#113266=DIRECTION('ref_axis',(-3.30569703989997E-8,0.289344971519085,-0.957224888652932));
#113267=DIRECTION('',(-6.19323182390956E-32,-1.23467863058847E-16,1.));
#113268=DIRECTION('center_axis',(0.997110719027039,-0.0759619154585161,
-3.74333490112874E-5));
#113269=DIRECTION('ref_axis',(0.0746245599506448,0.979463680395188,0.187302092457309));
#113270=DIRECTION('center_axis',(0.,0.,-1.));
#113271=DIRECTION('ref_axis',(-1.,0.,0.));
#113272=DIRECTION('center_axis',(-0.0109863751058524,0.174010750210057,
-0.984682465759072));
#113273=DIRECTION('ref_axis',(0.115492347803954,-0.977930751386158,-0.174106183382538));
#113274=DIRECTION('center_axis',(1.,-5.01606788234257E-16,0.));
#113275=DIRECTION('ref_axis',(-5.01606788234257E-16,-1.,0.));
#113276=DIRECTION('',(6.19323182390956E-32,1.23467863058847E-16,-1.));
#113277=DIRECTION('center_axis',(1.,0.,0.));
#113278=DIRECTION('ref_axis',(0.,0.97773854081723,0.20982694250404));
#113279=DIRECTION('',(6.19323182390956E-32,1.23467863058847E-16,-1.));
#113280=DIRECTION('center_axis',(0.,0.,-1.));
#113281=DIRECTION('ref_axis',(-1.,0.,0.));
#113282=DIRECTION('center_axis',(0.,0.,-1.));
#113283=DIRECTION('ref_axis',(-1.,0.,0.));
#113284=DIRECTION('center_axis',(-0.998403025832976,0.0564924526119683,
2.83803315785685E-5));
#113285=DIRECTION('ref_axis',(0.0553351197097672,0.977847823027442,0.201870402801399));
#113286=DIRECTION('center_axis',(0.,-1.18842113532926E-16,1.));
#113287=DIRECTION('ref_axis',(0.,1.,1.18842113532926E-16));
#113288=DIRECTION('center_axis',(-1.73309037721552E-31,1.19033121480991E-16,
-1.));
#113289=DIRECTION('ref_axis',(-3.90798504668055E-14,-1.,-1.19033121480991E-16));
#113290=DIRECTION('center_axis',(-1.,5.01606788234257E-16,0.));
#113291=DIRECTION('ref_axis',(0.,0.,1.));
#113292=DIRECTION('',(-6.19323182390956E-32,-1.23467863058847E-16,1.));
#113293=DIRECTION('center_axis',(-1.,0.,0.));
#113294=DIRECTION('ref_axis',(0.,0.976478786201388,0.215613497023408));
#113295=DIRECTION('',(-6.19323182390956E-32,-1.23467863058847E-16,1.));
#113296=DIRECTION('',(-2.85977186515575E-47,-5.70122241611331E-32,-1.));
#113297=DIRECTION('center_axis',(0.999946064618564,-0.0103859437316171,
-5.16237906977087E-6));
#113298=DIRECTION('ref_axis',(0.0101433645819431,0.976483796643044,0.215352053736538));
#113299=DIRECTION('center_axis',(0.,0.,-1.));
#113300=DIRECTION('ref_axis',(-1.,0.,0.));
#113301=DIRECTION('center_axis',(0.,0.,1.));
#113302=DIRECTION('ref_axis',(1.,0.,0.));
#113303=DIRECTION('center_axis',(2.85977186515575E-47,0.,1.));
#113304=DIRECTION('ref_axis',(0.,-1.,0.));
#113305=DIRECTION('center_axis',(1.0547118733939E-12,0.,1.));
#113306=DIRECTION('ref_axis',(1.,0.,-1.0547118733939E-12));
#113307=DIRECTION('',(2.85977186515575E-47,5.70122241611331E-32,1.));
#113308=DIRECTION('center_axis',(0.,0.,1.));
#113309=DIRECTION('ref_axis',(1.,0.,0.));
#113310=DIRECTION('center_axis',(-0.91200931366711,-0.410169491533009,-5.52463721181358E-12));
#113311=DIRECTION('ref_axis',(0.410169491533009,-0.91200931366711,-2.38205677224627E-27));
#113312=DIRECTION('center_axis',(0.,0.,-1.));
#113313=DIRECTION('ref_axis',(1.,0.,0.));
#113314=DIRECTION('center_axis',(-0.908150397510606,-0.418644067796653,
0.));
#113315=DIRECTION('ref_axis',(0.418644067796653,-0.908150397510606,0.));
#113316=DIRECTION('center_axis',(0.,0.,1.));
#113317=DIRECTION('ref_axis',(0.,-1.,0.));
#113318=DIRECTION('',(0.,-1.23467863058847E-16,1.));
#113319=DIRECTION('center_axis',(1.5706724042304E-30,1.99810034797076E-44,
-1.));
#113320=DIRECTION('ref_axis',(1.27213054904966E-14,-1.,2.98704733337335E-59));
#113321=DIRECTION('center_axis',(-0.999990764844661,-0.00426925256430225,
0.000493667835992639));
#113322=DIRECTION('ref_axis',(0.00426925308452771,-0.999990886697524,1.74890393922737E-21));
#113323=DIRECTION('center_axis',(0.,0.,-1.));
#113324=DIRECTION('ref_axis',(-1.,0.,0.));
#113325=DIRECTION('center_axis',(0.,0.,1.));
#113326=DIRECTION('ref_axis',(0.,-1.,0.));
#113327=DIRECTION('',(0.,1.23467863058847E-16,-1.));
#113328=DIRECTION('center_axis',(0.,-6.17339315294237E-17,1.));
#113329=DIRECTION('ref_axis',(0.,-1.,0.));
#113330=DIRECTION('center_axis',(-8.2246118621519E-31,1.09573841495595E-44,
-1.));
#113331=DIRECTION('ref_axis',(-1.33226762955019E-14,-1.,1.36906336112945E-59));
#113332=DIRECTION('center_axis',(0.,0.,1.));
#113333=DIRECTION('ref_axis',(0.664473794614039,0.747311565728258,0.));
#113334=DIRECTION('center_axis',(-1.66533453693774E-13,-1.96105155259282E-14,
-1.));
#113335=DIRECTION('ref_axis',(-1.,3.15330219577248E-42,1.66533453693774E-13));
#113336=DIRECTION('',(0.,-1.23467863058847E-16,1.));
#113337=DIRECTION('center_axis',(-0.99077695153738,-0.134510490459868,0.0163694917007939));
#113338=DIRECTION('ref_axis',(0.134528515815408,-0.990909722645057,-8.11100475129765E-19));
#113339=DIRECTION('center_axis',(0.00303671055821314,-0.143796114085276,
-0.989602675806285));
#113340=DIRECTION('ref_axis',(0.135485018598647,-0.980423214395597,0.142878026335506));
#113341=DIRECTION('center_axis',(-0.989571111262359,-0.142966967401199,
0.017591531686721));
#113342=DIRECTION('ref_axis',(0.142989093957737,-0.989724264130745,-6.72869096378782E-19));
#113343=DIRECTION('center_axis',(0.,0.,-1.));
#113344=DIRECTION('ref_axis',(-1.,0.,0.));
#113345=DIRECTION('center_axis',(0.,0.,1.));
#113346=DIRECTION('ref_axis',(0.,-1.,0.));
#113347=DIRECTION('',(0.,1.23467863058847E-16,-1.));
#113348=DIRECTION('center_axis',(0.,-6.17339315294237E-17,1.));
#113349=DIRECTION('ref_axis',(0.,-1.,0.));
#113350=DIRECTION('center_axis',(2.19322982990717E-31,7.79191761746451E-46,
-1.));
#113351=DIRECTION('ref_axis',(3.5527136788005E-15,-1.,-1.0890276736257E-60));
#113352=DIRECTION('center_axis',(0.,0.,1.));
#113353=DIRECTION('ref_axis',(0.610293066582435,0.792175720961838,0.));
#113354=DIRECTION('center_axis',(0.,0.,-1.));
#113355=DIRECTION('ref_axis',(-1.,0.,0.));
#113356=DIRECTION('',(0.,-1.23467863058847E-16,1.));
#113357=DIRECTION('center_axis',(-0.962287669136798,-0.272033898305467,
-2.53734057564779E-13));
#113358=DIRECTION('ref_axis',(0.272033898305467,-0.962287669136798,2.03523668564842E-29));
#113359=DIRECTION('center_axis',(0.,0.,1.));
#113360=DIRECTION('ref_axis',(1.,0.,0.));
#113361=DIRECTION('center_axis',(0.,0.,-1.));
#113362=DIRECTION('ref_axis',(1.,0.,0.));
#113363=DIRECTION('center_axis',(-0.959851548777671,-0.280508474576272,
0.));
#113364=DIRECTION('ref_axis',(0.280508474576272,-0.959851548777671,0.));
#113365=DIRECTION('center_axis',(0.,0.,-1.));
#113366=DIRECTION('ref_axis',(-1.,0.,0.));
#113367=DIRECTION('center_axis',(0.,0.,1.));
#113368=DIRECTION('ref_axis',(0.,-1.,0.));
#113369=DIRECTION('',(0.,1.23467863058847E-16,-1.));
#113370=DIRECTION('center_axis',(0.,-6.17339315294237E-17,1.));
#113371=DIRECTION('ref_axis',(0.,-1.,0.));
#113372=DIRECTION('center_axis',(1.37076864369198E-30,3.04371781932207E-44,
-1.));
#113373=DIRECTION('ref_axis',(2.22044604925031E-14,-1.,3.98272977783113E-59));
#113374=DIRECTION('center_axis',(0.,0.,1.));
#113375=DIRECTION('ref_axis',(0.550808342809402,0.834631756819474,0.));
#113376=DIRECTION('center_axis',(0.,0.,-1.));
#113377=DIRECTION('ref_axis',(-1.,0.,0.));
#113378=DIRECTION('',(0.,-1.23467863058847E-16,1.));
#113379=DIRECTION('center_axis',(0.,0.,-1.));
#113380=DIRECTION('ref_axis',(0.,1.,0.));
#113381=DIRECTION('',(0.,0.,-1.));
#113382=DIRECTION('center_axis',(0.,0.,-1.));
#113383=DIRECTION('ref_axis',(0.,1.,0.));
#113384=DIRECTION('center_axis',(0.,0.,-1.));
#113385=DIRECTION('ref_axis',(0.,1.,0.));
#113386=DIRECTION('',(0.,0.,-1.));
#113387=DIRECTION('center_axis',(0.,0.,-1.));
#113388=DIRECTION('ref_axis',(0.,-1.,0.));
#113389=DIRECTION('center_axis',(0.,-1.23467863058847E-16,1.));
#113390=DIRECTION('ref_axis',(0.,-1.,0.));
#113391=DIRECTION('center_axis',(0.902736181373369,0.430194591829591,-1.25279811715363E-14));
#113392=DIRECTION('ref_axis',(-0.430194591829591,0.902736181373369,2.66752875008673E-30));
#113393=DIRECTION('center_axis',(0.,0.,1.));
#113394=DIRECTION('ref_axis',(0.,-1.,0.));
#113395=DIRECTION('center_axis',(0.990268068741571,0.139173100960064,0.));
#113396=DIRECTION('ref_axis',(-0.139173100960064,0.990268068741571,0.));
#113397=DIRECTION('center_axis',(0.990268068741571,0.139173100960064,1.71834053708117E-17));
#113398=DIRECTION('ref_axis',(-0.139173100960064,0.990268068741571,-7.54967553857625E-35));
#113399=DIRECTION('',(-0.990268068741571,-0.139173100960059,-1.71834053708117E-17));
#113400=DIRECTION('center_axis',(0.990268068741571,0.139173100960064,7.72565905471723E-15));
#113401=DIRECTION('ref_axis',(-0.139173100960064,0.990268068741571,-6.67502150120727E-33));
#113402=DIRECTION('center_axis',(0.,-1.23467863058847E-16,1.));
#113403=DIRECTION('ref_axis',(0.,-1.,0.));
#113404=DIRECTION('center_axis',(3.11538328111815E-31,7.86084147552191E-46,
-1.));
#113405=DIRECTION('ref_axis',(2.52323414687536E-15,-1.,-6.22301527786114E-61));
#113406=DIRECTION('center_axis',(0.728126055379271,0.685443248911113,0.));
#113407=DIRECTION('ref_axis',(-0.685443248911113,0.728126055379271,0.));
#113408=DIRECTION('center_axis',(0.,-1.23467863058847E-16,1.));
#113409=DIRECTION('ref_axis',(0.,-1.,0.));
#113410=DIRECTION('center_axis',(0.,0.,-1.));
#113411=DIRECTION('ref_axis',(0.,-1.,0.));
#113412=DIRECTION('center_axis',(0.685443248911113,0.728126055379271,1.18468586241421E-15));
#113413=DIRECTION('ref_axis',(-0.728126055379271,0.685443248911113,-2.6468713136043E-31));
#113414=DIRECTION('center_axis',(0.,-1.23467863058847E-16,1.));
#113415=DIRECTION('ref_axis',(0.,-1.,0.));
#113416=DIRECTION('center_axis',(-1.24615331244726E-30,1.2577346360835E-44,
-1.));
#113417=DIRECTION('ref_axis',(-1.00929365875014E-14,-1.,-9.95682444457783E-60));
#113418=DIRECTION('center_axis',(0.139173100960064,0.990268068741571,3.86282952735861E-15));
#113419=DIRECTION('ref_axis',(-0.990268068741571,0.139173100960064,3.00533800087463E-32));
#113420=DIRECTION('center_axis',(0.139173100960064,0.990268068741571,1.22266282302934E-16));
#113421=DIRECTION('ref_axis',(-0.990268068741571,0.139173100960064,-6.46427645420959E-34));
#113422=DIRECTION('',(-0.139173100960065,-0.99026806874157,-1.22266282302933E-16));
#113423=DIRECTION('center_axis',(0.139173100960068,0.99026806874157,0.));
#113424=DIRECTION('ref_axis',(-0.99026806874157,0.139173100960068,0.));
#113425=DIRECTION('center_axis',(0.,-1.23467863058847E-16,1.));
#113426=DIRECTION('ref_axis',(0.,-1.,0.));
#113427=DIRECTION('center_axis',(0.,0.,1.));
#113428=DIRECTION('ref_axis',(0.,-1.,0.));
#113429=DIRECTION('center_axis',(0.425784239486448,0.90482472413443,-1.18178866550092E-14));
#113430=DIRECTION('ref_axis',(-0.90482472413443,0.425784239486448,3.74967935723291E-30));
#113431=DIRECTION('center_axis',(0.,-1.23467863058847E-16,1.));
#113432=DIRECTION('ref_axis',(0.,-1.,0.));
#113433=DIRECTION('center_axis',(-2.19322982990717E-31,3.89595880873225E-46,
-1.));
#113434=DIRECTION('ref_axis',(-1.77635683940025E-15,-1.,-5.4451383681285E-61));
#113435=DIRECTION('center_axis',(-0.425784239486454,0.904824724134427,0.));
#113436=DIRECTION('ref_axis',(-0.904824724134427,-0.425784239486454,0.));
#113437=DIRECTION('center_axis',(0.,-1.23467863058847E-16,1.));
#113438=DIRECTION('ref_axis',(0.,-1.,0.));
#113439=DIRECTION('center_axis',(0.,0.,1.));
#113440=DIRECTION('ref_axis',(0.,-1.,0.));
#113441=DIRECTION('center_axis',(-0.139173100960068,0.99026806874157,0.));
#113442=DIRECTION('ref_axis',(-0.99026806874157,-0.139173100960068,0.));
#113443=DIRECTION('center_axis',(-0.139173100960068,0.99026806874157,1.22266282302933E-16));
#113444=DIRECTION('ref_axis',(-0.99026806874157,-0.139173100960068,-6.9848527780828E-33));
#113445=DIRECTION('',(0.139173100960067,-0.99026806874157,-1.22266282302933E-16));
#113446=DIRECTION('center_axis',(-0.139173100960068,0.99026806874157,2.36226307343407E-14));
#113447=DIRECTION('ref_axis',(-0.99026806874157,-0.139173100960068,-1.46728138438144E-30));
#113448=DIRECTION('center_axis',(0.,-1.23467863058847E-16,1.));
#113449=DIRECTION('ref_axis',(0.,-1.,0.));
#113450=DIRECTION('center_axis',(-6.23076656223629E-31,3.14433659020876E-45,
-1.));
#113451=DIRECTION('ref_axis',(-5.04646829375071E-15,-1.,1.86690458335834E-60));
#113452=DIRECTION('center_axis',(-0.685443248911113,0.728126055379271,1.18468586241421E-15));
#113453=DIRECTION('ref_axis',(-0.728126055379271,-0.685443248911113,2.6468713136043E-31));
#113454=DIRECTION('center_axis',(0.,-1.23467863058847E-16,1.));
#113455=DIRECTION('ref_axis',(0.,-1.,0.));
#113456=DIRECTION('center_axis',(0.,0.,-1.));
#113457=DIRECTION('ref_axis',(0.,-1.,0.));
#113458=DIRECTION('center_axis',(-0.728126055379271,0.685443248911113,-1.18468586241421E-15));
#113459=DIRECTION('ref_axis',(-0.685443248911113,-0.728126055379271,2.48798705504199E-31));
#113460=DIRECTION('center_axis',(0.,-1.23467863058847E-16,1.));
#113461=DIRECTION('ref_axis',(0.,-1.,0.));
#113462=DIRECTION('center_axis',(3.11538328111815E-31,7.86084147552189E-46,
-1.));
#113463=DIRECTION('ref_axis',(2.52323414687536E-15,-1.,3.11150763893057E-61));
#113464=DIRECTION('center_axis',(-0.990268068741571,0.139173100960064,3.86282952735861E-15));
#113465=DIRECTION('ref_axis',(-0.139173100960064,-0.990268068741571,3.33751075060364E-33));
#113466=DIRECTION('center_axis',(-0.990268068741571,0.139173100960064,1.71834053708117E-17));
#113467=DIRECTION('ref_axis',(-0.139173100960064,-0.990268068741571,7.54967553857625E-35));
#113468=DIRECTION('',(0.990268068741571,-0.139173100960059,-1.71834053708117E-17));
#113469=DIRECTION('center_axis',(-0.990268068741572,0.139173100960051,1.7605559658208E-14));
#113470=DIRECTION('ref_axis',(-0.139173100960051,-0.990268068741572,2.08829111071605E-30));
#113471=DIRECTION('center_axis',(0.,-1.23467863058847E-16,1.));
#113472=DIRECTION('ref_axis',(0.,-1.,0.));
#113473=DIRECTION('center_axis',(0.,0.,1.));
#113474=DIRECTION('ref_axis',(0.,-1.,0.));
#113475=DIRECTION('center_axis',(-0.904824724134424,0.42578423948646,0.));
#113476=DIRECTION('ref_axis',(-0.42578423948646,-0.904824724134424,0.));
#113477=DIRECTION('center_axis',(0.,0.,-1.));
#113478=DIRECTION('ref_axis',(0.,-1.,0.));
#113479=DIRECTION('center_axis',(0.,0.,1.));
#113480=DIRECTION('ref_axis',(0.,-1.,0.));
#113481=DIRECTION('',(0.,1.23467863058847E-16,-1.));
#113482=DIRECTION('center_axis',(0.,0.,1.));
#113483=DIRECTION('ref_axis',(1.,0.,0.));
#113484=DIRECTION('center_axis',(0.990268068741572,-0.139173100960052,0.));
#113485=DIRECTION('ref_axis',(0.139173100960052,0.990268068741572,0.));
#113486=DIRECTION('center_axis',(0.990268068741571,-0.139173100960059,0.));
#113487=DIRECTION('ref_axis',(0.139173100960059,0.990268068741571,0.));
#113488=DIRECTION('',(-0.990268068741571,0.139173100960059,0.));
#113489=DIRECTION('center_axis',(0.,0.,1.));
#113490=DIRECTION('ref_axis',(1.,0.,0.));
#113491=DIRECTION('center_axis',(0.904824724134427,-0.425784239486454,0.));
#113492=DIRECTION('ref_axis',(0.425784239486454,0.904824724134427,0.));
#113493=DIRECTION('center_axis',(0.,0.,-1.));
#113494=DIRECTION('ref_axis',(1.,-1.5419764230905E-15,0.));
#113495=DIRECTION('center_axis',(0.,-1.,0.));
#113496=DIRECTION('ref_axis',(0.,0.,-1.));
#113497=DIRECTION('',(0.,1.,0.));
#113498=DIRECTION('',(0.,-1.,0.));
#113499=DIRECTION('center_axis',(0.,1.,0.));
#113500=DIRECTION('ref_axis',(0.,0.,-1.));
#113501=DIRECTION('center_axis',(-1.,0.,-1.6326809185664E-16));
#113502=DIRECTION('ref_axis',(-1.6326809185664E-16,0.,1.));
#113503=DIRECTION('',(1.6326809185664E-16,0.,-1.));
#113504=DIRECTION('',(0.,-1.,0.));
#113505=DIRECTION('center_axis',(0.,-1.,0.));
#113506=DIRECTION('ref_axis',(0.,0.,-1.));
#113507=DIRECTION('center_axis',(0.,-1.,0.));
#113508=DIRECTION('ref_axis',(0.,0.,-1.));
#113509=DIRECTION('',(0.,1.,0.));
#113510=DIRECTION('center_axis',(1.,0.,0.));
#113511=DIRECTION('ref_axis',(0.,1.,0.));
#113512=DIRECTION('',(1.,-4.38004274807345E-16,0.));
#113513=DIRECTION('center_axis',(0.,-1.,0.));
#113514=DIRECTION('ref_axis',(0.,0.,-1.));
#113515=DIRECTION('center_axis',(0.,1.,0.));
#113516=DIRECTION('ref_axis',(0.,0.,1.));
#113517=DIRECTION('',(0.,-1.,0.));
#113518=DIRECTION('center_axis',(0.,0.,-1.));
#113519=DIRECTION('ref_axis',(-1.,0.,0.));
#113520=DIRECTION('center_axis',(-1.,0.,0.));
#113521=DIRECTION('ref_axis',(0.,0.,1.));
#113522=DIRECTION('center_axis',(0.,0.,-1.));
#113523=DIRECTION('ref_axis',(-1.,0.,0.));
#113524=DIRECTION('center_axis',(1.,0.,0.));
#113525=DIRECTION('ref_axis',(0.,0.,-1.));
#113526=DIRECTION('center_axis',(-1.,0.,0.));
#113527=DIRECTION('ref_axis',(0.,0.,1.));
#113528=DIRECTION('',(1.,0.,0.));
#113529=DIRECTION('center_axis',(0.,0.,-1.));
#113530=DIRECTION('ref_axis',(-1.,0.,0.));
#113531=DIRECTION('center_axis',(0.,-1.,0.));
#113532=DIRECTION('ref_axis',(0.,0.,-1.));
#113533=DIRECTION('center_axis',(0.,0.,-1.));
#113534=DIRECTION('ref_axis',(-1.,0.,0.));
#113535=DIRECTION('center_axis',(0.,-1.,0.));
#113536=DIRECTION('ref_axis',(0.,0.,-1.));
#113537=DIRECTION('',(0.,1.,0.));
#113538=DIRECTION('center_axis',(1.,0.,0.));
#113539=DIRECTION('ref_axis',(0.,1.,0.));
#113540=DIRECTION('',(1.,-4.38004274807345E-16,0.));
#113541=DIRECTION('center_axis',(0.,-1.,0.));
#113542=DIRECTION('ref_axis',(0.,0.,-1.));
#113543=DIRECTION('center_axis',(0.,1.,0.));
#113544=DIRECTION('ref_axis',(0.,0.,1.));
#113545=DIRECTION('',(0.,-1.,0.));
#113546=DIRECTION('center_axis',(0.,0.,-1.));
#113547=DIRECTION('ref_axis',(-1.,0.,0.));
#113548=DIRECTION('center_axis',(-1.,0.,0.));
#113549=DIRECTION('ref_axis',(0.,0.,1.));
#113550=DIRECTION('center_axis',(0.,0.,-1.));
#113551=DIRECTION('ref_axis',(-1.,0.,0.));
#113552=DIRECTION('center_axis',(1.,0.,0.));
#113553=DIRECTION('ref_axis',(0.,0.,-1.));
#113554=DIRECTION('center_axis',(-1.,0.,0.));
#113555=DIRECTION('ref_axis',(0.,0.,1.));
#113556=DIRECTION('',(1.,0.,0.));
#113557=DIRECTION('center_axis',(0.,0.,-1.));
#113558=DIRECTION('ref_axis',(-1.,0.,0.));
#113559=DIRECTION('center_axis',(0.,-1.,0.));
#113560=DIRECTION('ref_axis',(0.,0.,-1.));
#113561=DIRECTION('center_axis',(0.,0.,-1.));
#113562=DIRECTION('ref_axis',(-1.,0.,0.));
#113563=DIRECTION('center_axis',(0.,-1.,0.));
#113564=DIRECTION('ref_axis',(0.,0.,-1.));
#113565=DIRECTION('',(0.,1.,0.));
#113566=DIRECTION('center_axis',(1.,0.,0.));
#113567=DIRECTION('ref_axis',(0.,1.,0.));
#113568=DIRECTION('',(1.,-4.38004274807345E-16,0.));
#113569=DIRECTION('center_axis',(1.,0.,-1.73472347597681E-14));
#113570=DIRECTION('ref_axis',(-1.73472347597681E-14,0.,-1.));
#113571=DIRECTION('center_axis',(0.950554487276066,-0.310557831521497,3.79371153572051E-14));
#113572=DIRECTION('ref_axis',(0.310557831521497,0.950554487276066,1.69736969313821E-30));
#113573=DIRECTION('center_axis',(0.,0.,-1.));
#113574=DIRECTION('ref_axis',(-1.,0.,0.));
#113575=DIRECTION('center_axis',(0.,0.,-1.));
#113576=DIRECTION('ref_axis',(-1.,0.,0.));
#113577=DIRECTION('center_axis',(0.,-1.,0.));
#113578=DIRECTION('ref_axis',(0.,0.,-1.));
#113579=DIRECTION('center_axis',(0.,1.,0.));
#113580=DIRECTION('ref_axis',(0.,0.,1.));
#113581=DIRECTION('',(0.,-1.,0.));
#113582=DIRECTION('center_axis',(0.,0.,-1.));
#113583=DIRECTION('ref_axis',(-1.,0.,0.));
#113584=DIRECTION('center_axis',(-1.,0.,0.));
#113585=DIRECTION('ref_axis',(0.,0.,1.));
#113586=DIRECTION('center_axis',(0.,0.,-1.));
#113587=DIRECTION('ref_axis',(-1.,0.,0.));
#113588=DIRECTION('center_axis',(1.,0.,0.));
#113589=DIRECTION('ref_axis',(0.,0.,-1.));
#113590=DIRECTION('center_axis',(-1.,0.,0.));
#113591=DIRECTION('ref_axis',(0.,0.,1.));
#113592=DIRECTION('',(1.,0.,0.));
#113593=DIRECTION('center_axis',(0.,0.,-1.));
#113594=DIRECTION('ref_axis',(-1.,0.,0.));
#113595=DIRECTION('center_axis',(0.,-1.,0.));
#113596=DIRECTION('ref_axis',(0.,0.,-1.));
#113597=DIRECTION('center_axis',(0.,0.,-1.));
#113598=DIRECTION('ref_axis',(-1.,0.,0.));
#113599=DIRECTION('center_axis',(0.,-1.,0.));
#113600=DIRECTION('ref_axis',(0.,0.,-1.));
#113601=DIRECTION('',(0.,1.,0.));
#113602=DIRECTION('center_axis',(0.,0.,-1.));
#113603=DIRECTION('ref_axis',(-1.,0.,0.));
#113604=DIRECTION('center_axis',(0.,0.,-1.));
#113605=DIRECTION('ref_axis',(-1.,0.,0.));
#113606=DIRECTION('center_axis',(0.,-1.,0.));
#113607=DIRECTION('ref_axis',(0.,0.,-1.));
#113608=DIRECTION('center_axis',(0.,1.,0.));
#113609=DIRECTION('ref_axis',(0.,0.,1.));
#113610=DIRECTION('',(0.,-1.,0.));
#113611=DIRECTION('center_axis',(0.,0.,-1.));
#113612=DIRECTION('ref_axis',(-1.,0.,0.));
#113613=DIRECTION('center_axis',(-1.,0.,0.));
#113614=DIRECTION('ref_axis',(0.,0.,1.));
#113615=DIRECTION('center_axis',(0.,0.,-1.));
#113616=DIRECTION('ref_axis',(-1.,0.,0.));
#113617=DIRECTION('center_axis',(1.,0.,0.));
#113618=DIRECTION('ref_axis',(0.,0.,-1.));
#113619=DIRECTION('center_axis',(-1.,0.,0.));
#113620=DIRECTION('ref_axis',(0.,0.,1.));
#113621=DIRECTION('',(1.,0.,0.));
#113622=DIRECTION('center_axis',(0.,0.,-1.));
#113623=DIRECTION('ref_axis',(-1.,0.,0.));
#113624=DIRECTION('center_axis',(0.,-1.,0.));
#113625=DIRECTION('ref_axis',(0.,0.,-1.));
#113626=DIRECTION('center_axis',(0.,0.,-1.));
#113627=DIRECTION('ref_axis',(-1.,0.,0.));
#113628=DIRECTION('center_axis',(0.,-1.,0.));
#113629=DIRECTION('ref_axis',(0.,0.,-1.));
#113630=DIRECTION('center_axis',(0.,-1.,0.));
#113631=DIRECTION('ref_axis',(0.,0.,-1.));
#113632=DIRECTION('',(0.,1.,0.));
#113633=DIRECTION('center_axis',(0.,-1.,0.));
#113634=DIRECTION('ref_axis',(0.,0.,-1.));
#113635=DIRECTION('center_axis',(0.,1.,0.));
#113636=DIRECTION('ref_axis',(0.,0.,-1.));
#113637=DIRECTION('',(0.,1.,0.));
#113638=DIRECTION('center_axis',(1.,0.,0.));
#113639=DIRECTION('ref_axis',(0.,0.,-1.));
#113640=DIRECTION('center_axis',(-1.,0.,0.));
#113641=DIRECTION('ref_axis',(0.,0.,1.));
#113642=DIRECTION('',(1.,0.,0.));
#113643=DIRECTION('center_axis',(0.,0.,-1.));
#113644=DIRECTION('ref_axis',(-1.,0.,0.));
#113645=DIRECTION('center_axis',(0.,0.,-1.));
#113646=DIRECTION('ref_axis',(-1.,0.,0.));
#113647=DIRECTION('center_axis',(0.,0.423401464461212,0.905942161449671));
#113648=DIRECTION('ref_axis',(0.,-0.905942161449671,0.423401464461211));
#113649=DIRECTION('center_axis',(0.999426495211847,-0.0338626728150633,
-7.64099929122785E-6));
#113650=DIRECTION('ref_axis',(-0.00722436375911664,-0.213000171029248,-0.97702545294879));
#113651=DIRECTION('center_axis',(6.703313282803E-15,0.423071618151431,0.90609624539269));
#113652=DIRECTION('ref_axis',(-9.44993610611347E-31,-0.90609624539269,0.423071618151431));
#113653=DIRECTION('center_axis',(-0.999690772268051,-0.0248668391563904,
1.23482154850145E-5));
#113654=DIRECTION('ref_axis',(0.0242988167036592,-0.976749496966587,0.213002318490482));
#113655=DIRECTION('center_axis',(0.,0.,-1.));
#113656=DIRECTION('ref_axis',(-1.,0.,0.));
#113657=DIRECTION('center_axis',(0.,-1.,0.));
#113658=DIRECTION('ref_axis',(1.,0.,0.));
#113659=DIRECTION('',(5.01606788234257E-16,1.,0.));
#113660=DIRECTION('center_axis',(0.,0.,-1.));
#113661=DIRECTION('ref_axis',(0.,-1.,0.));
#113662=DIRECTION('center_axis',(0.,0.,1.));
#113663=DIRECTION('ref_axis',(-1.,-5.55111512312579E-15,0.));
#113664=DIRECTION('center_axis',(0.,0.,-1.));
#113665=DIRECTION('ref_axis',(-1.,0.,0.));
#113666=DIRECTION('center_axis',(0.,1.23467863058847E-16,-1.));
#113667=DIRECTION('ref_axis',(-1.,0.,0.));
#113668=DIRECTION('',(-0.996194698091747,-0.0871557427476402,-1.07609333103578E-17));
#113669=DIRECTION('',(-0.0871557427476402,-0.996194698091747,-1.22998030563942E-16));
#113670=DIRECTION('center_axis',(0.,0.,-1.));
#113671=DIRECTION('ref_axis',(0.,1.,0.));
#113672=DIRECTION('',(-0.707106781186547,-0.707106781186548,-8.73049632275231E-17));
#113673=DIRECTION('center_axis',(0.,0.,-1.));
#113674=DIRECTION('ref_axis',(0.,1.,0.));
#113675=DIRECTION('center_axis',(0.,1.23467863058847E-16,-1.));
#113676=DIRECTION('ref_axis',(-1.,0.,0.));
#113677=DIRECTION('',(0.0871557427476566,-0.996194698091746,-1.22998030563941E-16));
#113678=DIRECTION('',(0.996194698091746,-0.0871557427476568,-1.07609333103598E-17));
#113679=DIRECTION('center_axis',(0.,0.,-1.));
#113680=DIRECTION('ref_axis',(0.,1.,0.));
#113681=DIRECTION('',(0.707106781186547,-0.707106781186548,-8.73049632275231E-17));
#113682=DIRECTION('center_axis',(0.,0.,-1.));
#113683=DIRECTION('ref_axis',(0.,1.,0.));
#113684=DIRECTION('center_axis',(-0.0871557427476394,-0.996194698091747,
-1.22998030563942E-16));
#113685=DIRECTION('ref_axis',(0.996194698091747,-0.0871557427476394,8.16488070285074E-35));
#113686=DIRECTION('',(0.0871557427476402,0.996194698091747,1.22998030563942E-16));
#113687=DIRECTION('center_axis',(0.0871557427476394,0.996194698091747,0.));
#113688=DIRECTION('ref_axis',(-0.996194698091747,0.0871557427476394,0.));
#113689=DIRECTION('center_axis',(0.,4.51531312649963E-33,-1.));
#113690=DIRECTION('ref_axis',(-1.,0.,0.));
#113691=DIRECTION('center_axis',(0.,0.,-1.));
#113692=DIRECTION('ref_axis',(-1.,0.,0.));
#113693=DIRECTION('',(-1.08020383274181E-17,4.42963887209064E-33,-1.));
#113694=DIRECTION('center_axis',(0.,0.,-1.));
#113695=DIRECTION('ref_axis',(-1.,0.,0.));
#113696=DIRECTION('center_axis',(-0.0871557427476469,-0.996194698091747,
1.3824978635387E-14));
#113697=DIRECTION('ref_axis',(0.996194698091747,-0.0871557427476469,-9.13671722807069E-31));
#113698=DIRECTION('center_axis',(0.0871557427476469,0.996194698091747,0.));
#113699=DIRECTION('ref_axis',(-0.996194698091747,0.0871557427476469,0.));
#113700=DIRECTION('center_axis',(-0.0871557427476469,-0.996194698091747,
0.));
#113701=DIRECTION('ref_axis',(0.996194698091747,-0.0871557427476469,0.));
#113702=DIRECTION('',(0.0871557427476402,0.996194698091747,0.));
#113703=DIRECTION('center_axis',(0.,0.,-1.));
#113704=DIRECTION('ref_axis',(-1.,0.,0.));
#113705=DIRECTION('center_axis',(0.,-4.51531312649963E-33,1.));
#113706=DIRECTION('ref_axis',(1.,0.,0.));
#113707=DIRECTION('',(1.08020383274181E-17,-4.42963887209064E-33,1.));
#113708=DIRECTION('center_axis',(-0.0871557427476394,-0.996194698091747,
-1.22998030563942E-16));
#113709=DIRECTION('ref_axis',(0.996194698091747,-0.0871557427476394,8.16488070285074E-35));
#113710=DIRECTION('',(0.0871557427476402,0.996194698091747,1.22998030563942E-16));
#113711=DIRECTION('center_axis',(0.,-4.51531312649963E-33,1.));
#113712=DIRECTION('ref_axis',(-0.737277336810104,-0.675590207615682,-3.0505013325817E-33));
#113713=DIRECTION('center_axis',(0.,0.,1.));
#113714=DIRECTION('ref_axis',(1.,0.,0.));
#113715=DIRECTION('',(-1.08020383274181E-17,4.42963887209064E-33,-1.));
#113716=DIRECTION('center_axis',(-0.0871557427476469,-0.996194698091747,
0.));
#113717=DIRECTION('ref_axis',(0.996194698091747,-0.0871557427476469,0.));
#113718=DIRECTION('center_axis',(0.0871557427476469,0.996194698091747,0.));
#113719=DIRECTION('ref_axis',(-0.996194698091747,0.0871557427476469,0.));
#113720=DIRECTION('center_axis',(-0.0871557427476469,-0.996194698091747,
1.3824978635387E-14));
#113721=DIRECTION('ref_axis',(0.996194698091747,-0.0871557427476469,-9.13671722807069E-31));
#113722=DIRECTION('',(0.0871557427476402,0.996194698091747,0.));
#113723=DIRECTION('center_axis',(0.,0.,-1.));
#113724=DIRECTION('ref_axis',(-1.,0.,0.));
#113725=DIRECTION('center_axis',(0.,-4.73133896404192E-33,1.));
#113726=DIRECTION('ref_axis',(1.,0.,0.));
#113727=DIRECTION('',(1.08020383274181E-17,-4.62223186652937E-33,1.));
#113728=DIRECTION('center_axis',(-0.0871557427476394,-0.996194698091747,
-1.22998030563942E-16));
#113729=DIRECTION('ref_axis',(0.996194698091747,-0.0871557427476394,8.16488070285074E-35));
#113730=DIRECTION('',(0.0871557427476402,0.996194698091747,1.22998030563942E-16));
#113731=DIRECTION('center_axis',(0.0871557427476394,0.996194698091747,0.));
#113732=DIRECTION('ref_axis',(-0.996194698091747,0.0871557427476394,0.));
#113733=DIRECTION('center_axis',(-0.0690733635565107,-0.78951215817867,
-0.609835570080205));
#113734=DIRECTION('ref_axis',(3.95541556389227E-18,0.611295598907861,-0.791402357057319));
#113735=DIRECTION('center_axis',(-0.996194698091743,0.0871557427476822,
-4.52226792607938E-16));
#113736=DIRECTION('ref_axis',(0.039915296454851,0.456233926159048,0.888964213976255));
#113737=DIRECTION('center_axis',(0.,0.,1.));
#113738=DIRECTION('ref_axis',(1.,0.,0.));
#113739=DIRECTION('center_axis',(0.,4.51531312649963E-33,-1.));
#113740=DIRECTION('ref_axis',(-1.,0.,0.));
#113741=DIRECTION('',(1.08020383274181E-17,-4.42963887209064E-33,1.));
#113742=DIRECTION('center_axis',(0.,-4.51531312650048E-33,-1.));
#113743=DIRECTION('ref_axis',(-1.,0.,0.));
#113744=DIRECTION('',(1.08020383274202E-17,-4.37133056147834E-33,-1.));
#113745=DIRECTION('center_axis',(0.,0.,-1.));
#113746=DIRECTION('ref_axis',(-1.,0.,0.));
#113747=DIRECTION('center_axis',(0.0871557427476538,-0.996194698091746,
-6.91248931769351E-15));
#113748=DIRECTION('ref_axis',(0.996194698091746,0.0871557427476538,2.78649888037662E-32));
#113749=DIRECTION('center_axis',(-0.0871557427476538,0.996194698091746,
0.));
#113750=DIRECTION('ref_axis',(-0.996194698091746,-0.0871557427476538,0.));
#113751=DIRECTION('center_axis',(0.0871557427476538,-0.996194698091746,
-6.91248931769351E-15));
#113752=DIRECTION('ref_axis',(0.996194698091746,0.0871557427476538,2.78649888037662E-32));
#113753=DIRECTION('',(-0.0871557427476566,0.996194698091746,0.));
#113754=DIRECTION('center_axis',(0.,0.,-1.));
#113755=DIRECTION('ref_axis',(-1.,0.,0.));
#113756=DIRECTION('center_axis',(0.,4.51531312650048E-33,1.));
#113757=DIRECTION('ref_axis',(-0.737277336810102,0.675590207615685,-3.05050133258229E-33));
#113758=DIRECTION('',(-1.08020383274202E-17,4.37133056147834E-33,1.));
#113759=DIRECTION('center_axis',(0.0871557427476572,-0.996194698091746,
-1.22998030563942E-16));
#113760=DIRECTION('ref_axis',(0.996194698091746,0.0871557427476572,1.44426287624373E-33));
#113761=DIRECTION('',(-0.0871557427476566,0.996194698091746,1.22998030563941E-16));
#113762=DIRECTION('center_axis',(0.0871557427476607,-0.996194698091745,
0.));
#113763=DIRECTION('ref_axis',(0.996194698091745,0.0871557427476607,0.));
#113764=DIRECTION('center_axis',(0.,4.51531312650048E-33,1.));
#113765=DIRECTION('ref_axis',(1.,0.,0.));
#113766=DIRECTION('center_axis',(0.,0.,1.));
#113767=DIRECTION('ref_axis',(1.,0.,0.));
#113768=DIRECTION('',(1.08020383274202E-17,-4.37133056147834E-33,-1.));
#113769=DIRECTION('center_axis',(0.0479130906931042,-0.547649132616206,
0.835335120346889));
#113770=DIRECTION('ref_axis',(2.39380283931159E-17,-0.836295598856108,-0.54827882626808));
#113771=DIRECTION('center_axis',(-0.996194698091723,-0.0871557427479135,
-1.21464724749175E-13));
#113772=DIRECTION('ref_axis',(-0.0257890725821804,0.294770448454491,-0.955220030387392));
#113773=DIRECTION('center_axis',(0.0871557427476572,-0.996194698091746,
-1.22998030563942E-16));
#113774=DIRECTION('ref_axis',(0.996194698091746,0.0871557427476572,1.44426287624373E-33));
#113775=DIRECTION('',(-0.0871557427476566,0.996194698091746,1.22998030563941E-16));
#113776=DIRECTION('center_axis',(-0.0871557427476572,0.996194698091746,
0.));
#113777=DIRECTION('ref_axis',(-0.996194698091746,-0.0871557427476572,0.));
#113778=DIRECTION('center_axis',(0.,-4.73133896404282E-33,-1.));
#113779=DIRECTION('ref_axis',(-1.,0.,0.));
#113780=DIRECTION('',(1.08020383274202E-17,-4.56392355591706E-33,-1.));
#113781=DIRECTION('center_axis',(0.,0.,-1.));
#113782=DIRECTION('ref_axis',(-1.,0.,0.));
#113783=DIRECTION('center_axis',(-0.0871557427476538,0.996194698091746,
0.));
#113784=DIRECTION('ref_axis',(-0.996194698091746,-0.0871557427476538,0.));
#113785=DIRECTION('center_axis',(-0.0871557427476538,0.996194698091746,
0.));
#113786=DIRECTION('ref_axis',(-0.996194698091746,-0.0871557427476538,0.));
#113787=DIRECTION('',(-0.0871557427476566,0.996194698091746,0.));
#113788=DIRECTION('center_axis',(-0.0871557427476538,0.996194698091746,
0.));
#113789=DIRECTION('ref_axis',(-0.996194698091746,-0.0871557427476538,0.));
#113790=DIRECTION('center_axis',(0.,0.,1.));
#113791=DIRECTION('ref_axis',(1.,0.,0.));
#113792=DIRECTION('center_axis',(0.,4.51531312650048E-33,1.));
#113793=DIRECTION('ref_axis',(-0.737277336810104,0.675590207615683,-3.05050133258228E-33));
#113794=DIRECTION('',(-1.08020383274202E-17,4.37133056147834E-33,1.));
#113795=DIRECTION('center_axis',(0.0871557427476572,-0.996194698091746,
-1.22998030563942E-16));
#113796=DIRECTION('ref_axis',(0.996194698091746,0.0871557427476572,1.44426287624373E-33));
#113797=DIRECTION('',(-0.0871557427476566,0.996194698091746,1.22998030563941E-16));
#113798=DIRECTION('center_axis',(0.707106781186548,-0.707106781186548,-8.7304963227523E-17));
#113799=DIRECTION('ref_axis',(0.707106781186548,0.707106781186548,2.5701266908181E-33));
#113800=DIRECTION('center_axis',(-0.707106781186544,0.707106781186551,0.));
#113801=DIRECTION('ref_axis',(-0.707106781186551,-0.707106781186544,0.));
#113802=DIRECTION('center_axis',(-0.707106781186548,0.707106781186548,0.));
#113803=DIRECTION('ref_axis',(-0.707106781186548,-0.707106781186548,0.));
#113804=DIRECTION('',(-0.707106781186547,0.707106781186548,8.73049632275231E-17));
#113805=DIRECTION('center_axis',(0.,-1.07104667533214E-16,1.));
#113806=DIRECTION('ref_axis',(1.,0.,0.));
#113807=DIRECTION('center_axis',(0.,0.,1.));
#113808=DIRECTION('ref_axis',(1.,0.,0.));
#113809=DIRECTION('',(1.87032180698308E-16,1.07104667533214E-16,-1.));
#113810=DIRECTION('center_axis',(0.996194698091745,-0.0871557427476607,
-1.2095289040845E-15));
#113811=DIRECTION('ref_axis',(0.0871557427476607,0.996194698091745,-5.51367835803032E-32));
#113812=DIRECTION('center_axis',(-0.996194698091746,0.0871557427476572,
0.));
#113813=DIRECTION('ref_axis',(-0.0871557427476572,-0.996194698091746,0.));
#113814=DIRECTION('center_axis',(0.996194698091745,-0.0871557427476607,
0.));
#113815=DIRECTION('ref_axis',(0.0871557427476607,0.996194698091745,0.));
#113816=DIRECTION('',(-0.996194698091746,0.0871557427476568,1.54074395550979E-33));
#113817=DIRECTION('center_axis',(0.,0.,-1.));
#113818=DIRECTION('ref_axis',(-1.,0.,0.));
#113819=DIRECTION('center_axis',(-5.40794518211031E-32,0.,1.));
#113820=DIRECTION('ref_axis',(0.,-1.,0.));
#113821=DIRECTION('',(-5.23852944873328E-32,-1.23467863058847E-16,1.));
#113822=DIRECTION('center_axis',(0.996194698091746,-0.0871557427476572,
-1.07609333103598E-17));
#113823=DIRECTION('ref_axis',(0.0871557427476572,0.996194698091746,-1.48387871229006E-34));
#113824=DIRECTION('',(-0.996194698091746,0.0871557427476568,1.07609333103598E-17));
#113825=DIRECTION('center_axis',(-0.996194698091746,0.0871557427476538,
0.));
#113826=DIRECTION('ref_axis',(-0.0871557427476538,-0.996194698091746,0.));
#113827=DIRECTION('center_axis',(-0.955086750882198,0.0835592633859996,
-0.284301156859545));
#113828=DIRECTION('ref_axis',(-0.28529890144429,-2.70823414235005E-19,0.958438593147564));
#113829=DIRECTION('center_axis',(0.,1.07104667533214E-16,-1.));
#113830=DIRECTION('ref_axis',(-1.,0.,0.));
#113831=DIRECTION('center_axis',(0.,0.,-1.));
#113832=DIRECTION('ref_axis',(-1.,0.,0.));
#113833=DIRECTION('',(1.87032180698308E-16,1.07104667533214E-16,-1.));
#113834=DIRECTION('center_axis',(-0.996194698091745,0.0871557427476607,
0.));
#113835=DIRECTION('ref_axis',(-0.0871557427476607,-0.996194698091745,0.));
#113836=DIRECTION('center_axis',(-0.996194698091746,0.0871557427476572,
0.));
#113837=DIRECTION('ref_axis',(-0.0871557427476572,-0.996194698091746,0.));
#113838=DIRECTION('',(-0.996194698091746,0.0871557427476568,1.54074395550979E-33));
#113839=DIRECTION('center_axis',(-0.996194698091746,0.0871557427476538,
0.));
#113840=DIRECTION('ref_axis',(-0.0871557427476538,-0.996194698091746,0.));
#113841=DIRECTION('center_axis',(0.,0.,1.));
#113842=DIRECTION('ref_axis',(1.,0.,0.));
#113843=DIRECTION('center_axis',(0.,0.,1.));
#113844=DIRECTION('ref_axis',(0.,-1.,0.));
#113845=DIRECTION('',(1.54074395550979E-33,-1.23467863058847E-16,1.));
#113846=DIRECTION('center_axis',(0.996194698091746,-0.0871557427476572,
-1.07609333103598E-17));
#113847=DIRECTION('ref_axis',(0.0871557427476572,0.996194698091746,-1.48387871229006E-34));
#113848=DIRECTION('',(-0.996194698091746,0.0871557427476568,1.07609333103598E-17));
#113849=DIRECTION('center_axis',(-0.913306614095669,0.407272671129681,2.94898912583324E-15));
#113850=DIRECTION('ref_axis',(-0.407272671129681,-0.913306614095669,-7.93980541862816E-31));
#113851=DIRECTION('center_axis',(-0.707106781186548,-0.707106781186548,
-8.7304963227523E-17));
#113852=DIRECTION('ref_axis',(0.707106781186548,-0.707106781186548,-2.5701266908181E-33));
#113853=DIRECTION('center_axis',(0.707106781186544,0.707106781186551,0.));
#113854=DIRECTION('ref_axis',(-0.707106781186551,0.707106781186544,0.));
#113855=DIRECTION('center_axis',(0.707106781186548,0.707106781186548,0.));
#113856=DIRECTION('ref_axis',(-0.707106781186548,0.707106781186548,0.));
#113857=DIRECTION('',(0.707106781186547,0.707106781186548,8.73049632275231E-17));
#113858=DIRECTION('center_axis',(6.19323182390956E-32,0.,-1.));
#113859=DIRECTION('ref_axis',(0.,1.,0.));
#113860=DIRECTION('',(6.16356212163056E-32,1.23467863058847E-16,-1.));
#113861=DIRECTION('center_axis',(0.,0.,-1.));
#113862=DIRECTION('ref_axis',(-1.,0.,0.));
#113863=DIRECTION('center_axis',(-0.996194698091747,-0.0871557427476457,
3.00690150789426E-14));
#113864=DIRECTION('ref_axis',(0.0871557427476457,-0.996194698091747,1.22577679051452E-30));
#113865=DIRECTION('center_axis',(0.996194698091747,0.0871557427476457,0.));
#113866=DIRECTION('ref_axis',(-0.0871557427476457,0.996194698091747,0.));
#113867=DIRECTION('center_axis',(-0.996194698091747,-0.0871557427476457,
0.));
#113868=DIRECTION('ref_axis',(0.0871557427476457,-0.996194698091747,0.));
#113869=DIRECTION('',(0.996194698091747,0.0871557427476402,1.54074395550979E-33));
#113870=DIRECTION('center_axis',(0.,0.,-1.));
#113871=DIRECTION('ref_axis',(-1.,0.,0.));
#113872=DIRECTION('center_axis',(-6.19323182390956E-32,0.,1.));
#113873=DIRECTION('ref_axis',(0.675590207615642,0.737277336810141,4.18408677372686E-32));
#113874=DIRECTION('',(-6.16356212163056E-32,-1.23467863058847E-16,1.));
#113875=DIRECTION('center_axis',(-0.996194698091747,-0.0871557427476409,
-1.07609333103578E-17));
#113876=DIRECTION('ref_axis',(0.0871557427476409,-0.996194698091747,2.79703111108876E-34));
#113877=DIRECTION('',(0.996194698091747,0.0871557427476402,1.07609333103578E-17));
#113878=DIRECTION('center_axis',(-0.996194698091747,-0.08715574274764,0.));
#113879=DIRECTION('ref_axis',(0.08715574274764,-0.996194698091747,0.));
#113880=DIRECTION('center_axis',(6.19323182390956E-32,0.,-1.));
#113881=DIRECTION('ref_axis',(0.,1.,0.));
#113882=DIRECTION('',(6.16356212163056E-32,1.23467863058847E-16,-1.));
#113883=DIRECTION('center_axis',(0.,0.,-1.));
#113884=DIRECTION('ref_axis',(-1.,0.,0.));
#113885=DIRECTION('center_axis',(-0.919081670180344,-0.0804092269952343,
0.385776152389619));
#113886=DIRECTION('ref_axis',(0.387029378450866,1.43097488374089E-17,0.922067383771889));
#113887=DIRECTION('center_axis',(-0.996194698091747,-0.0871557427476409,
-1.07609333103578E-17));
#113888=DIRECTION('ref_axis',(0.0871557427476409,-0.996194698091747,2.79703111108876E-34));
#113889=DIRECTION('',(0.996194698091747,0.0871557427476402,1.07609333103578E-17));
#113890=DIRECTION('center_axis',(0.996194698091747,0.0871557427476394,1.20952890408421E-15));
#113891=DIRECTION('ref_axis',(-0.0871557427476394,0.996194698091747,1.39857739234396E-32));
#113892=DIRECTION('center_axis',(0.,1.13523971920422E-16,-1.));
#113893=DIRECTION('ref_axis',(-1.,0.,0.));
#113894=DIRECTION('center_axis',(0.,0.,1.));
#113895=DIRECTION('ref_axis',(1.,0.,0.));
#113896=DIRECTION('',(-1.13659195805196E-16,1.13523971920422E-16,-1.));
#113897=DIRECTION('center_axis',(-0.996194698091747,-0.0871557427476457,
1.3824978635387E-14));
#113898=DIRECTION('ref_axis',(0.0871557427476457,-0.996194698091747,6.24837364119099E-31));
#113899=DIRECTION('center_axis',(0.996194698091747,0.0871557427476457,0.));
#113900=DIRECTION('ref_axis',(-0.0871557427476457,0.996194698091747,0.));
#113901=DIRECTION('center_axis',(-0.996194698091747,-0.0871557427476457,
0.));
#113902=DIRECTION('ref_axis',(0.0871557427476457,-0.996194698091747,0.));
#113903=DIRECTION('',(0.996194698091747,0.0871557427476402,1.54074395550979E-33));
#113904=DIRECTION('center_axis',(0.,0.,-1.));
#113905=DIRECTION('ref_axis',(-1.,0.,0.));
#113906=DIRECTION('center_axis',(-1.13659195805196E-16,0.,1.));
#113907=DIRECTION('ref_axis',(0.675590207615648,0.737277336810135,7.67870396914601E-17));
#113908=DIRECTION('',(-1.13659195805196E-16,-1.33411754197273E-16,1.));
#113909=DIRECTION('center_axis',(-0.996194698091747,-0.0871557427476409,
-1.07609333103578E-17));
#113910=DIRECTION('ref_axis',(0.0871557427476409,-0.996194698091747,2.79703111108876E-34));
#113911=DIRECTION('',(0.996194698091747,0.0871557427476402,1.07609333103578E-17));
#113912=DIRECTION('center_axis',(-0.405419774737912,0.90915150463265,0.0952803645860425));
#113913=DIRECTION('ref_axis',(-0.913306614095667,-0.407272671129684,-4.7539503937481E-18));
#113914=DIRECTION('center_axis',(0.,0.,1.));
#113915=DIRECTION('ref_axis',(1.,0.,0.));
#113916=DIRECTION('center_axis',(0.,0.,-1.));
#113917=DIRECTION('ref_axis',(0.,1.,0.));
#113918=DIRECTION('',(0.,-1.23467863058847E-16,1.));
#113919=DIRECTION('center_axis',(0.,-1.23467863058847E-16,1.));
#113920=DIRECTION('ref_axis',(0.,-1.,-1.21694324257719E-16));
#113921=DIRECTION('center_axis',(0.,-1.18842113532929E-16,1.));
#113922=DIRECTION('ref_axis',(0.,-1.,-1.18842113532929E-16));
#113923=DIRECTION('center_axis',(0.,0.,-1.));
#113924=DIRECTION('ref_axis',(0.,1.,0.));
#113925=DIRECTION('',(0.,1.23467863058847E-16,-1.));
#113926=DIRECTION('center_axis',(0.,0.,-1.));
#113927=DIRECTION('ref_axis',(-1.,0.,0.));
#113928=DIRECTION('center_axis',(-0.279133941838593,0.960252176521172,2.49865799020366E-15));
#113929=DIRECTION('ref_axis',(-0.960252176521172,-0.279133941838593,3.84227067759201E-30));
#113930=DIRECTION('center_axis',(0.,0.,-1.));
#113931=DIRECTION('ref_axis',(-1.,0.,0.));
#113932=DIRECTION('center_axis',(0.,0.,1.));
#113933=DIRECTION('ref_axis',(-1.,0.,0.));
#113934=DIRECTION('center_axis',(-0.270643175546941,0.962679734662503,0.));
#113935=DIRECTION('ref_axis',(-0.962679734662504,-0.270643175546941,0.));
#113936=DIRECTION('center_axis',(0.,0.,1.));
#113937=DIRECTION('ref_axis',(1.,0.,0.));
#113938=DIRECTION('center_axis',(0.,0.,-1.));
#113939=DIRECTION('ref_axis',(0.,1.,0.));
#113940=DIRECTION('',(0.,-1.23467863058847E-16,1.));
#113941=DIRECTION('center_axis',(0.,-1.23467863058847E-16,1.));
#113942=DIRECTION('ref_axis',(0.,-1.,-1.21694324257719E-16));
#113943=DIRECTION('center_axis',(0.,-1.18842113532929E-16,1.));
#113944=DIRECTION('ref_axis',(0.,-1.,-1.18842113532929E-16));
#113945=DIRECTION('center_axis',(0.,0.,-1.));
#113946=DIRECTION('ref_axis',(0.,1.,0.));
#113947=DIRECTION('',(0.,1.23467863058847E-16,-1.));
#113948=DIRECTION('center_axis',(0.,0.,-1.));
#113949=DIRECTION('ref_axis',(-1.,0.,0.));
#113950=DIRECTION('center_axis',(0.141334929101325,-0.989809819863889,-0.0173481502454526));
#113951=DIRECTION('ref_axis',(0.989958799240908,0.1413562018643,-1.53957070961197E-18));
#113952=DIRECTION('center_axis',(0.132860127107541,-0.991003467296,-0.0161342626814395));
#113953=DIRECTION('ref_axis',(0.991132478736687,0.132877423188709,7.57324997548269E-19));
#113954=DIRECTION('center_axis',(0.14258112270268,0.00286725800189432,0.989778966376026));
#113955=DIRECTION('ref_axis',(0.97964031348631,0.142384138292289,-0.141533082193549));
#113956=DIRECTION('center_axis',(0.,0.,-1.));
#113957=DIRECTION('ref_axis',(-1.,0.,0.));
#113958=DIRECTION('center_axis',(0.,0.,-1.));
#113959=DIRECTION('ref_axis',(0.,1.,0.));
#113960=DIRECTION('',(0.,-1.23467863058847E-16,1.));
#113961=DIRECTION('center_axis',(0.,-1.23467863058847E-16,1.));
#113962=DIRECTION('ref_axis',(0.,-1.,-1.21694324257719E-16));
#113963=DIRECTION('center_axis',(0.,-1.18842113532929E-16,1.));
#113964=DIRECTION('ref_axis',(0.,-1.,-1.18842113532929E-16));
#113965=DIRECTION('center_axis',(0.,0.,-1.));
#113966=DIRECTION('ref_axis',(0.,1.,0.));
#113967=DIRECTION('',(0.,1.23467863058847E-16,-1.));
#113968=DIRECTION('center_axis',(3.91353616180368E-12,0.,-1.));
#113969=DIRECTION('ref_axis',(-1.,0.,-3.91353616180368E-12));
#113970=DIRECTION('center_axis',(0.00235261362124023,-0.999997195602435,
-0.000272022820600068));
#113971=DIRECTION('ref_axis',(0.999997232600541,0.00235261370828272,8.12493746167259E-22));
#113972=DIRECTION('center_axis',(-0.00620231251671424,-0.999980508301815,
0.000717172147678158));
#113973=DIRECTION('ref_axis',(0.999980765464846,-0.00620231411175082,5.84684475171815E-22));
#113974=DIRECTION('center_axis',(0.115833873408401,-1.74164817710871E-9,
0.993268601019486));
#113975=DIRECTION('ref_axis',(0.993265814819633,0.00236857700963695,-0.115833548480737));
#113976=DIRECTION('center_axis',(0.,0.,-1.));
#113977=DIRECTION('ref_axis',(-1.,0.,0.));
#113978=DIRECTION('center_axis',(0.,0.,-1.));
#113979=DIRECTION('ref_axis',(0.,1.,0.));
#113980=DIRECTION('',(0.,-1.23467863058847E-16,1.));
#113981=DIRECTION('center_axis',(0.,-1.23467863058847E-16,1.));
#113982=DIRECTION('ref_axis',(0.,-1.,-1.21694324257719E-16));
#113983=DIRECTION('center_axis',(0.,-1.18842113532929E-16,1.));
#113984=DIRECTION('ref_axis',(0.,-1.,-1.18842113532929E-16));
#113985=DIRECTION('center_axis',(0.,0.,-1.));
#113986=DIRECTION('ref_axis',(0.,1.,0.));
#113987=DIRECTION('',(0.,1.23467863058847E-16,-1.));
#113988=DIRECTION('center_axis',(6.61970478432749E-12,0.,-1.));
#113989=DIRECTION('ref_axis',(-1.,0.,-6.61970478432749E-12));
#113990=DIRECTION('center_axis',(-0.136675079747296,-0.990475586151279,
0.0166744059669382));
#113991=DIRECTION('ref_axis',(0.990613308713893,-0.136694083993833,9.06110283290218E-19));
#113992=DIRECTION('center_axis',(-0.14514509610524,-0.989248239790814,0.0179114808817288));
#113993=DIRECTION('ref_axis',(0.989406963861029,-0.145168384517086,-1.21343959465114E-18));
#113994=DIRECTION('center_axis',(0.145269618843932,-0.00325155863630697,
0.989386762195338));
#113995=DIRECTION('ref_axis',(0.979906495320475,-0.137666580604216,-0.144330083535927));
#113996=DIRECTION('center_axis',(1.18805075949821E-12,7.25808302348696E-12,
-1.));
#113997=DIRECTION('ref_axis',(-5.87747175411144E-39,1.,7.25808302348696E-12));
#113998=DIRECTION('center_axis',(0.,0.,-1.));
#113999=DIRECTION('ref_axis',(0.,1.,0.));
#114000=DIRECTION('',(0.,-1.23467863058847E-16,1.));
#114001=DIRECTION('center_axis',(0.,-1.23467863058847E-16,1.));
#114002=DIRECTION('ref_axis',(0.,-1.,-1.21694324257719E-16));
#114003=DIRECTION('center_axis',(0.,-1.18842113532929E-16,1.));
#114004=DIRECTION('ref_axis',(0.,-1.,-1.18842113532929E-16));
#114005=DIRECTION('center_axis',(0.,0.,-1.));
#114006=DIRECTION('ref_axis',(0.,1.,0.));
#114007=DIRECTION('',(0.,1.23467863058847E-16,-1.));
#114008=DIRECTION('center_axis',(0.,0.,-1.));
#114009=DIRECTION('ref_axis',(-1.,0.,0.));
#114010=DIRECTION('center_axis',(0.274464020377229,0.96159736975429,0.));
#114011=DIRECTION('ref_axis',(-0.96159736975429,0.274464020377229,0.));
#114012=DIRECTION('center_axis',(0.,0.,-1.));
#114013=DIRECTION('ref_axis',(-1.,0.,0.));
#114014=DIRECTION('center_axis',(0.,0.,1.));
#114015=DIRECTION('ref_axis',(-1.,0.,0.));
#114016=DIRECTION('center_axis',(0.282954786668892,0.959133248668381,0.));
#114017=DIRECTION('ref_axis',(-0.959133248668381,0.282954786668892,0.));
#114018=DIRECTION('center_axis',(0.,0.,1.));
#114019=DIRECTION('ref_axis',(1.,0.,0.));
#114020=DIRECTION('center_axis',(0.,0.,-1.));
#114021=DIRECTION('ref_axis',(0.,1.,0.));
#114022=DIRECTION('',(0.,-1.23467863058847E-16,1.));
#114023=DIRECTION('center_axis',(0.,-1.23467863058847E-16,1.));
#114024=DIRECTION('ref_axis',(0.,-1.,-1.21694324257719E-16));
#114025=DIRECTION('center_axis',(0.,-1.18842113532929E-16,1.));
#114026=DIRECTION('ref_axis',(0.,-1.,-1.18842113532929E-16));
#114027=DIRECTION('center_axis',(0.,0.,-1.));
#114028=DIRECTION('ref_axis',(0.,1.,0.));
#114029=DIRECTION('center_axis',(0.,0.,1.));
#114030=DIRECTION('ref_axis',(1.,0.,0.));
#114031=DIRECTION('',(0.,1.23467863058847E-16,-1.));
#114032=DIRECTION('center_axis',(-0.388071473886494,-0.870248040119286,
0.303428541544968));
#114033=DIRECTION('ref_axis',(0.913306614096678,-0.407272671127417,-4.84423453041484E-17));
#114034=DIRECTION('center_axis',(0.0871557427476569,0.996194698091746,1.22998030563941E-16));
#114035=DIRECTION('ref_axis',(1.41124413247282E-15,4.52989727324155E-33,
-1.));
#114036=DIRECTION('',(1.54074395550979E-33,-1.23467863058847E-16,1.));
#114037=DIRECTION('',(0.996194698091746,-0.0871557427476568,0.));
#114038=DIRECTION('',(-3.08148791101958E-33,1.23467863058847E-16,-1.));
#114039=DIRECTION('center_axis',(0.,1.23467863058847E-16,-1.));
#114040=DIRECTION('ref_axis',(0.,1.,0.));
#114041=DIRECTION('center_axis',(5.71153601538325E-31,-2.64211616260596E-45,
1.));
#114042=DIRECTION('ref_axis',(4.62592926927148E-15,1.,1.24460305557223E-60));
#114043=DIRECTION('center_axis',(0.707106781186548,0.707106781186547,8.7304963227523E-17));
#114044=DIRECTION('ref_axis',(2.16153073061992E-33,1.23467863058847E-16,
-1.));
#114045=DIRECTION('',(1.23259516440783E-32,1.23467863058847E-16,-1.));
#114046=DIRECTION('',(-1.23259516440783E-32,-1.23467863058847E-16,1.));
#114047=DIRECTION('',(0.707106781186547,-0.707106781186548,0.));
#114048=DIRECTION('center_axis',(-1.67127905768941E-33,0.,-1.));
#114049=DIRECTION('ref_axis',(0.,1.,0.));
#114050=DIRECTION('center_axis',(5.71153601538325E-31,-2.64211616260596E-45,
1.));
#114051=DIRECTION('ref_axis',(4.62592926927148E-15,1.,1.24460305557223E-60));
#114052=DIRECTION('center_axis',(0.,1.23467863058847E-16,-1.));
#114053=DIRECTION('ref_axis',(0.,1.,0.));
#114054=DIRECTION('center_axis',(-2.85576800769162E-31,-6.6052904065149E-46,
1.));
#114055=DIRECTION('ref_axis',(-2.31296463463574E-15,1.,3.11150763893057E-61));
#114056=DIRECTION('center_axis',(0.996194698091746,0.0871557427476566,1.07609333103598E-17));
#114057=DIRECTION('ref_axis',(1.4714164960684E-33,1.23467863058847E-16,
-1.));
#114058=DIRECTION('',(0.,-1.23467863058847E-16,1.));
#114059=DIRECTION('',(0.0871557427476566,-0.996194698091746,-3.51482972517089E-16));
#114060=DIRECTION('',(0.,1.23467863058847E-16,-1.));
#114061=DIRECTION('center_axis',(-4.26141870503966E-34,0.,-1.));
#114062=DIRECTION('ref_axis',(0.,1.,0.));
#114063=DIRECTION('center_axis',(-2.85576800769162E-31,-6.6052904065149E-46,
1.));
#114064=DIRECTION('ref_axis',(-2.31296463463574E-15,1.,3.11150763893057E-61));
#114065=DIRECTION('center_axis',(0.272999209159005,-0.962014257585904,0.));
#114066=DIRECTION('ref_axis',(0.962014257585904,0.272999209159004,0.));
#114067=DIRECTION('center_axis',(0.,0.,-1.));
#114068=DIRECTION('ref_axis',(-1.,0.,0.));
#114069=DIRECTION('center_axis',(-0.384110320270104,0.923287204428827,0.));
#114070=DIRECTION('ref_axis',(-0.923287204428827,-0.384110320270104,0.));
#114071=DIRECTION('center_axis',(0.,0.,-1.));
#114072=DIRECTION('ref_axis',(-1.,0.,0.));
#114073=DIRECTION('center_axis',(-0.886109103059821,-0.368607756298431,
-0.280960814832168));
#114074=DIRECTION('ref_axis',(-0.25934119650515,-0.10807938690911,0.959719224523834));
#114075=DIRECTION('center_axis',(0.,1.18842113532929E-16,-1.));
#114076=DIRECTION('ref_axis',(0.,1.,1.18842113532929E-16));
#114077=DIRECTION('center_axis',(0.,0.,1.));
#114078=DIRECTION('ref_axis',(-1.,1.78263170299393E-15,0.));
#114079=DIRECTION('',(0.,1.23467863058847E-16,-1.));
#114080=DIRECTION('',(0.,-1.23467863058847E-16,1.));
#114081=DIRECTION('center_axis',(0.,0.,-1.));
#114082=DIRECTION('ref_axis',(0.,1.,0.));
#114083=DIRECTION('center_axis',(0.,0.,-1.));
#114084=DIRECTION('ref_axis',(0.,1.,0.));
#114085=DIRECTION('center_axis',(-0.334110320282714,-0.942533974921107,
0.));
#114086=DIRECTION('ref_axis',(0.942533974921107,-0.334110320282714,0.));
#114087=DIRECTION('center_axis',(0.,0.,-1.));
#114088=DIRECTION('ref_axis',(-1.,0.,0.));
#114089=DIRECTION('center_axis',(-0.222999209171599,-0.974818625544692,
0.));
#114090=DIRECTION('ref_axis',(0.974818625544692,-0.222999209171599,0.));
#114091=DIRECTION('center_axis',(0.,0.,-1.));
#114092=DIRECTION('ref_axis',(-1.,0.,0.));
#114093=DIRECTION('center_axis',(0.,0.,-1.));
#114094=DIRECTION('ref_axis',(0.688859710772108,-0.724894681229603,0.));
#114095=DIRECTION('',(0.,1.23467863058847E-16,-1.));
#114096=DIRECTION('center_axis',(0.,4.63518112781003E-12,-1.));
#114097=DIRECTION('ref_axis',(0.,1.,4.63518112781003E-12));
#114098=DIRECTION('center_axis',(-0.997624402707396,0.0684293228260734,
-0.00793592466417746));
#114099=DIRECTION('ref_axis',(-0.0684314777296081,-0.997655818835204,-3.0788904879186E-19));
#114100=DIRECTION('center_axis',(0.00012024518356205,0.117893637119934,
0.993026221138057));
#114101=DIRECTION('ref_axis',(0.0688956039867685,0.990665697053439,-0.117621734526076));
#114102=DIRECTION('center_axis',(-0.996993498376656,0.0769676640255834,
-0.00894107874490511));
#114103=DIRECTION('ref_axis',(-0.07697074071877,-0.997033352036532,7.99587428479913E-19));
#114104=DIRECTION('center_axis',(0.,0.,1.));
#114105=DIRECTION('ref_axis',(1.,0.,0.));
#114106=DIRECTION('center_axis',(0.,0.,-1.));
#114107=DIRECTION('ref_axis',(0.,1.,0.));
#114108=DIRECTION('',(0.,-1.23467863058847E-16,1.));
#114109=DIRECTION('center_axis',(0.,-1.23467863058847E-16,1.));
#114110=DIRECTION('ref_axis',(0.,-1.,-1.21694324257719E-16));
#114111=DIRECTION('center_axis',(0.,-1.18842113532929E-16,1.));
#114112=DIRECTION('ref_axis',(0.,-1.,-1.18842113532929E-16));
#114113=DIRECTION('center_axis',(0.,0.,-1.));
#114114=DIRECTION('ref_axis',(0.634315526883886,-0.773074260568814,0.));
#114115=DIRECTION('',(0.,1.23467863058847E-16,-1.));
#114116=DIRECTION('center_axis',(0.,-1.38777878078144E-14,-1.));
#114117=DIRECTION('ref_axis',(0.,1.,-1.38777878078144E-14));
#114118=DIRECTION('center_axis',(-0.976728808322011,0.212349635823786,-0.0301407889639504));
#114119=DIRECTION('ref_axis',(-0.212446157929364,-0.977172773863994,-1.17576428045677E-20));
#114120=DIRECTION('center_axis',(0.0251527414239144,0.25401807230836,0.966872358969686));
#114121=DIRECTION('ref_axis',(0.213030566219325,0.943601106365079,-0.253446108517911));
#114122=DIRECTION('center_axis',(-0.974807460973989,0.220687770576049,-0.0323623538639763));
#114123=DIRECTION('ref_axis',(-0.220803427003966,-0.975318330917298,-7.28333184199878E-18));
#114124=DIRECTION('center_axis',(2.7755575615626E-13,5.13478148889134E-13,
1.));
#114125=DIRECTION('ref_axis',(-1.14794370197489E-40,-1.,5.13478148889134E-13));
#114126=DIRECTION('center_axis',(0.,0.,-1.));
#114127=DIRECTION('ref_axis',(0.,1.,0.));
#114128=DIRECTION('',(0.,-1.23467863058847E-16,1.));
#114129=DIRECTION('center_axis',(0.,-1.23467863058847E-16,1.));
#114130=DIRECTION('ref_axis',(0.,-1.,-1.21694324257719E-16));
#114131=DIRECTION('center_axis',(0.,-1.18842113532929E-16,1.));
#114132=DIRECTION('ref_axis',(0.,-1.,-1.18842113532929E-16));
#114133=DIRECTION('center_axis',(0.,0.,-1.));
#114134=DIRECTION('ref_axis',(0.574616980402509,-0.818422461711006,0.));
#114135=DIRECTION('center_axis',(0.,0.,-1.));
#114136=DIRECTION('ref_axis',(-1.,0.,0.));
#114137=DIRECTION('',(0.,1.23467863058847E-16,-1.));
#114138=DIRECTION('center_axis',(-0.934252508717439,0.356612184249462,0.));
#114139=DIRECTION('ref_axis',(-0.356612184249462,-0.934252508717439,0.));
#114140=DIRECTION('center_axis',(0.,0.,1.));
#114141=DIRECTION('ref_axis',(1.,0.,0.));
#114142=DIRECTION('center_axis',(0.,0.,1.));
#114143=DIRECTION('ref_axis',(1.,0.,0.));
#114144=DIRECTION('center_axis',(-0.930967150605313,0.365102950541111,0.));
#114145=DIRECTION('ref_axis',(-0.365102950541111,-0.930967150605313,0.));
#114146=DIRECTION('center_axis',(0.,0.,1.));
#114147=DIRECTION('ref_axis',(1.,0.,0.));
#114148=DIRECTION('center_axis',(0.,0.,-1.));
#114149=DIRECTION('ref_axis',(0.,1.,0.));
#114150=DIRECTION('',(0.,-1.23467863058847E-16,1.));
#114151=DIRECTION('center_axis',(0.,1.23467863058847E-16,-1.));
#114152=DIRECTION('ref_axis',(0.,1.,1.21694324257719E-16));
#114153=DIRECTION('center_axis',(4.39608526712911E-31,-1.18842113532929E-16,
1.));
#114154=DIRECTION('ref_axis',(9.50350909079134E-14,1.,1.18842113532929E-16));
#114155=DIRECTION('center_axis',(0.,0.,-1.));
#114156=DIRECTION('ref_axis',(0.,1.,0.));
#114157=DIRECTION('',(0.,1.23467863058847E-16,-1.));
#114158=DIRECTION('center_axis',(0.,0.,-1.));
#114159=DIRECTION('ref_axis',(0.,1.,0.));
#114160=DIRECTION('center_axis',(0.,0.,-1.));
#114161=DIRECTION('ref_axis',(-1.,0.,0.));
#114162=DIRECTION('center_axis',(-0.911656491798923,-0.41095308851605,5.08035184938228E-15));
#114163=DIRECTION('ref_axis',(0.41095308851605,-0.911656491798923,7.81754519040083E-31));
#114164=DIRECTION('center_axis',(-0.911086081553275,-0.412216147184822,
0.));
#114165=DIRECTION('ref_axis',(0.412216147184823,-0.911086081553275,0.));
#114166=DIRECTION('center_axis',(0.,0.,1.));
#114167=DIRECTION('ref_axis',(-1.,0.,0.));
#114168=DIRECTION('center_axis',(0.,0.,-1.));
#114169=DIRECTION('ref_axis',(-1.,0.,0.));
#114170=DIRECTION('center_axis',(0.,0.,-1.));
#114171=DIRECTION('ref_axis',(0.,1.,0.));
#114172=DIRECTION('',(0.,-1.23467863058847E-16,1.));
#114173=DIRECTION('center_axis',(0.,-1.23467863058847E-16,1.));
#114174=DIRECTION('ref_axis',(0.,-1.,-1.21694324257719E-16));
#114175=DIRECTION('center_axis',(0.,-1.18842113532929E-16,1.));
#114176=DIRECTION('ref_axis',(0.,-1.,-1.18842113532929E-16));
#114177=DIRECTION('center_axis',(0.,0.,-1.));
#114178=DIRECTION('ref_axis',(0.,1.,0.));
#114179=DIRECTION('',(0.,1.23467863058847E-16,-1.));
#114180=DIRECTION('center_axis',(0.,0.,-1.));
#114181=DIRECTION('ref_axis',(-1.,0.,0.));
#114182=DIRECTION('center_axis',(-0.959694777166788,-0.28104436425374,-1.95400042656926E-13));
#114183=DIRECTION('ref_axis',(0.28104436425374,-0.959694777166788,-3.56742184214581E-30));
#114184=DIRECTION('center_axis',(0.,0.,-1.));
#114185=DIRECTION('ref_axis',(-1.,0.,0.));
#114186=DIRECTION('center_axis',(-0.962140601075499,-0.272553597962085,
1.24636926569648E-14));
#114187=DIRECTION('ref_axis',(0.272553597962085,-0.962140601075499,-4.52904126028793E-31));
#114188=DIRECTION('center_axis',(0.,0.,1.));
#114189=DIRECTION('ref_axis',(-1.,0.,0.));
#114190=DIRECTION('center_axis',(0.,0.,-1.));
#114191=DIRECTION('ref_axis',(-1.,0.,0.));
#114192=DIRECTION('center_axis',(0.,0.,-1.));
#114193=DIRECTION('ref_axis',(0.,1.,0.));
#114194=DIRECTION('',(0.,-1.23467863058847E-16,1.));
#114195=DIRECTION('center_axis',(0.,-1.23467863058847E-16,1.));
#114196=DIRECTION('ref_axis',(0.,-1.,-1.21694324257719E-16));
#114197=DIRECTION('center_axis',(0.,-1.18842113532929E-16,1.));
#114198=DIRECTION('ref_axis',(0.,-1.,-1.18842113532929E-16));
#114199=DIRECTION('center_axis',(0.,0.,-1.));
#114200=DIRECTION('ref_axis',(0.,1.,0.));
#114201=DIRECTION('',(0.,1.23467863058847E-16,-1.));
#114202=DIRECTION('center_axis',(0.,1.38777878078144E-14,-1.));
#114203=DIRECTION('ref_axis',(0.,1.,1.38777878078144E-14));
#114204=DIRECTION('center_axis',(-0.989538255790606,-0.14315195982541,-0.0179320028170335));
#114205=DIRECTION('ref_axis',(0.143174981115239,-0.989697390510176,-2.48873089681965E-18));
#114206=DIRECTION('center_axis',(-0.99074835547853,-0.134685218959648,-0.0166609696710313));
#114207=DIRECTION('ref_axis',(0.13470391634661,-0.99088589399632,2.11341644556228E-18));
#114208=DIRECTION('center_axis',(0.0035180468195045,-0.149207652782241,
0.988799625656174));
#114209=DIRECTION('ref_axis',(0.144246054961535,-0.978388820119922,-0.148149898050527));
#114210=DIRECTION('center_axis',(-5.55111512312579E-13,-6.5495003047383E-14,
-1.));
#114211=DIRECTION('ref_axis',(-1.,7.99467207819295E-41,5.55111512312579E-13));
#114212=DIRECTION('center_axis',(-5.55111512312579E-13,-6.5495003047383E-14,
-1.));
#114213=DIRECTION('ref_axis',(-1.,7.99467207819295E-41,5.55111512312579E-13));
#114214=DIRECTION('center_axis',(0.,0.,-1.));
#114215=DIRECTION('ref_axis',(0.,1.,0.));
#114216=DIRECTION('',(0.,-1.23467863058847E-16,1.));
#114217=DIRECTION('center_axis',(0.,-1.23467863058847E-16,1.));
#114218=DIRECTION('ref_axis',(0.,-1.,-1.21694324257719E-16));
#114219=DIRECTION('center_axis',(0.,-1.18842113532929E-16,1.));
#114220=DIRECTION('ref_axis',(0.,-1.,-1.18842113532929E-16));
#114221=DIRECTION('center_axis',(0.,0.,-1.));
#114222=DIRECTION('ref_axis',(0.,1.,0.));
#114223=DIRECTION('',(0.,1.23467863058847E-16,-1.));
#114224=DIRECTION('center_axis',(0.,1.38777878078144E-14,-1.));
#114225=DIRECTION('ref_axis',(0.,1.,1.38777878078144E-14));
#114226=DIRECTION('center_axis',(0.999990739418254,0.00427492665558239,
0.00049606433434234));
#114227=DIRECTION('ref_axis',(-0.00427492718156908,0.999990862457049,1.90763185875202E-22));
#114228=DIRECTION('center_axis',(0.,1.18842113532929E-16,-1.));
#114229=DIRECTION('ref_axis',(1.22464679914735E-16,-1.,-1.18842113532929E-16));
#114230=DIRECTION('center_axis',(0.,0.,1.));
#114231=DIRECTION('ref_axis',(-1.,0.,0.));
#114232=DIRECTION('center_axis',(7.9520675071357E-13,-0.116240704649149,
0.99322107236137));
#114233=DIRECTION('ref_axis',(0.00430412409636137,-0.993211872368101,-0.116239627936495));
#114234=DIRECTION('',(0.,-1.23467863058847E-16,1.));
#114235=DIRECTION('center_axis',(0.996194698091747,-0.0871557427476402,
-1.07609333103578E-17));
#114236=DIRECTION('ref_axis',(-4.87735489362744E-35,1.23467863058847E-16,
-1.));
#114237=DIRECTION('',(1.54660695142382E-33,-1.23467863058847E-16,1.));
#114238=DIRECTION('',(-0.0871557427476402,-0.996194698091747,0.));
#114239=DIRECTION('',(-1.54660695142382E-33,1.23467863058847E-16,-1.));
#114240=DIRECTION('center_axis',(0.,1.23467863058847E-16,-1.));
#114241=DIRECTION('ref_axis',(0.,1.,0.));
#114242=DIRECTION('center_axis',(-2.85576800769162E-31,-6.6052904065149E-46,
1.));
#114243=DIRECTION('ref_axis',(-2.31296463463574E-15,1.,3.11150763893057E-61));
#114244=DIRECTION('center_axis',(0.707106781186548,-0.707106781186547,-8.7304963227523E-17));
#114245=DIRECTION('ref_axis',(-2.16153073061992E-33,1.23467863058847E-16,
-1.));
#114246=DIRECTION('',(-1.23259516440783E-32,1.23467863058847E-16,-1.));
#114247=DIRECTION('',(-8.71576399210526E-33,-1.23467863058847E-16,1.));
#114248=DIRECTION('',(-0.707106781186547,-0.707106781186548,0.));
#114249=DIRECTION('center_axis',(1.35502005093696E-32,0.,-1.));
#114250=DIRECTION('ref_axis',(0.,1.,0.));
#114251=DIRECTION('center_axis',(-2.85576800769162E-31,-6.6052904065149E-46,
1.));
#114252=DIRECTION('ref_axis',(-2.31296463463574E-15,1.,3.11150763893057E-61));
#114253=DIRECTION('center_axis',(0.,1.23467863058847E-16,-1.));
#114254=DIRECTION('ref_axis',(0.,1.,0.));
#114255=DIRECTION('center_axis',(0.,0.,1.));
#114256=DIRECTION('ref_axis',(0.,1.,0.));
#114257=DIRECTION('center_axis',(0.0871557427476402,-0.996194698091747,
-1.22998030563942E-16));
#114258=DIRECTION('ref_axis',(1.53780943396195E-34,1.23467863058847E-16,
-1.));
#114259=DIRECTION('',(6.15711282612512E-33,-1.23467863058847E-16,1.));
#114260=DIRECTION('',(-0.996194698091747,-0.0871557427476402,0.));
#114261=DIRECTION('',(5.86299591403052E-36,1.23467863058847E-16,-1.));
#114262=DIRECTION('center_axis',(-5.61645494961161E-33,0.,-1.));
#114263=DIRECTION('ref_axis',(0.,1.,0.));
#114264=DIRECTION('center_axis',(0.,0.,1.));
#114265=DIRECTION('ref_axis',(0.,1.,0.));
#114266=DIRECTION('center_axis',(-0.970284356147939,-0.241967494127993,
1.34486472837252E-14));
#114267=DIRECTION('ref_axis',(0.241967494127993,-0.970284356147939,-2.62269727666659E-30));
#114268=DIRECTION('center_axis',(0.,0.,-1.));
#114269=DIRECTION('ref_axis',(-1.,0.,0.));
#114270=DIRECTION('center_axis',(0.,0.,-1.));
#114271=DIRECTION('ref_axis',(-1.,0.,0.));
#114272=DIRECTION('center_axis',(0.,0.,-1.));
#114273=DIRECTION('ref_axis',(0.,1.,0.));
#114274=DIRECTION('center_axis',(0.,0.,-1.));
#114275=DIRECTION('ref_axis',(0.,1.,0.));
#114276=DIRECTION('center_axis',(-7.4257679719932E-13,0.0392139963569502,
-0.999230835437797));
#114277=DIRECTION('ref_axis',(-0.00367973466771379,-0.9992240703987,-0.0392137308685247));
#114278=DIRECTION('center_axis',(0.,-1.,0.));
#114279=DIRECTION('ref_axis',(-0.00205411287980643,0.,0.999997890307913));
#114280=DIRECTION('center_axis',(-5.01606788234257E-16,-1.,5.70122241611331E-32));
#114281=DIRECTION('ref_axis',(-1.,5.01606788234257E-16,0.));
#114282=DIRECTION('center_axis',(0.,-1.,0.));
#114283=DIRECTION('ref_axis',(0.00228223725611616,0.,-0.999997395693162));
#114284=DIRECTION('center_axis',(-1.45825811553708E-13,0.0304934853273349,
0.999534965547775));
#114285=DIRECTION('ref_axis',(0.00367477153576914,-0.999528216691971,0.030493279435453));
#114286=DIRECTION('center_axis',(7.06462337057814E-14,0.115836593517192,
0.993268283799665));
#114287=DIRECTION('ref_axis',(0.00429820688470854,-0.993259108648899,0.115835523495903));
#114288=DIRECTION('center_axis',(0.,0.,1.));
#114289=DIRECTION('ref_axis',(0.,-1.,0.));
#114290=DIRECTION('center_axis',(0.,0.,1.));
#114291=DIRECTION('ref_axis',(0.,-1.,0.));
#114292=DIRECTION('center_axis',(0.,-1.23467863058847E-16,1.));
#114293=DIRECTION('ref_axis',(0.,-1.,0.));
#114294=DIRECTION('center_axis',(2.19322982990717E-31,3.89595880873225E-46,
-1.));
#114295=DIRECTION('ref_axis',(1.77635683940025E-15,-1.,-5.4451383681285E-61));
#114296=DIRECTION('center_axis',(0.,-1.23467863058847E-16,1.));
#114297=DIRECTION('ref_axis',(0.,-1.,-1.23467863058847E-16));
#114298=DIRECTION('center_axis',(2.19322982990717E-31,3.89595880873225E-46,
-1.));
#114299=DIRECTION('ref_axis',(1.77635683940025E-15,-1.,-5.4451383681285E-61));
#114300=DIRECTION('center_axis',(0.,-1.23467863058847E-16,1.));
#114301=DIRECTION('ref_axis',(1.22464679914735E-16,1.,0.));
#114302=DIRECTION('center_axis',(0.,0.,1.));
#114303=DIRECTION('ref_axis',(0.,-1.,0.));
#114304=DIRECTION('center_axis',(0.,0.,1.));
#114305=DIRECTION('ref_axis',(1.22464679914735E-16,1.,0.));
#114306=DIRECTION('center_axis',(0.,0.,-1.));
#114307=DIRECTION('ref_axis',(1.,-8.89601782552209E-16,0.));
#114308=DIRECTION('center_axis',(0.,0.,1.));
#114309=DIRECTION('ref_axis',(1.,0.,0.));
#114310=DIRECTION('center_axis',(0.,0.,1.));
#114311=DIRECTION('ref_axis',(1.,0.,0.));
#114312=DIRECTION('center_axis',(0.,0.,1.));
#114313=DIRECTION('ref_axis',(1.,0.,0.));
#114314=DIRECTION('',(-1.,0.,0.));
#114315=DIRECTION('center_axis',(0.,-1.,0.));
#114316=DIRECTION('ref_axis',(0.,0.,-1.));
#114317=DIRECTION('',(1.,0.,0.));
#114318=DIRECTION('center_axis',(0.,0.,-1.));
#114319=DIRECTION('ref_axis',(0.,-1.,0.));
#114320=DIRECTION('center_axis',(0.,0.,-1.));
#114321=DIRECTION('ref_axis',(-1.,0.,0.));
#114322=DIRECTION('center_axis',(0.,0.,-1.));
#114323=DIRECTION('ref_axis',(-1.,0.,0.));
#114324=DIRECTION('center_axis',(0.,0.,1.));
#114325=DIRECTION('ref_axis',(0.,-1.,0.));
#114326=DIRECTION('center_axis',(0.,-1.18842113532926E-16,1.));
#114327=DIRECTION('ref_axis',(0.,1.,1.18842113532926E-16));
#114328=DIRECTION('center_axis',(0.,1.19033121480991E-16,-1.));
#114329=DIRECTION('ref_axis',(0.,-1.,-1.19033121480991E-16));
#114330=DIRECTION('center_axis',(0.,-1.23467863058847E-16,1.));
#114331=DIRECTION('ref_axis',(-1.22464679914735E-16,1.,1.21694324257719E-16));
#114332=DIRECTION('center_axis',(0.,-1.18842113532929E-16,1.));
#114333=DIRECTION('ref_axis',(0.,-1.,-1.18842113532929E-16));
#114334=DIRECTION('center_axis',(0.,1.18842113532929E-16,-1.));
#114335=DIRECTION('ref_axis',(0.,1.,1.18842113532929E-16));
#114336=DIRECTION('center_axis',(0.,0.,1.));
#114337=DIRECTION('ref_axis',(-1.,1.78263170299393E-15,0.));
#114338=DIRECTION('center_axis',(0.,0.,-1.));
#114339=DIRECTION('ref_axis',(0.,1.,0.));
#114340=DIRECTION('center_axis',(0.,0.,-1.));
#114341=DIRECTION('ref_axis',(0.,1.,0.));
#114342=DIRECTION('center_axis',(0.,0.,-1.));
#114343=DIRECTION('ref_axis',(0.,-1.,0.));
#114344=DIRECTION('center_axis',(-0.5,0.866025403784438,1.0692630595994E-16));
#114345=DIRECTION('ref_axis',(2.13852611919879E-16,5.48307457472744E-35,
1.));
#114346=DIRECTION('',(0.,1.23467863058847E-16,-1.));
#114347=DIRECTION('',(0.,1.23467863058847E-16,-1.));
#114348=DIRECTION('center_axis',(-1.,0.,0.));
#114349=DIRECTION('ref_axis',(0.,0.,1.));
#114350=DIRECTION('',(0.,1.23467863058847E-16,-1.));
#114351=DIRECTION('center_axis',(-0.5,-0.866025403784439,-1.0692630595994E-16));
#114352=DIRECTION('ref_axis',(-0.866025403784439,0.5,-9.26929360883051E-34));
#114353=DIRECTION('',(0.,1.23467863058847E-16,-1.));
#114354=DIRECTION('center_axis',(0.5,-0.866025403784439,-1.0692630595994E-16));
#114355=DIRECTION('ref_axis',(-4.5474696259435E-34,1.23467863058847E-16,
-1.));
#114356=DIRECTION('',(0.,1.23467863058847E-16,-1.));
#114357=DIRECTION('center_axis',(1.,0.,0.));
#114358=DIRECTION('ref_axis',(0.,1.,0.));
#114359=DIRECTION('',(0.,1.23467863058847E-16,-1.));
#114360=DIRECTION('center_axis',(0.5,0.866025403784439,1.0692630595994E-16));
#114361=DIRECTION('ref_axis',(2.1385261191988E-16,-4.09037363277686E-33,
-1.));
#114362=DIRECTION('center_axis',(0.,0.,-1.));
#114363=DIRECTION('ref_axis',(0.,1.,0.));
#114364=DIRECTION('',(-1.06057523872491E-16,-0.866025403784439,-0.5));
#114365=DIRECTION('center_axis',(0.,0.,-1.));
#114366=DIRECTION('ref_axis',(0.,1.,0.));
#114367=DIRECTION('center_axis',(0.,0.,-1.));
#114368=DIRECTION('ref_axis',(0.,1.,0.));
#114369=DIRECTION('center_axis',(0.,0.,-1.));
#114370=DIRECTION('ref_axis',(0.,1.,0.));
#114371=DIRECTION('center_axis',(0.,0.,-1.));
#114372=DIRECTION('ref_axis',(0.,1.,0.));
#114373=DIRECTION('center_axis',(0.,0.,-1.));
#114374=DIRECTION('ref_axis',(0.,1.,0.));
#114375=DIRECTION('center_axis',(0.,0.,-1.));
#114376=DIRECTION('ref_axis',(0.,1.,0.));
#114377=DIRECTION('center_axis',(0.,0.,-1.));
#114378=DIRECTION('ref_axis',(0.,1.,0.));
#114379=DIRECTION('center_axis',(0.,0.,-1.));
#114380=DIRECTION('ref_axis',(0.,1.,0.));
#114381=DIRECTION('center_axis',(0.,0.,-1.));
#114382=DIRECTION('ref_axis',(0.,1.,0.));
#114383=DIRECTION('center_axis',(0.,0.,-1.));
#114384=DIRECTION('ref_axis',(0.,1.,0.));
#114385=DIRECTION('center_axis',(0.,0.,-1.));
#114386=DIRECTION('ref_axis',(0.,1.,0.));
#114387=DIRECTION('center_axis',(0.,0.,-1.));
#114388=DIRECTION('ref_axis',(0.,1.,0.));
#114389=DIRECTION('center_axis',(0.,1.23467863058847E-16,-1.));
#114390=DIRECTION('ref_axis',(0.,1.,0.));
#114391=DIRECTION('center_axis',(0.,0.,-1.));
#114392=DIRECTION('ref_axis',(0.,1.,0.));
#114393=DIRECTION('center_axis',(-1.,0.,0.));
#114394=DIRECTION('ref_axis',(0.,-1.,0.));
#114395=DIRECTION('center_axis',(0.,0.,1.));
#114396=DIRECTION('ref_axis',(0.,1.,0.));
#114397=DIRECTION('center_axis',(0.,0.,1.));
#114398=DIRECTION('ref_axis',(0.,1.,0.));
#114399=DIRECTION('center_axis',(0.,1.23467863058847E-16,-1.));
#114400=DIRECTION('ref_axis',(-1.,0.,0.));
#114401=DIRECTION('center_axis',(0.,0.,-1.));
#114402=DIRECTION('ref_axis',(0.,1.,0.));
#114403=DIRECTION('center_axis',(0.,1.23467863058847E-16,-1.));
#114404=DIRECTION('ref_axis',(-1.,0.,0.));
#114405=DIRECTION('center_axis',(0.,0.,1.));
#114406=DIRECTION('ref_axis',(0.,-1.,0.));
#114407=DIRECTION('',(0.,0.,-1.));
#114408=DIRECTION('center_axis',(0.,0.,-1.));
#114409=DIRECTION('ref_axis',(-1.,0.,0.));
#114410=DIRECTION('center_axis',(0.,0.,-1.));
#114411=DIRECTION('ref_axis',(1.,0.,0.));
#114412=DIRECTION('',(-0.707106781186552,8.65956056235499E-17,0.707106781186543));
#114413=DIRECTION('center_axis',(0.,0.,1.));
#114414=DIRECTION('ref_axis',(1.,0.,0.));
#114415=DIRECTION('center_axis',(0.,0.,1.));
#114416=DIRECTION('ref_axis',(1.,0.,0.));
#114417=DIRECTION('center_axis',(0.,0.,-1.));
#114418=DIRECTION('ref_axis',(-1.,0.,0.));
#114419=DIRECTION('center_axis',(0.,0.,1.));
#114420=DIRECTION('ref_axis',(1.,0.,0.));
#114421=DIRECTION('',(0.,0.,1.));
#114422=DIRECTION('center_axis',(0.,1.23467863058847E-16,-1.));
#114423=DIRECTION('ref_axis',(-1.,0.,0.));
#114424=DIRECTION('center_axis',(0.,0.,-1.));
#114425=DIRECTION('ref_axis',(0.,1.,0.));
#114426=DIRECTION('center_axis',(0.,0.,-1.));
#114427=DIRECTION('ref_axis',(-1.,0.,0.));
#114428=DIRECTION('center_axis',(0.,0.,1.));
#114429=DIRECTION('ref_axis',(1.,0.,0.));
#114430=DIRECTION('',(0.,0.,1.));
#114431=DIRECTION('center_axis',(0.,0.,1.));
#114432=DIRECTION('ref_axis',(1.,0.,0.));
#114433=DIRECTION('center_axis',(-0.592966514233392,-0.805227118891249,
0.));
#114434=DIRECTION('ref_axis',(0.805227118891249,-0.592966514233392,0.));
#114435=DIRECTION('center_axis',(0.807208114890536,0.590266938981735,-2.28940150095415E-14));
#114436=DIRECTION('ref_axis',(-0.590266938981735,0.807208114890536,-1.47426480814321E-30));
#114437=DIRECTION('center_axis',(0.,-1.23467863058847E-16,1.));
#114438=DIRECTION('ref_axis',(0.,-1.,0.));
#114439=DIRECTION('center_axis',(0.,0.,-1.));
#114440=DIRECTION('ref_axis',(0.,-1.,0.));
#114441=DIRECTION('center_axis',(-1.,0.,0.));
#114442=DIRECTION('ref_axis',(0.,1.,0.));
#114443=DIRECTION('center_axis',(0.,0.,1.));
#114444=DIRECTION('ref_axis',(0.,1.,0.));
#114445=DIRECTION('center_axis',(0.,0.,1.));
#114446=DIRECTION('ref_axis',(0.,1.,0.));
#114447=DIRECTION('center_axis',(-0.168369768252295,0.882882757183484,-0.438371598312161));
#114448=DIRECTION('ref_axis',(-2.05714353600353E-15,-0.444720469017533,
-0.895669416937313));
#114449=DIRECTION('center_axis',(-0.507675385487887,-0.517400512911953,
0.688884904906599));
#114450=DIRECTION('ref_axis',(-1.34605780150592E-16,0.799589295572927,0.600547215800049));
#114451=DIRECTION('center_axis',(-0.506894799267393,-0.516604973631544,
0.690055768539632));
#114452=DIRECTION('ref_axis',(-4.2861068992561E-17,0.800521374177574,0.599304204461181));
#114453=DIRECTION('center_axis',(0.,0.,1.));
#114454=DIRECTION('ref_axis',(1.,0.,0.));
#114455=DIRECTION('center_axis',(-0.663838127753914,0.747876286654537,9.2338686945498E-17));
#114456=DIRECTION('ref_axis',(0.747876286654537,0.663838127753914,1.66533453693772E-13));
#114457=DIRECTION('center_axis',(-0.187328576766759,0.982297309538482,0.));
#114458=DIRECTION('ref_axis',(-0.982297309538482,-0.187328576766759,0.));
#114459=DIRECTION('center_axis',(-0.668574108837973,0.743645521059268,0.));
#114460=DIRECTION('ref_axis',(-0.743645521059268,-0.668574108837973,0.));
#114461=DIRECTION('center_axis',(0.,-1.23467863058847E-16,1.));
#114462=DIRECTION('ref_axis',(0.,-1.,0.));
#114463=DIRECTION('center_axis',(-0.679956281045645,0.733252654865004,0.));
#114464=DIRECTION('ref_axis',(-0.733252654865004,-0.679956281045645,0.));
#114465=DIRECTION('center_axis',(0.,0.,-1.));
#114466=DIRECTION('ref_axis',(0.,-1.,0.));
#114467=DIRECTION('center_axis',(5.71153601538328E-31,-2.64211616260599E-45,
1.));
#114468=DIRECTION('ref_axis',(-4.6259292692715E-15,-1.,-3.11150763893057E-61));
#114469=DIRECTION('center_axis',(-0.775870249713592,0.63089250717485,-1.27793330397298E-14));
#114470=DIRECTION('ref_axis',(-0.63089250717485,-0.775870249713592,-7.13011169472736E-30));
#114471=DIRECTION('center_axis',(0.,-1.23467863058847E-16,1.));
#114472=DIRECTION('ref_axis',(0.,-1.,0.));
#114473=DIRECTION('center_axis',(-0.746021307914873,0.665922073621968,0.));
#114474=DIRECTION('ref_axis',(-0.665922073621968,-0.746021307914873,0.));
#114475=DIRECTION('center_axis',(0.,0.,-1.));
#114476=DIRECTION('ref_axis',(0.,-1.,0.));
#114477=DIRECTION('center_axis',(2.41254715360152E-30,-4.7140880421464E-44,
1.));
#114478=DIRECTION('ref_axis',(-1.95398793972133E-14,-1.,1.49352366668667E-58));
#114479=DIRECTION('center_axis',(0.507468854451513,0.517190025527329,-0.68919506618715));
#114480=DIRECTION('ref_axis',(-1.08020880515219E-16,-0.799836347973839,
-0.600218140728745));
#114481=DIRECTION('center_axis',(0.,-1.23467863058847E-16,1.));
#114482=DIRECTION('ref_axis',(0.,-1.,0.));
#114483=DIRECTION('center_axis',(-0.923323390669864,0.38402332773141,-1.28136860937081E-14));
#114484=DIRECTION('ref_axis',(-0.38402332773141,-0.923323390669864,2.90201745723254E-30));
#114485=DIRECTION('center_axis',(0.,0.,-1.));
#114486=DIRECTION('ref_axis',(0.,-1.,0.));
#114487=DIRECTION('center_axis',(-6.28268961692158E-30,-3.19696055675322E-43,
1.));
#114488=DIRECTION('ref_axis',(5.08852219619863E-14,-1.,-2.38963786669868E-58));
#114489=DIRECTION('center_axis',(0.511561679834273,0.521361253861094,-0.682998602266158));
#114490=DIRECTION('ref_axis',(1.21631079100244E-16,-0.79488081246627,-0.606765600518819));
#114491=DIRECTION('center_axis',(-0.987526870499689,0.134244619791538,-0.0822743100737742));
#114492=DIRECTION('ref_axis',(-0.134701294632915,-0.990886250396188,-7.62230551969098E-18));
#114493=DIRECTION('center_axis',(0.887573437172827,-0.12065692809958,-0.444584411925099));
#114494=DIRECTION('ref_axis',(-0.447856331161543,-5.04904183848934E-18,
-0.89410553439654));
#114495=DIRECTION('center_axis',(0.502571259550305,0.589216419045832,0.632650093338194));
#114496=DIRECTION('ref_axis',(-0.234843565694733,-0.611220822461641,0.755815854452061));
#114497=DIRECTION('center_axis',(0.,0.,1.));
#114498=DIRECTION('ref_axis',(1.,0.,0.));
#114499=DIRECTION('center_axis',(0.606371999687993,-0.771616335224111,0.192148976603301));
#114500=DIRECTION('ref_axis',(0.786267832350933,0.617885827487704,-3.1641897774151E-17));
#114501=DIRECTION('center_axis',(-0.645804421056786,-0.763502881293522,
-1.01980482580395E-14));
#114502=DIRECTION('ref_axis',(0.763502881293522,-0.645804421056786,-6.9816295225584E-30));
#114503=DIRECTION('center_axis',(0.48724015249101,-0.488874385354372,-0.723601319197887));
#114504=DIRECTION('ref_axis',(-1.47352524967685E-15,-0.828613098245121,
0.559821697879442));
#114505=DIRECTION('center_axis',(0.488418020654004,-0.490056204158282,-0.722006062208899));
#114506=DIRECTION('ref_axis',(3.20373038523992E-15,-0.827409999881363,0.561598336977882));
#114507=DIRECTION('center_axis',(-0.753146254930614,-0.657853113304171,
-3.00335537434998E-14));
#114508=DIRECTION('ref_axis',(0.657853113304171,-0.753146254930614,-2.96993835591878E-30));
#114509=DIRECTION('center_axis',(-0.171101227036283,-0.869601781127171,
-0.463159920942141));
#114510=DIRECTION('ref_axis',(-4.21773228904835E-17,-0.470092156192753,
0.882617337630554));
#114511=DIRECTION('center_axis',(0.484433158250521,-0.486057976285942,-0.727373465886845));
#114512=DIRECTION('ref_axis',(-3.34045680200078E-15,-0.831447136037245,
0.555603869654868));
#114513=DIRECTION('center_axis',(1.,0.,0.));
#114514=DIRECTION('ref_axis',(0.,-1.,0.));
#114515=DIRECTION('center_axis',(-0.193053842425666,-0.981173356447606,
0.00539059570228739));
#114516=DIRECTION('ref_axis',(0.981187612482096,-0.193056647416463,-1.03740416739262E-18));
#114517=DIRECTION('center_axis',(-0.663957144707683,-0.747700087626819,
0.0102707815899847));
#114518=DIRECTION('ref_axis',(0.747739527797473,-0.663992167551103,3.3311423852743E-19));
#114519=DIRECTION('center_axis',(0.485576620175616,-0.487205273451398,-0.725841833638689));
#114520=DIRECTION('ref_axis',(1.3020744827461E-16,-0.830298240911906,0.557319326004935));
#114521=DIRECTION('center_axis',(-0.210025631952355,-0.977695880078777,
0.));
#114522=DIRECTION('ref_axis',(0.977695880078777,-0.210025631952355,0.));
#114523=DIRECTION('center_axis',(0.869253009153379,0.170328745809824,-0.464098399510975));
#114524=DIRECTION('ref_axis',(-0.470980702241858,8.1123542202202E-17,-0.882143513333157));
#114525=DIRECTION('center_axis',(0.,1.23467863058847E-16,-1.));
#114526=DIRECTION('ref_axis',(0.,1.,0.));
#114527=DIRECTION('center_axis',(-0.67420688908099,-0.738542531419643,0.));
#114528=DIRECTION('ref_axis',(0.738542531419643,-0.67420688908099,0.));
#114529=DIRECTION('center_axis',(0.,0.,1.));
#114530=DIRECTION('ref_axis',(0.,1.,0.));
#114531=DIRECTION('center_axis',(-4.28365201153744E-31,1.48619034146585E-45,
-1.));
#114532=DIRECTION('ref_axis',(3.46944695195361E-15,1.,1.24460305557223E-60));
#114533=DIRECTION('center_axis',(1.,0.,0.));
#114534=DIRECTION('ref_axis',(0.,-1.,0.));
#114535=DIRECTION('center_axis',(0.752788125817861,0.658228853504028,0.00669432912290745));
#114536=DIRECTION('ref_axis',(0.658243602947644,-0.752804994124312,-1.11021690861332E-13));
#114537=DIRECTION('center_axis',(0.981331609270135,0.192290369398073,0.00356180909645361));
#114538=DIRECTION('ref_axis',(-0.192291589154029,0.981337834153263,-1.28820063606849E-18));
#114539=DIRECTION('center_axis',(0.,1.23467863058847E-16,-1.));
#114540=DIRECTION('ref_axis',(0.,1.,0.));
#114541=DIRECTION('center_axis',(-0.74079592940915,-0.671730147433353,0.));
#114542=DIRECTION('ref_axis',(0.671730147433353,-0.74079592940915,0.));
#114543=DIRECTION('center_axis',(0.,0.,1.));
#114544=DIRECTION('ref_axis',(0.,1.,0.));
#114545=DIRECTION('center_axis',(-1.64492525510334E-30,2.19148451090235E-44,
-1.));
#114546=DIRECTION('ref_axis',(1.33226996430588E-14,1.,1.74244427780112E-59));
#114547=DIRECTION('center_axis',(0.979119873047182,0.203283728330798,0.));
#114548=DIRECTION('ref_axis',(-0.203283728330798,0.979119873047182,0.));
#114549=DIRECTION('center_axis',(0.,1.23467863058847E-16,-1.));
#114550=DIRECTION('ref_axis',(0.,1.,0.));
#114551=DIRECTION('center_axis',(-2.57019120692247E-30,5.35028522927707E-44,
-1.));
#114552=DIRECTION('ref_axis',(2.08166817117217E-14,1.,-1.99136488891557E-59));
#114553=DIRECTION('center_axis',(0.,0.,1.));
#114554=DIRECTION('ref_axis',(0.,1.,0.));
#114555=DIRECTION('center_axis',(0.,-1.23467863058847E-16,1.));
#114556=DIRECTION('ref_axis',(0.,-1.,0.));
#114557=DIRECTION('center_axis',(0.777162624242377,0.629299813666508,0.));
#114558=DIRECTION('ref_axis',(-0.629299813666508,0.777162624242377,0.));
#114559=DIRECTION('center_axis',(0.,0.,-1.));
#114560=DIRECTION('ref_axis',(0.,-1.,0.));
#114561=DIRECTION('center_axis',(0.982297019165463,0.187330099393145,0.));
#114562=DIRECTION('ref_axis',(-0.187330099393145,0.982297019165463,0.));
#114563=DIRECTION('center_axis',(4.46763300492346E-31,-1.61659432440069E-45,
1.));
#114564=DIRECTION('ref_axis',(-3.61845819166247E-15,-1.,1.86690458335834E-60));
#114565=DIRECTION('center_axis',(0.,-1.23467863058847E-16,1.));
#114566=DIRECTION('ref_axis',(0.,-1.,0.));
#114567=DIRECTION('center_axis',(0.635030358342585,0.772487180465338,0.));
#114568=DIRECTION('ref_axis',(-0.772487180465338,0.635030358342585,0.));
#114569=DIRECTION('center_axis',(0.,0.,-1.));
#114570=DIRECTION('ref_axis',(0.,-1.,0.));
#114571=DIRECTION('center_axis',(1.09661491495359E-30,-9.73989702183063E-45,
1.));
#114572=DIRECTION('ref_axis',(-8.88178419700125E-15,-1.,2.48920611114446E-60));
#114573=DIRECTION('center_axis',(0.,-1.23467863058847E-16,1.));
#114574=DIRECTION('ref_axis',(0.,-1.,0.));
#114575=DIRECTION('center_axis',(0.0394959395290733,0.999219730970479,0.));
#114576=DIRECTION('ref_axis',(-0.999219730970479,0.0394959395290733,0.));
#114577=DIRECTION('center_axis',(0.,0.,-1.));
#114578=DIRECTION('ref_axis',(0.,-1.,0.));
#114579=DIRECTION('center_axis',(6.70144950738521E-31,-3.63733722990157E-45,
1.));
#114580=DIRECTION('ref_axis',(-5.42768728749372E-15,-1.,2.48920611114446E-60));
#114581=DIRECTION('center_axis',(0.,-1.23467863058847E-16,1.));
#114582=DIRECTION('ref_axis',(0.,-1.,-1.33055111034894E-16));
#114583=DIRECTION('center_axis',(-0.0394959395290663,0.999219730970479,
0.));
#114584=DIRECTION('ref_axis',(-0.999219730970479,-0.0394959395290663,0.));
#114585=DIRECTION('center_axis',(0.,1.29997489681772E-16,-1.));
#114586=DIRECTION('ref_axis',(0.,-1.,-1.29997489681772E-16));
#114587=DIRECTION('center_axis',(0.,-1.30058395245648E-16,1.));
#114588=DIRECTION('ref_axis',(0.,-1.,-1.30058395245648E-16));
#114589=DIRECTION('center_axis',(0.,-1.23467863058847E-16,1.));
#114590=DIRECTION('ref_axis',(0.,-1.,0.));
#114591=DIRECTION('center_axis',(-0.635030358342616,0.772487180465313,0.));
#114592=DIRECTION('ref_axis',(-0.772487180465313,-0.635030358342616,0.));
#114593=DIRECTION('center_axis',(0.,0.,-1.));
#114594=DIRECTION('ref_axis',(0.,-1.,0.));
#114595=DIRECTION('center_axis',(-5.21223850574408E-31,-2.20036449710098E-45,
1.));
#114596=DIRECTION('ref_axis',(4.22153455693958E-15,-1.,-9.33452291679171E-61));
#114597=DIRECTION('center_axis',(0.,-1.23467863058847E-16,1.));
#114598=DIRECTION('ref_axis',(0.,-1.,0.));
#114599=DIRECTION('center_axis',(-0.774287490710421,0.632834008037937,0.));
#114600=DIRECTION('ref_axis',(-0.632834008037937,-0.774287490710421,0.));
#114601=DIRECTION('center_axis',(0.,0.,-1.));
#114602=DIRECTION('ref_axis',(0.,-1.,0.));
#114603=DIRECTION('center_axis',(0.,0.,1.));
#114604=DIRECTION('ref_axis',(0.,-1.,0.));
#114605=DIRECTION('center_axis',(0.,-1.23467863058847E-16,1.));
#114606=DIRECTION('ref_axis',(0.,-1.,0.));
#114607=DIRECTION('center_axis',(-0.999225121087074,0.0393593367388477,
0.));
#114608=DIRECTION('ref_axis',(-0.0393593367388477,-0.999225121087074,0.));
#114609=DIRECTION('center_axis',(0.,0.,-1.));
#114610=DIRECTION('ref_axis',(0.,-1.,0.));
#114611=DIRECTION('center_axis',(5.21223850574404E-31,-2.20036449710094E-45,
1.));
#114612=DIRECTION('ref_axis',(-4.22153455693955E-15,-1.,2.48920611114446E-60));
#114613=DIRECTION('center_axis',(0.,0.,-1.));
#114614=DIRECTION('ref_axis',(-0.751703367637011,-0.659501362457407,0.));
#114615=DIRECTION('center_axis',(0.659496851377394,-0.751707325375577,0.));
#114616=DIRECTION('ref_axis',(0.751707325375577,0.659496851377394,0.));
#114617=DIRECTION('center_axis',(-0.00318935089126825,-0.00297677156874421,
0.999990483390677));
#114618=DIRECTION('ref_axis',(-0.747789842767528,-0.663921177326532,-0.0043613473913037));
#114619=DIRECTION('center_axis',(0.657034976183429,-0.753860093168249,1.01740733956786E-14));
#114620=DIRECTION('ref_axis',(0.753860093168249,0.657034976183429,-8.45764823615526E-31));
#114621=DIRECTION('center_axis',(-0.00280476608066071,-0.00263885430337773,
0.999992584840107));
#114622=DIRECTION('ref_axis',(0.937191712771117,-0.348810515489431,0.00170815606344439));
#114623=DIRECTION('center_axis',(0.768895279480121,0.207195498703726,-0.604871948853723));
#114624=DIRECTION('ref_axis',(-0.618289095466814,1.21523947502978E-17,-0.785950758271044));
#114625=DIRECTION('center_axis',(0.202724571193613,0.760898522337225,-0.616389638896853));
#114626=DIRECTION('ref_axis',(-1.87348493224475E-17,-0.629459870756021,
-0.777032992290426));
#114627=DIRECTION('center_axis',(0.767736348840716,0.206883199723352,-0.606448876939313));
#114628=DIRECTION('ref_axis',(-0.619859127336644,-1.17584790122141E-16,
-0.784713108248775));
#114629=DIRECTION('center_axis',(0.260190354028299,-0.965557341472079,1.40549396816343E-10));
#114630=DIRECTION('ref_axis',(-0.58403426831887,-0.15738069260472,-0.796326121023605));
#114631=DIRECTION('center_axis',(-0.243334995703589,0.96954396966785,0.0277951568918529));
#114632=DIRECTION('ref_axis',(-0.594809401908895,-0.126526334687349,-0.793846875682815));
#114633=DIRECTION('center_axis',(0.202457297762738,0.759895348634851,-0.617713608159743));
#114634=DIRECTION('ref_axis',(5.55058625584594E-17,-0.630776296546234,-0.775964730973913));
#114635=DIRECTION('center_axis',(0.966468863382725,-0.256741605888852,0.00465659932972454));
#114636=DIRECTION('ref_axis',(-0.154910761359747,-0.597411475844062,-0.786830467473625));
#114637=DIRECTION('center_axis',(-0.966292363520655,0.25744721439873,-4.29897349204163E-11));
#114638=DIRECTION('ref_axis',(-0.159028116924834,-0.596889950284185,-0.786404759190256));
#114639=DIRECTION('center_axis',(0.578576029254642,0.155909851599689,-0.800588468906525));
#114640=DIRECTION('ref_axis',(-0.810499837678775,1.21842170142303E-15,-0.585738860860947));
#114641=DIRECTION('center_axis',(0.153941565569776,0.577798286012631,-0.801530495409122));
#114642=DIRECTION('ref_axis',(-1.29290181198153E-17,-0.811200037627138,
-0.584768756820788));
#114643=DIRECTION('center_axis',(0.0544019837731304,-0.025960154057113,
-0.998181593981215));
#114644=DIRECTION('ref_axis',(-0.998518116145471,-1.61274188638027E-18,
-0.054420324597515));
#114645=DIRECTION('center_axis',(-0.025995718416376,0.0542003143889016,
-0.998191639187667));
#114646=DIRECTION('ref_axis',(1.6064497712818E-18,-0.99852908789078,-0.0542186373492239));
#114647=DIRECTION('center_axis',(0.734334158412678,-0.678788143523695,2.48736119588291E-13));
#114648=DIRECTION('ref_axis',(0.678788143523695,0.734334158412678,-6.81231552358944E-29));
#114649=DIRECTION('center_axis',(-0.680870844883917,0.73240350394237,1.91708814121709E-12));
#114650=DIRECTION('ref_axis',(-0.73240350394237,-0.680870844883917,-1.31317411609931E-27));
#114651=DIRECTION('center_axis',(0.,-1.23467863058847E-16,1.));
#114652=DIRECTION('ref_axis',(0.,-1.,0.));
#114653=DIRECTION('center_axis',(0.,0.,-1.));
#114654=DIRECTION('ref_axis',(0.,1.,0.));
#114655=DIRECTION('center_axis',(-9.86953423458227E-31,-7.88931658768281E-45,
1.));
#114656=DIRECTION('ref_axis',(7.99360577730113E-15,-1.,2.48920611114446E-60));
#114657=DIRECTION('center_axis',(0.0255375237255525,0.0535186253292443,
0.998240247447895));
#114658=DIRECTION('ref_axis',(-2.96412751937958E-19,0.998565915482956,-0.0535360853601283));
#114659=DIRECTION('center_axis',(-0.682537484892591,-0.730850587819765,
8.37209378123771E-13));
#114660=DIRECTION('ref_axis',(0.730850587819765,-0.682537484892591,3.92323810141884E-28));
#114661=DIRECTION('center_axis',(0.,-1.23467863058847E-16,1.));
#114662=DIRECTION('ref_axis',(0.,-1.,0.));
#114663=DIRECTION('center_axis',(-0.735878524541007,-0.677113577710085,
5.64206319996869E-13));
#114664=DIRECTION('ref_axis',(0.677113577710085,-0.735878524541007,-1.38055872491966E-28));
#114665=DIRECTION('center_axis',(0.,0.,1.));
#114666=DIRECTION('ref_axis',(0.,-1.,0.));
#114667=DIRECTION('center_axis',(5.92172054074936E-30,2.84015397156581E-43,
-1.));
#114668=DIRECTION('ref_axis',(-4.79616346638068E-14,1.,-2.78791084448179E-58));
#114669=DIRECTION('center_axis',(-0.152544532818274,0.577842847451632,0.801765432752152));
#114670=DIRECTION('ref_axis',(4.14384419008336E-17,0.811259933931047,-0.58468565879299));
#114671=DIRECTION('center_axis',(-0.0536778879072088,-0.0251150971461135,
0.998242413567548));
#114672=DIRECTION('ref_axis',(0.998557392321894,-9.29874389531901E-20,0.0536948250700053));
#114673=DIRECTION('center_axis',(-0.19315692461333,0.731683694333232,0.653704347485004));
#114674=DIRECTION('ref_axis',(-3.51224977473848E-17,0.66625127354731,-0.745727323152764));
#114675=DIRECTION('center_axis',(-0.576537673896198,0.156770156178271,0.801889910592596));
#114676=DIRECTION('ref_axis',(0.811929324239482,3.97972821433516E-17,0.583755747243673));
#114677=DIRECTION('center_axis',(-0.193538145022295,0.733127767631913,0.651971366509586));
#114678=DIRECTION('ref_axis',(1.09087611421558E-16,0.664535912353125,-0.747256328974871));
#114679=DIRECTION('center_axis',(0.967398007177023,0.253182433216653,0.00630485689132568));
#114680=DIRECTION('ref_axis',(-0.16111421782421,0.634435934472465,-0.755998183770929));
#114681=DIRECTION('center_axis',(-0.966876318105823,-0.255245343710962,
-5.9860823738661E-11));
#114682=DIRECTION('ref_axis',(-0.166411982471238,0.630373124957365,-0.758245854206588));
#114683=DIRECTION('center_axis',(-0.72784499809572,0.197913127261801,0.656560776169652));
#114684=DIRECTION('ref_axis',(0.669809908048189,2.97308687105849E-17,0.742532616846207));
#114685=DIRECTION('center_axis',(-0.72888212476865,0.19819513920631,0.655323992379136));
#114686=DIRECTION('ref_axis',(0.668587032943078,1.18015531912611E-16,0.743633901446385));
#114687=DIRECTION('center_axis',(0.262389207131878,0.964962125671627,-2.3868460211661E-11));
#114688=DIRECTION('ref_axis',(-0.633554268004896,0.172273913779853,-0.754274941996453));
#114689=DIRECTION('center_axis',(-0.257377402244523,-0.96626185396935,0.00974178513293261));
#114690=DIRECTION('ref_axis',(-0.635976884577247,0.161793976065296,-0.754556897518273));
#114691=DIRECTION('center_axis',(0.70592193778968,-0.708289642552581,-8.74510085926821E-17));
#114692=DIRECTION('ref_axis',(-0.708289642552581,-0.70592193778968,-3.19694546253078E-33));
#114693=DIRECTION('',(-0.70592193778968,0.708289642552581,8.74510085926821E-17));
#114694=DIRECTION('center_axis',(-0.705921937789676,0.708289642552585,-6.53108990768421E-15));
#114695=DIRECTION('ref_axis',(-0.708289642552585,-0.705921937789676,-2.24639971032546E-30));
#114696=DIRECTION('',(0.70592193778968,-0.708289642552581,-8.74510085926821E-17));
#114697=DIRECTION('center_axis',(0.,0.,-1.));
#114698=DIRECTION('ref_axis',(0.,1.,0.));
#114699=DIRECTION('center_axis',(0.,0.,1.));
#114700=DIRECTION('ref_axis',(0.,1.,0.));
#114701=DIRECTION('center_axis',(-0.74079592940915,-0.671730147433353,0.));
#114702=DIRECTION('ref_axis',(0.671730147433353,-0.74079592940915,0.));
#114703=DIRECTION('center_axis',(0.,1.23467863058847E-16,-1.));
#114704=DIRECTION('ref_axis',(0.,1.,0.));
#114705=DIRECTION('center_axis',(0.,0.,1.));
#114706=DIRECTION('ref_axis',(0.,1.,0.));
#114707=DIRECTION('center_axis',(-0.674206889080985,-0.738542531419647,
0.));
#114708=DIRECTION('ref_axis',(0.738542531419647,-0.674206889080985,0.));
#114709=DIRECTION('center_axis',(-2.41254715360153E-30,4.71408804214643E-44,
-1.));
#114710=DIRECTION('ref_axis',(1.95398793972133E-14,1.,5.9740946667467E-59));
#114711=DIRECTION('center_axis',(0.,0.,1.));
#114712=DIRECTION('ref_axis',(0.,1.,0.));
#114713=DIRECTION('center_axis',(0.7059219377897,-0.708289642552562,-2.19056695270365E-17));
#114714=DIRECTION('ref_axis',(0.708289642552562,0.7059219377897,4.72941823813195E-33));
#114715=DIRECTION('center_axis',(0.,0.,-1.));
#114716=DIRECTION('ref_axis',(0.,1.,0.));
#114717=DIRECTION('center_axis',(0.,0.,1.));
#114718=DIRECTION('ref_axis',(0.,1.,0.));
#114719=DIRECTION('center_axis',(-0.7059219377897,0.708289642552561,8.74510085926797E-17));
#114720=DIRECTION('ref_axis',(0.708289642552561,0.7059219377897,-8.55019604084016E-33));
#114721=DIRECTION('',(-0.7059219377897,0.708289642552561,8.74510085926797E-17));
#114722=DIRECTION('',(0.7059219377897,-0.708289642552561,-8.74510085926797E-17));
#114723=DIRECTION('center_axis',(-0.964962125666191,0.262389207151869,3.23966346967465E-17));
#114724=DIRECTION('ref_axis',(0.262389207151869,0.964962125666191,-4.57090956622107E-33));
#114725=DIRECTION('',(-0.964962125666191,0.262389207151869,3.23966346967465E-17));
#114726=DIRECTION('center_axis',(-0.964962125666191,0.26238920715187,2.42758782660955E-15));
#114727=DIRECTION('ref_axis',(-0.26238920715187,-0.964962125666191,2.22950724024121E-31));
#114728=DIRECTION('',(0.964962125666191,-0.262389207151869,-3.23966346967465E-17));
#114729=DIRECTION('center_axis',(0.,0.,-1.));
#114730=DIRECTION('ref_axis',(0.,1.,0.));
#114731=DIRECTION('center_axis',(0.,0.,1.));
#114732=DIRECTION('ref_axis',(0.,1.,0.));
#114733=DIRECTION('center_axis',(-0.735878524541004,-0.677113577710087,
0.));
#114734=DIRECTION('ref_axis',(0.677113577710087,-0.735878524541004,0.));
#114735=DIRECTION('center_axis',(0.,1.23467863058847E-16,-1.));
#114736=DIRECTION('ref_axis',(0.,1.,0.));
#114737=DIRECTION('center_axis',(-0.682537484892593,-0.730850587819763,
0.));
#114738=DIRECTION('ref_axis',(0.730850587819763,-0.682537484892593,0.));
#114739=DIRECTION('center_axis',(4.93476711729114E-30,1.97232914692071E-43,
-1.));
#114740=DIRECTION('ref_axis',(-3.99680288865056E-14,1.,0.));
#114741=DIRECTION('center_axis',(0.,0.,1.));
#114742=DIRECTION('ref_axis',(0.,1.,0.));
#114743=DIRECTION('center_axis',(0.255245343760721,-0.966876318092687,-2.36149381309596E-15));
#114744=DIRECTION('ref_axis',(0.966876318092687,0.255245343760721,9.80822191756775E-31));
#114745=DIRECTION('center_axis',(-5.71153601538325E-31,2.64211616260596E-45,
-1.));
#114746=DIRECTION('ref_axis',(4.62592926927148E-15,1.,1.24460305557223E-60));
#114747=DIRECTION('center_axis',(0.,0.,1.));
#114748=DIRECTION('ref_axis',(0.,1.,0.));
#114749=DIRECTION('center_axis',(0.255245343760725,-0.966876318092686,-1.1937815283711E-16));
#114750=DIRECTION('ref_axis',(-0.966876318092686,-0.255245343760725,-8.61241374820812E-33));
#114751=DIRECTION('',(-0.255245343760725,0.966876318092686,1.1937815283711E-16));
#114752=DIRECTION('',(0.255245343760725,-0.966876318092686,-1.1937815283711E-16));
#114753=DIRECTION('center_axis',(0.257447214431338,0.966292363511968,1.19306053212906E-16));
#114754=DIRECTION('ref_axis',(0.966292363511968,-0.257447214431338,-1.5335664280992E-33));
#114755=DIRECTION('',(-0.257447214431338,-0.966292363511968,-1.19306053212906E-16));
#114756=DIRECTION('center_axis',(-0.257447214431328,-0.96629236351197,1.78800005081742E-14));
#114757=DIRECTION('ref_axis',(0.96629236351197,-0.257447214431328,-3.12759209575828E-30));
#114758=DIRECTION('',(0.257447214431338,0.966292363511968,1.19306053212906E-16));
#114759=DIRECTION('center_axis',(0.680870844883904,-0.732403503942382,0.));
#114760=DIRECTION('ref_axis',(0.732403503942382,0.680870844883904,0.));
#114761=DIRECTION('center_axis',(0.,0.,-1.));
#114762=DIRECTION('ref_axis',(0.,-1.,0.));
#114763=DIRECTION('center_axis',(0.,0.,1.));
#114764=DIRECTION('ref_axis',(0.,-1.,0.));
#114765=DIRECTION('center_axis',(0.,-1.23467863058847E-16,1.));
#114766=DIRECTION('ref_axis',(0.,-1.,0.));
#114767=DIRECTION('center_axis',(0.734334158412675,-0.678788143523698,0.));
#114768=DIRECTION('ref_axis',(0.678788143523698,0.734334158412675,0.));
#114769=DIRECTION('center_axis',(0.,0.,-1.));
#114770=DIRECTION('ref_axis',(0.,-1.,0.));
#114771=DIRECTION('center_axis',(4.05747518532827E-30,-1.33339190228861E-43,
1.));
#114772=DIRECTION('ref_axis',(-3.28626015289047E-14,-1.,2.58877435559024E-58));
#114773=DIRECTION('center_axis',(0.,0.,1.));
#114774=DIRECTION('ref_axis',(0.,-1.,0.));
#114775=DIRECTION('center_axis',(0.965557341499939,0.260190353924909,-4.11871123919569E-15));
#114776=DIRECTION('ref_axis',(-0.260190353924909,0.965557341499939,-2.2632930465492E-31));
#114777=DIRECTION('center_axis',(0.,0.,-1.));
#114778=DIRECTION('ref_axis',(0.,-1.,0.));
#114779=DIRECTION('center_axis',(-0.965557341499939,-0.260190353924911,
-3.21251469876339E-17));
#114780=DIRECTION('ref_axis',(-0.260190353924911,0.965557341499939,-9.87488652925334E-34));
#114781=DIRECTION('',(-0.965557341499939,-0.260190353924911,-3.21251469876339E-17));
#114782=DIRECTION('',(0.965557341499939,0.260190353924911,3.21251469876339E-17));
#114783=DIRECTION('center_axis',(-0.700366780446484,-0.713783141330072,
-8.81292791474553E-17));
#114784=DIRECTION('ref_axis',(-0.713783141330072,0.700366780446484,-8.54636793605324E-33));
#114785=DIRECTION('',(-0.700366780446485,-0.713783141330072,-8.81292791474553E-17));
#114786=DIRECTION('center_axis',(-0.700366780446484,-0.713783141330073,
0.));
#114787=DIRECTION('ref_axis',(0.713783141330073,-0.700366780446484,0.));
#114788=DIRECTION('',(0.700366780446485,0.713783141330072,8.81292791474553E-17));
#114789=DIRECTION('center_axis',(0.679956281045647,-0.733252654865001,0.));
#114790=DIRECTION('ref_axis',(0.733252654865001,0.679956281045647,0.));
#114791=DIRECTION('center_axis',(0.,0.,-1.));
#114792=DIRECTION('ref_axis',(0.,-1.,0.));
#114793=DIRECTION('center_axis',(0.,0.,1.));
#114794=DIRECTION('ref_axis',(0.,-1.,0.));
#114795=DIRECTION('center_axis',(0.,-1.23467863058847E-16,1.));
#114796=DIRECTION('ref_axis',(0.,-1.,0.));
#114797=DIRECTION('center_axis',(0.746021307914879,-0.665922073621961,1.23220336456872E-14));
#114798=DIRECTION('ref_axis',(0.665922073621961,0.746021307914879,1.41534494748923E-30));
#114799=DIRECTION('center_axis',(0.,0.,-1.));
#114800=DIRECTION('ref_axis',(0.,-1.,0.));
#114801=DIRECTION('center_axis',(3.28984144636074E-30,-8.76588974171719E-44,
1.));
#114802=DIRECTION('ref_axis',(-2.66453258755498E-14,-1.,1.59309191113245E-58));
#114803=DIRECTION('center_axis',(0.,0.,1.));
#114804=DIRECTION('ref_axis',(0.,-1.,0.));
#114805=DIRECTION('center_axis',(0.700366780446456,0.7137831413301,0.));
#114806=DIRECTION('ref_axis',(-0.7137831413301,0.700366780446456,0.));
#114807=DIRECTION('center_axis',(0.,0.,-1.));
#114808=DIRECTION('ref_axis',(0.,-1.,0.));
#114809=DIRECTION('center_axis',(0.700366780446451,0.713783141330105,8.81292791474594E-17));
#114810=DIRECTION('ref_axis',(0.713783141330105,-0.700366780446451,4.73735951537523E-32));
#114811=DIRECTION('',(-0.700366780446451,-0.713783141330105,-8.81292791474594E-17));
#114812=DIRECTION('',(0.700366780446451,0.713783141330105,8.81292791474594E-17));
#114813=DIRECTION('center_axis',(0.,0.,-1.));
#114814=DIRECTION('ref_axis',(0.,1.,0.));
#114815=DIRECTION('',(0.,1.23467863058847E-16,-1.));
#114816=DIRECTION('',(6.16297582203915E-33,-1.23467863058847E-16,1.));
#114817=DIRECTION('center_axis',(0.,0.,-1.));
#114818=DIRECTION('ref_axis',(0.,1.,0.));
#114819=DIRECTION('',(-7.37292681274632E-34,1.23467863058847E-16,-1.));
#114820=DIRECTION('',(0.,-1.23467863058847E-16,1.));
#114821=DIRECTION('center_axis',(0.,0.,1.));
#114822=DIRECTION('ref_axis',(0.,-1.,0.));
#114823=DIRECTION('',(0.,1.23467863058847E-16,-1.));
#114824=DIRECTION('',(0.,-1.23467863058847E-16,1.));
#114825=DIRECTION('center_axis',(0.,0.,1.));
#114826=DIRECTION('ref_axis',(0.0252625808996282,0.999680850074808,0.));
#114827=DIRECTION('',(5.83684288299471E-35,1.23467863058847E-16,-1.));
#114828=DIRECTION('',(0.,-1.23467863058847E-16,1.));
#114829=DIRECTION('center_axis',(0.,0.,1.));
#114830=DIRECTION('ref_axis',(0.,-1.,0.));
#114831=DIRECTION('',(3.52789515968553E-33,1.23467863058847E-16,-1.));
#114832=DIRECTION('',(0.,-1.23467863058847E-16,1.));
#114833=DIRECTION('center_axis',(0.,0.,1.));
#114834=DIRECTION('ref_axis',(0.,-1.,0.));
#114835=DIRECTION('',(-1.21605822285869E-32,-1.23467863058847E-16,1.));
#114836=DIRECTION('',(0.,1.23467863058847E-16,-1.));
#114837=DIRECTION('center_axis',(0.,0.,-1.));
#114838=DIRECTION('ref_axis',(-0.239106811829941,-0.970993271107746,0.));
#114839=DIRECTION('',(0.,1.23467863058847E-16,-1.));
#114840=DIRECTION('',(6.62645671305077E-33,-1.23467863058847E-16,1.));
#114841=DIRECTION('center_axis',(0.,0.,-1.));
#114842=DIRECTION('ref_axis',(0.,1.,0.));
#114843=DIRECTION('',(6.16297582203915E-33,1.23467863058847E-16,-1.));
#114844=DIRECTION('',(0.,-1.23467863058847E-16,1.));
#114845=DIRECTION('center_axis',(0.,1.23467863058847E-16,-1.));
#114846=DIRECTION('ref_axis',(0.,1.,0.));
#114847=DIRECTION('center_axis',(0.,0.,-1.));
#114848=DIRECTION('ref_axis',(0.,1.,0.));
#114849=DIRECTION('center_axis',(0.,-1.,0.));
#114850=DIRECTION('ref_axis',(0.,0.,1.));
#114851=DIRECTION('center_axis',(0.,0.,1.));
#114852=DIRECTION('ref_axis',(0.,1.,0.));
#114853=DIRECTION('center_axis',(-0.994416787801726,-0.105523704152657,
0.));
#114854=DIRECTION('ref_axis',(0.105523704152657,-0.994416787801726,0.));
#114855=DIRECTION('center_axis',(-7.82779334765923E-17,1.,0.));
#114856=DIRECTION('ref_axis',(0.,0.,1.));
#114857=DIRECTION('center_axis',(0.,-1.,0.));
#114858=DIRECTION('ref_axis',(0.,0.,1.));
#114859=DIRECTION('',(-7.82779334765923E-17,1.,1.23467863058847E-16));
#114860=DIRECTION('',(7.82779334765923E-17,-1.,-1.23467863058847E-16));
#114861=DIRECTION('center_axis',(0.,1.23467863058847E-16,-1.));
#114862=DIRECTION('ref_axis',(0.,1.,1.38375392967352E-16));
#114863=DIRECTION('center_axis',(-0.992522955047552,-0.122058116090968,
0.));
#114864=DIRECTION('ref_axis',(0.122058116090968,-0.992522955047552,0.));
#114865=DIRECTION('center_axis',(6.16166569047948E-31,1.35428930001789E-16,
-1.));
#114866=DIRECTION('ref_axis',(5.15143483426073E-14,1.,1.35428930001789E-16));
#114867=DIRECTION('center_axis',(0.,-1.35726946151947E-16,1.));
#114868=DIRECTION('ref_axis',(0.,1.,1.35726946151947E-16));
#114869=DIRECTION('center_axis',(0.,1.23467863058847E-16,-1.));
#114870=DIRECTION('ref_axis',(0.,1.,0.));
#114871=DIRECTION('center_axis',(-1.,0.,0.));
#114872=DIRECTION('ref_axis',(0.,0.,1.));
#114873=DIRECTION('center_axis',(0.,0.,1.));
#114874=DIRECTION('ref_axis',(0.,1.,0.));
#114875=DIRECTION('center_axis',(0.,0.,-1.));
#114876=DIRECTION('ref_axis',(0.,1.,0.));
#114877=DIRECTION('center_axis',(0.,1.23467863058847E-16,-1.));
#114878=DIRECTION('ref_axis',(0.,1.,0.));
#114879=DIRECTION('center_axis',(-0.848949186868299,-0.528474481990998,
0.));
#114880=DIRECTION('ref_axis',(0.528474481990998,-0.848949186868299,0.));
#114881=DIRECTION('center_axis',(-2.06796993660427E-30,3.463654065723E-44,
-1.));
#114882=DIRECTION('ref_axis',(1.67490542508106E-14,1.,-2.09093313336134E-58));
#114883=DIRECTION('center_axis',(0.,0.,1.));
#114884=DIRECTION('ref_axis',(0.,1.,0.));
#114885=DIRECTION('center_axis',(-1.,0.,-1.17757899099328E-32));
#114886=DIRECTION('ref_axis',(0.,1.,0.));
#114887=DIRECTION('center_axis',(-1.,0.,0.));
#114888=DIRECTION('ref_axis',(0.,0.,1.));
#114889=DIRECTION('',(1.,9.53753439817791E-17,1.17757899099328E-32));
#114890=DIRECTION('',(-1.,-9.53753439817791E-17,-1.17757899099328E-32));
#114891=DIRECTION('center_axis',(0.,1.23467863058847E-16,-1.));
#114892=DIRECTION('ref_axis',(0.,1.,0.));
#114893=DIRECTION('center_axis',(-0.787431540449703,-0.616402116402116,
0.));
#114894=DIRECTION('ref_axis',(0.616402116402116,-0.787431540449703,0.));
#114895=DIRECTION('center_axis',(-7.6763044046751E-31,4.77254954069701E-45,
-1.));
#114896=DIRECTION('ref_axis',(6.21724893790088E-15,1.,-1.86690458335834E-60));
#114897=DIRECTION('center_axis',(0.,0.,1.));
#114898=DIRECTION('ref_axis',(0.,1.,0.));
#114899=DIRECTION('center_axis',(0.,1.23467863058847E-16,-1.));
#114900=DIRECTION('ref_axis',(0.,1.,0.));
#114901=DIRECTION('center_axis',(0.,1.,0.));
#114902=DIRECTION('ref_axis',(0.,0.,-1.));
#114903=DIRECTION('center_axis',(0.,0.,1.));
#114904=DIRECTION('ref_axis',(0.,1.,0.));
#114905=DIRECTION('center_axis',(0.,0.,-1.));
#114906=DIRECTION('ref_axis',(0.,1.,0.));
#114907=DIRECTION('center_axis',(0.,1.23467863058847E-16,-1.));
#114908=DIRECTION('ref_axis',(0.,1.,0.));
#114909=DIRECTION('center_axis',(0.,-1.,0.));
#114910=DIRECTION('ref_axis',(0.,0.,1.));
#114911=DIRECTION('center_axis',(-3.56971000961454E-31,1.03207662601796E-45,
-1.));
#114912=DIRECTION('ref_axis',(2.89120579329468E-15,1.,-3.11150763893057E-61));
#114913=DIRECTION('center_axis',(0.,0.,1.));
#114914=DIRECTION('ref_axis',(0.,1.,0.));
#114915=DIRECTION('center_axis',(0.,-1.,0.));
#114916=DIRECTION('ref_axis',(0.,0.,-1.));
#114917=DIRECTION('',(0.,1.,1.23467863058847E-16));
#114918=DIRECTION('',(0.,-1.,-1.23467863058847E-16));
#114919=DIRECTION('center_axis',(0.,1.23467863058847E-16,-1.));
#114920=DIRECTION('ref_axis',(0.,1.,0.));
#114921=DIRECTION('center_axis',(0.,0.,-1.));
#114922=DIRECTION('ref_axis',(0.,1.,0.));
#114923=DIRECTION('center_axis',(0.,-1.,0.));
#114924=DIRECTION('ref_axis',(0.,0.,1.));
#114925=DIRECTION('center_axis',(0.,0.,1.));
#114926=DIRECTION('ref_axis',(0.,1.,0.));
#114927=DIRECTION('center_axis',(-0.998440322660918,-0.0558294016156522,
0.));
#114928=DIRECTION('ref_axis',(0.0558294016156522,-0.998440322660918,0.));
#114929=DIRECTION('center_axis',(-5.87084501074442E-17,1.,0.));
#114930=DIRECTION('ref_axis',(0.,0.,1.));
#114931=DIRECTION('center_axis',(0.,-1.,0.));
#114932=DIRECTION('ref_axis',(0.,0.,1.));
#114933=DIRECTION('',(-5.87084501074442E-17,1.,1.23467863058847E-16));
#114934=DIRECTION('',(5.87084501074442E-17,-1.,-1.23467863058847E-16));
#114935=DIRECTION('center_axis',(0.,1.23467863058847E-16,-1.));
#114936=DIRECTION('ref_axis',(0.,1.,1.38375392967352E-16));
#114937=DIRECTION('center_axis',(-0.995642397459837,-0.0932535059953692,
0.));
#114938=DIRECTION('ref_axis',(0.0932535059953692,-0.995642397459837,0.));
#114939=DIRECTION('center_axis',(8.0739067668352E-31,1.35428930001789E-16,
-1.));
#114940=DIRECTION('ref_axis',(6.75015598972095E-14,1.,1.35428930001789E-16));
#114941=DIRECTION('center_axis',(0.,-1.35726946151947E-16,1.));
#114942=DIRECTION('ref_axis',(0.,1.,1.35726946151947E-16));
#114943=DIRECTION('center_axis',(0.,1.23467863058847E-16,-1.));
#114944=DIRECTION('ref_axis',(0.,1.,0.));
#114945=DIRECTION('center_axis',(-1.,0.,0.));
#114946=DIRECTION('ref_axis',(0.,0.,1.));
#114947=DIRECTION('center_axis',(0.,0.,1.));
#114948=DIRECTION('ref_axis',(0.,1.,0.));
#114949=DIRECTION('center_axis',(0.,0.,-1.));
#114950=DIRECTION('ref_axis',(0.,1.,0.));
#114951=DIRECTION('center_axis',(0.,1.23467863058847E-16,-1.));
#114952=DIRECTION('ref_axis',(0.,1.,0.));
#114953=DIRECTION('center_axis',(0.,-1.,0.));
#114954=DIRECTION('ref_axis',(0.,0.,1.));
#114955=DIRECTION('center_axis',(0.,0.,-1.));
#114956=DIRECTION('ref_axis',(0.,1.,0.));
#114957=DIRECTION('center_axis',(0.,0.,1.));
#114958=DIRECTION('ref_axis',(0.,1.,0.));
#114959=DIRECTION('center_axis',(-1.,0.,-1.17757899099328E-32));
#114960=DIRECTION('ref_axis',(0.,1.,0.));
#114961=DIRECTION('center_axis',(-1.,0.,0.));
#114962=DIRECTION('ref_axis',(0.,0.,1.));
#114963=DIRECTION('',(1.,9.53753439817791E-17,1.17757899099328E-32));
#114964=DIRECTION('',(-1.,-9.53753439817791E-17,-1.17757899099328E-32));
#114965=DIRECTION('center_axis',(-7.82779334765923E-17,-1.,0.));
#114966=DIRECTION('ref_axis',(0.,0.,-1.));
#114967=DIRECTION('center_axis',(0.,-1.,0.));
#114968=DIRECTION('ref_axis',(0.,0.,1.));
#114969=DIRECTION('',(7.82779334765923E-17,1.,1.23467863058847E-16));
#114970=DIRECTION('',(-7.82779334765923E-17,-1.,-1.23467863058847E-16));
#114971=DIRECTION('center_axis',(0.,1.23467863058847E-16,-1.));
#114972=DIRECTION('ref_axis',(0.,1.,0.));
#114973=DIRECTION('center_axis',(0.,0.,-1.));
#114974=DIRECTION('ref_axis',(0.,1.,0.));
#114975=DIRECTION('center_axis',(0.,0.,1.));
#114976=DIRECTION('ref_axis',(0.,1.,0.));
#114977=DIRECTION('center_axis',(0.,1.23467863058847E-16,-1.));
#114978=DIRECTION('ref_axis',(0.,1.,0.));
#114979=DIRECTION('center_axis',(0.,0.,-1.));
#114980=DIRECTION('ref_axis',(0.,1.,0.));
#114981=DIRECTION('center_axis',(0.,-1.,0.));
#114982=DIRECTION('ref_axis',(0.,0.,1.));
#114983=DIRECTION('center_axis',(0.,0.,1.));
#114984=DIRECTION('ref_axis',(0.,1.,0.));
#114985=DIRECTION('center_axis',(-0.999981180102553,-0.00613509907864248,
0.));
#114986=DIRECTION('ref_axis',(0.00613509907864248,-0.999981180102553,0.));
#114987=DIRECTION('center_axis',(-6.11546355285877E-17,1.,0.));
#114988=DIRECTION('ref_axis',(0.,0.,1.));
#114989=DIRECTION('center_axis',(0.,-1.,0.));
#114990=DIRECTION('ref_axis',(0.,0.,1.));
#114991=DIRECTION('',(-6.11546355285877E-17,1.,1.23467863058847E-16));
#114992=DIRECTION('',(6.11546355285877E-17,-1.,-1.23467863058847E-16));
#114993=DIRECTION('center_axis',(0.,1.23467863058847E-16,-1.));
#114994=DIRECTION('ref_axis',(0.,1.,1.38375392967352E-16));
#114995=DIRECTION('center_axis',(-0.999050847451757,-0.0435592034583644,
0.));
#114996=DIRECTION('ref_axis',(0.0435592034583644,-0.999050847451757,0.));
#114997=DIRECTION('center_axis',(-6.37413692118567E-32,1.35428930001789E-16,
-1.));
#114998=DIRECTION('ref_axis',(-5.32907051820075E-15,1.,1.35428930001789E-16));
#114999=DIRECTION('center_axis',(0.,-1.35726946151947E-16,1.));
#115000=DIRECTION('ref_axis',(0.,1.,1.35726946151947E-16));
#115001=DIRECTION('center_axis',(0.,1.23467863058847E-16,-1.));
#115002=DIRECTION('ref_axis',(0.,1.,0.));
#115003=DIRECTION('center_axis',(-1.,0.,0.));
#115004=DIRECTION('ref_axis',(0.,0.,1.));
#115005=DIRECTION('center_axis',(0.,0.,1.));
#115006=DIRECTION('ref_axis',(0.,1.,0.));
#115007=DIRECTION('center_axis',(0.,0.,-1.));
#115008=DIRECTION('ref_axis',(0.,1.,0.));
#115009=DIRECTION('center_axis',(0.,1.23467863058847E-16,-1.));
#115010=DIRECTION('ref_axis',(0.,1.,0.));
#115011=DIRECTION('center_axis',(0.,-1.,0.));
#115012=DIRECTION('ref_axis',(0.,0.,1.));
#115013=DIRECTION('center_axis',(-1.78485500480727E-31,2.58019156504489E-46,
-1.));
#115014=DIRECTION('ref_axis',(1.44560289664734E-15,1.,-3.88938454866321E-62));
#115015=DIRECTION('center_axis',(0.,0.,1.));
#115016=DIRECTION('ref_axis',(0.,1.,0.));
#115017=DIRECTION('center_axis',(-1.,0.,-1.17757899099328E-32));
#115018=DIRECTION('ref_axis',(0.,1.,0.));
#115019=DIRECTION('center_axis',(-1.,0.,0.));
#115020=DIRECTION('ref_axis',(0.,0.,1.));
#115021=DIRECTION('',(1.,9.53753439817791E-17,1.17757899099328E-32));
#115022=DIRECTION('',(-1.,-9.53753439817791E-17,-1.17757899099328E-32));
#115023=DIRECTION('center_axis',(0.,-1.,-1.23467863058847E-16));
#115024=DIRECTION('ref_axis',(-1.,0.,0.));
#115025=DIRECTION('center_axis',(0.,-1.,0.));
#115026=DIRECTION('ref_axis',(0.,0.,1.));
#115027=DIRECTION('',(-3.13111733906369E-16,1.,1.23467863058847E-16));
#115028=DIRECTION('',(3.13111733906369E-16,-1.,-1.23467863058847E-16));
#115029=DIRECTION('center_axis',(0.,1.23467863058847E-16,-1.));
#115030=DIRECTION('ref_axis',(0.,1.,0.));
#115031=DIRECTION('center_axis',(0.,0.,-1.));
#115032=DIRECTION('ref_axis',(0.,1.,0.));
#115033=DIRECTION('center_axis',(0.,0.,1.));
#115034=DIRECTION('ref_axis',(0.,1.,0.));
#115035=DIRECTION('center_axis',(0.,1.23467863058847E-16,-1.));
#115036=DIRECTION('ref_axis',(0.,1.,0.));
#115037=DIRECTION('center_axis',(-1.,-4.81867632215781E-16,0.));
#115038=DIRECTION('ref_axis',(4.81867632215781E-16,-1.,0.));
#115039=DIRECTION('center_axis',(0.,0.,-1.));
#115040=DIRECTION('ref_axis',(0.,1.,0.));
#115041=DIRECTION('center_axis',(0.,-1.,0.));
#115042=DIRECTION('ref_axis',(0.,0.,1.));
#115043=DIRECTION('center_axis',(0.,0.,1.));
#115044=DIRECTION('ref_axis',(0.,1.,0.));
#115045=DIRECTION('center_axis',(-6.11546355285877E-17,1.,0.));
#115046=DIRECTION('ref_axis',(0.,0.,1.));
#115047=DIRECTION('center_axis',(0.,-1.,0.));
#115048=DIRECTION('ref_axis',(0.,0.,1.));
#115049=DIRECTION('',(-6.11546355285877E-17,1.,1.23467863058847E-16));
#115050=DIRECTION('',(6.11546355285877E-17,-1.,-1.23467863058847E-16));
#115051=DIRECTION('center_axis',(1.,0.,5.88789495496639E-32));
#115052=DIRECTION('ref_axis',(0.,-1.,0.));
#115053=DIRECTION('center_axis',(-1.,0.,0.));
#115054=DIRECTION('ref_axis',(0.,0.,1.));
#115055=DIRECTION('',(1.,4.76876719908896E-16,5.88789495496639E-32));
#115056=DIRECTION('',(-1.,-4.76876719908896E-16,-5.88789495496639E-32));
#115057=DIRECTION('center_axis',(0.,1.23467863058847E-16,-1.));
#115058=DIRECTION('ref_axis',(0.,1.,0.));
#115059=DIRECTION('center_axis',(-1.,0.,0.));
#115060=DIRECTION('ref_axis',(0.,0.,1.));
#115061=DIRECTION('center_axis',(0.,0.,1.));
#115062=DIRECTION('ref_axis',(0.,1.,0.));
#115063=DIRECTION('center_axis',(0.,0.,-1.));
#115064=DIRECTION('ref_axis',(0.,1.,0.));
#115065=DIRECTION('center_axis',(0.,1.23467863058847E-16,-1.));
#115066=DIRECTION('ref_axis',(0.,1.,0.));
#115067=DIRECTION('center_axis',(0.,-1.,0.));
#115068=DIRECTION('ref_axis',(0.,0.,1.));
#115069=DIRECTION('center_axis',(0.,0.,-1.));
#115070=DIRECTION('ref_axis',(0.,1.,0.));
#115071=DIRECTION('center_axis',(0.,0.,1.));
#115072=DIRECTION('ref_axis',(0.,1.,0.));
#115073=DIRECTION('center_axis',(-1.,0.,-1.5273745825629E-32));
#115074=DIRECTION('ref_axis',(0.,1.,0.));
#115075=DIRECTION('center_axis',(-1.,0.,0.));
#115076=DIRECTION('ref_axis',(0.,0.,1.));
#115077=DIRECTION('',(1.,1.23706245878324E-16,1.52737458256291E-32));
#115078=DIRECTION('',(-1.,-1.23706245878324E-16,-1.52737458256291E-32));
#115079=DIRECTION('center_axis',(0.,-1.,-1.23467863058847E-16));
#115080=DIRECTION('ref_axis',(-1.,0.,0.));
#115081=DIRECTION('center_axis',(0.,-1.,0.));
#115082=DIRECTION('ref_axis',(0.,0.,1.));
#115083=DIRECTION('',(-3.13111733906369E-16,1.,1.23467863058847E-16));
#115084=DIRECTION('',(3.13111733906369E-16,-1.,-1.23467863058847E-16));
#115085=DIRECTION('center_axis',(0.,1.23467863058847E-16,-1.));
#115086=DIRECTION('ref_axis',(0.,1.,0.));
#115087=DIRECTION('center_axis',(-1.78485500480727E-31,2.58019156504489E-46,
-1.));
#115088=DIRECTION('ref_axis',(1.44560289664734E-15,1.,-3.88938454866321E-62));
#115089=DIRECTION('center_axis',(0.,0.,1.));
#115090=DIRECTION('ref_axis',(0.,1.,0.));
#115091=DIRECTION('center_axis',(0.,1.23467863058847E-16,-1.));
#115092=DIRECTION('ref_axis',(0.,1.,0.));
#115093=DIRECTION('center_axis',(-1.,0.,0.));
#115094=DIRECTION('ref_axis',(0.,0.,1.));
#115095=DIRECTION('center_axis',(0.,0.,-1.));
#115096=DIRECTION('ref_axis',(0.,1.,0.));
#115097=DIRECTION('center_axis',(0.,-1.,0.));
#115098=DIRECTION('ref_axis',(0.,0.,1.));
#115099=DIRECTION('center_axis',(0.,0.,1.));
#115100=DIRECTION('ref_axis',(0.,1.,0.));
#115101=DIRECTION('center_axis',(-6.11546355285877E-17,1.,0.));
#115102=DIRECTION('ref_axis',(0.,0.,1.));
#115103=DIRECTION('center_axis',(0.,-1.,0.));
#115104=DIRECTION('ref_axis',(0.,0.,1.));
#115105=DIRECTION('',(-6.11546355285877E-17,1.,1.23467863058847E-16));
#115106=DIRECTION('',(6.11546355285877E-17,-1.,-1.23467863058847E-16));
#115107=DIRECTION('center_axis',(1.,0.,-1.5273745825629E-32));
#115108=DIRECTION('ref_axis',(0.,-1.,0.));
#115109=DIRECTION('center_axis',(-1.,0.,0.));
#115110=DIRECTION('ref_axis',(0.,0.,1.));
#115111=DIRECTION('',(1.,-1.23706245878324E-16,-1.52737458256291E-32));
#115112=DIRECTION('',(-1.,1.23706245878324E-16,1.52737458256291E-32));
#115113=DIRECTION('center_axis',(0.,1.23467863058847E-16,-1.));
#115114=DIRECTION('ref_axis',(0.,1.,0.));
#115115=DIRECTION('center_axis',(-0.995922166025996,-0.0902166238455439,
0.));
#115116=DIRECTION('ref_axis',(0.0902166238455439,-0.995922166025996,0.));
#115117=DIRECTION('center_axis',(0.,0.,1.));
#115118=DIRECTION('ref_axis',(0.,1.,0.));
#115119=DIRECTION('center_axis',(1.11553437800454E-31,1.00788733009566E-46,
-1.));
#115120=DIRECTION('ref_axis',(-9.03501810404587E-16,1.,1.55575381946529E-61));
#115121=DIRECTION('center_axis',(0.,1.23467863058847E-16,-1.));
#115122=DIRECTION('ref_axis',(0.,1.,0.));
#115123=DIRECTION('center_axis',(0.,-1.,0.));
#115124=DIRECTION('ref_axis',(0.,0.,1.));
#115125=DIRECTION('center_axis',(1.78485500480727E-31,2.58019156504489E-46,
-1.));
#115126=DIRECTION('ref_axis',(-1.44560289664734E-15,1.,-3.88938454866321E-62));
#115127=DIRECTION('center_axis',(0.,0.,1.));
#115128=DIRECTION('ref_axis',(0.,1.,0.));
#115129=DIRECTION('center_axis',(0.,1.23467863058847E-16,-1.));
#115130=DIRECTION('ref_axis',(0.,1.,0.));
#115131=DIRECTION('center_axis',(-0.913440670994017,-0.406971916198157,
-3.63370493544251E-16));
#115132=DIRECTION('ref_axis',(0.406971916198157,-0.913440670994017,6.94755181634254E-32));
#115133=DIRECTION('center_axis',(-5.48307457476793E-31,2.43497425545765E-45,
-1.));
#115134=DIRECTION('ref_axis',(4.44089209850063E-15,1.,-3.42265840282363E-60));
#115135=DIRECTION('center_axis',(0.,0.,1.));
#115136=DIRECTION('ref_axis',(0.,1.,0.));
#115137=DIRECTION('center_axis',(0.,-1.,-1.23467863058847E-16));
#115138=DIRECTION('ref_axis',(-1.,0.,0.));
#115139=DIRECTION('center_axis',(3.61400724161834E-16,-1.,-1.20466908053943E-16));
#115140=DIRECTION('ref_axis',(1.,3.61400724161834E-16,-2.73691106313441E-47));
#115141=DIRECTION('',(-3.13111733906369E-16,1.,1.23467863058847E-16));
#115142=DIRECTION('',(3.13111733906369E-16,-1.,-1.23467863058847E-16));
#115143=DIRECTION('center_axis',(0.,1.23467863058847E-16,-1.));
#115144=DIRECTION('ref_axis',(0.,1.,0.));
#115145=DIRECTION('center_axis',(-0.99836765577839,-0.0571141304368959,
4.12821761995348E-17));
#115146=DIRECTION('ref_axis',(0.0571141304368959,-0.99836765577839,1.08996476499831E-33));
#115147=DIRECTION('center_axis',(0.,0.,1.));
#115148=DIRECTION('ref_axis',(0.,1.,0.));
#115149=DIRECTION('center_axis',(0.,0.,-1.));
#115150=DIRECTION('ref_axis',(0.,1.,0.));
#115151=DIRECTION('center_axis',(0.,1.23467863058847E-16,-1.));
#115152=DIRECTION('ref_axis',(-0.686617021913638,-0.727019301819729,0.));
#115153=DIRECTION('center_axis',(0.,0.,1.));
#115154=DIRECTION('ref_axis',(0.,1.,0.));
#115155=DIRECTION('center_axis',(-1.78485500480727E-31,2.58019156504489E-46,
-1.));
#115156=DIRECTION('ref_axis',(1.44560289664734E-15,1.,0.));
#115157=DIRECTION('center_axis',(0.,1.23467863058847E-16,-1.));
#115158=DIRECTION('ref_axis',(0.,1.,0.));
#115159=DIRECTION('center_axis',(-1.,0.,0.));
#115160=DIRECTION('ref_axis',(0.,0.,1.));
#115161=DIRECTION('center_axis',(0.,0.,-1.));
#115162=DIRECTION('ref_axis',(0.,1.,0.));
#115163=DIRECTION('center_axis',(0.,-1.,0.));
#115164=DIRECTION('ref_axis',(0.,0.,1.));
#115165=DIRECTION('center_axis',(0.,0.,1.));
#115166=DIRECTION('ref_axis',(0.,1.,0.));
#115167=DIRECTION('center_axis',(-5.87084501074442E-17,1.,0.));
#115168=DIRECTION('ref_axis',(0.,0.,1.));
#115169=DIRECTION('center_axis',(4.81867632215779E-16,-1.,-1.20466908053945E-16));
#115170=DIRECTION('ref_axis',(1.,4.81867632215779E-16,1.09476442525376E-47));
#115171=DIRECTION('',(-5.87084501074442E-17,1.,1.23467863058847E-16));
#115172=DIRECTION('',(5.87084501074442E-17,-1.,-1.23467863058847E-16));
#115173=DIRECTION('center_axis',(1.,0.,-1.5273745825629E-32));
#115174=DIRECTION('ref_axis',(0.,-1.,0.));
#115175=DIRECTION('center_axis',(-1.,0.,0.));
#115176=DIRECTION('ref_axis',(0.,0.,1.));
#115177=DIRECTION('',(1.,-1.23706245878324E-16,-1.52737458256291E-32));
#115178=DIRECTION('',(-1.,1.23706245878324E-16,1.52737458256291E-32));
#115179=DIRECTION('center_axis',(0.,1.23467863058847E-16,-1.));
#115180=DIRECTION('ref_axis',(0.,1.,0.));
#115181=DIRECTION('center_axis',(-1.,0.,0.));
#115182=DIRECTION('ref_axis',(0.,0.,1.));
#115183=DIRECTION('center_axis',(0.,0.,1.));
#115184=DIRECTION('ref_axis',(0.,1.,0.));
#115185=DIRECTION('center_axis',(0.,0.,-1.));
#115186=DIRECTION('ref_axis',(0.,1.,0.));
#115187=DIRECTION('center_axis',(0.,1.23467863058847E-16,-1.));
#115188=DIRECTION('ref_axis',(0.,1.,0.));
#115189=DIRECTION('center_axis',(0.,-1.,0.));
#115190=DIRECTION('ref_axis',(0.,0.,1.));
#115191=DIRECTION('center_axis',(3.56971000961454E-31,1.03207662601796E-45,
-1.));
#115192=DIRECTION('ref_axis',(-2.89120579329468E-15,1.,-3.11150763893057E-61));
#115193=DIRECTION('center_axis',(0.,0.,1.));
#115194=DIRECTION('ref_axis',(0.,1.,0.));
#115195=DIRECTION('center_axis',(-1.,0.,4.58212374768871E-32));
#115196=DIRECTION('ref_axis',(0.,1.,0.));
#115197=DIRECTION('center_axis',(-1.,0.,0.));
#115198=DIRECTION('ref_axis',(0.,0.,1.));
#115199=DIRECTION('',(1.,-3.71118737634973E-16,-4.58212374768871E-32));
#115200=DIRECTION('',(-1.,3.71118737634973E-16,4.58212374768871E-32));
#115201=DIRECTION('center_axis',(-7.82779334765923E-17,-1.,0.));
#115202=DIRECTION('ref_axis',(0.,0.,-1.));
#115203=DIRECTION('center_axis',(-1.20466908053945E-16,-1.,-1.20466908053943E-16));
#115204=DIRECTION('ref_axis',(1.,-1.20466908053945E-16,2.73691106313441E-48));
#115205=DIRECTION('',(7.82779334765923E-17,1.,1.23467863058847E-16));
#115206=DIRECTION('',(-7.82779334765923E-17,-1.,-1.23467863058847E-16));
#115207=DIRECTION('center_axis',(0.,1.23467863058847E-16,-1.));
#115208=DIRECTION('ref_axis',(0.,1.,0.));
#115209=DIRECTION('center_axis',(0.,0.,-1.));
#115210=DIRECTION('ref_axis',(0.,1.,0.));
#115211=DIRECTION('center_axis',(0.,0.,1.));
#115212=DIRECTION('ref_axis',(0.,1.,0.));
#115213=DIRECTION('center_axis',(0.,1.23467863058847E-16,-1.));
#115214=DIRECTION('ref_axis',(0.,1.,0.));
#115215=DIRECTION('center_axis',(-1.,0.,0.));
#115216=DIRECTION('ref_axis',(0.,0.,1.));
#115217=DIRECTION('center_axis',(0.,0.,-1.));
#115218=DIRECTION('ref_axis',(0.,1.,0.));
#115219=DIRECTION('center_axis',(0.,-1.,0.));
#115220=DIRECTION('ref_axis',(0.,0.,1.));
#115221=DIRECTION('center_axis',(0.,0.,1.));
#115222=DIRECTION('ref_axis',(0.,1.,0.));
#115223=DIRECTION('center_axis',(-5.87084501074442E-17,1.,0.));
#115224=DIRECTION('ref_axis',(0.,0.,1.));
#115225=DIRECTION('center_axis',(0.,-1.,0.));
#115226=DIRECTION('ref_axis',(0.,0.,1.));
#115227=DIRECTION('',(-5.87084501074442E-17,1.,1.23467863058847E-16));
#115228=DIRECTION('',(5.87084501074442E-17,-1.,-1.23467863058847E-16));
#115229=DIRECTION('center_axis',(1.,0.,5.88789495496639E-32));
#115230=DIRECTION('ref_axis',(0.,-1.,0.));
#115231=DIRECTION('center_axis',(-1.,0.,0.));
#115232=DIRECTION('ref_axis',(0.,0.,1.));
#115233=DIRECTION('',(1.,4.76876719908896E-16,5.88789495496639E-32));
#115234=DIRECTION('',(-1.,-4.76876719908896E-16,-5.88789495496639E-32));
#115235=DIRECTION('center_axis',(0.,1.23467863058847E-16,-1.));
#115236=DIRECTION('ref_axis',(0.,1.,0.));
#115237=DIRECTION('center_axis',(-1.,0.,0.));
#115238=DIRECTION('ref_axis',(0.,0.,1.));
#115239=DIRECTION('center_axis',(0.,0.,1.));
#115240=DIRECTION('ref_axis',(0.,1.,0.));
#115241=DIRECTION('center_axis',(1.78485500480727E-31,2.58019156504489E-46,
-1.));
#115242=DIRECTION('ref_axis',(-1.44560289664734E-15,1.,-3.88938454866321E-62));
#115243=DIRECTION('center_axis',(0.,1.23467863058847E-16,-1.));
#115244=DIRECTION('ref_axis',(0.,1.,0.));
#115245=DIRECTION('center_axis',(0.,-1.,0.));
#115246=DIRECTION('ref_axis',(0.,0.,1.));
#115247=DIRECTION('center_axis',(0.,0.,-1.));
#115248=DIRECTION('ref_axis',(0.,1.,0.));
#115249=DIRECTION('center_axis',(0.,0.,1.));
#115250=DIRECTION('ref_axis',(0.,1.,0.));
#115251=DIRECTION('center_axis',(-1.,0.,-1.5273745825629E-32));
#115252=DIRECTION('ref_axis',(0.,1.,0.));
#115253=DIRECTION('center_axis',(-1.,0.,0.));
#115254=DIRECTION('ref_axis',(0.,0.,1.));
#115255=DIRECTION('',(1.,1.23706245878324E-16,1.52737458256291E-32));
#115256=DIRECTION('',(-1.,-1.23706245878324E-16,-1.52737458256291E-32));
#115257=DIRECTION('center_axis',(-7.82779334765923E-17,-1.,0.));
#115258=DIRECTION('ref_axis',(0.,0.,-1.));
#115259=DIRECTION('center_axis',(0.,-1.,0.));
#115260=DIRECTION('ref_axis',(0.,0.,1.));
#115261=DIRECTION('',(7.82779334765923E-17,1.,1.23467863058847E-16));
#115262=DIRECTION('',(-7.82779334765923E-17,-1.,-1.23467863058847E-16));
#115263=DIRECTION('center_axis',(0.,1.23467863058847E-16,-1.));
#115264=DIRECTION('ref_axis',(0.,1.,0.));
#115265=DIRECTION('center_axis',(0.,0.,-1.));
#115266=DIRECTION('ref_axis',(0.,1.,0.));
#115267=DIRECTION('center_axis',(0.,0.,1.));
#115268=DIRECTION('ref_axis',(0.,1.,0.));
#115269=DIRECTION('center_axis',(0.,1.23467863058847E-16,-1.));
#115270=DIRECTION('ref_axis',(0.,1.,0.));
#115271=DIRECTION('center_axis',(-1.,0.,0.));
#115272=DIRECTION('ref_axis',(0.,0.,1.));
#115273=DIRECTION('center_axis',(0.,0.,-1.));
#115274=DIRECTION('ref_axis',(0.,1.,0.));
#115275=DIRECTION('center_axis',(0.,-1.,0.));
#115276=DIRECTION('ref_axis',(0.,0.,1.));
#115277=DIRECTION('center_axis',(0.,0.,1.));
#115278=DIRECTION('ref_axis',(0.,1.,0.));
#115279=DIRECTION('center_axis',(-7.82779334765923E-17,1.,0.));
#115280=DIRECTION('ref_axis',(0.,0.,1.));
#115281=DIRECTION('center_axis',(0.,-1.,0.));
#115282=DIRECTION('ref_axis',(0.,0.,1.));
#115283=DIRECTION('',(-7.82779334765923E-17,1.,1.23467863058847E-16));
#115284=DIRECTION('',(7.82779334765923E-17,-1.,-1.23467863058847E-16));
#115285=DIRECTION('center_axis',(1.,0.,5.88789495496639E-32));
#115286=DIRECTION('ref_axis',(0.,-1.,0.));
#115287=DIRECTION('center_axis',(-1.,0.,0.));
#115288=DIRECTION('ref_axis',(0.,0.,1.));
#115289=DIRECTION('',(1.,4.76876719908896E-16,5.88789495496639E-32));
#115290=DIRECTION('',(-1.,-4.76876719908896E-16,-5.88789495496639E-32));
#115291=DIRECTION('center_axis',(0.,1.23467863058847E-16,-1.));
#115292=DIRECTION('ref_axis',(0.,1.,0.));
#115293=DIRECTION('center_axis',(-1.,0.,0.));
#115294=DIRECTION('ref_axis',(0.,0.,1.));
#115295=DIRECTION('center_axis',(0.,0.,1.));
#115296=DIRECTION('ref_axis',(0.,1.,0.));
#115297=DIRECTION('center_axis',(0.,0.,-1.));
#115298=DIRECTION('ref_axis',(0.,1.,0.));
#115299=DIRECTION('center_axis',(0.,1.23467863058847E-16,-1.));
#115300=DIRECTION('ref_axis',(0.,1.,0.));
#115301=DIRECTION('center_axis',(0.,-1.,0.));
#115302=DIRECTION('ref_axis',(0.,0.,1.));
#115303=DIRECTION('center_axis',(0.,0.,-1.));
#115304=DIRECTION('ref_axis',(0.,1.,0.));
#115305=DIRECTION('center_axis',(0.,0.,1.));
#115306=DIRECTION('ref_axis',(0.,1.,0.));
#115307=DIRECTION('center_axis',(-1.,0.,-1.5273745825629E-32));
#115308=DIRECTION('ref_axis',(0.,1.,0.));
#115309=DIRECTION('center_axis',(-1.,0.,0.));
#115310=DIRECTION('ref_axis',(0.,0.,1.));
#115311=DIRECTION('',(1.,1.23706245878324E-16,1.52737458256291E-32));
#115312=DIRECTION('',(-1.,-1.23706245878324E-16,-1.52737458256291E-32));
#115313=DIRECTION('center_axis',(0.,-1.,0.));
#115314=DIRECTION('ref_axis',(0.,0.,-1.));
#115315=DIRECTION('center_axis',(0.,-1.,0.));
#115316=DIRECTION('ref_axis',(0.,0.,1.));
#115317=DIRECTION('',(0.,1.,1.23467863058847E-16));
#115318=DIRECTION('',(0.,-1.,-1.23467863058847E-16));
#115319=DIRECTION('center_axis',(0.,1.23467863058847E-16,-1.));
#115320=DIRECTION('ref_axis',(0.,1.,0.));
#115321=DIRECTION('center_axis',(0.,0.,-1.));
#115322=DIRECTION('ref_axis',(0.,1.,0.));
#115323=DIRECTION('center_axis',(0.,0.,1.));
#115324=DIRECTION('ref_axis',(0.,1.,0.));
#115325=DIRECTION('center_axis',(0.,1.23467863058847E-16,-1.));
#115326=DIRECTION('ref_axis',(0.,1.,0.));
#115327=DIRECTION('center_axis',(-1.,0.,0.));
#115328=DIRECTION('ref_axis',(0.,0.,1.));
#115329=DIRECTION('center_axis',(0.,0.,-1.));
#115330=DIRECTION('ref_axis',(0.,1.,0.));
#115331=DIRECTION('center_axis',(0.,-1.,0.));
#115332=DIRECTION('ref_axis',(0.,0.,1.));
#115333=DIRECTION('center_axis',(0.,0.,1.));
#115334=DIRECTION('ref_axis',(0.,1.,0.));
#115335=DIRECTION('center_axis',(-7.82779334765923E-17,1.,0.));
#115336=DIRECTION('ref_axis',(0.,0.,1.));
#115337=DIRECTION('center_axis',(-4.57774250604992E-15,-1.,-1.20466908053943E-16));
#115338=DIRECTION('ref_axis',(1.,-4.57774250604992E-15,-3.50324616081204E-46));
#115339=DIRECTION('',(-7.82779334765923E-17,1.,1.23467863058847E-16));
#115340=DIRECTION('',(7.82779334765923E-17,-1.,-1.23467863058847E-16));
#115341=DIRECTION('center_axis',(1.,0.,-1.5273745825629E-32));
#115342=DIRECTION('ref_axis',(0.,-1.,0.));
#115343=DIRECTION('center_axis',(-1.,0.,0.));
#115344=DIRECTION('ref_axis',(0.,0.,1.));
#115345=DIRECTION('',(1.,-1.23706245878324E-16,-1.52737458256291E-32));
#115346=DIRECTION('',(-1.,1.23706245878324E-16,1.52737458256291E-32));
#115347=DIRECTION('center_axis',(0.,1.23467863058847E-16,-1.));
#115348=DIRECTION('ref_axis',(0.,1.,0.));
#115349=DIRECTION('center_axis',(-1.,0.,0.));
#115350=DIRECTION('ref_axis',(0.,0.,1.));
#115351=DIRECTION('center_axis',(0.,0.,1.));
#115352=DIRECTION('ref_axis',(0.,1.,0.));
#115353=DIRECTION('center_axis',(0.,0.,-1.));
#115354=DIRECTION('ref_axis',(0.,1.,0.));
#115355=DIRECTION('center_axis',(0.,1.23467863058847E-16,-1.));
#115356=DIRECTION('ref_axis',(0.,1.,0.));
#115357=DIRECTION('center_axis',(0.,-1.,0.));
#115358=DIRECTION('ref_axis',(0.,0.,1.));
#115359=DIRECTION('center_axis',(0.,0.,-1.));
#115360=DIRECTION('ref_axis',(0.,1.,0.));
#115361=DIRECTION('center_axis',(0.,0.,1.));
#115362=DIRECTION('ref_axis',(0.,1.,0.));
#115363=DIRECTION('center_axis',(-1.,0.,4.58212374768871E-32));
#115364=DIRECTION('ref_axis',(0.,1.,0.));
#115365=DIRECTION('center_axis',(-1.,0.,0.));
#115366=DIRECTION('ref_axis',(0.,0.,1.));
#115367=DIRECTION('',(1.,-3.71118737634973E-16,-4.58212374768871E-32));
#115368=DIRECTION('',(-1.,3.71118737634973E-16,4.58212374768871E-32));
#115369=DIRECTION('center_axis',(0.,-1.,0.));
#115370=DIRECTION('ref_axis',(0.,0.,-1.));
#115371=DIRECTION('center_axis',(0.,-1.,-1.20466908053943E-16));
#115372=DIRECTION('ref_axis',(0.,-1.20466908053943E-16,1.));
#115373=DIRECTION('',(0.,1.,1.23467863058847E-16));
#115374=DIRECTION('',(0.,-1.,-1.23467863058847E-16));
#115375=DIRECTION('center_axis',(0.,1.23467863058847E-16,-1.));
#115376=DIRECTION('ref_axis',(0.,1.,0.));
#115377=DIRECTION('center_axis',(0.,0.,-1.));
#115378=DIRECTION('ref_axis',(0.,1.,0.));
#115379=DIRECTION('center_axis',(0.,0.,1.));
#115380=DIRECTION('ref_axis',(0.,1.,0.));
#115381=DIRECTION('center_axis',(0.,1.23467863058847E-16,-1.));
#115382=DIRECTION('ref_axis',(0.,1.,0.));
#115383=DIRECTION('center_axis',(-1.,0.,0.));
#115384=DIRECTION('ref_axis',(0.,0.,1.));
#115385=DIRECTION('center_axis',(0.,0.,-1.));
#115386=DIRECTION('ref_axis',(0.,1.,0.));
#115387=DIRECTION('center_axis',(0.,-1.,0.));
#115388=DIRECTION('ref_axis',(0.,0.,1.));
#115389=DIRECTION('center_axis',(0.,0.,1.));
#115390=DIRECTION('ref_axis',(0.,1.,0.));
#115391=DIRECTION('center_axis',(0.,1.,0.));
#115392=DIRECTION('ref_axis',(0.,0.,1.));
#115393=DIRECTION('center_axis',(-3.61400724161836E-16,-1.,-1.20466908053943E-16));
#115394=DIRECTION('ref_axis',(1.,-3.61400724161836E-16,1.09476442525376E-47));
#115395=DIRECTION('',(0.,1.,1.23467863058847E-16));
#115396=DIRECTION('',(0.,-1.,-1.23467863058847E-16));
#115397=DIRECTION('center_axis',(1.,0.,-1.5273745825629E-32));
#115398=DIRECTION('ref_axis',(0.,-1.,0.));
#115399=DIRECTION('center_axis',(-1.,0.,0.));
#115400=DIRECTION('ref_axis',(0.,0.,1.));
#115401=DIRECTION('',(1.,-1.23706245878324E-16,-1.52737458256291E-32));
#115402=DIRECTION('',(-1.,1.23706245878324E-16,1.52737458256291E-32));
#115403=DIRECTION('center_axis',(0.,1.23467863058847E-16,-1.));
#115404=DIRECTION('ref_axis',(0.,1.,0.));
#115405=DIRECTION('center_axis',(-1.,0.,0.));
#115406=DIRECTION('ref_axis',(0.,0.,1.));
#115407=DIRECTION('center_axis',(0.,0.,1.));
#115408=DIRECTION('ref_axis',(0.,1.,0.));
#115409=DIRECTION('center_axis',(0.,0.,-1.));
#115410=DIRECTION('ref_axis',(0.,1.,0.));
#115411=DIRECTION('center_axis',(0.,1.23467863058847E-16,-1.));
#115412=DIRECTION('ref_axis',(0.,1.,0.));
#115413=DIRECTION('center_axis',(-0.0294983404866172,-0.999564829267485,
0.));
#115414=DIRECTION('ref_axis',(0.999564829267485,-0.0294983404866172,0.));
#115415=DIRECTION('center_axis',(0.,0.,-1.));
#115416=DIRECTION('ref_axis',(0.,1.,0.));
#115417=DIRECTION('center_axis',(0.,0.,1.));
#115418=DIRECTION('ref_axis',(0.,1.,0.));
#115419=DIRECTION('center_axis',(-1.,0.,4.58212374768871E-32));
#115420=DIRECTION('ref_axis',(0.,1.,0.));
#115421=DIRECTION('center_axis',(-1.,0.,0.));
#115422=DIRECTION('ref_axis',(0.,0.,1.));
#115423=DIRECTION('',(1.,-3.71118737634973E-16,-4.58212374768871E-32));
#115424=DIRECTION('',(-1.,3.71118737634973E-16,4.58212374768871E-32));
#115425=DIRECTION('center_axis',(0.,1.23467863058847E-16,-1.));
#115426=DIRECTION('ref_axis',(0.,1.,1.25697703075927E-16));
#115427=DIRECTION('center_axis',(-0.0175200318846342,-0.999846512462169,
-1.20448417884836E-16));
#115428=DIRECTION('ref_axis',(0.999846512462169,-0.0175200318846342,1.51017636338582E-32));
#115429=DIRECTION('center_axis',(1.11644282221188E-31,1.22833149346405E-16,
-1.));
#115430=DIRECTION('ref_axis',(-1.75897069864052E-13,1.,1.22833149346405E-16));
#115431=DIRECTION('center_axis',(0.,-1.22914743790472E-16,1.));
#115432=DIRECTION('ref_axis',(0.,1.,1.22914743790472E-16));
#115433=DIRECTION('center_axis',(0.,1.23467863058847E-16,-1.));
#115434=DIRECTION('ref_axis',(0.,1.,0.));
#115435=DIRECTION('center_axis',(0.,0.,-1.));
#115436=DIRECTION('ref_axis',(0.,1.,0.));
#115437=DIRECTION('center_axis',(0.,0.,1.));
#115438=DIRECTION('ref_axis',(0.,1.,0.));
#115439=DIRECTION('center_axis',(0.,1.23467863058847E-16,-1.));
#115440=DIRECTION('ref_axis',(0.,1.,0.));
#115441=DIRECTION('center_axis',(-1.,0.,0.));
#115442=DIRECTION('ref_axis',(0.,0.,1.));
#115443=DIRECTION('center_axis',(0.,0.,-1.));
#115444=DIRECTION('ref_axis',(0.,1.,0.));
#115445=DIRECTION('center_axis',(0.,-1.,0.));
#115446=DIRECTION('ref_axis',(0.,0.,1.));
#115447=DIRECTION('center_axis',(0.,0.,1.));
#115448=DIRECTION('ref_axis',(0.,1.,0.));
#115449=DIRECTION('center_axis',(0.,1.,0.));
#115450=DIRECTION('ref_axis',(0.,0.,1.));
#115451=DIRECTION('center_axis',(0.,-1.,0.));
#115452=DIRECTION('ref_axis',(0.,0.,1.));
#115453=DIRECTION('',(0.,1.,1.23467863058847E-16));
#115454=DIRECTION('',(0.,-1.,-1.23467863058847E-16));
#115455=DIRECTION('center_axis',(1.,0.,5.88789495496639E-32));
#115456=DIRECTION('ref_axis',(0.,-1.,0.));
#115457=DIRECTION('center_axis',(-1.,0.,0.));
#115458=DIRECTION('ref_axis',(0.,0.,1.));
#115459=DIRECTION('',(1.,4.76876719908896E-16,5.88789495496639E-32));
#115460=DIRECTION('',(-1.,-4.76876719908896E-16,-5.88789495496639E-32));
#115461=DIRECTION('center_axis',(0.,1.23467863058847E-16,-1.));
#115462=DIRECTION('ref_axis',(0.,1.,0.));
#115463=DIRECTION('center_axis',(-1.,0.,0.));
#115464=DIRECTION('ref_axis',(0.,0.,1.));
#115465=DIRECTION('center_axis',(0.,0.,1.));
#115466=DIRECTION('ref_axis',(0.,1.,0.));
#115467=DIRECTION('center_axis',(0.,0.,-1.));
#115468=DIRECTION('ref_axis',(0.,1.,0.));
#115469=DIRECTION('center_axis',(0.,1.23467863058847E-16,-1.));
#115470=DIRECTION('ref_axis',(0.,1.,0.));
#115471=DIRECTION('center_axis',(-0.646912564190485,-0.762564183719962,
0.));
#115472=DIRECTION('ref_axis',(0.762564183719962,-0.646912564190485,0.));
#115473=DIRECTION('center_axis',(0.,0.,-1.));
#115474=DIRECTION('ref_axis',(0.,1.,0.));
#115475=DIRECTION('center_axis',(0.,0.,1.));
#115476=DIRECTION('ref_axis',(0.,1.,0.));
#115477=DIRECTION('center_axis',(-1.,0.,-1.5273745825629E-32));
#115478=DIRECTION('ref_axis',(0.,1.,0.));
#115479=DIRECTION('center_axis',(-1.,0.,0.));
#115480=DIRECTION('ref_axis',(0.,0.,1.));
#115481=DIRECTION('',(1.,1.23706245878324E-16,1.52737458256291E-32));
#115482=DIRECTION('',(-1.,-1.23706245878324E-16,-1.52737458256291E-32));
#115483=DIRECTION('center_axis',(0.,1.23467863058847E-16,-1.));
#115484=DIRECTION('ref_axis',(0.,1.,0.));
#115485=DIRECTION('center_axis',(-0.55837318130784,-0.829589892896582,0.));
#115486=DIRECTION('ref_axis',(0.829589892896582,-0.55837318130784,0.));
#115487=DIRECTION('center_axis',(-6.57968948972152E-31,3.50636292785903E-45,
-1.));
#115488=DIRECTION('ref_axis',(5.32907051820075E-15,1.,0.));
#115489=DIRECTION('center_axis',(0.,0.,1.));
#115490=DIRECTION('ref_axis',(0.,1.,0.));
#115491=DIRECTION('center_axis',(0.,1.23467863058847E-16,-1.));
#115492=DIRECTION('ref_axis',(0.,1.,0.));
#115493=DIRECTION('center_axis',(0.0331928226750539,0.999448966442441,0.));
#115494=DIRECTION('ref_axis',(-0.99944896644244,0.0331928226750539,0.));
#115495=DIRECTION('center_axis',(0.,0.,1.));
#115496=DIRECTION('ref_axis',(0.,1.,0.));
#115497=DIRECTION('center_axis',(0.,0.,-1.));
#115498=DIRECTION('ref_axis',(0.,1.,0.));
#115499=DIRECTION('center_axis',(0.,1.23467863058847E-16,-1.));
#115500=DIRECTION('ref_axis',(0.,1.,0.));
#115501=DIRECTION('center_axis',(-0.03879684915621,-0.999247118832749,0.));
#115502=DIRECTION('ref_axis',(0.999247118832749,-0.03879684915621,0.));
#115503=DIRECTION('center_axis',(-1.18169710663102E-30,1.13098908268507E-44,
-1.));
#115504=DIRECTION('ref_axis',(9.57088814332033E-15,1.,-2.7381267222589E-59));
#115505=DIRECTION('center_axis',(0.,0.,1.));
#115506=DIRECTION('ref_axis',(0.,1.,0.));
#115507=DIRECTION('center_axis',(0.,1.23467863058847E-16,-1.));
#115508=DIRECTION('ref_axis',(0.,1.,1.25697703075927E-16));
#115509=DIRECTION('center_axis',(1.18920911416235E-31,1.22833149346405E-16,
-1.));
#115510=DIRECTION('ref_axis',(-1.87361497136383E-13,1.,1.22833149346405E-16));
#115511=DIRECTION('center_axis',(0.,-1.22914743790472E-16,1.));
#115512=DIRECTION('ref_axis',(0.,1.,1.22914743790472E-16));
#115513=DIRECTION('center_axis',(0.,1.23467863058847E-16,-1.));
#115514=DIRECTION('ref_axis',(0.,1.,0.));
#115515=DIRECTION('center_axis',(-1.,0.,0.));
#115516=DIRECTION('ref_axis',(0.,0.,1.));
#115517=DIRECTION('center_axis',(0.,0.,-1.));
#115518=DIRECTION('ref_axis',(0.,1.,0.));
#115519=DIRECTION('center_axis',(0.,-1.,-9.63735264431547E-16));
#115520=DIRECTION('ref_axis',(0.,-9.63735264431547E-16,1.));
#115521=DIRECTION('center_axis',(0.,0.,1.));
#115522=DIRECTION('ref_axis',(0.,1.,0.));
#115523=DIRECTION('center_axis',(0.,1.,0.));
#115524=DIRECTION('ref_axis',(0.,0.,1.));
#115525=DIRECTION('center_axis',(-3.85494105772624E-15,-1.,0.));
#115526=DIRECTION('ref_axis',(1.,-3.85494105772625E-15,0.));
#115527=DIRECTION('',(0.,1.,1.23467863058847E-16));
#115528=DIRECTION('',(0.,-1.,-1.23467863058847E-16));
#115529=DIRECTION('center_axis',(1.,0.,4.58212374768871E-32));
#115530=DIRECTION('ref_axis',(0.,-1.,0.));
#115531=DIRECTION('center_axis',(-1.,0.,0.));
#115532=DIRECTION('ref_axis',(0.,0.,1.));
#115533=DIRECTION('',(1.,3.71118737634973E-16,4.58212374768871E-32));
#115534=DIRECTION('',(-1.,-3.71118737634973E-16,-4.58212374768871E-32));
#115535=DIRECTION('center_axis',(0.,1.23467863058847E-16,-1.));
#115536=DIRECTION('ref_axis',(0.,1.,0.));
#115537=DIRECTION('center_axis',(-1.,0.,0.));
#115538=DIRECTION('ref_axis',(0.,0.,1.));
#115539=DIRECTION('center_axis',(0.,0.,1.));
#115540=DIRECTION('ref_axis',(0.,1.,0.));
#115541=DIRECTION('center_axis',(0.,0.,-1.));
#115542=DIRECTION('ref_axis',(0.,1.,0.));
#115543=DIRECTION('center_axis',(0.,1.23467863058847E-16,-1.));
#115544=DIRECTION('ref_axis',(0.,1.,0.));
#115545=DIRECTION('center_axis',(-0.0138255496962061,-0.999904422520272,
0.));
#115546=DIRECTION('ref_axis',(0.999904422520272,-0.0138255496962061,0.));
#115547=DIRECTION('center_axis',(0.,0.,-1.));
#115548=DIRECTION('ref_axis',(0.,1.,0.));
#115549=DIRECTION('center_axis',(0.,0.,1.));
#115550=DIRECTION('ref_axis',(0.,1.,0.));
#115551=DIRECTION('center_axis',(-1.,0.,4.58212374768871E-32));
#115552=DIRECTION('ref_axis',(0.,1.,0.));
#115553=DIRECTION('center_axis',(-1.,0.,0.));
#115554=DIRECTION('ref_axis',(0.,0.,1.));
#115555=DIRECTION('',(1.,-3.71118737634973E-16,-4.58212374768871E-32));
#115556=DIRECTION('',(-1.,3.71118737634973E-16,4.58212374768871E-32));
#115557=DIRECTION('center_axis',(0.,1.23467863058847E-16,-1.));
#115558=DIRECTION('ref_axis',(0.,1.,1.25697703075927E-16));
#115559=DIRECTION('center_axis',(-0.00184724109421639,-0.999998293848714,
0.));
#115560=DIRECTION('ref_axis',(0.999998293848714,-0.00184724109421639,0.));
#115561=DIRECTION('center_axis',(5.51984300367294E-32,1.22833149346405E-16,
-1.));
#115562=DIRECTION('ref_axis',(-8.69658697372547E-14,1.,1.22833149346405E-16));
#115563=DIRECTION('center_axis',(0.,-1.22914743790472E-16,1.));
#115564=DIRECTION('ref_axis',(0.,1.,1.22914743790472E-16));
#115565=DIRECTION('center_axis',(0.,1.23467863058847E-16,-1.));
#115566=DIRECTION('ref_axis',(0.,1.,0.));
#115567=DIRECTION('center_axis',(0.,0.,-1.));
#115568=DIRECTION('ref_axis',(0.,1.,0.));
#115569=DIRECTION('center_axis',(0.,0.,1.));
#115570=DIRECTION('ref_axis',(0.,1.,0.));
#115571=DIRECTION('center_axis',(0.,1.23467863058847E-16,-1.));
#115572=DIRECTION('ref_axis',(0.,1.,0.));
#115573=DIRECTION('center_axis',(-1.,0.,0.));
#115574=DIRECTION('ref_axis',(0.,0.,1.));
#115575=DIRECTION('center_axis',(0.,0.,-1.));
#115576=DIRECTION('ref_axis',(0.,1.,0.));
#115577=DIRECTION('center_axis',(0.,-1.,-9.63735264431547E-16));
#115578=DIRECTION('ref_axis',(0.,-9.63735264431547E-16,1.));
#115579=DIRECTION('center_axis',(0.,0.,1.));
#115580=DIRECTION('ref_axis',(0.,1.,0.));
#115581=DIRECTION('center_axis',(-7.82779334765923E-17,1.,0.));
#115582=DIRECTION('ref_axis',(0.,0.,1.));
#115583=DIRECTION('center_axis',(-3.85494105772624E-15,-1.,0.));
#115584=DIRECTION('ref_axis',(1.,-3.85494105772625E-15,0.));
#115585=DIRECTION('',(-7.82779334765923E-17,1.,1.23467863058847E-16));
#115586=DIRECTION('',(7.82779334765923E-17,-1.,-1.23467863058847E-16));
#115587=DIRECTION('center_axis',(1.,0.,4.58212374768871E-32));
#115588=DIRECTION('ref_axis',(0.,-1.,0.));
#115589=DIRECTION('center_axis',(-1.,0.,0.));
#115590=DIRECTION('ref_axis',(0.,0.,1.));
#115591=DIRECTION('',(1.,3.71118737634973E-16,4.58212374768871E-32));
#115592=DIRECTION('',(-1.,-3.71118737634973E-16,-4.58212374768871E-32));
#115593=DIRECTION('center_axis',(0.,1.23467863058847E-16,-1.));
#115594=DIRECTION('ref_axis',(0.,1.,0.));
#115595=DIRECTION('center_axis',(-1.,0.,0.));
#115596=DIRECTION('ref_axis',(0.,0.,1.));
#115597=DIRECTION('center_axis',(0.,0.,1.));
#115598=DIRECTION('ref_axis',(0.,1.,0.));
#115599=DIRECTION('center_axis',(0.,0.,-1.));
#115600=DIRECTION('ref_axis',(0.,1.,0.));
#115601=DIRECTION('center_axis',(0.,1.23467863058847E-16,-1.));
#115602=DIRECTION('ref_axis',(0.,1.,0.));
#115603=DIRECTION('center_axis',(0.,-1.,0.));
#115604=DIRECTION('ref_axis',(0.,0.,1.));
#115605=DIRECTION('center_axis',(0.,0.,-1.));
#115606=DIRECTION('ref_axis',(0.,1.,0.));
#115607=DIRECTION('center_axis',(0.,0.,1.));
#115608=DIRECTION('ref_axis',(0.,1.,0.));
#115609=DIRECTION('center_axis',(-1.,0.,4.58212374768871E-32));
#115610=DIRECTION('ref_axis',(0.,1.,0.));
#115611=DIRECTION('center_axis',(-1.,0.,0.));
#115612=DIRECTION('ref_axis',(0.,0.,1.));
#115613=DIRECTION('',(1.,-3.71118737634973E-16,-4.58212374768871E-32));
#115614=DIRECTION('',(-1.,3.71118737634973E-16,4.58212374768871E-32));
#115615=DIRECTION('center_axis',(0.,-1.,0.));
#115616=DIRECTION('ref_axis',(0.,0.,-1.));
#115617=DIRECTION('center_axis',(0.,-1.,0.));
#115618=DIRECTION('ref_axis',(0.,0.,1.));
#115619=DIRECTION('',(0.,1.,1.23467863058847E-16));
#115620=DIRECTION('',(0.,-1.,-1.23467863058847E-16));
#115621=DIRECTION('center_axis',(0.,1.23467863058847E-16,-1.));
#115622=DIRECTION('ref_axis',(0.,1.,0.));
#115623=DIRECTION('center_axis',(0.,0.,-1.));
#115624=DIRECTION('ref_axis',(0.,1.,0.));
#115625=DIRECTION('center_axis',(0.,0.,1.));
#115626=DIRECTION('ref_axis',(0.,1.,0.));
#115627=DIRECTION('center_axis',(0.,1.23467863058847E-16,-1.));
#115628=DIRECTION('ref_axis',(0.,1.,0.));
#115629=DIRECTION('center_axis',(0.0972343474872435,0.995261514210577,0.));
#115630=DIRECTION('ref_axis',(-0.995261514210577,0.0972343474872435,0.));
#115631=DIRECTION('center_axis',(1.78485500480727E-31,2.58019156504489E-46,
-1.));
#115632=DIRECTION('ref_axis',(-1.44560289664734E-15,1.,-3.88938454866321E-62));
#115633=DIRECTION('center_axis',(-1.,0.,0.));
#115634=DIRECTION('ref_axis',(0.,0.,1.));
#115635=DIRECTION('center_axis',(0.,0.,1.));
#115636=DIRECTION('ref_axis',(0.,1.,0.));
#115637=DIRECTION('center_axis',(-1.,0.,4.58212374768871E-32));
#115638=DIRECTION('ref_axis',(0.,1.,0.));
#115639=DIRECTION('center_axis',(-1.,0.,0.));
#115640=DIRECTION('ref_axis',(0.,0.,1.));
#115641=DIRECTION('',(1.,-3.71118737634973E-16,-4.58212374768871E-32));
#115642=DIRECTION('',(-1.,3.71118737634973E-16,4.58212374768871E-32));
#115643=DIRECTION('center_axis',(0.,1.23467863058847E-16,-1.));
#115644=DIRECTION('ref_axis',(0.,1.,0.));
#115645=DIRECTION('center_axis',(0.359814015251205,0.933024048151389,0.));
#115646=DIRECTION('ref_axis',(-0.933024048151389,0.359814015251205,0.));
#115647=DIRECTION('center_axis',(0.,0.,1.));
#115648=DIRECTION('ref_axis',(0.,1.,0.));
#115649=DIRECTION('center_axis',(-9.86953423458227E-31,7.88931658768281E-45,
-1.));
#115650=DIRECTION('ref_axis',(7.99360577730113E-15,1.,-2.48920611114446E-60));
#115651=DIRECTION('center_axis',(0.,1.23467863058847E-16,-1.));
#115652=DIRECTION('ref_axis',(0.,1.,0.));
#115653=DIRECTION('center_axis',(0.,1.,0.));
#115654=DIRECTION('ref_axis',(0.,0.,-1.));
#115655=DIRECTION('center_axis',(0.,0.,1.));
#115656=DIRECTION('ref_axis',(0.,1.,0.));
#115657=DIRECTION('center_axis',(0.,0.,-1.));
#115658=DIRECTION('ref_axis',(0.,1.,0.));
#115659=DIRECTION('center_axis',(0.,1.23467863058847E-16,-1.));
#115660=DIRECTION('ref_axis',(0.,1.,0.));
#115661=DIRECTION('center_axis',(0.,1.,0.));
#115662=DIRECTION('ref_axis',(0.,0.,-1.));
#115663=DIRECTION('center_axis',(0.,0.,-1.));
#115664=DIRECTION('ref_axis',(0.,1.,0.));
#115665=DIRECTION('center_axis',(0.,0.,1.));
#115666=DIRECTION('ref_axis',(0.,1.,0.));
#115667=DIRECTION('center_axis',(-7.82779334765923E-17,-1.,0.));
#115668=DIRECTION('ref_axis',(0.,0.,-1.));
#115669=DIRECTION('center_axis',(0.,1.,0.));
#115670=DIRECTION('ref_axis',(0.,0.,-1.));
#115671=DIRECTION('',(-7.82779334765923E-17,-1.,-1.23467863058847E-16));
#115672=DIRECTION('',(7.82779334765923E-17,1.,1.23467863058847E-16));
#115673=DIRECTION('center_axis',(-5.87084501074442E-17,1.,0.));
#115674=DIRECTION('ref_axis',(0.,0.,1.));
#115675=DIRECTION('center_axis',(0.,1.,0.));
#115676=DIRECTION('ref_axis',(0.,0.,-1.));
#115677=DIRECTION('',(5.87084501074442E-17,-1.,-1.23467863058847E-16));
#115678=DIRECTION('',(-5.87084501074442E-17,1.,1.23467863058847E-16));
#115679=DIRECTION('center_axis',(0.,1.23467863058847E-16,-1.));
#115680=DIRECTION('ref_axis',(0.,1.,0.));
#115681=DIRECTION('center_axis',(1.,0.,0.));
#115682=DIRECTION('ref_axis',(0.,0.,-1.));
#115683=DIRECTION('center_axis',(0.,0.,1.));
#115684=DIRECTION('ref_axis',(0.,1.,0.));
#115685=DIRECTION('center_axis',(3.56971000961454E-31,1.03207662601795E-45,
-1.));
#115686=DIRECTION('ref_axis',(-2.89120579329468E-15,1.,-2.1780553472514E-60));
#115687=DIRECTION('center_axis',(0.,1.23467863058847E-16,-1.));
#115688=DIRECTION('ref_axis',(0.,1.,0.));
#115689=DIRECTION('center_axis',(-1.,0.,0.));
#115690=DIRECTION('ref_axis',(0.,0.,1.));
#115691=DIRECTION('center_axis',(0.,0.,-1.));
#115692=DIRECTION('ref_axis',(0.,1.,0.));
#115693=DIRECTION('center_axis',(0.,0.,1.));
#115694=DIRECTION('ref_axis',(0.,1.,0.));
#115695=DIRECTION('center_axis',(1.,0.,4.58212374768871E-32));
#115696=DIRECTION('ref_axis',(0.,-1.,0.));
#115697=DIRECTION('',(1.,3.71118737634973E-16,4.58212374768871E-32));
#115698=DIRECTION('',(-1.,-3.71118737634973E-16,-4.58212374768871E-32));
#115699=DIRECTION('center_axis',(0.,1.23467863058847E-16,-1.));
#115700=DIRECTION('ref_axis',(0.,1.,0.));
#115701=DIRECTION('center_axis',(7.70988211545246E-15,1.,0.));
#115702=DIRECTION('ref_axis',(-1.,7.70988211545246E-15,0.));
#115703=DIRECTION('center_axis',(1.78485500480727E-31,2.58019156504489E-46,
-1.));
#115704=DIRECTION('ref_axis',(-1.44560289664734E-15,1.,-3.88938454866321E-62));
#115705=DIRECTION('center_axis',(-1.,0.,0.));
#115706=DIRECTION('ref_axis',(0.,0.,1.));
#115707=DIRECTION('center_axis',(0.,0.,1.));
#115708=DIRECTION('ref_axis',(0.,1.,0.));
#115709=DIRECTION('center_axis',(-1.,0.,4.07299888683441E-32));
#115710=DIRECTION('ref_axis',(0.,1.,0.));
#115711=DIRECTION('center_axis',(-1.,0.,0.));
#115712=DIRECTION('ref_axis',(0.,0.,1.));
#115713=DIRECTION('',(1.,-3.29883322342198E-16,-4.07299888683441E-32));
#115714=DIRECTION('',(-1.,3.29883322342198E-16,4.07299888683441E-32));
#115715=DIRECTION('center_axis',(-5.87084501074442E-17,1.,0.));
#115716=DIRECTION('ref_axis',(0.,0.,1.));
#115717=DIRECTION('center_axis',(0.,1.,0.));
#115718=DIRECTION('ref_axis',(0.,0.,-1.));
#115719=DIRECTION('',(5.87084501074442E-17,-1.,-1.23467863058847E-16));
#115720=DIRECTION('',(-5.87084501074442E-17,1.,1.23467863058847E-16));
#115721=DIRECTION('center_axis',(0.,1.23467863058847E-16,-1.));
#115722=DIRECTION('ref_axis',(0.,1.,0.));
#115723=DIRECTION('center_axis',(0.,1.,0.));
#115724=DIRECTION('ref_axis',(0.,0.,-1.));
#115725=DIRECTION('center_axis',(0.,0.,1.));
#115726=DIRECTION('ref_axis',(0.,1.,0.));
#115727=DIRECTION('center_axis',(0.,0.,-1.));
#115728=DIRECTION('ref_axis',(0.,1.,0.));
#115729=DIRECTION('center_axis',(0.,1.23467863058847E-16,-1.));
#115730=DIRECTION('ref_axis',(0.,1.,0.));
#115731=DIRECTION('center_axis',(-0.359814015251208,0.933024048151388,0.));
#115732=DIRECTION('ref_axis',(-0.933024048151388,-0.359814015251207,0.));
#115733=DIRECTION('center_axis',(0.,0.,-1.));
#115734=DIRECTION('ref_axis',(0.,1.,0.));
#115735=DIRECTION('center_axis',(0.,0.,1.));
#115736=DIRECTION('ref_axis',(0.,1.,0.));
#115737=DIRECTION('center_axis',(-7.82779334765923E-17,-1.,0.));
#115738=DIRECTION('ref_axis',(0.,0.,-1.));
#115739=DIRECTION('center_axis',(-3.85494105772624E-15,1.,0.));
#115740=DIRECTION('ref_axis',(-1.,-3.85494105772625E-15,0.));
#115741=DIRECTION('',(-7.82779334765923E-17,-1.,-1.23467863058847E-16));
#115742=DIRECTION('',(7.82779334765923E-17,1.,1.23467863058847E-16));
#115743=DIRECTION('center_axis',(0.,1.23467863058847E-16,-1.));
#115744=DIRECTION('ref_axis',(0.,1.,0.));
#115745=DIRECTION('center_axis',(-0.0972343474872435,0.995261514210577,
0.));
#115746=DIRECTION('ref_axis',(-0.995261514210577,-0.0972343474872435,0.));
#115747=DIRECTION('center_axis',(0.,0.,1.));
#115748=DIRECTION('ref_axis',(0.,1.,0.));
#115749=DIRECTION('center_axis',(-8.77291931962869E-31,6.2335340939716E-45,
-1.));
#115750=DIRECTION('ref_axis',(7.105427357601E-15,1.,-3.73380916671668E-60));
#115751=DIRECTION('center_axis',(0.,1.23467863058847E-16,-1.));
#115752=DIRECTION('ref_axis',(0.,1.,0.));
#115753=DIRECTION('center_axis',(1.,0.,0.));
#115754=DIRECTION('ref_axis',(0.,0.,-1.));
#115755=DIRECTION('center_axis',(0.,0.,1.));
#115756=DIRECTION('ref_axis',(0.,1.,0.));
#115757=DIRECTION('center_axis',(0.,0.,-1.));
#115758=DIRECTION('ref_axis',(0.,1.,0.));
#115759=DIRECTION('center_axis',(0.,1.23467863058847E-16,-1.));
#115760=DIRECTION('ref_axis',(0.,1.,0.));
#115761=DIRECTION('center_axis',(-1.,0.,0.));
#115762=DIRECTION('ref_axis',(0.,0.,1.));
#115763=DIRECTION('center_axis',(0.,0.,-1.));
#115764=DIRECTION('ref_axis',(0.,1.,0.));
#115765=DIRECTION('center_axis',(0.,0.,1.));
#115766=DIRECTION('ref_axis',(0.,1.,0.));
#115767=DIRECTION('center_axis',(1.,0.,4.58212374768871E-32));
#115768=DIRECTION('ref_axis',(0.,-1.,0.));
#115769=DIRECTION('',(1.,3.71118737634973E-16,4.58212374768871E-32));
#115770=DIRECTION('',(-1.,-3.71118737634973E-16,-4.58212374768871E-32));
#115771=DIRECTION('center_axis',(0.,1.23467863058847E-16,-1.));
#115772=DIRECTION('ref_axis',(0.,1.,0.));
#115773=DIRECTION('center_axis',(0.,1.,0.));
#115774=DIRECTION('ref_axis',(0.,0.,-1.));
#115775=DIRECTION('center_axis',(0.,0.,-1.));
#115776=DIRECTION('ref_axis',(0.,1.,0.));
#115777=DIRECTION('center_axis',(-1.,0.,0.));
#115778=DIRECTION('ref_axis',(0.,0.,1.));
#115779=DIRECTION('center_axis',(0.,0.,1.));
#115780=DIRECTION('ref_axis',(0.,1.,0.));
#115781=DIRECTION('center_axis',(-1.,0.,4.07299888683441E-32));
#115782=DIRECTION('ref_axis',(0.,1.,0.));
#115783=DIRECTION('center_axis',(-1.,0.,0.));
#115784=DIRECTION('ref_axis',(0.,0.,1.));
#115785=DIRECTION('',(1.,-3.29883322342198E-16,-4.07299888683441E-32));
#115786=DIRECTION('',(-1.,3.29883322342198E-16,4.07299888683441E-32));
#115787=DIRECTION('center_axis',(-7.82779334765923E-17,1.,0.));
#115788=DIRECTION('ref_axis',(0.,0.,1.));
#115789=DIRECTION('center_axis',(0.,1.,0.));
#115790=DIRECTION('ref_axis',(0.,0.,-1.));
#115791=DIRECTION('',(7.82779334765923E-17,-1.,-1.23467863058847E-16));
#115792=DIRECTION('',(-7.82779334765923E-17,1.,1.23467863058847E-16));
#115793=DIRECTION('center_axis',(0.,1.23467863058847E-16,-1.));
#115794=DIRECTION('ref_axis',(0.,1.,0.));
#115795=DIRECTION('center_axis',(0.,1.,0.));
#115796=DIRECTION('ref_axis',(0.,0.,-1.));
#115797=DIRECTION('center_axis',(0.,0.,1.));
#115798=DIRECTION('ref_axis',(0.,1.,0.));
#115799=DIRECTION('center_axis',(0.,0.,-1.));
#115800=DIRECTION('ref_axis',(0.,1.,0.));
#115801=DIRECTION('center_axis',(0.,1.23467863058847E-16,-1.));
#115802=DIRECTION('ref_axis',(0.,1.,0.));
#115803=DIRECTION('center_axis',(-1.,0.,0.));
#115804=DIRECTION('ref_axis',(0.,0.,1.));
#115805=DIRECTION('center_axis',(0.,0.,-1.));
#115806=DIRECTION('ref_axis',(0.,1.,0.));
#115807=DIRECTION('center_axis',(0.,0.,1.));
#115808=DIRECTION('ref_axis',(0.,1.,0.));
#115809=DIRECTION('center_axis',(0.,-1.,0.));
#115810=DIRECTION('ref_axis',(0.,0.,-1.));
#115811=DIRECTION('center_axis',(-3.85494105772624E-15,1.,0.));
#115812=DIRECTION('ref_axis',(-1.,-3.85494105772625E-15,0.));
#115813=DIRECTION('',(0.,-1.,-1.23467863058847E-16));
#115814=DIRECTION('',(0.,1.,1.23467863058847E-16));
#115815=DIRECTION('center_axis',(1.,0.,4.58212374768871E-32));
#115816=DIRECTION('ref_axis',(0.,-1.,0.));
#115817=DIRECTION('center_axis',(-1.,0.,0.));
#115818=DIRECTION('ref_axis',(0.,0.,1.));
#115819=DIRECTION('',(1.,3.71118737634973E-16,4.58212374768871E-32));
#115820=DIRECTION('',(-1.,-3.71118737634973E-16,-4.58212374768871E-32));
#115821=DIRECTION('center_axis',(0.,1.23467863058847E-16,-1.));
#115822=DIRECTION('ref_axis',(0.,1.,0.));
#115823=DIRECTION('center_axis',(0.,0.,-1.));
#115824=DIRECTION('ref_axis',(0.,1.,0.));
#115825=DIRECTION('center_axis',(0.,0.,1.));
#115826=DIRECTION('ref_axis',(0.,1.,0.));
#115827=DIRECTION('center_axis',(0.,1.23467863058847E-16,-1.));
#115828=DIRECTION('ref_axis',(0.,1.,0.));
#115829=DIRECTION('center_axis',(0.,1.,0.));
#115830=DIRECTION('ref_axis',(0.,0.,-1.));
#115831=DIRECTION('center_axis',(0.,0.,-1.));
#115832=DIRECTION('ref_axis',(0.,1.,0.));
#115833=DIRECTION('center_axis',(-1.,0.,0.));
#115834=DIRECTION('ref_axis',(0.,0.,1.));
#115835=DIRECTION('center_axis',(0.,0.,1.));
#115836=DIRECTION('ref_axis',(0.,1.,0.));
#115837=DIRECTION('center_axis',(-1.,0.,4.07299888683441E-32));
#115838=DIRECTION('ref_axis',(0.,1.,0.));
#115839=DIRECTION('center_axis',(-1.,0.,0.));
#115840=DIRECTION('ref_axis',(0.,0.,1.));
#115841=DIRECTION('',(1.,-3.29883322342198E-16,-4.07299888683441E-32));
#115842=DIRECTION('',(-1.,3.29883322342198E-16,4.07299888683441E-32));
#115843=DIRECTION('center_axis',(0.,1.,0.));
#115844=DIRECTION('ref_axis',(0.,0.,1.));
#115845=DIRECTION('center_axis',(0.,1.,0.));
#115846=DIRECTION('ref_axis',(0.,0.,-1.));
#115847=DIRECTION('',(0.,-1.,-1.23467863058847E-16));
#115848=DIRECTION('',(0.,1.,1.23467863058847E-16));
#115849=DIRECTION('center_axis',(0.,1.23467863058847E-16,-1.));
#115850=DIRECTION('ref_axis',(0.,1.,0.));
#115851=DIRECTION('center_axis',(-0.0138255496962003,0.999904422520272,
-3.41098746684905E-15));
#115852=DIRECTION('ref_axis',(-0.999904422520272,-0.0138255496962003,-3.38006024551251E-32));
#115853=DIRECTION('center_axis',(0.,0.,1.));
#115854=DIRECTION('ref_axis',(0.,1.,0.));
#115855=DIRECTION('center_axis',(0.,0.,-1.));
#115856=DIRECTION('ref_axis',(0.,1.,0.));
#115857=DIRECTION('center_axis',(0.,1.23467863058847E-16,-1.));
#115858=DIRECTION('ref_axis',(0.,1.,0.));
#115859=DIRECTION('center_axis',(-1.,0.,0.));
#115860=DIRECTION('ref_axis',(0.,0.,1.));
#115861=DIRECTION('center_axis',(0.,0.,-1.));
#115862=DIRECTION('ref_axis',(0.,1.,0.));
#115863=DIRECTION('center_axis',(0.,0.,1.));
#115864=DIRECTION('ref_axis',(0.,1.,0.));
#115865=DIRECTION('center_axis',(0.,1.23467863058847E-16,-1.));
#115866=DIRECTION('ref_axis',(0.,1.,1.25697703075927E-16));
#115867=DIRECTION('center_axis',(-0.00184724109421639,0.999998293848714,
0.));
#115868=DIRECTION('ref_axis',(-0.999998293848714,-0.00184724109421639,0.));
#115869=DIRECTION('center_axis',(0.,-1.22914743790472E-16,1.));
#115870=DIRECTION('ref_axis',(0.,1.,1.22914743790472E-16));
#115871=DIRECTION('center_axis',(0.,1.22833149346405E-16,-1.));
#115872=DIRECTION('ref_axis',(0.,1.,1.22833149346405E-16));
#115873=DIRECTION('center_axis',(1.,0.,4.58212374768871E-32));
#115874=DIRECTION('ref_axis',(0.,-1.,0.));
#115875=DIRECTION('center_axis',(-1.,0.,0.));
#115876=DIRECTION('ref_axis',(0.,0.,1.));
#115877=DIRECTION('',(1.,3.71118737634973E-16,4.58212374768871E-32));
#115878=DIRECTION('',(-1.,-3.71118737634973E-16,-4.58212374768871E-32));
#115879=DIRECTION('center_axis',(0.,1.23467863058847E-16,-1.));
#115880=DIRECTION('ref_axis',(0.,1.,0.));
#115881=DIRECTION('center_axis',(0.,0.,-1.));
#115882=DIRECTION('ref_axis',(0.,1.,0.));
#115883=DIRECTION('center_axis',(0.,0.,1.));
#115884=DIRECTION('ref_axis',(0.,1.,0.));
#115885=DIRECTION('center_axis',(0.,1.23467863058847E-16,-1.));
#115886=DIRECTION('ref_axis',(0.,1.,0.));
#115887=DIRECTION('center_axis',(0.,-1.,0.));
#115888=DIRECTION('ref_axis',(0.,0.,1.));
#115889=DIRECTION('center_axis',(0.,0.,-1.));
#115890=DIRECTION('ref_axis',(0.,1.,0.));
#115891=DIRECTION('center_axis',(1.,0.,0.));
#115892=DIRECTION('ref_axis',(0.,0.,-1.));
#115893=DIRECTION('center_axis',(0.,0.,1.));
#115894=DIRECTION('ref_axis',(0.,1.,0.));
#115895=DIRECTION('center_axis',(1.,0.,4.07299888683441E-32));
#115896=DIRECTION('ref_axis',(0.,-1.,0.));
#115897=DIRECTION('center_axis',(1.,0.,0.));
#115898=DIRECTION('ref_axis',(0.,0.,-1.));
#115899=DIRECTION('',(-1.,-3.29883322342198E-16,-4.07299888683441E-32));
#115900=DIRECTION('',(1.,3.29883322342198E-16,4.07299888683441E-32));
#115901=DIRECTION('center_axis',(0.,-1.,0.));
#115902=DIRECTION('ref_axis',(0.,0.,-1.));
#115903=DIRECTION('center_axis',(0.,-1.,0.));
#115904=DIRECTION('ref_axis',(0.,0.,1.));
#115905=DIRECTION('',(0.,1.,1.23467863058847E-16));
#115906=DIRECTION('',(0.,-1.,-1.23467863058847E-16));
#115907=DIRECTION('center_axis',(0.,1.23467863058847E-16,-1.));
#115908=DIRECTION('ref_axis',(0.,1.,0.));
#115909=DIRECTION('center_axis',(0.,-1.,0.));
#115910=DIRECTION('ref_axis',(0.,0.,1.));
#115911=DIRECTION('center_axis',(0.,0.,1.));
#115912=DIRECTION('ref_axis',(0.,1.,0.));
#115913=DIRECTION('center_axis',(0.,0.,-1.));
#115914=DIRECTION('ref_axis',(0.,1.,0.));
#115915=DIRECTION('center_axis',(0.,1.23467863058847E-16,-1.));
#115916=DIRECTION('ref_axis',(0.,1.,0.));
#115917=DIRECTION('center_axis',(1.,0.,0.));
#115918=DIRECTION('ref_axis',(0.,0.,-1.));
#115919=DIRECTION('center_axis',(0.,0.,-1.));
#115920=DIRECTION('ref_axis',(0.,1.,0.));
#115921=DIRECTION('center_axis',(0.,0.,1.));
#115922=DIRECTION('ref_axis',(0.,1.,0.));
#115923=DIRECTION('center_axis',(-7.82779334765923E-17,1.,0.));
#115924=DIRECTION('ref_axis',(0.,0.,1.));
#115925=DIRECTION('center_axis',(1.5419764230905E-14,-1.,0.));
#115926=DIRECTION('ref_axis',(1.,1.5419764230905E-14,0.));
#115927=DIRECTION('',(-7.82779334765923E-17,1.,1.23467863058847E-16));
#115928=DIRECTION('',(7.82779334765923E-17,-1.,-1.23467863058847E-16));
#115929=DIRECTION('center_axis',(-1.,0.,4.07299888683445E-32));
#115930=DIRECTION('ref_axis',(0.,1.,0.));
#115931=DIRECTION('center_axis',(1.,0.,0.));
#115932=DIRECTION('ref_axis',(0.,0.,-1.));
#115933=DIRECTION('',(-1.,3.29883322342202E-16,4.07299888683446E-32));
#115934=DIRECTION('',(1.,-3.29883322342202E-16,-4.07299888683446E-32));
#115935=DIRECTION('center_axis',(0.,1.23467863058847E-16,-1.));
#115936=DIRECTION('ref_axis',(0.,1.,0.));
#115937=DIRECTION('center_axis',(0.,0.,-1.));
#115938=DIRECTION('ref_axis',(0.,1.,0.));
#115939=DIRECTION('center_axis',(0.,0.,1.));
#115940=DIRECTION('ref_axis',(0.,1.,0.));
#115941=DIRECTION('center_axis',(0.,1.23467863058847E-16,-1.));
#115942=DIRECTION('ref_axis',(0.,1.,0.));
#115943=DIRECTION('center_axis',(0.,-1.,0.));
#115944=DIRECTION('ref_axis',(0.,0.,1.));
#115945=DIRECTION('center_axis',(0.,0.,-1.));
#115946=DIRECTION('ref_axis',(0.,1.,0.));
#115947=DIRECTION('center_axis',(1.,0.,0.));
#115948=DIRECTION('ref_axis',(0.,0.,-1.));
#115949=DIRECTION('center_axis',(0.,0.,1.));
#115950=DIRECTION('ref_axis',(0.,1.,0.));
#115951=DIRECTION('center_axis',(1.,0.,4.07299888683441E-32));
#115952=DIRECTION('ref_axis',(0.,-1.,0.));
#115953=DIRECTION('center_axis',(1.,0.,0.));
#115954=DIRECTION('ref_axis',(0.,0.,-1.));
#115955=DIRECTION('',(-1.,-3.29883322342198E-16,-4.07299888683441E-32));
#115956=DIRECTION('',(1.,3.29883322342198E-16,4.07299888683441E-32));
#115957=DIRECTION('center_axis',(-7.82779334765923E-17,-1.,0.));
#115958=DIRECTION('ref_axis',(0.,0.,-1.));
#115959=DIRECTION('center_axis',(0.,-1.,0.));
#115960=DIRECTION('ref_axis',(0.,0.,1.));
#115961=DIRECTION('',(7.82779334765923E-17,1.,1.23467863058847E-16));
#115962=DIRECTION('',(-7.82779334765923E-17,-1.,-1.23467863058847E-16));
#115963=DIRECTION('center_axis',(0.,1.23467863058847E-16,-1.));
#115964=DIRECTION('ref_axis',(0.,1.,0.));
#115965=DIRECTION('center_axis',(0.,-1.,0.));
#115966=DIRECTION('ref_axis',(0.,0.,1.));
#115967=DIRECTION('center_axis',(0.,0.,1.));
#115968=DIRECTION('ref_axis',(0.,1.,0.));
#115969=DIRECTION('center_axis',(0.,0.,-1.));
#115970=DIRECTION('ref_axis',(0.,1.,0.));
#115971=DIRECTION('center_axis',(0.,1.23467863058847E-16,-1.));
#115972=DIRECTION('ref_axis',(0.,1.,0.));
#115973=DIRECTION('center_axis',(1.,0.,0.));
#115974=DIRECTION('ref_axis',(0.,0.,-1.));
#115975=DIRECTION('center_axis',(0.,0.,-1.));
#115976=DIRECTION('ref_axis',(0.,1.,0.));
#115977=DIRECTION('center_axis',(0.,0.,1.));
#115978=DIRECTION('ref_axis',(0.,1.,0.));
#115979=DIRECTION('center_axis',(-5.87084501074442E-17,1.,0.));
#115980=DIRECTION('ref_axis',(0.,0.,1.));
#115981=DIRECTION('center_axis',(1.5419764230905E-14,-1.,-5.94422822341731E-29));
#115982=DIRECTION('ref_axis',(1.,1.5419764230905E-14,1.59309191113245E-57));
#115983=DIRECTION('',(-5.87084501074442E-17,1.,1.23467863058847E-16));
#115984=DIRECTION('',(5.87084501074442E-17,-1.,-1.23467863058847E-16));
#115985=DIRECTION('center_axis',(-1.,0.,4.07299888683445E-32));
#115986=DIRECTION('ref_axis',(0.,1.,0.));
#115987=DIRECTION('center_axis',(1.,0.,0.));
#115988=DIRECTION('ref_axis',(0.,0.,-1.));
#115989=DIRECTION('',(-1.,3.29883322342202E-16,4.07299888683446E-32));
#115990=DIRECTION('',(1.,-3.29883322342202E-16,-4.07299888683446E-32));
#115991=DIRECTION('center_axis',(0.,1.23467863058847E-16,-1.));
#115992=DIRECTION('ref_axis',(0.,1.,0.));
#115993=DIRECTION('center_axis',(0.,0.,-1.));
#115994=DIRECTION('ref_axis',(0.,1.,0.));
#115995=DIRECTION('center_axis',(0.,0.,1.));
#115996=DIRECTION('ref_axis',(0.,1.,0.));
#115997=DIRECTION('center_axis',(0.,1.23467863058847E-16,-1.));
#115998=DIRECTION('ref_axis',(0.,1.,0.));
#115999=DIRECTION('center_axis',(0.,1.,0.));
#116000=DIRECTION('ref_axis',(0.,0.,-1.));
#116001=DIRECTION('center_axis',(0.,0.,-1.));
#116002=DIRECTION('ref_axis',(0.,1.,0.));
#116003=DIRECTION('center_axis',(-1.,4.81867632215781E-16,7.43028527927166E-30));
#116004=DIRECTION('ref_axis',(-4.81867632215781E-16,-1.,1.36218908067985E-60));
#116005=DIRECTION('center_axis',(0.,0.,1.));
#116006=DIRECTION('ref_axis',(0.,1.,0.));
#116007=DIRECTION('center_axis',(-1.,0.,4.07299888683445E-32));
#116008=DIRECTION('ref_axis',(0.,1.,0.));
#116009=DIRECTION('center_axis',(-1.,0.,0.));
#116010=DIRECTION('ref_axis',(0.,0.,1.));
#116011=DIRECTION('',(1.,-3.29883322342202E-16,-4.07299888683446E-32));
#116012=DIRECTION('',(-1.,3.29883322342202E-16,4.07299888683446E-32));
#116013=DIRECTION('center_axis',(-6.11546355285877E-17,1.,0.));
#116014=DIRECTION('ref_axis',(0.,0.,1.));
#116015=DIRECTION('center_axis',(0.,1.,0.));
#116016=DIRECTION('ref_axis',(0.,0.,-1.));
#116017=DIRECTION('',(6.11546355285877E-17,-1.,-1.23467863058847E-16));
#116018=DIRECTION('',(-6.11546355285877E-17,1.,1.23467863058847E-16));
#116019=DIRECTION('center_axis',(0.,1.23467863058847E-16,-1.));
#116020=DIRECTION('ref_axis',(0.,1.,0.));
#116021=DIRECTION('center_axis',(0.,1.,0.));
#116022=DIRECTION('ref_axis',(0.,0.,-1.));
#116023=DIRECTION('center_axis',(0.,0.,1.));
#116024=DIRECTION('ref_axis',(0.,1.,0.));
#116025=DIRECTION('center_axis',(0.,0.,-1.));
#116026=DIRECTION('ref_axis',(0.,1.,0.));
#116027=DIRECTION('center_axis',(0.,1.23467863058847E-16,-1.));
#116028=DIRECTION('ref_axis',(0.,1.,0.));
#116029=DIRECTION('center_axis',(-0.995922166025996,0.0902166238455435,
0.));
#116030=DIRECTION('ref_axis',(-0.0902166238455435,-0.995922166025996,0.));
#116031=DIRECTION('center_axis',(1.11553437800454E-31,1.00788733009566E-46,
-1.));
#116032=DIRECTION('ref_axis',(-9.03501810404587E-16,1.,1.16681536459896E-61));
#116033=DIRECTION('center_axis',(0.,0.,1.));
#116034=DIRECTION('ref_axis',(0.,1.,0.));
#116035=DIRECTION('center_axis',(0.,-1.,-1.23467863058847E-16));
#116036=DIRECTION('ref_axis',(-1.,0.,0.));
#116037=DIRECTION('center_axis',(0.,1.,0.));
#116038=DIRECTION('ref_axis',(0.,0.,-1.));
#116039=DIRECTION('',(3.13111733906369E-16,-1.,-1.23467863058847E-16));
#116040=DIRECTION('',(-3.13111733906369E-16,1.,1.23467863058847E-16));
#116041=DIRECTION('center_axis',(0.,1.23467863058847E-16,-1.));
#116042=DIRECTION('ref_axis',(0.,1.,0.));
#116043=DIRECTION('center_axis',(-0.913440670994019,0.406971916198153,0.));
#116044=DIRECTION('ref_axis',(-0.406971916198153,-0.913440670994019,0.));
#116045=DIRECTION('center_axis',(0.,0.,1.));
#116046=DIRECTION('ref_axis',(0.,1.,0.));
#116047=DIRECTION('center_axis',(0.,0.,-1.));
#116048=DIRECTION('ref_axis',(0.,1.,0.));
#116049=DIRECTION('center_axis',(0.,1.23467863058847E-16,-1.));
#116050=DIRECTION('ref_axis',(0.,1.,0.));
#116051=DIRECTION('center_axis',(0.,0.,-1.));
#116052=DIRECTION('ref_axis',(0.,1.,0.));
#116053=DIRECTION('center_axis',(0.99836765577839,-0.0571141304368842,0.));
#116054=DIRECTION('ref_axis',(0.0571141304368842,0.99836765577839,0.));
#116055=DIRECTION('center_axis',(0.,0.,1.));
#116056=DIRECTION('ref_axis',(0.,1.,0.));
#116057=DIRECTION('center_axis',(0.,1.23467863058847E-16,-1.));
#116058=DIRECTION('ref_axis',(0.,1.,0.));
#116059=DIRECTION('center_axis',(0.,0.,1.));
#116060=DIRECTION('ref_axis',(0.,1.,0.));
#116061=DIRECTION('center_axis',(0.,0.,-1.));
#116062=DIRECTION('ref_axis',(0.,1.,0.));
#116063=DIRECTION('center_axis',(0.,1.23467863058847E-16,-1.));
#116064=DIRECTION('ref_axis',(0.,1.,0.));
#116065=DIRECTION('center_axis',(0.,1.,0.));
#116066=DIRECTION('ref_axis',(0.,0.,-1.));
#116067=DIRECTION('center_axis',(0.,0.,-1.));
#116068=DIRECTION('ref_axis',(0.,1.,0.));
#116069=DIRECTION('center_axis',(-1.,0.,0.));
#116070=DIRECTION('ref_axis',(0.,0.,1.));
#116071=DIRECTION('center_axis',(0.,0.,1.));
#116072=DIRECTION('ref_axis',(0.,1.,0.));
#116073=DIRECTION('center_axis',(-1.,0.,4.07299888683445E-32));
#116074=DIRECTION('ref_axis',(0.,1.,0.));
#116075=DIRECTION('center_axis',(-1.,0.,0.));
#116076=DIRECTION('ref_axis',(0.,0.,1.));
#116077=DIRECTION('',(1.,-3.29883322342202E-16,-4.07299888683446E-32));
#116078=DIRECTION('',(-1.,3.29883322342202E-16,4.07299888683446E-32));
#116079=DIRECTION('center_axis',(0.,1.,0.));
#116080=DIRECTION('ref_axis',(0.,0.,1.));
#116081=DIRECTION('center_axis',(0.,1.,0.));
#116082=DIRECTION('ref_axis',(0.,0.,-1.));
#116083=DIRECTION('',(0.,-1.,-1.23467863058847E-16));
#116084=DIRECTION('',(0.,1.,1.23467863058847E-16));
#116085=DIRECTION('center_axis',(0.,1.23467863058847E-16,-1.));
#116086=DIRECTION('ref_axis',(0.,1.,0.));
#116087=DIRECTION('center_axis',(-0.0294983404866249,0.999564829267484,
0.));
#116088=DIRECTION('ref_axis',(-0.999564829267484,-0.0294983404866249,0.));
#116089=DIRECTION('center_axis',(0.,0.,1.));
#116090=DIRECTION('ref_axis',(0.,1.,0.));
#116091=DIRECTION('center_axis',(0.,0.,-1.));
#116092=DIRECTION('ref_axis',(0.,1.,0.));
#116093=DIRECTION('center_axis',(0.,1.23467863058847E-16,-1.));
#116094=DIRECTION('ref_axis',(0.,1.,0.));
#116095=DIRECTION('center_axis',(-1.,0.,0.));
#116096=DIRECTION('ref_axis',(0.,0.,1.));
#116097=DIRECTION('center_axis',(0.,0.,-1.));
#116098=DIRECTION('ref_axis',(0.,1.,0.));
#116099=DIRECTION('center_axis',(0.,0.,1.));
#116100=DIRECTION('ref_axis',(0.,1.,0.));
#116101=DIRECTION('center_axis',(0.,1.23467863058847E-16,-1.));
#116102=DIRECTION('ref_axis',(0.,1.,1.25697703075927E-16));
#116103=DIRECTION('center_axis',(-0.0175200318846409,0.999846512462168,
7.7086987446295E-15));
#116104=DIRECTION('ref_axis',(-0.999846512462168,-0.0175200318846409,1.3995963210887E-31));
#116105=DIRECTION('center_axis',(0.,-1.22914743790472E-16,1.));
#116106=DIRECTION('ref_axis',(0.,1.,1.22914743790472E-16));
#116107=DIRECTION('center_axis',(-1.09981052690886E-31,1.22833149346405E-16,
-1.));
#116108=DIRECTION('ref_axis',(1.73276629344662E-13,1.,1.22833149346405E-16));
#116109=DIRECTION('center_axis',(1.,0.,4.07299888683441E-32));
#116110=DIRECTION('ref_axis',(0.,-1.,0.));
#116111=DIRECTION('center_axis',(-1.,0.,0.));
#116112=DIRECTION('ref_axis',(0.,0.,1.));
#116113=DIRECTION('',(1.,3.29883322342198E-16,4.07299888683441E-32));
#116114=DIRECTION('',(-1.,-3.29883322342198E-16,-4.07299888683441E-32));
#116115=DIRECTION('center_axis',(0.,1.23467863058847E-16,-1.));
#116116=DIRECTION('ref_axis',(0.,1.,0.));
#116117=DIRECTION('center_axis',(0.,0.,-1.));
#116118=DIRECTION('ref_axis',(0.,1.,0.));
#116119=DIRECTION('center_axis',(0.,0.,1.));
#116120=DIRECTION('ref_axis',(0.,1.,0.));
#116121=DIRECTION('center_axis',(0.,1.23467863058847E-16,-1.));
#116122=DIRECTION('ref_axis',(0.,1.,0.));
#116123=DIRECTION('center_axis',(-1.5419764230905E-14,1.,0.));
#116124=DIRECTION('ref_axis',(-1.,-1.5419764230905E-14,0.));
#116125=DIRECTION('center_axis',(0.,0.,-1.));
#116126=DIRECTION('ref_axis',(0.,1.,0.));
#116127=DIRECTION('center_axis',(-1.,0.,0.));
#116128=DIRECTION('ref_axis',(0.,0.,1.));
#116129=DIRECTION('center_axis',(0.,0.,1.));
#116130=DIRECTION('ref_axis',(0.,1.,0.));
#116131=DIRECTION('center_axis',(-1.,0.,7.06547394595967E-32));
#116132=DIRECTION('ref_axis',(0.,1.,0.));
#116133=DIRECTION('center_axis',(-1.,0.,0.));
#116134=DIRECTION('ref_axis',(0.,0.,1.));
#116135=DIRECTION('',(1.,-5.72252063890675E-16,-7.06547394595967E-32));
#116136=DIRECTION('',(-1.,5.72252063890675E-16,7.06547394595967E-32));
#116137=DIRECTION('center_axis',(0.,1.,0.));
#116138=DIRECTION('ref_axis',(0.,0.,1.));
#116139=DIRECTION('center_axis',(0.,1.,0.));
#116140=DIRECTION('ref_axis',(0.,0.,-1.));
#116141=DIRECTION('',(0.,-1.,-1.23467863058847E-16));
#116142=DIRECTION('',(0.,1.,1.23467863058847E-16));
#116143=DIRECTION('center_axis',(0.,1.23467863058847E-16,-1.));
#116144=DIRECTION('ref_axis',(0.,1.,0.));
#116145=DIRECTION('center_axis',(-0.64691256419049,0.762564183719958,0.));
#116146=DIRECTION('ref_axis',(-0.762564183719958,-0.64691256419049,0.));
#116147=DIRECTION('center_axis',(0.,0.,1.));
#116148=DIRECTION('ref_axis',(0.,1.,0.));
#116149=DIRECTION('center_axis',(0.,0.,-1.));
#116150=DIRECTION('ref_axis',(0.,1.,0.));
#116151=DIRECTION('center_axis',(0.,1.23467863058847E-16,-1.));
#116152=DIRECTION('ref_axis',(0.,1.,0.));
#116153=DIRECTION('center_axis',(-1.,0.,0.));
#116154=DIRECTION('ref_axis',(0.,0.,1.));
#116155=DIRECTION('center_axis',(0.,0.,-1.));
#116156=DIRECTION('ref_axis',(0.,1.,0.));
#116157=DIRECTION('center_axis',(0.,0.,1.));
#116158=DIRECTION('ref_axis',(0.,1.,0.));
#116159=DIRECTION('center_axis',(0.,1.23467863058847E-16,-1.));
#116160=DIRECTION('ref_axis',(0.,1.,0.));
#116161=DIRECTION('center_axis',(-0.55837318130784,0.829589892896582,0.));
#116162=DIRECTION('ref_axis',(-0.829589892896582,-0.55837318130784,0.));
#116163=DIRECTION('center_axis',(0.,0.,1.));
#116164=DIRECTION('ref_axis',(0.,1.,0.));
#116165=DIRECTION('center_axis',(0.,0.,-1.));
#116166=DIRECTION('ref_axis',(0.,1.,0.));
#116167=DIRECTION('center_axis',(1.,0.,4.07299888683445E-32));
#116168=DIRECTION('ref_axis',(0.,-1.,0.));
#116169=DIRECTION('center_axis',(-1.,0.,0.));
#116170=DIRECTION('ref_axis',(0.,0.,1.));
#116171=DIRECTION('',(1.,3.29883322342202E-16,4.07299888683446E-32));
#116172=DIRECTION('',(-1.,-3.29883322342202E-16,-4.07299888683446E-32));
#116173=DIRECTION('center_axis',(0.,1.23467863058847E-16,-1.));
#116174=DIRECTION('ref_axis',(0.,1.,0.));
#116175=DIRECTION('center_axis',(-0.03879684915621,0.999247118832749,5.83634271056011E-15));
#116176=DIRECTION('ref_axis',(-0.999247118832749,-0.03879684915621,-4.4574149748685E-34));
#116177=DIRECTION('center_axis',(0.,0.,1.));
#116178=DIRECTION('ref_axis',(0.,1.,0.));
#116179=DIRECTION('center_axis',(0.,0.,-1.));
#116180=DIRECTION('ref_axis',(0.,1.,0.));
#116181=DIRECTION('center_axis',(0.,1.23467863058847E-16,-1.));
#116182=DIRECTION('ref_axis',(0.,1.,0.));
#116183=DIRECTION('center_axis',(0.0331928226750423,-0.999448966442441,
0.));
#116184=DIRECTION('ref_axis',(0.999448966442441,0.0331928226750423,0.));
#116185=DIRECTION('center_axis',(0.,0.,-1.));
#116186=DIRECTION('ref_axis',(0.,1.,0.));
#116187=DIRECTION('center_axis',(0.,0.,1.));
#116188=DIRECTION('ref_axis',(0.,1.,0.));
#116189=DIRECTION('center_axis',(0.,1.23467863058847E-16,-1.));
#116190=DIRECTION('ref_axis',(0.,1.,1.25697703075927E-16));
#116191=DIRECTION('center_axis',(-1.17257681885938E-31,1.22833149346405E-16,
-1.));
#116192=DIRECTION('ref_axis',(1.84741056616993E-13,1.,1.22833149346405E-16));
#116193=DIRECTION('center_axis',(0.,-1.22914743790472E-16,1.));
#116194=DIRECTION('ref_axis',(0.,1.,1.22914743790472E-16));
#116195=DIRECTION('center_axis',(0.,1.23467863058847E-16,-1.));
#116196=DIRECTION('ref_axis',(0.,1.,0.));
#116197=DIRECTION('center_axis',(0.,1.,0.));
#116198=DIRECTION('ref_axis',(0.,0.,-1.));
#116199=DIRECTION('center_axis',(0.,0.,-1.));
#116200=DIRECTION('ref_axis',(0.,1.,0.));
#116201=DIRECTION('center_axis',(-1.,0.,0.));
#116202=DIRECTION('ref_axis',(0.,0.,1.));
#116203=DIRECTION('center_axis',(0.,0.,1.));
#116204=DIRECTION('ref_axis',(0.,1.,0.));
#116205=DIRECTION('center_axis',(-1.,0.,7.06547394595967E-32));
#116206=DIRECTION('ref_axis',(0.,1.,0.));
#116207=DIRECTION('center_axis',(-1.,0.,0.));
#116208=DIRECTION('ref_axis',(0.,0.,1.));
#116209=DIRECTION('',(1.,-5.72252063890675E-16,-7.06547394595967E-32));
#116210=DIRECTION('',(-1.,5.72252063890675E-16,7.06547394595967E-32));
#116211=DIRECTION('center_axis',(-7.82779334765923E-17,1.,0.));
#116212=DIRECTION('ref_axis',(0.,0.,1.));
#116213=DIRECTION('center_axis',(0.,1.,0.));
#116214=DIRECTION('ref_axis',(0.,0.,-1.));
#116215=DIRECTION('',(7.82779334765923E-17,-1.,-1.23467863058847E-16));
#116216=DIRECTION('',(-7.82779334765923E-17,1.,1.23467863058847E-16));
#116217=DIRECTION('center_axis',(0.,1.23467863058847E-16,-1.));
#116218=DIRECTION('ref_axis',(0.,1.,0.));
#116219=DIRECTION('center_axis',(0.,1.,0.));
#116220=DIRECTION('ref_axis',(0.,0.,-1.));
#116221=DIRECTION('center_axis',(0.,0.,1.));
#116222=DIRECTION('ref_axis',(0.,1.,0.));
#116223=DIRECTION('center_axis',(0.,0.,-1.));
#116224=DIRECTION('ref_axis',(0.,1.,0.));
#116225=DIRECTION('center_axis',(0.,1.23467863058847E-16,-1.));
#116226=DIRECTION('ref_axis',(0.,1.,0.));
#116227=DIRECTION('center_axis',(-1.,0.,0.));
#116228=DIRECTION('ref_axis',(0.,0.,1.));
#116229=DIRECTION('center_axis',(0.,0.,-1.));
#116230=DIRECTION('ref_axis',(0.,1.,0.));
#116231=DIRECTION('center_axis',(0.,0.,1.));
#116232=DIRECTION('ref_axis',(0.,1.,0.));
#116233=DIRECTION('center_axis',(0.,-1.,0.));
#116234=DIRECTION('ref_axis',(0.,0.,-1.));
#116235=DIRECTION('center_axis',(1.5419764230905E-14,1.,0.));
#116236=DIRECTION('ref_axis',(-1.,1.5419764230905E-14,0.));
#116237=DIRECTION('',(0.,-1.,-1.23467863058847E-16));
#116238=DIRECTION('',(0.,1.,1.23467863058847E-16));
#116239=DIRECTION('center_axis',(1.,0.,4.07299888683445E-32));
#116240=DIRECTION('ref_axis',(0.,-1.,0.));
#116241=DIRECTION('center_axis',(-1.,0.,0.));
#116242=DIRECTION('ref_axis',(0.,0.,1.));
#116243=DIRECTION('',(1.,3.29883322342202E-16,4.07299888683446E-32));
#116244=DIRECTION('',(-1.,-3.29883322342202E-16,-4.07299888683446E-32));
#116245=DIRECTION('center_axis',(0.,1.23467863058847E-16,-1.));
#116246=DIRECTION('ref_axis',(0.,1.,0.));
#116247=DIRECTION('center_axis',(0.,0.,-1.));
#116248=DIRECTION('ref_axis',(0.,1.,0.));
#116249=DIRECTION('center_axis',(0.,0.,1.));
#116250=DIRECTION('ref_axis',(0.,1.,0.));
#116251=DIRECTION('center_axis',(0.,1.23467863058847E-16,-1.));
#116252=DIRECTION('ref_axis',(0.,1.,0.));
#116253=DIRECTION('center_axis',(-1.5419764230905E-14,-1.,0.));
#116254=DIRECTION('ref_axis',(1.,-1.5419764230905E-14,0.));
#116255=DIRECTION('center_axis',(0.,0.,-1.));
#116256=DIRECTION('ref_axis',(0.,1.,0.));
#116257=DIRECTION('center_axis',(1.,0.,0.));
#116258=DIRECTION('ref_axis',(0.,0.,-1.));
#116259=DIRECTION('center_axis',(0.,0.,1.));
#116260=DIRECTION('ref_axis',(0.,1.,0.));
#116261=DIRECTION('center_axis',(1.,0.,-2.35515798198655E-32));
#116262=DIRECTION('ref_axis',(0.,-1.,0.));
#116263=DIRECTION('center_axis',(1.,0.,0.));
#116264=DIRECTION('ref_axis',(0.,0.,-1.));
#116265=DIRECTION('',(-1.,1.90750687963558E-16,2.35515798198656E-32));
#116266=DIRECTION('',(1.,-1.90750687963558E-16,-2.35515798198656E-32));
#116267=DIRECTION('center_axis',(0.,-1.,0.));
#116268=DIRECTION('ref_axis',(0.,0.,-1.));
#116269=DIRECTION('center_axis',(0.,-1.,0.));
#116270=DIRECTION('ref_axis',(0.,0.,1.));
#116271=DIRECTION('',(0.,1.,1.23467863058847E-16));
#116272=DIRECTION('',(0.,-1.,-1.23467863058847E-16));
#116273=DIRECTION('center_axis',(0.,1.23467863058847E-16,-1.));
#116274=DIRECTION('ref_axis',(0.,1.,0.));
#116275=DIRECTION('center_axis',(0.,-1.,0.));
#116276=DIRECTION('ref_axis',(0.,0.,1.));
#116277=DIRECTION('center_axis',(0.,0.,1.));
#116278=DIRECTION('ref_axis',(0.,1.,0.));
#116279=DIRECTION('center_axis',(0.,0.,-1.));
#116280=DIRECTION('ref_axis',(0.,1.,0.));
#116281=DIRECTION('center_axis',(0.,1.23467863058847E-16,-1.));
#116282=DIRECTION('ref_axis',(0.,1.,0.));
#116283=DIRECTION('center_axis',(0.787431540449696,-0.616402116402125,0.));
#116284=DIRECTION('ref_axis',(0.616402116402125,0.787431540449696,0.));
#116285=DIRECTION('center_axis',(0.,0.,-1.));
#116286=DIRECTION('ref_axis',(0.,1.,0.));
#116287=DIRECTION('center_axis',(0.,0.,1.));
#116288=DIRECTION('ref_axis',(0.,1.,0.));
#116289=DIRECTION('center_axis',(-7.82779334765923E-17,1.,0.));
#116290=DIRECTION('ref_axis',(0.,0.,1.));
#116291=DIRECTION('center_axis',(0.,-1.,0.));
#116292=DIRECTION('ref_axis',(0.,0.,1.));
#116293=DIRECTION('',(-7.82779334765923E-17,1.,1.23467863058847E-16));
#116294=DIRECTION('',(7.82779334765923E-17,-1.,-1.23467863058847E-16));
#116295=DIRECTION('center_axis',(0.,1.23467863058847E-16,-1.));
#116296=DIRECTION('ref_axis',(0.,1.,0.));
#116297=DIRECTION('center_axis',(0.873059908686793,-0.487612957009766,0.));
#116298=DIRECTION('ref_axis',(0.487612957009766,0.873059908686793,0.));
#116299=DIRECTION('center_axis',(0.,0.,-1.));
#116300=DIRECTION('ref_axis',(0.,1.,0.));
#116301=DIRECTION('center_axis',(0.,0.,1.));
#116302=DIRECTION('ref_axis',(0.,1.,0.));
#116303=DIRECTION('center_axis',(0.,1.23467863058847E-16,-1.));
#116304=DIRECTION('ref_axis',(0.695782815675814,-0.718252235228152,0.));
#116305=DIRECTION('center_axis',(-0.99949512518498,0.0317725468205174,0.));
#116306=DIRECTION('ref_axis',(-0.0317725468205174,-0.99949512518498,0.));
#116307=DIRECTION('center_axis',(0.,0.,1.));
#116308=DIRECTION('ref_axis',(0.,1.,0.));
#116309=DIRECTION('center_axis',(0.,0.,-1.));
#116310=DIRECTION('ref_axis',(0.,1.,0.));
#116311=DIRECTION('center_axis',(0.,1.23467863058847E-16,-1.));
#116312=DIRECTION('ref_axis',(0.,1.,0.));
#116313=DIRECTION('center_axis',(0.999425898115847,-0.0338802918425069,
0.));
#116314=DIRECTION('ref_axis',(0.0338802918425069,0.999425898115847,0.));
#116315=DIRECTION('center_axis',(0.,0.,-1.));
#116316=DIRECTION('ref_axis',(0.,1.,0.));
#116317=DIRECTION('center_axis',(0.,0.,1.));
#116318=DIRECTION('ref_axis',(0.,1.,0.));
#116319=DIRECTION('center_axis',(0.,1.23467863058847E-16,-1.));
#116320=DIRECTION('ref_axis',(0.,1.,1.25697703075927E-16));
#116321=DIRECTION('center_axis',(0.,1.22833149346405E-16,-1.));
#116322=DIRECTION('ref_axis',(0.,1.,1.22833149346405E-16));
#116323=DIRECTION('center_axis',(0.,-1.22914743790472E-16,1.));
#116324=DIRECTION('ref_axis',(0.,1.,1.22914743790472E-16));
#116325=DIRECTION('center_axis',(0.,1.23467863058847E-16,-1.));
#116326=DIRECTION('ref_axis',(0.,1.,0.));
#116327=DIRECTION('center_axis',(-1.5419764230905E-14,-1.,0.));
#116328=DIRECTION('ref_axis',(1.,-1.5419764230905E-14,0.));
#116329=DIRECTION('center_axis',(0.,0.,-1.));
#116330=DIRECTION('ref_axis',(0.,1.,0.));
#116331=DIRECTION('center_axis',(1.,0.,0.));
#116332=DIRECTION('ref_axis',(0.,0.,-1.));
#116333=DIRECTION('center_axis',(0.,0.,1.));
#116334=DIRECTION('ref_axis',(0.,1.,0.));
#116335=DIRECTION('center_axis',(1.,0.,-2.35515798198655E-32));
#116336=DIRECTION('ref_axis',(0.,-1.,0.));
#116337=DIRECTION('center_axis',(1.,0.,0.));
#116338=DIRECTION('ref_axis',(0.,0.,-1.));
#116339=DIRECTION('',(-1.,1.90750687963558E-16,2.35515798198656E-32));
#116340=DIRECTION('',(1.,-1.90750687963558E-16,-2.35515798198656E-32));
#116341=DIRECTION('center_axis',(-7.82779334765923E-17,-1.,0.));
#116342=DIRECTION('ref_axis',(0.,0.,-1.));
#116343=DIRECTION('center_axis',(0.,-1.,0.));
#116344=DIRECTION('ref_axis',(0.,0.,1.));
#116345=DIRECTION('',(7.82779334765923E-17,1.,1.23467863058847E-16));
#116346=DIRECTION('',(-7.82779334765923E-17,-1.,-1.23467863058847E-16));
#116347=DIRECTION('center_axis',(0.,1.23467863058847E-16,-1.));
#116348=DIRECTION('ref_axis',(0.,1.,0.));
#116349=DIRECTION('center_axis',(0.,-1.,0.));
#116350=DIRECTION('ref_axis',(0.,0.,1.));
#116351=DIRECTION('center_axis',(0.,0.,1.));
#116352=DIRECTION('ref_axis',(0.,1.,0.));
#116353=DIRECTION('center_axis',(0.,0.,-1.));
#116354=DIRECTION('ref_axis',(0.,1.,0.));
#116355=DIRECTION('center_axis',(0.,1.23467863058847E-16,-1.));
#116356=DIRECTION('ref_axis',(0.,1.,0.));
#116357=DIRECTION('center_axis',(0.99960573342019,-0.0280780646320843,0.));
#116358=DIRECTION('ref_axis',(0.0280780646320843,0.99960573342019,0.));
#116359=DIRECTION('center_axis',(0.,0.,-1.));
#116360=DIRECTION('ref_axis',(0.,1.,0.));
#116361=DIRECTION('center_axis',(0.,0.,1.));
#116362=DIRECTION('ref_axis',(0.,1.,0.));
#116363=DIRECTION('center_axis',(-5.87084501074442E-17,1.,0.));
#116364=DIRECTION('ref_axis',(0.,0.,1.));
#116365=DIRECTION('center_axis',(0.,-1.,0.));
#116366=DIRECTION('ref_axis',(0.,0.,1.));
#116367=DIRECTION('',(-5.87084501074442E-17,1.,1.23467863058847E-16));
#116368=DIRECTION('',(5.87084501074442E-17,-1.,-1.23467863058847E-16));
#116369=DIRECTION('center_axis',(0.,1.23467863058847E-16,-1.));
#116370=DIRECTION('ref_axis',(0.,1.,1.25697703075927E-16));
#116371=DIRECTION('center_axis',(0.999858703750256,-0.0168098939573669,
0.));
#116372=DIRECTION('ref_axis',(0.0168098939573669,0.999858703750256,0.));
#116373=DIRECTION('center_axis',(0.,1.22833149346405E-16,-1.));
#116374=DIRECTION('ref_axis',(0.,1.,1.22833149346405E-16));
#116375=DIRECTION('center_axis',(0.,-1.22914743790472E-16,1.));
#116376=DIRECTION('ref_axis',(0.,1.,1.22914743790472E-16));
#116377=DIRECTION('center_axis',(0.,1.23467863058847E-16,-1.));
#116378=DIRECTION('ref_axis',(0.701138397908224,-0.713025207814344,0.));
#116379=DIRECTION('center_axis',(0.,0.,-1.));
#116380=DIRECTION('ref_axis',(0.,1.,0.));
#116381=DIRECTION('center_axis',(0.,0.,1.));
#116382=DIRECTION('ref_axis',(0.,1.,0.));
#116383=DIRECTION('center_axis',(0.,1.23467863058847E-16,-1.));
#116384=DIRECTION('ref_axis',(0.,1.,0.));
#116385=DIRECTION('center_axis',(-1.5419764230905E-14,1.,0.));
#116386=DIRECTION('ref_axis',(-1.,-1.5419764230905E-14,0.));
#116387=DIRECTION('center_axis',(0.,0.,-1.));
#116388=DIRECTION('ref_axis',(0.,1.,0.));
#116389=DIRECTION('center_axis',(-1.,0.,0.));
#116390=DIRECTION('ref_axis',(0.,0.,1.));
#116391=DIRECTION('center_axis',(0.,0.,1.));
#116392=DIRECTION('ref_axis',(0.,1.,0.));
#116393=DIRECTION('center_axis',(-1.,0.,7.06547394595967E-32));
#116394=DIRECTION('ref_axis',(0.,1.,0.));
#116395=DIRECTION('center_axis',(-1.,0.,0.));
#116396=DIRECTION('ref_axis',(0.,0.,1.));
#116397=DIRECTION('',(1.,-5.72252063890675E-16,-7.06547394595967E-32));
#116398=DIRECTION('',(-1.,5.72252063890675E-16,7.06547394595967E-32));
#116399=DIRECTION('center_axis',(-5.87084501074442E-17,1.,0.));
#116400=DIRECTION('ref_axis',(0.,0.,1.));
#116401=DIRECTION('center_axis',(0.,1.,0.));
#116402=DIRECTION('ref_axis',(0.,0.,-1.));
#116403=DIRECTION('',(5.87084501074442E-17,-1.,-1.23467863058847E-16));
#116404=DIRECTION('',(-5.87084501074442E-17,1.,1.23467863058847E-16));
#116405=DIRECTION('center_axis',(0.,1.23467863058847E-16,-1.));
#116406=DIRECTION('ref_axis',(0.,1.,0.));
#116407=DIRECTION('center_axis',(0.,1.,0.));
#116408=DIRECTION('ref_axis',(0.,0.,-1.));
#116409=DIRECTION('center_axis',(0.,0.,1.));
#116410=DIRECTION('ref_axis',(0.,1.,0.));
#116411=DIRECTION('center_axis',(0.,0.,-1.));
#116412=DIRECTION('ref_axis',(0.,1.,0.));
#116413=DIRECTION('center_axis',(0.,1.23467863058847E-16,-1.));
#116414=DIRECTION('ref_axis',(0.,1.,0.));
#116415=DIRECTION('center_axis',(-1.,0.,0.));
#116416=DIRECTION('ref_axis',(0.,0.,1.));
#116417=DIRECTION('center_axis',(0.,0.,-1.));
#116418=DIRECTION('ref_axis',(0.,1.,0.));
#116419=DIRECTION('center_axis',(0.,0.,1.));
#116420=DIRECTION('ref_axis',(0.,1.,0.));
#116421=DIRECTION('center_axis',(-7.82779334765923E-17,-1.,0.));
#116422=DIRECTION('ref_axis',(0.,0.,-1.));
#116423=DIRECTION('center_axis',(1.5419764230905E-14,1.,0.));
#116424=DIRECTION('ref_axis',(-1.,1.5419764230905E-14,0.));
#116425=DIRECTION('',(-7.82779334765923E-17,-1.,-1.23467863058847E-16));
#116426=DIRECTION('',(7.82779334765923E-17,1.,1.23467863058847E-16));
#116427=DIRECTION('center_axis',(1.,0.,4.07299888683445E-32));
#116428=DIRECTION('ref_axis',(0.,-1.,0.));
#116429=DIRECTION('center_axis',(-1.,0.,0.));
#116430=DIRECTION('ref_axis',(0.,0.,1.));
#116431=DIRECTION('',(1.,3.29883322342202E-16,4.07299888683446E-32));
#116432=DIRECTION('',(-1.,-3.29883322342202E-16,-4.07299888683446E-32));
#116433=DIRECTION('center_axis',(0.,1.23467863058847E-16,-1.));
#116434=DIRECTION('ref_axis',(0.,1.,0.));
#116435=DIRECTION('center_axis',(0.,0.,-1.));
#116436=DIRECTION('ref_axis',(0.,1.,0.));
#116437=DIRECTION('center_axis',(0.,0.,1.));
#116438=DIRECTION('ref_axis',(0.,1.,0.));
#116439=DIRECTION('center_axis',(0.,1.23467863058847E-16,-1.));
#116440=DIRECTION('ref_axis',(0.,1.,0.));
#116441=DIRECTION('center_axis',(0.,-1.,0.));
#116442=DIRECTION('ref_axis',(0.,0.,1.));
#116443=DIRECTION('center_axis',(0.,0.,-1.));
#116444=DIRECTION('ref_axis',(0.,1.,0.));
#116445=DIRECTION('center_axis',(1.,0.,0.));
#116446=DIRECTION('ref_axis',(0.,0.,-1.));
#116447=DIRECTION('center_axis',(0.,0.,1.));
#116448=DIRECTION('ref_axis',(0.,1.,0.));
#116449=DIRECTION('center_axis',(1.,0.,-2.35515798198655E-32));
#116450=DIRECTION('ref_axis',(0.,-1.,0.));
#116451=DIRECTION('center_axis',(1.,-4.81867632215781E-16,0.));
#116452=DIRECTION('ref_axis',(4.81867632215781E-16,1.,0.));
#116453=DIRECTION('',(-1.,1.90750687963558E-16,2.35515798198656E-32));
#116454=DIRECTION('',(1.,-1.90750687963558E-16,-2.35515798198656E-32));
#116455=DIRECTION('center_axis',(0.,-1.,-1.23467863058847E-16));
#116456=DIRECTION('ref_axis',(-1.,0.,0.));
#116457=DIRECTION('center_axis',(0.,-1.,0.));
#116458=DIRECTION('ref_axis',(0.,0.,1.));
#116459=DIRECTION('',(-3.13111733906369E-16,1.,1.23467863058847E-16));
#116460=DIRECTION('',(3.13111733906369E-16,-1.,-1.23467863058847E-16));
#116461=DIRECTION('center_axis',(0.,1.23467863058847E-16,-1.));
#116462=DIRECTION('ref_axis',(0.,1.,0.));
#116463=DIRECTION('center_axis',(0.,-1.,0.));
#116464=DIRECTION('ref_axis',(0.,0.,1.));
#116465=DIRECTION('center_axis',(0.,0.,1.));
#116466=DIRECTION('ref_axis',(0.,1.,0.));
#116467=DIRECTION('center_axis',(0.,0.,-1.));
#116468=DIRECTION('ref_axis',(0.,1.,0.));
#116469=DIRECTION('center_axis',(0.,1.23467863058847E-16,-1.));
#116470=DIRECTION('ref_axis',(0.,1.,0.));
#116471=DIRECTION('center_axis',(0.999913989288144,-0.0131154117689341,
0.));
#116472=DIRECTION('ref_axis',(0.0131154117689341,0.999913989288144,0.));
#116473=DIRECTION('center_axis',(0.,0.,-1.));
#116474=DIRECTION('ref_axis',(0.,1.,0.));
#116475=DIRECTION('center_axis',(0.,0.,1.));
#116476=DIRECTION('ref_axis',(0.,1.,0.));
#116477=DIRECTION('center_axis',(-6.11546355285877E-17,1.,0.));
#116478=DIRECTION('ref_axis',(0.,0.,1.));
#116479=DIRECTION('center_axis',(0.,-1.,0.));
#116480=DIRECTION('ref_axis',(0.,0.,1.));
#116481=DIRECTION('',(-6.11546355285877E-17,1.,1.23467863058847E-16));
#116482=DIRECTION('',(6.11546355285877E-17,-1.,-1.23467863058847E-16));
#116483=DIRECTION('center_axis',(0.,1.23467863058847E-16,-1.));
#116484=DIRECTION('ref_axis',(0.,1.,1.25697703075927E-16));
#116485=DIRECTION('center_axis',(0.999998293848715,-0.00184724109421639,
0.));
#116486=DIRECTION('ref_axis',(0.00184724109421639,0.999998293848714,0.));
#116487=DIRECTION('center_axis',(0.,1.22833149346405E-16,-1.));
#116488=DIRECTION('ref_axis',(0.,1.,1.22833149346405E-16));
#116489=DIRECTION('center_axis',(0.,-1.22914743790472E-16,1.));
#116490=DIRECTION('ref_axis',(0.,1.,1.22914743790472E-16));
#116491=DIRECTION('center_axis',(0.,1.23467863058847E-16,-1.));
#116492=DIRECTION('ref_axis',(0.706453380948024,-0.707759578209371,0.));
#116493=DIRECTION('center_axis',(0.,0.,-1.));
#116494=DIRECTION('ref_axis',(0.,1.,0.));
#116495=DIRECTION('center_axis',(0.,0.,1.));
#116496=DIRECTION('ref_axis',(0.,1.,0.));
#116497=DIRECTION('center_axis',(0.,1.23467863058847E-16,-1.));
#116498=DIRECTION('ref_axis',(0.,1.,0.));
#116499=DIRECTION('center_axis',(0.,1.,0.));
#116500=DIRECTION('ref_axis',(0.,0.,-1.));
#116501=DIRECTION('center_axis',(0.,0.,-1.));
#116502=DIRECTION('ref_axis',(0.,1.,0.));
#116503=DIRECTION('center_axis',(-1.,4.81867632215781E-16,-7.43028527927166E-30));
#116504=DIRECTION('ref_axis',(-4.81867632215781E-16,-1.,-1.36218908067985E-60));
#116505=DIRECTION('center_axis',(0.,0.,1.));
#116506=DIRECTION('ref_axis',(0.,1.,0.));
#116507=DIRECTION('center_axis',(-1.,0.,7.06547394595967E-32));
#116508=DIRECTION('ref_axis',(0.,1.,0.));
#116509=DIRECTION('center_axis',(-1.,0.,0.));
#116510=DIRECTION('ref_axis',(0.,0.,1.));
#116511=DIRECTION('',(1.,-5.72252063890675E-16,-7.06547394595967E-32));
#116512=DIRECTION('',(-1.,5.72252063890675E-16,7.06547394595967E-32));
#116513=DIRECTION('center_axis',(-6.11546355285877E-17,1.,0.));
#116514=DIRECTION('ref_axis',(0.,0.,1.));
#116515=DIRECTION('center_axis',(0.,1.,0.));
#116516=DIRECTION('ref_axis',(0.,0.,-1.));
#116517=DIRECTION('',(6.11546355285877E-17,-1.,-1.23467863058847E-16));
#116518=DIRECTION('',(-6.11546355285877E-17,1.,1.23467863058847E-16));
#116519=DIRECTION('center_axis',(0.,1.23467863058847E-16,-1.));
#116520=DIRECTION('ref_axis',(0.,1.,0.));
#116521=DIRECTION('center_axis',(0.,1.,0.));
#116522=DIRECTION('ref_axis',(0.,0.,-1.));
#116523=DIRECTION('center_axis',(0.,0.,1.));
#116524=DIRECTION('ref_axis',(0.,1.,0.));
#116525=DIRECTION('center_axis',(1.78485500480727E-31,2.58019156504489E-46,
-1.));
#116526=DIRECTION('ref_axis',(-1.44560289664734E-15,1.,-3.88938454866321E-62));
#116527=DIRECTION('center_axis',(0.,1.23467863058847E-16,-1.));
#116528=DIRECTION('ref_axis',(0.,1.,0.));
#116529=DIRECTION('center_axis',(-1.,-4.81867632215781E-16,0.));
#116530=DIRECTION('ref_axis',(4.81867632215781E-16,-1.,0.));
#116531=DIRECTION('center_axis',(0.,0.,-1.));
#116532=DIRECTION('ref_axis',(0.,1.,0.));
#116533=DIRECTION('center_axis',(0.,0.,1.));
#116534=DIRECTION('ref_axis',(0.,1.,0.));
#116535=DIRECTION('center_axis',(0.,-1.,-1.23467863058847E-16));
#116536=DIRECTION('ref_axis',(-1.,0.,0.));
#116537=DIRECTION('center_axis',(0.,1.,0.));
#116538=DIRECTION('ref_axis',(0.,0.,-1.));
#116539=DIRECTION('',(3.13111733906369E-16,-1.,-1.23467863058847E-16));
#116540=DIRECTION('',(-3.13111733906369E-16,1.,1.23467863058847E-16));
#116541=DIRECTION('center_axis',(1.,0.,4.07299888683445E-32));
#116542=DIRECTION('ref_axis',(0.,-1.,0.));
#116543=DIRECTION('center_axis',(-1.,0.,0.));
#116544=DIRECTION('ref_axis',(0.,0.,1.));
#116545=DIRECTION('',(1.,3.29883322342202E-16,4.07299888683446E-32));
#116546=DIRECTION('',(-1.,-3.29883322342202E-16,-4.07299888683446E-32));
#116547=DIRECTION('center_axis',(0.,1.23467863058847E-16,-1.));
#116548=DIRECTION('ref_axis',(0.,1.,0.));
#116549=DIRECTION('center_axis',(0.,0.,-1.));
#116550=DIRECTION('ref_axis',(0.,1.,0.));
#116551=DIRECTION('center_axis',(0.,0.,1.));
#116552=DIRECTION('ref_axis',(0.,1.,0.));
#116553=DIRECTION('center_axis',(0.,1.23467863058847E-16,-1.));
#116554=DIRECTION('ref_axis',(0.,1.,0.));
#116555=DIRECTION('center_axis',(0.699822617100543,-0.714316669688274,0.));
#116556=DIRECTION('ref_axis',(0.714316669688274,0.699822617100543,0.));
#116557=DIRECTION('center_axis',(0.,0.,-1.));
#116558=DIRECTION('ref_axis',(0.,1.,0.));
#116559=DIRECTION('center_axis',(1.,0.,0.));
#116560=DIRECTION('ref_axis',(0.,0.,-1.));
#116561=DIRECTION('center_axis',(0.,0.,1.));
#116562=DIRECTION('ref_axis',(0.,1.,0.));
#116563=DIRECTION('center_axis',(1.,0.,-2.35515798198655E-32));
#116564=DIRECTION('ref_axis',(0.,-1.,0.));
#116565=DIRECTION('center_axis',(1.,0.,0.));
#116566=DIRECTION('ref_axis',(0.,0.,-1.));
#116567=DIRECTION('',(-1.,1.90750687963558E-16,2.35515798198656E-32));
#116568=DIRECTION('',(1.,-1.90750687963558E-16,-2.35515798198656E-32));
#116569=DIRECTION('center_axis',(0.,1.23467863058847E-16,-1.));
#116570=DIRECTION('ref_axis',(0.,1.,0.));
#116571=DIRECTION('center_axis',(0.74298130529014,-0.669312169312168,0.));
#116572=DIRECTION('ref_axis',(0.669312169312168,0.742981305290139,0.));
#116573=DIRECTION('center_axis',(0.,0.,-1.));
#116574=DIRECTION('ref_axis',(0.,1.,0.));
#116575=DIRECTION('center_axis',(0.,0.,1.));
#116576=DIRECTION('ref_axis',(0.,1.,0.));
#116577=DIRECTION('center_axis',(0.,1.23467863058847E-16,-1.));
#116578=DIRECTION('ref_axis',(0.,1.,0.));
#116579=DIRECTION('center_axis',(0.,-1.,0.));
#116580=DIRECTION('ref_axis',(0.,0.,1.));
#116581=DIRECTION('center_axis',(0.,0.,1.));
#116582=DIRECTION('ref_axis',(0.,1.,0.));
#116583=DIRECTION('center_axis',(0.,0.,-1.));
#116584=DIRECTION('ref_axis',(0.,1.,0.));
#116585=DIRECTION('center_axis',(0.,1.23467863058847E-16,-1.));
#116586=DIRECTION('ref_axis',(0.406625030395211,-0.913595142640379,0.));
#116587=DIRECTION('center_axis',(0.,1.,0.));
#116588=DIRECTION('ref_axis',(0.,0.,-1.));
#116589=DIRECTION('center_axis',(0.,0.,-1.));
#116590=DIRECTION('ref_axis',(0.,1.,0.));
#116591=DIRECTION('center_axis',(0.,0.,1.));
#116592=DIRECTION('ref_axis',(0.,1.,0.));
#116593=DIRECTION('center_axis',(0.,1.,0.));
#116594=DIRECTION('ref_axis',(0.,0.,1.));
#116595=DIRECTION('',(0.,-1.,-1.23467863058847E-16));
#116596=DIRECTION('',(0.,1.,1.23467863058847E-16));
#116597=DIRECTION('center_axis',(0.,1.23467863058847E-16,-1.));
#116598=DIRECTION('ref_axis',(0.,1.,0.));
#116599=DIRECTION('center_axis',(0.,0.,-1.));
#116600=DIRECTION('ref_axis',(0.,1.,0.));
#116601=DIRECTION('center_axis',(0.,-1.,0.));
#116602=DIRECTION('ref_axis',(0.,0.,1.));
#116603=DIRECTION('center_axis',(0.,0.,1.));
#116604=DIRECTION('ref_axis',(0.,1.,0.));
#116605=DIRECTION('center_axis',(-0.742981305290128,-0.669312169312181,
0.));
#116606=DIRECTION('ref_axis',(0.669312169312181,-0.742981305290128,0.));
#116607=DIRECTION('center_axis',(0.,1.,0.));
#116608=DIRECTION('ref_axis',(0.,0.,1.));
#116609=DIRECTION('center_axis',(0.,-1.,0.));
#116610=DIRECTION('ref_axis',(0.,0.,1.));
#116611=DIRECTION('',(0.,1.,1.23467863058847E-16));
#116612=DIRECTION('',(0.,-1.,-1.23467863058847E-16));
#116613=DIRECTION('center_axis',(0.,1.23467863058847E-16,-1.));
#116614=DIRECTION('ref_axis',(0.,1.,0.));
#116615=DIRECTION('center_axis',(-0.699822617100527,-0.714316669688289,
0.));
#116616=DIRECTION('ref_axis',(0.714316669688289,-0.699822617100527,0.));
#116617=DIRECTION('center_axis',(-1.20627640644894E-30,1.17852753964151E-44,
-1.));
#116618=DIRECTION('ref_axis',(9.76996261670138E-15,1.,-4.97841222228891E-60));
#116619=DIRECTION('center_axis',(0.,0.,1.));
#116620=DIRECTION('ref_axis',(0.,1.,0.));
#116621=DIRECTION('center_axis',(0.,1.23467863058847E-16,-1.));
#116622=DIRECTION('ref_axis',(0.,1.,0.));
#116623=DIRECTION('center_axis',(-1.,0.,0.));
#116624=DIRECTION('ref_axis',(0.,0.,1.));
#116625=DIRECTION('center_axis',(0.,0.,1.));
#116626=DIRECTION('ref_axis',(0.,1.,0.));
#116627=DIRECTION('center_axis',(0.,0.,-1.));
#116628=DIRECTION('ref_axis',(0.,1.,0.));
#116629=DIRECTION('center_axis',(0.,1.23467863058847E-16,-1.));
#116630=DIRECTION('ref_axis',(0.,1.,0.));
#116631=DIRECTION('center_axis',(1.,0.,0.));
#116632=DIRECTION('ref_axis',(0.,0.,-1.));
#116633=DIRECTION('center_axis',(0.,0.,-1.));
#116634=DIRECTION('ref_axis',(0.,1.,0.));
#116635=DIRECTION('center_axis',(0.,0.,1.));
#116636=DIRECTION('ref_axis',(0.,1.,0.));
#116637=DIRECTION('center_axis',(-1.,0.,-1.17757899099328E-32));
#116638=DIRECTION('ref_axis',(0.,1.,0.));
#116639=DIRECTION('',(-1.,-9.53753439817791E-17,-1.17757899099328E-32));
#116640=DIRECTION('',(1.,9.53753439817791E-17,1.17757899099328E-32));
#116641=DIRECTION('center_axis',(0.,1.23467863058847E-16,-1.));
#116642=DIRECTION('ref_axis',(0.,1.,0.));
#116643=DIRECTION('center_axis',(-0.87305990868679,0.487612957009772,0.));
#116644=DIRECTION('ref_axis',(-0.487612957009772,-0.87305990868679,0.));
#116645=DIRECTION('center_axis',(0.,0.,1.));
#116646=DIRECTION('ref_axis',(0.,1.,0.));
#116647=DIRECTION('center_axis',(-0.999425898115847,0.0338802918424838,
-7.7054558576033E-15));
#116648=DIRECTION('ref_axis',(-0.0338802918424838,-0.999425898115847,2.67737997453887E-33));
#116649=DIRECTION('center_axis',(0.,0.,-1.));
#116650=DIRECTION('ref_axis',(0.,1.,0.));
#116651=DIRECTION('center_axis',(0.,1.23467863058847E-16,-1.));
#116652=DIRECTION('ref_axis',(0.,1.,0.));
#116653=DIRECTION('center_axis',(-0.55837318130784,0.829589892896582,0.));
#116654=DIRECTION('ref_axis',(-0.829589892896582,-0.55837318130784,0.));
#116655=DIRECTION('center_axis',(0.,0.,1.));
#116656=DIRECTION('ref_axis',(0.,1.,0.));
#116657=DIRECTION('center_axis',(4.38645965981435E-31,1.5583835234929E-45,
-1.));
#116658=DIRECTION('ref_axis',(-3.5527136788005E-15,1.,-1.24460305557223E-60));
#116659=DIRECTION('center_axis',(0.,1.23467863058847E-16,-1.));
#116660=DIRECTION('ref_axis',(0.,1.,0.));
#116661=DIRECTION('center_axis',(-0.03879684915621,0.999247118832749,5.83634271056011E-15));
#116662=DIRECTION('ref_axis',(-0.999247118832749,-0.03879684915621,-4.4574149748685E-34));
#116663=DIRECTION('center_axis',(0.,0.,1.));
#116664=DIRECTION('ref_axis',(0.,1.,0.));
#116665=DIRECTION('center_axis',(6.64132094812011E-31,3.57235825122499E-45,
-1.));
#116666=DIRECTION('ref_axis',(-5.37898752240871E-15,1.,2.61366641670168E-59));
#116667=DIRECTION('center_axis',(0.,1.23467863058847E-16,-1.));
#116668=DIRECTION('ref_axis',(0.,1.,1.24777965780772E-16));
#116669=DIRECTION('center_axis',(0.0387968491562139,0.999247118832749,0.));
#116670=DIRECTION('ref_axis',(-0.999247118832749,0.0387968491562139,0.));
#116671=DIRECTION('center_axis',(0.,-1.22014183466588E-16,1.));
#116672=DIRECTION('ref_axis',(0.,1.,1.22014183466588E-16));
#116673=DIRECTION('center_axis',(4.09030343683335E-32,1.21933779888604E-16,
-1.));
#116674=DIRECTION('ref_axis',(-2.66628532023081E-14,1.,1.21933779888604E-16));
#116675=DIRECTION('center_axis',(0.,1.23467863058847E-16,-1.));
#116676=DIRECTION('ref_axis',(0.,1.,0.));
#116677=DIRECTION('center_axis',(0.55837318130784,0.829589892896582,0.));
#116678=DIRECTION('ref_axis',(-0.829589892896582,0.55837318130784,0.));
#116679=DIRECTION('center_axis',(0.,0.,1.));
#116680=DIRECTION('ref_axis',(0.,1.,0.));
#116681=DIRECTION('center_axis',(-1.32826418962402E-31,1.42894330048999E-46,
-1.));
#116682=DIRECTION('ref_axis',(1.07579750448174E-15,1.,9.14005368935855E-61));
#116683=DIRECTION('center_axis',(0.,1.23467863058847E-16,-1.));
#116684=DIRECTION('ref_axis',(0.,1.,0.));
#116685=DIRECTION('center_axis',(0.848949186868297,0.528474481991002,8.14895191435076E-15));
#116686=DIRECTION('ref_axis',(-0.528474481991002,0.848949186868297,-1.25969070483717E-30));
#116687=DIRECTION('center_axis',(0.,0.,1.));
#116688=DIRECTION('ref_axis',(0.,1.,0.));
#116689=DIRECTION('center_axis',(-1.53526088093502E-30,1.90901981627881E-44,
-1.));
#116690=DIRECTION('ref_axis',(1.24344978758017E-14,1.,2.98704733337335E-59));
#116691=DIRECTION('center_axis',(0.,1.23467863058847E-16,-1.));
#116692=DIRECTION('ref_axis',(0.,1.,0.));
#116693=DIRECTION('center_axis',(0.992522955047552,0.122058116090968,0.));
#116694=DIRECTION('ref_axis',(-0.122058116090968,0.992522955047552,0.));
#116695=DIRECTION('center_axis',(0.,0.,1.));
#116696=DIRECTION('ref_axis',(0.,1.,0.));
#116697=DIRECTION('center_axis',(-1.32826418962402E-31,1.42894330048999E-46,
-1.));
#116698=DIRECTION('ref_axis',(1.07579750448174E-15,1.,5.05619991326218E-61));
#116699=DIRECTION('center_axis',(0.,1.23467863058847E-16,-1.));
#116700=DIRECTION('ref_axis',(0.,1.,0.));
#116701=DIRECTION('center_axis',(-0.87305990868679,0.487612957009772,0.));
#116702=DIRECTION('ref_axis',(-0.487612957009772,-0.87305990868679,0.));
#116703=DIRECTION('center_axis',(0.,0.,1.));
#116704=DIRECTION('ref_axis',(0.,1.,0.));
#116705=DIRECTION('center_axis',(-0.999425898115848,0.0338802918424761,
0.));
#116706=DIRECTION('ref_axis',(-0.0338802918424761,-0.999425898115848,0.));
#116707=DIRECTION('center_axis',(-4.46213751201822E-31,1.61261972815309E-45,
-1.));
#116708=DIRECTION('ref_axis',(3.61400724161835E-15,1.,1.6490990486332E-59));
#116709=DIRECTION('center_axis',(0.,1.23467863058847E-16,-1.));
#116710=DIRECTION('ref_axis',(0.,1.,0.));
#116711=DIRECTION('center_axis',(-0.55837318130784,0.829589892896582,0.));
#116712=DIRECTION('ref_axis',(-0.829589892896582,-0.55837318130784,0.));
#116713=DIRECTION('center_axis',(0.,0.,1.));
#116714=DIRECTION('ref_axis',(0.,1.,0.));
#116715=DIRECTION('center_axis',(4.38645965981435E-31,1.5583835234929E-45,
-1.));
#116716=DIRECTION('ref_axis',(-3.5527136788005E-15,1.,-1.24460305557223E-60));
#116717=DIRECTION('center_axis',(0.,1.23467863058847E-16,-1.));
#116718=DIRECTION('ref_axis',(0.,1.,0.));
#116719=DIRECTION('center_axis',(-0.0387968491561946,0.99924711883275,0.));
#116720=DIRECTION('ref_axis',(-0.99924711883275,-0.0387968491561946,0.));
#116721=DIRECTION('center_axis',(0.,0.,1.));
#116722=DIRECTION('ref_axis',(0.,1.,0.));
#116723=DIRECTION('center_axis',(-8.92427502403635E-31,6.45047891261223E-45,
-1.));
#116724=DIRECTION('ref_axis',(7.2280144832367E-15,1.,3.73380916671669E-60));
#116725=DIRECTION('center_axis',(0.,1.23467863058847E-16,-1.));
#116726=DIRECTION('ref_axis',(0.,1.,1.25162611019057E-16));
#116727=DIRECTION('center_axis',(0.0387968491562177,0.999247118832749,0.));
#116728=DIRECTION('ref_axis',(-0.999247118832749,0.0387968491562177,0.));
#116729=DIRECTION('center_axis',(0.,-1.22309905988566E-16,1.));
#116730=DIRECTION('ref_axis',(0.,1.,1.22309905988566E-16));
#116731=DIRECTION('center_axis',(3.29067448743359E-32,1.22229112323298E-16,
-1.));
#116732=DIRECTION('ref_axis',(-2.65644604115968E-14,1.,1.22229112323298E-16));
#116733=DIRECTION('center_axis',(0.,1.23467863058847E-16,-1.));
#116734=DIRECTION('ref_axis',(0.,1.,0.));
#116735=DIRECTION('center_axis',(0.55837318130784,0.829589892896582,0.));
#116736=DIRECTION('ref_axis',(-0.829589892896582,0.55837318130784,0.));
#116737=DIRECTION('center_axis',(0.,0.,1.));
#116738=DIRECTION('ref_axis',(0.,1.,0.));
#116739=DIRECTION('center_axis',(0.,0.,-1.));
#116740=DIRECTION('ref_axis',(0.,1.,0.));
#116741=DIRECTION('center_axis',(0.,1.23467863058847E-16,-1.));
#116742=DIRECTION('ref_axis',(0.,1.,0.));
#116743=DIRECTION('center_axis',(0.848949186868305,0.528474481990989,0.));
#116744=DIRECTION('ref_axis',(-0.528474481990989,0.848949186868305,0.));
#116745=DIRECTION('center_axis',(0.,0.,1.));
#116746=DIRECTION('ref_axis',(0.,1.,0.));
#116747=DIRECTION('center_axis',(-1.53526088093502E-30,1.90901981627881E-44,
-1.));
#116748=DIRECTION('ref_axis',(1.24344978758017E-14,1.,3.23596794448779E-59));
#116749=DIRECTION('center_axis',(0.,1.23467863058847E-16,-1.));
#116750=DIRECTION('ref_axis',(0.,1.,0.));
#116751=DIRECTION('center_axis',(0.992522955047553,0.12205811609096,0.));
#116752=DIRECTION('ref_axis',(-0.12205811609096,0.992522955047552,0.));
#116753=DIRECTION('center_axis',(0.,0.,1.));
#116754=DIRECTION('ref_axis',(0.,1.,0.));
#116755=DIRECTION('center_axis',(1.42788400384582E-30,1.65132260162873E-44,
-1.));
#116756=DIRECTION('ref_axis',(-1.15648231731787E-14,1.,-2.48920611114446E-60));
#116757=DIRECTION('center_axis',(0.,1.23467863058847E-16,-1.));
#116758=DIRECTION('ref_axis',(0.,1.,0.));
#116759=DIRECTION('center_axis',(-0.689680595319751,0.724113717892013,0.));
#116760=DIRECTION('ref_axis',(-0.724113717892013,-0.689680595319751,0.));
#116761=DIRECTION('center_axis',(0.,0.,-1.));
#116762=DIRECTION('ref_axis',(0.,1.,0.));
#116763=DIRECTION('center_axis',(0.,0.,1.));
#116764=DIRECTION('ref_axis',(0.,1.,0.));
#116765=DIRECTION('center_axis',(0.68968059531976,-0.724113717892004,-8.94047733597239E-17));
#116766=DIRECTION('ref_axis',(-0.724113717892004,-0.68968059531976,2.34589631629098E-32));
#116767=DIRECTION('center_axis',(-0.689680595319751,0.724113717892013,0.));
#116768=DIRECTION('ref_axis',(-0.724113717892013,-0.689680595319751,0.));
#116769=DIRECTION('',(0.689680595319752,-0.724113717892012,-8.94047733597238E-17));
#116770=DIRECTION('',(-0.689680595319752,0.724113717892012,8.94047733597238E-17));
#116771=DIRECTION('center_axis',(0.,1.23467863058847E-16,-1.));
#116772=DIRECTION('ref_axis',(0.,1.,0.));
#116773=DIRECTION('center_axis',(0.,0.,-1.));
#116774=DIRECTION('ref_axis',(0.,1.,0.));
#116775=DIRECTION('center_axis',(0.,0.,1.));
#116776=DIRECTION('ref_axis',(0.,1.,0.));
#116777=DIRECTION('center_axis',(-0.635568809204586,-0.772044227208691,
0.));
#116778=DIRECTION('ref_axis',(0.772044227208691,-0.635568809204586,0.));
#116779=DIRECTION('center_axis',(0.,1.23467863058847E-16,-1.));
#116780=DIRECTION('ref_axis',(0.,1.,0.));
#116781=DIRECTION('center_axis',(-0.120708341042265,-0.992688015643799,
0.));
#116782=DIRECTION('ref_axis',(0.992688015643799,-0.120708341042265,0.));
#116783=DIRECTION('center_axis',(-2.19322982990717E-31,3.89595880873225E-46,
-1.));
#116784=DIRECTION('ref_axis',(1.77635683940025E-15,1.,7.77876909732643E-62));
#116785=DIRECTION('center_axis',(0.,0.,1.));
#116786=DIRECTION('ref_axis',(0.,1.,0.));
#116787=DIRECTION('center_axis',(0.,1.23467863058847E-16,-1.));
#116788=DIRECTION('ref_axis',(0.,1.,0.));
#116789=DIRECTION('center_axis',(1.,0.,0.));
#116790=DIRECTION('ref_axis',(0.,0.,-1.));
#116791=DIRECTION('center_axis',(0.,0.,-1.));
#116792=DIRECTION('ref_axis',(0.,1.,0.));
#116793=DIRECTION('center_axis',(0.,0.,1.));
#116794=DIRECTION('ref_axis',(0.,1.,0.));
#116795=DIRECTION('center_axis',(-1.,0.,4.58212374768871E-32));
#116796=DIRECTION('ref_axis',(0.,1.,0.));
#116797=DIRECTION('center_axis',(1.,0.,0.));
#116798=DIRECTION('ref_axis',(0.,0.,-1.));
#116799=DIRECTION('',(-1.,3.71118737634973E-16,4.58212374768871E-32));
#116800=DIRECTION('',(1.,-3.71118737634973E-16,-4.58212374768871E-32));
#116801=DIRECTION('center_axis',(0.,1.23467863058847E-16,-1.));
#116802=DIRECTION('ref_axis',(0.,1.,0.));
#116803=DIRECTION('center_axis',(0.,0.,-1.));
#116804=DIRECTION('ref_axis',(0.,1.,0.));
#116805=DIRECTION('center_axis',(0.,0.,1.));
#116806=DIRECTION('ref_axis',(0.,1.,0.));
#116807=DIRECTION('center_axis',(0.,1.23467863058847E-16,-1.));
#116808=DIRECTION('ref_axis',(0.,1.,0.));
#116809=DIRECTION('center_axis',(-1.,0.,0.));
#116810=DIRECTION('ref_axis',(0.,0.,1.));
#116811=DIRECTION('center_axis',(0.,0.,-1.));
#116812=DIRECTION('ref_axis',(0.,1.,0.));
#116813=DIRECTION('center_axis',(0.,0.,1.));
#116814=DIRECTION('ref_axis',(0.,1.,0.));
#116815=DIRECTION('center_axis',(1.,0.,4.58212374768871E-32));
#116816=DIRECTION('ref_axis',(0.,-1.,0.));
#116817=DIRECTION('center_axis',(-1.,0.,0.));
#116818=DIRECTION('ref_axis',(0.,0.,1.));
#116819=DIRECTION('',(1.,3.71118737634973E-16,4.58212374768871E-32));
#116820=DIRECTION('',(-1.,-3.71118737634973E-16,-4.58212374768871E-32));
#116821=DIRECTION('center_axis',(0.,1.23467863058847E-16,-1.));
#116822=DIRECTION('ref_axis',(0.,1.,0.));
#116823=DIRECTION('center_axis',(0.120708341042269,-0.992688015643799,0.));
#116824=DIRECTION('ref_axis',(0.992688015643799,0.120708341042269,0.));
#116825=DIRECTION('center_axis',(1.78485500480727E-31,2.58019156504489E-46,
-1.));
#116826=DIRECTION('ref_axis',(-1.44560289664734E-15,1.,-3.88938454866321E-62));
#116827=DIRECTION('center_axis',(0.,0.,1.));
#116828=DIRECTION('ref_axis',(0.,1.,0.));
#116829=DIRECTION('center_axis',(0.,1.23467863058847E-16,-1.));
#116830=DIRECTION('ref_axis',(0.,1.,0.));
#116831=DIRECTION('center_axis',(0.635568809204587,-0.77204422720869,0.));
#116832=DIRECTION('ref_axis',(0.77204422720869,0.635568809204587,0.));
#116833=DIRECTION('center_axis',(6.57968948972152E-31,3.50636292785902E-45,
-1.));
#116834=DIRECTION('ref_axis',(-5.32907051820075E-15,1.,-4.3561106945028E-60));
#116835=DIRECTION('center_axis',(0.,0.,1.));
#116836=DIRECTION('ref_axis',(0.,1.,0.));
#116837=DIRECTION('center_axis',(0.,1.23467863058847E-16,-1.));
#116838=DIRECTION('ref_axis',(-0.0361435302645206,-0.999346609150208,0.));
#116839=DIRECTION('center_axis',(0.689680595319753,0.724113717892011,0.));
#116840=DIRECTION('ref_axis',(-0.724113717892011,0.689680595319753,0.));
#116841=DIRECTION('center_axis',(1.78485500480727E-31,2.58019156504489E-46,
-1.));
#116842=DIRECTION('ref_axis',(-1.44560289664734E-15,1.,-3.88938454866321E-62));
#116843=DIRECTION('center_axis',(0.,0.,1.));
#116844=DIRECTION('ref_axis',(0.,1.,0.));
#116845=DIRECTION('center_axis',(-0.689680595319751,-0.724113717892013,
-8.9404773359724E-17));
#116846=DIRECTION('ref_axis',(-0.724113717892013,0.689680595319751,4.19197973383322E-33));
#116847=DIRECTION('center_axis',(0.689680595319753,0.724113717892011,0.));
#116848=DIRECTION('ref_axis',(-0.724113717892011,0.689680595319753,0.));
#116849=DIRECTION('',(-0.689680595319751,-0.724113717892013,-8.9404773359724E-17));
#116850=DIRECTION('',(0.689680595319751,0.724113717892013,8.9404773359724E-17));
#116851=DIRECTION('center_axis',(0.,1.23467863058847E-16,-1.));
#116852=DIRECTION('ref_axis',(0.,1.,0.));
#116853=DIRECTION('center_axis',(-8.92427502403635E-32,6.45047891261222E-47,
-1.));
#116854=DIRECTION('ref_axis',(7.2280144832367E-16,1.,-6.80642296016062E-62));
#116855=DIRECTION('center_axis',(0.,0.,1.));
#116856=DIRECTION('ref_axis',(0.,1.,0.));
#116857=DIRECTION('center_axis',(0.,1.23467863058847E-16,-1.));
#116858=DIRECTION('ref_axis',(0.,1.,0.));
#116859=DIRECTION('center_axis',(1.92747052886312E-15,1.,0.));
#116860=DIRECTION('ref_axis',(-1.,1.92747052886312E-15,0.));
#116861=DIRECTION('center_axis',(0.,0.,-1.));
#116862=DIRECTION('ref_axis',(0.,1.,0.));
#116863=DIRECTION('center_axis',(0.,0.,1.));
#116864=DIRECTION('ref_axis',(0.,1.,0.));
#116865=DIRECTION('center_axis',(-6.11546355285877E-17,1.,0.));
#116866=DIRECTION('ref_axis',(0.,0.,1.));
#116867=DIRECTION('center_axis',(0.,1.,0.));
#116868=DIRECTION('ref_axis',(0.,0.,-1.));
#116869=DIRECTION('',(6.11546355285877E-17,-1.,-1.23467863058847E-16));
#116870=DIRECTION('',(-6.11546355285877E-17,1.,1.23467863058847E-16));
#116871=DIRECTION('center_axis',(0.,1.23467863058847E-16,-1.));
#116872=DIRECTION('ref_axis',(0.,1.,0.));
#116873=DIRECTION('center_axis',(0.,0.,-1.));
#116874=DIRECTION('ref_axis',(0.,1.,0.));
#116875=DIRECTION('center_axis',(0.,0.,1.));
#116876=DIRECTION('ref_axis',(0.,1.,0.));
#116877=DIRECTION('center_axis',(-0.992688015643799,-0.120708341042267,
-1.45413606216828E-17));
#116878=DIRECTION('ref_axis',(0.120708341042267,-0.992688015643799,-1.06337197076866E-33));
#116879=DIRECTION('center_axis',(0.,1.23467863058847E-16,-1.));
#116880=DIRECTION('ref_axis',(0.,1.,0.));
#116881=DIRECTION('center_axis',(-0.802069210224766,-0.597231095983306,
0.));
#116882=DIRECTION('ref_axis',(0.597231095983306,-0.802069210224766,0.));
#116883=DIRECTION('center_axis',(8.77291931962869E-31,6.2335340939716E-45,
-1.));
#116884=DIRECTION('ref_axis',(-7.105427357601E-15,1.,-4.97841222228891E-60));
#116885=DIRECTION('center_axis',(0.,0.,1.));
#116886=DIRECTION('ref_axis',(0.,1.,0.));
#116887=DIRECTION('center_axis',(0.,1.23467863058847E-16,-1.));
#116888=DIRECTION('ref_axis',(0.,1.,0.));
#116889=DIRECTION('center_axis',(0.689680595319753,-0.724113717892012,0.));
#116890=DIRECTION('ref_axis',(0.724113717892012,0.689680595319752,0.));
#116891=DIRECTION('center_axis',(0.,0.,-1.));
#116892=DIRECTION('ref_axis',(0.,1.,0.));
#116893=DIRECTION('center_axis',(0.,0.,1.));
#116894=DIRECTION('ref_axis',(0.,1.,0.));
#116895=DIRECTION('center_axis',(-0.68968059531976,0.724113717892004,8.94047733597239E-17));
#116896=DIRECTION('ref_axis',(0.724113717892004,0.68968059531976,-2.34589631629098E-32));
#116897=DIRECTION('center_axis',(0.689680595319752,-0.724113717892012,0.));
#116898=DIRECTION('ref_axis',(0.724113717892012,0.689680595319752,0.));
#116899=DIRECTION('',(-0.689680595319752,0.724113717892012,8.94047733597238E-17));
#116900=DIRECTION('',(0.689680595319752,-0.724113717892012,-8.94047733597238E-17));
#116901=DIRECTION('center_axis',(0.,1.23467863058847E-16,-1.));
#116902=DIRECTION('ref_axis',(-0.0950205176920742,-0.995475314218052,0.));
#116903=DIRECTION('center_axis',(0.,0.,-1.));
#116904=DIRECTION('ref_axis',(0.,1.,0.));
#116905=DIRECTION('center_axis',(0.,0.,1.));
#116906=DIRECTION('ref_axis',(0.,1.,0.));
#116907=DIRECTION('center_axis',(0.,1.23467863058847E-16,-1.));
#116908=DIRECTION('ref_axis',(0.,1.,0.));
#116909=DIRECTION('center_axis',(0.,0.,1.));
#116910=DIRECTION('ref_axis',(0.,1.,0.));
#116911=DIRECTION('center_axis',(-0.689680595319753,-0.724113717892011,
0.));
#116912=DIRECTION('ref_axis',(0.724113717892011,-0.689680595319753,0.));
#116913=DIRECTION('center_axis',(-1.60636950432654E-30,2.08995516768636E-44,
-1.));
#116914=DIRECTION('ref_axis',(1.30104260698261E-14,1.,2.24028550003001E-59));
#116915=DIRECTION('center_axis',(0.689680595319751,0.724113717892013,8.9404773359724E-17));
#116916=DIRECTION('ref_axis',(0.724113717892013,-0.689680595319751,-4.19197973383322E-33));
#116917=DIRECTION('center_axis',(-0.689680595319752,-0.724113717892012,
0.));
#116918=DIRECTION('ref_axis',(0.724113717892012,-0.689680595319752,0.));
#116919=DIRECTION('',(0.689680595319751,0.724113717892013,8.9404773359724E-17));
#116920=DIRECTION('',(-0.689680595319751,-0.724113717892013,-8.9404773359724E-17));
#116921=DIRECTION('center_axis',(0.,1.23467863058847E-16,-1.));
#116922=DIRECTION('ref_axis',(0.,1.,0.));
#116923=DIRECTION('center_axis',(0.802069210224767,-0.597231095983305,0.));
#116924=DIRECTION('ref_axis',(0.597231095983305,0.802069210224766,0.));
#116925=DIRECTION('center_axis',(0.,0.,-1.));
#116926=DIRECTION('ref_axis',(0.,1.,0.));
#116927=DIRECTION('center_axis',(0.,0.,1.));
#116928=DIRECTION('ref_axis',(0.,1.,0.));
#116929=DIRECTION('center_axis',(0.,1.23467863058847E-16,-1.));
#116930=DIRECTION('ref_axis',(0.,1.,0.));
#116931=DIRECTION('center_axis',(0.992688015643799,-0.120708341042267,0.));
#116932=DIRECTION('ref_axis',(0.120708341042267,0.992688015643799,0.));
#116933=DIRECTION('center_axis',(0.,0.,-1.));
#116934=DIRECTION('ref_axis',(0.,1.,0.));
#116935=DIRECTION('center_axis',(0.,0.,1.));
#116936=DIRECTION('ref_axis',(0.,1.,0.));
#116937=DIRECTION('center_axis',(0.,1.23467863058847E-16,-1.));
#116938=DIRECTION('ref_axis',(0.663057938251906,-0.748568080084325,0.));
#116939=DIRECTION('center_axis',(0.,1.,0.));
#116940=DIRECTION('ref_axis',(0.,0.,-1.));
#116941=DIRECTION('center_axis',(0.,0.,-1.));
#116942=DIRECTION('ref_axis',(0.,1.,0.));
#116943=DIRECTION('center_axis',(0.,0.,1.));
#116944=DIRECTION('ref_axis',(0.,1.,0.));
#116945=DIRECTION('center_axis',(-6.11546355285877E-17,1.,0.));
#116946=DIRECTION('ref_axis',(0.,0.,1.));
#116947=DIRECTION('center_axis',(0.,1.,0.));
#116948=DIRECTION('ref_axis',(0.,0.,-1.));
#116949=DIRECTION('',(6.11546355285877E-17,-1.,-1.23467863058847E-16));
#116950=DIRECTION('',(-6.11546355285877E-17,1.,1.23467863058847E-16));
#116951=DIRECTION('center_axis',(0.,1.23467863058847E-16,-1.));
#116952=DIRECTION('ref_axis',(0.,1.,0.));
#116953=DIRECTION('center_axis',(-2.23106875600908E-31,4.03154932038264E-46,
-1.));
#116954=DIRECTION('ref_axis',(1.80700362080917E-15,1.,2.33363072919793E-61));
#116955=DIRECTION('center_axis',(0.,0.,1.));
#116956=DIRECTION('ref_axis',(0.,1.,0.));
#116957=DIRECTION('center_axis',(0.,-1.23467863058847E-16,1.));
#116958=DIRECTION('ref_axis',(0.,-1.,0.));
#116959=DIRECTION('center_axis',(-0.777162624242383,-0.6292998136665,-1.36800580655942E-15));
#116960=DIRECTION('ref_axis',(0.6292998136665,-0.777162624242383,-6.36525986617897E-32));
#116961=DIRECTION('center_axis',(-7.93261518924905E-31,5.09657996678154E-45,
-1.));
#116962=DIRECTION('ref_axis',(6.42484205421795E-15,1.,4.3561106945028E-60));
#116963=DIRECTION('center_axis',(-0.982297019165463,-0.187330099393146,
-5.41061232187394E-15));
#116964=DIRECTION('ref_axis',(0.187330099393146,-0.982297019165463,5.34128931770042E-31));
#116965=DIRECTION('center_axis',(0.,0.,1.));
#116966=DIRECTION('ref_axis',(0.,-1.,0.));
#116967=DIRECTION('center_axis',(0.,-1.23467863058847E-16,1.));
#116968=DIRECTION('ref_axis',(0.,-1.,0.));
#116969=DIRECTION('center_axis',(-0.6350303583426,-0.772487180465326,0.));
#116970=DIRECTION('ref_axis',(0.772487180465326,-0.6350303583426,0.));
#116971=DIRECTION('center_axis',(-3.28984474486076E-31,8.76590731964757E-46,
-1.));
#116972=DIRECTION('ref_axis',(2.66453525910037E-15,1.,-6.22301527786114E-61));
#116973=DIRECTION('center_axis',(0.,0.,1.));
#116974=DIRECTION('ref_axis',(0.,-1.,0.));
#116975=DIRECTION('center_axis',(0.,-1.23467863058847E-16,1.));
#116976=DIRECTION('ref_axis',(0.,-1.,0.));
#116977=DIRECTION('center_axis',(-0.0394959395290685,-0.999219730970479,
7.30821690739571E-16));
#116978=DIRECTION('ref_axis',(0.999219730970479,-0.0394959395290685,1.49001220711228E-32));
#116979=DIRECTION('center_axis',(-1.22040233680755E-31,1.206291116398E-46,
-1.));
#116980=DIRECTION('ref_axis',(9.88437239110456E-16,1.,0.));
#116981=DIRECTION('center_axis',(-4.09907119868247E-31,-1.3608711024552E-45,
1.));
#116982=DIRECTION('ref_axis',(3.31994990204759E-15,-1.,-9.33452291679171E-61));
#116983=DIRECTION('center_axis',(0.,-1.23467863058847E-16,1.));
#116984=DIRECTION('ref_axis',(0.,-1.,-1.32864206562206E-16));
#116985=DIRECTION('center_axis',(0.0394959395290708,-0.999219730970479,
0.));
#116986=DIRECTION('ref_axis',(0.999219730970479,0.0394959395290708,0.));
#116987=DIRECTION('center_axis',(2.45193654393607E-31,1.29750229435012E-16,
-1.));
#116988=DIRECTION('ref_axis',(3.90288690140516E-14,1.,1.29750229435012E-16));
#116989=DIRECTION('center_axis',(0.,-1.29932421951445E-16,1.));
#116990=DIRECTION('ref_axis',(0.,-1.,-1.29932421951445E-16));
#116991=DIRECTION('center_axis',(0.,-1.23467863058847E-16,1.));
#116992=DIRECTION('ref_axis',(0.,-1.,0.));
#116993=DIRECTION('center_axis',(0.6350303583426,-0.772487180465326,1.66587444809586E-15));
#116994=DIRECTION('ref_axis',(0.772487180465326,0.6350303583426,9.8727026228538E-31));
#116995=DIRECTION('center_axis',(1.22040233680755E-31,1.20629111639801E-46,
-1.));
#116996=DIRECTION('ref_axis',(-9.88437239110458E-16,1.,-1.75022304689845E-61));
#116997=DIRECTION('center_axis',(3.41589266556873E-31,-9.45049376705E-46,
1.));
#116998=DIRECTION('ref_axis',(-2.766624918373E-15,-1.,6.22301527786114E-61));
#116999=DIRECTION('center_axis',(0.,-1.23467863058847E-16,1.));
#117000=DIRECTION('ref_axis',(0.,-1.,0.));
#117001=DIRECTION('center_axis',(0.77428749071043,-0.632834008037926,-3.58179916610815E-15));
#117002=DIRECTION('ref_axis',(0.632834008037926,0.77428749071043,7.75406439997931E-31));
#117003=DIRECTION('center_axis',(-1.09661491495359E-30,9.73989702183063E-45,
-1.));
#117004=DIRECTION('ref_axis',(8.88178419700125E-15,1.,-2.48920611114446E-60));
#117005=DIRECTION('center_axis',(-3.28984474486076E-31,-8.76590731964757E-46,
1.));
#117006=DIRECTION('ref_axis',(2.66453525910038E-15,-1.,4.66726145839586E-61));
#117007=DIRECTION('center_axis',(0.,-1.23467863058847E-16,1.));
#117008=DIRECTION('ref_axis',(0.,-1.,0.));
#117009=DIRECTION('center_axis',(0.999225121087074,-0.0393593367388569,
7.28294031357568E-16));
#117010=DIRECTION('ref_axis',(0.0393593367388569,0.999225121087074,-1.34329260515414E-32));
#117011=DIRECTION('center_axis',(-2.4408046736151E-31,4.82516446559199E-46,
-1.));
#117012=DIRECTION('ref_axis',(1.97687447822091E-15,1.,-3.11150763893057E-61));
#117013=DIRECTION('center_axis',(6.83178533113742E-31,-3.78019750681997E-45,
1.));
#117014=DIRECTION('ref_axis',(-5.53324983674598E-15,-1.,5.60071375007503E-60));
#117015=DIRECTION('center_axis',(-1.,0.,0.));
#117016=DIRECTION('ref_axis',(0.,-7.86407975776152E-14,-1.));
#117017=DIRECTION('center_axis',(-0.994526788819783,0.10448189469861,1.81517644375859E-14));
#117018=DIRECTION('ref_axis',(-0.10448189469861,-0.994526788819783,-2.86631910367634E-30));
#117019=DIRECTION('center_axis',(-0.993679318607912,-0.112256009954549,
-1.48651952901285E-13));
#117020=DIRECTION('ref_axis',(0.112256009954549,-0.993679318607912,-2.2981091857326E-29));
#117021=DIRECTION('center_axis',(-0.991556456479175,-0.129675724846491,
3.15431192506052E-12));
#117022=DIRECTION('ref_axis',(0.129675724846491,-0.991556456479175,7.41046500628616E-29));
#117023=DIRECTION('center_axis',(0.000137331807541708,-0.00219823298717573,
-0.999997574452913));
#117024=DIRECTION('ref_axis',(-0.11217860466933,0.993685625182725,-0.00219976354633589));
#117025=DIRECTION('center_axis',(-2.53853736684102E-13,2.16212897560678E-12,
1.));
#117026=DIRECTION('ref_axis',(-0.129669785749043,0.991557233176077,-2.17675059075509E-12));
#117027=DIRECTION('center_axis',(-0.858927270467749,-0.512097592307192,
1.49780811271862E-14));
#117028=DIRECTION('ref_axis',(0.512097592307192,-0.858927270467749,-6.01293732495529E-30));
#117029=DIRECTION('center_axis',(-0.536899969302814,-0.843645910890723,
-1.46316605705353E-12));
#117030=DIRECTION('ref_axis',(0.843645910890723,-0.536899969302814,1.20303121328766E-28));
#117031=DIRECTION('center_axis',(-0.040766102180794,-0.99916871694073,-1.55671748522919E-15));
#117032=DIRECTION('ref_axis',(0.99916871694073,-0.040766102180794,-1.4838474346331E-32));
#117033=DIRECTION('center_axis',(-0.0297586090124609,-0.999557114521048,
7.26582357398889E-15));
#117034=DIRECTION('ref_axis',(0.999557114521048,-0.0297586090124609,1.68195404251657E-31));
#117035=DIRECTION('center_axis',(-0.0210932860527463,5.46714727619952E-5,
-0.999777510396452));
#117036=DIRECTION('ref_axis',(-0.998923256585619,0.0413287487753403,0.0210775230292068));
#117037=DIRECTION('center_axis',(0.,0.,1.));
#117038=DIRECTION('ref_axis',(-0.999557147327683,0.0297575070552604,0.));
#117039=DIRECTION('center_axis',(0.233238585379144,-0.972419540265587,4.54398481782876E-15));
#117040=DIRECTION('ref_axis',(0.972419540265587,0.233238585379145,-6.30780798053809E-30));
#117041=DIRECTION('center_axis',(-0.229570335512527,-0.973292073867175,
-1.03212124729447E-14));
#117042=DIRECTION('ref_axis',(0.973292073867175,-0.229570335512527,2.98849951310675E-30));
#117043=DIRECTION('center_axis',(0.0298379862379757,-0.999554748164033,
-8.0054834066732E-15));
#117044=DIRECTION('ref_axis',(0.999554748164032,0.0298379862379757,9.39450193490723E-31));
#117045=DIRECTION('center_axis',(0.0407665603815583,-0.999168698246025,
-4.49007546874249E-14));
#117046=DIRECTION('ref_axis',(0.999168698246025,0.0407665603815583,1.08335075317432E-30));
#117047=DIRECTION('center_axis',(-0.0206791468565618,0.000130026885512925,
-0.999786155124332));
#117048=DIRECTION('ref_axis',(-0.9993253707471,-0.0303600651974135,0.0206656677215903));
#117049=DIRECTION('center_axis',(-5.11490712329098E-12,-1.76010917473445E-13,
1.));
#117050=DIRECTION('ref_axis',(-0.999168739570265,-0.040765547531809,-5.11784665730284E-12));
#117051=DIRECTION('center_axis',(0.536601093577061,-0.843836042351772,2.84249428416013E-15));
#117052=DIRECTION('ref_axis',(0.843836042351772,0.536601093577061,2.98189956073675E-31));
#117053=DIRECTION('center_axis',(0.882960425292266,-0.469447427693135,5.17032777304292E-14));
#117054=DIRECTION('ref_axis',(0.469447427693135,0.882960425292266,-2.22396706740103E-29));
#117055=DIRECTION('center_axis',(0.999360062311266,-0.0357696219888033,
-1.64961351615811E-15));
#117056=DIRECTION('ref_axis',(0.0357696219888033,0.999360062311266,4.316049615934E-32));
#117057=DIRECTION('center_axis',(0.999556853338411,-0.0297673805400138,
-1.82491045181999E-14));
#117058=DIRECTION('ref_axis',(0.0297673805400138,0.999556853338411,-8.47827291376735E-32));
#117059=DIRECTION('center_axis',(1.57626159414375E-5,-0.0233282309877023,
-0.999727859665081));
#117060=DIRECTION('ref_axis',(-0.0363487305279994,-0.999067219538478,0.023312242119934));
#117061=DIRECTION('center_axis',(-3.70157306512969E-13,-1.12910217712061E-11,
1.));
#117062=DIRECTION('ref_axis',(-0.0297644531368429,-0.999556940513878,-1.12970184589887E-11));
#117063=DIRECTION('center_axis',(0.972436723729276,0.233166932352493,0.));
#117064=DIRECTION('ref_axis',(-0.233166932352493,0.972436723729276,0.));
#117065=DIRECTION('center_axis',(-0.635093426738814,0.772416788158568,0.00535207286497078));
#117066=DIRECTION('ref_axis',(-0.77242785121363,-0.635102522959478,9.38368926324323E-20));
#117067=DIRECTION('center_axis',(0.00691691416309599,0.00571143710532978,
0.999959767082982));
#117068=DIRECTION('ref_axis',(-0.755062687525124,-0.655591277438894,0.0089674329312478));
#117069=DIRECTION('center_axis',(-0.563237659270021,0.823253026831934,-0.0708363818393295));
#117070=DIRECTION('ref_axis',(-0.825326289137892,-0.564656104596307,-9.62895252096333E-18));
#117071=DIRECTION('center_axis',(0.507471952069715,0.412437854735,0.756549558088658));
#117072=DIRECTION('ref_axis',(-0.587169164883915,-0.477074009384416,0.653936358814375));
#117073=DIRECTION('center_axis',(-0.341333328819756,-0.277129686002563,
-0.898159615977553));
#117074=DIRECTION('ref_axis',(-0.751460582051474,-0.493539243236486,0.437865286370611));
#117075=DIRECTION('center_axis',(-0.0353652067153621,0.980391286708013,
-0.193861360515669));
#117076=DIRECTION('ref_axis',(3.63487303375728E-18,-0.193982705344839,-0.981004949032928));
#117077=DIRECTION('center_axis',(-0.0385934612262193,0.999254003953662,
-0.00140724310442582));
#117078=DIRECTION('ref_axis',(-0.999254993383049,-0.0385934994402315,-2.19294060248386E-20));
#117079=DIRECTION('center_axis',(0.0149227809046296,-0.000160750066432761,
0.999888636183795));
#117080=DIRECTION('ref_axis',(-0.999085030892015,-0.0400869256955743,0.0149043428496258));
#117081=DIRECTION('center_axis',(0.0362455094603874,-7.24243967428071E-6,
-0.999342915615808));
#117082=DIRECTION('ref_axis',(-0.99884239871172,-0.0316458184758586,-0.036227126698248));
#117083=DIRECTION('center_axis',(-0.460561989867266,-0.543327519921019,
0.701910150650338));
#117084=DIRECTION('ref_axis',(1.68332661555862E-16,0.790771035553874,0.612112056186654));
#117085=DIRECTION('center_axis',(-0.469907551033905,-0.216399115636686,
0.855779361887735));
#117086=DIRECTION('ref_axis',(-0.876549208984677,-2.3138118535155E-14,-0.481312252314792));
#117087=DIRECTION('center_axis',(0.488505761670049,-0.207277391256933,-0.847583744469469));
#117088=DIRECTION('ref_axis',(-0.866400038259138,1.13916389737517E-16,-0.499350551921758));
#117089=DIRECTION('center_axis',(-0.485723325571869,0.464849177451359,0.740262178703059));
#117090=DIRECTION('ref_axis',(0.836086106459356,-1.21161241824207E-16,0.548598234216658));
#117091=DIRECTION('center_axis',(0.0366457249192154,-0.000264295716704561,
-0.999328284895869));
#117092=DIRECTION('ref_axis',(-0.998575905634023,0.0387881617069405,-0.0366283933388643));
#117093=DIRECTION('center_axis',(0.0387718059368437,0.999247421633299,0.00115647031964687));
#117094=DIRECTION('ref_axis',(-0.999248089842511,0.0387718318640339,-1.43119761272989E-20));
#117095=DIRECTION('center_axis',(0.015774878482318,-2.06992946781092E-6,
0.999875568860738));
#117096=DIRECTION('ref_axis',(-0.99934939359657,0.0324376701882913,0.0157666442505599));
#117097=DIRECTION('center_axis',(0.0362051861961663,0.986513040328005,0.159628336316885));
#117098=DIRECTION('ref_axis',(-3.13261606677306E-17,0.159733060933468,-0.987160244967769));
#117099=DIRECTION('center_axis',(0.586558422242651,0.80833932738343,0.0503661503543409));
#117100=DIRECTION('ref_axis',(-0.809366559200372,0.587303816476745,6.0201141129801E-17));
#117101=DIRECTION('center_axis',(0.635108704314869,0.772391525947514,-0.00694725470670599));
#117102=DIRECTION('ref_axis',(-0.772410166108943,0.635124031423434,-3.90764897276796E-18));
#117103=DIRECTION('center_axis',(0.533623207912185,-0.432878874101261,0.726541225488501));
#117104=DIRECTION('ref_axis',(-0.613440310270918,0.393261638349251,0.684862226683281));
#117105=DIRECTION('center_axis',(-0.367164830643458,0.297433524522046,-0.88131906006222));
#117106=DIRECTION('ref_axis',(-0.67960514144709,0.561137496245174,0.472505621158498));
#117107=DIRECTION('center_axis',(0.00311221115432024,-0.00394761201357374,
0.999987365170741));
#117108=DIRECTION('ref_axis',(-0.641176102355285,-0.767393078417564,-0.0010339077811091));
#117109=DIRECTION('center_axis',(0.119709524432718,0.500158371272784,-0.857619515522967));
#117110=DIRECTION('ref_axis',(-5.19703601812987E-17,-0.863831361964004,
-0.503781081510029));
#117111=DIRECTION('center_axis',(-0.501099625553759,-0.466384922602348,
0.728961088974634));
#117112=DIRECTION('ref_axis',(0.824074180962238,-2.20209609654532E-16,0.566481901097834));
#117113=DIRECTION('center_axis',(-0.089444411535165,0.865796085392892,0.492338131535099));
#117114=DIRECTION('ref_axis',(0.983291169652569,0.155450651542661,-0.0947289323187182));
#117115=DIRECTION('center_axis',(-0.254850131470821,0.841789549783716,0.475858975290195));
#117116=DIRECTION('ref_axis',(-0.487493726574647,-0.536841697226028,0.688586130175333));
#117117=DIRECTION('center_axis',(-2.30425867295841E-5,0.030784145628616,
-0.999526055611836));
#117118=DIRECTION('ref_axis',(-0.0383802756263916,-0.99878963808956,-0.0307605800947844));
#117119=DIRECTION('center_axis',(-0.999263201609641,0.0383614667420372,
0.00120489761000603));
#117120=DIRECTION('ref_axis',(-0.0383614945882391,-0.999263926964722,2.87536200646804E-20));
#117121=DIRECTION('center_axis',(-4.00197585461019E-5,0.0159615005705134,
0.999872606334405));
#117122=DIRECTION('ref_axis',(-0.0321201706221352,-0.999356707583681,0.0159519793978996));
#117123=DIRECTION('center_axis',(-0.974363720155827,0.0344964635874725,
0.222318093829667));
#117124=DIRECTION('ref_axis',(0.222450491940089,1.26241972147447E-18,0.974943987434977));
#117125=DIRECTION('center_axis',(-0.836810598831192,0.541308500745221,0.0820556439542334));
#117126=DIRECTION('ref_axis',(-0.543140105176027,-0.839642082169167,1.69471490770742E-17));
#117127=DIRECTION('center_axis',(-0.774120577489127,0.632943886852024,-0.0109255482495788));
#117128=DIRECTION('ref_axis',(-0.632981666732123,-0.774166784085331,5.39501067277511E-19));
#117129=DIRECTION('center_axis',(-0.266671211339203,-0.334921826443821,
-0.903722211309657));
#117130=DIRECTION('ref_axis',(-0.574038792157477,-0.698019134436299,0.428075639413392));
#117131=DIRECTION('center_axis',(0.0102380851882465,0.0116065194865278,
0.999880227985876));
#117132=DIRECTION('ref_axis',(0.775942434655157,-0.630803416456049,-0.000622807196781762));
#117133=DIRECTION('center_axis',(-1.07824096236302E-8,-0.998305357148899,
-0.0581929023834511));
#117134=DIRECTION('ref_axis',(0.,0.058192902383451,-0.998305357148899));
#117135=DIRECTION('center_axis',(-1.,0.,0.));
#117136=DIRECTION('ref_axis',(0.,-6.93889390390722E-15,-1.));
#117137=DIRECTION('center_axis',(-2.31017521133305E-9,0.986382705137784,
0.164466285314247));
#117138=DIRECTION('ref_axis',(0.99999903088274,0.000228972993696964,-0.00137324613565508));
#117139=DIRECTION('center_axis',(-0.99999635393917,-0.000157155077313813,
0.00269581354111146));
#117140=DIRECTION('ref_axis',(0.00269581357440168,1.24619272072387E-21,
0.999996366287984));
#117141=DIRECTION('center_axis',(-8.12532577157186E-9,-0.998207006171548,
-0.0598562680931181));
#117142=DIRECTION('ref_axis',(0.999311726713681,0.00222038745151431,-0.0370289445175939));
#117143=DIRECTION('center_axis',(0.244344449131117,-0.492606745559265,-0.835245104390514));
#117144=DIRECTION('ref_axis',(-4.32889927015855E-17,-0.86135403585069,0.508005142615435));
#117145=DIRECTION('center_axis',(-0.982994797178248,-0.183632204703407,
0.000664918236953841));
#117146=DIRECTION('ref_axis',(0.183632245296812,-0.982995014477312,5.7655403569157E-20));
#117147=DIRECTION('center_axis',(0.000179526560883581,-0.00456486630691949,
-0.999989564828461));
#117148=DIRECTION('ref_axis',(0.986444685005576,0.164093132907876,-0.000571976160476437));
#117149=DIRECTION('center_axis',(0.330813257101916,0.830741130674896,-0.447696060660149));
#117150=DIRECTION('ref_axis',(-0.932375699002072,0.214461635172499,-0.291001310906903));
#117151=DIRECTION('center_axis',(-0.433391148275503,0.470797811534069,0.768453989026781));
#117152=DIRECTION('ref_axis',(8.06979081629128E-16,0.852695228537141,-0.522408697506075));
#117153=DIRECTION('center_axis',(-0.96720597488598,-0.18129103740974,0.177893681449798));
#117154=DIRECTION('ref_axis',(0.184229551589837,-0.982883244501099,1.61805378326746E-17));
#117155=DIRECTION('center_axis',(-0.831503844166329,-0.548952032819844,
0.0851646804701234));
#117156=DIRECTION('ref_axis',(0.550953708881667,-0.834535805504794,3.15287181374443E-17));
#117157=DIRECTION('center_axis',(-0.777065025633406,-0.629380269512156,
-0.00710086516978589));
#117158=DIRECTION('ref_axis',(0.62939613750826,-0.777084617071837,1.0927692862107E-18));
#117159=DIRECTION('center_axis',(-0.295452400444952,0.370381022938362,-0.880639413675341));
#117160=DIRECTION('ref_axis',(-0.467331061476171,0.747944548358106,0.471360405168853));
#117161=DIRECTION('center_axis',(0.429530667833731,-0.537702321291583,0.725520240288272));
#117162=DIRECTION('ref_axis',(-0.451971122885174,0.567540558793691,0.68820042008274));
#117163=DIRECTION('center_axis',(0.,0.,-1.));
#117164=DIRECTION('ref_axis',(0.,1.,0.));
#117165=DIRECTION('center_axis',(0.,0.,1.));
#117166=DIRECTION('ref_axis',(0.,1.,0.));
#117167=DIRECTION('',(0.,1.23467863058847E-16,-1.));
#117168=DIRECTION('',(3.82498197630791E-33,-1.23467863058847E-16,1.));
#117169=DIRECTION('center_axis',(0.,0.,-1.));
#117170=DIRECTION('ref_axis',(0.,1.,0.));
#117171=DIRECTION('',(0.,-1.23467863058847E-16,1.));
#117172=DIRECTION('center_axis',(0.,0.,1.));
#117173=DIRECTION('ref_axis',(0.,1.,0.));
#117174=DIRECTION('',(0.,1.23467863058847E-16,-1.));
#117175=DIRECTION('center_axis',(0.,0.,-1.));
#117176=DIRECTION('ref_axis',(0.,1.,0.));
#117177=DIRECTION('',(0.,-1.23467863058847E-16,1.));
#117178=DIRECTION('center_axis',(0.,0.,1.));
#117179=DIRECTION('ref_axis',(0.,1.,0.));
#117180=DIRECTION('',(0.,1.23467863058847E-16,-1.));
#117181=DIRECTION('center_axis',(0.,0.,-1.));
#117182=DIRECTION('ref_axis',(0.,1.,0.));
#117183=DIRECTION('',(0.,-1.23467863058847E-16,1.));
#117184=DIRECTION('center_axis',(0.,0.,1.));
#117185=DIRECTION('ref_axis',(0.,1.,0.));
#117186=DIRECTION('',(0.,1.23467863058847E-16,-1.));
#117187=DIRECTION('center_axis',(0.,0.,-1.));
#117188=DIRECTION('ref_axis',(0.,1.,0.));
#117189=DIRECTION('',(0.,-1.23467863058847E-16,1.));
#117190=DIRECTION('center_axis',(0.,0.,1.));
#117191=DIRECTION('ref_axis',(0.,1.,0.));
#117192=DIRECTION('',(0.,1.23467863058847E-16,-1.));
#117193=DIRECTION('center_axis',(0.,0.,-1.));
#117194=DIRECTION('ref_axis',(0.,1.,0.));
#117195=DIRECTION('',(0.,-1.23467863058847E-16,1.));
#117196=DIRECTION('center_axis',(0.,0.,1.));
#117197=DIRECTION('ref_axis',(0.,1.,0.));
#117198=DIRECTION('',(0.,1.23467863058847E-16,-1.));
#117199=DIRECTION('center_axis',(0.,0.,-1.));
#117200=DIRECTION('ref_axis',(0.,1.,0.));
#117201=DIRECTION('',(0.,-1.23467863058847E-16,1.));
#117202=DIRECTION('center_axis',(0.,0.,1.));
#117203=DIRECTION('ref_axis',(0.,1.,0.));
#117204=DIRECTION('',(-1.27503726478586E-32,1.23467863058847E-16,-1.));
#117205=DIRECTION('center_axis',(0.,0.,-1.));
#117206=DIRECTION('ref_axis',(-0.0950205176920726,-0.995475314218053,0.));
#117207=DIRECTION('',(0.,-1.23467863058847E-16,1.));
#117208=DIRECTION('center_axis',(0.,0.,1.));
#117209=DIRECTION('ref_axis',(0.,1.,0.));
#117210=DIRECTION('',(0.,1.23467863058847E-16,-1.));
#117211=DIRECTION('center_axis',(0.,0.,-1.));
#117212=DIRECTION('ref_axis',(0.,1.,0.));
#117213=DIRECTION('',(0.,-1.23467863058847E-16,1.));
#117214=DIRECTION('center_axis',(0.,0.,1.));
#117215=DIRECTION('ref_axis',(0.,1.,0.));
#117216=DIRECTION('',(0.,1.23467863058847E-16,-1.));
#117217=DIRECTION('center_axis',(0.,0.,-1.));
#117218=DIRECTION('ref_axis',(0.,1.,0.));
#117219=DIRECTION('center_axis',(0.,0.,1.));
#117220=DIRECTION('ref_axis',(0.,1.,0.));
#117221=DIRECTION('',(0.,1.23467863058847E-16,-1.));
#117222=DIRECTION('',(0.,-1.23467863058847E-16,1.));
#117223=DIRECTION('center_axis',(0.,0.,-1.));
#117224=DIRECTION('ref_axis',(0.,1.,0.));
#117225=DIRECTION('',(0.,-1.23467863058847E-16,1.));
#117226=DIRECTION('center_axis',(0.,0.,1.));
#117227=DIRECTION('ref_axis',(0.,1.,0.));
#117228=DIRECTION('',(0.,1.23467863058847E-16,-1.));
#117229=DIRECTION('center_axis',(-1.3684555315672E-48,0.,1.));
#117230=DIRECTION('ref_axis',(0.,-1.,0.));
#117231=DIRECTION('',(0.,-1.23467863058847E-16,1.));
#117232=DIRECTION('center_axis',(0.,0.,1.));
#117233=DIRECTION('ref_axis',(0.,1.,0.));
#117234=DIRECTION('',(1.3684555315672E-48,1.23467863058847E-16,-1.));
#117235=DIRECTION('center_axis',(0.,0.,-1.));
#117236=DIRECTION('ref_axis',(0.,1.,0.));
#117237=DIRECTION('',(0.,-1.23467863058847E-16,1.));
#117238=DIRECTION('center_axis',(0.,0.,1.));
#117239=DIRECTION('ref_axis',(0.,1.,0.));
#117240=DIRECTION('',(0.,1.23467863058847E-16,-1.));
#117241=DIRECTION('center_axis',(0.,0.,1.));
#117242=DIRECTION('ref_axis',(0.,-1.,0.));
#117243=DIRECTION('',(0.,-1.23467863058847E-16,1.));
#117244=DIRECTION('center_axis',(0.,0.,1.));
#117245=DIRECTION('ref_axis',(0.,1.,0.));
#117246=DIRECTION('',(0.,1.23467863058847E-16,-1.));
#117247=DIRECTION('center_axis',(0.,0.,-1.));
#117248=DIRECTION('ref_axis',(0.,1.,0.));
#117249=DIRECTION('',(0.,-1.23467863058847E-16,1.));
#117250=DIRECTION('center_axis',(0.,0.,1.));
#117251=DIRECTION('ref_axis',(0.,1.,0.));
#117252=DIRECTION('',(0.,1.23467863058847E-16,-1.));
#117253=DIRECTION('center_axis',(0.,0.,-1.));
#117254=DIRECTION('ref_axis',(0.,1.,0.));
#117255=DIRECTION('',(0.,-1.23467863058847E-16,1.));
#117256=DIRECTION('center_axis',(0.,0.,1.));
#117257=DIRECTION('ref_axis',(0.,1.,0.));
#117258=DIRECTION('',(0.,1.23467863058847E-16,-1.));
#117259=DIRECTION('center_axis',(0.,0.,1.));
#117260=DIRECTION('ref_axis',(0.,-1.,0.));
#117261=DIRECTION('',(0.,-1.23467863058847E-16,1.));
#117262=DIRECTION('center_axis',(0.,0.,1.));
#117263=DIRECTION('ref_axis',(0.,1.,0.));
#117264=DIRECTION('',(0.,1.23467863058847E-16,-1.));
#117265=DIRECTION('center_axis',(1.3684555315672E-48,0.,-1.));
#117266=DIRECTION('ref_axis',(0.,1.,0.));
#117267=DIRECTION('',(-1.3684555315672E-48,-1.23467863058847E-16,1.));
#117268=DIRECTION('center_axis',(0.,0.,1.));
#117269=DIRECTION('ref_axis',(0.,1.,0.));
#117270=DIRECTION('',(0.,1.23467863058847E-16,-1.));
#117271=DIRECTION('center_axis',(0.,0.,-1.));
#117272=DIRECTION('ref_axis',(-0.686617021913642,-0.727019301819726,0.));
#117273=DIRECTION('',(0.,-1.23467863058847E-16,1.));
#117274=DIRECTION('center_axis',(0.,0.,1.));
#117275=DIRECTION('ref_axis',(0.,1.,0.));
#117276=DIRECTION('',(0.,1.23467863058847E-16,-1.));
#117277=DIRECTION('center_axis',(0.,0.,1.));
#117278=DIRECTION('ref_axis',(0.,-1.,0.));
#117279=DIRECTION('',(0.,-1.23467863058847E-16,1.));
#117280=DIRECTION('center_axis',(0.,0.,1.));
#117281=DIRECTION('ref_axis',(0.,1.,0.));
#117282=DIRECTION('',(0.,1.23467863058847E-16,-1.));
#117283=DIRECTION('center_axis',(0.,0.,-1.));
#117284=DIRECTION('ref_axis',(0.,1.,0.));
#117285=DIRECTION('',(0.,-1.23467863058847E-16,1.));
#117286=DIRECTION('center_axis',(0.,0.,1.));
#117287=DIRECTION('ref_axis',(0.,1.,0.));
#117288=DIRECTION('',(0.,1.23467863058847E-16,-1.));
#117289=DIRECTION('center_axis',(0.,0.,-1.));
#117290=DIRECTION('ref_axis',(0.,1.,0.));
#117291=DIRECTION('',(0.,-1.23467863058847E-16,1.));
#117292=DIRECTION('center_axis',(0.,0.,1.));
#117293=DIRECTION('ref_axis',(0.,1.,0.));
#117294=DIRECTION('',(0.,1.23467863058847E-16,-1.));
#117295=DIRECTION('center_axis',(0.,0.,-1.));
#117296=DIRECTION('ref_axis',(0.,1.,0.));
#117297=DIRECTION('',(0.,-1.23467863058847E-16,1.));
#117298=DIRECTION('center_axis',(0.,0.,1.));
#117299=DIRECTION('ref_axis',(0.,1.,0.));
#117300=DIRECTION('',(0.,1.23467863058847E-16,-1.));
#117301=DIRECTION('center_axis',(0.,0.,1.));
#117302=DIRECTION('ref_axis',(0.,-1.,0.));
#117303=DIRECTION('',(0.,-1.23467863058847E-16,1.));
#117304=DIRECTION('center_axis',(0.,0.,1.));
#117305=DIRECTION('ref_axis',(0.,1.,0.));
#117306=DIRECTION('',(0.,1.23467863058847E-16,-1.));
#117307=DIRECTION('center_axis',(0.,0.,-1.));
#117308=DIRECTION('ref_axis',(0.,1.,0.));
#117309=DIRECTION('',(0.,-1.23467863058847E-16,1.));
#117310=DIRECTION('center_axis',(0.,0.,1.));
#117311=DIRECTION('ref_axis',(0.,1.,0.));
#117312=DIRECTION('',(0.,1.23467863058847E-16,-1.));
#117313=DIRECTION('center_axis',(0.,0.,1.));
#117314=DIRECTION('ref_axis',(0.,-1.,0.));
#117315=DIRECTION('',(0.,-1.23467863058847E-16,1.));
#117316=DIRECTION('center_axis',(0.,0.,1.));
#117317=DIRECTION('ref_axis',(0.,1.,0.));
#117318=DIRECTION('',(0.,1.23467863058847E-16,-1.));
#117319=DIRECTION('center_axis',(0.,0.,-1.));
#117320=DIRECTION('ref_axis',(0.,1.,0.));
#117321=DIRECTION('',(0.,-1.23467863058847E-16,1.));
#117322=DIRECTION('center_axis',(0.,0.,1.));
#117323=DIRECTION('ref_axis',(0.,1.,0.));
#117324=DIRECTION('',(0.,1.23467863058847E-16,-1.));
#117325=DIRECTION('center_axis',(0.,0.,-1.));
#117326=DIRECTION('ref_axis',(0.,1.,0.));
#117327=DIRECTION('center_axis',(0.,0.,1.));
#117328=DIRECTION('ref_axis',(0.,1.,0.));
#117329=DIRECTION('',(0.,1.23467863058847E-16,-1.));
#117330=DIRECTION('',(0.,-1.23467863058847E-16,1.));
#117331=DIRECTION('center_axis',(0.,0.,1.));
#117332=DIRECTION('ref_axis',(0.,-1.,0.));
#117333=DIRECTION('',(0.,-1.23467863058847E-16,1.));
#117334=DIRECTION('center_axis',(0.,0.,1.));
#117335=DIRECTION('ref_axis',(0.,1.,0.));
#117336=DIRECTION('',(0.,1.23467863058847E-16,-1.));
#117337=DIRECTION('center_axis',(0.,0.,-1.));
#117338=DIRECTION('ref_axis',(0.,1.,0.));
#117339=DIRECTION('',(0.,-1.23467863058847E-16,1.));
#117340=DIRECTION('center_axis',(0.,0.,1.));
#117341=DIRECTION('ref_axis',(0.,1.,0.));
#117342=DIRECTION('',(0.,1.23467863058847E-16,-1.));
#117343=DIRECTION('center_axis',(0.,0.,1.));
#117344=DIRECTION('ref_axis',(0.,-1.,0.));
#117345=DIRECTION('',(0.,-1.23467863058847E-16,1.));
#117346=DIRECTION('center_axis',(0.,0.,1.));
#117347=DIRECTION('ref_axis',(0.,1.,0.));
#117348=DIRECTION('',(0.,1.23467863058847E-16,-1.));
#117349=DIRECTION('center_axis',(0.,0.,-1.));
#117350=DIRECTION('ref_axis',(0.,1.,0.));
#117351=DIRECTION('',(0.,-1.23467863058847E-16,1.));
#117352=DIRECTION('center_axis',(0.,0.,1.));
#117353=DIRECTION('ref_axis',(0.,1.,0.));
#117354=DIRECTION('',(0.,1.23467863058847E-16,-1.));
#117355=DIRECTION('center_axis',(0.,0.,1.));
#117356=DIRECTION('ref_axis',(0.,-1.,0.));
#117357=DIRECTION('',(0.,-1.23467863058847E-16,1.));
#117358=DIRECTION('center_axis',(0.,0.,1.));
#117359=DIRECTION('ref_axis',(0.,1.,0.));
#117360=DIRECTION('',(0.,1.23467863058847E-16,-1.));
#117361=DIRECTION('center_axis',(0.,0.,-1.));
#117362=DIRECTION('ref_axis',(0.,1.,0.));
#117363=DIRECTION('',(0.,-1.23467863058847E-16,1.));
#117364=DIRECTION('center_axis',(0.,0.,1.));
#117365=DIRECTION('ref_axis',(0.,1.,0.));
#117366=DIRECTION('',(0.,1.23467863058847E-16,-1.));
#117367=DIRECTION('center_axis',(0.,0.,1.));
#117368=DIRECTION('ref_axis',(0.,-1.,0.));
#117369=DIRECTION('',(0.,-1.23467863058847E-16,1.));
#117370=DIRECTION('center_axis',(0.,0.,1.));
#117371=DIRECTION('ref_axis',(0.,1.,0.));
#117372=DIRECTION('',(0.,1.23467863058847E-16,-1.));
#117373=DIRECTION('center_axis',(0.,0.,-1.));
#117374=DIRECTION('ref_axis',(0.,1.,0.));
#117375=DIRECTION('',(0.,-1.23467863058847E-16,1.));
#117376=DIRECTION('center_axis',(0.,0.,1.));
#117377=DIRECTION('ref_axis',(0.,1.,0.));
#117378=DIRECTION('',(0.,1.23467863058847E-16,-1.));
#117379=DIRECTION('center_axis',(0.,0.,1.));
#117380=DIRECTION('ref_axis',(0.,-1.,0.));
#117381=DIRECTION('',(0.,-1.23467863058847E-16,1.));
#117382=DIRECTION('center_axis',(0.,0.,1.));
#117383=DIRECTION('ref_axis',(0.,1.,0.));
#117384=DIRECTION('',(0.,1.23467863058847E-16,-1.));
#117385=DIRECTION('center_axis',(0.,0.,-1.));
#117386=DIRECTION('ref_axis',(0.,1.,0.));
#117387=DIRECTION('',(0.,-1.23467863058847E-16,1.));
#117388=DIRECTION('center_axis',(0.,0.,1.));
#117389=DIRECTION('ref_axis',(0.,1.,0.));
#117390=DIRECTION('',(0.,1.23467863058847E-16,-1.));
#117391=DIRECTION('center_axis',(0.,0.,-1.));
#117392=DIRECTION('ref_axis',(0.695782815675814,-0.718252235228151,0.));
#117393=DIRECTION('',(0.,-1.23467863058847E-16,1.));
#117394=DIRECTION('center_axis',(0.,0.,1.));
#117395=DIRECTION('ref_axis',(0.,1.,0.));
#117396=DIRECTION('',(0.,1.23467863058847E-16,-1.));
#117397=DIRECTION('center_axis',(0.,0.,-1.));
#117398=DIRECTION('ref_axis',(0.,1.,0.));
#117399=DIRECTION('',(0.,-1.23467863058847E-16,1.));
#117400=DIRECTION('center_axis',(0.,0.,1.));
#117401=DIRECTION('ref_axis',(0.,1.,0.));
#117402=DIRECTION('',(0.,1.23467863058847E-16,-1.));
#117403=DIRECTION('center_axis',(0.,0.,1.));
#117404=DIRECTION('ref_axis',(0.,-1.,0.));
#117405=DIRECTION('',(0.,-1.23467863058847E-16,1.));
#117406=DIRECTION('center_axis',(0.,0.,1.));
#117407=DIRECTION('ref_axis',(0.,1.,0.));
#117408=DIRECTION('',(0.,1.23467863058847E-16,-1.));
#117409=DIRECTION('center_axis',(0.,0.,-1.));
#117410=DIRECTION('ref_axis',(0.,1.,0.));
#117411=DIRECTION('',(0.,-1.23467863058847E-16,1.));
#117412=DIRECTION('center_axis',(0.,0.,1.));
#117413=DIRECTION('ref_axis',(0.,1.,0.));
#117414=DIRECTION('',(0.,1.23467863058847E-16,-1.));
#117415=DIRECTION('center_axis',(0.,0.,-1.));
#117416=DIRECTION('ref_axis',(0.,1.,0.));
#117417=DIRECTION('',(0.,-1.23467863058847E-16,1.));
#117418=DIRECTION('center_axis',(0.,0.,1.));
#117419=DIRECTION('ref_axis',(0.,1.,0.));
#117420=DIRECTION('',(0.,1.23467863058847E-16,-1.));
#117421=DIRECTION('center_axis',(0.,0.,-1.));
#117422=DIRECTION('ref_axis',(0.,1.,0.));
#117423=DIRECTION('',(0.,-1.23467863058847E-16,1.));
#117424=DIRECTION('center_axis',(0.,0.,1.));
#117425=DIRECTION('ref_axis',(0.,1.,0.));
#117426=DIRECTION('',(0.,1.23467863058847E-16,-1.));
#117427=DIRECTION('center_axis',(0.,0.,1.));
#117428=DIRECTION('ref_axis',(0.,-1.,0.));
#117429=DIRECTION('',(0.,-1.23467863058847E-16,1.));
#117430=DIRECTION('center_axis',(0.,0.,1.));
#117431=DIRECTION('ref_axis',(0.,1.,0.));
#117432=DIRECTION('',(0.,1.23467863058847E-16,-1.));
#117433=DIRECTION('center_axis',(0.,0.,-1.));
#117434=DIRECTION('ref_axis',(0.,1.,0.));
#117435=DIRECTION('',(0.,-1.23467863058847E-16,1.));
#117436=DIRECTION('center_axis',(0.,0.,1.));
#117437=DIRECTION('ref_axis',(0.,1.,0.));
#117438=DIRECTION('',(0.,1.23467863058847E-16,-1.));
#117439=DIRECTION('center_axis',(0.,0.,1.));
#117440=DIRECTION('ref_axis',(0.,-1.,0.));
#117441=DIRECTION('',(0.,-1.23467863058847E-16,1.));
#117442=DIRECTION('center_axis',(0.,0.,1.));
#117443=DIRECTION('ref_axis',(0.,1.,0.));
#117444=DIRECTION('',(0.,1.23467863058847E-16,-1.));
#117445=DIRECTION('center_axis',(0.,0.,-1.));
#117446=DIRECTION('ref_axis',(0.,1.,0.));
#117447=DIRECTION('',(0.,-1.23467863058847E-16,1.));
#117448=DIRECTION('center_axis',(0.,0.,1.));
#117449=DIRECTION('ref_axis',(0.,1.,0.));
#117450=DIRECTION('',(0.,1.23467863058847E-16,-1.));
#117451=DIRECTION('center_axis',(0.,0.,1.));
#117452=DIRECTION('ref_axis',(0.,-1.,0.));
#117453=DIRECTION('',(0.,-1.23467863058847E-16,1.));
#117454=DIRECTION('center_axis',(0.,0.,1.));
#117455=DIRECTION('ref_axis',(0.,1.,0.));
#117456=DIRECTION('',(0.,1.23467863058847E-16,-1.));
#117457=DIRECTION('center_axis',(0.,0.,-1.));
#117458=DIRECTION('ref_axis',(0.,1.,0.));
#117459=DIRECTION('',(0.,-1.23467863058847E-16,1.));
#117460=DIRECTION('center_axis',(0.,0.,1.));
#117461=DIRECTION('ref_axis',(0.,1.,0.));
#117462=DIRECTION('',(0.,1.23467863058847E-16,-1.));
#117463=DIRECTION('center_axis',(0.,0.,1.));
#117464=DIRECTION('ref_axis',(0.,-1.,0.));
#117465=DIRECTION('',(0.,-1.23467863058847E-16,1.));
#117466=DIRECTION('center_axis',(0.,0.,1.));
#117467=DIRECTION('ref_axis',(0.,1.,0.));
#117468=DIRECTION('',(0.,1.23467863058847E-16,-1.));
#117469=DIRECTION('center_axis',(0.,0.,-1.));
#117470=DIRECTION('ref_axis',(0.,1.,0.));
#117471=DIRECTION('',(0.,-1.23467863058847E-16,1.));
#117472=DIRECTION('center_axis',(0.,0.,1.));
#117473=DIRECTION('ref_axis',(0.,1.,0.));
#117474=DIRECTION('',(0.,1.23467863058847E-16,-1.));
#117475=DIRECTION('center_axis',(0.,0.,1.));
#117476=DIRECTION('ref_axis',(0.,-1.,0.));
#117477=DIRECTION('',(0.,-1.23467863058847E-16,1.));
#117478=DIRECTION('center_axis',(0.,0.,1.));
#117479=DIRECTION('ref_axis',(0.,1.,0.));
#117480=DIRECTION('',(0.,1.23467863058847E-16,-1.));
#117481=DIRECTION('center_axis',(0.,0.,-1.));
#117482=DIRECTION('ref_axis',(0.,1.,0.));
#117483=DIRECTION('',(0.,-1.23467863058847E-16,1.));
#117484=DIRECTION('center_axis',(0.,0.,1.));
#117485=DIRECTION('ref_axis',(0.,1.,0.));
#117486=DIRECTION('',(0.,1.23467863058847E-16,-1.));
#117487=DIRECTION('center_axis',(0.,0.,1.));
#117488=DIRECTION('ref_axis',(0.,-1.,0.));
#117489=DIRECTION('',(0.,-1.23467863058847E-16,1.));
#117490=DIRECTION('center_axis',(0.,0.,1.));
#117491=DIRECTION('ref_axis',(0.,1.,0.));
#117492=DIRECTION('',(0.,1.23467863058847E-16,-1.));
#117493=DIRECTION('center_axis',(0.,0.,-1.));
#117494=DIRECTION('ref_axis',(0.,1.,0.));
#117495=DIRECTION('',(0.,-1.23467863058847E-16,1.));
#117496=DIRECTION('center_axis',(0.,0.,1.));
#117497=DIRECTION('ref_axis',(0.,1.,0.));
#117498=DIRECTION('',(0.,1.23467863058847E-16,-1.));
#117499=DIRECTION('center_axis',(0.,0.,-1.));
#117500=DIRECTION('ref_axis',(0.,1.,0.));
#117501=DIRECTION('',(0.,-1.23467863058847E-16,1.));
#117502=DIRECTION('center_axis',(0.,0.,1.));
#117503=DIRECTION('ref_axis',(0.,1.,0.));
#117504=DIRECTION('',(0.,1.23467863058847E-16,-1.));
#117505=DIRECTION('center_axis',(0.,0.,-1.));
#117506=DIRECTION('ref_axis',(0.406625030395207,-0.91359514264038,0.));
#117507=DIRECTION('',(0.,-1.23467863058847E-16,1.));
#117508=DIRECTION('center_axis',(0.,0.,1.));
#117509=DIRECTION('ref_axis',(0.,1.,0.));
#117510=DIRECTION('',(0.,1.23467863058847E-16,-1.));
#117511=DIRECTION('center_axis',(0.,0.,-1.));
#117512=DIRECTION('ref_axis',(0.,1.,0.));
#117513=DIRECTION('',(0.,-1.23467863058847E-16,1.));
#117514=DIRECTION('center_axis',(0.,0.,1.));
#117515=DIRECTION('ref_axis',(0.,1.,0.));
#117516=DIRECTION('',(0.,1.23467863058847E-16,-1.));
#117517=DIRECTION('center_axis',(0.,0.,-1.));
#117518=DIRECTION('ref_axis',(0.,1.,0.));
#117519=DIRECTION('',(0.,-1.23467863058847E-16,1.));
#117520=DIRECTION('center_axis',(0.,0.,1.));
#117521=DIRECTION('ref_axis',(0.,1.,0.));
#117522=DIRECTION('',(0.,1.23467863058847E-16,-1.));
#117523=DIRECTION('center_axis',(0.,0.,1.));
#117524=DIRECTION('ref_axis',(0.,-1.,0.));
#117525=DIRECTION('',(0.,-1.23467863058847E-16,1.));
#117526=DIRECTION('center_axis',(0.,0.,1.));
#117527=DIRECTION('ref_axis',(0.,1.,0.));
#117528=DIRECTION('',(0.,1.23467863058847E-16,-1.));
#117529=DIRECTION('center_axis',(0.,0.,-1.));
#117530=DIRECTION('ref_axis',(0.,1.,0.));
#117531=DIRECTION('',(0.,-1.23467863058847E-16,1.));
#117532=DIRECTION('center_axis',(0.,0.,1.));
#117533=DIRECTION('ref_axis',(0.,1.,0.));
#117534=DIRECTION('',(0.,1.23467863058847E-16,-1.));
#117535=DIRECTION('center_axis',(0.,0.,1.));
#117536=DIRECTION('ref_axis',(0.,-1.,0.));
#117537=DIRECTION('',(0.,-1.23467863058847E-16,1.));
#117538=DIRECTION('center_axis',(0.,0.,1.));
#117539=DIRECTION('ref_axis',(0.,1.,0.));
#117540=DIRECTION('',(0.,1.23467863058847E-16,-1.));
#117541=DIRECTION('center_axis',(0.,0.,-1.));
#117542=DIRECTION('ref_axis',(0.,1.,0.));
#117543=DIRECTION('',(0.,-1.23467863058847E-16,1.));
#117544=DIRECTION('center_axis',(0.,0.,1.));
#117545=DIRECTION('ref_axis',(0.,1.,0.));
#117546=DIRECTION('',(0.,1.23467863058847E-16,-1.));
#117547=DIRECTION('center_axis',(0.,0.,1.));
#117548=DIRECTION('ref_axis',(0.,-1.,0.));
#117549=DIRECTION('',(0.,-1.23467863058847E-16,1.));
#117550=DIRECTION('center_axis',(0.,0.,1.));
#117551=DIRECTION('ref_axis',(0.,1.,0.));
#117552=DIRECTION('',(0.,1.23467863058847E-16,-1.));
#117553=DIRECTION('center_axis',(0.,0.,-1.));
#117554=DIRECTION('ref_axis',(0.,1.,0.));
#117555=DIRECTION('',(0.,-1.23467863058847E-16,1.));
#117556=DIRECTION('center_axis',(0.,0.,1.));
#117557=DIRECTION('ref_axis',(0.,1.,0.));
#117558=DIRECTION('',(0.,1.23467863058847E-16,-1.));
#117559=DIRECTION('center_axis',(0.,0.,-1.));
#117560=DIRECTION('ref_axis',(0.,1.,0.));
#117561=DIRECTION('',(0.,-1.23467863058847E-16,1.));
#117562=DIRECTION('center_axis',(0.,0.,1.));
#117563=DIRECTION('ref_axis',(0.,1.,0.));
#117564=DIRECTION('',(0.,1.23467863058847E-16,-1.));
#117565=DIRECTION('center_axis',(0.,0.,-1.));
#117566=DIRECTION('ref_axis',(0.,1.,0.));
#117567=DIRECTION('',(0.,-1.23467863058847E-16,1.));
#117568=DIRECTION('center_axis',(0.,0.,1.));
#117569=DIRECTION('ref_axis',(0.,1.,0.));
#117570=DIRECTION('',(0.,1.23467863058847E-16,-1.));
#117571=DIRECTION('center_axis',(0.,0.,1.));
#117572=DIRECTION('ref_axis',(0.,-1.,0.));
#117573=DIRECTION('',(0.,-1.23467863058847E-16,1.));
#117574=DIRECTION('center_axis',(0.,0.,1.));
#117575=DIRECTION('ref_axis',(0.,1.,0.));
#117576=DIRECTION('',(0.,1.23467863058847E-16,-1.));
#117577=DIRECTION('center_axis',(0.,0.,-1.));
#117578=DIRECTION('ref_axis',(0.,1.,0.));
#117579=DIRECTION('',(0.,-1.23467863058847E-16,1.));
#117580=DIRECTION('center_axis',(0.,0.,1.));
#117581=DIRECTION('ref_axis',(0.,1.,0.));
#117582=DIRECTION('',(0.,1.23467863058847E-16,-1.));
#117583=DIRECTION('center_axis',(0.,0.,-1.));
#117584=DIRECTION('ref_axis',(0.,1.,0.));
#117585=DIRECTION('',(0.,-1.23467863058847E-16,1.));
#117586=DIRECTION('center_axis',(0.,0.,1.));
#117587=DIRECTION('ref_axis',(0.,1.,0.));
#117588=DIRECTION('',(0.,1.23467863058847E-16,-1.));
#117589=DIRECTION('center_axis',(0.,0.,-1.));
#117590=DIRECTION('ref_axis',(0.,1.,0.));
#117591=DIRECTION('',(0.,-1.23467863058847E-16,1.));
#117592=DIRECTION('center_axis',(0.,0.,1.));
#117593=DIRECTION('ref_axis',(0.,1.,0.));
#117594=DIRECTION('',(0.,1.23467863058847E-16,-1.));
#117595=DIRECTION('center_axis',(0.,0.,1.));
#117596=DIRECTION('ref_axis',(0.,-1.,0.));
#117597=DIRECTION('',(0.,-1.23467863058847E-16,1.));
#117598=DIRECTION('center_axis',(0.,0.,1.));
#117599=DIRECTION('ref_axis',(0.,1.,0.));
#117600=DIRECTION('',(0.,1.23467863058847E-16,-1.));
#117601=DIRECTION('center_axis',(0.,0.,-1.));
#117602=DIRECTION('ref_axis',(0.,1.,0.));
#117603=DIRECTION('',(0.,-1.23467863058847E-16,1.));
#117604=DIRECTION('center_axis',(0.,0.,1.));
#117605=DIRECTION('ref_axis',(0.,1.,0.));
#117606=DIRECTION('',(0.,1.23467863058847E-16,-1.));
#117607=DIRECTION('center_axis',(0.,0.,-1.));
#117608=DIRECTION('ref_axis',(0.,1.,0.));
#117609=DIRECTION('',(0.,-1.23467863058847E-16,1.));
#117610=DIRECTION('center_axis',(0.,0.,1.));
#117611=DIRECTION('ref_axis',(0.,1.,0.));
#117612=DIRECTION('',(0.,1.23467863058847E-16,-1.));
#117613=DIRECTION('center_axis',(0.,0.,-1.));
#117614=DIRECTION('ref_axis',(0.,1.,0.));
#117615=DIRECTION('',(0.,-1.23467863058847E-16,1.));
#117616=DIRECTION('center_axis',(0.,0.,1.));
#117617=DIRECTION('ref_axis',(0.,1.,0.));
#117618=DIRECTION('',(0.,1.23467863058847E-16,-1.));
#117619=DIRECTION('center_axis',(0.,0.,1.));
#117620=DIRECTION('ref_axis',(0.,-1.,0.));
#117621=DIRECTION('',(0.,-1.23467863058847E-16,1.));
#117622=DIRECTION('center_axis',(0.,0.,1.));
#117623=DIRECTION('ref_axis',(0.,1.,0.));
#117624=DIRECTION('',(0.,1.23467863058847E-16,-1.));
#117625=DIRECTION('center_axis',(0.,0.,-1.));
#117626=DIRECTION('ref_axis',(0.,1.,0.));
#117627=DIRECTION('',(0.,-1.23467863058847E-16,1.));
#117628=DIRECTION('center_axis',(0.,0.,1.));
#117629=DIRECTION('ref_axis',(0.,1.,0.));
#117630=DIRECTION('',(0.,1.23467863058847E-16,-1.));
#117631=DIRECTION('center_axis',(0.,0.,-1.));
#117632=DIRECTION('ref_axis',(0.,1.,0.));
#117633=DIRECTION('',(0.,-1.23467863058847E-16,1.));
#117634=DIRECTION('center_axis',(0.,0.,1.));
#117635=DIRECTION('ref_axis',(0.,1.,0.));
#117636=DIRECTION('',(0.,1.23467863058847E-16,-1.));
#117637=DIRECTION('center_axis',(0.,0.,-1.));
#117638=DIRECTION('ref_axis',(0.,1.,0.));
#117639=DIRECTION('',(0.,-1.23467863058847E-16,1.));
#117640=DIRECTION('center_axis',(0.,0.,1.));
#117641=DIRECTION('ref_axis',(0.,1.,0.));
#117642=DIRECTION('',(0.,1.23467863058847E-16,-1.));
#117643=DIRECTION('center_axis',(0.,0.,1.));
#117644=DIRECTION('ref_axis',(0.,-1.,0.));
#117645=DIRECTION('',(0.,-1.23467863058847E-16,1.));
#117646=DIRECTION('center_axis',(0.,0.,1.));
#117647=DIRECTION('ref_axis',(0.,1.,0.));
#117648=DIRECTION('',(0.,1.23467863058847E-16,-1.));
#117649=DIRECTION('center_axis',(0.,0.,-1.));
#117650=DIRECTION('ref_axis',(0.,1.,0.));
#117651=DIRECTION('',(0.,-1.23467863058847E-16,1.));
#117652=DIRECTION('center_axis',(0.,0.,1.));
#117653=DIRECTION('ref_axis',(0.,1.,0.));
#117654=DIRECTION('',(0.,1.23467863058847E-16,-1.));
#117655=DIRECTION('center_axis',(0.,0.,-1.));
#117656=DIRECTION('ref_axis',(0.,1.,0.));
#117657=DIRECTION('',(0.,-1.23467863058847E-16,1.));
#117658=DIRECTION('center_axis',(0.,0.,1.));
#117659=DIRECTION('ref_axis',(0.,1.,0.));
#117660=DIRECTION('',(0.,1.23467863058847E-16,-1.));
#117661=DIRECTION('center_axis',(0.,0.,-1.));
#117662=DIRECTION('ref_axis',(0.,1.,0.));
#117663=DIRECTION('',(0.,-1.23467863058847E-16,1.));
#117664=DIRECTION('center_axis',(0.,0.,1.));
#117665=DIRECTION('ref_axis',(0.,1.,0.));
#117666=DIRECTION('',(0.,1.23467863058847E-16,-1.));
#117667=DIRECTION('center_axis',(0.,0.,-1.));
#117668=DIRECTION('ref_axis',(0.,1.,0.));
#117669=DIRECTION('',(0.,-1.23467863058847E-16,1.));
#117670=DIRECTION('center_axis',(0.,0.,1.));
#117671=DIRECTION('ref_axis',(0.,1.,0.));
#117672=DIRECTION('',(0.,1.23467863058847E-16,-1.));
#117673=DIRECTION('center_axis',(0.,0.,-1.));
#117674=DIRECTION('ref_axis',(0.,1.,0.));
#117675=DIRECTION('center_axis',(0.,0.,1.));
#117676=DIRECTION('ref_axis',(0.,1.,0.));
#117677=DIRECTION('',(0.,1.23467863058847E-16,-1.));
#117678=DIRECTION('',(0.,-1.23467863058847E-16,1.));
#117679=DIRECTION('center_axis',(0.,0.,1.));
#117680=DIRECTION('ref_axis',(0.,-1.,0.));
#117681=DIRECTION('',(0.,-1.23467863058847E-16,1.));
#117682=DIRECTION('center_axis',(0.,0.,1.));
#117683=DIRECTION('ref_axis',(0.,1.,0.));
#117684=DIRECTION('',(0.,1.23467863058847E-16,-1.));
#117685=DIRECTION('center_axis',(0.,0.,-1.));
#117686=DIRECTION('ref_axis',(0.,1.,0.));
#117687=DIRECTION('',(0.,-1.23467863058847E-16,1.));
#117688=DIRECTION('center_axis',(0.,0.,1.));
#117689=DIRECTION('ref_axis',(0.,1.,0.));
#117690=DIRECTION('',(0.,1.23467863058847E-16,-1.));
#117691=DIRECTION('center_axis',(0.,0.,1.));
#117692=DIRECTION('ref_axis',(0.,-1.,0.));
#117693=DIRECTION('',(0.,-1.23467863058847E-16,1.));
#117694=DIRECTION('center_axis',(0.,0.,1.));
#117695=DIRECTION('ref_axis',(0.,1.,0.));
#117696=DIRECTION('',(0.,1.23467863058847E-16,-1.));
#117697=DIRECTION('center_axis',(1.3684555315672E-48,0.,-1.));
#117698=DIRECTION('ref_axis',(0.,1.,0.));
#117699=DIRECTION('',(-1.3684555315672E-48,-1.23467863058847E-16,1.));
#117700=DIRECTION('center_axis',(0.,0.,1.));
#117701=DIRECTION('ref_axis',(0.,1.,0.));
#117702=DIRECTION('',(0.,1.23467863058847E-16,-1.));
#117703=DIRECTION('center_axis',(0.,0.,-1.));
#117704=DIRECTION('ref_axis',(0.701138397908223,-0.713025207814346,0.));
#117705=DIRECTION('',(0.,-1.23467863058847E-16,1.));
#117706=DIRECTION('center_axis',(0.,0.,1.));
#117707=DIRECTION('ref_axis',(0.,1.,0.));
#117708=DIRECTION('',(1.3684555315672E-48,1.23467863058847E-16,-1.));
#117709=DIRECTION('center_axis',(0.,0.,1.));
#117710=DIRECTION('ref_axis',(0.,-1.,0.));
#117711=DIRECTION('',(0.,-1.23467863058847E-16,1.));
#117712=DIRECTION('center_axis',(0.,0.,1.));
#117713=DIRECTION('ref_axis',(0.,1.,0.));
#117714=DIRECTION('',(0.,1.23467863058847E-16,-1.));
#117715=DIRECTION('center_axis',(1.3684555315672E-48,0.,-1.));
#117716=DIRECTION('ref_axis',(0.,1.,0.));
#117717=DIRECTION('',(-1.3684555315672E-48,-1.23467863058847E-16,1.));
#117718=DIRECTION('center_axis',(0.,0.,1.));
#117719=DIRECTION('ref_axis',(0.,1.,0.));
#117720=DIRECTION('',(0.,1.23467863058847E-16,-1.));
#117721=DIRECTION('center_axis',(-1.3684555315672E-48,0.,1.));
#117722=DIRECTION('ref_axis',(0.,-1.,0.));
#117723=DIRECTION('',(0.,-1.23467863058847E-16,1.));
#117724=DIRECTION('center_axis',(0.,0.,1.));
#117725=DIRECTION('ref_axis',(0.,1.,0.));
#117726=DIRECTION('',(1.3684555315672E-48,1.23467863058847E-16,-1.));
#117727=DIRECTION('center_axis',(0.,0.,-1.));
#117728=DIRECTION('ref_axis',(0.,1.,0.));
#117729=DIRECTION('',(0.,-1.23467863058847E-16,1.));
#117730=DIRECTION('center_axis',(0.,0.,1.));
#117731=DIRECTION('ref_axis',(0.,1.,0.));
#117732=DIRECTION('',(0.,1.23467863058847E-16,-1.));
#117733=DIRECTION('center_axis',(0.,0.,1.));
#117734=DIRECTION('ref_axis',(0.,-1.,0.));
#117735=DIRECTION('',(0.,-1.23467863058847E-16,1.));
#117736=DIRECTION('center_axis',(0.,0.,1.));
#117737=DIRECTION('ref_axis',(0.,1.,0.));
#117738=DIRECTION('',(0.,1.23467863058847E-16,-1.));
#117739=DIRECTION('center_axis',(1.3684555315672E-48,0.,-1.));
#117740=DIRECTION('ref_axis',(0.,1.,0.));
#117741=DIRECTION('',(-1.3684555315672E-48,-1.23467863058847E-16,1.));
#117742=DIRECTION('center_axis',(0.,0.,1.));
#117743=DIRECTION('ref_axis',(0.,1.,0.));
#117744=DIRECTION('',(0.,1.23467863058847E-16,-1.));
#117745=DIRECTION('center_axis',(-1.3684555315672E-48,0.,1.));
#117746=DIRECTION('ref_axis',(0.,-1.,0.));
#117747=DIRECTION('',(0.,-1.23467863058847E-16,1.));
#117748=DIRECTION('center_axis',(0.,0.,1.));
#117749=DIRECTION('ref_axis',(0.,1.,0.));
#117750=DIRECTION('',(1.3684555315672E-48,1.23467863058847E-16,-1.));
#117751=DIRECTION('center_axis',(0.,0.,-1.));
#117752=DIRECTION('ref_axis',(0.,1.,0.));
#117753=DIRECTION('',(0.,-1.23467863058847E-16,1.));
#117754=DIRECTION('center_axis',(0.,0.,1.));
#117755=DIRECTION('ref_axis',(0.,1.,0.));
#117756=DIRECTION('',(0.,1.23467863058847E-16,-1.));
#117757=DIRECTION('center_axis',(0.,0.,1.));
#117758=DIRECTION('ref_axis',(0.,-1.,0.));
#117759=DIRECTION('',(0.,-1.23467863058847E-16,1.));
#117760=DIRECTION('center_axis',(0.,0.,1.));
#117761=DIRECTION('ref_axis',(0.,1.,0.));
#117762=DIRECTION('',(0.,1.23467863058847E-16,-1.));
#117763=DIRECTION('center_axis',(1.3684555315672E-48,0.,-1.));
#117764=DIRECTION('ref_axis',(0.,1.,0.));
#117765=DIRECTION('',(-1.3684555315672E-48,-1.23467863058847E-16,1.));
#117766=DIRECTION('center_axis',(0.,0.,1.));
#117767=DIRECTION('ref_axis',(0.,1.,0.));
#117768=DIRECTION('',(0.,1.23467863058847E-16,-1.));
#117769=DIRECTION('center_axis',(-1.3684555315672E-48,0.,1.));
#117770=DIRECTION('ref_axis',(0.,-1.,0.));
#117771=DIRECTION('',(0.,-1.23467863058847E-16,1.));
#117772=DIRECTION('center_axis',(0.,0.,1.));
#117773=DIRECTION('ref_axis',(0.,1.,0.));
#117774=DIRECTION('',(1.3684555315672E-48,1.23467863058847E-16,-1.));
#117775=DIRECTION('center_axis',(0.,0.,-1.));
#117776=DIRECTION('ref_axis',(0.,1.,0.));
#117777=DIRECTION('',(0.,-1.23467863058847E-16,1.));
#117778=DIRECTION('center_axis',(0.,0.,1.));
#117779=DIRECTION('ref_axis',(0.,1.,0.));
#117780=DIRECTION('',(0.,1.23467863058847E-16,-1.));
#117781=DIRECTION('center_axis',(0.,0.,-1.));
#117782=DIRECTION('ref_axis',(0.,1.,0.));
#117783=DIRECTION('',(0.,-1.23467863058847E-16,1.));
#117784=DIRECTION('center_axis',(0.,0.,1.));
#117785=DIRECTION('ref_axis',(0.,1.,0.));
#117786=DIRECTION('',(0.,1.23467863058847E-16,-1.));
#117787=DIRECTION('center_axis',(0.,0.,1.));
#117788=DIRECTION('ref_axis',(0.,-1.,0.));
#117789=DIRECTION('',(0.,-1.23467863058847E-16,1.));
#117790=DIRECTION('center_axis',(0.,0.,1.));
#117791=DIRECTION('ref_axis',(0.,1.,0.));
#117792=DIRECTION('',(0.,1.23467863058847E-16,-1.));
#117793=DIRECTION('center_axis',(1.3684555315672E-48,0.,-1.));
#117794=DIRECTION('ref_axis',(0.,1.,0.));
#117795=DIRECTION('',(-1.3684555315672E-48,-1.23467863058847E-16,1.));
#117796=DIRECTION('center_axis',(0.,0.,1.));
#117797=DIRECTION('ref_axis',(0.,1.,0.));
#117798=DIRECTION('',(0.,1.23467863058847E-16,-1.));
#117799=DIRECTION('center_axis',(-1.3684555315672E-48,0.,1.));
#117800=DIRECTION('ref_axis',(0.,-1.,0.));
#117801=DIRECTION('',(0.,-1.23467863058847E-16,1.));
#117802=DIRECTION('center_axis',(0.,0.,1.));
#117803=DIRECTION('ref_axis',(0.,1.,0.));
#117804=DIRECTION('',(1.3684555315672E-48,1.23467863058847E-16,-1.));
#117805=DIRECTION('center_axis',(0.,0.,-1.));
#117806=DIRECTION('ref_axis',(0.,1.,0.));
#117807=DIRECTION('',(0.,-1.23467863058847E-16,1.));
#117808=DIRECTION('center_axis',(0.,0.,1.));
#117809=DIRECTION('ref_axis',(0.,1.,0.));
#117810=DIRECTION('',(0.,1.23467863058847E-16,-1.));
#117811=DIRECTION('center_axis',(0.,0.,-1.));
#117812=DIRECTION('ref_axis',(0.,1.,0.));
#117813=DIRECTION('',(0.,-1.23467863058847E-16,1.));
#117814=DIRECTION('center_axis',(0.,0.,1.));
#117815=DIRECTION('ref_axis',(0.,1.,0.));
#117816=DIRECTION('',(0.,1.23467863058847E-16,-1.));
#117817=DIRECTION('center_axis',(0.,0.,-1.));
#117818=DIRECTION('ref_axis',(0.,1.,0.));
#117819=DIRECTION('center_axis',(0.,0.,1.));
#117820=DIRECTION('ref_axis',(0.,1.,0.));
#117821=DIRECTION('',(0.,1.23467863058847E-16,-1.));
#117822=DIRECTION('',(-1.3684555315672E-48,-1.23467863058847E-16,1.));
#117823=DIRECTION('center_axis',(-1.3684555315672E-48,0.,1.));
#117824=DIRECTION('ref_axis',(0.,-1.,0.));
#117825=DIRECTION('',(-1.3684555315672E-48,-1.23467863058847E-16,1.));
#117826=DIRECTION('center_axis',(0.,0.,1.));
#117827=DIRECTION('ref_axis',(0.,1.,0.));
#117828=DIRECTION('',(1.3684555315672E-48,1.23467863058847E-16,-1.));
#117829=DIRECTION('center_axis',(0.,0.,-1.));
#117830=DIRECTION('ref_axis',(0.,1.,0.));
#117831=DIRECTION('',(0.,-1.23467863058847E-16,1.));
#117832=DIRECTION('center_axis',(0.,0.,1.));
#117833=DIRECTION('ref_axis',(0.,1.,0.));
#117834=DIRECTION('',(0.,1.23467863058847E-16,-1.));
#117835=DIRECTION('center_axis',(0.,0.,1.));
#117836=DIRECTION('ref_axis',(0.,-1.,0.));
#117837=DIRECTION('',(0.,-1.23467863058847E-16,1.));
#117838=DIRECTION('center_axis',(0.,0.,1.));
#117839=DIRECTION('ref_axis',(0.,1.,0.));
#117840=DIRECTION('',(0.,1.23467863058847E-16,-1.));
#117841=DIRECTION('center_axis',(0.,0.,-1.));
#117842=DIRECTION('ref_axis',(0.,1.,0.));
#117843=DIRECTION('',(0.,-1.23467863058847E-16,1.));
#117844=DIRECTION('center_axis',(0.,0.,1.));
#117845=DIRECTION('ref_axis',(0.,1.,0.));
#117846=DIRECTION('',(0.,1.23467863058847E-16,-1.));
#117847=DIRECTION('center_axis',(0.,0.,-1.));
#117848=DIRECTION('ref_axis',(0.706453380948025,-0.707759578209369,0.));
#117849=DIRECTION('',(0.,-1.23467863058847E-16,1.));
#117850=DIRECTION('center_axis',(0.,0.,1.));
#117851=DIRECTION('ref_axis',(0.,1.,0.));
#117852=DIRECTION('',(0.,1.23467863058847E-16,-1.));
#117853=DIRECTION('center_axis',(0.,0.,1.));
#117854=DIRECTION('ref_axis',(0.,-1.,0.));
#117855=DIRECTION('',(0.,-1.23467863058847E-16,1.));
#117856=DIRECTION('center_axis',(0.,0.,1.));
#117857=DIRECTION('ref_axis',(0.,1.,0.));
#117858=DIRECTION('',(0.,1.23467863058847E-16,-1.));
#117859=DIRECTION('center_axis',(0.,0.,-1.));
#117860=DIRECTION('ref_axis',(0.,1.,0.));
#117861=DIRECTION('',(0.,-1.23467863058847E-16,1.));
#117862=DIRECTION('center_axis',(0.,0.,1.));
#117863=DIRECTION('ref_axis',(0.,1.,0.));
#117864=DIRECTION('',(0.,1.23467863058847E-16,-1.));
#117865=DIRECTION('center_axis',(0.,0.,1.));
#117866=DIRECTION('ref_axis',(0.,-1.,0.));
#117867=DIRECTION('',(0.,-1.23467863058847E-16,1.));
#117868=DIRECTION('center_axis',(0.,0.,1.));
#117869=DIRECTION('ref_axis',(0.,1.,0.));
#117870=DIRECTION('',(0.,1.23467863058847E-16,-1.));
#117871=DIRECTION('center_axis',(0.,0.,-1.));
#117872=DIRECTION('ref_axis',(0.,1.,0.));
#117873=DIRECTION('',(0.,-1.23467863058847E-16,1.));
#117874=DIRECTION('center_axis',(0.,0.,1.));
#117875=DIRECTION('ref_axis',(0.,1.,0.));
#117876=DIRECTION('',(0.,1.23467863058847E-16,-1.));
#117877=DIRECTION('center_axis',(0.,0.,-1.));
#117878=DIRECTION('ref_axis',(0.,1.,0.));
#117879=DIRECTION('',(0.,-1.23467863058847E-16,1.));
#117880=DIRECTION('center_axis',(0.,0.,1.));
#117881=DIRECTION('ref_axis',(0.,1.,0.));
#117882=DIRECTION('',(0.,1.23467863058847E-16,-1.));
#117883=DIRECTION('center_axis',(0.,0.,1.));
#117884=DIRECTION('ref_axis',(0.,-1.,0.));
#117885=DIRECTION('',(0.,-1.23467863058847E-16,1.));
#117886=DIRECTION('center_axis',(0.,0.,1.));
#117887=DIRECTION('ref_axis',(0.,1.,0.));
#117888=DIRECTION('',(0.,1.23467863058847E-16,-1.));
#117889=DIRECTION('center_axis',(0.,0.,-1.));
#117890=DIRECTION('ref_axis',(0.,1.,0.));
#117891=DIRECTION('',(0.,-1.23467863058847E-16,1.));
#117892=DIRECTION('center_axis',(0.,0.,1.));
#117893=DIRECTION('ref_axis',(0.,1.,0.));
#117894=DIRECTION('',(0.,1.23467863058847E-16,-1.));
#117895=DIRECTION('center_axis',(0.,0.,1.));
#117896=DIRECTION('ref_axis',(0.,-1.,0.));
#117897=DIRECTION('',(0.,-1.23467863058847E-16,1.));
#117898=DIRECTION('center_axis',(0.,0.,1.));
#117899=DIRECTION('ref_axis',(0.,1.,0.));
#117900=DIRECTION('',(0.,1.23467863058847E-16,-1.));
#117901=DIRECTION('center_axis',(0.,0.,-1.));
#117902=DIRECTION('ref_axis',(0.,1.,0.));
#117903=DIRECTION('',(0.,-1.23467863058847E-16,1.));
#117904=DIRECTION('center_axis',(0.,0.,1.));
#117905=DIRECTION('ref_axis',(0.,1.,0.));
#117906=DIRECTION('',(0.,1.23467863058847E-16,-1.));
#117907=DIRECTION('center_axis',(0.,0.,-1.));
#117908=DIRECTION('ref_axis',(0.,1.,0.));
#117909=DIRECTION('',(0.,-1.23467863058847E-16,1.));
#117910=DIRECTION('center_axis',(0.,0.,1.));
#117911=DIRECTION('ref_axis',(0.,1.,0.));
#117912=DIRECTION('',(0.,1.23467863058847E-16,-1.));
#117913=DIRECTION('center_axis',(0.,0.,-1.));
#117914=DIRECTION('ref_axis',(0.,1.,0.));
#117915=DIRECTION('center_axis',(0.,0.,1.));
#117916=DIRECTION('ref_axis',(0.,1.,0.));
#117917=DIRECTION('',(0.,1.23467863058847E-16,-1.));
#117918=DIRECTION('',(0.,-1.23467863058847E-16,1.));
#117919=DIRECTION('center_axis',(0.,0.,1.));
#117920=DIRECTION('ref_axis',(0.,-1.,0.));
#117921=DIRECTION('',(0.,-1.23467863058847E-16,1.));
#117922=DIRECTION('center_axis',(0.,0.,1.));
#117923=DIRECTION('ref_axis',(0.,1.,0.));
#117924=DIRECTION('',(0.,1.23467863058847E-16,-1.));
#117925=DIRECTION('center_axis',(0.,0.,-1.));
#117926=DIRECTION('ref_axis',(-0.0361435302645155,-0.999346609150208,0.));
#117927=DIRECTION('',(0.,-1.23467863058847E-16,1.));
#117928=DIRECTION('center_axis',(0.,0.,1.));
#117929=DIRECTION('ref_axis',(0.,1.,0.));
#117930=DIRECTION('',(1.27503726478586E-32,1.23467863058847E-16,-1.));
#117931=DIRECTION('center_axis',(0.,0.,-1.));
#117932=DIRECTION('ref_axis',(0.,1.,0.));
#117933=DIRECTION('',(0.,-1.23467863058847E-16,1.));
#117934=DIRECTION('center_axis',(0.,0.,1.));
#117935=DIRECTION('ref_axis',(0.,1.,0.));
#117936=DIRECTION('',(0.,1.23467863058847E-16,-1.));
#117937=DIRECTION('center_axis',(0.,0.,-1.));
#117938=DIRECTION('ref_axis',(0.,1.,0.));
#117939=DIRECTION('',(0.,-1.23467863058847E-16,1.));
#117940=DIRECTION('center_axis',(0.,0.,1.));
#117941=DIRECTION('ref_axis',(0.,1.,0.));
#117942=DIRECTION('',(0.,1.23467863058847E-16,-1.));
#117943=DIRECTION('center_axis',(0.,0.,-1.));
#117944=DIRECTION('ref_axis',(0.,1.,0.));
#117945=DIRECTION('center_axis',(0.,0.,1.));
#117946=DIRECTION('ref_axis',(0.,1.,0.));
#117947=DIRECTION('',(0.,1.23467863058847E-16,-1.));
#117948=DIRECTION('',(0.,-1.23467863058847E-16,1.));
#117949=DIRECTION('center_axis',(0.,0.,-1.));
#117950=DIRECTION('ref_axis',(0.663057938251906,-0.748568080084324,0.));
#117951=DIRECTION('',(0.,-1.23467863058847E-16,1.));
#117952=DIRECTION('center_axis',(0.,0.,1.));
#117953=DIRECTION('ref_axis',(0.,1.,0.));
#117954=DIRECTION('',(0.,1.23467863058847E-16,-1.));
#117955=DIRECTION('center_axis',(0.,0.,-1.));
#117956=DIRECTION('ref_axis',(0.,1.,0.));
#117957=DIRECTION('center_axis',(0.,0.,1.));
#117958=DIRECTION('ref_axis',(0.,1.,0.));
#117959=DIRECTION('',(0.,1.23467863058847E-16,-1.));
#117960=DIRECTION('',(0.,-1.23467863058847E-16,1.));
#117961=DIRECTION('center_axis',(0.,0.,-1.));
#117962=DIRECTION('ref_axis',(0.,1.,0.));
#117963=DIRECTION('',(-3.82498197630791E-33,-1.23467863058847E-16,1.));
#117964=DIRECTION('center_axis',(0.,0.,1.));
#117965=DIRECTION('ref_axis',(0.,1.,0.));
#117966=DIRECTION('',(0.,1.23467863058847E-16,-1.));
#117967=DIRECTION('center_axis',(0.,0.,-1.));
#117968=DIRECTION('ref_axis',(0.,1.,0.));
#117969=DIRECTION('',(0.,-1.23467863058847E-16,1.));
#117970=DIRECTION('center_axis',(0.,0.,1.));
#117971=DIRECTION('ref_axis',(0.,1.,0.));
#117972=DIRECTION('',(1.3684555315672E-48,1.23467863058847E-16,-1.));
#117973=DIRECTION('center_axis',(0.,0.,-1.));
#117974=DIRECTION('ref_axis',(0.,1.,0.));
#117975=DIRECTION('',(-1.3684555315672E-48,-1.23467863058847E-16,1.));
#117976=DIRECTION('center_axis',(0.,0.,1.));
#117977=DIRECTION('ref_axis',(0.,1.,0.));
#117978=DIRECTION('',(0.,1.23467863058847E-16,-1.));
#117979=DIRECTION('center_axis',(0.,0.,-1.));
#117980=DIRECTION('ref_axis',(0.,1.,0.));
#117981=DIRECTION('',(0.,-1.23467863058847E-16,1.));
#117982=DIRECTION('center_axis',(0.,0.,1.));
#117983=DIRECTION('ref_axis',(0.,1.,0.));
#117984=DIRECTION('center_axis',(0.,0.,-1.));
#117985=DIRECTION('ref_axis',(0.,1.,0.));
#117986=DIRECTION('center_axis',(0.,0.,1.));
#117987=DIRECTION('ref_axis',(0.,1.,0.));
#117988=DIRECTION('',(0.,1.23467863058847E-16,-1.));
#117989=DIRECTION('center_axis',(0.,0.,-1.));
#117990=DIRECTION('ref_axis',(0.,1.,0.));
#117991=DIRECTION('center_axis',(0.,0.,-1.));
#117992=DIRECTION('ref_axis',(0.,1.,0.));
#117993=DIRECTION('center_axis',(0.,0.,-1.));
#117994=DIRECTION('ref_axis',(0.,1.,0.));
#117995=DIRECTION('center_axis',(-5.48307457476793E-31,2.43497425545765E-45,
-1.));
#117996=DIRECTION('ref_axis',(4.44089209850063E-15,1.,-3.42265840282363E-60));
#117997=DIRECTION('center_axis',(0.,0.,-1.));
#117998=DIRECTION('ref_axis',(0.,1.,0.));
#117999=DIRECTION('center_axis',(0.,0.,-1.));
#118000=DIRECTION('ref_axis',(0.,1.,0.));
#118001=DIRECTION('center_axis',(-0.724113717892013,0.689680595319751,8.51533892972833E-17));
#118002=DIRECTION('ref_axis',(1.17596707800504E-16,6.08324121309175E-33,
1.));
#118003=DIRECTION('',(0.689680595319751,0.724113717892013,8.9404773359724E-17));
#118004=DIRECTION('center_axis',(0.724113717892013,-0.689680595319751,-8.51533892972834E-17));
#118005=DIRECTION('ref_axis',(4.33608168928332E-33,1.23467863058847E-16,
-1.));
#118006=DIRECTION('',(-0.689680595319751,-0.724113717892013,-8.9404773359724E-17));
#118007=DIRECTION('center_axis',(0.,0.,-1.));
#118008=DIRECTION('ref_axis',(0.,1.,0.));
#118009=DIRECTION('center_axis',(2.19322982990717E-31,3.89595880873225E-46,
-1.));
#118010=DIRECTION('ref_axis',(-1.77635683940025E-15,1.,7.77876909732643E-62));
#118011=DIRECTION('center_axis',(0.,0.,-1.));
#118012=DIRECTION('ref_axis',(0.,1.,0.));
#118013=DIRECTION('center_axis',(-4.38645965981435E-31,1.5583835234929E-45,
-1.));
#118014=DIRECTION('ref_axis',(3.5527136788005E-15,1.,-9.33452291679171E-61));
#118015=DIRECTION('center_axis',(0.,0.,-1.));
#118016=DIRECTION('ref_axis',(0.,1.,0.));
#118017=DIRECTION('center_axis',(7.6763044046751E-31,4.77254954069701E-45,
-1.));
#118018=DIRECTION('ref_axis',(-6.21724893790088E-15,1.,-1.86690458335834E-60));
#118019=DIRECTION('center_axis',(0.724113717892013,0.689680595319752,8.51533892972834E-17));
#118020=DIRECTION('ref_axis',(1.94663562866425E-33,1.23467863058847E-16,
-1.));
#118021=DIRECTION('',(0.689680595319752,-0.724113717892012,-8.94047733597238E-17));
#118022=DIRECTION('center_axis',(-0.724113717892013,-0.689680595319752,
-8.51533892972833E-17));
#118023=DIRECTION('ref_axis',(-0.689680595319752,0.724113717892013,-1.8658423912347E-33));
#118024=DIRECTION('',(-0.689680595319752,0.724113717892012,8.94047733597238E-17));
#118025=DIRECTION('center_axis',(0.,0.,-1.));
#118026=DIRECTION('ref_axis',(0.,1.,0.));
#118027=DIRECTION('center_axis',(-1.09661491495359E-31,9.73989702183063E-47,
-1.));
#118028=DIRECTION('ref_axis',(8.88178419700125E-16,1.,0.));
#118029=DIRECTION('center_axis',(0.,0.,-1.));
#118030=DIRECTION('ref_axis',(0.,1.,0.));
#118031=DIRECTION('center_axis',(-9.86953423458227E-31,7.88931658768281E-45,
-1.));
#118032=DIRECTION('ref_axis',(7.99360577730113E-15,1.,-2.48920611114446E-60));
#118033=DIRECTION('center_axis',(-1.,0.,0.));
#118034=DIRECTION('ref_axis',(0.,0.,1.));
#118035=DIRECTION('',(0.,1.,0.));
#118036=DIRECTION('center_axis',(1.,0.,0.));
#118037=DIRECTION('ref_axis',(0.,1.,0.));
#118038=DIRECTION('',(0.,-1.,0.));
#118039=DIRECTION('center_axis',(1.,0.,0.));
#118040=DIRECTION('ref_axis',(0.,1.,0.));
#118041=DIRECTION('',(0.,-1.,0.));
#118042=DIRECTION('center_axis',(-1.,0.,0.));
#118043=DIRECTION('ref_axis',(0.,0.,1.));
#118044=DIRECTION('',(0.,1.,0.));
#118045=DIRECTION('center_axis',(1.,0.,0.));
#118046=DIRECTION('ref_axis',(0.,1.,0.));
#118047=DIRECTION('',(0.,-1.,0.));
#118048=DIRECTION('center_axis',(-1.,0.,0.));
#118049=DIRECTION('ref_axis',(0.,0.,1.));
#118050=DIRECTION('',(0.,1.,0.));
#118051=DIRECTION('center_axis',(1.,0.,0.));
#118052=DIRECTION('ref_axis',(0.,1.,0.));
#118053=DIRECTION('',(0.,-1.,0.));
#118054=DIRECTION('center_axis',(-1.,0.,0.));
#118055=DIRECTION('ref_axis',(0.,0.,1.));
#118056=DIRECTION('',(0.,1.,0.));
#118057=DIRECTION('center_axis',(1.,0.,0.));
#118058=DIRECTION('ref_axis',(0.,1.,0.));
#118059=DIRECTION('',(0.,-1.,0.));
#118060=DIRECTION('center_axis',(-1.,0.,0.));
#118061=DIRECTION('ref_axis',(0.,0.,1.));
#118062=DIRECTION('',(0.,1.,0.));
#118063=DIRECTION('center_axis',(1.,0.,0.));
#118064=DIRECTION('ref_axis',(0.,1.,0.));
#118065=DIRECTION('',(0.,-1.,0.));
#118066=DIRECTION('center_axis',(-1.,0.,0.));
#118067=DIRECTION('ref_axis',(0.,0.,1.));
#118068=DIRECTION('',(0.,1.,0.));
#118069=DIRECTION('center_axis',(1.,0.,0.));
#118070=DIRECTION('ref_axis',(0.,1.,0.));
#118071=DIRECTION('',(0.,-1.,0.));
#118072=DIRECTION('center_axis',(-1.,0.,0.));
#118073=DIRECTION('ref_axis',(0.,0.,1.));
#118074=DIRECTION('',(0.,1.,0.));
#118075=DIRECTION('center_axis',(1.,0.,0.));
#118076=DIRECTION('ref_axis',(0.,1.,0.));
#118077=DIRECTION('',(0.,-1.,0.));
#118078=DIRECTION('center_axis',(-1.,0.,0.));
#118079=DIRECTION('ref_axis',(0.,0.,1.));
#118080=DIRECTION('',(0.,1.,0.));
#118081=DIRECTION('center_axis',(-1.,7.82779334765923E-17,9.66480917101747E-33));
#118082=DIRECTION('ref_axis',(9.66480917101747E-33,0.,1.));
#118083=DIRECTION('',(7.82779334765923E-17,1.,0.));
#118084=DIRECTION('center_axis',(1.,7.82779334765923E-17,9.66480917101747E-33));
#118085=DIRECTION('ref_axis',(-7.82779334765923E-17,1.,1.39213059235047E-65));
#118086=DIRECTION('',(7.82779334765923E-17,-1.,0.));
#118087=DIRECTION('center_axis',(1.,7.82779334765923E-17,9.66480917101747E-33));
#118088=DIRECTION('ref_axis',(-7.82779334765923E-17,1.,1.39213059235047E-65));
#118089=DIRECTION('',(7.82779334765923E-17,-1.,0.));
#118090=DIRECTION('center_axis',(-1.,7.82779334765923E-17,9.66480917101747E-33));
#118091=DIRECTION('ref_axis',(9.66480917101747E-33,0.,1.));
#118092=DIRECTION('',(7.82779334765923E-17,1.,0.));
#118093=DIRECTION('center_axis',(1.,7.82779334765923E-17,9.66480917101747E-33));
#118094=DIRECTION('ref_axis',(-7.82779334765923E-17,1.,1.39213059235047E-65));
#118095=DIRECTION('',(7.82779334765923E-17,-1.,0.));
#118096=DIRECTION('center_axis',(-1.,7.82779334765923E-17,9.66480917101747E-33));
#118097=DIRECTION('ref_axis',(9.66480917101747E-33,0.,1.));
#118098=DIRECTION('',(7.82779334765923E-17,1.,0.));
#118099=DIRECTION('center_axis',(1.,7.82779334765923E-17,9.66480917101747E-33));
#118100=DIRECTION('ref_axis',(-7.82779334765923E-17,1.,1.39213059235047E-65));
#118101=DIRECTION('',(7.82779334765923E-17,-1.,0.));
#118102=DIRECTION('center_axis',(-1.,7.82779334765923E-17,9.66480917101747E-33));
#118103=DIRECTION('ref_axis',(9.66480917101747E-33,0.,1.));
#118104=DIRECTION('',(7.82779334765923E-17,1.,0.));
#118105=DIRECTION('center_axis',(1.,7.82779334765923E-17,9.66480917101747E-33));
#118106=DIRECTION('ref_axis',(-7.82779334765923E-17,1.,1.39213059235047E-65));
#118107=DIRECTION('',(7.82779334765923E-17,-1.,0.));
#118108=DIRECTION('center_axis',(-1.,7.82779334765923E-17,9.66480917101747E-33));
#118109=DIRECTION('ref_axis',(9.66480917101747E-33,0.,1.));
#118110=DIRECTION('',(7.82779334765923E-17,1.,0.));
#118111=DIRECTION('center_axis',(1.,7.82779334765923E-17,9.66480917101747E-33));
#118112=DIRECTION('ref_axis',(-7.82779334765923E-17,1.,1.39213059235047E-65));
#118113=DIRECTION('',(7.82779334765923E-17,-1.,0.));
#118114=DIRECTION('center_axis',(-1.,7.82779334765923E-17,9.66480917101747E-33));
#118115=DIRECTION('ref_axis',(9.66480917101747E-33,0.,1.));
#118116=DIRECTION('',(7.82779334765923E-17,1.,0.));
#118117=DIRECTION('center_axis',(1.,7.82779334765923E-17,9.66480917101747E-33));
#118118=DIRECTION('ref_axis',(-7.82779334765923E-17,1.,1.39213059235047E-65));
#118119=DIRECTION('',(7.82779334765923E-17,-1.,0.));
#118120=DIRECTION('center_axis',(-1.,7.82779334765923E-17,9.66480917101747E-33));
#118121=DIRECTION('ref_axis',(9.66480917101747E-33,0.,1.));
#118122=DIRECTION('',(7.82779334765923E-17,1.,0.));
#118123=DIRECTION('center_axis',(1.,7.82779334765923E-17,9.66480917101747E-33));
#118124=DIRECTION('ref_axis',(-7.82779334765923E-17,1.,1.39213059235047E-65));
#118125=DIRECTION('',(7.82779334765923E-17,-1.,0.));
#118126=DIRECTION('center_axis',(-1.,7.82779334765923E-17,9.66480917101747E-33));
#118127=DIRECTION('ref_axis',(9.66480917101747E-33,0.,1.));
#118128=DIRECTION('',(7.82779334765923E-17,1.,0.));
#118129=DIRECTION('center_axis',(0.,-1.,-1.23467863058847E-16));
#118130=DIRECTION('ref_axis',(0.,1.23467863058847E-16,-1.));
#118131=DIRECTION('',(0.,-1.23467863058847E-16,1.));
#118132=DIRECTION('',(-1.,0.,0.));
#118133=DIRECTION('',(0.,-1.23467863058847E-16,1.));
#118134=DIRECTION('',(1.,0.,0.));
#118135=DIRECTION('center_axis',(1.,7.82779334765923E-17,9.66480917101747E-33));
#118136=DIRECTION('ref_axis',(-7.82779334765923E-17,1.,1.39213059235047E-65));
#118137=DIRECTION('',(0.,-1.23467863058847E-16,1.));
#118138=DIRECTION('',(7.82779334765923E-17,-1.,0.));
#118139=DIRECTION('',(-7.82779334765923E-17,1.,1.23467863058847E-16));
#118140=DIRECTION('center_axis',(-1.,7.82779334765923E-17,9.66480917101747E-33));
#118141=DIRECTION('ref_axis',(9.66480917101747E-33,0.,1.));
#118142=DIRECTION('',(7.82779334765923E-17,1.,0.));
#118143=DIRECTION('',(0.,1.23467863058847E-16,-1.));
#118144=DIRECTION('',(-7.82779334765923E-17,-1.,-1.23467863058847E-16));
#118145=DIRECTION('center_axis',(-1.,-3.13111733906369E-16,-3.86592366840699E-32));
#118146=DIRECTION('ref_axis',(-3.13111733906369E-16,1.,9.91259258008946E-64));
#118147=DIRECTION('',(-3.13111733906369E-16,1.,0.));
#118148=DIRECTION('center_axis',(1.,5.87084501074442E-17,7.2486068782631E-33));
#118149=DIRECTION('ref_axis',(-5.87084501074442E-17,1.,-2.58656569862219E-65));
#118150=DIRECTION('',(5.87084501074442E-17,-1.,0.));
#118151=DIRECTION('center_axis',(1.,5.87084501074442E-17,7.2486068782631E-33));
#118152=DIRECTION('ref_axis',(-5.87084501074442E-17,1.,-2.58656569862219E-65));
#118153=DIRECTION('',(5.87084501074442E-17,-1.,0.));
#118154=DIRECTION('center_axis',(-1.,-3.13111733906369E-16,-3.86592366840699E-32));
#118155=DIRECTION('ref_axis',(-3.13111733906369E-16,1.,9.91259258008946E-64));
#118156=DIRECTION('',(-3.13111733906369E-16,1.,0.));
#118157=DIRECTION('center_axis',(1.,5.87084501074442E-17,7.2486068782631E-33));
#118158=DIRECTION('ref_axis',(-5.87084501074442E-17,1.,-2.58656569862219E-65));
#118159=DIRECTION('',(5.87084501074442E-17,-1.,0.));
#118160=DIRECTION('center_axis',(-1.,-3.13111733906369E-16,-3.86592366840699E-32));
#118161=DIRECTION('ref_axis',(-3.13111733906369E-16,1.,9.91259258008946E-64));
#118162=DIRECTION('',(-3.13111733906369E-16,1.,0.));
#118163=DIRECTION('center_axis',(1.,5.87084501074442E-17,7.2486068782631E-33));
#118164=DIRECTION('ref_axis',(-5.87084501074442E-17,1.,-2.58656569862219E-65));
#118165=DIRECTION('',(5.87084501074442E-17,-1.,0.));
#118166=DIRECTION('center_axis',(-1.,-3.13111733906369E-16,-3.86592366840699E-32));
#118167=DIRECTION('ref_axis',(-3.13111733906369E-16,1.,9.91259258008946E-64));
#118168=DIRECTION('',(-3.13111733906369E-16,1.,0.));
#118169=DIRECTION('center_axis',(1.,5.87084501074442E-17,7.2486068782631E-33));
#118170=DIRECTION('ref_axis',(-5.87084501074442E-17,1.,-2.58656569862219E-65));
#118171=DIRECTION('',(5.87084501074442E-17,-1.,0.));
#118172=DIRECTION('center_axis',(1.,5.87084501074442E-17,7.2486068782631E-33));
#118173=DIRECTION('ref_axis',(-5.87084501074442E-17,1.,-2.58656569862219E-65));
#118174=DIRECTION('',(5.87084501074442E-17,-1.,0.));
#118175=DIRECTION('center_axis',(1.,5.87084501074442E-17,7.2486068782631E-33));
#118176=DIRECTION('ref_axis',(-5.87084501074442E-17,1.,-2.58656569862219E-65));
#118177=DIRECTION('',(5.87084501074442E-17,-1.,0.));
#118178=DIRECTION('center_axis',(-1.,-3.13111733906369E-16,-3.86592366840699E-32));
#118179=DIRECTION('ref_axis',(-3.13111733906369E-16,1.,9.91259258008946E-64));
#118180=DIRECTION('',(-3.13111733906369E-16,1.,0.));
#118181=DIRECTION('center_axis',(1.,5.87084501074442E-17,7.2486068782631E-33));
#118182=DIRECTION('ref_axis',(-5.87084501074442E-17,1.,-2.58656569862219E-65));
#118183=DIRECTION('',(5.87084501074442E-17,-1.,0.));
#118184=DIRECTION('center_axis',(-1.,-3.13111733906369E-16,-3.86592366840699E-32));
#118185=DIRECTION('ref_axis',(-3.13111733906369E-16,1.,9.91259258008946E-64));
#118186=DIRECTION('',(-3.13111733906369E-16,1.,0.));
#118187=DIRECTION('center_axis',(1.,6.11546355285877E-17,7.5506321648574E-33));
#118188=DIRECTION('ref_axis',(-6.11546355285877E-17,1.,2.57447640954701E-65));
#118189=DIRECTION('',(6.11546355285877E-17,-1.,0.));
#118190=DIRECTION('center_axis',(1.,6.11546355285877E-17,7.5506321648574E-33));
#118191=DIRECTION('ref_axis',(-6.11546355285877E-17,1.,2.57447640954701E-65));
#118192=DIRECTION('',(6.11546355285877E-17,-1.,0.));
#118193=DIRECTION('center_axis',(1.,6.11546355285877E-17,7.5506321648574E-33));
#118194=DIRECTION('ref_axis',(-6.11546355285877E-17,1.,2.57447640954701E-65));
#118195=DIRECTION('',(6.11546355285877E-17,-1.,0.));
#118196=DIRECTION('center_axis',(1.,6.11546355285877E-17,7.5506321648574E-33));
#118197=DIRECTION('ref_axis',(-6.11546355285877E-17,1.,2.57447640954701E-65));
#118198=DIRECTION('',(6.11546355285877E-17,-1.,0.));
#118199=DIRECTION('center_axis',(1.,6.11546355285877E-17,7.5506321648574E-33));
#118200=DIRECTION('ref_axis',(-6.11546355285877E-17,1.,2.57447640954701E-65));
#118201=DIRECTION('',(6.11546355285877E-17,-1.,0.));
#118202=DIRECTION('center_axis',(1.,6.11546355285877E-17,7.5506321648574E-33));
#118203=DIRECTION('ref_axis',(-6.11546355285877E-17,1.,2.57447640954701E-65));
#118204=DIRECTION('',(6.11546355285877E-17,-1.,0.));
#118205=DIRECTION('center_axis',(1.,6.11546355285877E-17,7.5506321648574E-33));
#118206=DIRECTION('ref_axis',(-6.11546355285877E-17,1.,2.57447640954701E-65));
#118207=DIRECTION('',(6.11546355285877E-17,-1.,0.));
#118208=DIRECTION('center_axis',(1.,6.11546355285877E-17,7.5506321648574E-33));
#118209=DIRECTION('ref_axis',(-6.11546355285877E-17,1.,2.57447640954701E-65));
#118210=DIRECTION('',(6.11546355285877E-17,-1.,0.));
#118211=DIRECTION('center_axis',(0.,0.,-1.));
#118212=DIRECTION('ref_axis',(0.,1.,0.));
#118213=DIRECTION('',(0.,1.23467863058847E-16,-1.));
#118214=DIRECTION('center_axis',(0.,0.,1.));
#118215=DIRECTION('ref_axis',(0.,1.,0.));
#118216=DIRECTION('',(0.,1.23467863058847E-16,-1.));
#118217=DIRECTION('center_axis',(0.,0.,1.));
#118218=DIRECTION('ref_axis',(0.,1.,0.));
#118219=DIRECTION('center_axis',(0.,0.,-1.));
#118220=DIRECTION('ref_axis',(0.,1.,0.));
#118221=DIRECTION('center_axis',(-2.19322982990717E-31,3.89595880873225E-46,
-1.));
#118222=DIRECTION('ref_axis',(1.77635683940025E-15,1.,1.55575381946529E-61));
#118223=DIRECTION('',(0.,1.23467863058847E-16,-1.));
#118224=DIRECTION('center_axis',(0.,0.,1.));
#118225=DIRECTION('ref_axis',(0.,1.,0.));
#118226=DIRECTION('center_axis',(0.,0.,-1.));
#118227=DIRECTION('ref_axis',(0.,1.,0.));
#118228=DIRECTION('center_axis',(0.,0.,1.));
#118229=DIRECTION('ref_axis',(0.,1.,0.));
#118230=DIRECTION('',(0.,1.23467863058847E-16,-1.));
#118231=DIRECTION('center_axis',(0.,0.,1.));
#118232=DIRECTION('ref_axis',(0.,1.,0.));
#118233=DIRECTION('center_axis',(0.,1.22462808028055E-16,-1.));
#118234=DIRECTION('ref_axis',(0.,1.,1.22462808028055E-16));
#118235=DIRECTION('center_axis',(0.,-1.22462808028055E-16,1.));
#118236=DIRECTION('ref_axis',(0.,1.,1.22462808028055E-16));
#118237=DIRECTION('',(0.,1.23467863058847E-16,-1.));
#118238=DIRECTION('center_axis',(0.,-1.22462808028055E-16,1.));
#118239=DIRECTION('ref_axis',(0.,1.,1.22462808028055E-16));
#118240=DIRECTION('center_axis',(0.,0.,-1.));
#118241=DIRECTION('ref_axis',(0.,1.,0.));
#118242=DIRECTION('center_axis',(0.,0.,1.));
#118243=DIRECTION('ref_axis',(0.,1.,0.));
#118244=DIRECTION('',(0.,1.23467863058847E-16,-1.));
#118245=DIRECTION('center_axis',(0.,0.,1.));
#118246=DIRECTION('ref_axis',(0.,1.,0.));
#118247=DIRECTION('center_axis',(0.,0.,-1.));
#118248=DIRECTION('ref_axis',(0.,1.,0.));
#118249=DIRECTION('center_axis',(4.38645965981435E-31,1.5583835234929E-45,
-1.));
#118250=DIRECTION('ref_axis',(-3.5527136788005E-15,1.,-9.33452291679171E-61));
#118251=DIRECTION('',(0.,1.23467863058847E-16,-1.));
#118252=DIRECTION('center_axis',(0.,0.,1.));
#118253=DIRECTION('ref_axis',(0.,1.,0.));
#118254=DIRECTION('center_axis',(0.,0.,-1.));
#118255=DIRECTION('ref_axis',(0.,1.,0.));
#118256=DIRECTION('center_axis',(0.,0.,1.));
#118257=DIRECTION('ref_axis',(0.,1.,0.));
#118258=DIRECTION('',(0.,1.23467863058847E-16,-1.));
#118259=DIRECTION('center_axis',(0.,0.,1.));
#118260=DIRECTION('ref_axis',(0.,1.,0.));
#118261=DIRECTION('center_axis',(0.,-1.23467863058847E-16,1.));
#118262=DIRECTION('ref_axis',(0.,-1.,-1.23467863058847E-16));
#118263=DIRECTION('',(-0.700366780446485,-0.713783141330072,-8.81292791474553E-17));
#118264=DIRECTION('center_axis',(0.,0.,1.));
#118265=DIRECTION('ref_axis',(0.,-1.,0.));
#118266=DIRECTION('',(0.700366780446451,0.713783141330105,8.81292791474594E-17));
#118267=DIRECTION('center_axis',(0.713783141330072,-0.700366780446485,-8.64727897391324E-17));
#118268=DIRECTION('ref_axis',(-4.34651812646493E-33,1.23467863058847E-16,
-1.));
#118269=DIRECTION('',(0.0133576962200374,0.0136135788205688,-0.999818104668739));
#118270=DIRECTION('center_axis',(0.,1.23467863058847E-16,-1.));
#118271=DIRECTION('ref_axis',(-1.,0.,0.));
#118272=DIRECTION('center_axis',(-7.1617481931302E-31,4.1541690210802E-45,
-1.));
#118273=DIRECTION('ref_axis',(5.80049578546342E-15,1.,-2.48920611114446E-60));
#118274=DIRECTION('',(-0.70592193778968,0.708289642552581,8.74510085926821E-17));
#118275=DIRECTION('center_axis',(-0.708289642552581,-0.70592193778968,-8.71586731452524E-17));
#118276=DIRECTION('ref_axis',(-0.70592193778968,0.708289642552581,-2.39349531189888E-34));
#118277=DIRECTION('',(0.0134621338381862,-0.0135072866467963,-0.999818145544461));
#118278=DIRECTION('center_axis',(-0.966292363511968,0.257447214431338,3.17864574162902E-17));
#118279=DIRECTION('ref_axis',(3.28952795412384E-17,-9.22328292945695E-37,
1.));
#118280=DIRECTION('',(0.,1.23467863058847E-16,-1.));
#118281=DIRECTION('',(-0.257447214431338,-0.966292363511968,-1.19306053212906E-16));
#118282=DIRECTION('center_axis',(0.260190353924911,-0.965557341499939,-1.19215301615779E-16));
#118283=DIRECTION('ref_axis',(-3.12701465369725E-33,1.23467863058847E-16,
-1.));
#118284=DIRECTION('',(0.965557341499939,0.260190353924911,3.21251469876339E-17));
#118285=DIRECTION('',(0.,1.23467863058847E-16,-1.));
#118286=DIRECTION('center_axis',(0.,0.,-1.));
#118287=DIRECTION('ref_axis',(0.,1.,0.));
#118288=DIRECTION('center_axis',(0.,0.,-1.));
#118289=DIRECTION('ref_axis',(0.,-1.,0.));
#118290=DIRECTION('center_axis',(-4.93476711729114E-30,-1.97232914692071E-43,
1.));
#118291=DIRECTION('ref_axis',(3.99680288865056E-14,-1.,0.));
#118292=DIRECTION('center_axis',(-0.966876318092686,-0.255245343760725,
-3.15145971498576E-17));
#118293=DIRECTION('ref_axis',(-0.255245343760725,0.966876318092686,-1.94208817023009E-34));
#118294=DIRECTION('',(0.255245343760725,-0.966876318092686,-1.1937815283711E-16));
#118295=DIRECTION('',(0.,1.23467863058847E-16,-1.));
#118296=DIRECTION('center_axis',(0.262389207151869,0.964962125666191,1.19141811588728E-16));
#118297=DIRECTION('ref_axis',(4.54065214350716E-16,-4.72048517437092E-33,
-1.));
#118298=DIRECTION('',(0.,1.23467863058847E-16,-1.));
#118299=DIRECTION('',(-0.964962125666191,0.262389207151869,3.23966346967465E-17));
#118300=DIRECTION('center_axis',(0.,0.,-1.));
#118301=DIRECTION('ref_axis',(0.,1.,0.));
#118302=DIRECTION('center_axis',(0.,0.,-1.));
#118303=DIRECTION('ref_axis',(0.,-1.,0.));
#118304=DIRECTION('center_axis',(0.,0.,1.));
#118305=DIRECTION('ref_axis',(0.,1.,0.));
#118306=DIRECTION('center_axis',(0.,0.,-1.));
#118307=DIRECTION('ref_axis',(0.,1.,0.));
#118308=DIRECTION('center_axis',(0.,0.,1.));
#118309=DIRECTION('ref_axis',(0.,1.,0.));
#118310=DIRECTION('',(0.,1.23467863058847E-16,-1.));
#118311=DIRECTION('center_axis',(0.,0.,1.));
#118312=DIRECTION('ref_axis',(0.,1.,0.));
#118313=DIRECTION('',(0.,1.23467863058847E-16,-1.));
#118314=DIRECTION('center_axis',(0.,0.,-1.));
#118315=DIRECTION('ref_axis',(0.,1.,0.));
#118316=DIRECTION('center_axis',(0.,0.,1.));
#118317=DIRECTION('ref_axis',(0.,1.,0.));
#118318=DIRECTION('',(0.,1.23467863058847E-16,-1.));
#118319=DIRECTION('center_axis',(0.,0.,1.));
#118320=DIRECTION('ref_axis',(0.,1.,0.));
#118321=DIRECTION('',(0.,1.23467863058847E-16,-1.));
#118322=DIRECTION('center_axis',(0.,0.,-1.));
#118323=DIRECTION('ref_axis',(0.,1.,0.));
#118324=DIRECTION('center_axis',(0.,0.,1.));
#118325=DIRECTION('ref_axis',(0.,1.,0.));
#118326=DIRECTION('',(0.,1.23467863058847E-16,-1.));
#118327=DIRECTION('center_axis',(0.,0.,1.));
#118328=DIRECTION('ref_axis',(0.,1.,0.));
#118329=DIRECTION('center_axis',(0.,0.,-1.));
#118330=DIRECTION('ref_axis',(0.,1.,0.));
#118331=DIRECTION('center_axis',(0.,0.,1.));
#118332=DIRECTION('ref_axis',(0.,1.,0.));
#118333=DIRECTION('',(0.,1.23467863058847E-16,-1.));
#118334=DIRECTION('center_axis',(0.,0.,1.));
#118335=DIRECTION('ref_axis',(0.,1.,0.));
#118336=DIRECTION('center_axis',(0.,1.21568833848598E-16,-1.));
#118337=DIRECTION('ref_axis',(0.,1.,1.21568833848598E-16));
#118338=DIRECTION('center_axis',(0.,-1.21568833848598E-16,1.));
#118339=DIRECTION('ref_axis',(0.,1.,1.21568833848598E-16));
#118340=DIRECTION('center_axis',(0.,-1.21568833848598E-16,1.));
#118341=DIRECTION('ref_axis',(0.,1.,1.21568833848598E-16));
#118342=DIRECTION('center_axis',(0.,0.,-1.));
#118343=DIRECTION('ref_axis',(0.,1.,0.));
#118344=DIRECTION('center_axis',(0.,0.,1.));
#118345=DIRECTION('ref_axis',(0.,1.,0.));
#118346=DIRECTION('',(0.,1.23467863058847E-16,-1.));
#118347=DIRECTION('center_axis',(0.,0.,1.));
#118348=DIRECTION('ref_axis',(0.,1.,0.));
#118349=DIRECTION('',(0.,1.23467863058847E-16,-1.));
#118350=DIRECTION('center_axis',(0.,0.,-1.));
#118351=DIRECTION('ref_axis',(0.,1.,0.));
#118352=DIRECTION('center_axis',(0.,0.,1.));
#118353=DIRECTION('ref_axis',(0.,1.,0.));
#118354=DIRECTION('center_axis',(0.,0.,1.));
#118355=DIRECTION('ref_axis',(0.,1.,0.));
#118356=DIRECTION('center_axis',(0.,0.,1.));
#118357=DIRECTION('ref_axis',(0.,1.,0.));
#118358=DIRECTION('center_axis',(9.45862666529894E-32,-7.24606518465966E-47,
1.));
#118359=DIRECTION('ref_axis',(-7.66080049574581E-16,-1.,2.91703841149741E-62));
#118360=DIRECTION('',(-0.000686915141868458,-0.0174388829355556,0.999847695156391));
#118361=DIRECTION('',(-0.0110444763156131,-0.0135131799871829,0.999847695156391));
#118362=DIRECTION('center_axis',(0.,0.,1.));
#118363=DIRECTION('ref_axis',(0.,1.,0.));
#118364=DIRECTION('',(-0.013481760241072,-0.011082807913809,0.999847695156391));
#118365=DIRECTION('center_axis',(4.38645965981435E-31,-1.5583835234929E-45,
1.));
#118366=DIRECTION('ref_axis',(-3.5527136788005E-15,-1.,1.24460305557223E-60));
#118367=DIRECTION('center_axis',(0.,0.,1.));
#118368=DIRECTION('ref_axis',(0.,1.,0.));
#118369=DIRECTION('center_axis',(1.89172533305981E-31,-2.89842607386392E-46,
1.));
#118370=DIRECTION('ref_axis',(-1.53216009914918E-15,-1.,7.38983064246011E-61));
#118371=DIRECTION('center_axis',(-0.49830877570858,-0.40695051295028,-0.765558387101415));
#118372=DIRECTION('ref_axis',(-0.616776838376874,-0.454175066156573,0.642892946705359));
#118373=DIRECTION('',(-0.0174387888650499,-0.000689299189283617,0.999847695156391));
#118374=DIRECTION('center_axis',(0.,0.,1.));
#118375=DIRECTION('ref_axis',(0.,1.,0.));
#118376=DIRECTION('center_axis',(-6.62103866570927E-31,-3.55057194048325E-45,
1.));
#118377=DIRECTION('ref_axis',(5.36256034702207E-15,-1.,-1.86690458335834E-60));
#118378=DIRECTION('',(-0.0174387888650499,0.000689299189283565,0.999847695156391));
#118379=DIRECTION('center_axis',(0.524694313011686,-0.428071664090414,0.735833220435214));
#118380=DIRECTION('ref_axis',(-0.586317116676987,0.444960261348595,0.676936189394668));
#118381=DIRECTION('',(-0.0134817602410721,0.0110828079138087,0.999847695156391));
#118382=DIRECTION('center_axis',(0.,0.,1.));
#118383=DIRECTION('ref_axis',(0.,1.,0.));
#118384=DIRECTION('',(-0.0109827961190146,0.0135633579861438,0.999847695156391));
#118385=DIRECTION('center_axis',(1.09661491495359E-30,-9.73989702183064E-45,
1.));
#118386=DIRECTION('ref_axis',(-8.88178419700126E-15,-1.,3.73380916671668E-60));
#118387=DIRECTION('center_axis',(0.,0.,1.));
#118388=DIRECTION('ref_axis',(0.,1.,0.));
#118389=DIRECTION('center_axis',(0.,0.,1.));
#118390=DIRECTION('ref_axis',(0.,-1.,0.));
#118391=DIRECTION('center_axis',(-0.424375096187792,0.528257078927607,-0.735425207820941));
#118392=DIRECTION('ref_axis',(-0.426055759035728,0.600170551540012,0.676957752933407));
#118393=DIRECTION('',(-0.003269361032546,0.0171434468206077,0.999847695156391));
#118394=DIRECTION('center_axis',(0.,-1.30002649721837E-16,1.));
#118395=DIRECTION('ref_axis',(0.,1.,1.30002649721837E-16));
#118396=DIRECTION('center_axis',(0.,-1.30002742469137E-16,1.));
#118397=DIRECTION('ref_axis',(0.,-1.,-1.30002742469137E-16));
#118398=DIRECTION('',(-0.0174387888650499,-0.000689299189283839,0.999847695156391));
#118399=DIRECTION('center_axis',(2.57572279529701E-31,-1.30052077910778E-16,
1.));
#118400=DIRECTION('ref_axis',(3.91196650355621E-14,-1.,-1.30052077910778E-16));
#118401=DIRECTION('',(-0.0174387888650499,0.000689299189283565,0.999847695156391));
#118402=DIRECTION('center_axis',(0.,0.,1.));
#118403=DIRECTION('ref_axis',(0.,1.,0.));
#118404=DIRECTION('center_axis',(2.14851878863042E-31,-3.73873238811768E-46,
1.));
#118405=DIRECTION('ref_axis',(-1.74014414391086E-15,-1.,-5.4451383681285E-61));
#118406=DIRECTION('center_axis',(-2.96506482541439E-31,-7.12056498031345E-46,
1.));
#118407=DIRECTION('ref_axis',(2.40148711734095E-15,-1.,1.0890276736257E-60));
#118408=DIRECTION('',(-0.013481760241072,0.0110828079138088,0.999847695156391));
#118409=DIRECTION('center_axis',(0.,0.,1.));
#118410=DIRECTION('ref_axis',(0.,1.,0.));
#118411=DIRECTION('center_axis',(0.,0.,1.));
#118412=DIRECTION('ref_axis',(0.,-1.,0.));
#118413=DIRECTION('center_axis',(0.,0.,1.));
#118414=DIRECTION('ref_axis',(0.,-1.,0.));
#118415=DIRECTION('',(-0.0109827961190146,0.0135633579861438,0.999847695156391));
#118416=DIRECTION('center_axis',(0.,0.,1.));
#118417=DIRECTION('ref_axis',(0.,1.,0.));
#118418=DIRECTION('center_axis',(-3.58086464771735E-31,-1.03853677447713E-45,
1.));
#118419=DIRECTION('ref_axis',(2.90024023985143E-15,-1.,1.55575381946529E-61));
#118420=DIRECTION('center_axis',(0.,0.,1.));
#118421=DIRECTION('ref_axis',(0.,-1.,0.));
#118422=DIRECTION('',(-0.0032693610325459,0.0171434468206077,0.999847695156391));
#118423=DIRECTION('center_axis',(0.,0.,1.));
#118424=DIRECTION('ref_axis',(0.,1.,0.));
#118425=DIRECTION('center_axis',(-2.14851878863041E-31,-3.73873238811767E-46,
1.));
#118426=DIRECTION('ref_axis',(1.74014414391086E-15,-1.,-6.22301527786114E-61));
#118427=DIRECTION('',(-0.000686915141868465,-0.0174388829355556,0.999847695156391));
#118428=DIRECTION('center_axis',(9.63646068259673E-31,-7.52109676045604E-45,
1.));
#118429=DIRECTION('ref_axis',(-7.80483313135807E-15,-1.,-3.73380916671668E-60));
#118430=DIRECTION('',(-0.0110444763156131,-0.0135131799871829,0.999847695156391));
#118431=DIRECTION('center_axis',(0.,0.,1.));
#118432=DIRECTION('ref_axis',(0.,1.,0.));
#118433=DIRECTION('center_axis',(1.09661491495359E-30,-9.73989702183063E-45,
1.));
#118434=DIRECTION('ref_axis',(-8.88178419700125E-15,-1.,2.48920611114446E-60));
#118435=DIRECTION('center_axis',(7.6763044046751E-31,-4.77254954069701E-45,
1.));
#118436=DIRECTION('ref_axis',(-6.21724893790088E-15,-1.,1.86690458335834E-60));
#118437=DIRECTION('',(-0.013481760241072,-0.011082807913809,0.999847695156391));
#118438=DIRECTION('center_axis',(0.,0.,1.));
#118439=DIRECTION('ref_axis',(0.,-1.,0.));
#118440=DIRECTION('center_axis',(-2.14851878863042E-31,-3.73873238811769E-46,
1.));
#118441=DIRECTION('ref_axis',(1.74014414391087E-15,-1.,2.33363072919793E-61));
#118442=DIRECTION('center_axis',(2.22379861906079E-31,-4.00531780142632E-46,
1.));
#118443=DIRECTION('ref_axis',(-1.80111533800572E-15,-1.,8.55664600705907E-61));
#118444=DIRECTION('center_axis',(0.,-1.30362731016209E-16,1.));
#118445=DIRECTION('ref_axis',(0.,1.,1.30362731016209E-16));
#118446=DIRECTION('center_axis',(0.,-1.30357480714758E-16,1.));
#118447=DIRECTION('ref_axis',(0.,-1.,-1.30357480714758E-16));
#118448=DIRECTION('center_axis',(9.64693417405135E-8,-8.44902797496882E-7,
0.999999999999638));
#118449=DIRECTION('ref_axis',(-0.131285471389456,0.9913446045656,8.50254852648554E-7));
#118450=DIRECTION('center_axis',(0.,1.23467863058847E-16,-1.));
#118451=DIRECTION('ref_axis',(-1.,0.,0.));
#118452=DIRECTION('center_axis',(0.,-1.21568833848598E-16,1.));
#118453=DIRECTION('ref_axis',(0.,1.,1.21568833848598E-16));
#118454=DIRECTION('center_axis',(2.34983671542145E-7,7.16718722586561E-6,
0.999999999974288));
#118455=DIRECTION('ref_axis',(-0.0297033272165618,-0.999558758803525,7.17100456465166E-6));
#118456=DIRECTION('center_axis',(0.,-1.21568833848598E-16,1.));
#118457=DIRECTION('ref_axis',(0.,1.,1.21568833848598E-16));
#118458=DIRECTION('center_axis',(0.,1.23467863058847E-16,-1.));
#118459=DIRECTION('ref_axis',(-1.,0.,0.));
#118460=DIRECTION('center_axis',(0.,0.,1.));
#118461=DIRECTION('ref_axis',(0.,1.,0.));
#118462=DIRECTION('center_axis',(0.,-1.23467863058847E-16,1.));
#118463=DIRECTION('ref_axis',(0.,-1.,-1.23467863058847E-16));
#118464=DIRECTION('center_axis',(0.,0.,1.));
#118465=DIRECTION('ref_axis',(0.,1.,0.));
#118466=DIRECTION('center_axis',(0.,1.23467863058847E-16,-1.));
#118467=DIRECTION('ref_axis',(-1.,0.,0.));
#118468=DIRECTION('center_axis',(0.,-1.30925187718918E-16,1.));
#118469=DIRECTION('ref_axis',(0.,1.,1.30925187718918E-16));
#118470=DIRECTION('center_axis',(0.,1.23467863058847E-16,-1.));
#118471=DIRECTION('ref_axis',(-1.,0.,0.));
#118472=DIRECTION('center_axis',(0.,-1.30925187718918E-16,1.));
#118473=DIRECTION('ref_axis',(0.,1.,1.30925187718918E-16));
#118474=DIRECTION('center_axis',(0.,1.23467863058847E-16,-1.));
#118475=DIRECTION('ref_axis',(-1.,0.,0.));
#118476=DIRECTION('center_axis',(0.,-1.21568833848598E-16,1.));
#118477=DIRECTION('ref_axis',(0.,1.,1.21568833848598E-16));
#118478=DIRECTION('center_axis',(0.,1.23467863058847E-16,-1.));
#118479=DIRECTION('ref_axis',(-1.,0.,0.));
#118480=DIRECTION('center_axis',(0.,-1.21568833848598E-16,1.));
#118481=DIRECTION('ref_axis',(0.,1.,1.21568833848598E-16));
#118482=DIRECTION('center_axis',(0.,1.23467863058847E-16,-1.));
#118483=DIRECTION('ref_axis',(-1.,0.,0.));
#118484=DIRECTION('center_axis',(0.,-1.21568833848598E-16,1.));
#118485=DIRECTION('ref_axis',(0.,1.,1.21568833848598E-16));
#118486=DIRECTION('center_axis',(0.,1.23467863058847E-16,-1.));
#118487=DIRECTION('ref_axis',(-1.,0.,0.));
#118488=DIRECTION('center_axis',(0.,-1.21568833848598E-16,1.));
#118489=DIRECTION('ref_axis',(0.,1.,1.21568833848598E-16));
#118490=DIRECTION('center_axis',(0.,1.23467863058847E-16,-1.));
#118491=DIRECTION('ref_axis',(-1.,0.,0.));
#118492=DIRECTION('center_axis',(7.1617481931302E-31,4.1541690210802E-45,
-1.));
#118493=DIRECTION('ref_axis',(-5.80049578546342E-15,1.,-2.48920611114446E-60));
#118494=DIRECTION('',(0.7059219377897,-0.708289642552561,-8.74510085926797E-17));
#118495=DIRECTION('center_axis',(0.,1.21568833848598E-16,-1.));
#118496=DIRECTION('ref_axis',(0.,1.,1.21568833848598E-16));
#118497=DIRECTION('center_axis',(0.,-1.21568833848598E-16,1.));
#118498=DIRECTION('ref_axis',(0.,1.,1.21568833848598E-16));
#118499=DIRECTION('center_axis',(0.,1.21568833848598E-16,-1.));
#118500=DIRECTION('ref_axis',(0.,1.,1.21568833848598E-16));
#118501=DIRECTION('center_axis',(0.,-1.21568833848598E-16,1.));
#118502=DIRECTION('ref_axis',(0.,1.,1.21568833848598E-16));
#118503=DIRECTION('center_axis',(0.,1.21568833848598E-16,-1.));
#118504=DIRECTION('ref_axis',(0.,1.,1.21568833848598E-16));
#118505=DIRECTION('center_axis',(0.,-1.21568833848598E-16,1.));
#118506=DIRECTION('ref_axis',(0.,1.,1.21568833848598E-16));
#118507=DIRECTION('center_axis',(0.,1.21568833848598E-16,-1.));
#118508=DIRECTION('ref_axis',(0.,1.,1.21568833848598E-16));
#118509=DIRECTION('center_axis',(0.,-1.21568833848598E-16,1.));
#118510=DIRECTION('ref_axis',(0.,1.,1.21568833848598E-16));
#118511=DIRECTION('center_axis',(0.,1.21568833848598E-16,-1.));
#118512=DIRECTION('ref_axis',(0.,1.,1.21568833848598E-16));
#118513=DIRECTION('center_axis',(0.,-1.21568833848598E-16,1.));
#118514=DIRECTION('ref_axis',(0.,1.,1.21568833848598E-16));
#118515=DIRECTION('center_axis',(-0.713783141330105,0.700366780446451,8.64727897391283E-17));
#118516=DIRECTION('ref_axis',(1.21147145025014E-16,-2.46367577887085E-33,
1.));
#118517=DIRECTION('',(-0.0133579710326364,-0.0136138588975274,0.999818097183587));
#118518=DIRECTION('center_axis',(0.,0.,-1.));
#118519=DIRECTION('ref_axis',(0.705510697508504,-0.708699270283993,0.));
#118520=DIRECTION('',(-0.0134623247494151,0.0135074781986352,0.999818140386068));
#118521=DIRECTION('center_axis',(0.708289642552561,0.7059219377897,8.71586731452549E-17));
#118522=DIRECTION('ref_axis',(-2.22539097861278E-34,1.23467863058847E-16,
-1.));
#118523=DIRECTION('center_axis',(0.,0.,-1.));
#118524=DIRECTION('ref_axis',(0.,1.,0.));
#118525=DIRECTION('center_axis',(0.,0.,-1.));
#118526=DIRECTION('ref_axis',(0.,1.,0.));
#118527=DIRECTION('',(0.,1.23467863058847E-16,-1.));
#118528=DIRECTION('center_axis',(0.,0.,1.));
#118529=DIRECTION('ref_axis',(0.,1.,0.));
#118530=DIRECTION('',(0.,1.23467863058847E-16,-1.));
#118531=DIRECTION('center_axis',(0.,0.,-1.));
#118532=DIRECTION('ref_axis',(0.,1.,0.));
#118533=DIRECTION('center_axis',(0.,0.,1.));
#118534=DIRECTION('ref_axis',(0.,1.,0.));
#118535=DIRECTION('',(0.,1.23467863058847E-16,-1.));
#118536=DIRECTION('center_axis',(0.,0.,-1.));
#118537=DIRECTION('ref_axis',(0.,1.,0.));
#118538=DIRECTION('center_axis',(0.,0.,1.));
#118539=DIRECTION('ref_axis',(0.,1.,0.));
#118540=DIRECTION('',(0.,1.23467863058847E-16,-1.));
#118541=DIRECTION('center_axis',(0.,1.22914743790472E-16,-1.));
#118542=DIRECTION('ref_axis',(0.,1.,1.22914743790472E-16));
#118543=DIRECTION('center_axis',(0.,-1.22914743790472E-16,1.));
#118544=DIRECTION('ref_axis',(0.,1.,1.22914743790472E-16));
#118545=DIRECTION('center_axis',(0.,0.,-1.));
#118546=DIRECTION('ref_axis',(0.,1.,0.));
#118547=DIRECTION('',(0.,1.23467863058847E-16,-1.));
#118548=DIRECTION('center_axis',(0.,0.,1.));
#118549=DIRECTION('ref_axis',(0.,1.,0.));
#118550=DIRECTION('',(0.,1.23467863058847E-16,-1.));
#118551=DIRECTION('center_axis',(0.,0.,-1.));
#118552=DIRECTION('ref_axis',(0.,1.,0.));
#118553=DIRECTION('center_axis',(0.,0.,1.));
#118554=DIRECTION('ref_axis',(0.,1.,0.));
#118555=DIRECTION('center_axis',(0.,0.,-1.));
#118556=DIRECTION('ref_axis',(0.,1.,0.));
#118557=DIRECTION('',(0.,1.23467863058847E-16,-1.));
#118558=DIRECTION('center_axis',(0.,0.,1.));
#118559=DIRECTION('ref_axis',(0.,1.,0.));
#118560=DIRECTION('',(0.,1.23467863058847E-16,-1.));
#118561=DIRECTION('center_axis',(0.,1.23467863058847E-16,-1.));
#118562=DIRECTION('ref_axis',(-1.,0.,0.));
#118563=DIRECTION('center_axis',(0.,0.,1.));
#118564=DIRECTION('ref_axis',(0.,1.,0.));
#118565=DIRECTION('center_axis',(0.,0.,-1.));
#118566=DIRECTION('ref_axis',(0.,1.,0.));
#118567=DIRECTION('',(-2.13730336808358E-18,-0.0174524064372818,-0.999847695156391));
#118568=DIRECTION('center_axis',(0.,0.,1.));
#118569=DIRECTION('ref_axis',(0.,-1.,0.));
#118570=DIRECTION('center_axis',(0.,0.,1.));
#118571=DIRECTION('ref_axis',(0.,-1.,0.));
#118572=DIRECTION('center_axis',(0.,1.23467863058847E-16,-1.));
#118573=DIRECTION('ref_axis',(-1.,0.,0.));
#118574=DIRECTION('center_axis',(0.,0.,1.));
#118575=DIRECTION('ref_axis',(0.,1.,0.));
#118576=DIRECTION('center_axis',(0.,0.,-1.));
#118577=DIRECTION('ref_axis',(0.,1.,0.));
#118578=DIRECTION('',(-2.13730336808358E-18,-0.0174524064372818,-0.999847695156391));
#118579=DIRECTION('center_axis',(0.,-1.23467863058847E-16,1.));
#118580=DIRECTION('ref_axis',(0.,-1.,-1.23467863058847E-16));
#118581=DIRECTION('center_axis',(0.713783141330072,-0.700366780446485,-8.64727897391324E-17));
#118582=DIRECTION('ref_axis',(-4.34651812646493E-33,1.23467863058847E-16,
-1.));
#118583=DIRECTION('center_axis',(-0.713783141330105,0.700366780446451,8.64727897391283E-17));
#118584=DIRECTION('ref_axis',(1.21147145025014E-16,-2.46367577887085E-33,
1.));
#118585=DIRECTION('center_axis',(0.,0.,1.));
#118586=DIRECTION('ref_axis',(0.,-1.,0.));
#118587=DIRECTION('center_axis',(0.,1.23467863058847E-16,-1.));
#118588=DIRECTION('ref_axis',(-1.,0.,0.));
#118589=DIRECTION('center_axis',(0.,0.,-1.));
#118590=DIRECTION('ref_axis',(0.,1.,0.));
#118591=DIRECTION('center_axis',(-0.708289642552581,-0.70592193778968,-8.71586731452524E-17));
#118592=DIRECTION('ref_axis',(-0.70592193778968,0.708289642552581,-2.39349531189888E-34));
#118593=DIRECTION('center_axis',(0.708289642552561,0.7059219377897,8.71586731452549E-17));
#118594=DIRECTION('ref_axis',(-2.22539097861278E-34,1.23467863058847E-16,
-1.));
#118595=DIRECTION('center_axis',(0.,0.,1.));
#118596=DIRECTION('ref_axis',(0.,-1.,0.));
#118597=DIRECTION('center_axis',(-0.966292363511968,0.257447214431338,3.17864574162902E-17));
#118598=DIRECTION('ref_axis',(3.28952795412384E-17,-9.22328292945695E-37,
1.));
#118599=DIRECTION('center_axis',(0.260190353924911,-0.965557341499939,-1.19215301615779E-16));
#118600=DIRECTION('ref_axis',(-3.12701465369725E-33,1.23467863058847E-16,
-1.));
#118601=DIRECTION('center_axis',(0.,0.,-1.));
#118602=DIRECTION('ref_axis',(0.,1.,0.));
#118603=DIRECTION('center_axis',(-0.966876318092686,-0.255245343760725,
-3.15145971498576E-17));
#118604=DIRECTION('ref_axis',(-0.255245343760725,0.966876318092686,-1.94208817023009E-34));
#118605=DIRECTION('center_axis',(0.262389207151869,0.964962125666191,1.19141811588728E-16));
#118606=DIRECTION('ref_axis',(4.54065214350716E-16,-4.72048517437092E-33,
-1.));
#118607=DIRECTION('center_axis',(0.,0.,-1.));
#118608=DIRECTION('ref_axis',(0.,1.,0.));
#118609=DIRECTION('center_axis',(0.,0.,-1.));
#118610=DIRECTION('ref_axis',(0.,1.,0.));
#118611=DIRECTION('',(0.,1.23467863058847E-16,-1.));
#118612=DIRECTION('center_axis',(0.,0.,1.));
#118613=DIRECTION('ref_axis',(0.,1.,0.));
#118614=DIRECTION('',(0.,1.23467863058847E-16,-1.));
#118615=DIRECTION('center_axis',(0.,0.,-1.));
#118616=DIRECTION('ref_axis',(0.,1.,0.));
#118617=DIRECTION('',(0.,1.23467863058847E-16,-1.));
#118618=DIRECTION('center_axis',(0.,0.,1.));
#118619=DIRECTION('ref_axis',(0.,1.,0.));
#118620=DIRECTION('center_axis',(0.,1.22229112323298E-16,-1.));
#118621=DIRECTION('ref_axis',(0.,1.,1.22229112323298E-16));
#118622=DIRECTION('',(0.,1.23467863058847E-16,-1.));
#118623=DIRECTION('center_axis',(0.,-1.22229112323298E-16,1.));
#118624=DIRECTION('ref_axis',(0.,1.,1.22229112323298E-16));
#118625=DIRECTION('center_axis',(0.,0.,-1.));
#118626=DIRECTION('ref_axis',(0.,1.,0.));
#118627=DIRECTION('',(0.,1.23467863058847E-16,-1.));
#118628=DIRECTION('center_axis',(0.,0.,1.));
#118629=DIRECTION('ref_axis',(0.,1.,0.));
#118630=DIRECTION('center_axis',(0.,0.,-1.));
#118631=DIRECTION('ref_axis',(0.,1.,0.));
#118632=DIRECTION('',(0.,1.23467863058847E-16,-1.));
#118633=DIRECTION('center_axis',(0.,0.,1.));
#118634=DIRECTION('ref_axis',(0.,1.,0.));
#118635=DIRECTION('center_axis',(0.,0.,-1.));
#118636=DIRECTION('ref_axis',(0.,1.,0.));
#118637=DIRECTION('',(0.,1.23467863058847E-16,-1.));
#118638=DIRECTION('center_axis',(0.,0.,1.));
#118639=DIRECTION('ref_axis',(0.,1.,0.));
#118640=DIRECTION('center_axis',(0.,0.,-1.));
#118641=DIRECTION('ref_axis',(0.,1.,0.));
#118642=DIRECTION('center_axis',(0.,0.,1.));
#118643=DIRECTION('ref_axis',(0.,1.,0.));
#118644=DIRECTION('',(0.,1.23467863058847E-16,-1.));
#118645=DIRECTION('center_axis',(0.,0.,-1.));
#118646=DIRECTION('ref_axis',(0.,1.,0.));
#118647=DIRECTION('',(0.,1.23467863058847E-16,-1.));
#118648=DIRECTION('center_axis',(0.,0.,1.));
#118649=DIRECTION('ref_axis',(0.,1.,0.));
#118650=DIRECTION('',(0.,1.23467863058847E-16,-1.));
#118651=DIRECTION('center_axis',(0.,0.,-1.));
#118652=DIRECTION('ref_axis',(0.,1.,0.));
#118653=DIRECTION('',(0.,1.23467863058847E-16,-1.));
#118654=DIRECTION('center_axis',(0.,0.,1.));
#118655=DIRECTION('ref_axis',(0.,1.,0.));
#118656=DIRECTION('',(0.,1.23467863058847E-16,-1.));
#118657=DIRECTION('center_axis',(0.,0.,-1.));
#118658=DIRECTION('ref_axis',(0.,1.,0.));
#118659=DIRECTION('center_axis',(0.,0.,1.));
#118660=DIRECTION('ref_axis',(0.,1.,0.));
#118661=DIRECTION('',(0.,1.23467863058847E-16,-1.));
#118662=DIRECTION('center_axis',(0.,0.,-1.));
#118663=DIRECTION('ref_axis',(0.,1.,0.));
#118664=DIRECTION('center_axis',(0.,0.,1.));
#118665=DIRECTION('ref_axis',(0.,1.,0.));
#118666=DIRECTION('',(0.,1.23467863058847E-16,-1.));
#118667=DIRECTION('center_axis',(0.,1.22014183466588E-16,-1.));
#118668=DIRECTION('ref_axis',(0.,1.,1.22014183466588E-16));
#118669=DIRECTION('center_axis',(0.,-1.22014183466588E-16,1.));
#118670=DIRECTION('ref_axis',(0.,1.,1.22014183466588E-16));
#118671=DIRECTION('',(0.,1.23467863058847E-16,-1.));
#118672=DIRECTION('center_axis',(0.,0.,-1.));
#118673=DIRECTION('ref_axis',(0.,1.,0.));
#118674=DIRECTION('center_axis',(0.,0.,1.));
#118675=DIRECTION('ref_axis',(0.,1.,0.));
#118676=DIRECTION('',(0.,1.23467863058847E-16,-1.));
#118677=DIRECTION('center_axis',(0.,0.,-1.));
#118678=DIRECTION('ref_axis',(0.,1.,0.));
#118679=DIRECTION('center_axis',(0.,0.,1.));
#118680=DIRECTION('ref_axis',(0.,1.,0.));
#118681=DIRECTION('',(-0.459549353210719,-0.545727376107149,0.700711083779054));
#118682=DIRECTION('',(-0.595667475496749,-0.42912133257888,0.678995685230073));
#118683=DIRECTION('',(-0.580626046021037,0.392567954055243,0.713276801901518));
#118684=DIRECTION('',(0.484796374610729,-0.46748816331627,-0.739207205270264));
#118685=DIRECTION('center_axis',(0.,0.,1.));
#118686=DIRECTION('ref_axis',(0.,1.,0.));
#118687=DIRECTION('',(-0.0110444763156131,-0.0135131799871829,0.999847695156391));
#118688=DIRECTION('',(-0.000686915141868466,-0.0174388829355556,0.999847695156391));
#118689=DIRECTION('center_axis',(0.,0.,1.));
#118690=DIRECTION('ref_axis',(0.,1.,0.));
#118691=DIRECTION('',(-0.013481760241072,-0.011082807913809,0.999847695156391));
#118692=DIRECTION('center_axis',(0.,0.,1.));
#118693=DIRECTION('ref_axis',(0.,1.,0.));
#118694=DIRECTION('',(-0.0174387888650499,-0.000689299189283616,0.999847695156391));
#118695=DIRECTION('center_axis',(0.,0.,1.));
#118696=DIRECTION('ref_axis',(0.,1.,0.));
#118697=DIRECTION('',(-0.0134817602410721,0.0110828079138087,0.999847695156391));
#118698=DIRECTION('',(-0.0174387888650499,0.000689299189283565,0.999847695156391));
#118699=DIRECTION('center_axis',(0.,0.,1.));
#118700=DIRECTION('ref_axis',(0.,1.,0.));
#118701=DIRECTION('',(-0.0109827961190146,0.0135633579861438,0.999847695156391));
#118702=DIRECTION('center_axis',(0.,0.,1.));
#118703=DIRECTION('ref_axis',(0.,1.,0.));
#118704=DIRECTION('',(-0.00326936103254579,0.0171434468206077,0.999847695156391));
#118705=DIRECTION('center_axis',(0.,-1.29698951474901E-16,1.));
#118706=DIRECTION('ref_axis',(0.,1.,1.29698951474901E-16));
#118707=DIRECTION('',(-0.0174387888650499,-0.000689299189283839,0.999847695156391));
#118708=DIRECTION('center_axis',(0.,-1.29698951474901E-16,1.));
#118709=DIRECTION('ref_axis',(0.,1.,1.29698951474901E-16));
#118710=DIRECTION('',(-0.0174387888650499,0.000689299189283565,0.999847695156391));
#118711=DIRECTION('center_axis',(0.,0.,1.));
#118712=DIRECTION('ref_axis',(0.,1.,0.));
#118713=DIRECTION('center_axis',(0.,0.,1.));
#118714=DIRECTION('ref_axis',(0.,1.,0.));
#118715=DIRECTION('',(-0.0134817602410721,0.0110828079138088,0.999847695156391));
#118716=DIRECTION('center_axis',(0.,0.,1.));
#118717=DIRECTION('ref_axis',(0.,1.,0.));
#118718=DIRECTION('center_axis',(0.,0.,1.));
#118719=DIRECTION('ref_axis',(0.,1.,0.));
#118720=DIRECTION('',(-0.0109827961190146,0.0135633579861438,0.999847695156391));
#118721=DIRECTION('center_axis',(0.,0.,1.));
#118722=DIRECTION('ref_axis',(0.,1.,0.));
#118723=DIRECTION('center_axis',(0.,0.,1.));
#118724=DIRECTION('ref_axis',(0.,1.,0.));
#118725=DIRECTION('',(-0.0032693610325459,0.0171434468206077,0.999847695156391));
#118726=DIRECTION('center_axis',(0.,0.,1.));
#118727=DIRECTION('ref_axis',(0.,1.,0.));
#118728=DIRECTION('',(-0.000686915141868473,-0.0174388829355556,0.999847695156391));
#118729=DIRECTION('center_axis',(0.,0.,1.));
#118730=DIRECTION('ref_axis',(0.,1.,0.));
#118731=DIRECTION('',(-0.0110444763156131,-0.0135131799871829,0.999847695156391));
#118732=DIRECTION('center_axis',(0.,0.,1.));
#118733=DIRECTION('ref_axis',(0.,1.,0.));
#118734=DIRECTION('center_axis',(0.,0.,1.));
#118735=DIRECTION('ref_axis',(0.,1.,0.));
#118736=DIRECTION('',(-0.013481760241072,-0.011082807913809,0.999847695156391));
#118737=DIRECTION('center_axis',(0.,0.,1.));
#118738=DIRECTION('ref_axis',(0.,-1.,0.));
#118739=DIRECTION('center_axis',(0.,0.,1.));
#118740=DIRECTION('ref_axis',(0.,-1.,0.));
#118741=DIRECTION('center_axis',(0.,-1.30057350048735E-16,1.));
#118742=DIRECTION('ref_axis',(0.,1.,1.30057350048735E-16));
#118743=DIRECTION('center_axis',(0.,1.23467863058847E-16,-1.));
#118744=DIRECTION('ref_axis',(-1.,0.,0.));
#118745=DIRECTION('center_axis',(0.,-1.23467863058847E-16,1.));
#118746=DIRECTION('ref_axis',(0.,-1.,-1.23467863058847E-16));
#118747=DIRECTION('center_axis',(0.,1.22914743790472E-16,-1.));
#118748=DIRECTION('ref_axis',(0.,1.,1.22914743790472E-16));
#118749=DIRECTION('center_axis',(0.,-1.22914743790472E-16,1.));
#118750=DIRECTION('ref_axis',(0.,1.,1.22914743790472E-16));
#118751=DIRECTION('center_axis',(0.,1.22914743790472E-16,-1.));
#118752=DIRECTION('ref_axis',(0.,1.,1.22914743790472E-16));
#118753=DIRECTION('center_axis',(0.,-1.22914743790472E-16,1.));
#118754=DIRECTION('ref_axis',(0.,1.,1.22914743790472E-16));
#118755=DIRECTION('center_axis',(0.,1.22914743790472E-16,-1.));
#118756=DIRECTION('ref_axis',(0.,1.,1.22914743790472E-16));
#118757=DIRECTION('center_axis',(0.,-1.22914743790472E-16,1.));
#118758=DIRECTION('ref_axis',(0.,1.,1.22914743790472E-16));
#118759=DIRECTION('center_axis',(0.,1.22914743790472E-16,-1.));
#118760=DIRECTION('ref_axis',(0.,1.,1.22914743790472E-16));
#118761=DIRECTION('center_axis',(0.,-1.22914743790472E-16,1.));
#118762=DIRECTION('ref_axis',(0.,1.,1.22914743790472E-16));
#118763=DIRECTION('center_axis',(0.,1.22914743790472E-16,-1.));
#118764=DIRECTION('ref_axis',(0.,1.,1.22914743790472E-16));
#118765=DIRECTION('center_axis',(0.,-1.22914743790472E-16,1.));
#118766=DIRECTION('ref_axis',(0.,1.,1.22914743790472E-16));
#118767=DIRECTION('center_axis',(3.29883322342201E-16,1.,1.23467863058847E-16));
#118768=DIRECTION('ref_axis',(1.,-3.29883322342202E-16,0.));
#118769=DIRECTION('',(-1.,3.29883322342202E-16,0.));
#118770=DIRECTION('center_axis',(3.29883322342201E-16,-1.,-1.23467863058847E-16));
#118771=DIRECTION('ref_axis',(1.07891492167253E-48,1.23467863058847E-16,
-1.));
#118772=DIRECTION('',(1.,3.29883322342202E-16,0.));
#118773=DIRECTION('center_axis',(3.71118737634973E-16,1.,1.23467863058847E-16));
#118774=DIRECTION('ref_axis',(1.,-3.71118737634973E-16,0.));
#118775=DIRECTION('',(-1.,3.71118737634973E-16,0.));
#118776=DIRECTION('center_axis',(3.71118737634973E-16,-1.,-1.23467863058847E-16));
#118777=DIRECTION('ref_axis',(9.86109193995912E-49,1.23467863058847E-16,
-1.));
#118778=DIRECTION('',(1.,3.71118737634973E-16,0.));
#118779=DIRECTION('center_axis',(5.72252063890675E-16,1.,1.23467863058847E-16));
#118780=DIRECTION('ref_axis',(1.,-5.72252063890675E-16,0.));
#118781=DIRECTION('',(-1.,5.72252063890675E-16,0.));
#118782=DIRECTION('center_axis',(-1.90750687963558E-16,-1.,-1.23467863058847E-16));
#118783=DIRECTION('ref_axis',(-1.,1.90750687963558E-16,0.));
#118784=DIRECTION('',(1.,-1.90750687963558E-16,0.));
#118785=DIRECTION('center_axis',(-1.23706245878324E-16,-1.,-1.23467863058847E-16));
#118786=DIRECTION('ref_axis',(-1.,1.23706245878324E-16,0.));
#118787=DIRECTION('',(1.,-1.23706245878324E-16,0.));
#118788=DIRECTION('center_axis',(-1.23706245878324E-16,1.,1.23467863058847E-16));
#118789=DIRECTION('ref_axis',(1.,1.23706245878324E-16,0.));
#118790=DIRECTION('',(-1.,-1.23706245878324E-16,0.));
#118791=DIRECTION('center_axis',(4.76876719908896E-16,-1.,-1.23467863058847E-16));
#118792=DIRECTION('ref_axis',(8.72767235901404E-49,1.23467863058847E-16,
-1.));
#118793=DIRECTION('',(1.,4.76876719908896E-16,0.));
#118794=DIRECTION('center_axis',(-9.53753439817791E-17,1.,1.23467863058847E-16));
#118795=DIRECTION('ref_axis',(4.60419424770999E-49,1.23467863058847E-16,
-1.));
#118796=DIRECTION('',(-1.,-9.53753439817791E-17,0.));
#118797=DIRECTION('center_axis',(0.,1.35726946151947E-16,-1.));
#118798=DIRECTION('ref_axis',(0.,1.,1.35726946151947E-16));
#118799=DIRECTION('center_axis',(0.,-1.35726946151947E-16,1.));
#118800=DIRECTION('ref_axis',(0.,1.,1.35726946151947E-16));
#118801=DIRECTION('center_axis',(0.,1.22914743790472E-16,-1.));
#118802=DIRECTION('ref_axis',(0.,1.,1.22914743790472E-16));
#118803=DIRECTION('center_axis',(0.,-1.22914743790472E-16,1.));
#118804=DIRECTION('ref_axis',(0.,1.,1.22914743790472E-16));
#118805=DIRECTION('center_axis',(0.,1.34087697701688E-16,-1.));
#118806=DIRECTION('ref_axis',(0.,1.,1.34087697701688E-16));
#118807=DIRECTION('center_axis',(1.86759697420978E-30,1.34087697701688E-16,
-1.));
#118808=DIRECTION('ref_axis',(1.75859327100625E-13,1.,1.34087697701688E-16));
#118809=DIRECTION('center_axis',(0.,-1.34087697701688E-16,1.));
#118810=DIRECTION('ref_axis',(0.,1.,1.34087697701688E-16));
#118811=DIRECTION('center_axis',(3.29883322342201E-16,1.,1.23467863058847E-16));
#118812=DIRECTION('ref_axis',(1.,-3.29883322342202E-16,0.));
#118813=DIRECTION('',(-1.,3.29883322342202E-16,0.));
#118814=DIRECTION('center_axis',(3.29883322342201E-16,-1.,-1.23467863058847E-16));
#118815=DIRECTION('ref_axis',(1.07891492167253E-48,1.23467863058847E-16,
-1.));
#118816=DIRECTION('',(1.,3.29883322342202E-16,0.));
#118817=DIRECTION('center_axis',(3.29883322342198E-16,1.,1.23467863058847E-16));
#118818=DIRECTION('ref_axis',(1.,-3.29883322342198E-16,0.));
#118819=DIRECTION('',(-1.,3.29883322342198E-16,0.));
#118820=DIRECTION('center_axis',(3.29883322342198E-16,-1.,-1.23467863058847E-16));
#118821=DIRECTION('ref_axis',(8.54897290170095E-49,1.23467863058847E-16,
-1.));
#118822=DIRECTION('',(1.,3.29883322342198E-16,0.));
#118823=DIRECTION('center_axis',(3.71118737634973E-16,1.,1.23467863058847E-16));
#118824=DIRECTION('ref_axis',(1.,-3.71118737634973E-16,0.));
#118825=DIRECTION('',(-1.,3.71118737634973E-16,0.));
#118826=DIRECTION('center_axis',(3.71118737634973E-16,-1.,-1.23467863058847E-16));
#118827=DIRECTION('ref_axis',(9.86109193995912E-49,1.23467863058847E-16,
-1.));
#118828=DIRECTION('',(1.,3.71118737634973E-16,0.));
#118829=DIRECTION('center_axis',(3.71118737634973E-16,1.,1.23467863058847E-16));
#118830=DIRECTION('ref_axis',(1.,-3.71118737634973E-16,0.));
#118831=DIRECTION('',(-1.,3.71118737634973E-16,0.));
#118832=DIRECTION('center_axis',(3.71118737634973E-16,-1.,-1.23467863058847E-16));
#118833=DIRECTION('ref_axis',(9.86109193995912E-49,1.23467863058847E-16,
-1.));
#118834=DIRECTION('',(1.,3.71118737634973E-16,0.));
#118835=DIRECTION('center_axis',(5.72252063890675E-16,1.,1.23467863058847E-16));
#118836=DIRECTION('ref_axis',(1.,-5.72252063890675E-16,0.));
#118837=DIRECTION('',(-1.,5.72252063890675E-16,0.));
#118838=DIRECTION('center_axis',(-1.90750687963558E-16,-1.,-1.23467863058847E-16));
#118839=DIRECTION('ref_axis',(-1.,1.90750687963558E-16,0.));
#118840=DIRECTION('',(1.,-1.90750687963558E-16,0.));
#118841=DIRECTION('center_axis',(-1.23706245878324E-16,-1.,-1.23467863058847E-16));
#118842=DIRECTION('ref_axis',(-1.,1.23706245878324E-16,0.));
#118843=DIRECTION('',(1.,-1.23706245878324E-16,0.));
#118844=DIRECTION('center_axis',(-1.23706245878324E-16,1.,1.23467863058847E-16));
#118845=DIRECTION('ref_axis',(1.,1.23706245878324E-16,0.));
#118846=DIRECTION('',(-1.,-1.23706245878324E-16,0.));
#118847=DIRECTION('center_axis',(4.76876719908896E-16,-1.,-1.23467863058847E-16));
#118848=DIRECTION('ref_axis',(8.72767235901404E-49,1.23467863058847E-16,
-1.));
#118849=DIRECTION('',(1.,4.76876719908896E-16,0.));
#118850=DIRECTION('center_axis',(-9.53753439817791E-17,1.,1.23467863058847E-16));
#118851=DIRECTION('ref_axis',(4.60419424770999E-49,1.23467863058847E-16,
-1.));
#118852=DIRECTION('',(-1.,-9.53753439817791E-17,0.));
#118853=DIRECTION('center_axis',(0.,1.35726946151947E-16,-1.));
#118854=DIRECTION('ref_axis',(0.,1.,1.35726946151947E-16));
#118855=DIRECTION('center_axis',(0.,-1.35726946151947E-16,1.));
#118856=DIRECTION('ref_axis',(0.,1.,1.35726946151947E-16));
#118857=DIRECTION('center_axis',(0.,1.35726946151947E-16,-1.));
#118858=DIRECTION('ref_axis',(0.,1.,1.35726946151947E-16));
#118859=DIRECTION('center_axis',(0.,-1.35726946151947E-16,1.));
#118860=DIRECTION('ref_axis',(0.,1.,1.35726946151947E-16));
#118861=DIRECTION('center_axis',(0.,1.22914743790472E-16,-1.));
#118862=DIRECTION('ref_axis',(0.,1.,1.22914743790472E-16));
#118863=DIRECTION('center_axis',(0.,-1.22914743790472E-16,1.));
#118864=DIRECTION('ref_axis',(0.,1.,1.22914743790472E-16));
#118865=DIRECTION('center_axis',(0.,1.22914743790472E-16,-1.));
#118866=DIRECTION('ref_axis',(0.,1.,1.22914743790472E-16));
#118867=DIRECTION('center_axis',(0.,-1.22914743790472E-16,1.));
#118868=DIRECTION('ref_axis',(0.,1.,1.22914743790472E-16));
#118869=DIRECTION('center_axis',(0.,0.,-1.));
#118870=DIRECTION('ref_axis',(0.,1.,0.));
#118871=DIRECTION('center_axis',(0.,0.,1.));
#118872=DIRECTION('ref_axis',(0.,1.,0.));
#118873=DIRECTION('center_axis',(0.,0.,-1.));
#118874=DIRECTION('ref_axis',(0.,1.,0.));
#118875=DIRECTION('center_axis',(0.,0.,1.));
#118876=DIRECTION('ref_axis',(0.,1.,0.));
#118877=DIRECTION('center_axis',(0.,0.,-1.));
#118878=DIRECTION('ref_axis',(0.,1.,0.));
#118879=DIRECTION('center_axis',(0.,0.,1.));
#118880=DIRECTION('ref_axis',(0.,1.,0.));
#118881=DIRECTION('center_axis',(0.,0.,-1.));
#118882=DIRECTION('ref_axis',(0.,1.,0.));
#118883=DIRECTION('center_axis',(0.,0.,1.));
#118884=DIRECTION('ref_axis',(0.,1.,0.));
#118885=DIRECTION('center_axis',(3.29883322342201E-16,1.,1.23467863058847E-16));
#118886=DIRECTION('ref_axis',(1.,-3.29883322342202E-16,0.));
#118887=DIRECTION('',(-1.,3.29883322342202E-16,0.));
#118888=DIRECTION('center_axis',(3.29883322342201E-16,1.,1.23467863058847E-16));
#118889=DIRECTION('ref_axis',(1.,-3.29883322342202E-16,0.));
#118890=DIRECTION('',(-1.,3.29883322342202E-16,0.));
#118891=DIRECTION('center_axis',(3.29883322342201E-16,-1.,-1.23467863058847E-16));
#118892=DIRECTION('ref_axis',(1.07891492167253E-48,1.23467863058847E-16,
-1.));
#118893=DIRECTION('',(1.,3.29883322342202E-16,0.));
#118894=DIRECTION('center_axis',(3.29883322342201E-16,-1.,-1.23467863058847E-16));
#118895=DIRECTION('ref_axis',(1.07891492167253E-48,1.23467863058847E-16,
-1.));
#118896=DIRECTION('',(1.,3.29883322342202E-16,0.));
#118897=DIRECTION('center_axis',(3.29883322342198E-16,1.,1.23467863058847E-16));
#118898=DIRECTION('ref_axis',(1.,-3.29883322342198E-16,0.));
#118899=DIRECTION('',(-1.,3.29883322342198E-16,0.));
#118900=DIRECTION('center_axis',(3.29883322342198E-16,1.,1.23467863058847E-16));
#118901=DIRECTION('ref_axis',(1.,-3.29883322342198E-16,0.));
#118902=DIRECTION('',(-1.,3.29883322342198E-16,0.));
#118903=DIRECTION('center_axis',(3.29883322342198E-16,-1.,-1.23467863058847E-16));
#118904=DIRECTION('ref_axis',(8.54897290170095E-49,1.23467863058847E-16,
-1.));
#118905=DIRECTION('',(1.,3.29883322342198E-16,0.));
#118906=DIRECTION('center_axis',(3.29883322342198E-16,-1.,-1.23467863058847E-16));
#118907=DIRECTION('ref_axis',(8.54897290170095E-49,1.23467863058847E-16,
-1.));
#118908=DIRECTION('',(1.,3.29883322342198E-16,0.));
#118909=DIRECTION('center_axis',(3.71118737634973E-16,1.,1.23467863058847E-16));
#118910=DIRECTION('ref_axis',(1.,-3.71118737634973E-16,0.));
#118911=DIRECTION('',(-1.,3.71118737634973E-16,0.));
#118912=DIRECTION('center_axis',(3.71118737634973E-16,1.,1.23467863058847E-16));
#118913=DIRECTION('ref_axis',(1.,-3.71118737634973E-16,0.));
#118914=DIRECTION('',(-1.,3.71118737634973E-16,0.));
#118915=DIRECTION('center_axis',(3.71118737634973E-16,-1.,-1.23467863058847E-16));
#118916=DIRECTION('ref_axis',(9.86109193995912E-49,1.23467863058847E-16,
-1.));
#118917=DIRECTION('',(1.,3.71118737634973E-16,0.));
#118918=DIRECTION('center_axis',(3.71118737634973E-16,-1.,-1.23467863058847E-16));
#118919=DIRECTION('ref_axis',(9.86109193995912E-49,1.23467863058847E-16,
-1.));
#118920=DIRECTION('',(1.,3.71118737634973E-16,0.));
#118921=DIRECTION('center_axis',(3.71118737634973E-16,1.,1.23467863058847E-16));
#118922=DIRECTION('ref_axis',(1.,-3.71118737634973E-16,0.));
#118923=DIRECTION('',(-1.,3.71118737634973E-16,0.));
#118924=DIRECTION('center_axis',(3.71118737634973E-16,1.,1.23467863058847E-16));
#118925=DIRECTION('ref_axis',(1.,-3.71118737634973E-16,0.));
#118926=DIRECTION('',(-1.,3.71118737634973E-16,0.));
#118927=DIRECTION('center_axis',(3.71118737634973E-16,-1.,-1.23467863058847E-16));
#118928=DIRECTION('ref_axis',(9.86109193995912E-49,1.23467863058847E-16,
-1.));
#118929=DIRECTION('',(1.,3.71118737634973E-16,0.));
#118930=DIRECTION('center_axis',(3.71118737634973E-16,-1.,-1.23467863058847E-16));
#118931=DIRECTION('ref_axis',(9.86109193995912E-49,1.23467863058847E-16,
-1.));
#118932=DIRECTION('',(1.,3.71118737634973E-16,0.));
#118933=DIRECTION('center_axis',(5.72252063890675E-16,1.,1.23467863058847E-16));
#118934=DIRECTION('ref_axis',(1.,-5.72252063890675E-16,0.));
#118935=DIRECTION('',(-1.,5.72252063890675E-16,0.));
#118936=DIRECTION('center_axis',(5.72252063890675E-16,1.,1.23467863058847E-16));
#118937=DIRECTION('ref_axis',(1.,-5.72252063890675E-16,0.));
#118938=DIRECTION('',(-1.,5.72252063890675E-16,0.));
#118939=DIRECTION('center_axis',(-1.90750687963558E-16,-1.,-1.23467863058847E-16));
#118940=DIRECTION('ref_axis',(-1.,1.90750687963558E-16,0.));
#118941=DIRECTION('',(1.,-1.90750687963558E-16,0.));
#118942=DIRECTION('center_axis',(-1.90750687963558E-16,-1.,-1.23467863058847E-16));
#118943=DIRECTION('ref_axis',(-1.,1.90750687963558E-16,0.));
#118944=DIRECTION('',(1.,-1.90750687963558E-16,0.));
#118945=DIRECTION('center_axis',(-1.23706245878324E-16,-1.,-1.23467863058847E-16));
#118946=DIRECTION('ref_axis',(-1.,1.23706245878324E-16,0.));
#118947=DIRECTION('',(1.,-1.23706245878324E-16,0.));
#118948=DIRECTION('center_axis',(-1.23706245878324E-16,-1.,-1.23467863058847E-16));
#118949=DIRECTION('ref_axis',(-1.,1.23706245878324E-16,0.));
#118950=DIRECTION('',(1.,-1.23706245878324E-16,0.));
#118951=DIRECTION('center_axis',(-1.23706245878324E-16,1.,1.23467863058847E-16));
#118952=DIRECTION('ref_axis',(1.,1.23706245878324E-16,0.));
#118953=DIRECTION('',(-1.,-1.23706245878324E-16,0.));
#118954=DIRECTION('center_axis',(-1.23706245878324E-16,1.,1.23467863058847E-16));
#118955=DIRECTION('ref_axis',(1.,1.23706245878324E-16,0.));
#118956=DIRECTION('',(-1.,-1.23706245878324E-16,0.));
#118957=DIRECTION('center_axis',(4.76876719908896E-16,-1.,-1.23467863058847E-16));
#118958=DIRECTION('ref_axis',(8.72767235901404E-49,1.23467863058847E-16,
-1.));
#118959=DIRECTION('',(1.,4.76876719908896E-16,0.));
#118960=DIRECTION('center_axis',(4.76876719908896E-16,-1.,-1.23467863058847E-16));
#118961=DIRECTION('ref_axis',(8.72767235901404E-49,1.23467863058847E-16,
-1.));
#118962=DIRECTION('',(1.,4.76876719908896E-16,0.));
#118963=DIRECTION('center_axis',(-9.53753439817791E-17,1.,1.23467863058847E-16));
#118964=DIRECTION('ref_axis',(4.60419424770999E-49,1.23467863058847E-16,
-1.));
#118965=DIRECTION('',(-1.,-9.53753439817791E-17,0.));
#118966=DIRECTION('center_axis',(-9.53753439817791E-17,1.,1.23467863058847E-16));
#118967=DIRECTION('ref_axis',(4.60419424770999E-49,1.23467863058847E-16,
-1.));
#118968=DIRECTION('',(-1.,-9.53753439817791E-17,0.));
#118969=DIRECTION('center_axis',(-0.592966514233392,0.805227118891249,0.));
#118970=DIRECTION('ref_axis',(-0.805227118891249,-0.592966514233392,0.));
#118971=DIRECTION('center_axis',(0.807208114890536,-0.590266938981735,2.28940150095415E-14));
#118972=DIRECTION('ref_axis',(0.590266938981735,0.807208114890536,-1.47426480814321E-30));
#118973=DIRECTION('center_axis',(0.,1.23467863058847E-16,-1.));
#118974=DIRECTION('ref_axis',(-0.705921937789672,-0.708289642552589,0.));
#118975=DIRECTION('center_axis',(-1.06667316881548E-30,-9.2152858313306E-45,
1.));
#118976=DIRECTION('ref_axis',(-8.63927780386936E-15,1.,6.22301527786114E-60));
#118977=DIRECTION('center_axis',(0.,0.,-1.));
#118978=DIRECTION('ref_axis',(0.,-1.,0.));
#118979=DIRECTION('center_axis',(0.,0.,-1.));
#118980=DIRECTION('ref_axis',(0.,-1.,0.));
#118981=DIRECTION('center_axis',(0.,-1.23467863058847E-16,1.));
#118982=DIRECTION('ref_axis',(0.,-1.,0.));
#118983=DIRECTION('center_axis',(0.,0.,1.));
#118984=DIRECTION('ref_axis',(0.,-1.,0.));
#118985=DIRECTION('center_axis',(-1.,0.,0.));
#118986=DIRECTION('ref_axis',(0.,1.,0.));
#118987=DIRECTION('center_axis',(0.,0.,-1.));
#118988=DIRECTION('ref_axis',(0.,1.,0.));
#118989=DIRECTION('center_axis',(0.,0.,-1.));
#118990=DIRECTION('ref_axis',(0.,1.,0.));
#118991=DIRECTION('center_axis',(-0.168369768252295,-0.882882757183484,
0.438371598312161));
#118992=DIRECTION('ref_axis',(2.05714353600353E-15,-0.444720469017533,-0.895669416937313));
#118993=DIRECTION('center_axis',(-0.507675385487887,0.517400512911953,-0.688884904906599));
#118994=DIRECTION('ref_axis',(1.34605780150592E-16,0.799589295572927,0.600547215800049));
#118995=DIRECTION('center_axis',(-0.506894799267393,0.516604973631544,-0.690055768539632));
#118996=DIRECTION('ref_axis',(4.2861068992561E-17,0.800521374177574,0.599304204461181));
#118997=DIRECTION('center_axis',(0.,0.,1.));
#118998=DIRECTION('ref_axis',(1.,0.,0.));
#118999=DIRECTION('center_axis',(-0.663838127753914,-0.747876286654537,
-9.2338686945498E-17));
#119000=DIRECTION('ref_axis',(-0.747876286654537,0.663838127753914,1.66533453693772E-13));
#119001=DIRECTION('center_axis',(-0.187328576766759,-0.982297309538482,
0.));
#119002=DIRECTION('ref_axis',(0.982297309538482,-0.187328576766759,0.));
#119003=DIRECTION('center_axis',(-0.668574108837973,-0.743645521059268,
0.));
#119004=DIRECTION('ref_axis',(0.743645521059268,-0.668574108837973,0.));
#119005=DIRECTION('center_axis',(0.,-1.23467863058847E-16,1.));
#119006=DIRECTION('ref_axis',(0.,-1.,0.));
#119007=DIRECTION('center_axis',(-0.679956281045645,-0.733252654865004,
0.));
#119008=DIRECTION('ref_axis',(0.733252654865004,-0.679956281045645,0.));
#119009=DIRECTION('center_axis',(5.71153601538328E-31,2.64211616260599E-45,
-1.));
#119010=DIRECTION('ref_axis',(4.6259292692715E-15,-1.,-3.11150763893057E-61));
#119011=DIRECTION('center_axis',(0.,0.,1.));
#119012=DIRECTION('ref_axis',(0.,-1.,0.));
#119013=DIRECTION('center_axis',(-0.775870249713592,-0.63089250717485,1.27793330397298E-14));
#119014=DIRECTION('ref_axis',(0.63089250717485,-0.775870249713592,-7.13011169472736E-30));
#119015=DIRECTION('center_axis',(0.,-1.23467863058847E-16,1.));
#119016=DIRECTION('ref_axis',(0.,-1.,0.));
#119017=DIRECTION('center_axis',(-0.746021307914873,-0.665922073621968,
0.));
#119018=DIRECTION('ref_axis',(0.665922073621968,-0.746021307914873,0.));
#119019=DIRECTION('center_axis',(2.41254715360152E-30,4.7140880421464E-44,
-1.));
#119020=DIRECTION('ref_axis',(1.95398793972133E-14,-1.,1.49352366668667E-58));
#119021=DIRECTION('center_axis',(0.,0.,1.));
#119022=DIRECTION('ref_axis',(0.,-1.,0.));
#119023=DIRECTION('center_axis',(0.507468854451513,-0.517190025527329,0.68919506618715));
#119024=DIRECTION('ref_axis',(1.08020880515219E-16,-0.799836347973839,-0.600218140728745));
#119025=DIRECTION('center_axis',(0.,-1.23467863058847E-16,1.));
#119026=DIRECTION('ref_axis',(0.,-1.,0.));
#119027=DIRECTION('center_axis',(-0.923323390669864,-0.38402332773141,1.28136860937081E-14));
#119028=DIRECTION('ref_axis',(0.38402332773141,-0.923323390669864,2.90201745723254E-30));
#119029=DIRECTION('center_axis',(-6.28268961692158E-30,3.19696055675322E-43,
-1.));
#119030=DIRECTION('ref_axis',(-5.08852219619863E-14,-1.,-2.38963786669868E-58));
#119031=DIRECTION('center_axis',(0.,0.,1.));
#119032=DIRECTION('ref_axis',(0.,-1.,0.));
#119033=DIRECTION('center_axis',(0.511561679834273,-0.521361253861094,0.682998602266158));
#119034=DIRECTION('ref_axis',(-1.21631079100244E-16,-0.79488081246627,-0.606765600518819));
#119035=DIRECTION('center_axis',(-0.987526870499689,-0.134244619791538,
0.0822743100737742));
#119036=DIRECTION('ref_axis',(0.134701294632915,-0.990886250396188,-7.62230551969098E-18));
#119037=DIRECTION('center_axis',(0.887573437172827,0.12065692809958,0.444584411925099));
#119038=DIRECTION('ref_axis',(0.447856331161543,-5.04904183848934E-18,-0.89410553439654));
#119039=DIRECTION('center_axis',(0.502574642452133,-0.589207696134777,-0.632655529952643));
#119040=DIRECTION('ref_axis',(-0.234516419283699,0.611436391027521,-0.755743070635512));
#119041=DIRECTION('center_axis',(0.,0.,1.));
#119042=DIRECTION('ref_axis',(1.,0.,0.));
#119043=DIRECTION('center_axis',(0.606371999687993,0.771616335224111,-0.192148976603301));
#119044=DIRECTION('ref_axis',(-0.786267832350933,0.617885827487704,-3.1641897774151E-17));
#119045=DIRECTION('center_axis',(-0.645804421056786,0.763502881293522,1.01980482580395E-14));
#119046=DIRECTION('ref_axis',(-0.763502881293522,-0.645804421056786,-6.9816295225584E-30));
#119047=DIRECTION('center_axis',(0.48724015249101,0.488874385354372,0.723601319197887));
#119048=DIRECTION('ref_axis',(1.47352524967685E-15,-0.828613098245121,0.559821697879442));
#119049=DIRECTION('center_axis',(0.488418020654004,0.490056204158282,0.722006062208899));
#119050=DIRECTION('ref_axis',(-3.20373038523992E-15,-0.827409999881363,
0.561598336977882));
#119051=DIRECTION('center_axis',(-0.753146254930614,0.657853113304171,3.00335537434998E-14));
#119052=DIRECTION('ref_axis',(-0.657853113304171,-0.753146254930614,-2.96993835591878E-30));
#119053=DIRECTION('center_axis',(-0.171101227036283,0.869601781127171,0.463159920942141));
#119054=DIRECTION('ref_axis',(4.21773228904835E-17,-0.470092156192753,0.882617337630554));
#119055=DIRECTION('center_axis',(0.484433158250521,0.486057976285942,0.727373465886845));
#119056=DIRECTION('ref_axis',(3.34045680200078E-15,-0.831447136037245,0.555603869654868));
#119057=DIRECTION('center_axis',(1.,0.,0.));
#119058=DIRECTION('ref_axis',(0.,-1.,0.));
#119059=DIRECTION('center_axis',(-0.193053842425666,0.981173356447606,-0.00539059570228739));
#119060=DIRECTION('ref_axis',(-0.981187612482096,-0.193056647416463,-1.03740416739262E-18));
#119061=DIRECTION('center_axis',(-0.663957144707683,0.747700087626819,-0.0102707815899847));
#119062=DIRECTION('ref_axis',(-0.747739527797473,-0.663992167551103,3.3311423852743E-19));
#119063=DIRECTION('center_axis',(0.485576620175616,0.487205273451398,0.725841833638689));
#119064=DIRECTION('ref_axis',(-1.3020744827461E-16,-0.830298240911906,0.557319326004935));
#119065=DIRECTION('center_axis',(-0.210025631952355,0.977695880078777,0.));
#119066=DIRECTION('ref_axis',(-0.977695880078777,-0.210025631952355,0.));
#119067=DIRECTION('center_axis',(0.869253009153379,-0.170328745809824,0.464098399510975));
#119068=DIRECTION('ref_axis',(0.470980702241858,8.1123542202202E-17,-0.882143513333157));
#119069=DIRECTION('center_axis',(0.,1.23467863058847E-16,-1.));
#119070=DIRECTION('ref_axis',(0.,1.,0.));
#119071=DIRECTION('center_axis',(-0.67420688908099,0.738542531419643,0.));
#119072=DIRECTION('ref_axis',(-0.738542531419643,-0.67420688908099,0.));
#119073=DIRECTION('center_axis',(-4.28365201153744E-31,-1.48619034146585E-45,
1.));
#119074=DIRECTION('ref_axis',(-3.46944695195361E-15,1.,1.24460305557223E-60));
#119075=DIRECTION('center_axis',(0.,0.,-1.));
#119076=DIRECTION('ref_axis',(0.,1.,0.));
#119077=DIRECTION('center_axis',(1.,0.,0.));
#119078=DIRECTION('ref_axis',(0.,-1.,0.));
#119079=DIRECTION('center_axis',(0.752788125817861,-0.658228853504028,-0.00669432912290745));
#119080=DIRECTION('ref_axis',(-0.658243602947644,-0.752804994124312,-1.11021690861332E-13));
#119081=DIRECTION('center_axis',(0.981331609270135,-0.192290369398073,-0.00356180909645361));
#119082=DIRECTION('ref_axis',(0.192291589154029,0.981337834153263,-1.28820063606849E-18));
#119083=DIRECTION('center_axis',(0.,1.23467863058847E-16,-1.));
#119084=DIRECTION('ref_axis',(0.,1.,0.));
#119085=DIRECTION('center_axis',(-0.74079592940915,0.671730147433353,0.));
#119086=DIRECTION('ref_axis',(-0.671730147433353,-0.74079592940915,0.));
#119087=DIRECTION('center_axis',(-1.64492525510334E-30,-2.19148451090235E-44,
1.));
#119088=DIRECTION('ref_axis',(-1.33226996430588E-14,1.,1.74244427780112E-59));
#119089=DIRECTION('center_axis',(0.,0.,-1.));
#119090=DIRECTION('ref_axis',(0.,1.,0.));
#119091=DIRECTION('center_axis',(0.979119873047182,-0.203283728330798,0.));
#119092=DIRECTION('ref_axis',(0.203283728330798,0.979119873047182,0.));
#119093=DIRECTION('center_axis',(0.,1.23467863058847E-16,-1.));
#119094=DIRECTION('ref_axis',(0.,1.,0.));
#119095=DIRECTION('center_axis',(0.,0.,-1.));
#119096=DIRECTION('ref_axis',(0.,1.,0.));
#119097=DIRECTION('center_axis',(-2.57019120692247E-30,-5.35028522927707E-44,
1.));
#119098=DIRECTION('ref_axis',(-2.08166817117217E-14,1.,-1.99136488891557E-59));
#119099=DIRECTION('center_axis',(0.,-1.23467863058847E-16,1.));
#119100=DIRECTION('ref_axis',(1.22464679914735E-16,1.,1.21959207089992E-16));
#119101=DIRECTION('center_axis',(2.7383203336382E-32,1.19614019798162E-16,
-1.));
#119102=DIRECTION('ref_axis',(7.105427357601E-15,-1.,-1.19614019798162E-16));
#119103=DIRECTION('center_axis',(0.,-1.19356871810915E-16,1.));
#119104=DIRECTION('ref_axis',(0.,-1.,-1.19356871810915E-16));
#119105=DIRECTION('center_axis',(0.982297019165463,-0.187330099393145,0.));
#119106=DIRECTION('ref_axis',(0.187330099393145,0.982297019165463,0.));
#119107=DIRECTION('center_axis',(0.,-1.23467863058847E-16,1.));
#119108=DIRECTION('ref_axis',(0.,-1.,0.));
#119109=DIRECTION('center_axis',(0.777162624242377,-0.629299813666508,0.));
#119110=DIRECTION('ref_axis',(0.629299813666508,0.777162624242377,0.));
#119111=DIRECTION('center_axis',(4.46763300492346E-31,1.61659432440069E-45,
-1.));
#119112=DIRECTION('ref_axis',(3.61845819166247E-15,-1.,1.86690458335834E-60));
#119113=DIRECTION('center_axis',(0.,0.,1.));
#119114=DIRECTION('ref_axis',(0.,-1.,0.));
#119115=DIRECTION('center_axis',(0.,-1.23467863058847E-16,1.));
#119116=DIRECTION('ref_axis',(0.,-1.,0.));
#119117=DIRECTION('center_axis',(0.635030358342585,-0.772487180465338,0.));
#119118=DIRECTION('ref_axis',(0.772487180465338,0.635030358342585,0.));
#119119=DIRECTION('center_axis',(1.09661491495359E-30,9.73989702183063E-45,
-1.));
#119120=DIRECTION('ref_axis',(8.88178419700125E-15,-1.,2.48920611114446E-60));
#119121=DIRECTION('center_axis',(0.,0.,1.));
#119122=DIRECTION('ref_axis',(0.,-1.,0.));
#119123=DIRECTION('center_axis',(0.,-1.23467863058847E-16,1.));
#119124=DIRECTION('ref_axis',(0.,-1.,0.));
#119125=DIRECTION('center_axis',(0.0394959395290733,-0.999219730970479,
0.));
#119126=DIRECTION('ref_axis',(0.999219730970479,0.0394959395290733,0.));
#119127=DIRECTION('center_axis',(6.70144950738521E-31,3.63733722990157E-45,
-1.));
#119128=DIRECTION('ref_axis',(5.42768728749372E-15,-1.,2.48920611114446E-60));
#119129=DIRECTION('center_axis',(0.,0.,1.));
#119130=DIRECTION('ref_axis',(0.,-1.,0.));
#119131=DIRECTION('center_axis',(0.,-1.23467863058847E-16,1.));
#119132=DIRECTION('ref_axis',(0.,-1.,-1.33055111034894E-16));
#119133=DIRECTION('center_axis',(-0.0394959395290663,-0.999219730970479,
0.));
#119134=DIRECTION('ref_axis',(0.999219730970479,-0.0394959395290663,0.));
#119135=DIRECTION('center_axis',(0.,1.30058395245648E-16,-1.));
#119136=DIRECTION('ref_axis',(0.,-1.,-1.30058395245648E-16));
#119137=DIRECTION('center_axis',(0.,-1.29997489681772E-16,1.));
#119138=DIRECTION('ref_axis',(0.,-1.,-1.29997489681772E-16));
#119139=DIRECTION('center_axis',(0.,-1.23467863058847E-16,1.));
#119140=DIRECTION('ref_axis',(0.,-1.,0.));
#119141=DIRECTION('center_axis',(-0.635030358342616,-0.772487180465313,
0.));
#119142=DIRECTION('ref_axis',(0.772487180465313,-0.635030358342616,0.));
#119143=DIRECTION('center_axis',(-5.21223850574408E-31,2.20036449710098E-45,
-1.));
#119144=DIRECTION('ref_axis',(-4.22153455693958E-15,-1.,-9.33452291679171E-61));
#119145=DIRECTION('center_axis',(0.,0.,1.));
#119146=DIRECTION('ref_axis',(0.,-1.,0.));
#119147=DIRECTION('center_axis',(0.,-1.23467863058847E-16,1.));
#119148=DIRECTION('ref_axis',(0.,-1.,0.));
#119149=DIRECTION('center_axis',(-0.774287490710421,-0.632834008037937,
0.));
#119150=DIRECTION('ref_axis',(0.632834008037937,-0.774287490710421,0.));
#119151=DIRECTION('center_axis',(0.,0.,-1.));
#119152=DIRECTION('ref_axis',(0.,-1.,0.));
#119153=DIRECTION('center_axis',(0.,0.,1.));
#119154=DIRECTION('ref_axis',(0.,-1.,0.));
#119155=DIRECTION('center_axis',(0.,-1.23467863058847E-16,1.));
#119156=DIRECTION('ref_axis',(0.,-1.,0.));
#119157=DIRECTION('center_axis',(-0.999225121087074,-0.0393593367388477,
0.));
#119158=DIRECTION('ref_axis',(0.0393593367388477,-0.999225121087074,0.));
#119159=DIRECTION('center_axis',(5.21223850574404E-31,2.20036449710094E-45,
-1.));
#119160=DIRECTION('ref_axis',(4.22153455693955E-15,-1.,2.48920611114446E-60));
#119161=DIRECTION('center_axis',(0.,0.,1.));
#119162=DIRECTION('ref_axis',(0.,-1.,0.));
#119163=DIRECTION('center_axis',(0.,-1.23467863058847E-16,1.));
#119164=DIRECTION('ref_axis',(0.,-1.,-1.33055111034894E-16));
#119165=DIRECTION('center_axis',(0.,-1.29997489681772E-16,1.));
#119166=DIRECTION('ref_axis',(0.,-1.,-1.29997489681772E-16));
#119167=DIRECTION('center_axis',(-3.39506970834015E-31,1.30058395245648E-16,
-1.));
#119168=DIRECTION('ref_axis',(5.15143483426073E-14,-1.,-1.30058395245648E-16));
#119169=DIRECTION('center_axis',(0.,0.,1.));
#119170=DIRECTION('ref_axis',(0.75170336763964,-0.659501362454411,0.));
#119171=DIRECTION('center_axis',(-0.00318936290742699,0.00297678217545832,
-0.999990483320779));
#119172=DIRECTION('ref_axis',(0.747789842749455,-0.6639211772416,-0.00436136341903465));
#119173=DIRECTION('center_axis',(0.659496851377394,0.751707325375577,0.));
#119174=DIRECTION('ref_axis',(-0.751707325375577,0.659496851377394,0.));
#119175=DIRECTION('center_axis',(0.657034976183429,0.753860093168249,-1.01740733956786E-14));
#119176=DIRECTION('ref_axis',(-0.753860093168249,0.657034976183429,-8.45764823615526E-31));
#119177=DIRECTION('center_axis',(-0.00280476608066071,0.00263885430337773,
-0.999992584840107));
#119178=DIRECTION('ref_axis',(0.937191712771117,0.348810515489431,-0.00170815606344439));
#119179=DIRECTION('center_axis',(0.768895279480121,-0.207195498703726,0.604871948853723));
#119180=DIRECTION('ref_axis',(0.618289095466814,1.21523947502978E-17,-0.785950758271044));
#119181=DIRECTION('center_axis',(0.202724571193613,-0.760898522337225,0.616389638896853));
#119182=DIRECTION('ref_axis',(1.87348493224475E-17,-0.629459870756021,-0.777032992290426));
#119183=DIRECTION('center_axis',(0.767736348840716,-0.206883199723352,0.606448876939313));
#119184=DIRECTION('ref_axis',(0.619859127336644,-1.17584790122141E-16,-0.784713108248775));
#119185=DIRECTION('center_axis',(-0.243334995703589,-0.96954396966785,-0.0277951568918529));
#119186=DIRECTION('ref_axis',(0.594809401908895,-0.126526334687349,-0.793846875682815));
#119187=DIRECTION('center_axis',(0.260190354028299,0.965557341472079,-1.40549396816343E-10));
#119188=DIRECTION('ref_axis',(0.58403426831887,-0.15738069260472,-0.796326121023605));
#119189=DIRECTION('center_axis',(0.202457297762738,-0.759895348634851,0.617713608159743));
#119190=DIRECTION('ref_axis',(-5.55058625584594E-17,-0.630776296546234,
-0.775964730973913));
#119191=DIRECTION('center_axis',(-0.966292363520655,-0.25744721439873,4.29897349204163E-11));
#119192=DIRECTION('ref_axis',(0.159028116924834,-0.596889950284185,-0.786404759190256));
#119193=DIRECTION('center_axis',(0.966468863382725,0.256741605888852,-0.00465659932972454));
#119194=DIRECTION('ref_axis',(0.154910761359747,-0.597411475844062,-0.786830467473625));
#119195=DIRECTION('center_axis',(0.578576029254642,-0.155909851599689,0.800588468906525));
#119196=DIRECTION('ref_axis',(0.810499837678775,1.21842170142303E-15,-0.585738860860947));
#119197=DIRECTION('center_axis',(0.153941565569776,-0.577798286012631,0.801530495409122));
#119198=DIRECTION('ref_axis',(1.29290181198153E-17,-0.811200037627138,-0.584768756820788));
#119199=DIRECTION('center_axis',(0.0544019837731304,0.025960154057113,0.998181593981215));
#119200=DIRECTION('ref_axis',(0.998518116145471,-1.61274188638027E-18,-0.054420324597515));
#119201=DIRECTION('center_axis',(-0.025995718416376,-0.0542003143889016,
0.998191639187667));
#119202=DIRECTION('ref_axis',(-1.6064497712818E-18,-0.99852908789078,-0.0542186373492239));
#119203=DIRECTION('center_axis',(0.734334158412678,0.678788143523695,-2.48736119588291E-13));
#119204=DIRECTION('ref_axis',(-0.678788143523695,0.734334158412678,-6.81231552358944E-29));
#119205=DIRECTION('center_axis',(-0.680870844883917,-0.73240350394237,-1.91708814121709E-12));
#119206=DIRECTION('ref_axis',(0.73240350394237,-0.680870844883917,-1.31317411609931E-27));
#119207=DIRECTION('center_axis',(0.,-1.23467863058847E-16,1.));
#119208=DIRECTION('ref_axis',(0.,-1.,0.));
#119209=DIRECTION('center_axis',(-9.86953423458227E-31,7.88931658768281E-45,
-1.));
#119210=DIRECTION('ref_axis',(-7.99360577730113E-15,-1.,2.48920611114446E-60));
#119211=DIRECTION('center_axis',(0.,0.,1.));
#119212=DIRECTION('ref_axis',(0.,1.,0.));
#119213=DIRECTION('center_axis',(0.0255375237255525,-0.0535186253292443,
-0.998240247447895));
#119214=DIRECTION('ref_axis',(2.96412751937958E-19,0.998565915482956,-0.0535360853601283));
#119215=DIRECTION('center_axis',(-0.682537484892591,0.730850587819765,-8.37209378123771E-13));
#119216=DIRECTION('ref_axis',(-0.730850587819765,-0.682537484892591,3.92323810141884E-28));
#119217=DIRECTION('center_axis',(0.,-1.23467863058847E-16,1.));
#119218=DIRECTION('ref_axis',(0.,-1.,0.));
#119219=DIRECTION('center_axis',(-0.735878524541007,0.677113577710085,-5.64206319996869E-13));
#119220=DIRECTION('ref_axis',(-0.677113577710085,-0.735878524541007,-1.38055872491966E-28));
#119221=DIRECTION('center_axis',(5.92172054074936E-30,-2.84015397156581E-43,
1.));
#119222=DIRECTION('ref_axis',(4.79616346638068E-14,1.,-2.78791084448179E-58));
#119223=DIRECTION('center_axis',(0.,0.,-1.));
#119224=DIRECTION('ref_axis',(0.,-1.,0.));
#119225=DIRECTION('center_axis',(-0.152544532818274,-0.577842847451632,
-0.801765432752152));
#119226=DIRECTION('ref_axis',(-4.14384419008336E-17,0.811259933931047,-0.58468565879299));
#119227=DIRECTION('center_axis',(-0.0536778879072088,0.0251150971461135,
-0.998242413567548));
#119228=DIRECTION('ref_axis',(-0.998557392321894,-9.29874389531901E-20,
0.0536948250700053));
#119229=DIRECTION('center_axis',(-0.19315692461333,-0.731683694333232,-0.653704347485004));
#119230=DIRECTION('ref_axis',(3.51224977473848E-17,0.66625127354731,-0.745727323152764));
#119231=DIRECTION('center_axis',(-0.576537673896198,-0.156770156178271,
-0.801889910592596));
#119232=DIRECTION('ref_axis',(-0.811929324239482,3.97972821433516E-17,0.583755747243673));
#119233=DIRECTION('center_axis',(-0.193538145022295,-0.733127767631913,
-0.651971366509586));
#119234=DIRECTION('ref_axis',(-1.09087611421558E-16,0.664535912353125,-0.747256328974871));
#119235=DIRECTION('center_axis',(-0.966876318111592,0.25524534368911,8.60979798737377E-11));
#119236=DIRECTION('ref_axis',(0.166411982437669,0.630373124965737,-0.758245854206995));
#119237=DIRECTION('center_axis',(0.967398007177023,-0.253182433216653,-0.00630485689132568));
#119238=DIRECTION('ref_axis',(0.16111421782421,0.634435934472465,-0.755998183770929));
#119239=DIRECTION('center_axis',(-0.72784499809572,-0.197913127261801,-0.656560776169652));
#119240=DIRECTION('ref_axis',(-0.669809908048189,2.97308687105849E-17,0.742532616846207));
#119241=DIRECTION('center_axis',(-0.72888212476865,-0.19819513920631,-0.655323992379136));
#119242=DIRECTION('ref_axis',(-0.668587032943078,1.18015531912611E-16,0.743633901446385));
#119243=DIRECTION('center_axis',(-0.257377402244523,0.96626185396935,-0.00974178513293261));
#119244=DIRECTION('ref_axis',(0.635976884577247,0.161793976065296,-0.754556897518273));
#119245=DIRECTION('center_axis',(0.262389207131878,-0.964962125671627,2.3868460211661E-11));
#119246=DIRECTION('ref_axis',(0.633554268004896,0.172273913779853,-0.754274941996453));
#119247=DIRECTION('center_axis',(-0.70592193778968,-0.708289642552581,-8.74510085926821E-17));
#119248=DIRECTION('ref_axis',(0.708289642552581,-0.70592193778968,-3.19694546253078E-33));
#119249=DIRECTION('',(0.70592193778968,0.708289642552581,8.74510085926821E-17));
#119250=DIRECTION('',(-0.70592193778968,-0.708289642552581,-8.74510085926821E-17));
#119251=DIRECTION('center_axis',(-0.705921937789676,-0.708289642552585,
6.53108990768421E-15));
#119252=DIRECTION('ref_axis',(0.708289642552585,-0.705921937789676,-2.24639971032546E-30));
#119253=DIRECTION('center_axis',(0.,0.,1.));
#119254=DIRECTION('ref_axis',(0.,1.,0.));
#119255=DIRECTION('center_axis',(-0.74079592940915,0.671730147433353,0.));
#119256=DIRECTION('ref_axis',(-0.671730147433353,-0.74079592940915,0.));
#119257=DIRECTION('center_axis',(0.,0.,-1.));
#119258=DIRECTION('ref_axis',(0.,1.,0.));
#119259=DIRECTION('center_axis',(0.,1.23467863058847E-16,-1.));
#119260=DIRECTION('ref_axis',(0.,1.,0.));
#119261=DIRECTION('center_axis',(0.,0.,-1.));
#119262=DIRECTION('ref_axis',(0.,1.,0.));
#119263=DIRECTION('center_axis',(0.,0.,-1.));
#119264=DIRECTION('ref_axis',(0.,1.,0.));
#119265=DIRECTION('center_axis',(-2.41254715360153E-30,-4.71408804214643E-44,
1.));
#119266=DIRECTION('ref_axis',(-1.95398793972133E-14,1.,5.9740946667467E-59));
#119267=DIRECTION('center_axis',(-0.674206889080985,0.738542531419647,0.));
#119268=DIRECTION('ref_axis',(-0.738542531419647,-0.674206889080985,0.));
#119269=DIRECTION('center_axis',(0.7059219377897,0.708289642552562,2.19056695270365E-17));
#119270=DIRECTION('ref_axis',(-0.708289642552562,0.7059219377897,4.72941823813195E-33));
#119271=DIRECTION('center_axis',(0.,0.,-1.));
#119272=DIRECTION('ref_axis',(0.,1.,0.));
#119273=DIRECTION('center_axis',(0.,0.,1.));
#119274=DIRECTION('ref_axis',(0.,1.,0.));
#119275=DIRECTION('center_axis',(0.7059219377897,0.708289642552561,8.74510085926797E-17));
#119276=DIRECTION('ref_axis',(-0.708289642552561,0.7059219377897,-8.55019604084016E-33));
#119277=DIRECTION('',(0.7059219377897,0.708289642552561,8.74510085926797E-17));
#119278=DIRECTION('',(-0.7059219377897,-0.708289642552561,-8.74510085926797E-17));
#119279=DIRECTION('center_axis',(0.964962125666191,0.262389207151869,3.23966346967465E-17));
#119280=DIRECTION('ref_axis',(-0.262389207151869,0.964962125666191,-4.57090956622107E-33));
#119281=DIRECTION('',(0.964962125666191,0.262389207151869,3.23966346967465E-17));
#119282=DIRECTION('',(-0.964962125666191,-0.262389207151869,-3.23966346967465E-17));
#119283=DIRECTION('center_axis',(-0.964962125666191,-0.26238920715187,-2.42758782660955E-15));
#119284=DIRECTION('ref_axis',(0.26238920715187,-0.964962125666191,2.22950724024121E-31));
#119285=DIRECTION('center_axis',(0.,0.,1.));
#119286=DIRECTION('ref_axis',(0.,1.,0.));
#119287=DIRECTION('center_axis',(-0.735878524541004,0.677113577710087,0.));
#119288=DIRECTION('ref_axis',(-0.677113577710087,-0.735878524541004,0.));
#119289=DIRECTION('center_axis',(0.,0.,-1.));
#119290=DIRECTION('ref_axis',(0.,1.,0.));
#119291=DIRECTION('center_axis',(0.,1.23467863058847E-16,-1.));
#119292=DIRECTION('ref_axis',(0.,1.,0.));
#119293=DIRECTION('center_axis',(-0.682537484892593,0.730850587819763,0.));
#119294=DIRECTION('ref_axis',(-0.730850587819763,-0.682537484892593,0.));
#119295=DIRECTION('center_axis',(0.,0.,-1.));
#119296=DIRECTION('ref_axis',(0.,1.,0.));
#119297=DIRECTION('center_axis',(4.93476711729114E-30,-1.97232914692071E-43,
1.));
#119298=DIRECTION('ref_axis',(3.99680288865056E-14,1.,0.));
#119299=DIRECTION('center_axis',(0.255245343760721,0.966876318092687,2.36149381309596E-15));
#119300=DIRECTION('ref_axis',(-0.966876318092687,0.255245343760721,9.80822191756775E-31));
#119301=DIRECTION('center_axis',(0.,0.,-1.));
#119302=DIRECTION('ref_axis',(0.,1.,0.));
#119303=DIRECTION('center_axis',(-5.71153601538325E-31,-2.64211616260596E-45,
1.));
#119304=DIRECTION('ref_axis',(-4.62592926927148E-15,1.,1.24460305557223E-60));
#119305=DIRECTION('center_axis',(-0.255245343760725,-0.966876318092686,
-1.1937815283711E-16));
#119306=DIRECTION('ref_axis',(0.966876318092686,-0.255245343760725,-8.61241374820812E-33));
#119307=DIRECTION('',(-0.255245343760725,-0.966876318092686,-1.1937815283711E-16));
#119308=DIRECTION('',(0.255245343760725,0.966876318092686,1.1937815283711E-16));
#119309=DIRECTION('center_axis',(-0.257447214431338,0.966292363511968,1.19306053212906E-16));
#119310=DIRECTION('ref_axis',(-0.966292363511968,-0.257447214431338,-1.5335664280992E-33));
#119311=DIRECTION('',(0.257447214431338,-0.966292363511968,-1.19306053212906E-16));
#119312=DIRECTION('',(-0.257447214431338,0.966292363511968,1.19306053212906E-16));
#119313=DIRECTION('center_axis',(-0.257447214431328,0.96629236351197,-1.78800005081742E-14));
#119314=DIRECTION('ref_axis',(-0.96629236351197,-0.257447214431328,-3.12759209575828E-30));
#119315=DIRECTION('center_axis',(0.680870844883904,0.732403503942382,0.));
#119316=DIRECTION('ref_axis',(-0.732403503942382,0.680870844883904,0.));
#119317=DIRECTION('center_axis',(0.,0.,-1.));
#119318=DIRECTION('ref_axis',(0.,-1.,0.));
#119319=DIRECTION('center_axis',(0.,0.,1.));
#119320=DIRECTION('ref_axis',(0.,-1.,0.));
#119321=DIRECTION('center_axis',(0.,-1.23467863058847E-16,1.));
#119322=DIRECTION('ref_axis',(0.,-1.,0.));
#119323=DIRECTION('center_axis',(0.734334158412675,0.678788143523698,0.));
#119324=DIRECTION('ref_axis',(-0.678788143523698,0.734334158412675,0.));
#119325=DIRECTION('center_axis',(4.05747518532827E-30,1.33339190228861E-43,
-1.));
#119326=DIRECTION('ref_axis',(3.28626015289047E-14,-1.,2.58877435559024E-58));
#119327=DIRECTION('center_axis',(0.,0.,1.));
#119328=DIRECTION('ref_axis',(0.,-1.,0.));
#119329=DIRECTION('center_axis',(-1.14230720307665E-30,1.05684646504238E-44,
-1.));
#119330=DIRECTION('ref_axis',(-9.25185853854296E-15,-1.,-3.73380916671668E-60));
#119331=DIRECTION('center_axis',(0.,0.,1.));
#119332=DIRECTION('ref_axis',(0.,-1.,0.));
#119333=DIRECTION('center_axis',(0.965557341499939,-0.260190353924909,4.11871123919569E-15));
#119334=DIRECTION('ref_axis',(0.260190353924909,0.965557341499939,-2.2632930465492E-31));
#119335=DIRECTION('center_axis',(0.965557341499939,-0.260190353924911,-3.21251469876339E-17));
#119336=DIRECTION('ref_axis',(0.260190353924911,0.965557341499939,-9.87488652925334E-34));
#119337=DIRECTION('',(-0.965557341499939,0.260190353924911,3.21251469876339E-17));
#119338=DIRECTION('',(0.965557341499939,-0.260190353924911,-3.21251469876339E-17));
#119339=DIRECTION('center_axis',(0.700366780446484,-0.713783141330072,-8.81292791474553E-17));
#119340=DIRECTION('ref_axis',(0.713783141330072,0.700366780446484,-8.54636793605324E-33));
#119341=DIRECTION('',(0.700366780446485,-0.713783141330072,-8.81292791474553E-17));
#119342=DIRECTION('',(-0.700366780446485,0.713783141330072,8.81292791474553E-17));
#119343=DIRECTION('center_axis',(-0.700366780446484,0.713783141330073,0.));
#119344=DIRECTION('ref_axis',(-0.713783141330073,-0.700366780446484,0.));
#119345=DIRECTION('center_axis',(0.679956281045647,0.733252654865001,0.));
#119346=DIRECTION('ref_axis',(-0.733252654865001,0.679956281045647,0.));
#119347=DIRECTION('center_axis',(0.,0.,-1.));
#119348=DIRECTION('ref_axis',(0.,-1.,0.));
#119349=DIRECTION('center_axis',(0.,0.,1.));
#119350=DIRECTION('ref_axis',(0.,-1.,0.));
#119351=DIRECTION('center_axis',(0.,-1.23467863058847E-16,1.));
#119352=DIRECTION('ref_axis',(0.,-1.,0.));
#119353=DIRECTION('center_axis',(0.746021307914879,0.665922073621961,-1.23220336456872E-14));
#119354=DIRECTION('ref_axis',(-0.665922073621961,0.746021307914879,1.41534494748923E-30));
#119355=DIRECTION('center_axis',(3.28984144636074E-30,8.76588974171719E-44,
-1.));
#119356=DIRECTION('ref_axis',(2.66453258755498E-14,-1.,1.59309191113245E-58));
#119357=DIRECTION('center_axis',(0.,0.,1.));
#119358=DIRECTION('ref_axis',(0.,-1.,0.));
#119359=DIRECTION('center_axis',(0.,0.,-1.));
#119360=DIRECTION('ref_axis',(0.,-1.,0.));
#119361=DIRECTION('center_axis',(0.,0.,1.));
#119362=DIRECTION('ref_axis',(0.,-1.,0.));
#119363=DIRECTION('center_axis',(0.700366780446456,-0.7137831413301,0.));
#119364=DIRECTION('ref_axis',(0.7137831413301,0.700366780446456,0.));
#119365=DIRECTION('center_axis',(-0.700366780446451,0.713783141330105,8.81292791474594E-17));
#119366=DIRECTION('ref_axis',(-0.713783141330105,-0.700366780446451,4.73735951537523E-32));
#119367=DIRECTION('',(0.700366780446451,-0.713783141330105,-8.81292791474594E-17));
#119368=DIRECTION('',(-0.700366780446451,0.713783141330105,8.81292791474594E-17));
#119369=DIRECTION('center_axis',(0.,0.,-1.));
#119370=DIRECTION('ref_axis',(0.,1.,0.));
#119371=DIRECTION('',(0.,1.23467863058847E-16,-1.));
#119372=DIRECTION('',(-6.16297582203915E-33,-1.23467863058847E-16,1.));
#119373=DIRECTION('center_axis',(0.,0.,-1.));
#119374=DIRECTION('ref_axis',(0.,1.,0.));
#119375=DIRECTION('',(0.,-1.23467863058847E-16,1.));
#119376=DIRECTION('',(7.37292681274632E-34,1.23467863058847E-16,-1.));
#119377=DIRECTION('center_axis',(0.,0.,1.));
#119378=DIRECTION('ref_axis',(0.,-1.,0.));
#119379=DIRECTION('',(0.,1.23467863058847E-16,-1.));
#119380=DIRECTION('',(0.,-1.23467863058847E-16,1.));
#119381=DIRECTION('center_axis',(0.,0.,1.));
#119382=DIRECTION('ref_axis',(-0.0252625808996327,0.999680850074807,0.));
#119383=DIRECTION('',(-5.83684288299471E-35,1.23467863058847E-16,-1.));
#119384=DIRECTION('',(0.,-1.23467863058847E-16,1.));
#119385=DIRECTION('center_axis',(0.,0.,1.));
#119386=DIRECTION('ref_axis',(0.,-1.,0.));
#119387=DIRECTION('',(-3.52789515968553E-33,1.23467863058847E-16,-1.));
#119388=DIRECTION('',(0.,-1.23467863058847E-16,1.));
#119389=DIRECTION('center_axis',(0.,0.,1.));
#119390=DIRECTION('ref_axis',(0.,-1.,0.));
#119391=DIRECTION('',(0.,1.23467863058847E-16,-1.));
#119392=DIRECTION('',(1.21605822285869E-32,-1.23467863058847E-16,1.));
#119393=DIRECTION('center_axis',(0.,0.,-1.));
#119394=DIRECTION('ref_axis',(0.239106811829941,-0.970993271107746,0.));
#119395=DIRECTION('',(-6.62645671305077E-33,-1.23467863058847E-16,1.));
#119396=DIRECTION('',(0.,1.23467863058847E-16,-1.));
#119397=DIRECTION('center_axis',(0.,0.,-1.));
#119398=DIRECTION('ref_axis',(0.,1.,0.));
#119399=DIRECTION('',(0.,-1.23467863058847E-16,1.));
#119400=DIRECTION('',(-6.16297582203915E-33,1.23467863058847E-16,-1.));
#119401=DIRECTION('center_axis',(0.,1.23467863058847E-16,-1.));
#119402=DIRECTION('ref_axis',(0.,1.,0.));
#119403=DIRECTION('center_axis',(4.99759401346035E-30,-2.02287018699519E-43,
1.));
#119404=DIRECTION('ref_axis',(4.04768811061255E-14,1.,2.78791084448179E-58));
#119405=DIRECTION('center_axis',(-0.994416787801726,0.105523704152657,0.));
#119406=DIRECTION('ref_axis',(-0.105523704152657,-0.994416787801726,0.));
#119407=DIRECTION('center_axis',(0.,0.,-1.));
#119408=DIRECTION('ref_axis',(0.,1.,0.));
#119409=DIRECTION('center_axis',(0.,1.,0.));
#119410=DIRECTION('ref_axis',(0.,0.,1.));
#119411=DIRECTION('center_axis',(7.82779334765923E-17,1.,0.));
#119412=DIRECTION('ref_axis',(0.,0.,1.));
#119413=DIRECTION('center_axis',(0.,1.,0.));
#119414=DIRECTION('ref_axis',(0.,0.,1.));
#119415=DIRECTION('',(-7.82779334765923E-17,-1.,-1.23467863058847E-16));
#119416=DIRECTION('',(7.82779334765923E-17,1.,1.23467863058847E-16));
#119417=DIRECTION('center_axis',(0.,1.23467863058847E-16,-1.));
#119418=DIRECTION('ref_axis',(0.,1.,1.38375392967352E-16));
#119419=DIRECTION('center_axis',(-0.992522955047552,0.122058116090968,0.));
#119420=DIRECTION('ref_axis',(-0.122058116090968,-0.992522955047552,0.));
#119421=DIRECTION('center_axis',(0.,1.35726946151947E-16,-1.));
#119422=DIRECTION('ref_axis',(0.,1.,1.35726946151947E-16));
#119423=DIRECTION('center_axis',(6.16166569047948E-31,-1.35428930001789E-16,
1.));
#119424=DIRECTION('ref_axis',(-5.15143483426073E-14,1.,1.35428930001789E-16));
#119425=DIRECTION('center_axis',(0.,1.23467863058847E-16,-1.));
#119426=DIRECTION('ref_axis',(0.,1.,0.));
#119427=DIRECTION('center_axis',(-1.,0.,0.));
#119428=DIRECTION('ref_axis',(0.,0.,1.));
#119429=DIRECTION('center_axis',(0.,0.,1.));
#119430=DIRECTION('ref_axis',(0.,1.,0.));
#119431=DIRECTION('center_axis',(0.,0.,-1.));
#119432=DIRECTION('ref_axis',(0.,1.,0.));
#119433=DIRECTION('center_axis',(0.,1.23467863058847E-16,-1.));
#119434=DIRECTION('ref_axis',(0.,1.,0.));
#119435=DIRECTION('center_axis',(-0.848949186868299,0.528474481990998,0.));
#119436=DIRECTION('ref_axis',(-0.528474481990998,-0.848949186868299,0.));
#119437=DIRECTION('center_axis',(0.,0.,-1.));
#119438=DIRECTION('ref_axis',(0.,1.,0.));
#119439=DIRECTION('center_axis',(-2.06796993660427E-30,-3.463654065723E-44,
1.));
#119440=DIRECTION('ref_axis',(-1.67490542508106E-14,1.,-2.09093313336134E-58));
#119441=DIRECTION('center_axis',(1.,0.,-1.17757899099328E-32));
#119442=DIRECTION('ref_axis',(0.,1.,0.));
#119443=DIRECTION('center_axis',(-1.,0.,0.));
#119444=DIRECTION('ref_axis',(0.,0.,1.));
#119445=DIRECTION('',(1.,-9.53753439817791E-17,-1.17757899099328E-32));
#119446=DIRECTION('',(-1.,9.53753439817791E-17,1.17757899099328E-32));
#119447=DIRECTION('center_axis',(0.,1.23467863058847E-16,-1.));
#119448=DIRECTION('ref_axis',(0.,1.,0.));
#119449=DIRECTION('center_axis',(-0.787431540449703,0.616402116402116,0.));
#119450=DIRECTION('ref_axis',(-0.616402116402116,-0.787431540449703,0.));
#119451=DIRECTION('center_axis',(0.,0.,-1.));
#119452=DIRECTION('ref_axis',(0.,1.,0.));
#119453=DIRECTION('center_axis',(-7.6763044046751E-31,-4.77254954069701E-45,
1.));
#119454=DIRECTION('ref_axis',(-6.21724893790088E-15,1.,-1.86690458335834E-60));
#119455=DIRECTION('center_axis',(0.,1.23467863058847E-16,-1.));
#119456=DIRECTION('ref_axis',(0.,1.,0.));
#119457=DIRECTION('center_axis',(0.,-1.,0.));
#119458=DIRECTION('ref_axis',(0.,0.,-1.));
#119459=DIRECTION('center_axis',(0.,0.,1.));
#119460=DIRECTION('ref_axis',(0.,1.,0.));
#119461=DIRECTION('center_axis',(0.,0.,-1.));
#119462=DIRECTION('ref_axis',(0.,1.,0.));
#119463=DIRECTION('center_axis',(0.,1.23467863058847E-16,-1.));
#119464=DIRECTION('ref_axis',(0.,1.,0.));
#119465=DIRECTION('center_axis',(0.,1.,0.));
#119466=DIRECTION('ref_axis',(0.,0.,1.));
#119467=DIRECTION('center_axis',(0.,0.,-1.));
#119468=DIRECTION('ref_axis',(0.,1.,0.));
#119469=DIRECTION('center_axis',(-3.56971000961454E-31,-1.03207662601796E-45,
1.));
#119470=DIRECTION('ref_axis',(-2.89120579329468E-15,1.,-3.11150763893057E-61));
#119471=DIRECTION('center_axis',(0.,-1.,0.));
#119472=DIRECTION('ref_axis',(0.,0.,-1.));
#119473=DIRECTION('',(0.,-1.,-1.23467863058847E-16));
#119474=DIRECTION('',(0.,1.,1.23467863058847E-16));
#119475=DIRECTION('center_axis',(0.,1.23467863058847E-16,-1.));
#119476=DIRECTION('ref_axis',(0.,1.,0.));
#119477=DIRECTION('center_axis',(3.56971000961454E-30,-1.03207662601796E-43,
1.));
#119478=DIRECTION('ref_axis',(2.89120579329468E-14,1.,-3.98272977783113E-59));
#119479=DIRECTION('center_axis',(-0.998440322660918,0.0558294016156522,
0.));
#119480=DIRECTION('ref_axis',(-0.0558294016156522,-0.998440322660918,0.));
#119481=DIRECTION('center_axis',(0.,0.,-1.));
#119482=DIRECTION('ref_axis',(0.,1.,0.));
#119483=DIRECTION('center_axis',(0.,1.,0.));
#119484=DIRECTION('ref_axis',(0.,0.,1.));
#119485=DIRECTION('center_axis',(5.87084501074442E-17,1.,0.));
#119486=DIRECTION('ref_axis',(0.,0.,1.));
#119487=DIRECTION('center_axis',(0.,1.,0.));
#119488=DIRECTION('ref_axis',(0.,0.,1.));
#119489=DIRECTION('',(-5.87084501074442E-17,-1.,-1.23467863058847E-16));
#119490=DIRECTION('',(5.87084501074442E-17,1.,1.23467863058847E-16));
#119491=DIRECTION('center_axis',(0.,1.23467863058847E-16,-1.));
#119492=DIRECTION('ref_axis',(0.,1.,1.38375392967352E-16));
#119493=DIRECTION('center_axis',(-0.995642397459837,0.0932535059953692,
0.));
#119494=DIRECTION('ref_axis',(-0.0932535059953692,-0.995642397459837,0.));
#119495=DIRECTION('center_axis',(0.,1.35726946151947E-16,-1.));
#119496=DIRECTION('ref_axis',(0.,1.,1.35726946151947E-16));
#119497=DIRECTION('center_axis',(8.0739067668352E-31,-1.35428930001789E-16,
1.));
#119498=DIRECTION('ref_axis',(-6.75015598972095E-14,1.,1.35428930001789E-16));
#119499=DIRECTION('center_axis',(0.,1.23467863058847E-16,-1.));
#119500=DIRECTION('ref_axis',(0.,1.,0.));
#119501=DIRECTION('center_axis',(-1.,0.,0.));
#119502=DIRECTION('ref_axis',(0.,0.,1.));
#119503=DIRECTION('center_axis',(0.,0.,1.));
#119504=DIRECTION('ref_axis',(0.,1.,0.));
#119505=DIRECTION('center_axis',(0.,0.,-1.));
#119506=DIRECTION('ref_axis',(0.,1.,0.));
#119507=DIRECTION('center_axis',(0.,1.23467863058847E-16,-1.));
#119508=DIRECTION('ref_axis',(0.,1.,0.));
#119509=DIRECTION('center_axis',(0.,1.,0.));
#119510=DIRECTION('ref_axis',(0.,0.,1.));
#119511=DIRECTION('center_axis',(0.,0.,-1.));
#119512=DIRECTION('ref_axis',(0.,1.,0.));
#119513=DIRECTION('center_axis',(0.,0.,1.));
#119514=DIRECTION('ref_axis',(0.,1.,0.));
#119515=DIRECTION('center_axis',(1.,0.,-1.17757899099328E-32));
#119516=DIRECTION('ref_axis',(0.,1.,0.));
#119517=DIRECTION('center_axis',(-1.,0.,0.));
#119518=DIRECTION('ref_axis',(0.,0.,1.));
#119519=DIRECTION('',(1.,-9.53753439817791E-17,-1.17757899099328E-32));
#119520=DIRECTION('',(-1.,9.53753439817791E-17,1.17757899099328E-32));
#119521=DIRECTION('center_axis',(7.82779334765923E-17,-1.,0.));
#119522=DIRECTION('ref_axis',(0.,0.,-1.));
#119523=DIRECTION('center_axis',(0.,1.,0.));
#119524=DIRECTION('ref_axis',(0.,0.,1.));
#119525=DIRECTION('',(7.82779334765923E-17,-1.,-1.23467863058847E-16));
#119526=DIRECTION('',(-7.82779334765923E-17,1.,1.23467863058847E-16));
#119527=DIRECTION('center_axis',(0.,1.23467863058847E-16,-1.));
#119528=DIRECTION('ref_axis',(0.,1.,0.));
#119529=DIRECTION('center_axis',(0.,0.,-1.));
#119530=DIRECTION('ref_axis',(0.,1.,0.));
#119531=DIRECTION('center_axis',(0.,0.,1.));
#119532=DIRECTION('ref_axis',(0.,1.,0.));
#119533=DIRECTION('center_axis',(0.,1.23467863058847E-16,-1.));
#119534=DIRECTION('ref_axis',(0.,1.,0.));
#119535=DIRECTION('center_axis',(-6.13543907902499E-30,-3.04885917353938E-43,
1.));
#119536=DIRECTION('ref_axis',(-4.96925995722523E-14,1.,2.78791084448179E-58));
#119537=DIRECTION('center_axis',(-0.999981180102553,0.00613509907864248,
0.));
#119538=DIRECTION('ref_axis',(-0.00613509907864248,-0.999981180102553,0.));
#119539=DIRECTION('center_axis',(0.,0.,-1.));
#119540=DIRECTION('ref_axis',(0.,1.,0.));
#119541=DIRECTION('center_axis',(0.,1.,0.));
#119542=DIRECTION('ref_axis',(0.,0.,1.));
#119543=DIRECTION('center_axis',(6.11546355285877E-17,1.,0.));
#119544=DIRECTION('ref_axis',(0.,0.,1.));
#119545=DIRECTION('center_axis',(0.,1.,0.));
#119546=DIRECTION('ref_axis',(0.,0.,1.));
#119547=DIRECTION('',(-6.11546355285877E-17,-1.,-1.23467863058847E-16));
#119548=DIRECTION('',(6.11546355285877E-17,1.,1.23467863058847E-16));
#119549=DIRECTION('center_axis',(0.,1.23467863058847E-16,-1.));
#119550=DIRECTION('ref_axis',(0.,1.,1.38375392967352E-16));
#119551=DIRECTION('center_axis',(-0.999050847451757,0.0435592034583644,
0.));
#119552=DIRECTION('ref_axis',(-0.0435592034583644,-0.999050847451757,0.));
#119553=DIRECTION('center_axis',(0.,1.35726946151947E-16,-1.));
#119554=DIRECTION('ref_axis',(0.,1.,1.35726946151947E-16));
#119555=DIRECTION('center_axis',(-6.37413692118567E-32,-1.35428930001789E-16,
1.));
#119556=DIRECTION('ref_axis',(5.32907051820075E-15,1.,1.35428930001789E-16));
#119557=DIRECTION('center_axis',(0.,1.23467863058847E-16,-1.));
#119558=DIRECTION('ref_axis',(0.,1.,0.));
#119559=DIRECTION('center_axis',(-1.,0.,0.));
#119560=DIRECTION('ref_axis',(0.,0.,1.));
#119561=DIRECTION('center_axis',(0.,0.,1.));
#119562=DIRECTION('ref_axis',(0.,1.,0.));
#119563=DIRECTION('center_axis',(0.,0.,-1.));
#119564=DIRECTION('ref_axis',(0.,1.,0.));
#119565=DIRECTION('center_axis',(0.,1.23467863058847E-16,-1.));
#119566=DIRECTION('ref_axis',(0.,1.,0.));
#119567=DIRECTION('center_axis',(0.,1.,0.));
#119568=DIRECTION('ref_axis',(0.,0.,1.));
#119569=DIRECTION('center_axis',(0.,0.,-1.));
#119570=DIRECTION('ref_axis',(0.,1.,0.));
#119571=DIRECTION('center_axis',(-1.78485500480727E-31,-2.58019156504489E-46,
1.));
#119572=DIRECTION('ref_axis',(-1.44560289664734E-15,1.,-3.88938454866321E-62));
#119573=DIRECTION('center_axis',(1.,0.,-1.17757899099328E-32));
#119574=DIRECTION('ref_axis',(0.,1.,0.));
#119575=DIRECTION('center_axis',(-1.,0.,0.));
#119576=DIRECTION('ref_axis',(0.,0.,1.));
#119577=DIRECTION('',(1.,-9.53753439817791E-17,-1.17757899099328E-32));
#119578=DIRECTION('',(-1.,9.53753439817791E-17,1.17757899099328E-32));
#119579=DIRECTION('center_axis',(0.,-1.,-1.23467863058847E-16));
#119580=DIRECTION('ref_axis',(1.,0.,0.));
#119581=DIRECTION('center_axis',(0.,1.,0.));
#119582=DIRECTION('ref_axis',(0.,0.,1.));
#119583=DIRECTION('',(-3.13111733906369E-16,-1.,-1.23467863058847E-16));
#119584=DIRECTION('',(3.13111733906369E-16,1.,1.23467863058847E-16));
#119585=DIRECTION('center_axis',(0.,1.23467863058847E-16,-1.));
#119586=DIRECTION('ref_axis',(0.,1.,0.));
#119587=DIRECTION('center_axis',(0.,0.,-1.));
#119588=DIRECTION('ref_axis',(0.,1.,0.));
#119589=DIRECTION('center_axis',(0.,0.,1.));
#119590=DIRECTION('ref_axis',(0.,1.,0.));
#119591=DIRECTION('center_axis',(0.,1.23467863058847E-16,-1.));
#119592=DIRECTION('ref_axis',(0.,1.,0.));
#119593=DIRECTION('center_axis',(-1.,4.81867632215781E-16,0.));
#119594=DIRECTION('ref_axis',(-4.81867632215781E-16,-1.,0.));
#119595=DIRECTION('center_axis',(0.,0.,-1.));
#119596=DIRECTION('ref_axis',(0.,1.,0.));
#119597=DIRECTION('center_axis',(0.,1.,0.));
#119598=DIRECTION('ref_axis',(0.,0.,1.));
#119599=DIRECTION('center_axis',(0.,0.,1.));
#119600=DIRECTION('ref_axis',(0.,1.,0.));
#119601=DIRECTION('center_axis',(6.11546355285877E-17,1.,0.));
#119602=DIRECTION('ref_axis',(0.,0.,1.));
#119603=DIRECTION('center_axis',(0.,1.,0.));
#119604=DIRECTION('ref_axis',(0.,0.,1.));
#119605=DIRECTION('',(-6.11546355285877E-17,-1.,-1.23467863058847E-16));
#119606=DIRECTION('',(6.11546355285877E-17,1.,1.23467863058847E-16));
#119607=DIRECTION('center_axis',(-1.,0.,5.88789495496639E-32));
#119608=DIRECTION('ref_axis',(0.,-1.,0.));
#119609=DIRECTION('center_axis',(-1.,0.,0.));
#119610=DIRECTION('ref_axis',(0.,0.,1.));
#119611=DIRECTION('',(1.,-4.76876719908896E-16,-5.88789495496639E-32));
#119612=DIRECTION('',(-1.,4.76876719908896E-16,5.88789495496639E-32));
#119613=DIRECTION('center_axis',(0.,1.23467863058847E-16,-1.));
#119614=DIRECTION('ref_axis',(0.,1.,0.));
#119615=DIRECTION('center_axis',(-1.,0.,0.));
#119616=DIRECTION('ref_axis',(0.,0.,1.));
#119617=DIRECTION('center_axis',(0.,0.,1.));
#119618=DIRECTION('ref_axis',(0.,1.,0.));
#119619=DIRECTION('center_axis',(0.,0.,-1.));
#119620=DIRECTION('ref_axis',(0.,1.,0.));
#119621=DIRECTION('center_axis',(0.,1.23467863058847E-16,-1.));
#119622=DIRECTION('ref_axis',(0.,1.,0.));
#119623=DIRECTION('center_axis',(0.,1.,0.));
#119624=DIRECTION('ref_axis',(0.,0.,1.));
#119625=DIRECTION('center_axis',(0.,0.,-1.));
#119626=DIRECTION('ref_axis',(0.,1.,0.));
#119627=DIRECTION('center_axis',(0.,0.,1.));
#119628=DIRECTION('ref_axis',(0.,1.,0.));
#119629=DIRECTION('center_axis',(1.,0.,-1.5273745825629E-32));
#119630=DIRECTION('ref_axis',(0.,1.,0.));
#119631=DIRECTION('center_axis',(-1.,0.,0.));
#119632=DIRECTION('ref_axis',(0.,0.,1.));
#119633=DIRECTION('',(1.,-1.23706245878324E-16,-1.52737458256291E-32));
#119634=DIRECTION('',(-1.,1.23706245878324E-16,1.52737458256291E-32));
#119635=DIRECTION('center_axis',(0.,-1.,-1.23467863058847E-16));
#119636=DIRECTION('ref_axis',(1.,0.,0.));
#119637=DIRECTION('center_axis',(0.,1.,0.));
#119638=DIRECTION('ref_axis',(0.,0.,1.));
#119639=DIRECTION('',(-3.13111733906369E-16,-1.,-1.23467863058847E-16));
#119640=DIRECTION('',(3.13111733906369E-16,1.,1.23467863058847E-16));
#119641=DIRECTION('center_axis',(0.,1.23467863058847E-16,-1.));
#119642=DIRECTION('ref_axis',(0.,1.,0.));
#119643=DIRECTION('center_axis',(0.,0.,-1.));
#119644=DIRECTION('ref_axis',(0.,1.,0.));
#119645=DIRECTION('center_axis',(-1.78485500480727E-31,-2.58019156504489E-46,
1.));
#119646=DIRECTION('ref_axis',(-1.44560289664734E-15,1.,-3.88938454866321E-62));
#119647=DIRECTION('center_axis',(0.,1.23467863058847E-16,-1.));
#119648=DIRECTION('ref_axis',(0.,1.,0.));
#119649=DIRECTION('center_axis',(-1.,0.,0.));
#119650=DIRECTION('ref_axis',(0.,0.,1.));
#119651=DIRECTION('center_axis',(0.,0.,-1.));
#119652=DIRECTION('ref_axis',(0.,1.,0.));
#119653=DIRECTION('center_axis',(0.,1.,0.));
#119654=DIRECTION('ref_axis',(0.,0.,1.));
#119655=DIRECTION('center_axis',(0.,0.,1.));
#119656=DIRECTION('ref_axis',(0.,1.,0.));
#119657=DIRECTION('center_axis',(6.11546355285877E-17,1.,0.));
#119658=DIRECTION('ref_axis',(0.,0.,1.));
#119659=DIRECTION('center_axis',(0.,1.,0.));
#119660=DIRECTION('ref_axis',(0.,0.,1.));
#119661=DIRECTION('',(-6.11546355285877E-17,-1.,-1.23467863058847E-16));
#119662=DIRECTION('',(6.11546355285877E-17,1.,1.23467863058847E-16));
#119663=DIRECTION('center_axis',(-1.,0.,-1.5273745825629E-32));
#119664=DIRECTION('ref_axis',(0.,-1.,0.));
#119665=DIRECTION('center_axis',(-1.,0.,0.));
#119666=DIRECTION('ref_axis',(0.,0.,1.));
#119667=DIRECTION('',(1.,1.23706245878324E-16,1.52737458256291E-32));
#119668=DIRECTION('',(-1.,-1.23706245878324E-16,-1.52737458256291E-32));
#119669=DIRECTION('center_axis',(0.,1.23467863058847E-16,-1.));
#119670=DIRECTION('ref_axis',(0.,1.,0.));
#119671=DIRECTION('center_axis',(-0.995922166025996,0.0902166238455439,
0.));
#119672=DIRECTION('ref_axis',(-0.0902166238455439,-0.995922166025996,0.));
#119673=DIRECTION('center_axis',(1.11553437800454E-31,-1.00788733009566E-46,
1.));
#119674=DIRECTION('ref_axis',(9.03501810404587E-16,1.,1.55575381946529E-61));
#119675=DIRECTION('center_axis',(0.,0.,-1.));
#119676=DIRECTION('ref_axis',(0.,1.,0.));
#119677=DIRECTION('center_axis',(0.,1.23467863058847E-16,-1.));
#119678=DIRECTION('ref_axis',(0.,1.,0.));
#119679=DIRECTION('center_axis',(0.,1.,0.));
#119680=DIRECTION('ref_axis',(0.,0.,1.));
#119681=DIRECTION('center_axis',(0.,0.,-1.));
#119682=DIRECTION('ref_axis',(0.,1.,0.));
#119683=DIRECTION('center_axis',(1.78485500480727E-31,-2.58019156504489E-46,
1.));
#119684=DIRECTION('ref_axis',(1.44560289664734E-15,1.,-3.88938454866321E-62));
#119685=DIRECTION('center_axis',(0.,1.23467863058847E-16,-1.));
#119686=DIRECTION('ref_axis',(0.,1.,0.));
#119687=DIRECTION('center_axis',(-0.913440670994017,0.406971916198157,3.63370493544251E-16));
#119688=DIRECTION('ref_axis',(-0.406971916198157,-0.913440670994017,6.94755181634254E-32));
#119689=DIRECTION('center_axis',(0.,0.,-1.));
#119690=DIRECTION('ref_axis',(0.,1.,0.));
#119691=DIRECTION('center_axis',(-5.48307457476793E-31,-2.43497425545765E-45,
1.));
#119692=DIRECTION('ref_axis',(-4.44089209850063E-15,1.,-3.42265840282363E-60));
#119693=DIRECTION('center_axis',(0.,-1.,-1.23467863058847E-16));
#119694=DIRECTION('ref_axis',(1.,0.,0.));
#119695=DIRECTION('center_axis',(3.61400724161834E-16,1.,1.20466908053943E-16));
#119696=DIRECTION('ref_axis',(-1.,3.61400724161834E-16,-2.73691106313441E-47));
#119697=DIRECTION('',(-3.13111733906369E-16,-1.,-1.23467863058847E-16));
#119698=DIRECTION('',(3.13111733906369E-16,1.,1.23467863058847E-16));
#119699=DIRECTION('center_axis',(0.,1.23467863058847E-16,-1.));
#119700=DIRECTION('ref_axis',(0.,1.,0.));
#119701=DIRECTION('center_axis',(-0.99836765577839,0.0571141304368959,-4.12821761995348E-17));
#119702=DIRECTION('ref_axis',(-0.0571141304368959,-0.99836765577839,1.08996476499831E-33));
#119703=DIRECTION('center_axis',(0.,0.,1.));
#119704=DIRECTION('ref_axis',(0.,1.,0.));
#119705=DIRECTION('center_axis',(0.,0.,-1.));
#119706=DIRECTION('ref_axis',(0.,1.,0.));
#119707=DIRECTION('center_axis',(0.,1.23467863058847E-16,-1.));
#119708=DIRECTION('ref_axis',(0.686617021913638,-0.727019301819729,0.));
#119709=DIRECTION('center_axis',(-1.78485500480727E-31,-2.58019156504489E-46,
1.));
#119710=DIRECTION('ref_axis',(-1.44560289664734E-15,1.,0.));
#119711=DIRECTION('center_axis',(0.,0.,-1.));
#119712=DIRECTION('ref_axis',(0.,1.,0.));
#119713=DIRECTION('center_axis',(0.,1.23467863058847E-16,-1.));
#119714=DIRECTION('ref_axis',(0.,1.,0.));
#119715=DIRECTION('center_axis',(-1.,0.,0.));
#119716=DIRECTION('ref_axis',(0.,0.,1.));
#119717=DIRECTION('center_axis',(0.,0.,-1.));
#119718=DIRECTION('ref_axis',(0.,1.,0.));
#119719=DIRECTION('center_axis',(0.,1.,0.));
#119720=DIRECTION('ref_axis',(0.,0.,1.));
#119721=DIRECTION('center_axis',(0.,0.,1.));
#119722=DIRECTION('ref_axis',(0.,1.,0.));
#119723=DIRECTION('center_axis',(5.87084501074442E-17,1.,0.));
#119724=DIRECTION('ref_axis',(0.,0.,1.));
#119725=DIRECTION('center_axis',(4.81867632215779E-16,1.,1.20466908053945E-16));
#119726=DIRECTION('ref_axis',(-1.,4.81867632215779E-16,1.09476442525376E-47));
#119727=DIRECTION('',(-5.87084501074442E-17,-1.,-1.23467863058847E-16));
#119728=DIRECTION('',(5.87084501074442E-17,1.,1.23467863058847E-16));
#119729=DIRECTION('center_axis',(-1.,0.,-1.5273745825629E-32));
#119730=DIRECTION('ref_axis',(0.,-1.,0.));
#119731=DIRECTION('center_axis',(-1.,0.,0.));
#119732=DIRECTION('ref_axis',(0.,0.,1.));
#119733=DIRECTION('',(1.,1.23706245878324E-16,1.52737458256291E-32));
#119734=DIRECTION('',(-1.,-1.23706245878324E-16,-1.52737458256291E-32));
#119735=DIRECTION('center_axis',(0.,1.23467863058847E-16,-1.));
#119736=DIRECTION('ref_axis',(0.,1.,0.));
#119737=DIRECTION('center_axis',(-1.,0.,0.));
#119738=DIRECTION('ref_axis',(0.,0.,1.));
#119739=DIRECTION('center_axis',(0.,0.,1.));
#119740=DIRECTION('ref_axis',(0.,1.,0.));
#119741=DIRECTION('center_axis',(0.,0.,-1.));
#119742=DIRECTION('ref_axis',(0.,1.,0.));
#119743=DIRECTION('center_axis',(0.,1.23467863058847E-16,-1.));
#119744=DIRECTION('ref_axis',(0.,1.,0.));
#119745=DIRECTION('center_axis',(0.,1.,0.));
#119746=DIRECTION('ref_axis',(0.,0.,1.));
#119747=DIRECTION('center_axis',(0.,0.,-1.));
#119748=DIRECTION('ref_axis',(0.,1.,0.));
#119749=DIRECTION('center_axis',(3.56971000961454E-31,-1.03207662601796E-45,
1.));
#119750=DIRECTION('ref_axis',(2.89120579329468E-15,1.,-3.11150763893057E-61));
#119751=DIRECTION('center_axis',(1.,0.,4.58212374768871E-32));
#119752=DIRECTION('ref_axis',(0.,1.,0.));
#119753=DIRECTION('center_axis',(-1.,0.,0.));
#119754=DIRECTION('ref_axis',(0.,0.,1.));
#119755=DIRECTION('',(1.,3.71118737634973E-16,4.58212374768871E-32));
#119756=DIRECTION('',(-1.,-3.71118737634973E-16,-4.58212374768871E-32));
#119757=DIRECTION('center_axis',(7.82779334765923E-17,-1.,0.));
#119758=DIRECTION('ref_axis',(0.,0.,-1.));
#119759=DIRECTION('center_axis',(-1.20466908053945E-16,1.,1.20466908053943E-16));
#119760=DIRECTION('ref_axis',(-1.,-1.20466908053945E-16,2.73691106313441E-48));
#119761=DIRECTION('',(7.82779334765923E-17,-1.,-1.23467863058847E-16));
#119762=DIRECTION('',(-7.82779334765923E-17,1.,1.23467863058847E-16));
#119763=DIRECTION('center_axis',(0.,1.23467863058847E-16,-1.));
#119764=DIRECTION('ref_axis',(0.,1.,0.));
#119765=DIRECTION('center_axis',(0.,0.,-1.));
#119766=DIRECTION('ref_axis',(0.,1.,0.));
#119767=DIRECTION('center_axis',(0.,0.,1.));
#119768=DIRECTION('ref_axis',(0.,1.,0.));
#119769=DIRECTION('center_axis',(0.,1.23467863058847E-16,-1.));
#119770=DIRECTION('ref_axis',(0.,1.,0.));
#119771=DIRECTION('center_axis',(-1.,0.,0.));
#119772=DIRECTION('ref_axis',(0.,0.,1.));
#119773=DIRECTION('center_axis',(0.,0.,-1.));
#119774=DIRECTION('ref_axis',(0.,1.,0.));
#119775=DIRECTION('center_axis',(0.,1.,0.));
#119776=DIRECTION('ref_axis',(0.,0.,1.));
#119777=DIRECTION('center_axis',(0.,0.,1.));
#119778=DIRECTION('ref_axis',(0.,1.,0.));
#119779=DIRECTION('center_axis',(5.87084501074442E-17,1.,0.));
#119780=DIRECTION('ref_axis',(0.,0.,1.));
#119781=DIRECTION('center_axis',(0.,1.,0.));
#119782=DIRECTION('ref_axis',(0.,0.,1.));
#119783=DIRECTION('',(-5.87084501074442E-17,-1.,-1.23467863058847E-16));
#119784=DIRECTION('',(5.87084501074442E-17,1.,1.23467863058847E-16));
#119785=DIRECTION('center_axis',(-1.,0.,5.88789495496639E-32));
#119786=DIRECTION('ref_axis',(0.,-1.,0.));
#119787=DIRECTION('center_axis',(-1.,0.,0.));
#119788=DIRECTION('ref_axis',(0.,0.,1.));
#119789=DIRECTION('',(1.,-4.76876719908896E-16,-5.88789495496639E-32));
#119790=DIRECTION('',(-1.,4.76876719908896E-16,5.88789495496639E-32));
#119791=DIRECTION('center_axis',(0.,1.23467863058847E-16,-1.));
#119792=DIRECTION('ref_axis',(0.,1.,0.));
#119793=DIRECTION('center_axis',(-1.,0.,0.));
#119794=DIRECTION('ref_axis',(0.,0.,1.));
#119795=DIRECTION('center_axis',(1.78485500480727E-31,-2.58019156504489E-46,
1.));
#119796=DIRECTION('ref_axis',(1.44560289664734E-15,1.,-3.88938454866321E-62));
#119797=DIRECTION('center_axis',(0.,0.,-1.));
#119798=DIRECTION('ref_axis',(0.,1.,0.));
#119799=DIRECTION('center_axis',(0.,1.23467863058847E-16,-1.));
#119800=DIRECTION('ref_axis',(0.,1.,0.));
#119801=DIRECTION('center_axis',(0.,1.,0.));
#119802=DIRECTION('ref_axis',(0.,0.,1.));
#119803=DIRECTION('center_axis',(0.,0.,-1.));
#119804=DIRECTION('ref_axis',(0.,1.,0.));
#119805=DIRECTION('center_axis',(0.,0.,1.));
#119806=DIRECTION('ref_axis',(0.,1.,0.));
#119807=DIRECTION('center_axis',(1.,0.,-1.5273745825629E-32));
#119808=DIRECTION('ref_axis',(0.,1.,0.));
#119809=DIRECTION('center_axis',(-1.,0.,0.));
#119810=DIRECTION('ref_axis',(0.,0.,1.));
#119811=DIRECTION('',(1.,-1.23706245878324E-16,-1.52737458256291E-32));
#119812=DIRECTION('',(-1.,1.23706245878324E-16,1.52737458256291E-32));
#119813=DIRECTION('center_axis',(7.82779334765923E-17,-1.,0.));
#119814=DIRECTION('ref_axis',(0.,0.,-1.));
#119815=DIRECTION('center_axis',(0.,1.,0.));
#119816=DIRECTION('ref_axis',(0.,0.,1.));
#119817=DIRECTION('',(7.82779334765923E-17,-1.,-1.23467863058847E-16));
#119818=DIRECTION('',(-7.82779334765923E-17,1.,1.23467863058847E-16));
#119819=DIRECTION('center_axis',(0.,1.23467863058847E-16,-1.));
#119820=DIRECTION('ref_axis',(0.,1.,0.));
#119821=DIRECTION('center_axis',(0.,0.,-1.));
#119822=DIRECTION('ref_axis',(0.,1.,0.));
#119823=DIRECTION('center_axis',(0.,0.,1.));
#119824=DIRECTION('ref_axis',(0.,1.,0.));
#119825=DIRECTION('center_axis',(0.,1.23467863058847E-16,-1.));
#119826=DIRECTION('ref_axis',(0.,1.,0.));
#119827=DIRECTION('center_axis',(-1.,0.,0.));
#119828=DIRECTION('ref_axis',(0.,0.,1.));
#119829=DIRECTION('center_axis',(0.,0.,-1.));
#119830=DIRECTION('ref_axis',(0.,1.,0.));
#119831=DIRECTION('center_axis',(0.,1.,0.));
#119832=DIRECTION('ref_axis',(0.,0.,1.));
#119833=DIRECTION('center_axis',(0.,0.,1.));
#119834=DIRECTION('ref_axis',(0.,1.,0.));
#119835=DIRECTION('center_axis',(7.82779334765923E-17,1.,0.));
#119836=DIRECTION('ref_axis',(0.,0.,1.));
#119837=DIRECTION('center_axis',(0.,1.,0.));
#119838=DIRECTION('ref_axis',(0.,0.,1.));
#119839=DIRECTION('',(-7.82779334765923E-17,-1.,-1.23467863058847E-16));
#119840=DIRECTION('',(7.82779334765923E-17,1.,1.23467863058847E-16));
#119841=DIRECTION('center_axis',(-1.,0.,5.88789495496639E-32));
#119842=DIRECTION('ref_axis',(0.,-1.,0.));
#119843=DIRECTION('center_axis',(-1.,0.,0.));
#119844=DIRECTION('ref_axis',(0.,0.,1.));
#119845=DIRECTION('',(1.,-4.76876719908896E-16,-5.88789495496639E-32));
#119846=DIRECTION('',(-1.,4.76876719908896E-16,5.88789495496639E-32));
#119847=DIRECTION('center_axis',(0.,1.23467863058847E-16,-1.));
#119848=DIRECTION('ref_axis',(0.,1.,0.));
#119849=DIRECTION('center_axis',(-1.,0.,0.));
#119850=DIRECTION('ref_axis',(0.,0.,1.));
#119851=DIRECTION('center_axis',(0.,0.,1.));
#119852=DIRECTION('ref_axis',(0.,1.,0.));
#119853=DIRECTION('center_axis',(0.,0.,-1.));
#119854=DIRECTION('ref_axis',(0.,1.,0.));
#119855=DIRECTION('center_axis',(0.,1.23467863058847E-16,-1.));
#119856=DIRECTION('ref_axis',(0.,1.,0.));
#119857=DIRECTION('center_axis',(0.,1.,0.));
#119858=DIRECTION('ref_axis',(0.,0.,1.));
#119859=DIRECTION('center_axis',(0.,0.,-1.));
#119860=DIRECTION('ref_axis',(0.,1.,0.));
#119861=DIRECTION('center_axis',(0.,0.,1.));
#119862=DIRECTION('ref_axis',(0.,1.,0.));
#119863=DIRECTION('center_axis',(1.,0.,-1.5273745825629E-32));
#119864=DIRECTION('ref_axis',(0.,1.,0.));
#119865=DIRECTION('center_axis',(-1.,0.,0.));
#119866=DIRECTION('ref_axis',(0.,0.,1.));
#119867=DIRECTION('',(1.,-1.23706245878324E-16,-1.52737458256291E-32));
#119868=DIRECTION('',(-1.,1.23706245878324E-16,1.52737458256291E-32));
#119869=DIRECTION('center_axis',(0.,-1.,0.));
#119870=DIRECTION('ref_axis',(0.,0.,-1.));
#119871=DIRECTION('center_axis',(0.,1.,0.));
#119872=DIRECTION('ref_axis',(0.,0.,1.));
#119873=DIRECTION('',(0.,-1.,-1.23467863058847E-16));
#119874=DIRECTION('',(0.,1.,1.23467863058847E-16));
#119875=DIRECTION('center_axis',(0.,1.23467863058847E-16,-1.));
#119876=DIRECTION('ref_axis',(0.,1.,0.));
#119877=DIRECTION('center_axis',(0.,0.,-1.));
#119878=DIRECTION('ref_axis',(0.,1.,0.));
#119879=DIRECTION('center_axis',(0.,0.,1.));
#119880=DIRECTION('ref_axis',(0.,1.,0.));
#119881=DIRECTION('center_axis',(0.,1.23467863058847E-16,-1.));
#119882=DIRECTION('ref_axis',(0.,1.,0.));
#119883=DIRECTION('center_axis',(-1.,0.,0.));
#119884=DIRECTION('ref_axis',(0.,0.,1.));
#119885=DIRECTION('center_axis',(0.,0.,-1.));
#119886=DIRECTION('ref_axis',(0.,1.,0.));
#119887=DIRECTION('center_axis',(0.,1.,0.));
#119888=DIRECTION('ref_axis',(0.,0.,1.));
#119889=DIRECTION('center_axis',(0.,0.,1.));
#119890=DIRECTION('ref_axis',(0.,1.,0.));
#119891=DIRECTION('center_axis',(7.82779334765923E-17,1.,0.));
#119892=DIRECTION('ref_axis',(0.,0.,1.));
#119893=DIRECTION('center_axis',(-4.57774250604992E-15,1.,1.20466908053943E-16));
#119894=DIRECTION('ref_axis',(-1.,-4.57774250604992E-15,-3.50324616081204E-46));
#119895=DIRECTION('',(-7.82779334765923E-17,-1.,-1.23467863058847E-16));
#119896=DIRECTION('',(7.82779334765923E-17,1.,1.23467863058847E-16));
#119897=DIRECTION('center_axis',(-1.,0.,-1.5273745825629E-32));
#119898=DIRECTION('ref_axis',(0.,-1.,0.));
#119899=DIRECTION('center_axis',(-1.,0.,0.));
#119900=DIRECTION('ref_axis',(0.,0.,1.));
#119901=DIRECTION('',(1.,1.23706245878324E-16,1.52737458256291E-32));
#119902=DIRECTION('',(-1.,-1.23706245878324E-16,-1.52737458256291E-32));
#119903=DIRECTION('center_axis',(0.,1.23467863058847E-16,-1.));
#119904=DIRECTION('ref_axis',(0.,1.,0.));
#119905=DIRECTION('center_axis',(-1.,0.,0.));
#119906=DIRECTION('ref_axis',(0.,0.,1.));
#119907=DIRECTION('center_axis',(0.,0.,1.));
#119908=DIRECTION('ref_axis',(0.,1.,0.));
#119909=DIRECTION('center_axis',(0.,0.,-1.));
#119910=DIRECTION('ref_axis',(0.,1.,0.));
#119911=DIRECTION('center_axis',(0.,1.23467863058847E-16,-1.));
#119912=DIRECTION('ref_axis',(0.,1.,0.));
#119913=DIRECTION('center_axis',(0.,1.,0.));
#119914=DIRECTION('ref_axis',(0.,0.,1.));
#119915=DIRECTION('center_axis',(0.,0.,-1.));
#119916=DIRECTION('ref_axis',(0.,1.,0.));
#119917=DIRECTION('center_axis',(0.,0.,1.));
#119918=DIRECTION('ref_axis',(0.,1.,0.));
#119919=DIRECTION('center_axis',(1.,0.,4.58212374768871E-32));
#119920=DIRECTION('ref_axis',(0.,1.,0.));
#119921=DIRECTION('center_axis',(-1.,0.,0.));
#119922=DIRECTION('ref_axis',(0.,0.,1.));
#119923=DIRECTION('',(1.,3.71118737634973E-16,4.58212374768871E-32));
#119924=DIRECTION('',(-1.,-3.71118737634973E-16,-4.58212374768871E-32));
#119925=DIRECTION('center_axis',(0.,-1.,0.));
#119926=DIRECTION('ref_axis',(0.,0.,-1.));
#119927=DIRECTION('center_axis',(0.,1.,1.20466908053943E-16));
#119928=DIRECTION('ref_axis',(0.,-1.20466908053943E-16,1.));
#119929=DIRECTION('',(0.,-1.,-1.23467863058847E-16));
#119930=DIRECTION('',(0.,1.,1.23467863058847E-16));
#119931=DIRECTION('center_axis',(0.,1.23467863058847E-16,-1.));
#119932=DIRECTION('ref_axis',(0.,1.,0.));
#119933=DIRECTION('center_axis',(0.,0.,-1.));
#119934=DIRECTION('ref_axis',(0.,1.,0.));
#119935=DIRECTION('center_axis',(0.,0.,1.));
#119936=DIRECTION('ref_axis',(0.,1.,0.));
#119937=DIRECTION('center_axis',(0.,1.23467863058847E-16,-1.));
#119938=DIRECTION('ref_axis',(0.,1.,0.));
#119939=DIRECTION('center_axis',(-1.,0.,0.));
#119940=DIRECTION('ref_axis',(0.,0.,1.));
#119941=DIRECTION('center_axis',(0.,0.,-1.));
#119942=DIRECTION('ref_axis',(0.,1.,0.));
#119943=DIRECTION('center_axis',(0.,1.,0.));
#119944=DIRECTION('ref_axis',(0.,0.,1.));
#119945=DIRECTION('center_axis',(0.,0.,1.));
#119946=DIRECTION('ref_axis',(0.,1.,0.));
#119947=DIRECTION('center_axis',(0.,1.,0.));
#119948=DIRECTION('ref_axis',(0.,0.,1.));
#119949=DIRECTION('center_axis',(-3.61400724161836E-16,1.,1.20466908053943E-16));
#119950=DIRECTION('ref_axis',(-1.,-3.61400724161836E-16,1.09476442525376E-47));
#119951=DIRECTION('',(0.,-1.,-1.23467863058847E-16));
#119952=DIRECTION('',(0.,1.,1.23467863058847E-16));
#119953=DIRECTION('center_axis',(-1.,0.,-1.5273745825629E-32));
#119954=DIRECTION('ref_axis',(0.,-1.,0.));
#119955=DIRECTION('center_axis',(-1.,0.,0.));
#119956=DIRECTION('ref_axis',(0.,0.,1.));
#119957=DIRECTION('',(1.,1.23706245878324E-16,1.52737458256291E-32));
#119958=DIRECTION('',(-1.,-1.23706245878324E-16,-1.52737458256291E-32));
#119959=DIRECTION('center_axis',(0.,1.23467863058847E-16,-1.));
#119960=DIRECTION('ref_axis',(0.,1.,0.));
#119961=DIRECTION('center_axis',(-1.,0.,0.));
#119962=DIRECTION('ref_axis',(0.,0.,1.));
#119963=DIRECTION('center_axis',(0.,0.,1.));
#119964=DIRECTION('ref_axis',(0.,1.,0.));
#119965=DIRECTION('center_axis',(0.,0.,-1.));
#119966=DIRECTION('ref_axis',(0.,1.,0.));
#119967=DIRECTION('center_axis',(0.,1.23467863058847E-16,-1.));
#119968=DIRECTION('ref_axis',(0.,1.,0.));
#119969=DIRECTION('center_axis',(-0.0294983404866172,0.999564829267485,
0.));
#119970=DIRECTION('ref_axis',(-0.999564829267485,-0.0294983404866172,0.));
#119971=DIRECTION('center_axis',(0.,0.,-1.));
#119972=DIRECTION('ref_axis',(0.,1.,0.));
#119973=DIRECTION('center_axis',(0.,0.,1.));
#119974=DIRECTION('ref_axis',(0.,1.,0.));
#119975=DIRECTION('center_axis',(1.,0.,4.58212374768871E-32));
#119976=DIRECTION('ref_axis',(0.,1.,0.));
#119977=DIRECTION('center_axis',(-1.,0.,0.));
#119978=DIRECTION('ref_axis',(0.,0.,1.));
#119979=DIRECTION('',(1.,3.71118737634973E-16,4.58212374768871E-32));
#119980=DIRECTION('',(-1.,-3.71118737634973E-16,-4.58212374768871E-32));
#119981=DIRECTION('center_axis',(0.,1.23467863058847E-16,-1.));
#119982=DIRECTION('ref_axis',(0.,1.,1.25697703075927E-16));
#119983=DIRECTION('center_axis',(-0.0175200318846342,0.999846512462169,
1.20448417884836E-16));
#119984=DIRECTION('ref_axis',(-0.999846512462169,-0.0175200318846342,1.51017636338582E-32));
#119985=DIRECTION('center_axis',(0.,1.22914743790472E-16,-1.));
#119986=DIRECTION('ref_axis',(0.,1.,1.22914743790472E-16));
#119987=DIRECTION('center_axis',(1.11644282221188E-31,-1.22833149346405E-16,
1.));
#119988=DIRECTION('ref_axis',(1.75897069864052E-13,1.,1.22833149346405E-16));
#119989=DIRECTION('center_axis',(0.,1.23467863058847E-16,-1.));
#119990=DIRECTION('ref_axis',(0.,1.,0.));
#119991=DIRECTION('center_axis',(0.,0.,-1.));
#119992=DIRECTION('ref_axis',(0.,1.,0.));
#119993=DIRECTION('center_axis',(0.,0.,1.));
#119994=DIRECTION('ref_axis',(0.,1.,0.));
#119995=DIRECTION('center_axis',(0.,1.23467863058847E-16,-1.));
#119996=DIRECTION('ref_axis',(0.,1.,0.));
#119997=DIRECTION('center_axis',(-1.,0.,0.));
#119998=DIRECTION('ref_axis',(0.,0.,1.));
#119999=DIRECTION('center_axis',(0.,0.,-1.));
#120000=DIRECTION('ref_axis',(0.,1.,0.));
#120001=DIRECTION('center_axis',(0.,1.,0.));
#120002=DIRECTION('ref_axis',(0.,0.,1.));
#120003=DIRECTION('center_axis',(0.,0.,1.));
#120004=DIRECTION('ref_axis',(0.,1.,0.));
#120005=DIRECTION('center_axis',(0.,1.,0.));
#120006=DIRECTION('ref_axis',(0.,0.,1.));
#120007=DIRECTION('center_axis',(0.,1.,0.));
#120008=DIRECTION('ref_axis',(0.,0.,1.));
#120009=DIRECTION('',(0.,-1.,-1.23467863058847E-16));
#120010=DIRECTION('',(0.,1.,1.23467863058847E-16));
#120011=DIRECTION('center_axis',(-1.,0.,5.88789495496639E-32));
#120012=DIRECTION('ref_axis',(0.,-1.,0.));
#120013=DIRECTION('center_axis',(-1.,0.,0.));
#120014=DIRECTION('ref_axis',(0.,0.,1.));
#120015=DIRECTION('',(1.,-4.76876719908896E-16,-5.88789495496639E-32));
#120016=DIRECTION('',(-1.,4.76876719908896E-16,5.88789495496639E-32));
#120017=DIRECTION('center_axis',(0.,1.23467863058847E-16,-1.));
#120018=DIRECTION('ref_axis',(0.,1.,0.));
#120019=DIRECTION('center_axis',(-1.,0.,0.));
#120020=DIRECTION('ref_axis',(0.,0.,1.));
#120021=DIRECTION('center_axis',(0.,0.,1.));
#120022=DIRECTION('ref_axis',(0.,1.,0.));
#120023=DIRECTION('center_axis',(0.,0.,-1.));
#120024=DIRECTION('ref_axis',(0.,1.,0.));
#120025=DIRECTION('center_axis',(0.,1.23467863058847E-16,-1.));
#120026=DIRECTION('ref_axis',(0.,1.,0.));
#120027=DIRECTION('center_axis',(-0.646912564190485,0.762564183719962,0.));
#120028=DIRECTION('ref_axis',(-0.762564183719962,-0.646912564190485,0.));
#120029=DIRECTION('center_axis',(0.,0.,-1.));
#120030=DIRECTION('ref_axis',(0.,1.,0.));
#120031=DIRECTION('center_axis',(0.,0.,1.));
#120032=DIRECTION('ref_axis',(0.,1.,0.));
#120033=DIRECTION('center_axis',(1.,0.,-1.5273745825629E-32));
#120034=DIRECTION('ref_axis',(0.,1.,0.));
#120035=DIRECTION('center_axis',(-1.,0.,0.));
#120036=DIRECTION('ref_axis',(0.,0.,1.));
#120037=DIRECTION('',(1.,-1.23706245878324E-16,-1.52737458256291E-32));
#120038=DIRECTION('',(-1.,1.23706245878324E-16,1.52737458256291E-32));
#120039=DIRECTION('center_axis',(0.,1.23467863058847E-16,-1.));
#120040=DIRECTION('ref_axis',(0.,1.,0.));
#120041=DIRECTION('center_axis',(-0.55837318130784,0.829589892896582,0.));
#120042=DIRECTION('ref_axis',(-0.829589892896582,-0.55837318130784,0.));
#120043=DIRECTION('center_axis',(0.,0.,-1.));
#120044=DIRECTION('ref_axis',(0.,1.,0.));
#120045=DIRECTION('center_axis',(-6.57968948972152E-31,-3.50636292785903E-45,
1.));
#120046=DIRECTION('ref_axis',(-5.32907051820075E-15,1.,0.));
#120047=DIRECTION('center_axis',(0.,1.23467863058847E-16,-1.));
#120048=DIRECTION('ref_axis',(0.,1.,0.));
#120049=DIRECTION('center_axis',(0.0331928226750539,-0.999448966442441,
0.));
#120050=DIRECTION('ref_axis',(0.99944896644244,0.0331928226750539,0.));
#120051=DIRECTION('center_axis',(0.,0.,1.));
#120052=DIRECTION('ref_axis',(0.,1.,0.));
#120053=DIRECTION('center_axis',(0.,0.,-1.));
#120054=DIRECTION('ref_axis',(0.,1.,0.));
#120055=DIRECTION('center_axis',(0.,1.23467863058847E-16,-1.));
#120056=DIRECTION('ref_axis',(0.,1.,0.));
#120057=DIRECTION('center_axis',(-0.03879684915621,0.999247118832749,0.));
#120058=DIRECTION('ref_axis',(-0.999247118832749,-0.03879684915621,0.));
#120059=DIRECTION('center_axis',(0.,0.,-1.));
#120060=DIRECTION('ref_axis',(0.,1.,0.));
#120061=DIRECTION('center_axis',(-1.18169710663102E-30,-1.13098908268507E-44,
1.));
#120062=DIRECTION('ref_axis',(-9.57088814332033E-15,1.,-2.7381267222589E-59));
#120063=DIRECTION('center_axis',(0.,1.23467863058847E-16,-1.));
#120064=DIRECTION('ref_axis',(0.,1.,1.25697703075927E-16));
#120065=DIRECTION('center_axis',(0.,1.22914743790472E-16,-1.));
#120066=DIRECTION('ref_axis',(0.,1.,1.22914743790472E-16));
#120067=DIRECTION('center_axis',(1.18920911416235E-31,-1.22833149346405E-16,
1.));
#120068=DIRECTION('ref_axis',(1.87361497136383E-13,1.,1.22833149346405E-16));
#120069=DIRECTION('center_axis',(0.,1.23467863058847E-16,-1.));
#120070=DIRECTION('ref_axis',(0.,1.,0.));
#120071=DIRECTION('center_axis',(-1.,0.,0.));
#120072=DIRECTION('ref_axis',(0.,0.,1.));
#120073=DIRECTION('center_axis',(0.,0.,-1.));
#120074=DIRECTION('ref_axis',(0.,1.,0.));
#120075=DIRECTION('center_axis',(0.,1.,9.63735264431547E-16));
#120076=DIRECTION('ref_axis',(0.,-9.63735264431547E-16,1.));
#120077=DIRECTION('center_axis',(0.,0.,1.));
#120078=DIRECTION('ref_axis',(0.,1.,0.));
#120079=DIRECTION('center_axis',(0.,1.,0.));
#120080=DIRECTION('ref_axis',(0.,0.,1.));
#120081=DIRECTION('center_axis',(-3.85494105772624E-15,1.,0.));
#120082=DIRECTION('ref_axis',(-1.,-3.85494105772625E-15,0.));
#120083=DIRECTION('',(0.,-1.,-1.23467863058847E-16));
#120084=DIRECTION('',(0.,1.,1.23467863058847E-16));
#120085=DIRECTION('center_axis',(-1.,0.,4.58212374768871E-32));
#120086=DIRECTION('ref_axis',(0.,-1.,0.));
#120087=DIRECTION('center_axis',(-1.,0.,0.));
#120088=DIRECTION('ref_axis',(0.,0.,1.));
#120089=DIRECTION('',(1.,-3.71118737634973E-16,-4.58212374768871E-32));
#120090=DIRECTION('',(-1.,3.71118737634973E-16,4.58212374768871E-32));
#120091=DIRECTION('center_axis',(0.,1.23467863058847E-16,-1.));
#120092=DIRECTION('ref_axis',(0.,1.,0.));
#120093=DIRECTION('center_axis',(-1.,0.,0.));
#120094=DIRECTION('ref_axis',(0.,0.,1.));
#120095=DIRECTION('center_axis',(0.,0.,1.));
#120096=DIRECTION('ref_axis',(0.,1.,0.));
#120097=DIRECTION('center_axis',(0.,0.,-1.));
#120098=DIRECTION('ref_axis',(0.,1.,0.));
#120099=DIRECTION('center_axis',(0.,1.23467863058847E-16,-1.));
#120100=DIRECTION('ref_axis',(0.,1.,0.));
#120101=DIRECTION('center_axis',(-0.0138255496962061,0.999904422520272,
0.));
#120102=DIRECTION('ref_axis',(-0.999904422520272,-0.0138255496962061,0.));
#120103=DIRECTION('center_axis',(0.,0.,-1.));
#120104=DIRECTION('ref_axis',(0.,1.,0.));
#120105=DIRECTION('center_axis',(0.,0.,1.));
#120106=DIRECTION('ref_axis',(0.,1.,0.));
#120107=DIRECTION('center_axis',(1.,0.,4.58212374768871E-32));
#120108=DIRECTION('ref_axis',(0.,1.,0.));
#120109=DIRECTION('center_axis',(-1.,0.,0.));
#120110=DIRECTION('ref_axis',(0.,0.,1.));
#120111=DIRECTION('',(1.,3.71118737634973E-16,4.58212374768871E-32));
#120112=DIRECTION('',(-1.,-3.71118737634973E-16,-4.58212374768871E-32));
#120113=DIRECTION('center_axis',(0.,1.23467863058847E-16,-1.));
#120114=DIRECTION('ref_axis',(0.,1.,1.25697703075927E-16));
#120115=DIRECTION('center_axis',(-0.00184724109421639,0.999998293848714,
0.));
#120116=DIRECTION('ref_axis',(-0.999998293848714,-0.00184724109421639,0.));
#120117=DIRECTION('center_axis',(0.,1.22914743790472E-16,-1.));
#120118=DIRECTION('ref_axis',(0.,1.,1.22914743790472E-16));
#120119=DIRECTION('center_axis',(5.51984300367294E-32,-1.22833149346405E-16,
1.));
#120120=DIRECTION('ref_axis',(8.69658697372547E-14,1.,1.22833149346405E-16));
#120121=DIRECTION('center_axis',(0.,1.23467863058847E-16,-1.));
#120122=DIRECTION('ref_axis',(0.,1.,0.));
#120123=DIRECTION('center_axis',(0.,0.,-1.));
#120124=DIRECTION('ref_axis',(0.,1.,0.));
#120125=DIRECTION('center_axis',(0.,0.,1.));
#120126=DIRECTION('ref_axis',(0.,1.,0.));
#120127=DIRECTION('center_axis',(0.,1.23467863058847E-16,-1.));
#120128=DIRECTION('ref_axis',(0.,1.,0.));
#120129=DIRECTION('center_axis',(-1.,0.,0.));
#120130=DIRECTION('ref_axis',(0.,0.,1.));
#120131=DIRECTION('center_axis',(0.,0.,-1.));
#120132=DIRECTION('ref_axis',(0.,1.,0.));
#120133=DIRECTION('center_axis',(0.,1.,9.63735264431547E-16));
#120134=DIRECTION('ref_axis',(0.,-9.63735264431547E-16,1.));
#120135=DIRECTION('center_axis',(0.,0.,1.));
#120136=DIRECTION('ref_axis',(0.,1.,0.));
#120137=DIRECTION('center_axis',(7.82779334765923E-17,1.,0.));
#120138=DIRECTION('ref_axis',(0.,0.,1.));
#120139=DIRECTION('center_axis',(-3.85494105772624E-15,1.,0.));
#120140=DIRECTION('ref_axis',(-1.,-3.85494105772625E-15,0.));
#120141=DIRECTION('',(-7.82779334765923E-17,-1.,-1.23467863058847E-16));
#120142=DIRECTION('',(7.82779334765923E-17,1.,1.23467863058847E-16));
#120143=DIRECTION('center_axis',(-1.,0.,4.58212374768871E-32));
#120144=DIRECTION('ref_axis',(0.,-1.,0.));
#120145=DIRECTION('center_axis',(-1.,0.,0.));
#120146=DIRECTION('ref_axis',(0.,0.,1.));
#120147=DIRECTION('',(1.,-3.71118737634973E-16,-4.58212374768871E-32));
#120148=DIRECTION('',(-1.,3.71118737634973E-16,4.58212374768871E-32));
#120149=DIRECTION('center_axis',(0.,1.23467863058847E-16,-1.));
#120150=DIRECTION('ref_axis',(0.,1.,0.));
#120151=DIRECTION('center_axis',(-1.,0.,0.));
#120152=DIRECTION('ref_axis',(0.,0.,1.));
#120153=DIRECTION('center_axis',(0.,0.,1.));
#120154=DIRECTION('ref_axis',(0.,1.,0.));
#120155=DIRECTION('center_axis',(0.,0.,-1.));
#120156=DIRECTION('ref_axis',(0.,1.,0.));
#120157=DIRECTION('center_axis',(0.,1.23467863058847E-16,-1.));
#120158=DIRECTION('ref_axis',(0.,1.,0.));
#120159=DIRECTION('center_axis',(0.,1.,0.));
#120160=DIRECTION('ref_axis',(0.,0.,1.));
#120161=DIRECTION('center_axis',(0.,0.,-1.));
#120162=DIRECTION('ref_axis',(0.,1.,0.));
#120163=DIRECTION('center_axis',(0.,0.,1.));
#120164=DIRECTION('ref_axis',(0.,1.,0.));
#120165=DIRECTION('center_axis',(1.,0.,4.58212374768871E-32));
#120166=DIRECTION('ref_axis',(0.,1.,0.));
#120167=DIRECTION('center_axis',(-1.,0.,0.));
#120168=DIRECTION('ref_axis',(0.,0.,1.));
#120169=DIRECTION('',(1.,3.71118737634973E-16,4.58212374768871E-32));
#120170=DIRECTION('',(-1.,-3.71118737634973E-16,-4.58212374768871E-32));
#120171=DIRECTION('center_axis',(0.,-1.,0.));
#120172=DIRECTION('ref_axis',(0.,0.,-1.));
#120173=DIRECTION('center_axis',(0.,1.,0.));
#120174=DIRECTION('ref_axis',(0.,0.,1.));
#120175=DIRECTION('',(0.,-1.,-1.23467863058847E-16));
#120176=DIRECTION('',(0.,1.,1.23467863058847E-16));
#120177=DIRECTION('center_axis',(0.,1.23467863058847E-16,-1.));
#120178=DIRECTION('ref_axis',(0.,1.,0.));
#120179=DIRECTION('center_axis',(0.,0.,-1.));
#120180=DIRECTION('ref_axis',(0.,1.,0.));
#120181=DIRECTION('center_axis',(0.,0.,1.));
#120182=DIRECTION('ref_axis',(0.,1.,0.));
#120183=DIRECTION('center_axis',(0.,1.23467863058847E-16,-1.));
#120184=DIRECTION('ref_axis',(0.,1.,0.));
#120185=DIRECTION('center_axis',(0.0972343474872435,-0.995261514210577,
0.));
#120186=DIRECTION('ref_axis',(0.995261514210577,0.0972343474872435,0.));
#120187=DIRECTION('center_axis',(0.,0.,-1.));
#120188=DIRECTION('ref_axis',(0.,1.,0.));
#120189=DIRECTION('center_axis',(-1.,0.,0.));
#120190=DIRECTION('ref_axis',(0.,0.,1.));
#120191=DIRECTION('center_axis',(1.78485500480727E-31,-2.58019156504489E-46,
1.));
#120192=DIRECTION('ref_axis',(1.44560289664734E-15,1.,-3.88938454866321E-62));
#120193=DIRECTION('center_axis',(1.,0.,4.58212374768871E-32));
#120194=DIRECTION('ref_axis',(0.,1.,0.));
#120195=DIRECTION('center_axis',(-1.,0.,0.));
#120196=DIRECTION('ref_axis',(0.,0.,1.));
#120197=DIRECTION('',(1.,3.71118737634973E-16,4.58212374768871E-32));
#120198=DIRECTION('',(-1.,-3.71118737634973E-16,-4.58212374768871E-32));
#120199=DIRECTION('center_axis',(0.,1.23467863058847E-16,-1.));
#120200=DIRECTION('ref_axis',(0.,1.,0.));
#120201=DIRECTION('center_axis',(0.359814015251205,-0.933024048151389,0.));
#120202=DIRECTION('ref_axis',(0.933024048151389,0.359814015251205,0.));
#120203=DIRECTION('center_axis',(-9.86953423458227E-31,-7.88931658768281E-45,
1.));
#120204=DIRECTION('ref_axis',(-7.99360577730113E-15,1.,-2.48920611114446E-60));
#120205=DIRECTION('center_axis',(0.,0.,-1.));
#120206=DIRECTION('ref_axis',(0.,1.,0.));
#120207=DIRECTION('center_axis',(0.,1.23467863058847E-16,-1.));
#120208=DIRECTION('ref_axis',(0.,1.,0.));
#120209=DIRECTION('center_axis',(0.,-1.,0.));
#120210=DIRECTION('ref_axis',(0.,0.,-1.));
#120211=DIRECTION('center_axis',(0.,0.,1.));
#120212=DIRECTION('ref_axis',(0.,1.,0.));
#120213=DIRECTION('center_axis',(0.,0.,-1.));
#120214=DIRECTION('ref_axis',(0.,1.,0.));
#120215=DIRECTION('center_axis',(0.,1.23467863058847E-16,-1.));
#120216=DIRECTION('ref_axis',(0.,1.,0.));
#120217=DIRECTION('center_axis',(0.,-1.,0.));
#120218=DIRECTION('ref_axis',(0.,0.,-1.));
#120219=DIRECTION('center_axis',(0.,0.,-1.));
#120220=DIRECTION('ref_axis',(0.,1.,0.));
#120221=DIRECTION('center_axis',(0.,0.,1.));
#120222=DIRECTION('ref_axis',(0.,1.,0.));
#120223=DIRECTION('center_axis',(7.82779334765923E-17,-1.,0.));
#120224=DIRECTION('ref_axis',(0.,0.,-1.));
#120225=DIRECTION('center_axis',(0.,-1.,0.));
#120226=DIRECTION('ref_axis',(0.,0.,-1.));
#120227=DIRECTION('',(-7.82779334765923E-17,1.,1.23467863058847E-16));
#120228=DIRECTION('',(7.82779334765923E-17,-1.,-1.23467863058847E-16));
#120229=DIRECTION('center_axis',(5.87084501074442E-17,1.,0.));
#120230=DIRECTION('ref_axis',(0.,0.,1.));
#120231=DIRECTION('center_axis',(0.,-1.,0.));
#120232=DIRECTION('ref_axis',(0.,0.,-1.));
#120233=DIRECTION('',(5.87084501074442E-17,1.,1.23467863058847E-16));
#120234=DIRECTION('',(-5.87084501074442E-17,-1.,-1.23467863058847E-16));
#120235=DIRECTION('center_axis',(0.,1.23467863058847E-16,-1.));
#120236=DIRECTION('ref_axis',(0.,1.,0.));
#120237=DIRECTION('center_axis',(1.,0.,0.));
#120238=DIRECTION('ref_axis',(0.,0.,-1.));
#120239=DIRECTION('center_axis',(3.56971000961454E-31,-1.03207662601795E-45,
1.));
#120240=DIRECTION('ref_axis',(2.89120579329468E-15,1.,-2.1780553472514E-60));
#120241=DIRECTION('center_axis',(0.,0.,-1.));
#120242=DIRECTION('ref_axis',(0.,1.,0.));
#120243=DIRECTION('center_axis',(0.,1.23467863058847E-16,-1.));
#120244=DIRECTION('ref_axis',(0.,1.,0.));
#120245=DIRECTION('center_axis',(-1.,0.,0.));
#120246=DIRECTION('ref_axis',(0.,0.,1.));
#120247=DIRECTION('center_axis',(0.,0.,-1.));
#120248=DIRECTION('ref_axis',(0.,1.,0.));
#120249=DIRECTION('center_axis',(0.,0.,1.));
#120250=DIRECTION('ref_axis',(0.,1.,0.));
#120251=DIRECTION('center_axis',(-1.,0.,4.58212374768871E-32));
#120252=DIRECTION('ref_axis',(0.,-1.,0.));
#120253=DIRECTION('',(1.,-3.71118737634973E-16,-4.58212374768871E-32));
#120254=DIRECTION('',(-1.,3.71118737634973E-16,4.58212374768871E-32));
#120255=DIRECTION('center_axis',(0.,1.23467863058847E-16,-1.));
#120256=DIRECTION('ref_axis',(0.,1.,0.));
#120257=DIRECTION('center_axis',(7.70988211545246E-15,-1.,0.));
#120258=DIRECTION('ref_axis',(1.,7.70988211545246E-15,0.));
#120259=DIRECTION('center_axis',(0.,0.,-1.));
#120260=DIRECTION('ref_axis',(0.,1.,0.));
#120261=DIRECTION('center_axis',(-1.,0.,0.));
#120262=DIRECTION('ref_axis',(0.,0.,1.));
#120263=DIRECTION('center_axis',(1.78485500480727E-31,-2.58019156504489E-46,
1.));
#120264=DIRECTION('ref_axis',(1.44560289664734E-15,1.,-3.88938454866321E-62));
#120265=DIRECTION('center_axis',(1.,0.,4.07299888683441E-32));
#120266=DIRECTION('ref_axis',(0.,1.,0.));
#120267=DIRECTION('center_axis',(-1.,0.,0.));
#120268=DIRECTION('ref_axis',(0.,0.,1.));
#120269=DIRECTION('',(1.,3.29883322342198E-16,4.07299888683441E-32));
#120270=DIRECTION('',(-1.,-3.29883322342198E-16,-4.07299888683441E-32));
#120271=DIRECTION('center_axis',(5.87084501074442E-17,1.,0.));
#120272=DIRECTION('ref_axis',(0.,0.,1.));
#120273=DIRECTION('center_axis',(0.,-1.,0.));
#120274=DIRECTION('ref_axis',(0.,0.,-1.));
#120275=DIRECTION('',(5.87084501074442E-17,1.,1.23467863058847E-16));
#120276=DIRECTION('',(-5.87084501074442E-17,-1.,-1.23467863058847E-16));
#120277=DIRECTION('center_axis',(0.,1.23467863058847E-16,-1.));
#120278=DIRECTION('ref_axis',(0.,1.,0.));
#120279=DIRECTION('center_axis',(0.,-1.,0.));
#120280=DIRECTION('ref_axis',(0.,0.,-1.));
#120281=DIRECTION('center_axis',(0.,0.,1.));
#120282=DIRECTION('ref_axis',(0.,1.,0.));
#120283=DIRECTION('center_axis',(0.,0.,-1.));
#120284=DIRECTION('ref_axis',(0.,1.,0.));
#120285=DIRECTION('center_axis',(0.,1.23467863058847E-16,-1.));
#120286=DIRECTION('ref_axis',(0.,1.,0.));
#120287=DIRECTION('center_axis',(-0.359814015251208,-0.933024048151388,
0.));
#120288=DIRECTION('ref_axis',(0.933024048151388,-0.359814015251207,0.));
#120289=DIRECTION('center_axis',(0.,0.,-1.));
#120290=DIRECTION('ref_axis',(0.,1.,0.));
#120291=DIRECTION('center_axis',(0.,0.,1.));
#120292=DIRECTION('ref_axis',(0.,1.,0.));
#120293=DIRECTION('center_axis',(7.82779334765923E-17,-1.,0.));
#120294=DIRECTION('ref_axis',(0.,0.,-1.));
#120295=DIRECTION('center_axis',(-3.85494105772624E-15,-1.,0.));
#120296=DIRECTION('ref_axis',(1.,-3.85494105772625E-15,0.));
#120297=DIRECTION('',(-7.82779334765923E-17,1.,1.23467863058847E-16));
#120298=DIRECTION('',(7.82779334765923E-17,-1.,-1.23467863058847E-16));
#120299=DIRECTION('center_axis',(0.,1.23467863058847E-16,-1.));
#120300=DIRECTION('ref_axis',(0.,1.,0.));
#120301=DIRECTION('center_axis',(-0.0972343474872435,-0.995261514210577,
0.));
#120302=DIRECTION('ref_axis',(0.995261514210577,-0.0972343474872435,0.));
#120303=DIRECTION('center_axis',(-8.77291931962869E-31,-6.2335340939716E-45,
1.));
#120304=DIRECTION('ref_axis',(-7.105427357601E-15,1.,-3.73380916671668E-60));
#120305=DIRECTION('center_axis',(0.,0.,-1.));
#120306=DIRECTION('ref_axis',(0.,1.,0.));
#120307=DIRECTION('center_axis',(0.,1.23467863058847E-16,-1.));
#120308=DIRECTION('ref_axis',(0.,1.,0.));
#120309=DIRECTION('center_axis',(1.,0.,0.));
#120310=DIRECTION('ref_axis',(0.,0.,-1.));
#120311=DIRECTION('center_axis',(0.,0.,1.));
#120312=DIRECTION('ref_axis',(0.,1.,0.));
#120313=DIRECTION('center_axis',(0.,0.,-1.));
#120314=DIRECTION('ref_axis',(0.,1.,0.));
#120315=DIRECTION('center_axis',(0.,1.23467863058847E-16,-1.));
#120316=DIRECTION('ref_axis',(0.,1.,0.));
#120317=DIRECTION('center_axis',(-1.,0.,0.));
#120318=DIRECTION('ref_axis',(0.,0.,1.));
#120319=DIRECTION('center_axis',(0.,0.,-1.));
#120320=DIRECTION('ref_axis',(0.,1.,0.));
#120321=DIRECTION('center_axis',(0.,0.,1.));
#120322=DIRECTION('ref_axis',(0.,1.,0.));
#120323=DIRECTION('center_axis',(-1.,0.,4.58212374768871E-32));
#120324=DIRECTION('ref_axis',(0.,-1.,0.));
#120325=DIRECTION('',(1.,-3.71118737634973E-16,-4.58212374768871E-32));
#120326=DIRECTION('',(-1.,3.71118737634973E-16,4.58212374768871E-32));
#120327=DIRECTION('center_axis',(0.,1.23467863058847E-16,-1.));
#120328=DIRECTION('ref_axis',(0.,1.,0.));
#120329=DIRECTION('center_axis',(0.,-1.,0.));
#120330=DIRECTION('ref_axis',(0.,0.,-1.));
#120331=DIRECTION('center_axis',(0.,0.,-1.));
#120332=DIRECTION('ref_axis',(0.,1.,0.));
#120333=DIRECTION('center_axis',(-1.,0.,0.));
#120334=DIRECTION('ref_axis',(0.,0.,1.));
#120335=DIRECTION('center_axis',(0.,0.,1.));
#120336=DIRECTION('ref_axis',(0.,1.,0.));
#120337=DIRECTION('center_axis',(1.,0.,4.07299888683441E-32));
#120338=DIRECTION('ref_axis',(0.,1.,0.));
#120339=DIRECTION('center_axis',(-1.,0.,0.));
#120340=DIRECTION('ref_axis',(0.,0.,1.));
#120341=DIRECTION('',(1.,3.29883322342198E-16,4.07299888683441E-32));
#120342=DIRECTION('',(-1.,-3.29883322342198E-16,-4.07299888683441E-32));
#120343=DIRECTION('center_axis',(7.82779334765923E-17,1.,0.));
#120344=DIRECTION('ref_axis',(0.,0.,1.));
#120345=DIRECTION('center_axis',(0.,-1.,0.));
#120346=DIRECTION('ref_axis',(0.,0.,-1.));
#120347=DIRECTION('',(7.82779334765923E-17,1.,1.23467863058847E-16));
#120348=DIRECTION('',(-7.82779334765923E-17,-1.,-1.23467863058847E-16));
#120349=DIRECTION('center_axis',(0.,1.23467863058847E-16,-1.));
#120350=DIRECTION('ref_axis',(0.,1.,0.));
#120351=DIRECTION('center_axis',(0.,-1.,0.));
#120352=DIRECTION('ref_axis',(0.,0.,-1.));
#120353=DIRECTION('center_axis',(0.,0.,1.));
#120354=DIRECTION('ref_axis',(0.,1.,0.));
#120355=DIRECTION('center_axis',(0.,0.,-1.));
#120356=DIRECTION('ref_axis',(0.,1.,0.));
#120357=DIRECTION('center_axis',(0.,1.23467863058847E-16,-1.));
#120358=DIRECTION('ref_axis',(0.,1.,0.));
#120359=DIRECTION('center_axis',(-1.,0.,0.));
#120360=DIRECTION('ref_axis',(0.,0.,1.));
#120361=DIRECTION('center_axis',(0.,0.,-1.));
#120362=DIRECTION('ref_axis',(0.,1.,0.));
#120363=DIRECTION('center_axis',(0.,0.,1.));
#120364=DIRECTION('ref_axis',(0.,1.,0.));
#120365=DIRECTION('center_axis',(0.,-1.,0.));
#120366=DIRECTION('ref_axis',(0.,0.,-1.));
#120367=DIRECTION('center_axis',(-3.85494105772624E-15,-1.,0.));
#120368=DIRECTION('ref_axis',(1.,-3.85494105772625E-15,0.));
#120369=DIRECTION('',(0.,1.,1.23467863058847E-16));
#120370=DIRECTION('',(0.,-1.,-1.23467863058847E-16));
#120371=DIRECTION('center_axis',(-1.,0.,4.58212374768871E-32));
#120372=DIRECTION('ref_axis',(0.,-1.,0.));
#120373=DIRECTION('center_axis',(-1.,0.,0.));
#120374=DIRECTION('ref_axis',(0.,0.,1.));
#120375=DIRECTION('',(1.,-3.71118737634973E-16,-4.58212374768871E-32));
#120376=DIRECTION('',(-1.,3.71118737634973E-16,4.58212374768871E-32));
#120377=DIRECTION('center_axis',(0.,1.23467863058847E-16,-1.));
#120378=DIRECTION('ref_axis',(0.,1.,0.));
#120379=DIRECTION('center_axis',(0.,0.,-1.));
#120380=DIRECTION('ref_axis',(0.,1.,0.));
#120381=DIRECTION('center_axis',(0.,0.,1.));
#120382=DIRECTION('ref_axis',(0.,1.,0.));
#120383=DIRECTION('center_axis',(0.,1.23467863058847E-16,-1.));
#120384=DIRECTION('ref_axis',(0.,1.,0.));
#120385=DIRECTION('center_axis',(0.,-1.,0.));
#120386=DIRECTION('ref_axis',(0.,0.,-1.));
#120387=DIRECTION('center_axis',(0.,0.,-1.));
#120388=DIRECTION('ref_axis',(0.,1.,0.));
#120389=DIRECTION('center_axis',(-1.,0.,0.));
#120390=DIRECTION('ref_axis',(0.,0.,1.));
#120391=DIRECTION('center_axis',(0.,0.,1.));
#120392=DIRECTION('ref_axis',(0.,1.,0.));
#120393=DIRECTION('center_axis',(1.,0.,4.07299888683441E-32));
#120394=DIRECTION('ref_axis',(0.,1.,0.));
#120395=DIRECTION('center_axis',(-1.,0.,0.));
#120396=DIRECTION('ref_axis',(0.,0.,1.));
#120397=DIRECTION('',(1.,3.29883322342198E-16,4.07299888683441E-32));
#120398=DIRECTION('',(-1.,-3.29883322342198E-16,-4.07299888683441E-32));
#120399=DIRECTION('center_axis',(0.,1.,0.));
#120400=DIRECTION('ref_axis',(0.,0.,1.));
#120401=DIRECTION('center_axis',(0.,-1.,0.));
#120402=DIRECTION('ref_axis',(0.,0.,-1.));
#120403=DIRECTION('',(0.,1.,1.23467863058847E-16));
#120404=DIRECTION('',(0.,-1.,-1.23467863058847E-16));
#120405=DIRECTION('center_axis',(0.,1.23467863058847E-16,-1.));
#120406=DIRECTION('ref_axis',(0.,1.,0.));
#120407=DIRECTION('center_axis',(-0.0138255496962003,-0.999904422520272,
3.41098746684905E-15));
#120408=DIRECTION('ref_axis',(0.999904422520272,-0.0138255496962003,-3.38006024551251E-32));
#120409=DIRECTION('center_axis',(0.,0.,1.));
#120410=DIRECTION('ref_axis',(0.,1.,0.));
#120411=DIRECTION('center_axis',(0.,0.,-1.));
#120412=DIRECTION('ref_axis',(0.,1.,0.));
#120413=DIRECTION('center_axis',(0.,1.23467863058847E-16,-1.));
#120414=DIRECTION('ref_axis',(0.,1.,0.));
#120415=DIRECTION('center_axis',(-1.,0.,0.));
#120416=DIRECTION('ref_axis',(0.,0.,1.));
#120417=DIRECTION('center_axis',(0.,0.,-1.));
#120418=DIRECTION('ref_axis',(0.,1.,0.));
#120419=DIRECTION('center_axis',(0.,0.,1.));
#120420=DIRECTION('ref_axis',(0.,1.,0.));
#120421=DIRECTION('center_axis',(0.,1.23467863058847E-16,-1.));
#120422=DIRECTION('ref_axis',(0.,1.,1.25697703075927E-16));
#120423=DIRECTION('center_axis',(-0.00184724109421639,-0.999998293848714,
0.));
#120424=DIRECTION('ref_axis',(0.999998293848714,-0.00184724109421639,0.));
#120425=DIRECTION('center_axis',(0.,-1.22833149346405E-16,1.));
#120426=DIRECTION('ref_axis',(0.,1.,1.22833149346405E-16));
#120427=DIRECTION('center_axis',(0.,1.22914743790472E-16,-1.));
#120428=DIRECTION('ref_axis',(0.,1.,1.22914743790472E-16));
#120429=DIRECTION('center_axis',(-1.,0.,4.58212374768871E-32));
#120430=DIRECTION('ref_axis',(0.,-1.,0.));
#120431=DIRECTION('center_axis',(-1.,0.,0.));
#120432=DIRECTION('ref_axis',(0.,0.,1.));
#120433=DIRECTION('',(1.,-3.71118737634973E-16,-4.58212374768871E-32));
#120434=DIRECTION('',(-1.,3.71118737634973E-16,4.58212374768871E-32));
#120435=DIRECTION('center_axis',(0.,1.23467863058847E-16,-1.));
#120436=DIRECTION('ref_axis',(0.,1.,0.));
#120437=DIRECTION('center_axis',(0.,0.,-1.));
#120438=DIRECTION('ref_axis',(0.,1.,0.));
#120439=DIRECTION('center_axis',(0.,0.,1.));
#120440=DIRECTION('ref_axis',(0.,1.,0.));
#120441=DIRECTION('center_axis',(0.,1.23467863058847E-16,-1.));
#120442=DIRECTION('ref_axis',(0.,1.,0.));
#120443=DIRECTION('center_axis',(0.,1.,0.));
#120444=DIRECTION('ref_axis',(0.,0.,1.));
#120445=DIRECTION('center_axis',(0.,0.,-1.));
#120446=DIRECTION('ref_axis',(0.,1.,0.));
#120447=DIRECTION('center_axis',(1.,0.,0.));
#120448=DIRECTION('ref_axis',(0.,0.,-1.));
#120449=DIRECTION('center_axis',(0.,0.,1.));
#120450=DIRECTION('ref_axis',(0.,1.,0.));
#120451=DIRECTION('center_axis',(-1.,0.,4.07299888683441E-32));
#120452=DIRECTION('ref_axis',(0.,-1.,0.));
#120453=DIRECTION('center_axis',(1.,0.,0.));
#120454=DIRECTION('ref_axis',(0.,0.,-1.));
#120455=DIRECTION('',(-1.,3.29883322342198E-16,4.07299888683441E-32));
#120456=DIRECTION('',(1.,-3.29883322342198E-16,-4.07299888683441E-32));
#120457=DIRECTION('center_axis',(0.,-1.,0.));
#120458=DIRECTION('ref_axis',(0.,0.,-1.));
#120459=DIRECTION('center_axis',(0.,1.,0.));
#120460=DIRECTION('ref_axis',(0.,0.,1.));
#120461=DIRECTION('',(0.,-1.,-1.23467863058847E-16));
#120462=DIRECTION('',(0.,1.,1.23467863058847E-16));
#120463=DIRECTION('center_axis',(0.,1.23467863058847E-16,-1.));
#120464=DIRECTION('ref_axis',(0.,1.,0.));
#120465=DIRECTION('center_axis',(0.,1.,0.));
#120466=DIRECTION('ref_axis',(0.,0.,1.));
#120467=DIRECTION('center_axis',(0.,0.,1.));
#120468=DIRECTION('ref_axis',(0.,1.,0.));
#120469=DIRECTION('center_axis',(0.,0.,-1.));
#120470=DIRECTION('ref_axis',(0.,1.,0.));
#120471=DIRECTION('center_axis',(0.,1.23467863058847E-16,-1.));
#120472=DIRECTION('ref_axis',(0.,1.,0.));
#120473=DIRECTION('center_axis',(1.,0.,0.));
#120474=DIRECTION('ref_axis',(0.,0.,-1.));
#120475=DIRECTION('center_axis',(0.,0.,-1.));
#120476=DIRECTION('ref_axis',(0.,1.,0.));
#120477=DIRECTION('center_axis',(0.,0.,1.));
#120478=DIRECTION('ref_axis',(0.,1.,0.));
#120479=DIRECTION('center_axis',(7.82779334765923E-17,1.,0.));
#120480=DIRECTION('ref_axis',(0.,0.,1.));
#120481=DIRECTION('center_axis',(1.5419764230905E-14,1.,0.));
#120482=DIRECTION('ref_axis',(-1.,1.5419764230905E-14,0.));
#120483=DIRECTION('',(-7.82779334765923E-17,-1.,-1.23467863058847E-16));
#120484=DIRECTION('',(7.82779334765923E-17,1.,1.23467863058847E-16));
#120485=DIRECTION('center_axis',(1.,0.,4.07299888683445E-32));
#120486=DIRECTION('ref_axis',(0.,1.,0.));
#120487=DIRECTION('center_axis',(1.,0.,0.));
#120488=DIRECTION('ref_axis',(0.,0.,-1.));
#120489=DIRECTION('',(-1.,-3.29883322342202E-16,-4.07299888683446E-32));
#120490=DIRECTION('',(1.,3.29883322342202E-16,4.07299888683446E-32));
#120491=DIRECTION('center_axis',(0.,1.23467863058847E-16,-1.));
#120492=DIRECTION('ref_axis',(0.,1.,0.));
#120493=DIRECTION('center_axis',(0.,0.,-1.));
#120494=DIRECTION('ref_axis',(0.,1.,0.));
#120495=DIRECTION('center_axis',(0.,0.,1.));
#120496=DIRECTION('ref_axis',(0.,1.,0.));
#120497=DIRECTION('center_axis',(0.,1.23467863058847E-16,-1.));
#120498=DIRECTION('ref_axis',(0.,1.,0.));
#120499=DIRECTION('center_axis',(0.,1.,0.));
#120500=DIRECTION('ref_axis',(0.,0.,1.));
#120501=DIRECTION('center_axis',(0.,0.,-1.));
#120502=DIRECTION('ref_axis',(0.,1.,0.));
#120503=DIRECTION('center_axis',(1.,0.,0.));
#120504=DIRECTION('ref_axis',(0.,0.,-1.));
#120505=DIRECTION('center_axis',(0.,0.,1.));
#120506=DIRECTION('ref_axis',(0.,1.,0.));
#120507=DIRECTION('center_axis',(-1.,0.,4.07299888683441E-32));
#120508=DIRECTION('ref_axis',(0.,-1.,0.));
#120509=DIRECTION('center_axis',(1.,0.,0.));
#120510=DIRECTION('ref_axis',(0.,0.,-1.));
#120511=DIRECTION('',(-1.,3.29883322342198E-16,4.07299888683441E-32));
#120512=DIRECTION('',(1.,-3.29883322342198E-16,-4.07299888683441E-32));
#120513=DIRECTION('center_axis',(7.82779334765923E-17,-1.,0.));
#120514=DIRECTION('ref_axis',(0.,0.,-1.));
#120515=DIRECTION('center_axis',(0.,1.,0.));
#120516=DIRECTION('ref_axis',(0.,0.,1.));
#120517=DIRECTION('',(7.82779334765923E-17,-1.,-1.23467863058847E-16));
#120518=DIRECTION('',(-7.82779334765923E-17,1.,1.23467863058847E-16));
#120519=DIRECTION('center_axis',(0.,1.23467863058847E-16,-1.));
#120520=DIRECTION('ref_axis',(0.,1.,0.));
#120521=DIRECTION('center_axis',(0.,1.,0.));
#120522=DIRECTION('ref_axis',(0.,0.,1.));
#120523=DIRECTION('center_axis',(0.,0.,1.));
#120524=DIRECTION('ref_axis',(0.,1.,0.));
#120525=DIRECTION('center_axis',(0.,0.,-1.));
#120526=DIRECTION('ref_axis',(0.,1.,0.));
#120527=DIRECTION('center_axis',(0.,1.23467863058847E-16,-1.));
#120528=DIRECTION('ref_axis',(0.,1.,0.));
#120529=DIRECTION('center_axis',(1.,0.,0.));
#120530=DIRECTION('ref_axis',(0.,0.,-1.));
#120531=DIRECTION('center_axis',(0.,0.,-1.));
#120532=DIRECTION('ref_axis',(0.,1.,0.));
#120533=DIRECTION('center_axis',(0.,0.,1.));
#120534=DIRECTION('ref_axis',(0.,1.,0.));
#120535=DIRECTION('center_axis',(5.87084501074442E-17,1.,0.));
#120536=DIRECTION('ref_axis',(0.,0.,1.));
#120537=DIRECTION('center_axis',(1.5419764230905E-14,1.,5.94422822341731E-29));
#120538=DIRECTION('ref_axis',(-1.,1.5419764230905E-14,1.59309191113245E-57));
#120539=DIRECTION('',(-5.87084501074442E-17,-1.,-1.23467863058847E-16));
#120540=DIRECTION('',(5.87084501074442E-17,1.,1.23467863058847E-16));
#120541=DIRECTION('center_axis',(1.,0.,4.07299888683445E-32));
#120542=DIRECTION('ref_axis',(0.,1.,0.));
#120543=DIRECTION('center_axis',(1.,0.,0.));
#120544=DIRECTION('ref_axis',(0.,0.,-1.));
#120545=DIRECTION('',(-1.,-3.29883322342202E-16,-4.07299888683446E-32));
#120546=DIRECTION('',(1.,3.29883322342202E-16,4.07299888683446E-32));
#120547=DIRECTION('center_axis',(0.,1.23467863058847E-16,-1.));
#120548=DIRECTION('ref_axis',(0.,1.,0.));
#120549=DIRECTION('center_axis',(0.,0.,-1.));
#120550=DIRECTION('ref_axis',(0.,1.,0.));
#120551=DIRECTION('center_axis',(0.,0.,1.));
#120552=DIRECTION('ref_axis',(0.,1.,0.));
#120553=DIRECTION('center_axis',(0.,1.23467863058847E-16,-1.));
#120554=DIRECTION('ref_axis',(0.,1.,0.));
#120555=DIRECTION('center_axis',(0.,-1.,0.));
#120556=DIRECTION('ref_axis',(0.,0.,-1.));
#120557=DIRECTION('center_axis',(0.,0.,-1.));
#120558=DIRECTION('ref_axis',(0.,1.,0.));
#120559=DIRECTION('center_axis',(-1.,-4.81867632215781E-16,-7.43028527927166E-30));
#120560=DIRECTION('ref_axis',(4.81867632215781E-16,-1.,1.36218908067985E-60));
#120561=DIRECTION('center_axis',(0.,0.,1.));
#120562=DIRECTION('ref_axis',(0.,1.,0.));
#120563=DIRECTION('center_axis',(1.,0.,4.07299888683445E-32));
#120564=DIRECTION('ref_axis',(0.,1.,0.));
#120565=DIRECTION('center_axis',(-1.,0.,0.));
#120566=DIRECTION('ref_axis',(0.,0.,1.));
#120567=DIRECTION('',(1.,3.29883322342202E-16,4.07299888683446E-32));
#120568=DIRECTION('',(-1.,-3.29883322342202E-16,-4.07299888683446E-32));
#120569=DIRECTION('center_axis',(6.11546355285877E-17,1.,0.));
#120570=DIRECTION('ref_axis',(0.,0.,1.));
#120571=DIRECTION('center_axis',(0.,-1.,0.));
#120572=DIRECTION('ref_axis',(0.,0.,-1.));
#120573=DIRECTION('',(6.11546355285877E-17,1.,1.23467863058847E-16));
#120574=DIRECTION('',(-6.11546355285877E-17,-1.,-1.23467863058847E-16));
#120575=DIRECTION('center_axis',(0.,1.23467863058847E-16,-1.));
#120576=DIRECTION('ref_axis',(0.,1.,0.));
#120577=DIRECTION('center_axis',(0.,-1.,0.));
#120578=DIRECTION('ref_axis',(0.,0.,-1.));
#120579=DIRECTION('center_axis',(0.,0.,1.));
#120580=DIRECTION('ref_axis',(0.,1.,0.));
#120581=DIRECTION('center_axis',(0.,0.,-1.));
#120582=DIRECTION('ref_axis',(0.,1.,0.));
#120583=DIRECTION('center_axis',(0.,1.23467863058847E-16,-1.));
#120584=DIRECTION('ref_axis',(0.,1.,0.));
#120585=DIRECTION('center_axis',(-0.995922166025996,-0.0902166238455435,
0.));
#120586=DIRECTION('ref_axis',(0.0902166238455435,-0.995922166025996,0.));
#120587=DIRECTION('center_axis',(0.,0.,-1.));
#120588=DIRECTION('ref_axis',(0.,1.,0.));
#120589=DIRECTION('center_axis',(1.11553437800454E-31,-1.00788733009566E-46,
1.));
#120590=DIRECTION('ref_axis',(9.03501810404587E-16,1.,1.16681536459896E-61));
#120591=DIRECTION('center_axis',(0.,-1.,-1.23467863058847E-16));
#120592=DIRECTION('ref_axis',(1.,0.,0.));
#120593=DIRECTION('center_axis',(0.,-1.,0.));
#120594=DIRECTION('ref_axis',(0.,0.,-1.));
#120595=DIRECTION('',(3.13111733906369E-16,1.,1.23467863058847E-16));
#120596=DIRECTION('',(-3.13111733906369E-16,-1.,-1.23467863058847E-16));
#120597=DIRECTION('center_axis',(0.,1.23467863058847E-16,-1.));
#120598=DIRECTION('ref_axis',(0.,1.,0.));
#120599=DIRECTION('center_axis',(-0.913440670994019,-0.406971916198153,
0.));
#120600=DIRECTION('ref_axis',(0.406971916198153,-0.913440670994019,0.));
#120601=DIRECTION('center_axis',(0.,0.,1.));
#120602=DIRECTION('ref_axis',(0.,1.,0.));
#120603=DIRECTION('center_axis',(0.,0.,-1.));
#120604=DIRECTION('ref_axis',(0.,1.,0.));
#120605=DIRECTION('center_axis',(0.,1.23467863058847E-16,-1.));
#120606=DIRECTION('ref_axis',(0.,1.,0.));
#120607=DIRECTION('center_axis',(0.,0.,1.));
#120608=DIRECTION('ref_axis',(0.,1.,0.));
#120609=DIRECTION('center_axis',(0.,0.,-1.));
#120610=DIRECTION('ref_axis',(0.,1.,0.));
#120611=DIRECTION('center_axis',(0.99836765577839,0.0571141304368842,0.));
#120612=DIRECTION('ref_axis',(-0.0571141304368842,0.99836765577839,0.));
#120613=DIRECTION('center_axis',(0.,1.23467863058847E-16,-1.));
#120614=DIRECTION('ref_axis',(0.,1.,0.));
#120615=DIRECTION('center_axis',(0.,0.,1.));
#120616=DIRECTION('ref_axis',(0.,1.,0.));
#120617=DIRECTION('center_axis',(0.,0.,-1.));
#120618=DIRECTION('ref_axis',(0.,1.,0.));
#120619=DIRECTION('center_axis',(0.,1.23467863058847E-16,-1.));
#120620=DIRECTION('ref_axis',(0.,1.,0.));
#120621=DIRECTION('center_axis',(0.,-1.,0.));
#120622=DIRECTION('ref_axis',(0.,0.,-1.));
#120623=DIRECTION('center_axis',(0.,0.,-1.));
#120624=DIRECTION('ref_axis',(0.,1.,0.));
#120625=DIRECTION('center_axis',(-1.,0.,0.));
#120626=DIRECTION('ref_axis',(0.,0.,1.));
#120627=DIRECTION('center_axis',(0.,0.,1.));
#120628=DIRECTION('ref_axis',(0.,1.,0.));
#120629=DIRECTION('center_axis',(1.,0.,4.07299888683445E-32));
#120630=DIRECTION('ref_axis',(0.,1.,0.));
#120631=DIRECTION('center_axis',(-1.,0.,0.));
#120632=DIRECTION('ref_axis',(0.,0.,1.));
#120633=DIRECTION('',(1.,3.29883322342202E-16,4.07299888683446E-32));
#120634=DIRECTION('',(-1.,-3.29883322342202E-16,-4.07299888683446E-32));
#120635=DIRECTION('center_axis',(0.,1.,0.));
#120636=DIRECTION('ref_axis',(0.,0.,1.));
#120637=DIRECTION('center_axis',(0.,-1.,0.));
#120638=DIRECTION('ref_axis',(0.,0.,-1.));
#120639=DIRECTION('',(0.,1.,1.23467863058847E-16));
#120640=DIRECTION('',(0.,-1.,-1.23467863058847E-16));
#120641=DIRECTION('center_axis',(0.,1.23467863058847E-16,-1.));
#120642=DIRECTION('ref_axis',(0.,1.,0.));
#120643=DIRECTION('center_axis',(-0.0294983404866249,-0.999564829267484,
0.));
#120644=DIRECTION('ref_axis',(0.999564829267484,-0.0294983404866249,0.));
#120645=DIRECTION('center_axis',(0.,0.,1.));
#120646=DIRECTION('ref_axis',(0.,1.,0.));
#120647=DIRECTION('center_axis',(0.,0.,-1.));
#120648=DIRECTION('ref_axis',(0.,1.,0.));
#120649=DIRECTION('center_axis',(0.,1.23467863058847E-16,-1.));
#120650=DIRECTION('ref_axis',(0.,1.,0.));
#120651=DIRECTION('center_axis',(-1.,0.,0.));
#120652=DIRECTION('ref_axis',(0.,0.,1.));
#120653=DIRECTION('center_axis',(0.,0.,-1.));
#120654=DIRECTION('ref_axis',(0.,1.,0.));
#120655=DIRECTION('center_axis',(0.,0.,1.));
#120656=DIRECTION('ref_axis',(0.,1.,0.));
#120657=DIRECTION('center_axis',(0.,1.23467863058847E-16,-1.));
#120658=DIRECTION('ref_axis',(0.,1.,1.25697703075927E-16));
#120659=DIRECTION('center_axis',(-0.0175200318846409,-0.999846512462168,
-7.7086987446295E-15));
#120660=DIRECTION('ref_axis',(0.999846512462168,-0.0175200318846409,1.3995963210887E-31));
#120661=DIRECTION('center_axis',(-1.09981052690886E-31,-1.22833149346405E-16,
1.));
#120662=DIRECTION('ref_axis',(-1.73276629344662E-13,1.,1.22833149346405E-16));
#120663=DIRECTION('center_axis',(0.,1.22914743790472E-16,-1.));
#120664=DIRECTION('ref_axis',(0.,1.,1.22914743790472E-16));
#120665=DIRECTION('center_axis',(-1.,0.,4.07299888683441E-32));
#120666=DIRECTION('ref_axis',(0.,-1.,0.));
#120667=DIRECTION('center_axis',(-1.,0.,0.));
#120668=DIRECTION('ref_axis',(0.,0.,1.));
#120669=DIRECTION('',(1.,-3.29883322342198E-16,-4.07299888683441E-32));
#120670=DIRECTION('',(-1.,3.29883322342198E-16,4.07299888683441E-32));
#120671=DIRECTION('center_axis',(0.,1.23467863058847E-16,-1.));
#120672=DIRECTION('ref_axis',(0.,1.,0.));
#120673=DIRECTION('center_axis',(0.,0.,-1.));
#120674=DIRECTION('ref_axis',(0.,1.,0.));
#120675=DIRECTION('center_axis',(0.,0.,1.));
#120676=DIRECTION('ref_axis',(0.,1.,0.));
#120677=DIRECTION('center_axis',(0.,1.23467863058847E-16,-1.));
#120678=DIRECTION('ref_axis',(0.,1.,0.));
#120679=DIRECTION('center_axis',(-1.5419764230905E-14,-1.,0.));
#120680=DIRECTION('ref_axis',(1.,-1.5419764230905E-14,0.));
#120681=DIRECTION('center_axis',(0.,0.,-1.));
#120682=DIRECTION('ref_axis',(0.,1.,0.));
#120683=DIRECTION('center_axis',(-1.,0.,0.));
#120684=DIRECTION('ref_axis',(0.,0.,1.));
#120685=DIRECTION('center_axis',(0.,0.,1.));
#120686=DIRECTION('ref_axis',(0.,1.,0.));
#120687=DIRECTION('center_axis',(1.,0.,7.06547394595967E-32));
#120688=DIRECTION('ref_axis',(0.,1.,0.));
#120689=DIRECTION('center_axis',(-1.,0.,0.));
#120690=DIRECTION('ref_axis',(0.,0.,1.));
#120691=DIRECTION('',(1.,5.72252063890675E-16,7.06547394595967E-32));
#120692=DIRECTION('',(-1.,-5.72252063890675E-16,-7.06547394595967E-32));
#120693=DIRECTION('center_axis',(0.,1.,0.));
#120694=DIRECTION('ref_axis',(0.,0.,1.));
#120695=DIRECTION('center_axis',(0.,-1.,0.));
#120696=DIRECTION('ref_axis',(0.,0.,-1.));
#120697=DIRECTION('',(0.,1.,1.23467863058847E-16));
#120698=DIRECTION('',(0.,-1.,-1.23467863058847E-16));
#120699=DIRECTION('center_axis',(0.,1.23467863058847E-16,-1.));
#120700=DIRECTION('ref_axis',(0.,1.,0.));
#120701=DIRECTION('center_axis',(-0.64691256419049,-0.762564183719958,0.));
#120702=DIRECTION('ref_axis',(0.762564183719958,-0.64691256419049,0.));
#120703=DIRECTION('center_axis',(0.,0.,1.));
#120704=DIRECTION('ref_axis',(0.,1.,0.));
#120705=DIRECTION('center_axis',(0.,0.,-1.));
#120706=DIRECTION('ref_axis',(0.,1.,0.));
#120707=DIRECTION('center_axis',(0.,1.23467863058847E-16,-1.));
#120708=DIRECTION('ref_axis',(0.,1.,0.));
#120709=DIRECTION('center_axis',(-1.,0.,0.));
#120710=DIRECTION('ref_axis',(0.,0.,1.));
#120711=DIRECTION('center_axis',(0.,0.,-1.));
#120712=DIRECTION('ref_axis',(0.,1.,0.));
#120713=DIRECTION('center_axis',(0.,0.,1.));
#120714=DIRECTION('ref_axis',(0.,1.,0.));
#120715=DIRECTION('center_axis',(0.,1.23467863058847E-16,-1.));
#120716=DIRECTION('ref_axis',(0.,1.,0.));
#120717=DIRECTION('center_axis',(-0.55837318130784,-0.829589892896582,0.));
#120718=DIRECTION('ref_axis',(0.829589892896582,-0.55837318130784,0.));
#120719=DIRECTION('center_axis',(0.,0.,1.));
#120720=DIRECTION('ref_axis',(0.,1.,0.));
#120721=DIRECTION('center_axis',(0.,0.,-1.));
#120722=DIRECTION('ref_axis',(0.,1.,0.));
#120723=DIRECTION('center_axis',(-1.,0.,4.07299888683445E-32));
#120724=DIRECTION('ref_axis',(0.,-1.,0.));
#120725=DIRECTION('center_axis',(-1.,0.,0.));
#120726=DIRECTION('ref_axis',(0.,0.,1.));
#120727=DIRECTION('',(1.,-3.29883322342202E-16,-4.07299888683446E-32));
#120728=DIRECTION('',(-1.,3.29883322342202E-16,4.07299888683446E-32));
#120729=DIRECTION('center_axis',(0.,1.23467863058847E-16,-1.));
#120730=DIRECTION('ref_axis',(0.,1.,0.));
#120731=DIRECTION('center_axis',(-0.03879684915621,-0.999247118832749,-5.83634271056011E-15));
#120732=DIRECTION('ref_axis',(0.999247118832749,-0.03879684915621,-4.4574149748685E-34));
#120733=DIRECTION('center_axis',(0.,0.,1.));
#120734=DIRECTION('ref_axis',(0.,1.,0.));
#120735=DIRECTION('center_axis',(0.,0.,-1.));
#120736=DIRECTION('ref_axis',(0.,1.,0.));
#120737=DIRECTION('center_axis',(0.,1.23467863058847E-16,-1.));
#120738=DIRECTION('ref_axis',(0.,1.,0.));
#120739=DIRECTION('center_axis',(0.0331928226750423,0.999448966442441,0.));
#120740=DIRECTION('ref_axis',(-0.999448966442441,0.0331928226750423,0.));
#120741=DIRECTION('center_axis',(0.,0.,-1.));
#120742=DIRECTION('ref_axis',(0.,1.,0.));
#120743=DIRECTION('center_axis',(0.,0.,1.));
#120744=DIRECTION('ref_axis',(0.,1.,0.));
#120745=DIRECTION('center_axis',(0.,1.23467863058847E-16,-1.));
#120746=DIRECTION('ref_axis',(0.,1.,1.25697703075927E-16));
#120747=DIRECTION('center_axis',(0.,1.22914743790472E-16,-1.));
#120748=DIRECTION('ref_axis',(0.,1.,1.22914743790472E-16));
#120749=DIRECTION('center_axis',(-1.17257681885938E-31,-1.22833149346405E-16,
1.));
#120750=DIRECTION('ref_axis',(-1.84741056616993E-13,1.,1.22833149346405E-16));
#120751=DIRECTION('center_axis',(0.,1.23467863058847E-16,-1.));
#120752=DIRECTION('ref_axis',(0.,1.,0.));
#120753=DIRECTION('center_axis',(0.,-1.,0.));
#120754=DIRECTION('ref_axis',(0.,0.,-1.));
#120755=DIRECTION('center_axis',(0.,0.,-1.));
#120756=DIRECTION('ref_axis',(0.,1.,0.));
#120757=DIRECTION('center_axis',(-1.,0.,0.));
#120758=DIRECTION('ref_axis',(0.,0.,1.));
#120759=DIRECTION('center_axis',(0.,0.,1.));
#120760=DIRECTION('ref_axis',(0.,1.,0.));
#120761=DIRECTION('center_axis',(1.,0.,7.06547394595967E-32));
#120762=DIRECTION('ref_axis',(0.,1.,0.));
#120763=DIRECTION('center_axis',(-1.,0.,0.));
#120764=DIRECTION('ref_axis',(0.,0.,1.));
#120765=DIRECTION('',(1.,5.72252063890675E-16,7.06547394595967E-32));
#120766=DIRECTION('',(-1.,-5.72252063890675E-16,-7.06547394595967E-32));
#120767=DIRECTION('center_axis',(7.82779334765923E-17,1.,0.));
#120768=DIRECTION('ref_axis',(0.,0.,1.));
#120769=DIRECTION('center_axis',(0.,-1.,0.));
#120770=DIRECTION('ref_axis',(0.,0.,-1.));
#120771=DIRECTION('',(7.82779334765923E-17,1.,1.23467863058847E-16));
#120772=DIRECTION('',(-7.82779334765923E-17,-1.,-1.23467863058847E-16));
#120773=DIRECTION('center_axis',(0.,1.23467863058847E-16,-1.));
#120774=DIRECTION('ref_axis',(0.,1.,0.));
#120775=DIRECTION('center_axis',(0.,-1.,0.));
#120776=DIRECTION('ref_axis',(0.,0.,-1.));
#120777=DIRECTION('center_axis',(0.,0.,1.));
#120778=DIRECTION('ref_axis',(0.,1.,0.));
#120779=DIRECTION('center_axis',(0.,0.,-1.));
#120780=DIRECTION('ref_axis',(0.,1.,0.));
#120781=DIRECTION('center_axis',(0.,1.23467863058847E-16,-1.));
#120782=DIRECTION('ref_axis',(0.,1.,0.));
#120783=DIRECTION('center_axis',(-1.,0.,0.));
#120784=DIRECTION('ref_axis',(0.,0.,1.));
#120785=DIRECTION('center_axis',(0.,0.,-1.));
#120786=DIRECTION('ref_axis',(0.,1.,0.));
#120787=DIRECTION('center_axis',(0.,0.,1.));
#120788=DIRECTION('ref_axis',(0.,1.,0.));
#120789=DIRECTION('center_axis',(0.,-1.,0.));
#120790=DIRECTION('ref_axis',(0.,0.,-1.));
#120791=DIRECTION('center_axis',(1.5419764230905E-14,-1.,0.));
#120792=DIRECTION('ref_axis',(1.,1.5419764230905E-14,0.));
#120793=DIRECTION('',(0.,1.,1.23467863058847E-16));
#120794=DIRECTION('',(0.,-1.,-1.23467863058847E-16));
#120795=DIRECTION('center_axis',(-1.,0.,4.07299888683445E-32));
#120796=DIRECTION('ref_axis',(0.,-1.,0.));
#120797=DIRECTION('center_axis',(-1.,0.,0.));
#120798=DIRECTION('ref_axis',(0.,0.,1.));
#120799=DIRECTION('',(1.,-3.29883322342202E-16,-4.07299888683446E-32));
#120800=DIRECTION('',(-1.,3.29883322342202E-16,4.07299888683446E-32));
#120801=DIRECTION('center_axis',(0.,1.23467863058847E-16,-1.));
#120802=DIRECTION('ref_axis',(0.,1.,0.));
#120803=DIRECTION('center_axis',(0.,0.,-1.));
#120804=DIRECTION('ref_axis',(0.,1.,0.));
#120805=DIRECTION('center_axis',(0.,0.,1.));
#120806=DIRECTION('ref_axis',(0.,1.,0.));
#120807=DIRECTION('center_axis',(0.,1.23467863058847E-16,-1.));
#120808=DIRECTION('ref_axis',(0.,1.,0.));
#120809=DIRECTION('center_axis',(-1.5419764230905E-14,1.,0.));
#120810=DIRECTION('ref_axis',(-1.,-1.5419764230905E-14,0.));
#120811=DIRECTION('center_axis',(0.,0.,-1.));
#120812=DIRECTION('ref_axis',(0.,1.,0.));
#120813=DIRECTION('center_axis',(1.,0.,0.));
#120814=DIRECTION('ref_axis',(0.,0.,-1.));
#120815=DIRECTION('center_axis',(0.,0.,1.));
#120816=DIRECTION('ref_axis',(0.,1.,0.));
#120817=DIRECTION('center_axis',(-1.,0.,-2.35515798198655E-32));
#120818=DIRECTION('ref_axis',(0.,-1.,0.));
#120819=DIRECTION('center_axis',(1.,0.,0.));
#120820=DIRECTION('ref_axis',(0.,0.,-1.));
#120821=DIRECTION('',(-1.,-1.90750687963558E-16,-2.35515798198656E-32));
#120822=DIRECTION('',(1.,1.90750687963558E-16,2.35515798198656E-32));
#120823=DIRECTION('center_axis',(0.,-1.,0.));
#120824=DIRECTION('ref_axis',(0.,0.,-1.));
#120825=DIRECTION('center_axis',(0.,1.,0.));
#120826=DIRECTION('ref_axis',(0.,0.,1.));
#120827=DIRECTION('',(0.,-1.,-1.23467863058847E-16));
#120828=DIRECTION('',(0.,1.,1.23467863058847E-16));
#120829=DIRECTION('center_axis',(0.,1.23467863058847E-16,-1.));
#120830=DIRECTION('ref_axis',(0.,1.,0.));
#120831=DIRECTION('center_axis',(0.,1.,0.));
#120832=DIRECTION('ref_axis',(0.,0.,1.));
#120833=DIRECTION('center_axis',(0.,0.,1.));
#120834=DIRECTION('ref_axis',(0.,1.,0.));
#120835=DIRECTION('center_axis',(0.,0.,-1.));
#120836=DIRECTION('ref_axis',(0.,1.,0.));
#120837=DIRECTION('center_axis',(0.,1.23467863058847E-16,-1.));
#120838=DIRECTION('ref_axis',(0.,1.,0.));
#120839=DIRECTION('center_axis',(0.787431540449696,0.616402116402125,0.));
#120840=DIRECTION('ref_axis',(-0.616402116402125,0.787431540449696,0.));
#120841=DIRECTION('center_axis',(0.,0.,-1.));
#120842=DIRECTION('ref_axis',(0.,1.,0.));
#120843=DIRECTION('center_axis',(0.,0.,1.));
#120844=DIRECTION('ref_axis',(0.,1.,0.));
#120845=DIRECTION('center_axis',(7.82779334765923E-17,1.,0.));
#120846=DIRECTION('ref_axis',(0.,0.,1.));
#120847=DIRECTION('center_axis',(0.,1.,0.));
#120848=DIRECTION('ref_axis',(0.,0.,1.));
#120849=DIRECTION('',(-7.82779334765923E-17,-1.,-1.23467863058847E-16));
#120850=DIRECTION('',(7.82779334765923E-17,1.,1.23467863058847E-16));
#120851=DIRECTION('center_axis',(0.,1.23467863058847E-16,-1.));
#120852=DIRECTION('ref_axis',(0.,1.,0.));
#120853=DIRECTION('center_axis',(0.873059908686793,0.487612957009766,0.));
#120854=DIRECTION('ref_axis',(-0.487612957009766,0.873059908686793,0.));
#120855=DIRECTION('center_axis',(0.,0.,-1.));
#120856=DIRECTION('ref_axis',(0.,1.,0.));
#120857=DIRECTION('center_axis',(0.,0.,1.));
#120858=DIRECTION('ref_axis',(0.,1.,0.));
#120859=DIRECTION('center_axis',(0.,1.23467863058847E-16,-1.));
#120860=DIRECTION('ref_axis',(-0.695782815675815,-0.718252235228151,0.));
#120861=DIRECTION('center_axis',(-0.99949512518498,-0.0317725468205174,
0.));
#120862=DIRECTION('ref_axis',(0.0317725468205174,-0.99949512518498,0.));
#120863=DIRECTION('center_axis',(0.,0.,1.));
#120864=DIRECTION('ref_axis',(0.,1.,0.));
#120865=DIRECTION('center_axis',(0.,0.,-1.));
#120866=DIRECTION('ref_axis',(0.,1.,0.));
#120867=DIRECTION('center_axis',(0.,1.23467863058847E-16,-1.));
#120868=DIRECTION('ref_axis',(0.,1.,0.));
#120869=DIRECTION('center_axis',(0.999425898115847,0.0338802918425069,0.));
#120870=DIRECTION('ref_axis',(-0.0338802918425069,0.999425898115847,0.));
#120871=DIRECTION('center_axis',(0.,0.,-1.));
#120872=DIRECTION('ref_axis',(0.,1.,0.));
#120873=DIRECTION('center_axis',(0.,0.,1.));
#120874=DIRECTION('ref_axis',(0.,1.,0.));
#120875=DIRECTION('center_axis',(0.,1.23467863058847E-16,-1.));
#120876=DIRECTION('ref_axis',(0.,1.,1.25697703075927E-16));
#120877=DIRECTION('center_axis',(0.,1.22914743790472E-16,-1.));
#120878=DIRECTION('ref_axis',(0.,1.,1.22914743790472E-16));
#120879=DIRECTION('center_axis',(0.,-1.22833149346405E-16,1.));
#120880=DIRECTION('ref_axis',(0.,1.,1.22833149346405E-16));
#120881=DIRECTION('center_axis',(0.,1.23467863058847E-16,-1.));
#120882=DIRECTION('ref_axis',(0.,1.,0.));
#120883=DIRECTION('center_axis',(-1.5419764230905E-14,1.,0.));
#120884=DIRECTION('ref_axis',(-1.,-1.5419764230905E-14,0.));
#120885=DIRECTION('center_axis',(0.,0.,-1.));
#120886=DIRECTION('ref_axis',(0.,1.,0.));
#120887=DIRECTION('center_axis',(1.,0.,0.));
#120888=DIRECTION('ref_axis',(0.,0.,-1.));
#120889=DIRECTION('center_axis',(0.,0.,1.));
#120890=DIRECTION('ref_axis',(0.,1.,0.));
#120891=DIRECTION('center_axis',(-1.,0.,-2.35515798198655E-32));
#120892=DIRECTION('ref_axis',(0.,-1.,0.));
#120893=DIRECTION('center_axis',(1.,0.,0.));
#120894=DIRECTION('ref_axis',(0.,0.,-1.));
#120895=DIRECTION('',(-1.,-1.90750687963558E-16,-2.35515798198656E-32));
#120896=DIRECTION('',(1.,1.90750687963558E-16,2.35515798198656E-32));
#120897=DIRECTION('center_axis',(7.82779334765923E-17,-1.,0.));
#120898=DIRECTION('ref_axis',(0.,0.,-1.));
#120899=DIRECTION('center_axis',(0.,1.,0.));
#120900=DIRECTION('ref_axis',(0.,0.,1.));
#120901=DIRECTION('',(7.82779334765923E-17,-1.,-1.23467863058847E-16));
#120902=DIRECTION('',(-7.82779334765923E-17,1.,1.23467863058847E-16));
#120903=DIRECTION('center_axis',(0.,1.23467863058847E-16,-1.));
#120904=DIRECTION('ref_axis',(0.,1.,0.));
#120905=DIRECTION('center_axis',(0.,1.,0.));
#120906=DIRECTION('ref_axis',(0.,0.,1.));
#120907=DIRECTION('center_axis',(0.,0.,1.));
#120908=DIRECTION('ref_axis',(0.,1.,0.));
#120909=DIRECTION('center_axis',(0.,0.,-1.));
#120910=DIRECTION('ref_axis',(0.,1.,0.));
#120911=DIRECTION('center_axis',(0.,1.23467863058847E-16,-1.));
#120912=DIRECTION('ref_axis',(0.,1.,0.));
#120913=DIRECTION('center_axis',(0.99960573342019,0.0280780646320843,0.));
#120914=DIRECTION('ref_axis',(-0.0280780646320843,0.99960573342019,0.));
#120915=DIRECTION('center_axis',(0.,0.,-1.));
#120916=DIRECTION('ref_axis',(0.,1.,0.));
#120917=DIRECTION('center_axis',(0.,0.,1.));
#120918=DIRECTION('ref_axis',(0.,1.,0.));
#120919=DIRECTION('center_axis',(5.87084501074442E-17,1.,0.));
#120920=DIRECTION('ref_axis',(0.,0.,1.));
#120921=DIRECTION('center_axis',(0.,1.,0.));
#120922=DIRECTION('ref_axis',(0.,0.,1.));
#120923=DIRECTION('',(-5.87084501074442E-17,-1.,-1.23467863058847E-16));
#120924=DIRECTION('',(5.87084501074442E-17,1.,1.23467863058847E-16));
#120925=DIRECTION('center_axis',(0.,1.23467863058847E-16,-1.));
#120926=DIRECTION('ref_axis',(0.,1.,1.25697703075927E-16));
#120927=DIRECTION('center_axis',(0.999858703750256,0.0168098939573669,0.));
#120928=DIRECTION('ref_axis',(-0.0168098939573669,0.999858703750256,0.));
#120929=DIRECTION('center_axis',(0.,1.22914743790472E-16,-1.));
#120930=DIRECTION('ref_axis',(0.,1.,1.22914743790472E-16));
#120931=DIRECTION('center_axis',(0.,-1.22833149346405E-16,1.));
#120932=DIRECTION('ref_axis',(0.,1.,1.22833149346405E-16));
#120933=DIRECTION('center_axis',(0.,1.23467863058847E-16,-1.));
#120934=DIRECTION('ref_axis',(-0.701138397908224,-0.713025207814344,0.));
#120935=DIRECTION('center_axis',(0.,0.,-1.));
#120936=DIRECTION('ref_axis',(0.,1.,0.));
#120937=DIRECTION('center_axis',(0.,0.,1.));
#120938=DIRECTION('ref_axis',(0.,1.,0.));
#120939=DIRECTION('center_axis',(0.,1.23467863058847E-16,-1.));
#120940=DIRECTION('ref_axis',(0.,1.,0.));
#120941=DIRECTION('center_axis',(-1.5419764230905E-14,-1.,0.));
#120942=DIRECTION('ref_axis',(1.,-1.5419764230905E-14,0.));
#120943=DIRECTION('center_axis',(0.,0.,-1.));
#120944=DIRECTION('ref_axis',(0.,1.,0.));
#120945=DIRECTION('center_axis',(-1.,0.,0.));
#120946=DIRECTION('ref_axis',(0.,0.,1.));
#120947=DIRECTION('center_axis',(0.,0.,1.));
#120948=DIRECTION('ref_axis',(0.,1.,0.));
#120949=DIRECTION('center_axis',(1.,0.,7.06547394595967E-32));
#120950=DIRECTION('ref_axis',(0.,1.,0.));
#120951=DIRECTION('center_axis',(-1.,0.,0.));
#120952=DIRECTION('ref_axis',(0.,0.,1.));
#120953=DIRECTION('',(1.,5.72252063890675E-16,7.06547394595967E-32));
#120954=DIRECTION('',(-1.,-5.72252063890675E-16,-7.06547394595967E-32));
#120955=DIRECTION('center_axis',(5.87084501074442E-17,1.,0.));
#120956=DIRECTION('ref_axis',(0.,0.,1.));
#120957=DIRECTION('center_axis',(0.,-1.,0.));
#120958=DIRECTION('ref_axis',(0.,0.,-1.));
#120959=DIRECTION('',(5.87084501074442E-17,1.,1.23467863058847E-16));
#120960=DIRECTION('',(-5.87084501074442E-17,-1.,-1.23467863058847E-16));
#120961=DIRECTION('center_axis',(0.,1.23467863058847E-16,-1.));
#120962=DIRECTION('ref_axis',(0.,1.,0.));
#120963=DIRECTION('center_axis',(0.,-1.,0.));
#120964=DIRECTION('ref_axis',(0.,0.,-1.));
#120965=DIRECTION('center_axis',(0.,0.,1.));
#120966=DIRECTION('ref_axis',(0.,1.,0.));
#120967=DIRECTION('center_axis',(0.,0.,-1.));
#120968=DIRECTION('ref_axis',(0.,1.,0.));
#120969=DIRECTION('center_axis',(0.,1.23467863058847E-16,-1.));
#120970=DIRECTION('ref_axis',(0.,1.,0.));
#120971=DIRECTION('center_axis',(-1.,0.,0.));
#120972=DIRECTION('ref_axis',(0.,0.,1.));
#120973=DIRECTION('center_axis',(0.,0.,-1.));
#120974=DIRECTION('ref_axis',(0.,1.,0.));
#120975=DIRECTION('center_axis',(0.,0.,1.));
#120976=DIRECTION('ref_axis',(0.,1.,0.));
#120977=DIRECTION('center_axis',(7.82779334765923E-17,-1.,0.));
#120978=DIRECTION('ref_axis',(0.,0.,-1.));
#120979=DIRECTION('center_axis',(1.5419764230905E-14,-1.,0.));
#120980=DIRECTION('ref_axis',(1.,1.5419764230905E-14,0.));
#120981=DIRECTION('',(-7.82779334765923E-17,1.,1.23467863058847E-16));
#120982=DIRECTION('',(7.82779334765923E-17,-1.,-1.23467863058847E-16));
#120983=DIRECTION('center_axis',(-1.,0.,4.07299888683445E-32));
#120984=DIRECTION('ref_axis',(0.,-1.,0.));
#120985=DIRECTION('center_axis',(-1.,0.,0.));
#120986=DIRECTION('ref_axis',(0.,0.,1.));
#120987=DIRECTION('',(1.,-3.29883322342202E-16,-4.07299888683446E-32));
#120988=DIRECTION('',(-1.,3.29883322342202E-16,4.07299888683446E-32));
#120989=DIRECTION('center_axis',(0.,1.23467863058847E-16,-1.));
#120990=DIRECTION('ref_axis',(0.,1.,0.));
#120991=DIRECTION('center_axis',(0.,0.,-1.));
#120992=DIRECTION('ref_axis',(0.,1.,0.));
#120993=DIRECTION('center_axis',(0.,0.,1.));
#120994=DIRECTION('ref_axis',(0.,1.,0.));
#120995=DIRECTION('center_axis',(0.,1.23467863058847E-16,-1.));
#120996=DIRECTION('ref_axis',(0.,1.,0.));
#120997=DIRECTION('center_axis',(0.,1.,0.));
#120998=DIRECTION('ref_axis',(0.,0.,1.));
#120999=DIRECTION('center_axis',(0.,0.,-1.));
#121000=DIRECTION('ref_axis',(0.,1.,0.));
#121001=DIRECTION('center_axis',(1.,0.,0.));
#121002=DIRECTION('ref_axis',(0.,0.,-1.));
#121003=DIRECTION('center_axis',(0.,0.,1.));
#121004=DIRECTION('ref_axis',(0.,1.,0.));
#121005=DIRECTION('center_axis',(-1.,0.,-2.35515798198655E-32));
#121006=DIRECTION('ref_axis',(0.,-1.,0.));
#121007=DIRECTION('center_axis',(1.,4.81867632215781E-16,0.));
#121008=DIRECTION('ref_axis',(-4.81867632215781E-16,1.,0.));
#121009=DIRECTION('',(-1.,-1.90750687963558E-16,-2.35515798198656E-32));
#121010=DIRECTION('',(1.,1.90750687963558E-16,2.35515798198656E-32));
#121011=DIRECTION('center_axis',(0.,-1.,-1.23467863058847E-16));
#121012=DIRECTION('ref_axis',(1.,0.,0.));
#121013=DIRECTION('center_axis',(0.,1.,0.));
#121014=DIRECTION('ref_axis',(0.,0.,1.));
#121015=DIRECTION('',(-3.13111733906369E-16,-1.,-1.23467863058847E-16));
#121016=DIRECTION('',(3.13111733906369E-16,1.,1.23467863058847E-16));
#121017=DIRECTION('center_axis',(0.,1.23467863058847E-16,-1.));
#121018=DIRECTION('ref_axis',(0.,1.,0.));
#121019=DIRECTION('center_axis',(0.,1.,0.));
#121020=DIRECTION('ref_axis',(0.,0.,1.));
#121021=DIRECTION('center_axis',(0.,0.,1.));
#121022=DIRECTION('ref_axis',(0.,1.,0.));
#121023=DIRECTION('center_axis',(0.,0.,-1.));
#121024=DIRECTION('ref_axis',(0.,1.,0.));
#121025=DIRECTION('center_axis',(0.,1.23467863058847E-16,-1.));
#121026=DIRECTION('ref_axis',(0.,1.,0.));
#121027=DIRECTION('center_axis',(0.999913989288144,0.0131154117689341,0.));
#121028=DIRECTION('ref_axis',(-0.0131154117689341,0.999913989288144,0.));
#121029=DIRECTION('center_axis',(0.,0.,-1.));
#121030=DIRECTION('ref_axis',(0.,1.,0.));
#121031=DIRECTION('center_axis',(0.,0.,1.));
#121032=DIRECTION('ref_axis',(0.,1.,0.));
#121033=DIRECTION('center_axis',(6.11546355285877E-17,1.,0.));
#121034=DIRECTION('ref_axis',(0.,0.,1.));
#121035=DIRECTION('center_axis',(0.,1.,0.));
#121036=DIRECTION('ref_axis',(0.,0.,1.));
#121037=DIRECTION('',(-6.11546355285877E-17,-1.,-1.23467863058847E-16));
#121038=DIRECTION('',(6.11546355285877E-17,1.,1.23467863058847E-16));
#121039=DIRECTION('center_axis',(0.,1.23467863058847E-16,-1.));
#121040=DIRECTION('ref_axis',(0.,1.,1.25697703075927E-16));
#121041=DIRECTION('center_axis',(0.999998293848715,0.00184724109421639,
0.));
#121042=DIRECTION('ref_axis',(-0.00184724109421639,0.999998293848714,0.));
#121043=DIRECTION('center_axis',(0.,1.22914743790472E-16,-1.));
#121044=DIRECTION('ref_axis',(0.,1.,1.22914743790472E-16));
#121045=DIRECTION('center_axis',(0.,-1.22833149346405E-16,1.));
#121046=DIRECTION('ref_axis',(0.,1.,1.22833149346405E-16));
#121047=DIRECTION('center_axis',(0.,1.23467863058847E-16,-1.));
#121048=DIRECTION('ref_axis',(-0.706453380948024,-0.707759578209371,0.));
#121049=DIRECTION('center_axis',(0.,0.,-1.));
#121050=DIRECTION('ref_axis',(0.,1.,0.));
#121051=DIRECTION('center_axis',(0.,0.,1.));
#121052=DIRECTION('ref_axis',(0.,1.,0.));
#121053=DIRECTION('center_axis',(0.,1.23467863058847E-16,-1.));
#121054=DIRECTION('ref_axis',(0.,1.,0.));
#121055=DIRECTION('center_axis',(0.,-1.,0.));
#121056=DIRECTION('ref_axis',(0.,0.,-1.));
#121057=DIRECTION('center_axis',(0.,0.,-1.));
#121058=DIRECTION('ref_axis',(0.,1.,0.));
#121059=DIRECTION('center_axis',(-1.,-4.81867632215781E-16,7.43028527927166E-30));
#121060=DIRECTION('ref_axis',(4.81867632215781E-16,-1.,-1.36218908067985E-60));
#121061=DIRECTION('center_axis',(0.,0.,1.));
#121062=DIRECTION('ref_axis',(0.,1.,0.));
#121063=DIRECTION('center_axis',(1.,0.,7.06547394595967E-32));
#121064=DIRECTION('ref_axis',(0.,1.,0.));
#121065=DIRECTION('center_axis',(-1.,0.,0.));
#121066=DIRECTION('ref_axis',(0.,0.,1.));
#121067=DIRECTION('',(1.,5.72252063890675E-16,7.06547394595967E-32));
#121068=DIRECTION('',(-1.,-5.72252063890675E-16,-7.06547394595967E-32));
#121069=DIRECTION('center_axis',(6.11546355285877E-17,1.,0.));
#121070=DIRECTION('ref_axis',(0.,0.,1.));
#121071=DIRECTION('center_axis',(0.,-1.,0.));
#121072=DIRECTION('ref_axis',(0.,0.,-1.));
#121073=DIRECTION('',(6.11546355285877E-17,1.,1.23467863058847E-16));
#121074=DIRECTION('',(-6.11546355285877E-17,-1.,-1.23467863058847E-16));
#121075=DIRECTION('center_axis',(0.,1.23467863058847E-16,-1.));
#121076=DIRECTION('ref_axis',(0.,1.,0.));
#121077=DIRECTION('center_axis',(0.,-1.,0.));
#121078=DIRECTION('ref_axis',(0.,0.,-1.));
#121079=DIRECTION('center_axis',(1.78485500480727E-31,-2.58019156504489E-46,
1.));
#121080=DIRECTION('ref_axis',(1.44560289664734E-15,1.,-3.88938454866321E-62));
#121081=DIRECTION('center_axis',(0.,0.,-1.));
#121082=DIRECTION('ref_axis',(0.,1.,0.));
#121083=DIRECTION('center_axis',(0.,1.23467863058847E-16,-1.));
#121084=DIRECTION('ref_axis',(0.,1.,0.));
#121085=DIRECTION('center_axis',(-1.,4.81867632215781E-16,0.));
#121086=DIRECTION('ref_axis',(-4.81867632215781E-16,-1.,0.));
#121087=DIRECTION('center_axis',(0.,0.,-1.));
#121088=DIRECTION('ref_axis',(0.,1.,0.));
#121089=DIRECTION('center_axis',(0.,0.,1.));
#121090=DIRECTION('ref_axis',(0.,1.,0.));
#121091=DIRECTION('center_axis',(0.,-1.,-1.23467863058847E-16));
#121092=DIRECTION('ref_axis',(1.,0.,0.));
#121093=DIRECTION('center_axis',(0.,-1.,0.));
#121094=DIRECTION('ref_axis',(0.,0.,-1.));
#121095=DIRECTION('',(3.13111733906369E-16,1.,1.23467863058847E-16));
#121096=DIRECTION('',(-3.13111733906369E-16,-1.,-1.23467863058847E-16));
#121097=DIRECTION('center_axis',(-1.,0.,4.07299888683445E-32));
#121098=DIRECTION('ref_axis',(0.,-1.,0.));
#121099=DIRECTION('center_axis',(-1.,0.,0.));
#121100=DIRECTION('ref_axis',(0.,0.,1.));
#121101=DIRECTION('',(1.,-3.29883322342202E-16,-4.07299888683446E-32));
#121102=DIRECTION('',(-1.,3.29883322342202E-16,4.07299888683446E-32));
#121103=DIRECTION('center_axis',(0.,1.23467863058847E-16,-1.));
#121104=DIRECTION('ref_axis',(0.,1.,0.));
#121105=DIRECTION('center_axis',(0.,0.,-1.));
#121106=DIRECTION('ref_axis',(0.,1.,0.));
#121107=DIRECTION('center_axis',(0.,0.,1.));
#121108=DIRECTION('ref_axis',(0.,1.,0.));
#121109=DIRECTION('center_axis',(0.,1.23467863058847E-16,-1.));
#121110=DIRECTION('ref_axis',(0.,1.,0.));
#121111=DIRECTION('center_axis',(0.699822617100543,0.714316669688274,0.));
#121112=DIRECTION('ref_axis',(-0.714316669688274,0.699822617100543,0.));
#121113=DIRECTION('center_axis',(0.,0.,-1.));
#121114=DIRECTION('ref_axis',(0.,1.,0.));
#121115=DIRECTION('center_axis',(1.,0.,0.));
#121116=DIRECTION('ref_axis',(0.,0.,-1.));
#121117=DIRECTION('center_axis',(0.,0.,1.));
#121118=DIRECTION('ref_axis',(0.,1.,0.));
#121119=DIRECTION('center_axis',(-1.,0.,-2.35515798198655E-32));
#121120=DIRECTION('ref_axis',(0.,-1.,0.));
#121121=DIRECTION('center_axis',(1.,0.,0.));
#121122=DIRECTION('ref_axis',(0.,0.,-1.));
#121123=DIRECTION('',(-1.,-1.90750687963558E-16,-2.35515798198656E-32));
#121124=DIRECTION('',(1.,1.90750687963558E-16,2.35515798198656E-32));
#121125=DIRECTION('center_axis',(0.,1.23467863058847E-16,-1.));
#121126=DIRECTION('ref_axis',(0.,1.,0.));
#121127=DIRECTION('center_axis',(0.74298130529014,0.669312169312168,0.));
#121128=DIRECTION('ref_axis',(-0.669312169312168,0.742981305290139,0.));
#121129=DIRECTION('center_axis',(0.,0.,-1.));
#121130=DIRECTION('ref_axis',(0.,1.,0.));
#121131=DIRECTION('center_axis',(0.,0.,1.));
#121132=DIRECTION('ref_axis',(0.,1.,0.));
#121133=DIRECTION('center_axis',(0.,1.23467863058847E-16,-1.));
#121134=DIRECTION('ref_axis',(0.,1.,0.));
#121135=DIRECTION('center_axis',(0.,1.,0.));
#121136=DIRECTION('ref_axis',(0.,0.,1.));
#121137=DIRECTION('center_axis',(0.,0.,1.));
#121138=DIRECTION('ref_axis',(0.,1.,0.));
#121139=DIRECTION('center_axis',(0.,0.,-1.));
#121140=DIRECTION('ref_axis',(0.,1.,0.));
#121141=DIRECTION('center_axis',(0.,1.23467863058847E-16,-1.));
#121142=DIRECTION('ref_axis',(-0.406625030395211,-0.913595142640379,0.));
#121143=DIRECTION('center_axis',(0.,-1.,0.));
#121144=DIRECTION('ref_axis',(0.,0.,-1.));
#121145=DIRECTION('center_axis',(0.,0.,-1.));
#121146=DIRECTION('ref_axis',(0.,1.,0.));
#121147=DIRECTION('center_axis',(0.,0.,1.));
#121148=DIRECTION('ref_axis',(0.,1.,0.));
#121149=DIRECTION('center_axis',(0.,1.,0.));
#121150=DIRECTION('ref_axis',(0.,0.,1.));
#121151=DIRECTION('',(0.,1.,1.23467863058847E-16));
#121152=DIRECTION('',(0.,-1.,-1.23467863058847E-16));
#121153=DIRECTION('center_axis',(0.,1.23467863058847E-16,-1.));
#121154=DIRECTION('ref_axis',(0.,1.,0.));
#121155=DIRECTION('center_axis',(7.13942001922908E-31,-4.12830650407183E-45,
1.));
#121156=DIRECTION('ref_axis',(5.78241158658936E-15,1.,0.));
#121157=DIRECTION('center_axis',(-0.742981305290128,0.669312169312181,0.));
#121158=DIRECTION('ref_axis',(-0.669312169312181,-0.742981305290128,0.));
#121159=DIRECTION('center_axis',(0.,0.,-1.));
#121160=DIRECTION('ref_axis',(0.,1.,0.));
#121161=DIRECTION('center_axis',(0.,1.,0.));
#121162=DIRECTION('ref_axis',(0.,0.,1.));
#121163=DIRECTION('center_axis',(0.,1.,0.));
#121164=DIRECTION('ref_axis',(0.,0.,1.));
#121165=DIRECTION('center_axis',(0.,1.,0.));
#121166=DIRECTION('ref_axis',(0.,0.,1.));
#121167=DIRECTION('',(0.,-1.,-1.23467863058847E-16));
#121168=DIRECTION('',(0.,1.,1.23467863058847E-16));
#121169=DIRECTION('center_axis',(0.,1.23467863058847E-16,-1.));
#121170=DIRECTION('ref_axis',(0.,1.,0.));
#121171=DIRECTION('center_axis',(-0.699822617100527,0.714316669688289,0.));
#121172=DIRECTION('ref_axis',(-0.714316669688289,-0.699822617100527,0.));
#121173=DIRECTION('center_axis',(0.,0.,-1.));
#121174=DIRECTION('ref_axis',(0.,1.,0.));
#121175=DIRECTION('center_axis',(-1.20627640644894E-30,-1.17852753964151E-44,
1.));
#121176=DIRECTION('ref_axis',(-9.76996261670138E-15,1.,-4.97841222228891E-60));
#121177=DIRECTION('center_axis',(0.,1.23467863058847E-16,-1.));
#121178=DIRECTION('ref_axis',(0.,1.,0.));
#121179=DIRECTION('center_axis',(-1.,0.,0.));
#121180=DIRECTION('ref_axis',(0.,0.,1.));
#121181=DIRECTION('center_axis',(0.,0.,1.));
#121182=DIRECTION('ref_axis',(0.,1.,0.));
#121183=DIRECTION('center_axis',(0.,0.,-1.));
#121184=DIRECTION('ref_axis',(0.,1.,0.));
#121185=DIRECTION('center_axis',(0.,1.23467863058847E-16,-1.));
#121186=DIRECTION('ref_axis',(0.,1.,0.));
#121187=DIRECTION('center_axis',(1.,0.,0.));
#121188=DIRECTION('ref_axis',(0.,0.,-1.));
#121189=DIRECTION('center_axis',(0.,0.,-1.));
#121190=DIRECTION('ref_axis',(0.,1.,0.));
#121191=DIRECTION('center_axis',(0.,0.,1.));
#121192=DIRECTION('ref_axis',(0.,1.,0.));
#121193=DIRECTION('center_axis',(1.,0.,-1.17757899099328E-32));
#121194=DIRECTION('ref_axis',(0.,1.,0.));
#121195=DIRECTION('',(-1.,9.53753439817791E-17,1.17757899099328E-32));
#121196=DIRECTION('',(1.,-9.53753439817791E-17,-1.17757899099328E-32));
#121197=DIRECTION('center_axis',(0.,1.23467863058847E-16,-1.));
#121198=DIRECTION('ref_axis',(0.,1.,0.));
#121199=DIRECTION('center_axis',(0.,0.,-1.));
#121200=DIRECTION('ref_axis',(0.,1.,0.));
#121201=DIRECTION('center_axis',(-1.,1.22464679914735E-16,1.51204523292581E-32));
#121202=DIRECTION('ref_axis',(-1.22464679914735E-16,-1.,0.));
#121203=DIRECTION('center_axis',(0.,0.,1.));
#121204=DIRECTION('ref_axis',(0.,1.,0.));
#121205=DIRECTION('center_axis',(0.,1.23467863058847E-16,-1.));
#121206=DIRECTION('ref_axis',(0.,1.,0.));
#121207=DIRECTION('center_axis',(0.,0.,-1.));
#121208=DIRECTION('ref_axis',(0.,1.,0.));
#121209=DIRECTION('center_axis',(-1.,1.22464679914735E-16,1.51204523292581E-32));
#121210=DIRECTION('ref_axis',(-1.22464679914735E-16,-1.,0.));
#121211=DIRECTION('center_axis',(0.,0.,1.));
#121212=DIRECTION('ref_axis',(0.,1.,0.));
#121213=DIRECTION('center_axis',(0.,1.23467863058847E-16,-1.));
#121214=DIRECTION('ref_axis',(1.22464679914735E-16,-1.,-1.24777965780772E-16));
#121215=DIRECTION('center_axis',(-0.999425898115847,-0.0338802918424838,
7.7054558576033E-15));
#121216=DIRECTION('ref_axis',(0.0338802918424838,-0.999425898115847,2.67737997453887E-33));
#121217=DIRECTION('center_axis',(3.13384100142148E-32,-1.21933779888604E-16,
1.));
#121218=DIRECTION('ref_axis',(2.04281036531029E-14,1.,1.21933779888604E-16));
#121219=DIRECTION('center_axis',(0.,1.22014183466588E-16,-1.));
#121220=DIRECTION('ref_axis',(0.,1.,1.22014183466588E-16));
#121221=DIRECTION('center_axis',(0.,1.23467863058847E-16,-1.));
#121222=DIRECTION('ref_axis',(0.,1.,0.));
#121223=DIRECTION('center_axis',(-0.87305990868679,-0.487612957009772,0.));
#121224=DIRECTION('ref_axis',(0.487612957009772,-0.87305990868679,0.));
#121225=DIRECTION('center_axis',(0.,0.,1.));
#121226=DIRECTION('ref_axis',(0.,1.,0.));
#121227=DIRECTION('center_axis',(0.,0.,-1.));
#121228=DIRECTION('ref_axis',(0.,1.,0.));
#121229=DIRECTION('center_axis',(0.,1.23467863058847E-16,-1.));
#121230=DIRECTION('ref_axis',(0.,1.,0.));
#121231=DIRECTION('center_axis',(-0.55837318130784,-0.829589892896582,0.));
#121232=DIRECTION('ref_axis',(0.829589892896582,-0.55837318130784,0.));
#121233=DIRECTION('center_axis',(4.38645965981435E-31,-1.5583835234929E-45,
1.));
#121234=DIRECTION('ref_axis',(3.5527136788005E-15,1.,-1.24460305557223E-60));
#121235=DIRECTION('center_axis',(0.,0.,-1.));
#121236=DIRECTION('ref_axis',(0.,1.,0.));
#121237=DIRECTION('center_axis',(0.,1.23467863058847E-16,-1.));
#121238=DIRECTION('ref_axis',(0.,1.,0.));
#121239=DIRECTION('center_axis',(-0.03879684915621,-0.999247118832749,-5.83634271056011E-15));
#121240=DIRECTION('ref_axis',(0.999247118832749,-0.03879684915621,-4.4574149748685E-34));
#121241=DIRECTION('center_axis',(6.64132094812011E-31,-3.57235825122499E-45,
1.));
#121242=DIRECTION('ref_axis',(5.37898752240871E-15,1.,2.61366641670168E-59));
#121243=DIRECTION('center_axis',(0.,0.,-1.));
#121244=DIRECTION('ref_axis',(0.,1.,0.));
#121245=DIRECTION('center_axis',(0.,1.23467863058847E-16,-1.));
#121246=DIRECTION('ref_axis',(0.,1.,1.24777965780772E-16));
#121247=DIRECTION('center_axis',(0.0387968491562139,-0.999247118832749,
0.));
#121248=DIRECTION('ref_axis',(0.999247118832749,0.0387968491562139,0.));
#121249=DIRECTION('center_axis',(4.09030343683335E-32,-1.21933779888604E-16,
1.));
#121250=DIRECTION('ref_axis',(2.66628532023081E-14,1.,1.21933779888604E-16));
#121251=DIRECTION('center_axis',(0.,1.22014183466588E-16,-1.));
#121252=DIRECTION('ref_axis',(0.,1.,1.22014183466588E-16));
#121253=DIRECTION('center_axis',(0.,1.23467863058847E-16,-1.));
#121254=DIRECTION('ref_axis',(0.,1.,0.));
#121255=DIRECTION('center_axis',(0.55837318130784,-0.829589892896582,0.));
#121256=DIRECTION('ref_axis',(0.829589892896582,0.55837318130784,0.));
#121257=DIRECTION('center_axis',(-1.32826418962402E-31,-1.42894330048999E-46,
1.));
#121258=DIRECTION('ref_axis',(-1.07579750448174E-15,1.,9.14005368935855E-61));
#121259=DIRECTION('center_axis',(0.,0.,-1.));
#121260=DIRECTION('ref_axis',(0.,1.,0.));
#121261=DIRECTION('center_axis',(0.,1.23467863058847E-16,-1.));
#121262=DIRECTION('ref_axis',(0.,1.,0.));
#121263=DIRECTION('center_axis',(0.848949186868297,-0.528474481991002,-8.14895191435076E-15));
#121264=DIRECTION('ref_axis',(0.528474481991002,0.848949186868297,-1.25969070483717E-30));
#121265=DIRECTION('center_axis',(-1.53526088093502E-30,-1.90901981627881E-44,
1.));
#121266=DIRECTION('ref_axis',(-1.24344978758017E-14,1.,2.98704733337335E-59));
#121267=DIRECTION('center_axis',(0.,0.,-1.));
#121268=DIRECTION('ref_axis',(0.,1.,0.));
#121269=DIRECTION('center_axis',(0.,1.23467863058847E-16,-1.));
#121270=DIRECTION('ref_axis',(0.,1.,0.));
#121271=DIRECTION('center_axis',(0.992522955047552,-0.122058116090968,0.));
#121272=DIRECTION('ref_axis',(0.122058116090968,0.992522955047552,0.));
#121273=DIRECTION('center_axis',(-1.32826418962402E-31,-1.42894330048999E-46,
1.));
#121274=DIRECTION('ref_axis',(-1.07579750448174E-15,1.,5.05619991326218E-61));
#121275=DIRECTION('center_axis',(0.,0.,-1.));
#121276=DIRECTION('ref_axis',(0.,1.,0.));
#121277=DIRECTION('center_axis',(0.,1.23467863058847E-16,-1.));
#121278=DIRECTION('ref_axis',(0.,1.,1.35086937000622E-16));
#121279=DIRECTION('center_axis',(1.70695598787294E-31,-1.32203597548532E-16,
1.));
#121280=DIRECTION('ref_axis',(-1.95399252334027E-14,1.,1.32203597548532E-16));
#121281=DIRECTION('center_axis',(0.,1.32487572930867E-16,-1.));
#121282=DIRECTION('ref_axis',(0.,1.,1.32487572930867E-16));
#121283=DIRECTION('center_axis',(0.,1.23467863058847E-16,-1.));
#121284=DIRECTION('ref_axis',(1.22464679914735E-16,-1.,-1.25162611019057E-16));
#121285=DIRECTION('center_axis',(-0.999425898115848,-0.0338802918424761,
0.));
#121286=DIRECTION('ref_axis',(0.0338802918424761,-0.999425898115848,0.));
#121287=DIRECTION('center_axis',(2.53053284261581E-32,-1.22229112323298E-16,
1.));
#121288=DIRECTION('ref_axis',(2.04281036531029E-14,1.,1.22229112323298E-16));
#121289=DIRECTION('center_axis',(0.,1.22309905988566E-16,-1.));
#121290=DIRECTION('ref_axis',(0.,1.,1.22309905988566E-16));
#121291=DIRECTION('center_axis',(0.,1.23467863058847E-16,-1.));
#121292=DIRECTION('ref_axis',(0.,1.,0.));
#121293=DIRECTION('center_axis',(-0.87305990868679,-0.487612957009772,0.));
#121294=DIRECTION('ref_axis',(0.487612957009772,-0.87305990868679,0.));
#121295=DIRECTION('center_axis',(-4.46213751201822E-31,-1.61261972815309E-45,
1.));
#121296=DIRECTION('ref_axis',(-3.61400724161835E-15,1.,1.6490990486332E-59));
#121297=DIRECTION('center_axis',(0.,0.,-1.));
#121298=DIRECTION('ref_axis',(0.,1.,0.));
#121299=DIRECTION('center_axis',(0.,1.23467863058847E-16,-1.));
#121300=DIRECTION('ref_axis',(0.,1.,0.));
#121301=DIRECTION('center_axis',(-0.55837318130784,-0.829589892896582,0.));
#121302=DIRECTION('ref_axis',(0.829589892896582,-0.55837318130784,0.));
#121303=DIRECTION('center_axis',(4.38645965981435E-31,-1.5583835234929E-45,
1.));
#121304=DIRECTION('ref_axis',(3.5527136788005E-15,1.,-1.24460305557223E-60));
#121305=DIRECTION('center_axis',(0.,0.,-1.));
#121306=DIRECTION('ref_axis',(0.,1.,0.));
#121307=DIRECTION('center_axis',(0.,1.23467863058847E-16,-1.));
#121308=DIRECTION('ref_axis',(0.,1.,0.));
#121309=DIRECTION('center_axis',(-0.0387968491561946,-0.99924711883275,
0.));
#121310=DIRECTION('ref_axis',(0.99924711883275,-0.0387968491561946,0.));
#121311=DIRECTION('center_axis',(-8.92427502403635E-31,-6.45047891261223E-45,
1.));
#121312=DIRECTION('ref_axis',(-7.2280144832367E-15,1.,3.73380916671669E-60));
#121313=DIRECTION('center_axis',(0.,0.,-1.));
#121314=DIRECTION('ref_axis',(0.,1.,0.));
#121315=DIRECTION('center_axis',(0.,1.23467863058847E-16,-1.));
#121316=DIRECTION('ref_axis',(0.,1.,1.25162611019057E-16));
#121317=DIRECTION('center_axis',(0.0387968491562177,-0.999247118832749,
0.));
#121318=DIRECTION('ref_axis',(0.999247118832749,0.0387968491562177,0.));
#121319=DIRECTION('center_axis',(3.29067448743359E-32,-1.22229112323298E-16,
1.));
#121320=DIRECTION('ref_axis',(2.65644604115968E-14,1.,1.22229112323298E-16));
#121321=DIRECTION('center_axis',(0.,1.22309905988566E-16,-1.));
#121322=DIRECTION('ref_axis',(0.,1.,1.22309905988566E-16));
#121323=DIRECTION('center_axis',(0.,1.23467863058847E-16,-1.));
#121324=DIRECTION('ref_axis',(0.,1.,0.));
#121325=DIRECTION('center_axis',(0.55837318130784,-0.829589892896582,0.));
#121326=DIRECTION('ref_axis',(0.829589892896582,0.55837318130784,0.));
#121327=DIRECTION('center_axis',(0.,0.,1.));
#121328=DIRECTION('ref_axis',(0.,1.,0.));
#121329=DIRECTION('center_axis',(0.,0.,-1.));
#121330=DIRECTION('ref_axis',(0.,1.,0.));
#121331=DIRECTION('center_axis',(0.,1.23467863058847E-16,-1.));
#121332=DIRECTION('ref_axis',(0.,1.,0.));
#121333=DIRECTION('center_axis',(0.848949186868305,-0.528474481990989,0.));
#121334=DIRECTION('ref_axis',(0.528474481990989,0.848949186868305,0.));
#121335=DIRECTION('center_axis',(-1.53526088093502E-30,-1.90901981627881E-44,
1.));
#121336=DIRECTION('ref_axis',(-1.24344978758017E-14,1.,3.23596794448779E-59));
#121337=DIRECTION('center_axis',(0.,0.,-1.));
#121338=DIRECTION('ref_axis',(0.,1.,0.));
#121339=DIRECTION('center_axis',(0.,1.23467863058847E-16,-1.));
#121340=DIRECTION('ref_axis',(0.,1.,0.));
#121341=DIRECTION('center_axis',(0.992522955047553,-0.12205811609096,0.));
#121342=DIRECTION('ref_axis',(0.12205811609096,0.992522955047552,0.));
#121343=DIRECTION('center_axis',(1.42788400384582E-30,-1.65132260162873E-44,
1.));
#121344=DIRECTION('ref_axis',(1.15648231731787E-14,1.,-2.48920611114446E-60));
#121345=DIRECTION('center_axis',(0.,0.,-1.));
#121346=DIRECTION('ref_axis',(0.,1.,0.));
#121347=DIRECTION('center_axis',(0.,1.23467863058847E-16,-1.));
#121348=DIRECTION('ref_axis',(0.,1.,1.36448859403292E-16));
#121349=DIRECTION('center_axis',(-1.91158623550752E-31,-1.33250839261027E-16,
1.));
#121350=DIRECTION('ref_axis',(1.95399252334028E-14,1.,1.33250839261027E-16));
#121351=DIRECTION('center_axis',(0.,1.33539336354386E-16,-1.));
#121352=DIRECTION('ref_axis',(0.,1.,1.33539336354386E-16));
#121353=DIRECTION('center_axis',(0.,1.23467863058847E-16,-1.));
#121354=DIRECTION('ref_axis',(0.,1.,0.));
#121355=DIRECTION('center_axis',(-0.689680595319751,-0.724113717892013,
0.));
#121356=DIRECTION('ref_axis',(0.724113717892013,-0.689680595319751,0.));
#121357=DIRECTION('center_axis',(0.,0.,-1.));
#121358=DIRECTION('ref_axis',(0.,1.,0.));
#121359=DIRECTION('center_axis',(0.,0.,1.));
#121360=DIRECTION('ref_axis',(0.,1.,0.));
#121361=DIRECTION('center_axis',(-0.68968059531976,-0.724113717892004,-8.94047733597239E-17));
#121362=DIRECTION('ref_axis',(0.724113717892004,-0.68968059531976,2.34589631629098E-32));
#121363=DIRECTION('center_axis',(-0.689680595319751,-0.724113717892013,
0.));
#121364=DIRECTION('ref_axis',(0.724113717892013,-0.689680595319751,0.));
#121365=DIRECTION('',(0.689680595319752,0.724113717892012,8.94047733597238E-17));
#121366=DIRECTION('',(-0.689680595319752,-0.724113717892012,-8.94047733597238E-17));
#121367=DIRECTION('center_axis',(0.,1.23467863058847E-16,-1.));
#121368=DIRECTION('ref_axis',(0.,1.,0.));
#121369=DIRECTION('center_axis',(1.78485500480727E-31,-2.58019156504489E-46,
1.));
#121370=DIRECTION('ref_axis',(1.44560289664734E-15,1.,-3.88938454866321E-62));
#121371=DIRECTION('center_axis',(-0.635568809204586,0.772044227208691,0.));
#121372=DIRECTION('ref_axis',(-0.772044227208691,-0.635568809204586,0.));
#121373=DIRECTION('center_axis',(0.,0.,-1.));
#121374=DIRECTION('ref_axis',(0.,1.,0.));
#121375=DIRECTION('center_axis',(0.,1.23467863058847E-16,-1.));
#121376=DIRECTION('ref_axis',(0.,1.,0.));
#121377=DIRECTION('center_axis',(-0.120708341042265,0.992688015643799,0.));
#121378=DIRECTION('ref_axis',(-0.992688015643799,-0.120708341042265,0.));
#121379=DIRECTION('center_axis',(0.,0.,-1.));
#121380=DIRECTION('ref_axis',(0.,1.,0.));
#121381=DIRECTION('center_axis',(-2.19322982990717E-31,-3.89595880873225E-46,
1.));
#121382=DIRECTION('ref_axis',(-1.77635683940025E-15,1.,7.77876909732643E-62));
#121383=DIRECTION('center_axis',(0.,1.23467863058847E-16,-1.));
#121384=DIRECTION('ref_axis',(0.,1.,0.));
#121385=DIRECTION('center_axis',(1.,0.,0.));
#121386=DIRECTION('ref_axis',(0.,0.,-1.));
#121387=DIRECTION('center_axis',(0.,0.,-1.));
#121388=DIRECTION('ref_axis',(0.,1.,0.));
#121389=DIRECTION('center_axis',(0.,0.,1.));
#121390=DIRECTION('ref_axis',(0.,1.,0.));
#121391=DIRECTION('center_axis',(1.,0.,4.58212374768871E-32));
#121392=DIRECTION('ref_axis',(0.,1.,0.));
#121393=DIRECTION('center_axis',(1.,0.,0.));
#121394=DIRECTION('ref_axis',(0.,0.,-1.));
#121395=DIRECTION('',(-1.,-3.71118737634973E-16,-4.58212374768871E-32));
#121396=DIRECTION('',(1.,3.71118737634973E-16,4.58212374768871E-32));
#121397=DIRECTION('center_axis',(0.,1.23467863058847E-16,-1.));
#121398=DIRECTION('ref_axis',(0.,1.,0.));
#121399=DIRECTION('center_axis',(0.,0.,-1.));
#121400=DIRECTION('ref_axis',(0.,1.,0.));
#121401=DIRECTION('center_axis',(0.,0.,1.));
#121402=DIRECTION('ref_axis',(0.,1.,0.));
#121403=DIRECTION('center_axis',(0.,1.23467863058847E-16,-1.));
#121404=DIRECTION('ref_axis',(0.,1.,0.));
#121405=DIRECTION('center_axis',(-1.,0.,0.));
#121406=DIRECTION('ref_axis',(0.,0.,1.));
#121407=DIRECTION('center_axis',(0.,0.,-1.));
#121408=DIRECTION('ref_axis',(0.,1.,0.));
#121409=DIRECTION('center_axis',(0.,0.,1.));
#121410=DIRECTION('ref_axis',(0.,1.,0.));
#121411=DIRECTION('center_axis',(-1.,0.,4.58212374768871E-32));
#121412=DIRECTION('ref_axis',(0.,-1.,0.));
#121413=DIRECTION('center_axis',(-1.,0.,0.));
#121414=DIRECTION('ref_axis',(0.,0.,1.));
#121415=DIRECTION('',(1.,-3.71118737634973E-16,-4.58212374768871E-32));
#121416=DIRECTION('',(-1.,3.71118737634973E-16,4.58212374768871E-32));
#121417=DIRECTION('center_axis',(0.,1.23467863058847E-16,-1.));
#121418=DIRECTION('ref_axis',(0.,1.,0.));
#121419=DIRECTION('center_axis',(0.120708341042269,0.992688015643799,0.));
#121420=DIRECTION('ref_axis',(-0.992688015643799,0.120708341042269,0.));
#121421=DIRECTION('center_axis',(0.,0.,-1.));
#121422=DIRECTION('ref_axis',(0.,1.,0.));
#121423=DIRECTION('center_axis',(1.78485500480727E-31,-2.58019156504489E-46,
1.));
#121424=DIRECTION('ref_axis',(1.44560289664734E-15,1.,-3.88938454866321E-62));
#121425=DIRECTION('center_axis',(0.,1.23467863058847E-16,-1.));
#121426=DIRECTION('ref_axis',(0.,1.,0.));
#121427=DIRECTION('center_axis',(0.635568809204587,0.77204422720869,0.));
#121428=DIRECTION('ref_axis',(-0.77204422720869,0.635568809204587,0.));
#121429=DIRECTION('center_axis',(0.,0.,-1.));
#121430=DIRECTION('ref_axis',(0.,1.,0.));
#121431=DIRECTION('center_axis',(6.57968948972152E-31,-3.50636292785902E-45,
1.));
#121432=DIRECTION('ref_axis',(5.32907051820075E-15,1.,-4.3561106945028E-60));
#121433=DIRECTION('center_axis',(0.,1.23467863058847E-16,-1.));
#121434=DIRECTION('ref_axis',(0.0361435302645206,-0.999346609150208,0.));
#121435=DIRECTION('center_axis',(0.689680595319753,-0.724113717892011,0.));
#121436=DIRECTION('ref_axis',(0.724113717892011,0.689680595319753,0.));
#121437=DIRECTION('center_axis',(0.,0.,-1.));
#121438=DIRECTION('ref_axis',(0.,1.,0.));
#121439=DIRECTION('center_axis',(1.78485500480727E-31,-2.58019156504489E-46,
1.));
#121440=DIRECTION('ref_axis',(1.44560289664734E-15,1.,-3.88938454866321E-62));
#121441=DIRECTION('center_axis',(0.689680595319751,-0.724113717892013,-8.9404773359724E-17));
#121442=DIRECTION('ref_axis',(0.724113717892013,0.689680595319751,4.19197973383322E-33));
#121443=DIRECTION('center_axis',(0.689680595319753,-0.724113717892011,0.));
#121444=DIRECTION('ref_axis',(0.724113717892011,0.689680595319753,0.));
#121445=DIRECTION('',(-0.689680595319751,0.724113717892013,8.9404773359724E-17));
#121446=DIRECTION('',(0.689680595319751,-0.724113717892013,-8.9404773359724E-17));
#121447=DIRECTION('center_axis',(0.,1.23467863058847E-16,-1.));
#121448=DIRECTION('ref_axis',(0.,1.,0.));
#121449=DIRECTION('center_axis',(0.,0.,-1.));
#121450=DIRECTION('ref_axis',(0.,1.,0.));
#121451=DIRECTION('center_axis',(-8.92427502403635E-32,-6.45047891261222E-47,
1.));
#121452=DIRECTION('ref_axis',(-7.2280144832367E-16,1.,-6.80642296016062E-62));
#121453=DIRECTION('center_axis',(0.,1.23467863058847E-16,-1.));
#121454=DIRECTION('ref_axis',(0.,1.,0.));
#121455=DIRECTION('center_axis',(1.92747052886312E-15,-1.,0.));
#121456=DIRECTION('ref_axis',(1.,1.92747052886312E-15,0.));
#121457=DIRECTION('center_axis',(0.,0.,-1.));
#121458=DIRECTION('ref_axis',(0.,1.,0.));
#121459=DIRECTION('center_axis',(0.,0.,1.));
#121460=DIRECTION('ref_axis',(0.,1.,0.));
#121461=DIRECTION('center_axis',(6.11546355285877E-17,1.,0.));
#121462=DIRECTION('ref_axis',(0.,0.,1.));
#121463=DIRECTION('center_axis',(0.,-1.,0.));
#121464=DIRECTION('ref_axis',(0.,0.,-1.));
#121465=DIRECTION('',(6.11546355285877E-17,1.,1.23467863058847E-16));
#121466=DIRECTION('',(-6.11546355285877E-17,-1.,-1.23467863058847E-16));
#121467=DIRECTION('center_axis',(0.,1.23467863058847E-16,-1.));
#121468=DIRECTION('ref_axis',(0.,1.,0.));
#121469=DIRECTION('center_axis',(-2.63266113209072E-30,-5.61352927370078E-44,
1.));
#121470=DIRECTION('ref_axis',(-2.13226427255483E-14,1.,-2.98704733337335E-59));
#121471=DIRECTION('center_axis',(-0.992688015643799,0.120708341042267,1.45413606216828E-17));
#121472=DIRECTION('ref_axis',(-0.120708341042267,-0.992688015643799,-1.06337197076866E-33));
#121473=DIRECTION('center_axis',(0.,0.,-1.));
#121474=DIRECTION('ref_axis',(0.,1.,0.));
#121475=DIRECTION('center_axis',(0.,1.23467863058847E-16,-1.));
#121476=DIRECTION('ref_axis',(0.,1.,0.));
#121477=DIRECTION('center_axis',(-0.802069210224766,0.597231095983306,0.));
#121478=DIRECTION('ref_axis',(-0.597231095983306,-0.802069210224766,0.));
#121479=DIRECTION('center_axis',(0.,0.,-1.));
#121480=DIRECTION('ref_axis',(0.,1.,0.));
#121481=DIRECTION('center_axis',(8.77291931962869E-31,-6.2335340939716E-45,
1.));
#121482=DIRECTION('ref_axis',(7.105427357601E-15,1.,-4.97841222228891E-60));
#121483=DIRECTION('center_axis',(0.,1.23467863058847E-16,-1.));
#121484=DIRECTION('ref_axis',(0.,1.,0.));
#121485=DIRECTION('center_axis',(0.689680595319753,0.724113717892012,0.));
#121486=DIRECTION('ref_axis',(-0.724113717892012,0.689680595319752,0.));
#121487=DIRECTION('center_axis',(0.,0.,-1.));
#121488=DIRECTION('ref_axis',(0.,1.,0.));
#121489=DIRECTION('center_axis',(0.,0.,1.));
#121490=DIRECTION('ref_axis',(0.,1.,0.));
#121491=DIRECTION('center_axis',(0.68968059531976,0.724113717892004,8.94047733597239E-17));
#121492=DIRECTION('ref_axis',(-0.724113717892004,0.68968059531976,-2.34589631629098E-32));
#121493=DIRECTION('center_axis',(0.689680595319752,0.724113717892012,0.));
#121494=DIRECTION('ref_axis',(-0.724113717892012,0.689680595319752,0.));
#121495=DIRECTION('',(-0.689680595319752,-0.724113717892012,-8.94047733597238E-17));
#121496=DIRECTION('',(0.689680595319752,0.724113717892012,8.94047733597238E-17));
#121497=DIRECTION('center_axis',(0.,1.23467863058847E-16,-1.));
#121498=DIRECTION('ref_axis',(0.0950205176920742,-0.995475314218052,0.));
#121499=DIRECTION('center_axis',(0.,0.,-1.));
#121500=DIRECTION('ref_axis',(0.,1.,0.));
#121501=DIRECTION('center_axis',(0.,0.,1.));
#121502=DIRECTION('ref_axis',(0.,1.,0.));
#121503=DIRECTION('center_axis',(0.,1.23467863058847E-16,-1.));
#121504=DIRECTION('ref_axis',(0.,1.,0.));
#121505=DIRECTION('center_axis',(-1.60636950432654E-30,-2.08995516768636E-44,
1.));
#121506=DIRECTION('ref_axis',(-1.30104260698261E-14,1.,2.24028550003001E-59));
#121507=DIRECTION('center_axis',(-0.689680595319753,0.724113717892011,0.));
#121508=DIRECTION('ref_axis',(-0.724113717892011,-0.689680595319753,0.));
#121509=DIRECTION('center_axis',(0.,0.,-1.));
#121510=DIRECTION('ref_axis',(0.,1.,0.));
#121511=DIRECTION('center_axis',(-0.689680595319751,0.724113717892013,8.9404773359724E-17));
#121512=DIRECTION('ref_axis',(-0.724113717892013,-0.689680595319751,-4.19197973383322E-33));
#121513=DIRECTION('center_axis',(-0.689680595319752,0.724113717892012,0.));
#121514=DIRECTION('ref_axis',(-0.724113717892012,-0.689680595319752,0.));
#121515=DIRECTION('',(0.689680595319751,-0.724113717892013,-8.9404773359724E-17));
#121516=DIRECTION('',(-0.689680595319751,0.724113717892013,8.9404773359724E-17));
#121517=DIRECTION('center_axis',(0.,1.23467863058847E-16,-1.));
#121518=DIRECTION('ref_axis',(0.,1.,0.));
#121519=DIRECTION('center_axis',(0.802069210224767,0.597231095983305,0.));
#121520=DIRECTION('ref_axis',(-0.597231095983305,0.802069210224766,0.));
#121521=DIRECTION('center_axis',(0.,0.,-1.));
#121522=DIRECTION('ref_axis',(0.,1.,0.));
#121523=DIRECTION('center_axis',(0.,0.,1.));
#121524=DIRECTION('ref_axis',(0.,1.,0.));
#121525=DIRECTION('center_axis',(0.,1.23467863058847E-16,-1.));
#121526=DIRECTION('ref_axis',(0.,1.,0.));
#121527=DIRECTION('center_axis',(0.992688015643799,0.120708341042267,0.));
#121528=DIRECTION('ref_axis',(-0.120708341042267,0.992688015643799,0.));
#121529=DIRECTION('center_axis',(0.,0.,-1.));
#121530=DIRECTION('ref_axis',(0.,1.,0.));
#121531=DIRECTION('center_axis',(0.,0.,1.));
#121532=DIRECTION('ref_axis',(0.,1.,0.));
#121533=DIRECTION('center_axis',(0.,1.23467863058847E-16,-1.));
#121534=DIRECTION('ref_axis',(-0.663057938251906,-0.748568080084325,0.));
#121535=DIRECTION('center_axis',(0.,-1.,0.));
#121536=DIRECTION('ref_axis',(0.,0.,-1.));
#121537=DIRECTION('center_axis',(0.,0.,-1.));
#121538=DIRECTION('ref_axis',(0.,1.,0.));
#121539=DIRECTION('center_axis',(0.,0.,1.));
#121540=DIRECTION('ref_axis',(0.,1.,0.));
#121541=DIRECTION('center_axis',(6.11546355285877E-17,1.,0.));
#121542=DIRECTION('ref_axis',(0.,0.,1.));
#121543=DIRECTION('center_axis',(0.,-1.,0.));
#121544=DIRECTION('ref_axis',(0.,0.,-1.));
#121545=DIRECTION('',(6.11546355285877E-17,1.,1.23467863058847E-16));
#121546=DIRECTION('',(-6.11546355285877E-17,-1.,-1.23467863058847E-16));
#121547=DIRECTION('center_axis',(0.,1.23467863058847E-16,-1.));
#121548=DIRECTION('ref_axis',(0.,1.,0.));
#121549=DIRECTION('center_axis',(0.,0.,-1.));
#121550=DIRECTION('ref_axis',(0.,1.,0.));
#121551=DIRECTION('center_axis',(-2.23106875600908E-31,-4.03154932038264E-46,
1.));
#121552=DIRECTION('ref_axis',(-1.80700362080917E-15,1.,2.33363072919793E-61));
#121553=DIRECTION('center_axis',(0.,-1.23467863058847E-16,1.));
#121554=DIRECTION('ref_axis',(1.22464679914735E-16,1.,1.21161349753609E-16));
#121555=DIRECTION('center_axis',(1.55777898081371E-32,1.19083105035399E-16,
-1.));
#121556=DIRECTION('ref_axis',(3.5527136788005E-15,-1.,-1.19083105035399E-16));
#121557=DIRECTION('center_axis',(0.,-1.18321745853506E-16,1.));
#121558=DIRECTION('ref_axis',(0.,1.,1.18321745853506E-16));
#121559=DIRECTION('center_axis',(-0.982297019165463,0.187330099393146,5.41061232187394E-15));
#121560=DIRECTION('ref_axis',(-0.187330099393146,-0.982297019165463,5.34128931770042E-31));
#121561=DIRECTION('center_axis',(0.,-1.23467863058847E-16,1.));
#121562=DIRECTION('ref_axis',(0.,-1.,0.));
#121563=DIRECTION('center_axis',(-0.777162624242383,0.6292998136665,1.36800580655942E-15));
#121564=DIRECTION('ref_axis',(-0.6292998136665,-0.777162624242383,-6.36525986617897E-32));
#121565=DIRECTION('center_axis',(0.,0.,-1.));
#121566=DIRECTION('ref_axis',(0.,-1.,0.));
#121567=DIRECTION('center_axis',(-7.93261518924905E-31,-5.09657996678154E-45,
1.));
#121568=DIRECTION('ref_axis',(-6.42484205421795E-15,1.,4.3561106945028E-60));
#121569=DIRECTION('center_axis',(0.,-1.23467863058847E-16,1.));
#121570=DIRECTION('ref_axis',(0.,-1.,0.));
#121571=DIRECTION('center_axis',(-0.6350303583426,0.772487180465326,0.));
#121572=DIRECTION('ref_axis',(-0.772487180465326,-0.6350303583426,0.));
#121573=DIRECTION('center_axis',(0.,0.,-1.));
#121574=DIRECTION('ref_axis',(0.,-1.,0.));
#121575=DIRECTION('center_axis',(-3.28984474486076E-31,-8.76590731964757E-46,
1.));
#121576=DIRECTION('ref_axis',(-2.66453525910037E-15,1.,-6.22301527786114E-61));
#121577=DIRECTION('center_axis',(0.,-1.23467863058847E-16,1.));
#121578=DIRECTION('ref_axis',(0.,-1.,0.));
#121579=DIRECTION('center_axis',(-0.0394959395290685,0.999219730970479,
-7.30821690739571E-16));
#121580=DIRECTION('ref_axis',(-0.999219730970479,-0.0394959395290685,1.49001220711228E-32));
#121581=DIRECTION('center_axis',(-4.09907119868247E-31,1.3608711024552E-45,
-1.));
#121582=DIRECTION('ref_axis',(-3.31994990204759E-15,-1.,-9.33452291679171E-61));
#121583=DIRECTION('center_axis',(-1.22040233680755E-31,-1.206291116398E-46,
1.));
#121584=DIRECTION('ref_axis',(-9.88437239110456E-16,1.,0.));
#121585=DIRECTION('center_axis',(0.,-1.23467863058847E-16,1.));
#121586=DIRECTION('ref_axis',(0.,-1.,-1.32864206562206E-16));
#121587=DIRECTION('center_axis',(0.0394959395290708,0.999219730970479,0.));
#121588=DIRECTION('ref_axis',(-0.999219730970479,0.0394959395290708,0.));
#121589=DIRECTION('center_axis',(0.,1.29932421951445E-16,-1.));
#121590=DIRECTION('ref_axis',(0.,-1.,-1.29932421951445E-16));
#121591=DIRECTION('center_axis',(2.45193654393607E-31,-1.29750229435012E-16,
1.));
#121592=DIRECTION('ref_axis',(-3.90288690140516E-14,1.,1.29750229435012E-16));
#121593=DIRECTION('center_axis',(0.,-1.23467863058847E-16,1.));
#121594=DIRECTION('ref_axis',(0.,-1.,0.));
#121595=DIRECTION('center_axis',(0.6350303583426,0.772487180465326,-1.66587444809586E-15));
#121596=DIRECTION('ref_axis',(-0.772487180465326,0.6350303583426,9.8727026228538E-31));
#121597=DIRECTION('center_axis',(3.41589266556873E-31,9.45049376705E-46,
-1.));
#121598=DIRECTION('ref_axis',(2.766624918373E-15,-1.,6.22301527786114E-61));
#121599=DIRECTION('center_axis',(1.22040233680755E-31,-1.20629111639801E-46,
1.));
#121600=DIRECTION('ref_axis',(9.88437239110458E-16,1.,-1.75022304689845E-61));
#121601=DIRECTION('center_axis',(0.,-1.23467863058847E-16,1.));
#121602=DIRECTION('ref_axis',(0.,-1.,0.));
#121603=DIRECTION('center_axis',(0.77428749071043,0.632834008037926,3.58179916610815E-15));
#121604=DIRECTION('ref_axis',(-0.632834008037926,0.77428749071043,7.75406439997931E-31));
#121605=DIRECTION('center_axis',(-3.28984474486076E-31,8.76590731964757E-46,
-1.));
#121606=DIRECTION('ref_axis',(-2.66453525910038E-15,-1.,4.66726145839586E-61));
#121607=DIRECTION('center_axis',(-1.09661491495359E-30,-9.73989702183063E-45,
1.));
#121608=DIRECTION('ref_axis',(-8.88178419700125E-15,1.,-2.48920611114446E-60));
#121609=DIRECTION('center_axis',(0.,-1.23467863058847E-16,1.));
#121610=DIRECTION('ref_axis',(0.,-1.,0.));
#121611=DIRECTION('center_axis',(0.999225121087074,0.0393593367388569,-7.28294031357568E-16));
#121612=DIRECTION('ref_axis',(-0.0393593367388569,0.999225121087074,-1.34329260515414E-32));
#121613=DIRECTION('center_axis',(6.83178533113742E-31,3.78019750681997E-45,
-1.));
#121614=DIRECTION('ref_axis',(5.53324983674598E-15,-1.,5.60071375007503E-60));
#121615=DIRECTION('center_axis',(-2.4408046736151E-31,-4.82516446559199E-46,
1.));
#121616=DIRECTION('ref_axis',(-1.97687447822091E-15,1.,-3.11150763893057E-61));
#121617=DIRECTION('center_axis',(0.,-1.23467863058847E-16,1.));
#121618=DIRECTION('ref_axis',(0.,-1.,-1.32864206562206E-16));
#121619=DIRECTION('center_axis',(1.26316997428288E-31,1.29932421951445E-16,
-1.));
#121620=DIRECTION('ref_axis',(-1.95399252334027E-14,-1.,-1.29932421951445E-16));
#121621=DIRECTION('center_axis',(-2.23194489598359E-31,-1.29750229435012E-16,
1.));
#121622=DIRECTION('ref_axis',(3.5527136788005E-14,1.,1.29750229435012E-16));
#121623=DIRECTION('center_axis',(-0.994526788819783,-0.10448189469861,-1.81517644375859E-14));
#121624=DIRECTION('ref_axis',(0.10448189469861,-0.994526788819783,-2.86631910367634E-30));
#121625=DIRECTION('center_axis',(-0.993679318607912,0.112256009954549,1.48651952901285E-13));
#121626=DIRECTION('ref_axis',(-0.112256009954549,-0.993679318607912,-2.2981091857326E-29));
#121627=DIRECTION('center_axis',(0.173003591922937,0.223692887116409,0.959182594418439));
#121628=DIRECTION('ref_axis',(0.884537270739863,0.393052221940888,-0.251204632718837));
#121629=DIRECTION('center_axis',(-0.991556456479175,0.129675724846491,-3.15431192506052E-12));
#121630=DIRECTION('ref_axis',(-0.129675724846491,-0.991556456479175,7.41046500628616E-29));
#121631=DIRECTION('center_axis',(-2.53853736684027E-13,-2.16212897560618E-12,
-1.));
#121632=DIRECTION('ref_axis',(0.129669785749073,0.991557233176073,-2.1767505907557E-12));
#121633=DIRECTION('center_axis',(0.000137331807541708,0.00219823298717573,
0.999997574452913));
#121634=DIRECTION('ref_axis',(0.11217860466933,0.993685625182725,-0.00219976354633589));
#121635=DIRECTION('center_axis',(-0.858927270467749,0.512097592307192,-1.49780811271862E-14));
#121636=DIRECTION('ref_axis',(-0.512097592307192,-0.858927270467749,-6.01293732495529E-30));
#121637=DIRECTION('center_axis',(-0.536899969302814,0.843645910890723,1.46316605705353E-12));
#121638=DIRECTION('ref_axis',(-0.843645910890723,-0.536899969302814,1.20303121328766E-28));
#121639=DIRECTION('center_axis',(-0.040766102180794,0.99916871694073,1.55671748522919E-15));
#121640=DIRECTION('ref_axis',(-0.99916871694073,-0.040766102180794,-1.4838474346331E-32));
#121641=DIRECTION('center_axis',(-0.0297586090124609,0.999557114521048,
-7.26582357398889E-15));
#121642=DIRECTION('ref_axis',(-0.999557114521048,-0.0297586090124609,1.68195404251657E-31));
#121643=DIRECTION('center_axis',(0.,0.,-1.));
#121644=DIRECTION('ref_axis',(0.999557147327688,0.0297575070551087,0.));
#121645=DIRECTION('center_axis',(-0.0210932860527463,-5.46714727619952E-5,
0.999777510396452));
#121646=DIRECTION('ref_axis',(0.998923256585619,0.0413287487753403,0.0210775230292068));
#121647=DIRECTION('center_axis',(0.233238585379144,0.972419540265587,-4.54398481782876E-15));
#121648=DIRECTION('ref_axis',(-0.972419540265587,0.233238585379145,-6.30780798053809E-30));
#121649=DIRECTION('center_axis',(-0.229570335512527,0.973292073867175,1.03212124729447E-14));
#121650=DIRECTION('ref_axis',(-0.973292073867175,-0.229570335512527,2.98849951310675E-30));
#121651=DIRECTION('center_axis',(0.0298379862379757,0.999554748164033,8.0054834066732E-15));
#121652=DIRECTION('ref_axis',(-0.999554748164032,0.0298379862379757,9.39450193490723E-31));
#121653=DIRECTION('center_axis',(0.0407665603815583,0.999168698246025,4.49007546874249E-14));
#121654=DIRECTION('ref_axis',(-0.999168698246025,0.0407665603815583,1.08335075317432E-30));
#121655=DIRECTION('center_axis',(-1.70507880518925E-12,5.55629427464142E-14,
-1.));
#121656=DIRECTION('ref_axis',(0.999168739570264,-0.040765547531825,-1.70593188493018E-12));
#121657=DIRECTION('center_axis',(-0.0206791468565618,-0.000130026885512925,
0.999786155124332));
#121658=DIRECTION('ref_axis',(0.9993253707471,-0.0303600651974135,0.0206656677215903));
#121659=DIRECTION('center_axis',(0.536601093577061,0.843836042351772,-2.84249428416013E-15));
#121660=DIRECTION('ref_axis',(-0.843836042351772,0.536601093577061,2.98189956073675E-31));
#121661=DIRECTION('center_axis',(0.882960425292266,0.469447427693135,-5.17032777304292E-14));
#121662=DIRECTION('ref_axis',(-0.469447427693135,0.882960425292266,-2.22396706740103E-29));
#121663=DIRECTION('center_axis',(0.999360062311266,0.0357696219888033,1.64961351615811E-15));
#121664=DIRECTION('ref_axis',(-0.0357696219888033,0.999360062311266,4.316049615934E-32));
#121665=DIRECTION('center_axis',(0.999556853338411,0.0297673805400138,1.82491045181999E-14));
#121666=DIRECTION('ref_axis',(-0.0297673805400138,0.999556853338411,-8.47827291376735E-32));
#121667=DIRECTION('center_axis',(0.,0.,-1.));
#121668=DIRECTION('ref_axis',(0.0297644531369321,-0.999556940513875,0.));
#121669=DIRECTION('center_axis',(1.57626159414375E-5,0.0233282309877023,
0.999727859665081));
#121670=DIRECTION('ref_axis',(0.0363487305279994,-0.999067219538478,0.023312242119934));
#121671=DIRECTION('center_axis',(0.972436723729276,-0.233166932352493,0.));
#121672=DIRECTION('ref_axis',(0.233166932352493,0.972436723729276,0.));
#121673=DIRECTION('center_axis',(0.0068520731291586,-0.00565696608596777,
-0.999960523135056));
#121674=DIRECTION('ref_axis',(0.755063620042167,-0.655591356155534,0.00888275987323359));
#121675=DIRECTION('center_axis',(-0.635093426738814,-0.772416788158568,
-0.00535207286497078));
#121676=DIRECTION('ref_axis',(0.77242785121363,-0.635102522959478,9.38368926324323E-20));
#121677=DIRECTION('center_axis',(-0.563237659270021,-0.823253026831934,
0.0708363818393295));
#121678=DIRECTION('ref_axis',(0.825326289137892,-0.564656104596307,-9.62895252096333E-18));
#121679=DIRECTION('center_axis',(-0.341333328819756,0.277129686002563,0.898159615977553));
#121680=DIRECTION('ref_axis',(0.751460582051474,-0.493539243236486,0.437865286370611));
#121681=DIRECTION('center_axis',(0.509059682279704,-0.413543807234115,-0.754877314121705));
#121682=DIRECTION('ref_axis',(0.798913102792373,0.55338237641331,0.235596688562935));
#121683=DIRECTION('center_axis',(-0.0353652067153621,-0.980391286708013,
0.193861360515669));
#121684=DIRECTION('ref_axis',(-3.63487303375728E-18,-0.193982705344839,
-0.981004949032928));
#121685=DIRECTION('center_axis',(-0.0385934612262193,-0.999254003953662,
0.00140724310442582));
#121686=DIRECTION('ref_axis',(0.999254993383049,-0.0385934994402315,-2.19294060248386E-20));
#121687=DIRECTION('center_axis',(0.0362455094603874,7.24243967428071E-6,
0.999342915615808));
#121688=DIRECTION('ref_axis',(0.99884239871172,-0.0316458184758586,-0.036227126698248));
#121689=DIRECTION('center_axis',(0.0149227809046296,0.000160750066432761,
-0.999888636183795));
#121690=DIRECTION('ref_axis',(0.999085030892015,-0.0400869256955743,0.0149043428496258));
#121691=DIRECTION('center_axis',(-0.803581860357368,-0.445034265274962,
0.395222337976698));
#121692=DIRECTION('ref_axis',(0.439140785392348,-0.891532545451671,-0.111018426423077));
#121693=DIRECTION('center_axis',(-0.469907551033905,0.216399115636686,-0.855779361887735));
#121694=DIRECTION('ref_axis',(0.876549208984677,-2.3138118535155E-14,-0.481312252314792));
#121695=DIRECTION('center_axis',(-0.460561989867266,0.543327519921019,-0.701910150650338));
#121696=DIRECTION('ref_axis',(-1.68332661555862E-16,0.790771035553874,0.612112056186654));
#121697=DIRECTION('center_axis',(0.488505761670049,0.207277391256933,0.847583744469469));
#121698=DIRECTION('ref_axis',(0.866400038259138,1.13916389737517E-16,-0.499350551921758));
#121699=DIRECTION('center_axis',(-0.485723325571869,-0.464849177451359,
-0.740262178703059));
#121700=DIRECTION('ref_axis',(-0.836086106459356,-1.21161241824207E-16,
0.548598234216658));
#121701=DIRECTION('center_axis',(0.015774878482318,2.06992946781092E-6,
-0.999875568860738));
#121702=DIRECTION('ref_axis',(0.99934939359657,0.0324376701882913,0.0157666442505599));
#121703=DIRECTION('center_axis',(0.0387718059368437,-0.999247421633299,
-0.00115647031964687));
#121704=DIRECTION('ref_axis',(0.999248089842511,0.0387718318640339,-1.43119761272989E-20));
#121705=DIRECTION('center_axis',(0.0366457249192154,0.000264295716704561,
0.999328284895869));
#121706=DIRECTION('ref_axis',(0.998575905634023,0.0387881617069405,-0.0366283933388643));
#121707=DIRECTION('center_axis',(0.0362051861961663,-0.986513040328005,
-0.159628336316885));
#121708=DIRECTION('ref_axis',(3.13261606677306E-17,0.159733060933468,-0.987160244967769));
#121709=DIRECTION('center_axis',(0.586558422242651,-0.80833932738343,-0.0503661503543409));
#121710=DIRECTION('ref_axis',(0.809366559200372,0.587303816476745,6.0201141129801E-17));
#121711=DIRECTION('center_axis',(0.635108704314869,-0.772391525947514,0.00694725470670599));
#121712=DIRECTION('ref_axis',(0.772410166108943,0.635124031423434,-3.90764897276796E-18));
#121713=DIRECTION('center_axis',(-0.367164830643458,-0.297433524522046,
0.88131906006222));
#121714=DIRECTION('ref_axis',(0.67960514144709,0.561137496245174,0.472505621158498));
#121715=DIRECTION('center_axis',(0.533623207901549,0.432878874093675,-0.726541225500833));
#121716=DIRECTION('ref_axis',(0.613440310257391,0.393261638389221,0.684862226672446));
#121717=DIRECTION('center_axis',(0.00304815896002169,0.0038938690271396,
-0.99998777318073));
#121718=DIRECTION('ref_axis',(-0.641245941557608,0.767334721447853,0.00103329397685693));
#121719=DIRECTION('center_axis',(0.119709524432718,-0.500158371272784,0.857619515522967));
#121720=DIRECTION('ref_axis',(5.19703601812987E-17,-0.863831361964004,-0.503781081510029));
#121721=DIRECTION('center_axis',(-0.998342751080717,-0.0344241690564106,
0.0461164607202445));
#121722=DIRECTION('ref_axis',(0.0536635038266924,-0.267462686432825,0.962072730994481));
#121723=DIRECTION('center_axis',(-0.501099625553759,0.466384922602348,-0.728961088974634));
#121724=DIRECTION('ref_axis',(-0.824074180962238,-2.20209609654532E-16,
0.566481901097834));
#121725=DIRECTION('center_axis',(-0.254850132245688,-0.841789549666582,
-0.475858975082417));
#121726=DIRECTION('ref_axis',(-0.487493661504454,0.536841701873146,-0.688586172619612));
#121727=DIRECTION('center_axis',(-0.0894444115370802,-0.865796085393033,
-0.492338131534503));
#121728=DIRECTION('ref_axis',(0.983291176009294,-0.155450632474041,0.0947288976272861));
#121729=DIRECTION('center_axis',(-4.00197585461019E-5,-0.0159615005705134,
-0.999872606334405));
#121730=DIRECTION('ref_axis',(0.0321201706221352,-0.999356707583681,0.0159519793978996));
#121731=DIRECTION('center_axis',(-0.999263201609641,-0.0383614667420372,
-0.00120489761000603));
#121732=DIRECTION('ref_axis',(0.0383614945882391,-0.999263926964722,2.87536200646804E-20));
#121733=DIRECTION('center_axis',(-2.30441962568634E-5,-0.0307840994537002,
0.999526057033927));
#121734=DIRECTION('ref_axis',(0.0383802756232838,-0.998789639512621,-0.0307605338921488));
#121735=DIRECTION('center_axis',(-0.974363720155827,-0.0344964635874725,
-0.222318093829667));
#121736=DIRECTION('ref_axis',(-0.222450491940089,1.26241972147447E-18,0.974943987434977));
#121737=DIRECTION('center_axis',(-0.836810598831192,-0.541308500745221,
-0.0820556439542334));
#121738=DIRECTION('ref_axis',(0.543140105176027,-0.839642082169167,1.69471490770742E-17));
#121739=DIRECTION('center_axis',(-0.774120577489127,-0.632943886852024,
0.0109255482495788));
#121740=DIRECTION('ref_axis',(0.632981666732123,-0.774166784085331,5.39501067277511E-19));
#121741=DIRECTION('center_axis',(-0.26668203931152,0.334936975495388,0.903713401668167));
#121742=DIRECTION('ref_axis',(0.574033930782738,-0.698011739529375,0.428094216019436));
#121743=DIRECTION('center_axis',(0.0101770580641384,-0.0115323051715096,
-0.999881709717));
#121744=DIRECTION('ref_axis',(0.775808985621547,0.630967538505684,0.000619016109577773));
#121745=DIRECTION('center_axis',(-4.45320928885371E-8,0.998303409681459,
0.0582263017748053));
#121746=DIRECTION('ref_axis',(0.,-0.0582263017748052,0.99830340968146));
#121747=DIRECTION('center_axis',(-8.12532577157186E-9,0.998207006171548,
0.0598562680931181));
#121748=DIRECTION('ref_axis',(0.999311726713681,-0.00222038745151431,0.0370289445175939));
#121749=DIRECTION('center_axis',(-0.99999635393917,0.000157155077313813,
-0.00269581354111146));
#121750=DIRECTION('ref_axis',(-0.00269581357440168,1.24619272072387E-21,
0.999996366287984));
#121751=DIRECTION('center_axis',(-2.33119191152438E-9,-0.986382708044219,
-0.164466267882973));
#121752=DIRECTION('ref_axis',(0.999999030863823,-0.000228975224915186,0.00137325953914107));
#121753=DIRECTION('center_axis',(0.244344449131117,0.492606745559265,0.835245104390514));
#121754=DIRECTION('ref_axis',(4.32889927015855E-17,-0.86135403585069,0.508005142615435));
#121755=DIRECTION('center_axis',(0.330813257101916,-0.830741130674896,0.447696060660149));
#121756=DIRECTION('ref_axis',(0.932375699002072,0.214461635172499,-0.291001310906903));
#121757=DIRECTION('center_axis',(0.000178107895792883,0.00455637129950124,
0.999989603825039));
#121758=DIRECTION('ref_axis',(0.986443060931718,-0.16410289554268,0.000572026372399929));
#121759=DIRECTION('center_axis',(-0.982994797178248,0.183632204703407,-0.000664918236953841));
#121760=DIRECTION('ref_axis',(-0.183632245296812,-0.982995014477312,5.7655403569157E-20));
#121761=DIRECTION('center_axis',(-0.433391148275503,-0.470797811534069,
-0.768453989026781));
#121762=DIRECTION('ref_axis',(-8.06979081629128E-16,0.852695228537141,-0.522408697506075));
#121763=DIRECTION('center_axis',(-0.96720597488598,0.18129103740974,-0.177893681449798));
#121764=DIRECTION('ref_axis',(-0.184229551589837,-0.982883244501099,1.61805378326746E-17));
#121765=DIRECTION('center_axis',(-0.831503844166329,0.548952032819844,-0.0851646804701234));
#121766=DIRECTION('ref_axis',(-0.550953708881667,-0.834535805504794,3.15287181374443E-17));
#121767=DIRECTION('center_axis',(-0.777065025633406,0.629380269512156,0.00710086516978589));
#121768=DIRECTION('ref_axis',(-0.62939613750826,-0.777084617071837,1.0927692862107E-18));
#121769=DIRECTION('center_axis',(-0.295452400444952,-0.370381022938362,
0.880639413675341));
#121770=DIRECTION('ref_axis',(0.467331061476171,0.747944548358106,0.471360405168853));
#121771=DIRECTION('center_axis',(0.,0.,-1.));
#121772=DIRECTION('ref_axis',(0.,1.,0.));
#121773=DIRECTION('center_axis',(0.,0.,-1.));
#121774=DIRECTION('ref_axis',(0.,1.,0.));
#121775=DIRECTION('',(-3.82498197630791E-33,-1.23467863058847E-16,1.));
#121776=DIRECTION('',(0.,1.23467863058847E-16,-1.));
#121777=DIRECTION('center_axis',(0.,0.,-1.));
#121778=DIRECTION('ref_axis',(0.,1.,0.));
#121779=DIRECTION('',(0.,-1.23467863058847E-16,1.));
#121780=DIRECTION('',(0.,1.23467863058847E-16,-1.));
#121781=DIRECTION('center_axis',(0.,0.,-1.));
#121782=DIRECTION('ref_axis',(0.,1.,0.));
#121783=DIRECTION('center_axis',(0.,0.,-1.));
#121784=DIRECTION('ref_axis',(0.,1.,0.));
#121785=DIRECTION('',(0.,-1.23467863058847E-16,1.));
#121786=DIRECTION('',(0.,1.23467863058847E-16,-1.));
#121787=DIRECTION('center_axis',(0.,0.,-1.));
#121788=DIRECTION('ref_axis',(0.,1.,0.));
#121789=DIRECTION('center_axis',(0.,0.,-1.));
#121790=DIRECTION('ref_axis',(0.,1.,0.));
#121791=DIRECTION('',(0.,-1.23467863058847E-16,1.));
#121792=DIRECTION('',(0.,1.23467863058847E-16,-1.));
#121793=DIRECTION('center_axis',(0.,0.,-1.));
#121794=DIRECTION('ref_axis',(0.,1.,0.));
#121795=DIRECTION('center_axis',(0.,0.,-1.));
#121796=DIRECTION('ref_axis',(0.,1.,0.));
#121797=DIRECTION('',(0.,-1.23467863058847E-16,1.));
#121798=DIRECTION('',(0.,1.23467863058847E-16,-1.));
#121799=DIRECTION('center_axis',(0.,0.,-1.));
#121800=DIRECTION('ref_axis',(0.,1.,0.));
#121801=DIRECTION('center_axis',(0.,0.,-1.));
#121802=DIRECTION('ref_axis',(0.,1.,0.));
#121803=DIRECTION('',(0.,-1.23467863058847E-16,1.));
#121804=DIRECTION('',(0.,1.23467863058847E-16,-1.));
#121805=DIRECTION('center_axis',(0.,0.,-1.));
#121806=DIRECTION('ref_axis',(0.,1.,0.));
#121807=DIRECTION('center_axis',(0.,0.,-1.));
#121808=DIRECTION('ref_axis',(0.,1.,0.));
#121809=DIRECTION('',(0.,-1.23467863058847E-16,1.));
#121810=DIRECTION('',(1.27503726478586E-32,1.23467863058847E-16,-1.));
#121811=DIRECTION('center_axis',(0.,0.,-1.));
#121812=DIRECTION('ref_axis',(0.,1.,0.));
#121813=DIRECTION('center_axis',(0.,0.,-1.));
#121814=DIRECTION('ref_axis',(0.0950205176920726,-0.995475314218053,0.));
#121815=DIRECTION('',(0.,-1.23467863058847E-16,1.));
#121816=DIRECTION('',(0.,1.23467863058847E-16,-1.));
#121817=DIRECTION('center_axis',(0.,0.,-1.));
#121818=DIRECTION('ref_axis',(0.,1.,0.));
#121819=DIRECTION('center_axis',(0.,0.,-1.));
#121820=DIRECTION('ref_axis',(0.,1.,0.));
#121821=DIRECTION('',(0.,-1.23467863058847E-16,1.));
#121822=DIRECTION('',(0.,1.23467863058847E-16,-1.));
#121823=DIRECTION('center_axis',(0.,0.,-1.));
#121824=DIRECTION('ref_axis',(0.,1.,0.));
#121825=DIRECTION('center_axis',(0.,0.,-1.));
#121826=DIRECTION('ref_axis',(0.,1.,0.));
#121827=DIRECTION('center_axis',(0.,0.,-1.));
#121828=DIRECTION('ref_axis',(0.,1.,0.));
#121829=DIRECTION('',(0.,-1.23467863058847E-16,1.));
#121830=DIRECTION('',(0.,1.23467863058847E-16,-1.));
#121831=DIRECTION('center_axis',(0.,0.,-1.));
#121832=DIRECTION('ref_axis',(0.,1.,0.));
#121833=DIRECTION('',(0.,-1.23467863058847E-16,1.));
#121834=DIRECTION('',(0.,1.23467863058847E-16,-1.));
#121835=DIRECTION('center_axis',(0.,0.,-1.));
#121836=DIRECTION('ref_axis',(0.,1.,0.));
#121837=DIRECTION('center_axis',(1.3684555315672E-48,0.,1.));
#121838=DIRECTION('ref_axis',(0.,-1.,0.));
#121839=DIRECTION('',(0.,-1.23467863058847E-16,1.));
#121840=DIRECTION('',(-1.3684555315672E-48,1.23467863058847E-16,-1.));
#121841=DIRECTION('center_axis',(0.,0.,-1.));
#121842=DIRECTION('ref_axis',(0.,1.,0.));
#121843=DIRECTION('center_axis',(0.,0.,-1.));
#121844=DIRECTION('ref_axis',(0.,1.,0.));
#121845=DIRECTION('',(0.,-1.23467863058847E-16,1.));
#121846=DIRECTION('',(0.,1.23467863058847E-16,-1.));
#121847=DIRECTION('center_axis',(0.,0.,-1.));
#121848=DIRECTION('ref_axis',(0.,1.,0.));
#121849=DIRECTION('center_axis',(0.,0.,1.));
#121850=DIRECTION('ref_axis',(0.,-1.,0.));
#121851=DIRECTION('',(0.,-1.23467863058847E-16,1.));
#121852=DIRECTION('',(0.,1.23467863058847E-16,-1.));
#121853=DIRECTION('center_axis',(0.,0.,-1.));
#121854=DIRECTION('ref_axis',(0.,1.,0.));
#121855=DIRECTION('center_axis',(0.,0.,-1.));
#121856=DIRECTION('ref_axis',(0.,1.,0.));
#121857=DIRECTION('',(0.,-1.23467863058847E-16,1.));
#121858=DIRECTION('',(0.,1.23467863058847E-16,-1.));
#121859=DIRECTION('center_axis',(0.,0.,-1.));
#121860=DIRECTION('ref_axis',(0.,1.,0.));
#121861=DIRECTION('center_axis',(0.,0.,-1.));
#121862=DIRECTION('ref_axis',(0.,1.,0.));
#121863=DIRECTION('',(0.,-1.23467863058847E-16,1.));
#121864=DIRECTION('',(0.,1.23467863058847E-16,-1.));
#121865=DIRECTION('center_axis',(0.,0.,-1.));
#121866=DIRECTION('ref_axis',(0.,1.,0.));
#121867=DIRECTION('center_axis',(0.,0.,1.));
#121868=DIRECTION('ref_axis',(0.,-1.,0.));
#121869=DIRECTION('',(0.,-1.23467863058847E-16,1.));
#121870=DIRECTION('',(0.,1.23467863058847E-16,-1.));
#121871=DIRECTION('center_axis',(0.,0.,-1.));
#121872=DIRECTION('ref_axis',(0.,1.,0.));
#121873=DIRECTION('center_axis',(-1.3684555315672E-48,0.,-1.));
#121874=DIRECTION('ref_axis',(0.,1.,0.));
#121875=DIRECTION('',(1.3684555315672E-48,-1.23467863058847E-16,1.));
#121876=DIRECTION('',(0.,1.23467863058847E-16,-1.));
#121877=DIRECTION('center_axis',(0.,0.,-1.));
#121878=DIRECTION('ref_axis',(0.,1.,0.));
#121879=DIRECTION('center_axis',(0.,0.,-1.));
#121880=DIRECTION('ref_axis',(0.686617021913642,-0.727019301819726,0.));
#121881=DIRECTION('',(0.,-1.23467863058847E-16,1.));
#121882=DIRECTION('',(0.,1.23467863058847E-16,-1.));
#121883=DIRECTION('center_axis',(0.,0.,-1.));
#121884=DIRECTION('ref_axis',(0.,1.,0.));
#121885=DIRECTION('center_axis',(0.,0.,1.));
#121886=DIRECTION('ref_axis',(0.,-1.,0.));
#121887=DIRECTION('',(0.,-1.23467863058847E-16,1.));
#121888=DIRECTION('',(0.,1.23467863058847E-16,-1.));
#121889=DIRECTION('center_axis',(0.,0.,-1.));
#121890=DIRECTION('ref_axis',(0.,1.,0.));
#121891=DIRECTION('center_axis',(0.,0.,-1.));
#121892=DIRECTION('ref_axis',(0.,1.,0.));
#121893=DIRECTION('',(0.,-1.23467863058847E-16,1.));
#121894=DIRECTION('',(0.,1.23467863058847E-16,-1.));
#121895=DIRECTION('center_axis',(0.,0.,-1.));
#121896=DIRECTION('ref_axis',(0.,1.,0.));
#121897=DIRECTION('center_axis',(0.,0.,-1.));
#121898=DIRECTION('ref_axis',(0.,1.,0.));
#121899=DIRECTION('',(0.,-1.23467863058847E-16,1.));
#121900=DIRECTION('',(0.,1.23467863058847E-16,-1.));
#121901=DIRECTION('center_axis',(0.,0.,-1.));
#121902=DIRECTION('ref_axis',(0.,1.,0.));
#121903=DIRECTION('center_axis',(0.,0.,-1.));
#121904=DIRECTION('ref_axis',(0.,1.,0.));
#121905=DIRECTION('',(0.,-1.23467863058847E-16,1.));
#121906=DIRECTION('',(0.,1.23467863058847E-16,-1.));
#121907=DIRECTION('center_axis',(0.,0.,-1.));
#121908=DIRECTION('ref_axis',(0.,1.,0.));
#121909=DIRECTION('center_axis',(0.,0.,1.));
#121910=DIRECTION('ref_axis',(0.,-1.,0.));
#121911=DIRECTION('',(0.,-1.23467863058847E-16,1.));
#121912=DIRECTION('',(0.,1.23467863058847E-16,-1.));
#121913=DIRECTION('center_axis',(0.,0.,-1.));
#121914=DIRECTION('ref_axis',(0.,1.,0.));
#121915=DIRECTION('center_axis',(0.,0.,-1.));
#121916=DIRECTION('ref_axis',(0.,1.,0.));
#121917=DIRECTION('',(0.,-1.23467863058847E-16,1.));
#121918=DIRECTION('',(0.,1.23467863058847E-16,-1.));
#121919=DIRECTION('center_axis',(0.,0.,-1.));
#121920=DIRECTION('ref_axis',(0.,1.,0.));
#121921=DIRECTION('center_axis',(0.,0.,1.));
#121922=DIRECTION('ref_axis',(0.,-1.,0.));
#121923=DIRECTION('',(0.,-1.23467863058847E-16,1.));
#121924=DIRECTION('',(0.,1.23467863058847E-16,-1.));
#121925=DIRECTION('center_axis',(0.,0.,-1.));
#121926=DIRECTION('ref_axis',(0.,1.,0.));
#121927=DIRECTION('center_axis',(0.,0.,-1.));
#121928=DIRECTION('ref_axis',(0.,1.,0.));
#121929=DIRECTION('',(0.,-1.23467863058847E-16,1.));
#121930=DIRECTION('',(0.,1.23467863058847E-16,-1.));
#121931=DIRECTION('center_axis',(0.,0.,-1.));
#121932=DIRECTION('ref_axis',(0.,1.,0.));
#121933=DIRECTION('center_axis',(0.,0.,-1.));
#121934=DIRECTION('ref_axis',(0.,1.,0.));
#121935=DIRECTION('center_axis',(0.,0.,-1.));
#121936=DIRECTION('ref_axis',(0.,1.,0.));
#121937=DIRECTION('',(0.,-1.23467863058847E-16,1.));
#121938=DIRECTION('',(0.,1.23467863058847E-16,-1.));
#121939=DIRECTION('center_axis',(0.,0.,1.));
#121940=DIRECTION('ref_axis',(0.,-1.,0.));
#121941=DIRECTION('',(0.,-1.23467863058847E-16,1.));
#121942=DIRECTION('',(0.,1.23467863058847E-16,-1.));
#121943=DIRECTION('center_axis',(0.,0.,-1.));
#121944=DIRECTION('ref_axis',(0.,1.,0.));
#121945=DIRECTION('center_axis',(0.,0.,-1.));
#121946=DIRECTION('ref_axis',(0.,1.,0.));
#121947=DIRECTION('',(0.,-1.23467863058847E-16,1.));
#121948=DIRECTION('',(0.,1.23467863058847E-16,-1.));
#121949=DIRECTION('center_axis',(0.,0.,-1.));
#121950=DIRECTION('ref_axis',(0.,1.,0.));
#121951=DIRECTION('center_axis',(0.,0.,1.));
#121952=DIRECTION('ref_axis',(0.,-1.,0.));
#121953=DIRECTION('',(0.,-1.23467863058847E-16,1.));
#121954=DIRECTION('',(0.,1.23467863058847E-16,-1.));
#121955=DIRECTION('center_axis',(0.,0.,-1.));
#121956=DIRECTION('ref_axis',(0.,1.,0.));
#121957=DIRECTION('center_axis',(0.,0.,-1.));
#121958=DIRECTION('ref_axis',(0.,1.,0.));
#121959=DIRECTION('',(0.,-1.23467863058847E-16,1.));
#121960=DIRECTION('',(0.,1.23467863058847E-16,-1.));
#121961=DIRECTION('center_axis',(0.,0.,-1.));
#121962=DIRECTION('ref_axis',(0.,1.,0.));
#121963=DIRECTION('center_axis',(0.,0.,1.));
#121964=DIRECTION('ref_axis',(0.,-1.,0.));
#121965=DIRECTION('',(0.,-1.23467863058847E-16,1.));
#121966=DIRECTION('',(0.,1.23467863058847E-16,-1.));
#121967=DIRECTION('center_axis',(0.,0.,-1.));
#121968=DIRECTION('ref_axis',(0.,1.,0.));
#121969=DIRECTION('center_axis',(0.,0.,-1.));
#121970=DIRECTION('ref_axis',(0.,1.,0.));
#121971=DIRECTION('',(0.,-1.23467863058847E-16,1.));
#121972=DIRECTION('',(0.,1.23467863058847E-16,-1.));
#121973=DIRECTION('center_axis',(0.,0.,-1.));
#121974=DIRECTION('ref_axis',(0.,1.,0.));
#121975=DIRECTION('center_axis',(0.,0.,1.));
#121976=DIRECTION('ref_axis',(0.,-1.,0.));
#121977=DIRECTION('',(0.,-1.23467863058847E-16,1.));
#121978=DIRECTION('',(0.,1.23467863058847E-16,-1.));
#121979=DIRECTION('center_axis',(0.,0.,-1.));
#121980=DIRECTION('ref_axis',(0.,1.,0.));
#121981=DIRECTION('center_axis',(0.,0.,-1.));
#121982=DIRECTION('ref_axis',(0.,1.,0.));
#121983=DIRECTION('',(0.,-1.23467863058847E-16,1.));
#121984=DIRECTION('',(0.,1.23467863058847E-16,-1.));
#121985=DIRECTION('center_axis',(0.,0.,-1.));
#121986=DIRECTION('ref_axis',(0.,1.,0.));
#121987=DIRECTION('center_axis',(0.,0.,1.));
#121988=DIRECTION('ref_axis',(0.,-1.,0.));
#121989=DIRECTION('',(0.,-1.23467863058847E-16,1.));
#121990=DIRECTION('',(0.,1.23467863058847E-16,-1.));
#121991=DIRECTION('center_axis',(0.,0.,-1.));
#121992=DIRECTION('ref_axis',(0.,1.,0.));
#121993=DIRECTION('center_axis',(0.,0.,-1.));
#121994=DIRECTION('ref_axis',(0.,1.,0.));
#121995=DIRECTION('',(0.,-1.23467863058847E-16,1.));
#121996=DIRECTION('',(0.,1.23467863058847E-16,-1.));
#121997=DIRECTION('center_axis',(0.,0.,-1.));
#121998=DIRECTION('ref_axis',(0.,1.,0.));
#121999=DIRECTION('center_axis',(0.,0.,-1.));
#122000=DIRECTION('ref_axis',(-0.695782815675815,-0.718252235228151,0.));
#122001=DIRECTION('',(0.,-1.23467863058847E-16,1.));
#122002=DIRECTION('',(0.,1.23467863058847E-16,-1.));
#122003=DIRECTION('center_axis',(0.,0.,-1.));
#122004=DIRECTION('ref_axis',(0.,1.,0.));
#122005=DIRECTION('center_axis',(0.,0.,-1.));
#122006=DIRECTION('ref_axis',(0.,1.,0.));
#122007=DIRECTION('',(0.,-1.23467863058847E-16,1.));
#122008=DIRECTION('',(0.,1.23467863058847E-16,-1.));
#122009=DIRECTION('center_axis',(0.,0.,-1.));
#122010=DIRECTION('ref_axis',(0.,1.,0.));
#122011=DIRECTION('center_axis',(0.,0.,1.));
#122012=DIRECTION('ref_axis',(0.,-1.,0.));
#122013=DIRECTION('',(0.,-1.23467863058847E-16,1.));
#122014=DIRECTION('',(0.,1.23467863058847E-16,-1.));
#122015=DIRECTION('center_axis',(0.,0.,-1.));
#122016=DIRECTION('ref_axis',(0.,1.,0.));
#122017=DIRECTION('center_axis',(0.,0.,-1.));
#122018=DIRECTION('ref_axis',(0.,1.,0.));
#122019=DIRECTION('',(0.,-1.23467863058847E-16,1.));
#122020=DIRECTION('',(0.,1.23467863058847E-16,-1.));
#122021=DIRECTION('center_axis',(0.,0.,-1.));
#122022=DIRECTION('ref_axis',(0.,1.,0.));
#122023=DIRECTION('center_axis',(0.,0.,-1.));
#122024=DIRECTION('ref_axis',(0.,1.,0.));
#122025=DIRECTION('',(0.,-1.23467863058847E-16,1.));
#122026=DIRECTION('',(0.,1.23467863058847E-16,-1.));
#122027=DIRECTION('center_axis',(0.,0.,-1.));
#122028=DIRECTION('ref_axis',(0.,1.,0.));
#122029=DIRECTION('center_axis',(0.,0.,-1.));
#122030=DIRECTION('ref_axis',(0.,1.,0.));
#122031=DIRECTION('',(0.,-1.23467863058847E-16,1.));
#122032=DIRECTION('',(0.,1.23467863058847E-16,-1.));
#122033=DIRECTION('center_axis',(0.,0.,-1.));
#122034=DIRECTION('ref_axis',(0.,1.,0.));
#122035=DIRECTION('center_axis',(0.,0.,1.));
#122036=DIRECTION('ref_axis',(0.,-1.,0.));
#122037=DIRECTION('',(0.,-1.23467863058847E-16,1.));
#122038=DIRECTION('',(0.,1.23467863058847E-16,-1.));
#122039=DIRECTION('center_axis',(0.,0.,-1.));
#122040=DIRECTION('ref_axis',(0.,1.,0.));
#122041=DIRECTION('center_axis',(0.,0.,-1.));
#122042=DIRECTION('ref_axis',(0.,1.,0.));
#122043=DIRECTION('',(0.,-1.23467863058847E-16,1.));
#122044=DIRECTION('',(0.,1.23467863058847E-16,-1.));
#122045=DIRECTION('center_axis',(0.,0.,-1.));
#122046=DIRECTION('ref_axis',(0.,1.,0.));
#122047=DIRECTION('center_axis',(0.,0.,1.));
#122048=DIRECTION('ref_axis',(0.,-1.,0.));
#122049=DIRECTION('',(0.,-1.23467863058847E-16,1.));
#122050=DIRECTION('',(0.,1.23467863058847E-16,-1.));
#122051=DIRECTION('center_axis',(0.,0.,-1.));
#122052=DIRECTION('ref_axis',(0.,1.,0.));
#122053=DIRECTION('center_axis',(0.,0.,-1.));
#122054=DIRECTION('ref_axis',(0.,1.,0.));
#122055=DIRECTION('',(0.,-1.23467863058847E-16,1.));
#122056=DIRECTION('',(0.,1.23467863058847E-16,-1.));
#122057=DIRECTION('center_axis',(0.,0.,-1.));
#122058=DIRECTION('ref_axis',(0.,1.,0.));
#122059=DIRECTION('center_axis',(0.,0.,1.));
#122060=DIRECTION('ref_axis',(0.,-1.,0.));
#122061=DIRECTION('',(0.,-1.23467863058847E-16,1.));
#122062=DIRECTION('',(0.,1.23467863058847E-16,-1.));
#122063=DIRECTION('center_axis',(0.,0.,-1.));
#122064=DIRECTION('ref_axis',(0.,1.,0.));
#122065=DIRECTION('center_axis',(0.,0.,-1.));
#122066=DIRECTION('ref_axis',(0.,1.,0.));
#122067=DIRECTION('',(0.,-1.23467863058847E-16,1.));
#122068=DIRECTION('',(0.,1.23467863058847E-16,-1.));
#122069=DIRECTION('center_axis',(0.,0.,-1.));
#122070=DIRECTION('ref_axis',(0.,1.,0.));
#122071=DIRECTION('center_axis',(0.,0.,1.));
#122072=DIRECTION('ref_axis',(0.,-1.,0.));
#122073=DIRECTION('',(0.,-1.23467863058847E-16,1.));
#122074=DIRECTION('',(0.,1.23467863058847E-16,-1.));
#122075=DIRECTION('center_axis',(0.,0.,-1.));
#122076=DIRECTION('ref_axis',(0.,1.,0.));
#122077=DIRECTION('center_axis',(0.,0.,-1.));
#122078=DIRECTION('ref_axis',(0.,1.,0.));
#122079=DIRECTION('',(0.,-1.23467863058847E-16,1.));
#122080=DIRECTION('',(0.,1.23467863058847E-16,-1.));
#122081=DIRECTION('center_axis',(0.,0.,-1.));
#122082=DIRECTION('ref_axis',(0.,1.,0.));
#122083=DIRECTION('center_axis',(0.,0.,1.));
#122084=DIRECTION('ref_axis',(0.,-1.,0.));
#122085=DIRECTION('',(0.,-1.23467863058847E-16,1.));
#122086=DIRECTION('',(0.,1.23467863058847E-16,-1.));
#122087=DIRECTION('center_axis',(0.,0.,-1.));
#122088=DIRECTION('ref_axis',(0.,1.,0.));
#122089=DIRECTION('center_axis',(0.,0.,-1.));
#122090=DIRECTION('ref_axis',(0.,1.,0.));
#122091=DIRECTION('',(0.,-1.23467863058847E-16,1.));
#122092=DIRECTION('',(0.,1.23467863058847E-16,-1.));
#122093=DIRECTION('center_axis',(0.,0.,-1.));
#122094=DIRECTION('ref_axis',(0.,1.,0.));
#122095=DIRECTION('center_axis',(0.,0.,1.));
#122096=DIRECTION('ref_axis',(0.,-1.,0.));
#122097=DIRECTION('',(0.,-1.23467863058847E-16,1.));
#122098=DIRECTION('',(0.,1.23467863058847E-16,-1.));
#122099=DIRECTION('center_axis',(0.,0.,-1.));
#122100=DIRECTION('ref_axis',(0.,1.,0.));
#122101=DIRECTION('center_axis',(0.,0.,-1.));
#122102=DIRECTION('ref_axis',(0.,1.,0.));
#122103=DIRECTION('',(0.,-1.23467863058847E-16,1.));
#122104=DIRECTION('',(0.,1.23467863058847E-16,-1.));
#122105=DIRECTION('center_axis',(0.,0.,-1.));
#122106=DIRECTION('ref_axis',(0.,1.,0.));
#122107=DIRECTION('center_axis',(0.,0.,-1.));
#122108=DIRECTION('ref_axis',(0.,1.,0.));
#122109=DIRECTION('',(0.,-1.23467863058847E-16,1.));
#122110=DIRECTION('',(0.,1.23467863058847E-16,-1.));
#122111=DIRECTION('center_axis',(0.,0.,-1.));
#122112=DIRECTION('ref_axis',(0.,1.,0.));
#122113=DIRECTION('center_axis',(0.,0.,-1.));
#122114=DIRECTION('ref_axis',(-0.406625030395207,-0.91359514264038,0.));
#122115=DIRECTION('',(0.,-1.23467863058847E-16,1.));
#122116=DIRECTION('',(0.,1.23467863058847E-16,-1.));
#122117=DIRECTION('center_axis',(0.,0.,-1.));
#122118=DIRECTION('ref_axis',(0.,1.,0.));
#122119=DIRECTION('center_axis',(0.,0.,-1.));
#122120=DIRECTION('ref_axis',(0.,1.,0.));
#122121=DIRECTION('',(0.,-1.23467863058847E-16,1.));
#122122=DIRECTION('',(0.,1.23467863058847E-16,-1.));
#122123=DIRECTION('center_axis',(0.,0.,-1.));
#122124=DIRECTION('ref_axis',(0.,1.,0.));
#122125=DIRECTION('center_axis',(0.,0.,-1.));
#122126=DIRECTION('ref_axis',(0.,1.,0.));
#122127=DIRECTION('',(0.,-1.23467863058847E-16,1.));
#122128=DIRECTION('',(0.,1.23467863058847E-16,-1.));
#122129=DIRECTION('center_axis',(0.,0.,-1.));
#122130=DIRECTION('ref_axis',(0.,1.,0.));
#122131=DIRECTION('center_axis',(0.,0.,1.));
#122132=DIRECTION('ref_axis',(0.,-1.,0.));
#122133=DIRECTION('',(0.,-1.23467863058847E-16,1.));
#122134=DIRECTION('',(0.,1.23467863058847E-16,-1.));
#122135=DIRECTION('center_axis',(0.,0.,-1.));
#122136=DIRECTION('ref_axis',(0.,1.,0.));
#122137=DIRECTION('center_axis',(0.,0.,-1.));
#122138=DIRECTION('ref_axis',(0.,1.,0.));
#122139=DIRECTION('',(0.,-1.23467863058847E-16,1.));
#122140=DIRECTION('',(0.,1.23467863058847E-16,-1.));
#122141=DIRECTION('center_axis',(0.,0.,-1.));
#122142=DIRECTION('ref_axis',(0.,1.,0.));
#122143=DIRECTION('center_axis',(0.,0.,1.));
#122144=DIRECTION('ref_axis',(0.,-1.,0.));
#122145=DIRECTION('',(0.,-1.23467863058847E-16,1.));
#122146=DIRECTION('',(0.,1.23467863058847E-16,-1.));
#122147=DIRECTION('center_axis',(0.,0.,-1.));
#122148=DIRECTION('ref_axis',(0.,1.,0.));
#122149=DIRECTION('center_axis',(0.,0.,-1.));
#122150=DIRECTION('ref_axis',(0.,1.,0.));
#122151=DIRECTION('',(0.,-1.23467863058847E-16,1.));
#122152=DIRECTION('',(0.,1.23467863058847E-16,-1.));
#122153=DIRECTION('center_axis',(0.,0.,-1.));
#122154=DIRECTION('ref_axis',(0.,1.,0.));
#122155=DIRECTION('center_axis',(0.,0.,1.));
#122156=DIRECTION('ref_axis',(0.,-1.,0.));
#122157=DIRECTION('',(0.,-1.23467863058847E-16,1.));
#122158=DIRECTION('',(0.,1.23467863058847E-16,-1.));
#122159=DIRECTION('center_axis',(0.,0.,-1.));
#122160=DIRECTION('ref_axis',(0.,1.,0.));
#122161=DIRECTION('center_axis',(0.,0.,-1.));
#122162=DIRECTION('ref_axis',(0.,1.,0.));
#122163=DIRECTION('',(0.,-1.23467863058847E-16,1.));
#122164=DIRECTION('',(0.,1.23467863058847E-16,-1.));
#122165=DIRECTION('center_axis',(0.,0.,-1.));
#122166=DIRECTION('ref_axis',(0.,1.,0.));
#122167=DIRECTION('center_axis',(0.,0.,-1.));
#122168=DIRECTION('ref_axis',(0.,1.,0.));
#122169=DIRECTION('',(0.,-1.23467863058847E-16,1.));
#122170=DIRECTION('',(0.,1.23467863058847E-16,-1.));
#122171=DIRECTION('center_axis',(0.,0.,-1.));
#122172=DIRECTION('ref_axis',(0.,1.,0.));
#122173=DIRECTION('center_axis',(0.,0.,-1.));
#122174=DIRECTION('ref_axis',(0.,1.,0.));
#122175=DIRECTION('',(0.,-1.23467863058847E-16,1.));
#122176=DIRECTION('',(0.,1.23467863058847E-16,-1.));
#122177=DIRECTION('center_axis',(0.,0.,-1.));
#122178=DIRECTION('ref_axis',(0.,1.,0.));
#122179=DIRECTION('center_axis',(0.,0.,1.));
#122180=DIRECTION('ref_axis',(0.,-1.,0.));
#122181=DIRECTION('',(0.,-1.23467863058847E-16,1.));
#122182=DIRECTION('',(0.,1.23467863058847E-16,-1.));
#122183=DIRECTION('center_axis',(0.,0.,-1.));
#122184=DIRECTION('ref_axis',(0.,1.,0.));
#122185=DIRECTION('center_axis',(0.,0.,-1.));
#122186=DIRECTION('ref_axis',(0.,1.,0.));
#122187=DIRECTION('',(0.,-1.23467863058847E-16,1.));
#122188=DIRECTION('',(0.,1.23467863058847E-16,-1.));
#122189=DIRECTION('center_axis',(0.,0.,-1.));
#122190=DIRECTION('ref_axis',(0.,1.,0.));
#122191=DIRECTION('center_axis',(0.,0.,-1.));
#122192=DIRECTION('ref_axis',(0.,1.,0.));
#122193=DIRECTION('',(0.,-1.23467863058847E-16,1.));
#122194=DIRECTION('',(0.,1.23467863058847E-16,-1.));
#122195=DIRECTION('center_axis',(0.,0.,-1.));
#122196=DIRECTION('ref_axis',(0.,1.,0.));
#122197=DIRECTION('center_axis',(0.,0.,-1.));
#122198=DIRECTION('ref_axis',(0.,1.,0.));
#122199=DIRECTION('',(0.,-1.23467863058847E-16,1.));
#122200=DIRECTION('',(0.,1.23467863058847E-16,-1.));
#122201=DIRECTION('center_axis',(0.,0.,-1.));
#122202=DIRECTION('ref_axis',(0.,1.,0.));
#122203=DIRECTION('center_axis',(0.,0.,1.));
#122204=DIRECTION('ref_axis',(0.,-1.,0.));
#122205=DIRECTION('',(0.,-1.23467863058847E-16,1.));
#122206=DIRECTION('',(0.,1.23467863058847E-16,-1.));
#122207=DIRECTION('center_axis',(0.,0.,-1.));
#122208=DIRECTION('ref_axis',(0.,1.,0.));
#122209=DIRECTION('center_axis',(0.,0.,-1.));
#122210=DIRECTION('ref_axis',(0.,1.,0.));
#122211=DIRECTION('',(0.,-1.23467863058847E-16,1.));
#122212=DIRECTION('',(0.,1.23467863058847E-16,-1.));
#122213=DIRECTION('center_axis',(0.,0.,-1.));
#122214=DIRECTION('ref_axis',(0.,1.,0.));
#122215=DIRECTION('center_axis',(0.,0.,-1.));
#122216=DIRECTION('ref_axis',(0.,1.,0.));
#122217=DIRECTION('',(0.,-1.23467863058847E-16,1.));
#122218=DIRECTION('',(0.,1.23467863058847E-16,-1.));
#122219=DIRECTION('center_axis',(0.,0.,-1.));
#122220=DIRECTION('ref_axis',(0.,1.,0.));
#122221=DIRECTION('center_axis',(0.,0.,-1.));
#122222=DIRECTION('ref_axis',(0.,1.,0.));
#122223=DIRECTION('',(0.,-1.23467863058847E-16,1.));
#122224=DIRECTION('',(0.,1.23467863058847E-16,-1.));
#122225=DIRECTION('center_axis',(0.,0.,-1.));
#122226=DIRECTION('ref_axis',(0.,1.,0.));
#122227=DIRECTION('center_axis',(0.,0.,1.));
#122228=DIRECTION('ref_axis',(0.,-1.,0.));
#122229=DIRECTION('',(0.,-1.23467863058847E-16,1.));
#122230=DIRECTION('',(0.,1.23467863058847E-16,-1.));
#122231=DIRECTION('center_axis',(0.,0.,-1.));
#122232=DIRECTION('ref_axis',(0.,1.,0.));
#122233=DIRECTION('center_axis',(0.,0.,-1.));
#122234=DIRECTION('ref_axis',(0.,1.,0.));
#122235=DIRECTION('',(0.,-1.23467863058847E-16,1.));
#122236=DIRECTION('',(0.,1.23467863058847E-16,-1.));
#122237=DIRECTION('center_axis',(0.,0.,-1.));
#122238=DIRECTION('ref_axis',(0.,1.,0.));
#122239=DIRECTION('center_axis',(0.,0.,-1.));
#122240=DIRECTION('ref_axis',(0.,1.,0.));
#122241=DIRECTION('',(0.,-1.23467863058847E-16,1.));
#122242=DIRECTION('',(0.,1.23467863058847E-16,-1.));
#122243=DIRECTION('center_axis',(0.,0.,-1.));
#122244=DIRECTION('ref_axis',(0.,1.,0.));
#122245=DIRECTION('center_axis',(0.,0.,-1.));
#122246=DIRECTION('ref_axis',(0.,1.,0.));
#122247=DIRECTION('',(0.,-1.23467863058847E-16,1.));
#122248=DIRECTION('',(0.,1.23467863058847E-16,-1.));
#122249=DIRECTION('center_axis',(0.,0.,-1.));
#122250=DIRECTION('ref_axis',(0.,1.,0.));
#122251=DIRECTION('center_axis',(0.,0.,1.));
#122252=DIRECTION('ref_axis',(0.,-1.,0.));
#122253=DIRECTION('',(0.,-1.23467863058847E-16,1.));
#122254=DIRECTION('',(0.,1.23467863058847E-16,-1.));
#122255=DIRECTION('center_axis',(0.,0.,-1.));
#122256=DIRECTION('ref_axis',(0.,1.,0.));
#122257=DIRECTION('center_axis',(0.,0.,-1.));
#122258=DIRECTION('ref_axis',(0.,1.,0.));
#122259=DIRECTION('',(0.,-1.23467863058847E-16,1.));
#122260=DIRECTION('',(0.,1.23467863058847E-16,-1.));
#122261=DIRECTION('center_axis',(0.,0.,-1.));
#122262=DIRECTION('ref_axis',(0.,1.,0.));
#122263=DIRECTION('center_axis',(0.,0.,-1.));
#122264=DIRECTION('ref_axis',(0.,1.,0.));
#122265=DIRECTION('',(0.,-1.23467863058847E-16,1.));
#122266=DIRECTION('',(0.,1.23467863058847E-16,-1.));
#122267=DIRECTION('center_axis',(0.,0.,-1.));
#122268=DIRECTION('ref_axis',(0.,1.,0.));
#122269=DIRECTION('center_axis',(0.,0.,-1.));
#122270=DIRECTION('ref_axis',(0.,1.,0.));
#122271=DIRECTION('',(0.,-1.23467863058847E-16,1.));
#122272=DIRECTION('',(0.,1.23467863058847E-16,-1.));
#122273=DIRECTION('center_axis',(0.,0.,-1.));
#122274=DIRECTION('ref_axis',(0.,1.,0.));
#122275=DIRECTION('center_axis',(0.,0.,-1.));
#122276=DIRECTION('ref_axis',(0.,1.,0.));
#122277=DIRECTION('',(0.,-1.23467863058847E-16,1.));
#122278=DIRECTION('',(0.,1.23467863058847E-16,-1.));
#122279=DIRECTION('center_axis',(0.,0.,-1.));
#122280=DIRECTION('ref_axis',(0.,1.,0.));
#122281=DIRECTION('center_axis',(0.,0.,-1.));
#122282=DIRECTION('ref_axis',(0.,1.,0.));
#122283=DIRECTION('center_axis',(0.,0.,-1.));
#122284=DIRECTION('ref_axis',(0.,1.,0.));
#122285=DIRECTION('',(0.,-1.23467863058847E-16,1.));
#122286=DIRECTION('',(0.,1.23467863058847E-16,-1.));
#122287=DIRECTION('center_axis',(0.,0.,1.));
#122288=DIRECTION('ref_axis',(0.,-1.,0.));
#122289=DIRECTION('',(0.,-1.23467863058847E-16,1.));
#122290=DIRECTION('',(0.,1.23467863058847E-16,-1.));
#122291=DIRECTION('center_axis',(0.,0.,-1.));
#122292=DIRECTION('ref_axis',(0.,1.,0.));
#122293=DIRECTION('center_axis',(0.,0.,-1.));
#122294=DIRECTION('ref_axis',(0.,1.,0.));
#122295=DIRECTION('',(0.,-1.23467863058847E-16,1.));
#122296=DIRECTION('',(0.,1.23467863058847E-16,-1.));
#122297=DIRECTION('center_axis',(0.,0.,-1.));
#122298=DIRECTION('ref_axis',(0.,1.,0.));
#122299=DIRECTION('center_axis',(0.,0.,1.));
#122300=DIRECTION('ref_axis',(0.,-1.,0.));
#122301=DIRECTION('',(0.,-1.23467863058847E-16,1.));
#122302=DIRECTION('',(0.,1.23467863058847E-16,-1.));
#122303=DIRECTION('center_axis',(0.,0.,-1.));
#122304=DIRECTION('ref_axis',(0.,1.,0.));
#122305=DIRECTION('center_axis',(-1.3684555315672E-48,0.,-1.));
#122306=DIRECTION('ref_axis',(0.,1.,0.));
#122307=DIRECTION('',(1.3684555315672E-48,-1.23467863058847E-16,1.));
#122308=DIRECTION('',(0.,1.23467863058847E-16,-1.));
#122309=DIRECTION('center_axis',(0.,0.,-1.));
#122310=DIRECTION('ref_axis',(0.,1.,0.));
#122311=DIRECTION('center_axis',(0.,0.,-1.));
#122312=DIRECTION('ref_axis',(-0.701138397908223,-0.713025207814346,0.));
#122313=DIRECTION('',(0.,-1.23467863058847E-16,1.));
#122314=DIRECTION('',(-1.3684555315672E-48,1.23467863058847E-16,-1.));
#122315=DIRECTION('center_axis',(0.,0.,-1.));
#122316=DIRECTION('ref_axis',(0.,1.,0.));
#122317=DIRECTION('center_axis',(0.,0.,1.));
#122318=DIRECTION('ref_axis',(0.,-1.,0.));
#122319=DIRECTION('',(0.,-1.23467863058847E-16,1.));
#122320=DIRECTION('',(0.,1.23467863058847E-16,-1.));
#122321=DIRECTION('center_axis',(0.,0.,-1.));
#122322=DIRECTION('ref_axis',(0.,1.,0.));
#122323=DIRECTION('center_axis',(-1.3684555315672E-48,0.,-1.));
#122324=DIRECTION('ref_axis',(0.,1.,0.));
#122325=DIRECTION('',(1.3684555315672E-48,-1.23467863058847E-16,1.));
#122326=DIRECTION('',(0.,1.23467863058847E-16,-1.));
#122327=DIRECTION('center_axis',(0.,0.,-1.));
#122328=DIRECTION('ref_axis',(0.,1.,0.));
#122329=DIRECTION('center_axis',(1.3684555315672E-48,0.,1.));
#122330=DIRECTION('ref_axis',(0.,-1.,0.));
#122331=DIRECTION('',(0.,-1.23467863058847E-16,1.));
#122332=DIRECTION('',(-1.3684555315672E-48,1.23467863058847E-16,-1.));
#122333=DIRECTION('center_axis',(0.,0.,-1.));
#122334=DIRECTION('ref_axis',(0.,1.,0.));
#122335=DIRECTION('center_axis',(0.,0.,-1.));
#122336=DIRECTION('ref_axis',(0.,1.,0.));
#122337=DIRECTION('',(0.,-1.23467863058847E-16,1.));
#122338=DIRECTION('',(0.,1.23467863058847E-16,-1.));
#122339=DIRECTION('center_axis',(0.,0.,-1.));
#122340=DIRECTION('ref_axis',(0.,1.,0.));
#122341=DIRECTION('center_axis',(0.,0.,1.));
#122342=DIRECTION('ref_axis',(0.,-1.,0.));
#122343=DIRECTION('',(0.,-1.23467863058847E-16,1.));
#122344=DIRECTION('',(0.,1.23467863058847E-16,-1.));
#122345=DIRECTION('center_axis',(0.,0.,-1.));
#122346=DIRECTION('ref_axis',(0.,1.,0.));
#122347=DIRECTION('center_axis',(-1.3684555315672E-48,0.,-1.));
#122348=DIRECTION('ref_axis',(0.,1.,0.));
#122349=DIRECTION('',(1.3684555315672E-48,-1.23467863058847E-16,1.));
#122350=DIRECTION('',(0.,1.23467863058847E-16,-1.));
#122351=DIRECTION('center_axis',(0.,0.,-1.));
#122352=DIRECTION('ref_axis',(0.,1.,0.));
#122353=DIRECTION('center_axis',(1.3684555315672E-48,0.,1.));
#122354=DIRECTION('ref_axis',(0.,-1.,0.));
#122355=DIRECTION('',(0.,-1.23467863058847E-16,1.));
#122356=DIRECTION('',(-1.3684555315672E-48,1.23467863058847E-16,-1.));
#122357=DIRECTION('center_axis',(0.,0.,-1.));
#122358=DIRECTION('ref_axis',(0.,1.,0.));
#122359=DIRECTION('center_axis',(0.,0.,-1.));
#122360=DIRECTION('ref_axis',(0.,1.,0.));
#122361=DIRECTION('',(0.,-1.23467863058847E-16,1.));
#122362=DIRECTION('',(0.,1.23467863058847E-16,-1.));
#122363=DIRECTION('center_axis',(0.,0.,-1.));
#122364=DIRECTION('ref_axis',(0.,1.,0.));
#122365=DIRECTION('center_axis',(0.,0.,1.));
#122366=DIRECTION('ref_axis',(0.,-1.,0.));
#122367=DIRECTION('',(0.,-1.23467863058847E-16,1.));
#122368=DIRECTION('',(0.,1.23467863058847E-16,-1.));
#122369=DIRECTION('center_axis',(0.,0.,-1.));
#122370=DIRECTION('ref_axis',(0.,1.,0.));
#122371=DIRECTION('center_axis',(-1.3684555315672E-48,0.,-1.));
#122372=DIRECTION('ref_axis',(0.,1.,0.));
#122373=DIRECTION('',(1.3684555315672E-48,-1.23467863058847E-16,1.));
#122374=DIRECTION('',(0.,1.23467863058847E-16,-1.));
#122375=DIRECTION('center_axis',(0.,0.,-1.));
#122376=DIRECTION('ref_axis',(0.,1.,0.));
#122377=DIRECTION('center_axis',(1.3684555315672E-48,0.,1.));
#122378=DIRECTION('ref_axis',(0.,-1.,0.));
#122379=DIRECTION('',(0.,-1.23467863058847E-16,1.));
#122380=DIRECTION('',(-1.3684555315672E-48,1.23467863058847E-16,-1.));
#122381=DIRECTION('center_axis',(0.,0.,-1.));
#122382=DIRECTION('ref_axis',(0.,1.,0.));
#122383=DIRECTION('center_axis',(0.,0.,-1.));
#122384=DIRECTION('ref_axis',(0.,1.,0.));
#122385=DIRECTION('',(0.,-1.23467863058847E-16,1.));
#122386=DIRECTION('',(0.,1.23467863058847E-16,-1.));
#122387=DIRECTION('center_axis',(0.,0.,-1.));
#122388=DIRECTION('ref_axis',(0.,1.,0.));
#122389=DIRECTION('center_axis',(0.,0.,-1.));
#122390=DIRECTION('ref_axis',(0.,1.,0.));
#122391=DIRECTION('',(0.,-1.23467863058847E-16,1.));
#122392=DIRECTION('',(0.,1.23467863058847E-16,-1.));
#122393=DIRECTION('center_axis',(0.,0.,-1.));
#122394=DIRECTION('ref_axis',(0.,1.,0.));
#122395=DIRECTION('center_axis',(0.,0.,1.));
#122396=DIRECTION('ref_axis',(0.,-1.,0.));
#122397=DIRECTION('',(0.,-1.23467863058847E-16,1.));
#122398=DIRECTION('',(0.,1.23467863058847E-16,-1.));
#122399=DIRECTION('center_axis',(0.,0.,-1.));
#122400=DIRECTION('ref_axis',(0.,1.,0.));
#122401=DIRECTION('center_axis',(-1.3684555315672E-48,0.,-1.));
#122402=DIRECTION('ref_axis',(0.,1.,0.));
#122403=DIRECTION('',(1.3684555315672E-48,-1.23467863058847E-16,1.));
#122404=DIRECTION('',(0.,1.23467863058847E-16,-1.));
#122405=DIRECTION('center_axis',(0.,0.,-1.));
#122406=DIRECTION('ref_axis',(0.,1.,0.));
#122407=DIRECTION('center_axis',(1.3684555315672E-48,0.,1.));
#122408=DIRECTION('ref_axis',(0.,-1.,0.));
#122409=DIRECTION('',(0.,-1.23467863058847E-16,1.));
#122410=DIRECTION('',(-1.3684555315672E-48,1.23467863058847E-16,-1.));
#122411=DIRECTION('center_axis',(0.,0.,-1.));
#122412=DIRECTION('ref_axis',(0.,1.,0.));
#122413=DIRECTION('center_axis',(0.,0.,-1.));
#122414=DIRECTION('ref_axis',(0.,1.,0.));
#122415=DIRECTION('',(0.,-1.23467863058847E-16,1.));
#122416=DIRECTION('',(0.,1.23467863058847E-16,-1.));
#122417=DIRECTION('center_axis',(0.,0.,-1.));
#122418=DIRECTION('ref_axis',(0.,1.,0.));
#122419=DIRECTION('center_axis',(0.,0.,-1.));
#122420=DIRECTION('ref_axis',(0.,1.,0.));
#122421=DIRECTION('',(0.,-1.23467863058847E-16,1.));
#122422=DIRECTION('',(0.,1.23467863058847E-16,-1.));
#122423=DIRECTION('center_axis',(0.,0.,-1.));
#122424=DIRECTION('ref_axis',(0.,1.,0.));
#122425=DIRECTION('center_axis',(0.,0.,-1.));
#122426=DIRECTION('ref_axis',(0.,1.,0.));
#122427=DIRECTION('center_axis',(0.,0.,-1.));
#122428=DIRECTION('ref_axis',(0.,1.,0.));
#122429=DIRECTION('',(1.3684555315672E-48,-1.23467863058847E-16,1.));
#122430=DIRECTION('',(0.,1.23467863058847E-16,-1.));
#122431=DIRECTION('center_axis',(1.3684555315672E-48,0.,1.));
#122432=DIRECTION('ref_axis',(0.,-1.,0.));
#122433=DIRECTION('',(1.3684555315672E-48,-1.23467863058847E-16,1.));
#122434=DIRECTION('',(-1.3684555315672E-48,1.23467863058847E-16,-1.));
#122435=DIRECTION('center_axis',(0.,0.,-1.));
#122436=DIRECTION('ref_axis',(0.,1.,0.));
#122437=DIRECTION('center_axis',(0.,0.,-1.));
#122438=DIRECTION('ref_axis',(0.,1.,0.));
#122439=DIRECTION('',(0.,-1.23467863058847E-16,1.));
#122440=DIRECTION('',(0.,1.23467863058847E-16,-1.));
#122441=DIRECTION('center_axis',(0.,0.,-1.));
#122442=DIRECTION('ref_axis',(0.,1.,0.));
#122443=DIRECTION('center_axis',(0.,0.,1.));
#122444=DIRECTION('ref_axis',(0.,-1.,0.));
#122445=DIRECTION('',(0.,-1.23467863058847E-16,1.));
#122446=DIRECTION('',(0.,1.23467863058847E-16,-1.));
#122447=DIRECTION('center_axis',(0.,0.,-1.));
#122448=DIRECTION('ref_axis',(0.,1.,0.));
#122449=DIRECTION('center_axis',(0.,0.,-1.));
#122450=DIRECTION('ref_axis',(0.,1.,0.));
#122451=DIRECTION('',(0.,-1.23467863058847E-16,1.));
#122452=DIRECTION('',(0.,1.23467863058847E-16,-1.));
#122453=DIRECTION('center_axis',(0.,0.,-1.));
#122454=DIRECTION('ref_axis',(0.,1.,0.));
#122455=DIRECTION('center_axis',(0.,0.,-1.));
#122456=DIRECTION('ref_axis',(-0.706453380948025,-0.707759578209369,0.));
#122457=DIRECTION('',(0.,-1.23467863058847E-16,1.));
#122458=DIRECTION('',(0.,1.23467863058847E-16,-1.));
#122459=DIRECTION('center_axis',(0.,0.,-1.));
#122460=DIRECTION('ref_axis',(0.,1.,0.));
#122461=DIRECTION('center_axis',(0.,0.,1.));
#122462=DIRECTION('ref_axis',(0.,-1.,0.));
#122463=DIRECTION('',(0.,-1.23467863058847E-16,1.));
#122464=DIRECTION('',(0.,1.23467863058847E-16,-1.));
#122465=DIRECTION('center_axis',(0.,0.,-1.));
#122466=DIRECTION('ref_axis',(0.,1.,0.));
#122467=DIRECTION('center_axis',(0.,0.,-1.));
#122468=DIRECTION('ref_axis',(0.,1.,0.));
#122469=DIRECTION('',(0.,-1.23467863058847E-16,1.));
#122470=DIRECTION('',(0.,1.23467863058847E-16,-1.));
#122471=DIRECTION('center_axis',(0.,0.,-1.));
#122472=DIRECTION('ref_axis',(0.,1.,0.));
#122473=DIRECTION('center_axis',(0.,0.,1.));
#122474=DIRECTION('ref_axis',(0.,-1.,0.));
#122475=DIRECTION('',(0.,-1.23467863058847E-16,1.));
#122476=DIRECTION('',(0.,1.23467863058847E-16,-1.));
#122477=DIRECTION('center_axis',(0.,0.,-1.));
#122478=DIRECTION('ref_axis',(0.,1.,0.));
#122479=DIRECTION('center_axis',(0.,0.,-1.));
#122480=DIRECTION('ref_axis',(0.,1.,0.));
#122481=DIRECTION('',(0.,-1.23467863058847E-16,1.));
#122482=DIRECTION('',(0.,1.23467863058847E-16,-1.));
#122483=DIRECTION('center_axis',(0.,0.,-1.));
#122484=DIRECTION('ref_axis',(0.,1.,0.));
#122485=DIRECTION('center_axis',(0.,0.,-1.));
#122486=DIRECTION('ref_axis',(0.,1.,0.));
#122487=DIRECTION('',(0.,-1.23467863058847E-16,1.));
#122488=DIRECTION('',(0.,1.23467863058847E-16,-1.));
#122489=DIRECTION('center_axis',(0.,0.,-1.));
#122490=DIRECTION('ref_axis',(0.,1.,0.));
#122491=DIRECTION('center_axis',(0.,0.,1.));
#122492=DIRECTION('ref_axis',(0.,-1.,0.));
#122493=DIRECTION('',(0.,-1.23467863058847E-16,1.));
#122494=DIRECTION('',(0.,1.23467863058847E-16,-1.));
#122495=DIRECTION('center_axis',(0.,0.,-1.));
#122496=DIRECTION('ref_axis',(0.,1.,0.));
#122497=DIRECTION('center_axis',(0.,0.,-1.));
#122498=DIRECTION('ref_axis',(0.,1.,0.));
#122499=DIRECTION('',(0.,-1.23467863058847E-16,1.));
#122500=DIRECTION('',(0.,1.23467863058847E-16,-1.));
#122501=DIRECTION('center_axis',(0.,0.,-1.));
#122502=DIRECTION('ref_axis',(0.,1.,0.));
#122503=DIRECTION('center_axis',(0.,0.,1.));
#122504=DIRECTION('ref_axis',(0.,-1.,0.));
#122505=DIRECTION('',(0.,-1.23467863058847E-16,1.));
#122506=DIRECTION('',(0.,1.23467863058847E-16,-1.));
#122507=DIRECTION('center_axis',(0.,0.,-1.));
#122508=DIRECTION('ref_axis',(0.,1.,0.));
#122509=DIRECTION('center_axis',(0.,0.,-1.));
#122510=DIRECTION('ref_axis',(0.,1.,0.));
#122511=DIRECTION('',(0.,-1.23467863058847E-16,1.));
#122512=DIRECTION('',(0.,1.23467863058847E-16,-1.));
#122513=DIRECTION('center_axis',(0.,0.,-1.));
#122514=DIRECTION('ref_axis',(0.,1.,0.));
#122515=DIRECTION('center_axis',(0.,0.,-1.));
#122516=DIRECTION('ref_axis',(0.,1.,0.));
#122517=DIRECTION('',(0.,-1.23467863058847E-16,1.));
#122518=DIRECTION('',(0.,1.23467863058847E-16,-1.));
#122519=DIRECTION('center_axis',(0.,0.,-1.));
#122520=DIRECTION('ref_axis',(0.,1.,0.));
#122521=DIRECTION('center_axis',(0.,0.,-1.));
#122522=DIRECTION('ref_axis',(0.,1.,0.));
#122523=DIRECTION('center_axis',(0.,0.,-1.));
#122524=DIRECTION('ref_axis',(0.,1.,0.));
#122525=DIRECTION('',(0.,-1.23467863058847E-16,1.));
#122526=DIRECTION('',(0.,1.23467863058847E-16,-1.));
#122527=DIRECTION('center_axis',(0.,0.,1.));
#122528=DIRECTION('ref_axis',(0.,-1.,0.));
#122529=DIRECTION('',(0.,-1.23467863058847E-16,1.));
#122530=DIRECTION('',(0.,1.23467863058847E-16,-1.));
#122531=DIRECTION('center_axis',(0.,0.,-1.));
#122532=DIRECTION('ref_axis',(0.,1.,0.));
#122533=DIRECTION('center_axis',(0.,0.,-1.));
#122534=DIRECTION('ref_axis',(0.0361435302645155,-0.999346609150208,0.));
#122535=DIRECTION('',(0.,-1.23467863058847E-16,1.));
#122536=DIRECTION('',(-1.27503726478586E-32,1.23467863058847E-16,-1.));
#122537=DIRECTION('center_axis',(0.,0.,-1.));
#122538=DIRECTION('ref_axis',(0.,1.,0.));
#122539=DIRECTION('center_axis',(0.,0.,-1.));
#122540=DIRECTION('ref_axis',(0.,1.,0.));
#122541=DIRECTION('',(0.,-1.23467863058847E-16,1.));
#122542=DIRECTION('',(0.,1.23467863058847E-16,-1.));
#122543=DIRECTION('center_axis',(0.,0.,-1.));
#122544=DIRECTION('ref_axis',(0.,1.,0.));
#122545=DIRECTION('center_axis',(0.,0.,-1.));
#122546=DIRECTION('ref_axis',(0.,1.,0.));
#122547=DIRECTION('',(0.,-1.23467863058847E-16,1.));
#122548=DIRECTION('',(0.,1.23467863058847E-16,-1.));
#122549=DIRECTION('center_axis',(0.,0.,-1.));
#122550=DIRECTION('ref_axis',(0.,1.,0.));
#122551=DIRECTION('center_axis',(0.,0.,-1.));
#122552=DIRECTION('ref_axis',(0.,1.,0.));
#122553=DIRECTION('center_axis',(0.,0.,-1.));
#122554=DIRECTION('ref_axis',(0.,1.,0.));
#122555=DIRECTION('',(0.,-1.23467863058847E-16,1.));
#122556=DIRECTION('',(0.,1.23467863058847E-16,-1.));
#122557=DIRECTION('center_axis',(0.,0.,-1.));
#122558=DIRECTION('ref_axis',(-0.663057938251906,-0.748568080084324,0.));
#122559=DIRECTION('',(0.,-1.23467863058847E-16,1.));
#122560=DIRECTION('',(0.,1.23467863058847E-16,-1.));
#122561=DIRECTION('center_axis',(0.,0.,-1.));
#122562=DIRECTION('ref_axis',(0.,1.,0.));
#122563=DIRECTION('center_axis',(0.,0.,-1.));
#122564=DIRECTION('ref_axis',(0.,1.,0.));
#122565=DIRECTION('center_axis',(0.,0.,-1.));
#122566=DIRECTION('ref_axis',(0.,1.,0.));
#122567=DIRECTION('',(0.,-1.23467863058847E-16,1.));
#122568=DIRECTION('',(0.,1.23467863058847E-16,-1.));
#122569=DIRECTION('center_axis',(0.,0.,-1.));
#122570=DIRECTION('ref_axis',(0.,1.,0.));
#122571=DIRECTION('',(3.82498197630791E-33,-1.23467863058847E-16,1.));
#122572=DIRECTION('',(0.,1.23467863058847E-16,-1.));
#122573=DIRECTION('center_axis',(0.,0.,-1.));
#122574=DIRECTION('ref_axis',(0.,1.,0.));
#122575=DIRECTION('center_axis',(0.,0.,-1.));
#122576=DIRECTION('ref_axis',(0.,1.,0.));
#122577=DIRECTION('',(0.,-1.23467863058847E-16,1.));
#122578=DIRECTION('',(-1.3684555315672E-48,1.23467863058847E-16,-1.));
#122579=DIRECTION('center_axis',(0.,0.,-1.));
#122580=DIRECTION('ref_axis',(0.,1.,0.));
#122581=DIRECTION('center_axis',(0.,0.,-1.));
#122582=DIRECTION('ref_axis',(0.,1.,0.));
#122583=DIRECTION('',(1.3684555315672E-48,-1.23467863058847E-16,1.));
#122584=DIRECTION('',(0.,1.23467863058847E-16,-1.));
#122585=DIRECTION('center_axis',(0.,0.,-1.));
#122586=DIRECTION('ref_axis',(0.,1.,0.));
#122587=DIRECTION('center_axis',(0.,0.,-1.));
#122588=DIRECTION('ref_axis',(0.,1.,0.));
#122589=DIRECTION('',(0.,-1.23467863058847E-16,1.));
#122590=DIRECTION('center_axis',(0.,0.,-1.));
#122591=DIRECTION('ref_axis',(0.,1.,0.));
#122592=DIRECTION('center_axis',(0.,0.,-1.));
#122593=DIRECTION('ref_axis',(0.,1.,0.));
#122594=DIRECTION('',(0.,1.23467863058847E-16,-1.));
#122595=DIRECTION('center_axis',(0.,0.,-1.));
#122596=DIRECTION('ref_axis',(0.,1.,0.));
#122597=DIRECTION('center_axis',(0.,1.23467863058847E-16,-1.));
#122598=DIRECTION('ref_axis',(-1.,0.,0.));
#122599=DIRECTION('center_axis',(0.,0.,-1.));
#122600=DIRECTION('ref_axis',(0.,1.,0.));
#122601=DIRECTION('center_axis',(0.,0.,-1.));
#122602=DIRECTION('ref_axis',(0.,1.,0.));
#122603=DIRECTION('',(0.,0.,-1.));
#122604=DIRECTION('center_axis',(0.,1.23467863058847E-16,-1.));
#122605=DIRECTION('ref_axis',(-1.,0.,0.));
#122606=DIRECTION('center_axis',(0.,0.,-1.));
#122607=DIRECTION('ref_axis',(0.,1.,0.));
#122608=DIRECTION('center_axis',(0.,0.,1.));
#122609=DIRECTION('ref_axis',(0.,1.,0.));
#122610=DIRECTION('center_axis',(0.,0.,-1.));
#122611=DIRECTION('ref_axis',(0.,1.,0.));
#122612=DIRECTION('center_axis',(-5.48307457476793E-31,-2.43497425545765E-45,
1.));
#122613=DIRECTION('ref_axis',(-4.44089209850063E-15,1.,-3.42265840282363E-60));
#122614=DIRECTION('center_axis',(0.,0.,-1.));
#122615=DIRECTION('ref_axis',(0.,1.,0.));
#122616=DIRECTION('',(0.,0.,1.));
#122617=DIRECTION('center_axis',(0.,0.,-1.));
#122618=DIRECTION('ref_axis',(0.,1.,0.));
#122619=DIRECTION('center_axis',(0.,0.,-1.));
#122620=DIRECTION('ref_axis',(0.,1.,0.));
#122621=DIRECTION('center_axis',(0.,0.,1.));
#122622=DIRECTION('ref_axis',(0.,1.,0.));
#122623=DIRECTION('center_axis',(0.,0.,-1.));
#122624=DIRECTION('ref_axis',(0.,1.,0.));
#122625=DIRECTION('center_axis',(0.,0.,1.));
#122626=DIRECTION('ref_axis',(0.,1.,0.));
#122627=DIRECTION('center_axis',(-6.57968948972152E-31,3.50636292785902E-45,
-1.));
#122628=DIRECTION('ref_axis',(5.32907051820075E-15,1.,-4.97841222228891E-60));
#122629=DIRECTION('center_axis',(0.,0.,1.));
#122630=DIRECTION('ref_axis',(0.,1.,0.));
#122631=DIRECTION('center_axis',(7.6763044046751E-31,4.77254954069701E-45,
-1.));
#122632=DIRECTION('ref_axis',(-6.21724893790088E-15,1.,-2.48920611114446E-60));
#122633=DIRECTION('center_axis',(0.,0.,-1.));
#122634=DIRECTION('ref_axis',(0.,1.,0.));
#122635=DIRECTION('center_axis',(7.6763044046751E-31,-4.77254954069701E-45,
1.));
#122636=DIRECTION('ref_axis',(6.21724893790088E-15,1.,-2.48920611114446E-60));
#122637=DIRECTION('center_axis',(0.,0.,-1.));
#122638=DIRECTION('ref_axis',(0.,1.,0.));
#122639=DIRECTION('center_axis',(-6.57968948972152E-31,-3.50636292785902E-45,
1.));
#122640=DIRECTION('ref_axis',(-5.32907051820075E-15,1.,-4.97841222228891E-60));
#122641=DIRECTION('center_axis',(0.,0.,-1.));
#122642=DIRECTION('ref_axis',(0.,1.,0.));
#122643=DIRECTION('center_axis',(0.,0.,1.));
#122644=DIRECTION('ref_axis',(0.,1.,0.));
#122645=DIRECTION('center_axis',(0.,0.,-1.));
#122646=DIRECTION('ref_axis',(0.,1.,0.));
#122647=DIRECTION('center_axis',(0.,0.,1.));
#122648=DIRECTION('ref_axis',(0.,1.,0.));
#122649=DIRECTION('center_axis',(0.,0.,-1.));
#122650=DIRECTION('ref_axis',(0.,1.,0.));
#122651=DIRECTION('center_axis',(0.,0.,-1.));
#122652=DIRECTION('ref_axis',(0.,1.,0.));
#122653=DIRECTION('center_axis',(0.,0.,1.));
#122654=DIRECTION('ref_axis',(0.,1.,0.));
#122655=DIRECTION('center_axis',(0.724113717892013,0.689680595319751,8.51533892972834E-17));
#122656=DIRECTION('ref_axis',(-4.33608168928332E-33,1.23467863058847E-16,
-1.));
#122657=DIRECTION('',(-0.689680595319751,0.724113717892013,8.9404773359724E-17));
#122658=DIRECTION('center_axis',(-0.724113717892013,-0.689680595319751,
-8.51533892972834E-17));
#122659=DIRECTION('ref_axis',(-0.689680595319751,0.724113717892013,-2.49214163614276E-33));
#122660=DIRECTION('',(0.689680595319751,-0.724113717892013,-8.9404773359724E-17));
#122661=DIRECTION('center_axis',(0.,0.,-1.));
#122662=DIRECTION('ref_axis',(0.,1.,0.));
#122663=DIRECTION('center_axis',(2.19322982990717E-31,-3.89595880873225E-46,
1.));
#122664=DIRECTION('ref_axis',(1.77635683940025E-15,1.,7.77876909732643E-62));
#122665=DIRECTION('center_axis',(0.,0.,-1.));
#122666=DIRECTION('ref_axis',(0.,1.,0.));
#122667=DIRECTION('center_axis',(-4.38645965981435E-31,-1.5583835234929E-45,
1.));
#122668=DIRECTION('ref_axis',(-3.5527136788005E-15,1.,-9.33452291679171E-61));
#122669=DIRECTION('center_axis',(0.,0.,-1.));
#122670=DIRECTION('ref_axis',(0.,1.,0.));
#122671=DIRECTION('center_axis',(7.6763044046751E-31,-4.77254954069701E-45,
1.));
#122672=DIRECTION('ref_axis',(6.21724893790088E-15,1.,-1.86690458335834E-60));
#122673=DIRECTION('center_axis',(-0.724113717892013,0.689680595319752,8.51533892972836E-17));
#122674=DIRECTION('ref_axis',(1.17596707800504E-16,1.43114502276974E-33,
1.));
#122675=DIRECTION('',(-0.689680595319752,-0.724113717892012,-8.94047733597238E-17));
#122676=DIRECTION('center_axis',(0.724113717892013,-0.689680595319752,-8.51533892972834E-17));
#122677=DIRECTION('ref_axis',(-1.94663562866425E-33,1.23467863058847E-16,
-1.));
#122678=DIRECTION('',(0.689680595319752,0.724113717892012,8.94047733597238E-17));
#122679=DIRECTION('center_axis',(0.,0.,-1.));
#122680=DIRECTION('ref_axis',(0.,1.,0.));
#122681=DIRECTION('center_axis',(-1.09661491495359E-31,-9.73989702183063E-47,
1.));
#122682=DIRECTION('ref_axis',(-8.88178419700125E-16,1.,0.));
#122683=DIRECTION('center_axis',(0.,0.,-1.));
#122684=DIRECTION('ref_axis',(0.,1.,0.));
#122685=DIRECTION('center_axis',(-9.86953423458227E-31,-7.88931658768281E-45,
1.));
#122686=DIRECTION('ref_axis',(-7.99360577730113E-15,1.,-2.48920611114446E-60));
#122687=DIRECTION('center_axis',(1.,0.,0.));
#122688=DIRECTION('ref_axis',(0.,1.,0.));
#122689=DIRECTION('',(0.,1.,0.));
#122690=DIRECTION('center_axis',(-1.,0.,0.));
#122691=DIRECTION('ref_axis',(0.,0.,1.));
#122692=DIRECTION('',(0.,-1.,0.));
#122693=DIRECTION('center_axis',(-1.,0.,0.));
#122694=DIRECTION('ref_axis',(0.,0.,1.));
#122695=DIRECTION('',(0.,-1.,0.));
#122696=DIRECTION('center_axis',(1.,0.,0.));
#122697=DIRECTION('ref_axis',(0.,1.,0.));
#122698=DIRECTION('',(0.,1.,0.));
#122699=DIRECTION('center_axis',(-1.,0.,0.));
#122700=DIRECTION('ref_axis',(0.,0.,1.));
#122701=DIRECTION('',(0.,-1.,0.));
#122702=DIRECTION('center_axis',(1.,0.,0.));
#122703=DIRECTION('ref_axis',(0.,1.,0.));
#122704=DIRECTION('',(0.,1.,0.));
#122705=DIRECTION('center_axis',(-1.,0.,0.));
#122706=DIRECTION('ref_axis',(0.,0.,1.));
#122707=DIRECTION('',(0.,-1.,0.));
#122708=DIRECTION('center_axis',(1.,0.,0.));
#122709=DIRECTION('ref_axis',(0.,1.,0.));
#122710=DIRECTION('',(0.,1.,0.));
#122711=DIRECTION('center_axis',(-1.,0.,0.));
#122712=DIRECTION('ref_axis',(0.,0.,1.));
#122713=DIRECTION('',(0.,-1.,0.));
#122714=DIRECTION('center_axis',(1.,0.,0.));
#122715=DIRECTION('ref_axis',(0.,1.,0.));
#122716=DIRECTION('',(0.,1.,0.));
#122717=DIRECTION('center_axis',(-1.,0.,0.));
#122718=DIRECTION('ref_axis',(0.,0.,1.));
#122719=DIRECTION('',(0.,-1.,0.));
#122720=DIRECTION('center_axis',(1.,0.,0.));
#122721=DIRECTION('ref_axis',(0.,1.,0.));
#122722=DIRECTION('',(0.,1.,0.));
#122723=DIRECTION('center_axis',(-1.,0.,0.));
#122724=DIRECTION('ref_axis',(0.,0.,1.));
#122725=DIRECTION('',(0.,-1.,0.));
#122726=DIRECTION('center_axis',(1.,0.,0.));
#122727=DIRECTION('ref_axis',(0.,1.,0.));
#122728=DIRECTION('',(0.,1.,0.));
#122729=DIRECTION('center_axis',(-1.,0.,0.));
#122730=DIRECTION('ref_axis',(0.,0.,1.));
#122731=DIRECTION('',(0.,-1.,0.));
#122732=DIRECTION('center_axis',(1.,0.,0.));
#122733=DIRECTION('ref_axis',(0.,1.,0.));
#122734=DIRECTION('',(0.,1.,0.));
#122735=DIRECTION('center_axis',(1.,7.82779334765923E-17,9.66480917101747E-33));
#122736=DIRECTION('ref_axis',(-7.82779334765923E-17,1.,1.39213059235047E-65));
#122737=DIRECTION('',(-7.82779334765923E-17,1.,0.));
#122738=DIRECTION('center_axis',(-1.,7.82779334765923E-17,9.66480917101747E-33));
#122739=DIRECTION('ref_axis',(9.66480917101747E-33,0.,1.));
#122740=DIRECTION('',(-7.82779334765923E-17,-1.,0.));
#122741=DIRECTION('center_axis',(-1.,7.82779334765923E-17,9.66480917101747E-33));
#122742=DIRECTION('ref_axis',(9.66480917101747E-33,0.,1.));
#122743=DIRECTION('',(-7.82779334765923E-17,-1.,0.));
#122744=DIRECTION('center_axis',(1.,7.82779334765923E-17,9.66480917101747E-33));
#122745=DIRECTION('ref_axis',(-7.82779334765923E-17,1.,1.39213059235047E-65));
#122746=DIRECTION('',(-7.82779334765923E-17,1.,0.));
#122747=DIRECTION('center_axis',(-1.,7.82779334765923E-17,9.66480917101747E-33));
#122748=DIRECTION('ref_axis',(9.66480917101747E-33,0.,1.));
#122749=DIRECTION('',(-7.82779334765923E-17,-1.,0.));
#122750=DIRECTION('center_axis',(1.,7.82779334765923E-17,9.66480917101747E-33));
#122751=DIRECTION('ref_axis',(-7.82779334765923E-17,1.,1.39213059235047E-65));
#122752=DIRECTION('',(-7.82779334765923E-17,1.,0.));
#122753=DIRECTION('center_axis',(-1.,7.82779334765923E-17,9.66480917101747E-33));
#122754=DIRECTION('ref_axis',(9.66480917101747E-33,0.,1.));
#122755=DIRECTION('',(-7.82779334765923E-17,-1.,0.));
#122756=DIRECTION('center_axis',(1.,7.82779334765923E-17,9.66480917101747E-33));
#122757=DIRECTION('ref_axis',(-7.82779334765923E-17,1.,1.39213059235047E-65));
#122758=DIRECTION('',(-7.82779334765923E-17,1.,0.));
#122759=DIRECTION('center_axis',(-1.,7.82779334765923E-17,9.66480917101747E-33));
#122760=DIRECTION('ref_axis',(9.66480917101747E-33,0.,1.));
#122761=DIRECTION('',(-7.82779334765923E-17,-1.,0.));
#122762=DIRECTION('center_axis',(1.,7.82779334765923E-17,9.66480917101747E-33));
#122763=DIRECTION('ref_axis',(-7.82779334765923E-17,1.,1.39213059235047E-65));
#122764=DIRECTION('',(-7.82779334765923E-17,1.,0.));
#122765=DIRECTION('center_axis',(-1.,7.82779334765923E-17,9.66480917101747E-33));
#122766=DIRECTION('ref_axis',(9.66480917101747E-33,0.,1.));
#122767=DIRECTION('',(-7.82779334765923E-17,-1.,0.));
#122768=DIRECTION('center_axis',(1.,7.82779334765923E-17,9.66480917101747E-33));
#122769=DIRECTION('ref_axis',(-7.82779334765923E-17,1.,1.39213059235047E-65));
#122770=DIRECTION('',(-7.82779334765923E-17,1.,0.));
#122771=DIRECTION('center_axis',(-1.,7.82779334765923E-17,9.66480917101747E-33));
#122772=DIRECTION('ref_axis',(9.66480917101747E-33,0.,1.));
#122773=DIRECTION('',(-7.82779334765923E-17,-1.,0.));
#122774=DIRECTION('center_axis',(1.,7.82779334765923E-17,9.66480917101747E-33));
#122775=DIRECTION('ref_axis',(-7.82779334765923E-17,1.,1.39213059235047E-65));
#122776=DIRECTION('',(-7.82779334765923E-17,1.,0.));
#122777=DIRECTION('center_axis',(-1.,7.82779334765923E-17,9.66480917101747E-33));
#122778=DIRECTION('ref_axis',(9.66480917101747E-33,0.,1.));
#122779=DIRECTION('',(-7.82779334765923E-17,-1.,0.));
#122780=DIRECTION('center_axis',(1.,7.82779334765923E-17,9.66480917101747E-33));
#122781=DIRECTION('ref_axis',(-7.82779334765923E-17,1.,1.39213059235047E-65));
#122782=DIRECTION('',(-7.82779334765923E-17,1.,0.));
#122783=DIRECTION('center_axis',(0.,-1.,-1.23467863058847E-16));
#122784=DIRECTION('ref_axis',(0.,1.23467863058847E-16,-1.));
#122785=DIRECTION('',(0.,-1.23467863058847E-16,1.));
#122786=DIRECTION('',(-1.,0.,0.));
#122787=DIRECTION('',(0.,-1.23467863058847E-16,1.));
#122788=DIRECTION('',(1.,0.,0.));
#122789=DIRECTION('center_axis',(-1.,7.82779334765923E-17,9.66480917101747E-33));
#122790=DIRECTION('ref_axis',(9.66480917101747E-33,0.,1.));
#122791=DIRECTION('',(0.,-1.23467863058847E-16,1.));
#122792=DIRECTION('',(7.82779334765923E-17,1.,1.23467863058847E-16));
#122793=DIRECTION('',(-7.82779334765923E-17,-1.,0.));
#122794=DIRECTION('center_axis',(1.,7.82779334765923E-17,9.66480917101747E-33));
#122795=DIRECTION('ref_axis',(-7.82779334765923E-17,1.,1.39213059235047E-65));
#122796=DIRECTION('',(7.82779334765923E-17,-1.,-1.23467863058847E-16));
#122797=DIRECTION('',(0.,1.23467863058847E-16,-1.));
#122798=DIRECTION('',(-7.82779334765923E-17,1.,0.));
#122799=DIRECTION('center_axis',(1.,-3.13111733906369E-16,-3.86592366840699E-32));
#122800=DIRECTION('ref_axis',(-3.13111733906369E-16,-1.,-9.91259258008946E-64));
#122801=DIRECTION('',(3.13111733906369E-16,1.,0.));
#122802=DIRECTION('center_axis',(-1.,5.87084501074442E-17,7.2486068782631E-33));
#122803=DIRECTION('ref_axis',(7.2486068782631E-33,0.,1.));
#122804=DIRECTION('',(-5.87084501074442E-17,-1.,0.));
#122805=DIRECTION('center_axis',(-1.,5.87084501074442E-17,7.2486068782631E-33));
#122806=DIRECTION('ref_axis',(7.2486068782631E-33,0.,1.));
#122807=DIRECTION('',(-5.87084501074442E-17,-1.,0.));
#122808=DIRECTION('center_axis',(1.,-3.13111733906369E-16,-3.86592366840699E-32));
#122809=DIRECTION('ref_axis',(-3.13111733906369E-16,-1.,-9.91259258008946E-64));
#122810=DIRECTION('',(3.13111733906369E-16,1.,0.));
#122811=DIRECTION('center_axis',(-1.,5.87084501074442E-17,7.2486068782631E-33));
#122812=DIRECTION('ref_axis',(7.2486068782631E-33,0.,1.));
#122813=DIRECTION('',(-5.87084501074442E-17,-1.,0.));
#122814=DIRECTION('center_axis',(1.,-3.13111733906369E-16,-3.86592366840699E-32));
#122815=DIRECTION('ref_axis',(-3.13111733906369E-16,-1.,-9.91259258008946E-64));
#122816=DIRECTION('',(3.13111733906369E-16,1.,0.));
#122817=DIRECTION('center_axis',(-1.,5.87084501074442E-17,7.2486068782631E-33));
#122818=DIRECTION('ref_axis',(7.2486068782631E-33,0.,1.));
#122819=DIRECTION('',(-5.87084501074442E-17,-1.,0.));
#122820=DIRECTION('center_axis',(1.,-3.13111733906369E-16,-3.86592366840699E-32));
#122821=DIRECTION('ref_axis',(-3.13111733906369E-16,-1.,-9.91259258008946E-64));
#122822=DIRECTION('',(3.13111733906369E-16,1.,0.));
#122823=DIRECTION('center_axis',(-1.,5.87084501074442E-17,7.2486068782631E-33));
#122824=DIRECTION('ref_axis',(7.2486068782631E-33,0.,1.));
#122825=DIRECTION('',(-5.87084501074442E-17,-1.,0.));
#122826=DIRECTION('center_axis',(-1.,5.87084501074442E-17,7.2486068782631E-33));
#122827=DIRECTION('ref_axis',(7.2486068782631E-33,0.,1.));
#122828=DIRECTION('',(-5.87084501074442E-17,-1.,0.));
#122829=DIRECTION('center_axis',(-1.,5.87084501074442E-17,7.2486068782631E-33));
#122830=DIRECTION('ref_axis',(7.2486068782631E-33,0.,1.));
#122831=DIRECTION('',(-5.87084501074442E-17,-1.,0.));
#122832=DIRECTION('center_axis',(1.,-3.13111733906369E-16,-3.86592366840699E-32));
#122833=DIRECTION('ref_axis',(-3.13111733906369E-16,-1.,-9.91259258008946E-64));
#122834=DIRECTION('',(3.13111733906369E-16,1.,0.));
#122835=DIRECTION('center_axis',(-1.,5.87084501074442E-17,7.2486068782631E-33));
#122836=DIRECTION('ref_axis',(7.2486068782631E-33,0.,1.));
#122837=DIRECTION('',(-5.87084501074442E-17,-1.,0.));
#122838=DIRECTION('center_axis',(1.,-3.13111733906369E-16,-3.86592366840699E-32));
#122839=DIRECTION('ref_axis',(-3.13111733906369E-16,-1.,-9.91259258008946E-64));
#122840=DIRECTION('',(3.13111733906369E-16,1.,0.));
#122841=DIRECTION('center_axis',(-1.,6.11546355285877E-17,7.5506321648574E-33));
#122842=DIRECTION('ref_axis',(7.5506321648574E-33,0.,1.));
#122843=DIRECTION('',(-6.11546355285877E-17,-1.,0.));
#122844=DIRECTION('center_axis',(-1.,6.11546355285877E-17,7.5506321648574E-33));
#122845=DIRECTION('ref_axis',(7.5506321648574E-33,0.,1.));
#122846=DIRECTION('',(-6.11546355285877E-17,-1.,0.));
#122847=DIRECTION('center_axis',(-1.,6.11546355285877E-17,7.5506321648574E-33));
#122848=DIRECTION('ref_axis',(7.5506321648574E-33,0.,1.));
#122849=DIRECTION('',(-6.11546355285877E-17,-1.,0.));
#122850=DIRECTION('center_axis',(-1.,6.11546355285877E-17,7.5506321648574E-33));
#122851=DIRECTION('ref_axis',(7.5506321648574E-33,0.,1.));
#122852=DIRECTION('',(-6.11546355285877E-17,-1.,0.));
#122853=DIRECTION('center_axis',(-1.,6.11546355285877E-17,7.5506321648574E-33));
#122854=DIRECTION('ref_axis',(7.5506321648574E-33,0.,1.));
#122855=DIRECTION('',(-6.11546355285877E-17,-1.,0.));
#122856=DIRECTION('center_axis',(-1.,6.11546355285877E-17,7.5506321648574E-33));
#122857=DIRECTION('ref_axis',(7.5506321648574E-33,0.,1.));
#122858=DIRECTION('',(-6.11546355285877E-17,-1.,0.));
#122859=DIRECTION('center_axis',(-1.,6.11546355285877E-17,7.5506321648574E-33));
#122860=DIRECTION('ref_axis',(7.5506321648574E-33,0.,1.));
#122861=DIRECTION('',(-6.11546355285877E-17,-1.,0.));
#122862=DIRECTION('center_axis',(-1.,6.11546355285877E-17,7.5506321648574E-33));
#122863=DIRECTION('ref_axis',(7.5506321648574E-33,0.,1.));
#122864=DIRECTION('',(-6.11546355285877E-17,-1.,0.));
#122865=DIRECTION('center_axis',(0.,1.23467863058847E-16,-1.));
#122866=DIRECTION('ref_axis',(-1.,0.,0.));
#122867=DIRECTION('center_axis',(0.,1.34087697701688E-16,-1.));
#122868=DIRECTION('ref_axis',(0.,1.,1.34087697701688E-16));
#122869=DIRECTION('center_axis',(0.,1.22462808028055E-16,-1.));
#122870=DIRECTION('ref_axis',(0.,1.,1.22462808028055E-16));
#122871=DIRECTION('center_axis',(0.,0.,-1.));
#122872=DIRECTION('ref_axis',(0.,1.,0.));
#122873=DIRECTION('center_axis',(0.,0.,-1.));
#122874=DIRECTION('ref_axis',(0.,1.,0.));
#122875=DIRECTION('center_axis',(0.,0.,-1.));
#122876=DIRECTION('ref_axis',(0.,1.,0.));
#122877=DIRECTION('center_axis',(0.,1.22462808028055E-16,-1.));
#122878=DIRECTION('ref_axis',(0.,1.,1.22462808028055E-16));
#122879=DIRECTION('center_axis',(0.,0.,-1.));
#122880=DIRECTION('ref_axis',(0.,1.,0.));
#122881=DIRECTION('center_axis',(0.,0.,-1.));
#122882=DIRECTION('ref_axis',(0.,1.,0.));
#122883=DIRECTION('center_axis',(0.,0.,-1.));
#122884=DIRECTION('ref_axis',(0.,1.,0.));
#122885=DIRECTION('center_axis',(0.,1.34087697701688E-16,-1.));
#122886=DIRECTION('ref_axis',(0.,1.,1.34087697701688E-16));
#122887=DIRECTION('center_axis',(0.,1.22914743790472E-16,-1.));
#122888=DIRECTION('ref_axis',(0.,1.,1.22914743790472E-16));
#122889=DIRECTION('',(-1.,-1.90750687963558E-16,0.));
#122890=DIRECTION('',(-1.,4.76876719908896E-16,0.));
#122891=DIRECTION('',(1.,-1.23706245878324E-16,0.));
#122892=DIRECTION('',(-1.,-1.23706245878324E-16,0.));
#122893=DIRECTION('',(1.,3.71118737634973E-16,0.));
#122894=DIRECTION('',(-1.,3.29883322342198E-16,0.));
#122895=DIRECTION('',(1.,3.29883322342202E-16,0.));
#122896=DIRECTION('',(1.,5.72252063890675E-16,0.));
#122897=DIRECTION('',(-1.,3.29883322342202E-16,0.));
#122898=DIRECTION('center_axis',(0.,1.35726946151947E-16,-1.));
#122899=DIRECTION('ref_axis',(0.,1.,1.35726946151947E-16));
#122900=DIRECTION('',(1.,-9.53753439817791E-17,0.));
#122901=DIRECTION('center_axis',(0.,1.35726946151947E-16,-1.));
#122902=DIRECTION('ref_axis',(0.,1.,1.35726946151947E-16));
#122903=DIRECTION('',(1.,-9.53753439817791E-17,0.));
#122904=DIRECTION('',(1.,5.72252063890675E-16,0.));
#122905=DIRECTION('',(-1.,3.29883322342202E-16,0.));
#122906=DIRECTION('',(-1.,4.76876719908896E-16,0.));
#122907=DIRECTION('',(1.,-1.23706245878324E-16,0.));
#122908=DIRECTION('center_axis',(0.,1.22914743790472E-16,-1.));
#122909=DIRECTION('ref_axis',(0.,1.,1.22914743790472E-16));
#122910=DIRECTION('',(-1.,-1.90750687963558E-16,0.));
#122911=DIRECTION('',(1.,-9.53753439817791E-17,0.));
#122912=DIRECTION('center_axis',(0.,1.35726946151947E-16,-1.));
#122913=DIRECTION('ref_axis',(0.,1.,1.35726946151947E-16));
#122914=DIRECTION('center_axis',(0.,0.,-1.));
#122915=DIRECTION('ref_axis',(0.,1.,0.));
#122916=DIRECTION('center_axis',(0.,0.,-1.));
#122917=DIRECTION('ref_axis',(0.,1.,0.));
#122918=DIRECTION('',(1.,-1.23706245878324E-16,0.));
#122919=DIRECTION('',(-1.,4.76876719908896E-16,0.));
#122920=DIRECTION('center_axis',(0.,0.,-1.));
#122921=DIRECTION('ref_axis',(0.,1.,0.));
#122922=DIRECTION('center_axis',(0.,0.,-1.));
#122923=DIRECTION('ref_axis',(0.,1.,0.));
#122924=DIRECTION('center_axis',(0.,1.22914743790472E-16,-1.));
#122925=DIRECTION('ref_axis',(0.,1.,1.22914743790472E-16));
#122926=DIRECTION('',(1.,3.71118737634973E-16,0.));
#122927=DIRECTION('',(-1.,-1.23706245878324E-16,0.));
#122928=DIRECTION('center_axis',(0.,1.22914743790472E-16,-1.));
#122929=DIRECTION('ref_axis',(0.,1.,1.22914743790472E-16));
#122930=DIRECTION('',(1.,3.71118737634973E-16,0.));
#122931=DIRECTION('',(-1.,3.71118737634973E-16,0.));
#122932=DIRECTION('center_axis',(0.,1.22914743790472E-16,-1.));
#122933=DIRECTION('ref_axis',(0.,1.,1.22914743790472E-16));
#122934=DIRECTION('',(1.,3.29883322342198E-16,0.));
#122935=DIRECTION('',(-1.,3.71118737634973E-16,0.));
#122936=DIRECTION('center_axis',(0.,1.22914743790472E-16,-1.));
#122937=DIRECTION('ref_axis',(0.,1.,1.22914743790472E-16));
#122938=DIRECTION('',(1.,3.29883322342202E-16,0.));
#122939=DIRECTION('',(-1.,3.29883322342198E-16,0.));
#122940=DIRECTION('center_axis',(0.,1.22914743790472E-16,-1.));
#122941=DIRECTION('ref_axis',(0.,1.,1.22914743790472E-16));
#122942=DIRECTION('',(1.,5.72252063890675E-16,0.));
#122943=DIRECTION('',(-1.,3.29883322342202E-16,0.));
#122944=DIRECTION('',(-1.,-1.90750687963558E-16,0.));
#122945=DIRECTION('center_axis',(0.,0.,-1.));
#122946=DIRECTION('ref_axis',(0.,1.,0.));
#122947=DIRECTION('',(-1.,3.29883322342198E-16,0.));
#122948=DIRECTION('',(1.,3.29883322342202E-16,0.));
#122949=DIRECTION('',(-1.,3.71118737634973E-16,0.));
#122950=DIRECTION('',(1.,3.29883322342198E-16,0.));
#122951=DIRECTION('',(-1.,3.71118737634973E-16,0.));
#122952=DIRECTION('',(1.,3.71118737634973E-16,0.));
#122953=DIRECTION('',(1.,5.72252063890675E-16,0.));
#122954=DIRECTION('',(-1.,3.29883322342202E-16,0.));
#122955=DIRECTION('center_axis',(0.,1.22914743790472E-16,-1.));
#122956=DIRECTION('ref_axis',(0.,1.,1.22914743790472E-16));
#122957=DIRECTION('center_axis',(0.,0.,-1.));
#122958=DIRECTION('ref_axis',(0.,1.,0.));
#122959=DIRECTION('center_axis',(0.,0.,-1.));
#122960=DIRECTION('ref_axis',(0.,1.,0.));
#122961=DIRECTION('',(-1.,-1.90750687963558E-16,0.));
#122962=DIRECTION('center_axis',(0.,0.,-1.));
#122963=DIRECTION('ref_axis',(0.,1.,0.));
#122964=DIRECTION('center_axis',(0.,0.,-1.));
#122965=DIRECTION('ref_axis',(0.,1.,0.));
#122966=DIRECTION('center_axis',(0.,1.22914743790472E-16,-1.));
#122967=DIRECTION('ref_axis',(0.,1.,1.22914743790472E-16));
#122968=DIRECTION('',(-1.,-1.23706245878324E-16,0.));
#122969=DIRECTION('',(1.,3.71118737634973E-16,0.));
#122970=DIRECTION('',(-1.,4.76876719908896E-16,0.));
#122971=DIRECTION('',(1.,-1.23706245878324E-16,0.));
#122972=DIRECTION('',(1.,-9.53753439817791E-17,0.));
#122973=DIRECTION('center_axis',(0.,0.,-1.));
#122974=DIRECTION('ref_axis',(0.,1.,0.));
#122975=DIRECTION('',(1.,3.71118737634973E-16,0.));
#122976=DIRECTION('',(-1.,3.71118737634973E-16,0.));
#122977=DIRECTION('',(1.,3.29883322342202E-16,0.));
#122978=DIRECTION('',(-1.,3.71118737634973E-16,0.));
#122979=DIRECTION('',(-1.,-1.23706245878324E-16,0.));
#122980=DIRECTION('',(1.,3.71118737634973E-16,0.));
#122981=DIRECTION('',(-1.,3.71118737634973E-16,0.));
#122982=DIRECTION('',(1.,3.29883322342198E-16,0.));
#122983=DIRECTION('center_axis',(0.,0.,-1.));
#122984=DIRECTION('ref_axis',(0.,1.,0.));
#122985=DIRECTION('',(0.,1.23467863058847E-16,-1.));
#122986=DIRECTION('',(0.,1.23467863058847E-16,-1.));
#122987=DIRECTION('center_axis',(0.,0.,-1.));
#122988=DIRECTION('ref_axis',(0.,1.,0.));
#122989=DIRECTION('center_axis',(0.,0.,-1.));
#122990=DIRECTION('ref_axis',(0.,1.,0.));
#122991=DIRECTION('center_axis',(-2.19322982990717E-31,-3.89595880873225E-46,
1.));
#122992=DIRECTION('ref_axis',(-1.77635683940025E-15,1.,1.55575381946529E-61));
#122993=DIRECTION('',(0.,1.23467863058847E-16,-1.));
#122994=DIRECTION('center_axis',(0.,0.,-1.));
#122995=DIRECTION('ref_axis',(0.,1.,0.));
#122996=DIRECTION('',(0.,1.23467863058847E-16,-1.));
#122997=DIRECTION('center_axis',(0.,0.,-1.));
#122998=DIRECTION('ref_axis',(0.,1.,0.));
#122999=DIRECTION('center_axis',(0.,1.22462808028055E-16,-1.));
#123000=DIRECTION('ref_axis',(0.,1.,1.22462808028055E-16));
#123001=DIRECTION('',(0.,1.23467863058847E-16,-1.));
#123002=DIRECTION('center_axis',(0.,1.22462808028055E-16,-1.));
#123003=DIRECTION('ref_axis',(0.,1.,1.22462808028055E-16));
#123004=DIRECTION('center_axis',(0.,0.,-1.));
#123005=DIRECTION('ref_axis',(0.,1.,0.));
#123006=DIRECTION('',(0.,1.23467863058847E-16,-1.));
#123007=DIRECTION('center_axis',(0.,0.,-1.));
#123008=DIRECTION('ref_axis',(0.,1.,0.));
#123009=DIRECTION('center_axis',(0.,0.,-1.));
#123010=DIRECTION('ref_axis',(0.,1.,0.));
#123011=DIRECTION('center_axis',(4.38645965981435E-31,-1.5583835234929E-45,
1.));
#123012=DIRECTION('ref_axis',(3.5527136788005E-15,1.,-9.33452291679171E-61));
#123013=DIRECTION('',(0.,1.23467863058847E-16,-1.));
#123014=DIRECTION('center_axis',(0.,0.,-1.));
#123015=DIRECTION('ref_axis',(0.,1.,0.));
#123016=DIRECTION('',(0.,1.23467863058847E-16,-1.));
#123017=DIRECTION('center_axis',(0.,0.,-1.));
#123018=DIRECTION('ref_axis',(0.,1.,0.));
#123019=DIRECTION('center_axis',(0.,1.22462808028055E-16,-1.));
#123020=DIRECTION('ref_axis',(1.22464679914735E-16,-1.,-1.22462808028055E-16));
#123021=DIRECTION('center_axis',(0.,1.22462808028055E-16,-1.));
#123022=DIRECTION('ref_axis',(0.,1.,1.22462808028055E-16));
#123023=DIRECTION('center_axis',(0.,-1.23467863058847E-16,1.));
#123024=DIRECTION('ref_axis',(0.,-1.,-1.23467863058847E-16));
#123025=DIRECTION('',(0.700366780446485,-0.713783141330072,-8.81292791474553E-17));
#123026=DIRECTION('',(-0.700366780446451,0.713783141330105,8.81292791474594E-17));
#123027=DIRECTION('center_axis',(0.,0.,-1.));
#123028=DIRECTION('ref_axis',(0.,-1.,0.));
#123029=DIRECTION('center_axis',(-0.713783141330072,-0.700366780446485,
-8.64727897391325E-17));
#123030=DIRECTION('ref_axis',(-0.700366780446485,0.713783141330072,-1.3612391051092E-33));
#123031=DIRECTION('',(-0.507302896983364,0.517020784572389,-0.689444181230387));
#123032=DIRECTION('',(-0.0133576962200374,0.0136135788205688,-0.999818104668739));
#123033=DIRECTION('center_axis',(0.,1.23467863058847E-16,-1.));
#123034=DIRECTION('ref_axis',(-1.,0.,0.));
#123035=DIRECTION('center_axis',(-7.1617481931302E-31,-4.1541690210802E-45,
1.));
#123036=DIRECTION('ref_axis',(-5.80049578546342E-15,1.,-2.48920611114446E-60));
#123037=DIRECTION('',(0.70592193778968,0.708289642552581,8.74510085926821E-17));
#123038=DIRECTION('center_axis',(0.708289642552581,-0.70592193778968,-8.71586731452524E-17));
#123039=DIRECTION('ref_axis',(9.155251692876E-34,1.23467863058847E-16,-1.));
#123040=DIRECTION('',(-0.0134621338381862,-0.0135072866467963,-0.999818145544461));
#123041=DIRECTION('center_axis',(0.966292363511968,0.257447214431338,3.17864574162902E-17));
#123042=DIRECTION('ref_axis',(-3.29101538697003E-33,1.23467863058847E-16,
-1.));
#123043=DIRECTION('',(0.257447214431338,-0.966292363511968,-1.19306053212906E-16));
#123044=DIRECTION('',(0.,1.23467863058847E-16,-1.));
#123045=DIRECTION('center_axis',(-0.260190353924911,-0.965557341499939,
-1.19215301615779E-16));
#123046=DIRECTION('ref_axis',(-0.965557341499939,0.260190353924911,3.58038858923534E-33));
#123047=DIRECTION('',(0.,1.23467863058847E-16,-1.));
#123048=DIRECTION('',(-0.965557341499939,0.260190353924911,3.21251469876339E-17));
#123049=DIRECTION('center_axis',(0.,0.,-1.));
#123050=DIRECTION('ref_axis',(0.,1.,0.));
#123051=DIRECTION('center_axis',(0.,0.,1.));
#123052=DIRECTION('ref_axis',(0.,-1.,0.));
#123053=DIRECTION('center_axis',(-4.93476711729114E-30,1.97232914692071E-43,
-1.));
#123054=DIRECTION('ref_axis',(-3.99680288865056E-14,-1.,0.));
#123055=DIRECTION('center_axis',(0.966876318092686,-0.255245343760725,-3.15145971498576E-17));
#123056=DIRECTION('ref_axis',(-1.08811059507331E-34,1.23467863058847E-16,
-1.));
#123057=DIRECTION('',(0.,1.23467863058847E-16,-1.));
#123058=DIRECTION('',(-0.255245343760725,-0.966876318092686,-1.1937815283711E-16));
#123059=DIRECTION('center_axis',(-0.262389207151869,0.964962125666191,1.19141811588728E-16));
#123060=DIRECTION('ref_axis',(4.54065214350716E-16,4.72048517437092E-33,
1.));
#123061=DIRECTION('',(0.964962125666191,0.262389207151869,3.23966346967465E-17));
#123062=DIRECTION('',(0.,1.23467863058847E-16,-1.));
#123063=DIRECTION('center_axis',(0.,0.,-1.));
#123064=DIRECTION('ref_axis',(0.,1.,0.));
#123065=DIRECTION('center_axis',(0.,0.,1.));
#123066=DIRECTION('ref_axis',(0.,-1.,0.));
#123067=DIRECTION('center_axis',(0.,0.,-1.));
#123068=DIRECTION('ref_axis',(0.,1.,0.));
#123069=DIRECTION('center_axis',(0.,0.,-1.));
#123070=DIRECTION('ref_axis',(0.,1.,0.));
#123071=DIRECTION('center_axis',(0.,0.,-1.));
#123072=DIRECTION('ref_axis',(0.,1.,0.));
#123073=DIRECTION('',(0.,1.23467863058847E-16,-1.));
#123074=DIRECTION('center_axis',(0.,0.,-1.));
#123075=DIRECTION('ref_axis',(0.,1.,0.));
#123076=DIRECTION('',(0.,1.23467863058847E-16,-1.));
#123077=DIRECTION('center_axis',(0.,1.21568833848598E-16,-1.));
#123078=DIRECTION('ref_axis',(1.01064309961486E-15,-1.,-1.21568833848598E-16));
#123079=DIRECTION('center_axis',(0.,1.21568833848598E-16,-1.));
#123080=DIRECTION('ref_axis',(0.,1.,1.21568833848598E-16));
#123081=DIRECTION('center_axis',(0.,1.21568833848598E-16,-1.));
#123082=DIRECTION('ref_axis',(0.,1.,1.21568833848598E-16));
#123083=DIRECTION('center_axis',(0.,1.30925187718918E-16,-1.));
#123084=DIRECTION('ref_axis',(0.,1.,1.30925187718918E-16));
#123085=DIRECTION('center_axis',(0.,1.30925187718918E-16,-1.));
#123086=DIRECTION('ref_axis',(0.,1.,1.30925187718918E-16));
#123087=DIRECTION('',(0.,1.23467863058847E-16,-1.));
#123088=DIRECTION('center_axis',(0.,1.30925187718918E-16,-1.));
#123089=DIRECTION('ref_axis',(0.,1.,1.30925187718918E-16));
#123090=DIRECTION('center_axis',(0.,1.30925187718918E-16,-1.));
#123091=DIRECTION('ref_axis',(0.,1.,1.30925187718918E-16));
#123092=DIRECTION('center_axis',(0.,1.30925187718918E-16,-1.));
#123093=DIRECTION('ref_axis',(0.,1.,1.30925187718918E-16));
#123094=DIRECTION('center_axis',(0.,0.,-1.));
#123095=DIRECTION('ref_axis',(0.,1.,0.));
#123096=DIRECTION('center_axis',(0.,0.,-1.));
#123097=DIRECTION('ref_axis',(0.,1.,0.));
#123098=DIRECTION('center_axis',(0.,0.,-1.));
#123099=DIRECTION('ref_axis',(0.,1.,0.));
#123100=DIRECTION('',(0.,1.23467863058847E-16,-1.));
#123101=DIRECTION('center_axis',(0.,0.,-1.));
#123102=DIRECTION('ref_axis',(0.,1.,0.));
#123103=DIRECTION('center_axis',(0.,0.,-1.));
#123104=DIRECTION('ref_axis',(0.,1.,0.));
#123105=DIRECTION('center_axis',(0.,0.,-1.));
#123106=DIRECTION('ref_axis',(0.,1.,0.));
#123107=DIRECTION('',(0.,1.23467863058847E-16,-1.));
#123108=DIRECTION('center_axis',(0.,0.,-1.));
#123109=DIRECTION('ref_axis',(0.,1.,0.));
#123110=DIRECTION('center_axis',(0.,0.,-1.));
#123111=DIRECTION('ref_axis',(0.,1.,0.));
#123112=DIRECTION('center_axis',(0.,0.,-1.));
#123113=DIRECTION('ref_axis',(0.,1.,0.));
#123114=DIRECTION('',(0.,1.23467863058847E-16,-1.));
#123115=DIRECTION('center_axis',(0.,1.21568833848598E-16,-1.));
#123116=DIRECTION('ref_axis',(0.,1.,1.21568833848598E-16));
#123117=DIRECTION('center_axis',(0.,1.21568833848598E-16,-1.));
#123118=DIRECTION('ref_axis',(0.,1.,1.21568833848598E-16));
#123119=DIRECTION('center_axis',(0.,1.21568833848598E-16,-1.));
#123120=DIRECTION('ref_axis',(0.,1.,1.21568833848598E-16));
#123121=DIRECTION('center_axis',(0.,0.,-1.));
#123122=DIRECTION('ref_axis',(0.,1.,0.));
#123123=DIRECTION('center_axis',(0.,0.,-1.));
#123124=DIRECTION('ref_axis',(0.,1.,0.));
#123125=DIRECTION('',(0.,1.23467863058847E-16,-1.));
#123126=DIRECTION('center_axis',(0.,0.,-1.));
#123127=DIRECTION('ref_axis',(0.,1.,0.));
#123128=DIRECTION('',(0.,1.23467863058847E-16,-1.));
#123129=DIRECTION('center_axis',(0.,0.,-1.));
#123130=DIRECTION('ref_axis',(0.,1.,0.));
#123131=DIRECTION('center_axis',(0.,0.,-1.));
#123132=DIRECTION('ref_axis',(0.,1.,0.));
#123133=DIRECTION('center_axis',(0.,0.,-1.));
#123134=DIRECTION('ref_axis',(0.,1.,0.));
#123135=DIRECTION('center_axis',(0.,0.,1.));
#123136=DIRECTION('ref_axis',(0.,1.,0.));
#123137=DIRECTION('center_axis',(9.45862666529894E-32,7.24606518465966E-47,
-1.));
#123138=DIRECTION('ref_axis',(7.66080049574581E-16,-1.,2.91703841149741E-62));
#123139=DIRECTION('',(0.0110444763156131,-0.0135131799871829,0.999847695156391));
#123140=DIRECTION('',(0.000686915141868458,-0.0174388829355556,0.999847695156391));
#123141=DIRECTION('center_axis',(0.,0.,1.));
#123142=DIRECTION('ref_axis',(0.,1.,0.));
#123143=DIRECTION('center_axis',(4.38645965981435E-31,1.5583835234929E-45,
-1.));
#123144=DIRECTION('ref_axis',(3.5527136788005E-15,-1.,1.24460305557223E-60));
#123145=DIRECTION('',(0.013481760241072,-0.011082807913809,0.999847695156391));
#123146=DIRECTION('center_axis',(0.,0.,1.));
#123147=DIRECTION('ref_axis',(0.,1.,0.));
#123148=DIRECTION('center_axis',(1.89172533305981E-31,2.89842607386392E-46,
-1.));
#123149=DIRECTION('ref_axis',(1.53216009914918E-15,-1.,7.38983064246011E-61));
#123150=DIRECTION('',(0.0174387888650499,-0.000689299189283617,0.999847695156391));
#123151=DIRECTION('center_axis',(-0.49830877570858,0.40695051295028,0.765558387101415));
#123152=DIRECTION('ref_axis',(0.616776838376874,-0.454175066156573,0.642892946705359));
#123153=DIRECTION('center_axis',(0.,0.,1.));
#123154=DIRECTION('ref_axis',(0.,1.,0.));
#123155=DIRECTION('center_axis',(-6.62103866570927E-31,3.55057194048325E-45,
-1.));
#123156=DIRECTION('ref_axis',(-5.36256034702207E-15,-1.,-1.86690458335834E-60));
#123157=DIRECTION('',(0.0134817602410721,0.0110828079138087,0.999847695156391));
#123158=DIRECTION('center_axis',(0.524694312992163,0.428071664074771,-0.735833220458236));
#123159=DIRECTION('ref_axis',(0.586317116694794,0.444960261363177,0.67693618936966));
#123160=DIRECTION('',(0.0174387888650499,0.000689299189283565,0.999847695156391));
#123161=DIRECTION('center_axis',(0.,0.,1.));
#123162=DIRECTION('ref_axis',(0.,1.,0.));
#123163=DIRECTION('center_axis',(1.09661491495359E-30,9.73989702183064E-45,
-1.));
#123164=DIRECTION('ref_axis',(8.88178419700126E-15,-1.,3.73380916671668E-60));
#123165=DIRECTION('',(0.0109827961190146,0.0135633579861438,0.999847695156391));
#123166=DIRECTION('center_axis',(0.,0.,1.));
#123167=DIRECTION('ref_axis',(0.,1.,0.));
#123168=DIRECTION('center_axis',(0.,0.,-1.));
#123169=DIRECTION('ref_axis',(0.,-1.,0.));
#123170=DIRECTION('',(0.003269361032546,0.0171434468206077,0.999847695156391));
#123171=DIRECTION('center_axis',(-0.424375096187792,-0.528257078927607,
0.735425207820941));
#123172=DIRECTION('ref_axis',(0.426055759035728,0.600170551540012,0.676957752933407));
#123173=DIRECTION('center_axis',(0.,-1.30362731016209E-16,1.));
#123174=DIRECTION('ref_axis',(-1.22464679914735E-16,-1.,-1.30362731016209E-16));
#123175=DIRECTION('center_axis',(0.,1.30357480714758E-16,-1.));
#123176=DIRECTION('ref_axis',(0.,-1.,-1.30357480714758E-16));
#123177=DIRECTION('center_axis',(0.,-1.23467863058847E-16,1.));
#123178=DIRECTION('ref_axis',(0.,-1.,-1.23467863058847E-16));
#123179=DIRECTION('center_axis',(2.75730074378449E-32,1.19587307245642E-16,
-1.));
#123180=DIRECTION('ref_axis',(7.105427357601E-15,-1.,-1.19587307245642E-16));
#123181=DIRECTION('center_axis',(0.,1.30052077910778E-16,-1.));
#123182=DIRECTION('ref_axis',(0.,-1.,-1.30052077910778E-16));
#123183=DIRECTION('center_axis',(9.63646068259673E-31,7.52109676045604E-45,
-1.));
#123184=DIRECTION('ref_axis',(7.80483313135807E-15,-1.,-3.73380916671668E-60));
#123185=DIRECTION('center_axis',(7.6763044046751E-31,4.77254954069701E-45,
-1.));
#123186=DIRECTION('ref_axis',(6.21724893790088E-15,-1.,1.86690458335834E-60));
#123187=DIRECTION('center_axis',(2.22379861906079E-31,4.00531780142632E-46,
-1.));
#123188=DIRECTION('ref_axis',(1.80111533800572E-15,-1.,8.55664600705907E-61));
#123189=DIRECTION('center_axis',(2.57572279529701E-31,1.30052077910778E-16,
-1.));
#123190=DIRECTION('ref_axis',(-3.91196650355621E-14,-1.,-1.30052077910778E-16));
#123191=DIRECTION('center_axis',(-2.96506482541439E-31,7.12056498031345E-46,
-1.));
#123192=DIRECTION('ref_axis',(-2.40148711734095E-15,-1.,1.0890276736257E-60));
#123193=DIRECTION('center_axis',(0.,0.,-1.));
#123194=DIRECTION('ref_axis',(0.,-1.,0.));
#123195=DIRECTION('center_axis',(0.,0.,-1.));
#123196=DIRECTION('ref_axis',(0.,-1.,0.));
#123197=DIRECTION('center_axis',(1.83206263248512E-32,1.20889464124791E-16,
-1.));
#123198=DIRECTION('ref_axis',(7.105427357601E-15,-1.,-1.20889464124791E-16));
#123199=DIRECTION('center_axis',(0.,1.30357480714758E-16,-1.));
#123200=DIRECTION('ref_axis',(0.,-1.,-1.30357480714758E-16));
#123201=DIRECTION('center_axis',(0.,-1.30002649721837E-16,1.));
#123202=DIRECTION('ref_axis',(0.,1.,1.30002649721837E-16));
#123203=DIRECTION('center_axis',(0.,1.30002742469137E-16,-1.));
#123204=DIRECTION('ref_axis',(0.,-1.,-1.30002742469137E-16));
#123205=DIRECTION('',(0.0174387888650499,0.000689299189283565,0.999847695156391));
#123206=DIRECTION('',(0.0174387888650499,-0.000689299189283839,0.999847695156391));
#123207=DIRECTION('center_axis',(0.,0.,1.));
#123208=DIRECTION('ref_axis',(0.,1.,0.));
#123209=DIRECTION('center_axis',(2.14851878863042E-31,3.73873238811768E-46,
-1.));
#123210=DIRECTION('ref_axis',(1.74014414391086E-15,-1.,-5.4451383681285E-61));
#123211=DIRECTION('',(0.013481760241072,0.0110828079138088,0.999847695156391));
#123212=DIRECTION('center_axis',(0.,0.,1.));
#123213=DIRECTION('ref_axis',(0.,1.,0.));
#123214=DIRECTION('center_axis',(0.,0.,-1.));
#123215=DIRECTION('ref_axis',(0.,-1.,0.));
#123216=DIRECTION('',(0.0109827961190146,0.0135633579861438,0.999847695156391));
#123217=DIRECTION('center_axis',(0.,0.,1.));
#123218=DIRECTION('ref_axis',(0.,1.,0.));
#123219=DIRECTION('center_axis',(-3.58086464771735E-31,1.03853677447713E-45,
-1.));
#123220=DIRECTION('ref_axis',(-2.90024023985143E-15,-1.,1.55575381946529E-61));
#123221=DIRECTION('',(0.0032693610325459,0.0171434468206077,0.999847695156391));
#123222=DIRECTION('center_axis',(0.,-1.19378624347407E-16,1.));
#123223=DIRECTION('ref_axis',(0.,1.,1.19378624347407E-16));
#123224=DIRECTION('center_axis',(2.90530101061278E-32,1.19379015387349E-16,
-1.));
#123225=DIRECTION('ref_axis',(7.105427357601E-15,-1.,-1.19379015387349E-16));
#123226=DIRECTION('center_axis',(0.,-1.30002649721837E-16,1.));
#123227=DIRECTION('ref_axis',(-1.22464679914735E-16,-1.,-1.30002649721837E-16));
#123228=DIRECTION('center_axis',(0.,1.30002742469137E-16,-1.));
#123229=DIRECTION('ref_axis',(0.,-1.,-1.30002742469137E-16));
#123230=DIRECTION('',(0.000686915141868465,-0.0174388829355556,0.999847695156391));
#123231=DIRECTION('center_axis',(0.,0.,1.));
#123232=DIRECTION('ref_axis',(0.,1.,0.));
#123233=DIRECTION('center_axis',(-2.14851878863041E-31,3.73873238811767E-46,
-1.));
#123234=DIRECTION('ref_axis',(-1.74014414391086E-15,-1.,-6.22301527786114E-61));
#123235=DIRECTION('',(0.0110444763156131,-0.0135131799871829,0.999847695156391));
#123236=DIRECTION('center_axis',(0.,0.,1.));
#123237=DIRECTION('ref_axis',(0.,1.,0.));
#123238=DIRECTION('center_axis',(1.09661491495359E-30,9.73989702183063E-45,
-1.));
#123239=DIRECTION('ref_axis',(8.88178419700125E-15,-1.,2.48920611114446E-60));
#123240=DIRECTION('',(0.013481760241072,-0.011082807913809,0.999847695156391));
#123241=DIRECTION('center_axis',(0.,0.,1.));
#123242=DIRECTION('ref_axis',(0.,-1.,0.));
#123243=DIRECTION('center_axis',(-2.14851878863042E-31,3.73873238811769E-46,
-1.));
#123244=DIRECTION('ref_axis',(-1.74014414391087E-15,-1.,2.33363072919793E-61));
#123245=DIRECTION('center_axis',(0.,-1.30362731016209E-16,1.));
#123246=DIRECTION('ref_axis',(0.,1.,1.30362731016209E-16));
#123247=DIRECTION('center_axis',(9.64691113863996E-8,8.44900850580662E-7,
-0.999999999999639));
#123248=DIRECTION('ref_axis',(0.131285471389481,0.991344604565596,8.5025289246305E-7));
#123249=DIRECTION('center_axis',(0.,-1.20912044068284E-16,1.));
#123250=DIRECTION('ref_axis',(0.,1.,1.20912044068284E-16));
#123251=DIRECTION('center_axis',(0.,1.23467863058847E-16,-1.));
#123252=DIRECTION('ref_axis',(-1.,0.,0.));
#123253=DIRECTION('center_axis',(0.,1.21568833848598E-16,-1.));
#123254=DIRECTION('ref_axis',(0.,1.,1.21568833848598E-16));
#123255=DIRECTION('center_axis',(0.,1.21568833848598E-16,-1.));
#123256=DIRECTION('ref_axis',(0.,1.,1.21568833848598E-16));
#123257=DIRECTION('center_axis',(2.34984018715753E-7,-7.16719780920963E-6,
-0.999999999974288));
#123258=DIRECTION('ref_axis',(0.0297033272169244,-0.999558758803514,7.17101515365848E-6));
#123259=DIRECTION('center_axis',(0.,1.23467863058847E-16,-1.));
#123260=DIRECTION('ref_axis',(-1.,0.,0.));
#123261=DIRECTION('center_axis',(0.,0.,-1.));
#123262=DIRECTION('ref_axis',(0.,1.,0.));
#123263=DIRECTION('center_axis',(0.,-1.23467863058847E-16,1.));
#123264=DIRECTION('ref_axis',(0.,-1.,-1.23467863058847E-16));
#123265=DIRECTION('center_axis',(0.,0.,-1.));
#123266=DIRECTION('ref_axis',(0.,1.,0.));
#123267=DIRECTION('center_axis',(0.,1.23467863058847E-16,-1.));
#123268=DIRECTION('ref_axis',(-1.,0.,0.));
#123269=DIRECTION('center_axis',(0.,1.23467863058847E-16,-1.));
#123270=DIRECTION('ref_axis',(-1.,0.,0.));
#123271=DIRECTION('center_axis',(0.,1.23467863058847E-16,-1.));
#123272=DIRECTION('ref_axis',(-1.,0.,0.));
#123273=DIRECTION('center_axis',(0.,1.23467863058847E-16,-1.));
#123274=DIRECTION('ref_axis',(-1.,0.,0.));
#123275=DIRECTION('center_axis',(0.,1.21568833848598E-16,-1.));
#123276=DIRECTION('ref_axis',(0.,1.,1.21568833848598E-16));
#123277=DIRECTION('center_axis',(0.,1.23467863058847E-16,-1.));
#123278=DIRECTION('ref_axis',(-1.,0.,0.));
#123279=DIRECTION('center_axis',(0.,1.21568833848598E-16,-1.));
#123280=DIRECTION('ref_axis',(0.,1.,1.21568833848598E-16));
#123281=DIRECTION('center_axis',(0.,1.23467863058847E-16,-1.));
#123282=DIRECTION('ref_axis',(-1.,0.,0.));
#123283=DIRECTION('center_axis',(0.,1.21568833848598E-16,-1.));
#123284=DIRECTION('ref_axis',(0.,1.,1.21568833848598E-16));
#123285=DIRECTION('center_axis',(0.,1.23467863058847E-16,-1.));
#123286=DIRECTION('ref_axis',(-1.,0.,0.));
#123287=DIRECTION('center_axis',(0.,1.23467863058847E-16,-1.));
#123288=DIRECTION('ref_axis',(-1.,0.,0.));
#123289=DIRECTION('center_axis',(0.,1.21568833848598E-16,-1.));
#123290=DIRECTION('ref_axis',(0.,1.,1.21568833848598E-16));
#123291=DIRECTION('center_axis',(0.,1.23467863058847E-16,-1.));
#123292=DIRECTION('ref_axis',(-1.,0.,0.));
#123293=DIRECTION('',(-0.7059219377897,-0.708289642552561,-8.74510085926797E-17));
#123294=DIRECTION('center_axis',(7.1617481931302E-31,-4.1541690210802E-45,
1.));
#123295=DIRECTION('ref_axis',(5.80049578546342E-15,1.,-2.48920611114446E-60));
#123296=DIRECTION('center_axis',(0.,1.21568833848598E-16,-1.));
#123297=DIRECTION('ref_axis',(0.,1.,1.21568833848598E-16));
#123298=DIRECTION('center_axis',(0.,1.21568833848598E-16,-1.));
#123299=DIRECTION('ref_axis',(0.,1.,1.21568833848598E-16));
#123300=DIRECTION('center_axis',(0.,1.21568833848598E-16,-1.));
#123301=DIRECTION('ref_axis',(0.,1.,1.21568833848598E-16));
#123302=DIRECTION('center_axis',(0.,1.21568833848598E-16,-1.));
#123303=DIRECTION('ref_axis',(0.,1.,1.21568833848598E-16));
#123304=DIRECTION('center_axis',(0.,1.21568833848598E-16,-1.));
#123305=DIRECTION('ref_axis',(0.,1.,1.21568833848598E-16));
#123306=DIRECTION('center_axis',(0.,1.21568833848598E-16,-1.));
#123307=DIRECTION('ref_axis',(0.,1.,1.21568833848598E-16));
#123308=DIRECTION('center_axis',(0.,1.21568833848598E-16,-1.));
#123309=DIRECTION('ref_axis',(0.,1.,1.21568833848598E-16));
#123310=DIRECTION('center_axis',(0.,1.21568833848598E-16,-1.));
#123311=DIRECTION('ref_axis',(0.,1.,1.21568833848598E-16));
#123312=DIRECTION('center_axis',(0.,1.21568833848598E-16,-1.));
#123313=DIRECTION('ref_axis',(0.,1.,1.21568833848598E-16));
#123314=DIRECTION('center_axis',(0.,1.21568833848598E-16,-1.));
#123315=DIRECTION('ref_axis',(0.,1.,1.21568833848598E-16));
#123316=DIRECTION('center_axis',(0.713783141330105,0.700366780446451,8.64727897391283E-17));
#123317=DIRECTION('ref_axis',(-6.33941656186775E-33,1.23467863058847E-16,
-1.));
#123318=DIRECTION('',(0.0133579710326364,-0.0136138588975274,0.999818097183587));
#123319=DIRECTION('center_axis',(0.,0.,-1.));
#123320=DIRECTION('ref_axis',(-0.705510697508481,-0.708699270284015,0.));
#123321=DIRECTION('',(0.0134623247494151,0.0135074781986352,0.999818140386068));
#123322=DIRECTION('center_axis',(-0.708289642552561,0.7059219377897,8.71586731452547E-17));
#123323=DIRECTION('ref_axis',(1.23055128733987E-16,2.43647158576037E-33,
1.));
#123324=DIRECTION('center_axis',(0.,0.,-1.));
#123325=DIRECTION('ref_axis',(0.,1.,0.));
#123326=DIRECTION('center_axis',(0.,0.,-1.));
#123327=DIRECTION('ref_axis',(0.,1.,0.));
#123328=DIRECTION('',(0.,1.23467863058847E-16,-1.));
#123329=DIRECTION('',(0.,1.23467863058847E-16,-1.));
#123330=DIRECTION('center_axis',(0.,0.,-1.));
#123331=DIRECTION('ref_axis',(0.,1.,0.));
#123332=DIRECTION('',(0.,1.23467863058847E-16,-1.));
#123333=DIRECTION('center_axis',(0.,0.,-1.));
#123334=DIRECTION('ref_axis',(0.,1.,0.));
#123335=DIRECTION('',(0.,1.23467863058847E-16,-1.));
#123336=DIRECTION('center_axis',(0.,1.22914743790472E-16,-1.));
#123337=DIRECTION('ref_axis',(0.,1.,1.22914743790472E-16));
#123338=DIRECTION('center_axis',(0.,0.,-1.));
#123339=DIRECTION('ref_axis',(0.,1.,0.));
#123340=DIRECTION('',(0.,1.23467863058847E-16,-1.));
#123341=DIRECTION('',(0.,1.23467863058847E-16,-1.));
#123342=DIRECTION('center_axis',(0.,0.,-1.));
#123343=DIRECTION('ref_axis',(0.,1.,0.));
#123344=DIRECTION('center_axis',(0.,0.,-1.));
#123345=DIRECTION('ref_axis',(0.,1.,0.));
#123346=DIRECTION('',(0.,1.23467863058847E-16,-1.));
#123347=DIRECTION('',(0.,1.23467863058847E-16,-1.));
#123348=DIRECTION('center_axis',(0.,1.23467863058847E-16,-1.));
#123349=DIRECTION('ref_axis',(-1.,0.,0.));
#123350=DIRECTION('center_axis',(0.,0.,-1.));
#123351=DIRECTION('ref_axis',(0.,1.,0.));
#123352=DIRECTION('center_axis',(0.,0.,-1.));
#123353=DIRECTION('ref_axis',(0.,1.,0.));
#123354=DIRECTION('',(-2.13730336808358E-18,-0.0174524064372818,-0.999847695156391));
#123355=DIRECTION('center_axis',(0.,1.23467863058847E-16,-1.));
#123356=DIRECTION('ref_axis',(-1.,0.,0.));
#123357=DIRECTION('center_axis',(0.,0.,-1.));
#123358=DIRECTION('ref_axis',(0.,1.,0.));
#123359=DIRECTION('center_axis',(0.,0.,-1.));
#123360=DIRECTION('ref_axis',(0.,1.,0.));
#123361=DIRECTION('',(-2.13730336808358E-18,-0.0174524064372818,-0.999847695156391));
#123362=DIRECTION('center_axis',(0.,-1.23467863058847E-16,1.));
#123363=DIRECTION('ref_axis',(0.,-1.,-1.23467863058847E-16));
#123364=DIRECTION('center_axis',(-0.713783141330072,-0.700366780446485,
-8.64727897391325E-17));
#123365=DIRECTION('ref_axis',(-0.700366780446485,0.713783141330072,-1.3612391051092E-33));
#123366=DIRECTION('center_axis',(0.713783141330105,0.700366780446451,8.64727897391283E-17));
#123367=DIRECTION('ref_axis',(-6.33941656186775E-33,1.23467863058847E-16,
-1.));
#123368=DIRECTION('center_axis',(0.,0.,1.));
#123369=DIRECTION('ref_axis',(0.,-1.,0.));
#123370=DIRECTION('center_axis',(0.,1.23467863058847E-16,-1.));
#123371=DIRECTION('ref_axis',(-1.,0.,0.));
#123372=DIRECTION('center_axis',(0.708289642552581,-0.70592193778968,-8.71586731452524E-17));
#123373=DIRECTION('ref_axis',(9.155251692876E-34,1.23467863058847E-16,-1.));
#123374=DIRECTION('center_axis',(-0.708289642552561,0.7059219377897,8.71586731452547E-17));
#123375=DIRECTION('ref_axis',(1.23055128733987E-16,2.43647158576037E-33,
1.));
#123376=DIRECTION('center_axis',(0.,0.,1.));
#123377=DIRECTION('ref_axis',(0.,-1.,0.));
#123378=DIRECTION('center_axis',(0.966292363511968,0.257447214431338,3.17864574162902E-17));
#123379=DIRECTION('ref_axis',(-3.29101538697003E-33,1.23467863058847E-16,
-1.));
#123380=DIRECTION('center_axis',(-0.260190353924911,-0.965557341499939,
-1.19215301615779E-16));
#123381=DIRECTION('ref_axis',(-0.965557341499939,0.260190353924911,3.58038858923534E-33));
#123382=DIRECTION('center_axis',(0.,0.,-1.));
#123383=DIRECTION('ref_axis',(0.,1.,0.));
#123384=DIRECTION('center_axis',(0.966876318092686,-0.255245343760725,-3.15145971498576E-17));
#123385=DIRECTION('ref_axis',(-1.08811059507331E-34,1.23467863058847E-16,
-1.));
#123386=DIRECTION('center_axis',(-0.262389207151869,0.964962125666191,1.19141811588728E-16));
#123387=DIRECTION('ref_axis',(4.54065214350716E-16,4.72048517437092E-33,
1.));
#123388=DIRECTION('center_axis',(0.,0.,-1.));
#123389=DIRECTION('ref_axis',(0.,1.,0.));
#123390=DIRECTION('center_axis',(0.,1.23467863058847E-16,-1.));
#123391=DIRECTION('ref_axis',(-1.,0.,0.));
#123392=DIRECTION('center_axis',(0.,0.,-1.));
#123393=DIRECTION('ref_axis',(0.,1.,0.));
#123394=DIRECTION('',(0.,1.23467863058847E-16,-1.));
#123395=DIRECTION('',(0.,1.23467863058847E-16,-1.));
#123396=DIRECTION('center_axis',(0.,0.,-1.));
#123397=DIRECTION('ref_axis',(0.,1.,0.));
#123398=DIRECTION('center_axis',(0.,0.,-1.));
#123399=DIRECTION('ref_axis',(0.,1.,0.));
#123400=DIRECTION('',(0.,1.23467863058847E-16,-1.));
#123401=DIRECTION('center_axis',(0.,0.,-1.));
#123402=DIRECTION('ref_axis',(0.,1.,0.));
#123403=DIRECTION('center_axis',(0.,1.22229112323298E-16,-1.));
#123404=DIRECTION('ref_axis',(0.,1.,1.22229112323298E-16));
#123405=DIRECTION('',(0.,1.23467863058847E-16,-1.));
#123406=DIRECTION('center_axis',(0.,1.22229112323298E-16,-1.));
#123407=DIRECTION('ref_axis',(0.,1.,1.22229112323298E-16));
#123408=DIRECTION('center_axis',(0.,0.,-1.));
#123409=DIRECTION('ref_axis',(0.,1.,0.));
#123410=DIRECTION('',(0.,1.23467863058847E-16,-1.));
#123411=DIRECTION('center_axis',(0.,0.,-1.));
#123412=DIRECTION('ref_axis',(0.,1.,0.));
#123413=DIRECTION('center_axis',(0.,0.,-1.));
#123414=DIRECTION('ref_axis',(0.,1.,0.));
#123415=DIRECTION('',(0.,1.23467863058847E-16,-1.));
#123416=DIRECTION('center_axis',(0.,0.,-1.));
#123417=DIRECTION('ref_axis',(0.,1.,0.));
#123418=DIRECTION('center_axis',(0.,0.,-1.));
#123419=DIRECTION('ref_axis',(0.,1.,0.));
#123420=DIRECTION('',(0.,1.23467863058847E-16,-1.));
#123421=DIRECTION('center_axis',(0.,0.,-1.));
#123422=DIRECTION('ref_axis',(0.,1.,0.));
#123423=DIRECTION('center_axis',(0.,1.22229112323298E-16,-1.));
#123424=DIRECTION('ref_axis',(1.22464679914735E-16,-1.,-1.22229112323298E-16));
#123425=DIRECTION('center_axis',(0.,1.22229112323298E-16,-1.));
#123426=DIRECTION('ref_axis',(0.,1.,1.22229112323298E-16));
#123427=DIRECTION('center_axis',(0.,1.33250839261027E-16,-1.));
#123428=DIRECTION('ref_axis',(0.,1.,1.33250839261027E-16));
#123429=DIRECTION('center_axis',(0.,1.33250839261027E-16,-1.));
#123430=DIRECTION('ref_axis',(0.,-1.,-1.33250839261027E-16));
#123431=DIRECTION('',(0.,1.23467863058847E-16,-1.));
#123432=DIRECTION('center_axis',(0.,0.,-1.));
#123433=DIRECTION('ref_axis',(0.,1.,0.));
#123434=DIRECTION('center_axis',(0.,0.,-1.));
#123435=DIRECTION('ref_axis',(0.,1.,0.));
#123436=DIRECTION('center_axis',(0.,1.23467863058847E-16,-1.));
#123437=DIRECTION('ref_axis',(-1.,0.,0.));
#123438=DIRECTION('center_axis',(0.,1.22014183466588E-16,-1.));
#123439=DIRECTION('ref_axis',(0.,1.,1.22014183466588E-16));
#123440=DIRECTION('center_axis',(0.,1.32487572930867E-16,-1.));
#123441=DIRECTION('ref_axis',(0.,-1.,-1.32487572930867E-16));
#123442=DIRECTION('center_axis',(0.,0.,-1.));
#123443=DIRECTION('ref_axis',(0.,1.,0.));
#123444=DIRECTION('center_axis',(0.,0.,-1.));
#123445=DIRECTION('ref_axis',(0.,1.,0.));
#123446=DIRECTION('center_axis',(0.,0.,-1.));
#123447=DIRECTION('ref_axis',(0.,1.,0.));
#123448=DIRECTION('center_axis',(0.,1.22014183466588E-16,-1.));
#123449=DIRECTION('ref_axis',(0.,1.,1.22014183466588E-16));
#123450=DIRECTION('center_axis',(0.,0.,-1.));
#123451=DIRECTION('ref_axis',(0.,1.,0.));
#123452=DIRECTION('center_axis',(0.,0.,-1.));
#123453=DIRECTION('ref_axis',(0.,1.,0.));
#123454=DIRECTION('center_axis',(0.,0.,-1.));
#123455=DIRECTION('ref_axis',(0.,1.,0.));
#123456=DIRECTION('center_axis',(0.,0.,-1.));
#123457=DIRECTION('ref_axis',(0.,1.,0.));
#123458=DIRECTION('',(0.,1.23467863058847E-16,-1.));
#123459=DIRECTION('',(0.,1.23467863058847E-16,-1.));
#123460=DIRECTION('center_axis',(0.,1.22014183466588E-16,-1.));
#123461=DIRECTION('ref_axis',(1.22464679914735E-16,-1.,-1.22014183466588E-16));
#123462=DIRECTION('center_axis',(0.,1.32487572930867E-16,-1.));
#123463=DIRECTION('ref_axis',(0.,1.,1.32487572930867E-16));
#123464=DIRECTION('',(0.,1.23467863058847E-16,-1.));
#123465=DIRECTION('center_axis',(0.,0.,-1.));
#123466=DIRECTION('ref_axis',(0.,1.,0.));
#123467=DIRECTION('',(0.,1.23467863058847E-16,-1.));
#123468=DIRECTION('center_axis',(0.,0.,-1.));
#123469=DIRECTION('ref_axis',(0.,1.,0.));
#123470=DIRECTION('',(0.,1.23467863058847E-16,-1.));
#123471=DIRECTION('center_axis',(0.,0.,-1.));
#123472=DIRECTION('ref_axis',(0.,1.,0.));
#123473=DIRECTION('',(0.,1.23467863058847E-16,-1.));
#123474=DIRECTION('center_axis',(0.,1.22014183466588E-16,-1.));
#123475=DIRECTION('ref_axis',(0.,1.,1.22014183466588E-16));
#123476=DIRECTION('',(0.,1.23467863058847E-16,-1.));
#123477=DIRECTION('center_axis',(0.,0.,-1.));
#123478=DIRECTION('ref_axis',(0.,1.,0.));
#123479=DIRECTION('',(0.,1.23467863058847E-16,-1.));
#123480=DIRECTION('center_axis',(0.,0.,-1.));
#123481=DIRECTION('ref_axis',(0.,1.,0.));
#123482=DIRECTION('',(0.459549353210719,-0.545727376107149,0.700711083779054));
#123483=DIRECTION('',(0.595667475496749,-0.42912133257888,0.678995685230073));
#123484=DIRECTION('',(0.580626046021037,0.392567954055243,0.713276801901518));
#123485=DIRECTION('',(-0.484796374610729,-0.46748816331627,-0.739207205270264));
#123486=DIRECTION('center_axis',(0.,0.,1.));
#123487=DIRECTION('ref_axis',(0.,1.,0.));
#123488=DIRECTION('',(0.0110444763156131,-0.0135131799871829,0.999847695156391));
#123489=DIRECTION('',(0.000686915141868466,-0.0174388829355556,0.999847695156391));
#123490=DIRECTION('center_axis',(0.,0.,1.));
#123491=DIRECTION('ref_axis',(0.,1.,0.));
#123492=DIRECTION('',(0.013481760241072,-0.011082807913809,0.999847695156391));
#123493=DIRECTION('center_axis',(0.,0.,1.));
#123494=DIRECTION('ref_axis',(0.,1.,0.));
#123495=DIRECTION('',(0.0174387888650499,-0.000689299189283616,0.999847695156391));
#123496=DIRECTION('center_axis',(0.,0.,1.));
#123497=DIRECTION('ref_axis',(0.,1.,0.));
#123498=DIRECTION('',(0.0134817602410721,0.0110828079138087,0.999847695156391));
#123499=DIRECTION('',(0.0174387888650499,0.000689299189283565,0.999847695156391));
#123500=DIRECTION('center_axis',(0.,0.,1.));
#123501=DIRECTION('ref_axis',(0.,1.,0.));
#123502=DIRECTION('',(0.0109827961190146,0.0135633579861438,0.999847695156391));
#123503=DIRECTION('center_axis',(0.,0.,1.));
#123504=DIRECTION('ref_axis',(0.,1.,0.));
#123505=DIRECTION('',(0.00326936103254579,0.0171434468206077,0.999847695156391));
#123506=DIRECTION('center_axis',(0.,-1.30057350048735E-16,1.));
#123507=DIRECTION('ref_axis',(1.22464679914735E-16,-1.,-1.30057350048735E-16));
#123508=DIRECTION('center_axis',(0.,-1.23467863058847E-16,1.));
#123509=DIRECTION('ref_axis',(0.,-1.,-1.23467863058847E-16));
#123510=DIRECTION('center_axis',(0.,1.18108832406932E-16,-1.));
#123511=DIRECTION('ref_axis',(0.,1.,1.18108832406932E-16));
#123512=DIRECTION('center_axis',(0.,1.29698951474901E-16,-1.));
#123513=DIRECTION('ref_axis',(0.,1.,1.29698951474901E-16));
#123514=DIRECTION('center_axis',(0.,0.,-1.));
#123515=DIRECTION('ref_axis',(0.,1.,0.));
#123516=DIRECTION('center_axis',(0.,0.,-1.));
#123517=DIRECTION('ref_axis',(0.,1.,0.));
#123518=DIRECTION('center_axis',(0.,0.,-1.));
#123519=DIRECTION('ref_axis',(0.,-1.,0.));
#123520=DIRECTION('center_axis',(0.,1.29698951474901E-16,-1.));
#123521=DIRECTION('ref_axis',(0.,1.,1.29698951474901E-16));
#123522=DIRECTION('center_axis',(0.,0.,-1.));
#123523=DIRECTION('ref_axis',(0.,1.,0.));
#123524=DIRECTION('center_axis',(0.,0.,-1.));
#123525=DIRECTION('ref_axis',(0.,1.,0.));
#123526=DIRECTION('center_axis',(0.,0.,-1.));
#123527=DIRECTION('ref_axis',(0.,1.,0.));
#123528=DIRECTION('center_axis',(0.,-1.23467863058847E-16,1.));
#123529=DIRECTION('ref_axis',(0.,-1.,-1.23467863058847E-16));
#123530=DIRECTION('center_axis',(0.,-1.29698951474901E-16,1.));
#123531=DIRECTION('ref_axis',(0.,1.,1.29698951474901E-16));
#123532=DIRECTION('',(0.0174387888650499,-0.000689299189283839,0.999847695156391));
#123533=DIRECTION('',(0.0174387888650499,0.000689299189283565,0.999847695156391));
#123534=DIRECTION('center_axis',(0.,0.,1.));
#123535=DIRECTION('ref_axis',(0.,1.,0.));
#123536=DIRECTION('',(0.0134817602410721,0.0110828079138088,0.999847695156391));
#123537=DIRECTION('center_axis',(0.,0.,1.));
#123538=DIRECTION('ref_axis',(0.,1.,0.));
#123539=DIRECTION('',(0.0109827961190146,0.0135633579861438,0.999847695156391));
#123540=DIRECTION('center_axis',(0.,0.,1.));
#123541=DIRECTION('ref_axis',(0.,1.,0.));
#123542=DIRECTION('',(0.0032693610325459,0.0171434468206077,0.999847695156391));
#123543=DIRECTION('center_axis',(0.,-1.18108832406932E-16,1.));
#123544=DIRECTION('ref_axis',(0.,1.,1.18108832406932E-16));
#123545=DIRECTION('center_axis',(0.,-1.29698951474901E-16,1.));
#123546=DIRECTION('ref_axis',(-1.22464679914735E-16,-1.,-1.29698951474901E-16));
#123547=DIRECTION('',(0.000686915141868473,-0.0174388829355556,0.999847695156391));
#123548=DIRECTION('center_axis',(0.,0.,1.));
#123549=DIRECTION('ref_axis',(0.,1.,0.));
#123550=DIRECTION('',(0.0110444763156131,-0.0135131799871829,0.999847695156391));
#123551=DIRECTION('center_axis',(0.,0.,1.));
#123552=DIRECTION('ref_axis',(0.,1.,0.));
#123553=DIRECTION('',(0.013481760241072,-0.011082807913809,0.999847695156391));
#123554=DIRECTION('center_axis',(0.,0.,1.));
#123555=DIRECTION('ref_axis',(0.,-1.,0.));
#123556=DIRECTION('center_axis',(0.,-1.30057350048735E-16,1.));
#123557=DIRECTION('ref_axis',(0.,1.,1.30057350048735E-16));
#123558=DIRECTION('center_axis',(0.,-1.1960959958765E-16,1.));
#123559=DIRECTION('ref_axis',(0.,1.,1.1960959958765E-16));
#123560=DIRECTION('center_axis',(0.,1.23467863058847E-16,-1.));
#123561=DIRECTION('ref_axis',(-1.,0.,0.));
#123562=DIRECTION('center_axis',(0.,1.23467863058847E-16,-1.));
#123563=DIRECTION('ref_axis',(-1.,0.,0.));
#123564=DIRECTION('center_axis',(0.,-1.23467863058847E-16,1.));
#123565=DIRECTION('ref_axis',(0.,-1.,-1.23467863058847E-16));
#123566=DIRECTION('center_axis',(0.,1.22914743790472E-16,-1.));
#123567=DIRECTION('ref_axis',(0.,1.,1.22914743790472E-16));
#123568=DIRECTION('center_axis',(0.,1.22914743790472E-16,-1.));
#123569=DIRECTION('ref_axis',(0.,1.,1.22914743790472E-16));
#123570=DIRECTION('center_axis',(0.,1.22914743790472E-16,-1.));
#123571=DIRECTION('ref_axis',(0.,1.,1.22914743790472E-16));
#123572=DIRECTION('center_axis',(0.,1.22914743790472E-16,-1.));
#123573=DIRECTION('ref_axis',(0.,1.,1.22914743790472E-16));
#123574=DIRECTION('center_axis',(0.,1.22914743790472E-16,-1.));
#123575=DIRECTION('ref_axis',(0.,1.,1.22914743790472E-16));
#123576=DIRECTION('center_axis',(-3.29883322342201E-16,1.,1.23467863058847E-16));
#123577=DIRECTION('ref_axis',(1.,3.29883322342202E-16,0.));
#123578=DIRECTION('center_axis',(-3.29883322342201E-16,-1.,-1.23467863058847E-16));
#123579=DIRECTION('ref_axis',(-1.,3.29883322342202E-16,0.));
#123580=DIRECTION('center_axis',(-3.71118737634973E-16,1.,1.23467863058847E-16));
#123581=DIRECTION('ref_axis',(1.,3.71118737634973E-16,0.));
#123582=DIRECTION('center_axis',(-3.71118737634973E-16,-1.,-1.23467863058847E-16));
#123583=DIRECTION('ref_axis',(-1.,3.71118737634973E-16,0.));
#123584=DIRECTION('center_axis',(-5.72252063890675E-16,1.,1.23467863058847E-16));
#123585=DIRECTION('ref_axis',(1.,5.72252063890675E-16,0.));
#123586=DIRECTION('center_axis',(1.90750687963558E-16,-1.,-1.23467863058847E-16));
#123587=DIRECTION('ref_axis',(-2.39311615755447E-50,1.23467863058847E-16,
-1.));
#123588=DIRECTION('center_axis',(1.23706245878324E-16,-1.,-1.23467863058847E-16));
#123589=DIRECTION('ref_axis',(9.34199996189111E-49,1.23467863058847E-16,
-1.));
#123590=DIRECTION('center_axis',(1.23706245878324E-16,1.,1.23467863058847E-16));
#123591=DIRECTION('ref_axis',(1.,-1.23706245878324E-16,0.));
#123592=DIRECTION('center_axis',(-4.76876719908896E-16,-1.,-1.23467863058847E-16));
#123593=DIRECTION('ref_axis',(-1.,4.76876719908896E-16,0.));
#123594=DIRECTION('center_axis',(9.53753439817791E-17,1.,1.23467863058847E-16));
#123595=DIRECTION('ref_axis',(-4.60419424770999E-49,1.23467863058847E-16,
-1.));
#123596=DIRECTION('center_axis',(0.,1.35726946151947E-16,-1.));
#123597=DIRECTION('ref_axis',(0.,1.,1.35726946151947E-16));
#123598=DIRECTION('center_axis',(0.,1.22914743790472E-16,-1.));
#123599=DIRECTION('ref_axis',(0.,1.,1.22914743790472E-16));
#123600=DIRECTION('center_axis',(0.,1.34087697701688E-16,-1.));
#123601=DIRECTION('ref_axis',(0.,1.,1.34087697701688E-16));
#123602=DIRECTION('center_axis',(0.,-1.34087697701688E-16,1.));
#123603=DIRECTION('ref_axis',(0.,1.,1.34087697701688E-16));
#123604=DIRECTION('center_axis',(0.,1.34087697701688E-16,-1.));
#123605=DIRECTION('ref_axis',(0.,1.,1.34087697701688E-16));
#123606=DIRECTION('center_axis',(1.86759697420978E-30,-1.34087697701688E-16,
1.));
#123607=DIRECTION('ref_axis',(-1.75859327100625E-13,1.,1.34087697701688E-16));
#123608=DIRECTION('center_axis',(0.,1.23467863058847E-16,-1.));
#123609=DIRECTION('ref_axis',(-1.,0.,0.));
#123610=DIRECTION('center_axis',(-3.29883322342201E-16,1.,1.23467863058847E-16));
#123611=DIRECTION('ref_axis',(1.,3.29883322342202E-16,0.));
#123612=DIRECTION('center_axis',(-3.29883322342201E-16,-1.,-1.23467863058847E-16));
#123613=DIRECTION('ref_axis',(-1.,3.29883322342202E-16,0.));
#123614=DIRECTION('center_axis',(-3.29883322342198E-16,1.,1.23467863058847E-16));
#123615=DIRECTION('ref_axis',(1.,3.29883322342198E-16,0.));
#123616=DIRECTION('center_axis',(-3.29883322342198E-16,-1.,-1.23467863058847E-16));
#123617=DIRECTION('ref_axis',(-1.,3.29883322342198E-16,0.));
#123618=DIRECTION('center_axis',(-3.71118737634973E-16,1.,1.23467863058847E-16));
#123619=DIRECTION('ref_axis',(1.,3.71118737634973E-16,0.));
#123620=DIRECTION('center_axis',(-3.71118737634973E-16,-1.,-1.23467863058847E-16));
#123621=DIRECTION('ref_axis',(-1.,3.71118737634973E-16,0.));
#123622=DIRECTION('center_axis',(-3.71118737634973E-16,1.,1.23467863058847E-16));
#123623=DIRECTION('ref_axis',(1.,3.71118737634973E-16,0.));
#123624=DIRECTION('center_axis',(-3.71118737634973E-16,-1.,-1.23467863058847E-16));
#123625=DIRECTION('ref_axis',(-1.,3.71118737634973E-16,0.));
#123626=DIRECTION('center_axis',(-5.72252063890675E-16,1.,1.23467863058847E-16));
#123627=DIRECTION('ref_axis',(1.,5.72252063890675E-16,0.));
#123628=DIRECTION('center_axis',(1.90750687963558E-16,-1.,-1.23467863058847E-16));
#123629=DIRECTION('ref_axis',(-2.39311615755447E-50,1.23467863058847E-16,
-1.));
#123630=DIRECTION('center_axis',(1.23706245878324E-16,-1.,-1.23467863058847E-16));
#123631=DIRECTION('ref_axis',(9.34199996189111E-49,1.23467863058847E-16,
-1.));
#123632=DIRECTION('center_axis',(1.23706245878324E-16,1.,1.23467863058847E-16));
#123633=DIRECTION('ref_axis',(1.,-1.23706245878324E-16,0.));
#123634=DIRECTION('center_axis',(-4.76876719908896E-16,-1.,-1.23467863058847E-16));
#123635=DIRECTION('ref_axis',(-1.,4.76876719908896E-16,0.));
#123636=DIRECTION('center_axis',(9.53753439817791E-17,1.,1.23467863058847E-16));
#123637=DIRECTION('ref_axis',(-4.60419424770999E-49,1.23467863058847E-16,
-1.));
#123638=DIRECTION('center_axis',(0.,1.35726946151947E-16,-1.));
#123639=DIRECTION('ref_axis',(0.,1.,1.35726946151947E-16));
#123640=DIRECTION('center_axis',(0.,1.35726946151947E-16,-1.));
#123641=DIRECTION('ref_axis',(0.,1.,1.35726946151947E-16));
#123642=DIRECTION('center_axis',(0.,1.22914743790472E-16,-1.));
#123643=DIRECTION('ref_axis',(0.,1.,1.22914743790472E-16));
#123644=DIRECTION('center_axis',(0.,1.22914743790472E-16,-1.));
#123645=DIRECTION('ref_axis',(0.,1.,1.22914743790472E-16));
#123646=DIRECTION('center_axis',(0.,0.,-1.));
#123647=DIRECTION('ref_axis',(0.,1.,0.));
#123648=DIRECTION('center_axis',(0.,0.,-1.));
#123649=DIRECTION('ref_axis',(0.,1.,0.));
#123650=DIRECTION('center_axis',(0.,0.,-1.));
#123651=DIRECTION('ref_axis',(0.,1.,0.));
#123652=DIRECTION('center_axis',(0.,0.,-1.));
#123653=DIRECTION('ref_axis',(0.,1.,0.));
#123654=DIRECTION('center_axis',(-3.29883322342201E-16,1.,1.23467863058847E-16));
#123655=DIRECTION('ref_axis',(1.,3.29883322342202E-16,0.));
#123656=DIRECTION('center_axis',(-3.29883322342201E-16,1.,1.23467863058847E-16));
#123657=DIRECTION('ref_axis',(1.,3.29883322342202E-16,0.));
#123658=DIRECTION('center_axis',(-3.29883322342201E-16,-1.,-1.23467863058847E-16));
#123659=DIRECTION('ref_axis',(-1.,3.29883322342202E-16,0.));
#123660=DIRECTION('center_axis',(-3.29883322342201E-16,-1.,-1.23467863058847E-16));
#123661=DIRECTION('ref_axis',(-1.,3.29883322342202E-16,0.));
#123662=DIRECTION('center_axis',(-3.29883322342198E-16,1.,1.23467863058847E-16));
#123663=DIRECTION('ref_axis',(1.,3.29883322342198E-16,0.));
#123664=DIRECTION('center_axis',(-3.29883322342198E-16,1.,1.23467863058847E-16));
#123665=DIRECTION('ref_axis',(1.,3.29883322342198E-16,0.));
#123666=DIRECTION('center_axis',(-3.29883322342198E-16,-1.,-1.23467863058847E-16));
#123667=DIRECTION('ref_axis',(-1.,3.29883322342198E-16,0.));
#123668=DIRECTION('center_axis',(-3.29883322342198E-16,-1.,-1.23467863058847E-16));
#123669=DIRECTION('ref_axis',(-1.,3.29883322342198E-16,0.));
#123670=DIRECTION('center_axis',(-3.71118737634973E-16,1.,1.23467863058847E-16));
#123671=DIRECTION('ref_axis',(1.,3.71118737634973E-16,0.));
#123672=DIRECTION('center_axis',(-3.71118737634973E-16,1.,1.23467863058847E-16));
#123673=DIRECTION('ref_axis',(1.,3.71118737634973E-16,0.));
#123674=DIRECTION('center_axis',(-3.71118737634973E-16,-1.,-1.23467863058847E-16));
#123675=DIRECTION('ref_axis',(-1.,3.71118737634973E-16,0.));
#123676=DIRECTION('center_axis',(-3.71118737634973E-16,-1.,-1.23467863058847E-16));
#123677=DIRECTION('ref_axis',(-1.,3.71118737634973E-16,0.));
#123678=DIRECTION('center_axis',(-3.71118737634973E-16,1.,1.23467863058847E-16));
#123679=DIRECTION('ref_axis',(1.,3.71118737634973E-16,0.));
#123680=DIRECTION('center_axis',(-3.71118737634973E-16,1.,1.23467863058847E-16));
#123681=DIRECTION('ref_axis',(1.,3.71118737634973E-16,0.));
#123682=DIRECTION('center_axis',(-3.71118737634973E-16,-1.,-1.23467863058847E-16));
#123683=DIRECTION('ref_axis',(-1.,3.71118737634973E-16,0.));
#123684=DIRECTION('center_axis',(-3.71118737634973E-16,-1.,-1.23467863058847E-16));
#123685=DIRECTION('ref_axis',(-1.,3.71118737634973E-16,0.));
#123686=DIRECTION('center_axis',(-5.72252063890675E-16,1.,1.23467863058847E-16));
#123687=DIRECTION('ref_axis',(1.,5.72252063890675E-16,0.));
#123688=DIRECTION('center_axis',(-5.72252063890675E-16,1.,1.23467863058847E-16));
#123689=DIRECTION('ref_axis',(1.,5.72252063890675E-16,0.));
#123690=DIRECTION('center_axis',(1.90750687963558E-16,-1.,-1.23467863058847E-16));
#123691=DIRECTION('ref_axis',(-2.39311615755447E-50,1.23467863058847E-16,
-1.));
#123692=DIRECTION('center_axis',(1.90750687963558E-16,-1.,-1.23467863058847E-16));
#123693=DIRECTION('ref_axis',(-2.39311615755447E-50,1.23467863058847E-16,
-1.));
#123694=DIRECTION('center_axis',(1.23706245878324E-16,-1.,-1.23467863058847E-16));
#123695=DIRECTION('ref_axis',(9.34199996189111E-49,1.23467863058847E-16,
-1.));
#123696=DIRECTION('center_axis',(1.23706245878324E-16,-1.,-1.23467863058847E-16));
#123697=DIRECTION('ref_axis',(9.34199996189111E-49,1.23467863058847E-16,
-1.));
#123698=DIRECTION('center_axis',(1.23706245878324E-16,1.,1.23467863058847E-16));
#123699=DIRECTION('ref_axis',(1.,-1.23706245878324E-16,0.));
#123700=DIRECTION('center_axis',(1.23706245878324E-16,1.,1.23467863058847E-16));
#123701=DIRECTION('ref_axis',(1.,-1.23706245878324E-16,0.));
#123702=DIRECTION('center_axis',(-4.76876719908896E-16,-1.,-1.23467863058847E-16));
#123703=DIRECTION('ref_axis',(-1.,4.76876719908896E-16,0.));
#123704=DIRECTION('center_axis',(-4.76876719908896E-16,-1.,-1.23467863058847E-16));
#123705=DIRECTION('ref_axis',(-1.,4.76876719908896E-16,0.));
#123706=DIRECTION('center_axis',(9.53753439817791E-17,1.,1.23467863058847E-16));
#123707=DIRECTION('ref_axis',(-4.60419424770999E-49,1.23467863058847E-16,
-1.));
#123708=DIRECTION('center_axis',(9.53753439817791E-17,1.,1.23467863058847E-16));
#123709=DIRECTION('ref_axis',(-4.60419424770999E-49,1.23467863058847E-16,
-1.));
#123710=DIRECTION('center_axis',(0.,1.23467863058847E-16,-1.));
#123711=DIRECTION('ref_axis',(0.705921937789673,-0.708289642552588,0.));
#123712=DIRECTION('center_axis',(0.5,0.866025403784438,1.0692630595994E-16));
#123713=DIRECTION('ref_axis',(2.13852611919879E-16,-5.48307457472744E-35,
-1.));
#123714=DIRECTION('',(0.,1.23467863058847E-16,-1.));
#123715=DIRECTION('',(0.,1.23467863058847E-16,-1.));
#123716=DIRECTION('center_axis',(1.,0.,0.));
#123717=DIRECTION('ref_axis',(0.,1.,0.));
#123718=DIRECTION('',(0.,1.23467863058847E-16,-1.));
#123719=DIRECTION('center_axis',(0.5,-0.866025403784439,-1.0692630595994E-16));
#123720=DIRECTION('ref_axis',(4.1166144903646E-33,1.23467863058847E-16,
-1.));
#123721=DIRECTION('',(0.,1.23467863058847E-16,-1.));
#123722=DIRECTION('center_axis',(-0.5,-0.866025403784439,-1.0692630595994E-16));
#123723=DIRECTION('ref_axis',(-0.866025403784439,0.5,-7.83367607530638E-34));
#123724=DIRECTION('',(0.,1.23467863058847E-16,-1.));
#123725=DIRECTION('center_axis',(-1.,0.,0.));
#123726=DIRECTION('ref_axis',(0.,0.,1.));
#123727=DIRECTION('',(0.,1.23467863058847E-16,-1.));
#123728=DIRECTION('center_axis',(-0.5,0.866025403784439,1.0692630595994E-16));
#123729=DIRECTION('ref_axis',(2.1385261191988E-16,4.09037363277686E-33,
1.));
#123730=DIRECTION('center_axis',(0.,0.,-1.));
#123731=DIRECTION('ref_axis',(0.,1.,0.));
#123732=DIRECTION('',(-1.06057523872491E-16,-0.866025403784439,-0.5));
#123733=DIRECTION('center_axis',(0.,0.,-1.));
#123734=DIRECTION('ref_axis',(0.,1.,0.));
#123735=DIRECTION('center_axis',(0.,0.,1.));
#123736=DIRECTION('ref_axis',(0.,1.,0.));
#123737=DIRECTION('center_axis',(0.,0.,-1.));
#123738=DIRECTION('ref_axis',(0.,1.,0.));
#123739=DIRECTION('center_axis',(0.,0.,1.));
#123740=DIRECTION('ref_axis',(0.,1.,0.));
#123741=DIRECTION('center_axis',(0.,0.,-1.));
#123742=DIRECTION('ref_axis',(0.,1.,0.));
#123743=DIRECTION('center_axis',(0.,0.,1.));
#123744=DIRECTION('ref_axis',(0.,1.,0.));
#123745=DIRECTION('center_axis',(0.,0.,-1.));
#123746=DIRECTION('ref_axis',(0.,1.,0.));
#123747=DIRECTION('center_axis',(0.,0.,1.));
#123748=DIRECTION('ref_axis',(0.,1.,0.));
#123749=DIRECTION('center_axis',(0.,0.,-1.));
#123750=DIRECTION('ref_axis',(0.,1.,0.));
#123751=DIRECTION('center_axis',(0.,0.,1.));
#123752=DIRECTION('ref_axis',(0.,1.,0.));
#123753=DIRECTION('center_axis',(0.,0.,-1.));
#123754=DIRECTION('ref_axis',(0.,1.,0.));
#123755=DIRECTION('center_axis',(0.,0.,1.));
#123756=DIRECTION('ref_axis',(0.,1.,0.));
#123757=DIRECTION('center_axis',(0.,1.23467863058847E-16,-1.));
#123758=DIRECTION('ref_axis',(0.,1.,0.));
#123759=DIRECTION('center_axis',(0.,0.,1.));
#123760=DIRECTION('ref_axis',(0.,1.,0.));
#123761=DIRECTION('center_axis',(-1.,0.,0.));
#123762=DIRECTION('ref_axis',(0.,-1.,0.));
#123763=DIRECTION('center_axis',(0.,0.,-1.));
#123764=DIRECTION('ref_axis',(0.,1.,0.));
#123765=DIRECTION('center_axis',(0.,0.,-1.));
#123766=DIRECTION('ref_axis',(0.,1.,0.));
#123767=DIRECTION('center_axis',(0.,1.23467863058847E-16,-1.));
#123768=DIRECTION('ref_axis',(-1.,0.,0.));
#123769=DIRECTION('center_axis',(0.,0.,1.));
#123770=DIRECTION('ref_axis',(0.,1.,0.));
#123771=DIRECTION('center_axis',(0.,1.23467863058847E-16,-1.));
#123772=DIRECTION('ref_axis',(-1.,0.,0.));
#123773=DIRECTION('center_axis',(0.,0.,1.));
#123774=DIRECTION('ref_axis',(0.,-1.,0.));
#123775=DIRECTION('',(0.,0.,-1.));
#123776=DIRECTION('center_axis',(1.51575151553259E-16,1.51575151553259E-16,
-1.));
#123777=DIRECTION('ref_axis',(-1.,-2.17577274266937E-49,-1.51575151553259E-16));
#123778=DIRECTION('center_axis',(1.51575151553259E-16,4.20705558038691E-31,
-1.));
#123779=DIRECTION('ref_axis',(2.77555756156289E-15,-1.,-1.66404192638572E-45));
#123780=DIRECTION('center_axis',(1.51575151553259E-16,4.20705558038691E-31,
-1.));
#123781=DIRECTION('ref_axis',(2.77555756156289E-15,-1.,-1.66404192638572E-45));
#123782=DIRECTION('center_axis',(1.51575151553259E-16,4.20705558038691E-31,
-1.));
#123783=DIRECTION('ref_axis',(2.77555756156289E-15,-1.,-1.66404192638572E-45));
#123784=DIRECTION('center_axis',(1.51575151553259E-16,4.20705558038691E-31,
-1.));
#123785=DIRECTION('ref_axis',(2.77555756156289E-15,-1.,-1.66404192638572E-45));
#123786=DIRECTION('center_axis',(1.51575151553259E-16,4.20705558038691E-31,
-1.));
#123787=DIRECTION('ref_axis',(2.77555756156289E-15,-1.,-1.66404192638572E-45));
#123788=DIRECTION('center_axis',(1.51575151553259E-16,4.20705558038691E-31,
-1.));
#123789=DIRECTION('ref_axis',(2.77555756156289E-15,-1.,-1.66404192638572E-45));
#123790=DIRECTION('center_axis',(-1.51575151553259E-16,-4.20705558038691E-31,
1.));
#123791=DIRECTION('ref_axis',(2.77555756156289E-15,-1.,-1.66404192638572E-45));
#123792=DIRECTION('center_axis',(-1.51575151553259E-16,-4.20705558038691E-31,
1.));
#123793=DIRECTION('ref_axis',(2.77555756156289E-15,-1.,-1.66404192638572E-45));
#123794=DIRECTION('center_axis',(-1.51575151553259E-16,-4.20705558038691E-31,
1.));
#123795=DIRECTION('ref_axis',(2.77555756156289E-15,-1.,-1.66404192638572E-45));
#123796=DIRECTION('center_axis',(-1.51575151553259E-16,-4.20705558038691E-31,
1.));
#123797=DIRECTION('ref_axis',(2.77555756156289E-15,-1.,-1.66404192638572E-45));
#123798=DIRECTION('center_axis',(-1.51575151553259E-16,-4.20705558038691E-31,
1.));
#123799=DIRECTION('ref_axis',(2.77555756156289E-15,-1.,-1.66404192638572E-45));
#123800=DIRECTION('center_axis',(-1.51575151553259E-16,-4.20705558038691E-31,
1.));
#123801=DIRECTION('ref_axis',(2.77555756156289E-15,-1.,-1.66404192638572E-45));
#123802=DIRECTION('center_axis',(1.51575151553259E-16,1.51575151553259E-16,
-1.));
#123803=DIRECTION('ref_axis',(-1.,-2.17577274266937E-49,-1.51575151553259E-16));
#123804=DIRECTION('center_axis',(1.51575151553259E-16,4.20705558038691E-31,
-1.));
#123805=DIRECTION('ref_axis',(2.77555756156289E-15,-1.,-1.66404192638572E-45));
#123806=DIRECTION('center_axis',(-1.51575151553259E-16,-8.41411116077385E-31,
1.));
#123807=DIRECTION('ref_axis',(5.55111512312578E-15,-1.,-3.67840846885265E-45));
#123808=DIRECTION('center_axis',(-1.51575151553259E-16,-8.41411116077385E-31,
1.));
#123809=DIRECTION('ref_axis',(5.55111512312578E-15,-1.,-3.67840846885265E-45));
#123810=DIRECTION('center_axis',(-1.51575151553259E-16,0.,1.));
#123811=DIRECTION('ref_axis',(0.,-1.,0.));
#123812=DIRECTION('center_axis',(-1.51575151553259E-16,-4.20705558038691E-31,
1.));
#123813=DIRECTION('ref_axis',(2.77555756156289E-15,-1.,-1.66404192638572E-45));
#123814=DIRECTION('center_axis',(-1.51575151553258E-16,4.20705558038689E-31,
1.));
#123815=DIRECTION('ref_axis',(-2.77555756156289E-15,-1.,7.00649232162409E-46));
#123816=DIRECTION('center_axis',(1.51575151553259E-16,4.20705558038691E-31,
-1.));
#123817=DIRECTION('ref_axis',(2.77555756156289E-15,-1.,-1.66404192638572E-45));
#123818=DIRECTION('center_axis',(1.51575151553259E-16,4.20705558038691E-31,
-1.));
#123819=DIRECTION('ref_axis',(2.77555756156289E-15,-1.,-1.66404192638572E-45));
#123820=DIRECTION('center_axis',(1.51575151553259E-16,4.20705558038691E-31,
-1.));
#123821=DIRECTION('ref_axis',(2.77555756156289E-15,-1.,-1.66404192638572E-45));
#123822=DIRECTION('center_axis',(1.51575151553259E-16,4.20705558038691E-31,
-1.));
#123823=DIRECTION('ref_axis',(2.77555756156289E-15,-1.,-1.66404192638572E-45));
#123824=DIRECTION('center_axis',(1.51575151553259E-16,4.20705558038691E-31,
-1.));
#123825=DIRECTION('ref_axis',(2.77555756156289E-15,-1.,-1.66404192638572E-45));
#123826=DIRECTION('center_axis',(1.51575151553259E-16,4.20705558038691E-31,
-1.));
#123827=DIRECTION('ref_axis',(2.77555756156289E-15,-1.,-1.66404192638572E-45));
#123828=DIRECTION('center_axis',(-3.49148133884314E-15,1.,1.51575151553259E-16));
#123829=DIRECTION('ref_axis',(1.,3.49148133884314E-15,0.));
#123830=DIRECTION('',(3.95893176803294E-18,-1.51575151553259E-16,1.));
#123831=DIRECTION('',(3.95893176803294E-18,-1.51575151553259E-16,1.));
#123832=DIRECTION('center_axis',(-0.866025403784439,0.499999999999999,7.92161112595944E-17));
#123833=DIRECTION('ref_axis',(9.14708863197643E-17,-1.05181136389903E-33,
1.));
#123834=DIRECTION('',(3.95893176803294E-18,-1.51575151553259E-16,1.));
#123835=DIRECTION('center_axis',(-0.866025403784438,-0.500000000000001,
-7.23590402936645E-17));
#123836=DIRECTION('ref_axis',(-0.500000000000001,0.866025403784438,-2.57334411451296E-33));
#123837=DIRECTION('',(3.95893176803294E-18,-1.51575151553259E-16,1.));
#123838=DIRECTION('center_axis',(3.64171279871685E-15,-1.,-1.51575151553259E-16));
#123839=DIRECTION('ref_axis',(5.87651897213004E-48,1.51575151553259E-16,
-1.));
#123840=DIRECTION('',(3.95893176803294E-18,-1.51575151553259E-16,1.));
#123841=DIRECTION('center_axis',(0.866025403784439,-0.499999999999999,-7.92161112595951E-17));
#123842=DIRECTION('ref_axis',(8.15047850955652E-33,1.5843222251919E-16,
-1.));
#123843=DIRECTION('',(3.95893176803294E-18,-1.51575151553259E-16,1.));
#123844=DIRECTION('center_axis',(0.866025403784438,0.500000000000001,7.23590402936639E-17));
#123845=DIRECTION('ref_axis',(-3.44176788548726E-33,1.44718080587327E-16,
-1.));
#123846=DIRECTION('center_axis',(0.,0.,-1.));
#123847=DIRECTION('ref_axis',(0.,-1.,0.));
#123848=DIRECTION('center_axis',(0.,0.,-1.));
#123849=DIRECTION('ref_axis',(-1.,0.,0.));
#123850=DIRECTION('center_axis',(0.,0.,-1.));
#123851=DIRECTION('ref_axis',(-1.,0.,0.));
#123852=DIRECTION('center_axis',(0.,0.,-1.));
#123853=DIRECTION('ref_axis',(-1.,0.,0.));
#123854=DIRECTION('center_axis',(0.,0.,-1.));
#123855=DIRECTION('ref_axis',(-1.,0.,0.));
#123856=DIRECTION('center_axis',(0.,0.,-1.));
#123857=DIRECTION('ref_axis',(-1.,0.,0.));
#123858=DIRECTION('center_axis',(0.,0.,-1.));
#123859=DIRECTION('ref_axis',(-1.,0.,0.));
#123860=DIRECTION('center_axis',(0.,0.,1.));
#123861=DIRECTION('ref_axis',(-1.,0.,0.));
#123862=DIRECTION('center_axis',(0.,0.,1.));
#123863=DIRECTION('ref_axis',(-1.,0.,0.));
#123864=DIRECTION('center_axis',(0.,0.,1.));
#123865=DIRECTION('ref_axis',(-1.,0.,0.));
#123866=DIRECTION('center_axis',(0.,0.,1.));
#123867=DIRECTION('ref_axis',(-1.,0.,0.));
#123868=DIRECTION('center_axis',(0.,0.,1.));
#123869=DIRECTION('ref_axis',(-1.,0.,0.));
#123870=DIRECTION('center_axis',(0.,0.,1.));
#123871=DIRECTION('ref_axis',(-1.,0.,0.));
#123872=DIRECTION('center_axis',(0.,0.,-1.));
#123873=DIRECTION('ref_axis',(0.,-1.,0.));
#123874=DIRECTION('center_axis',(0.,0.,-1.));
#123875=DIRECTION('ref_axis',(-1.,0.,0.));
#123876=DIRECTION('center_axis',(0.,0.,1.));
#123877=DIRECTION('ref_axis',(-1.,0.,0.));
#123878=DIRECTION('center_axis',(0.,0.,1.));
#123879=DIRECTION('ref_axis',(-1.,-1.38777878078145E-15,0.));
#123880=DIRECTION('center_axis',(0.,0.,1.));
#123881=DIRECTION('ref_axis',(-1.,1.38777878078145E-15,0.));
#123882=DIRECTION('center_axis',(0.,0.,1.));
#123883=DIRECTION('ref_axis',(-1.,-1.38777878078145E-15,0.));
#123884=DIRECTION('center_axis',(0.,0.,1.));
#123885=DIRECTION('ref_axis',(-1.,4.16333634234434E-15,0.));
#123886=DIRECTION('center_axis',(0.,0.,-1.));
#123887=DIRECTION('ref_axis',(-1.,0.,0.));
#123888=DIRECTION('center_axis',(0.,0.,-1.));
#123889=DIRECTION('ref_axis',(-1.,0.,0.));
#123890=DIRECTION('center_axis',(0.,0.,-1.));
#123891=DIRECTION('ref_axis',(-1.,0.,0.));
#123892=DIRECTION('center_axis',(0.,0.,-1.));
#123893=DIRECTION('ref_axis',(-1.,0.,0.));
#123894=DIRECTION('center_axis',(0.,0.,-1.));
#123895=DIRECTION('ref_axis',(-1.,0.,0.));
#123896=DIRECTION('center_axis',(0.,0.,-1.));
#123897=DIRECTION('ref_axis',(-1.,0.,0.));
#123898=DIRECTION('center_axis',(1.,0.,0.));
#123899=DIRECTION('ref_axis',(0.,1.,0.));
#123900=DIRECTION('',(0.,-1.55534083321291E-16,1.));
#123901=DIRECTION('',(0.,-1.55534083321291E-16,1.));
#123902=DIRECTION('center_axis',(0.5,0.866025403784439,1.34696467310564E-16));
#123903=DIRECTION('ref_axis',(2.69392934621129E-16,1.24972477443329E-33,
-1.));
#123904=DIRECTION('',(0.,-1.55534083321291E-16,1.));
#123905=DIRECTION('center_axis',(-0.5,0.866025403784438,1.34696467310564E-16));
#123906=DIRECTION('ref_axis',(2.69392934621128E-16,-2.09027289648572E-32,
1.));
#123907=DIRECTION('',(0.,-1.55534083321291E-16,1.));
#123908=DIRECTION('center_axis',(-1.,-1.50231459873716E-16,-2.33661123974778E-32));
#123909=DIRECTION('ref_axis',(-1.50231459873716E-16,1.,-1.23954453046792E-64));
#123910=DIRECTION('',(0.,-1.55534083321291E-16,1.));
#123911=DIRECTION('center_axis',(-0.5,-0.866025403784439,-1.34696467310564E-16));
#123912=DIRECTION('ref_axis',(-0.866025403784439,0.5,-3.71223821158428E-33));
#123913=DIRECTION('',(0.,-1.55534083321291E-16,1.));
#123914=DIRECTION('center_axis',(0.5,-0.866025403784438,-1.34696467310564E-16));
#123915=DIRECTION('ref_axis',(4.44087077315589E-33,1.55534083321292E-16,
-1.));
#123916=DIRECTION('center_axis',(-0.5,0.866025403784438,1.0692630595994E-16));
#123917=DIRECTION('ref_axis',(2.13852611919879E-16,5.48307457472744E-35,
1.));
#123918=DIRECTION('',(0.,1.23467863058847E-16,-1.));
#123919=DIRECTION('',(0.,1.23467863058847E-16,-1.));
#123920=DIRECTION('center_axis',(-1.,0.,0.));
#123921=DIRECTION('ref_axis',(0.,0.,1.));
#123922=DIRECTION('',(0.,1.23467863058847E-16,-1.));
#123923=DIRECTION('center_axis',(-0.5,-0.866025403784439,-1.0692630595994E-16));
#123924=DIRECTION('ref_axis',(-0.866025403784439,0.5,-9.26929360883051E-34));
#123925=DIRECTION('',(0.,1.23467863058847E-16,-1.));
#123926=DIRECTION('center_axis',(0.5,-0.866025403784439,-1.0692630595994E-16));
#123927=DIRECTION('ref_axis',(-4.5474696259435E-34,1.23467863058847E-16,
-1.));
#123928=DIRECTION('',(0.,1.23467863058847E-16,-1.));
#123929=DIRECTION('center_axis',(1.,0.,0.));
#123930=DIRECTION('ref_axis',(0.,1.,0.));
#123931=DIRECTION('',(0.,1.23467863058847E-16,-1.));
#123932=DIRECTION('center_axis',(0.5,0.866025403784439,1.0692630595994E-16));
#123933=DIRECTION('ref_axis',(2.1385261191988E-16,-4.09037363277686E-33,
-1.));
#123934=DIRECTION('center_axis',(0.,0.,-1.));
#123935=DIRECTION('ref_axis',(0.,1.,0.));
#123936=DIRECTION('',(-1.06057523872491E-16,-0.866025403784439,-0.5));
#123937=DIRECTION('center_axis',(0.,0.,-1.));
#123938=DIRECTION('ref_axis',(0.,1.,0.));
#123939=DIRECTION('center_axis',(0.,0.,-1.));
#123940=DIRECTION('ref_axis',(0.,1.,0.));
#123941=DIRECTION('center_axis',(0.,0.,-1.));
#123942=DIRECTION('ref_axis',(0.,1.,0.));
#123943=DIRECTION('center_axis',(0.,0.,-1.));
#123944=DIRECTION('ref_axis',(0.,1.,0.));
#123945=DIRECTION('center_axis',(0.,0.,-1.));
#123946=DIRECTION('ref_axis',(0.,1.,0.));
#123947=DIRECTION('center_axis',(0.,0.,-1.));
#123948=DIRECTION('ref_axis',(0.,1.,0.));
#123949=DIRECTION('center_axis',(0.,0.,-1.));
#123950=DIRECTION('ref_axis',(0.,1.,0.));
#123951=DIRECTION('center_axis',(0.,0.,-1.));
#123952=DIRECTION('ref_axis',(0.,1.,0.));
#123953=DIRECTION('center_axis',(0.,0.,-1.));
#123954=DIRECTION('ref_axis',(0.,1.,0.));
#123955=DIRECTION('center_axis',(0.,0.,-1.));
#123956=DIRECTION('ref_axis',(0.,1.,0.));
#123957=DIRECTION('center_axis',(0.,0.,-1.));
#123958=DIRECTION('ref_axis',(0.,1.,0.));
#123959=DIRECTION('center_axis',(0.,0.,-1.));
#123960=DIRECTION('ref_axis',(0.,1.,0.));
#123961=DIRECTION('center_axis',(0.,1.23467863058847E-16,-1.));
#123962=DIRECTION('ref_axis',(0.,1.,0.));
#123963=DIRECTION('center_axis',(0.,0.,-1.));
#123964=DIRECTION('ref_axis',(0.,1.,0.));
#123965=DIRECTION('center_axis',(-1.,0.,0.));
#123966=DIRECTION('ref_axis',(0.,-1.,0.));
#123967=DIRECTION('center_axis',(0.,0.,1.));
#123968=DIRECTION('ref_axis',(0.,1.,0.));
#123969=DIRECTION('center_axis',(0.,0.,1.));
#123970=DIRECTION('ref_axis',(0.,1.,0.));
#123971=DIRECTION('center_axis',(0.,1.23467863058847E-16,-1.));
#123972=DIRECTION('ref_axis',(-1.,0.,0.));
#123973=DIRECTION('center_axis',(0.,0.,-1.));
#123974=DIRECTION('ref_axis',(0.,1.,0.));
#123975=DIRECTION('center_axis',(0.,1.23467863058847E-16,-1.));
#123976=DIRECTION('ref_axis',(-1.,0.,0.));
#123977=DIRECTION('center_axis',(0.,0.,1.));
#123978=DIRECTION('ref_axis',(0.,-1.,0.));
#123979=DIRECTION('',(0.,0.,-1.));
#123980=DIRECTION('center_axis',(0.,0.,-1.));
#123981=DIRECTION('ref_axis',(1.,0.,0.));
#123982=DIRECTION('center_axis',(1.,0.,0.));
#123983=DIRECTION('ref_axis',(0.,0.,1.));
#123984=DIRECTION('center_axis',(0.0436193873653361,0.,0.999048221581858));
#123985=DIRECTION('ref_axis',(-0.999048221581858,0.,0.0436193873653362));
#123986=DIRECTION('center_axis',(0.0436193873653361,0.,-0.999048221581858));
#123987=DIRECTION('ref_axis',(0.999048221581858,0.,0.0436193873653362));
#123988=DIRECTION('center_axis',(-1.,0.,0.));
#123989=DIRECTION('ref_axis',(0.,0.,1.));
#123990=DIRECTION('center_axis',(-1.,0.,0.));
#123991=DIRECTION('ref_axis',(0.,0.,1.));
#123992=DIRECTION('center_axis',(-1.,0.,0.));
#123993=DIRECTION('ref_axis',(0.,0.,1.));
#123994=DIRECTION('center_axis',(0.,-1.,0.));
#123995=DIRECTION('ref_axis',(0.,0.,-1.));
#123996=DIRECTION('center_axis',(-1.,0.,0.));
#123997=DIRECTION('ref_axis',(0.,0.,1.));
#123998=DIRECTION('center_axis',(-1.,0.,0.));
#123999=DIRECTION('ref_axis',(0.,0.,1.));
#124000=DIRECTION('center_axis',(0.,-1.,0.));
#124001=DIRECTION('ref_axis',(0.,0.,-1.));
#124002=DIRECTION('center_axis',(1.,0.,0.));
#124003=DIRECTION('ref_axis',(0.,0.,1.));
#124004=DIRECTION('center_axis',(1.,0.,0.));
#124005=DIRECTION('ref_axis',(0.,0.,1.));
#124006=DIRECTION('center_axis',(-1.,0.,0.));
#124007=DIRECTION('ref_axis',(0.,0.,1.));
#124008=DIRECTION('center_axis',(-1.,0.,0.));
#124009=DIRECTION('ref_axis',(0.,0.,1.));
#124010=DIRECTION('',(0.,1.,0.));
#124011=DIRECTION('center_axis',(-1.,0.,0.));
#124012=DIRECTION('ref_axis',(0.,0.,1.));
#124013=DIRECTION('',(0.,-1.,0.));
#124014=DIRECTION('center_axis',(-0.0436193873653361,0.,-0.999048221581858));
#124015=DIRECTION('ref_axis',(-0.999048221581858,0.,0.0436193873653361));
#124016=DIRECTION('',(-0.999048221581858,-8.07120802883996E-16,0.0436193873653362));
#124017=DIRECTION('',(-0.999048221581858,0.,0.0436193873653362));
#124018=DIRECTION('center_axis',(1.,0.,0.));
#124019=DIRECTION('ref_axis',(0.,0.,1.));
#124020=DIRECTION('',(-0.999048221581858,0.,-0.0436193873653362));
#124021=DIRECTION('center_axis',(-0.0436193873653361,0.,0.999048221581858));
#124022=DIRECTION('ref_axis',(0.,1.,0.));
#124023=DIRECTION('',(-0.999048221581858,0.,-0.0436193873653362));
#124024=DIRECTION('center_axis',(1.,0.,0.));
#124025=DIRECTION('ref_axis',(0.,0.,1.));
#124026=DIRECTION('center_axis',(-1.,0.,0.));
#124027=DIRECTION('ref_axis',(0.,0.,1.));
#124028=DIRECTION('center_axis',(-1.,0.,0.));
#124029=DIRECTION('ref_axis',(0.,0.,1.));
#124030=DIRECTION('center_axis',(1.,0.,0.));
#124031=DIRECTION('ref_axis',(0.,0.,-1.));
#124032=DIRECTION('center_axis',(-1.,0.,0.));
#124033=DIRECTION('ref_axis',(0.,0.,1.));
#124034=DIRECTION('',(-1.,0.,0.));
#124035=DIRECTION('center_axis',(1.,0.,0.));
#124036=DIRECTION('ref_axis',(0.,0.,-1.));
#124037=DIRECTION('',(-1.,0.,0.));
#124038=DIRECTION('center_axis',(-1.,0.,0.));
#124039=DIRECTION('ref_axis',(0.,0.,1.));
#124040=DIRECTION('center_axis',(0.,0.,-1.));
#124041=DIRECTION('ref_axis',(1.,0.,0.));
#124042=DIRECTION('center_axis',(0.,0.,1.));
#124043=DIRECTION('ref_axis',(-1.,0.,0.));
#124044=DIRECTION('',(0.707106781186552,-8.65956056235499E-17,0.707106781186543));
#124045=DIRECTION('center_axis',(0.,0.,-1.));
#124046=DIRECTION('ref_axis',(-1.,0.,0.));
#124047=DIRECTION('center_axis',(0.,0.,1.));
#124048=DIRECTION('ref_axis',(1.,0.,0.));
#124049=DIRECTION('center_axis',(0.,0.,-1.));
#124050=DIRECTION('ref_axis',(1.,0.,0.));
#124051=DIRECTION('center_axis',(0.,0.,-1.));
#124052=DIRECTION('ref_axis',(-1.,0.,0.));
#124053=DIRECTION('',(0.,0.,1.));
#124054=DIRECTION('center_axis',(0.,1.23467863058847E-16,-1.));
#124055=DIRECTION('ref_axis',(-1.,0.,0.));
#124056=DIRECTION('center_axis',(0.,0.,1.));
#124057=DIRECTION('ref_axis',(0.,1.,0.));
#124058=DIRECTION('center_axis',(0.,0.,-1.));
#124059=DIRECTION('ref_axis',(1.,0.,0.));
#124060=DIRECTION('center_axis',(0.,0.,-1.));
#124061=DIRECTION('ref_axis',(-1.,0.,0.));
#124062=DIRECTION('',(0.,0.,1.));
#124063=DIRECTION('center_axis',(0.,0.,1.));
#124064=DIRECTION('ref_axis',(1.,0.,0.));
#124065=DIRECTION('center_axis',(0.,1.,0.));
#124066=DIRECTION('ref_axis',(0.,0.,1.));
#124067=DIRECTION('center_axis',(1.,0.,0.));
#124068=DIRECTION('ref_axis',(0.,0.,-1.));
#124069=DIRECTION('center_axis',(0.,-1.,0.));
#124070=DIRECTION('ref_axis',(0.,0.,1.));
#124071=DIRECTION('center_axis',(0.,0.,1.));
#124072=DIRECTION('ref_axis',(1.,0.,0.));
#124073=DIRECTION('center_axis',(0.,1.,0.));
#124074=DIRECTION('ref_axis',(0.,0.,1.));
#124075=DIRECTION('center_axis',(0.,0.,-1.));
#124076=DIRECTION('ref_axis',(-1.,0.,0.));
#124077=DIRECTION('center_axis',(0.,0.,1.));
#124078=DIRECTION('ref_axis',(1.,0.,0.));
#124079=DIRECTION('',(0.,0.,-1.));
#124080=DIRECTION('',(0.,0.,1.));
#124081=DIRECTION('center_axis',(1.,0.,0.));
#124082=DIRECTION('ref_axis',(0.,0.,-1.));
#124083=DIRECTION('center_axis',(1.,0.,0.));
#124084=DIRECTION('ref_axis',(0.,0.,-1.));
#124085=DIRECTION('',(-1.,0.,0.));
#124086=DIRECTION('',(1.,0.,0.));
#124087=DIRECTION('center_axis',(0.,1.,0.));
#124088=DIRECTION('ref_axis',(0.,0.,1.));
#124089=DIRECTION('center_axis',(1.,0.,0.));
#124090=DIRECTION('ref_axis',(0.,0.,-1.));
#124091=DIRECTION('center_axis',(0.,1.,0.));
#124092=DIRECTION('ref_axis',(0.,0.,1.));
#124093=DIRECTION('center_axis',(0.,-1.,0.));
#124094=DIRECTION('ref_axis',(0.,0.,1.));
#124095=DIRECTION('center_axis',(0.,1.,0.));
#124096=DIRECTION('ref_axis',(0.,0.,1.));
#124097=DIRECTION('center_axis',(0.,0.,1.));
#124098=DIRECTION('ref_axis',(1.,0.,0.));
#124099=DIRECTION('center_axis',(0.,-1.,0.));
#124100=DIRECTION('ref_axis',(0.,0.,1.));
#124101=DIRECTION('center_axis',(0.,1.,0.));
#124102=DIRECTION('ref_axis',(0.,0.,1.));
#124103=DIRECTION('center_axis',(-1.,0.,0.));
#124104=DIRECTION('ref_axis',(0.,0.,1.));
#124105=DIRECTION('center_axis',(1.,0.,0.));
#124106=DIRECTION('ref_axis',(0.,0.,-1.));
#124107=DIRECTION('',(-1.,0.,0.));
#124108=DIRECTION('',(1.,0.,0.));
#124109=DIRECTION('center_axis',(0.,0.,-1.));
#124110=DIRECTION('ref_axis',(-1.,0.,0.));
#124111=DIRECTION('center_axis',(0.,0.,1.));
#124112=DIRECTION('ref_axis',(1.,0.,0.));
#124113=DIRECTION('',(0.,0.,-1.));
#124114=DIRECTION('',(0.,0.,1.));
#124115=DIRECTION('center_axis',(0.,1.,0.));
#124116=DIRECTION('ref_axis',(0.,0.,1.));
#124117=DIRECTION('center_axis',(0.,-1.,0.));
#124118=DIRECTION('ref_axis',(0.,0.,1.));
#124119=DIRECTION('center_axis',(0.,1.,0.));
#124120=DIRECTION('ref_axis',(0.,0.,1.));
#124121=DIRECTION('center_axis',(1.,0.,0.));
#124122=DIRECTION('ref_axis',(0.,1.,0.));
#124123=DIRECTION('',(0.,-1.,0.));
#124124=DIRECTION('',(0.,-1.,0.));
#124125=DIRECTION('',(0.,3.03450170724806E-16,1.));
#124126=DIRECTION('center_axis',(0.,-1.,0.));
#124127=DIRECTION('ref_axis',(0.,0.,-1.));
#124128=DIRECTION('',(0.,-1.,0.));
#124129=DIRECTION('center_axis',(0.,1.,0.));
#124130=DIRECTION('ref_axis',(0.,0.,-1.));
#124131=DIRECTION('center_axis',(0.,-1.,0.));
#124132=DIRECTION('ref_axis',(0.,0.,-1.));
#124133=DIRECTION('',(0.,-1.,0.));
#124134=DIRECTION('center_axis',(0.,1.,0.));
#124135=DIRECTION('ref_axis',(0.,0.,-1.));
#124136=DIRECTION('center_axis',(1.,0.,0.));
#124137=DIRECTION('ref_axis',(0.,1.,0.));
#124138=DIRECTION('',(0.,-1.,0.));
#124139=DIRECTION('',(0.,0.,1.));
#124140=DIRECTION('',(0.,1.,0.));
#124141=DIRECTION('',(0.,0.,-1.));
#124142=DIRECTION('center_axis',(-1.,0.,0.));
#124143=DIRECTION('ref_axis',(0.,0.,1.));
#124144=DIRECTION('center_axis',(-1.,0.,0.));
#124145=DIRECTION('ref_axis',(0.,0.,1.));
#124146=DIRECTION('center_axis',(0.,1.,0.));
#124147=DIRECTION('ref_axis',(0.,0.,1.));
#124148=DIRECTION('center_axis',(0.,0.,1.));
#124149=DIRECTION('ref_axis',(1.,0.,0.));
#124150=DIRECTION('center_axis',(0.,1.,0.));
#124151=DIRECTION('ref_axis',(5.20417042793042E-15,0.,1.));
#124152=DIRECTION('center_axis',(1.,0.,0.));
#124153=DIRECTION('ref_axis',(0.,0.,-1.));
#124154=DIRECTION('center_axis',(0.,-1.,0.));
#124155=DIRECTION('ref_axis',(0.,0.,1.));
#124156=DIRECTION('center_axis',(0.,0.,1.));
#124157=DIRECTION('ref_axis',(-1.,0.,0.));
#124158=DIRECTION('center_axis',(0.,0.,1.));
#124159=DIRECTION('ref_axis',(1.,0.,0.));
#124160=DIRECTION('',(0.,0.,-1.));
#124161=DIRECTION('center_axis',(0.,1.,0.));
#124162=DIRECTION('ref_axis',(0.,0.,1.));
#124163=DIRECTION('center_axis',(-1.,0.,0.));
#124164=DIRECTION('ref_axis',(0.,0.,1.));
#124165=DIRECTION('center_axis',(0.,1.,0.));
#124166=DIRECTION('ref_axis',(0.,0.,1.));
#124167=DIRECTION('center_axis',(0.,-1.,0.));
#124168=DIRECTION('ref_axis',(0.,0.,1.));
#124169=DIRECTION('center_axis',(0.,-1.,0.));
#124170=DIRECTION('ref_axis',(0.,0.,-1.));
#124171=DIRECTION('',(0.,-1.,0.));
#124172=DIRECTION('center_axis',(0.,-1.,0.));
#124173=DIRECTION('ref_axis',(0.,0.,-1.));
#124174=DIRECTION('center_axis',(0.,-1.,0.));
#124175=DIRECTION('ref_axis',(0.,0.,-1.));
#124176=DIRECTION('center_axis',(1.,0.,0.));
#124177=DIRECTION('ref_axis',(0.,0.,-1.));
#124178=DIRECTION('center_axis',(0.,1.,0.));
#124179=DIRECTION('ref_axis',(0.,0.,-1.));
#124180=DIRECTION('center_axis',(0.,0.,-1.));
#124181=DIRECTION('ref_axis',(-1.,0.,0.));
#124182=DIRECTION('center_axis',(0.,-1.,0.));
#124183=DIRECTION('ref_axis',(0.,0.,-1.));
#124184=DIRECTION('center_axis',(0.,0.,-1.));
#124185=DIRECTION('ref_axis',(-1.,0.,0.));
#124186=DIRECTION('center_axis',(0.,1.,0.));
#124187=DIRECTION('ref_axis',(0.,0.,-1.));
#124188=DIRECTION('center_axis',(-1.,0.,0.));
#124189=DIRECTION('ref_axis',(0.,0.,1.));
#124190=DIRECTION('center_axis',(0.,-1.,0.));
#124191=DIRECTION('ref_axis',(0.,0.,-1.));
#124192=DIRECTION('center_axis',(0.,0.,1.));
#124193=DIRECTION('ref_axis',(-1.,0.,0.));
#124194=DIRECTION('',(0.,0.,1.));
#124195=DIRECTION('center_axis',(0.,-1.,0.));
#124196=DIRECTION('ref_axis',(0.,0.,-1.));
#124197=DIRECTION('',(0.,1.,0.));
#124198=DIRECTION('center_axis',(0.,-1.,0.));
#124199=DIRECTION('ref_axis',(0.,0.,-1.));
#124200=DIRECTION('',(0.,1.,0.));
#124201=DIRECTION('center_axis',(0.,1.,0.));
#124202=DIRECTION('ref_axis',(0.,0.,-1.));
#124203=DIRECTION('',(0.,-1.,0.));
#124204=DIRECTION('center_axis',(0.,-1.,0.));
#124205=DIRECTION('ref_axis',(-5.20417042793042E-15,0.,1.));
#124206=DIRECTION('center_axis',(0.,0.,1.));
#124207=DIRECTION('ref_axis',(1.,0.,0.));
#124208=DIRECTION('center_axis',(0.,0.,1.));
#124209=DIRECTION('ref_axis',(1.,0.,0.));
#124210=DIRECTION('',(0.,0.,-1.));
#124211=DIRECTION('center_axis',(0.,0.,1.));
#124212=DIRECTION('ref_axis',(1.,0.,0.));
#124213=DIRECTION('',(0.,0.,1.));
#124214=DIRECTION('center_axis',(0.,-1.,0.));
#124215=DIRECTION('ref_axis',(0.,0.,-1.));
#124216=DIRECTION('center_axis',(-1.,0.,0.));
#124217=DIRECTION('ref_axis',(0.,0.,1.));
#124218=DIRECTION('center_axis',(0.,-1.,0.));
#124219=DIRECTION('ref_axis',(0.,0.,-1.));
#124220=DIRECTION('center_axis',(0.,-1.,0.));
#124221=DIRECTION('ref_axis',(0.,0.,-1.));
#124222=DIRECTION('center_axis',(1.,0.,0.));
#124223=DIRECTION('ref_axis',(0.,0.,-1.));
#124224=DIRECTION('center_axis',(0.,1.,0.));
#124225=DIRECTION('ref_axis',(0.,0.,-1.));
#124226=DIRECTION('center_axis',(0.,-1.,0.));
#124227=DIRECTION('ref_axis',(0.,0.,-1.));
#124228=DIRECTION('center_axis',(0.,-1.,0.));
#124229=DIRECTION('ref_axis',(0.,0.,-1.));
#124230=DIRECTION('',(0.,1.,0.));
#124231=DIRECTION('',(0.,-1.,0.));
#124232=DIRECTION('center_axis',(0.,-1.,0.));
#124233=DIRECTION('ref_axis',(0.,0.,1.));
#124234=DIRECTION('center_axis',(0.,1.,0.));
#124235=DIRECTION('ref_axis',(0.,0.,1.));
#124236=DIRECTION('center_axis',(-1.,0.,0.));
#124237=DIRECTION('ref_axis',(0.,0.,1.));
#124238=DIRECTION('center_axis',(0.,1.,0.));
#124239=DIRECTION('ref_axis',(0.,0.,1.));
#124240=DIRECTION('center_axis',(0.,0.,-1.));
#124241=DIRECTION('ref_axis',(-1.,0.,0.));
#124242=DIRECTION('center_axis',(0.,0.,1.));
#124243=DIRECTION('ref_axis',(1.,0.,0.));
#124244=DIRECTION('',(0.,0.,-1.));
#124245=DIRECTION('center_axis',(0.,0.,-1.));
#124246=DIRECTION('ref_axis',(-1.,0.,0.));
#124247=DIRECTION('',(0.,0.,1.));
#124248=DIRECTION('center_axis',(0.,1.,0.));
#124249=DIRECTION('ref_axis',(0.,0.,1.));
#124250=DIRECTION('center_axis',(0.,1.,0.));
#124251=DIRECTION('ref_axis',(0.,0.,1.));
#124252=DIRECTION('center_axis',(1.,0.,0.));
#124253=DIRECTION('ref_axis',(0.,0.,-1.));
#124254=DIRECTION('center_axis',(-1.,0.,0.));
#124255=DIRECTION('ref_axis',(0.,0.,1.));
#124256=DIRECTION('center_axis',(-1.,0.,0.));
#124257=DIRECTION('ref_axis',(0.,0.,1.));
#124258=DIRECTION('center_axis',(-1.,0.,0.));
#124259=DIRECTION('ref_axis',(0.,0.,1.));
#124260=DIRECTION('center_axis',(0.,-1.,0.));
#124261=DIRECTION('ref_axis',(0.,0.,-1.));
#124262=DIRECTION('',(0.,-1.,0.));
#124263=DIRECTION('',(0.,-1.,0.));
#124264=DIRECTION('center_axis',(0.,-1.,0.));
#124265=DIRECTION('ref_axis',(0.,0.,-1.));
#124266=DIRECTION('center_axis',(0.,-1.,0.));
#124267=DIRECTION('ref_axis',(0.,0.,-1.));
#124268=DIRECTION('',(0.,-1.,0.));
#124269=DIRECTION('',(0.,-1.,0.));
#124270=DIRECTION('center_axis',(0.,-1.,0.));
#124271=DIRECTION('ref_axis',(0.,0.,-1.));
#124272=DIRECTION('center_axis',(-1.,0.,0.));
#124273=DIRECTION('ref_axis',(0.,0.,1.));
#124274=DIRECTION('',(1.,0.,0.));
#124275=DIRECTION('',(-1.,0.,0.));
#124276=DIRECTION('center_axis',(0.,0.,-1.));
#124277=DIRECTION('ref_axis',(0.,-1.,0.));
#124278=DIRECTION('',(1.,0.,0.));
#124279=DIRECTION('center_axis',(-1.,0.,0.));
#124280=DIRECTION('ref_axis',(0.,0.,1.));
#124281=DIRECTION('',(-1.,0.,0.));
#124282=DIRECTION('center_axis',(0.,-1.,0.));
#124283=DIRECTION('ref_axis',(0.,0.,-1.));
#124284=DIRECTION('',(1.,0.,0.));
#124285=DIRECTION('center_axis',(1.,0.,0.));
#124286=DIRECTION('ref_axis',(0.,0.,-1.));
#124287=DIRECTION('',(-1.,0.,0.));
#124288=DIRECTION('center_axis',(0.,0.,1.));
#124289=DIRECTION('ref_axis',(1.,0.,0.));
#124290=DIRECTION('',(1.,0.,0.));
#124291=DIRECTION('center_axis',(1.,0.,0.));
#124292=DIRECTION('ref_axis',(0.,0.,-1.));
#124293=DIRECTION('',(-1.,0.,0.));
#124294=DIRECTION('center_axis',(0.,1.,0.));
#124295=DIRECTION('ref_axis',(1.,0.,0.));
#124296=DIRECTION('center_axis',(0.,0.,1.));
#124297=DIRECTION('ref_axis',(1.,0.,0.));
#124298=DIRECTION('',(1.,0.,0.));
#124299=DIRECTION('center_axis',(0.,0.,-1.));
#124300=DIRECTION('ref_axis',(0.,-1.,0.));
#124301=DIRECTION('',(-1.,0.,0.));
#124302=DIRECTION('center_axis',(-1.,0.,0.));
#124303=DIRECTION('ref_axis',(0.,0.,1.));
#124304=DIRECTION('',(-1.,0.,0.));
#124305=DIRECTION('center_axis',(-1.,0.,0.));
#124306=DIRECTION('ref_axis',(0.,0.,1.));
#124307=DIRECTION('',(-1.,0.,0.));
#124308=DIRECTION('center_axis',(-1.,0.,0.));
#124309=DIRECTION('ref_axis',(0.,0.,1.));
#124310=DIRECTION('',(0.,3.03450170724806E-16,1.));
#124311=DIRECTION('center_axis',(0.,-1.,3.03450170724806E-16));
#124312=DIRECTION('ref_axis',(-1.,0.,0.));
#124313=DIRECTION('center_axis',(0.,0.,-1.));
#124314=DIRECTION('ref_axis',(1.,0.,0.));
#124315=DIRECTION('center_axis',(1.,0.,0.));
#124316=DIRECTION('ref_axis',(0.,0.,1.));
#124317=DIRECTION('center_axis',(0.0436193873653361,0.,0.999048221581858));
#124318=DIRECTION('ref_axis',(-0.999048221581858,0.,0.0436193873653362));
#124319=DIRECTION('center_axis',(0.0436193873653361,0.,-0.999048221581858));
#124320=DIRECTION('ref_axis',(0.999048221581858,0.,0.0436193873653362));
#124321=DIRECTION('center_axis',(-1.,0.,0.));
#124322=DIRECTION('ref_axis',(0.,0.,1.));
#124323=DIRECTION('center_axis',(-1.,0.,0.));
#124324=DIRECTION('ref_axis',(0.,0.,1.));
#124325=DIRECTION('center_axis',(-1.,0.,0.));
#124326=DIRECTION('ref_axis',(0.,0.,1.));
#124327=DIRECTION('center_axis',(0.,-1.,0.));
#124328=DIRECTION('ref_axis',(0.,0.,-1.));
#124329=DIRECTION('center_axis',(-1.,0.,0.));
#124330=DIRECTION('ref_axis',(0.,0.,1.));
#124331=DIRECTION('center_axis',(-1.,0.,0.));
#124332=DIRECTION('ref_axis',(0.,0.,1.));
#124333=DIRECTION('center_axis',(0.,-1.,0.));
#124334=DIRECTION('ref_axis',(0.,0.,-1.));
#124335=DIRECTION('center_axis',(1.,0.,0.));
#124336=DIRECTION('ref_axis',(0.,0.,1.));
#124337=DIRECTION('center_axis',(1.,0.,0.));
#124338=DIRECTION('ref_axis',(0.,0.,1.));
#124339=DIRECTION('center_axis',(-1.,0.,0.));
#124340=DIRECTION('ref_axis',(0.,0.,1.));
#124341=DIRECTION('center_axis',(-1.,0.,0.));
#124342=DIRECTION('ref_axis',(0.,0.,1.));
#124343=DIRECTION('',(0.,1.,0.));
#124344=DIRECTION('center_axis',(-1.,0.,0.));
#124345=DIRECTION('ref_axis',(0.,0.,1.));
#124346=DIRECTION('',(0.,-1.,0.));
#124347=DIRECTION('center_axis',(-0.0436193873653361,0.,-0.999048221581858));
#124348=DIRECTION('ref_axis',(-0.999048221581858,0.,0.0436193873653361));
#124349=DIRECTION('',(-0.999048221581858,-8.07120802883996E-16,0.0436193873653362));
#124350=DIRECTION('',(-0.999048221581858,0.,0.0436193873653362));
#124351=DIRECTION('center_axis',(1.,0.,0.));
#124352=DIRECTION('ref_axis',(0.,0.,1.));
#124353=DIRECTION('',(-0.999048221581858,0.,-0.0436193873653362));
#124354=DIRECTION('center_axis',(-0.0436193873653361,0.,0.999048221581858));
#124355=DIRECTION('ref_axis',(0.,1.,0.));
#124356=DIRECTION('',(-0.999048221581858,0.,-0.0436193873653362));
#124357=DIRECTION('center_axis',(1.,0.,0.));
#124358=DIRECTION('ref_axis',(0.,0.,1.));
#124359=DIRECTION('center_axis',(-1.,0.,0.));
#124360=DIRECTION('ref_axis',(0.,0.,1.));
#124361=DIRECTION('center_axis',(-1.,0.,0.));
#124362=DIRECTION('ref_axis',(0.,0.,1.));
#124363=DIRECTION('center_axis',(1.,0.,0.));
#124364=DIRECTION('ref_axis',(0.,0.,-1.));
#124365=DIRECTION('center_axis',(-1.,0.,0.));
#124366=DIRECTION('ref_axis',(0.,0.,1.));
#124367=DIRECTION('',(-1.,0.,0.));
#124368=DIRECTION('center_axis',(1.,0.,0.));
#124369=DIRECTION('ref_axis',(0.,0.,-1.));
#124370=DIRECTION('',(-1.,0.,0.));
#124371=DIRECTION('center_axis',(-1.,0.,0.));
#124372=DIRECTION('ref_axis',(0.,0.,1.));
#124373=DIRECTION('center_axis',(-0.707106781186548,-0.707106781186548,
-8.73049632275228E-17));
#124374=DIRECTION('ref_axis',(0.707106781186548,-0.707106781186548,1.64082548650651E-34));
#124375=DIRECTION('center_axis',(0.707106781186548,0.707106781186548,0.));
#124376=DIRECTION('ref_axis',(-0.707106781186548,0.707106781186548,0.));
#124377=DIRECTION('',(-0.707106781186549,-0.707106781186546,-8.73049632275229E-17));
#124378=DIRECTION('',(0.707106781186549,0.707106781186546,8.73049632275229E-17));
#124379=DIRECTION('center_axis',(0.,-1.23467863058847E-16,1.));
#124380=DIRECTION('ref_axis',(0.,-1.,0.));
#124381=DIRECTION('center_axis',(1.,0.,-1.38777878078144E-14));
#124382=DIRECTION('ref_axis',(-1.38777878078144E-14,0.,-1.));
#124383=DIRECTION('center_axis',(-1.19942256323048E-29,1.16517322770923E-42,
-1.));
#124384=DIRECTION('ref_axis',(-9.71445146547011E-14,-1.,-7.96545955566226E-58));
#124385=DIRECTION('center_axis',(0.,0.,1.));
#124386=DIRECTION('ref_axis',(0.,-1.,0.));
#124387=DIRECTION('center_axis',(-1.,0.,-8.56730402307488E-31));
#124388=DIRECTION('ref_axis',(0.,-1.,0.));
#124389=DIRECTION('center_axis',(1.,0.,0.));
#124390=DIRECTION('ref_axis',(0.,0.,-1.));
#124391=DIRECTION('',(-1.,-6.93889390390722E-15,-8.56730402307488E-31));
#124392=DIRECTION('',(1.,6.93889390390722E-15,8.56730402307488E-31));
#124393=DIRECTION('center_axis',(0.,-1.23467863058847E-16,1.));
#124394=DIRECTION('ref_axis',(0.,-1.,0.));
#124395=DIRECTION('center_axis',(0.,-1.,0.));
#124396=DIRECTION('ref_axis',(0.,0.,-1.));
#124397=DIRECTION('center_axis',(0.,0.,-1.));
#124398=DIRECTION('ref_axis',(0.,-1.,0.));
#124399=DIRECTION('center_axis',(0.,0.,1.));
#124400=DIRECTION('ref_axis',(0.,-1.,0.));
#124401=DIRECTION('center_axis',(0.,1.,0.));
#124402=DIRECTION('ref_axis',(0.,0.,1.));
#124403=DIRECTION('',(0.,1.,1.23467863058847E-16));
#124404=DIRECTION('',(0.,-1.,-1.23467863058847E-16));
#124405=DIRECTION('center_axis',(0.,1.,0.));
#124406=DIRECTION('ref_axis',(0.,0.,1.));
#124407=DIRECTION('center_axis',(0.,-1.,0.));
#124408=DIRECTION('ref_axis',(0.,0.,-1.));
#124409=DIRECTION('',(0.,1.,1.23467863058847E-16));
#124410=DIRECTION('center_axis',(0.,-1.,0.));
#124411=DIRECTION('ref_axis',(0.,0.,1.));
#124412=DIRECTION('',(0.,-1.,-1.23467863058847E-16));
#124413=DIRECTION('center_axis',(0.,-1.23467863058847E-16,1.));
#124414=DIRECTION('ref_axis',(0.,-1.,0.));
#124415=DIRECTION('center_axis',(-1.,2.77555756156289E-14,0.));
#124416=DIRECTION('ref_axis',(-2.77555756156289E-14,-1.,0.));
#124417=DIRECTION('center_axis',(0.,0.,-1.));
#124418=DIRECTION('ref_axis',(0.,-1.,0.));
#124419=DIRECTION('center_axis',(0.,0.,1.));
#124420=DIRECTION('ref_axis',(0.,-1.,0.));
#124421=DIRECTION('center_axis',(1.,-2.77555756156289E-14,-3.42692160922995E-30));
#124422=DIRECTION('ref_axis',(2.77555756156289E-14,1.,-4.38683821655986E-59));
#124423=DIRECTION('center_axis',(-1.,2.77555756156289E-14,0.));
#124424=DIRECTION('ref_axis',(-2.77555756156289E-14,-1.,0.));
#124425=DIRECTION('',(1.,-2.77555756156289E-14,-3.42692160922995E-30));
#124426=DIRECTION('',(-1.,2.77555756156289E-14,3.42692160922995E-30));
#124427=DIRECTION('center_axis',(0.,-1.23467863058847E-16,1.));
#124428=DIRECTION('ref_axis',(0.,-1.,0.));
#124429=DIRECTION('center_axis',(-0.707106781186548,0.707106781186548,0.));
#124430=DIRECTION('ref_axis',(-0.707106781186548,-0.707106781186548,0.));
#124431=DIRECTION('center_axis',(0.,0.,-1.));
#124432=DIRECTION('ref_axis',(0.,-1.,0.));
#124433=DIRECTION('center_axis',(0.,0.,1.));
#124434=DIRECTION('ref_axis',(0.,-1.,0.));
#124435=DIRECTION('center_axis',(0.707106781186548,-0.707106781186548,-8.73049632275231E-17));
#124436=DIRECTION('ref_axis',(0.707106781186548,0.707106781186548,-4.20650685500144E-34));
#124437=DIRECTION('',(0.707106781186546,-0.707106781186549,-8.73049632275233E-17));
#124438=DIRECTION('',(-0.707106781186546,0.707106781186549,8.73049632275232E-17));
#124439=DIRECTION('center_axis',(0.,0.,-1.));
#124440=DIRECTION('ref_axis',(-1.,0.,0.));
#124441=DIRECTION('center_axis',(0.,0.,-1.));
#124442=DIRECTION('ref_axis',(-1.,0.,0.));
#124443=DIRECTION('',(1.03377769602066E-32,0.,1.));
#124444=DIRECTION('center_axis',(0.,0.,-1.));
#124445=DIRECTION('ref_axis',(0.,-1.,0.));
#124446=DIRECTION('',(-1.03377769602066E-32,-1.51929083932157E-64,-1.));
#124447=DIRECTION('center_axis',(0.,1.,0.));
#124448=DIRECTION('ref_axis',(0.,0.,1.));
#124449=DIRECTION('center_axis',(1.,0.,0.));
#124450=DIRECTION('ref_axis',(0.,0.,-1.));
#124451=DIRECTION('center_axis',(0.,-1.,0.));
#124452=DIRECTION('ref_axis',(0.,0.,1.));
#124453=DIRECTION('center_axis',(0.,1.,0.));
#124454=DIRECTION('ref_axis',(0.,0.,1.));
#124455=DIRECTION('center_axis',(1.,0.,0.));
#124456=DIRECTION('ref_axis',(0.,0.,-1.));
#124457=DIRECTION('center_axis',(1.,0.,0.));
#124458=DIRECTION('ref_axis',(0.,0.,-1.));
#124459=DIRECTION('',(-1.,0.,0.));
#124460=DIRECTION('',(1.,0.,0.));
#124461=DIRECTION('center_axis',(0.,-1.23467863058847E-16,1.));
#124462=DIRECTION('ref_axis',(0.,-1.,0.));
#124463=DIRECTION('center_axis',(0.139173100960066,0.99026806874157,0.));
#124464=DIRECTION('ref_axis',(-0.99026806874157,0.139173100960066,0.));
#124465=DIRECTION('center_axis',(0.,0.,1.));
#124466=DIRECTION('ref_axis',(0.,-1.,0.));
#124467=DIRECTION('center_axis',(0.,0.,-1.));
#124468=DIRECTION('ref_axis',(0.,-1.,0.));
#124469=DIRECTION('center_axis',(-0.139173100960066,-0.99026806874157,-1.22266282302934E-16));
#124470=DIRECTION('ref_axis',(0.99026806874157,-0.139173100960066,-1.22723965167578E-33));
#124471=DIRECTION('center_axis',(0.139173100960066,0.99026806874157,0.));
#124472=DIRECTION('ref_axis',(-0.99026806874157,0.139173100960066,0.));
#124473=DIRECTION('',(-0.139173100960065,-0.99026806874157,-1.22266282302933E-16));
#124474=DIRECTION('',(0.139173100960065,0.99026806874157,1.22266282302933E-16));
#124475=DIRECTION('center_axis',(0.,-1.23467863058847E-16,1.));
#124476=DIRECTION('ref_axis',(0.,-1.,0.));
#124477=DIRECTION('center_axis',(-1.,0.,0.));
#124478=DIRECTION('ref_axis',(0.,0.,1.));
#124479=DIRECTION('center_axis',(0.,0.,1.));
#124480=DIRECTION('ref_axis',(0.,-1.,0.));
#124481=DIRECTION('center_axis',(0.,0.,-1.));
#124482=DIRECTION('ref_axis',(0.,-1.,0.));
#124483=DIRECTION('center_axis',(-1.,0.,0.));
#124484=DIRECTION('ref_axis',(0.,0.,1.));
#124485=DIRECTION('center_axis',(-1.,0.,0.));
#124486=DIRECTION('ref_axis',(0.,0.,1.));
#124487=DIRECTION('',(1.,0.,0.));
#124488=DIRECTION('',(-1.,0.,0.));
#124489=DIRECTION('center_axis',(0.,-1.,0.));
#124490=DIRECTION('ref_axis',(0.,0.,-1.));
#124491=DIRECTION('center_axis',(0.,0.,1.));
#124492=DIRECTION('ref_axis',(1.,0.,0.));
#124493=DIRECTION('center_axis',(0.,1.,0.));
#124494=DIRECTION('ref_axis',(0.,0.,-1.));
#124495=DIRECTION('center_axis',(0.,-1.,0.));
#124496=DIRECTION('ref_axis',(0.,0.,-1.));
#124497=DIRECTION('center_axis',(0.,0.,1.));
#124498=DIRECTION('ref_axis',(1.,0.,0.));
#124499=DIRECTION('center_axis',(0.,0.,-1.));
#124500=DIRECTION('ref_axis',(0.,-1.,0.));
#124501=DIRECTION('',(-1.03377769602066E-32,0.,-1.));
#124502=DIRECTION('',(1.03377769602066E-32,1.51929083932157E-64,1.));
#124503=DIRECTION('center_axis',(1.3684555315672E-48,0.,1.));
#124504=DIRECTION('ref_axis',(0.,-1.,0.));
#124505=DIRECTION('center_axis',(0.,0.,-1.));
#124506=DIRECTION('ref_axis',(0.,-1.,0.));
#124507=DIRECTION('',(-1.3684555315672E-48,1.23467863058847E-16,-1.));
#124508=DIRECTION('center_axis',(0.,0.,-1.));
#124509=DIRECTION('ref_axis',(-1.,0.,0.));
#124510=DIRECTION('',(1.3684555315672E-48,-1.23467863058847E-16,1.));
#124511=DIRECTION('center_axis',(0.,1.,1.23467863058847E-16));
#124512=DIRECTION('ref_axis',(0.,0.,1.));
#124513=DIRECTION('center_axis',(1.,0.,0.));
#124514=DIRECTION('ref_axis',(0.,0.,-1.));
#124515=DIRECTION('center_axis',(0.,-1.,0.));
#124516=DIRECTION('ref_axis',(0.,0.,1.));
#124517=DIRECTION('center_axis',(0.,1.,0.));
#124518=DIRECTION('ref_axis',(0.,0.,1.));
#124519=DIRECTION('center_axis',(1.,0.,0.));
#124520=DIRECTION('ref_axis',(0.,0.,-1.));
#124521=DIRECTION('center_axis',(1.,0.,0.));
#124522=DIRECTION('ref_axis',(0.,0.,-1.));
#124523=DIRECTION('',(-1.,0.,0.));
#124524=DIRECTION('',(1.,0.,0.));
#124525=DIRECTION('center_axis',(0.,-1.23467863058847E-16,1.));
#124526=DIRECTION('ref_axis',(0.,-1.,0.));
#124527=DIRECTION('center_axis',(-0.707106781186548,0.707106781186548,0.));
#124528=DIRECTION('ref_axis',(-0.707106781186548,-0.707106781186548,0.));
#124529=DIRECTION('center_axis',(0.,0.,1.));
#124530=DIRECTION('ref_axis',(0.,-1.,0.));
#124531=DIRECTION('center_axis',(0.,0.,-1.));
#124532=DIRECTION('ref_axis',(0.,-1.,0.));
#124533=DIRECTION('center_axis',(-0.707106781186548,0.707106781186548,8.73049632275231E-17));
#124534=DIRECTION('ref_axis',(-0.707106781186548,-0.707106781186548,8.65064369663437E-31));
#124535=DIRECTION('',(0.707106781186546,-0.707106781186549,-8.73049632275232E-17));
#124536=DIRECTION('',(-0.707106781186546,0.707106781186549,8.73049632275232E-17));
#124537=DIRECTION('center_axis',(0.,0.,-1.));
#124538=DIRECTION('ref_axis',(-1.,0.,0.));
#124539=DIRECTION('center_axis',(0.,0.,-1.));
#124540=DIRECTION('ref_axis',(-1.,0.,0.));
#124541=DIRECTION('',(1.03377769602066E-32,0.,1.));
#124542=DIRECTION('center_axis',(0.,0.,-1.));
#124543=DIRECTION('ref_axis',(0.,-1.,0.));
#124544=DIRECTION('',(-1.03377769602066E-32,-1.51929083932157E-64,-1.));
#124545=DIRECTION('center_axis',(0.,1.,0.));
#124546=DIRECTION('ref_axis',(0.,0.,1.));
#124547=DIRECTION('center_axis',(1.,0.,0.));
#124548=DIRECTION('ref_axis',(0.,0.,-1.));
#124549=DIRECTION('center_axis',(0.,-1.,0.));
#124550=DIRECTION('ref_axis',(0.,0.,1.));
#124551=DIRECTION('center_axis',(0.,1.,0.));
#124552=DIRECTION('ref_axis',(0.,0.,1.));
#124553=DIRECTION('center_axis',(1.,0.,0.));
#124554=DIRECTION('ref_axis',(0.,0.,-1.));
#124555=DIRECTION('center_axis',(1.,0.,0.));
#124556=DIRECTION('ref_axis',(0.,0.,-1.));
#124557=DIRECTION('',(-1.,0.,0.));
#124558=DIRECTION('',(1.,0.,0.));
#124559=DIRECTION('center_axis',(0.,-1.23467863058847E-16,1.));
#124560=DIRECTION('ref_axis',(0.,-1.,0.));
#124561=DIRECTION('center_axis',(0.272177601648339,0.962247033334454,0.));
#124562=DIRECTION('ref_axis',(-0.962247033334454,0.272177601648339,0.));
#124563=DIRECTION('center_axis',(0.,0.,1.));
#124564=DIRECTION('ref_axis',(0.,-1.,0.));
#124565=DIRECTION('center_axis',(0.,0.,-1.));
#124566=DIRECTION('ref_axis',(0.,-1.,0.));
#124567=DIRECTION('center_axis',(0.,-1.23467863058847E-16,1.));
#124568=DIRECTION('ref_axis',(0.,-1.,0.));
#124569=DIRECTION('center_axis',(0.139173100960066,0.99026806874157,0.));
#124570=DIRECTION('ref_axis',(-0.99026806874157,0.139173100960066,0.));
#124571=DIRECTION('center_axis',(0.,0.,1.));
#124572=DIRECTION('ref_axis',(0.,-1.,0.));
#124573=DIRECTION('center_axis',(0.,0.,-1.));
#124574=DIRECTION('ref_axis',(0.,-1.,0.));
#124575=DIRECTION('center_axis',(-0.139173100960066,-0.99026806874157,-1.22266282302934E-16));
#124576=DIRECTION('ref_axis',(0.99026806874157,-0.139173100960066,-1.22723965167578E-33));
#124577=DIRECTION('center_axis',(0.139173100960066,0.99026806874157,0.));
#124578=DIRECTION('ref_axis',(-0.99026806874157,0.139173100960066,0.));
#124579=DIRECTION('',(-0.139173100960065,-0.99026806874157,-1.22266282302933E-16));
#124580=DIRECTION('',(0.139173100960065,0.99026806874157,1.22266282302933E-16));
#124581=DIRECTION('center_axis',(0.,-1.23467863058847E-16,1.));
#124582=DIRECTION('ref_axis',(0.,-1.,0.));
#124583=DIRECTION('center_axis',(-1.,0.,0.));
#124584=DIRECTION('ref_axis',(0.,0.,1.));
#124585=DIRECTION('center_axis',(0.,0.,1.));
#124586=DIRECTION('ref_axis',(0.,-1.,0.));
#124587=DIRECTION('center_axis',(0.,0.,-1.));
#124588=DIRECTION('ref_axis',(0.,-1.,0.));
#124589=DIRECTION('center_axis',(-1.,0.,0.));
#124590=DIRECTION('ref_axis',(0.,0.,1.));
#124591=DIRECTION('center_axis',(-1.,0.,0.));
#124592=DIRECTION('ref_axis',(0.,0.,1.));
#124593=DIRECTION('',(1.,0.,0.));
#124594=DIRECTION('',(-1.,0.,0.));
#124595=DIRECTION('center_axis',(0.,-1.,0.));
#124596=DIRECTION('ref_axis',(0.,0.,-1.));
#124597=DIRECTION('center_axis',(0.,0.,1.));
#124598=DIRECTION('ref_axis',(1.,0.,0.));
#124599=DIRECTION('center_axis',(0.,1.,0.));
#124600=DIRECTION('ref_axis',(0.,0.,-1.));
#124601=DIRECTION('center_axis',(0.,-1.,0.));
#124602=DIRECTION('ref_axis',(0.,0.,-1.));
#124603=DIRECTION('center_axis',(0.,0.,1.));
#124604=DIRECTION('ref_axis',(1.,0.,0.));
#124605=DIRECTION('center_axis',(0.,0.,-1.));
#124606=DIRECTION('ref_axis',(0.,-1.,0.));
#124607=DIRECTION('',(-1.03377769602066E-32,0.,-1.));
#124608=DIRECTION('',(1.03377769602066E-32,1.51929083932157E-64,1.));
#124609=DIRECTION('center_axis',(0.,-2.74330011127376E-48,-1.));
#124610=DIRECTION('ref_axis',(-1.,0.,0.));
#124611=DIRECTION('center_axis',(0.,0.,-1.));
#124612=DIRECTION('ref_axis',(-1.,0.,0.));
#124613=DIRECTION('',(1.03377769602066E-32,2.74330011127376E-48,1.));
#124614=DIRECTION('center_axis',(0.,0.,-1.));
#124615=DIRECTION('ref_axis',(0.,-1.,0.));
#124616=DIRECTION('',(-1.03377769602066E-32,-2.74330011127376E-48,-1.));
#124617=DIRECTION('center_axis',(-2.65366540778891E-16,1.,0.));
#124618=DIRECTION('ref_axis',(-1.,0.,0.));
#124619=DIRECTION('center_axis',(1.,0.,0.));
#124620=DIRECTION('ref_axis',(0.,0.,-1.));
#124621=DIRECTION('center_axis',(0.,-1.,0.));
#124622=DIRECTION('ref_axis',(-1.,0.,0.));
#124623=DIRECTION('center_axis',(0.,1.,0.));
#124624=DIRECTION('ref_axis',(-1.,0.,0.));
#124625=DIRECTION('center_axis',(1.,0.,3.27642397172882E-32));
#124626=DIRECTION('ref_axis',(0.,1.,0.));
#124627=DIRECTION('center_axis',(1.,0.,0.));
#124628=DIRECTION('ref_axis',(0.,0.,-1.));
#124629=DIRECTION('',(-1.,-2.65366540778891E-16,-3.27642397172882E-32));
#124630=DIRECTION('',(1.,2.65366540778891E-16,3.27642397172882E-32));
#124631=DIRECTION('center_axis',(0.,-1.23467863058847E-16,1.));
#124632=DIRECTION('ref_axis',(0.,-1.,0.));
#124633=DIRECTION('center_axis',(0.299364406779191,0.954138853602421,0.));
#124634=DIRECTION('ref_axis',(-0.954138853602421,0.299364406779191,0.));
#124635=DIRECTION('center_axis',(0.,0.,1.));
#124636=DIRECTION('ref_axis',(0.,-1.,0.));
#124637=DIRECTION('center_axis',(0.,0.,-1.));
#124638=DIRECTION('ref_axis',(0.,-1.,0.));
#124639=DIRECTION('center_axis',(0.,-1.23467863058847E-16,1.));
#124640=DIRECTION('ref_axis',(0.,-1.,0.));
#124641=DIRECTION('center_axis',(0.395127118643591,0.918626452978801,0.));
#124642=DIRECTION('ref_axis',(-0.918626452978801,0.395127118643591,0.));
#124643=DIRECTION('center_axis',(-2.74153728738396E-30,6.08743563864414E-44,
-1.));
#124644=DIRECTION('ref_axis',(-2.22044604925031E-14,-1.,9.95682444457782E-59));
#124645=DIRECTION('center_axis',(0.,0.,1.));
#124646=DIRECTION('ref_axis',(0.,-1.,0.));
#124647=DIRECTION('center_axis',(0.,-1.23467863058847E-16,1.));
#124648=DIRECTION('ref_axis',(0.,-1.,0.));
#124649=DIRECTION('center_axis',(-1.,0.,0.));
#124650=DIRECTION('ref_axis',(0.,0.,1.));
#124651=DIRECTION('center_axis',(0.,0.,1.));
#124652=DIRECTION('ref_axis',(0.,-1.,0.));
#124653=DIRECTION('center_axis',(0.,0.,-1.));
#124654=DIRECTION('ref_axis',(0.,-1.,0.));
#124655=DIRECTION('center_axis',(-1.,0.,0.));
#124656=DIRECTION('ref_axis',(0.,0.,1.));
#124657=DIRECTION('center_axis',(-1.,0.,0.));
#124658=DIRECTION('ref_axis',(0.,0.,1.));
#124659=DIRECTION('',(1.,0.,0.));
#124660=DIRECTION('',(-1.,0.,0.));
#124661=DIRECTION('center_axis',(0.,-1.,0.));
#124662=DIRECTION('ref_axis',(0.,0.,-1.));
#124663=DIRECTION('center_axis',(0.,0.,1.));
#124664=DIRECTION('ref_axis',(1.,0.,0.));
#124665=DIRECTION('center_axis',(0.,1.,0.));
#124666=DIRECTION('ref_axis',(0.,0.,-1.));
#124667=DIRECTION('center_axis',(0.,-1.,0.));
#124668=DIRECTION('ref_axis',(0.,0.,-1.));
#124669=DIRECTION('center_axis',(0.,0.,1.));
#124670=DIRECTION('ref_axis',(1.,0.,0.));
#124671=DIRECTION('center_axis',(0.,0.,-1.));
#124672=DIRECTION('ref_axis',(0.,-1.,0.));
#124673=DIRECTION('',(-1.03377769602066E-32,0.,-1.));
#124674=DIRECTION('',(1.03377769602066E-32,1.51929083932157E-64,1.));
#124675=DIRECTION('center_axis',(0.,0.,-1.));
#124676=DIRECTION('ref_axis',(-1.,0.,0.));
#124677=DIRECTION('center_axis',(0.,0.,-1.));
#124678=DIRECTION('ref_axis',(-1.,0.,0.));
#124679=DIRECTION('',(1.03377769602066E-32,0.,1.));
#124680=DIRECTION('center_axis',(0.,0.,-1.));
#124681=DIRECTION('ref_axis',(0.,-1.,0.));
#124682=DIRECTION('',(-1.03377769602066E-32,-1.51929083932157E-64,-1.));
#124683=DIRECTION('center_axis',(0.,1.,0.));
#124684=DIRECTION('ref_axis',(0.,0.,1.));
#124685=DIRECTION('center_axis',(1.,0.,0.));
#124686=DIRECTION('ref_axis',(0.,0.,-1.));
#124687=DIRECTION('center_axis',(0.,-1.,0.));
#124688=DIRECTION('ref_axis',(0.,0.,1.));
#124689=DIRECTION('center_axis',(0.,1.,0.));
#124690=DIRECTION('ref_axis',(0.,0.,1.));
#124691=DIRECTION('center_axis',(1.,0.,0.));
#124692=DIRECTION('ref_axis',(0.,0.,-1.));
#124693=DIRECTION('center_axis',(1.,0.,0.));
#124694=DIRECTION('ref_axis',(0.,0.,-1.));
#124695=DIRECTION('',(-1.,0.,0.));
#124696=DIRECTION('',(1.,0.,0.));
#124697=DIRECTION('center_axis',(0.,-1.23467863058847E-16,1.));
#124698=DIRECTION('ref_axis',(0.,-1.,0.));
#124699=DIRECTION('center_axis',(0.161228813558844,0.986917053089269,0.));
#124700=DIRECTION('ref_axis',(-0.986917053089269,0.161228813558844,0.));
#124701=DIRECTION('center_axis',(0.,0.,1.));
#124702=DIRECTION('ref_axis',(0.,-1.,0.));
#124703=DIRECTION('center_axis',(8.56730402307488E-31,5.94476136586342E-45,
-1.));
#124704=DIRECTION('ref_axis',(6.93889390390722E-15,-1.,-9.95682444457783E-60));
#124705=DIRECTION('center_axis',(0.,-1.23467863058847E-16,1.));
#124706=DIRECTION('ref_axis',(0.,-1.,0.));
#124707=DIRECTION('center_axis',(0.256991525423251,0.966413656702258,0.));
#124708=DIRECTION('ref_axis',(-0.966413656702259,0.256991525423251,0.));
#124709=DIRECTION('center_axis',(-4.16713667682363E-30,1.40644112995234E-43,
-1.));
#124710=DIRECTION('ref_axis',(-3.37507799486048E-14,-1.,3.98272977783113E-59));
#124711=DIRECTION('center_axis',(0.,0.,1.));
#124712=DIRECTION('ref_axis',(0.,-1.,0.));
#124713=DIRECTION('center_axis',(0.,-1.23467863058847E-16,1.));
#124714=DIRECTION('ref_axis',(0.,-1.,0.));
#124715=DIRECTION('center_axis',(-1.,0.,0.));
#124716=DIRECTION('ref_axis',(0.,0.,1.));
#124717=DIRECTION('center_axis',(0.,0.,1.));
#124718=DIRECTION('ref_axis',(0.,-1.,0.));
#124719=DIRECTION('center_axis',(0.,0.,-1.));
#124720=DIRECTION('ref_axis',(0.,-1.,0.));
#124721=DIRECTION('center_axis',(-1.,0.,-3.39012271766808E-32));
#124722=DIRECTION('ref_axis',(0.,-1.,0.));
#124723=DIRECTION('center_axis',(-1.,0.,0.));
#124724=DIRECTION('ref_axis',(0.,0.,1.));
#124725=DIRECTION('',(1.,2.74575313258015E-16,3.39012271766808E-32));
#124726=DIRECTION('',(-1.,-2.74575313258015E-16,-3.39012271766808E-32));
#124727=DIRECTION('center_axis',(2.74575313258015E-16,-1.,0.));
#124728=DIRECTION('ref_axis',(1.,0.,0.));
#124729=DIRECTION('center_axis',(0.,0.,1.));
#124730=DIRECTION('ref_axis',(1.,0.,0.));
#124731=DIRECTION('center_axis',(0.,1.,0.));
#124732=DIRECTION('ref_axis',(1.,0.,0.));
#124733=DIRECTION('center_axis',(0.,-1.,0.));
#124734=DIRECTION('ref_axis',(1.,0.,0.));
#124735=DIRECTION('center_axis',(0.,2.83849834724024E-48,1.));
#124736=DIRECTION('ref_axis',(1.,0.,0.));
#124737=DIRECTION('center_axis',(0.,0.,-1.));
#124738=DIRECTION('ref_axis',(0.,-1.,0.));
#124739=DIRECTION('',(-1.03377769602066E-32,-2.83849834724023E-48,-1.));
#124740=DIRECTION('',(1.03377769602066E-32,2.83849834724023E-48,1.));
#124741=DIRECTION('center_axis',(0.,0.,-1.));
#124742=DIRECTION('ref_axis',(-1.,0.,0.));
#124743=DIRECTION('center_axis',(0.,0.,-1.));
#124744=DIRECTION('ref_axis',(-1.,0.,0.));
#124745=DIRECTION('',(1.03377769602066E-32,0.,1.));
#124746=DIRECTION('center_axis',(0.,0.,-1.));
#124747=DIRECTION('ref_axis',(0.,-1.,0.));
#124748=DIRECTION('',(-1.03377769602066E-32,-1.51929083932157E-64,-1.));
#124749=DIRECTION('center_axis',(0.,1.,0.));
#124750=DIRECTION('ref_axis',(0.,0.,1.));
#124751=DIRECTION('center_axis',(1.,0.,0.));
#124752=DIRECTION('ref_axis',(0.,0.,-1.));
#124753=DIRECTION('center_axis',(0.,-1.,0.));
#124754=DIRECTION('ref_axis',(0.,0.,1.));
#124755=DIRECTION('center_axis',(0.,1.,0.));
#124756=DIRECTION('ref_axis',(0.,0.,1.));
#124757=DIRECTION('center_axis',(1.,0.,0.));
#124758=DIRECTION('ref_axis',(0.,0.,-1.));
#124759=DIRECTION('center_axis',(1.,0.,0.));
#124760=DIRECTION('ref_axis',(0.,0.,-1.));
#124761=DIRECTION('',(-1.,0.,0.));
#124762=DIRECTION('',(1.,0.,0.));
#124763=DIRECTION('center_axis',(0.,-1.23467863058847E-16,1.));
#124764=DIRECTION('ref_axis',(0.,-1.,0.));
#124765=DIRECTION('center_axis',(0.0230932203385063,0.999733316027028,0.));
#124766=DIRECTION('ref_axis',(-0.999733316027028,0.0230932203385063,0.));
#124767=DIRECTION('center_axis',(0.,0.,1.));
#124768=DIRECTION('ref_axis',(0.,-1.,0.));
#124769=DIRECTION('center_axis',(0.,0.,-1.));
#124770=DIRECTION('ref_axis',(0.,-1.,0.));
#124771=DIRECTION('center_axis',(0.,-1.23467863058847E-16,1.));
#124772=DIRECTION('ref_axis',(0.,-1.,0.));
#124773=DIRECTION('center_axis',(0.118855932202914,0.99291151034731,0.));
#124774=DIRECTION('ref_axis',(-0.99291151034731,0.118855932202914,0.));
#124775=DIRECTION('center_axis',(-1.3159378979443E-30,1.40254517114361E-44,
-1.));
#124776=DIRECTION('ref_axis',(-1.06581410364015E-14,-1.,-2.48920611114446E-60));
#124777=DIRECTION('center_axis',(0.,0.,1.));
#124778=DIRECTION('ref_axis',(0.,-1.,0.));
#124779=DIRECTION('center_axis',(0.,-1.23467863058847E-16,1.));
#124780=DIRECTION('ref_axis',(0.,-1.,0.));
#124781=DIRECTION('center_axis',(-1.,0.,0.));
#124782=DIRECTION('ref_axis',(0.,0.,1.));
#124783=DIRECTION('center_axis',(0.,0.,1.));
#124784=DIRECTION('ref_axis',(0.,-1.,0.));
#124785=DIRECTION('center_axis',(0.,0.,-1.));
#124786=DIRECTION('ref_axis',(0.,-1.,0.));
#124787=DIRECTION('center_axis',(-1.,0.,0.));
#124788=DIRECTION('ref_axis',(0.,0.,1.));
#124789=DIRECTION('center_axis',(-1.,0.,0.));
#124790=DIRECTION('ref_axis',(0.,0.,1.));
#124791=DIRECTION('',(1.,0.,0.));
#124792=DIRECTION('',(-1.,0.,0.));
#124793=DIRECTION('center_axis',(0.,-1.,0.));
#124794=DIRECTION('ref_axis',(0.,0.,-1.));
#124795=DIRECTION('center_axis',(0.,0.,1.));
#124796=DIRECTION('ref_axis',(1.,0.,0.));
#124797=DIRECTION('center_axis',(0.,1.,0.));
#124798=DIRECTION('ref_axis',(0.,0.,-1.));
#124799=DIRECTION('center_axis',(0.,-1.,0.));
#124800=DIRECTION('ref_axis',(0.,0.,-1.));
#124801=DIRECTION('center_axis',(0.,0.,1.));
#124802=DIRECTION('ref_axis',(1.,0.,0.));
#124803=DIRECTION('center_axis',(0.,0.,-1.));
#124804=DIRECTION('ref_axis',(0.,-1.,0.));
#124805=DIRECTION('',(-1.03377769602066E-32,0.,-1.));
#124806=DIRECTION('',(1.03377769602066E-32,1.51929083932157E-64,1.));
#124807=DIRECTION('center_axis',(0.,-1.63688369328374E-48,-1.));
#124808=DIRECTION('ref_axis',(-1.,0.,0.));
#124809=DIRECTION('center_axis',(0.,0.,-1.));
#124810=DIRECTION('ref_axis',(-1.,0.,0.));
#124811=DIRECTION('',(1.03377769602066E-32,1.63688369328374E-48,1.));
#124812=DIRECTION('center_axis',(0.,0.,-1.));
#124813=DIRECTION('ref_axis',(0.,-1.,0.));
#124814=DIRECTION('',(-1.03377769602066E-32,-1.63688369328374E-48,-1.));
#124815=DIRECTION('center_axis',(-1.58340008648341E-16,1.,0.));
#124816=DIRECTION('ref_axis',(-1.,0.,0.));
#124817=DIRECTION('center_axis',(1.,0.,0.));
#124818=DIRECTION('ref_axis',(0.,0.,-1.));
#124819=DIRECTION('center_axis',(0.,-1.,0.));
#124820=DIRECTION('ref_axis',(-1.,0.,0.));
#124821=DIRECTION('center_axis',(-2.89120579329468E-16,1.,0.));
#124822=DIRECTION('ref_axis',(-1.,-2.89120579329468E-16,0.));
#124823=DIRECTION('center_axis',(1.,0.,1.95499025045301E-32));
#124824=DIRECTION('ref_axis',(0.,1.,0.));
#124825=DIRECTION('center_axis',(1.,0.,0.));
#124826=DIRECTION('ref_axis',(0.,0.,-1.));
#124827=DIRECTION('',(-1.,-1.58340008648341E-16,-1.95499025045301E-32));
#124828=DIRECTION('',(1.,1.58340008648341E-16,1.95499025045301E-32));
#124829=DIRECTION('center_axis',(0.,-1.23467863058847E-16,1.));
#124830=DIRECTION('ref_axis',(0.,-1.,0.));
#124831=DIRECTION('center_axis',(-0.115042372881831,0.993360585307127,0.));
#124832=DIRECTION('ref_axis',(-0.993360585307127,-0.115042372881831,0.));
#124833=DIRECTION('center_axis',(0.,0.,1.));
#124834=DIRECTION('ref_axis',(0.,-1.,0.));
#124835=DIRECTION('center_axis',(0.,0.,-1.));
#124836=DIRECTION('ref_axis',(0.,-1.,0.));
#124837=DIRECTION('center_axis',(0.,-1.23467863058847E-16,1.));
#124838=DIRECTION('ref_axis',(0.,-1.,0.));
#124839=DIRECTION('center_axis',(-0.0192796610174253,0.99981413006171,0.));
#124840=DIRECTION('ref_axis',(-0.99981413006171,-0.0192796610174253,0.));
#124841=DIRECTION('center_axis',(0.,0.,-1.));
#124842=DIRECTION('ref_axis',(0.,-1.,0.));
#124843=DIRECTION('center_axis',(0.,0.,1.));
#124844=DIRECTION('ref_axis',(0.,-1.,0.));
#124845=DIRECTION('center_axis',(0.,-1.23467863058847E-16,1.));
#124846=DIRECTION('ref_axis',(0.,-1.,0.));
#124847=DIRECTION('center_axis',(-1.,0.,0.));
#124848=DIRECTION('ref_axis',(0.,0.,1.));
#124849=DIRECTION('center_axis',(0.,0.,1.));
#124850=DIRECTION('ref_axis',(0.,-1.,0.));
#124851=DIRECTION('center_axis',(0.,0.,-1.));
#124852=DIRECTION('ref_axis',(0.,-1.,0.));
#124853=DIRECTION('center_axis',(-1.,0.,0.));
#124854=DIRECTION('ref_axis',(0.,0.,1.));
#124855=DIRECTION('center_axis',(-1.,0.,0.));
#124856=DIRECTION('ref_axis',(0.,0.,1.));
#124857=DIRECTION('',(1.,0.,0.));
#124858=DIRECTION('',(-1.,0.,0.));
#124859=DIRECTION('center_axis',(0.,-1.,0.));
#124860=DIRECTION('ref_axis',(0.,0.,-1.));
#124861=DIRECTION('center_axis',(0.,0.,1.));
#124862=DIRECTION('ref_axis',(1.,0.,0.));
#124863=DIRECTION('center_axis',(0.,1.,0.));
#124864=DIRECTION('ref_axis',(0.,0.,-1.));
#124865=DIRECTION('center_axis',(0.,-1.,0.));
#124866=DIRECTION('ref_axis',(0.,0.,-1.));
#124867=DIRECTION('center_axis',(0.,0.,1.));
#124868=DIRECTION('ref_axis',(1.,0.,0.));
#124869=DIRECTION('center_axis',(0.,0.,-1.));
#124870=DIRECTION('ref_axis',(0.,-1.,0.));
#124871=DIRECTION('',(-1.03377769602066E-32,0.,-1.));
#124872=DIRECTION('',(1.03377769602066E-32,1.51929083932157E-64,1.));
#124873=DIRECTION('center_axis',(0.,0.,-1.));
#124874=DIRECTION('ref_axis',(-1.,0.,0.));
#124875=DIRECTION('center_axis',(0.,0.,-1.));
#124876=DIRECTION('ref_axis',(-1.,0.,0.));
#124877=DIRECTION('',(1.03377769602066E-32,0.,1.));
#124878=DIRECTION('center_axis',(0.,0.,-1.));
#124879=DIRECTION('ref_axis',(0.,-1.,0.));
#124880=DIRECTION('',(-1.03377769602066E-32,-1.51929083932157E-64,-1.));
#124881=DIRECTION('center_axis',(0.,1.,0.));
#124882=DIRECTION('ref_axis',(0.,0.,1.));
#124883=DIRECTION('center_axis',(1.,0.,0.));
#124884=DIRECTION('ref_axis',(0.,0.,-1.));
#124885=DIRECTION('center_axis',(0.,-1.,0.));
#124886=DIRECTION('ref_axis',(0.,0.,1.));
#124887=DIRECTION('center_axis',(0.,1.,0.));
#124888=DIRECTION('ref_axis',(0.,0.,1.));
#124889=DIRECTION('center_axis',(1.,0.,0.));
#124890=DIRECTION('ref_axis',(0.,0.,-1.));
#124891=DIRECTION('center_axis',(1.,0.,0.));
#124892=DIRECTION('ref_axis',(0.,0.,-1.));
#124893=DIRECTION('',(-1.,0.,0.));
#124894=DIRECTION('',(1.,0.,0.));
#124895=DIRECTION('center_axis',(0.,-1.23467863058847E-16,1.));
#124896=DIRECTION('ref_axis',(0.,-1.,0.));
#124897=DIRECTION('center_axis',(-0.25317796610217,0.967419721465491,0.));
#124898=DIRECTION('ref_axis',(-0.967419721465491,-0.25317796610217,0.));
#124899=DIRECTION('center_axis',(0.,0.,1.));
#124900=DIRECTION('ref_axis',(0.,-1.,0.));
#124901=DIRECTION('center_axis',(0.,0.,-1.));
#124902=DIRECTION('ref_axis',(0.,-1.,0.));
#124903=DIRECTION('center_axis',(0.,-1.23467863058847E-16,1.));
#124904=DIRECTION('ref_axis',(0.,-1.,0.));
#124905=DIRECTION('center_axis',(-0.157415254237766,0.98753249958331,0.));
#124906=DIRECTION('ref_axis',(-0.98753249958331,-0.157415254237765,0.));
#124907=DIRECTION('center_axis',(-3.72849071084219E-30,1.12593209572362E-43,
-1.));
#124908=DIRECTION('ref_axis',(-3.01980662698043E-14,-1.,1.99136488891557E-59));
#124909=DIRECTION('center_axis',(0.,0.,1.));
#124910=DIRECTION('ref_axis',(0.,-1.,0.));
#124911=DIRECTION('center_axis',(0.,-1.23467863058847E-16,1.));
#124912=DIRECTION('ref_axis',(0.,-1.,0.));
#124913=DIRECTION('center_axis',(-1.,0.,0.));
#124914=DIRECTION('ref_axis',(0.,0.,1.));
#124915=DIRECTION('center_axis',(0.,0.,1.));
#124916=DIRECTION('ref_axis',(0.,-1.,0.));
#124917=DIRECTION('center_axis',(0.,0.,-1.));
#124918=DIRECTION('ref_axis',(0.,-1.,0.));
#124919=DIRECTION('center_axis',(-1.,0.,0.));
#124920=DIRECTION('ref_axis',(0.,0.,1.));
#124921=DIRECTION('center_axis',(-1.,0.,0.));
#124922=DIRECTION('ref_axis',(0.,0.,1.));
#124923=DIRECTION('',(1.,0.,0.));
#124924=DIRECTION('',(-1.,0.,0.));
#124925=DIRECTION('center_axis',(0.,-1.,0.));
#124926=DIRECTION('ref_axis',(0.,0.,-1.));
#124927=DIRECTION('center_axis',(0.,0.,1.));
#124928=DIRECTION('ref_axis',(1.,0.,0.));
#124929=DIRECTION('center_axis',(0.,1.,0.));
#124930=DIRECTION('ref_axis',(0.,0.,-1.));
#124931=DIRECTION('center_axis',(0.,-1.,0.));
#124932=DIRECTION('ref_axis',(0.,0.,-1.));
#124933=DIRECTION('center_axis',(0.,0.,1.));
#124934=DIRECTION('ref_axis',(1.,0.,0.));
#124935=DIRECTION('center_axis',(0.,0.,-1.));
#124936=DIRECTION('ref_axis',(0.,-1.,0.));
#124937=DIRECTION('',(-1.03377769602066E-32,0.,-1.));
#124938=DIRECTION('',(1.03377769602066E-32,0.,1.));
#124939=DIRECTION('center_axis',(0.,1.15951658690774E-48,-1.));
#124940=DIRECTION('ref_axis',(-1.,0.,0.));
#124941=DIRECTION('center_axis',(0.,0.,-1.));
#124942=DIRECTION('ref_axis',(-1.,0.,0.));
#124943=DIRECTION('',(1.03377769602066E-32,-1.15951658690774E-48,1.));
#124944=DIRECTION('center_axis',(0.,0.,-1.));
#124945=DIRECTION('ref_axis',(0.,-1.,0.));
#124946=DIRECTION('',(-1.03377769602066E-32,1.15951658690774E-48,-1.));
#124947=DIRECTION('center_axis',(1.12163049306547E-16,1.,0.));
#124948=DIRECTION('ref_axis',(-1.,0.,0.));
#124949=DIRECTION('center_axis',(1.,0.,0.));
#124950=DIRECTION('ref_axis',(0.,0.,-1.));
#124951=DIRECTION('center_axis',(0.,-1.,0.));
#124952=DIRECTION('ref_axis',(-1.,0.,0.));
#124953=DIRECTION('center_axis',(0.,1.,0.));
#124954=DIRECTION('ref_axis',(-1.,0.,0.));
#124955=DIRECTION('center_axis',(1.,0.,-1.38485320120435E-32));
#124956=DIRECTION('ref_axis',(0.,1.,0.));
#124957=DIRECTION('center_axis',(1.,0.,0.));
#124958=DIRECTION('ref_axis',(0.,0.,-1.));
#124959=DIRECTION('',(-1.,1.12163049306547E-16,1.38485320120435E-32));
#124960=DIRECTION('',(1.,-1.12163049306547E-16,-1.38485320120435E-32));
#124961=DIRECTION('center_axis',(0.,-1.23467863058847E-16,1.));
#124962=DIRECTION('ref_axis',(0.,-1.,0.));
#124963=DIRECTION('center_axis',(-0.391313559322503,0.920257408712559,0.));
#124964=DIRECTION('ref_axis',(-0.920257408712559,-0.391313559322503,0.));
#124965=DIRECTION('center_axis',(0.,0.,1.));
#124966=DIRECTION('ref_axis',(0.,-1.,0.));
#124967=DIRECTION('center_axis',(0.,0.,-1.));
#124968=DIRECTION('ref_axis',(0.,-1.,0.));
#124969=DIRECTION('center_axis',(0.,-1.23467863058847E-16,1.));
#124970=DIRECTION('ref_axis',(0.,-1.,0.));
#124971=DIRECTION('center_axis',(-0.295550847458105,0.955327010278049,0.));
#124972=DIRECTION('ref_axis',(-0.955327010278049,-0.295550847458105,0.));
#124973=DIRECTION('center_axis',(2.30289132140253E-30,4.29529458662731E-44,
-1.));
#124974=DIRECTION('ref_axis',(1.86517468137027E-14,-1.,3.48488855560224E-59));
#124975=DIRECTION('center_axis',(0.,0.,1.));
#124976=DIRECTION('ref_axis',(0.,-1.,0.));
#124977=DIRECTION('center_axis',(0.,-1.23467863058847E-16,1.));
#124978=DIRECTION('ref_axis',(0.,-1.,0.));
#124979=DIRECTION('center_axis',(-1.,0.,0.));
#124980=DIRECTION('ref_axis',(0.,0.,1.));
#124981=DIRECTION('center_axis',(0.,0.,1.));
#124982=DIRECTION('ref_axis',(0.,-1.,0.));
#124983=DIRECTION('center_axis',(0.,0.,-1.));
#124984=DIRECTION('ref_axis',(0.,-1.,0.));
#124985=DIRECTION('center_axis',(-1.,0.,1.64684708935465E-32));
#124986=DIRECTION('ref_axis',(0.,-1.,0.));
#124987=DIRECTION('center_axis',(-1.,0.,0.));
#124988=DIRECTION('ref_axis',(0.,0.,1.));
#124989=DIRECTION('',(1.,-1.33382651044161E-16,-1.64684708935465E-32));
#124990=DIRECTION('',(-1.,1.33382651044161E-16,1.64684708935465E-32));
#124991=DIRECTION('center_axis',(-1.33382651044161E-16,-1.,0.));
#124992=DIRECTION('ref_axis',(1.,-1.48029736616688E-16,0.));
#124993=DIRECTION('center_axis',(0.,0.,1.));
#124994=DIRECTION('ref_axis',(1.,0.,0.));
#124995=DIRECTION('center_axis',(0.,1.,0.));
#124996=DIRECTION('ref_axis',(1.,0.,0.));
#124997=DIRECTION('center_axis',(-1.44560289664734E-16,-1.,0.));
#124998=DIRECTION('ref_axis',(1.,-1.44560289664734E-16,0.));
#124999=DIRECTION('center_axis',(0.,-1.37888009685561E-48,1.));
#125000=DIRECTION('ref_axis',(1.,0.,0.));
#125001=DIRECTION('center_axis',(0.,0.,-1.));
#125002=DIRECTION('ref_axis',(0.,-1.,0.));
#125003=DIRECTION('',(-1.03377769602066E-32,1.37888009685561E-48,-1.));
#125004=DIRECTION('',(1.03377769602066E-32,-1.37888009685561E-48,1.));
#125005=DIRECTION('center_axis',(0.,0.,-1.));
#125006=DIRECTION('ref_axis',(-1.,0.,0.));
#125007=DIRECTION('center_axis',(0.,0.,-1.));
#125008=DIRECTION('ref_axis',(-1.,0.,0.));
#125009=DIRECTION('',(1.03377769602066E-32,0.,1.));
#125010=DIRECTION('center_axis',(0.,0.,-1.));
#125011=DIRECTION('ref_axis',(0.,-1.,0.));
#125012=DIRECTION('',(-1.03377769602066E-32,-1.51929083932157E-64,-1.));
#125013=DIRECTION('center_axis',(0.,1.,0.));
#125014=DIRECTION('ref_axis',(0.,0.,1.));
#125015=DIRECTION('center_axis',(1.,0.,0.));
#125016=DIRECTION('ref_axis',(0.,0.,-1.));
#125017=DIRECTION('center_axis',(0.,-1.,0.));
#125018=DIRECTION('ref_axis',(0.,0.,1.));
#125019=DIRECTION('center_axis',(0.,1.,0.));
#125020=DIRECTION('ref_axis',(0.,0.,1.));
#125021=DIRECTION('center_axis',(1.,0.,0.));
#125022=DIRECTION('ref_axis',(0.,0.,-1.));
#125023=DIRECTION('center_axis',(1.,0.,0.));
#125024=DIRECTION('ref_axis',(0.,0.,-1.));
#125025=DIRECTION('',(-1.,0.,0.));
#125026=DIRECTION('',(1.,0.,0.));
#125027=DIRECTION('center_axis',(0.,-1.23467863058847E-16,1.));
#125028=DIRECTION('ref_axis',(0.,-1.,0.));
#125029=DIRECTION('center_axis',(-0.139173100960066,0.99026806874157,0.));
#125030=DIRECTION('ref_axis',(-0.99026806874157,-0.139173100960066,0.));
#125031=DIRECTION('center_axis',(0.,0.,1.));
#125032=DIRECTION('ref_axis',(0.,-1.,0.));
#125033=DIRECTION('center_axis',(0.,0.,-1.));
#125034=DIRECTION('ref_axis',(0.,-1.,0.));
#125035=DIRECTION('center_axis',(0.139173100960066,-0.99026806874157,-1.22266282302933E-16));
#125036=DIRECTION('ref_axis',(0.99026806874157,0.139173100960066,9.57340194962255E-34));
#125037=DIRECTION('center_axis',(-0.139173100960066,0.99026806874157,0.));
#125038=DIRECTION('ref_axis',(-0.99026806874157,-0.139173100960066,0.));
#125039=DIRECTION('',(0.139173100960067,-0.99026806874157,-1.22266282302933E-16));
#125040=DIRECTION('',(-0.139173100960067,0.99026806874157,1.22266282302933E-16));
#125041=DIRECTION('center_axis',(0.,-1.23467863058847E-16,1.));
#125042=DIRECTION('ref_axis',(0.,-1.,0.));
#125043=DIRECTION('center_axis',(-0.322177601635812,0.94667924504776,0.));
#125044=DIRECTION('ref_axis',(-0.94667924504776,-0.322177601635812,0.));
#125045=DIRECTION('center_axis',(0.,0.,1.));
#125046=DIRECTION('ref_axis',(0.,-1.,0.));
#125047=DIRECTION('center_axis',(6.23076656223628E-31,3.14433659020876E-45,
-1.));
#125048=DIRECTION('ref_axis',(5.04646829375071E-15,-1.,-4.3561106945028E-60));
#125049=DIRECTION('center_axis',(0.,-1.23467863058847E-16,1.));
#125050=DIRECTION('ref_axis',(0.,-1.,0.));
#125051=DIRECTION('center_axis',(-1.,0.,0.));
#125052=DIRECTION('ref_axis',(0.,0.,1.));
#125053=DIRECTION('center_axis',(0.,0.,1.));
#125054=DIRECTION('ref_axis',(0.,-1.,0.));
#125055=DIRECTION('center_axis',(0.,0.,-1.));
#125056=DIRECTION('ref_axis',(0.,-1.,0.));
#125057=DIRECTION('center_axis',(-1.,0.,0.));
#125058=DIRECTION('ref_axis',(0.,0.,1.));
#125059=DIRECTION('center_axis',(-1.,0.,0.));
#125060=DIRECTION('ref_axis',(0.,0.,1.));
#125061=DIRECTION('',(1.,0.,0.));
#125062=DIRECTION('',(-1.,0.,0.));
#125063=DIRECTION('center_axis',(0.,-1.,0.));
#125064=DIRECTION('ref_axis',(0.,0.,-1.));
#125065=DIRECTION('center_axis',(0.,0.,1.));
#125066=DIRECTION('ref_axis',(1.,0.,0.));
#125067=DIRECTION('center_axis',(0.,1.,0.));
#125068=DIRECTION('ref_axis',(0.,0.,-1.));
#125069=DIRECTION('center_axis',(0.,-1.,0.));
#125070=DIRECTION('ref_axis',(0.,0.,-1.));
#125071=DIRECTION('center_axis',(0.,0.,1.));
#125072=DIRECTION('ref_axis',(1.,0.,0.));
#125073=DIRECTION('center_axis',(0.,0.,-1.));
#125074=DIRECTION('ref_axis',(0.,-1.,0.));
#125075=DIRECTION('',(-1.03377769602066E-32,0.,-1.));
#125076=DIRECTION('',(1.03377769602066E-32,1.51929083932157E-64,1.));
#125077=DIRECTION('center_axis',(0.,0.,-1.));
#125078=DIRECTION('ref_axis',(-1.,0.,0.));
#125079=DIRECTION('center_axis',(0.,0.,-1.));
#125080=DIRECTION('ref_axis',(-1.,0.,0.));
#125081=DIRECTION('',(1.03377769602066E-32,0.,1.));
#125082=DIRECTION('center_axis',(0.,0.,-1.));
#125083=DIRECTION('ref_axis',(0.,-1.,0.));
#125084=DIRECTION('',(-1.03377769602066E-32,-1.51929083932157E-64,-1.));
#125085=DIRECTION('center_axis',(0.,1.,0.));
#125086=DIRECTION('ref_axis',(0.,0.,1.));
#125087=DIRECTION('center_axis',(1.,0.,0.));
#125088=DIRECTION('ref_axis',(0.,0.,-1.));
#125089=DIRECTION('center_axis',(0.,-1.,0.));
#125090=DIRECTION('ref_axis',(0.,0.,1.));
#125091=DIRECTION('center_axis',(0.,1.,0.));
#125092=DIRECTION('ref_axis',(0.,0.,1.));
#125093=DIRECTION('center_axis',(1.,0.,0.));
#125094=DIRECTION('ref_axis',(0.,0.,-1.));
#125095=DIRECTION('center_axis',(1.,0.,0.));
#125096=DIRECTION('ref_axis',(0.,0.,-1.));
#125097=DIRECTION('',(-1.,0.,0.));
#125098=DIRECTION('',(1.,0.,0.));
#125099=DIRECTION('center_axis',(0.,-1.23467863058847E-16,1.));
#125100=DIRECTION('ref_axis',(0.,-1.,0.));
#125101=DIRECTION('center_axis',(-0.139173100960066,0.99026806874157,0.));
#125102=DIRECTION('ref_axis',(-0.99026806874157,-0.139173100960066,0.));
#125103=DIRECTION('center_axis',(0.,0.,1.));
#125104=DIRECTION('ref_axis',(0.,-1.,0.));
#125105=DIRECTION('center_axis',(0.,0.,-1.));
#125106=DIRECTION('ref_axis',(0.,-1.,0.));
#125107=DIRECTION('center_axis',(0.139173100960066,-0.99026806874157,-1.22266282302933E-16));
#125108=DIRECTION('ref_axis',(0.99026806874157,0.139173100960066,9.57340194962255E-34));
#125109=DIRECTION('center_axis',(-0.139173100960066,0.99026806874157,0.));
#125110=DIRECTION('ref_axis',(-0.99026806874157,-0.139173100960066,0.));
#125111=DIRECTION('',(0.139173100960067,-0.99026806874157,-1.22266282302933E-16));
#125112=DIRECTION('',(-0.139173100960067,0.99026806874157,1.22266282302933E-16));
#125113=DIRECTION('center_axis',(0.,-1.23467863058847E-16,1.));
#125114=DIRECTION('ref_axis',(0.,-1.,0.));
#125115=DIRECTION('center_axis',(-1.,0.,0.));
#125116=DIRECTION('ref_axis',(0.,0.,1.));
#125117=DIRECTION('center_axis',(0.,0.,1.));
#125118=DIRECTION('ref_axis',(0.,-1.,0.));
#125119=DIRECTION('center_axis',(0.,0.,-1.));
#125120=DIRECTION('ref_axis',(0.,-1.,0.));
#125121=DIRECTION('center_axis',(-1.,0.,-2.45282604044407E-32));
#125122=DIRECTION('ref_axis',(0.,-1.,0.));
#125123=DIRECTION('center_axis',(-1.,0.,0.));
#125124=DIRECTION('ref_axis',(0.,0.,1.));
#125125=DIRECTION('',(1.,1.98661091208406E-16,2.45282604044407E-32));
#125126=DIRECTION('',(-1.,-1.98661091208406E-16,-2.45282604044407E-32));
#125127=DIRECTION('center_axis',(1.98661091208406E-16,-1.,0.));
#125128=DIRECTION('ref_axis',(1.,0.,0.));
#125129=DIRECTION('center_axis',(0.,0.,1.));
#125130=DIRECTION('ref_axis',(1.,0.,0.));
#125131=DIRECTION('center_axis',(0.,1.,0.));
#125132=DIRECTION('ref_axis',(1.,0.,0.));
#125133=DIRECTION('center_axis',(0.,-1.,0.));
#125134=DIRECTION('ref_axis',(1.,0.,0.));
#125135=DIRECTION('center_axis',(0.,2.05371405158377E-48,1.));
#125136=DIRECTION('ref_axis',(1.,0.,0.));
#125137=DIRECTION('center_axis',(0.,0.,-1.));
#125138=DIRECTION('ref_axis',(0.,-1.,0.));
#125139=DIRECTION('',(-1.03377769602066E-32,-2.05371405158378E-48,-1.));
#125140=DIRECTION('',(1.03377769602066E-32,2.05371405158377E-48,1.));
#125141=DIRECTION('center_axis',(0.707106781186548,0.707106781186548,8.73049632275229E-17));
#125142=DIRECTION('ref_axis',(-0.707106781186548,0.707106781186548,3.00811589707026E-33));
#125143=DIRECTION('',(0.707106781186548,0.707106781186547,8.7304963227523E-17));
#125144=DIRECTION('center_axis',(0.707106781186537,0.707106781186558,0.));
#125145=DIRECTION('ref_axis',(-0.707106781186558,0.707106781186537,0.));
#125146=DIRECTION('',(-0.707106781186548,-0.707106781186547,-8.7304963227523E-17));
#125147=DIRECTION('center_axis',(0.,-1.23467863058847E-16,1.));
#125148=DIRECTION('ref_axis',(0.,-1.,0.));
#125149=DIRECTION('center_axis',(-1.,0.,0.));
#125150=DIRECTION('ref_axis',(0.,0.,1.));
#125151=DIRECTION('center_axis',(0.,0.,1.));
#125152=DIRECTION('ref_axis',(0.,-1.,0.));
#125153=DIRECTION('center_axis',(0.,0.,-1.));
#125154=DIRECTION('ref_axis',(0.,-1.,0.));
#125155=DIRECTION('center_axis',(-1.,0.,0.));
#125156=DIRECTION('ref_axis',(0.,0.,1.));
#125157=DIRECTION('center_axis',(-1.,0.,0.));
#125158=DIRECTION('ref_axis',(0.,0.,1.));
#125159=DIRECTION('',(1.,0.,0.));
#125160=DIRECTION('',(-1.,0.,0.));
#125161=DIRECTION('center_axis',(0.,-1.,-1.23467863058847E-16));
#125162=DIRECTION('ref_axis',(0.,0.,-1.));
#125163=DIRECTION('center_axis',(0.,0.,1.));
#125164=DIRECTION('ref_axis',(1.,0.,0.));
#125165=DIRECTION('center_axis',(0.,1.,0.));
#125166=DIRECTION('ref_axis',(0.,0.,-1.));
#125167=DIRECTION('center_axis',(0.,-1.,0.));
#125168=DIRECTION('ref_axis',(0.,0.,-1.));
#125169=DIRECTION('center_axis',(1.3684555315672E-48,0.,1.));
#125170=DIRECTION('ref_axis',(0.,-1.,0.));
#125171=DIRECTION('center_axis',(0.,0.,-1.));
#125172=DIRECTION('ref_axis',(0.,-1.,0.));
#125173=DIRECTION('',(-1.3684555315672E-48,1.23467863058847E-16,-1.));
#125174=DIRECTION('',(1.3684555315672E-48,-1.23467863058847E-16,1.));
#125175=DIRECTION('center_axis',(1.74315279842105E-32,0.,-1.));
#125176=DIRECTION('ref_axis',(0.,1.,0.));
#125177=DIRECTION('',(1.74315279842105E-32,1.23467863058847E-16,-1.));
#125178=DIRECTION('',(-2.46519032881566E-32,-1.23467863058847E-16,1.));
#125179=DIRECTION('center_axis',(0.,0.,1.));
#125180=DIRECTION('ref_axis',(0.,-1.,0.));
#125181=DIRECTION('center_axis',(0.,0.,-1.));
#125182=DIRECTION('ref_axis',(0.,1.,0.));
#125183=DIRECTION('',(3.61018765197304E-33,1.23467863058847E-16,-1.));
#125184=DIRECTION('',(0.,-1.23467863058847E-16,1.));
#125185=DIRECTION('center_axis',(0.,0.,1.));
#125186=DIRECTION('ref_axis',(0.,-1.,0.));
#125187=DIRECTION('center_axis',(-5.10557634013221E-33,0.,-1.));
#125188=DIRECTION('ref_axis',(0.,1.,0.));
#125189=DIRECTION('',(-8.71576399210524E-33,1.23467863058847E-16,-1.));
#125190=DIRECTION('',(5.10557634013221E-33,-1.23467863058847E-16,1.));
#125191=DIRECTION('center_axis',(0.,0.,1.));
#125192=DIRECTION('ref_axis',(0.,-1.,0.));
#125193=DIRECTION('center_axis',(-1.74315279842107E-32,0.,-1.));
#125194=DIRECTION('ref_axis',(0.,1.,0.));
#125195=DIRECTION('',(-1.74315279842107E-32,1.23467863058847E-16,-1.));
#125196=DIRECTION('',(2.46519032881566E-32,-1.23467863058847E-16,1.));
#125197=DIRECTION('center_axis',(0.,0.,1.));
#125198=DIRECTION('ref_axis',(0.,-1.,0.));
#125199=DIRECTION('center_axis',(0.,0.,-1.));
#125200=DIRECTION('ref_axis',(0.,1.,0.));
#125201=DIRECTION('',(0.,1.23467863058847E-16,-1.));
#125202=DIRECTION('',(0.,-1.23467863058847E-16,1.));
#125203=DIRECTION('center_axis',(0.,0.,1.));
#125204=DIRECTION('ref_axis',(0.,-1.,0.));
#125205=DIRECTION('center_axis',(0.,0.,1.));
#125206=DIRECTION('ref_axis',(-0.754709580222749,0.656059028990534,0.));
#125207=DIRECTION('',(1.73522765332111E-17,0.,-1.));
#125208=DIRECTION('',(-1.73522765332111E-17,-7.66623374189429E-34,1.));
#125209=DIRECTION('center_axis',(0.,0.,1.));
#125210=DIRECTION('ref_axis',(0.,-1.,0.));
#125211=DIRECTION('center_axis',(0.,0.,1.));
#125212=DIRECTION('ref_axis',(-0.754709580222751,0.656059028990531,0.));
#125213=DIRECTION('',(1.73522765332111E-17,0.,-1.));
#125214=DIRECTION('',(-1.73522765332111E-17,-7.66623374189429E-34,1.));
#125215=DIRECTION('center_axis',(0.,0.,1.));
#125216=DIRECTION('ref_axis',(0.,-1.,0.));
#125217=DIRECTION('center_axis',(0.,0.,1.));
#125218=DIRECTION('ref_axis',(0.,-1.,0.));
#125219=DIRECTION('',(-1.38485320120435E-32,1.55329357889012E-48,-1.));
#125220=DIRECTION('',(0.,-1.23467863058847E-16,1.));
#125221=DIRECTION('center_axis',(0.,0.,1.));
#125222=DIRECTION('ref_axis',(0.,-1.,0.));
#125223=DIRECTION('center_axis',(0.,0.,1.));
#125224=DIRECTION('ref_axis',(0.,-1.,0.));
#125225=DIRECTION('',(0.,0.,-1.));
#125226=DIRECTION('',(0.,-1.23467863058847E-16,1.));
#125227=DIRECTION('center_axis',(0.,0.,1.));
#125228=DIRECTION('ref_axis',(0.,-1.,0.));
#125229=DIRECTION('center_axis',(0.,0.,1.));
#125230=DIRECTION('ref_axis',(0.,-1.,0.));
#125231=DIRECTION('',(1.95499025045301E-32,3.09553173164152E-48,-1.));
#125232=DIRECTION('',(0.,-1.23467863058847E-16,1.));
#125233=DIRECTION('center_axis',(0.,0.,1.));
#125234=DIRECTION('ref_axis',(0.,-1.,0.));
#125235=DIRECTION('center_axis',(0.,0.,1.));
#125236=DIRECTION('ref_axis',(0.,-1.,0.));
#125237=DIRECTION('',(0.,0.,-1.));
#125238=DIRECTION('',(0.,-1.23467863058847E-16,1.));
#125239=DIRECTION('center_axis',(0.,0.,1.));
#125240=DIRECTION('ref_axis',(0.,-1.,0.));
#125241=DIRECTION('center_axis',(0.,0.,1.));
#125242=DIRECTION('ref_axis',(0.,-1.,0.));
#125243=DIRECTION('',(0.,1.23467863058847E-16,-1.));
#125244=DIRECTION('',(0.,0.,1.));
#125245=DIRECTION('center_axis',(0.,0.,1.));
#125246=DIRECTION('ref_axis',(0.,-1.,0.));
#125247=DIRECTION('center_axis',(0.,0.,1.));
#125248=DIRECTION('ref_axis',(0.,-1.,0.));
#125249=DIRECTION('',(0.,1.23467863058847E-16,-1.));
#125250=DIRECTION('',(0.,0.,1.));
#125251=DIRECTION('center_axis',(0.,0.,1.));
#125252=DIRECTION('ref_axis',(0.,-1.,0.));
#125253=DIRECTION('center_axis',(0.,0.,1.));
#125254=DIRECTION('ref_axis',(0.,-1.,0.));
#125255=DIRECTION('',(0.,1.23467863058847E-16,-1.));
#125256=DIRECTION('',(1.64684708935465E-32,-2.19660830642484E-48,1.));
#125257=DIRECTION('center_axis',(0.,0.,1.));
#125258=DIRECTION('ref_axis',(0.,-1.,0.));
#125259=DIRECTION('center_axis',(0.,0.,1.));
#125260=DIRECTION('ref_axis',(0.,-1.,0.));
#125261=DIRECTION('',(0.,1.23467863058847E-16,-1.));
#125262=DIRECTION('',(0.,0.,1.));
#125263=DIRECTION('center_axis',(0.,0.,1.));
#125264=DIRECTION('ref_axis',(0.,-1.,0.));
#125265=DIRECTION('center_axis',(0.,-3.44722219103775E-33,1.));
#125266=DIRECTION('ref_axis',(1.,0.,0.));
#125267=DIRECTION('',(1.73522765332111E-17,4.28072011692203E-33,-1.));
#125268=DIRECTION('',(-1.73522765332111E-17,-3.44722219103775E-33,1.));
#125269=DIRECTION('center_axis',(0.,0.,1.));
#125270=DIRECTION('ref_axis',(0.,-1.,0.));
#125271=DIRECTION('center_axis',(0.,0.,1.));
#125272=DIRECTION('ref_axis',(0.,-1.,0.));
#125273=DIRECTION('',(0.,1.23467863058847E-16,-1.));
#125274=DIRECTION('',(0.,0.,1.));
#125275=DIRECTION('center_axis',(0.,0.,1.));
#125276=DIRECTION('ref_axis',(0.,-1.,0.));
#125277=DIRECTION('center_axis',(0.,0.,1.));
#125278=DIRECTION('ref_axis',(0.,-1.,0.));
#125279=DIRECTION('',(0.,0.,-1.));
#125280=DIRECTION('',(0.,-1.23467863058847E-16,1.));
#125281=DIRECTION('center_axis',(0.,0.,1.));
#125282=DIRECTION('ref_axis',(0.,-1.,0.));
#125283=DIRECTION('center_axis',(0.,0.,1.));
#125284=DIRECTION('ref_axis',(0.,-1.,0.));
#125285=DIRECTION('',(0.,1.23467863058847E-16,-1.));
#125286=DIRECTION('',(-3.39012271766808E-32,-9.30844007186829E-48,1.));
#125287=DIRECTION('center_axis',(0.,0.,1.));
#125288=DIRECTION('ref_axis',(0.,-1.,0.));
#125289=DIRECTION('center_axis',(0.,0.,1.));
#125290=DIRECTION('ref_axis',(0.,-1.,0.));
#125291=DIRECTION('',(3.27642397172882E-32,8.69453295502712E-48,-1.));
#125292=DIRECTION('',(0.,-1.23467863058847E-16,1.));
#125293=DIRECTION('center_axis',(0.,0.,1.));
#125294=DIRECTION('ref_axis',(0.,-1.,0.));
#125295=DIRECTION('center_axis',(0.,0.,1.));
#125296=DIRECTION('ref_axis',(0.,-1.,0.));
#125297=DIRECTION('',(0.,0.,-1.));
#125298=DIRECTION('',(0.,-1.23467863058847E-16,1.));
#125299=DIRECTION('center_axis',(0.,0.,1.));
#125300=DIRECTION('ref_axis',(0.,-1.,0.));
#125301=DIRECTION('center_axis',(0.,0.,1.));
#125302=DIRECTION('ref_axis',(0.,-1.,0.));
#125303=DIRECTION('',(0.,1.23467863058847E-16,-1.));
#125304=DIRECTION('',(0.,0.,1.));
#125305=DIRECTION('center_axis',(0.,0.,1.));
#125306=DIRECTION('ref_axis',(0.,-1.,0.));
#125307=DIRECTION('center_axis',(0.,-4.33074883140017E-34,1.));
#125308=DIRECTION('ref_axis',(-0.754709580222784,-0.656059028990493,-2.84122687313011E-34));
#125309=DIRECTION('',(-1.73522765332109E-17,0.,-1.));
#125310=DIRECTION('',(1.73522765332109E-17,0.,1.));
#125311=DIRECTION('center_axis',(0.,0.,1.));
#125312=DIRECTION('ref_axis',(0.,-1.,0.));
#125313=DIRECTION('center_axis',(0.,-1.72738015942773E-49,1.));
#125314=DIRECTION('ref_axis',(1.,0.,0.));
#125315=DIRECTION('',(-1.73522765332109E-17,0.,-1.));
#125316=DIRECTION('',(1.73522765332109E-17,3.85185988877447E-34,1.));
#125317=DIRECTION('center_axis',(0.,0.,1.));
#125318=DIRECTION('ref_axis',(0.,-1.,0.));
#125319=DIRECTION('center_axis',(0.,-4.33074883140017E-34,1.));
#125320=DIRECTION('ref_axis',(-0.754709580222761,-0.656059028990519,-2.84122687313022E-34));
#125321=DIRECTION('',(-1.73522765332109E-17,0.,-1.));
#125322=DIRECTION('',(1.73522765332109E-17,0.,1.));
#125323=DIRECTION('center_axis',(0.,0.,1.));
#125324=DIRECTION('ref_axis',(0.,-1.,0.));
#125325=DIRECTION('center_axis',(0.,0.,-1.));
#125326=DIRECTION('ref_axis',(0.,1.,0.));
#125327=DIRECTION('',(0.,1.23467863058847E-16,-1.));
#125328=DIRECTION('',(0.,-1.23467863058847E-16,1.));
#125329=DIRECTION('center_axis',(0.,0.,1.));
#125330=DIRECTION('ref_axis',(0.,-1.,0.));
#125331=DIRECTION('center_axis',(0.,-1.23467863058847E-16,1.));
#125332=DIRECTION('ref_axis',(0.,-1.,-1.23467863058847E-16));
#125333=DIRECTION('center_axis',(0.,0.,-1.));
#125334=DIRECTION('ref_axis',(0.,-1.,0.));
#125335=DIRECTION('center_axis',(0.,1.19636298170419E-16,-1.));
#125336=DIRECTION('ref_axis',(0.,1.,1.19636298170419E-16));
#125337=DIRECTION('',(1.23138919323476E-16,1.,0.));
#125338=DIRECTION('',(-1.,0.,0.));
#125339=DIRECTION('center_axis',(0.,0.,-1.));
#125340=DIRECTION('ref_axis',(0.,-1.,0.));
#125341=DIRECTION('',(8.37284837049414E-17,1.,1.23467863058847E-16));
#125342=DIRECTION('',(8.37284837049414E-17,1.,1.23467863058847E-16));
#125343=DIRECTION('',(8.37284837049414E-17,1.,1.23467863058847E-16));
#125344=DIRECTION('',(8.37284837049414E-17,1.,1.23467863058847E-16));
#125345=DIRECTION('',(8.37284837049414E-17,1.,1.23467863058847E-16));
#125346=DIRECTION('',(8.37284837049414E-17,1.,1.23467863058847E-16));
#125347=DIRECTION('',(8.37284837049414E-17,1.,1.23467863058847E-16));
#125348=DIRECTION('',(8.37284837049414E-17,1.,1.23467863058847E-16));
#125349=DIRECTION('',(8.37284837049414E-17,1.,1.23467863058847E-16));
#125350=DIRECTION('',(8.37284837049414E-17,1.,1.23467863058847E-16));
#125351=DIRECTION('',(8.37284837049414E-17,1.,1.23467863058847E-16));
#125352=DIRECTION('center_axis',(0.,1.,1.23467863058847E-16));
#125353=DIRECTION('ref_axis',(0.,1.23467863058847E-16,-1.));
#125354=DIRECTION('',(-1.,0.,0.));
#125355=DIRECTION('center_axis',(0.,-1.19636298170419E-16,1.));
#125356=DIRECTION('ref_axis',(0.,-1.,-1.19636298170419E-16));
#125357=DIRECTION('',(0.,-1.23467863058847E-16,1.));
#125358=DIRECTION('center_axis',(0.,1.19636298170419E-16,-1.));
#125359=DIRECTION('ref_axis',(0.,1.,1.19636298170419E-16));
#125360=DIRECTION('',(0.,-1.23467863058847E-16,1.));
#125361=DIRECTION('center_axis',(-1.,0.,0.));
#125362=DIRECTION('ref_axis',(0.,0.,1.));
#125363=DIRECTION('',(0.,-1.,0.));
#125364=DIRECTION('center_axis',(2.77555756156289E-14,1.,1.23467863058847E-16));
#125365=DIRECTION('ref_axis',(1.,-2.77555756156289E-14,0.));
#125366=DIRECTION('',(-1.,2.77555756156289E-14,0.));
#125367=DIRECTION('center_axis',(-1.,0.,0.));
#125368=DIRECTION('ref_axis',(0.,0.,1.));
#125369=DIRECTION('',(0.,-1.23467863058847E-16,1.));
#125370=DIRECTION('',(0.,-1.,0.));
#125371=DIRECTION('center_axis',(0.,-1.,0.));
#125372=DIRECTION('ref_axis',(0.,0.,-1.));
#125373=DIRECTION('',(1.,0.,0.));
#125374=DIRECTION('center_axis',(0.,1.,0.));
#125375=DIRECTION('ref_axis',(1.,0.,0.));
#125376=DIRECTION('',(-1.,0.,0.));
#125377=DIRECTION('center_axis',(0.,-1.,0.));
#125378=DIRECTION('ref_axis',(0.,0.,-1.));
#125379=DIRECTION('',(1.,0.,0.));
#125380=DIRECTION('center_axis',(0.,1.,0.));
#125381=DIRECTION('ref_axis',(1.,0.,0.));
#125382=DIRECTION('',(-1.,0.,0.));
#125383=DIRECTION('center_axis',(-1.33382651044161E-16,-1.,0.));
#125384=DIRECTION('ref_axis',(-1.,1.33382651044161E-16,0.));
#125385=DIRECTION('',(1.,-1.33382651044161E-16,-1.64684708935465E-32));
#125386=DIRECTION('center_axis',(1.12163049306547E-16,1.,0.));
#125387=DIRECTION('ref_axis',(1.,-1.12163049306547E-16,0.));
#125388=DIRECTION('',(-1.,1.12163049306547E-16,1.38485320120435E-32));
#125389=DIRECTION('center_axis',(0.,1.,0.));
#125390=DIRECTION('ref_axis',(1.,0.,0.));
#125391=DIRECTION('',(-1.,0.,0.));
#125392=DIRECTION('center_axis',(0.,-1.,0.));
#125393=DIRECTION('ref_axis',(0.,0.,-1.));
#125394=DIRECTION('',(1.,0.,0.));
#125395=DIRECTION('center_axis',(0.,-1.,0.));
#125396=DIRECTION('ref_axis',(0.,0.,-1.));
#125397=DIRECTION('',(1.,0.,0.));
#125398=DIRECTION('center_axis',(-1.58340008648341E-16,1.,0.));
#125399=DIRECTION('ref_axis',(1.,1.58340008648341E-16,0.));
#125400=DIRECTION('',(-1.,-1.58340008648341E-16,-1.95499025045301E-32));
#125401=DIRECTION('center_axis',(-1.,8.37284837049414E-17,1.03377769602066E-32));
#125402=DIRECTION('ref_axis',(1.03377769602066E-32,0.,1.));
#125403=DIRECTION('',(-8.37284837049414E-17,-1.,0.));
#125404=DIRECTION('',(-8.37284837049414E-17,-1.,-1.23467863058847E-16));
#125405=DIRECTION('center_axis',(8.37284837049414E-17,1.,0.));
#125406=DIRECTION('ref_axis',(0.,0.,1.));
#125407=DIRECTION('center_axis',(0.,0.,1.));
#125408=DIRECTION('ref_axis',(0.,-1.,0.));
#125409=DIRECTION('center_axis',(0.,0.,-1.));
#125410=DIRECTION('ref_axis',(0.,-1.,0.));
#125411=DIRECTION('center_axis',(0.,-1.,0.));
#125412=DIRECTION('ref_axis',(0.,0.,-1.));
#125413=DIRECTION('',(1.,0.,0.));
#125414=DIRECTION('center_axis',(0.,1.,0.));
#125415=DIRECTION('ref_axis',(1.,0.,0.));
#125416=DIRECTION('',(-1.,0.,0.));
#125417=DIRECTION('center_axis',(-1.,8.37284837049414E-17,1.03377769602066E-32));
#125418=DIRECTION('ref_axis',(1.03377769602066E-32,0.,1.));
#125419=DIRECTION('',(-8.37284837049414E-17,-1.,0.));
#125420=DIRECTION('',(-8.37284837049414E-17,-1.,-1.23467863058847E-16));
#125421=DIRECTION('center_axis',(8.37284837049414E-17,1.,0.));
#125422=DIRECTION('ref_axis',(0.,0.,1.));
#125423=DIRECTION('center_axis',(0.,0.,1.));
#125424=DIRECTION('ref_axis',(0.,-1.,0.));
#125425=DIRECTION('center_axis',(-1.3159378979443E-30,1.40254517114361E-44,
-1.));
#125426=DIRECTION('ref_axis',(-1.06581410364015E-14,-1.,-2.48920611114446E-60));
#125427=DIRECTION('center_axis',(2.74575313258015E-16,-1.,0.));
#125428=DIRECTION('ref_axis',(0.,0.,-1.));
#125429=DIRECTION('',(1.,2.74575313258015E-16,3.39012271766808E-32));
#125430=DIRECTION('center_axis',(0.,1.,0.));
#125431=DIRECTION('ref_axis',(1.,0.,0.));
#125432=DIRECTION('',(-1.,0.,0.));
#125433=DIRECTION('center_axis',(-1.,8.37284837049414E-17,1.03377769602066E-32));
#125434=DIRECTION('ref_axis',(1.03377769602066E-32,0.,1.));
#125435=DIRECTION('',(-8.37284837049414E-17,-1.,0.));
#125436=DIRECTION('',(-8.37284837049414E-17,-1.,-1.23467863058847E-16));
#125437=DIRECTION('center_axis',(8.37284837049414E-17,1.,0.));
#125438=DIRECTION('ref_axis',(0.,0.,1.));
#125439=DIRECTION('center_axis',(0.,0.,1.));
#125440=DIRECTION('ref_axis',(0.,-1.,0.));
#125441=DIRECTION('center_axis',(-4.16713667682363E-30,1.40644112995234E-43,
-1.));
#125442=DIRECTION('ref_axis',(-3.37507799486048E-14,-1.,7.96545955566226E-59));
#125443=DIRECTION('center_axis',(0.,-1.,0.));
#125444=DIRECTION('ref_axis',(0.,0.,-1.));
#125445=DIRECTION('',(1.,0.,0.));
#125446=DIRECTION('center_axis',(-2.65366540778891E-16,1.,0.));
#125447=DIRECTION('ref_axis',(1.,2.65366540778891E-16,0.));
#125448=DIRECTION('',(-1.,-2.65366540778891E-16,-3.27642397172882E-32));
#125449=DIRECTION('center_axis',(-1.,8.37284837049414E-17,1.03377769602066E-32));
#125450=DIRECTION('ref_axis',(1.03377769602066E-32,0.,1.));
#125451=DIRECTION('',(-8.37284837049414E-17,-1.,0.));
#125452=DIRECTION('',(-8.37284837049414E-17,-1.,-1.23467863058847E-16));
#125453=DIRECTION('center_axis',(8.37284837049414E-17,1.,0.));
#125454=DIRECTION('ref_axis',(0.,0.,1.));
#125455=DIRECTION('center_axis',(0.,0.,1.));
#125456=DIRECTION('ref_axis',(0.,-1.,0.));
#125457=DIRECTION('center_axis',(-2.74153728738396E-30,6.08743563864414E-44,
-1.));
#125458=DIRECTION('ref_axis',(-2.22044604925031E-14,-1.,9.95682444457782E-59));
#125459=DIRECTION('center_axis',(1.98661091208406E-16,-1.,0.));
#125460=DIRECTION('ref_axis',(0.,0.,-1.));
#125461=DIRECTION('',(1.,1.98661091208406E-16,2.45282604044407E-32));
#125462=DIRECTION('center_axis',(0.,1.,0.));
#125463=DIRECTION('ref_axis',(1.,0.,0.));
#125464=DIRECTION('',(-1.,0.,0.));
#125465=DIRECTION('center_axis',(-1.,8.37284837049414E-17,1.03377769602066E-32));
#125466=DIRECTION('ref_axis',(1.03377769602066E-32,0.,1.));
#125467=DIRECTION('',(-8.37284837049414E-17,-1.,0.));
#125468=DIRECTION('',(-8.37284837049414E-17,-1.,-1.23467863058847E-16));
#125469=DIRECTION('center_axis',(8.37284837049414E-17,1.,0.));
#125470=DIRECTION('ref_axis',(0.,0.,1.));
#125471=DIRECTION('center_axis',(0.99026806874157,0.139173100960067,1.71834053708127E-17));
#125472=DIRECTION('ref_axis',(1.48746998541713E-33,1.23467863058847E-16,
-1.));
#125473=DIRECTION('',(0.139173100960066,-0.99026806874157,-1.22266282302933E-16));
#125474=DIRECTION('center_axis',(0.,0.,1.));
#125475=DIRECTION('ref_axis',(0.,-1.,0.));
#125476=DIRECTION('',(-3.79382742684518E-34,-1.23467863058847E-16,1.));
#125477=DIRECTION('center_axis',(0.,0.,1.));
#125478=DIRECTION('ref_axis',(0.,-1.,0.));
#125479=DIRECTION('center_axis',(0.99026806874157,-0.139173100960065,-1.71834053708124E-17));
#125480=DIRECTION('ref_axis',(2.50622989185404E-33,1.23467863058847E-16,
-1.));
#125481=DIRECTION('',(-0.139173100960064,-0.99026806874157,-1.22266282302934E-16));
#125482=DIRECTION('center_axis',(0.,0.,1.));
#125483=DIRECTION('ref_axis',(0.,-1.,0.));
#125484=DIRECTION('',(3.05149908249585E-33,1.23467863058847E-16,-1.));
#125485=DIRECTION('center_axis',(0.,0.,1.));
#125486=DIRECTION('ref_axis',(0.,-1.,0.));
#125487=DIRECTION('center_axis',(0.,-1.,0.));
#125488=DIRECTION('ref_axis',(0.,0.,-1.));
#125489=DIRECTION('',(1.,0.,0.));
#125490=DIRECTION('center_axis',(0.,-1.23467863058847E-16,1.));
#125491=DIRECTION('ref_axis',(0.,-1.,-1.23467863058847E-16));
#125492=DIRECTION('',(1.,0.,0.));
#125493=DIRECTION('',(-8.37284837049414E-17,-1.,0.));
#125494=DIRECTION('',(0.139173100960067,-0.99026806874157,-1.22266282302933E-16));
#125495=DIRECTION('',(-8.37284837049414E-17,-1.,0.));
#125496=DIRECTION('center_axis',(2.30289132140253E-30,4.29529458662731E-44,
-1.));
#125497=DIRECTION('ref_axis',(1.86517468137027E-14,-1.,3.48488855560224E-59));
#125498=DIRECTION('',(-8.37284837049414E-17,-1.,0.));
#125499=DIRECTION('center_axis',(-3.72849071084219E-30,1.12593209572362E-43,
-1.));
#125500=DIRECTION('ref_axis',(-3.01980662698043E-14,-1.,1.99136488891557E-59));
#125501=DIRECTION('',(-8.37284837049414E-17,-1.,0.));
#125502=DIRECTION('',(-1.,0.,0.));
#125503=DIRECTION('',(-8.37284837049414E-17,-1.,0.));
#125504=DIRECTION('',(-0.139173100960064,-0.99026806874157,-1.22266282302933E-16));
#125505=DIRECTION('',(-8.37284837049414E-17,-1.,0.));
#125506=DIRECTION('',(0.707106781186546,-0.707106781186549,0.));
#125507=DIRECTION('center_axis',(0.,0.,-1.));
#125508=DIRECTION('ref_axis',(0.,-1.,0.));
#125509=DIRECTION('',(-0.707106781186546,0.707106781186549,0.));
#125510=DIRECTION('',(-1.,0.,0.));
#125511=DIRECTION('',(1.23138919323476E-16,1.,0.));
#125512=DIRECTION('',(1.,6.93889390390722E-15,0.));
#125513=DIRECTION('',(0.707106781186549,0.707106781186546,0.));
#125514=DIRECTION('center_axis',(0.,0.,-1.));
#125515=DIRECTION('ref_axis',(0.,-1.,0.));
#125516=DIRECTION('',(-0.707106781186548,-0.707106781186547,0.));
#125517=DIRECTION('center_axis',(0.99026806874157,0.139173100960067,1.71834053708127E-17));
#125518=DIRECTION('ref_axis',(1.48746998541713E-33,1.23467863058847E-16,
-1.));
#125519=DIRECTION('center_axis',(0.,1.,0.));
#125520=DIRECTION('ref_axis',(1.,0.,0.));
#125521=DIRECTION('center_axis',(8.37284837049414E-17,1.,0.));
#125522=DIRECTION('ref_axis',(0.,0.,1.));
#125523=DIRECTION('',(-8.37284837049414E-17,-1.,-1.23467863058847E-16));
#125524=DIRECTION('center_axis',(-1.,8.37284837049414E-17,1.03377769602066E-32));
#125525=DIRECTION('ref_axis',(1.03377769602066E-32,0.,1.));
#125526=DIRECTION('center_axis',(8.37284837049414E-17,1.,0.));
#125527=DIRECTION('ref_axis',(0.,0.,1.));
#125528=DIRECTION('',(-8.37284837049414E-17,-1.,-1.23467863058847E-16));
#125529=DIRECTION('center_axis',(-1.,8.37284837049414E-17,1.03377769602066E-32));
#125530=DIRECTION('ref_axis',(1.03377769602066E-32,0.,1.));
#125531=DIRECTION('center_axis',(8.37284837049414E-17,1.,0.));
#125532=DIRECTION('ref_axis',(0.,0.,1.));
#125533=DIRECTION('',(-8.37284837049414E-17,-1.,-1.23467863058847E-16));
#125534=DIRECTION('center_axis',(-1.,8.37284837049414E-17,1.03377769602066E-32));
#125535=DIRECTION('ref_axis',(1.03377769602066E-32,0.,1.));
#125536=DIRECTION('center_axis',(8.37284837049414E-17,1.,0.));
#125537=DIRECTION('ref_axis',(0.,0.,1.));
#125538=DIRECTION('',(-8.37284837049414E-17,-1.,-1.23467863058847E-16));
#125539=DIRECTION('center_axis',(-1.,8.37284837049414E-17,1.03377769602066E-32));
#125540=DIRECTION('ref_axis',(1.03377769602066E-32,0.,1.));
#125541=DIRECTION('center_axis',(0.,0.,1.));
#125542=DIRECTION('ref_axis',(0.,-1.,0.));
#125543=DIRECTION('center_axis',(8.37284837049414E-17,1.,0.));
#125544=DIRECTION('ref_axis',(0.,0.,1.));
#125545=DIRECTION('',(-8.37284837049414E-17,-1.,-1.23467863058847E-16));
#125546=DIRECTION('center_axis',(-1.,8.37284837049414E-17,1.03377769602066E-32));
#125547=DIRECTION('ref_axis',(1.03377769602066E-32,0.,1.));
#125548=DIRECTION('center_axis',(0.,0.,1.));
#125549=DIRECTION('ref_axis',(0.,-1.,0.));
#125550=DIRECTION('center_axis',(0.99026806874157,-0.139173100960065,-1.71834053708124E-17));
#125551=DIRECTION('ref_axis',(2.50622989185404E-33,1.23467863058847E-16,
-1.));
#125552=DIRECTION('center_axis',(8.37284837049414E-17,1.,0.));
#125553=DIRECTION('ref_axis',(0.,0.,1.));
#125554=DIRECTION('',(-8.37284837049414E-17,-1.,-1.23467863058847E-16));
#125555=DIRECTION('center_axis',(-1.,8.37284837049414E-17,1.03377769602066E-32));
#125556=DIRECTION('ref_axis',(1.03377769602066E-32,0.,1.));
#125557=DIRECTION('center_axis',(0.707106781186549,0.707106781186546,8.73049632275228E-17));
#125558=DIRECTION('ref_axis',(-1.37111453708203E-33,1.23467863058847E-16,
-1.));
#125559=DIRECTION('',(0.,-1.23467863058847E-16,1.));
#125560=DIRECTION('center_axis',(0.,1.,1.23467863058847E-16));
#125561=DIRECTION('ref_axis',(0.,1.23467863058847E-16,-1.));
#125562=DIRECTION('',(0.,-1.23467863058847E-16,1.));
#125563=DIRECTION('center_axis',(-1.,0.,0.));
#125564=DIRECTION('ref_axis',(0.,0.,1.));
#125565=DIRECTION('center_axis',(6.93889390390722E-15,-1.,-1.23467863058847E-16));
#125566=DIRECTION('ref_axis',(1.7439285617587E-47,1.23467863058847E-16,
-1.));
#125567=DIRECTION('center_axis',(0.707106781186546,-0.707106781186549,-8.73049632275232E-17));
#125568=DIRECTION('ref_axis',(6.2670764807642E-34,1.23467863058847E-16,
-1.));
#125569=DIRECTION('',(0.,-1.23467863058847E-16,1.));
#125570=DIRECTION('center_axis',(0.,0.,1.));
#125571=DIRECTION('ref_axis',(0.,-1.,0.));
#125572=DIRECTION('',(0.,-1.23467863058847E-16,1.));
#125573=DIRECTION('center_axis',(-0.707106781186547,0.707106781186548,8.73049632275232E-17));
#125574=DIRECTION('ref_axis',(1.23467863058848E-16,-3.38443013258907E-33,
1.));
#125575=DIRECTION('center_axis',(0.,-1.,-1.23467863058847E-16));
#125576=DIRECTION('ref_axis',(0.,1.23467863058847E-16,-1.));
#125577=DIRECTION('center_axis',(-0.707106781186549,-0.707106781186546,
-8.73049632275229E-17));
#125578=DIRECTION('ref_axis',(-0.707106781186546,0.707106781186549,-5.88012513992254E-33));
#125579=DIRECTION('',(0.,-1.23467863058847E-16,1.));
#125580=DIRECTION('center_axis',(0.,0.,1.));
#125581=DIRECTION('ref_axis',(0.,-1.,0.));
#125582=DIRECTION('center_axis',(-1.51575151553259E-16,1.51575151553257E-16,
-1.));
#125583=DIRECTION('ref_axis',(-1.,-7.79357634404829E-50,1.51575151553259E-16));
#125584=DIRECTION('center_axis',(-1.51575151553257E-16,-1.68282223215474E-30,
-1.));
#125585=DIRECTION('ref_axis',(-1.11022302462516E-14,1.,-5.25486924121806E-45));
#125586=DIRECTION('center_axis',(-1.51575151553257E-16,-1.68282223215474E-30,
-1.));
#125587=DIRECTION('ref_axis',(-1.11022302462516E-14,1.,-5.25486924121806E-45));
#125588=DIRECTION('center_axis',(-1.51575151553257E-16,-1.68282223215474E-30,
-1.));
#125589=DIRECTION('ref_axis',(-1.11022302462516E-14,1.,-5.25486924121806E-45));
#125590=DIRECTION('center_axis',(-1.51575151553257E-16,-1.68282223215474E-30,
-1.));
#125591=DIRECTION('ref_axis',(-1.11022302462516E-14,1.,-5.25486924121806E-45));
#125592=DIRECTION('center_axis',(-1.51575151553257E-16,-1.68282223215474E-30,
-1.));
#125593=DIRECTION('ref_axis',(-1.11022302462516E-14,1.,-5.25486924121806E-45));
#125594=DIRECTION('center_axis',(-1.51575151553257E-16,-1.68282223215474E-30,
-1.));
#125595=DIRECTION('ref_axis',(-1.11022302462516E-14,1.,-5.25486924121806E-45));
#125596=DIRECTION('center_axis',(1.51575151553257E-16,1.68282223215474E-30,
1.));
#125597=DIRECTION('ref_axis',(-1.11022302462516E-14,1.,-5.25486924121806E-45));
#125598=DIRECTION('center_axis',(1.51575151553257E-16,1.68282223215474E-30,
1.));
#125599=DIRECTION('ref_axis',(-1.11022302462516E-14,1.,-5.25486924121806E-45));
#125600=DIRECTION('center_axis',(1.51575151553257E-16,1.68282223215474E-30,
1.));
#125601=DIRECTION('ref_axis',(-1.11022302462516E-14,1.,-5.25486924121806E-45));
#125602=DIRECTION('center_axis',(1.51575151553257E-16,1.68282223215474E-30,
1.));
#125603=DIRECTION('ref_axis',(-1.11022302462516E-14,1.,-5.25486924121806E-45));
#125604=DIRECTION('center_axis',(1.51575151553257E-16,1.68282223215474E-30,
1.));
#125605=DIRECTION('ref_axis',(-1.11022302462516E-14,1.,-5.25486924121806E-45));
#125606=DIRECTION('center_axis',(1.51575151553257E-16,1.68282223215474E-30,
1.));
#125607=DIRECTION('ref_axis',(-1.11022302462516E-14,1.,-5.25486924121806E-45));
#125608=DIRECTION('center_axis',(-1.51575151553259E-16,1.51575151553257E-16,
-1.));
#125609=DIRECTION('ref_axis',(-1.,-7.79357634404829E-50,1.51575151553259E-16));
#125610=DIRECTION('center_axis',(-1.51575151553257E-16,-1.68282223215474E-30,
-1.));
#125611=DIRECTION('ref_axis',(-1.11022302462516E-14,1.,-5.25486924121806E-45));
#125612=DIRECTION('center_axis',(1.51575151553257E-16,1.68282223215474E-30,
1.));
#125613=DIRECTION('ref_axis',(-1.11022302462516E-14,1.,-5.25486924121806E-45));
#125614=DIRECTION('center_axis',(1.51575151553256E-16,2.10352779019342E-30,
1.));
#125615=DIRECTION('ref_axis',(-1.38777878078145E-14,1.,-8.0574661698677E-45));
#125616=DIRECTION('center_axis',(1.51575151553257E-16,1.26211667411606E-30,
1.));
#125617=DIRECTION('ref_axis',(-8.32667268468868E-15,1.,-4.55422000905566E-45));
#125618=DIRECTION('center_axis',(1.51575151553258E-16,8.41411116077375E-31,
1.));
#125619=DIRECTION('ref_axis',(-5.55111512312578E-15,1.,-2.10194769648723E-45));
#125620=DIRECTION('center_axis',(1.51575151553256E-16,2.94493890627077E-30,
1.));
#125621=DIRECTION('ref_axis',(-1.94289029309402E-14,1.,-3.50324616081204E-45));
#125622=DIRECTION('center_axis',(-1.51575151553257E-16,-1.68282223215474E-30,
-1.));
#125623=DIRECTION('ref_axis',(-1.11022302462516E-14,1.,-5.25486924121806E-45));
#125624=DIRECTION('center_axis',(-1.51575151553257E-16,-1.68282223215474E-30,
-1.));
#125625=DIRECTION('ref_axis',(-1.11022302462516E-14,1.,-5.25486924121806E-45));
#125626=DIRECTION('center_axis',(-1.51575151553257E-16,-1.68282223215474E-30,
-1.));
#125627=DIRECTION('ref_axis',(-1.11022302462516E-14,1.,-5.25486924121806E-45));
#125628=DIRECTION('center_axis',(-1.51575151553257E-16,-1.68282223215474E-30,
-1.));
#125629=DIRECTION('ref_axis',(-1.11022302462516E-14,1.,-5.25486924121806E-45));
#125630=DIRECTION('center_axis',(-1.51575151553257E-16,-1.68282223215474E-30,
-1.));
#125631=DIRECTION('ref_axis',(-1.11022302462516E-14,1.,-5.25486924121806E-45));
#125632=DIRECTION('center_axis',(-1.51575151553257E-16,-1.68282223215474E-30,
-1.));
#125633=DIRECTION('ref_axis',(-1.11022302462516E-14,1.,-5.25486924121806E-45));
#125634=DIRECTION('center_axis',(1.04744440165294E-14,-1.,-1.51575151553259E-16));
#125635=DIRECTION('ref_axis',(1.25902247940101E-46,1.51575151553259E-16,
-1.));
#125636=DIRECTION('',(-3.95893176803294E-18,-1.51575151553259E-16,1.));
#125637=DIRECTION('',(-3.95893176803294E-18,-1.51575151553259E-16,1.));
#125638=DIRECTION('center_axis',(0.866025403784444,-0.49999999999999,-7.23590402936621E-17));
#125639=DIRECTION('ref_axis',(-3.6604109175554E-33,1.44718080587327E-16,
-1.));
#125640=DIRECTION('',(-3.95893176803294E-18,-1.51575151553259E-16,1.));
#125641=DIRECTION('center_axis',(0.866025403784433,0.50000000000001,7.92161112595966E-17));
#125642=DIRECTION('ref_axis',(-8.33872958215071E-33,1.5843222251919E-16,
-1.));
#125643=DIRECTION('',(-3.95893176803294E-18,-1.51575151553259E-16,1.));
#125644=DIRECTION('center_axis',(-1.06246754764031E-14,1.,1.51575151553259E-16));
#125645=DIRECTION('ref_axis',(1.,1.06246754764031E-14,0.));
#125646=DIRECTION('',(-3.95893176803294E-18,-1.51575151553259E-16,1.));
#125647=DIRECTION('center_axis',(-0.866025403784444,0.499999999999991,7.23590402936622E-17));
#125648=DIRECTION('ref_axis',(8.35530227836972E-17,-4.07346201807404E-33,
1.));
#125649=DIRECTION('',(-3.95893176803294E-18,-1.51575151553259E-16,1.));
#125650=DIRECTION('center_axis',(-0.866025403784432,-0.500000000000011,
-7.92161112595969E-17));
#125651=DIRECTION('ref_axis',(-0.500000000000011,0.866025403784432,1.10736588620036E-33));
#125652=DIRECTION('center_axis',(0.,3.03150303106518E-16,-1.));
#125653=DIRECTION('ref_axis',(-1.,0.,0.));
#125654=DIRECTION('center_axis',(0.,3.03150303106518E-16,-1.));
#125655=DIRECTION('ref_axis',(1.,0.,0.));
#125656=DIRECTION('center_axis',(0.,3.03150303106518E-16,-1.));
#125657=DIRECTION('ref_axis',(1.,0.,0.));
#125658=DIRECTION('center_axis',(0.,3.03150303106518E-16,-1.));
#125659=DIRECTION('ref_axis',(1.,0.,0.));
#125660=DIRECTION('center_axis',(0.,3.03150303106518E-16,-1.));
#125661=DIRECTION('ref_axis',(1.,0.,0.));
#125662=DIRECTION('center_axis',(0.,3.03150303106518E-16,-1.));
#125663=DIRECTION('ref_axis',(1.,0.,0.));
#125664=DIRECTION('center_axis',(0.,3.03150303106518E-16,-1.));
#125665=DIRECTION('ref_axis',(1.,0.,0.));
#125666=DIRECTION('center_axis',(0.,-3.03150303106518E-16,1.));
#125667=DIRECTION('ref_axis',(1.,0.,0.));
#125668=DIRECTION('center_axis',(0.,-3.03150303106518E-16,1.));
#125669=DIRECTION('ref_axis',(1.,0.,0.));
#125670=DIRECTION('center_axis',(0.,-3.03150303106518E-16,1.));
#125671=DIRECTION('ref_axis',(1.,0.,0.));
#125672=DIRECTION('center_axis',(0.,-3.03150303106518E-16,1.));
#125673=DIRECTION('ref_axis',(1.,0.,0.));
#125674=DIRECTION('center_axis',(0.,-3.03150303106518E-16,1.));
#125675=DIRECTION('ref_axis',(1.,0.,0.));
#125676=DIRECTION('center_axis',(0.,-3.03150303106518E-16,1.));
#125677=DIRECTION('ref_axis',(1.,0.,0.));
#125678=DIRECTION('center_axis',(0.,3.03150303106518E-16,-1.));
#125679=DIRECTION('ref_axis',(-1.,0.,0.));
#125680=DIRECTION('center_axis',(0.,3.03150303106518E-16,-1.));
#125681=DIRECTION('ref_axis',(1.,0.,0.));
#125682=DIRECTION('center_axis',(0.,-3.03150303106518E-16,1.));
#125683=DIRECTION('ref_axis',(1.,0.,0.));
#125684=DIRECTION('center_axis',(-8.4141111607738E-31,-3.03150303106518E-16,
1.));
#125685=DIRECTION('ref_axis',(1.,-2.77555756156289E-15,2.83543986140725E-45));
#125686=DIRECTION('center_axis',(-8.4141111607738E-31,-3.03150303106518E-16,
1.));
#125687=DIRECTION('ref_axis',(1.,-2.77555756156289E-15,2.83543986140725E-45));
#125688=DIRECTION('center_axis',(8.4141111607738E-31,-3.03150303106518E-16,
1.));
#125689=DIRECTION('ref_axis',(1.,2.77555756156289E-15,-2.83543986140725E-45));
#125690=DIRECTION('center_axis',(-1.68282223215476E-30,-3.03150303106518E-16,
1.));
#125691=DIRECTION('ref_axis',(1.,-5.55111512312578E-15,5.67087972281449E-45));
#125692=DIRECTION('center_axis',(0.,3.03150303106518E-16,-1.));
#125693=DIRECTION('ref_axis',(1.,0.,0.));
#125694=DIRECTION('center_axis',(0.,3.03150303106518E-16,-1.));
#125695=DIRECTION('ref_axis',(1.,0.,0.));
#125696=DIRECTION('center_axis',(0.,3.03150303106518E-16,-1.));
#125697=DIRECTION('ref_axis',(1.,0.,0.));
#125698=DIRECTION('center_axis',(0.,3.03150303106518E-16,-1.));
#125699=DIRECTION('ref_axis',(1.,0.,0.));
#125700=DIRECTION('center_axis',(0.,3.03150303106518E-16,-1.));
#125701=DIRECTION('ref_axis',(1.,0.,0.));
#125702=DIRECTION('center_axis',(0.,3.03150303106518E-16,-1.));
#125703=DIRECTION('ref_axis',(1.,0.,0.));
#125704=DIRECTION('center_axis',(-1.,0.,0.));
#125705=DIRECTION('ref_axis',(0.,0.,1.));
#125706=DIRECTION('',(0.,-1.47616219785226E-16,1.));
#125707=DIRECTION('',(0.,-1.47616219785226E-16,1.));
#125708=DIRECTION('center_axis',(-0.5,-0.866025403784439,-1.27839396344633E-16));
#125709=DIRECTION('ref_axis',(-0.866025403784439,0.5,-4.56072208893389E-33));
#125710=DIRECTION('',(0.,-1.47616219785226E-16,1.));
#125711=DIRECTION('center_axis',(0.5,-0.866025403784438,-1.27839396344633E-16));
#125712=DIRECTION('ref_axis',(-5.60121745056272E-33,1.47616219785226E-16,
-1.));
#125713=DIRECTION('',(0.,-1.47616219785226E-16,1.));
#125714=DIRECTION('center_axis',(1.,1.50231459873716E-16,2.21766001993738E-32));
#125715=DIRECTION('ref_axis',(-1.50231459873716E-16,1.,5.05166336074856E-65));
#125716=DIRECTION('',(0.,-1.47616219785226E-16,1.));
#125717=DIRECTION('center_axis',(0.5,0.866025403784439,1.27839396344633E-16));
#125718=DIRECTION('ref_axis',(2.55678792689265E-16,1.22570872579745E-32,
-1.));
#125719=DIRECTION('',(0.,-1.47616219785226E-16,1.));
#125720=DIRECTION('center_axis',(-0.5,0.866025403784438,1.27839396344632E-16));
#125721=DIRECTION('ref_axis',(2.55678792689264E-16,1.21193584857665E-32,
1.));
#125722=DIRECTION('center_axis',(0.5,0.866025403784438,1.0692630595994E-16));
#125723=DIRECTION('ref_axis',(2.13852611919879E-16,-5.48307457472744E-35,
-1.));
#125724=DIRECTION('',(0.,1.23467863058847E-16,-1.));
#125725=DIRECTION('',(0.,1.23467863058847E-16,-1.));
#125726=DIRECTION('center_axis',(1.,0.,0.));
#125727=DIRECTION('ref_axis',(0.,1.,0.));
#125728=DIRECTION('',(0.,1.23467863058847E-16,-1.));
#125729=DIRECTION('center_axis',(0.5,-0.866025403784439,-1.0692630595994E-16));
#125730=DIRECTION('ref_axis',(4.1166144903646E-33,1.23467863058847E-16,
-1.));
#125731=DIRECTION('',(0.,1.23467863058847E-16,-1.));
#125732=DIRECTION('center_axis',(-0.5,-0.866025403784439,-1.0692630595994E-16));
#125733=DIRECTION('ref_axis',(-0.866025403784439,0.5,-7.83367607530638E-34));
#125734=DIRECTION('',(0.,1.23467863058847E-16,-1.));
#125735=DIRECTION('center_axis',(-1.,0.,0.));
#125736=DIRECTION('ref_axis',(0.,0.,1.));
#125737=DIRECTION('',(0.,1.23467863058847E-16,-1.));
#125738=DIRECTION('center_axis',(-0.5,0.866025403784439,1.0692630595994E-16));
#125739=DIRECTION('ref_axis',(2.1385261191988E-16,4.09037363277686E-33,
1.));
#125740=DIRECTION('center_axis',(0.,0.,-1.));
#125741=DIRECTION('ref_axis',(0.,1.,0.));
#125742=DIRECTION('',(-1.06057523872491E-16,-0.866025403784439,-0.5));
#125743=DIRECTION('center_axis',(0.,0.,-1.));
#125744=DIRECTION('ref_axis',(0.,1.,0.));
#125745=DIRECTION('center_axis',(0.,0.,1.));
#125746=DIRECTION('ref_axis',(0.,1.,0.));
#125747=DIRECTION('center_axis',(0.,0.,-1.));
#125748=DIRECTION('ref_axis',(0.,1.,0.));
#125749=DIRECTION('center_axis',(0.,0.,1.));
#125750=DIRECTION('ref_axis',(0.,1.,0.));
#125751=DIRECTION('center_axis',(0.,0.,-1.));
#125752=DIRECTION('ref_axis',(0.,1.,0.));
#125753=DIRECTION('center_axis',(0.,0.,1.));
#125754=DIRECTION('ref_axis',(0.,1.,0.));
#125755=DIRECTION('center_axis',(0.,0.,-1.));
#125756=DIRECTION('ref_axis',(0.,1.,0.));
#125757=DIRECTION('center_axis',(0.,0.,1.));
#125758=DIRECTION('ref_axis',(0.,1.,0.));
#125759=DIRECTION('center_axis',(0.,0.,-1.));
#125760=DIRECTION('ref_axis',(0.,1.,0.));
#125761=DIRECTION('center_axis',(0.,0.,1.));
#125762=DIRECTION('ref_axis',(0.,1.,0.));
#125763=DIRECTION('center_axis',(0.,0.,-1.));
#125764=DIRECTION('ref_axis',(0.,1.,0.));
#125765=DIRECTION('center_axis',(0.,0.,1.));
#125766=DIRECTION('ref_axis',(0.,1.,0.));
#125767=DIRECTION('center_axis',(0.,1.23467863058847E-16,-1.));
#125768=DIRECTION('ref_axis',(0.,1.,0.));
#125769=DIRECTION('center_axis',(0.,0.,1.));
#125770=DIRECTION('ref_axis',(0.,1.,0.));
#125771=DIRECTION('center_axis',(-1.,0.,0.));
#125772=DIRECTION('ref_axis',(0.,-1.,0.));
#125773=DIRECTION('center_axis',(0.,0.,-1.));
#125774=DIRECTION('ref_axis',(0.,1.,0.));
#125775=DIRECTION('center_axis',(0.,0.,-1.));
#125776=DIRECTION('ref_axis',(0.,1.,0.));
#125777=DIRECTION('center_axis',(0.,1.23467863058847E-16,-1.));
#125778=DIRECTION('ref_axis',(-1.,0.,0.));
#125779=DIRECTION('center_axis',(0.,0.,1.));
#125780=DIRECTION('ref_axis',(0.,1.,0.));
#125781=DIRECTION('center_axis',(0.,1.23467863058847E-16,-1.));
#125782=DIRECTION('ref_axis',(-1.,0.,0.));
#125783=DIRECTION('center_axis',(0.,0.,1.));
#125784=DIRECTION('ref_axis',(0.,-1.,0.));
#125785=DIRECTION('',(0.,0.,-1.));
#125786=DIRECTION('center_axis',(0.,0.581981048437469,0.813202348287082));
#125787=DIRECTION('ref_axis',(0.,-0.813202348287082,0.581981048437469));
#125788=DIRECTION('center_axis',(-4.57440509151562E-13,-3.7199169624361E-13,
1.));
#125789=DIRECTION('ref_axis',(1.53744223053601E-12,-1.,-3.71991696242907E-13));
#125790=DIRECTION('center_axis',(6.93710496602244E-15,-1.,3.73149770104689E-14));
#125791=DIRECTION('ref_axis',(-7.99856117158489E-13,-3.73149770104744E-14,
-1.));
#125792=DIRECTION('',(0.,-0.581981048437474,-0.813202348287079));
#125793=DIRECTION('center_axis',(0.,-0.581981048437448,0.813202348287097));
#125794=DIRECTION('ref_axis',(0.,-0.813202348287097,-0.581981048437448));
#125795=DIRECTION('',(0.,0.581981048437457,-0.813202348287091));
#125796=DIRECTION('center_axis',(-2.04313070362676E-13,-1.,-2.05422270127779E-14));
#125797=DIRECTION('ref_axis',(-1.51334794436645E-12,2.05422270130871E-14,
-1.));
#125798=DIRECTION('center_axis',(0.,-0.581981048437448,0.813202348287097));
#125799=DIRECTION('ref_axis',(0.,-0.813202348287097,-0.581981048437448));
#125800=DIRECTION('center_axis',(0.,0.,-1.));
#125801=DIRECTION('ref_axis',(-1.,0.,0.));
#125802=DIRECTION('center_axis',(0.,-1.,0.));
#125803=DIRECTION('ref_axis',(-4.85369761888787E-14,0.,1.));
#125804=DIRECTION('center_axis',(-1.,2.31296463463574E-14,0.));
#125805=DIRECTION('ref_axis',(-2.31296463463574E-14,-1.,0.));
#125806=DIRECTION('center_axis',(0.,-1.,0.));
#125807=DIRECTION('ref_axis',(0.,0.,1.));
#125808=DIRECTION('center_axis',(1.,0.,0.));
#125809=DIRECTION('ref_axis',(0.,0.,1.));
#125810=DIRECTION('',(-1.,0.,0.));
#125811=DIRECTION('center_axis',(-1.,-9.25185853854296E-15,0.));
#125812=DIRECTION('ref_axis',(9.25185853854296E-15,-1.,0.));
#125813=DIRECTION('',(1.,0.,0.));
#125814=DIRECTION('center_axis',(0.,0.,-1.));
#125815=DIRECTION('ref_axis',(-1.,0.,0.));
#125816=DIRECTION('center_axis',(0.,-1.,0.));
#125817=DIRECTION('ref_axis',(0.,0.,1.));
#125818=DIRECTION('center_axis',(0.79173164804714,0.610869051008938,0.));
#125819=DIRECTION('ref_axis',(0.610869051008938,-0.79173164804714,0.));
#125820=DIRECTION('center_axis',(1.,0.,0.));
#125821=DIRECTION('ref_axis',(0.,0.,1.));
#125822=DIRECTION('center_axis',(0.,0.598310875192794,0.801264061733729));
#125823=DIRECTION('ref_axis',(0.,-0.801264061733729,0.598310875192794));
#125824=DIRECTION('center_axis',(0.,0.,-1.));
#125825=DIRECTION('ref_axis',(-1.,0.,0.));
#125826=DIRECTION('center_axis',(-1.,0.,0.));
#125827=DIRECTION('ref_axis',(0.,0.,1.));
#125828=DIRECTION('center_axis',(0.,0.,-1.));
#125829=DIRECTION('ref_axis',(-1.,0.,0.));
#125830=DIRECTION('center_axis',(-1.8733679913752E-13,0.0769742127966581,
0.997033083986853));
#125831=DIRECTION('ref_axis',(5.10679254440911E-30,0.997033083986853,-0.0769742127966581));
#125832=DIRECTION('center_axis',(0.,-1.,0.));
#125833=DIRECTION('ref_axis',(9.86527759356758E-14,0.,1.));
#125834=DIRECTION('center_axis',(1.,0.,0.));
#125835=DIRECTION('ref_axis',(0.,0.,1.));
#125836=DIRECTION('center_axis',(1.,0.,0.));
#125837=DIRECTION('ref_axis',(0.,2.66826051581462E-14,1.));
#125838=DIRECTION('center_axis',(1.,0.,0.));
#125839=DIRECTION('ref_axis',(0.,0.,1.));
#125840=DIRECTION('center_axis',(2.95998963611366E-29,-0.0769742127965279,
0.997033083986863));
#125841=DIRECTION('ref_axis',(1.85037170770858E-14,-0.997033083986863,-0.0769742127965279));
#125842=DIRECTION('center_axis',(1.,0.,0.));
#125843=DIRECTION('ref_axis',(0.,2.66826051581462E-14,1.));
#125844=DIRECTION('center_axis',(0.,0.,-1.));
#125845=DIRECTION('ref_axis',(-1.,0.,0.));
#125846=DIRECTION('center_axis',(2.36831436293266E-13,-0.598310875192877,
0.801264061733667));
#125847=DIRECTION('ref_axis',(4.05016586084113E-29,0.801264061733667,0.598310875192877));
#125848=DIRECTION('center_axis',(0.,-1.,0.));
#125849=DIRECTION('ref_axis',(0.,0.,1.));
#125850=DIRECTION('center_axis',(1.,0.,0.));
#125851=DIRECTION('ref_axis',(0.,0.,1.));
#125852=DIRECTION('center_axis',(0.,0.,1.));
#125853=DIRECTION('ref_axis',(1.,0.,0.));
#125854=DIRECTION('center_axis',(-1.,0.,0.));
#125855=DIRECTION('ref_axis',(0.,0.,1.));
#125856=DIRECTION('center_axis',(0.,0.,1.));
#125857=DIRECTION('ref_axis',(-1.,0.,0.));
#125858=DIRECTION('center_axis',(1.,0.,0.));
#125859=DIRECTION('ref_axis',(0.,0.,-1.));
#125860=DIRECTION('center_axis',(0.,0.,-1.));
#125861=DIRECTION('ref_axis',(-1.,0.,0.));
#125862=DIRECTION('center_axis',(0.,0.,-1.));
#125863=DIRECTION('ref_axis',(1.,0.,0.));
#125864=DIRECTION('center_axis',(1.,0.,-9.25185853854296E-15));
#125865=DIRECTION('ref_axis',(-9.25185853854296E-15,0.,-1.));
#125866=DIRECTION('center_axis',(0.,0.,1.));
#125867=DIRECTION('ref_axis',(1.,0.,0.));
#125868=DIRECTION('center_axis',(0.,0.581981048437445,0.813202348287099));
#125869=DIRECTION('ref_axis',(0.,-0.813202348287099,0.581981048437445));
#125870=DIRECTION('center_axis',(6.06486161256154E-14,-1.,-1.46202248832107E-14));
#125871=DIRECTION('ref_axis',(7.25749190859778E-12,1.46202248836508E-14,
-1.));
#125872=DIRECTION('',(0.,-0.581981048437472,-0.81320234828708));
#125873=DIRECTION('center_axis',(1.71540190931773E-13,1.39496886091321E-13,
-1.));
#125874=DIRECTION('ref_axis',(1.40059985610807E-12,1.,1.39496886091562E-13));
#125875=DIRECTION('',(0.,0.581981048437472,0.81320234828708));
#125876=DIRECTION('center_axis',(0.,-0.581981048437456,0.813202348287091));
#125877=DIRECTION('ref_axis',(0.,-0.813202348287091,-0.581981048437456));
#125878=DIRECTION('center_axis',(8.57700954657943E-14,-1.,4.99165700837713E-14));
#125879=DIRECTION('ref_axis',(-3.54373217756707E-13,-4.99165700838017E-14,
-1.));
#125880=DIRECTION('',(0.,-0.581981048437457,0.813202348287091));
#125881=DIRECTION('',(0.,0.581981048437457,-0.813202348287091));
#125882=DIRECTION('center_axis',(-1.,0.,0.));
#125883=DIRECTION('ref_axis',(0.,0.,1.));
#125884=DIRECTION('',(0.,0.,-1.));
#125885=DIRECTION('',(0.,1.,0.));
#125886=DIRECTION('center_axis',(-1.,0.,0.));
#125887=DIRECTION('ref_axis',(0.,0.,1.));
#125888=DIRECTION('',(0.,0.,-1.));
#125889=DIRECTION('',(0.,1.,0.));
#125890=DIRECTION('center_axis',(1.,0.,0.));
#125891=DIRECTION('ref_axis',(0.,1.,0.));
#125892=DIRECTION('',(0.,0.,1.));
#125893=DIRECTION('',(0.,0.,1.));
#125894=DIRECTION('',(0.,-1.,0.));
#125895=DIRECTION('',(0.,3.03450170724806E-16,1.));
#125896=DIRECTION('',(0.,-1.,0.));
#125897=DIRECTION('',(0.,0.,1.));
#125898=DIRECTION('center_axis',(0.,0.581981048437469,0.813202348287082));
#125899=DIRECTION('ref_axis',(0.,-0.813202348287082,0.581981048437469));
#125900=DIRECTION('',(0.,-0.581981048437474,-0.813202348287079));
#125901=DIRECTION('center_axis',(1.64603085965779E-13,-1.,1.37148117178086E-13));
#125902=DIRECTION('ref_axis',(6.31098224630747E-13,-1.37148117177982E-13,
-1.));
#125903=DIRECTION('center_axis',(-4.57440509151577E-13,3.71991696243625E-13,
-1.));
#125904=DIRECTION('ref_axis',(1.52275222876736E-12,1.,3.71991696242928E-13));
#125905=DIRECTION('center_axis',(0.,-0.581981048437448,0.813202348287097));
#125906=DIRECTION('ref_axis',(0.,-0.813202348287097,-0.581981048437448));
#125907=DIRECTION('center_axis',(0.,0.581981048437448,-0.813202348287097));
#125908=DIRECTION('ref_axis',(0.,-0.813202348287097,-0.581981048437448));
#125909=DIRECTION('center_axis',(2.04313070362666E-13,-1.,-2.05422270127758E-14));
#125910=DIRECTION('ref_axis',(7.96460775263604E-12,2.05422270144031E-14,
-1.));
#125911=DIRECTION('',(0.,0.581981048437457,-0.813202348287091));
#125912=DIRECTION('center_axis',(0.,0.,-1.));
#125913=DIRECTION('ref_axis',(1.,0.,0.));
#125914=DIRECTION('center_axis',(-1.,-2.31296463463574E-14,0.));
#125915=DIRECTION('ref_axis',(2.31296463463574E-14,-1.,0.));
#125916=DIRECTION('center_axis',(0.,-1.,0.));
#125917=DIRECTION('ref_axis',(-1.61789920629596E-14,0.,1.));
#125918=DIRECTION('center_axis',(0.,1.,0.));
#125919=DIRECTION('ref_axis',(0.,0.,1.));
#125920=DIRECTION('center_axis',(-1.,0.,0.));
#125921=DIRECTION('ref_axis',(0.,0.,1.));
#125922=DIRECTION('center_axis',(-1.,9.25185853854296E-15,0.));
#125923=DIRECTION('ref_axis',(-9.25185853854296E-15,-1.,0.));
#125924=DIRECTION('',(-1.,0.,0.));
#125925=DIRECTION('',(-1.,0.,0.));
#125926=DIRECTION('center_axis',(0.,0.,-1.));
#125927=DIRECTION('ref_axis',(1.,0.,0.));
#125928=DIRECTION('center_axis',(0.79173164804714,-0.610869051008938,0.));
#125929=DIRECTION('ref_axis',(-0.610869051008938,-0.79173164804714,0.));
#125930=DIRECTION('center_axis',(0.,-1.,0.));
#125931=DIRECTION('ref_axis',(1.29431936503677E-13,0.,1.));
#125932=DIRECTION('center_axis',(-1.,0.,0.));
#125933=DIRECTION('ref_axis',(0.,0.,1.));
#125934=DIRECTION('center_axis',(0.,0.,1.));
#125935=DIRECTION('ref_axis',(1.,0.,0.));
#125936=DIRECTION('center_axis',(0.,-0.598310875192794,-0.801264061733729));
#125937=DIRECTION('ref_axis',(0.,-0.801264061733729,0.598310875192794));
#125938=DIRECTION('center_axis',(-1.,0.,0.));
#125939=DIRECTION('ref_axis',(0.,0.,1.));
#125940=DIRECTION('center_axis',(0.,0.,-1.));
#125941=DIRECTION('ref_axis',(1.,0.,0.));
#125942=DIRECTION('center_axis',(0.,-1.,0.));
#125943=DIRECTION('ref_axis',(2.30189810516577E-13,0.,1.));
#125944=DIRECTION('center_axis',(-1.8733679913752E-13,-0.0769742127966581,
-0.997033083986853));
#125945=DIRECTION('ref_axis',(-5.10679254440911E-30,0.997033083986853,-0.0769742127966581));
#125946=DIRECTION('center_axis',(-1.,0.,0.));
#125947=DIRECTION('ref_axis',(0.,0.,1.));
#125948=DIRECTION('center_axis',(1.,0.,0.));
#125949=DIRECTION('ref_axis',(0.,2.66826051581462E-14,1.));
#125950=DIRECTION('center_axis',(-1.,0.,0.));
#125951=DIRECTION('ref_axis',(0.,0.,1.));
#125952=DIRECTION('center_axis',(1.,0.,0.));
#125953=DIRECTION('ref_axis',(0.,2.66826051581462E-14,1.));
#125954=DIRECTION('center_axis',(2.95998963611366E-29,0.0769742127965279,
-0.997033083986863));
#125955=DIRECTION('ref_axis',(-1.85037170770858E-14,-0.997033083986863,
-0.0769742127965279));
#125956=DIRECTION('center_axis',(0.,0.,-1.));
#125957=DIRECTION('ref_axis',(1.,0.,0.));
#125958=DIRECTION('center_axis',(0.,-1.,0.));
#125959=DIRECTION('ref_axis',(-2.19228390968164E-14,0.,1.));
#125960=DIRECTION('center_axis',(2.36831436293266E-13,0.598310875192877,
-0.801264061733667));
#125961=DIRECTION('ref_axis',(-4.05016586084113E-29,0.801264061733667,0.598310875192877));
#125962=DIRECTION('center_axis',(-1.,0.,0.));
#125963=DIRECTION('ref_axis',(0.,0.,1.));
#125964=DIRECTION('center_axis',(0.,0.,-1.));
#125965=DIRECTION('ref_axis',(-1.,0.,0.));
#125966=DIRECTION('center_axis',(-1.,0.,0.));
#125967=DIRECTION('ref_axis',(0.,0.,1.));
#125968=DIRECTION('center_axis',(0.,0.,1.));
#125969=DIRECTION('ref_axis',(1.,0.,0.));
#125970=DIRECTION('center_axis',(0.,0.,1.));
#125971=DIRECTION('ref_axis',(1.,0.,0.));
#125972=DIRECTION('center_axis',(1.,0.,0.));
#125973=DIRECTION('ref_axis',(0.,0.,-1.));
#125974=DIRECTION('center_axis',(0.,0.,-1.));
#125975=DIRECTION('ref_axis',(-1.,0.,0.));
#125976=DIRECTION('center_axis',(1.,0.,9.25185853854296E-15));
#125977=DIRECTION('ref_axis',(9.25185853854296E-15,0.,-1.));
#125978=DIRECTION('center_axis',(0.,0.,-1.));
#125979=DIRECTION('ref_axis',(-1.,0.,0.));
#125980=DIRECTION('center_axis',(0.,0.581981048437445,0.813202348287099));
#125981=DIRECTION('ref_axis',(0.,-0.813202348287099,0.581981048437445));
#125982=DIRECTION('center_axis',(-6.06486161256147E-14,-1.,-1.46202248832103E-14));
#125983=DIRECTION('ref_axis',(-6.92803770888931E-12,1.46202248836305E-14,
-1.));
#125984=DIRECTION('',(0.,0.581981048437472,0.81320234828708));
#125985=DIRECTION('center_axis',(1.71540190931776E-13,-1.39496886091324E-13,
1.));
#125986=DIRECTION('ref_axis',(1.4629488977046E-12,-1.,-1.39496886091575E-13));
#125987=DIRECTION('',(0.,-0.581981048437472,-0.81320234828708));
#125988=DIRECTION('center_axis',(0.,-0.581981048437456,0.813202348287091));
#125989=DIRECTION('ref_axis',(0.,-0.813202348287091,-0.581981048437456));
#125990=DIRECTION('center_axis',(-8.5770095465791E-14,-1.,4.99165700837693E-14));
#125991=DIRECTION('ref_axis',(8.1434249535045E-13,-4.99165700838392E-14,
-1.));
#125992=DIRECTION('',(0.,0.581981048437457,-0.813202348287091));
#125993=DIRECTION('',(0.,-0.581981048437457,0.813202348287091));
#125994=DIRECTION('center_axis',(1.,0.,0.));
#125995=DIRECTION('ref_axis',(0.,1.,0.));
#125996=DIRECTION('',(0.,0.,1.));
#125997=DIRECTION('',(0.,1.,0.));
#125998=DIRECTION('center_axis',(1.,0.,0.));
#125999=DIRECTION('ref_axis',(0.,1.,0.));
#126000=DIRECTION('',(0.,0.,1.));
#126001=DIRECTION('',(0.,1.,0.));
#126002=DIRECTION('center_axis',(0.,0.81320234828708,-0.581981048437472));
#126003=DIRECTION('ref_axis',(-1.,0.,0.));
#126004=DIRECTION('',(1.,0.,0.));
#126005=DIRECTION('',(-1.,0.,0.));
#126006=DIRECTION('center_axis',(0.,0.813202348287091,0.581981048437457));
#126007=DIRECTION('ref_axis',(1.,0.,0.));
#126008=DIRECTION('',(-1.,0.,0.));
#126009=DIRECTION('',(1.,0.,0.));
#126010=DIRECTION('center_axis',(-1.,0.,0.));
#126011=DIRECTION('ref_axis',(0.,0.,1.));
#126012=DIRECTION('',(0.,0.,-1.));
#126013=DIRECTION('',(0.,0.,1.));
#126014=DIRECTION('',(0.,-1.,0.));
#126015=DIRECTION('',(0.,3.03450170724806E-16,1.));
#126016=DIRECTION('',(0.,-1.,0.));
#126017=DIRECTION('',(0.,0.,1.));
#126018=DIRECTION('center_axis',(0.,-1.,0.));
#126019=DIRECTION('ref_axis',(0.,0.,-1.));
#126020=DIRECTION('center_axis',(0.,-1.,0.));
#126021=DIRECTION('ref_axis',(0.,0.,1.));
#126022=DIRECTION('',(0.,-1.,0.));
#126023=DIRECTION('center_axis',(1.,0.,0.));
#126024=DIRECTION('ref_axis',(0.,0.,-1.));
#126025=DIRECTION('center_axis',(0.,0.,-1.));
#126026=DIRECTION('ref_axis',(1.,0.,0.));
#126027=DIRECTION('center_axis',(0.,0.,-1.));
#126028=DIRECTION('ref_axis',(-1.,0.,0.));
#126029=DIRECTION('',(0.,0.,-1.));
#126030=DIRECTION('center_axis',(0.,1.,0.));
#126031=DIRECTION('ref_axis',(0.,0.,1.));
#126032=DIRECTION('center_axis',(1.,0.,0.));
#126033=DIRECTION('ref_axis',(0.,0.,-1.));
#126034=DIRECTION('center_axis',(0.,1.,0.));
#126035=DIRECTION('ref_axis',(0.,0.,1.));
#126036=DIRECTION('center_axis',(0.,-1.,0.));
#126037=DIRECTION('ref_axis',(0.,0.,1.));
#126038=DIRECTION('center_axis',(1.,0.,0.));
#126039=DIRECTION('ref_axis',(0.,0.,1.));
#126040=DIRECTION('',(-1.,0.,0.));
#126041=DIRECTION('',(1.,0.,0.));
#126042=DIRECTION('center_axis',(0.,0.,1.));
#126043=DIRECTION('ref_axis',(-1.,0.,0.));
#126044=DIRECTION('center_axis',(0.,0.,1.));
#126045=DIRECTION('ref_axis',(1.,0.,0.));
#126046=DIRECTION('',(0.,0.,-1.));
#126047=DIRECTION('center_axis',(0.,-1.,0.));
#126048=DIRECTION('ref_axis',(0.,0.,-1.));
#126049=DIRECTION('center_axis',(1.,0.,0.));
#126050=DIRECTION('ref_axis',(0.,0.,-1.));
#126051=DIRECTION('center_axis',(0.,-1.,0.));
#126052=DIRECTION('ref_axis',(0.,0.,-1.));
#126053=DIRECTION('center_axis',(0.,1.,0.));
#126054=DIRECTION('ref_axis',(0.,0.,-1.));
#126055=DIRECTION('center_axis',(1.,0.,0.));
#126056=DIRECTION('ref_axis',(0.,0.,1.));
#126057=DIRECTION('',(-1.,0.,0.));
#126058=DIRECTION('',(1.,0.,0.));
#126059=DIRECTION('center_axis',(0.,-1.,0.));
#126060=DIRECTION('ref_axis',(0.,0.,-1.));
#126061=DIRECTION('center_axis',(0.,1.,0.));
#126062=DIRECTION('ref_axis',(0.,0.,-1.));
#126063=DIRECTION('',(0.,-1.,0.));
#126064=DIRECTION('center_axis',(0.,-1.,0.));
#126065=DIRECTION('ref_axis',(0.,0.,-1.));
#126066=DIRECTION('center_axis',(0.,1.,0.));
#126067=DIRECTION('ref_axis',(0.,0.,-1.));
#126068=DIRECTION('',(0.,-1.,0.));
#126069=DIRECTION('center_axis',(0.,-1.,3.03450170724806E-16));
#126070=DIRECTION('ref_axis',(-1.,0.,0.));
#126071=DIRECTION('',(1.,0.,0.));
#126072=DIRECTION('center_axis',(0.,-1.,0.));
#126073=DIRECTION('ref_axis',(0.,0.,-1.));
#126074=DIRECTION('center_axis',(0.,-1.,0.));
#126075=DIRECTION('ref_axis',(0.,0.,-1.));
#126076=DIRECTION('',(-1.,0.,0.));
#126077=DIRECTION('center_axis',(0.,-1.,0.));
#126078=DIRECTION('ref_axis',(0.,0.,-1.));
#126079=DIRECTION('center_axis',(0.,1.,0.));
#126080=DIRECTION('ref_axis',(0.,0.,1.));
#126081=DIRECTION('',(0.,-1.,0.));
#126082=DIRECTION('center_axis',(1.,0.,0.));
#126083=DIRECTION('ref_axis',(0.,0.,-1.));
#126084=DIRECTION('center_axis',(-1.,0.,0.));
#126085=DIRECTION('ref_axis',(0.,0.,1.));
#126086=DIRECTION('',(-1.,0.,0.));
#126087=DIRECTION('center_axis',(0.,0.,-1.));
#126088=DIRECTION('ref_axis',(-1.,0.,0.));
#126089=DIRECTION('center_axis',(0.,0.,1.));
#126090=DIRECTION('ref_axis',(1.,0.,0.));
#126091=DIRECTION('',(0.,0.,-1.));
#126092=DIRECTION('center_axis',(0.,1.,0.));
#126093=DIRECTION('ref_axis',(0.,0.,1.));
#126094=DIRECTION('center_axis',(1.,0.,0.));
#126095=DIRECTION('ref_axis',(0.,0.,-1.));
#126096=DIRECTION('center_axis',(0.,1.,0.));
#126097=DIRECTION('ref_axis',(0.,0.,1.));
#126098=DIRECTION('center_axis',(0.,-1.,0.));
#126099=DIRECTION('ref_axis',(0.,0.,1.));
#126100=DIRECTION('center_axis',(-1.,0.,0.));
#126101=DIRECTION('ref_axis',(0.,0.,1.));
#126102=DIRECTION('',(-1.,0.,0.));
#126103=DIRECTION('',(1.,0.,0.));
#126104=DIRECTION('center_axis',(0.,0.,1.));
#126105=DIRECTION('ref_axis',(1.,0.,0.));
#126106=DIRECTION('center_axis',(0.,0.,-1.));
#126107=DIRECTION('ref_axis',(-1.,0.,0.));
#126108=DIRECTION('',(0.,0.,-1.));
#126109=DIRECTION('center_axis',(0.,-1.,0.));
#126110=DIRECTION('ref_axis',(0.,0.,-1.));
#126111=DIRECTION('center_axis',(1.,0.,0.));
#126112=DIRECTION('ref_axis',(0.,0.,-1.));
#126113=DIRECTION('center_axis',(0.,-1.,0.));
#126114=DIRECTION('ref_axis',(0.,0.,-1.));
#126115=DIRECTION('center_axis',(0.,1.,0.));
#126116=DIRECTION('ref_axis',(0.,0.,-1.));
#126117=DIRECTION('center_axis',(-1.,0.,0.));
#126118=DIRECTION('ref_axis',(0.,0.,1.));
#126119=DIRECTION('',(-1.,0.,0.));
#126120=DIRECTION('',(1.,0.,0.));
#126121=DIRECTION('center_axis',(0.,1.,0.));
#126122=DIRECTION('ref_axis',(1.,0.,0.));
#126123=DIRECTION('',(1.,0.,0.));
#126124=DIRECTION('',(-1.,0.,0.));
#126125=DIRECTION('center_axis',(0.,0.,1.));
#126126=DIRECTION('ref_axis',(1.,0.,0.));
#126127=DIRECTION('',(0.,-1.,0.));
#126128=DIRECTION('center_axis',(0.,0.,-1.));
#126129=DIRECTION('ref_axis',(0.,-1.,0.));
#126130=DIRECTION('',(0.,-1.,0.));
#126131=DIRECTION('center_axis',(0.,-1.,0.));
#126132=DIRECTION('ref_axis',(0.,0.,-1.));
#126133=DIRECTION('center_axis',(0.,-1.,0.));
#126134=DIRECTION('ref_axis',(0.,0.,-1.));
#126135=DIRECTION('center_axis',(0.,0.,-1.));
#126136=DIRECTION('ref_axis',(0.,1.,0.));
#126137=DIRECTION('',(0.,0.,-1.));
#126138=DIRECTION('center_axis',(0.,0.,1.));
#126139=DIRECTION('ref_axis',(-1.,0.,0.));
#126140=DIRECTION('center_axis',(0.,0.,-1.));
#126141=DIRECTION('ref_axis',(0.,1.,0.));
#126142=DIRECTION('',(0.,0.,-1.));
#126143=DIRECTION('center_axis',(0.,0.,-1.));
#126144=DIRECTION('ref_axis',(0.,1.,0.));
#126145=DIRECTION('',(0.,0.,-1.));
#126146=DIRECTION('center_axis',(0.,0.,-1.));
#126147=DIRECTION('ref_axis',(0.,1.,0.));
#126148=DIRECTION('',(0.,0.,-1.));
#126149=DIRECTION('center_axis',(0.,0.,-1.));
#126150=DIRECTION('ref_axis',(0.,1.,0.));
#126151=DIRECTION('',(0.,0.,-1.));
#126152=DIRECTION('center_axis',(0.,0.,-1.));
#126153=DIRECTION('ref_axis',(0.,1.,0.));
#126154=DIRECTION('',(0.,0.,-1.));
#126155=DIRECTION('center_axis',(0.,0.,-1.));
#126156=DIRECTION('ref_axis',(0.,1.,0.));
#126157=DIRECTION('',(0.,0.,-1.));
#126158=DIRECTION('center_axis',(0.,0.,-1.));
#126159=DIRECTION('ref_axis',(0.,1.,0.));
#126160=DIRECTION('',(0.,0.,-1.));
#126161=DIRECTION('center_axis',(0.,0.,-1.));
#126162=DIRECTION('ref_axis',(0.,1.,0.));
#126163=DIRECTION('',(0.,0.,-1.));
#126164=DIRECTION('center_axis',(0.,0.,-1.));
#126165=DIRECTION('ref_axis',(0.,1.,0.));
#126166=DIRECTION('',(0.,0.,-1.));
#126167=DIRECTION('center_axis',(0.,0.,-1.));
#126168=DIRECTION('ref_axis',(0.,1.,0.));
#126169=DIRECTION('',(0.,0.,-1.));
#126170=DIRECTION('center_axis',(0.,0.,-1.));
#126171=DIRECTION('ref_axis',(0.,1.,0.));
#126172=DIRECTION('',(0.,0.,-1.));
#126173=DIRECTION('center_axis',(0.,0.,-1.));
#126174=DIRECTION('ref_axis',(0.,1.,0.));
#126175=DIRECTION('',(0.,0.,-1.));
#126176=DIRECTION('center_axis',(0.,0.,-1.));
#126177=DIRECTION('ref_axis',(0.,1.,0.));
#126178=DIRECTION('',(0.,0.,-1.));
#126179=DIRECTION('center_axis',(0.,0.,-1.));
#126180=DIRECTION('ref_axis',(0.,1.,0.));
#126181=DIRECTION('',(0.,0.,-1.));
#126182=DIRECTION('center_axis',(0.,0.,-1.));
#126183=DIRECTION('ref_axis',(0.,1.,0.));
#126184=DIRECTION('',(0.,0.,-1.));
#126185=DIRECTION('center_axis',(0.,0.,-1.));
#126186=DIRECTION('ref_axis',(0.,1.,0.));
#126187=DIRECTION('',(0.,0.,-1.));
#126188=DIRECTION('center_axis',(0.,0.,-1.));
#126189=DIRECTION('ref_axis',(0.,1.,0.));
#126190=DIRECTION('',(0.,0.,-1.));
#126191=DIRECTION('center_axis',(0.,0.,-1.));
#126192=DIRECTION('ref_axis',(0.,1.,0.));
#126193=DIRECTION('',(0.,0.,-1.));
#126194=DIRECTION('center_axis',(0.,0.,-1.));
#126195=DIRECTION('ref_axis',(0.,1.,0.));
#126196=DIRECTION('',(0.,0.,-1.));
#126197=DIRECTION('center_axis',(0.,0.,-1.));
#126198=DIRECTION('ref_axis',(1.,0.,0.));
#126199=DIRECTION('center_axis',(0.,0.,-1.));
#126200=DIRECTION('ref_axis',(0.,1.,0.));
#126201=DIRECTION('',(0.,0.,-1.));
#126202=DIRECTION('center_axis',(0.,0.,-1.));
#126203=DIRECTION('ref_axis',(0.,1.,0.));
#126204=DIRECTION('',(0.,0.,-1.));
#126205=DIRECTION('center_axis',(0.,0.,-1.));
#126206=DIRECTION('ref_axis',(0.,1.,0.));
#126207=DIRECTION('',(0.,0.,-1.));
#126208=DIRECTION('center_axis',(0.,0.,-1.));
#126209=DIRECTION('ref_axis',(0.,1.,0.));
#126210=DIRECTION('',(0.,0.,-1.));
#126211=DIRECTION('center_axis',(0.,0.,-1.));
#126212=DIRECTION('ref_axis',(0.,1.,0.));
#126213=DIRECTION('',(0.,0.,-1.));
#126214=DIRECTION('center_axis',(0.,0.,-1.));
#126215=DIRECTION('ref_axis',(0.,1.,0.));
#126216=DIRECTION('',(0.,0.,-1.));
#126217=DIRECTION('center_axis',(0.,0.,-1.));
#126218=DIRECTION('ref_axis',(0.,1.,0.));
#126219=DIRECTION('',(0.,0.,-1.));
#126220=DIRECTION('center_axis',(0.,0.,-1.));
#126221=DIRECTION('ref_axis',(0.,1.,0.));
#126222=DIRECTION('',(0.,0.,-1.));
#126223=DIRECTION('center_axis',(0.,0.,-1.));
#126224=DIRECTION('ref_axis',(0.,1.,0.));
#126225=DIRECTION('',(0.,0.,-1.));
#126226=DIRECTION('center_axis',(0.,0.,-1.));
#126227=DIRECTION('ref_axis',(0.,1.,0.));
#126228=DIRECTION('',(0.,0.,-1.));
#126229=DIRECTION('center_axis',(0.,0.,-1.));
#126230=DIRECTION('ref_axis',(0.,1.,0.));
#126231=DIRECTION('',(0.,0.,-1.));
#126232=DIRECTION('center_axis',(0.,0.,-1.));
#126233=DIRECTION('ref_axis',(0.,1.,0.));
#126234=DIRECTION('',(0.,0.,-1.));
#126235=DIRECTION('center_axis',(0.,0.,-1.));
#126236=DIRECTION('ref_axis',(0.,1.,0.));
#126237=DIRECTION('',(0.,0.,-1.));
#126238=DIRECTION('center_axis',(0.,0.,-1.));
#126239=DIRECTION('ref_axis',(0.,1.,0.));
#126240=DIRECTION('',(0.,0.,-1.));
#126241=DIRECTION('center_axis',(0.,0.,-1.));
#126242=DIRECTION('ref_axis',(0.,1.,0.));
#126243=DIRECTION('',(0.,0.,-1.));
#126244=DIRECTION('center_axis',(0.,0.,-1.));
#126245=DIRECTION('ref_axis',(0.,1.,0.));
#126246=DIRECTION('',(0.,0.,-1.));
#126247=DIRECTION('center_axis',(0.,0.,-1.));
#126248=DIRECTION('ref_axis',(0.,1.,0.));
#126249=DIRECTION('',(0.,0.,-1.));
#126250=DIRECTION('center_axis',(0.,0.,-1.));
#126251=DIRECTION('ref_axis',(0.,1.,0.));
#126252=DIRECTION('',(0.,0.,-1.));
#126253=DIRECTION('center_axis',(0.,0.,1.));
#126254=DIRECTION('ref_axis',(1.,-1.06448650818115E-14,0.));
#126255=DIRECTION('',(0.,0.,1.));
#126256=DIRECTION('center_axis',(0.,0.,1.));
#126257=DIRECTION('ref_axis',(1.,-1.06448650818115E-14,0.));
#126258=DIRECTION('',(0.,0.,1.));
#126259=DIRECTION('center_axis',(0.,0.,1.));
#126260=DIRECTION('ref_axis',(1.,-1.06448650818115E-14,0.));
#126261=DIRECTION('',(0.,0.,1.));
#126262=DIRECTION('center_axis',(0.,0.,1.));
#126263=DIRECTION('ref_axis',(1.,-1.06448650818115E-14,0.));
#126264=DIRECTION('',(0.,0.,1.));
#126265=DIRECTION('center_axis',(0.,0.,1.));
#126266=DIRECTION('ref_axis',(1.,-1.06448650818115E-14,0.));
#126267=DIRECTION('',(0.,0.,1.));
#126268=DIRECTION('center_axis',(0.,0.,1.));
#126269=DIRECTION('ref_axis',(1.,-1.06448650818115E-14,0.));
#126270=DIRECTION('',(0.,0.,1.));
#126271=DIRECTION('center_axis',(0.,0.,1.));
#126272=DIRECTION('ref_axis',(1.,-1.06448650818115E-14,0.));
#126273=DIRECTION('',(0.,0.,1.));
#126274=DIRECTION('center_axis',(0.,0.,1.));
#126275=DIRECTION('ref_axis',(1.,-1.06448650818115E-14,0.));
#126276=DIRECTION('',(0.,0.,1.));
#126277=DIRECTION('center_axis',(0.,0.,1.));
#126278=DIRECTION('ref_axis',(1.,-1.06448650818115E-14,0.));
#126279=DIRECTION('',(0.,0.,1.));
#126280=DIRECTION('center_axis',(0.,0.,1.));
#126281=DIRECTION('ref_axis',(1.,-1.06448650818115E-14,0.));
#126282=DIRECTION('',(0.,0.,1.));
#126283=DIRECTION('center_axis',(0.,0.,1.));
#126284=DIRECTION('ref_axis',(1.,-1.06448650818115E-14,0.));
#126285=DIRECTION('',(0.,0.,1.));
#126286=DIRECTION('center_axis',(0.,0.,1.));
#126287=DIRECTION('ref_axis',(1.,-1.06448650818115E-14,0.));
#126288=DIRECTION('',(0.,0.,1.));
#126289=DIRECTION('center_axis',(0.,0.,1.));
#126290=DIRECTION('ref_axis',(1.,-1.06448650818115E-14,0.));
#126291=DIRECTION('',(0.,0.,1.));
#126292=DIRECTION('center_axis',(0.,0.,1.));
#126293=DIRECTION('ref_axis',(1.,-1.06448650818115E-14,0.));
#126294=DIRECTION('',(0.,0.,1.));
#126295=DIRECTION('center_axis',(0.,0.,1.));
#126296=DIRECTION('ref_axis',(1.,-1.06448650818115E-14,0.));
#126297=DIRECTION('',(0.,0.,1.));
#126298=DIRECTION('center_axis',(0.,0.,1.));
#126299=DIRECTION('ref_axis',(1.,-1.06448650818115E-14,0.));
#126300=DIRECTION('',(0.,0.,1.));
#126301=DIRECTION('center_axis',(0.,0.,1.));
#126302=DIRECTION('ref_axis',(1.,-1.06448650818115E-14,0.));
#126303=DIRECTION('',(0.,0.,1.));
#126304=DIRECTION('center_axis',(0.,0.,1.));
#126305=DIRECTION('ref_axis',(1.,-1.06448650818115E-14,0.));
#126306=DIRECTION('',(0.,0.,1.));
#126307=DIRECTION('center_axis',(0.,0.,1.));
#126308=DIRECTION('ref_axis',(1.,-1.06448650818115E-14,0.));
#126309=DIRECTION('',(0.,0.,1.));
#126310=DIRECTION('center_axis',(0.,0.,1.));
#126311=DIRECTION('ref_axis',(1.,-1.06448650818115E-14,0.));
#126312=DIRECTION('center_axis',(0.,0.,-1.));
#126313=DIRECTION('ref_axis',(0.,1.,0.));
#126314=DIRECTION('',(0.,0.,-1.));
#126315=DIRECTION('center_axis',(0.,0.,1.));
#126316=DIRECTION('ref_axis',(-1.,0.,0.));
#126317=DIRECTION('center_axis',(0.,0.,-1.));
#126318=DIRECTION('ref_axis',(0.,1.,0.));
#126319=DIRECTION('',(0.,0.,-1.));
#126320=DIRECTION('center_axis',(0.,0.,-1.));
#126321=DIRECTION('ref_axis',(0.,1.,0.));
#126322=DIRECTION('',(0.,0.,-1.));
#126323=DIRECTION('center_axis',(0.,0.,-1.));
#126324=DIRECTION('ref_axis',(0.,1.,0.));
#126325=DIRECTION('',(0.,0.,-1.));
#126326=DIRECTION('center_axis',(0.,0.,-1.));
#126327=DIRECTION('ref_axis',(0.,1.,0.));
#126328=DIRECTION('',(0.,0.,-1.));
#126329=DIRECTION('center_axis',(0.,0.,-1.));
#126330=DIRECTION('ref_axis',(0.,1.,0.));
#126331=DIRECTION('',(0.,0.,-1.));
#126332=DIRECTION('center_axis',(0.,0.,-1.));
#126333=DIRECTION('ref_axis',(0.,1.,0.));
#126334=DIRECTION('',(0.,0.,-1.));
#126335=DIRECTION('center_axis',(0.,0.,-1.));
#126336=DIRECTION('ref_axis',(0.,1.,0.));
#126337=DIRECTION('',(0.,0.,-1.));
#126338=DIRECTION('center_axis',(0.,0.,-1.));
#126339=DIRECTION('ref_axis',(0.,1.,0.));
#126340=DIRECTION('',(0.,0.,-1.));
#126341=DIRECTION('center_axis',(0.,0.,-1.));
#126342=DIRECTION('ref_axis',(0.,1.,0.));
#126343=DIRECTION('',(0.,0.,-1.));
#126344=DIRECTION('center_axis',(0.,0.,-1.));
#126345=DIRECTION('ref_axis',(0.,1.,0.));
#126346=DIRECTION('',(0.,0.,-1.));
#126347=DIRECTION('center_axis',(0.,0.,-1.));
#126348=DIRECTION('ref_axis',(0.,1.,0.));
#126349=DIRECTION('',(0.,0.,-1.));
#126350=DIRECTION('center_axis',(0.,0.,-1.));
#126351=DIRECTION('ref_axis',(0.,1.,0.));
#126352=DIRECTION('',(0.,0.,-1.));
#126353=DIRECTION('center_axis',(0.,0.,-1.));
#126354=DIRECTION('ref_axis',(0.,1.,0.));
#126355=DIRECTION('',(0.,0.,-1.));
#126356=DIRECTION('center_axis',(0.,0.,-1.));
#126357=DIRECTION('ref_axis',(0.,1.,0.));
#126358=DIRECTION('',(0.,0.,-1.));
#126359=DIRECTION('center_axis',(0.,0.,-1.));
#126360=DIRECTION('ref_axis',(0.,1.,0.));
#126361=DIRECTION('',(0.,0.,-1.));
#126362=DIRECTION('center_axis',(0.,0.,-1.));
#126363=DIRECTION('ref_axis',(0.,1.,0.));
#126364=DIRECTION('',(0.,0.,-1.));
#126365=DIRECTION('center_axis',(0.,0.,-1.));
#126366=DIRECTION('ref_axis',(0.,1.,0.));
#126367=DIRECTION('',(0.,0.,-1.));
#126368=DIRECTION('center_axis',(0.18797044408042,-0.201600124387681,0.961261932045101));
#126369=DIRECTION('ref_axis',(-0.567481399358022,-0.82110585529472,-0.0612375357390118));
#126370=DIRECTION('center_axis',(0.,0.,1.));
#126371=DIRECTION('ref_axis',(-3.72570277863391E-14,-1.,0.));
#126372=DIRECTION('',(0.,0.,1.));
#126373=DIRECTION('center_axis',(0.,0.,1.));
#126374=DIRECTION('ref_axis',(-3.72570277863391E-14,-1.,0.));
#126375=DIRECTION('',(0.,0.,1.));
#126376=DIRECTION('center_axis',(0.,0.,1.));
#126377=DIRECTION('ref_axis',(-3.72570277863391E-14,-1.,0.));
#126378=DIRECTION('',(0.,0.,1.));
#126379=DIRECTION('center_axis',(0.,0.,1.));
#126380=DIRECTION('ref_axis',(-3.72570277863391E-14,-1.,0.));
#126381=DIRECTION('',(0.,0.,1.));
#126382=DIRECTION('center_axis',(0.,0.,1.));
#126383=DIRECTION('ref_axis',(-3.72570277863391E-14,-1.,0.));
#126384=DIRECTION('',(0.,0.,1.));
#126385=DIRECTION('center_axis',(0.,0.,1.));
#126386=DIRECTION('ref_axis',(-3.72570277863391E-14,-1.,0.));
#126387=DIRECTION('',(0.,0.,1.));
#126388=DIRECTION('center_axis',(0.,0.,1.));
#126389=DIRECTION('ref_axis',(-3.72570277863391E-14,-1.,0.));
#126390=DIRECTION('',(0.,0.,1.));
#126391=DIRECTION('center_axis',(0.,0.,1.));
#126392=DIRECTION('ref_axis',(-3.72570277863391E-14,-1.,0.));
#126393=DIRECTION('',(0.,0.,1.));
#126394=DIRECTION('center_axis',(0.,0.,1.));
#126395=DIRECTION('ref_axis',(-3.72570277863391E-14,-1.,0.));
#126396=DIRECTION('',(0.,0.,1.));
#126397=DIRECTION('center_axis',(0.,0.,1.));
#126398=DIRECTION('ref_axis',(-3.72570277863391E-14,-1.,0.));
#126399=DIRECTION('',(0.,0.,1.));
#126400=DIRECTION('center_axis',(0.,0.,1.));
#126401=DIRECTION('ref_axis',(-3.72570277863391E-14,-1.,0.));
#126402=DIRECTION('',(0.,0.,1.));
#126403=DIRECTION('center_axis',(0.,0.,1.));
#126404=DIRECTION('ref_axis',(-3.72570277863391E-14,-1.,0.));
#126405=DIRECTION('',(0.,0.,1.));
#126406=DIRECTION('center_axis',(0.,0.,1.));
#126407=DIRECTION('ref_axis',(-3.72570277863391E-14,-1.,0.));
#126408=DIRECTION('',(0.,0.,1.));
#126409=DIRECTION('center_axis',(0.,0.,1.));
#126410=DIRECTION('ref_axis',(-3.72570277863391E-14,-1.,0.));
#126411=DIRECTION('',(0.,0.,1.));
#126412=DIRECTION('center_axis',(0.,0.,1.));
#126413=DIRECTION('ref_axis',(-3.72570277863391E-14,-1.,0.));
#126414=DIRECTION('',(0.,0.,1.));
#126415=DIRECTION('center_axis',(0.,0.,1.));
#126416=DIRECTION('ref_axis',(-3.72570277863391E-14,-1.,0.));
#126417=DIRECTION('',(0.,0.,1.));
#126418=DIRECTION('center_axis',(0.,0.,1.));
#126419=DIRECTION('ref_axis',(-3.72570277863391E-14,-1.,0.));
#126420=DIRECTION('',(0.,0.,1.));
#126421=DIRECTION('center_axis',(0.,0.,1.));
#126422=DIRECTION('ref_axis',(-3.72570277863391E-14,-1.,0.));
#126423=DIRECTION('',(0.,0.,1.));
#126424=DIRECTION('center_axis',(0.,0.,1.));
#126425=DIRECTION('ref_axis',(-3.72570277863391E-14,-1.,0.));
#126426=DIRECTION('',(0.,0.,1.));
#126427=DIRECTION('center_axis',(0.,0.,1.));
#126428=DIRECTION('ref_axis',(-3.72570277863391E-14,-1.,0.));
#126429=DIRECTION('center_axis',(0.,0.,-1.));
#126430=DIRECTION('ref_axis',(0.,1.,0.));
#126431=DIRECTION('',(0.,0.,-1.));
#126432=DIRECTION('center_axis',(0.,0.,-1.));
#126433=DIRECTION('ref_axis',(1.,0.,0.));
#126434=DIRECTION('center_axis',(0.,0.,-1.));
#126435=DIRECTION('ref_axis',(0.,1.,0.));
#126436=DIRECTION('',(0.,0.,-1.));
#126437=DIRECTION('center_axis',(0.,0.,-1.));
#126438=DIRECTION('ref_axis',(0.,1.,0.));
#126439=DIRECTION('',(0.,0.,-1.));
#126440=DIRECTION('center_axis',(0.,0.,-1.));
#126441=DIRECTION('ref_axis',(0.,1.,0.));
#126442=DIRECTION('',(0.,0.,-1.));
#126443=DIRECTION('center_axis',(0.,0.,-1.));
#126444=DIRECTION('ref_axis',(0.,1.,0.));
#126445=DIRECTION('',(0.,0.,-1.));
#126446=DIRECTION('center_axis',(0.,0.,-1.));
#126447=DIRECTION('ref_axis',(0.,1.,0.));
#126448=DIRECTION('',(0.,0.,-1.));
#126449=DIRECTION('center_axis',(0.,0.,-1.));
#126450=DIRECTION('ref_axis',(0.,1.,0.));
#126451=DIRECTION('',(0.,0.,-1.));
#126452=DIRECTION('center_axis',(0.,0.,-1.));
#126453=DIRECTION('ref_axis',(0.,1.,0.));
#126454=DIRECTION('',(0.,0.,-1.));
#126455=DIRECTION('center_axis',(0.,0.,-1.));
#126456=DIRECTION('ref_axis',(0.,1.,0.));
#126457=DIRECTION('',(0.,0.,-1.));
#126458=DIRECTION('center_axis',(0.,0.,-1.));
#126459=DIRECTION('ref_axis',(0.,1.,0.));
#126460=DIRECTION('',(0.,0.,-1.));
#126461=DIRECTION('center_axis',(0.,0.,-1.));
#126462=DIRECTION('ref_axis',(0.,1.,0.));
#126463=DIRECTION('',(0.,0.,-1.));
#126464=DIRECTION('center_axis',(0.,0.,-1.));
#126465=DIRECTION('ref_axis',(0.,1.,0.));
#126466=DIRECTION('',(0.,0.,-1.));
#126467=DIRECTION('center_axis',(0.,0.,-1.));
#126468=DIRECTION('ref_axis',(0.,1.,0.));
#126469=DIRECTION('',(0.,0.,-1.));
#126470=DIRECTION('center_axis',(0.,0.,-1.));
#126471=DIRECTION('ref_axis',(0.,1.,0.));
#126472=DIRECTION('',(0.,0.,-1.));
#126473=DIRECTION('center_axis',(0.,0.,-1.));
#126474=DIRECTION('ref_axis',(0.,1.,0.));
#126475=DIRECTION('',(0.,0.,-1.));
#126476=DIRECTION('center_axis',(0.,0.,-1.));
#126477=DIRECTION('ref_axis',(0.,1.,0.));
#126478=DIRECTION('',(0.,0.,-1.));
#126479=DIRECTION('center_axis',(0.,0.,-1.));
#126480=DIRECTION('ref_axis',(0.,1.,0.));
#126481=DIRECTION('',(0.,0.,-1.));
#126482=DIRECTION('center_axis',(0.,0.,-1.));
#126483=DIRECTION('ref_axis',(0.,1.,0.));
#126484=DIRECTION('',(0.,0.,-1.));
#126485=DIRECTION('center_axis',(0.,0.,-1.));
#126486=DIRECTION('ref_axis',(0.,1.,0.));
#126487=DIRECTION('',(0.,0.,-1.));
#126488=DIRECTION('center_axis',(0.,0.,1.));
#126489=DIRECTION('ref_axis',(-1.,-2.66121627045289E-15,0.));
#126490=DIRECTION('',(0.,0.,1.));
#126491=DIRECTION('center_axis',(0.,0.,1.));
#126492=DIRECTION('ref_axis',(-1.,-2.66121627045289E-15,0.));
#126493=DIRECTION('',(0.,0.,1.));
#126494=DIRECTION('center_axis',(0.,0.,1.));
#126495=DIRECTION('ref_axis',(-1.,-2.66121627045289E-15,0.));
#126496=DIRECTION('',(0.,0.,1.));
#126497=DIRECTION('center_axis',(0.,0.,1.));
#126498=DIRECTION('ref_axis',(-1.,-2.66121627045289E-15,0.));
#126499=DIRECTION('',(0.,0.,1.));
#126500=DIRECTION('center_axis',(0.,0.,1.));
#126501=DIRECTION('ref_axis',(-1.,-2.66121627045289E-15,0.));
#126502=DIRECTION('',(0.,0.,1.));
#126503=DIRECTION('center_axis',(0.,0.,1.));
#126504=DIRECTION('ref_axis',(-1.,-2.66121627045289E-15,0.));
#126505=DIRECTION('',(0.,0.,1.));
#126506=DIRECTION('center_axis',(0.,0.,1.));
#126507=DIRECTION('ref_axis',(-1.,-2.66121627045289E-15,0.));
#126508=DIRECTION('',(0.,0.,1.));
#126509=DIRECTION('center_axis',(0.,0.,1.));
#126510=DIRECTION('ref_axis',(-1.,-2.66121627045289E-15,0.));
#126511=DIRECTION('',(0.,0.,1.));
#126512=DIRECTION('center_axis',(0.,0.,1.));
#126513=DIRECTION('ref_axis',(-1.,-2.66121627045289E-15,0.));
#126514=DIRECTION('',(0.,0.,1.));
#126515=DIRECTION('center_axis',(0.,0.,1.));
#126516=DIRECTION('ref_axis',(-1.,-2.66121627045289E-15,0.));
#126517=DIRECTION('',(0.,0.,1.));
#126518=DIRECTION('center_axis',(0.,0.,1.));
#126519=DIRECTION('ref_axis',(-1.,-2.66121627045289E-15,0.));
#126520=DIRECTION('',(0.,0.,1.));
#126521=DIRECTION('center_axis',(0.,0.,1.));
#126522=DIRECTION('ref_axis',(-1.,-2.66121627045289E-15,0.));
#126523=DIRECTION('',(0.,0.,1.));
#126524=DIRECTION('center_axis',(0.,0.,1.));
#126525=DIRECTION('ref_axis',(-1.,-2.66121627045289E-15,0.));
#126526=DIRECTION('',(0.,0.,1.));
#126527=DIRECTION('center_axis',(0.,0.,1.));
#126528=DIRECTION('ref_axis',(-1.,-2.66121627045289E-15,0.));
#126529=DIRECTION('',(0.,0.,1.));
#126530=DIRECTION('center_axis',(0.,0.,1.));
#126531=DIRECTION('ref_axis',(-1.,-2.66121627045289E-15,0.));
#126532=DIRECTION('',(0.,0.,1.));
#126533=DIRECTION('center_axis',(0.,0.,1.));
#126534=DIRECTION('ref_axis',(-1.,-2.66121627045289E-15,0.));
#126535=DIRECTION('',(0.,0.,1.));
#126536=DIRECTION('center_axis',(0.,0.,1.));
#126537=DIRECTION('ref_axis',(-1.,-2.66121627045289E-15,0.));
#126538=DIRECTION('',(0.,0.,1.));
#126539=DIRECTION('center_axis',(0.,0.,1.));
#126540=DIRECTION('ref_axis',(-1.,-2.66121627045289E-15,0.));
#126541=DIRECTION('',(0.,0.,1.));
#126542=DIRECTION('center_axis',(0.,0.,1.));
#126543=DIRECTION('ref_axis',(-1.,-2.66121627045289E-15,0.));
#126544=DIRECTION('',(0.,0.,1.));
#126545=DIRECTION('center_axis',(0.,0.,1.));
#126546=DIRECTION('ref_axis',(-1.,-2.66121627045289E-15,0.));
#126547=DIRECTION('center_axis',(0.,0.,1.));
#126548=DIRECTION('ref_axis',(-1.59672976227174E-14,1.,0.));
#126549=DIRECTION('',(0.,0.,1.));
#126550=DIRECTION('center_axis',(0.,0.,1.));
#126551=DIRECTION('ref_axis',(-1.59672976227174E-14,1.,0.));
#126552=DIRECTION('',(0.,0.,1.));
#126553=DIRECTION('center_axis',(0.,0.,1.));
#126554=DIRECTION('ref_axis',(-1.59672976227174E-14,1.,0.));
#126555=DIRECTION('',(0.,0.,1.));
#126556=DIRECTION('center_axis',(0.,0.,1.));
#126557=DIRECTION('ref_axis',(-1.59672976227174E-14,1.,0.));
#126558=DIRECTION('',(0.,0.,1.));
#126559=DIRECTION('center_axis',(0.,0.,1.));
#126560=DIRECTION('ref_axis',(-1.59672976227174E-14,1.,0.));
#126561=DIRECTION('',(0.,0.,1.));
#126562=DIRECTION('center_axis',(0.,0.,1.));
#126563=DIRECTION('ref_axis',(-1.59672976227174E-14,1.,0.));
#126564=DIRECTION('',(0.,0.,1.));
#126565=DIRECTION('center_axis',(0.,0.,1.));
#126566=DIRECTION('ref_axis',(-1.59672976227174E-14,1.,0.));
#126567=DIRECTION('',(0.,0.,1.));
#126568=DIRECTION('center_axis',(0.,0.,1.));
#126569=DIRECTION('ref_axis',(-1.59672976227174E-14,1.,0.));
#126570=DIRECTION('',(0.,0.,1.));
#126571=DIRECTION('center_axis',(0.,0.,1.));
#126572=DIRECTION('ref_axis',(-1.59672976227174E-14,1.,0.));
#126573=DIRECTION('',(0.,0.,1.));
#126574=DIRECTION('center_axis',(0.,0.,1.));
#126575=DIRECTION('ref_axis',(-1.59672976227174E-14,1.,0.));
#126576=DIRECTION('',(0.,0.,1.));
#126577=DIRECTION('center_axis',(0.,0.,1.));
#126578=DIRECTION('ref_axis',(-1.59672976227174E-14,1.,0.));
#126579=DIRECTION('',(0.,0.,1.));
#126580=DIRECTION('center_axis',(0.,0.,1.));
#126581=DIRECTION('ref_axis',(-1.59672976227174E-14,1.,0.));
#126582=DIRECTION('',(0.,0.,1.));
#126583=DIRECTION('center_axis',(0.,0.,1.));
#126584=DIRECTION('ref_axis',(-1.59672976227174E-14,1.,0.));
#126585=DIRECTION('',(0.,0.,1.));
#126586=DIRECTION('center_axis',(0.,0.,1.));
#126587=DIRECTION('ref_axis',(-1.59672976227174E-14,1.,0.));
#126588=DIRECTION('',(0.,0.,1.));
#126589=DIRECTION('center_axis',(0.,0.,1.));
#126590=DIRECTION('ref_axis',(-1.59672976227174E-14,1.,0.));
#126591=DIRECTION('',(0.,0.,1.));
#126592=DIRECTION('center_axis',(0.,0.,1.));
#126593=DIRECTION('ref_axis',(-1.59672976227174E-14,1.,0.));
#126594=DIRECTION('',(0.,0.,1.));
#126595=DIRECTION('center_axis',(0.,0.,1.));
#126596=DIRECTION('ref_axis',(-1.59672976227174E-14,1.,0.));
#126597=DIRECTION('',(0.,0.,1.));
#126598=DIRECTION('center_axis',(0.,0.,1.));
#126599=DIRECTION('ref_axis',(-1.59672976227174E-14,1.,0.));
#126600=DIRECTION('',(0.,0.,1.));
#126601=DIRECTION('center_axis',(0.,0.,1.));
#126602=DIRECTION('ref_axis',(-1.59672976227174E-14,1.,0.));
#126603=DIRECTION('',(0.,0.,1.));
#126604=DIRECTION('center_axis',(0.,0.,1.));
#126605=DIRECTION('ref_axis',(-1.59672976227174E-14,1.,0.));
#126606=DIRECTION('center_axis',(0.,-1.,0.));
#126607=DIRECTION('ref_axis',(0.,0.,-1.));
#126608=DIRECTION('',(-1.,0.,0.));
#126609=DIRECTION('',(0.,0.,1.));
#126610=DIRECTION('',(-1.,0.,0.));
#126611=DIRECTION('',(1.23917670974841E-16,0.,1.));
#126612=DIRECTION('',(-1.,0.,0.));
#126613=DIRECTION('',(0.,0.,-1.));
#126614=DIRECTION('',(-1.,0.,0.));
#126615=DIRECTION('',(0.,0.,-1.));
#126616=DIRECTION('center_axis',(-1.,0.,0.));
#126617=DIRECTION('ref_axis',(0.,0.,1.));
#126618=DIRECTION('',(0.,0.,-1.));
#126619=DIRECTION('center_axis',(1.,0.,0.));
#126620=DIRECTION('ref_axis',(0.,0.,1.));
#126621=DIRECTION('',(0.,1.,0.));
#126622=DIRECTION('',(0.,1.,0.));
#126623=DIRECTION('center_axis',(1.,0.,0.));
#126624=DIRECTION('ref_axis',(0.,0.,1.));
#126625=DIRECTION('center_axis',(0.,1.,0.));
#126626=DIRECTION('ref_axis',(0.,0.,1.));
#126627=DIRECTION('',(1.,0.,0.));
#126628=DIRECTION('',(-1.,0.,0.));
#126629=DIRECTION('',(0.,0.,-1.));
#126630=DIRECTION('',(1.,0.,0.));
#126631=DIRECTION('center_axis',(1.,0.,0.));
#126632=DIRECTION('ref_axis',(0.,0.,-1.));
#126633=DIRECTION('',(0.,1.,0.));
#126634=DIRECTION('',(0.,0.,-1.));
#126635=DIRECTION('',(0.,-1.,0.));
#126636=DIRECTION('',(0.,0.,1.));
#126637=DIRECTION('center_axis',(1.,0.,-1.23917670974841E-16));
#126638=DIRECTION('ref_axis',(-1.23917670974841E-16,0.,-1.));
#126639=DIRECTION('',(-2.06949078009218E-16,-1.,0.));
#126640=DIRECTION('',(1.23917670974841E-16,0.,1.));
#126641=DIRECTION('',(0.,-1.,0.));
#126642=DIRECTION('center_axis',(-1.,0.,0.));
#126643=DIRECTION('ref_axis',(0.,0.,1.));
#126644=DIRECTION('',(0.,1.,0.));
#126645=DIRECTION('',(0.,-1.,0.));
#126646=DIRECTION('',(0.,0.,-1.));
#126647=DIRECTION('center_axis',(0.,1.,0.));
#126648=DIRECTION('ref_axis',(1.,0.,0.));
#126649=DIRECTION('',(-1.,0.,0.));
#126650=DIRECTION('',(-1.,0.,0.));
#126651=DIRECTION('center_axis',(0.,0.,-1.));
#126652=DIRECTION('ref_axis',(-1.,0.,0.));
#126653=DIRECTION('',(-1.,0.,0.));
#126654=DIRECTION('center_axis',(0.,0.,-1.));
#126655=DIRECTION('ref_axis',(0.,-1.,0.));
#126656=DIRECTION('',(-1.,0.,0.));
#126657=DIRECTION('',(0.,1.,0.));
#126658=DIRECTION('center_axis',(-5.2588194754836E-31,1.51575151553259E-16,
-1.));
#126659=DIRECTION('ref_axis',(-1.,-3.46944695195361E-15,-1.08106823316757E-45));
#126660=DIRECTION('',(0.,1.,0.));
#126661=DIRECTION('center_axis',(-1.57764584264508E-30,1.51575151553259E-16,
-1.));
#126662=DIRECTION('ref_axis',(1.,1.04083408558608E-14,2.98046123744179E-45));
#126663=DIRECTION('center_axis',(0.,0.,-1.));
#126664=DIRECTION('ref_axis',(0.,1.,0.));
#126665=DIRECTION('',(-0.38268343236509,0.923879532511287,1.43936534571762E-16));
#126666=DIRECTION('',(0.923879532511287,0.38268343236509,5.95203168551499E-17));
#126667=DIRECTION('center_axis',(5.37437186243472E-32,-1.25279059425027E-16,
1.));
#126668=DIRECTION('ref_axis',(1.77635683940025E-15,1.,1.25279059425027E-16));
#126669=DIRECTION('',(-0.923879532511287,-0.38268343236509,-5.95203168551499E-17));
#126670=DIRECTION('',(-0.38268343236509,0.923879532511287,1.43936534571762E-16));
#126671=DIRECTION('center_axis',(1.93192743997308E-15,8.00230547157578E-16,
1.));
#126672=DIRECTION('ref_axis',(0.92387953251129,0.382683432365083,-2.09110319255771E-15));
#126673=DIRECTION('center_axis',(0.,0.,-1.));
#126674=DIRECTION('ref_axis',(0.,-1.,0.));
#126675=DIRECTION('center_axis',(0.,0.,-1.));
#126676=DIRECTION('ref_axis',(-1.,0.,0.));
#126677=DIRECTION('center_axis',(0.,0.,-1.));
#126678=DIRECTION('ref_axis',(-1.,0.,0.));
#126679=DIRECTION('center_axis',(0.,0.,1.));
#126680=DIRECTION('ref_axis',(0.,-1.,0.));
#126681=DIRECTION('',(0.,0.,1.));
#126682=DIRECTION('center_axis',(0.,0.,-1.));
#126683=DIRECTION('ref_axis',(0.,1.,0.));
#126684=DIRECTION('center_axis',(0.,0.,1.));
#126685=DIRECTION('ref_axis',(0.,-1.,0.));
#126686=DIRECTION('',(0.,0.,-1.));
#126687=DIRECTION('center_axis',(0.,0.,-1.));
#126688=DIRECTION('ref_axis',(-1.,0.,0.));
#126689=DIRECTION('center_axis',(-1.51575151553259E-16,1.51575151553257E-16,
-1.));
#126690=DIRECTION('ref_axis',(-1.,-7.79357634404829E-50,1.51575151553259E-16));
#126691=DIRECTION('center_axis',(-1.51575151553257E-16,-1.75293982516118E-30,
-1.));
#126692=DIRECTION('ref_axis',(-1.15648231731787E-14,1.,2.10194769648723E-45));
#126693=DIRECTION('center_axis',(-1.51575151553257E-16,-1.40235186012895E-30,
-1.));
#126694=DIRECTION('ref_axis',(-9.25185853854297E-15,1.,-3.50324616081204E-46));
#126695=DIRECTION('center_axis',(1.57764584264508E-30,-1.51575151553259E-16,
1.));
#126696=DIRECTION('ref_axis',(-1.,-1.04083408558608E-14,-2.98046123744179E-45));
#126697=DIRECTION('',(1.57764584264508E-30,-1.51575151553259E-16,1.));
#126698=DIRECTION('center_axis',(-1.57764584264508E-30,1.51575151553259E-16,
-1.));
#126699=DIRECTION('ref_axis',(1.,1.04083408558608E-14,2.98046123744179E-45));
#126700=DIRECTION('center_axis',(1.57764584264509E-30,-1.51575151553259E-16,
1.));
#126701=DIRECTION('ref_axis',(-1.,-1.04083408558608E-14,1.09360074820117E-47));
#126702=DIRECTION('',(-1.57764584264509E-30,1.51575151553259E-16,-1.));
#126703=DIRECTION('center_axis',(0.,0.,-1.));
#126704=DIRECTION('ref_axis',(-1.,0.,0.));
#126705=DIRECTION('center_axis',(1.51575151553259E-16,1.51575151553259E-16,
-1.));
#126706=DIRECTION('ref_axis',(-1.,-2.17577274266937E-49,-1.51575151553259E-16));
#126707=DIRECTION('center_axis',(1.51575151553259E-16,7.01175930064484E-31,
-1.));
#126708=DIRECTION('ref_axis',(4.62592926927148E-15,-1.,1.75162308040602E-46));
#126709=DIRECTION('center_axis',(1.51575151553259E-16,7.01175930064484E-31,
-1.));
#126710=DIRECTION('ref_axis',(4.62592926927148E-15,-1.,8.75811540203011E-47));
#126711=DIRECTION('center_axis',(5.2588194754836E-31,-1.51575151553259E-16,
1.));
#126712=DIRECTION('ref_axis',(1.,3.46944695195361E-15,1.08106823316757E-45));
#126713=DIRECTION('',(5.2588194754836E-31,-1.51575151553259E-16,1.));
#126714=DIRECTION('center_axis',(-5.2588194754836E-31,1.51575151553259E-16,
-1.));
#126715=DIRECTION('ref_axis',(-1.,-3.46944695195361E-15,-1.08106823316757E-45));
#126716=DIRECTION('center_axis',(5.25881947548361E-31,-1.51575151553259E-16,
1.));
#126717=DIRECTION('ref_axis',(1.,3.46944695195362E-15,6.8773879687219E-46));
#126718=DIRECTION('',(-5.25881947548361E-31,1.51575151553259E-16,-1.));
#126719=DIRECTION('center_axis',(0.,0.,-1.));
#126720=DIRECTION('ref_axis',(-1.,0.,0.));
#126721=DIRECTION('center_axis',(0.,3.03150303106518E-16,-1.));
#126722=DIRECTION('ref_axis',(-1.,0.,0.));
#126723=DIRECTION('center_axis',(0.,3.03150303106518E-16,-1.));
#126724=DIRECTION('ref_axis',(1.,0.,0.));
#126725=DIRECTION('center_axis',(0.,3.03150303106518E-16,-1.));
#126726=DIRECTION('ref_axis',(1.,0.,0.));
#126727=DIRECTION('center_axis',(0.,0.,1.));
#126728=DIRECTION('ref_axis',(0.,1.,0.));
#126729=DIRECTION('',(0.,0.,1.));
#126730=DIRECTION('center_axis',(0.,0.,-1.));
#126731=DIRECTION('ref_axis',(0.,-1.,0.));
#126732=DIRECTION('center_axis',(0.,0.,1.));
#126733=DIRECTION('ref_axis',(0.,1.,0.));
#126734=DIRECTION('center_axis',(0.,0.,-1.));
#126735=DIRECTION('ref_axis',(0.,-1.,0.));
#126736=DIRECTION('',(0.,0.,-1.));
#126737=DIRECTION('center_axis',(0.,0.,-1.));
#126738=DIRECTION('ref_axis',(0.,-1.,0.));
#126739=DIRECTION('center_axis',(0.,0.,-1.));
#126740=DIRECTION('ref_axis',(-1.,0.,0.));
#126741=DIRECTION('center_axis',(-0.868162779195992,-0.359604797490499,
-0.342020143325665));
#126742=DIRECTION('ref_axis',(0.315985410125154,0.130885442385879,-0.939692620785909));
#126743=DIRECTION('center_axis',(-0.868162779195992,-0.359604797490498,
-0.342020143325665));
#126744=DIRECTION('ref_axis',(0.38268343236509,-0.923879532511287,1.23981593187411E-17));
#126745=DIRECTION('center_axis',(-0.868162779195992,-0.359604797490498,
-0.342020143325665));
#126746=DIRECTION('ref_axis',(0.38268343236509,-0.923879532511287,1.23981593187411E-17));
#126747=DIRECTION('center_axis',(0.868162779195992,0.359604797490499,0.342020143325665));
#126748=DIRECTION('ref_axis',(0.38268343236509,-0.923879532511287,1.71567912920634E-16));
#126749=DIRECTION('center_axis',(-0.868162779195992,-0.359604797490499,
-0.342020143325665));
#126750=DIRECTION('ref_axis',(0.382683432365091,-0.923879532511286,0.));
#126751=DIRECTION('center_axis',(-0.868162779195992,-0.359604797490499,
-0.342020143325665));
#126752=DIRECTION('ref_axis',(0.382683432365091,-0.923879532511286,-1.45911995829617E-16));
#126753=DIRECTION('center_axis',(0.315985410125159,0.130885442385866,-0.93969262078591));
#126754=DIRECTION('ref_axis',(-0.38268343236509,0.923879532511287,0.));
#126755=DIRECTION('center_axis',(0.868162779195992,0.359604797490499,0.342020143325665));
#126756=DIRECTION('ref_axis',(0.382683432365091,-0.923879532511287,-1.04982926230618E-18));
#126757=DIRECTION('center_axis',(0.868162779195992,0.359604797490499,0.342020143325665));
#126758=DIRECTION('ref_axis',(0.382683432365091,-0.923879532511287,-1.04982926230618E-18));
#126759=DIRECTION('center_axis',(-0.868162779195992,-0.359604797490499,
-0.342020143325665));
#126760=DIRECTION('ref_axis',(0.382683432365091,-0.923879532511286,0.));
#126761=DIRECTION('center_axis',(-0.868162779195992,-0.359604797490499,
-0.342020143325665));
#126762=DIRECTION('ref_axis',(-0.382683432365091,0.923879532511286,1.1958072337233E-16));
#126763=DIRECTION('center_axis',(-0.868162779195992,-0.359604797490499,
-0.342020143325665));
#126764=DIRECTION('ref_axis',(-0.382683432365091,0.923879532511286,1.1958072337233E-16));
#126765=DIRECTION('center_axis',(0.315985410125158,0.130885442385866,-0.93969262078591));
#126766=DIRECTION('ref_axis',(-0.382683432365091,0.923879532511286,0.));
#126767=DIRECTION('center_axis',(0.868162779195992,0.359604797490499,0.342020143325665));
#126768=DIRECTION('ref_axis',(0.382683432365091,-0.923879532511286,-1.88969662411402E-16));
#126769=DIRECTION('center_axis',(0.868162779195992,0.359604797490499,0.342020143325665));
#126770=DIRECTION('ref_axis',(0.382683432365091,-0.923879532511286,-1.88969662411402E-16));
#126771=DIRECTION('center_axis',(-0.489406279098172,0.734660423998332,0.469846310392955));
#126772=DIRECTION('ref_axis',(0.692544317692113,6.99668119051868E-17,0.721375330900888));
#126773=DIRECTION('',(-0.868162779195992,-0.359604797490499,-0.342020143325665));
#126774=DIRECTION('',(-0.868162779195992,-0.359604797490499,-0.342020143325665));
#126775=DIRECTION('center_axis',(-0.315985410125159,-0.130885442385866,
0.93969262078591));
#126776=DIRECTION('ref_axis',(-0.382683432365091,0.923879532511286,-9.25792640816383E-18));
#126777=DIRECTION('',(-0.868162779195992,-0.359604797490499,-0.342020143325665));
#126778=DIRECTION('center_axis',(0.173420868973012,-0.865545866384198,0.469846310392956));
#126779=DIRECTION('ref_axis',(-0.980512713657042,-0.196455639666833,-1.27106818020157E-17));
#126780=DIRECTION('',(-0.868162779195992,-0.359604797490499,-0.342020143325665));
#126781=DIRECTION('center_axis',(0.489406279098172,-0.734660423998332,-0.469846310392956));
#126782=DIRECTION('ref_axis',(2.69783883395398E-17,0.538780036928174,-0.842446480085041));
#126783=DIRECTION('',(-0.868162779195992,-0.359604797490499,-0.342020143325665));
#126784=DIRECTION('center_axis',(0.315985410125159,0.130885442385866,-0.93969262078591));
#126785=DIRECTION('ref_axis',(4.33389766930712E-18,-0.990438688967689,-0.137953627701358));
#126786=DIRECTION('',(-0.868162779195992,-0.359604797490499,-0.342020143325665));
#126787=DIRECTION('center_axis',(-0.173420868973013,0.865545866384198,-0.469846310392955));
#126788=DIRECTION('ref_axis',(-0.938135943967436,-1.39985742631978E-17,
0.346267166558321));
#126789=DIRECTION('center_axis',(-0.868162779195992,-0.359604797490499,
-0.342020143325665));
#126790=DIRECTION('ref_axis',(0.38268343236509,-0.923879532511287,1.84142372121514E-16));
#126791=DIRECTION('',(-0.765494963633587,0.620300746446016,-0.171010071662833));
#126792=DIRECTION('center_axis',(-0.868162779195992,-0.359604797490499,
-0.342020143325665));
#126793=DIRECTION('ref_axis',(0.38268343236509,-0.923879532511287,4.70737048728512E-17));
#126794=DIRECTION('center_axis',(-0.868162779195992,-0.359604797490499,
-0.342020143325665));
#126795=DIRECTION('ref_axis',(0.38268343236509,-0.923879532511287,4.70737048728512E-17));
#126796=DIRECTION('center_axis',(-0.868162779195992,-0.359604797490499,
-0.342020143325665));
#126797=DIRECTION('ref_axis',(0.38268343236509,-0.923879532511287,4.70737048728512E-17));
#126798=DIRECTION('center_axis',(-0.868162779195992,-0.359604797490499,
-0.342020143325665));
#126799=DIRECTION('ref_axis',(0.38268343236509,-0.923879532511287,4.70737048728512E-17));
#126800=DIRECTION('center_axis',(-0.868162779195992,-0.359604797490499,
-0.342020143325665));
#126801=DIRECTION('ref_axis',(0.38268343236509,-0.923879532511287,4.70737048728512E-17));
#126802=DIRECTION('center_axis',(-0.868162779195992,-0.359604797490499,
-0.342020143325665));
#126803=DIRECTION('ref_axis',(0.38268343236509,-0.923879532511287,4.70737048728512E-17));
#126804=DIRECTION('center_axis',(-0.868162779195992,-0.359604797490499,
-0.342020143325665));
#126805=DIRECTION('ref_axis',(0.38268343236509,-0.923879532511287,4.70737048728512E-17));
#126806=DIRECTION('center_axis',(-0.868162779195992,-0.359604797490499,
-0.342020143325665));
#126807=DIRECTION('ref_axis',(0.38268343236509,-0.923879532511287,4.70737048728512E-17));
#126808=DIRECTION('center_axis',(-0.868162779195992,-0.359604797490499,
-0.342020143325665));
#126809=DIRECTION('ref_axis',(0.38268343236509,-0.923879532511287,4.70737048728512E-17));
#126810=DIRECTION('center_axis',(-0.868162779195992,-0.359604797490499,
-0.342020143325665));
#126811=DIRECTION('ref_axis',(0.38268343236509,-0.923879532511287,4.70737048728512E-17));
#126812=DIRECTION('center_axis',(-0.868162779195992,-0.359604797490499,
-0.342020143325665));
#126813=DIRECTION('ref_axis',(0.38268343236509,-0.923879532511287,4.70737048728512E-17));
#126814=DIRECTION('center_axis',(-0.868162779195992,-0.359604797490499,
-0.342020143325665));
#126815=DIRECTION('ref_axis',(0.38268343236509,-0.923879532511287,4.70737048728512E-17));
#126816=DIRECTION('center_axis',(0.868162779195992,0.3596047974905,0.342020143325665));
#126817=DIRECTION('ref_axis',(-0.382683432365091,0.923879532511286,1.50485916215286E-17));
#126818=DIRECTION('',(-0.884481838416343,0.399002491585443,-0.241844762647972));
#126819=DIRECTION('center_axis',(-0.868162779195992,-0.359604797490499,
-0.342020143325665));
#126820=DIRECTION('ref_axis',(-0.38268343236509,0.923879532511287,-1.64291196909507E-17));
#126821=DIRECTION('center_axis',(0.868162779195992,0.359604797490499,0.342020143325665));
#126822=DIRECTION('ref_axis',(-0.382683432365091,0.923879532511286,1.45911995829617E-16));
#126823=DIRECTION('',(-0.868162779195992,-0.359604797490499,-0.342020143325665));
#126824=DIRECTION('center_axis',(0.207767103126159,0.124142226786913,-0.970268796976874));
#126825=DIRECTION('ref_axis',(0.558629433047175,-0.829307248729054,0.0135145750520801));
#126826=DIRECTION('center_axis',(-0.382637984861907,0.923898340295368,-0.000171290056814656));
#126827=DIRECTION('ref_axis',(0.892345806659134,0.369618341309029,0.259039076407058));
#126828=DIRECTION('center_axis',(0.803015285854003,0.544766314634934,0.241652877334176));
#126829=DIRECTION('ref_axis',(-0.561404803271713,0.827541326377994,1.44349153113304E-16));
#126830=DIRECTION('center_axis',(0.0669619156029896,-0.957600006962959,
0.280211221265884));
#126831=DIRECTION('ref_axis',(4.52485696084786E-18,-0.280841561131646,-0.959754144320898));
#126832=DIRECTION('center_axis',(0.0693609655093104,-0.991908018991874,
0.106336909505741));
#126833=DIRECTION('ref_axis',(3.26002624601434E-19,-0.106593626600315,-0.994302669597237));
#126834=DIRECTION('center_axis',(0.997564050259817,0.0697564737442329,5.27888523360413E-13));
#126835=DIRECTION('ref_axis',(0.0681007776048493,-0.973886492346363,-0.216581125943402));
#126836=DIRECTION('center_axis',(-0.997974582307943,-0.063160693020796,
0.00758023247798644));
#126837=DIRECTION('ref_axis',(0.0591504890733341,-0.96518844253331,-0.254779296730542));
#126838=DIRECTION('center_axis',(0.424778659972963,-0.88724503879059,0.179886995564043));
#126839=DIRECTION('ref_axis',(0.901958432317943,0.431822864575925,-3.94566691152879E-17));
#126840=DIRECTION('center_axis',(0.240037971429266,-0.880321972893445,-0.409163776882944));
#126841=DIRECTION('ref_axis',(-3.13002221110141E-17,0.421486569103856,-0.906834644279243));
#126842=DIRECTION('center_axis',(-0.877516698994613,0.406924946271124,0.253725306360719));
#126843=DIRECTION('ref_axis',(-0.420691523302729,-0.907203749011891,-9.67787277356546E-18));
#126844=DIRECTION('center_axis',(-0.489478788704461,0.506750770244223,0.709657785320009));
#126845=DIRECTION('ref_axis',(4.89383052204965E-17,-0.813813546305325,0.581126072251065));
#126846=DIRECTION('',(-0.489348180803406,0.50550620705824,0.710634809568169));
#126847=DIRECTION('',(-0.0114108069061362,0.703450190767272,-0.710652955102024));
#126848=DIRECTION('center_axis',(-0.0122131352712882,0.704440676751092,
-0.709657785320015));
#126849=DIRECTION('ref_axis',(1.46094887112304E-18,0.709710717758151,0.704493220051982));
#126850=DIRECTION('center_axis',(0.332758619521767,0.908237397405967,-0.253725306359464));
#126851=DIRECTION('ref_axis',(-0.938963751759069,0.344016093929534,5.28665875370305E-17));
#126852=DIRECTION('',(-0.796920821694072,-0.55369873650563,-0.241526216263399));
#126853=DIRECTION('center_axis',(0.315985410124948,0.130885442386372,-0.93969262078591));
#126854=DIRECTION('ref_axis',(-0.947846471025676,1.41403886388541E-17,-0.31872726172101));
#126855=DIRECTION('center_axis',(0.868162779110503,0.359604797646558,0.342020143378583));
#126856=DIRECTION('ref_axis',(-0.305572312858413,-0.155701183571717,0.93935227846039));
#126857=DIRECTION('center_axis',(0.31598541012516,0.130885442385866,-0.939692620785909));
#126858=DIRECTION('ref_axis',(-0.947846471025611,1.76887230820116E-17,-0.318727261721202));
#126859=DIRECTION('center_axis',(0.315985410125156,0.130885442385873,-0.93969262078591));
#126860=DIRECTION('ref_axis',(-0.947846471025612,-3.00392539194327E-17,
-0.318727261721199));
#126861=DIRECTION('',(-0.315985410125159,-0.130885442385866,0.93969262078591));
#126862=DIRECTION('',(0.315985410125159,0.130885442385866,-0.93969262078591));
#126863=DIRECTION('center_axis',(0.315985410125156,0.130885442385873,-0.93969262078591));
#126864=DIRECTION('ref_axis',(-0.947846471025612,-3.00392539194327E-17,
-0.318727261721199));
#126865=DIRECTION('center_axis',(0.315985410126442,0.130885442386398,-0.939692620785404));
#126866=DIRECTION('ref_axis',(-0.947846471025169,5.20709087205665E-17,-0.318727261722518));
#126867=DIRECTION('center_axis',(0.868162779214872,0.359604797427702,0.342020143343766));
#126868=DIRECTION('ref_axis',(-0.32168655692517,-0.117021230958172,0.939587031944707));
#126869=DIRECTION('center_axis',(-0.315985410125157,-0.130885442385866,
0.93969262078591));
#126870=DIRECTION('ref_axis',(0.947846471025612,-2.96658686303126E-17,0.318727261721199));
#126871=DIRECTION('center_axis',(0.315985410125168,0.130885442385872,-0.939692620785906));
#126872=DIRECTION('ref_axis',(-0.947846471025608,-1.83411763673086E-17,
-0.318727261721211));
#126873=DIRECTION('',(-0.315985410125159,-0.130885442385866,0.93969262078591));
#126874=DIRECTION('',(0.315985410125159,0.130885442385866,-0.93969262078591));
#126875=DIRECTION('center_axis',(-0.483641379709625,0.875232579647714,0.00767771813624582));
#126876=DIRECTION('ref_axis',(-0.583254653729399,-0.328814087806622,0.742761943399699));
#126877=DIRECTION('center_axis',(0.382683432364578,-0.923879532511499,2.29641113224045E-12));
#126878=DIRECTION('ref_axis',(-0.336984534075557,-0.139583564321541,0.931105714924559));
#126879=DIRECTION('center_axis',(0.897231051697274,0.371645270195287,0.238445450809354));
#126880=DIRECTION('ref_axis',(-0.38268343236509,0.923879532511287,-5.599049694823E-17));
#126881=DIRECTION('center_axis',(0.89730838161834,0.371677301297369,0.238104288028965));
#126882=DIRECTION('ref_axis',(-0.38268343236509,0.923879532511287,1.43867310709335E-17));
#126883=DIRECTION('center_axis',(-0.333396134868013,0.924692779654905,-0.183821327677601));
#126884=DIRECTION('ref_axis',(-0.288398744889462,0.0856014296512129,0.953676338800461));
#126885=DIRECTION('center_axis',(0.382683432406618,-0.923879532494085,-1.8240588452439E-10));
#126886=DIRECTION('ref_axis',(-0.220298531052334,-0.0912506395364631,0.97115491967058));
#126887=DIRECTION('center_axis',(0.382683432365091,-0.923879532511286,0.));
#126888=DIRECTION('ref_axis',(-0.923879532511287,-0.382683432365088,0.));
#126889=DIRECTION('center_axis',(0.,0.,1.));
#126890=DIRECTION('ref_axis',(1.,0.,0.));
#126891=DIRECTION('center_axis',(0.207956138914421,-0.978138151943684,-1.20768627396809E-16));
#126892=DIRECTION('ref_axis',(-0.978138151943684,-0.207956138914421,-6.93889390390724E-15));
#126893=DIRECTION('center_axis',(0.,0.,-1.));
#126894=DIRECTION('ref_axis',(0.,1.,0.));
#126895=DIRECTION('center_axis',(0.,0.,1.));
#126896=DIRECTION('ref_axis',(1.,0.,0.));
#126897=DIRECTION('',(0.,-1.23467863058847E-16,1.));
#126898=DIRECTION('',(-5.72527083528863E-17,2.61688128046977E-16,-1.));
#126899=DIRECTION('center_axis',(-0.923879532511287,-0.38268343236509,7.73840192406943E-15));
#126900=DIRECTION('ref_axis',(0.38268343236509,-0.923879532511287,1.1683584407418E-30));
#126901=DIRECTION('center_axis',(-0.923879532511287,-0.38268343236509,-5.95203168551499E-17));
#126902=DIRECTION('ref_axis',(0.38268343236509,-0.923879532511287,-2.30223036877952E-33));
#126903=DIRECTION('',(0.923879532511287,0.38268343236509,5.95203168551499E-17));
#126904=DIRECTION('center_axis',(-0.382683432316632,0.923879532531359,-2.13765135084401E-10));
#126905=DIRECTION('ref_axis',(-0.219984261016821,-0.0911204641832574,0.971238377491289));
#126906=DIRECTION('center_axis',(0.418112262482855,-0.889598787804806,-0.183837245131902));
#126907=DIRECTION('ref_axis',(-0.143722924471232,-0.264610116560947,0.953585448292411));
#126908=DIRECTION('center_axis',(0.897308381618341,0.371677301297376,0.238104288028952));
#126909=DIRECTION('ref_axis',(-0.382683432365096,0.923879532511284,6.65294430386245E-16));
#126910=DIRECTION('center_axis',(0.382683432365091,-0.923879532511286,0.));
#126911=DIRECTION('ref_axis',(-0.923879532511286,-0.382683432365091,0.));
#126912=DIRECTION('center_axis',(-0.5446009241609,0.838695316192414,1.03551918447742E-16));
#126913=DIRECTION('ref_axis',(-0.838695316192414,-0.5446009241609,4.64565385920393E-32));
#126914=DIRECTION('center_axis',(3.84325181751198E-15,-6.93889390390722E-15,
1.));
#126915=DIRECTION('ref_axis',(5.60519385729927E-45,-1.,-6.93889390390722E-15));
#126916=DIRECTION('center_axis',(0.,0.,-1.));
#126917=DIRECTION('ref_axis',(0.,1.,0.));
#126918=DIRECTION('center_axis',(0.,0.,1.));
#126919=DIRECTION('ref_axis',(1.,0.,0.));
#126920=DIRECTION('',(5.72527083528863E-17,-2.61688128046977E-16,1.));
#126921=DIRECTION('',(0.,1.23467863058847E-16,-1.));
#126922=DIRECTION('center_axis',(-0.923879532511287,-0.38268343236509,0.));
#126923=DIRECTION('ref_axis',(0.38268343236509,-0.923879532511287,0.));
#126924=DIRECTION('center_axis',(0.923879532511287,0.38268343236509,5.95203168551498E-17));
#126925=DIRECTION('ref_axis',(-0.38268343236509,0.923879532511287,-1.86999513136017E-32));
#126926=DIRECTION('',(-0.923879532511287,-0.38268343236509,-5.95203168551499E-17));
#126927=DIRECTION('center_axis',(-0.38268343236509,0.923879532511287,-2.16840434497101E-16));
#126928=DIRECTION('ref_axis',(-5.66631362003227E-16,-2.40839253845808E-32,
1.));
#126929=DIRECTION('center_axis',(0.868162779195992,0.359604797490499,0.342020143325665));
#126930=DIRECTION('ref_axis',(-0.382683432365091,0.923879532511286,9.04008445983594E-17));
#126931=DIRECTION('center_axis',(-0.868162779195992,-0.359604797490499,
-0.342020143325665));
#126932=DIRECTION('ref_axis',(0.38268343236509,-0.923879532511287,-1.25544037310089E-16));
#126933=DIRECTION('center_axis',(-0.38268343236509,0.923879532511287,2.63677968348474E-16));
#126934=DIRECTION('ref_axis',(6.89023736195924E-16,-2.65450765404649E-32,
1.));
#126935=DIRECTION('center_axis',(-0.38268343236509,0.923879532511287,2.63677968348474E-16));
#126936=DIRECTION('ref_axis',(6.89023736195924E-16,-2.65450765404649E-32,
1.));
#126937=DIRECTION('center_axis',(0.868162779195992,0.359604797490499,0.342020143325665));
#126938=DIRECTION('ref_axis',(2.46876234589468E-17,0.689168323296269,-0.724601284959535));
#126939=DIRECTION('center_axis',(0.,0.,-1.));
#126940=DIRECTION('ref_axis',(0.,1.,0.));
#126941=DIRECTION('',(0.,1.23467863058847E-16,-1.));
#126942=DIRECTION('center_axis',(1.42788400384581E-31,1.65132260162873E-46,
-1.));
#126943=DIRECTION('ref_axis',(-1.15648231731787E-15,1.,-3.88938454866321E-62));
#126944=DIRECTION('',(0.,-1.23467863058847E-16,1.));
#126945=DIRECTION('center_axis',(0.,0.,-1.));
#126946=DIRECTION('ref_axis',(0.,1.,0.));
#126947=DIRECTION('',(0.,1.23467863058847E-16,-1.));
#126948=DIRECTION('center_axis',(0.,0.,-1.));
#126949=DIRECTION('ref_axis',(0.,1.,0.));
#126950=DIRECTION('',(0.,-1.23467863058847E-16,1.));
#126951=DIRECTION('center_axis',(0.,0.,-1.));
#126952=DIRECTION('ref_axis',(0.,1.,0.));
#126953=DIRECTION('',(0.,1.23467863058847E-16,-1.));
#126954=DIRECTION('center_axis',(4.28365201153745E-31,1.48619034146585E-45,
-1.));
#126955=DIRECTION('ref_axis',(-3.46944695195361E-15,1.,-6.22301527786114E-61));
#126956=DIRECTION('',(0.,-1.23467863058847E-16,1.));
#126957=DIRECTION('center_axis',(0.901958432317944,0.431822864575923,-2.31577870403057E-15));
#126958=DIRECTION('ref_axis',(-0.431822864575923,0.901958432317944,-1.23890881716737E-31));
#126959=DIRECTION('center_axis',(0.992770886529525,0.0694213030853436,0.0979114372140112));
#126960=DIRECTION('ref_axis',(0.0981482265735623,2.06880671420837E-18,-0.995171807086829));
#126961=DIRECTION('center_axis',(0.,0.,-1.));
#126962=DIRECTION('ref_axis',(0.,1.,0.));
#126963=DIRECTION('',(0.,1.23467863058847E-16,-1.));
#126964=DIRECTION('center_axis',(0.,0.,1.));
#126965=DIRECTION('ref_axis',(0.,1.,0.));
#126966=DIRECTION('',(0.,-1.23467863058847E-16,1.));
#126967=DIRECTION('center_axis',(0.,0.,-1.));
#126968=DIRECTION('ref_axis',(0.,1.,0.));
#126969=DIRECTION('',(0.,1.23467863058847E-16,-1.));
#126970=DIRECTION('center_axis',(0.,0.,1.));
#126971=DIRECTION('ref_axis',(0.,1.,0.));
#126972=DIRECTION('',(0.,-1.23467863058847E-16,1.));
#126973=DIRECTION('center_axis',(-0.0697564737441281,0.997564050259824,
1.23167101549909E-16));
#126974=DIRECTION('ref_axis',(1.76567270303392E-15,-9.8268693212801E-33,
1.));
#126975=DIRECTION('',(0.997564050259824,0.0697564737441281,8.61268274770809E-18));
#126976=DIRECTION('center_axis',(0.98660590693345,0.0689902057164932,0.147814532165213));
#126977=DIRECTION('ref_axis',(0.148167565509255,-4.52088703569399E-18,-0.988962270529599));
#126978=DIRECTION('center_axis',(0.747470084264675,0.664295471254592,-6.06224791631038E-16));
#126979=DIRECTION('ref_axis',(-0.664295471254592,0.747470084264675,9.59955536918487E-32));
#126980=DIRECTION('center_axis',(0.,0.,-1.));
#126981=DIRECTION('ref_axis',(0.,1.,0.));
#126982=DIRECTION('center_axis',(1.10148875902005E-31,1.02798428206033E-16,
-1.));
#126983=DIRECTION('ref_axis',(-5.32907051820075E-15,1.,1.02798428206033E-16));
#126984=DIRECTION('center_axis',(0.,-1.02798428206033E-16,1.));
#126985=DIRECTION('ref_axis',(0.,-1.,-1.02798428206033E-16));
#126986=DIRECTION('center_axis',(0.664295471254592,0.747470084264675,-2.95837698315952E-15));
#126987=DIRECTION('ref_axis',(-0.747470084264675,0.664295471254592,-5.32960101812494E-31));
#126988=DIRECTION('center_axis',(0.0689902057164909,0.986605906933449,-0.14781453216522));
#126989=DIRECTION('ref_axis',(4.37731061835132E-18,-0.148167565509262,-0.988962270529598));
#126990=DIRECTION('center_axis',(-0.997564050259824,0.0697564737441242,
8.61268274770762E-18));
#126991=DIRECTION('ref_axis',(8.63371404118299E-18,-2.27387344266631E-35,
1.));
#126992=DIRECTION('',(0.0697564737441243,0.997564050259824,1.23167101549909E-16));
#126993=DIRECTION('center_axis',(0.0694213030853413,0.992770886529525,-0.0979114372140151));
#126994=DIRECTION('ref_axis',(-3.30612675079287E-17,-0.0981482265735662,
-0.995171807086829));
#126995=DIRECTION('center_axis',(0.431822864575922,0.901958432317945,1.52768647491022E-15));
#126996=DIRECTION('ref_axis',(-0.901958432317945,0.431822864575922,-1.17097176385396E-30));
#126997=DIRECTION('center_axis',(0.,0.,-1.));
#126998=DIRECTION('ref_axis',(0.,1.,0.));
#126999=DIRECTION('',(0.,1.23467863058847E-16,-1.));
#127000=DIRECTION('center_axis',(0.,0.,1.));
#127001=DIRECTION('ref_axis',(0.,1.,0.));
#127002=DIRECTION('',(0.,-1.23467863058847E-16,1.));
#127003=DIRECTION('center_axis',(0.,0.,-1.));
#127004=DIRECTION('ref_axis',(0.,1.,0.));
#127005=DIRECTION('',(-1.53699078067169E-33,1.23467863058847E-16,-1.));
#127006=DIRECTION('center_axis',(0.,0.,1.));
#127007=DIRECTION('ref_axis',(0.,1.,0.));
#127008=DIRECTION('',(0.,-1.23467863058847E-16,1.));
#127009=DIRECTION('center_axis',(-0.997564050259824,-0.069756473744129,
-8.6126827477082E-18));
#127010=DIRECTION('ref_axis',(-0.069756473744129,0.997564050259824,-8.38175983410215E-37));
#127011=DIRECTION('',(1.53699078067169E-33,-1.23467863058847E-16,1.));
#127012=DIRECTION('',(-0.069756473744129,0.997564050259824,1.23167101549909E-16));
#127013=DIRECTION('center_axis',(-0.0689902057164932,0.98660590693345,0.147814532165213));
#127014=DIRECTION('ref_axis',(5.43774297173137E-18,0.148167565509255,-0.988962270529599));
#127015=DIRECTION('center_axis',(-0.664295471254594,0.747470084264672,2.08541328321077E-15));
#127016=DIRECTION('ref_axis',(-0.747470084264672,-0.664295471254594,-8.18696566210924E-31));
#127017=DIRECTION('center_axis',(0.,0.,-1.));
#127018=DIRECTION('ref_axis',(0.,1.,0.));
#127019=DIRECTION('center_axis',(0.,1.02798428206033E-16,-1.));
#127020=DIRECTION('ref_axis',(0.,1.,1.02798428206033E-16));
#127021=DIRECTION('center_axis',(0.,-1.02798428206033E-16,1.));
#127022=DIRECTION('ref_axis',(0.,-1.,-1.02798428206033E-16));
#127023=DIRECTION('center_axis',(-0.747470084264675,0.664295471254592,1.01845764994016E-15));
#127024=DIRECTION('ref_axis',(-0.664295471254592,-0.747470084264675,3.38786561065658E-30));
#127025=DIRECTION('center_axis',(-0.986605906933449,0.068990205716489,-0.147814532165218));
#127026=DIRECTION('ref_axis',(-0.14816756550926,4.04951997064162E-18,0.988962270529599));
#127027=DIRECTION('center_axis',(-0.0697564737441252,-0.997564050259824,
-1.23167101549909E-16));
#127028=DIRECTION('ref_axis',(-0.997564050259824,0.0697564737441252,1.56258158132391E-34));
#127029=DIRECTION('',(-0.997564050259824,0.0697564737441252,8.61268274770774E-18));
#127030=DIRECTION('center_axis',(-0.992770886529525,0.0694213030853416,
-0.0979114372140158));
#127031=DIRECTION('ref_axis',(-0.0981482265735668,2.47795101036114E-18,
0.995171807086829));
#127032=DIRECTION('center_axis',(-0.901958432317947,0.431822864575918,-5.06803925803546E-15));
#127033=DIRECTION('ref_axis',(-0.431822864575917,-0.901958432317947,6.66597837156041E-31));
#127034=DIRECTION('center_axis',(0.,-1.23467863058847E-16,1.));
#127035=DIRECTION('ref_axis',(0.,-1.,-1.05265590482978E-16));
#127036=DIRECTION('center_axis',(0.,1.04559862480377E-16,-1.));
#127037=DIRECTION('ref_axis',(0.,-1.,-1.04559862480377E-16));
#127038=DIRECTION('center_axis',(0.,-1.23467863058847E-16,1.));
#127039=DIRECTION('ref_axis',(0.,-1.,-1.05265590482978E-16));
#127040=DIRECTION('center_axis',(0.,1.04559862480377E-16,-1.));
#127041=DIRECTION('ref_axis',(0.,-1.,-1.04559862480377E-16));
#127042=DIRECTION('center_axis',(0.,0.,-1.));
#127043=DIRECTION('ref_axis',(0.,1.,0.));
#127044=DIRECTION('',(0.,1.23467863058847E-16,-1.));
#127045=DIRECTION('',(0.,-1.23467863058847E-16,1.));
#127046=DIRECTION('center_axis',(1.42788400384581E-31,-1.65132260162873E-46,
1.));
#127047=DIRECTION('ref_axis',(1.15648231731787E-15,1.,-3.88938454866321E-62));
#127048=DIRECTION('center_axis',(0.,0.,-1.));
#127049=DIRECTION('ref_axis',(0.,1.,0.));
#127050=DIRECTION('',(0.,1.23467863058847E-16,-1.));
#127051=DIRECTION('',(-1.53699078067169E-33,-1.23467863058847E-16,1.));
#127052=DIRECTION('center_axis',(0.,0.,1.));
#127053=DIRECTION('ref_axis',(0.,1.,0.));
#127054=DIRECTION('center_axis',(0.,0.,-1.));
#127055=DIRECTION('ref_axis',(0.,1.,0.));
#127056=DIRECTION('',(0.,1.23467863058847E-16,-1.));
#127057=DIRECTION('',(0.,-1.23467863058847E-16,1.));
#127058=DIRECTION('center_axis',(0.,0.,1.));
#127059=DIRECTION('ref_axis',(0.,1.,0.));
#127060=DIRECTION('center_axis',(0.,0.,-1.));
#127061=DIRECTION('ref_axis',(0.,1.,0.));
#127062=DIRECTION('',(0.,1.23467863058847E-16,-1.));
#127063=DIRECTION('',(0.,-1.23467863058847E-16,1.));
#127064=DIRECTION('center_axis',(4.28365201153745E-31,-1.48619034146585E-45,
1.));
#127065=DIRECTION('ref_axis',(3.46944695195361E-15,1.,-6.22301527786114E-61));
#127066=DIRECTION('center_axis',(0.,1.18842113532929E-16,-1.));
#127067=DIRECTION('ref_axis',(0.,1.,1.18842113532929E-16));
#127068=DIRECTION('center_axis',(0.,1.18842113532929E-16,-1.));
#127069=DIRECTION('ref_axis',(0.,-1.,-1.18842113532929E-16));
#127070=DIRECTION('center_axis',(0.,-1.18842113532929E-16,1.));
#127071=DIRECTION('ref_axis',(0.,1.,1.18842113532929E-16));
#127072=DIRECTION('center_axis',(0.901958432317944,-0.431822864575923,2.31577870403057E-15));
#127073=DIRECTION('ref_axis',(0.431822864575923,0.901958432317944,-1.23890881716737E-31));
#127074=DIRECTION('center_axis',(0.992770886529525,-0.0694213030853436,
-0.0979114372140112));
#127075=DIRECTION('ref_axis',(-0.0981482265735623,2.06880671420837E-18,
-0.995171807086829));
#127076=DIRECTION('center_axis',(0.,0.,-1.));
#127077=DIRECTION('ref_axis',(0.,1.,0.));
#127078=DIRECTION('',(0.,1.23467863058847E-16,-1.));
#127079=DIRECTION('',(0.,-1.23467863058847E-16,1.));
#127080=DIRECTION('center_axis',(0.,0.,-1.));
#127081=DIRECTION('ref_axis',(0.,1.,0.));
#127082=DIRECTION('center_axis',(0.,0.,-1.));
#127083=DIRECTION('ref_axis',(0.,1.,0.));
#127084=DIRECTION('',(0.,1.23467863058847E-16,-1.));
#127085=DIRECTION('',(0.,-1.23467863058847E-16,1.));
#127086=DIRECTION('center_axis',(0.,0.,-1.));
#127087=DIRECTION('ref_axis',(0.,1.,0.));
#127088=DIRECTION('center_axis',(0.0697564737441281,0.997564050259824,1.23167101549909E-16));
#127089=DIRECTION('ref_axis',(1.76567270303392E-15,9.8268693212801E-33,
-1.));
#127090=DIRECTION('',(-0.997564050259824,0.0697564737441281,8.61268274770809E-18));
#127091=DIRECTION('center_axis',(0.98660590693345,-0.0689902057164932,-0.147814532165213));
#127092=DIRECTION('ref_axis',(-0.148167565509255,-4.52088703569399E-18,
-0.988962270529599));
#127093=DIRECTION('center_axis',(0.747470084264675,-0.664295471254592,6.06224791631038E-16));
#127094=DIRECTION('ref_axis',(0.664295471254592,0.747470084264675,9.59955536918487E-32));
#127095=DIRECTION('center_axis',(0.,0.,-1.));
#127096=DIRECTION('ref_axis',(0.,1.,0.));
#127097=DIRECTION('center_axis',(0.,1.02798428206033E-16,-1.));
#127098=DIRECTION('ref_axis',(0.,-1.,-1.02798428206033E-16));
#127099=DIRECTION('center_axis',(1.10148875902005E-31,-1.02798428206033E-16,
1.));
#127100=DIRECTION('ref_axis',(5.32907051820075E-15,1.,1.02798428206033E-16));
#127101=DIRECTION('center_axis',(0.664295471254592,-0.747470084264675,2.95837698315952E-15));
#127102=DIRECTION('ref_axis',(0.747470084264675,0.664295471254592,-5.32960101812494E-31));
#127103=DIRECTION('center_axis',(0.0689902057164909,-0.986605906933449,
0.14781453216522));
#127104=DIRECTION('ref_axis',(-4.37731061835132E-18,-0.148167565509262,
-0.988962270529598));
#127105=DIRECTION('center_axis',(0.997564050259824,0.0697564737441242,8.61268274770761E-18));
#127106=DIRECTION('ref_axis',(-6.56745262755161E-34,1.23467863058847E-16,
-1.));
#127107=DIRECTION('',(-0.0697564737441243,0.997564050259824,1.23167101549909E-16));
#127108=DIRECTION('center_axis',(0.0694213030853413,-0.992770886529525,
0.0979114372140151));
#127109=DIRECTION('ref_axis',(3.30612675079287E-17,-0.0981482265735662,
-0.995171807086829));
#127110=DIRECTION('center_axis',(0.431822864575922,-0.901958432317945,-1.52768647491022E-15));
#127111=DIRECTION('ref_axis',(0.901958432317945,0.431822864575922,-1.17097176385396E-30));
#127112=DIRECTION('center_axis',(0.,1.18842113532929E-16,-1.));
#127113=DIRECTION('ref_axis',(0.,1.,1.18842113532929E-16));
#127114=DIRECTION('center_axis',(0.,-1.18842113532929E-16,1.));
#127115=DIRECTION('ref_axis',(0.,1.,1.18842113532929E-16));
#127116=DIRECTION('center_axis',(8.21698180771796E-33,1.18842113532929E-16,
-1.));
#127117=DIRECTION('ref_axis',(1.77635683940025E-15,-1.,-1.18842113532929E-16));
#127118=DIRECTION('center_axis',(-0.431822864575923,-0.901958432317944,
1.69742941656691E-16));
#127119=DIRECTION('ref_axis',(0.901958432317944,-0.431822864575923,7.92903681942359E-33));
#127120=DIRECTION('center_axis',(-0.0694213030853481,-0.992770886529524,
-0.0979114372140207));
#127121=DIRECTION('ref_axis',(-3.05094293527062E-18,0.0981482265735718,
-0.995171807086828));
#127122=DIRECTION('center_axis',(0.,0.,-1.));
#127123=DIRECTION('ref_axis',(0.,1.,0.));
#127124=DIRECTION('',(0.,1.23467863058847E-16,-1.));
#127125=DIRECTION('',(0.,-1.23467863058847E-16,1.));
#127126=DIRECTION('center_axis',(0.,0.,-1.));
#127127=DIRECTION('ref_axis',(0.,1.,0.));
#127128=DIRECTION('center_axis',(0.,0.,-1.));
#127129=DIRECTION('ref_axis',(0.,1.,0.));
#127130=DIRECTION('',(1.53699078067169E-33,1.23467863058847E-16,-1.));
#127131=DIRECTION('',(0.,-1.23467863058847E-16,1.));
#127132=DIRECTION('center_axis',(0.,0.,-1.));
#127133=DIRECTION('ref_axis',(0.,1.,0.));
#127134=DIRECTION('center_axis',(0.997564050259824,-0.069756473744129,-8.6126827477082E-18));
#127135=DIRECTION('ref_axis',(-2.43965120172245E-34,1.23467863058847E-16,
-1.));
#127136=DIRECTION('',(0.069756473744129,0.997564050259824,1.23167101549909E-16));
#127137=DIRECTION('center_axis',(-0.0689902057164932,-0.98660590693345,
-0.147814532165213));
#127138=DIRECTION('ref_axis',(-5.43774297173137E-18,0.148167565509255,-0.988962270529599));
#127139=DIRECTION('center_axis',(-0.664295471254594,-0.747470084264672,
-2.08541328321077E-15));
#127140=DIRECTION('ref_axis',(0.747470084264672,-0.664295471254594,-8.18696566210924E-31));
#127141=DIRECTION('center_axis',(0.,0.,-1.));
#127142=DIRECTION('ref_axis',(0.,1.,0.));
#127143=DIRECTION('center_axis',(0.,1.02798428206033E-16,-1.));
#127144=DIRECTION('ref_axis',(0.,-1.,-1.02798428206033E-16));
#127145=DIRECTION('center_axis',(0.,-1.02798428206033E-16,1.));
#127146=DIRECTION('ref_axis',(0.,1.,1.02798428206033E-16));
#127147=DIRECTION('center_axis',(-0.747470084264675,-0.664295471254592,
-1.01845764994016E-15));
#127148=DIRECTION('ref_axis',(0.664295471254592,-0.747470084264675,3.38786561065658E-30));
#127149=DIRECTION('center_axis',(-0.986605906933449,-0.068990205716489,
0.147814532165218));
#127150=DIRECTION('ref_axis',(0.14816756550926,4.04951997064162E-18,0.988962270529599));
#127151=DIRECTION('center_axis',(0.0697564737441252,-0.997564050259824,
-1.23167101549909E-16));
#127152=DIRECTION('ref_axis',(9.67324855439588E-34,1.23467863058847E-16,
-1.));
#127153=DIRECTION('',(0.997564050259824,0.0697564737441252,8.61268274770774E-18));
#127154=DIRECTION('center_axis',(-0.992770886529525,-0.0694213030853416,
0.0979114372140158));
#127155=DIRECTION('ref_axis',(0.0981482265735668,2.47795101036114E-18,0.995171807086829));
#127156=DIRECTION('center_axis',(-0.901958432317947,-0.431822864575918,
5.06803925803546E-15));
#127157=DIRECTION('ref_axis',(0.431822864575917,-0.901958432317947,6.66597837156041E-31));
#127158=DIRECTION('center_axis',(0.,1.18842113532929E-16,-1.));
#127159=DIRECTION('ref_axis',(1.22464679914735E-16,-1.,-1.18842113532929E-16));
#127160=DIRECTION('center_axis',(-8.21698180771796E-33,1.18842113532929E-16,
-1.));
#127161=DIRECTION('ref_axis',(-1.77635683940025E-15,-1.,-1.18842113532929E-16));
#127162=DIRECTION('center_axis',(8.21698180771796E-33,-1.18842113532929E-16,
1.));
#127163=DIRECTION('ref_axis',(1.77635683940025E-15,1.,1.18842113532929E-16));
#127164=DIRECTION('center_axis',(0.,-1.23467863058847E-16,1.));
#127165=DIRECTION('ref_axis',(0.,-1.,-1.21694324257719E-16));
#127166=DIRECTION('center_axis',(0.,-1.21202576459344E-16,1.));
#127167=DIRECTION('ref_axis',(0.,-1.,-1.21202576459344E-16));
#127168=DIRECTION('center_axis',(0.,1.23467863058847E-16,-1.));
#127169=DIRECTION('ref_axis',(0.923879532507622,0.382683432373937,0.));
#127170=DIRECTION('center_axis',(0.,1.26979970650999E-16,-1.));
#127171=DIRECTION('ref_axis',(0.,1.,1.26979970650999E-16));
#127172=DIRECTION('center_axis',(0.,-1.28766298379097E-16,1.));
#127173=DIRECTION('ref_axis',(0.,1.,1.28766298379097E-16));
#127174=DIRECTION('center_axis',(0.,1.55534083321291E-16,-1.));
#127175=DIRECTION('ref_axis',(0.923879532511285,0.382683432365093,6.24515698316632E-17));
#127176=DIRECTION('center_axis',(0.,1.28766298379097E-16,-1.));
#127177=DIRECTION('ref_axis',(0.,1.,1.28766298379097E-16));
#127178=DIRECTION('center_axis',(0.,-1.23467863058847E-16,1.));
#127179=DIRECTION('ref_axis',(1.22464679914735E-16,1.,1.21694324257719E-16));
#127180=DIRECTION('center_axis',(0.,-1.21202576459343E-16,1.));
#127181=DIRECTION('ref_axis',(0.,-1.,-1.21202576459343E-16));
#127182=DIRECTION('center_axis',(0.,-1.23467863058847E-16,1.));
#127183=DIRECTION('ref_axis',(0.,-1.,-1.21694324257719E-16));
#127184=DIRECTION('center_axis',(0.,-1.21202576459343E-16,1.));
#127185=DIRECTION('ref_axis',(0.,-1.,-1.21202576459343E-16));
#127186=DIRECTION('center_axis',(0.,-1.23467863058847E-16,1.));
#127187=DIRECTION('ref_axis',(0.,-1.,-1.05265590482978E-16));
#127188=DIRECTION('center_axis',(0.,-1.04559862480377E-16,1.));
#127189=DIRECTION('ref_axis',(0.,-1.,-1.04559862480377E-16));
#127190=DIRECTION('center_axis',(0.,-1.23467863058847E-16,1.));
#127191=DIRECTION('ref_axis',(0.,-1.,-1.05265590482978E-16));
#127192=DIRECTION('center_axis',(0.,-1.04559862480377E-16,1.));
#127193=DIRECTION('ref_axis',(0.,-1.,-1.04559862480377E-16));
#127194=DIRECTION('center_axis',(0.,0.,-1.));
#127195=DIRECTION('ref_axis',(0.,1.,0.));
#127196=DIRECTION('',(0.,1.23467863058847E-16,-1.));
#127197=DIRECTION('center_axis',(0.,0.,-1.));
#127198=DIRECTION('ref_axis',(0.,1.,0.));
#127199=DIRECTION('center_axis',(0.,1.18842113532929E-16,-1.));
#127200=DIRECTION('ref_axis',(0.,1.,1.18842113532929E-16));
#127201=DIRECTION('center_axis',(1.64339636154359E-32,-1.18842113532929E-16,
1.));
#127202=DIRECTION('ref_axis',(-3.5527136788005E-15,-1.,-1.18842113532929E-16));
#127203=DIRECTION('center_axis',(0.,1.18842113532929E-16,-1.));
#127204=DIRECTION('ref_axis',(0.,1.,1.18842113532929E-16));
#127205=DIRECTION('center_axis',(0.,-1.23467863058847E-16,1.));
#127206=DIRECTION('ref_axis',(0.,-1.,-1.21694324257719E-16));
#127207=DIRECTION('center_axis',(0.,1.21202576459343E-16,-1.));
#127208=DIRECTION('ref_axis',(0.,-1.,-1.21202576459343E-16));
#127209=DIRECTION('center_axis',(0.,0.,-1.));
#127210=DIRECTION('ref_axis',(0.,1.,0.));
#127211=DIRECTION('',(-0.654839500710631,0.0924107866510669,-0.75009697694337));
#127212=DIRECTION('',(0.425886568670936,-0.388175269924452,-0.817276324412236));
#127213=DIRECTION('center_axis',(0.189676565537595,0.200807286409187,0.961092729246685));
#127214=DIRECTION('ref_axis',(-0.938097396016776,0.326004004576076,0.117024205132558));
#127215=DIRECTION('',(0.425886568671724,-0.38817526992251,-0.817276324412748));
#127216=DIRECTION('',(-0.654839500710178,0.0924107866496375,-0.750096976943942));
#127217=DIRECTION('center_axis',(0.200678112292284,0.188576796953589,0.961336094660723));
#127218=DIRECTION('ref_axis',(0.903627963715395,-0.41466272120114,-0.107290870243625));
#127219=DIRECTION('center_axis',(0.,0.,1.));
#127220=DIRECTION('ref_axis',(-1.59672976227174E-14,1.,0.));
#127221=DIRECTION('center_axis',(0.,0.,-1.));
#127222=DIRECTION('ref_axis',(0.535742164068221,-0.844381627961847,0.));
#127223=DIRECTION('',(-0.425886568670953,-0.388175269924826,-0.81727632441205));
#127224=DIRECTION('center_axis',(-0.188086755331098,0.201586350617653,0.961242069259183));
#127225=DIRECTION('ref_axis',(0.629481269533852,-0.726522398490792,0.275533184566283));
#127226=DIRECTION('',(-0.425886568671143,-0.388175269923767,-0.817276324412454));
#127227=DIRECTION('',(0.654839500710178,0.0924107866496375,-0.750096976943942));
#127228=DIRECTION('center_axis',(0.,0.,1.));
#127229=DIRECTION('ref_axis',(-1.,-2.66121627045289E-15,0.));
#127230=DIRECTION('center_axis',(0.,0.,-1.));
#127231=DIRECTION('ref_axis',(0.,1.,0.));
#127232=DIRECTION('center_axis',(0.,0.,-1.));
#127233=DIRECTION('ref_axis',(0.,1.,0.));
#127234=DIRECTION('',(0.435638227654975,-0.396444898338133,-0.808115571677281));
#127235=DIRECTION('center_axis',(-0.201738744861899,-0.187890027474552,
0.96124857159694));
#127236=DIRECTION('ref_axis',(-0.681118454259118,0.732173219627526,0.000166517061419875));
#127237=DIRECTION('',(0.435638227812403,-0.396444898257199,-0.80811557163212));
#127238=DIRECTION('',(-0.141856700036149,0.637752802814605,-0.757065412733252));
#127239=DIRECTION('center_axis',(0.,0.,1.));
#127240=DIRECTION('ref_axis',(-3.72570277863391E-14,-1.,0.));
#127241=DIRECTION('center_axis',(0.,0.,-1.));
#127242=DIRECTION('ref_axis',(0.,1.,0.));
#127243=DIRECTION('center_axis',(0.,0.,-1.));
#127244=DIRECTION('ref_axis',(0.,1.,0.));
#127245=DIRECTION('',(0.141856700036448,0.637752802815158,-0.75706541273273));
#127246=DIRECTION('',(-0.435638227813814,-0.39644489825645,-0.808115571631727));
#127247=DIRECTION('center_axis',(0.200985107811872,-0.189230679181084,0.961143452609711));
#127248=DIRECTION('ref_axis',(0.32607544192224,0.938135929232121,0.116515168364468));
#127249=DIRECTION('',(-0.43563822781117,-0.396444898257902,-0.80811557163244));
#127250=DIRECTION('',(0.141856700036051,0.637752802814614,-0.757065412733263));
#127251=DIRECTION('center_axis',(0.188364697331784,-0.201014679344831,0.961307359530239));
#127252=DIRECTION('ref_axis',(-0.494479298944248,-0.865119964932013,-0.0840099350769745));
#127253=DIRECTION('center_axis',(0.,0.,-1.));
#127254=DIRECTION('ref_axis',(0.,-1.,0.));
#127255=DIRECTION('center_axis',(0.,0.,1.));
#127256=DIRECTION('ref_axis',(1.,-1.06448650818115E-14,0.));
#127257=DIRECTION('center_axis',(0.,0.,-1.));
#127258=DIRECTION('ref_axis',(0.,1.,0.));
#127259=DIRECTION('center_axis',(0.,0.,-1.));
#127260=DIRECTION('ref_axis',(0.,1.,0.));
#127261=DIRECTION('center_axis',(0.,1.18842113532929E-16,-1.));
#127262=DIRECTION('ref_axis',(0.927815008667248,0.373040627401085,4.43329365939947E-17));
#127263=DIRECTION('center_axis',(0.,1.28766298379097E-16,-1.));
#127264=DIRECTION('ref_axis',(0.923879532511286,0.382683432365091,4.92767290366603E-17));
#127265=DIRECTION('',(-0.141856700036947,0.637752802814889,-0.757065412732863));
#127266=DIRECTION('',(0.654839500710788,0.0924107866506205,-0.750096976943288));
#127267=DIRECTION('center_axis',(0.,0.,1.));
#127268=DIRECTION('ref_axis',(1.,0.,0.));
#127269=DIRECTION('center_axis',(0.,0.,1.));
#127270=DIRECTION('ref_axis',(1.,0.,0.));
#127271=DIRECTION('',(0.,-1.,0.));
#127272=DIRECTION('',(1.,0.,0.));
#127273=DIRECTION('center_axis',(-1.,0.,0.));
#127274=DIRECTION('ref_axis',(0.,0.,1.));
#127275=DIRECTION('center_axis',(-1.,-1.73472347597681E-16,0.));
#127276=DIRECTION('ref_axis',(1.73472347597681E-16,-1.,0.));
#127277=DIRECTION('center_axis',(-1.,0.,4.35694038576837E-17));
#127278=DIRECTION('ref_axis',(4.35694038576837E-17,0.,1.));
#127279=DIRECTION('center_axis',(-1.,0.,-2.60208521396521E-16));
#127280=DIRECTION('ref_axis',(-2.60208521396521E-16,0.,1.));
#127281=DIRECTION('center_axis',(-1.,0.,0.));
#127282=DIRECTION('ref_axis',(0.,0.,1.));
#127283=DIRECTION('center_axis',(-1.,0.,0.));
#127284=DIRECTION('ref_axis',(0.,0.,1.));
#127285=DIRECTION('center_axis',(0.,0.,-1.));
#127286=DIRECTION('ref_axis',(-1.,0.,0.));
#127287=DIRECTION('center_axis',(0.,0.,-1.));
#127288=DIRECTION('ref_axis',(-1.,0.,0.));
#127289=DIRECTION('center_axis',(0.,0.,1.));
#127290=DIRECTION('ref_axis',(1.,0.,0.));
#127291=DIRECTION('center_axis',(-1.,0.,0.));
#127292=DIRECTION('ref_axis',(0.,0.,1.));
#127293=DIRECTION('center_axis',(-1.,0.,0.));
#127294=DIRECTION('ref_axis',(0.,0.,1.));
#127295=DIRECTION('center_axis',(1.,0.,0.));
#127296=DIRECTION('ref_axis',(0.,0.,-1.));
#127297=DIRECTION('center_axis',(0.,1.,0.));
#127298=DIRECTION('ref_axis',(0.,0.,-1.));
#127299=DIRECTION('center_axis',(1.,0.,0.));
#127300=DIRECTION('ref_axis',(0.,0.,-1.));
#127301=DIRECTION('center_axis',(0.,1.,0.));
#127302=DIRECTION('ref_axis',(0.,0.,-1.));
#127303=DIRECTION('center_axis',(0.,1.,0.));
#127304=DIRECTION('ref_axis',(0.,0.,1.));
#127305=DIRECTION('center_axis',(5.58059449121998E-15,0.707106781186545,
-0.70710678118655));
#127306=DIRECTION('ref_axis',(1.98375245311818E-13,0.70710678118655,0.707106781186545));
#127307=DIRECTION('center_axis',(0.,1.,0.));
#127308=DIRECTION('ref_axis',(0.,0.,1.));
#127309=DIRECTION('center_axis',(9.84810792568227E-16,0.707106781186547,
0.707106781186548));
#127310=DIRECTION('ref_axis',(-8.25384288032917E-14,-0.707106781186548,
0.707106781186547));
#127311=DIRECTION('center_axis',(0.,0.,-1.));
#127312=DIRECTION('ref_axis',(-1.,0.,0.));
#127313=DIRECTION('axis',(0.,0.,1.));
#127314=DIRECTION('refdir',(1.,0.,0.));
#127315=DIRECTION('center_axis',(0.,0.,-1.));
#127316=DIRECTION('ref_axis',(-1.,0.,0.));
#127317=DIRECTION('',(0.,-1.,0.));
#127318=DIRECTION('',(-1.,0.,0.));
#127319=DIRECTION('',(0.,-1.,0.));
#127320=DIRECTION('',(-1.,0.,0.));
#127321=DIRECTION('center_axis',(0.,1.,1.52503162723236E-17));
#127322=DIRECTION('ref_axis',(0.,-1.52503162723236E-17,1.));
#127323=DIRECTION('',(0.,1.52503162723236E-17,-1.));
#127324=DIRECTION('',(-1.,0.,0.));
#127325=DIRECTION('',(0.,1.52503162723236E-17,-1.));
#127326=DIRECTION('center_axis',(0.,0.,1.));
#127327=DIRECTION('ref_axis',(1.,0.,0.));
#127328=DIRECTION('',(0.,1.,0.));
#127329=DIRECTION('',(-1.,0.,0.));
#127330=DIRECTION('',(0.,1.,0.));
#127331=DIRECTION('center_axis',(0.,-1.,0.));
#127332=DIRECTION('ref_axis',(0.,0.,-1.));
#127333=DIRECTION('',(0.,0.,1.));
#127334=DIRECTION('',(0.,0.,1.));
#127335=DIRECTION('center_axis',(1.,0.,0.));
#127336=DIRECTION('ref_axis',(0.,0.,-1.));
#127337=DIRECTION('center_axis',(1.,0.,0.));
#127338=DIRECTION('ref_axis',(0.,0.,-1.));
#127339=DIRECTION('axis',(0.,0.,1.));
#127340=DIRECTION('refdir',(1.,0.,0.));
#127341=DIRECTION('axis',(0.,0.,1.));
#127342=DIRECTION('refdir',(1.,0.,0.));
#127343=DIRECTION('center_axis',(1.,0.,0.));
#127344=DIRECTION('ref_axis',(0.,0.,-1.));
#127345=DIRECTION('center_axis',(1.,0.,0.));
#127346=DIRECTION('ref_axis',(0.,0.,-1.));
#127347=DIRECTION('center_axis',(0.,1.,1.15813679845853E-16));
#127348=DIRECTION('ref_axis',(0.,-1.15813679845853E-16,1.));
#127349=DIRECTION('center_axis',(-1.,0.,0.));
#127350=DIRECTION('ref_axis',(0.,0.,-1.));
#127351=DIRECTION('center_axis',(1.,0.,0.));
#127352=DIRECTION('ref_axis',(0.,0.,-1.));
#127353=DIRECTION('',(-1.,0.,0.));
#127354=DIRECTION('center_axis',(-1.,0.,0.));
#127355=DIRECTION('ref_axis',(0.,0.,1.));
#127356=DIRECTION('center_axis',(-1.,0.,0.));
#127357=DIRECTION('ref_axis',(0.,0.,1.));
#127358=DIRECTION('',(-1.,0.,0.));
#127359=DIRECTION('',(1.,0.,0.));
#127360=DIRECTION('center_axis',(-1.,0.,0.));
#127361=DIRECTION('ref_axis',(0.,0.,1.));
#127362=DIRECTION('',(-1.,0.,0.));
#127363=DIRECTION('center_axis',(-1.,0.,0.));
#127364=DIRECTION('ref_axis',(0.,0.,-1.));
#127365=DIRECTION('',(-1.,0.,0.));
#127366=DIRECTION('center_axis',(1.,0.,0.));
#127367=DIRECTION('ref_axis',(0.,0.587785252292479,-0.809016994374943));
#127368=DIRECTION('center_axis',(-1.,0.,0.));
#127369=DIRECTION('ref_axis',(0.,0.,1.));
#127370=DIRECTION('center_axis',(1.,0.,0.));
#127371=DIRECTION('ref_axis',(0.,0.866025403784443,-0.499999999999992));
#127372=DIRECTION('',(-1.,0.,0.));
#127373=DIRECTION('center_axis',(-1.,0.,0.));
#127374=DIRECTION('ref_axis',(0.,6.00877412544304E-16,-1.));
#127375=DIRECTION('',(-1.,0.,0.));
#127376=DIRECTION('center_axis',(-1.,0.,0.));
#127377=DIRECTION('ref_axis',(0.,0.,1.));
#127378=DIRECTION('center_axis',(1.,0.,0.));
#127379=DIRECTION('ref_axis',(0.,0.743144825477386,0.669130606358867));
#127380=DIRECTION('',(-1.,0.,0.));
#127381=DIRECTION('center_axis',(-1.,0.,0.));
#127382=DIRECTION('ref_axis',(0.,0.,-1.));
#127383=DIRECTION('',(-1.,0.,0.));
#127384=DIRECTION('center_axis',(-1.,0.,0.));
#127385=DIRECTION('ref_axis',(0.,0.,1.));
#127386=DIRECTION('center_axis',(1.,0.,0.));
#127387=DIRECTION('ref_axis',(0.,0.406736643075789,0.913545457642606));
#127388=DIRECTION('',(-1.,0.,0.));
#127389=DIRECTION('center_axis',(-1.,0.,0.));
#127390=DIRECTION('ref_axis',(0.,0.,-1.));
#127391=DIRECTION('',(-1.,0.,0.));
#127392=DIRECTION('center_axis',(-1.,0.,0.));
#127393=DIRECTION('ref_axis',(0.,0.,1.));
#127394=DIRECTION('center_axis',(1.,0.,0.));
#127395=DIRECTION('ref_axis',(0.,0.95105651629515,0.309016994374958));
#127396=DIRECTION('',(-1.,0.,0.));
#127397=DIRECTION('center_axis',(-1.,0.,0.));
#127398=DIRECTION('ref_axis',(0.,-1.80263223763291E-15,-1.));
#127399=DIRECTION('',(-1.,0.,0.));
#127400=DIRECTION('center_axis',(-1.,0.,0.));
#127401=DIRECTION('ref_axis',(0.,0.,1.));
#127402=DIRECTION('center_axis',(1.,0.,0.));
#127403=DIRECTION('ref_axis',(0.,0.994521895368274,-0.104528463267644));
#127404=DIRECTION('',(-1.,0.,0.));
#127405=DIRECTION('center_axis',(-1.,0.,0.));
#127406=DIRECTION('ref_axis',(0.,-2.66639351816535E-15,-1.));
#127407=DIRECTION('',(-1.,0.,0.));
#127408=DIRECTION('center_axis',(-1.,0.,0.));
#127409=DIRECTION('ref_axis',(0.,0.,1.));
#127410=DIRECTION('',(-1.,0.,0.));
#127411=DIRECTION('',(-1.,0.,0.));
#127412=DIRECTION('center_axis',(-1.,0.,0.));
#127413=DIRECTION('ref_axis',(0.,-1.,-1.83697019872103E-16));
#127414=DIRECTION('center_axis',(1.,0.,0.));
#127415=DIRECTION('ref_axis',(0.,0.,1.));
#127416=DIRECTION('',(-1.,0.,0.));
#127417=DIRECTION('center_axis',(1.,0.,0.));
#127418=DIRECTION('ref_axis',(0.,0.,1.));
#127419=DIRECTION('',(1.,0.,0.));
#127420=DIRECTION('center_axis',(-1.,0.,0.));
#127421=DIRECTION('ref_axis',(0.,0.,1.));
#127422=DIRECTION('center_axis',(1.,0.,0.));
#127423=DIRECTION('ref_axis',(0.,-0.994521895368273,-0.104528463267657));
#127424=DIRECTION('center_axis',(-1.,0.,0.));
#127425=DIRECTION('ref_axis',(0.,0.,1.));
#127426=DIRECTION('center_axis',(1.,0.,0.));
#127427=DIRECTION('ref_axis',(0.,-0.866025403784436,-0.500000000000004));
#127428=DIRECTION('center_axis',(-1.,0.,0.));
#127429=DIRECTION('ref_axis',(0.,0.,1.));
#127430=DIRECTION('center_axis',(1.,0.,0.));
#127431=DIRECTION('ref_axis',(0.,-0.587785252292469,-0.80901699437495));
#127432=DIRECTION('center_axis',(-1.,0.,0.));
#127433=DIRECTION('ref_axis',(0.,0.,1.));
#127434=DIRECTION('center_axis',(1.,0.,0.));
#127435=DIRECTION('ref_axis',(0.,-0.207911690817753,-0.978147600733807));
#127436=DIRECTION('center_axis',(-1.,0.,0.));
#127437=DIRECTION('ref_axis',(0.,0.,1.));
#127438=DIRECTION('center_axis',(1.,0.,0.));
#127439=DIRECTION('ref_axis',(0.,0.207911690817766,-0.978147600733804));
#127440=DIRECTION('center_axis',(-1.,0.,0.));
#127441=DIRECTION('ref_axis',(0.,0.,1.));
#127442=DIRECTION('center_axis',(-1.,0.,0.));
#127443=DIRECTION('ref_axis',(0.,0.,1.));
#127444=DIRECTION('center_axis',(-1.,0.,0.));
#127445=DIRECTION('ref_axis',(0.,0.,1.));
#127446=DIRECTION('center_axis',(-1.,0.,0.));
#127447=DIRECTION('ref_axis',(0.,0.,1.));
#127448=DIRECTION('center_axis',(-1.,0.,0.));
#127449=DIRECTION('ref_axis',(0.,0.,1.));
#127450=DIRECTION('center_axis',(-1.,0.,0.));
#127451=DIRECTION('ref_axis',(0.,0.,1.));
#127452=DIRECTION('center_axis',(-1.,0.,0.));
#127453=DIRECTION('ref_axis',(0.,0.,1.));
#127454=DIRECTION('center_axis',(1.,0.,0.));
#127455=DIRECTION('ref_axis',(0.,0.,1.));
#127456=DIRECTION('center_axis',(-1.,0.,0.));
#127457=DIRECTION('ref_axis',(0.,0.,1.));
#127458=DIRECTION('center_axis',(1.,0.,0.));
#127459=DIRECTION('ref_axis',(0.,-0.406736643075801,0.913545457642601));
#127460=DIRECTION('center_axis',(-1.,0.,0.));
#127461=DIRECTION('ref_axis',(0.,0.,1.));
#127462=DIRECTION('center_axis',(1.,0.,0.));
#127463=DIRECTION('ref_axis',(0.,-0.743144825477396,0.669130606358857));
#127464=DIRECTION('center_axis',(-1.,0.,0.));
#127465=DIRECTION('ref_axis',(0.,0.,1.));
#127466=DIRECTION('center_axis',(1.,0.,0.));
#127467=DIRECTION('ref_axis',(0.,-0.951056516295155,0.309016994374945));
#127468=DIRECTION('center_axis',(-1.,0.,0.));
#127469=DIRECTION('ref_axis',(0.,0.,1.));
#127470=DIRECTION('',(0.,1.,0.));
#127471=DIRECTION('',(0.,-1.,0.));
#127472=DIRECTION('',(0.,0.,1.));
#127473=DIRECTION('center_axis',(-1.,0.,0.));
#127474=DIRECTION('ref_axis',(0.,0.,1.));
#127475=DIRECTION('',(0.,1.,0.));
#127476=DIRECTION('',(0.,0.,1.));
#127477=DIRECTION('',(0.,-1.,0.));
#127478=DIRECTION('center_axis',(-1.,0.,0.));
#127479=DIRECTION('ref_axis',(0.,0.,1.));
#127480=DIRECTION('center_axis',(-1.,0.,0.));
#127481=DIRECTION('ref_axis',(0.,0.,1.));
#127482=DIRECTION('center_axis',(-1.,0.,0.));
#127483=DIRECTION('ref_axis',(0.,0.,1.));
#127484=DIRECTION('center_axis',(-1.,0.,0.));
#127485=DIRECTION('ref_axis',(0.,0.,1.));
#127486=DIRECTION('center_axis',(-1.,0.,0.));
#127487=DIRECTION('ref_axis',(0.,0.,1.));
#127488=DIRECTION('center_axis',(-1.,0.,0.));
#127489=DIRECTION('ref_axis',(0.,0.,1.));
#127490=DIRECTION('center_axis',(-1.,0.,0.));
#127491=DIRECTION('ref_axis',(0.,0.,1.));
#127492=DIRECTION('center_axis',(-1.,0.,0.));
#127493=DIRECTION('ref_axis',(0.,0.,1.));
#127494=DIRECTION('center_axis',(-1.,0.,0.));
#127495=DIRECTION('ref_axis',(0.,0.,1.));
#127496=DIRECTION('center_axis',(-1.,0.,0.));
#127497=DIRECTION('ref_axis',(0.,0.,1.));
#127498=DIRECTION('center_axis',(-1.,0.,0.));
#127499=DIRECTION('ref_axis',(0.,0.,1.));
#127500=DIRECTION('center_axis',(-1.,0.,0.));
#127501=DIRECTION('ref_axis',(0.,0.,1.));
#127502=DIRECTION('center_axis',(-1.,0.,0.));
#127503=DIRECTION('ref_axis',(0.,0.,1.));
#127504=DIRECTION('center_axis',(-1.,0.,0.));
#127505=DIRECTION('ref_axis',(0.,0.,1.));
#127506=DIRECTION('center_axis',(-1.,0.,0.));
#127507=DIRECTION('ref_axis',(0.,0.,1.));
#127508=DIRECTION('center_axis',(-1.,0.,0.));
#127509=DIRECTION('ref_axis',(0.,0.,1.));
#127510=DIRECTION('center_axis',(-1.,0.,0.));
#127511=DIRECTION('ref_axis',(0.,0.,1.));
#127512=DIRECTION('center_axis',(-1.,0.,0.));
#127513=DIRECTION('ref_axis',(0.,0.,1.));
#127514=DIRECTION('center_axis',(-1.,0.,0.));
#127515=DIRECTION('ref_axis',(0.,0.,1.));
#127516=DIRECTION('center_axis',(-1.,0.,0.));
#127517=DIRECTION('ref_axis',(0.,0.,1.));
#127518=DIRECTION('center_axis',(-1.,0.,0.));
#127519=DIRECTION('ref_axis',(0.,0.,1.));
#127520=DIRECTION('center_axis',(-1.,0.,0.));
#127521=DIRECTION('ref_axis',(0.,0.,1.));
#127522=DIRECTION('center_axis',(-1.,0.,0.));
#127523=DIRECTION('ref_axis',(0.,0.,1.));
#127524=DIRECTION('center_axis',(-1.,0.,0.));
#127525=DIRECTION('ref_axis',(0.,0.,1.));
#127526=DIRECTION('center_axis',(-1.,0.,0.));
#127527=DIRECTION('ref_axis',(0.,0.,1.));
#127528=DIRECTION('center_axis',(-1.,0.,0.));
#127529=DIRECTION('ref_axis',(0.,0.,1.));
#127530=DIRECTION('center_axis',(-1.,0.,0.));
#127531=DIRECTION('ref_axis',(0.,0.,1.));
#127532=DIRECTION('center_axis',(-1.,0.,0.));
#127533=DIRECTION('ref_axis',(0.,0.,1.));
#127534=DIRECTION('center_axis',(-1.,0.,0.));
#127535=DIRECTION('ref_axis',(0.,0.,1.));
#127536=DIRECTION('',(1.,0.,0.));
#127537=DIRECTION('center_axis',(-1.,0.,0.));
#127538=DIRECTION('ref_axis',(0.,0.,1.));
#127539=DIRECTION('',(-1.,0.,0.));
#127540=DIRECTION('center_axis',(-1.,0.,0.));
#127541=DIRECTION('ref_axis',(0.,0.,1.));
#127542=DIRECTION('',(-1.,0.,0.));
#127543=DIRECTION('',(1.,0.,0.));
#127544=DIRECTION('center_axis',(-1.,0.,0.));
#127545=DIRECTION('ref_axis',(0.,0.,1.));
#127546=DIRECTION('center_axis',(-1.,0.,0.));
#127547=DIRECTION('ref_axis',(0.,0.,1.));
#127548=DIRECTION('',(-1.,0.,0.));
#127549=DIRECTION('',(1.,0.,0.));
#127550=DIRECTION('center_axis',(-1.,0.,0.));
#127551=DIRECTION('ref_axis',(0.,0.,1.));
#127552=DIRECTION('center_axis',(-1.,0.,0.));
#127553=DIRECTION('ref_axis',(0.,0.,1.));
#127554=DIRECTION('',(-1.,0.,0.));
#127555=DIRECTION('',(1.,0.,0.));
#127556=DIRECTION('center_axis',(-1.,0.,0.));
#127557=DIRECTION('ref_axis',(0.,0.,1.));
#127558=DIRECTION('center_axis',(-1.,0.,0.));
#127559=DIRECTION('ref_axis',(0.,0.,1.));
#127560=DIRECTION('center_axis',(-1.,0.,0.));
#127561=DIRECTION('ref_axis',(0.,0.,1.));
#127562=DIRECTION('',(-1.,0.,0.));
#127563=DIRECTION('center_axis',(-1.,0.,0.));
#127564=DIRECTION('ref_axis',(0.,0.,1.));
#127565=DIRECTION('',(-1.,0.,0.));
#127566=DIRECTION('',(1.,0.,0.));
#127567=DIRECTION('center_axis',(-1.,0.,0.));
#127568=DIRECTION('ref_axis',(0.,0.,1.));
#127569=DIRECTION('center_axis',(-1.,0.,0.));
#127570=DIRECTION('ref_axis',(0.,0.,1.));
#127571=DIRECTION('',(1.,0.,0.));
#127572=DIRECTION('center_axis',(-1.,0.,0.));
#127573=DIRECTION('ref_axis',(0.,0.,1.));
#127574=DIRECTION('',(-1.,0.,0.));
#127575=DIRECTION('center_axis',(-1.,0.,0.));
#127576=DIRECTION('ref_axis',(0.,0.,1.));
#127577=DIRECTION('',(1.,0.,0.));
#127578=DIRECTION('center_axis',(-1.,0.,0.));
#127579=DIRECTION('ref_axis',(0.,0.,1.));
#127580=DIRECTION('',(-1.,0.,0.));
#127581=DIRECTION('center_axis',(-1.,0.,0.));
#127582=DIRECTION('ref_axis',(0.,0.,1.));
#127583=DIRECTION('',(-1.,0.,0.));
#127584=DIRECTION('',(1.,0.,0.));
#127585=DIRECTION('center_axis',(-1.,0.,0.));
#127586=DIRECTION('ref_axis',(0.,0.,1.));
#127587=DIRECTION('center_axis',(-1.,0.,0.));
#127588=DIRECTION('ref_axis',(0.,0.,1.));
#127589=DIRECTION('',(1.,0.,0.));
#127590=DIRECTION('center_axis',(-1.,0.,0.));
#127591=DIRECTION('ref_axis',(0.,0.,1.));
#127592=DIRECTION('',(-1.,0.,0.));
#127593=DIRECTION('center_axis',(-1.,0.,0.));
#127594=DIRECTION('ref_axis',(0.,0.,1.));
#127595=DIRECTION('',(1.,0.,0.));
#127596=DIRECTION('center_axis',(-1.,0.,0.));
#127597=DIRECTION('ref_axis',(0.,0.,1.));
#127598=DIRECTION('',(-1.,0.,0.));
#127599=DIRECTION('center_axis',(-1.,0.,0.));
#127600=DIRECTION('ref_axis',(0.,0.,1.));
#127601=DIRECTION('',(-1.,0.,0.));
#127602=DIRECTION('',(1.,0.,0.));
#127603=DIRECTION('center_axis',(-1.,0.,0.));
#127604=DIRECTION('ref_axis',(0.,0.,1.));
#127605=DIRECTION('center_axis',(-1.,0.,0.));
#127606=DIRECTION('ref_axis',(0.,0.,1.));
#127607=DIRECTION('',(1.,0.,0.));
#127608=DIRECTION('center_axis',(-1.,0.,0.));
#127609=DIRECTION('ref_axis',(0.,0.,1.));
#127610=DIRECTION('',(-1.,0.,0.));
#127611=DIRECTION('center_axis',(-1.,0.,0.));
#127612=DIRECTION('ref_axis',(0.,0.,1.));
#127613=DIRECTION('',(-1.,0.,0.));
#127614=DIRECTION('',(1.,0.,0.));
#127615=DIRECTION('center_axis',(-1.,0.,0.));
#127616=DIRECTION('ref_axis',(0.,0.,1.));
#127617=DIRECTION('center_axis',(-1.,0.,0.));
#127618=DIRECTION('ref_axis',(0.,0.,1.));
#127619=DIRECTION('center_axis',(-1.,0.,0.));
#127620=DIRECTION('ref_axis',(0.,0.,1.));
#127621=DIRECTION('center_axis',(-1.,0.,0.));
#127622=DIRECTION('ref_axis',(0.,0.,1.));
#127623=DIRECTION('center_axis',(-1.,0.,0.));
#127624=DIRECTION('ref_axis',(0.,0.,1.));
#127625=DIRECTION('center_axis',(-1.,0.,0.));
#127626=DIRECTION('ref_axis',(0.,0.,1.));
#127627=DIRECTION('center_axis',(-1.,0.,0.));
#127628=DIRECTION('ref_axis',(0.,0.,1.));
#127629=DIRECTION('center_axis',(-1.,0.,0.));
#127630=DIRECTION('ref_axis',(0.,0.,1.));
#127631=DIRECTION('center_axis',(-1.,0.,0.));
#127632=DIRECTION('ref_axis',(0.,0.,1.));
#127633=DIRECTION('center_axis',(-1.,0.,0.));
#127634=DIRECTION('ref_axis',(0.,0.,1.));
#127635=DIRECTION('center_axis',(-1.,0.,0.));
#127636=DIRECTION('ref_axis',(0.,0.,1.));
#127637=DIRECTION('center_axis',(-1.,0.,0.));
#127638=DIRECTION('ref_axis',(0.,0.,1.));
#127639=DIRECTION('center_axis',(-1.,0.,0.));
#127640=DIRECTION('ref_axis',(0.,0.,1.));
#127641=DIRECTION('center_axis',(-1.,0.,0.));
#127642=DIRECTION('ref_axis',(0.,0.,1.));
#127643=DIRECTION('center_axis',(-1.,0.,0.));
#127644=DIRECTION('ref_axis',(0.,0.,1.));
#127645=DIRECTION('center_axis',(-1.,0.,0.));
#127646=DIRECTION('ref_axis',(0.,0.,1.));
#127647=DIRECTION('center_axis',(-1.,0.,0.));
#127648=DIRECTION('ref_axis',(0.,0.,1.));
#127649=DIRECTION('center_axis',(-1.,0.,0.));
#127650=DIRECTION('ref_axis',(0.,0.,1.));
#127651=DIRECTION('center_axis',(-1.,0.,0.));
#127652=DIRECTION('ref_axis',(0.,0.,1.));
#127653=DIRECTION('center_axis',(-1.,0.,0.));
#127654=DIRECTION('ref_axis',(0.,0.,1.));
#127655=DIRECTION('center_axis',(-1.,0.,0.));
#127656=DIRECTION('ref_axis',(0.,0.,1.));
#127657=DIRECTION('center_axis',(-1.,0.,0.));
#127658=DIRECTION('ref_axis',(0.,0.,1.));
#127659=DIRECTION('center_axis',(-1.,0.,0.));
#127660=DIRECTION('ref_axis',(0.,0.,1.));
#127661=DIRECTION('center_axis',(-1.,0.,0.));
#127662=DIRECTION('ref_axis',(0.,0.,1.));
#127663=DIRECTION('center_axis',(-1.,0.,0.));
#127664=DIRECTION('ref_axis',(0.,0.,1.));
#127665=DIRECTION('center_axis',(-1.,0.,0.));
#127666=DIRECTION('ref_axis',(0.,0.,1.));
#127667=DIRECTION('center_axis',(-1.,0.,0.));
#127668=DIRECTION('ref_axis',(0.,0.,1.));
#127669=DIRECTION('center_axis',(-1.,0.,0.));
#127670=DIRECTION('ref_axis',(0.,0.,1.));
#127671=DIRECTION('center_axis',(-1.,0.,0.));
#127672=DIRECTION('ref_axis',(0.,0.,1.));
#127673=DIRECTION('center_axis',(-1.,0.,0.));
#127674=DIRECTION('ref_axis',(0.,0.,1.));
#127675=DIRECTION('center_axis',(-1.,0.,0.));
#127676=DIRECTION('ref_axis',(0.,0.,1.));
#127677=DIRECTION('center_axis',(-1.,0.,0.));
#127678=DIRECTION('ref_axis',(0.,0.,1.));
#127679=DIRECTION('',(1.,0.,0.));
#127680=DIRECTION('center_axis',(-1.,0.,0.));
#127681=DIRECTION('ref_axis',(0.,0.,1.));
#127682=DIRECTION('center_axis',(-1.,0.,0.));
#127683=DIRECTION('ref_axis',(0.,0.,1.));
#127684=DIRECTION('center_axis',(-1.,0.,0.));
#127685=DIRECTION('ref_axis',(0.,0.,1.));
#127686=DIRECTION('center_axis',(1.,0.,0.));
#127687=DIRECTION('ref_axis',(0.,0.,-1.));
#127688=DIRECTION('center_axis',(-1.,0.,0.));
#127689=DIRECTION('ref_axis',(0.,-3.56770963698181E-15,-1.));
#127690=DIRECTION('center_axis',(-1.,0.,0.));
#127691=DIRECTION('ref_axis',(0.,0.,-1.));
#127692=DIRECTION('center_axis',(-1.,0.,0.));
#127693=DIRECTION('ref_axis',(0.,-3.60526447526582E-15,-1.));
#127694=DIRECTION('center_axis',(-1.,0.,0.));
#127695=DIRECTION('ref_axis',(0.,1.20175482508861E-15,-1.));
#127696=DIRECTION('center_axis',(-1.,0.,0.));
#127697=DIRECTION('ref_axis',(0.,-1.20175482508861E-15,-1.));
#127698=DIRECTION('center_axis',(-1.,0.,0.));
#127699=DIRECTION('ref_axis',(0.,0.,-1.));
#127700=DIRECTION('center_axis',(-1.,0.,0.));
#127701=DIRECTION('ref_axis',(0.,0.,-1.));
#127702=DIRECTION('center_axis',(-1.,0.,0.));
#127703=DIRECTION('ref_axis',(0.,-1.20175482508861E-15,-1.));
#127704=DIRECTION('center_axis',(-1.,0.,0.));
#127705=DIRECTION('ref_axis',(0.,0.,-1.));
#127706=DIRECTION('center_axis',(-1.,0.,0.));
#127707=DIRECTION('ref_axis',(0.,0.,1.));
#127708=DIRECTION('',(-1.,0.,0.));
#127709=DIRECTION('center_axis',(-1.,0.,0.));
#127710=DIRECTION('ref_axis',(0.,0.,1.));
#127711=DIRECTION('',(-1.,0.,0.));
#127712=DIRECTION('center_axis',(-1.,0.,0.));
#127713=DIRECTION('ref_axis',(0.,0.,1.));
#127714=DIRECTION('center_axis',(-1.,0.,0.));
#127715=DIRECTION('ref_axis',(0.,0.,1.));
#127716=DIRECTION('',(-1.,0.,0.));
#127717=DIRECTION('center_axis',(-1.,0.,0.));
#127718=DIRECTION('ref_axis',(0.,-0.913545457642603,-0.406736643075796));
#127719=DIRECTION('center_axis',(-1.,0.,0.));
#127720=DIRECTION('ref_axis',(0.,0.,1.));
#127721=DIRECTION('center_axis',(-1.,0.,0.));
#127722=DIRECTION('ref_axis',(0.,0.,1.));
#127723=DIRECTION('center_axis',(-1.,0.,0.));
#127724=DIRECTION('ref_axis',(0.,0.,1.));
#127725=DIRECTION('center_axis',(-1.,0.,0.));
#127726=DIRECTION('ref_axis',(0.,0.,1.));
#127727=DIRECTION('center_axis',(-1.,0.,0.));
#127728=DIRECTION('ref_axis',(0.,0.160274827576825,-0.987072428773704));
#127729=DIRECTION('center_axis',(-1.,0.,0.));
#127730=DIRECTION('ref_axis',(0.,0.,1.));
#127731=DIRECTION('center_axis',(-1.,0.,0.));
#127732=DIRECTION('ref_axis',(0.,0.,1.));
#127733=DIRECTION('center_axis',(-1.,0.,0.));
#127734=DIRECTION('ref_axis',(0.,0.,1.));
#127735=DIRECTION('center_axis',(-1.,0.,0.));
#127736=DIRECTION('ref_axis',(0.,0.,1.));
#127737=DIRECTION('',(-1.,0.,0.));
#127738=DIRECTION('center_axis',(-1.,0.,0.));
#127739=DIRECTION('ref_axis',(0.,0.,1.));
#127740=DIRECTION('',(-1.,0.,0.));
#127741=DIRECTION('center_axis',(-1.,0.,0.));
#127742=DIRECTION('ref_axis',(0.,0.,1.));
#127743=DIRECTION('center_axis',(-1.,0.,0.));
#127744=DIRECTION('ref_axis',(0.,0.,1.));
#127745=DIRECTION('center_axis',(-1.,0.,0.));
#127746=DIRECTION('ref_axis',(0.,0.,1.));
#127747=DIRECTION('center_axis',(-1.,0.,0.));
#127748=DIRECTION('ref_axis',(0.,0.,1.));
#127749=DIRECTION('center_axis',(-1.,0.,0.));
#127750=DIRECTION('ref_axis',(0.,0.0484514595736587,-0.99882553835251));
#127751=DIRECTION('center_axis',(-1.,0.,0.));
#127752=DIRECTION('ref_axis',(0.,0.,1.));
#127753=DIRECTION('',(-1.,0.,0.));
#127754=DIRECTION('center_axis',(-1.,0.,0.));
#127755=DIRECTION('ref_axis',(0.,0.,1.));
#127756=DIRECTION('',(-1.,0.,0.));
#127757=DIRECTION('center_axis',(-1.,0.,0.));
#127758=DIRECTION('ref_axis',(0.,0.499999999999999,-0.866025403784439));
#127759=DIRECTION('center_axis',(-1.,0.,0.));
#127760=DIRECTION('ref_axis',(0.,0.,1.));
#127761=DIRECTION('',(-1.,0.,0.));
#127762=DIRECTION('center_axis',(-1.,0.,0.));
#127763=DIRECTION('ref_axis',(0.,0.,1.));
#127764=DIRECTION('',(-1.,0.,0.));
#127765=DIRECTION('center_axis',(-1.,0.,0.));
#127766=DIRECTION('ref_axis',(0.,0.,1.));
#127767=DIRECTION('center_axis',(-1.,0.,0.));
#127768=DIRECTION('ref_axis',(0.,0.,1.));
#127769=DIRECTION('',(-1.,0.,0.));
#127770=DIRECTION('center_axis',(-1.,0.,0.));
#127771=DIRECTION('ref_axis',(0.,0.809016994374948,-0.587785252292472));
#127772=DIRECTION('center_axis',(-1.,0.,0.));
#127773=DIRECTION('ref_axis',(0.,0.,1.));
#127774=DIRECTION('',(-1.,0.,0.));
#127775=DIRECTION('center_axis',(-1.,0.,0.));
#127776=DIRECTION('ref_axis',(0.,0.,1.));
#127777=DIRECTION('',(-1.,0.,0.));
#127778=DIRECTION('center_axis',(-1.,0.,0.));
#127779=DIRECTION('ref_axis',(0.,-0.669130606358862,-0.743144825477391));
#127780=DIRECTION('center_axis',(-1.,0.,0.));
#127781=DIRECTION('ref_axis',(0.,0.,1.));
#127782=DIRECTION('',(-1.,0.,0.));
#127783=DIRECTION('center_axis',(-1.,0.,0.));
#127784=DIRECTION('ref_axis',(0.,0.,1.));
#127785=DIRECTION('',(-1.,0.,0.));
#127786=DIRECTION('center_axis',(-1.,0.,0.));
#127787=DIRECTION('ref_axis',(0.,-0.309016994374949,-0.951056516295153));
#127788=DIRECTION('center_axis',(-1.,0.,0.));
#127789=DIRECTION('ref_axis',(0.,0.,1.));
#127790=DIRECTION('',(-1.,0.,0.));
#127791=DIRECTION('center_axis',(-1.,0.,0.));
#127792=DIRECTION('ref_axis',(0.,0.,1.));
#127793=DIRECTION('',(-1.,0.,0.));
#127794=DIRECTION('center_axis',(-1.,0.,0.));
#127795=DIRECTION('ref_axis',(0.,0.104528463267655,-0.994521895368273));
#127796=DIRECTION('center_axis',(0.,-1.,0.));
#127797=DIRECTION('ref_axis',(0.,0.,-1.));
#127798=DIRECTION('',(-1.,0.,0.));
#127799=DIRECTION('',(-1.,0.,0.));
#127800=DIRECTION('center_axis',(0.,0.,1.));
#127801=DIRECTION('ref_axis',(1.,0.,0.));
#127802=DIRECTION('center_axis',(0.,0.,-1.));
#127803=DIRECTION('ref_axis',(-1.,0.,0.));
#127804=DIRECTION('center_axis',(1.,0.,0.));
#127805=DIRECTION('ref_axis',(0.,0.,-1.));
#127806=DIRECTION('center_axis',(-1.,0.,0.));
#127807=DIRECTION('ref_axis',(0.,0.,-1.));
#127808=DIRECTION('',(1.,0.,0.));
#127809=DIRECTION('center_axis',(1.,0.,0.));
#127810=DIRECTION('ref_axis',(0.,0.,-1.));
#127811=DIRECTION('center_axis',(1.,0.,0.));
#127812=DIRECTION('ref_axis',(0.,-1.,1.83697019872103E-16));
#127813=DIRECTION('center_axis',(-1.,0.,0.));
#127814=DIRECTION('ref_axis',(0.,8.89160511826737E-16,-1.));
#127815=DIRECTION('',(1.,0.,0.));
#127816=DIRECTION('center_axis',(1.,0.,0.));
#127817=DIRECTION('ref_axis',(0.,0.,-1.));
#127818=DIRECTION('',(1.,0.,0.));
#127819=DIRECTION('center_axis',(0.,0.,-1.));
#127820=DIRECTION('ref_axis',(-1.,0.,0.));
#127821=DIRECTION('',(0.,-1.,0.));
#127822=DIRECTION('',(1.,0.,0.));
#127823=DIRECTION('',(0.,1.,0.));
#127824=DIRECTION('center_axis',(0.,1.,0.));
#127825=DIRECTION('ref_axis',(0.,0.,1.));
#127826=DIRECTION('',(0.,0.,-1.));
#127827=DIRECTION('',(1.,0.,0.));
#127828=DIRECTION('',(0.,0.,1.));
#127829=DIRECTION('center_axis',(0.,0.,1.));
#127830=DIRECTION('ref_axis',(1.,0.,0.));
#127831=DIRECTION('',(0.,1.,0.));
#127832=DIRECTION('',(0.,-1.,0.));
#127833=DIRECTION('center_axis',(1.,0.,0.));
#127834=DIRECTION('ref_axis',(0.,0.,-1.));
#127835=DIRECTION('center_axis',(1.,0.,0.));
#127836=DIRECTION('ref_axis',(0.,0.,-1.));
#127837=DIRECTION('axis',(0.,0.,1.));
#127838=DIRECTION('refdir',(1.,0.,0.));
#127839=DIRECTION('center_axis',(1.,0.,0.));
#127840=DIRECTION('ref_axis',(0.,0.,-1.));
#127841=DIRECTION('center_axis',(1.,0.,0.));
#127842=DIRECTION('ref_axis',(0.,0.,-1.));
#127843=DIRECTION('center_axis',(0.,1.,8.58242907100461E-17));
#127844=DIRECTION('ref_axis',(0.,-8.58242907100461E-17,1.));
#127845=DIRECTION('center_axis',(-1.,0.,0.));
#127846=DIRECTION('ref_axis',(0.,0.,-1.));
#127847=DIRECTION('center_axis',(1.,0.,0.));
#127848=DIRECTION('ref_axis',(0.,0.,-1.));
#127849=DIRECTION('',(-1.,0.,0.));
#127850=DIRECTION('center_axis',(-1.,0.,0.));
#127851=DIRECTION('ref_axis',(0.,0.,1.));
#127852=DIRECTION('center_axis',(-1.,0.,0.));
#127853=DIRECTION('ref_axis',(0.,0.,1.));
#127854=DIRECTION('',(-1.,0.,0.));
#127855=DIRECTION('',(-1.,0.,0.));
#127856=DIRECTION('center_axis',(-1.,0.,0.));
#127857=DIRECTION('ref_axis',(0.,0.,1.));
#127858=DIRECTION('',(-1.,0.,0.));
#127859=DIRECTION('',(1.,0.,0.));
#127860=DIRECTION('center_axis',(-1.,0.,0.));
#127861=DIRECTION('ref_axis',(0.,0.,1.));
#127862=DIRECTION('center_axis',(1.,0.,0.));
#127863=DIRECTION('ref_axis',(0.,0.994521895368274,-0.104528463267644));
#127864=DIRECTION('',(-1.,0.,0.));
#127865=DIRECTION('center_axis',(-1.,0.,0.));
#127866=DIRECTION('ref_axis',(0.,0.,-1.));
#127867=DIRECTION('',(-1.,0.,0.));
#127868=DIRECTION('center_axis',(-1.,0.,0.));
#127869=DIRECTION('ref_axis',(0.,0.,1.));
#127870=DIRECTION('center_axis',(1.,0.,0.));
#127871=DIRECTION('ref_axis',(0.,0.951056516295157,-0.309016994374938));
#127872=DIRECTION('',(-1.,0.,0.));
#127873=DIRECTION('center_axis',(-1.,0.,0.));
#127874=DIRECTION('ref_axis',(0.,-2.06015112872333E-15,-1.));
#127875=DIRECTION('',(-1.,0.,0.));
#127876=DIRECTION('center_axis',(-1.,0.,0.));
#127877=DIRECTION('ref_axis',(0.,0.,1.));
#127878=DIRECTION('center_axis',(1.,0.,0.));
#127879=DIRECTION('ref_axis',(0.,0.743144825477399,-0.669130606358852));
#127880=DIRECTION('',(-1.,0.,0.));
#127881=DIRECTION('center_axis',(-1.,0.,0.));
#127882=DIRECTION('ref_axis',(0.,0.,-1.));
#127883=DIRECTION('',(-1.,0.,0.));
#127884=DIRECTION('center_axis',(-1.,0.,0.));
#127885=DIRECTION('ref_axis',(0.,0.,1.));
#127886=DIRECTION('center_axis',(1.,0.,0.));
#127887=DIRECTION('ref_axis',(0.,0.866025403784443,-0.499999999999993));
#127888=DIRECTION('',(-1.,0.,0.));
#127889=DIRECTION('center_axis',(-1.,0.,0.));
#127890=DIRECTION('ref_axis',(0.,0.,-1.));
#127891=DIRECTION('',(-1.,0.,0.));
#127892=DIRECTION('center_axis',(-1.,0.,0.));
#127893=DIRECTION('ref_axis',(0.,0.,1.));
#127894=DIRECTION('',(-1.,0.,0.));
#127895=DIRECTION('center_axis',(-1.,0.,0.));
#127896=DIRECTION('ref_axis',(0.,4.12030225744667E-15,-1.));
#127897=DIRECTION('',(-1.,0.,0.));
#127898=DIRECTION('center_axis',(1.,0.,0.));
#127899=DIRECTION('ref_axis',(0.,0.406736643075806,-0.913545457642598));
#127900=DIRECTION('center_axis',(-1.,0.,0.));
#127901=DIRECTION('ref_axis',(0.,0.,1.));
#127902=DIRECTION('',(-1.,0.,0.));
#127903=DIRECTION('center_axis',(-1.,0.,0.));
#127904=DIRECTION('ref_axis',(0.,0.,-1.));
#127905=DIRECTION('',(-1.,0.,0.));
#127906=DIRECTION('center_axis',(1.,0.,0.));
#127907=DIRECTION('ref_axis',(0.,0.58778525229248,-0.809016994374943));
#127908=DIRECTION('center_axis',(-1.,0.,0.));
#127909=DIRECTION('ref_axis',(0.,0.,1.));
#127910=DIRECTION('center_axis',(1.,0.,0.));
#127911=DIRECTION('ref_axis',(0.,0.587785252292463,0.809016994374955));
#127912=DIRECTION('',(-1.,0.,0.));
#127913=DIRECTION('center_axis',(-1.,0.,0.));
#127914=DIRECTION('ref_axis',(0.,0.,-1.));
#127915=DIRECTION('',(-1.,0.,0.));
#127916=DIRECTION('center_axis',(-1.,0.,0.));
#127917=DIRECTION('ref_axis',(0.,0.,1.));
#127918=DIRECTION('center_axis',(1.,0.,0.));
#127919=DIRECTION('ref_axis',(0.,0.743144825477386,0.669130606358867));
#127920=DIRECTION('',(-1.,0.,0.));
#127921=DIRECTION('center_axis',(-1.,0.,0.));
#127922=DIRECTION('ref_axis',(0.,0.,-1.));
#127923=DIRECTION('',(-1.,0.,0.));
#127924=DIRECTION('center_axis',(-1.,0.,0.));
#127925=DIRECTION('ref_axis',(0.,0.,1.));
#127926=DIRECTION('center_axis',(1.,0.,0.));
#127927=DIRECTION('ref_axis',(0.,0.406736643075789,0.913545457642606));
#127928=DIRECTION('',(-1.,0.,0.));
#127929=DIRECTION('center_axis',(-1.,0.,0.));
#127930=DIRECTION('ref_axis',(0.,0.,-1.));
#127931=DIRECTION('',(-1.,0.,0.));
#127932=DIRECTION('center_axis',(-1.,0.,0.));
#127933=DIRECTION('ref_axis',(0.,0.,1.));
#127934=DIRECTION('center_axis',(1.,0.,0.));
#127935=DIRECTION('ref_axis',(0.,0.866025403784433,0.50000000000001));
#127936=DIRECTION('',(-1.,0.,0.));
#127937=DIRECTION('center_axis',(-1.,0.,0.));
#127938=DIRECTION('ref_axis',(0.,0.,-1.));
#127939=DIRECTION('',(-1.,0.,0.));
#127940=DIRECTION('center_axis',(-1.,0.,0.));
#127941=DIRECTION('ref_axis',(0.,0.,1.));
#127942=DIRECTION('center_axis',(1.,0.,0.));
#127943=DIRECTION('ref_axis',(0.,0.951056516295151,0.309016994374957));
#127944=DIRECTION('',(-1.,0.,0.));
#127945=DIRECTION('center_axis',(-1.,0.,0.));
#127946=DIRECTION('ref_axis',(0.,0.,-1.));
#127947=DIRECTION('',(-1.,0.,0.));
#127948=DIRECTION('center_axis',(-1.,0.,0.));
#127949=DIRECTION('ref_axis',(0.,0.,1.));
#127950=DIRECTION('center_axis',(1.,0.,0.));
#127951=DIRECTION('ref_axis',(0.,0.994521895368272,0.104528463267663));
#127952=DIRECTION('',(-1.,0.,0.));
#127953=DIRECTION('center_axis',(-1.,0.,0.));
#127954=DIRECTION('ref_axis',(0.,3.60526447526583E-15,-1.));
#127955=DIRECTION('',(-1.,0.,0.));
#127956=DIRECTION('center_axis',(-1.,0.,0.));
#127957=DIRECTION('ref_axis',(0.,0.,1.));
#127958=DIRECTION('center_axis',(-1.,0.,0.));
#127959=DIRECTION('ref_axis',(0.,0.,1.));
#127960=DIRECTION('center_axis',(-1.,0.,0.));
#127961=DIRECTION('ref_axis',(0.,0.,1.));
#127962=DIRECTION('center_axis',(-1.,0.,0.));
#127963=DIRECTION('ref_axis',(0.,0.,1.));
#127964=DIRECTION('center_axis',(-1.,0.,0.));
#127965=DIRECTION('ref_axis',(0.,0.,1.));
#127966=DIRECTION('',(1.,0.,0.));
#127967=DIRECTION('',(-1.,0.,0.));
#127968=DIRECTION('center_axis',(-1.,0.,0.));
#127969=DIRECTION('ref_axis',(0.,0.,1.));
#127970=DIRECTION('center_axis',(-1.,0.,0.));
#127971=DIRECTION('ref_axis',(0.,0.,1.));
#127972=DIRECTION('center_axis',(-1.,0.,0.));
#127973=DIRECTION('ref_axis',(0.,-1.,-1.83697019872103E-16));
#127974=DIRECTION('center_axis',(1.,0.,0.));
#127975=DIRECTION('ref_axis',(0.,0.,1.));
#127976=DIRECTION('',(-1.,0.,0.));
#127977=DIRECTION('center_axis',(1.,0.,0.));
#127978=DIRECTION('ref_axis',(0.,0.,1.));
#127979=DIRECTION('',(1.,0.,0.));
#127980=DIRECTION('center_axis',(-1.,0.,0.));
#127981=DIRECTION('ref_axis',(0.,0.,1.));
#127982=DIRECTION('center_axis',(1.,0.,0.));
#127983=DIRECTION('ref_axis',(0.,-0.994521895368273,-0.104528463267657));
#127984=DIRECTION('center_axis',(-1.,0.,0.));
#127985=DIRECTION('ref_axis',(0.,0.,1.));
#127986=DIRECTION('center_axis',(1.,0.,0.));
#127987=DIRECTION('ref_axis',(0.,-0.951056516295153,-0.30901699437495));
#127988=DIRECTION('center_axis',(-1.,0.,0.));
#127989=DIRECTION('ref_axis',(0.,0.,1.));
#127990=DIRECTION('center_axis',(1.,0.,0.));
#127991=DIRECTION('ref_axis',(0.,-0.866025403784437,-0.500000000000003));
#127992=DIRECTION('center_axis',(-1.,0.,0.));
#127993=DIRECTION('ref_axis',(0.,0.,1.));
#127994=DIRECTION('center_axis',(1.,0.,0.));
#127995=DIRECTION('ref_axis',(0.,-0.74314482547739,-0.669130606358862));
#127996=DIRECTION('center_axis',(-1.,0.,0.));
#127997=DIRECTION('ref_axis',(0.,0.,1.));
#127998=DIRECTION('center_axis',(1.,0.,0.));
#127999=DIRECTION('ref_axis',(0.,-0.587785252292469,-0.80901699437495));
#128000=DIRECTION('center_axis',(-1.,0.,0.));
#128001=DIRECTION('ref_axis',(0.,0.,1.));
#128002=DIRECTION('center_axis',(1.,0.,0.));
#128003=DIRECTION('ref_axis',(0.,-0.406736643075793,-0.913545457642604));
#128004=DIRECTION('center_axis',(-1.,0.,0.));
#128005=DIRECTION('ref_axis',(0.,0.,1.));
#128006=DIRECTION('center_axis',(1.,0.,0.));
#128007=DIRECTION('ref_axis',(0.,-0.207911690817753,-0.978147600733807));
#128008=DIRECTION('center_axis',(-1.,0.,0.));
#128009=DIRECTION('ref_axis',(0.,0.,1.));
#128010=DIRECTION('center_axis',(1.,0.,0.));
#128011=DIRECTION('ref_axis',(0.,8.24060451489334E-15,-1.));
#128012=DIRECTION('center_axis',(-1.,0.,0.));
#128013=DIRECTION('ref_axis',(0.,0.,1.));
#128014=DIRECTION('center_axis',(1.,0.,0.));
#128015=DIRECTION('ref_axis',(0.,0.207911690817766,-0.978147600733804));
#128016=DIRECTION('center_axis',(-1.,0.,0.));
#128017=DIRECTION('ref_axis',(0.,0.,1.));
#128018=DIRECTION('center_axis',(-1.,0.,0.));
#128019=DIRECTION('ref_axis',(0.,0.,1.));
#128020=DIRECTION('center_axis',(-1.,0.,0.));
#128021=DIRECTION('ref_axis',(0.,0.,1.));
#128022=DIRECTION('center_axis',(-1.,0.,0.));
#128023=DIRECTION('ref_axis',(0.,0.,1.));
#128024=DIRECTION('center_axis',(-1.,0.,0.));
#128025=DIRECTION('ref_axis',(0.,0.,1.));
#128026=DIRECTION('center_axis',(-1.,0.,0.));
#128027=DIRECTION('ref_axis',(0.,0.,1.));
#128028=DIRECTION('center_axis',(-1.,0.,0.));
#128029=DIRECTION('ref_axis',(0.,0.,1.));
#128030=DIRECTION('center_axis',(-1.,0.,0.));
#128031=DIRECTION('ref_axis',(0.,0.,1.));
#128032=DIRECTION('center_axis',(-1.,0.,0.));
#128033=DIRECTION('ref_axis',(0.,0.,1.));
#128034=DIRECTION('center_axis',(-1.,0.,0.));
#128035=DIRECTION('ref_axis',(0.,0.,1.));
#128036=DIRECTION('center_axis',(-1.,0.,0.));
#128037=DIRECTION('ref_axis',(0.,0.,1.));
#128038=DIRECTION('center_axis',(-1.,0.,0.));
#128039=DIRECTION('ref_axis',(0.,0.,1.));
#128040=DIRECTION('center_axis',(-1.,0.,0.));
#128041=DIRECTION('ref_axis',(0.,0.,1.));
#128042=DIRECTION('center_axis',(1.,0.,0.));
#128043=DIRECTION('ref_axis',(0.,0.207911690817747,0.978147600733808));
#128044=DIRECTION('center_axis',(-1.,0.,0.));
#128045=DIRECTION('ref_axis',(0.,0.,1.));
#128046=DIRECTION('center_axis',(1.,0.,0.));
#128047=DIRECTION('ref_axis',(0.,0.,1.));
#128048=DIRECTION('center_axis',(-1.,0.,0.));
#128049=DIRECTION('ref_axis',(0.,0.,1.));
#128050=DIRECTION('center_axis',(1.,0.,0.));
#128051=DIRECTION('ref_axis',(0.,-0.20791169081776,0.978147600733806));
#128052=DIRECTION('center_axis',(-1.,0.,0.));
#128053=DIRECTION('ref_axis',(0.,0.,1.));
#128054=DIRECTION('center_axis',(1.,0.,0.));
#128055=DIRECTION('ref_axis',(0.,-0.406736643075801,0.9135454576426));
#128056=DIRECTION('center_axis',(-1.,0.,0.));
#128057=DIRECTION('ref_axis',(0.,0.,1.));
#128058=DIRECTION('center_axis',(1.,0.,0.));
#128059=DIRECTION('ref_axis',(0.,-0.587785252292474,0.809016994374947));
#128060=DIRECTION('center_axis',(-1.,0.,0.));
#128061=DIRECTION('ref_axis',(0.,0.,1.));
#128062=DIRECTION('center_axis',(1.,0.,0.));
#128063=DIRECTION('ref_axis',(0.,-0.743144825477395,0.669130606358857));
#128064=DIRECTION('center_axis',(-1.,0.,0.));
#128065=DIRECTION('ref_axis',(0.,0.,1.));
#128066=DIRECTION('center_axis',(1.,0.,0.));
#128067=DIRECTION('ref_axis',(0.,-0.866025403784439,0.499999999999999));
#128068=DIRECTION('center_axis',(-1.,0.,0.));
#128069=DIRECTION('ref_axis',(0.,0.,1.));
#128070=DIRECTION('center_axis',(1.,0.,0.));
#128071=DIRECTION('ref_axis',(0.,-0.951056516295155,0.309016994374944));
#128072=DIRECTION('center_axis',(-1.,0.,0.));
#128073=DIRECTION('ref_axis',(0.,0.,1.));
#128074=DIRECTION('center_axis',(1.,0.,0.));
#128075=DIRECTION('ref_axis',(0.,-0.994521895368274,0.104528463267651));
#128076=DIRECTION('',(0.,1.,0.));
#128077=DIRECTION('',(0.,-1.,0.));
#128078=DIRECTION('',(0.,0.,1.));
#128079=DIRECTION('center_axis',(-1.,0.,0.));
#128080=DIRECTION('ref_axis',(0.,0.,1.));
#128081=DIRECTION('',(0.,1.,0.));
#128082=DIRECTION('',(0.,0.,1.));
#128083=DIRECTION('',(0.,-1.,0.));
#128084=DIRECTION('center_axis',(-1.,0.,0.));
#128085=DIRECTION('ref_axis',(0.,0.,1.));
#128086=DIRECTION('center_axis',(-1.,0.,0.));
#128087=DIRECTION('ref_axis',(0.,0.,1.));
#128088=DIRECTION('center_axis',(-1.,0.,0.));
#128089=DIRECTION('ref_axis',(0.,0.,1.));
#128090=DIRECTION('center_axis',(-1.,0.,0.));
#128091=DIRECTION('ref_axis',(0.,0.,1.));
#128092=DIRECTION('center_axis',(-1.,0.,0.));
#128093=DIRECTION('ref_axis',(0.,0.,1.));
#128094=DIRECTION('center_axis',(-1.,0.,0.));
#128095=DIRECTION('ref_axis',(0.,0.,1.));
#128096=DIRECTION('center_axis',(-1.,0.,0.));
#128097=DIRECTION('ref_axis',(0.,0.,1.));
#128098=DIRECTION('center_axis',(-1.,0.,0.));
#128099=DIRECTION('ref_axis',(0.,0.,1.));
#128100=DIRECTION('center_axis',(-1.,0.,0.));
#128101=DIRECTION('ref_axis',(0.,0.,1.));
#128102=DIRECTION('center_axis',(-1.,0.,0.));
#128103=DIRECTION('ref_axis',(0.,0.,1.));
#128104=DIRECTION('center_axis',(-1.,0.,0.));
#128105=DIRECTION('ref_axis',(0.,0.,1.));
#128106=DIRECTION('center_axis',(-1.,0.,0.));
#128107=DIRECTION('ref_axis',(0.,0.,1.));
#128108=DIRECTION('center_axis',(-1.,0.,0.));
#128109=DIRECTION('ref_axis',(0.,0.,1.));
#128110=DIRECTION('center_axis',(-1.,0.,0.));
#128111=DIRECTION('ref_axis',(0.,0.,1.));
#128112=DIRECTION('center_axis',(-1.,0.,0.));
#128113=DIRECTION('ref_axis',(0.,0.,1.));
#128114=DIRECTION('center_axis',(-1.,0.,0.));
#128115=DIRECTION('ref_axis',(0.,0.,1.));
#128116=DIRECTION('center_axis',(-1.,0.,0.));
#128117=DIRECTION('ref_axis',(0.,0.,1.));
#128118=DIRECTION('center_axis',(-1.,0.,0.));
#128119=DIRECTION('ref_axis',(0.,0.,1.));
#128120=DIRECTION('center_axis',(-1.,0.,0.));
#128121=DIRECTION('ref_axis',(0.,0.,1.));
#128122=DIRECTION('center_axis',(-1.,0.,0.));
#128123=DIRECTION('ref_axis',(0.,0.,1.));
#128124=DIRECTION('center_axis',(-1.,0.,0.));
#128125=DIRECTION('ref_axis',(0.,0.,1.));
#128126=DIRECTION('center_axis',(-1.,0.,0.));
#128127=DIRECTION('ref_axis',(0.,0.,1.));
#128128=DIRECTION('center_axis',(-1.,0.,0.));
#128129=DIRECTION('ref_axis',(0.,0.,1.));
#128130=DIRECTION('center_axis',(-1.,0.,0.));
#128131=DIRECTION('ref_axis',(0.,0.,1.));
#128132=DIRECTION('center_axis',(-1.,0.,0.));
#128133=DIRECTION('ref_axis',(0.,0.,1.));
#128134=DIRECTION('center_axis',(-1.,0.,0.));
#128135=DIRECTION('ref_axis',(0.,0.,1.));
#128136=DIRECTION('center_axis',(-1.,0.,0.));
#128137=DIRECTION('ref_axis',(0.,0.,1.));
#128138=DIRECTION('center_axis',(-1.,0.,0.));
#128139=DIRECTION('ref_axis',(0.,0.,1.));
#128140=DIRECTION('center_axis',(-1.,0.,0.));
#128141=DIRECTION('ref_axis',(0.,9.62924104759778E-15,-1.));
#128142=DIRECTION('center_axis',(-1.,0.,0.));
#128143=DIRECTION('ref_axis',(0.,0.,1.));
#128144=DIRECTION('center_axis',(-1.,0.,0.));
#128145=DIRECTION('ref_axis',(0.,0.,1.));
#128146=DIRECTION('center_axis',(-1.,0.,0.));
#128147=DIRECTION('ref_axis',(0.,0.,1.));
#128148=DIRECTION('center_axis',(-1.,0.,0.));
#128149=DIRECTION('ref_axis',(0.,0.,1.));
#128150=DIRECTION('center_axis',(-1.,0.,0.));
#128151=DIRECTION('ref_axis',(0.,0.,1.));
#128152=DIRECTION('center_axis',(-1.,0.,0.));
#128153=DIRECTION('ref_axis',(0.,0.,1.));
#128154=DIRECTION('center_axis',(-1.,0.,0.));
#128155=DIRECTION('ref_axis',(0.,0.,1.));
#128156=DIRECTION('center_axis',(-1.,0.,0.));
#128157=DIRECTION('ref_axis',(0.,0.,1.));
#128158=DIRECTION('center_axis',(-1.,0.,0.));
#128159=DIRECTION('ref_axis',(0.,0.,1.));
#128160=DIRECTION('center_axis',(-1.,0.,0.));
#128161=DIRECTION('ref_axis',(0.,0.,1.));
#128162=DIRECTION('center_axis',(-1.,0.,0.));
#128163=DIRECTION('ref_axis',(0.,0.,1.));
#128164=DIRECTION('center_axis',(-1.,0.,0.));
#128165=DIRECTION('ref_axis',(0.,0.,1.));
#128166=DIRECTION('center_axis',(-1.,0.,0.));
#128167=DIRECTION('ref_axis',(0.,0.,1.));
#128168=DIRECTION('center_axis',(-1.,0.,0.));
#128169=DIRECTION('ref_axis',(0.,0.,1.));
#128170=DIRECTION('center_axis',(-1.,0.,0.));
#128171=DIRECTION('ref_axis',(0.,0.,1.));
#128172=DIRECTION('center_axis',(-1.,0.,0.));
#128173=DIRECTION('ref_axis',(0.,0.,1.));
#128174=DIRECTION('center_axis',(-1.,0.,0.));
#128175=DIRECTION('ref_axis',(0.,0.,1.));
#128176=DIRECTION('center_axis',(-1.,0.,0.));
#128177=DIRECTION('ref_axis',(0.,0.,1.));
#128178=DIRECTION('center_axis',(-1.,0.,0.));
#128179=DIRECTION('ref_axis',(0.,0.,1.));
#128180=DIRECTION('center_axis',(-1.,0.,0.));
#128181=DIRECTION('ref_axis',(0.,0.,1.));
#128182=DIRECTION('center_axis',(-1.,0.,0.));
#128183=DIRECTION('ref_axis',(0.,0.,1.));
#128184=DIRECTION('center_axis',(-1.,0.,0.));
#128185=DIRECTION('ref_axis',(0.,0.,1.));
#128186=DIRECTION('center_axis',(-1.,0.,0.));
#128187=DIRECTION('ref_axis',(0.,0.,1.));
#128188=DIRECTION('center_axis',(-1.,0.,0.));
#128189=DIRECTION('ref_axis',(0.,0.,1.));
#128190=DIRECTION('center_axis',(-1.,0.,0.));
#128191=DIRECTION('ref_axis',(0.,0.,1.));
#128192=DIRECTION('center_axis',(-1.,0.,0.));
#128193=DIRECTION('ref_axis',(0.,0.,1.));
#128194=DIRECTION('center_axis',(-1.,0.,0.));
#128195=DIRECTION('ref_axis',(0.,0.,1.));
#128196=DIRECTION('center_axis',(-1.,0.,0.));
#128197=DIRECTION('ref_axis',(0.,0.,1.));
#128198=DIRECTION('',(1.,0.,0.));
#128199=DIRECTION('center_axis',(-1.,0.,0.));
#128200=DIRECTION('ref_axis',(0.,0.,1.));
#128201=DIRECTION('',(-1.,0.,0.));
#128202=DIRECTION('center_axis',(-1.,0.,0.));
#128203=DIRECTION('ref_axis',(0.,0.,1.));
#128204=DIRECTION('',(-1.,0.,0.));
#128205=DIRECTION('',(1.,0.,0.));
#128206=DIRECTION('center_axis',(-1.,0.,0.));
#128207=DIRECTION('ref_axis',(0.,0.,1.));
#128208=DIRECTION('center_axis',(-1.,0.,0.));
#128209=DIRECTION('ref_axis',(0.,0.,1.));
#128210=DIRECTION('',(-1.,0.,0.));
#128211=DIRECTION('',(1.,0.,0.));
#128212=DIRECTION('center_axis',(-1.,0.,0.));
#128213=DIRECTION('ref_axis',(0.,0.,1.));
#128214=DIRECTION('center_axis',(-1.,0.,0.));
#128215=DIRECTION('ref_axis',(0.,0.,1.));
#128216=DIRECTION('',(-1.,0.,0.));
#128217=DIRECTION('',(1.,0.,0.));
#128218=DIRECTION('center_axis',(-1.,0.,0.));
#128219=DIRECTION('ref_axis',(0.,0.,1.));
#128220=DIRECTION('center_axis',(-1.,0.,0.));
#128221=DIRECTION('ref_axis',(0.,0.,1.));
#128222=DIRECTION('',(1.,0.,0.));
#128223=DIRECTION('center_axis',(-1.,0.,0.));
#128224=DIRECTION('ref_axis',(0.,0.,1.));
#128225=DIRECTION('',(-1.,0.,0.));
#128226=DIRECTION('center_axis',(-1.,0.,0.));
#128227=DIRECTION('ref_axis',(0.,0.,1.));
#128228=DIRECTION('',(1.,0.,0.));
#128229=DIRECTION('center_axis',(-1.,0.,0.));
#128230=DIRECTION('ref_axis',(0.,0.,1.));
#128231=DIRECTION('center_axis',(-1.,0.,0.));
#128232=DIRECTION('ref_axis',(0.,0.,1.));
#128233=DIRECTION('',(-1.,0.,0.));
#128234=DIRECTION('',(1.,0.,0.));
#128235=DIRECTION('center_axis',(-1.,0.,0.));
#128236=DIRECTION('ref_axis',(0.,0.,1.));
#128237=DIRECTION('center_axis',(-1.,0.,0.));
#128238=DIRECTION('ref_axis',(0.,0.,1.));
#128239=DIRECTION('',(1.,0.,0.));
#128240=DIRECTION('center_axis',(-1.,0.,0.));
#128241=DIRECTION('ref_axis',(0.,0.,1.));
#128242=DIRECTION('',(-1.,0.,0.));
#128243=DIRECTION('center_axis',(-1.,0.,0.));
#128244=DIRECTION('ref_axis',(0.,0.,1.));
#128245=DIRECTION('',(-1.,0.,0.));
#128246=DIRECTION('',(1.,0.,0.));
#128247=DIRECTION('center_axis',(-1.,0.,0.));
#128248=DIRECTION('ref_axis',(0.,0.,1.));
#128249=DIRECTION('center_axis',(-1.,0.,0.));
#128250=DIRECTION('ref_axis',(0.,0.,1.));
#128251=DIRECTION('',(-1.,0.,0.));
#128252=DIRECTION('center_axis',(-1.,0.,0.));
#128253=DIRECTION('ref_axis',(0.,0.,1.));
#128254=DIRECTION('center_axis',(-1.,0.,0.));
#128255=DIRECTION('ref_axis',(0.,0.,1.));
#128256=DIRECTION('',(1.,0.,0.));
#128257=DIRECTION('center_axis',(-1.,0.,0.));
#128258=DIRECTION('ref_axis',(0.,0.,1.));
#128259=DIRECTION('',(-1.,0.,0.));
#128260=DIRECTION('center_axis',(-1.,0.,0.));
#128261=DIRECTION('ref_axis',(0.,0.,1.));
#128262=DIRECTION('',(-1.,0.,0.));
#128263=DIRECTION('',(1.,0.,0.));
#128264=DIRECTION('center_axis',(-1.,0.,0.));
#128265=DIRECTION('ref_axis',(0.,0.,1.));
#128266=DIRECTION('center_axis',(-1.,0.,0.));
#128267=DIRECTION('ref_axis',(0.,0.,1.));
#128268=DIRECTION('',(1.,0.,0.));
#128269=DIRECTION('center_axis',(-1.,0.,0.));
#128270=DIRECTION('ref_axis',(0.,0.,1.));
#128271=DIRECTION('',(-1.,0.,0.));
#128272=DIRECTION('center_axis',(-1.,0.,0.));
#128273=DIRECTION('ref_axis',(0.,0.,1.));
#128274=DIRECTION('',(-1.,0.,0.));
#128275=DIRECTION('',(1.,0.,0.));
#128276=DIRECTION('center_axis',(-1.,0.,0.));
#128277=DIRECTION('ref_axis',(0.,0.,1.));
#128278=DIRECTION('center_axis',(-1.,0.,0.));
#128279=DIRECTION('ref_axis',(0.,9.64749793678664E-15,-1.));
#128280=DIRECTION('',(1.,0.,0.));
#128281=DIRECTION('center_axis',(-1.,0.,0.));
#128282=DIRECTION('ref_axis',(0.,0.,1.));
#128283=DIRECTION('',(-1.,0.,0.));
#128284=DIRECTION('center_axis',(-1.,0.,0.));
#128285=DIRECTION('ref_axis',(0.,0.,1.));
#128286=DIRECTION('',(-1.,0.,0.));
#128287=DIRECTION('',(1.,0.,0.));
#128288=DIRECTION('center_axis',(-1.,0.,0.));
#128289=DIRECTION('ref_axis',(0.,0.,1.));
#128290=DIRECTION('center_axis',(-1.,0.,0.));
#128291=DIRECTION('ref_axis',(0.,0.,1.));
#128292=DIRECTION('',(-1.,0.,0.));
#128293=DIRECTION('',(1.,0.,0.));
#128294=DIRECTION('center_axis',(-1.,0.,0.));
#128295=DIRECTION('ref_axis',(0.,0.,1.));
#128296=DIRECTION('center_axis',(-1.,0.,0.));
#128297=DIRECTION('ref_axis',(0.,0.,1.));
#128298=DIRECTION('',(1.,0.,0.));
#128299=DIRECTION('center_axis',(-1.,0.,0.));
#128300=DIRECTION('ref_axis',(0.,0.,1.));
#128301=DIRECTION('',(-1.,0.,0.));
#128302=DIRECTION('center_axis',(-1.,0.,0.));
#128303=DIRECTION('ref_axis',(0.,0.,1.));
#128304=DIRECTION('',(-1.,0.,0.));
#128305=DIRECTION('',(1.,0.,0.));
#128306=DIRECTION('center_axis',(-1.,0.,0.));
#128307=DIRECTION('ref_axis',(0.,0.,1.));
#128308=DIRECTION('center_axis',(-1.,0.,0.));
#128309=DIRECTION('ref_axis',(0.,0.,1.));
#128310=DIRECTION('',(1.,0.,0.));
#128311=DIRECTION('center_axis',(-1.,0.,0.));
#128312=DIRECTION('ref_axis',(0.,0.,1.));
#128313=DIRECTION('',(-1.,0.,0.));
#128314=DIRECTION('center_axis',(-1.,0.,0.));
#128315=DIRECTION('ref_axis',(0.,0.,1.));
#128316=DIRECTION('',(-1.,0.,0.));
#128317=DIRECTION('',(1.,0.,0.));
#128318=DIRECTION('center_axis',(-1.,0.,0.));
#128319=DIRECTION('ref_axis',(0.,0.,1.));
#128320=DIRECTION('center_axis',(-1.,0.,0.));
#128321=DIRECTION('ref_axis',(0.,0.,1.));
#128322=DIRECTION('',(1.,0.,0.));
#128323=DIRECTION('center_axis',(-1.,0.,0.));
#128324=DIRECTION('ref_axis',(0.,0.,1.));
#128325=DIRECTION('',(-1.,0.,0.));
#128326=DIRECTION('center_axis',(-1.,0.,0.));
#128327=DIRECTION('ref_axis',(0.,0.,1.));
#128328=DIRECTION('',(-1.,0.,0.));
#128329=DIRECTION('',(1.,0.,0.));
#128330=DIRECTION('center_axis',(-1.,0.,0.));
#128331=DIRECTION('ref_axis',(0.,0.,1.));
#128332=DIRECTION('center_axis',(-1.,0.,0.));
#128333=DIRECTION('ref_axis',(0.,0.,1.));
#128334=DIRECTION('',(-1.,0.,0.));
#128335=DIRECTION('',(1.,0.,0.));
#128336=DIRECTION('center_axis',(-1.,0.,0.));
#128337=DIRECTION('ref_axis',(0.,0.,1.));
#128338=DIRECTION('center_axis',(-1.,0.,0.));
#128339=DIRECTION('ref_axis',(0.,0.,1.));
#128340=DIRECTION('',(1.,0.,0.));
#128341=DIRECTION('center_axis',(-1.,0.,0.));
#128342=DIRECTION('ref_axis',(0.,0.,1.));
#128343=DIRECTION('',(-1.,0.,0.));
#128344=DIRECTION('center_axis',(-1.,0.,0.));
#128345=DIRECTION('ref_axis',(0.,0.,1.));
#128346=DIRECTION('',(1.,0.,0.));
#128347=DIRECTION('center_axis',(-1.,0.,0.));
#128348=DIRECTION('ref_axis',(0.,0.,1.));
#128349=DIRECTION('',(-1.,0.,0.));
#128350=DIRECTION('center_axis',(-1.,0.,0.));
#128351=DIRECTION('ref_axis',(0.,0.,1.));
#128352=DIRECTION('',(-1.,0.,0.));
#128353=DIRECTION('',(1.,0.,0.));
#128354=DIRECTION('center_axis',(-1.,0.,0.));
#128355=DIRECTION('ref_axis',(0.,0.,1.));
#128356=DIRECTION('center_axis',(-1.,0.,0.));
#128357=DIRECTION('ref_axis',(0.,0.,1.));
#128358=DIRECTION('',(-1.,0.,0.));
#128359=DIRECTION('',(1.,0.,0.));
#128360=DIRECTION('center_axis',(-1.,0.,0.));
#128361=DIRECTION('ref_axis',(0.,0.,1.));
#128362=DIRECTION('center_axis',(-1.,0.,0.));
#128363=DIRECTION('ref_axis',(0.,0.,1.));
#128364=DIRECTION('center_axis',(-1.,0.,0.));
#128365=DIRECTION('ref_axis',(0.,0.,1.));
#128366=DIRECTION('center_axis',(-1.,0.,0.));
#128367=DIRECTION('ref_axis',(0.,0.,1.));
#128368=DIRECTION('center_axis',(-1.,0.,0.));
#128369=DIRECTION('ref_axis',(0.,0.,1.));
#128370=DIRECTION('center_axis',(-1.,0.,0.));
#128371=DIRECTION('ref_axis',(0.,0.,1.));
#128372=DIRECTION('center_axis',(-1.,0.,0.));
#128373=DIRECTION('ref_axis',(0.,0.,1.));
#128374=DIRECTION('center_axis',(-1.,0.,0.));
#128375=DIRECTION('ref_axis',(0.,0.,1.));
#128376=DIRECTION('center_axis',(-1.,0.,0.));
#128377=DIRECTION('ref_axis',(0.,0.,1.));
#128378=DIRECTION('center_axis',(-1.,0.,0.));
#128379=DIRECTION('ref_axis',(0.,0.,1.));
#128380=DIRECTION('center_axis',(-1.,0.,0.));
#128381=DIRECTION('ref_axis',(0.,0.,1.));
#128382=DIRECTION('center_axis',(-1.,0.,0.));
#128383=DIRECTION('ref_axis',(0.,0.,1.));
#128384=DIRECTION('center_axis',(-1.,0.,0.));
#128385=DIRECTION('ref_axis',(0.,0.,1.));
#128386=DIRECTION('center_axis',(-1.,0.,0.));
#128387=DIRECTION('ref_axis',(0.,0.,1.));
#128388=DIRECTION('center_axis',(-1.,0.,0.));
#128389=DIRECTION('ref_axis',(0.,0.,1.));
#128390=DIRECTION('center_axis',(-1.,0.,0.));
#128391=DIRECTION('ref_axis',(0.,0.,1.));
#128392=DIRECTION('center_axis',(-1.,0.,0.));
#128393=DIRECTION('ref_axis',(0.,0.,1.));
#128394=DIRECTION('center_axis',(-1.,0.,0.));
#128395=DIRECTION('ref_axis',(0.,0.,1.));
#128396=DIRECTION('center_axis',(-1.,0.,0.));
#128397=DIRECTION('ref_axis',(0.,0.,1.));
#128398=DIRECTION('center_axis',(-1.,0.,0.));
#128399=DIRECTION('ref_axis',(0.,0.,1.));
#128400=DIRECTION('center_axis',(-1.,0.,0.));
#128401=DIRECTION('ref_axis',(0.,0.,1.));
#128402=DIRECTION('center_axis',(-1.,0.,0.));
#128403=DIRECTION('ref_axis',(0.,0.,1.));
#128404=DIRECTION('center_axis',(-1.,0.,0.));
#128405=DIRECTION('ref_axis',(0.,0.,1.));
#128406=DIRECTION('center_axis',(-1.,0.,0.));
#128407=DIRECTION('ref_axis',(0.,0.,1.));
#128408=DIRECTION('center_axis',(-1.,0.,0.));
#128409=DIRECTION('ref_axis',(0.,0.,1.));
#128410=DIRECTION('center_axis',(-1.,0.,0.));
#128411=DIRECTION('ref_axis',(0.,0.,1.));
#128412=DIRECTION('center_axis',(-1.,0.,0.));
#128413=DIRECTION('ref_axis',(0.,0.,1.));
#128414=DIRECTION('center_axis',(-1.,0.,0.));
#128415=DIRECTION('ref_axis',(0.,0.,1.));
#128416=DIRECTION('center_axis',(-1.,0.,0.));
#128417=DIRECTION('ref_axis',(0.,0.,1.));
#128418=DIRECTION('center_axis',(-1.,0.,0.));
#128419=DIRECTION('ref_axis',(0.,1.05802772004469E-14,-1.));
#128420=DIRECTION('center_axis',(-1.,0.,0.));
#128421=DIRECTION('ref_axis',(0.,0.,1.));
#128422=DIRECTION('center_axis',(-1.,0.,0.));
#128423=DIRECTION('ref_axis',(0.,0.,1.));
#128424=DIRECTION('center_axis',(-1.,0.,0.));
#128425=DIRECTION('ref_axis',(0.,0.,1.));
#128426=DIRECTION('center_axis',(-1.,0.,0.));
#128427=DIRECTION('ref_axis',(0.,0.,1.));
#128428=DIRECTION('center_axis',(-1.,0.,0.));
#128429=DIRECTION('ref_axis',(0.,0.,1.));
#128430=DIRECTION('center_axis',(-1.,0.,0.));
#128431=DIRECTION('ref_axis',(0.,0.,1.));
#128432=DIRECTION('center_axis',(-1.,0.,0.));
#128433=DIRECTION('ref_axis',(0.,0.,1.));
#128434=DIRECTION('center_axis',(-1.,0.,0.));
#128435=DIRECTION('ref_axis',(0.,0.,1.));
#128436=DIRECTION('center_axis',(-1.,0.,0.));
#128437=DIRECTION('ref_axis',(0.,0.,1.));
#128438=DIRECTION('center_axis',(-1.,0.,0.));
#128439=DIRECTION('ref_axis',(0.,0.,1.));
#128440=DIRECTION('center_axis',(-1.,0.,0.));
#128441=DIRECTION('ref_axis',(0.,0.,1.));
#128442=DIRECTION('center_axis',(-1.,0.,0.));
#128443=DIRECTION('ref_axis',(0.,0.,1.));
#128444=DIRECTION('center_axis',(-1.,0.,0.));
#128445=DIRECTION('ref_axis',(0.,0.,1.));
#128446=DIRECTION('center_axis',(-1.,0.,0.));
#128447=DIRECTION('ref_axis',(0.,0.,1.));
#128448=DIRECTION('center_axis',(-1.,0.,0.));
#128449=DIRECTION('ref_axis',(0.,0.,1.));
#128450=DIRECTION('center_axis',(-1.,0.,0.));
#128451=DIRECTION('ref_axis',(0.,0.,1.));
#128452=DIRECTION('center_axis',(-1.,0.,0.));
#128453=DIRECTION('ref_axis',(0.,0.,1.));
#128454=DIRECTION('center_axis',(-1.,0.,0.));
#128455=DIRECTION('ref_axis',(0.,0.,1.));
#128456=DIRECTION('center_axis',(-1.,0.,0.));
#128457=DIRECTION('ref_axis',(0.,0.,1.));
#128458=DIRECTION('center_axis',(-1.,0.,0.));
#128459=DIRECTION('ref_axis',(0.,0.,1.));
#128460=DIRECTION('center_axis',(-1.,0.,0.));
#128461=DIRECTION('ref_axis',(0.,0.,1.));
#128462=DIRECTION('center_axis',(-1.,0.,0.));
#128463=DIRECTION('ref_axis',(0.,0.,1.));
#128464=DIRECTION('center_axis',(-1.,0.,0.));
#128465=DIRECTION('ref_axis',(0.,0.,1.));
#128466=DIRECTION('center_axis',(-1.,0.,0.));
#128467=DIRECTION('ref_axis',(0.,0.,1.));
#128468=DIRECTION('center_axis',(-1.,0.,0.));
#128469=DIRECTION('ref_axis',(0.,0.,1.));
#128470=DIRECTION('center_axis',(-1.,0.,0.));
#128471=DIRECTION('ref_axis',(0.,0.,1.));
#128472=DIRECTION('center_axis',(-1.,0.,0.));
#128473=DIRECTION('ref_axis',(0.,0.,1.));
#128474=DIRECTION('center_axis',(-1.,0.,0.));
#128475=DIRECTION('ref_axis',(0.,0.,1.));
#128476=DIRECTION('center_axis',(-1.,0.,0.));
#128477=DIRECTION('ref_axis',(0.,0.,1.));
#128478=DIRECTION('center_axis',(-1.,0.,0.));
#128479=DIRECTION('ref_axis',(0.,0.,1.));
#128480=DIRECTION('',(-1.,0.,0.));
#128481=DIRECTION('',(1.,0.,0.));
#128482=DIRECTION('center_axis',(-1.,0.,0.));
#128483=DIRECTION('ref_axis',(0.,0.,1.));
#128484=DIRECTION('center_axis',(-1.,0.,0.));
#128485=DIRECTION('ref_axis',(0.,0.,1.));
#128486=DIRECTION('center_axis',(-1.,0.,0.));
#128487=DIRECTION('ref_axis',(0.,0.,1.));
#128488=DIRECTION('center_axis',(1.,0.,0.));
#128489=DIRECTION('ref_axis',(0.,0.,-1.));
#128490=DIRECTION('center_axis',(-1.,0.,0.));
#128491=DIRECTION('ref_axis',(0.,-3.090226693085E-15,-1.));
#128492=DIRECTION('center_axis',(-1.,0.,0.));
#128493=DIRECTION('ref_axis',(0.,-7.21052895053167E-15,-1.));
#128494=DIRECTION('center_axis',(-1.,0.,0.));
#128495=DIRECTION('ref_axis',(0.,3.54088475249323E-15,-1.));
#128496=DIRECTION('center_axis',(-1.,0.,0.));
#128497=DIRECTION('ref_axis',(0.,0.,-1.));
#128498=DIRECTION('center_axis',(-1.,0.,0.));
#128499=DIRECTION('ref_axis',(0.,0.,-1.));
#128500=DIRECTION('center_axis',(-1.,0.,0.));
#128501=DIRECTION('ref_axis',(0.,0.,-1.));
#128502=DIRECTION('center_axis',(-1.,0.,0.));
#128503=DIRECTION('ref_axis',(0.,0.,-1.));
#128504=DIRECTION('center_axis',(-1.,0.,0.));
#128505=DIRECTION('ref_axis',(0.,0.,-1.));
#128506=DIRECTION('center_axis',(-1.,0.,0.));
#128507=DIRECTION('ref_axis',(0.,0.,-1.));
#128508=DIRECTION('center_axis',(-1.,0.,0.));
#128509=DIRECTION('ref_axis',(0.,0.,-1.));
#128510=DIRECTION('center_axis',(-1.,0.,0.));
#128511=DIRECTION('ref_axis',(0.,4.12030225744667E-15,-1.));
#128512=DIRECTION('center_axis',(-1.,0.,0.));
#128513=DIRECTION('ref_axis',(0.,0.,-1.));
#128514=DIRECTION('center_axis',(-1.,0.,0.));
#128515=DIRECTION('ref_axis',(0.,8.24060451489334E-15,-1.));
#128516=DIRECTION('center_axis',(-1.,0.,0.));
#128517=DIRECTION('ref_axis',(0.,0.,-1.));
#128518=DIRECTION('center_axis',(-1.,0.,0.));
#128519=DIRECTION('ref_axis',(0.,2.06015112872333E-15,-1.));
#128520=DIRECTION('center_axis',(-1.,0.,0.));
#128521=DIRECTION('ref_axis',(0.,-4.12030225744667E-15,-1.));
#128522=DIRECTION('center_axis',(-1.,0.,0.));
#128523=DIRECTION('ref_axis',(0.,4.12030225744667E-15,-1.));
#128524=DIRECTION('center_axis',(-1.,0.,0.));
#128525=DIRECTION('ref_axis',(0.,4.12030225744667E-15,-1.));
#128526=DIRECTION('center_axis',(-1.,0.,0.));
#128527=DIRECTION('ref_axis',(0.,0.,1.));
#128528=DIRECTION('',(-1.,0.,0.));
#128529=DIRECTION('center_axis',(-1.,0.,0.));
#128530=DIRECTION('ref_axis',(0.,0.,1.));
#128531=DIRECTION('',(-1.,0.,0.));
#128532=DIRECTION('center_axis',(-1.,0.,0.));
#128533=DIRECTION('ref_axis',(0.,0.,1.));
#128534=DIRECTION('center_axis',(-1.,0.,0.));
#128535=DIRECTION('ref_axis',(0.,0.,1.));
#128536=DIRECTION('',(-1.,0.,0.));
#128537=DIRECTION('center_axis',(-1.,0.,0.));
#128538=DIRECTION('ref_axis',(0.,0.,1.));
#128539=DIRECTION('',(-1.,0.,0.));
#128540=DIRECTION('center_axis',(-1.,0.,0.));
#128541=DIRECTION('ref_axis',(0.,0.,1.));
#128542=DIRECTION('center_axis',(-1.,0.,0.));
#128543=DIRECTION('ref_axis',(0.,0.,1.));
#128544=DIRECTION('center_axis',(-1.,0.,0.));
#128545=DIRECTION('ref_axis',(0.,0.,1.));
#128546=DIRECTION('center_axis',(-1.,0.,0.));
#128547=DIRECTION('ref_axis',(0.,0.,1.));
#128548=DIRECTION('center_axis',(-1.,0.,0.));
#128549=DIRECTION('ref_axis',(0.,0.,1.));
#128550=DIRECTION('center_axis',(-1.,0.,0.));
#128551=DIRECTION('ref_axis',(0.,0.,1.));
#128552=DIRECTION('center_axis',(-1.,0.,0.));
#128553=DIRECTION('ref_axis',(0.,0.,1.));
#128554=DIRECTION('center_axis',(-1.,0.,0.));
#128555=DIRECTION('ref_axis',(0.,0.,1.));
#128556=DIRECTION('',(-1.,0.,0.));
#128557=DIRECTION('center_axis',(-1.,0.,0.));
#128558=DIRECTION('ref_axis',(0.,0.,1.));
#128559=DIRECTION('',(-1.,0.,0.));
#128560=DIRECTION('center_axis',(-1.,0.,0.));
#128561=DIRECTION('ref_axis',(0.,0.,1.));
#128562=DIRECTION('center_axis',(-1.,0.,0.));
#128563=DIRECTION('ref_axis',(0.,0.0500387861363127,-0.998747275281392));
#128564=DIRECTION('center_axis',(-1.,0.,0.));
#128565=DIRECTION('ref_axis',(0.,0.,1.));
#128566=DIRECTION('center_axis',(-1.,0.,0.));
#128567=DIRECTION('ref_axis',(0.,0.,1.));
#128568=DIRECTION('center_axis',(-1.,0.,0.));
#128569=DIRECTION('ref_axis',(0.,0.,1.));
#128570=DIRECTION('center_axis',(-1.,0.,0.));
#128571=DIRECTION('ref_axis',(0.,0.,1.));
#128572=DIRECTION('center_axis',(-1.,0.,0.));
#128573=DIRECTION('ref_axis',(0.,0.,1.));
#128574=DIRECTION('center_axis',(-1.,0.,0.));
#128575=DIRECTION('ref_axis',(0.,0.,1.));
#128576=DIRECTION('',(-1.,0.,0.));
#128577=DIRECTION('center_axis',(-1.,0.,0.));
#128578=DIRECTION('ref_axis',(0.,0.,1.));
#128579=DIRECTION('',(-1.,0.,0.));
#128580=DIRECTION('center_axis',(-1.,0.,0.));
#128581=DIRECTION('ref_axis',(0.,0.,1.));
#128582=DIRECTION('center_axis',(-1.,0.,0.));
#128583=DIRECTION('ref_axis',(0.,0.,1.));
#128584=DIRECTION('center_axis',(-1.,0.,0.));
#128585=DIRECTION('ref_axis',(0.,0.,1.));
#128586=DIRECTION('center_axis',(-1.,0.,0.));
#128587=DIRECTION('ref_axis',(0.,0.,1.));
#128588=DIRECTION('center_axis',(-1.,0.,0.));
#128589=DIRECTION('ref_axis',(0.,-0.0500387861362921,-0.998747275281393));
#128590=DIRECTION('center_axis',(-1.,0.,0.));
#128591=DIRECTION('ref_axis',(0.,0.,1.));
#128592=DIRECTION('center_axis',(-1.,0.,0.));
#128593=DIRECTION('ref_axis',(0.,0.,1.));
#128594=DIRECTION('center_axis',(-1.,0.,0.));
#128595=DIRECTION('ref_axis',(0.,0.,1.));
#128596=DIRECTION('center_axis',(-1.,0.,0.));
#128597=DIRECTION('ref_axis',(0.,0.,1.));
#128598=DIRECTION('center_axis',(-1.,0.,0.));
#128599=DIRECTION('ref_axis',(0.,0.,1.));
#128600=DIRECTION('center_axis',(-1.,0.,0.));
#128601=DIRECTION('ref_axis',(0.,0.,1.));
#128602=DIRECTION('center_axis',(-1.,0.,0.));
#128603=DIRECTION('ref_axis',(0.,0.,1.));
#128604=DIRECTION('center_axis',(-1.,0.,0.));
#128605=DIRECTION('ref_axis',(0.,0.,1.));
#128606=DIRECTION('center_axis',(-1.,0.,0.));
#128607=DIRECTION('ref_axis',(0.,0.,1.));
#128608=DIRECTION('',(-1.,0.,0.));
#128609=DIRECTION('center_axis',(-1.,0.,0.));
#128610=DIRECTION('ref_axis',(0.,0.,1.));
#128611=DIRECTION('',(-1.,0.,0.));
#128612=DIRECTION('center_axis',(-1.,0.,0.));
#128613=DIRECTION('ref_axis',(0.,0.309016994374949,-0.951056516295153));
#128614=DIRECTION('center_axis',(-1.,0.,0.));
#128615=DIRECTION('ref_axis',(0.,0.,1.));
#128616=DIRECTION('',(-1.,0.,0.));
#128617=DIRECTION('center_axis',(-1.,0.,0.));
#128618=DIRECTION('ref_axis',(0.,0.,1.));
#128619=DIRECTION('',(-1.,0.,0.));
#128620=DIRECTION('center_axis',(-1.,0.,0.));
#128621=DIRECTION('ref_axis',(0.,0.669130606358861,-0.743144825477392));
#128622=DIRECTION('center_axis',(-1.,0.,0.));
#128623=DIRECTION('ref_axis',(0.,0.,1.));
#128624=DIRECTION('',(-1.,0.,0.));
#128625=DIRECTION('center_axis',(-1.,0.,0.));
#128626=DIRECTION('ref_axis',(0.,0.,1.));
#128627=DIRECTION('',(-1.,0.,0.));
#128628=DIRECTION('center_axis',(-1.,0.,0.));
#128629=DIRECTION('ref_axis',(0.,0.500000000000004,-0.866025403784436));
#128630=DIRECTION('center_axis',(-1.,0.,0.));
#128631=DIRECTION('ref_axis',(0.,0.,1.));
#128632=DIRECTION('',(-1.,0.,0.));
#128633=DIRECTION('center_axis',(-1.,0.,0.));
#128634=DIRECTION('ref_axis',(0.,0.913545457642602,-0.406736643075798));
#128635=DIRECTION('center_axis',(-1.,0.,0.));
#128636=DIRECTION('ref_axis',(0.,0.,1.));
#128637=DIRECTION('',(-1.,0.,0.));
#128638=DIRECTION('center_axis',(-1.,0.,0.));
#128639=DIRECTION('ref_axis',(0.,0.,1.));
#128640=DIRECTION('',(-1.,0.,0.));
#128641=DIRECTION('center_axis',(-1.,0.,0.));
#128642=DIRECTION('ref_axis',(0.,0.809016994374951,-0.587785252292468));
#128643=DIRECTION('center_axis',(-1.,0.,0.));
#128644=DIRECTION('ref_axis',(0.,0.,1.));
#128645=DIRECTION('',(-1.,0.,0.));
#128646=DIRECTION('center_axis',(-1.,0.,0.));
#128647=DIRECTION('ref_axis',(0.,0.,1.));
#128648=DIRECTION('',(-1.,0.,0.));
#128649=DIRECTION('center_axis',(-1.,0.,0.));
#128650=DIRECTION('ref_axis',(0.,0.,1.));
#128651=DIRECTION('center_axis',(-1.,0.,0.));
#128652=DIRECTION('ref_axis',(0.,0.,1.));
#128653=DIRECTION('',(-1.,0.,0.));
#128654=DIRECTION('center_axis',(-1.,0.,0.));
#128655=DIRECTION('ref_axis',(0.,0.,1.));
#128656=DIRECTION('',(-1.,0.,0.));
#128657=DIRECTION('center_axis',(-1.,0.,0.));
#128658=DIRECTION('ref_axis',(0.,0.,1.));
#128659=DIRECTION('center_axis',(-1.,0.,0.));
#128660=DIRECTION('ref_axis',(0.,0.,1.));
#128661=DIRECTION('',(-1.,0.,0.));
#128662=DIRECTION('center_axis',(-1.,0.,0.));
#128663=DIRECTION('ref_axis',(0.,0.,1.));
#128664=DIRECTION('',(-1.,0.,0.));
#128665=DIRECTION('center_axis',(-1.,0.,0.));
#128666=DIRECTION('ref_axis',(0.,-0.809016994374947,-0.587785252292473));
#128667=DIRECTION('center_axis',(-1.,0.,0.));
#128668=DIRECTION('ref_axis',(0.,0.,1.));
#128669=DIRECTION('',(-1.,0.,0.));
#128670=DIRECTION('center_axis',(-1.,0.,0.));
#128671=DIRECTION('ref_axis',(0.,0.,1.));
#128672=DIRECTION('',(-1.,0.,0.));
#128673=DIRECTION('center_axis',(-1.,0.,0.));
#128674=DIRECTION('ref_axis',(0.,-0.669130606358855,-0.743144825477397));
#128675=DIRECTION('center_axis',(-1.,0.,0.));
#128676=DIRECTION('ref_axis',(0.,0.,1.));
#128677=DIRECTION('',(-1.,0.,0.));
#128678=DIRECTION('center_axis',(-1.,0.,0.));
#128679=DIRECTION('ref_axis',(0.,-0.9135454576426,-0.406736643075802));
#128680=DIRECTION('center_axis',(-1.,0.,0.));
#128681=DIRECTION('ref_axis',(0.,0.,1.));
#128682=DIRECTION('',(-1.,0.,0.));
#128683=DIRECTION('center_axis',(-1.,0.,0.));
#128684=DIRECTION('ref_axis',(0.,0.,1.));
#128685=DIRECTION('',(-1.,0.,0.));
#128686=DIRECTION('center_axis',(-1.,0.,0.));
#128687=DIRECTION('ref_axis',(0.,-0.499999999999997,-0.866025403784441));
#128688=DIRECTION('center_axis',(-1.,0.,0.));
#128689=DIRECTION('ref_axis',(0.,0.,1.));
#128690=DIRECTION('',(-1.,0.,0.));
#128691=DIRECTION('center_axis',(-1.,0.,0.));
#128692=DIRECTION('ref_axis',(0.,0.,1.));
#128693=DIRECTION('',(-1.,0.,0.));
#128694=DIRECTION('center_axis',(-1.,0.,0.));
#128695=DIRECTION('ref_axis',(0.,-0.309016994374942,-0.951056516295155));
#128696=DIRECTION('center_axis',(-1.,0.,0.));
#128697=DIRECTION('ref_axis',(0.,0.,1.));
#128698=DIRECTION('',(-1.,0.,0.));
#128699=DIRECTION('center_axis',(-1.,0.,0.));
#128700=DIRECTION('ref_axis',(0.,0.,1.));
#128701=DIRECTION('',(-1.,0.,0.));
#128702=DIRECTION('center_axis',(-1.,0.,0.));
#128703=DIRECTION('ref_axis',(0.,-0.104528463267644,-0.994521895368274));
#128704=DIRECTION('center_axis',(-1.,0.,0.));
#128705=DIRECTION('ref_axis',(0.,0.,1.));
#128706=DIRECTION('',(-1.,0.,0.));
#128707=DIRECTION('center_axis',(-1.,0.,0.));
#128708=DIRECTION('ref_axis',(0.,0.,1.));
#128709=DIRECTION('',(-1.,0.,0.));
#128710=DIRECTION('center_axis',(-1.,0.,0.));
#128711=DIRECTION('ref_axis',(0.,0.104528463267661,-0.994521895368273));
#128712=DIRECTION('center_axis',(0.,-1.,0.));
#128713=DIRECTION('ref_axis',(0.,0.,-1.));
#128714=DIRECTION('',(-1.,0.,0.));
#128715=DIRECTION('',(-1.,0.,0.));
#128716=DIRECTION('center_axis',(0.,0.,1.));
#128717=DIRECTION('ref_axis',(1.,0.,0.));
#128718=DIRECTION('center_axis',(0.,0.,-1.));
#128719=DIRECTION('ref_axis',(-1.,0.,0.));
#128720=DIRECTION('axis',(0.,0.,1.));
#128721=DIRECTION('refdir',(1.,0.,0.));
#128722=DIRECTION('center_axis',(0.,0.,-1.));
#128723=DIRECTION('ref_axis',(-1.,0.,0.));
#128724=DIRECTION('center_axis',(0.,0.,1.));
#128725=DIRECTION('ref_axis',(1.,0.,0.));
#128726=DIRECTION('',(0.,0.,-1.));
#128727=DIRECTION('center_axis',(0.,0.,1.));
#128728=DIRECTION('ref_axis',(1.,0.,0.));
#128729=DIRECTION('center_axis',(0.,0.,-1.));
#128730=DIRECTION('ref_axis',(-1.,0.,0.));
#128731=DIRECTION('center_axis',(0.,0.,1.));
#128732=DIRECTION('ref_axis',(1.,0.,0.));
#128733=DIRECTION('',(0.,0.,-1.));
#128734=DIRECTION('center_axis',(0.,0.,1.));
#128735=DIRECTION('ref_axis',(1.,0.,0.));
#128736=DIRECTION('',(0.,0.,-1.));
#128737=DIRECTION('center_axis',(0.,0.,-1.));
#128738=DIRECTION('ref_axis',(-1.,0.,0.));
#128739=DIRECTION('center_axis',(0.,0.,1.));
#128740=DIRECTION('ref_axis',(1.,0.,0.));
#128741=DIRECTION('',(0.,0.,-1.));
#128742=DIRECTION('center_axis',(0.,0.,1.));
#128743=DIRECTION('ref_axis',(1.,0.,0.));
#128744=DIRECTION('center_axis',(0.,0.,-1.));
#128745=DIRECTION('ref_axis',(-1.,0.,0.));
#128746=DIRECTION('center_axis',(0.,0.,-1.));
#128747=DIRECTION('ref_axis',(1.,0.,0.));
#128748=DIRECTION('',(0.,0.,-1.));
#128749=DIRECTION('center_axis',(0.,0.,-1.));
#128750=DIRECTION('ref_axis',(1.,0.,0.));
#128751=DIRECTION('center_axis',(0.,0.,-1.));
#128752=DIRECTION('ref_axis',(1.,1.22464679914735E-16,0.));
#128753=DIRECTION('center_axis',(0.,0.,1.));
#128754=DIRECTION('ref_axis',(1.,0.,0.));
#128755=DIRECTION('',(0.,0.,-1.));
#128756=DIRECTION('center_axis',(0.,0.,1.));
#128757=DIRECTION('ref_axis',(1.,0.,0.));
#128758=DIRECTION('center_axis',(0.,0.,-1.));
#128759=DIRECTION('ref_axis',(-1.,0.,0.));
#128760=DIRECTION('center_axis',(0.,0.,1.));
#128761=DIRECTION('ref_axis',(1.,0.,0.));
#128762=DIRECTION('center_axis',(0.,0.,1.));
#128763=DIRECTION('ref_axis',(1.,0.,0.));
#128764=DIRECTION('center_axis',(0.,0.,1.));
#128765=DIRECTION('ref_axis',(1.,0.,0.));
#128766=DIRECTION('center_axis',(0.,0.,1.));
#128767=DIRECTION('ref_axis',(1.,0.,0.));
#128768=DIRECTION('center_axis',(0.,0.,-1.));
#128769=DIRECTION('ref_axis',(-1.,0.,0.));
#128770=DIRECTION('center_axis',(0.,0.,1.));
#128771=DIRECTION('ref_axis',(1.,0.,0.));
#128772=DIRECTION('',(0.,0.,-1.));
#128773=DIRECTION('center_axis',(0.,0.,1.));
#128774=DIRECTION('ref_axis',(1.,0.,0.));
#128775=DIRECTION('center_axis',(0.,0.,-1.));
#128776=DIRECTION('ref_axis',(-1.,0.,0.));
#128777=DIRECTION('center_axis',(0.,0.,1.));
#128778=DIRECTION('ref_axis',(1.,0.,0.));
#128779=DIRECTION('',(0.,0.,-1.));
#128780=DIRECTION('center_axis',(0.,0.,1.));
#128781=DIRECTION('ref_axis',(1.,0.,0.));
#128782=DIRECTION('center_axis',(0.,0.,-1.));
#128783=DIRECTION('ref_axis',(-1.,0.,0.));
#128784=DIRECTION('center_axis',(0.,0.,1.));
#128785=DIRECTION('ref_axis',(1.,0.,0.));
#128786=DIRECTION('',(0.,0.,-1.));
#128787=DIRECTION('center_axis',(0.,0.,1.));
#128788=DIRECTION('ref_axis',(1.,0.,0.));
#128789=DIRECTION('',(0.,0.,-1.));
#128790=DIRECTION('center_axis',(0.,0.,1.));
#128791=DIRECTION('ref_axis',(1.,0.,0.));
#128792=DIRECTION('center_axis',(0.,0.,-1.));
#128793=DIRECTION('ref_axis',(1.,0.,0.));
#128794=DIRECTION('center_axis',(0.,0.,1.));
#128795=DIRECTION('ref_axis',(1.,0.,0.));
#128796=DIRECTION('center_axis',(0.,0.,-1.));
#128797=DIRECTION('ref_axis',(1.,0.,0.));
#128798=DIRECTION('center_axis',(0.,0.,1.));
#128799=DIRECTION('ref_axis',(1.,0.,0.));
#128800=DIRECTION('center_axis',(0.,0.,-1.));
#128801=DIRECTION('ref_axis',(1.,0.,0.));
#128802=DIRECTION('center_axis',(0.,0.,-1.));
#128803=DIRECTION('ref_axis',(1.,0.,0.));
#128804=DIRECTION('center_axis',(0.,0.,1.));
#128805=DIRECTION('ref_axis',(1.,0.,0.));
#128806=DIRECTION('center_axis',(0.,0.,-1.));
#128807=DIRECTION('ref_axis',(-1.,0.,0.));
#128808=DIRECTION('',(0.,0.,-1.));
#128809=DIRECTION('center_axis',(0.,0.,-1.));
#128810=DIRECTION('ref_axis',(1.,-3.21624529935327E-16,0.));
#128811=DIRECTION('',(0.,0.,-1.));
#128812=DIRECTION('center_axis',(0.,0.,-1.));
#128813=DIRECTION('ref_axis',(-1.,0.,0.));
#128814=DIRECTION('center_axis',(0.,0.,-1.));
#128815=DIRECTION('ref_axis',(-1.,0.,0.));
#128816=DIRECTION('center_axis',(0.,0.,1.));
#128817=DIRECTION('ref_axis',(1.,0.,0.));
#128818=DIRECTION('',(0.,0.,1.));
#128819=DIRECTION('center_axis',(0.,0.,1.));
#128820=DIRECTION('ref_axis',(1.,0.,0.));
#128821=DIRECTION('center_axis',(0.,0.,1.));
#128822=DIRECTION('ref_axis',(1.,0.,0.));
#128823=DIRECTION('center_axis',(0.,0.,1.));
#128824=DIRECTION('ref_axis',(1.,0.,0.));
#128825=DIRECTION('center_axis',(0.,0.,-1.));
#128826=DIRECTION('ref_axis',(-1.,0.,0.));
#128827=DIRECTION('center_axis',(0.,0.,1.));
#128828=DIRECTION('ref_axis',(1.,0.,0.));
#128829=DIRECTION('',(0.,0.,1.));
#128830=DIRECTION('center_axis',(0.,0.,1.));
#128831=DIRECTION('ref_axis',(1.,0.,0.));
#128832=DIRECTION('center_axis',(0.,0.,1.));
#128833=DIRECTION('ref_axis',(1.,0.,0.));
#128834=DIRECTION('center_axis',(0.,0.,1.));
#128835=DIRECTION('ref_axis',(1.,0.,0.));
#128836=DIRECTION('',(0.,-0.00452103900291789,0.999989780050943));
#128837=DIRECTION('',(1.,0.,0.));
#128838=DIRECTION('',(-3.43690365988575E-17,-0.924224592736303,-0.381849318686593));
#128839=DIRECTION('',(1.,-5.83333790925112E-17,5.11827728358266E-17));
#128840=DIRECTION('',(1.,0.,-3.49148133884313E-15));
#128841=DIRECTION('',(-3.49148133884313E-15,0.,-1.));
#128842=DIRECTION('',(1.,0.,-3.49148133884313E-15));
#128843=DIRECTION('',(-3.49148133884313E-15,0.,-1.));
#128844=DIRECTION('',(1.,0.,-3.49148133884313E-15));
#128845=DIRECTION('',(-3.49148133884313E-15,0.,-1.));
#128846=DIRECTION('',(1.,0.,-3.49148133884313E-15));
#128847=DIRECTION('',(-3.49148133884313E-15,0.,-1.));
#128848=DIRECTION('',(1.,0.,-3.49148133884313E-15));
#128849=DIRECTION('',(-3.49148133884313E-15,0.,-1.));
#128850=DIRECTION('',(1.,0.,-3.49148133884313E-15));
#128851=DIRECTION('',(-3.49148133884313E-15,0.,-1.));
#128852=DIRECTION('',(1.,0.,-3.49148133884313E-15));
#128853=DIRECTION('',(-3.49148133884313E-15,0.,-1.));
#128854=DIRECTION('',(1.,0.,-3.49148133884313E-15));
#128855=DIRECTION('',(-3.49148133884313E-15,0.,-1.));
#128856=DIRECTION('',(1.,0.,-3.49148133884313E-15));
#128857=DIRECTION('',(-3.49148133884313E-15,0.,-1.));
#128858=DIRECTION('',(1.,0.,-3.49148133884313E-15));
#128859=DIRECTION('',(-3.49148133884313E-15,0.,-1.));
#128860=DIRECTION('',(1.,0.,-3.49148133884313E-15));
#128861=DIRECTION('',(-3.49148133884313E-15,0.,-1.));
#128862=DIRECTION('',(1.,0.,-3.49148133884313E-15));
#128863=DIRECTION('',(-3.49148133884313E-15,0.,-1.));
#128864=DIRECTION('',(1.,0.,-3.49148133884313E-15));
#128865=DIRECTION('',(-3.49148133884313E-15,0.,-1.));
#128866=DIRECTION('',(1.,0.,-3.49148133884313E-15));
#128867=DIRECTION('',(-3.49148133884313E-15,0.,-1.));
#128868=DIRECTION('',(1.,0.,-3.49148133884313E-15));
#128869=DIRECTION('',(-3.49148133884313E-15,0.,-1.));
#128870=DIRECTION('',(1.,0.,-3.49148133884313E-15));
#128871=DIRECTION('',(-3.49148133884313E-15,0.,-1.));
#128872=DIRECTION('',(1.,0.,-3.49148133884313E-15));
#128873=DIRECTION('',(-3.49148133884313E-15,0.,-1.));
#128874=DIRECTION('',(1.,0.,-3.49148133884313E-15));
#128875=DIRECTION('',(-3.49148133884313E-15,0.,-1.));
#128876=DIRECTION('',(1.,0.,-3.49148133884313E-15));
#128877=DIRECTION('',(-3.49148133884313E-15,0.,-1.));
#128878=DIRECTION('',(1.,0.,-3.49148133884313E-15));
#128879=DIRECTION('',(-3.49148133884313E-15,0.,-1.));
#128880=DIRECTION('',(1.,0.,-3.49148133884313E-15));
#128881=DIRECTION('',(-3.49148133884313E-15,0.,-1.));
#128882=DIRECTION('',(1.,0.,-3.49148133884313E-15));
#128883=DIRECTION('',(-3.49148133884313E-15,0.,-1.));
#128884=DIRECTION('',(1.,0.,-3.49148133884313E-15));
#128885=DIRECTION('',(-3.49148133884313E-15,0.,-1.));
#128886=DIRECTION('',(1.,0.,-3.49148133884313E-15));
#128887=DIRECTION('',(-3.49148133884313E-15,0.,-1.));
#128888=DIRECTION('',(1.,0.,-3.49148133884313E-15));
#128889=DIRECTION('',(-3.49148133884313E-15,0.,-1.));
#128890=DIRECTION('',(1.,0.,-3.49148133884313E-15));
#128891=DIRECTION('',(-3.49148133884313E-15,0.,-1.));
#128892=DIRECTION('',(1.,0.,-3.49148133884313E-15));
#128893=DIRECTION('',(-3.49148133884313E-15,0.,-1.));
#128894=DIRECTION('',(1.,0.,-3.49148133884313E-15));
#128895=DIRECTION('',(-3.49148133884313E-15,0.,-1.));
#128896=DIRECTION('',(1.,0.,-3.49148133884313E-15));
#128897=DIRECTION('',(-3.49148133884313E-15,0.,-1.));
#128898=DIRECTION('',(1.,0.,-3.49148133884313E-15));
#128899=DIRECTION('',(-3.49148133884313E-15,0.,-1.));
#128900=DIRECTION('',(1.,0.,-3.49148133884313E-15));
#128901=DIRECTION('',(-3.49148133884313E-15,0.,-1.));
#128902=DIRECTION('',(1.,0.,-3.49148133884313E-15));
#128903=DIRECTION('',(-3.49148133884313E-15,0.,-1.));
#128904=DIRECTION('',(1.,0.,-3.49148133884313E-15));
#128905=DIRECTION('',(-3.49148133884313E-15,0.,-1.));
#128906=DIRECTION('',(1.,0.,-3.49148133884313E-15));
#128907=DIRECTION('',(-3.49148133884313E-15,0.,-1.));
#128908=DIRECTION('',(1.,0.,-3.49148133884313E-15));
#128909=DIRECTION('',(-3.49148133884313E-15,0.,-1.));
#128910=DIRECTION('',(1.,0.,-3.49148133884313E-15));
#128911=DIRECTION('',(-3.49148133884313E-15,0.,-1.));
#128912=DIRECTION('',(1.,0.,-3.49148133884313E-15));
#128913=DIRECTION('',(-3.49148133884313E-15,0.,-1.));
#128914=DIRECTION('',(1.,0.,-3.49148133884313E-15));
#128915=DIRECTION('',(-3.49148133884313E-15,0.,-1.));
#128916=DIRECTION('',(1.,0.,-3.49148133884313E-15));
#128917=DIRECTION('',(-3.49148133884313E-15,0.,-1.));
#128918=DIRECTION('',(1.,0.,-3.49148133884313E-15));
#128919=DIRECTION('',(-3.49148133884313E-15,0.,-1.));
#128920=DIRECTION('',(1.,0.,-3.49148133884313E-15));
#128921=DIRECTION('',(-3.49148133884313E-15,0.,-1.));
#128922=DIRECTION('',(1.,0.,-3.49148133884313E-15));
#128923=DIRECTION('',(-3.49148133884313E-15,0.,-1.));
#128924=DIRECTION('',(1.,0.,-3.49148133884313E-15));
#128925=DIRECTION('',(-3.49148133884313E-15,0.,-1.));
#128926=DIRECTION('',(1.,0.,-3.49148133884313E-15));
#128927=DIRECTION('',(-3.49148133884313E-15,0.,-1.));
#128928=DIRECTION('',(1.,0.,-3.49148133884313E-15));
#128929=DIRECTION('',(-3.49148133884313E-15,0.,-1.));
#128930=DIRECTION('',(1.,0.,-3.49148133884313E-15));
#128931=DIRECTION('',(-3.49148133884313E-15,0.,-1.));
#128932=DIRECTION('',(1.,0.,-3.49148133884313E-15));
#128933=DIRECTION('',(-3.49148133884313E-15,0.,-1.));
#128934=DIRECTION('',(1.,0.,-3.49148133884313E-15));
#128935=DIRECTION('',(-3.49148133884313E-15,0.,-1.));
#128936=DIRECTION('',(1.,0.,-3.49148133884313E-15));
#128937=DIRECTION('',(-3.49148133884313E-15,0.,-1.));
#128938=DIRECTION('',(1.,0.,-3.49148133884313E-15));
#128939=DIRECTION('',(-3.49148133884313E-15,0.,-1.));
#128940=DIRECTION('',(1.,0.,-3.49148133884313E-15));
#128941=DIRECTION('',(-3.49148133884313E-15,0.,-1.));
#128942=DIRECTION('',(1.,0.,-3.49148133884313E-15));
#128943=DIRECTION('',(-3.49148133884313E-15,0.,-1.));
#128944=DIRECTION('',(1.,0.,-3.49148133884313E-15));
#128945=DIRECTION('',(-3.49148133884313E-15,0.,-1.));
#128946=DIRECTION('',(1.,0.,-3.49148133884313E-15));
#128947=DIRECTION('',(-3.49148133884313E-15,0.,-1.));
#128948=DIRECTION('',(1.,0.,-3.49148133884313E-15));
#128949=DIRECTION('',(-3.49148133884313E-15,0.,-1.));
#128950=DIRECTION('',(1.,0.,-3.49148133884313E-15));
#128951=DIRECTION('',(-3.49148133884313E-15,0.,-1.));
#128952=DIRECTION('',(1.,0.,-3.49148133884313E-15));
#128953=DIRECTION('',(-3.49148133884313E-15,0.,-1.));
#128954=DIRECTION('',(1.,0.,-3.49148133884313E-15));
#128955=DIRECTION('',(-3.49148133884313E-15,0.,-1.));
#128956=DIRECTION('',(1.,0.,-3.49148133884313E-15));
#128957=DIRECTION('',(-3.49148133884313E-15,0.,-1.));
#128958=DIRECTION('',(1.,0.,-3.49148133884313E-15));
#128959=DIRECTION('',(-3.49148133884313E-15,0.,-1.));
#128960=DIRECTION('',(1.,0.,-3.49148133884313E-15));
#128961=DIRECTION('',(-3.49148133884313E-15,0.,-1.));
#128962=DIRECTION('',(1.,0.,-3.49148133884313E-15));
#128963=DIRECTION('',(-3.49148133884313E-15,0.,-1.));
#128964=DIRECTION('',(1.,0.,-3.49148133884313E-15));
#128965=DIRECTION('',(-3.49148133884313E-15,0.,-1.));
#128966=DIRECTION('',(1.,0.,-3.49148133884313E-15));
#128967=DIRECTION('',(-3.49148133884313E-15,0.,-1.));
#128968=DIRECTION('',(1.,0.,-3.49148133884313E-15));
#128969=DIRECTION('',(-3.49148133884313E-15,0.,-1.));
#128970=DIRECTION('',(1.,0.,-3.49148133884313E-15));
#128971=DIRECTION('',(-3.49148133884313E-15,0.,-1.));
#128972=DIRECTION('',(1.,0.,-3.49148133884313E-15));
#128973=DIRECTION('',(-3.49148133884313E-15,0.,-1.));
#128974=DIRECTION('',(1.,0.,-3.49148133884313E-15));
#128975=DIRECTION('',(-3.49148133884313E-15,0.,-1.));
#128976=DIRECTION('',(1.,0.,-3.49148133884313E-15));
#128977=DIRECTION('',(-3.49148133884313E-15,0.,-1.));
#128978=DIRECTION('',(1.,0.,-3.49148133884313E-15));
#128979=DIRECTION('',(-3.49148133884313E-15,0.,-1.));
#128980=DIRECTION('',(1.,0.,-3.49148133884313E-15));
#128981=DIRECTION('',(-3.49148133884313E-15,0.,-1.));
#128982=DIRECTION('',(1.,0.,-3.49148133884313E-15));
#128983=DIRECTION('',(-3.49148133884313E-15,0.,-1.));
#128984=DIRECTION('',(1.,0.,-3.49148133884313E-15));
#128985=DIRECTION('',(-3.49148133884313E-15,0.,-1.));
#128986=DIRECTION('',(1.,0.,-3.49148133884313E-15));
#128987=DIRECTION('',(-3.49148133884313E-15,0.,-1.));
#128988=DIRECTION('',(1.,0.,-3.49148133884313E-15));
#128989=DIRECTION('',(-3.49148133884313E-15,0.,-1.));
#128990=DIRECTION('',(1.,0.,-3.49148133884313E-15));
#128991=DIRECTION('',(-3.49148133884313E-15,0.,-1.));
#128992=DIRECTION('',(1.,0.,-3.49148133884313E-15));
#128993=DIRECTION('',(-3.49148133884313E-15,0.,-1.));
#128994=DIRECTION('',(1.,0.,-3.49148133884313E-15));
#128995=DIRECTION('',(-3.49148133884313E-15,0.,-1.));
#128996=DIRECTION('',(1.,0.,-3.49148133884313E-15));
#128997=DIRECTION('',(-3.49148133884313E-15,0.,-1.));
#128998=DIRECTION('',(1.,0.,-3.49148133884313E-15));
#128999=DIRECTION('',(-3.49148133884313E-15,0.,-1.));
#129000=DIRECTION('',(1.,0.,-3.49148133884313E-15));
#129001=DIRECTION('',(-3.49148133884313E-15,0.,-1.));
#129002=DIRECTION('',(1.,0.,-3.49148133884313E-15));
#129003=DIRECTION('',(-3.49148133884313E-15,0.,-1.));
#129004=DIRECTION('',(1.,0.,-3.49148133884313E-15));
#129005=DIRECTION('',(-3.49148133884313E-15,0.,-1.));
#129006=DIRECTION('',(1.,0.,-3.49148133884313E-15));
#129007=DIRECTION('',(-3.49148133884313E-15,0.,-1.));
#129008=DIRECTION('',(1.,0.,-3.49148133884313E-15));
#129009=DIRECTION('',(-3.49148133884313E-15,0.,-1.));
#129010=DIRECTION('',(1.,0.,-3.49148133884313E-15));
#129011=DIRECTION('',(-3.49148133884313E-15,0.,-1.));
#129012=DIRECTION('',(1.,0.,-3.49148133884313E-15));
#129013=DIRECTION('',(-3.49148133884313E-15,0.,-1.));
#129014=DIRECTION('',(1.,0.,-3.49148133884313E-15));
#129015=DIRECTION('',(-3.49148133884313E-15,0.,-1.));
#129016=DIRECTION('',(1.,0.,-3.49148133884313E-15));
#129017=DIRECTION('',(-3.49148133884313E-15,0.,-1.));
#129018=DIRECTION('',(1.,0.,-3.49148133884313E-15));
#129019=DIRECTION('',(-3.49148133884313E-15,0.,-1.));
#129020=DIRECTION('',(1.,0.,-3.49148133884313E-15));
#129021=DIRECTION('',(-3.49148133884313E-15,0.,-1.));
#129022=DIRECTION('',(1.,0.,-3.49148133884313E-15));
#129023=DIRECTION('',(-3.49148133884313E-15,0.,-1.));
#129024=DIRECTION('',(1.,0.,-3.49148133884313E-15));
#129025=DIRECTION('',(-3.49148133884313E-15,0.,-1.));
#129026=DIRECTION('',(1.,0.,-3.49148133884313E-15));
#129027=DIRECTION('',(-3.49148133884313E-15,0.,-1.));
#129028=DIRECTION('',(1.,0.,-3.49148133884313E-15));
#129029=DIRECTION('',(-3.49148133884313E-15,0.,-1.));
#129030=DIRECTION('',(1.,0.,-3.49148133884313E-15));
#129031=DIRECTION('',(-3.49148133884313E-15,0.,-1.));
#129032=DIRECTION('',(1.,0.,-3.49148133884313E-15));
#129033=DIRECTION('',(-3.49148133884313E-15,0.,-1.));
#129034=DIRECTION('',(1.,0.,-3.49148133884313E-15));
#129035=DIRECTION('',(-3.49148133884313E-15,0.,-1.));
#129036=DIRECTION('',(1.,0.,-3.49148133884313E-15));
#129037=DIRECTION('',(-3.49148133884313E-15,0.,-1.));
#129038=DIRECTION('',(1.,0.,-3.49148133884313E-15));
#129039=DIRECTION('',(-3.49148133884313E-15,0.,-1.));
#129040=DIRECTION('',(1.,0.,-3.49148133884313E-15));
#129041=DIRECTION('',(-3.49148133884313E-15,0.,-1.));
#129042=DIRECTION('',(1.,0.,-3.49148133884313E-15));
#129043=DIRECTION('',(-3.49148133884313E-15,0.,-1.));
#129044=DIRECTION('',(1.,0.,-3.49148133884313E-15));
#129045=DIRECTION('',(-3.49148133884313E-15,0.,-1.));
#129046=DIRECTION('',(1.,0.,-3.49148133884313E-15));
#129047=DIRECTION('',(-3.49148133884313E-15,0.,-1.));
#129048=DIRECTION('',(1.,0.,-3.49148133884313E-15));
#129049=DIRECTION('',(-3.49148133884313E-15,0.,-1.));
#129050=DIRECTION('',(1.,0.,-3.49148133884313E-15));
#129051=DIRECTION('',(-3.49148133884313E-15,0.,-1.));
#129052=DIRECTION('',(1.,0.,-3.49148133884313E-15));
#129053=DIRECTION('',(-3.49148133884313E-15,0.,-1.));
#129054=DIRECTION('',(1.,0.,-3.49148133884313E-15));
#129055=DIRECTION('',(-3.49148133884313E-15,0.,-1.));
#129056=DIRECTION('',(1.,0.,-3.49148133884313E-15));
#129057=DIRECTION('',(-3.49148133884313E-15,0.,-1.));
#129058=DIRECTION('',(1.,0.,-3.49148133884313E-15));
#129059=DIRECTION('',(-3.49148133884313E-15,0.,-1.));
#129060=DIRECTION('',(1.,0.,-3.49148133884313E-15));
#129061=DIRECTION('',(-3.49148133884313E-15,0.,-1.));
#129062=DIRECTION('',(1.,0.,-3.49148133884313E-15));
#129063=DIRECTION('',(-3.49148133884313E-15,0.,-1.));
#129064=DIRECTION('',(1.,0.,-3.49148133884313E-15));
#129065=DIRECTION('',(-3.49148133884313E-15,0.,-1.));
#129066=DIRECTION('',(1.,0.,-3.49148133884313E-15));
#129067=DIRECTION('',(-3.49148133884313E-15,0.,-1.));
#129068=DIRECTION('',(1.,0.,-3.49148133884313E-15));
#129069=DIRECTION('',(-3.49148133884313E-15,0.,-1.));
#129070=DIRECTION('',(1.,0.,-3.49148133884313E-15));
#129071=DIRECTION('',(-3.49148133884313E-15,0.,-1.));
#129072=DIRECTION('',(1.,0.,-3.49148133884313E-15));
#129073=DIRECTION('',(-3.49148133884313E-15,0.,-1.));
#129074=DIRECTION('',(1.,0.,-3.49148133884313E-15));
#129075=DIRECTION('',(-3.49148133884313E-15,0.,-1.));
#129076=DIRECTION('',(1.,0.,-3.49148133884313E-15));
#129077=DIRECTION('',(-3.49148133884313E-15,0.,-1.));
#129078=DIRECTION('',(1.,0.,-3.49148133884313E-15));
#129079=DIRECTION('',(-3.49148133884313E-15,0.,-1.));
#129080=DIRECTION('',(1.,0.,-3.49148133884313E-15));
#129081=DIRECTION('',(-3.49148133884313E-15,0.,-1.));
#129082=DIRECTION('',(1.,0.,-3.49148133884313E-15));
#129083=DIRECTION('',(-3.49148133884313E-15,0.,-1.));
#129084=DIRECTION('',(1.,9.65374577791131E-30,-3.4914813388431E-15));
#129085=DIRECTION('',(-3.49135697470333E-15,-0.00844022167184764,-0.999964380694698));
#129086=DIRECTION('',(1.,1.06745972397395E-29,-3.49148133884309E-15));
#129087=DIRECTION('',(-2.96571340095325E-15,0.527726941461837,-0.849414077617821));
#129088=DIRECTION('',(1.,9.32689713996097E-30,-3.49148133884309E-15));
#129089=DIRECTION('',(-1.74202794907944E-15,0.866638468234047,-0.498936634631036));
#129090=DIRECTION('',(1.,6.74969661092022E-30,-3.49148133884308E-15));
#129091=DIRECTION('',(1.21048069720614E-16,0.999398830619188,0.0346695450936394));
#129092=DIRECTION('',(1.,4.04481835547107E-30,-3.49148133884307E-15));
#129093=DIRECTION('',(1.67188041123057E-15,0.877899145282375,0.478845581281143));
#129094=DIRECTION('',(1.,-4.25185483557716E-31,-3.49148133884305E-15));
#129095=DIRECTION('',(3.48798059263881E-15,-0.0447694294319336,0.998997346437086));
#129096=DIRECTION('',(1.,2.74231679625196E-30,-3.49148133884305E-15));
#129097=DIRECTION('',(2.84394206430947E-15,0.580111071720941,0.814537380644241));
#129098=DIRECTION('',(1.,4.00099730444732E-32,-3.49148133884313E-15));
#129099=DIRECTION('',(2.96571340092003E-15,0.527726941477166,0.849414077608298));
#129100=DIRECTION('',(1.,-1.48059218504606E-31,-3.49148133884313E-15));
#129101=DIRECTION('',(1.7420279491673E-15,0.866638468219562,0.498936634656196));
#129102=DIRECTION('',(1.,-1.87556957514649E-33,-3.49148133884313E-15));
#129103=DIRECTION('',(3.49135697470389E-15,-0.00844022165414145,0.999964380694847));
#129104=DIRECTION('',(1.,5.95872724299332E-30,3.49148133884308E-15));
#129105=DIRECTION('',(1.2104806976182E-16,0.999398830618778,-0.034669545105441));
#129106=DIRECTION('',(1.,3.54798802181784E-30,3.49148133884307E-15));
#129107=DIRECTION('',(1.67188041122573E-15,0.877899145283131,-0.478845581279757));
#129108=DIRECTION('',(1.,3.50592938271775E-30,3.49148133884305E-15));
#129109=DIRECTION('',(2.84394206430153E-15,0.580111071724131,-0.814537380641969));
#129110=DIRECTION('',(1.,-3.11014044088404E-31,3.49148133884305E-15));
#129111=DIRECTION('',(3.48798059264001E-15,-0.0447694294242762,-0.998997346437429));
#129112=DIRECTION('axis',(0.,0.,1.));
#129113=DIRECTION('refdir',(1.,0.,0.));
#129114=DIRECTION('center_axis',(0.,0.,-1.));
#129115=DIRECTION('ref_axis',(-1.,0.,0.));
#129116=DIRECTION('center_axis',(0.,0.,1.));
#129117=DIRECTION('ref_axis',(1.,0.,0.));
#129118=DIRECTION('',(0.,0.,-1.));
#129119=DIRECTION('center_axis',(0.,0.,1.));
#129120=DIRECTION('ref_axis',(1.,0.,0.));
#129121=DIRECTION('center_axis',(0.,0.,1.));
#129122=DIRECTION('ref_axis',(1.,0.,0.));
#129123=DIRECTION('center_axis',(0.,0.,1.));
#129124=DIRECTION('ref_axis',(1.,0.,0.));
#129125=DIRECTION('',(0.,0.,1.));
#129126=DIRECTION('center_axis',(0.,0.,1.));
#129127=DIRECTION('ref_axis',(1.,0.,0.));
#129128=DIRECTION('center_axis',(0.,0.,-1.));
#129129=DIRECTION('ref_axis',(-1.,0.,0.));
#129130=DIRECTION('center_axis',(0.,0.,1.));
#129131=DIRECTION('ref_axis',(1.,0.,0.));
#129132=DIRECTION('',(0.,0.,1.));
#129133=DIRECTION('center_axis',(0.,0.,1.));
#129134=DIRECTION('ref_axis',(1.,0.,0.));
#129135=DIRECTION('center_axis',(0.,0.,-1.));
#129136=DIRECTION('ref_axis',(-1.,0.,0.));
#129137=DIRECTION('center_axis',(0.,0.,1.));
#129138=DIRECTION('ref_axis',(1.,0.,0.));
#129139=DIRECTION('',(0.,0.,-1.));
#129140=DIRECTION('center_axis',(0.,0.,-1.));
#129141=DIRECTION('ref_axis',(-1.,0.,0.));
#129142=DIRECTION('center_axis',(0.,0.,1.));
#129143=DIRECTION('ref_axis',(1.,0.,0.));
#129144=DIRECTION('center_axis',(0.,0.,1.));
#129145=DIRECTION('ref_axis',(1.,0.,0.));
#129146=DIRECTION('center_axis',(0.,0.,1.));
#129147=DIRECTION('ref_axis',(1.,0.,0.));
#129148=DIRECTION('center_axis',(0.,0.,-1.));
#129149=DIRECTION('ref_axis',(1.,0.,0.));
#129150=DIRECTION('axis',(0.,0.,1.));
#129151=DIRECTION('refdir',(1.,0.,0.));
#129152=DIRECTION('center_axis',(0.,0.,1.));
#129153=DIRECTION('ref_axis',(1.,0.,0.));
#129154=DIRECTION('center_axis',(0.,0.,1.));
#129155=DIRECTION('ref_axis',(1.,0.,0.));
#129156=DIRECTION('center_axis',(1.22464679914735E-16,-1.,0.));
#129157=DIRECTION('ref_axis',(-1.,-1.22464679914735E-16,0.));
#129158=DIRECTION('center_axis',(0.,0.,1.));
#129159=DIRECTION('ref_axis',(1.,0.,0.));
#129160=DIRECTION('center_axis',(0.,0.,1.));
#129161=DIRECTION('ref_axis',(1.,0.,0.));
#129162=DIRECTION('center_axis',(0.,0.,1.));
#129163=DIRECTION('ref_axis',(1.,0.,0.));
#129164=DIRECTION('center_axis',(-1.22464679914735E-16,1.,0.));
#129165=DIRECTION('ref_axis',(-1.,-1.22464679914735E-16,0.));
#129166=DIRECTION('center_axis',(0.,0.,1.));
#129167=DIRECTION('ref_axis',(1.,0.,0.));
#129168=DIRECTION('center_axis',(0.,0.,1.));
#129169=DIRECTION('ref_axis',(1.,0.,0.));
#129170=DIRECTION('center_axis',(0.,0.,1.));
#129171=DIRECTION('ref_axis',(1.,0.,0.));
#129172=DIRECTION('center_axis',(-1.22464679914735E-16,1.,0.));
#129173=DIRECTION('ref_axis',(-1.,-1.22464679914735E-16,0.));
#129174=DIRECTION('center_axis',(0.,0.,1.));
#129175=DIRECTION('ref_axis',(1.,0.,0.));
#129176=DIRECTION('center_axis',(0.,0.,1.));
#129177=DIRECTION('ref_axis',(1.,0.,0.));
#129178=DIRECTION('',(-0.0416304744296221,-5.09826272572225E-18,0.999133076020789));
#129179=DIRECTION('center_axis',(0.,0.,1.));
#129180=DIRECTION('ref_axis',(1.,0.,0.));
#129181=DIRECTION('center_axis',(0.,0.,1.));
#129182=DIRECTION('ref_axis',(1.,0.,0.));
#129183=DIRECTION('center_axis',(1.22464679914735E-16,-1.,0.));
#129184=DIRECTION('ref_axis',(-1.,-1.22464679914735E-16,0.));
#129185=DIRECTION('center_axis',(0.,0.,1.));
#129186=DIRECTION('ref_axis',(1.,0.,0.));
#129187=DIRECTION('center_axis',(0.,0.,1.));
#129188=DIRECTION('ref_axis',(1.,0.,0.));
#129189=DIRECTION('center_axis',(0.,0.,1.));
#129190=DIRECTION('ref_axis',(1.,0.,0.));
#129191=DIRECTION('center_axis',(1.22464679914735E-16,-1.,0.));
#129192=DIRECTION('ref_axis',(-1.,-1.22464679914735E-16,0.));
#129193=DIRECTION('center_axis',(0.,0.,1.));
#129194=DIRECTION('ref_axis',(1.,0.,0.));
#129195=DIRECTION('center_axis',(0.,0.,1.));
#129196=DIRECTION('ref_axis',(1.,0.,0.));
#129197=DIRECTION('',(0.,0.,-1.));
#129198=DIRECTION('center_axis',(0.,0.,1.));
#129199=DIRECTION('ref_axis',(1.,0.,0.));
#129200=DIRECTION('',(0.,0.,-1.));
#129201=DIRECTION('center_axis',(0.,0.,1.));
#129202=DIRECTION('ref_axis',(1.,0.,0.));
#129203=DIRECTION('',(0.,0.,-1.));
#129204=DIRECTION('center_axis',(0.,0.,1.));
#129205=DIRECTION('ref_axis',(1.,0.,0.));
#129206=DIRECTION('center_axis',(0.,0.,1.));
#129207=DIRECTION('ref_axis',(1.,0.,0.));
#129208=DIRECTION('center_axis',(1.22464679914735E-16,-1.,0.));
#129209=DIRECTION('ref_axis',(-1.,-1.22464679914735E-16,0.));
#129210=DIRECTION('center_axis',(0.,0.,1.));
#129211=DIRECTION('ref_axis',(1.,0.,0.));
#129212=DIRECTION('center_axis',(0.,0.,-1.));
#129213=DIRECTION('ref_axis',(-1.,0.,0.));
#129214=DIRECTION('center_axis',(0.,0.,1.));
#129215=DIRECTION('ref_axis',(1.,0.,0.));
#129216=DIRECTION('center_axis',(-1.,6.12323399573677E-17,0.));
#129217=DIRECTION('ref_axis',(0.,1.,0.));
#129218=DIRECTION('center_axis',(0.,-1.22464679914735E-16,-1.));
#129219=DIRECTION('ref_axis',(0.,-1.,1.22464679914735E-16));
#129220=DIRECTION('center_axis',(0.,0.,1.));
#129221=DIRECTION('ref_axis',(1.,0.,0.));
#129222=DIRECTION('center_axis',(0.,0.,1.));
#129223=DIRECTION('ref_axis',(1.,0.,0.));
#129224=DIRECTION('center_axis',(0.,0.,1.));
#129225=DIRECTION('ref_axis',(1.,0.,0.));
#129226=DIRECTION('center_axis',(0.,0.,1.));
#129227=DIRECTION('ref_axis',(1.,0.,0.));
#129228=DIRECTION('center_axis',(1.22464679914735E-16,-1.,0.));
#129229=DIRECTION('ref_axis',(-1.,-1.22464679914735E-16,0.));
#129230=DIRECTION('center_axis',(0.,0.,1.));
#129231=DIRECTION('ref_axis',(1.,0.,0.));
#129232=DIRECTION('center_axis',(0.,0.,1.));
#129233=DIRECTION('ref_axis',(1.,0.,0.));
#129234=DIRECTION('',(0.,0.,-1.));
#129235=DIRECTION('center_axis',(0.,0.,1.));
#129236=DIRECTION('ref_axis',(1.,0.,0.));
#129237=DIRECTION('center_axis',(0.,0.,1.));
#129238=DIRECTION('ref_axis',(1.,0.,0.));
#129239=DIRECTION('center_axis',(1.22464679914735E-16,-1.,0.));
#129240=DIRECTION('ref_axis',(-1.,-1.22464679914735E-16,0.));
#129241=DIRECTION('center_axis',(0.,0.,1.));
#129242=DIRECTION('ref_axis',(1.,0.,0.));
#129243=DIRECTION('center_axis',(0.,0.,-1.));
#129244=DIRECTION('ref_axis',(-1.,0.,0.));
#129245=DIRECTION('center_axis',(0.,0.,1.));
#129246=DIRECTION('ref_axis',(1.,0.,0.));
#129247=DIRECTION('center_axis',(-1.,0.,0.));
#129248=DIRECTION('ref_axis',(0.,0.,-1.));
#129249=DIRECTION('center_axis',(0.,1.,0.));
#129250=DIRECTION('ref_axis',(0.,0.,1.));
#129251=DIRECTION('center_axis',(-1.,0.,0.));
#129252=DIRECTION('ref_axis',(0.,0.,-1.));
#129253=DIRECTION('center_axis',(0.,1.,0.));
#129254=DIRECTION('ref_axis',(0.,0.,1.));
#129255=DIRECTION('center_axis',(-0.866025403784438,-0.500000000000001,
0.));
#129256=DIRECTION('ref_axis',(0.,0.,-1.));
#129257=DIRECTION('center_axis',(-0.500000000000001,0.866025403784438,0.));
#129258=DIRECTION('ref_axis',(0.,0.,1.));
#129259=DIRECTION('center_axis',(-0.499999999999998,-0.86602540378444,0.));
#129260=DIRECTION('ref_axis',(0.,0.,-1.));
#129261=DIRECTION('center_axis',(-0.86602540378444,0.499999999999998,0.));
#129262=DIRECTION('ref_axis',(0.,0.,1.));
#129263=DIRECTION('center_axis',(3.39128835318872E-15,-1.,0.));
#129264=DIRECTION('ref_axis',(0.,0.,-1.));
#129265=DIRECTION('center_axis',(-1.,-3.49148133884313E-15,0.));
#129266=DIRECTION('ref_axis',(0.,0.,1.));
#129267=DIRECTION('center_axis',(0.500000000000004,-0.866025403784436,0.));
#129268=DIRECTION('ref_axis',(0.,0.,-1.));
#129269=DIRECTION('center_axis',(-0.866025403784436,-0.500000000000004,
0.));
#129270=DIRECTION('ref_axis',(0.,0.,1.));
#129271=DIRECTION('center_axis',(0.866025403784442,-0.499999999999995,0.));
#129272=DIRECTION('ref_axis',(0.,0.,-1.));
#129273=DIRECTION('center_axis',(-0.499999999999995,-0.866025403784442,
0.));
#129274=DIRECTION('ref_axis',(0.,0.,1.));
#129275=DIRECTION('center_axis',(1.,0.,0.));
#129276=DIRECTION('ref_axis',(0.,0.,-1.));
#129277=DIRECTION('center_axis',(0.,-1.,0.));
#129278=DIRECTION('ref_axis',(0.,0.,1.));
#129279=DIRECTION('center_axis',(0.866025403784435,0.500000000000007,0.));
#129280=DIRECTION('ref_axis',(0.,0.,-1.));
#129281=DIRECTION('center_axis',(0.500000000000007,-0.866025403784435,0.));
#129282=DIRECTION('ref_axis',(0.,0.,1.));
#129283=DIRECTION('center_axis',(0.499999999999992,0.866025403784443,0.));
#129284=DIRECTION('ref_axis',(0.,0.,-1.));
#129285=DIRECTION('center_axis',(0.866025403784443,-0.499999999999992,0.));
#129286=DIRECTION('ref_axis',(0.,0.,1.));
#129287=DIRECTION('center_axis',(-1.01738650595661E-14,1.,0.));
#129288=DIRECTION('ref_axis',(0.,0.,-1.));
#129289=DIRECTION('center_axis',(1.,1.04744440165294E-14,0.));
#129290=DIRECTION('ref_axis',(0.,0.,1.));
#129291=DIRECTION('center_axis',(-0.500000000000011,0.866025403784433,0.));
#129292=DIRECTION('ref_axis',(0.,0.,-1.));
#129293=DIRECTION('center_axis',(0.866025403784433,0.50000000000001,0.));
#129294=DIRECTION('ref_axis',(0.,0.,1.));
#129295=DIRECTION('center_axis',(-0.866025403784445,0.499999999999989,0.));
#129296=DIRECTION('ref_axis',(0.,0.,-1.));
#129297=DIRECTION('center_axis',(0.499999999999989,0.866025403784445,0.));
#129298=DIRECTION('ref_axis',(0.,0.,1.));
#129299=DIRECTION('center_axis',(-0.866025403784438,-0.500000000000001,
0.));
#129300=DIRECTION('ref_axis',(0.,0.,-1.));
#129301=DIRECTION('center_axis',(-0.500000000000001,0.866025403784438,0.));
#129302=DIRECTION('ref_axis',(0.,0.,1.));
#129303=DIRECTION('center_axis',(-0.499999999999998,-0.86602540378444,0.));
#129304=DIRECTION('ref_axis',(0.,0.,-1.));
#129305=DIRECTION('center_axis',(-0.86602540378444,0.499999999999998,0.));
#129306=DIRECTION('ref_axis',(0.,0.,1.));
#129307=DIRECTION('center_axis',(3.39128835318872E-15,-1.,0.));
#129308=DIRECTION('ref_axis',(0.,0.,-1.));
#129309=DIRECTION('center_axis',(-1.,-3.49148133884313E-15,0.));
#129310=DIRECTION('ref_axis',(0.,0.,1.));
#129311=DIRECTION('center_axis',(0.500000000000004,-0.866025403784436,0.));
#129312=DIRECTION('ref_axis',(0.,0.,-1.));
#129313=DIRECTION('center_axis',(-0.866025403784436,-0.500000000000004,
0.));
#129314=DIRECTION('ref_axis',(0.,0.,1.));
#129315=DIRECTION('center_axis',(0.866025403784442,-0.499999999999995,0.));
#129316=DIRECTION('ref_axis',(0.,0.,-1.));
#129317=DIRECTION('center_axis',(-0.499999999999995,-0.866025403784442,
0.));
#129318=DIRECTION('ref_axis',(0.,0.,1.));
#129319=DIRECTION('center_axis',(1.,0.,0.));
#129320=DIRECTION('ref_axis',(0.,0.,-1.));
#129321=DIRECTION('center_axis',(0.,-1.,0.));
#129322=DIRECTION('ref_axis',(0.,0.,1.));
#129323=DIRECTION('center_axis',(0.866025403784435,0.500000000000007,0.));
#129324=DIRECTION('ref_axis',(0.,0.,-1.));
#129325=DIRECTION('center_axis',(0.500000000000007,-0.866025403784435,0.));
#129326=DIRECTION('ref_axis',(0.,0.,1.));
#129327=DIRECTION('center_axis',(0.499999999999992,0.866025403784443,0.));
#129328=DIRECTION('ref_axis',(0.,0.,-1.));
#129329=DIRECTION('center_axis',(0.866025403784443,-0.499999999999992,0.));
#129330=DIRECTION('ref_axis',(0.,0.,1.));
#129331=DIRECTION('center_axis',(-1.01738650595661E-14,1.,0.));
#129332=DIRECTION('ref_axis',(0.,0.,-1.));
#129333=DIRECTION('center_axis',(1.,1.04744440165294E-14,0.));
#129334=DIRECTION('ref_axis',(0.,0.,1.));
#129335=DIRECTION('center_axis',(-0.500000000000011,0.866025403784433,0.));
#129336=DIRECTION('ref_axis',(0.,0.,-1.));
#129337=DIRECTION('center_axis',(0.866025403784433,0.50000000000001,0.));
#129338=DIRECTION('ref_axis',(0.,0.,1.));
#129339=DIRECTION('center_axis',(-0.866025403784445,0.499999999999989,0.));
#129340=DIRECTION('ref_axis',(0.,0.,-1.));
#129341=DIRECTION('center_axis',(0.499999999999989,0.866025403784445,0.));
#129342=DIRECTION('ref_axis',(0.,0.,1.));
#129343=DIRECTION('axis',(0.,0.,1.));
#129344=DIRECTION('refdir',(1.,0.,0.));
#129345=DIRECTION('center_axis',(0.,0.,1.));
#129346=DIRECTION('ref_axis',(1.,0.,0.));
#129347=DIRECTION('center_axis',(0.,0.,1.));
#129348=DIRECTION('ref_axis',(1.,0.,0.));
#129349=DIRECTION('',(0.,0.,-1.));
#129350=DIRECTION('center_axis',(0.,0.,1.));
#129351=DIRECTION('ref_axis',(1.,0.,0.));
#129352=DIRECTION('center_axis',(0.,0.,1.));
#129353=DIRECTION('ref_axis',(1.,0.,0.));
#129354=DIRECTION('center_axis',(0.,0.,1.));
#129355=DIRECTION('ref_axis',(1.,0.,0.));
#129356=DIRECTION('',(0.,0.,-1.));
#129357=DIRECTION('center_axis',(0.,0.,1.));
#129358=DIRECTION('ref_axis',(1.,0.,0.));
#129359=DIRECTION('center_axis',(0.,0.,-1.));
#129360=DIRECTION('ref_axis',(-1.,0.,0.));
#129361=DIRECTION('center_axis',(0.,0.,1.));
#129362=DIRECTION('ref_axis',(1.,0.,0.));
#129363=DIRECTION('',(0.,0.,1.));
#129364=DIRECTION('center_axis',(0.,0.,1.));
#129365=DIRECTION('ref_axis',(1.,0.,0.));
#129366=DIRECTION('center_axis',(0.,0.,-1.));
#129367=DIRECTION('ref_axis',(-1.,0.,0.));
#129368=DIRECTION('center_axis',(0.,0.,1.));
#129369=DIRECTION('ref_axis',(1.,0.,0.));
#129370=DIRECTION('',(0.,0.,1.));
#129371=DIRECTION('center_axis',(0.,0.,1.));
#129372=DIRECTION('ref_axis',(1.,0.,0.));
#129373=DIRECTION('center_axis',(-0.5,-0.866025403784439,0.));
#129374=DIRECTION('ref_axis',(0.866025403784439,-0.5,0.));
#129375=DIRECTION('',(-0.866025403784439,0.5,0.));
#129376=DIRECTION('',(0.,0.,-1.));
#129377=DIRECTION('',(-0.866025403784439,0.5,0.));
#129378=DIRECTION('',(0.,0.,-1.));
#129379=DIRECTION('center_axis',(0.5,-0.866025403784439,0.));
#129380=DIRECTION('ref_axis',(0.866025403784439,0.5,0.));
#129381=DIRECTION('',(-0.866025403784439,-0.5,0.));
#129382=DIRECTION('',(0.,0.,-1.));
#129383=DIRECTION('',(-0.866025403784439,-0.5,0.));
#129384=DIRECTION('center_axis',(1.,1.38777878078145E-16,0.));
#129385=DIRECTION('ref_axis',(-1.38777878078145E-16,1.,0.));
#129386=DIRECTION('',(1.38777878078145E-16,-1.,0.));
#129387=DIRECTION('',(0.,0.,-1.));
#129388=DIRECTION('',(1.38777878078145E-16,-1.,0.));
#129389=DIRECTION('center_axis',(0.5,0.866025403784439,0.));
#129390=DIRECTION('ref_axis',(-0.866025403784439,0.5,0.));
#129391=DIRECTION('',(0.866025403784438,-0.5,0.));
#129392=DIRECTION('',(0.,0.,-1.));
#129393=DIRECTION('',(0.866025403784438,-0.5,0.));
#129394=DIRECTION('center_axis',(-0.5,0.866025403784439,0.));
#129395=DIRECTION('ref_axis',(-0.866025403784439,-0.5,0.));
#129396=DIRECTION('',(0.866025403784439,0.5,0.));
#129397=DIRECTION('',(0.,0.,-1.));
#129398=DIRECTION('',(0.866025403784439,0.5,0.));
#129399=DIRECTION('center_axis',(-1.,-1.38777878078144E-16,0.));
#129400=DIRECTION('ref_axis',(1.38777878078145E-16,-1.,0.));
#129401=DIRECTION('',(-1.38777878078144E-16,1.,0.));
#129402=DIRECTION('',(-1.38777878078144E-16,1.,0.));
#129403=DIRECTION('center_axis',(0.,0.,1.));
#129404=DIRECTION('ref_axis',(1.,0.,0.));
#129405=DIRECTION('center_axis',(0.,0.,1.));
#129406=DIRECTION('ref_axis',(1.,0.,0.));
#129407=DIRECTION('center_axis',(0.,0.,1.));
#129408=DIRECTION('ref_axis',(1.,0.,0.));
#129409=DIRECTION('center_axis',(0.,0.,1.));
#129410=DIRECTION('ref_axis',(1.,0.,0.));
#129411=DIRECTION('center_axis',(0.,0.,-1.));
#129412=DIRECTION('ref_axis',(1.,0.,0.));
#129413=DIRECTION('center_axis',(0.,0.,-1.));
#129414=DIRECTION('ref_axis',(1.,0.,0.));
#129415=DIRECTION('axis',(0.,0.,1.));
#129416=DIRECTION('refdir',(1.,0.,0.));
#129417=DIRECTION('center_axis',(-1.8547604288613E-34,-1.,8.30248970910064E-18));
#129418=DIRECTION('ref_axis',(-1.,0.,-2.23398100310589E-17));
#129419=DIRECTION('',(1.8547604288613E-34,1.,-8.30248970910064E-18));
#129420=DIRECTION('center_axis',(-1.8547604288613E-34,-1.,8.30248970910064E-18));
#129421=DIRECTION('ref_axis',(-1.,0.,-2.23398100310589E-17));
#129422=DIRECTION('center_axis',(-1.8547604288613E-34,-1.,8.30248970910064E-18));
#129423=DIRECTION('ref_axis',(-1.,0.,-2.23398100310589E-17));
#129424=DIRECTION('',(1.8547604288613E-34,1.,-8.30248970910064E-18));
#129425=DIRECTION('center_axis',(-1.8547604288613E-34,-1.,8.30248970910064E-18));
#129426=DIRECTION('ref_axis',(-1.,0.,-2.23398100310589E-17));
#129427=DIRECTION('center_axis',(-1.8547604288613E-34,-1.,8.30248970910064E-18));
#129428=DIRECTION('ref_axis',(-1.,0.,-2.23398100310589E-17));
#129429=DIRECTION('',(1.8547604288613E-34,1.,-8.30248970910064E-18));
#129430=DIRECTION('center_axis',(-1.8547604288613E-34,-1.,8.30248970910064E-18));
#129431=DIRECTION('ref_axis',(-1.,0.,-2.23398100310589E-17));
#129432=DIRECTION('',(1.8547604288613E-34,1.,-8.30248970910064E-18));
#129433=DIRECTION('center_axis',(-1.8547604288613E-34,-1.,8.30248970910064E-18));
#129434=DIRECTION('ref_axis',(-1.,0.,-2.23398100310589E-17));
#129435=DIRECTION('',(1.8547604288613E-34,1.,-8.30248970910064E-18));
#129436=DIRECTION('center_axis',(1.85999217976422E-14,1.,-1.41266321642785E-14));
#129437=DIRECTION('ref_axis',(-0.505304800152355,2.12071862805656E-14,0.862940935952739));
#129438=DIRECTION('center_axis',(-5.75903090556243E-16,1.,0.));
#129439=DIRECTION('ref_axis',(-1.,-5.75903090556243E-16,0.));
#129440=DIRECTION('',(0.707106781186546,0.707106781186549,-8.65956056235492E-17));
#129441=DIRECTION('center_axis',(5.75903090556247E-16,-1.,0.));
#129442=DIRECTION('ref_axis',(1.,5.75903090556247E-16,0.));
#129443=DIRECTION('',(-0.707106781186543,-0.707106781186552,-8.65956056235488E-17));
#129444=DIRECTION('center_axis',(5.7590309055625E-16,-1.,0.));
#129445=DIRECTION('ref_axis',(1.,5.7590309055625E-16,0.));
#129446=DIRECTION('',(5.7590309055625E-16,-1.,0.));
#129447=DIRECTION('center_axis',(-5.75903090556247E-16,1.,0.));
#129448=DIRECTION('ref_axis',(1.,5.75903090556247E-16,1.77635683940025E-15));
#129449=DIRECTION('center_axis',(5.7590309055625E-16,-1.,0.));
#129450=DIRECTION('ref_axis',(1.,5.7590309055625E-16,0.));
#129451=DIRECTION('',(5.7590309055625E-16,-1.,0.));
#129452=DIRECTION('center_axis',(-5.75903090556247E-16,1.,0.));
#129453=DIRECTION('ref_axis',(1.,5.75903090556247E-16,1.77635683940025E-15));
#129454=DIRECTION('center_axis',(5.7590309055625E-16,-1.,0.));
#129455=DIRECTION('ref_axis',(1.,5.7590309055625E-16,0.));
#129456=DIRECTION('',(5.7590309055625E-16,-1.,0.));
#129457=DIRECTION('center_axis',(5.7590309055625E-16,-1.,0.));
#129458=DIRECTION('ref_axis',(1.,5.7590309055625E-16,0.));
#129459=DIRECTION('',(5.7590309055625E-16,-1.,0.));
#129460=DIRECTION('center_axis',(5.7590309055625E-16,-1.,0.));
#129461=DIRECTION('ref_axis',(1.,5.7590309055625E-16,0.));
#129462=DIRECTION('',(5.7590309055625E-16,-1.,0.));
#129463=DIRECTION('center_axis',(5.7590309055625E-16,-1.,0.));
#129464=DIRECTION('ref_axis',(1.,5.7590309055625E-16,0.));
#129465=DIRECTION('',(5.7590309055625E-16,-1.,0.));
#129466=DIRECTION('center_axis',(5.75903090556243E-16,-1.,0.));
#129467=DIRECTION('ref_axis',(-1.,-5.75903090556243E-16,0.));
#129468=DIRECTION('center_axis',(5.7590309055625E-16,-1.,0.));
#129469=DIRECTION('ref_axis',(1.,5.7590309055625E-16,0.));
#129470=DIRECTION('center_axis',(5.75903090556247E-16,-1.,0.));
#129471=DIRECTION('ref_axis',(1.,5.75903090556247E-16,0.));
#129472=DIRECTION('',(-0.707106781186543,-0.707106781186552,-8.65956056235488E-17));
#129473=DIRECTION('center_axis',(0.,1.,0.));
#129474=DIRECTION('ref_axis',(0.,0.,1.));
#129475=DIRECTION('center_axis',(-5.75903090556243E-16,1.,0.));
#129476=DIRECTION('ref_axis',(-1.,-5.75903090556243E-16,0.));
#129477=DIRECTION('',(0.707106781186546,0.707106781186549,-8.65956056235492E-17));
#129478=DIRECTION('center_axis',(0.,-1.,0.));
#129479=DIRECTION('ref_axis',(0.,0.,1.));
#129480=DIRECTION('center_axis',(0.,1.,0.));
#129481=DIRECTION('ref_axis',(0.,0.,1.));
#129482=DIRECTION('center_axis',(0.,1.,0.));
#129483=DIRECTION('ref_axis',(0.,0.,1.));
#129484=DIRECTION('center_axis',(0.,-1.,0.));
#129485=DIRECTION('ref_axis',(0.,0.,1.));
#129486=DIRECTION('center_axis',(0.,-1.,0.));
#129487=DIRECTION('ref_axis',(0.,0.,1.));
#129488=DIRECTION('center_axis',(0.,-1.,0.));
#129489=DIRECTION('ref_axis',(1.77635683940025E-15,0.,1.));
#129490=DIRECTION('center_axis',(0.,-1.,0.));
#129491=DIRECTION('ref_axis',(0.,0.,1.));
#129492=DIRECTION('center_axis',(0.,-1.,0.));
#129493=DIRECTION('ref_axis',(-8.88178419700125E-16,0.,1.));
#129494=DIRECTION('center_axis',(-0.866025403784439,-4.98746706539683E-16,
0.5));
#129495=DIRECTION('ref_axis',(0.5,1.55703595698071E-32,0.866025403784439));
#129496=DIRECTION('',(-5.7590309055625E-16,1.,0.));
#129497=DIRECTION('',(-5.7590309055625E-16,1.,0.));
#129498=DIRECTION('center_axis',(-0.866025403784439,-4.98746706539683E-16,
-0.5));
#129499=DIRECTION('ref_axis',(-0.5,-4.12937143755386E-33,0.866025403784439));
#129500=DIRECTION('',(-5.7590309055625E-16,1.,0.));
#129501=DIRECTION('center_axis',(0.,0.,-1.));
#129502=DIRECTION('ref_axis',(-1.,0.,0.));
#129503=DIRECTION('',(-5.7590309055625E-16,1.,0.));
#129504=DIRECTION('center_axis',(0.866025403784439,4.98746706539683E-16,
-0.5));
#129505=DIRECTION('ref_axis',(-0.5,-4.50262904462734E-32,-0.866025403784439));
#129506=DIRECTION('',(-5.7590309055625E-16,1.,0.));
#129507=DIRECTION('center_axis',(0.866025403784439,4.98746706539683E-16,
0.5));
#129508=DIRECTION('ref_axis',(0.5,1.3768929580165E-32,-0.866025403784439));
#129509=DIRECTION('',(-5.7590309055625E-16,1.,0.));
#129510=DIRECTION('center_axis',(0.,0.,1.));
#129511=DIRECTION('ref_axis',(1.,0.,0.));
#129512=DIRECTION('center_axis',(0.,1.,0.));
#129513=DIRECTION('ref_axis',(0.,0.,1.));
#129514=DIRECTION('center_axis',(0.,1.,0.));
#129515=DIRECTION('ref_axis',(0.,0.,1.));
#129516=DIRECTION('center_axis',(0.,1.,0.));
#129517=DIRECTION('ref_axis',(0.,0.,1.));
#129518=DIRECTION('center_axis',(0.,1.,0.));
#129519=DIRECTION('ref_axis',(0.,0.,1.));
#129520=DIRECTION('center_axis',(0.,1.,0.));
#129521=DIRECTION('ref_axis',(0.,0.,1.));
#129522=DIRECTION('center_axis',(0.,1.,0.));
#129523=DIRECTION('ref_axis',(0.,0.,1.));
#129524=DIRECTION('center_axis',(0.,1.,0.));
#129525=DIRECTION('ref_axis',(0.,0.,1.));
#129526=DIRECTION('center_axis',(0.,-1.,0.));
#129527=DIRECTION('ref_axis',(0.,0.,1.));
#129528=DIRECTION('center_axis',(0.,-1.,0.));
#129529=DIRECTION('ref_axis',(0.,0.,1.));
#129530=DIRECTION('center_axis',(0.,-1.,0.));
#129531=DIRECTION('ref_axis',(0.,0.,1.));
#129532=DIRECTION('center_axis',(0.,-1.,0.));
#129533=DIRECTION('ref_axis',(0.,0.,1.));
#129534=DIRECTION('center_axis',(0.,-1.,0.));
#129535=DIRECTION('ref_axis',(0.,0.,1.));
#129536=DIRECTION('center_axis',(0.,-1.,0.));
#129537=DIRECTION('ref_axis',(0.,0.,1.));
#129538=DIRECTION('center_axis',(0.,1.,0.));
#129539=DIRECTION('ref_axis',(0.,0.,1.));
#129540=DIRECTION('center_axis',(0.,1.,0.));
#129541=DIRECTION('ref_axis',(0.,0.,1.));
#129542=DIRECTION('center_axis',(0.,1.,0.));
#129543=DIRECTION('ref_axis',(0.,0.,1.));
#129544=DIRECTION('center_axis',(0.,1.,0.));
#129545=DIRECTION('ref_axis',(0.,0.,1.));
#129546=DIRECTION('center_axis',(0.,1.,0.));
#129547=DIRECTION('ref_axis',(0.,0.,1.));
#129548=DIRECTION('center_axis',(0.,1.,0.));
#129549=DIRECTION('ref_axis',(0.,0.,1.));
#129550=DIRECTION('center_axis',(-1.8547604288613E-34,-1.,8.30248970910064E-18));
#129551=DIRECTION('ref_axis',(-1.,0.,-2.23398100310589E-17));
#129552=DIRECTION('center_axis',(-1.8547604288613E-34,-1.,8.30248970910064E-18));
#129553=DIRECTION('ref_axis',(-1.,0.,-2.23398100310589E-17));
#129554=DIRECTION('',(1.8547604288613E-34,1.,-8.30248970910064E-18));
#129555=DIRECTION('center_axis',(-2.90604864291398E-15,-1.,-4.10722704360696E-16));
#129556=DIRECTION('ref_axis',(-0.743877835774618,2.42999009464821E-15,-0.668315618135077));
#129557=DIRECTION('center_axis',(-1.8547604288613E-34,-1.,8.30248970910064E-18));
#129558=DIRECTION('ref_axis',(-1.,0.,-2.23398100310589E-17));
#129559=DIRECTION('',(1.8547604288613E-34,1.,-8.30248970910064E-18));
#129560=DIRECTION('center_axis',(-1.8547604288613E-34,-1.,8.30248970910064E-18));
#129561=DIRECTION('ref_axis',(-1.,0.,-2.23398100310589E-17));
#129562=DIRECTION('',(1.8547604288613E-34,1.,-8.30248970910064E-18));
#129563=DIRECTION('center_axis',(-1.8547604288613E-34,-1.,8.30248970910064E-18));
#129564=DIRECTION('ref_axis',(-1.,0.,-2.23398100310589E-17));
#129565=DIRECTION('',(1.8547604288613E-34,1.,-8.30248970910064E-18));
#129566=DIRECTION('center_axis',(-1.8547604288613E-34,-1.,8.30248970910064E-18));
#129567=DIRECTION('ref_axis',(-1.,0.,-2.23398100310589E-17));
#129568=DIRECTION('',(1.8547604288613E-34,1.,-8.30248970910064E-18));
#129569=DIRECTION('center_axis',(-1.8547604288613E-34,-1.,8.30248970910064E-18));
#129570=DIRECTION('ref_axis',(-1.,0.,-2.23398100310589E-17));
#129571=DIRECTION('',(1.8547604288613E-34,1.,-8.30248970910064E-18));
#129572=DIRECTION('center_axis',(-5.7590309055625E-16,1.,0.));
#129573=DIRECTION('ref_axis',(-1.,0.,-2.23398100310589E-17));
#129574=DIRECTION('center_axis',(5.7590309055625E-16,-1.,0.));
#129575=DIRECTION('ref_axis',(1.,5.7590309055625E-16,0.));
#129576=DIRECTION('',(5.7590309055625E-16,-1.,0.));
#129577=DIRECTION('center_axis',(-5.7590309055625E-16,1.,0.));
#129578=DIRECTION('ref_axis',(-1.,-5.7590309055625E-16,0.));
#129579=DIRECTION('center_axis',(5.7590309055625E-16,-1.,0.));
#129580=DIRECTION('ref_axis',(1.,5.7590309055625E-16,0.));
#129581=DIRECTION('',(5.7590309055625E-16,-1.,0.));
#129582=DIRECTION('center_axis',(5.7590309055625E-16,-1.,0.));
#129583=DIRECTION('ref_axis',(1.,5.7590309055625E-16,0.));
#129584=DIRECTION('',(5.7590309055625E-16,-1.,0.));
#129585=DIRECTION('center_axis',(5.7590309055625E-16,-1.,0.));
#129586=DIRECTION('ref_axis',(1.,5.7590309055625E-16,0.));
#129587=DIRECTION('',(5.7590309055625E-16,-1.,0.));
#129588=DIRECTION('center_axis',(5.7590309055625E-16,-1.,0.));
#129589=DIRECTION('ref_axis',(1.,5.7590309055625E-16,0.));
#129590=DIRECTION('',(5.7590309055625E-16,-1.,0.));
#129591=DIRECTION('center_axis',(5.7590309055625E-16,-1.,0.));
#129592=DIRECTION('ref_axis',(1.,5.7590309055625E-16,0.));
#129593=DIRECTION('',(5.7590309055625E-16,-1.,0.));
#129594=DIRECTION('center_axis',(5.7590309055625E-16,-1.,0.));
#129595=DIRECTION('ref_axis',(1.,5.7590309055625E-16,0.));
#129596=DIRECTION('',(5.7590309055625E-16,-1.,0.));
#129597=DIRECTION('center_axis',(0.,-1.,0.));
#129598=DIRECTION('ref_axis',(0.,0.,1.));
#129599=DIRECTION('center_axis',(5.7590309055625E-16,-1.,0.));
#129600=DIRECTION('ref_axis',(1.,5.7590309055625E-16,0.));
#129601=DIRECTION('center_axis',(-6.12323399573677E-17,0.,1.));
#129602=DIRECTION('ref_axis',(-1.,0.,0.));
#129603=DIRECTION('center_axis',(4.12652725799652E-17,1.,0.));
#129604=DIRECTION('ref_axis',(-1.,4.12652725799652E-17,0.));
#129605=DIRECTION('center_axis',(-6.12323399573677E-17,0.,1.));
#129606=DIRECTION('ref_axis',(-1.,0.,0.));
#129607=DIRECTION('center_axis',(4.12652725799652E-17,1.,0.));
#129608=DIRECTION('ref_axis',(-1.,4.12652725799652E-17,0.));
#129609=DIRECTION('center_axis',(0.866025403784439,0.,0.5));
#129610=DIRECTION('ref_axis',(0.5,0.,-0.866025403784439));
#129611=DIRECTION('center_axis',(-4.32612527870318E-16,0.,1.));
#129612=DIRECTION('ref_axis',(1.,0.,4.32612527870318E-16));
#129613=DIRECTION('center_axis',(-0.866025403784439,0.,0.5));
#129614=DIRECTION('ref_axis',(0.5,0.,0.866025403784439));
#129615=DIRECTION('center_axis',(-0.866025403784439,0.,-0.5));
#129616=DIRECTION('ref_axis',(-0.5,0.,0.866025403784439));
#129617=DIRECTION('center_axis',(0.,0.,-1.));
#129618=DIRECTION('ref_axis',(-1.,0.,0.));
#129619=DIRECTION('center_axis',(0.866025403784438,0.,-0.500000000000001));
#129620=DIRECTION('ref_axis',(-0.500000000000001,0.,-0.866025403784438));
#129621=DIRECTION('center_axis',(0.,-1.,0.));
#129622=DIRECTION('ref_axis',(0.,0.,1.));
#129623=DIRECTION('',(-7.02428546843655E-17,0.819152044288991,0.573576436351047));
#129624=DIRECTION('center_axis',(0.,1.,0.));
#129625=DIRECTION('ref_axis',(0.,0.,1.));
#129626=DIRECTION('center_axis',(0.,1.,0.));
#129627=DIRECTION('ref_axis',(0.,0.,1.));
#129628=DIRECTION('',(-8.659560562355E-17,0.707106781186542,-0.707106781186553));
#129629=DIRECTION('center_axis',(0.,-1.,0.));
#129630=DIRECTION('ref_axis',(0.,0.,1.));
#129631=DIRECTION('center_axis',(0.,1.,0.));
#129632=DIRECTION('ref_axis',(0.,0.,1.));
#129633=DIRECTION('center_axis',(0.866025403784439,0.,0.5));
#129634=DIRECTION('ref_axis',(0.5,0.,-0.866025403784439));
#129635=DIRECTION('',(0.,-1.,0.));
#129636=DIRECTION('',(0.,-1.,0.));
#129637=DIRECTION('center_axis',(0.866025403784438,0.,-0.500000000000001));
#129638=DIRECTION('ref_axis',(-0.500000000000001,0.,-0.866025403784438));
#129639=DIRECTION('',(0.,-1.,0.));
#129640=DIRECTION('center_axis',(0.,0.,-1.));
#129641=DIRECTION('ref_axis',(-1.,0.,0.));
#129642=DIRECTION('',(0.,-1.,0.));
#129643=DIRECTION('center_axis',(-0.866025403784439,0.,-0.5));
#129644=DIRECTION('ref_axis',(-0.5,0.,0.866025403784439));
#129645=DIRECTION('',(0.,-1.,0.));
#129646=DIRECTION('center_axis',(-0.866025403784439,0.,0.5));
#129647=DIRECTION('ref_axis',(0.5,0.,0.866025403784439));
#129648=DIRECTION('',(0.,-1.,0.));
#129649=DIRECTION('center_axis',(-4.32612527870318E-16,0.,1.));
#129650=DIRECTION('ref_axis',(1.,0.,4.32612527870318E-16));
#129651=DIRECTION('center_axis',(4.12652725799652E-17,1.,0.));
#129652=DIRECTION('ref_axis',(-1.,4.12652725799652E-17,0.));
#129653=DIRECTION('center_axis',(-5.7590309055625E-16,1.,0.));
#129654=DIRECTION('ref_axis',(-1.,-5.7590309055625E-16,0.));
#129655=DIRECTION('center_axis',(-1.8547604288613E-34,-1.,8.30248970910064E-18));
#129656=DIRECTION('ref_axis',(-1.,0.,-2.23398100310589E-17));
#129657=DIRECTION('center_axis',(-1.8547604288613E-34,-1.,8.30248970910064E-18));
#129658=DIRECTION('ref_axis',(-1.,0.,-2.23398100310589E-17));
#129659=DIRECTION('',(-1.8547604288613E-34,-1.,8.30248970910064E-18));
#129660=DIRECTION('center_axis',(-4.29158568362712E-14,-1.,1.24422947616665E-14));
#129661=DIRECTION('ref_axis',(-1.,4.32980053228238E-14,1.0804960395692E-14));
#129662=DIRECTION('center_axis',(-5.75903090556246E-16,1.,0.));
#129663=DIRECTION('ref_axis',(-1.,-5.75903090556246E-16,0.));
#129664=DIRECTION('',(0.707106781186546,0.707106781186549,-8.65956056235492E-17));
#129665=DIRECTION('center_axis',(0.,1.,0.));
#129666=DIRECTION('ref_axis',(0.,0.,-1.));
#129667=DIRECTION('center_axis',(5.75903090556246E-16,-1.,0.));
#129668=DIRECTION('ref_axis',(-1.,-5.75903090556246E-16,-8.88178419700125E-16));
#129669=DIRECTION('center_axis',(5.7590309055625E-16,-1.,0.));
#129670=DIRECTION('ref_axis',(1.,5.7590309055625E-16,0.));
#129671=DIRECTION('center_axis',(0.,-1.,0.));
#129672=DIRECTION('ref_axis',(0.,0.,-1.));
#129673=DIRECTION('center_axis',(-1.8547604288613E-34,-1.,8.30248970910064E-18));
#129674=DIRECTION('ref_axis',(-1.,0.,-2.23398100310589E-17));
#129675=DIRECTION('center_axis',(0.,-1.,0.));
#129676=DIRECTION('ref_axis',(-1.,0.,-2.23398100310589E-17));
#129677=DIRECTION('center_axis',(0.,-1.,0.));
#129678=DIRECTION('ref_axis',(0.,0.,-1.));
#129679=DIRECTION('center_axis',(-1.8547604288613E-34,-1.,8.30248970910064E-18));
#129680=DIRECTION('ref_axis',(-1.,0.,-2.23398100310589E-17));
#129681=DIRECTION('',(-1.8547604288613E-34,-1.,8.30248970910064E-18));
#129682=DIRECTION('center_axis',(-5.7590309055625E-16,1.,0.));
#129683=DIRECTION('ref_axis',(-1.,0.,-2.23398100310589E-17));
#129684=DIRECTION('center_axis',(-1.8547604288613E-34,-1.,8.30248970910064E-18));
#129685=DIRECTION('ref_axis',(-1.,0.,-2.23398100310589E-17));
#129686=DIRECTION('',(-1.8547604288613E-34,-1.,8.30248970910064E-18));
#129687=DIRECTION('center_axis',(-1.8547604288613E-34,-1.,8.30248970910064E-18));
#129688=DIRECTION('ref_axis',(-1.,0.,-2.23398100310589E-17));
#129689=DIRECTION('',(-1.8547604288613E-34,-1.,8.30248970910064E-18));
#129690=DIRECTION('center_axis',(-1.8547604288613E-34,-1.,8.30248970910064E-18));
#129691=DIRECTION('ref_axis',(-1.,0.,-2.23398100310589E-17));
#129692=DIRECTION('',(-1.8547604288613E-34,-1.,8.30248970910064E-18));
#129693=DIRECTION('center_axis',(-1.8547604288613E-34,-1.,8.30248970910064E-18));
#129694=DIRECTION('ref_axis',(-1.,0.,-2.23398100310589E-17));
#129695=DIRECTION('',(-1.8547604288613E-34,-1.,8.30248970910064E-18));
#129696=DIRECTION('center_axis',(-1.8547604288613E-34,-1.,8.30248970910064E-18));
#129697=DIRECTION('ref_axis',(-1.,0.,-2.23398100310589E-17));
#129698=DIRECTION('',(-1.8547604288613E-34,-1.,8.30248970910064E-18));
#129699=DIRECTION('center_axis',(-1.8547604288613E-34,-1.,8.30248970910064E-18));
#129700=DIRECTION('ref_axis',(-1.,0.,-2.23398100310589E-17));
#129701=DIRECTION('',(-1.8547604288613E-34,-1.,8.30248970910064E-18));
#129702=DIRECTION('center_axis',(-1.8547604288613E-34,-1.,8.30248970910064E-18));
#129703=DIRECTION('ref_axis',(-1.,0.,-2.23398100310589E-17));
#129704=DIRECTION('',(-1.8547604288613E-34,-1.,8.30248970910064E-18));
#129705=DIRECTION('center_axis',(-1.8547604288613E-34,-1.,8.30248970910064E-18));
#129706=DIRECTION('ref_axis',(-1.,0.,-2.23398100310589E-17));
#129707=DIRECTION('',(-1.8547604288613E-34,-1.,8.30248970910064E-18));
#129708=DIRECTION('center_axis',(-1.8547604288613E-34,-1.,8.30248970910064E-18));
#129709=DIRECTION('ref_axis',(-1.,0.,-2.23398100310589E-17));
#129710=DIRECTION('',(-1.8547604288613E-34,-1.,8.30248970910064E-18));
#129711=DIRECTION('center_axis',(-1.8547604288613E-34,-1.,8.30248970910064E-18));
#129712=DIRECTION('ref_axis',(-1.,0.,-2.23398100310589E-17));
#129713=DIRECTION('',(-1.8547604288613E-34,-1.,8.30248970910064E-18));
#129714=DIRECTION('center_axis',(-1.8547604288613E-34,-1.,8.30248970910064E-18));
#129715=DIRECTION('ref_axis',(-1.,0.,-2.23398100310589E-17));
#129716=DIRECTION('',(-1.8547604288613E-34,-1.,8.30248970910064E-18));
#129717=DIRECTION('center_axis',(-1.8547604288613E-34,-1.,8.30248970910064E-18));
#129718=DIRECTION('ref_axis',(-1.,0.,-2.23398100310589E-17));
#129719=DIRECTION('',(-1.8547604288613E-34,-1.,8.30248970910064E-18));
#129720=DIRECTION('center_axis',(-1.8547604288613E-34,-1.,8.30248970910064E-18));
#129721=DIRECTION('ref_axis',(-1.,0.,-2.23398100310589E-17));
#129722=DIRECTION('',(-1.8547604288613E-34,-1.,8.30248970910064E-18));
#129723=DIRECTION('center_axis',(-1.8547604288613E-34,-1.,8.30248970910064E-18));
#129724=DIRECTION('ref_axis',(-1.,0.,-2.23398100310589E-17));
#129725=DIRECTION('',(-1.8547604288613E-34,-1.,8.30248970910064E-18));
#129726=DIRECTION('center_axis',(-1.8547604288613E-34,-1.,8.30248970910064E-18));
#129727=DIRECTION('ref_axis',(-1.,0.,-2.23398100310589E-17));
#129728=DIRECTION('',(-1.8547604288613E-34,-1.,8.30248970910064E-18));
#129729=DIRECTION('center_axis',(-1.8547604288613E-34,-1.,8.30248970910064E-18));
#129730=DIRECTION('ref_axis',(-1.,0.,-2.23398100310589E-17));
#129731=DIRECTION('',(-1.8547604288613E-34,-1.,8.30248970910064E-18));
#129732=DIRECTION('center_axis',(-1.8547604288613E-34,-1.,8.30248970910064E-18));
#129733=DIRECTION('ref_axis',(-1.,0.,-2.23398100310589E-17));
#129734=DIRECTION('',(-1.8547604288613E-34,-1.,8.30248970910064E-18));
#129735=DIRECTION('center_axis',(-1.8547604288613E-34,-1.,8.30248970910064E-18));
#129736=DIRECTION('ref_axis',(-1.,0.,-2.23398100310589E-17));
#129737=DIRECTION('',(-1.8547604288613E-34,-1.,8.30248970910064E-18));
#129738=DIRECTION('center_axis',(-1.8547604288613E-34,-1.,8.30248970910064E-18));
#129739=DIRECTION('ref_axis',(-1.,0.,-2.23398100310589E-17));
#129740=DIRECTION('',(-1.8547604288613E-34,-1.,8.30248970910064E-18));
#129741=DIRECTION('center_axis',(-1.8547604288613E-34,-1.,8.30248970910064E-18));
#129742=DIRECTION('ref_axis',(-1.,0.,-2.23398100310589E-17));
#129743=DIRECTION('',(-1.8547604288613E-34,-1.,8.30248970910064E-18));
#129744=DIRECTION('center_axis',(0.,-1.,0.));
#129745=DIRECTION('ref_axis',(-1.,0.,-2.23398100310589E-17));
#129746=DIRECTION('center_axis',(-1.8547604288613E-34,-1.,8.30248970910064E-18));
#129747=DIRECTION('ref_axis',(-1.,0.,-2.23398100310589E-17));
#129748=DIRECTION('',(-1.8547604288613E-34,-1.,8.30248970910064E-18));
#129749=DIRECTION('center_axis',(-1.8547604288613E-34,-1.,8.30248970910064E-18));
#129750=DIRECTION('ref_axis',(-1.,0.,-2.23398100310589E-17));
#129751=DIRECTION('',(-1.8547604288613E-34,-1.,8.30248970910064E-18));
#129752=DIRECTION('center_axis',(-1.8547604288613E-34,-1.,8.30248970910064E-18));
#129753=DIRECTION('ref_axis',(-1.,0.,-2.23398100310589E-17));
#129754=DIRECTION('',(-1.8547604288613E-34,-1.,8.30248970910064E-18));
#129755=DIRECTION('center_axis',(-1.8547604288613E-34,-1.,8.30248970910064E-18));
#129756=DIRECTION('ref_axis',(-1.,0.,-2.23398100310589E-17));
#129757=DIRECTION('',(-1.8547604288613E-34,-1.,8.30248970910064E-18));
#129758=DIRECTION('center_axis',(-1.8547604288613E-34,-1.,8.30248970910064E-18));
#129759=DIRECTION('ref_axis',(-1.,0.,-2.23398100310589E-17));
#129760=DIRECTION('',(-1.8547604288613E-34,-1.,8.30248970910064E-18));
#129761=DIRECTION('center_axis',(-1.8547604288613E-34,-1.,8.30248970910064E-18));
#129762=DIRECTION('ref_axis',(-1.,0.,-2.23398100310589E-17));
#129763=DIRECTION('',(-1.8547604288613E-34,-1.,8.30248970910064E-18));
#129764=DIRECTION('center_axis',(-1.8547604288613E-34,-1.,8.30248970910064E-18));
#129765=DIRECTION('ref_axis',(-1.,0.,-2.23398100310589E-17));
#129766=DIRECTION('',(-1.8547604288613E-34,-1.,8.30248970910064E-18));
#129767=DIRECTION('center_axis',(-1.8547604288613E-34,-1.,8.30248970910064E-18));
#129768=DIRECTION('ref_axis',(-1.,0.,-2.23398100310589E-17));
#129769=DIRECTION('',(-1.8547604288613E-34,-1.,8.30248970910064E-18));
#129770=DIRECTION('center_axis',(-1.8547604288613E-34,-1.,8.30248970910064E-18));
#129771=DIRECTION('ref_axis',(-1.,0.,-2.23398100310589E-17));
#129772=DIRECTION('',(-1.8547604288613E-34,-1.,8.30248970910064E-18));
#129773=DIRECTION('center_axis',(-1.8547604288613E-34,-1.,8.30248970910064E-18));
#129774=DIRECTION('ref_axis',(-1.,0.,-2.23398100310589E-17));
#129775=DIRECTION('',(-1.8547604288613E-34,-1.,8.30248970910064E-18));
#129776=DIRECTION('center_axis',(-1.8547604288613E-34,-1.,8.30248970910064E-18));
#129777=DIRECTION('ref_axis',(-1.,0.,-2.23398100310589E-17));
#129778=DIRECTION('',(-1.8547604288613E-34,-1.,8.30248970910064E-18));
#129779=DIRECTION('center_axis',(-1.8547604288613E-34,-1.,8.30248970910064E-18));
#129780=DIRECTION('ref_axis',(-1.,0.,-2.23398100310589E-17));
#129781=DIRECTION('',(-1.8547604288613E-34,-1.,8.30248970910064E-18));
#129782=DIRECTION('center_axis',(5.7590309055625E-16,-1.,0.));
#129783=DIRECTION('ref_axis',(1.,5.7590309055625E-16,0.));
#129784=DIRECTION('',(-5.7590309055625E-16,1.,0.));
#129785=DIRECTION('center_axis',(5.7590309055625E-16,-1.,0.));
#129786=DIRECTION('ref_axis',(-1.,-5.7590309055625E-16,8.88178419700125E-16));
#129787=DIRECTION('center_axis',(5.7590309055625E-16,-1.,0.));
#129788=DIRECTION('ref_axis',(1.,5.7590309055625E-16,0.));
#129789=DIRECTION('',(-5.7590309055625E-16,1.,0.));
#129790=DIRECTION('center_axis',(5.7590309055625E-16,-1.,0.));
#129791=DIRECTION('ref_axis',(1.,5.7590309055625E-16,0.));
#129792=DIRECTION('',(-5.7590309055625E-16,1.,0.));
#129793=DIRECTION('center_axis',(5.7590309055625E-16,-1.,0.));
#129794=DIRECTION('ref_axis',(1.,5.7590309055625E-16,0.));
#129795=DIRECTION('',(-5.7590309055625E-16,1.,0.));
#129796=DIRECTION('center_axis',(5.7590309055625E-16,-1.,0.));
#129797=DIRECTION('ref_axis',(1.,5.7590309055625E-16,0.));
#129798=DIRECTION('',(-5.7590309055625E-16,1.,0.));
#129799=DIRECTION('center_axis',(5.7590309055625E-16,-1.,0.));
#129800=DIRECTION('ref_axis',(1.,5.7590309055625E-16,0.));
#129801=DIRECTION('',(-5.7590309055625E-16,1.,0.));
#129802=DIRECTION('center_axis',(5.7590309055625E-16,-1.,0.));
#129803=DIRECTION('ref_axis',(1.,5.7590309055625E-16,0.));
#129804=DIRECTION('',(-5.7590309055625E-16,1.,0.));
#129805=DIRECTION('center_axis',(5.7590309055625E-16,-1.,0.));
#129806=DIRECTION('ref_axis',(1.,5.7590309055625E-16,0.));
#129807=DIRECTION('',(-5.7590309055625E-16,1.,0.));
#129808=DIRECTION('center_axis',(5.7590309055625E-16,-1.,0.));
#129809=DIRECTION('ref_axis',(1.,5.7590309055625E-16,0.));
#129810=DIRECTION('',(-5.7590309055625E-16,1.,0.));
#129811=DIRECTION('center_axis',(5.7590309055625E-16,-1.,0.));
#129812=DIRECTION('ref_axis',(1.,5.7590309055625E-16,0.));
#129813=DIRECTION('',(-5.7590309055625E-16,1.,0.));
#129814=DIRECTION('center_axis',(5.7590309055625E-16,-1.,0.));
#129815=DIRECTION('ref_axis',(1.,5.7590309055625E-16,0.));
#129816=DIRECTION('',(-5.7590309055625E-16,1.,0.));
#129817=DIRECTION('center_axis',(5.7590309055625E-16,-1.,0.));
#129818=DIRECTION('ref_axis',(1.,5.7590309055625E-16,0.));
#129819=DIRECTION('',(-5.7590309055625E-16,1.,0.));
#129820=DIRECTION('center_axis',(5.7590309055625E-16,-1.,0.));
#129821=DIRECTION('ref_axis',(1.,5.7590309055625E-16,0.));
#129822=DIRECTION('',(-5.7590309055625E-16,1.,0.));
#129823=DIRECTION('center_axis',(5.7590309055625E-16,-1.,0.));
#129824=DIRECTION('ref_axis',(1.,5.7590309055625E-16,0.));
#129825=DIRECTION('',(-5.7590309055625E-16,1.,0.));
#129826=DIRECTION('center_axis',(-5.7590309055625E-16,1.,0.));
#129827=DIRECTION('ref_axis',(1.,5.7590309055625E-16,-3.5527136788005E-15));
#129828=DIRECTION('center_axis',(5.7590309055625E-16,-1.,0.));
#129829=DIRECTION('ref_axis',(1.,5.7590309055625E-16,0.));
#129830=DIRECTION('',(-5.7590309055625E-16,1.,0.));
#129831=DIRECTION('center_axis',(5.7590309055625E-16,-1.,0.));
#129832=DIRECTION('ref_axis',(1.,5.7590309055625E-16,0.));
#129833=DIRECTION('',(-5.7590309055625E-16,1.,0.));
#129834=DIRECTION('center_axis',(5.7590309055625E-16,-1.,0.));
#129835=DIRECTION('ref_axis',(1.,5.7590309055625E-16,0.));
#129836=DIRECTION('',(-5.7590309055625E-16,1.,0.));
#129837=DIRECTION('center_axis',(5.7590309055625E-16,-1.,0.));
#129838=DIRECTION('ref_axis',(1.,5.7590309055625E-16,0.));
#129839=DIRECTION('',(-5.7590309055625E-16,1.,0.));
#129840=DIRECTION('center_axis',(5.7590309055625E-16,-1.,0.));
#129841=DIRECTION('ref_axis',(1.,5.7590309055625E-16,0.));
#129842=DIRECTION('',(-5.7590309055625E-16,1.,0.));
#129843=DIRECTION('center_axis',(5.7590309055625E-16,-1.,0.));
#129844=DIRECTION('ref_axis',(1.,5.7590309055625E-16,0.));
#129845=DIRECTION('',(-5.7590309055625E-16,1.,0.));
#129846=DIRECTION('center_axis',(5.7590309055625E-16,-1.,0.));
#129847=DIRECTION('ref_axis',(1.,5.7590309055625E-16,0.));
#129848=DIRECTION('',(-5.7590309055625E-16,1.,0.));
#129849=DIRECTION('center_axis',(5.7590309055625E-16,-1.,0.));
#129850=DIRECTION('ref_axis',(1.,5.7590309055625E-16,0.));
#129851=DIRECTION('',(-5.7590309055625E-16,1.,0.));
#129852=DIRECTION('center_axis',(5.7590309055625E-16,-1.,0.));
#129853=DIRECTION('ref_axis',(1.,5.7590309055625E-16,0.));
#129854=DIRECTION('',(-5.7590309055625E-16,1.,0.));
#129855=DIRECTION('center_axis',(5.7590309055625E-16,-1.,0.));
#129856=DIRECTION('ref_axis',(1.,5.7590309055625E-16,0.));
#129857=DIRECTION('',(-5.7590309055625E-16,1.,0.));
#129858=DIRECTION('center_axis',(5.7590309055625E-16,-1.,0.));
#129859=DIRECTION('ref_axis',(1.,5.7590309055625E-16,0.));
#129860=DIRECTION('',(-5.7590309055625E-16,1.,0.));
#129861=DIRECTION('center_axis',(5.7590309055625E-16,-1.,0.));
#129862=DIRECTION('ref_axis',(1.,5.7590309055625E-16,0.));
#129863=DIRECTION('',(-5.7590309055625E-16,1.,0.));
#129864=DIRECTION('center_axis',(5.7590309055625E-16,-1.,0.));
#129865=DIRECTION('ref_axis',(1.,5.7590309055625E-16,0.));
#129866=DIRECTION('',(-5.7590309055625E-16,1.,0.));
#129867=DIRECTION('center_axis',(5.7590309055625E-16,-1.,0.));
#129868=DIRECTION('ref_axis',(1.,5.7590309055625E-16,0.));
#129869=DIRECTION('',(-5.7590309055625E-16,1.,0.));
#129870=DIRECTION('center_axis',(5.7590309055625E-16,-1.,0.));
#129871=DIRECTION('ref_axis',(1.,5.7590309055625E-16,0.));
#129872=DIRECTION('',(-5.7590309055625E-16,1.,0.));
#129873=DIRECTION('center_axis',(5.7590309055625E-16,-1.,0.));
#129874=DIRECTION('ref_axis',(1.,5.7590309055625E-16,0.));
#129875=DIRECTION('',(-5.7590309055625E-16,1.,0.));
#129876=DIRECTION('center_axis',(5.7590309055625E-16,-1.,0.));
#129877=DIRECTION('ref_axis',(1.,5.7590309055625E-16,0.));
#129878=DIRECTION('',(-5.7590309055625E-16,1.,0.));
#129879=DIRECTION('center_axis',(5.7590309055625E-16,-1.,0.));
#129880=DIRECTION('ref_axis',(1.,5.7590309055625E-16,0.));
#129881=DIRECTION('',(-5.7590309055625E-16,1.,0.));
#129882=DIRECTION('center_axis',(5.7590309055625E-16,-1.,0.));
#129883=DIRECTION('ref_axis',(1.,5.7590309055625E-16,0.));
#129884=DIRECTION('center_axis',(-5.7590309055625E-16,1.,0.));
#129885=DIRECTION('ref_axis',(-1.,-5.7590309055625E-16,0.));
#129886=DIRECTION('center_axis',(5.7590309055625E-16,-1.,0.));
#129887=DIRECTION('ref_axis',(1.,5.7590309055625E-16,0.));
#129888=DIRECTION('',(-0.707106781186543,-0.707106781186552,-8.65956056235488E-17));
#129889=DIRECTION('center_axis',(0.,1.,0.));
#129890=DIRECTION('ref_axis',(0.,0.,1.));
#129891=DIRECTION('center_axis',(-4.06800079821994E-15,1.,1.09435932434982E-14));
#129892=DIRECTION('ref_axis',(-0.0356547078254615,1.0603593140283E-14,-0.99936416876426));
#129893=DIRECTION('center_axis',(5.7590309055625E-16,-1.,0.));
#129894=DIRECTION('ref_axis',(1.,5.7590309055625E-16,0.));
#129895=DIRECTION('center_axis',(-1.00842205057537E-14,-1.,9.21063889230093E-14));
#129896=DIRECTION('ref_axis',(-0.481354876138532,8.48287451222583E-14,0.876525802938886));
#129897=DIRECTION('',(0.707106781186546,0.707106781186549,8.65956056235493E-17));
#129898=DIRECTION('center_axis',(-5.7590309055625E-16,1.,0.));
#129899=DIRECTION('ref_axis',(-1.,-5.7590309055625E-16,0.));
#129900=DIRECTION('center_axis',(5.7590309055625E-16,-1.,0.));
#129901=DIRECTION('ref_axis',(1.,5.7590309055625E-16,0.));
#129902=DIRECTION('center_axis',(0.,-1.,0.));
#129903=DIRECTION('ref_axis',(0.,0.,-1.));
#129904=DIRECTION('center_axis',(-1.8547604288613E-34,-1.,8.30248970910064E-18));
#129905=DIRECTION('ref_axis',(-1.,0.,-2.23398100310589E-17));
#129906=DIRECTION('center_axis',(-5.7590309055625E-16,1.,0.));
#129907=DIRECTION('ref_axis',(-1.,-5.7590309055625E-16,0.));
#129908=DIRECTION('center_axis',(0.,-1.,0.));
#129909=DIRECTION('ref_axis',(0.,0.,-1.));
#129910=DIRECTION('',(0.,0.,-1.));
#129911=DIRECTION('',(-1.,0.,0.));
#129912=DIRECTION('',(0.,0.,1.));
#129913=DIRECTION('',(1.,0.,0.));
#129914=DIRECTION('center_axis',(0.,-1.,0.));
#129915=DIRECTION('ref_axis',(0.,0.,-1.));
#129916=DIRECTION('',(0.,0.,-1.));
#129917=DIRECTION('',(1.,0.,0.));
#129918=DIRECTION('',(0.,0.,1.));
#129919=DIRECTION('',(-1.,0.,0.));
#129920=DIRECTION('center_axis',(0.,1.,0.));
#129921=DIRECTION('ref_axis',(0.,0.,1.));
#129922=DIRECTION('center_axis',(0.,1.,0.));
#129923=DIRECTION('ref_axis',(0.,0.,1.));
#129924=DIRECTION('center_axis',(0.,1.,0.));
#129925=DIRECTION('ref_axis',(0.,0.,1.));
#129926=DIRECTION('center_axis',(0.,1.,0.));
#129927=DIRECTION('ref_axis',(0.,0.,1.));
#129928=DIRECTION('center_axis',(0.,1.,0.));
#129929=DIRECTION('ref_axis',(0.,0.,1.));
#129930=DIRECTION('center_axis',(0.,1.,0.));
#129931=DIRECTION('ref_axis',(0.,0.,1.));
#129932=DIRECTION('center_axis',(-1.,0.,0.));
#129933=DIRECTION('ref_axis',(0.,0.,1.));
#129934=DIRECTION('',(0.,-1.,0.));
#129935=DIRECTION('',(0.,-1.,0.));
#129936=DIRECTION('center_axis',(0.,0.,1.));
#129937=DIRECTION('ref_axis',(1.,0.,0.));
#129938=DIRECTION('',(0.,-1.,0.));
#129939=DIRECTION('center_axis',(1.,0.,0.));
#129940=DIRECTION('ref_axis',(0.,0.,-1.));
#129941=DIRECTION('',(0.,-1.,0.));
#129942=DIRECTION('center_axis',(0.,0.,-1.));
#129943=DIRECTION('ref_axis',(-1.,0.,0.));
#129944=DIRECTION('center_axis',(0.866025403784439,4.98746706539683E-16,
0.5));
#129945=DIRECTION('ref_axis',(0.5,-2.05225318506028E-32,-0.866025403784439));
#129946=DIRECTION('',(-5.7590309055625E-16,1.,0.));
#129947=DIRECTION('',(-5.7590309055625E-16,1.,0.));
#129948=DIRECTION('center_axis',(0.,0.,1.));
#129949=DIRECTION('ref_axis',(1.,0.,0.));
#129950=DIRECTION('',(-5.7590309055625E-16,1.,0.));
#129951=DIRECTION('center_axis',(-0.866025403784439,-4.98746706539683E-16,
0.5));
#129952=DIRECTION('ref_axis',(0.5,-2.05225318506028E-32,0.866025403784439));
#129953=DIRECTION('',(-5.7590309055625E-16,1.,0.));
#129954=DIRECTION('center_axis',(-0.866025403784439,-4.98746706539683E-16,
-0.5));
#129955=DIRECTION('ref_axis',(-0.5,-1.07348290155056E-32,0.866025403784439));
#129956=DIRECTION('',(-5.7590309055625E-16,1.,0.));
#129957=DIRECTION('center_axis',(-1.66923844304129E-16,-9.61319578222781E-32,
-1.));
#129958=DIRECTION('ref_axis',(-1.,-9.085955592469E-64,1.66923844304129E-16));
#129959=DIRECTION('',(-5.7590309055625E-16,1.,0.));
#129960=DIRECTION('center_axis',(0.866025403784439,4.98746706539683E-16,
-0.5));
#129961=DIRECTION('ref_axis',(-0.5,-2.03743871581167E-32,-0.866025403784439));
#129962=DIRECTION('center_axis',(0.,1.,0.));
#129963=DIRECTION('ref_axis',(0.,0.,1.));
#129964=DIRECTION('center_axis',(0.,1.,0.));
#129965=DIRECTION('ref_axis',(0.,0.,1.));
#129966=DIRECTION('center_axis',(0.,-1.,0.));
#129967=DIRECTION('ref_axis',(0.,0.,1.));
#129968=DIRECTION('center_axis',(0.,-1.,0.));
#129969=DIRECTION('ref_axis',(0.,0.,1.));
#129970=DIRECTION('center_axis',(0.,-1.,0.));
#129971=DIRECTION('ref_axis',(1.77635683940025E-15,0.,1.));
#129972=DIRECTION('center_axis',(0.,-1.,0.));
#129973=DIRECTION('ref_axis',(0.,0.,1.));
#129974=DIRECTION('center_axis',(0.,-1.,0.));
#129975=DIRECTION('ref_axis',(1.77635683940025E-15,0.,1.));
#129976=DIRECTION('center_axis',(-2.16306263935159E-15,1.,3.41586791986892E-31));
#129977=DIRECTION('ref_axis',(7.38873627842809E-46,-3.41586791986892E-31,
1.));
#129978=DIRECTION('center_axis',(-2.16306263935159E-15,1.,3.41586791986892E-31));
#129979=DIRECTION('ref_axis',(7.38873627842809E-46,-3.41586791986892E-31,
1.));
#129980=DIRECTION('center_axis',(-2.16306263935159E-15,1.,3.41586791986892E-31));
#129981=DIRECTION('ref_axis',(7.38873627842809E-46,-3.41586791986892E-31,
1.));
#129982=DIRECTION('center_axis',(-2.16306263935159E-15,1.,3.41586791986892E-31));
#129983=DIRECTION('ref_axis',(7.38873627842809E-46,-3.41586791986892E-31,
1.));
#129984=DIRECTION('center_axis',(-2.16306263935159E-15,1.,3.41586791986892E-31));
#129985=DIRECTION('ref_axis',(7.38873627842809E-46,-3.41586791986892E-31,
1.));
#129986=DIRECTION('center_axis',(-2.16306263935159E-15,1.,3.41586791986892E-31));
#129987=DIRECTION('ref_axis',(7.38873627842809E-46,-3.41586791986892E-31,
1.));
#129988=DIRECTION('center_axis',(2.16306263935159E-15,-1.,-3.41586791986892E-31));
#129989=DIRECTION('ref_axis',(7.38873627842809E-46,-3.41586791986892E-31,
1.));
#129990=DIRECTION('center_axis',(2.16306263935159E-15,-1.,-3.41586791986892E-31));
#129991=DIRECTION('ref_axis',(7.38873627842809E-46,-3.41586791986892E-31,
1.));
#129992=DIRECTION('center_axis',(2.16306263935159E-15,-1.,-3.41586791986892E-31));
#129993=DIRECTION('ref_axis',(7.38873627842809E-46,-3.41586791986892E-31,
1.));
#129994=DIRECTION('center_axis',(2.16306263935159E-15,-1.,-3.41586791986892E-31));
#129995=DIRECTION('ref_axis',(7.38873627842809E-46,-3.41586791986892E-31,
1.));
#129996=DIRECTION('center_axis',(2.16306263935159E-15,-1.,-3.41586791986892E-31));
#129997=DIRECTION('ref_axis',(7.38873627842809E-46,-3.41586791986892E-31,
1.));
#129998=DIRECTION('center_axis',(2.16306263935159E-15,-1.,-3.41586791986892E-31));
#129999=DIRECTION('ref_axis',(7.38873627842809E-46,-3.41586791986892E-31,
1.));
#130000=DIRECTION('center_axis',(-5.7590309055625E-16,1.,0.));
#130001=DIRECTION('ref_axis',(-1.,-5.7590309055625E-16,0.));
#130002=DIRECTION('center_axis',(-1.8547604288613E-34,-1.,8.30248970910064E-18));
#130003=DIRECTION('ref_axis',(-1.,0.,-2.23398100310589E-17));
#130004=DIRECTION('center_axis',(0.,-1.,0.));
#130005=DIRECTION('ref_axis',(0.,0.,-1.));
#130006=DIRECTION('center_axis',(0.,-1.,0.));
#130007=DIRECTION('ref_axis',(0.,0.,-1.));
#130008=DIRECTION('',(0.,-1.,0.));
#130009=DIRECTION('center_axis',(0.,-1.,0.));
#130010=DIRECTION('ref_axis',(0.,0.,-1.));
#130011=DIRECTION('center_axis',(0.,-1.,0.));
#130012=DIRECTION('ref_axis',(0.,0.,-1.));
#130013=DIRECTION('center_axis',(0.,-1.,0.));
#130014=DIRECTION('ref_axis',(0.,0.,-1.));
#130015=DIRECTION('',(0.,-1.,0.));
#130016=DIRECTION('center_axis',(0.,-1.,0.));
#130017=DIRECTION('ref_axis',(0.,0.,-1.));
#130018=DIRECTION('center_axis',(0.,-1.,0.));
#130019=DIRECTION('ref_axis',(0.,0.,-1.));
#130020=DIRECTION('center_axis',(0.,-1.,0.));
#130021=DIRECTION('ref_axis',(0.,0.,-1.));
#130022=DIRECTION('',(0.,-1.,0.));
#130023=DIRECTION('center_axis',(0.,-1.,0.));
#130024=DIRECTION('ref_axis',(0.,0.,-1.));
#130025=DIRECTION('center_axis',(0.,-1.,0.));
#130026=DIRECTION('ref_axis',(0.,0.,-1.));
#130027=DIRECTION('center_axis',(0.,-1.,0.));
#130028=DIRECTION('ref_axis',(0.,0.,-1.));
#130029=DIRECTION('',(0.,-1.,0.));
#130030=DIRECTION('center_axis',(0.,-1.,0.));
#130031=DIRECTION('ref_axis',(0.,0.,-1.));
#130032=DIRECTION('center_axis',(0.,-1.,0.));
#130033=DIRECTION('ref_axis',(0.,0.,-1.));
#130034=DIRECTION('center_axis',(0.,-1.,0.));
#130035=DIRECTION('ref_axis',(0.,0.,-1.));
#130036=DIRECTION('',(0.,-1.,0.));
#130037=DIRECTION('center_axis',(0.,-1.,0.));
#130038=DIRECTION('ref_axis',(0.,0.,-1.));
#130039=DIRECTION('center_axis',(0.,-1.,0.));
#130040=DIRECTION('ref_axis',(0.,0.,-1.));
#130041=DIRECTION('center_axis',(0.,-1.,0.));
#130042=DIRECTION('ref_axis',(0.,0.,-1.));
#130043=DIRECTION('',(0.,-1.,0.));
#130044=DIRECTION('center_axis',(0.,-1.,0.));
#130045=DIRECTION('ref_axis',(0.,0.,-1.));
#130046=DIRECTION('center_axis',(0.,-1.,0.));
#130047=DIRECTION('ref_axis',(0.,0.,-1.));
#130048=DIRECTION('center_axis',(0.,-1.,0.));
#130049=DIRECTION('ref_axis',(0.,0.,-1.));
#130050=DIRECTION('',(0.,-1.,0.));
#130051=DIRECTION('center_axis',(0.,-1.,0.));
#130052=DIRECTION('ref_axis',(0.,0.,-1.));
#130053=DIRECTION('center_axis',(0.,-1.,0.));
#130054=DIRECTION('ref_axis',(0.,0.,-1.));
#130055=DIRECTION('center_axis',(0.,-1.,0.));
#130056=DIRECTION('ref_axis',(0.,0.,-1.));
#130057=DIRECTION('',(0.,-1.,0.));
#130058=DIRECTION('center_axis',(0.,-1.,0.));
#130059=DIRECTION('ref_axis',(0.,0.,-1.));
#130060=DIRECTION('center_axis',(0.,-1.,0.));
#130061=DIRECTION('ref_axis',(0.,0.,-1.));
#130062=DIRECTION('center_axis',(0.,-1.,0.));
#130063=DIRECTION('ref_axis',(0.,0.,-1.));
#130064=DIRECTION('',(0.,-1.,0.));
#130065=DIRECTION('center_axis',(0.,-1.,0.));
#130066=DIRECTION('ref_axis',(0.,0.,-1.));
#130067=DIRECTION('center_axis',(0.,-1.,0.));
#130068=DIRECTION('ref_axis',(0.,0.,-1.));
#130069=DIRECTION('center_axis',(0.,-1.,0.));
#130070=DIRECTION('ref_axis',(0.,0.,-1.));
#130071=DIRECTION('',(0.,1.,0.));
#130072=DIRECTION('center_axis',(0.,1.,0.));
#130073=DIRECTION('ref_axis',(0.,0.,1.));
#130074=DIRECTION('center_axis',(0.,1.,0.));
#130075=DIRECTION('ref_axis',(0.,0.,1.));
#130076=DIRECTION('center_axis',(0.,1.,0.));
#130077=DIRECTION('ref_axis',(0.,0.,1.));
#130078=DIRECTION('',(0.,1.,0.));
#130079=DIRECTION('center_axis',(0.,1.,0.));
#130080=DIRECTION('ref_axis',(0.,0.,1.));
#130081=DIRECTION('center_axis',(-6.12323399573677E-17,0.,1.));
#130082=DIRECTION('ref_axis',(-1.,0.,0.));
#130083=DIRECTION('center_axis',(1.22000879772301E-18,1.,0.));
#130084=DIRECTION('ref_axis',(-1.,1.22000879772301E-18,0.));
#130085=DIRECTION('center_axis',(1.22000879772301E-18,1.,0.));
#130086=DIRECTION('ref_axis',(-1.,1.22000879772301E-18,0.));
#130087=DIRECTION('center_axis',(0.,1.,0.));
#130088=DIRECTION('ref_axis',(0.,0.,1.));
#130089=DIRECTION('center_axis',(0.,1.,0.));
#130090=DIRECTION('ref_axis',(0.,0.,1.));
#130091=DIRECTION('center_axis',(-1.,0.,1.22464679914735E-16));
#130092=DIRECTION('ref_axis',(-1.22464679914735E-16,0.,-1.));
#130093=DIRECTION('center_axis',(0.,-1.,0.));
#130094=DIRECTION('ref_axis',(0.,0.,1.));
#130095=DIRECTION('center_axis',(0.,-1.,0.));
#130096=DIRECTION('ref_axis',(0.,0.,-1.));
#130097=DIRECTION('center_axis',(0.,-1.,0.));
#130098=DIRECTION('ref_axis',(0.,0.,-1.));
#130099=DIRECTION('center_axis',(-1.,0.,-1.22464679914735E-16));
#130100=DIRECTION('ref_axis',(-1.22464679914735E-16,0.,1.));
#130101=DIRECTION('center_axis',(0.,1.,0.));
#130102=DIRECTION('ref_axis',(0.,0.,-1.));
#130103=DIRECTION('center_axis',(0.,1.,0.));
#130104=DIRECTION('ref_axis',(0.,0.,-1.));
#130105=DIRECTION('center_axis',(0.,1.,0.));
#130106=DIRECTION('ref_axis',(0.,0.,1.));
#130107=DIRECTION('',(0.,1.,0.));
#130108=DIRECTION('center_axis',(0.,1.,0.));
#130109=DIRECTION('ref_axis',(0.,0.,1.));
#130110=DIRECTION('center_axis',(0.,1.,0.));
#130111=DIRECTION('ref_axis',(0.,0.,1.));
#130112=DIRECTION('center_axis',(1.,0.,-1.22464679914735E-16));
#130113=DIRECTION('ref_axis',(-1.22464679914735E-16,0.,-1.));
#130114=DIRECTION('center_axis',(0.,1.,0.));
#130115=DIRECTION('ref_axis',(0.,0.,1.));
#130116=DIRECTION('center_axis',(0.,1.,0.));
#130117=DIRECTION('ref_axis',(0.,0.,1.));
#130118=DIRECTION('',(0.,1.,0.));
#130119=DIRECTION('center_axis',(0.,1.,0.));
#130120=DIRECTION('ref_axis',(0.,0.,1.));
#130121=DIRECTION('center_axis',(0.,-1.,0.));
#130122=DIRECTION('ref_axis',(0.,0.,-1.));
#130123=DIRECTION('center_axis',(0.,-1.,0.));
#130124=DIRECTION('ref_axis',(0.,0.,-1.));
#130125=DIRECTION('center_axis',(0.,1.,0.));
#130126=DIRECTION('ref_axis',(0.,0.,1.));
#130127=DIRECTION('center_axis',(0.,-1.,0.));
#130128=DIRECTION('ref_axis',(0.,0.,-1.));
#130129=DIRECTION('center_axis',(0.,-1.,0.));
#130130=DIRECTION('ref_axis',(0.,0.,-1.));
#130131=DIRECTION('center_axis',(0.,-1.,0.));
#130132=DIRECTION('ref_axis',(0.,0.,-1.));
#130133=DIRECTION('center_axis',(0.,-1.,0.));
#130134=DIRECTION('ref_axis',(0.,0.,-1.));
#130135=DIRECTION('center_axis',(0.,-1.,0.));
#130136=DIRECTION('ref_axis',(0.,0.,-1.));
#130137=DIRECTION('center_axis',(0.,-1.,0.));
#130138=DIRECTION('ref_axis',(0.,0.,-1.));
#130139=DIRECTION('center_axis',(0.,-1.,0.));
#130140=DIRECTION('ref_axis',(0.,0.,-1.));
#130141=DIRECTION('center_axis',(0.,-1.,0.));
#130142=DIRECTION('ref_axis',(0.,0.,-1.));
#130143=DIRECTION('center_axis',(0.,-1.,0.));
#130144=DIRECTION('ref_axis',(0.,0.,-1.));
#130145=DIRECTION('center_axis',(0.,1.,0.));
#130146=DIRECTION('ref_axis',(0.,0.,1.));
#130147=DIRECTION('axis',(0.,0.,1.));
#130148=DIRECTION('refdir',(1.,0.,0.));
#130149=DIRECTION('center_axis',(0.,0.,-1.));
#130150=DIRECTION('ref_axis',(-1.,0.,0.));
#130151=DIRECTION('',(0.,1.,0.));
#130152=DIRECTION('',(-1.,0.,0.));
#130153=DIRECTION('',(0.,-1.,0.));
#130154=DIRECTION('',(1.,0.,0.));
#130155=DIRECTION('',(0.,1.,0.));
#130156=DIRECTION('',(1.,0.,0.));
#130157=DIRECTION('',(0.,-1.,0.));
#130158=DIRECTION('',(-1.,0.,0.));
#130159=DIRECTION('center_axis',(0.,0.,-1.));
#130160=DIRECTION('ref_axis',(-1.,0.,0.));
#130161=DIRECTION('',(0.,1.,0.));
#130162=DIRECTION('',(1.,0.,0.));
#130163=DIRECTION('',(0.,-1.,0.));
#130164=DIRECTION('',(-1.,0.,0.));
#130165=DIRECTION('',(1.,0.,0.));
#130166=DIRECTION('',(0.,1.,0.));
#130167=DIRECTION('',(-1.,0.,0.));
#130168=DIRECTION('',(0.,-1.,0.));
#130169=DIRECTION('center_axis',(-1.,0.,0.));
#130170=DIRECTION('ref_axis',(0.,0.,1.));
#130171=DIRECTION('',(0.,0.,-1.));
#130172=DIRECTION('',(0.,0.,-1.));
#130173=DIRECTION('center_axis',(0.,-1.,0.));
#130174=DIRECTION('ref_axis',(0.,0.,-1.));
#130175=DIRECTION('',(0.,0.,-1.));
#130176=DIRECTION('center_axis',(1.,0.,0.));
#130177=DIRECTION('ref_axis',(0.,0.,-1.));
#130178=DIRECTION('',(0.,0.,-1.));
#130179=DIRECTION('center_axis',(0.,1.,0.));
#130180=DIRECTION('ref_axis',(0.,0.,1.));
#130181=DIRECTION('center_axis',(-1.,0.,0.));
#130182=DIRECTION('ref_axis',(0.,0.,1.));
#130183=DIRECTION('',(0.,0.,-1.));
#130184=DIRECTION('',(0.,0.,-1.));
#130185=DIRECTION('center_axis',(0.,-1.,0.));
#130186=DIRECTION('ref_axis',(0.,0.,-1.));
#130187=DIRECTION('',(0.,0.,-1.));
#130188=DIRECTION('center_axis',(1.,0.,0.));
#130189=DIRECTION('ref_axis',(0.,0.,-1.));
#130190=DIRECTION('',(0.,0.,-1.));
#130191=DIRECTION('center_axis',(0.,1.,0.));
#130192=DIRECTION('ref_axis',(0.,0.,1.));
#130193=DIRECTION('axis',(0.,0.,1.));
#130194=DIRECTION('refdir',(1.,0.,0.));
#130195=DIRECTION('center_axis',(-1.,0.,0.));
#130196=DIRECTION('ref_axis',(0.,0.,1.));
#130197=DIRECTION('',(0.,1.,0.));
#130198=DIRECTION('',(0.,0.,-1.));
#130199=DIRECTION('',(0.,1.,0.));
#130200=DIRECTION('',(0.,0.,-1.));
#130201=DIRECTION('center_axis',(0.,-1.,0.));
#130202=DIRECTION('ref_axis',(0.,0.,-1.));
#130203=DIRECTION('',(-1.,0.,0.));
#130204=DIRECTION('',(0.,0.,-1.));
#130205=DIRECTION('',(-1.,0.,0.));
#130206=DIRECTION('center_axis',(1.,4.2700885562506E-16,0.));
#130207=DIRECTION('ref_axis',(-4.2700885562506E-16,1.,0.));
#130208=DIRECTION('',(4.2700885562506E-16,-1.,0.));
#130209=DIRECTION('',(0.,0.,-1.));
#130210=DIRECTION('',(4.2700885562506E-16,-1.,0.));
#130211=DIRECTION('center_axis',(-5.55111512312578E-16,1.,0.));
#130212=DIRECTION('ref_axis',(-1.,-5.55111512312578E-16,0.));
#130213=DIRECTION('',(1.,5.55111512312578E-16,0.));
#130214=DIRECTION('',(1.,5.55111512312578E-16,0.));
#130215=DIRECTION('center_axis',(0.,0.,-1.));
#130216=DIRECTION('ref_axis',(-1.,0.,0.));
#130217=DIRECTION('center_axis',(0.,0.,-1.));
#130218=DIRECTION('ref_axis',(-1.,0.,0.));
#130219=DIRECTION('axis',(0.,0.,1.));
#130220=DIRECTION('refdir',(1.,0.,0.));
#130221=DIRECTION('axis',(0.,0.,1.));
#130222=DIRECTION('refdir',(1.,0.,0.));
#130223=DIRECTION('center_axis',(0.,-1.,0.));
#130224=DIRECTION('ref_axis',(0.,0.,-1.));
#130225=DIRECTION('center_axis',(0.,-1.,0.));
#130226=DIRECTION('ref_axis',(0.,0.,-1.));
#130227=DIRECTION('',(0.,-1.,0.));
#130228=DIRECTION('center_axis',(0.,-1.,0.));
#130229=DIRECTION('ref_axis',(0.,0.,-1.));
#130230=DIRECTION('center_axis',(0.,-1.,0.));
#130231=DIRECTION('ref_axis',(0.,0.,-1.));
#130232=DIRECTION('center_axis',(0.,-1.,0.));
#130233=DIRECTION('ref_axis',(0.,0.,1.));
#130234=DIRECTION('',(0.,-1.,0.));
#130235=DIRECTION('center_axis',(0.,-1.,0.));
#130236=DIRECTION('ref_axis',(0.,0.,-1.));
#130237=DIRECTION('center_axis',(1.,0.,0.));
#130238=DIRECTION('ref_axis',(0.,0.,-1.));
#130239=DIRECTION('center_axis',(-1.,-1.40133336246657E-16,0.));
#130240=DIRECTION('ref_axis',(1.40133336246657E-16,-1.,0.));
#130241=DIRECTION('',(1.,0.,0.));
#130242=DIRECTION('center_axis',(1.,0.,0.));
#130243=DIRECTION('ref_axis',(0.,0.,-1.));
#130244=DIRECTION('center_axis',(1.,0.,0.));
#130245=DIRECTION('ref_axis',(0.,0.,-1.));
#130246=DIRECTION('center_axis',(-1.,-1.40133336246657E-16,0.));
#130247=DIRECTION('ref_axis',(1.40133336246657E-16,-1.,0.));
#130248=DIRECTION('',(1.,0.,0.));
#130249=DIRECTION('center_axis',(1.,0.,0.));
#130250=DIRECTION('ref_axis',(0.,0.,-1.));
#130251=DIRECTION('center_axis',(1.,0.,0.));
#130252=DIRECTION('ref_axis',(0.,0.,-1.));
#130253=DIRECTION('center_axis',(-1.,-1.40133336246657E-16,0.));
#130254=DIRECTION('ref_axis',(1.40133336246657E-16,-1.,0.));
#130255=DIRECTION('',(1.,0.,0.));
#130256=DIRECTION('center_axis',(1.,0.,0.));
#130257=DIRECTION('ref_axis',(0.,0.,-1.));
#130258=DIRECTION('center_axis',(1.,0.,0.));
#130259=DIRECTION('ref_axis',(0.,0.,-1.));
#130260=DIRECTION('center_axis',(1.,0.,0.));
#130261=DIRECTION('ref_axis',(0.,0.,-1.));
#130262=DIRECTION('',(1.,0.,0.));
#130263=DIRECTION('center_axis',(1.,0.,0.));
#130264=DIRECTION('ref_axis',(0.,0.,-1.));
#130265=DIRECTION('center_axis',(1.,0.,0.));
#130266=DIRECTION('ref_axis',(0.,0.,-1.));
#130267=DIRECTION('center_axis',(1.,0.,0.));
#130268=DIRECTION('ref_axis',(0.,0.,-1.));
#130269=DIRECTION('',(1.,0.,0.));
#130270=DIRECTION('center_axis',(1.,0.,0.));
#130271=DIRECTION('ref_axis',(0.,0.,-1.));
#130272=DIRECTION('center_axis',(1.,0.,0.));
#130273=DIRECTION('ref_axis',(0.,0.,-1.));
#130274=DIRECTION('center_axis',(1.,0.,0.));
#130275=DIRECTION('ref_axis',(0.,0.,-1.));
#130276=DIRECTION('',(1.,0.,0.));
#130277=DIRECTION('center_axis',(1.,0.,0.));
#130278=DIRECTION('ref_axis',(0.,0.,-1.));
#130279=DIRECTION('center_axis',(0.,-0.450478595617232,0.892787228230068));
#130280=DIRECTION('ref_axis',(0.,-0.892787228230068,-0.450478595617232));
#130281=DIRECTION('',(1.,0.,0.));
#130282=DIRECTION('',(1.25109252850285E-16,-0.892787228230068,-0.450478595617232));
#130283=DIRECTION('',(1.,0.,0.));
#130284=DIRECTION('',(0.,-0.892787228230068,-0.450478595617232));
#130285=DIRECTION('',(1.,0.,0.));
#130286=DIRECTION('',(0.,-0.892787228230068,-0.450478595617232));
#130287=DIRECTION('',(1.,0.,0.));
#130288=DIRECTION('',(0.,0.892787228230068,0.450478595617232));
#130289=DIRECTION('center_axis',(0.,-0.450478595617233,-0.892787228230067));
#130290=DIRECTION('ref_axis',(0.,0.892787228230067,-0.450478595617233));
#130291=DIRECTION('',(1.,0.,0.));
#130292=DIRECTION('',(-1.25109252850285E-16,0.892787228230067,-0.450478595617233));
#130293=DIRECTION('',(-1.,0.,0.));
#130294=DIRECTION('',(0.,-0.892787228230067,0.450478595617233));
#130295=DIRECTION('',(1.,0.,0.));
#130296=DIRECTION('',(0.,0.892787228230067,-0.450478595617233));
#130297=DIRECTION('',(1.,0.,0.));
#130298=DIRECTION('',(0.,0.892787228230067,-0.450478595617233));
#130299=DIRECTION('center_axis',(0.,-1.,-2.31296463463574E-16));
#130300=DIRECTION('ref_axis',(0.,2.31296463463574E-16,-1.));
#130301=DIRECTION('',(-3.24123450872038E-32,2.31296463463574E-16,-1.));
#130302=DIRECTION('',(0.,2.31296463463574E-16,-1.));
#130303=DIRECTION('center_axis',(0.,-1.,-2.31296463463574E-16));
#130304=DIRECTION('ref_axis',(0.,2.31296463463574E-16,-1.));
#130305=DIRECTION('',(0.,-2.31296463463574E-16,1.));
#130306=DIRECTION('',(0.,2.31296463463574E-16,-1.));
#130307=DIRECTION('center_axis',(0.,1.,1.22464679914735E-16));
#130308=DIRECTION('ref_axis',(0.,-1.22464679914735E-16,1.));
#130309=DIRECTION('',(0.,-1.22464679914735E-16,1.));
#130310=DIRECTION('',(0.,-1.22464679914735E-16,1.));
#130311=DIRECTION('center_axis',(-1.,0.,0.));
#130312=DIRECTION('ref_axis',(0.,0.,1.));
#130313=DIRECTION('center_axis',(-1.,0.,0.));
#130314=DIRECTION('ref_axis',(0.,0.,1.));
#130315=DIRECTION('center_axis',(-1.,-1.40133336246657E-16,0.));
#130316=DIRECTION('ref_axis',(1.40133336246657E-16,-1.,0.));
#130317=DIRECTION('',(0.,0.,-1.));
#130318=DIRECTION('center_axis',(0.,-1.,0.));
#130319=DIRECTION('ref_axis',(0.,0.,-1.));
#130320=DIRECTION('',(0.,0.,-1.));
#130321=DIRECTION('center_axis',(1.,0.,0.));
#130322=DIRECTION('ref_axis',(0.,0.,-1.));
#130323=DIRECTION('axis',(0.,0.,1.));
#130324=DIRECTION('refdir',(1.,0.,0.));
#130325=DIRECTION('center_axis',(-1.,7.59645419660784E-65,0.));
#130326=DIRECTION('ref_axis',(0.,0.,1.));
#130327=DIRECTION('center_axis',(-1.,7.59645419660784E-65,0.));
#130328=DIRECTION('ref_axis',(0.,0.,1.));
#130329=DIRECTION('',(-1.,7.59645419660784E-65,0.));
#130330=DIRECTION('center_axis',(-1.,7.59645419660784E-65,0.));
#130331=DIRECTION('ref_axis',(0.,0.,1.));
#130332=DIRECTION('center_axis',(-1.,7.59645419660784E-65,0.));
#130333=DIRECTION('ref_axis',(0.,0.,1.));
#130334=DIRECTION('center_axis',(-1.,7.59645419660784E-65,0.));
#130335=DIRECTION('ref_axis',(0.,0.,1.));
#130336=DIRECTION('',(-1.,7.59645419660784E-65,0.));
#130337=DIRECTION('center_axis',(-1.,7.59645419660784E-65,0.));
#130338=DIRECTION('ref_axis',(0.,0.,1.));
#130339=DIRECTION('center_axis',(7.59645419660784E-65,-1.,0.));
#130340=DIRECTION('ref_axis',(0.,0.,-1.));
#130341=DIRECTION('',(-1.,0.,1.22464679914735E-16));
#130342=DIRECTION('',(0.,0.,1.));
#130343=DIRECTION('',(-1.,0.,1.22464679914735E-16));
#130344=DIRECTION('',(0.,0.,-1.));
#130345=DIRECTION('center_axis',(-7.59645419660784E-65,1.,0.));
#130346=DIRECTION('ref_axis',(0.,0.,1.));
#130347=DIRECTION('',(1.,-7.59645419660784E-65,0.));
#130348=DIRECTION('',(0.,0.,-1.));
#130349=DIRECTION('',(1.,-7.59645419660784E-65,0.));
#130350=DIRECTION('',(0.,0.,1.));
#130351=DIRECTION('center_axis',(0.,0.,-1.));
#130352=DIRECTION('ref_axis',(-1.,7.59645419660784E-65,0.));
#130353=DIRECTION('',(7.59645419660784E-65,-1.,0.));
#130354=DIRECTION('',(7.59645419660784E-65,-1.,0.));
#130355=DIRECTION('',(1.,-7.59645419660784E-65,0.));
#130356=DIRECTION('center_axis',(0.,0.,-1.));
#130357=DIRECTION('ref_axis',(-1.,7.59645419660784E-65,0.));
#130358=DIRECTION('',(7.59645419660784E-65,-1.,0.));
#130359=DIRECTION('',(1.,-7.59645419660784E-65,0.));
#130360=DIRECTION('',(7.59645419660784E-65,-1.,0.));
#130361=DIRECTION('center_axis',(1.22464679914735E-16,0.,1.));
#130362=DIRECTION('ref_axis',(1.,0.,-1.22464679914735E-16));
#130363=DIRECTION('',(-7.59645419660784E-65,1.,0.));
#130364=DIRECTION('',(-1.,0.,1.22464679914735E-16));
#130365=DIRECTION('',(7.59645419660784E-65,-1.,0.));
#130366=DIRECTION('center_axis',(1.22464679914735E-16,0.,1.));
#130367=DIRECTION('ref_axis',(1.,0.,-1.22464679914735E-16));
#130368=DIRECTION('',(-7.59645419660784E-65,1.,0.));
#130369=DIRECTION('',(7.59645419660784E-65,-1.,0.));
#130370=DIRECTION('',(-1.,0.,1.22464679914735E-16));
#130371=DIRECTION('center_axis',(7.59645419660784E-65,1.,0.));
#130372=DIRECTION('ref_axis',(1.,-7.59645419660784E-65,0.));
#130373=DIRECTION('',(0.,0.,-1.));
#130374=DIRECTION('',(0.,0.,1.));
#130375=DIRECTION('center_axis',(7.59645419660784E-65,1.,0.));
#130376=DIRECTION('ref_axis',(1.,-7.59645419660784E-65,0.));
#130377=DIRECTION('',(0.,0.,-1.));
#130378=DIRECTION('',(0.,0.,-1.));
#130379=DIRECTION('center_axis',(-7.59645419660784E-65,1.,0.));
#130380=DIRECTION('ref_axis',(0.,0.,1.));
#130381=DIRECTION('',(1.,-7.59645419660784E-65,0.));
#130382=DIRECTION('center_axis',(7.59645419660784E-65,-1.,0.));
#130383=DIRECTION('ref_axis',(0.,0.,1.));
#130384=DIRECTION('center_axis',(7.59645419660784E-65,-1.,0.));
#130385=DIRECTION('ref_axis',(1.,7.59645419660784E-65,0.));
#130386=DIRECTION('center_axis',(-7.59645419660784E-65,1.,0.));
#130387=DIRECTION('ref_axis',(0.,0.,1.));
#130388=DIRECTION('',(0.,0.,-1.));
#130389=DIRECTION('',(0.,0.,-1.));
#130390=DIRECTION('',(-1.,7.59645419660784E-65,0.));
#130391=DIRECTION('center_axis',(7.59645419660784E-65,-1.,0.));
#130392=DIRECTION('ref_axis',(0.,0.,-1.));
#130393=DIRECTION('center_axis',(7.59645419660784E-65,-1.,0.));
#130394=DIRECTION('ref_axis',(0.,0.,1.));
#130395=DIRECTION('',(-1.,7.59645419660784E-65,0.));
#130396=DIRECTION('center_axis',(7.59645419660784E-65,-1.,0.));
#130397=DIRECTION('ref_axis',(1.,7.59645419660784E-65,0.));
#130398=DIRECTION('center_axis',(-7.59645419660784E-65,1.,0.));
#130399=DIRECTION('ref_axis',(0.,0.,1.));
#130400=DIRECTION('center_axis',(7.59645419660784E-65,-1.,0.));
#130401=DIRECTION('ref_axis',(0.,0.,1.));
#130402=DIRECTION('center_axis',(7.59645419660784E-65,-1.,0.));
#130403=DIRECTION('ref_axis',(1.,7.59645419660784E-65,0.));
#130404=DIRECTION('center_axis',(7.59645419660784E-65,-1.,0.));
#130405=DIRECTION('ref_axis',(0.,0.,-1.));
#130406=DIRECTION('',(1.,-7.59645419660784E-65,0.));
#130407=DIRECTION('center_axis',(7.59645419660784E-65,-1.,0.));
#130408=DIRECTION('ref_axis',(0.,0.,1.));
#130409=DIRECTION('center_axis',(7.59645419660784E-65,-1.,0.));
#130410=DIRECTION('ref_axis',(1.,7.59645419660784E-65,0.));
#130411=DIRECTION('center_axis',(7.59645419660784E-65,-1.,0.));
#130412=DIRECTION('ref_axis',(0.,0.,-1.));
#130413=DIRECTION('',(0.,0.,-1.));
#130414=DIRECTION('',(0.,0.,-1.));
#130415=DIRECTION('center_axis',(7.59645419660784E-65,-1.,0.));
#130416=DIRECTION('ref_axis',(0.,0.,-1.));
#130417=DIRECTION('',(7.59645419660784E-65,-1.,0.));
#130418=DIRECTION('center_axis',(-1.,7.59645419660784E-65,0.));
#130419=DIRECTION('ref_axis',(0.,0.,1.));
#130420=DIRECTION('',(7.59645419660784E-65,-1.,0.));
#130421=DIRECTION('center_axis',(7.59645419660784E-65,-1.,0.));
#130422=DIRECTION('ref_axis',(0.,0.,-1.));
#130423=DIRECTION('center_axis',(7.59645419660784E-65,-1.,0.));
#130424=DIRECTION('ref_axis',(0.,0.,-1.));
#130425=DIRECTION('',(7.59645419660784E-65,-1.,0.));
#130426=DIRECTION('center_axis',(-1.,7.59645419660784E-65,0.));
#130427=DIRECTION('ref_axis',(0.,0.,1.));
#130428=DIRECTION('',(7.59645419660784E-65,-1.,0.));
#130429=DIRECTION('center_axis',(7.59645419660784E-65,-1.,0.));
#130430=DIRECTION('ref_axis',(0.,0.,-1.));
#130431=DIRECTION('center_axis',(1.,-7.59645419660784E-65,0.));
#130432=DIRECTION('ref_axis',(0.,0.,-1.));
#130433=DIRECTION('center_axis',(1.,-7.59645419660784E-65,0.));
#130434=DIRECTION('ref_axis',(0.,0.,-1.));
#130435=DIRECTION('',(0.,0.,1.));
#130436=DIRECTION('',(1.,0.,0.));
#130437=DIRECTION('',(5.40642287378652E-49,-2.22044604925031E-16,-1.));
#130438=DIRECTION('',(-1.,-3.97558035948902E-33,3.42113882891801E-49));
#130439=DIRECTION('axis',(0.,0.,1.));
#130440=DIRECTION('refdir',(1.,0.,0.));
#130441=DIRECTION('axis',(0.,0.,1.));
#130442=DIRECTION('refdir',(1.,0.,0.));
#130443=DIRECTION('center_axis',(0.,0.,1.));
#130444=DIRECTION('ref_axis',(-1.,0.,0.));
#130445=DIRECTION('',(-0.513541252058171,-6.28906650563163E-17,-0.858064905723644));
#130446=DIRECTION('center_axis',(-9.49891985197351E-13,2.74163925470746E-14,
1.));
#130447=DIRECTION('ref_axis',(0.353289074262459,-0.935514206202543,3.61145267726798E-13));
#130448=DIRECTION('center_axis',(-9.49891985197351E-13,2.74163925470746E-14,
1.));
#130449=DIRECTION('ref_axis',(0.353289074262459,-0.935514206202543,3.61145267726798E-13));
#130450=DIRECTION('center_axis',(0.,0.,1.));
#130451=DIRECTION('ref_axis',(-1.,0.,0.));
#130452=DIRECTION('',(-0.513541252058171,-6.28906650563163E-17,-0.858064905723644));
#130453=DIRECTION('center_axis',(0.,0.,-1.));
#130454=DIRECTION('ref_axis',(-1.,0.,0.));
#130455=DIRECTION('center_axis',(0.,0.,1.));
#130456=DIRECTION('ref_axis',(0.,-1.,0.));
#130457=DIRECTION('',(0.,0.,-1.));
#130458=DIRECTION('center_axis',(0.,0.,1.));
#130459=DIRECTION('ref_axis',(0.,-1.,0.));
#130460=DIRECTION('center_axis',(0.,0.,1.));
#130461=DIRECTION('ref_axis',(0.,-1.,0.));
#130462=DIRECTION('',(0.,0.,-1.));
#130463=DIRECTION('center_axis',(0.,0.,1.));
#130464=DIRECTION('ref_axis',(0.,-1.,0.));
#130465=DIRECTION('',(0.,0.,-1.));
#130466=DIRECTION('center_axis',(0.,0.,1.));
#130467=DIRECTION('ref_axis',(0.,-1.,0.));
#130468=DIRECTION('',(0.,0.,-1.));
#130469=DIRECTION('center_axis',(0.,0.,1.));
#130470=DIRECTION('ref_axis',(0.,-1.,0.));
#130471=DIRECTION('',(0.,0.,-1.));
#130472=DIRECTION('center_axis',(0.,0.,1.));
#130473=DIRECTION('ref_axis',(0.,-1.,0.));
#130474=DIRECTION('',(0.,0.,-1.));
#130475=DIRECTION('center_axis',(0.,0.,1.));
#130476=DIRECTION('ref_axis',(0.,-1.,0.));
#130477=DIRECTION('',(0.,0.,-1.));
#130478=DIRECTION('center_axis',(0.,0.,1.));
#130479=DIRECTION('ref_axis',(0.,-1.,0.));
#130480=DIRECTION('',(0.,0.,-1.));
#130481=DIRECTION('center_axis',(0.,0.,1.));
#130482=DIRECTION('ref_axis',(0.,-1.,0.));
#130483=DIRECTION('',(0.,0.,-1.));
#130484=DIRECTION('center_axis',(0.,0.,1.));
#130485=DIRECTION('ref_axis',(0.,-1.,0.));
#130486=DIRECTION('',(0.,0.,-1.));
#130487=DIRECTION('center_axis',(0.,0.,1.));
#130488=DIRECTION('ref_axis',(0.,-1.,0.));
#130489=DIRECTION('',(0.,0.,-1.));
#130490=DIRECTION('center_axis',(0.,0.,1.));
#130491=DIRECTION('ref_axis',(0.,-1.,0.));
#130492=DIRECTION('',(0.,0.,-1.));
#130493=DIRECTION('center_axis',(0.,0.,1.));
#130494=DIRECTION('ref_axis',(0.,-1.,0.));
#130495=DIRECTION('',(0.,0.,-1.));
#130496=DIRECTION('center_axis',(0.,0.,1.));
#130497=DIRECTION('ref_axis',(0.,-1.,0.));
#130498=DIRECTION('',(0.,0.,-1.));
#130499=DIRECTION('center_axis',(0.,0.,1.));
#130500=DIRECTION('ref_axis',(0.,-1.,0.));
#130501=DIRECTION('',(0.,0.,-1.));
#130502=DIRECTION('center_axis',(0.,0.,1.));
#130503=DIRECTION('ref_axis',(0.,-1.,0.));
#130504=DIRECTION('',(0.,0.,-1.));
#130505=DIRECTION('center_axis',(0.,0.,1.));
#130506=DIRECTION('ref_axis',(0.,-1.,0.));
#130507=DIRECTION('center_axis',(0.,0.,1.));
#130508=DIRECTION('ref_axis',(0.,-1.,0.));
#130509=DIRECTION('',(0.,0.,-1.));
#130510=DIRECTION('center_axis',(0.,0.,-1.));
#130511=DIRECTION('ref_axis',(-1.,0.,0.));
#130512=DIRECTION('',(0.,0.,-1.));
#130513=DIRECTION('center_axis',(0.,0.,-1.));
#130514=DIRECTION('ref_axis',(-1.,0.,0.));
#130515=DIRECTION('center_axis',(0.,0.,-1.));
#130516=DIRECTION('ref_axis',(7.84913906999881E-16,1.,0.));
#130517=DIRECTION('',(0.,0.,1.));
#130518=DIRECTION('center_axis',(0.,0.,-1.));
#130519=DIRECTION('ref_axis',(7.84913906999881E-16,1.,0.));
#130520=DIRECTION('',(0.,0.,1.));
#130521=DIRECTION('center_axis',(0.,0.,-1.));
#130522=DIRECTION('ref_axis',(7.84913906999881E-16,1.,0.));
#130523=DIRECTION('',(0.,0.,1.));
#130524=DIRECTION('center_axis',(0.,0.,-1.));
#130525=DIRECTION('ref_axis',(7.84913906999881E-16,1.,0.));
#130526=DIRECTION('',(0.,0.,1.));
#130527=DIRECTION('center_axis',(0.,0.,-1.));
#130528=DIRECTION('ref_axis',(7.84913906999881E-16,1.,0.));
#130529=DIRECTION('',(0.,0.,1.));
#130530=DIRECTION('center_axis',(0.,0.,-1.));
#130531=DIRECTION('ref_axis',(7.84913906999881E-16,1.,0.));
#130532=DIRECTION('',(0.,0.,1.));
#130533=DIRECTION('center_axis',(0.,0.,-1.));
#130534=DIRECTION('ref_axis',(7.84913906999881E-16,1.,0.));
#130535=DIRECTION('',(0.,0.,1.));
#130536=DIRECTION('center_axis',(0.,0.,-1.));
#130537=DIRECTION('ref_axis',(7.84913906999881E-16,1.,0.));
#130538=DIRECTION('',(0.,0.,1.));
#130539=DIRECTION('center_axis',(0.,0.,-1.));
#130540=DIRECTION('ref_axis',(7.84913906999881E-16,1.,0.));
#130541=DIRECTION('',(0.,0.,1.));
#130542=DIRECTION('center_axis',(0.,0.,-1.));
#130543=DIRECTION('ref_axis',(7.84913906999881E-16,1.,0.));
#130544=DIRECTION('',(0.,0.,1.));
#130545=DIRECTION('center_axis',(0.,0.,-1.));
#130546=DIRECTION('ref_axis',(7.84913906999881E-16,1.,0.));
#130547=DIRECTION('',(0.,0.,1.));
#130548=DIRECTION('center_axis',(0.,0.,-1.));
#130549=DIRECTION('ref_axis',(7.84913906999881E-16,1.,0.));
#130550=DIRECTION('',(0.,0.,1.));
#130551=DIRECTION('center_axis',(0.,0.,-1.));
#130552=DIRECTION('ref_axis',(7.84913906999881E-16,1.,0.));
#130553=DIRECTION('',(0.,0.,1.));
#130554=DIRECTION('center_axis',(0.,0.,-1.));
#130555=DIRECTION('ref_axis',(7.84913906999881E-16,1.,0.));
#130556=DIRECTION('',(0.,0.,1.));
#130557=DIRECTION('center_axis',(0.,0.,-1.));
#130558=DIRECTION('ref_axis',(7.84913906999881E-16,1.,0.));
#130559=DIRECTION('',(0.,0.,1.));
#130560=DIRECTION('center_axis',(0.,0.,-1.));
#130561=DIRECTION('ref_axis',(7.84913906999881E-16,1.,0.));
#130562=DIRECTION('',(0.,0.,1.));
#130563=DIRECTION('center_axis',(0.,0.,-1.));
#130564=DIRECTION('ref_axis',(7.84913906999881E-16,1.,0.));
#130565=DIRECTION('',(0.,0.,1.));
#130566=DIRECTION('center_axis',(0.,0.,1.));
#130567=DIRECTION('ref_axis',(7.84913906999881E-16,1.,0.));
#130568=DIRECTION('center_axis',(0.,8.12506049434301E-17,1.));
#130569=DIRECTION('ref_axis',(0.,-1.,8.12506049434301E-17));
#130570=DIRECTION('center_axis',(0.,0.,1.));
#130571=DIRECTION('ref_axis',(0.,-1.,0.));
#130572=DIRECTION('center_axis',(0.,0.,1.));
#130573=DIRECTION('ref_axis',(0.,-1.,0.));
#130574=DIRECTION('center_axis',(0.,0.,1.));
#130575=DIRECTION('ref_axis',(7.84913906999881E-16,1.,0.));
#130576=DIRECTION('',(8.659560562355E-17,-0.707106781186553,-0.707106781186542));
#130577=DIRECTION('center_axis',(0.,0.,-1.));
#130578=DIRECTION('ref_axis',(7.84913906999881E-16,1.,0.));
#130579=DIRECTION('center_axis',(0.,0.,1.));
#130580=DIRECTION('ref_axis',(1.,0.,0.));
#130581=DIRECTION('center_axis',(0.,0.,1.));
#130582=DIRECTION('ref_axis',(1.,0.,0.));
#130583=DIRECTION('center_axis',(0.,0.,1.));
#130584=DIRECTION('ref_axis',(1.,0.,0.));
#130585=DIRECTION('center_axis',(0.,0.,1.));
#130586=DIRECTION('ref_axis',(1.,0.,0.));
#130587=DIRECTION('',(0.,0.,1.));
#130588=DIRECTION('',(0.,0.,1.));
#130589=DIRECTION('',(0.,0.,1.));
#130590=DIRECTION('',(0.,0.,1.));
#130591=DIRECTION('',(0.,0.,1.));
#130592=DIRECTION('',(0.,0.,1.));
#130593=DIRECTION('',(0.,0.,1.));
#130594=DIRECTION('',(0.,0.,1.));
#130595=DIRECTION('',(0.,0.,1.));
#130596=DIRECTION('',(0.,0.,1.));
#130597=DIRECTION('',(0.,0.,1.));
#130598=DIRECTION('',(0.,0.,1.));
#130599=DIRECTION('',(0.,0.,1.));
#130600=DIRECTION('',(0.,0.,1.));
#130601=DIRECTION('',(0.,0.,1.));
#130602=DIRECTION('',(0.,0.,1.));
#130603=DIRECTION('center_axis',(0.,0.,1.));
#130604=DIRECTION('ref_axis',(1.,0.,0.));
#130605=DIRECTION('center_axis',(0.,0.,1.));
#130606=DIRECTION('ref_axis',(1.,0.,0.));
#130607=DIRECTION('center_axis',(0.,0.,1.));
#130608=DIRECTION('ref_axis',(1.,0.,0.));
#130609=DIRECTION('',(0.,-1.,0.));
#130610=DIRECTION('',(1.,0.,0.));
#130611=DIRECTION('',(0.,1.,0.));
#130612=DIRECTION('',(-1.,0.,0.));
#130613=DIRECTION('',(0.,0.,1.));
#130614=DIRECTION('',(0.,0.,1.));
#130615=DIRECTION('',(0.,0.,1.));
#130616=DIRECTION('',(0.,0.,1.));
#130617=DIRECTION('',(0.,0.,1.));
#130618=DIRECTION('',(0.,0.,1.));
#130619=DIRECTION('',(0.,0.,1.));
#130620=DIRECTION('',(0.,0.,1.));
#130621=DIRECTION('',(0.,0.,1.));
#130622=DIRECTION('',(0.,0.,1.));
#130623=DIRECTION('',(0.,0.,1.));
#130624=DIRECTION('',(0.,0.,1.));
#130625=DIRECTION('',(0.,0.,1.));
#130626=DIRECTION('',(0.,0.,1.));
#130627=DIRECTION('',(0.,0.,1.));
#130628=DIRECTION('',(0.,0.,1.));
#130629=DIRECTION('center_axis',(1.,0.,0.));
#130630=DIRECTION('ref_axis',(0.,1.,0.));
#130631=DIRECTION('',(0.,0.,1.));
#130632=DIRECTION('',(0.,0.,1.));
#130633=DIRECTION('',(0.,1.,0.));
#130634=DIRECTION('center_axis',(0.,1.,0.));
#130635=DIRECTION('ref_axis',(1.,0.,0.));
#130636=DIRECTION('',(0.,0.,1.));
#130637=DIRECTION('',(-1.,0.,0.));
#130638=DIRECTION('center_axis',(-1.,0.,0.));
#130639=DIRECTION('ref_axis',(0.,0.,1.));
#130640=DIRECTION('',(0.,0.,1.));
#130641=DIRECTION('',(0.,-1.,0.));
#130642=DIRECTION('center_axis',(0.,-1.,0.));
#130643=DIRECTION('ref_axis',(0.,0.,-1.));
#130644=DIRECTION('',(1.,0.,0.));
#130645=DIRECTION('center_axis',(0.,0.,1.));
#130646=DIRECTION('ref_axis',(1.,0.,0.));
#130647=DIRECTION('center_axis',(0.,0.,1.));
#130648=DIRECTION('ref_axis',(1.,0.,0.));
#130649=DIRECTION('center_axis',(0.,0.,1.));
#130650=DIRECTION('ref_axis',(1.,0.,0.));
#130651=DIRECTION('center_axis',(0.,0.,1.));
#130652=DIRECTION('ref_axis',(1.,0.,0.));
#130653=DIRECTION('center_axis',(0.,0.,1.));
#130654=DIRECTION('ref_axis',(1.,0.,0.));
#130655=DIRECTION('center_axis',(0.,0.,1.));
#130656=DIRECTION('ref_axis',(1.,0.,0.));
#130657=DIRECTION('center_axis',(0.,0.,1.));
#130658=DIRECTION('ref_axis',(1.,0.,0.));
#130659=DIRECTION('center_axis',(0.,0.,-1.));
#130660=DIRECTION('ref_axis',(1.,0.,0.));
#130661=DIRECTION('center_axis',(0.,0.,-1.));
#130662=DIRECTION('ref_axis',(1.,0.,0.));
#130663=DIRECTION('center_axis',(0.,0.,-1.));
#130664=DIRECTION('ref_axis',(1.,0.,0.));
#130665=DIRECTION('center_axis',(0.,0.,-1.));
#130666=DIRECTION('ref_axis',(1.,0.,0.));
#130667=DIRECTION('center_axis',(0.,0.,-1.));
#130668=DIRECTION('ref_axis',(1.,0.,0.));
#130669=DIRECTION('center_axis',(0.,0.,-1.));
#130670=DIRECTION('ref_axis',(1.,0.,0.));
#130671=DIRECTION('center_axis',(0.5,0.866025403784439,0.));
#130672=DIRECTION('ref_axis',(0.,0.,-1.));
#130673=DIRECTION('',(0.,0.,-1.));
#130674=DIRECTION('',(0.866025403784439,-0.5,0.));
#130675=DIRECTION('',(0.,0.,-1.));
#130676=DIRECTION('center_axis',(-0.5,0.866025403784439,0.));
#130677=DIRECTION('ref_axis',(0.,0.,1.));
#130678=DIRECTION('',(0.866025403784439,0.5,0.));
#130679=DIRECTION('',(0.,0.,-1.));
#130680=DIRECTION('center_axis',(-1.,0.,0.));
#130681=DIRECTION('ref_axis',(0.,0.,1.));
#130682=DIRECTION('',(0.,1.,0.));
#130683=DIRECTION('',(0.,0.,-1.));
#130684=DIRECTION('center_axis',(-0.5,-0.866025403784439,0.));
#130685=DIRECTION('ref_axis',(-0.866025403784439,0.5,0.));
#130686=DIRECTION('',(-0.866025403784439,0.5,0.));
#130687=DIRECTION('',(0.,0.,-1.));
#130688=DIRECTION('center_axis',(0.5,-0.866025403784439,0.));
#130689=DIRECTION('ref_axis',(0.,0.,-1.));
#130690=DIRECTION('',(-0.866025403784439,-0.5,0.));
#130691=DIRECTION('',(0.,0.,-1.));
#130692=DIRECTION('center_axis',(1.,1.58138378814438E-16,0.));
#130693=DIRECTION('ref_axis',(-1.58138378814438E-16,1.,0.));
#130694=DIRECTION('',(1.58138378814438E-16,-1.,0.));
#130695=DIRECTION('center_axis',(0.,0.,1.));
#130696=DIRECTION('ref_axis',(1.,0.,0.));
#130697=DIRECTION('center_axis',(0.,0.,1.));
#130698=DIRECTION('ref_axis',(0.,-1.,0.));
#130699=DIRECTION('center_axis',(0.,0.,1.));
#130700=DIRECTION('ref_axis',(-1.,0.,0.));
#130701=DIRECTION('axis',(0.,0.,1.));
#130702=DIRECTION('refdir',(1.,0.,0.));
#130703=DIRECTION('center_axis',(0.,0.,1.));
#130704=DIRECTION('ref_axis',(1.,0.,0.));
#130705=DIRECTION('',(-0.70710678118655,-8.65956056235497E-17,0.707106781186545));
#130706=DIRECTION('center_axis',(0.,0.,1.));
#130707=DIRECTION('ref_axis',(-6.16388274026379E-15,1.,0.));
#130708=DIRECTION('center_axis',(0.,0.,-1.));
#130709=DIRECTION('ref_axis',(-1.,0.,0.));
#130710=DIRECTION('',(0.,0.,-1.));
#130711=DIRECTION('center_axis',(0.,0.,-1.));
#130712=DIRECTION('ref_axis',(1.,0.,0.));
#130713=DIRECTION('center_axis',(0.,0.,-1.));
#130714=DIRECTION('ref_axis',(-1.,0.,0.));
#130715=DIRECTION('',(0.,0.,-1.));
#130716=DIRECTION('center_axis',(0.,0.,-1.));
#130717=DIRECTION('ref_axis',(-1.,0.,0.));
#130718=DIRECTION('',(0.,0.,-1.));
#130719=DIRECTION('center_axis',(0.,0.,-1.));
#130720=DIRECTION('ref_axis',(-1.,0.,0.));
#130721=DIRECTION('',(0.,0.,-1.));
#130722=DIRECTION('center_axis',(0.,0.,-1.));
#130723=DIRECTION('ref_axis',(-1.,0.,0.));
#130724=DIRECTION('',(0.,0.,-1.));
#130725=DIRECTION('center_axis',(0.,0.,1.));
#130726=DIRECTION('ref_axis',(1.,0.,0.));
#130727=DIRECTION('center_axis',(0.,0.,1.));
#130728=DIRECTION('ref_axis',(1.,0.,0.));
#130729=DIRECTION('center_axis',(0.,0.,1.));
#130730=DIRECTION('ref_axis',(-6.16388274026379E-15,1.,0.));
#130731=DIRECTION('',(0.,0.,1.));
#130732=DIRECTION('center_axis',(0.,0.,1.));
#130733=DIRECTION('ref_axis',(-6.16388274026379E-15,1.,0.));
#130734=DIRECTION('',(0.,0.,1.));
#130735=DIRECTION('center_axis',(0.,0.,1.));
#130736=DIRECTION('ref_axis',(-6.16388274026379E-15,1.,0.));
#130737=DIRECTION('',(0.,0.,1.));
#130738=DIRECTION('center_axis',(0.,0.,1.));
#130739=DIRECTION('ref_axis',(-6.16388274026379E-15,1.,0.));
#130740=DIRECTION('',(0.,0.,1.));
#130741=DIRECTION('center_axis',(0.,0.,-1.));
#130742=DIRECTION('ref_axis',(-6.16388274026379E-15,1.,0.));
#130743=DIRECTION('center_axis',(0.,0.,1.));
#130744=DIRECTION('ref_axis',(-6.16388274026379E-15,1.,0.));
#130745=DIRECTION('center_axis',(0.,0.,-1.));
#130746=DIRECTION('ref_axis',(-6.16388274026379E-15,1.,0.));
#130747=DIRECTION('center_axis',(0.,0.,-1.));
#130748=DIRECTION('ref_axis',(-1.,0.,0.));
#130749=DIRECTION('',(0.,0.,1.));
#130750=DIRECTION('',(0.,0.,-1.));
#130751=DIRECTION('center_axis',(0.,0.,-1.));
#130752=DIRECTION('ref_axis',(-1.,0.,0.));
#130753=DIRECTION('',(0.,0.,1.));
#130754=DIRECTION('',(0.,0.,-1.));
#130755=DIRECTION('center_axis',(0.,0.,-1.));
#130756=DIRECTION('ref_axis',(-1.,0.,0.));
#130757=DIRECTION('',(0.,0.,1.));
#130758=DIRECTION('',(0.,0.,-1.));
#130759=DIRECTION('center_axis',(0.,0.,-1.));
#130760=DIRECTION('ref_axis',(-1.,0.,0.));
#130761=DIRECTION('',(0.,0.,1.));
#130762=DIRECTION('',(0.,0.,-1.));
#130763=DIRECTION('center_axis',(0.,0.,-1.));
#130764=DIRECTION('ref_axis',(-1.,0.,0.));
#130765=DIRECTION('',(0.,0.,1.));
#130766=DIRECTION('',(0.,0.,-1.));
#130767=DIRECTION('center_axis',(0.,0.,-1.));
#130768=DIRECTION('ref_axis',(-1.,0.,0.));
#130769=DIRECTION('',(0.,0.,1.));
#130770=DIRECTION('',(0.,0.,-1.));
#130771=DIRECTION('center_axis',(0.,0.,1.));
#130772=DIRECTION('ref_axis',(1.,0.,0.));
#130773=DIRECTION('center_axis',(0.,0.,-1.));
#130774=DIRECTION('ref_axis',(1.,0.,0.));
#130775=DIRECTION('center_axis',(0.,0.,1.));
#130776=DIRECTION('ref_axis',(1.,0.,0.));
#130777=DIRECTION('center_axis',(0.,0.,-1.));
#130778=DIRECTION('ref_axis',(1.,0.,0.));
#130779=DIRECTION('center_axis',(0.,0.,1.));
#130780=DIRECTION('ref_axis',(1.,0.,0.));
#130781=DIRECTION('center_axis',(0.,0.,-1.));
#130782=DIRECTION('ref_axis',(1.,1.77635683940025E-15,0.));
#130783=DIRECTION('center_axis',(0.,0.,1.));
#130784=DIRECTION('ref_axis',(1.,0.,0.));
#130785=DIRECTION('center_axis',(0.,0.,-1.));
#130786=DIRECTION('ref_axis',(1.,0.,0.));
#130787=DIRECTION('center_axis',(0.,0.,1.));
#130788=DIRECTION('ref_axis',(1.,0.,0.));
#130789=DIRECTION('center_axis',(0.,0.,-1.));
#130790=DIRECTION('ref_axis',(1.,1.77635683940025E-15,0.));
#130791=DIRECTION('center_axis',(0.,0.,1.));
#130792=DIRECTION('ref_axis',(1.,0.,0.));
#130793=DIRECTION('center_axis',(0.,0.,1.));
#130794=DIRECTION('ref_axis',(1.,0.,0.));
#130795=DIRECTION('center_axis',(0.,0.,-1.));
#130796=DIRECTION('ref_axis',(1.,0.,0.));
#130797=DIRECTION('center_axis',(0.,0.,1.));
#130798=DIRECTION('ref_axis',(1.,0.,0.));
#130799=DIRECTION('center_axis',(0.,0.,-1.));
#130800=DIRECTION('ref_axis',(1.,0.,0.));
#130801=DIRECTION('center_axis',(0.,0.,1.));
#130802=DIRECTION('ref_axis',(1.,0.,0.));
#130803=DIRECTION('center_axis',(0.,0.,-1.));
#130804=DIRECTION('ref_axis',(1.,0.,0.));
#130805=DIRECTION('center_axis',(0.,0.,1.));
#130806=DIRECTION('ref_axis',(1.,0.,0.));
#130807=DIRECTION('center_axis',(0.,0.,-1.));
#130808=DIRECTION('ref_axis',(1.,0.,0.));
#130809=DIRECTION('center_axis',(0.,0.,1.));
#130810=DIRECTION('ref_axis',(1.,0.,0.));
#130811=DIRECTION('center_axis',(0.,0.,-1.));
#130812=DIRECTION('ref_axis',(1.,0.,0.));
#130813=DIRECTION('center_axis',(0.,0.,1.));
#130814=DIRECTION('ref_axis',(1.,0.,0.));
#130815=DIRECTION('center_axis',(0.,0.,-1.));
#130816=DIRECTION('ref_axis',(1.,0.,0.));
#130817=DIRECTION('center_axis',(0.,0.,1.));
#130818=DIRECTION('ref_axis',(1.,0.,0.));
#130819=DIRECTION('center_axis',(0.,0.,-1.));
#130820=DIRECTION('ref_axis',(-1.,0.,0.));
#130821=DIRECTION('center_axis',(-1.,0.,0.));
#130822=DIRECTION('ref_axis',(0.,0.,1.));
#130823=DIRECTION('center_axis',(-0.5,0.866025403784439,0.));
#130824=DIRECTION('ref_axis',(0.,0.,1.));
#130825=DIRECTION('center_axis',(0.5,0.866025403784439,0.));
#130826=DIRECTION('ref_axis',(0.,0.,-1.));
#130827=DIRECTION('center_axis',(1.,0.,0.));
#130828=DIRECTION('ref_axis',(0.,1.,0.));
#130829=DIRECTION('center_axis',(0.5,-0.866025403784439,0.));
#130830=DIRECTION('ref_axis',(0.,0.,-1.));
#130831=DIRECTION('center_axis',(-0.5,-0.866025403784439,0.));
#130832=DIRECTION('ref_axis',(-0.866025403784439,0.5,0.));
#130833=DIRECTION('center_axis',(0.,0.,1.));
#130834=DIRECTION('ref_axis',(1.,0.,0.));
#130835=DIRECTION('center_axis',(0.,0.,-1.));
#130836=DIRECTION('ref_axis',(1.,0.,0.));
#130837=DIRECTION('center_axis',(0.,0.,1.));
#130838=DIRECTION('ref_axis',(1.,0.,0.));
#130839=DIRECTION('center_axis',(0.,0.,1.));
#130840=DIRECTION('ref_axis',(1.,0.,0.));
#130841=DIRECTION('center_axis',(0.,0.,-1.));
#130842=DIRECTION('ref_axis',(-1.,0.,0.));
#130843=DIRECTION('',(0.707106781186547,-8.65956056235493E-17,-0.707106781186548));
#130844=DIRECTION('center_axis',(0.,0.,1.));
#130845=DIRECTION('ref_axis',(1.,0.,0.));
#130846=DIRECTION('',(-0.70710678118655,-8.65956056235497E-17,0.707106781186545));
#130847=DIRECTION('',(1.,5.31067157344458E-32,-1.22464679914734E-16));
#130848=DIRECTION('',(1.1808214670939E-16,-0.265125543547439,0.964213900625102));
#130849=DIRECTION('',(1.,-4.45628041133992E-31,-1.22464679914735E-16));
#130850=DIRECTION('',(-1.21962262477508E-16,-0.0904890518706492,-0.995897450288709));
#130851=DIRECTION('',(0.,1.,0.));
#130852=DIRECTION('',(1.,0.,0.));
#130853=DIRECTION('',(3.90064541592219E-19,1.,0.));
#130854=DIRECTION('',(-1.,3.90064541592219E-19,1.11699870097193E-17));
#130855=DIRECTION('',(1.,2.0186787935127E-15,3.23718682095607E-15));
#130856=DIRECTION('',(2.13318284168551E-15,0.407621673022892,-0.913150903017688));
#130857=DIRECTION('',(1.,8.34286578595115E-16,1.67622553865062E-15));
#130858=DIRECTION('',(-1.61396175467979E-15,-0.0697393352651721,0.997565248551077));
#130859=DIRECTION('',(1.,-5.83333790925111E-17,-6.80836812848342E-17));
#130860=DIRECTION('',(1.11599864470576E-18,-0.751231511739873,0.660038798684612));
#130861=DIRECTION('',(0.,0.,1.));
#130862=DIRECTION('',(1.,0.,0.));
#130863=DIRECTION('',(0.,0.,1.));
#130864=DIRECTION('',(1.,0.,0.));
#130865=DIRECTION('',(1.,0.,-3.49148133884313E-15));
#130866=DIRECTION('',(-3.49148133884313E-15,0.,-1.));
#130867=DIRECTION('',(-1.21076774565012E-16,5.55111512312578E-17,-1.));
#130868=DIRECTION('',(-1.,-4.76186235917668E-17,1.21076774565012E-16));
#130869=DIRECTION('',(0.,0.,1.));
#130870=DIRECTION('',(1.,0.,0.));
#130871=DIRECTION('',(0.,0.,1.));
#130872=DIRECTION('',(1.,0.,0.));
#130873=DIRECTION('',(0.,0.,1.));
#130874=DIRECTION('',(1.,0.,0.));
#130875=DIRECTION('',(0.,0.,1.));
#130876=DIRECTION('',(1.,0.,0.));
#130877=DIRECTION('',(1.,2.0186787935127E-15,3.23718682095607E-15));
#130878=DIRECTION('',(2.13318284168551E-15,0.407621673022892,-0.913150903017688));
#130879=DIRECTION('',(1.,2.0186787935127E-15,3.23718682095607E-15));
#130880=DIRECTION('',(2.13318284168551E-15,0.407621673022892,-0.913150903017688));
#130881=DIRECTION('',(1.,2.0186787935127E-15,3.23718682095607E-15));
#130882=DIRECTION('',(2.13318284168551E-15,0.407621673022892,-0.913150903017688));
#130883=DIRECTION('',(1.,2.0186787935127E-15,3.23718682095607E-15));
#130884=DIRECTION('',(2.13318284168551E-15,0.407621673022892,-0.913150903017688));
#130885=DIRECTION('',(1.,2.0186787935127E-15,3.23718682095607E-15));
#130886=DIRECTION('',(2.13318284168551E-15,0.407621673022892,-0.913150903017688));
#130887=DIRECTION('',(1.,2.0186787935127E-15,3.23718682095607E-15));
#130888=DIRECTION('',(2.13318284168551E-15,0.407621673022892,-0.913150903017688));
#130889=DIRECTION('',(1.,2.0186787935127E-15,3.23718682095607E-15));
#130890=DIRECTION('',(2.13318284168551E-15,0.407621673022892,-0.913150903017688));
#130891=DIRECTION('',(1.,2.0186787935127E-15,3.23718682095607E-15));
#130892=DIRECTION('',(2.13318284168551E-15,0.407621673022892,-0.913150903017688));
#130893=DIRECTION('',(1.,2.0186787935127E-15,3.23718682095607E-15));
#130894=DIRECTION('',(2.13318284168551E-15,0.407621673022892,-0.913150903017688));
#130895=DIRECTION('',(1.,2.0186787935127E-15,3.23718682095607E-15));
#130896=DIRECTION('',(2.13318284168551E-15,0.407621673022892,-0.913150903017688));
#130897=DIRECTION('',(1.,2.0186787935127E-15,3.23718682095607E-15));
#130898=DIRECTION('',(2.13318284168551E-15,0.407621673022892,-0.913150903017688));
#130899=DIRECTION('',(1.,8.34286578595119E-16,1.67622553865062E-15));
#130900=DIRECTION('',(7.41987019546992E-16,-0.998523097623667,0.0543288460399947));
#130901=DIRECTION('',(1.,8.34286578595119E-16,1.67622553865062E-15));
#130902=DIRECTION('',(7.41987019546992E-16,-0.998523097623667,0.0543288460399947));
#130903=DIRECTION('',(1.,8.34286578595119E-16,1.67622553865062E-15));
#130904=DIRECTION('',(7.41987019546992E-16,-0.998523097623667,0.0543288460399947));
#130905=DIRECTION('',(1.,8.34286578595119E-16,1.67622553865062E-15));
#130906=DIRECTION('',(7.41987019546992E-16,-0.998523097623667,0.0543288460399947));
#130907=DIRECTION('',(1.,8.34286578595119E-16,1.67622553865062E-15));
#130908=DIRECTION('',(7.41987019546992E-16,-0.998523097623667,0.0543288460399947));
#130909=DIRECTION('',(1.,8.34286578595119E-16,1.67622553865062E-15));
#130910=DIRECTION('',(7.41987019546992E-16,-0.998523097623667,0.0543288460399947));
#130911=DIRECTION('',(1.,8.34286578595119E-16,1.67622553865062E-15));
#130912=DIRECTION('',(7.41987019546992E-16,-0.998523097623667,0.0543288460399947));
#130913=DIRECTION('',(1.,8.34286578595119E-16,1.67622553865062E-15));
#130914=DIRECTION('',(7.41987019546992E-16,-0.998523097623667,0.0543288460399947));
#130915=DIRECTION('',(1.,8.34286578595119E-16,1.67622553865062E-15));
#130916=DIRECTION('',(7.41987019546992E-16,-0.998523097623667,0.0543288460399947));
#130917=DIRECTION('',(1.,8.34286578595119E-16,1.67622553865062E-15));
#130918=DIRECTION('',(7.41987019546992E-16,-0.998523097623667,0.0543288460399947));
#130919=DIRECTION('',(1.,8.34286578595119E-16,1.67622553865062E-15));
#130920=DIRECTION('',(7.41987019546992E-16,-0.998523097623667,0.0543288460399947));
#130921=DIRECTION('',(1.,8.34286578595119E-16,1.67622553865062E-15));
#130922=DIRECTION('',(7.41987019546992E-16,-0.998523097623667,0.0543288460399947));
#130923=DIRECTION('',(1.,8.34286578595115E-16,1.67622553865062E-15));
#130924=DIRECTION('',(-1.61396175467979E-15,-0.0697393352651721,0.997565248551077));
#130925=DIRECTION('',(1.,8.34286578595115E-16,1.67622553865062E-15));
#130926=DIRECTION('',(-1.61396175467979E-15,-0.0697393352651721,0.997565248551077));
#130927=DIRECTION('',(1.,8.34286578595115E-16,1.67622553865062E-15));
#130928=DIRECTION('',(-1.61396175467979E-15,-0.0697393352651721,0.997565248551077));
#130929=DIRECTION('',(1.,8.34286578595115E-16,1.67622553865062E-15));
#130930=DIRECTION('',(-1.61396175467979E-15,-0.0697393352651721,0.997565248551077));
#130931=DIRECTION('',(1.,8.34286578595115E-16,1.67622553865062E-15));
#130932=DIRECTION('',(-1.61396175467979E-15,-0.0697393352651721,0.997565248551077));
#130933=DIRECTION('',(1.,8.34286578595115E-16,1.67622553865062E-15));
#130934=DIRECTION('',(-1.61396175467979E-15,-0.0697393352651721,0.997565248551077));
#130935=DIRECTION('',(1.,8.34286578595115E-16,1.67622553865062E-15));
#130936=DIRECTION('',(-1.61396175467979E-15,-0.0697393352651721,0.997565248551077));
#130937=DIRECTION('',(1.,8.34286578595115E-16,1.67622553865062E-15));
#130938=DIRECTION('',(-1.61396175467979E-15,-0.0697393352651721,0.997565248551077));
#130939=DIRECTION('',(1.,8.34286578595115E-16,1.67622553865062E-15));
#130940=DIRECTION('',(-1.61396175467979E-15,-0.0697393352651721,0.997565248551077));
#130941=DIRECTION('',(1.,8.34286578595115E-16,1.67622553865062E-15));
#130942=DIRECTION('',(-1.61396175467979E-15,-0.0697393352651721,0.997565248551077));
#130943=DIRECTION('',(1.,8.34286578595115E-16,1.67622553865062E-15));
#130944=DIRECTION('',(-1.61396175467979E-15,-0.0697393352651721,0.997565248551077));
#130945=DIRECTION('',(1.,-5.83333790925111E-17,-6.80836812848342E-17));
#130946=DIRECTION('',(1.11599864470576E-18,-0.751231511739873,0.660038798684612));
#130947=DIRECTION('',(1.,-5.83333790925111E-17,-6.80836812848342E-17));
#130948=DIRECTION('',(1.11599864470576E-18,-0.751231511739873,0.660038798684612));
#130949=DIRECTION('',(1.,-5.83333790925111E-17,-6.80836812848342E-17));
#130950=DIRECTION('',(1.11599864470576E-18,-0.751231511739873,0.660038798684612));
#130951=DIRECTION('',(1.,-5.83333790925111E-17,-6.80836812848342E-17));
#130952=DIRECTION('',(1.11599864470576E-18,-0.751231511739873,0.660038798684612));
#130953=DIRECTION('',(1.,-5.83333790925111E-17,-6.80836812848342E-17));
#130954=DIRECTION('',(1.11599864470576E-18,-0.751231511739873,0.660038798684612));
#130955=DIRECTION('',(1.,-5.83333790925111E-17,-6.80836812848342E-17));
#130956=DIRECTION('',(1.11599864470576E-18,-0.751231511739873,0.660038798684612));
#130957=DIRECTION('',(1.,-5.83333790925111E-17,-6.80836812848342E-17));
#130958=DIRECTION('',(1.11599864470576E-18,-0.751231511739873,0.660038798684612));
#130959=DIRECTION('',(1.,-5.83333790925111E-17,-6.80836812848342E-17));
#130960=DIRECTION('',(1.11599864470576E-18,-0.751231511739873,0.660038798684612));
#130961=DIRECTION('',(1.,-5.83333790925111E-17,-6.80836812848342E-17));
#130962=DIRECTION('',(1.11599864470576E-18,-0.751231511739873,0.660038798684612));
#130963=DIRECTION('',(1.,-5.83333790925111E-17,-6.80836812848342E-17));
#130964=DIRECTION('',(1.11599864470576E-18,-0.751231511739873,0.660038798684612));
#130965=DIRECTION('',(1.,-5.83333790925111E-17,-6.80836812848342E-17));
#130966=DIRECTION('',(1.11599864470576E-18,-0.751231511739873,0.660038798684612));
#130967=DIRECTION('',(0.,0.,1.));
#130968=DIRECTION('',(1.,0.,0.));
#130969=DIRECTION('',(5.40642287378652E-49,-2.22044604925031E-16,-1.));
#130970=DIRECTION('',(-1.,-3.97558035948902E-33,3.42113882891801E-49));
#130971=DIRECTION('',(0.,0.,1.));
#130972=DIRECTION('',(1.,0.,0.));
#130973=DIRECTION('',(-1.11699870097193E-17,2.1785079312686E-36,-1.));
#130974=DIRECTION('',(-1.,3.90064541592219E-19,1.11699870097193E-17));
#130975=DIRECTION('',(0.,0.,1.));
#130976=DIRECTION('',(1.,0.,0.));
#130977=DIRECTION('',(-1.11699870097193E-17,2.1785079312686E-36,-1.));
#130978=DIRECTION('',(-1.,3.90064541592219E-19,1.11699870097193E-17));
#130979=DIRECTION('',(1.,0.,-3.49148133884313E-15));
#130980=DIRECTION('',(-3.49148133884313E-15,0.,-1.));
#130981=DIRECTION('',(-1.11699870097193E-17,2.1785079312686E-36,-1.));
#130982=DIRECTION('',(-1.,3.90064541592219E-19,1.11699870097193E-17));
#130983=DIRECTION('',(0.,0.,1.));
#130984=DIRECTION('',(1.,0.,0.));
#130985=DIRECTION('',(0.,0.,1.));
#130986=DIRECTION('',(1.,0.,0.));
#130987=DIRECTION('',(0.,0.,1.));
#130988=DIRECTION('',(1.,0.,0.));
#130989=DIRECTION('',(-1.40241613969251E-16,-0.158552753262548,0.987350507384721));
#130990=DIRECTION('',(1.,-5.41084509282512E-17,1.33349371996123E-16));
#130991=DIRECTION('',(5.55111512312578E-17,-0.282983625147426,0.959124740530877));
#130992=DIRECTION('',(1.,1.30606871313547E-16,-1.93421611744877E-17));
#130993=DIRECTION('',(5.55111512312578E-17,-0.371153744479045,0.928571428571428));
#130994=DIRECTION('',(1.,3.02043455234294E-17,-4.77084410822903E-17));
#130995=DIRECTION('',(-5.55111512312578E-17,-0.421153577725023,0.906989340604074));
#130996=DIRECTION('',(1.,-2.33787199446791E-17,5.03480224514116E-17));
#130997=DIRECTION('',(5.55111512312578E-17,-0.429956734220656,0.902849492827187));
#130998=DIRECTION('',(1.,1.80087733049557E-16,2.42773380481109E-17));
#130999=DIRECTION('',(-1.11699870097193E-17,2.1785079312686E-36,-1.));
#131000=DIRECTION('',(-1.,3.90064541592219E-19,1.11699870097193E-17));
#131001=DIRECTION('',(-1.11699870097193E-17,2.17850793126864E-36,-1.));
#131002=DIRECTION('',(-1.,3.90064541592225E-19,1.11699870097193E-17));
#131003=DIRECTION('',(2.47416513115296E-17,0.282983625147426,-0.959124740530877));
#131004=DIRECTION('',(-1.,1.25290154811922E-16,1.11699870097193E-17));
#131005=DIRECTION('',(-1.51208220980365E-16,0.158552753262548,-0.987350507384721));
#131006=DIRECTION('',(-1.,-5.37183484095654E-17,1.44519122512297E-16));
#131007=DIRECTION('',(1.13467952761192E-16,0.371153744479045,-0.928571428571428));
#131008=DIRECTION('',(-1.,5.590121577285E-17,-9.98523154527963E-17));
#131009=DIRECTION('',(-9.96678207526618E-18,0.421153577725023,-0.906989340604074));
#131010=DIRECTION('',(-1.,3.90064541592224E-19,1.11699870097193E-17));
#131011=DIRECTION('',(-5.04850524604105E-17,0.429956734220656,-0.902849492827187));
#131012=DIRECTION('',(-1.,1.39167942619737E-16,1.22192289472235E-16));
#131013=CARTESIAN_POINT('',(0.,0.,0.));
#131014=CARTESIAN_POINT('',(0.,0.,0.));
#131015=CARTESIAN_POINT('Origin',(-55.,-786.679542586191,65.));
#131016=CARTESIAN_POINT('',(-50.,-786.679542586191,72.5));
#131017=CARTESIAN_POINT('Origin',(-50.,-786.679542586191,65.));
#131018=CARTESIAN_POINT('',(-45.,-786.679542586191,72.5));
#131019=CARTESIAN_POINT('',(-55.,-786.679542586191,72.5));
#131020=CARTESIAN_POINT('Origin',(-45.,-786.679542586191,65.));
#131021=CARTESIAN_POINT('Origin',(-55.,-646.67954258619,65.));
#131022=CARTESIAN_POINT('',(-50.,-646.67954258619,72.5));
#131023=CARTESIAN_POINT('Origin',(-50.,-646.67954258619,65.));
#131024=CARTESIAN_POINT('',(-45.,-646.67954258619,72.5));
#131025=CARTESIAN_POINT('',(-55.,-646.67954258619,72.5));
#131026=CARTESIAN_POINT('Origin',(-45.,-646.67954258619,65.));
#131027=CARTESIAN_POINT('Origin',(-55.,-506.67954258619,65.));
#131028=CARTESIAN_POINT('',(-50.,-506.67954258619,72.5));
#131029=CARTESIAN_POINT('Origin',(-50.,-506.67954258619,65.));
#131030=CARTESIAN_POINT('',(-45.,-506.67954258619,72.5));
#131031=CARTESIAN_POINT('',(-55.,-506.67954258619,72.5));
#131032=CARTESIAN_POINT('Origin',(-45.,-506.67954258619,65.));
#131033=CARTESIAN_POINT('Origin',(-55.,-366.67954258619,65.));
#131034=CARTESIAN_POINT('',(-50.,-366.67954258619,72.5));
#131035=CARTESIAN_POINT('Origin',(-50.,-366.67954258619,65.));
#131036=CARTESIAN_POINT('',(-45.,-366.67954258619,72.5));
#131037=CARTESIAN_POINT('',(-55.,-366.67954258619,72.5));
#131038=CARTESIAN_POINT('Origin',(-45.,-366.67954258619,65.));
#131039=CARTESIAN_POINT('Origin',(-55.,-226.67954258619,65.));
#131040=CARTESIAN_POINT('',(-50.,-226.67954258619,72.5));
#131041=CARTESIAN_POINT('Origin',(-50.,-226.67954258619,65.));
#131042=CARTESIAN_POINT('',(-45.,-226.67954258619,72.5));
#131043=CARTESIAN_POINT('',(-55.,-226.67954258619,72.5));
#131044=CARTESIAN_POINT('Origin',(-45.,-226.67954258619,65.));
#131045=CARTESIAN_POINT('Origin',(-55.,-86.6795425861914,65.));
#131046=CARTESIAN_POINT('',(-50.,-86.6795425861914,72.5));
#131047=CARTESIAN_POINT('Origin',(-50.,-86.6795425861914,65.));
#131048=CARTESIAN_POINT('',(-45.,-86.6795425861914,72.5));
#131049=CARTESIAN_POINT('',(-55.,-86.6795425861914,72.5));
#131050=CARTESIAN_POINT('Origin',(-45.,-86.6795425861914,65.));
#131051=CARTESIAN_POINT('Origin',(-55.,53.3204574138085,65.));
#131052=CARTESIAN_POINT('',(-50.,53.3204574138085,72.5));
#131053=CARTESIAN_POINT('Origin',(-50.,53.3204574138085,65.));
#131054=CARTESIAN_POINT('',(-45.,53.3204574138085,72.5));
#131055=CARTESIAN_POINT('',(-55.,53.3204574138085,72.5));
#131056=CARTESIAN_POINT('Origin',(-45.,53.3204574138085,65.));
#131057=CARTESIAN_POINT('Origin',(-55.,193.320457413809,65.));
#131058=CARTESIAN_POINT('',(-50.,193.320457413809,72.5));
#131059=CARTESIAN_POINT('Origin',(-50.,193.320457413809,65.));
#131060=CARTESIAN_POINT('',(-45.,193.320457413809,72.5));
#131061=CARTESIAN_POINT('',(-55.,193.320457413809,72.5));
#131062=CARTESIAN_POINT('Origin',(-45.,193.320457413809,65.));
#131063=CARTESIAN_POINT('Origin',(-55.,333.32045741381,65.));
#131064=CARTESIAN_POINT('',(-50.,333.32045741381,72.5));
#131065=CARTESIAN_POINT('Origin',(-50.,333.32045741381,65.));
#131066=CARTESIAN_POINT('',(-45.,333.32045741381,72.5));
#131067=CARTESIAN_POINT('',(-55.,333.32045741381,72.5));
#131068=CARTESIAN_POINT('Origin',(-45.,333.32045741381,65.));
#131069=CARTESIAN_POINT('Origin',(-55.,473.320457413809,65.));
#131070=CARTESIAN_POINT('',(-50.,473.320457413809,72.5));
#131071=CARTESIAN_POINT('Origin',(-50.,473.320457413809,65.));
#131072=CARTESIAN_POINT('',(-45.,473.320457413809,72.5));
#131073=CARTESIAN_POINT('',(-55.,473.320457413809,72.5));
#131074=CARTESIAN_POINT('Origin',(-45.,473.320457413809,65.));
#131075=CARTESIAN_POINT('Origin',(-55.,613.320457413809,65.));
#131076=CARTESIAN_POINT('',(-50.,613.320457413809,72.5));
#131077=CARTESIAN_POINT('Origin',(-50.,613.320457413809,65.));
#131078=CARTESIAN_POINT('',(-45.,613.320457413809,72.5));
#131079=CARTESIAN_POINT('',(-55.,613.320457413809,72.5));
#131080=CARTESIAN_POINT('Origin',(-45.,613.320457413809,65.));
#131081=CARTESIAN_POINT('Origin',(-55.,753.32045741381,65.));
#131082=CARTESIAN_POINT('',(-50.,753.32045741381,72.5));
#131083=CARTESIAN_POINT('Origin',(-50.,753.32045741381,65.));
#131084=CARTESIAN_POINT('',(-45.,753.32045741381,72.5));
#131085=CARTESIAN_POINT('',(-55.,753.32045741381,72.5));
#131086=CARTESIAN_POINT('Origin',(-45.,753.32045741381,65.));
#131087=CARTESIAN_POINT('Origin',(0.,900.,5.));
#131088=CARTESIAN_POINT('',(0.,-900.,5.));
#131089=CARTESIAN_POINT('',(0.,-900.,0.));
#131090=CARTESIAN_POINT('',(0.,-900.,5.));
#131091=CARTESIAN_POINT('',(0.,900.,0.));
#131092=CARTESIAN_POINT('',(0.,900.,0.));
#131093=CARTESIAN_POINT('',(0.,900.,5.));
#131094=CARTESIAN_POINT('',(0.,900.,5.));
#131095=CARTESIAN_POINT('',(0.,900.,5.));
#131096=CARTESIAN_POINT('Origin',(0.,900.,0.));
#131097=CARTESIAN_POINT('',(-48.,-900.,5.8783046359073E-15));
#131098=CARTESIAN_POINT('',(0.,-900.,0.));
#131099=CARTESIAN_POINT('',(-48.,900.,5.8783046359073E-15));
#131100=CARTESIAN_POINT('',(-48.,900.,5.8783046359073E-15));
#131101=CARTESIAN_POINT('',(0.,900.,0.));
#131102=CARTESIAN_POINT('Origin',(-50.,900.,6.12323399573677E-15));
#131103=CARTESIAN_POINT('',(-50.,-900.,2.00000000000001));
#131104=CARTESIAN_POINT('',(-50.,-900.,128.));
#131105=CARTESIAN_POINT('',(-50.,-900.,6.12323399573677E-15));
#131106=CARTESIAN_POINT('',(-50.,900.,128.));
#131107=CARTESIAN_POINT('',(-50.,900.,128.));
#131108=CARTESIAN_POINT('',(-50.,900.,2.00000000000001));
#131109=CARTESIAN_POINT('',(-50.,900.,6.12323399573677E-15));
#131110=CARTESIAN_POINT('',(-50.,900.,2.00000000000001));
#131111=CARTESIAN_POINT('Origin',(-50.,900.,130.));
#131112=CARTESIAN_POINT('',(-48.,900.,130.));
#131113=CARTESIAN_POINT('',(0.,900.,130.));
#131114=CARTESIAN_POINT('',(-50.,900.,130.));
#131115=CARTESIAN_POINT('',(-48.,-900.,130.));
#131116=CARTESIAN_POINT('',(-48.,900.,130.));
#131117=CARTESIAN_POINT('',(0.,-900.,130.));
#131118=CARTESIAN_POINT('',(-50.,-900.,130.));
#131119=CARTESIAN_POINT('',(0.,900.,130.));
#131120=CARTESIAN_POINT('Origin',(0.,900.,130.));
#131121=CARTESIAN_POINT('',(0.,-900.,125.));
#131122=CARTESIAN_POINT('',(0.,-900.,130.));
#131123=CARTESIAN_POINT('',(0.,900.,125.));
#131124=CARTESIAN_POINT('',(0.,900.,125.));
#131125=CARTESIAN_POINT('',(0.,900.,130.));
#131126=CARTESIAN_POINT('Origin',(0.,900.,125.));
#131127=CARTESIAN_POINT('',(-43.,-900.,125.));
#131128=CARTESIAN_POINT('',(0.,-900.,125.));
#131129=CARTESIAN_POINT('',(-43.,900.,125.));
#131130=CARTESIAN_POINT('',(-43.,900.,125.));
#131131=CARTESIAN_POINT('',(0.,900.,125.));
#131132=CARTESIAN_POINT('Origin',(-45.,900.,125.));
#131133=CARTESIAN_POINT('',(-45.,-900.,123.));
#131134=CARTESIAN_POINT('',(-45.,-900.,7.00000000000001));
#131135=CARTESIAN_POINT('',(-45.,-900.,125.));
#131136=CARTESIAN_POINT('',(-45.,900.,7.00000000000001));
#131137=CARTESIAN_POINT('',(-45.,900.,7.));
#131138=CARTESIAN_POINT('',(-45.,900.,123.));
#131139=CARTESIAN_POINT('',(-45.,900.,125.));
#131140=CARTESIAN_POINT('',(-45.,-900.,123.));
#131141=CARTESIAN_POINT('Origin',(-45.,900.,5.));
#131142=CARTESIAN_POINT('',(-43.,900.,5.));
#131143=CARTESIAN_POINT('',(-45.,900.,5.));
#131144=CARTESIAN_POINT('',(-43.,-900.,5.));
#131145=CARTESIAN_POINT('',(-43.,-900.,5.));
#131146=CARTESIAN_POINT('',(-45.,-900.,5.));
#131147=CARTESIAN_POINT('Origin',(0.,900.,0.));
#131148=CARTESIAN_POINT('Origin',(-48.,900.,128.));
#131149=CARTESIAN_POINT('Origin',(-43.,900.,123.));
#131150=CARTESIAN_POINT('Origin',(-43.,900.,7.));
#131151=CARTESIAN_POINT('Origin',(-48.,900.,2.00000000000001));
#131152=CARTESIAN_POINT('Origin',(0.,-900.,0.));
#131153=CARTESIAN_POINT('Origin',(-48.,-900.,128.));
#131154=CARTESIAN_POINT('Origin',(-48.,-900.,2.00000000000001));
#131155=CARTESIAN_POINT('Origin',(-43.,-900.,7.));
#131156=CARTESIAN_POINT('Origin',(-43.,-900.,123.));
#131157=CARTESIAN_POINT('Origin',(-48.,900.,128.));
#131158=CARTESIAN_POINT('Origin',(-48.,900.,2.00000000000001));
#131159=CARTESIAN_POINT('Origin',(-43.,900.,7.));
#131160=CARTESIAN_POINT('Origin',(-43.,900.,123.));
#131161=CARTESIAN_POINT('',(0.,0.,0.));
#131162=CARTESIAN_POINT('Origin',(-55.,-753.32045741381,64.9999999999994));
#131163=CARTESIAN_POINT('',(-50.,-753.32045741381,72.4999999999994));
#131164=CARTESIAN_POINT('Origin',(-50.,-753.32045741381,64.9999999999994));
#131165=CARTESIAN_POINT('',(-45.,-753.32045741381,72.4999999999994));
#131166=CARTESIAN_POINT('',(-55.,-753.32045741381,72.4999999999994));
#131167=CARTESIAN_POINT('Origin',(-45.,-753.32045741381,64.9999999999994));
#131168=CARTESIAN_POINT('Origin',(-55.,366.67954258619,64.9999999999994));
#131169=CARTESIAN_POINT('',(-50.,366.67954258619,72.4999999999994));
#131170=CARTESIAN_POINT('Origin',(-50.,366.67954258619,64.9999999999994));
#131171=CARTESIAN_POINT('',(-45.,366.67954258619,72.4999999999994));
#131172=CARTESIAN_POINT('',(-55.,366.67954258619,72.4999999999994));
#131173=CARTESIAN_POINT('Origin',(-45.,366.67954258619,64.9999999999994));
#131174=CARTESIAN_POINT('Origin',(-55.,-333.32045741381,64.9999999999994));
#131175=CARTESIAN_POINT('',(-50.,-333.32045741381,72.4999999999994));
#131176=CARTESIAN_POINT('Origin',(-50.,-333.32045741381,64.9999999999994));
#131177=CARTESIAN_POINT('',(-45.,-333.32045741381,72.4999999999994));
#131178=CARTESIAN_POINT('',(-55.,-333.32045741381,72.4999999999994));
#131179=CARTESIAN_POINT('Origin',(-45.,-333.32045741381,64.9999999999994));
#131180=CARTESIAN_POINT('Origin',(-55.,86.6795425861912,65.));
#131181=CARTESIAN_POINT('',(-50.,86.6795425861912,72.5));
#131182=CARTESIAN_POINT('Origin',(-50.,86.6795425861912,65.));
#131183=CARTESIAN_POINT('',(-45.,86.6795425861912,72.5));
#131184=CARTESIAN_POINT('',(-55.,86.6795425861912,72.5));
#131185=CARTESIAN_POINT('Origin',(-45.,86.6795425861912,65.));
#131186=CARTESIAN_POINT('Origin',(-55.,786.679542586191,65.));
#131187=CARTESIAN_POINT('',(-50.,786.679542586191,72.5));
#131188=CARTESIAN_POINT('Origin',(-50.,786.679542586191,65.));
#131189=CARTESIAN_POINT('',(-45.,786.679542586191,72.5));
#131190=CARTESIAN_POINT('',(-55.,786.679542586191,72.5));
#131191=CARTESIAN_POINT('Origin',(-45.,786.679542586191,65.));
#131192=CARTESIAN_POINT('Origin',(-55.,646.679542586191,64.9999999999994));
#131193=CARTESIAN_POINT('',(-50.,646.679542586191,72.4999999999994));
#131194=CARTESIAN_POINT('Origin',(-50.,646.679542586191,64.9999999999994));
#131195=CARTESIAN_POINT('',(-45.,646.679542586191,72.4999999999994));
#131196=CARTESIAN_POINT('',(-55.,646.679542586191,72.4999999999994));
#131197=CARTESIAN_POINT('Origin',(-45.,646.679542586191,64.9999999999994));
#131198=CARTESIAN_POINT('Origin',(-55.,506.679542586191,64.9999999999994));
#131199=CARTESIAN_POINT('',(-50.,506.679542586191,72.4999999999994));
#131200=CARTESIAN_POINT('Origin',(-50.,506.679542586191,64.9999999999994));
#131201=CARTESIAN_POINT('',(-45.,506.679542586191,72.4999999999994));
#131202=CARTESIAN_POINT('',(-55.,506.679542586191,72.4999999999994));
#131203=CARTESIAN_POINT('Origin',(-45.,506.679542586191,64.9999999999994));
#131204=CARTESIAN_POINT('Origin',(-55.,226.67954258619,64.9999999999994));
#131205=CARTESIAN_POINT('',(-50.,226.67954258619,72.4999999999994));
#131206=CARTESIAN_POINT('Origin',(-50.,226.67954258619,64.9999999999994));
#131207=CARTESIAN_POINT('',(-45.,226.67954258619,72.4999999999994));
#131208=CARTESIAN_POINT('',(-55.,226.67954258619,72.4999999999994));
#131209=CARTESIAN_POINT('Origin',(-45.,226.67954258619,64.9999999999994));
#131210=CARTESIAN_POINT('Origin',(-55.,-53.3204574138096,64.9999999999994));
#131211=CARTESIAN_POINT('',(-50.,-53.3204574138096,72.4999999999994));
#131212=CARTESIAN_POINT('Origin',(-50.,-53.3204574138096,64.9999999999994));
#131213=CARTESIAN_POINT('',(-45.,-53.3204574138096,72.4999999999994));
#131214=CARTESIAN_POINT('',(-55.,-53.3204574138096,72.4999999999994));
#131215=CARTESIAN_POINT('Origin',(-45.,-53.3204574138096,64.9999999999994));
#131216=CARTESIAN_POINT('Origin',(-55.,-193.32045741381,64.9999999999994));
#131217=CARTESIAN_POINT('',(-50.,-193.32045741381,72.4999999999994));
#131218=CARTESIAN_POINT('Origin',(-50.,-193.32045741381,64.9999999999994));
#131219=CARTESIAN_POINT('',(-45.,-193.32045741381,72.4999999999994));
#131220=CARTESIAN_POINT('',(-55.,-193.32045741381,72.4999999999994));
#131221=CARTESIAN_POINT('Origin',(-45.,-193.32045741381,64.9999999999994));
#131222=CARTESIAN_POINT('Origin',(-55.,-473.32045741381,64.9999999999994));
#131223=CARTESIAN_POINT('',(-50.,-473.32045741381,72.4999999999994));
#131224=CARTESIAN_POINT('Origin',(-50.,-473.32045741381,64.9999999999994));
#131225=CARTESIAN_POINT('',(-45.,-473.32045741381,72.4999999999994));
#131226=CARTESIAN_POINT('',(-55.,-473.32045741381,72.4999999999994));
#131227=CARTESIAN_POINT('Origin',(-45.,-473.32045741381,64.9999999999994));
#131228=CARTESIAN_POINT('Origin',(-55.,-613.32045741381,64.9999999999994));
#131229=CARTESIAN_POINT('',(-50.,-613.32045741381,72.4999999999994));
#131230=CARTESIAN_POINT('Origin',(-50.,-613.32045741381,64.9999999999994));
#131231=CARTESIAN_POINT('',(-45.,-613.32045741381,72.4999999999994));
#131232=CARTESIAN_POINT('',(-55.,-613.32045741381,72.4999999999994));
#131233=CARTESIAN_POINT('Origin',(-45.,-613.32045741381,64.9999999999994));
#131234=CARTESIAN_POINT('Origin',(0.,900.,5.));
#131235=CARTESIAN_POINT('',(0.,-900.,5.));
#131236=CARTESIAN_POINT('',(0.,-900.,0.));
#131237=CARTESIAN_POINT('',(0.,-900.,5.));
#131238=CARTESIAN_POINT('',(0.,900.,0.));
#131239=CARTESIAN_POINT('',(0.,900.,0.));
#131240=CARTESIAN_POINT('',(0.,900.,5.));
#131241=CARTESIAN_POINT('',(0.,900.,5.));
#131242=CARTESIAN_POINT('',(0.,900.,5.));
#131243=CARTESIAN_POINT('Origin',(0.,900.,0.));
#131244=CARTESIAN_POINT('',(-48.,-900.,5.8783046359073E-15));
#131245=CARTESIAN_POINT('',(0.,-900.,0.));
#131246=CARTESIAN_POINT('',(-48.,900.,5.8783046359073E-15));
#131247=CARTESIAN_POINT('',(-48.,900.,5.8783046359073E-15));
#131248=CARTESIAN_POINT('',(0.,900.,0.));
#131249=CARTESIAN_POINT('Origin',(-50.,900.,6.12323399573677E-15));
#131250=CARTESIAN_POINT('',(-50.,-900.,2.00000000000001));
#131251=CARTESIAN_POINT('',(-50.,-900.,128.));
#131252=CARTESIAN_POINT('',(-50.,-900.,6.12323399573677E-15));
#131253=CARTESIAN_POINT('',(-50.,900.,128.));
#131254=CARTESIAN_POINT('',(-50.,900.,128.));
#131255=CARTESIAN_POINT('',(-50.,900.,2.00000000000001));
#131256=CARTESIAN_POINT('',(-50.,900.,6.12323399573677E-15));
#131257=CARTESIAN_POINT('',(-50.,900.,2.00000000000001));
#131258=CARTESIAN_POINT('Origin',(-50.,900.,130.));
#131259=CARTESIAN_POINT('',(-48.,900.,130.));
#131260=CARTESIAN_POINT('',(0.,900.,130.));
#131261=CARTESIAN_POINT('',(-50.,900.,130.));
#131262=CARTESIAN_POINT('',(-48.,-900.,130.));
#131263=CARTESIAN_POINT('',(-48.,900.,130.));
#131264=CARTESIAN_POINT('',(0.,-900.,130.));
#131265=CARTESIAN_POINT('',(-50.,-900.,130.));
#131266=CARTESIAN_POINT('',(0.,900.,130.));
#131267=CARTESIAN_POINT('Origin',(0.,900.,130.));
#131268=CARTESIAN_POINT('',(0.,-900.,125.));
#131269=CARTESIAN_POINT('',(0.,-900.,130.));
#131270=CARTESIAN_POINT('',(0.,900.,125.));
#131271=CARTESIAN_POINT('',(0.,900.,125.));
#131272=CARTESIAN_POINT('',(0.,900.,130.));
#131273=CARTESIAN_POINT('Origin',(0.,900.,125.));
#131274=CARTESIAN_POINT('',(-43.,-900.,125.));
#131275=CARTESIAN_POINT('',(0.,-900.,125.));
#131276=CARTESIAN_POINT('',(-43.,900.,125.));
#131277=CARTESIAN_POINT('',(-43.,900.,125.));
#131278=CARTESIAN_POINT('',(0.,900.,125.));
#131279=CARTESIAN_POINT('Origin',(-45.,900.,125.));
#131280=CARTESIAN_POINT('',(-45.,-900.,123.));
#131281=CARTESIAN_POINT('',(-45.,-900.,7.00000000000001));
#131282=CARTESIAN_POINT('',(-45.,-900.,125.));
#131283=CARTESIAN_POINT('',(-45.,900.,7.00000000000001));
#131284=CARTESIAN_POINT('',(-45.,900.,7.));
#131285=CARTESIAN_POINT('',(-45.,900.,123.));
#131286=CARTESIAN_POINT('',(-45.,900.,125.));
#131287=CARTESIAN_POINT('',(-45.,-900.,123.));
#131288=CARTESIAN_POINT('Origin',(-45.,900.,5.));
#131289=CARTESIAN_POINT('',(-43.,900.,5.));
#131290=CARTESIAN_POINT('',(-45.,900.,5.));
#131291=CARTESIAN_POINT('',(-43.,-900.,5.));
#131292=CARTESIAN_POINT('',(-43.,-900.,5.));
#131293=CARTESIAN_POINT('',(-45.,-900.,5.));
#131294=CARTESIAN_POINT('Origin',(0.,900.,0.));
#131295=CARTESIAN_POINT('Origin',(-48.,900.,128.));
#131296=CARTESIAN_POINT('Origin',(-43.,900.,123.));
#131297=CARTESIAN_POINT('Origin',(-43.,900.,7.));
#131298=CARTESIAN_POINT('Origin',(-48.,900.,2.00000000000001));
#131299=CARTESIAN_POINT('Origin',(0.,-900.,0.));
#131300=CARTESIAN_POINT('Origin',(-48.,-900.,128.));
#131301=CARTESIAN_POINT('Origin',(-48.,-900.,2.00000000000001));
#131302=CARTESIAN_POINT('Origin',(-43.,-900.,7.));
#131303=CARTESIAN_POINT('Origin',(-43.,-900.,123.));
#131304=CARTESIAN_POINT('Origin',(-48.,900.,128.));
#131305=CARTESIAN_POINT('Origin',(-48.,900.,2.00000000000001));
#131306=CARTESIAN_POINT('Origin',(-43.,900.,7.));
#131307=CARTESIAN_POINT('Origin',(-43.,900.,123.));
#131308=CARTESIAN_POINT('',(0.,0.,0.));
#131309=CARTESIAN_POINT('Origin',(-44.5079524583208,31.5404524382925,-39.8944822890418));
#131310=CARTESIAN_POINT('',(-46.5079524583208,31.5404524382925,-40.4194822890418));
#131311=CARTESIAN_POINT('Origin',(-44.5079524583208,31.5404524382925,-40.4194822890418));
#131312=CARTESIAN_POINT('',(-45.9829524583208,31.5404524382925,-39.8944822890418));
#131313=CARTESIAN_POINT('',(-45.9829524583208,31.5404524382925,-39.8944822890418));
#131314=CARTESIAN_POINT('Origin',(-44.5079524583208,31.5404524382925,-39.8944822890418));
#131315=CARTESIAN_POINT('Origin',(-44.5079524583208,31.5404524382925,-39.8944822890418));
#131316=CARTESIAN_POINT('Origin',(-44.5079524583208,31.5404524382925,-39.8944822890418));
#131317=CARTESIAN_POINT('',(-46.5079524583208,31.5404524382925,-55.24995));
#131318=CARTESIAN_POINT('Origin',(-44.5079524583208,31.5404524382925,-55.24995));
#131319=CARTESIAN_POINT('',(-46.5079524583208,31.5404524382925,-39.8944822890418));
#131320=CARTESIAN_POINT('Origin',(0.,45.41999998,-55.24995));
#131321=CARTESIAN_POINT('',(-47.0079524583208,31.5404524382925,-55.24995));
#131322=CARTESIAN_POINT('Origin',(-44.5079524583208,31.5404524382925,-55.24995));
#131323=CARTESIAN_POINT('Origin',(-44.5079524583208,31.5404524382925,-48.1788821881345));
#131324=CARTESIAN_POINT('',(-47.0079524583208,31.5404524382925,-179.64995));
#131325=CARTESIAN_POINT('Origin',(-44.5079524583208,31.5404524382925,-179.64995));
#131326=CARTESIAN_POINT('',(-47.0079524583208,31.5404524382925,-48.1788821881345));
#131327=CARTESIAN_POINT('Origin',(-44.5079524583208,31.5404524382925,-179.64995));
#131328=CARTESIAN_POINT('Origin',(44.5079524583208,31.5404524382925,-39.8944822890418));
#131329=CARTESIAN_POINT('',(46.5079524583208,31.5404524382925,-40.4194822890418));
#131330=CARTESIAN_POINT('Origin',(44.5079524583208,31.5404524382925,-40.4194822890418));
#131331=CARTESIAN_POINT('',(45.9829524583208,31.5404524382925,-39.8944822890418));
#131332=CARTESIAN_POINT('',(45.9829524583208,31.5404524382925,-39.8944822890418));
#131333=CARTESIAN_POINT('Origin',(44.5079524583208,31.5404524382925,-39.8944822890418));
#131334=CARTESIAN_POINT('Origin',(44.5079524583208,31.5404524382925,-39.8944822890418));
#131335=CARTESIAN_POINT('Origin',(44.5079524583208,31.5404524382925,-39.8944822890418));
#131336=CARTESIAN_POINT('',(46.5079524583208,31.5404524382925,-55.24995));
#131337=CARTESIAN_POINT('Origin',(44.5079524583208,31.5404524382925,-55.24995));
#131338=CARTESIAN_POINT('',(46.5079524583208,31.5404524382925,-39.8944822890418));
#131339=CARTESIAN_POINT('Origin',(0.,45.41999998,-55.24995));
#131340=CARTESIAN_POINT('',(47.0079524583208,31.5404524382925,-55.24995));
#131341=CARTESIAN_POINT('Origin',(44.5079524583208,31.5404524382925,-55.24995));
#131342=CARTESIAN_POINT('Origin',(44.5079524583208,31.5404524382925,-48.1788821881345));
#131343=CARTESIAN_POINT('',(47.0079524583208,31.5404524382925,-179.64995));
#131344=CARTESIAN_POINT('Origin',(44.5079524583208,31.5404524382925,-179.64995));
#131345=CARTESIAN_POINT('',(47.0079524583208,31.5404524382925,-48.1788821881345));
#131346=CARTESIAN_POINT('Origin',(44.5079524583208,31.5404524382925,-179.64995));
#131347=CARTESIAN_POINT('Origin',(-57.8922230010149,-38.7834964612722,-55.24995));
#131348=CARTESIAN_POINT('',(-52.9112495105562,-38.347717747534,-54.9585476429427));
#131349=CARTESIAN_POINT('',(-52.9112495105562,-38.347717747534,-52.64995));
#131350=CARTESIAN_POINT('',(-52.9112495105562,-38.347717747534,-52.64995));
#131351=CARTESIAN_POINT('',(-53.3256899305366,-36.7471331056238,-52.64995));
#131352=CARTESIAN_POINT('Origin',(-57.8922230010149,-38.7834964612722,-52.64995));
#131353=CARTESIAN_POINT('',(-53.3256899305366,-36.7471331056238,-54.8057004429536));
#131354=CARTESIAN_POINT('',(-53.3256899305366,-36.7471331056238,-55.24995));
#131355=CARTESIAN_POINT('',(-53.1795531264094,-37.1129448598587,-54.74995));
#131356=CARTESIAN_POINT('Ctrl Pts',(-53.1795531264094,-37.1129448598586,
-54.74995));
#131357=CARTESIAN_POINT('Ctrl Pts',(-53.2037450099618,-37.0446989219713,
-54.7499500137454));
#131358=CARTESIAN_POINT('Ctrl Pts',(-53.2291153576388,-36.9778304553028,
-54.7554548649733));
#131359=CARTESIAN_POINT('Ctrl Pts',(-53.2555724802117,-36.9122732840979,
-54.7662993117295));
#131360=CARTESIAN_POINT('Ctrl Pts',(-53.2781697189553,-36.8562803829428,
-54.7755616399256));
#131361=CARTESIAN_POINT('Ctrl Pts',(-53.3015600056389,-36.8012443229211,
-54.7887202323915));
#131362=CARTESIAN_POINT('Ctrl Pts',(-53.3256899305359,-36.7471331056253,
-54.8057004429567));
#131363=CARTESIAN_POINT('',(-53.0181298732915,-37.6685004154142,-54.74995));
#131364=CARTESIAN_POINT('Origin',(-57.8922230010149,-38.7834964612722,-54.74995));
#131365=CARTESIAN_POINT('Ctrl Pts',(-52.9112495105562,-38.347717747534,
-54.9585476429427));
#131366=CARTESIAN_POINT('Ctrl Pts',(-52.9283556128915,-38.1521941031454,
-54.8226237570584));
#131367=CARTESIAN_POINT('Ctrl Pts',(-52.9626456126999,-37.9110442829472,
-54.7499500131212));
#131368=CARTESIAN_POINT('Ctrl Pts',(-53.0181298732915,-37.6685004154142,
-54.74995));
#131369=CARTESIAN_POINT('Origin',(-25.30491873532,-68.8967968514054,-55.24995));
#131370=CARTESIAN_POINT('',(-24.0682702937655,-66.1635386067456,-54.74995));
#131371=CARTESIAN_POINT('',(-24.579016252936,-65.9859437829616,-54.74995));
#131372=CARTESIAN_POINT('Origin',(-25.30491873532,-68.8967968514054,-54.74995));
#131373=CARTESIAN_POINT('',(-24.0682702937655,-66.1635386067456,-52.64995));
#131374=CARTESIAN_POINT('',(-24.0682702937655,-66.1635386067456,-55.24995));
#131375=CARTESIAN_POINT('',(-25.043451507077,-65.9082127571302,-52.64995));
#131376=CARTESIAN_POINT('Origin',(-25.30491873532,-68.8967968514054,-52.64995));
#131377=CARTESIAN_POINT('',(-25.043451507077,-65.9082127571302,-54.8278826162281));
#131378=CARTESIAN_POINT('',(-25.043451507077,-65.9082127571302,-55.24995));
#131379=CARTESIAN_POINT('Ctrl Pts',(-24.579016252936,-65.9859437829616,
-54.74995));
#131380=CARTESIAN_POINT('Ctrl Pts',(-24.7361092859404,-65.946768249212,
-54.749950009163));
#131381=CARTESIAN_POINT('Ctrl Pts',(-24.8931309886626,-65.9213640983868,
-54.7753029040978));
#131382=CARTESIAN_POINT('Ctrl Pts',(-25.043451507077,-65.9082127571302,
-54.8278826162281));
#131383=CARTESIAN_POINT('Origin',(-25.30491873532,-68.8967968514054,-54.74995));
#131384=CARTESIAN_POINT('',(-24.2743783673579,-66.6190816475223,-55.24995));
#131385=CARTESIAN_POINT('Origin',(-24.2743783673579,-66.6190816475223,-54.74995));
#131386=CARTESIAN_POINT('',(-24.7,-66.4710859610356,-55.24995));
#131387=CARTESIAN_POINT('Origin',(-24.7,-66.4710859610356,-54.74995));
#131388=CARTESIAN_POINT('Origin',(-25.30491873532,-68.8967968514054,-55.24995));
#131389=CARTESIAN_POINT('Ctrl Pts',(-24.7,-66.4710859610356,-55.24995));
#131390=CARTESIAN_POINT('Ctrl Pts',(-24.579016252936,-65.9859437829616,
-55.24995));
#131391=CARTESIAN_POINT('Ctrl Pts',(-24.579016252936,-65.9859437829616,
-54.74995));
#131392=CARTESIAN_POINT('Ctrl Pts',(-24.7654791450057,-66.4384278647148,
-55.24995));
#131393=CARTESIAN_POINT('Ctrl Pts',(-24.67310951117,-65.9624790000681,-55.2343403176332));
#131394=CARTESIAN_POINT('Ctrl Pts',(-24.7361092859404,-65.946768249212,
-54.749950009163));
#131395=CARTESIAN_POINT('Ctrl Pts',(-24.8308799729202,-66.4172697443503,
-55.2626259569449));
#131396=CARTESIAN_POINT('Ctrl Pts',(-24.7709452774937,-65.9414368141194,
-55.24317591549));
#131397=CARTESIAN_POINT('Ctrl Pts',(-24.8931309886626,-65.9213640983868,
-54.7753029040978));
#131398=CARTESIAN_POINT('Ctrl Pts',(-24.8935146892254,-66.4063101061761,
-55.2889163081141));
#131399=CARTESIAN_POINT('Ctrl Pts',(-24.8576734148988,-65.9244662341272,
-55.273872259957));
#131400=CARTESIAN_POINT('Ctrl Pts',(-25.043451507077,-65.9082127571302,
-54.8278826162281));
#131401=CARTESIAN_POINT('',(-24.8935146892254,-66.4063101061761,-55.2889163081141));
#131402=CARTESIAN_POINT('Origin',(-25.0870293784509,-66.4063101061761,-54.8278826162281));
#131403=CARTESIAN_POINT('Ctrl Pts',(-24.8935146892254,-66.4063101061761,
-55.2889163081141));
#131404=CARTESIAN_POINT('Ctrl Pts',(-24.870965187297,-66.410255751606,-55.2794513602487));
#131405=CARTESIAN_POINT('Ctrl Pts',(-24.8480399226665,-66.4155232380401,
-55.271770535973));
#131406=CARTESIAN_POINT('Ctrl Pts',(-24.8248933073001,-66.4221732960834,
-55.2657995463271));
#131407=CARTESIAN_POINT('Ctrl Pts',(-24.8005026591807,-66.4291807666419,
-55.2595076412226));
#131408=CARTESIAN_POINT('Ctrl Pts',(-24.7758648518602,-66.4377234172793,
-55.2551132760505));
#131409=CARTESIAN_POINT('Ctrl Pts',(-24.7511183249211,-66.44787230635,-55.2525699472664));
#131410=CARTESIAN_POINT('Ctrl Pts',(-24.7341178138436,-66.4548444484004,
-55.2508227166642));
#131411=CARTESIAN_POINT('Ctrl Pts',(-24.7170650830423,-66.4625746537229,
-55.24995));
#131412=CARTESIAN_POINT('Ctrl Pts',(-24.7,-66.4710859610356,-55.24995));
#131413=CARTESIAN_POINT('Origin',(-42.8449509429986,-61.3393238500942,-52.64995));
#131414=CARTESIAN_POINT('',(-43.1064181712415,-64.3279079443695,-59.64995));
#131415=CARTESIAN_POINT('',(-43.1064181712415,-64.3279079443695,-52.64995));
#131416=CARTESIAN_POINT('',(-43.1064181712415,-64.3279079443695,-52.64995));
#131417=CARTESIAN_POINT('',(-44.9662712865582,-63.4606441936539,-52.64995));
#131418=CARTESIAN_POINT('Origin',(-42.8449509429986,-61.3393238500942,-52.64995));
#131419=CARTESIAN_POINT('',(-44.9662712865582,-63.4606441936539,-59.64995));
#131420=CARTESIAN_POINT('',(-44.9662712865582,-63.4606441936539,-52.64995));
#131421=CARTESIAN_POINT('Origin',(-42.8449509429986,-61.3393238500942,-59.64995));
#131422=CARTESIAN_POINT('Origin',(-44.1941738241591,-64.2327416560529,-52.64995));
#131423=CARTESIAN_POINT('',(-33.8064221286261,-65.1415521689341,-59.64995));
#131424=CARTESIAN_POINT('',(-39.4564221286262,-64.6472412200127,-59.64995));
#131425=CARTESIAN_POINT('',(-44.1941738241591,-64.2327416560529,-59.64995));
#131426=CARTESIAN_POINT('',(-33.8064221286261,-65.1415521689341,-55.74995));
#131427=CARTESIAN_POINT('',(-33.8064221286261,-65.1415521689341,-52.64995));
#131428=CARTESIAN_POINT('',(-32.8064221286262,-65.22904083246,-54.74995));
#131429=CARTESIAN_POINT('Ctrl Pts',(-32.8064221286262,-65.22904083246,-54.74995));
#131430=CARTESIAN_POINT('Ctrl Pts',(-33.0689568200132,-65.2060720231813,
-54.7499500000659));
#131431=CARTESIAN_POINT('Ctrl Pts',(-33.3284088181247,-65.1833729146174,
-54.8577231271255));
#131432=CARTESIAN_POINT('Ctrl Pts',(-33.5135289098127,-65.1671770052039,
-55.0428432188135));
#131433=CARTESIAN_POINT('Ctrl Pts',(-33.6986490015007,-65.1509810957903,
-55.2279633105015));
#131434=CARTESIAN_POINT('Ctrl Pts',(-33.8064221285606,-65.1415521689398,
-55.487415308613));
#131435=CARTESIAN_POINT('Ctrl Pts',(-33.8064221286261,-65.1415521689341,
-55.74995));
#131436=CARTESIAN_POINT('',(-32.3064221286262,-65.2727851642229,-54.74995));
#131437=CARTESIAN_POINT('',(-44.1941738241591,-64.2327416560529,-54.74995));
#131438=CARTESIAN_POINT('',(-31.3064221286262,-65.3602738277489,-55.74995));
#131439=CARTESIAN_POINT('Ctrl Pts',(-31.3064221286262,-65.3602738277489,
-55.74995));
#131440=CARTESIAN_POINT('Ctrl Pts',(-31.3064221286917,-65.3602738277431,
-55.4874153086129));
#131441=CARTESIAN_POINT('Ctrl Pts',(-31.4141952557525,-65.3508449008926,
-55.2279633105016));
#131442=CARTESIAN_POINT('Ctrl Pts',(-31.5993153474396,-65.3346489914791,
-55.0428432188135));
#131443=CARTESIAN_POINT('Ctrl Pts',(-31.7844354391267,-65.3184530820656,
-54.8577231271254));
#131444=CARTESIAN_POINT('Ctrl Pts',(-32.0438874372397,-65.2957539735015,
-54.7499500000659));
#131445=CARTESIAN_POINT('Ctrl Pts',(-32.3064221286262,-65.2727851642229,
-54.74995));
#131446=CARTESIAN_POINT('',(-31.3064221286262,-65.3602738277489,-59.64995));
#131447=CARTESIAN_POINT('',(-31.3064221286262,-65.3602738277489,-52.64995));
#131448=CARTESIAN_POINT('',(-28.7021688185769,-65.588116469328,-59.64995));
#131449=CARTESIAN_POINT('',(-44.1941738241591,-64.2327416560529,-59.64995));
#131450=CARTESIAN_POINT('',(-25.6564221281368,-65.8545847710806,-60.0322609860572));
#131451=CARTESIAN_POINT('Ctrl Pts',(-25.6564221266688,-65.8545847543119,
-60.0322609860537));
#131452=CARTESIAN_POINT('Ctrl Pts',(-25.7808509976504,-65.8436986122352,
-59.9993769765733));
#131453=CARTESIAN_POINT('Ctrl Pts',(-25.9056363008897,-65.8327812988126,
-59.9689324054821));
#131454=CARTESIAN_POINT('Ctrl Pts',(-26.0307566852339,-65.8218346938133,
-59.9407811370796));
#131455=CARTESIAN_POINT('Ctrl Pts',(-26.2520372217489,-65.8024751734605,
-59.8909944631628));
#131456=CARTESIAN_POINT('Ctrl Pts',(-26.474388494988,-65.783021979914,-59.8484921029749));
#131457=CARTESIAN_POINT('Ctrl Pts',(-26.6976513564664,-65.763489017205,
-59.812264924349));
#131458=CARTESIAN_POINT('Ctrl Pts',(-26.7996931166554,-65.7545615230246,
-59.7957073784626));
#131459=CARTESIAN_POINT('Ctrl Pts',(-26.9019251840797,-65.7456173770719,
-59.7804614113619));
#131460=CARTESIAN_POINT('Ctrl Pts',(-27.0043315823481,-65.7366579782249,
-59.7664341473284));
#131461=CARTESIAN_POINT('Ctrl Pts',(-27.0579416473936,-65.7319677053213,
-59.7590908313837));
#131462=CARTESIAN_POINT('Ctrl Pts',(-27.1116030957325,-65.7272729367138,
-59.7520917680714));
#131463=CARTESIAN_POINT('Ctrl Pts',(-27.1653166053581,-65.7225736127227,
-59.7454407818488));
#131464=CARTESIAN_POINT('Ctrl Pts',(-27.466811923079,-65.6961961857093,
-59.7081086242913));
#131465=CARTESIAN_POINT('Ctrl Pts',(-27.7698631240412,-65.6696826439603,
-59.681449712741));
#131466=CARTESIAN_POINT('Ctrl Pts',(-28.0745495814084,-65.6430260356544,
-59.6659440379886));
#131467=CARTESIAN_POINT('Ctrl Pts',(-28.2829846777342,-65.6247903294534,
-59.6553366521582));
#131468=CARTESIAN_POINT('Ctrl Pts',(-28.4921848717831,-65.6064876841949,
-59.6499500008557));
#131469=CARTESIAN_POINT('Ctrl Pts',(-28.7021688185769,-65.588116469328,
-59.64995));
#131470=CARTESIAN_POINT('',(-25.6564221286262,-65.8545847766702,-55.74995));
#131471=CARTESIAN_POINT('',(-25.6564221286262,-65.8545847766702,-52.64995));
#131472=CARTESIAN_POINT('Ctrl Pts',(-25.043451507077,-65.9082127571302,
-54.8278826162281));
#131473=CARTESIAN_POINT('Ctrl Pts',(-25.0742713040834,-65.90551637428,-54.8408189450663));
#131474=CARTESIAN_POINT('Ctrl Pts',(-25.104915072702,-65.9028353919181,
-54.8555499531048));
#131475=CARTESIAN_POINT('Ctrl Pts',(-25.1350929986057,-65.9001951655129,
-54.8720618327809));
#131476=CARTESIAN_POINT('Ctrl Pts',(-25.1657431004607,-65.8975136290646,
-54.8888320639594));
#131477=CARTESIAN_POINT('Ctrl Pts',(-25.1959121242359,-65.8948741814946,
-54.9074392518001));
#131478=CARTESIAN_POINT('Ctrl Pts',(-25.2252929736523,-65.892303690246,
-54.9278152010716));
#131479=CARTESIAN_POINT('Ctrl Pts',(-25.2553889373856,-65.8896706346014,
-54.9486870901588));
#131480=CARTESIAN_POINT('Ctrl Pts',(-25.2846571909018,-65.8871099942175,
-54.9714147499623));
#131481=CARTESIAN_POINT('Ctrl Pts',(-25.3127736146752,-65.8846501258785,
-54.9958704922167));
#131482=CARTESIAN_POINT('Ctrl Pts',(-25.3411372062356,-65.88216863316,-55.0205412216878));
#131483=CARTESIAN_POINT('Ctrl Pts',(-25.3683278367126,-65.8797897612392,
-55.0469701419947));
#131484=CARTESIAN_POINT('Ctrl Pts',(-25.3940301284273,-65.8775411020875,
-55.0749758606088));
#131485=CARTESIAN_POINT('Ctrl Pts',(-25.4197097931075,-65.8752944225448,
-55.1029569243646));
#131486=CARTESIAN_POINT('Ctrl Pts',(-25.4439029560561,-65.873177795052,
-55.1325114406684));
#131487=CARTESIAN_POINT('Ctrl Pts',(-25.4663241567112,-65.871216194172,
-55.1634160027496));
#131488=CARTESIAN_POINT('Ctrl Pts',(-25.4741688835925,-65.8705298695015,
-55.1742288870657));
#131489=CARTESIAN_POINT('Ctrl Pts',(-25.4817970097154,-65.8698624949418,
-55.1852066986187));
#131490=CARTESIAN_POINT('Ctrl Pts',(-25.4891974219829,-65.869215042763,
-55.1963388451498));
#131491=CARTESIAN_POINT('Ctrl Pts',(-25.510338242743,-65.8673654606088,
-55.228140142967));
#131492=CARTESIAN_POINT('Ctrl Pts',(-25.5295950731415,-65.8656807062535,
-55.2611692657123));
#131493=CARTESIAN_POINT('Ctrl Pts',(-25.5468557307134,-65.864170594391,
-55.295083999148));
#131494=CARTESIAN_POINT('Ctrl Pts',(-25.5641515040968,-65.862657410293,
-55.3290677301512));
#131495=CARTESIAN_POINT('Ctrl Pts',(-25.5794427196934,-65.8613196022768,
-55.363939731283));
#131496=CARTESIAN_POINT('Ctrl Pts',(-25.5926659905796,-65.8601627159795,
-55.3993402855053));
#131497=CARTESIAN_POINT('Ctrl Pts',(-25.6056853291763,-65.8590236714457,
-55.4341948843334));
#131498=CARTESIAN_POINT('Ctrl Pts',(-25.6166999804352,-65.8580600143278,
-55.4695609780295));
#131499=CARTESIAN_POINT('Ctrl Pts',(-25.6256992872677,-65.8572726770004,
-55.5050939643816));
#131500=CARTESIAN_POINT('Ctrl Pts',(-25.6345695399044,-65.8564966304521,
-55.5401173913793));
#131501=CARTESIAN_POINT('Ctrl Pts',(-25.641481865841,-65.855891880294,-55.5753022272925));
#131502=CARTESIAN_POINT('Ctrl Pts',(-25.6464749038184,-65.8554550460744,
-55.6103291116175));
#131503=CARTESIAN_POINT('Ctrl Pts',(-25.6513699614093,-65.8550267840279,
-55.6446686493459));
#131504=CARTESIAN_POINT('Ctrl Pts',(-25.6544204578572,-65.8547599001706,
-55.6788558270728));
#131505=CARTESIAN_POINT('Ctrl Pts',(-25.6557087574904,-65.8546471885575,
-55.7126093508298));
#131506=CARTESIAN_POINT('Ctrl Pts',(-25.6561862637138,-65.8546054121762,
-55.7251200410772));
#131507=CARTESIAN_POINT('Ctrl Pts',(-25.6564221286231,-65.8545847766705,
-55.7375713926724));
#131508=CARTESIAN_POINT('Ctrl Pts',(-25.6564221286262,-65.8545847766702,
-55.74995));
#131509=CARTESIAN_POINT('',(-44.1941738241591,-64.2327416560529,-52.64995));
#131510=CARTESIAN_POINT('',(-41.9564221286262,-64.428519561198,-59.64995));
#131511=CARTESIAN_POINT('',(-44.1941738241591,-64.2327416560529,-59.64995));
#131512=CARTESIAN_POINT('',(-41.9564221286262,-64.428519561198,-55.74995));
#131513=CARTESIAN_POINT('',(-41.9564221286262,-64.428519561198,-52.64995));
#131514=CARTESIAN_POINT('',(-40.9564221286262,-64.5160082247239,-54.74995));
#131515=CARTESIAN_POINT('Ctrl Pts',(-40.9564221286262,-64.5160082247239,
-54.74995));
#131516=CARTESIAN_POINT('Ctrl Pts',(-41.2189568200132,-64.4930394154452,
-54.7499500000659));
#131517=CARTESIAN_POINT('Ctrl Pts',(-41.4784088181247,-64.4703403068813,
-54.8577231271255));
#131518=CARTESIAN_POINT('Ctrl Pts',(-41.6635289098127,-64.4541443974678,
-55.0428432188135));
#131519=CARTESIAN_POINT('Ctrl Pts',(-41.8486490015007,-64.4379484880542,
-55.2279633105015));
#131520=CARTESIAN_POINT('Ctrl Pts',(-41.9564221285606,-64.4285195612037,
-55.487415308613));
#131521=CARTESIAN_POINT('Ctrl Pts',(-41.9564221286262,-64.428519561198,
-55.74995));
#131522=CARTESIAN_POINT('',(-40.4564221286262,-64.5597525564868,-54.74995));
#131523=CARTESIAN_POINT('',(-44.1941738241591,-64.2327416560529,-54.74995));
#131524=CARTESIAN_POINT('',(-39.4564221286262,-64.6472412200127,-55.74995));
#131525=CARTESIAN_POINT('Ctrl Pts',(-39.4564221286262,-64.6472412200127,
-55.74995));
#131526=CARTESIAN_POINT('Ctrl Pts',(-39.4564221286917,-64.647241220007,
-55.4874153086129));
#131527=CARTESIAN_POINT('Ctrl Pts',(-39.5641952557525,-64.6378122931564,
-55.2279633105016));
#131528=CARTESIAN_POINT('Ctrl Pts',(-39.7493153474396,-64.6216163837429,
-55.0428432188135));
#131529=CARTESIAN_POINT('Ctrl Pts',(-39.9344354391268,-64.6054204743294,
-54.8577231271254));
#131530=CARTESIAN_POINT('Ctrl Pts',(-40.1938874372398,-64.5827213657654,
-54.7499500000659));
#131531=CARTESIAN_POINT('Ctrl Pts',(-40.4564221286262,-64.5597525564868,
-54.74995));
#131532=CARTESIAN_POINT('',(-39.4564221286262,-64.6472412200127,-52.64995));
#131533=CARTESIAN_POINT('Origin',(-42.8449509429986,-61.3393238500942,-59.64995));
#131534=CARTESIAN_POINT('',(-43.0192624284939,-63.3317132462777,-60.64995));
#131535=CARTESIAN_POINT('Origin',(-43.0192624284939,-63.3317132462777,-59.64995));
#131536=CARTESIAN_POINT('',(-44.2591645053717,-62.7535374124673,-60.64995));
#131537=CARTESIAN_POINT('Origin',(-44.2591645053717,-62.7535374124673,-59.64995));
#131538=CARTESIAN_POINT('Origin',(-42.8449509429986,-61.3393238500942,-60.64995));
#131539=CARTESIAN_POINT('Origin',(-48.3718238300662,-55.8124509630266,-52.64995));
#131540=CARTESIAN_POINT('',(-50.4931441736259,-57.9337713065862,-59.64995));
#131541=CARTESIAN_POINT('',(-50.4931441736259,-57.9337713065862,-52.64995));
#131542=CARTESIAN_POINT('',(-50.4931441736259,-57.9337713065862,-52.64995));
#131543=CARTESIAN_POINT('',(-51.3604079243415,-56.0739181912695,-52.64995));
#131544=CARTESIAN_POINT('Origin',(-48.3718238300662,-55.8124509630266,-52.64995));
#131545=CARTESIAN_POINT('',(-51.3604079243415,-56.0739181912695,-59.64995));
#131546=CARTESIAN_POINT('',(-51.3604079243415,-56.0739181912695,-52.64995));
#131547=CARTESIAN_POINT('Origin',(-48.3718238300662,-55.8124509630266,-59.64995));
#131548=CARTESIAN_POINT('Origin',(-51.265241636025,-57.1616738441871,-52.64995));
#131549=CARTESIAN_POINT('',(-51.265241636025,-57.1616738441871,-52.64995));
#131550=CARTESIAN_POINT('',(-51.265241636025,-57.1616738441871,-59.64995));
#131551=CARTESIAN_POINT('Origin',(-48.3718238300662,-55.8124509630266,-59.64995));
#131552=CARTESIAN_POINT('',(-49.7860373924393,-57.2266645253997,-60.64995));
#131553=CARTESIAN_POINT('Origin',(-49.7860373924393,-57.2266645253997,-59.64995));
#131554=CARTESIAN_POINT('',(-50.3642132262497,-55.9867624485218,-60.64995));
#131555=CARTESIAN_POINT('Origin',(-50.3642132262497,-55.9867624485218,-59.64995));
#131556=CARTESIAN_POINT('Origin',(-48.3718238300662,-55.8124509630266,-60.64995));
#131557=CARTESIAN_POINT('Origin',(-52.9858497431864,-37.4950331867729,-52.64995));
#131558=CARTESIAN_POINT('',(-52.6206164493,-41.6696688386047,-59.64995));
#131559=CARTESIAN_POINT('',(-52.8772422786263,-38.736422148331,-60.0032396521556));
#131560=CARTESIAN_POINT('Ctrl Pts',(-52.6206164493,-41.6696688386047,-59.64995));
#131561=CARTESIAN_POINT('Ctrl Pts',(-52.6471771938443,-41.3660781392638,
-59.649950001162));
#131562=CARTESIAN_POINT('Ctrl Pts',(-52.6736027803766,-41.0640322847433,
-59.6612277190036));
#131563=CARTESIAN_POINT('Ctrl Pts',(-52.6998985433591,-40.7634703219199,
-59.6832689389194));
#131564=CARTESIAN_POINT('Ctrl Pts',(-52.7166476389898,-40.5720272722695,
-59.6973081018229));
#131565=CARTESIAN_POINT('Ctrl Pts',(-52.7333441220444,-40.3811856093979,
-59.715714898338));
#131566=CARTESIAN_POINT('Ctrl Pts',(-52.7499897489645,-40.1909252438875,
-59.7383666003326));
#131567=CARTESIAN_POINT('Ctrl Pts',(-52.7543856861046,-40.1406794579502,
-59.7443486795034));
#131568=CARTESIAN_POINT('Ctrl Pts',(-52.7587779570344,-40.0904755740926,
-59.7506312543479));
#131569=CARTESIAN_POINT('Ctrl Pts',(-52.7631665715902,-40.0403134816151,
-59.7572129455377));
#131570=CARTESIAN_POINT('Ctrl Pts',(-52.7801318002605,-39.8464000361234,
-59.7826560311971));
#131571=CARTESIAN_POINT('Ctrl Pts',(-52.7970456659898,-39.6530737072156,
-59.8124579292866));
#131572=CARTESIAN_POINT('Ctrl Pts',(-52.813898709432,-39.4604424150672,
-59.8472750881764));
#131573=CARTESIAN_POINT('Ctrl Pts',(-52.8286848633261,-39.2914357937844,
-59.8778222039694));
#131574=CARTESIAN_POINT('Ctrl Pts',(-52.8434252414647,-39.1229522134554,
-59.9121898106588));
#131575=CARTESIAN_POINT('Ctrl Pts',(-52.8581158408284,-38.9550379662894,
-59.9506823384324));
#131576=CARTESIAN_POINT('Ctrl Pts',(-52.8645007938114,-38.882057651002,
-59.9674122875614));
#131577=CARTESIAN_POINT('Ctrl Pts',(-52.870876360439,-38.8091846968969,
-59.9849220508822));
#131578=CARTESIAN_POINT('Ctrl Pts',(-52.8772422685109,-38.7364221474456,
-60.003239652154));
#131579=CARTESIAN_POINT('',(-52.3829313330767,-44.3864221486262,-59.64995));
#131580=CARTESIAN_POINT('',(-52.9858497431864,-37.4950331867729,-59.64995));
#131581=CARTESIAN_POINT('',(-52.3829313330767,-44.3864221486262,-55.74995));
#131582=CARTESIAN_POINT('',(-52.3829313330767,-44.3864221486262,-52.64995));
#131583=CARTESIAN_POINT('',(-52.2954426695508,-45.3864221486261,-54.74995));
#131584=CARTESIAN_POINT('Ctrl Pts',(-52.2954426695508,-45.3864221486261,
-54.74995));
#131585=CARTESIAN_POINT('Ctrl Pts',(-52.3184114788294,-45.123887457239,
-54.7499500000658));
#131586=CARTESIAN_POINT('Ctrl Pts',(-52.3411105873933,-44.8644354591276,
-54.8577231271254));
#131587=CARTESIAN_POINT('Ctrl Pts',(-52.3573064968069,-44.6793153674396,
-55.0428432188135));
#131588=CARTESIAN_POINT('Ctrl Pts',(-52.3735024062205,-44.4941952757516,
-55.2279633105015));
#131589=CARTESIAN_POINT('Ctrl Pts',(-52.3829313330709,-44.3864221486917,
-55.4874153086129));
#131590=CARTESIAN_POINT('Ctrl Pts',(-52.3829313330767,-44.3864221486262,
-55.74995));
#131591=CARTESIAN_POINT('',(-52.2516983377878,-45.8864221486262,-54.74995));
#131592=CARTESIAN_POINT('',(-52.9858497431864,-37.4950331867729,-54.74995));
#131593=CARTESIAN_POINT('',(-52.1642096742619,-46.8864221486262,-55.74995));
#131594=CARTESIAN_POINT('Ctrl Pts',(-52.1642096742619,-46.8864221486262,
-55.74995));
#131595=CARTESIAN_POINT('Ctrl Pts',(-52.1642096742676,-46.8864221485606,
-55.487415308613));
#131596=CARTESIAN_POINT('Ctrl Pts',(-52.1736386011181,-46.7786490215007,
-55.2279633105015));
#131597=CARTESIAN_POINT('Ctrl Pts',(-52.1898345105317,-46.5935289298127,
-55.0428432188135));
#131598=CARTESIAN_POINT('Ctrl Pts',(-52.2060304199453,-46.4084088381247,
-54.8577231271255));
#131599=CARTESIAN_POINT('Ctrl Pts',(-52.2287295285091,-46.1489568400132,
-54.7499500000658));
#131600=CARTESIAN_POINT('Ctrl Pts',(-52.2516983377878,-45.8864221486262,
-54.74995));
#131601=CARTESIAN_POINT('',(-52.1642096742619,-46.8864221486262,-59.64995));
#131602=CARTESIAN_POINT('',(-52.1642096742619,-46.8864221486262,-52.64995));
#131603=CARTESIAN_POINT('',(-51.6698987253405,-52.5364221486262,-59.64995));
#131604=CARTESIAN_POINT('',(-52.9858497431864,-37.4950331867729,-59.64995));
#131605=CARTESIAN_POINT('',(-51.6698987253405,-52.5364221486262,-55.74995));
#131606=CARTESIAN_POINT('',(-51.6698987253405,-52.5364221486262,-52.64995));
#131607=CARTESIAN_POINT('',(-51.5824100618146,-53.5364221486262,-54.74995));
#131608=CARTESIAN_POINT('Ctrl Pts',(-51.5824100618146,-53.5364221486262,
-54.74995));
#131609=CARTESIAN_POINT('Ctrl Pts',(-51.6053788710933,-53.2738874572391,
-54.7499500000658));
#131610=CARTESIAN_POINT('Ctrl Pts',(-51.6280779796571,-53.0144354591276,
-54.8577231271254));
#131611=CARTESIAN_POINT('Ctrl Pts',(-51.6442738890707,-52.8293153674396,
-55.0428432188135));
#131612=CARTESIAN_POINT('Ctrl Pts',(-51.6604697984843,-52.6441952757516,
-55.2279633105015));
#131613=CARTESIAN_POINT('Ctrl Pts',(-51.6698987253348,-52.5364221486917,
-55.4874153086129));
#131614=CARTESIAN_POINT('Ctrl Pts',(-51.6698987253405,-52.5364221486262,
-55.74995));
#131615=CARTESIAN_POINT('',(-51.5386657300517,-54.0364221486261,-54.74995));
#131616=CARTESIAN_POINT('',(-52.9858497431864,-37.4950331867729,-54.74995));
#131617=CARTESIAN_POINT('',(-51.4511770665258,-55.0364221486262,-55.74995));
#131618=CARTESIAN_POINT('Ctrl Pts',(-51.4511770665258,-55.0364221486262,
-55.74995));
#131619=CARTESIAN_POINT('Ctrl Pts',(-51.4511770665315,-55.0364221485606,
-55.4874153086129));
#131620=CARTESIAN_POINT('Ctrl Pts',(-51.460605993382,-54.9286490214999,
-55.2279633105015));
#131621=CARTESIAN_POINT('Ctrl Pts',(-51.4768019027956,-54.7435289298127,
-55.0428432188135));
#131622=CARTESIAN_POINT('Ctrl Pts',(-51.4929978122091,-54.5584088381255,
-54.8577231271254));
#131623=CARTESIAN_POINT('Ctrl Pts',(-51.5156969207731,-54.2989568400126,
-54.7499500000658));
#131624=CARTESIAN_POINT('Ctrl Pts',(-51.5386657300517,-54.0364221486262,
-54.74995));
#131625=CARTESIAN_POINT('',(-51.4511770665258,-55.0364221486262,-59.64995));
#131626=CARTESIAN_POINT('',(-51.4511770665258,-55.0364221486262,-52.64995));
#131627=CARTESIAN_POINT('',(-52.9858497431864,-37.4950331867729,-59.64995));
#131628=CARTESIAN_POINT('',(-52.9858497431864,-37.4950331867729,-52.64995));
#131629=CARTESIAN_POINT('',(-52.877242281998,-38.7364221486262,-55.74995));
#131630=CARTESIAN_POINT('Origin',(-52.9541266237314,-37.8576301013502,-55.6904184160493));
#131631=CARTESIAN_POINT('',(-52.877242281998,-38.7364221486262,-52.64995));
#131632=CARTESIAN_POINT('Ctrl Pts',(-1.2393865421354,-71.3418443611208,
-56.1920015047684));
#131633=CARTESIAN_POINT('Ctrl Pts',(-0.749999999999951,-71.3522348691612,
-56.1920015047684));
#131634=CARTESIAN_POINT('Ctrl Pts',(-0.749999999999965,-71.8417317029411,
-56.1920015047684));
#131635=CARTESIAN_POINT('Ctrl Pts',(-1.23938657388158,-71.3418443604468,
-55.8977818815622));
#131636=CARTESIAN_POINT('Ctrl Pts',(-0.817143227758975,-71.350809303989,
-55.9852769982734));
#131637=CARTESIAN_POINT('Ctrl Pts',(-0.749999999999968,-71.7679993860759,
-55.9713019100196));
#131638=CARTESIAN_POINT('Ctrl Pts',(-1.17148444765176,-71.3435038399877,
-55.5953607449048));
#131639=CARTESIAN_POINT('Ctrl Pts',(-0.822125649397247,-71.3503107976076,
-55.7434666115786));
#131640=CARTESIAN_POINT('Ctrl Pts',(-0.715758200751532,-71.705555960146,
-55.7746050694403));
#131641=CARTESIAN_POINT('Ctrl Pts',(-0.911534986295056,-71.3479485504093,
-55.2320500655911));
#131642=CARTESIAN_POINT('Ctrl Pts',(-0.680372527884655,-71.3515033251648,
-55.4569572564689));
#131643=CARTESIAN_POINT('Ctrl Pts',(-0.584670453989408,-71.6422004184537,
-55.5485996630821));
#131644=CARTESIAN_POINT('Ctrl Pts',(-0.802354774810878,-71.3496303532999,
-55.1310699758717));
#131645=CARTESIAN_POINT('Ctrl Pts',(-0.61343369370942,-71.3521282334297,
-55.3772175182816));
#131646=CARTESIAN_POINT('Ctrl Pts',(-0.529612862082923,-71.6265518657637,
-55.4878844649265));
#131647=CARTESIAN_POINT('Ctrl Pts',(-0.543457447472851,-71.3526142995993,
-54.9878205454944));
#131648=CARTESIAN_POINT('Ctrl Pts',(-0.446700352388622,-71.3534136965962,
-55.2655230738672));
#131649=CARTESIAN_POINT('Ctrl Pts',(-0.399055664911118,-71.6054835497946,
-55.4025039623078));
#131650=CARTESIAN_POINT('Ctrl Pts',(-0.399927732415193,-71.3538238656642,
-54.9488753843798));
#131651=CARTESIAN_POINT('Ctrl Pts',(-0.350200382979481,-71.3540360830669,
-55.2347429562386));
#131652=CARTESIAN_POINT('Ctrl Pts',(-0.326675282358978,-71.6004595978917,
-55.3797802668488));
#131653=CARTESIAN_POINT('Ctrl Pts',(-0.24960231081565,-71.3544665017672,
-54.948950578459));
#131654=CARTESIAN_POINT('Ctrl Pts',(-0.249744175924072,-71.3544658952987,
-55.234934426787));
#131655=CARTESIAN_POINT('Ctrl Pts',(-0.250869887203208,-71.6009673739965,
-55.3799259279328));
#131656=CARTESIAN_POINT('',(-0.749999999999963,-71.8417317505524,-56.1920013490171));
#131657=CARTESIAN_POINT('',(-1.2393865421354,-71.3418443611208,-56.1920015047684));
#131658=CARTESIAN_POINT('Origin',(-1.24999999999996,-71.8417317029411,-56.1920015047684));
#131659=CARTESIAN_POINT('',(-0.250869887203081,-71.6009673739936,-55.3799259279326));
#131660=CARTESIAN_POINT('Ctrl Pts',(-0.749999999999961,-71.8417316609121,
-56.1920013789646));
#131661=CARTESIAN_POINT('Ctrl Pts',(-0.749999986987558,-71.7679993623464,
-55.9713018352718));
#131662=CARTESIAN_POINT('Ctrl Pts',(-0.715758184146415,-71.7055559521206,
-55.7746050408118));
#131663=CARTESIAN_POINT('Ctrl Pts',(-0.584670453989408,-71.6422004184537,
-55.5485996630821));
#131664=CARTESIAN_POINT('Ctrl Pts',(-0.529612862082923,-71.6265518657637,
-55.4878844649265));
#131665=CARTESIAN_POINT('Ctrl Pts',(-0.399055664911118,-71.6054835497946,
-55.4025039623078));
#131666=CARTESIAN_POINT('Ctrl Pts',(-0.326675282358978,-71.6004595978917,
-55.3797802668488));
#131667=CARTESIAN_POINT('Ctrl Pts',(-0.250869887203096,-71.6009673739964,
-55.3799259279342));
#131668=CARTESIAN_POINT('',(-0.249602310815417,-71.3544665017672,-54.9489505784606));
#131669=CARTESIAN_POINT('Origin',(-0.251739774406202,-71.8544619329957,
-54.9489505784606));
#131670=CARTESIAN_POINT('Ctrl Pts',(-0.249602310815417,-71.3544665017672,
-54.9489505784606));
#131671=CARTESIAN_POINT('Ctrl Pts',(-0.399927732415193,-71.3538238656642,
-54.9488753843798));
#131672=CARTESIAN_POINT('Ctrl Pts',(-0.543457447472851,-71.3526142995993,
-54.9878205454944));
#131673=CARTESIAN_POINT('Ctrl Pts',(-0.802354774810878,-71.3496303532999,
-55.1310699758717));
#131674=CARTESIAN_POINT('Ctrl Pts',(-0.911534986295056,-71.3479485504093,
-55.2320500655911));
#131675=CARTESIAN_POINT('Ctrl Pts',(-1.17148444765176,-71.3435038399877,
-55.5953607449048));
#131676=CARTESIAN_POINT('Ctrl Pts',(-1.23938657388158,-71.3418443604468,
-55.8977818815622));
#131677=CARTESIAN_POINT('Ctrl Pts',(-1.2393865421354,-71.3418443611208,
-56.1920015047684));
#131678=CARTESIAN_POINT('Origin',(-1.24999999999996,-71.8417317029411,-55.24995));
#131679=CARTESIAN_POINT('',(-0.749999999999965,-71.8417317029411,-60.42825533736));
#131680=CARTESIAN_POINT('',(-1.2393865421354,-71.3418443611208,-60.42825533736));
#131681=CARTESIAN_POINT('Origin',(-1.24999999999996,-71.8417317029411,-60.42825533736));
#131682=CARTESIAN_POINT('',(-0.749999999999965,-71.8417317029411,-55.24995));
#131683=CARTESIAN_POINT('',(-1.2393865421354,-71.3418443611208,-55.24995));
#131684=CARTESIAN_POINT('Origin',(0.,-12.9675000200281,-60.42825533736));
#131685=CARTESIAN_POINT('',(-6.84677576889373,-70.8578246683297,-60.8508735991007));
#131686=CARTESIAN_POINT('',(-1.24035792914739,-71.2481103336038,-60.8508735991007));
#131687=CARTESIAN_POINT('Origin',(0.,-12.9675000200281,-60.8508735991007));
#131688=CARTESIAN_POINT('Origin',(-1.24990493606806,-70.3423238919629,-60.4282489645659));
#131689=CARTESIAN_POINT('',(-6.84141371258755,-70.9528017323285,-60.42825533736));
#131690=CARTESIAN_POINT('Origin',(0.,-12.9675000200281,-60.42825533736));
#131691=CARTESIAN_POINT('Origin',(-6.92387950998942,-69.4954305645409,-60.33066203808));
#131692=CARTESIAN_POINT('Origin',(-6.9,-71.449357516634,-55.24995));
#131693=CARTESIAN_POINT('',(-6.9,-70.949357516634,-56.0666111687498));
#131694=CARTESIAN_POINT('',(-7.40000000638209,-71.4493575166325,-56.0666111687523));
#131695=CARTESIAN_POINT('Origin',(-6.9,-71.449357516634,-56.0666111687498));
#131696=CARTESIAN_POINT('',(-7.4,-71.449357516634,-60.42825533736));
#131697=CARTESIAN_POINT('',(-7.4,-71.449357516634,-55.24995));
#131698=CARTESIAN_POINT('',(-6.9,-70.949357516634,-60.42825533736));
#131699=CARTESIAN_POINT('Origin',(-6.9,-71.449357516634,-60.42825533736));
#131700=CARTESIAN_POINT('Origin',(-6.9,-71.449357516634,-60.42825533736));
#131701=CARTESIAN_POINT('',(-6.84141371258755,-70.9528017323285,-56.0666111687498));
#131702=CARTESIAN_POINT('',(-6.84141371258755,-70.9528017323285,-55.24995));
#131703=CARTESIAN_POINT('Origin',(-6.9,-71.449357516634,-56.0666111687498));
#131704=CARTESIAN_POINT('Ctrl Pts',(-7.86502491569091,-70.8228501557662,
-54.8850140141151));
#131705=CARTESIAN_POINT('Ctrl Pts',(-7.87072047725574,-70.8220758845275,
-55.2299609924928));
#131706=CARTESIAN_POINT('Ctrl Pts',(-7.91618843693208,-71.1413940909409,
-55.352394666395));
#131707=CARTESIAN_POINT('Ctrl Pts',(-7.72241706825884,-70.8422366821738,
-54.8874327557878));
#131708=CARTESIAN_POINT('Ctrl Pts',(-7.77985413280654,-70.8344428879727,
-55.236521459352));
#131709=CARTESIAN_POINT('Ctrl Pts',(-7.844285602846,-71.157562039706,-55.3560236134997));
#131710=CARTESIAN_POINT('Ctrl Pts',(-7.5794821547774,-70.8610938450093,
-54.9239881329105));
#131711=CARTESIAN_POINT('Ctrl Pts',(-7.69016530757976,-70.8464897855799,
-55.2681271844367));
#131712=CARTESIAN_POINT('Ctrl Pts',(-7.77219443565847,-71.177222127411,
-55.3781864762555));
#131713=CARTESIAN_POINT('Ctrl Pts',(-7.32391158111293,-70.8939799308472,
-55.0534925677837));
#131714=CARTESIAN_POINT('Ctrl Pts',(-7.53737924067218,-70.8668804541439,
-55.3692852810369));
#131715=CARTESIAN_POINT('Ctrl Pts',(-7.64331486532417,-71.2207339188645,
-55.4539331018544));
#131716=CARTESIAN_POINT('Ctrl Pts',(-7.20960774580809,-70.9082476913312,
-55.1469663768362));
#131717=CARTESIAN_POINT('Ctrl Pts',(-7.47303212720142,-70.8754018535837,
-55.4405214339084));
#131718=CARTESIAN_POINT('Ctrl Pts',(-7.58567352642291,-71.2449041853563,
-55.5078568245776));
#131719=CARTESIAN_POINT('Ctrl Pts',(-7.02628770602923,-70.9307639518508,
-55.3693141862512));
#131720=CARTESIAN_POINT('Ctrl Pts',(-7.38267219174721,-70.8874980297502,
-55.6027965247728));
#131721=CARTESIAN_POINT('Ctrl Pts',(-7.49322857950783,-71.2966779191941,
-55.6376571876191));
#131722=CARTESIAN_POINT('Ctrl Pts',(-6.95597670016225,-70.9391888126349,
-55.4992549495758));
#131723=CARTESIAN_POINT('Ctrl Pts',(-7.35664509914443,-70.8910885028411,
-55.6963616877968));
#131724=CARTESIAN_POINT('Ctrl Pts',(-7.45777202258463,-71.3246266217341,
-55.7141753031788));
#131725=CARTESIAN_POINT('Ctrl Pts',(-6.86374100295758,-70.950181682438,
-55.7748476118441));
#131726=CARTESIAN_POINT('Ctrl Pts',(-7.34624804767826,-70.8930407983775,
-55.8848711139694));
#131727=CARTESIAN_POINT('Ctrl Pts',(-7.41125924474539,-71.38419243799,-55.8811540356734));
#131728=CARTESIAN_POINT('Ctrl Pts',(-6.84141371299613,-70.9528017322803,
-55.9212771125469));
#131729=CARTESIAN_POINT('Ctrl Pts',(-7.36384050363832,-70.8911630457611,
-55.9819410866112));
#131730=CARTESIAN_POINT('Ctrl Pts',(-7.4,-71.4160375965177,-55.9720928529598));
#131731=CARTESIAN_POINT('Ctrl Pts',(-6.84141371258755,-70.9528017323285,
-56.0666111687498));
#131732=CARTESIAN_POINT('Ctrl Pts',(-7.3999999999998,-70.8868967568689,
-56.06661116875));
#131733=CARTESIAN_POINT('Ctrl Pts',(-7.4,-71.4493575166339,-56.06661116875));
#131734=CARTESIAN_POINT('',(-7.86502491569136,-70.8228501557662,-54.8850140141151));
#131735=CARTESIAN_POINT('Ctrl Pts',(-6.84141371258755,-70.9528017323285,
-56.0666111687498));
#131736=CARTESIAN_POINT('Ctrl Pts',(-6.84141371272281,-70.9528017323125,
-56.0185004951022));
#131737=CARTESIAN_POINT('Ctrl Pts',(-6.84385625486988,-70.9525150960356,
-55.9705185340178));
#131738=CARTESIAN_POINT('Ctrl Pts',(-6.84874395952159,-70.951938515923,
-55.922884915407));
#131739=CARTESIAN_POINT('Ctrl Pts',(-6.85371160739848,-70.9513525052747,
-55.8744722020329));
#131740=CARTESIAN_POINT('Ctrl Pts',(-6.86120476133718,-70.9504670347036,
-55.8264180258316));
#131741=CARTESIAN_POINT('Ctrl Pts',(-6.87128050874744,-70.9492722819139,
-55.7789472465282));
#131742=CARTESIAN_POINT('Ctrl Pts',(-6.88084558986922,-70.9481380824458,
-55.7338824154579));
#131743=CARTESIAN_POINT('Ctrl Pts',(-6.89273836925603,-70.9467251353176,
-55.6893423359324));
#131744=CARTESIAN_POINT('Ctrl Pts',(-6.90705554696955,-70.9450193012212,
-55.645530903299));
#131745=CARTESIAN_POINT('Ctrl Pts',(-6.90781992104138,-70.9449282291272,
-55.6431918722535));
#131746=CARTESIAN_POINT('Ctrl Pts',(-6.90859121688158,-70.9448363208197,
-55.6408549230079));
#131747=CARTESIAN_POINT('Ctrl Pts',(-6.90936945309023,-70.944743573674,
-55.638520088397));
#131748=CARTESIAN_POINT('Ctrl Pts',(-6.90953264041296,-70.9447241256476,
-55.6380305000112));
#131749=CARTESIAN_POINT('Ctrl Pts',(-6.90969612810931,-70.9447046413087,
-55.6375410188016));
#131750=CARTESIAN_POINT('Ctrl Pts',(-6.90985991625218,-70.9446851206452,
-55.6370516451987));
#131751=CARTESIAN_POINT('Ctrl Pts',(-6.93890470840657,-70.9412234926851,
-55.5502703047941));
#131752=CARTESIAN_POINT('Ctrl Pts',(-6.97755496303225,-70.9365992546703,
-55.4665613054832));
#131753=CARTESIAN_POINT('Ctrl Pts',(-7.02515534568038,-70.9308292795787,
-55.3886379526022));
#131754=CARTESIAN_POINT('Ctrl Pts',(-7.05265246384246,-70.9274961616906,
-55.3436242883719));
#131755=CARTESIAN_POINT('Ctrl Pts',(-7.08313672341662,-70.92378064339,-55.3005419198596));
#131756=CARTESIAN_POINT('Ctrl Pts',(-7.11648530834341,-70.9196854249332,
-55.2599212236758));
#131757=CARTESIAN_POINT('Ctrl Pts',(-7.11697272521332,-70.9196255699628,
-55.2593275189465));
#131758=CARTESIAN_POINT('Ctrl Pts',(-7.11746075366589,-70.9195656339149,
-55.2587343401393));
#131759=CARTESIAN_POINT('Ctrl Pts',(-7.11794939330103,-70.9195056167998,
-55.2581416889457));
#131760=CARTESIAN_POINT('Ctrl Pts',(-7.1776695866293,-70.912170489928,-55.1857094887856));
#131761=CARTESIAN_POINT('Ctrl Pts',(-7.24707274855763,-70.9035491680656,
-55.1207030262982));
#131762=CARTESIAN_POINT('Ctrl Pts',(-7.32365993963484,-70.8938669826859,
-55.0662525944787));
#131763=CARTESIAN_POINT('Ctrl Pts',(-7.36395975880774,-70.8887722623481,
-55.0376010337496));
#131764=CARTESIAN_POINT('Ctrl Pts',(-7.406247882039,-70.8833838941671,-55.0118727368965));
#131765=CARTESIAN_POINT('Ctrl Pts',(-7.450155212976,-70.8777352422905,-54.9895263260323));
#131766=CARTESIAN_POINT('Ctrl Pts',(-7.45066930715087,-70.8776691043822,
-54.989264680439));
#131767=CARTESIAN_POINT('Ctrl Pts',(-7.45118359869241,-70.877602933957,
-54.9890035107279));
#131768=CARTESIAN_POINT('Ctrl Pts',(-7.45169808724107,-70.8775367310404,
-54.9887428173532));
#131769=CARTESIAN_POINT('Ctrl Pts',(-7.48702485166255,-70.8729909839197,
-54.9708426066328));
#131770=CARTESIAN_POINT('Ctrl Pts',(-7.52340553096599,-70.8682741670682,
-54.9551443604244));
#131771=CARTESIAN_POINT('Ctrl Pts',(-7.56060369340833,-70.8634146986663,
-54.9417107539087));
#131772=CARTESIAN_POINT('Ctrl Pts',(-7.59755058615547,-70.8585880554651,
-54.9283678899994));
#131773=CARTESIAN_POINT('Ctrl Pts',(-7.63530511490777,-70.8536205390166,
-54.9172587967144));
#131774=CARTESIAN_POINT('Ctrl Pts',(-7.67365359691511,-70.8485368945066,
-54.9084923483496));
#131775=CARTESIAN_POINT('Ctrl Pts',(-7.71043547056378,-70.8436609265346,
-54.9000840260582));
#131776=CARTESIAN_POINT('Ctrl Pts',(-7.74776474509219,-70.8386779998652,
-54.8938307755624));
#131777=CARTESIAN_POINT('Ctrl Pts',(-7.78545391476949,-70.8336090347271,
-54.8898753244176));
#131778=CARTESIAN_POINT('Ctrl Pts',(-7.81182391853939,-70.8300624288733,
-54.887107811562));
#131779=CARTESIAN_POINT('Ctrl Pts',(-7.83837014274923,-70.8264736832847,
-54.8854661001065));
#131780=CARTESIAN_POINT('Ctrl Pts',(-7.86502491569091,-70.8228501557662,
-54.8850140141151));
#131781=CARTESIAN_POINT('',(-7.91618843693321,-71.1413940908982,-55.3523946663788));
#131782=CARTESIAN_POINT('Origin',(-7.93237687386467,-71.3182931027643,-54.8850140141151));
#131783=CARTESIAN_POINT('Ctrl Pts',(-7.91618843693208,-71.1413940909408,
-55.3523946663949));
#131784=CARTESIAN_POINT('Ctrl Pts',(-7.844285602846,-71.157562039706,-55.3560236134997));
#131785=CARTESIAN_POINT('Ctrl Pts',(-7.77219443565847,-71.177222127411,
-55.3781864762555));
#131786=CARTESIAN_POINT('Ctrl Pts',(-7.64331486532417,-71.2207339188645,
-55.4539331018544));
#131787=CARTESIAN_POINT('Ctrl Pts',(-7.58567352642291,-71.2449041853563,
-55.5078568245776));
#131788=CARTESIAN_POINT('Ctrl Pts',(-7.49322857950783,-71.2966779191941,
-55.6376571876191));
#131789=CARTESIAN_POINT('Ctrl Pts',(-7.45777202258463,-71.3246266217341,
-55.7141753031788));
#131790=CARTESIAN_POINT('Ctrl Pts',(-7.41125924474539,-71.38419243799,-55.8811540356734));
#131791=CARTESIAN_POINT('Ctrl Pts',(-7.4,-71.4160375965177,-55.9720928529598));
#131792=CARTESIAN_POINT('Ctrl Pts',(-7.4,-71.449357516634,-56.06661116875));
#131793=CARTESIAN_POINT('Ctrl Pts',(-8.35962920986988,-70.7534564084689,
-54.8763024037297));
#131794=CARTESIAN_POINT('Ctrl Pts',(-8.36589323739404,-70.752550220344,
-55.2292031667489));
#131795=CARTESIAN_POINT('Ctrl Pts',(-8.41560835021369,-71.0814043774777,
-55.3473655916165));
#131796=CARTESIAN_POINT('Ctrl Pts',(-8.19486187074245,-70.7772925435282,
-54.8793138184774));
#131797=CARTESIAN_POINT('Ctrl Pts',(-8.2013544983267,-70.7763714724242,
-55.2294679275358));
#131798=CARTESIAN_POINT('Ctrl Pts',(-8.24918690883785,-71.102010310254,
-55.3491521481271));
#131799=CARTESIAN_POINT('Ctrl Pts',(-8.02999374674379,-70.8004238120746,
-54.8822160506073));
#131800=CARTESIAN_POINT('Ctrl Pts',(-8.03626733023182,-70.7995543826982,
-55.2297202388378));
#131801=CARTESIAN_POINT('Ctrl Pts',(-8.08271475024063,-71.1220068981801,
-55.3508246944299));
#131802=CARTESIAN_POINT('Ctrl Pts',(-7.86502491569137,-70.8228501557662,
-54.8850140141151));
#131803=CARTESIAN_POINT('Ctrl Pts',(-7.87072047725699,-70.8220758845274,
-55.2299609924931));
#131804=CARTESIAN_POINT('Ctrl Pts',(-7.91618843693366,-71.141394090941,
-55.3523946663951));
#131805=CARTESIAN_POINT('',(-8.35962920986979,-70.7534564084689,-54.8763024037297));
#131806=CARTESIAN_POINT('Origin',(-0.0280298706588222,-14.2420762575821,
-46.319218516546));
#131807=CARTESIAN_POINT('',(-8.41560835064733,-71.0814043774055,-55.3473655916053));
#131808=CARTESIAN_POINT('Origin',(-8.4312167004274,-71.248305103724,-54.8763024037297));
#131809=CARTESIAN_POINT('Origin',(-0.0696643368815508,-4.70111132130388,
-43.5213887605807));
#131810=CARTESIAN_POINT('Ctrl Pts',(-9.32018679685842,-70.6063261212332,
-55.8925850873));
#131811=CARTESIAN_POINT('Ctrl Pts',(-8.89999999999995,-70.674270243298,
-55.8925850872999));
#131812=CARTESIAN_POINT('Ctrl Pts',(-8.9,-71.0999148696911,-55.8925850873));
#131813=CARTESIAN_POINT('Ctrl Pts',(-9.32018679646957,-70.606326121296,
-55.7609765242912));
#131814=CARTESIAN_POINT('Ctrl Pts',(-8.92045674363165,-70.670962391591,
-55.8099505084873));
#131815=CARTESIAN_POINT('Ctrl Pts',(-8.9,-71.0753963340341,-55.8158206410579));
#131816=CARTESIAN_POINT('Ctrl Pts',(-9.29866745626329,-70.6098198655576,
-55.6301334688925));
#131817=CARTESIAN_POINT('Ctrl Pts',(-8.92288173642606,-70.6704214883702,
-55.7222104842267));
#131818=CARTESIAN_POINT('Ctrl Pts',(-8.88914819160783,-71.0574685211989,
-55.7424878932553));
#131819=CARTESIAN_POINT('Ctrl Pts',(-9.20823066610786,-70.6243360556297,
-55.3829240249879));
#131820=CARTESIAN_POINT('Ctrl Pts',(-8.88787909971282,-70.6754793338957,
-55.5563944136962));
#131821=CARTESIAN_POINT('Ctrl Pts',(-8.84354256567003,-71.0340357122248,
-55.606998619986));
#131822=CARTESIAN_POINT('Ctrl Pts',(-9.14039822217997,-70.6351795268323,
-55.2697323706429));
#131823=CARTESIAN_POINT('Ctrl Pts',(-8.8515542998134,-70.6809070626089,
-55.4791108159719));
#131824=CARTESIAN_POINT('Ctrl Pts',(-8.80933590722104,-71.0287732217429,
-55.5465658668829));
#131825=CARTESIAN_POINT('Ctrl Pts',(-8.96386239650929,-70.6628838067398,
-55.0780797399289));
#131826=CARTESIAN_POINT('Ctrl Pts',(-8.74741150404566,-70.6964574226719,
-55.3507681953891));
#131827=CARTESIAN_POINT('Ctrl Pts',(-8.72031210976081,-71.028802992332,
-55.4457995958176));
#131828=CARTESIAN_POINT('Ctrl Pts',(-8.85596081453515,-70.679599541712,
-55.0012953993776));
#131829=CARTESIAN_POINT('Ctrl Pts',(-8.67980906181977,-70.7065384951403,
-55.2998814604833));
#131830=CARTESIAN_POINT('Ctrl Pts',(-8.66589931539785,-71.0341559413021,
-55.4063653507056));
#131831=CARTESIAN_POINT('Ctrl Pts',(-8.61934915026951,-70.7154116132197,
-54.8994528680703));
#131832=CARTESIAN_POINT('Ctrl Pts',(-8.53037007175256,-70.7286009969627,
-55.2361886195963));
#131833=CARTESIAN_POINT('Ctrl Pts',(-8.5465803724842,-71.0525391488732,
-55.3555557927532));
#131834=CARTESIAN_POINT('Ctrl Pts',(-8.48994814797731,-70.7346037655486,
-54.8739206038906));
#131835=CARTESIAN_POINT('Ctrl Pts',(-8.44749087161521,-70.7407315090392,
-55.2227831389152));
#131836=CARTESIAN_POINT('Ctrl Pts',(-8.48132333269968,-71.0655965765406,
-55.3439422058852));
#131837=CARTESIAN_POINT('Ctrl Pts',(-8.35962920986983,-70.7534564084689,
-54.8763024037294));
#131838=CARTESIAN_POINT('Ctrl Pts',(-8.36589323739407,-70.7525502203441,
-55.2292031667485));
#131839=CARTESIAN_POINT('Ctrl Pts',(-8.41560835021371,-71.0814043774774,
-55.3473655916161));
#131840=CARTESIAN_POINT('',(-9.32018679685842,-70.6063261212332,-55.8925850873));
#131841=CARTESIAN_POINT('Ctrl Pts',(-8.35962920986984,-70.7534564084689,
-54.8763024037297));
#131842=CARTESIAN_POINT('Ctrl Pts',(-8.42669320976301,-70.7437545672695,
-54.8750766952757));
#131843=CARTESIAN_POINT('Ctrl Pts',(-8.49356141096547,-70.7339558949385,
-54.8812481493055));
#131844=CARTESIAN_POINT('Ctrl Pts',(-8.5587840601874,-70.7242909712569,
-54.894476436547));
#131845=CARTESIAN_POINT('Ctrl Pts',(-8.62027176255611,-70.715179505258,
-54.9069472116299));
#131846=CARTESIAN_POINT('Ctrl Pts',(-8.68029576330479,-70.7061871116828,
-54.9256889700024));
#131847=CARTESIAN_POINT('Ctrl Pts',(-8.73765415640112,-70.6975057024889,
-54.9503761135537));
#131848=CARTESIAN_POINT('Ctrl Pts',(-8.73812533670876,-70.6974343875717,
-54.950578910307));
#131849=CARTESIAN_POINT('Ctrl Pts',(-8.7385963482321,-70.6973630921029,
-54.9507821155763));
#131850=CARTESIAN_POINT('Ctrl Pts',(-8.73906719037139,-70.697291816191,
-54.9509857288994));
#131851=CARTESIAN_POINT('Ctrl Pts',(-8.81806341257093,-70.6853333967876,
-54.9851472492404));
#131852=CARTESIAN_POINT('Ctrl Pts',(-8.89230144999735,-70.6739241189874,
-55.0307996075112));
#131853=CARTESIAN_POINT('Ctrl Pts',(-8.95909820839892,-70.6635530304614,
-55.0858633072379));
#131854=CARTESIAN_POINT('Ctrl Pts',(-8.99202329692719,-70.658440970894,
-55.1130050014095));
#131855=CARTESIAN_POINT('Ctrl Pts',(-9.02314073107063,-70.6535810854988,
-55.1424341547024));
#131856=CARTESIAN_POINT('Ctrl Pts',(-9.05213028602995,-70.6490316704449,
-55.1739060774789));
#131857=CARTESIAN_POINT('Ctrl Pts',(-9.05261593139238,-70.6489554567077,
-55.1744333085235));
#131858=CARTESIAN_POINT('Ctrl Pts',(-9.05310095531286,-70.6488793344915,
-55.1749610621635));
#131859=CARTESIAN_POINT('Ctrl Pts',(-9.05358535746144,-70.6488033038874,
-55.1754893372344));
#131860=CARTESIAN_POINT('Ctrl Pts',(-9.1020755169914,-70.641192404282,-55.2283713125433));
#131861=CARTESIAN_POINT('Ctrl Pts',(-9.14429186553979,-70.6345063768039,
-55.2864243412901));
#131862=CARTESIAN_POINT('Ctrl Pts',(-9.17994788064335,-70.6288295105426,
-55.348502954041));
#131863=CARTESIAN_POINT('Ctrl Pts',(-9.20880098471981,-70.6242357495014,
-55.3987374143254));
#131864=CARTESIAN_POINT('Ctrl Pts',(-9.23335776597293,-70.6203028545583,
-55.4516091557798));
#131865=CARTESIAN_POINT('Ctrl Pts',(-9.25344901950571,-70.6170779672838,
-55.5065287627148));
#131866=CARTESIAN_POINT('Ctrl Pts',(-9.25361952044245,-70.6170505998375,
-55.506994828429));
#131867=CARTESIAN_POINT('Ctrl Pts',(-9.25378968425506,-70.6170232859403,
-55.5074609965585));
#131868=CARTESIAN_POINT('Ctrl Pts',(-9.25395951106862,-70.6169960255762,
-55.5079272667724));
#131869=CARTESIAN_POINT('Ctrl Pts',(-9.26917261736368,-70.6145540388982,
-55.5496958083666));
#131870=CARTESIAN_POINT('Ctrl Pts',(-9.28164780823391,-70.6125470433612,
-55.5921779695173));
#131871=CARTESIAN_POINT('Ctrl Pts',(-9.2915203488035,-70.6109563835461,
-55.6352174890368));
#131872=CARTESIAN_POINT('Ctrl Pts',(-9.30173630321666,-70.609310393029,
-55.6797541274306));
#131873=CARTESIAN_POINT('Ctrl Pts',(-9.30916540444186,-70.6081101941254,
-55.7248883638109));
#131874=CARTESIAN_POINT('Ctrl Pts',(-9.31390296845358,-70.6073438342246,
-55.7704597578367));
#131875=CARTESIAN_POINT('Ctrl Pts',(-9.31810307746837,-70.606664414354,
-55.8108612853708));
#131876=CARTESIAN_POINT('Ctrl Pts',(-9.32018679673735,-70.6063261212527,
-55.8516070077996));
#131877=CARTESIAN_POINT('Ctrl Pts',(-9.32018679685842,-70.6063261212332,
-55.8925850873));
#131878=CARTESIAN_POINT('',(-8.89999999157093,-71.0999148696892,-55.8925850873042));
#131879=CARTESIAN_POINT('Origin',(-9.4,-71.0999148696911,-55.8925850873));
#131880=CARTESIAN_POINT('Ctrl Pts',(-8.9,-71.0999148696911,-55.8925850873));
#131881=CARTESIAN_POINT('Ctrl Pts',(-8.9,-71.0753963340341,-55.8158206410579));
#131882=CARTESIAN_POINT('Ctrl Pts',(-8.88914819160783,-71.0574685211989,
-55.7424878932553));
#131883=CARTESIAN_POINT('Ctrl Pts',(-8.84354256567003,-71.0340357122248,
-55.606998619986));
#131884=CARTESIAN_POINT('Ctrl Pts',(-8.80933590722104,-71.0287732217429,
-55.5465658668829));
#131885=CARTESIAN_POINT('Ctrl Pts',(-8.72031210976081,-71.028802992332,
-55.4457995958176));
#131886=CARTESIAN_POINT('Ctrl Pts',(-8.66589931539785,-71.0341559413021,
-55.4063653507056));
#131887=CARTESIAN_POINT('Ctrl Pts',(-8.5465803724842,-71.0525391488732,
-55.3555557927532));
#131888=CARTESIAN_POINT('Ctrl Pts',(-8.48132333269968,-71.0655965765406,
-55.3439422058852));
#131889=CARTESIAN_POINT('Ctrl Pts',(-8.41560835021378,-71.0814043774777,
-55.3473655916165));
#131890=CARTESIAN_POINT('Origin',(-9.4,-71.0999148696911,-55.24995));
#131891=CARTESIAN_POINT('',(-8.9,-71.0999148696911,-60.4282553373601));
#131892=CARTESIAN_POINT('',(-9.32018679685842,-70.6063261212332,-60.4282553373601));
#131893=CARTESIAN_POINT('Origin',(-9.4,-71.0999148696911,-60.4282553373601));
#131894=CARTESIAN_POINT('',(-8.9,-71.0999148696911,-55.24995));
#131895=CARTESIAN_POINT('',(-9.32018679685842,-70.6063261212332,-55.24995));
#131896=CARTESIAN_POINT('Origin',(0.,-12.9675000200281,-60.42825533736));
#131897=CARTESIAN_POINT('',(-14.9339094669349,-69.3159372152925,-60.8508735991008));
#131898=CARTESIAN_POINT('',(-9.32749162718857,-70.5102313269446,-60.8508735991008));
#131899=CARTESIAN_POINT('Origin',(0.,-12.9675000200281,-60.8508735991007));
#131900=CARTESIAN_POINT('Origin',(-9.4006078237226,-69.5628833426966,-60.4240593941771));
#131901=CARTESIAN_POINT('',(-14.9222139673106,-69.4159516070034,-60.4282553373601));
#131902=CARTESIAN_POINT('Origin',(0.,-12.9675000200281,-60.42825533736));
#131903=CARTESIAN_POINT('Origin',(-15.0817374974215,-68.0546682136643,-60.3659067766217));
#131904=CARTESIAN_POINT('Origin',(-15.05,-69.8993466109593,-55.24995));
#131905=CARTESIAN_POINT('',(-14.9222139673106,-69.4159516070034,-55.74995));
#131906=CARTESIAN_POINT('',(-15.55,-69.8993466109593,-55.74995));
#131907=CARTESIAN_POINT('Origin',(-15.05,-69.8993466109593,-55.74995));
#131908=CARTESIAN_POINT('',(-15.55,-69.8993466109592,-60.4282553373601));
#131909=CARTESIAN_POINT('',(-15.55,-69.8993466109593,-55.24995));
#131910=CARTESIAN_POINT('',(-15.05,-69.3993466109593,-60.4282553373601));
#131911=CARTESIAN_POINT('Origin',(-15.05,-69.8993466109592,-60.4282553373601));
#131912=CARTESIAN_POINT('Origin',(-15.05,-69.8993466109592,-60.4282553373601));
#131913=CARTESIAN_POINT('',(-14.9222139673106,-69.4159516070034,-55.24995));
#131914=CARTESIAN_POINT('Ctrl Pts',(-15.9137232010189,-69.1444843653509,
-54.74995));
#131915=CARTESIAN_POINT('Ctrl Pts',(-15.9137232010189,-69.1444843653508,
-55.24995));
#131916=CARTESIAN_POINT('Ctrl Pts',(-16.05,-69.6255546658887,-55.24995));
#131917=CARTESIAN_POINT('Ctrl Pts',(-15.6596579837658,-69.2164555398362,
-54.7499500371751));
#131918=CARTESIAN_POINT('Ctrl Pts',(-15.771227820187,-69.1848502198413,
-55.2866827527478));
#131919=CARTESIAN_POINT('Ctrl Pts',(-15.9218478003938,-69.698160151404,
-55.24995));
#131920=CARTESIAN_POINT('Ctrl Pts',(-15.40465081614,-69.286534600552,-54.8528648356211));
#131921=CARTESIAN_POINT('Ctrl Pts',(-15.6724279126842,-69.212867833855,
-55.3793785506899));
#131922=CARTESIAN_POINT('Ctrl Pts',(-15.7932840899848,-69.7688213437999,
-55.3014074151129));
#131923=CARTESIAN_POINT('Ctrl Pts',(-15.0344159790517,-69.3864973437867,
-55.2190131651604));
#131924=CARTESIAN_POINT('Ctrl Pts',(-15.5617369148846,-69.2455690283436,
-55.5713612535417));
#131925=CARTESIAN_POINT('Ctrl Pts',(-15.6065814283354,-69.8696401180232,
-55.4844815852779));
#131926=CARTESIAN_POINT('Ctrl Pts',(-14.9222139938746,-69.4159515999812,
-55.4795342126294));
#131927=CARTESIAN_POINT('Ctrl Pts',(-15.5500000039585,-69.2499956362206,
-55.6640902421462));
#131928=CARTESIAN_POINT('Ctrl Pts',(-15.55,-69.8993466038797,-55.6147421042263));
#131929=CARTESIAN_POINT('Ctrl Pts',(-14.9222139673106,-69.4159516070034,
-55.74995));
#131930=CARTESIAN_POINT('Ctrl Pts',(-15.55,-69.2499956375816,-55.74995));
#131931=CARTESIAN_POINT('Ctrl Pts',(-15.55,-69.8993466109593,-55.74995));
#131932=CARTESIAN_POINT('',(-15.913723201019,-69.1444843653509,-54.74995));
#131933=CARTESIAN_POINT('Ctrl Pts',(-14.9222139673106,-69.4159516070034,
-55.74995));
#131934=CARTESIAN_POINT('Ctrl Pts',(-14.9222139938746,-69.4159515999812,
-55.4795342126294));
#131935=CARTESIAN_POINT('Ctrl Pts',(-15.0344159790517,-69.3864973437867,
-55.2190131651604));
#131936=CARTESIAN_POINT('Ctrl Pts',(-15.40465081614,-69.286534600552,-54.8528648356211));
#131937=CARTESIAN_POINT('Ctrl Pts',(-15.6596579837658,-69.2164555398362,
-54.7499500371751));
#131938=CARTESIAN_POINT('Ctrl Pts',(-15.913723201019,-69.1444843653509,
-54.74995));
#131939=CARTESIAN_POINT('',(-16.05,-69.6255546658886,-55.24995));
#131940=CARTESIAN_POINT('Origin',(-16.05,-69.6255546658886,-54.74995));
#131941=CARTESIAN_POINT('Ctrl Pts',(-16.05,-69.6255546658886,-55.24995));
#131942=CARTESIAN_POINT('Ctrl Pts',(-15.9218478003938,-69.698160151404,
-55.24995));
#131943=CARTESIAN_POINT('Ctrl Pts',(-15.7932840899848,-69.7688213437999,
-55.3014074151129));
#131944=CARTESIAN_POINT('Ctrl Pts',(-15.6065814283354,-69.8696401180232,
-55.4844815852779));
#131945=CARTESIAN_POINT('Ctrl Pts',(-15.55,-69.8993466038797,-55.6147421042263));
#131946=CARTESIAN_POINT('Ctrl Pts',(-15.55,-69.8993466109593,-55.74995));
#131947=CARTESIAN_POINT('Origin',(0.,-12.9675000200281,-54.74995));
#131948=CARTESIAN_POINT('',(-16.4094778178732,-69.001678821881,-54.74995));
#131949=CARTESIAN_POINT('Origin',(0.,-12.9675000200281,-54.74995));
#131950=CARTESIAN_POINT('',(-16.55,-69.4815262104643,-55.24995));
#131951=CARTESIAN_POINT('Origin',(-16.55,-69.4815262104644,-54.74995));
#131952=CARTESIAN_POINT('Origin',(0.,-12.9675000200281,-55.24995));
#131953=CARTESIAN_POINT('Ctrl Pts',(-17.4009870515814,-68.7017426890013,
-55.74995));
#131954=CARTESIAN_POINT('Ctrl Pts',(-17.05,-68.8113256105117,-55.74995));
#131955=CARTESIAN_POINT('Ctrl Pts',(-17.05,-69.1790215814778,-55.74995));
#131956=CARTESIAN_POINT('Ctrl Pts',(-17.4009870278268,-68.7017426964178,
-55.6164169522954));
#131957=CARTESIAN_POINT('Ctrl Pts',(-17.0499999824983,-68.8113256158083,
-55.6678220871153));
#131958=CARTESIAN_POINT('Ctrl Pts',(-17.05,-69.179021588958,-55.683183477332));
#131959=CARTESIAN_POINT('Ctrl Pts',(-17.3738309471109,-68.7102398223756,
-55.4822907797671));
#131960=CARTESIAN_POINT('Ctrl Pts',(-17.0296370884236,-68.8175010382642,
-55.5850039716587));
#131961=CARTESIAN_POINT('Ctrl Pts',(-17.0363056762739,-69.1875914802515,
-55.6161203882819));
#131962=CARTESIAN_POINT('Ctrl Pts',(-17.2712219065013,-68.7421173320939,
-55.237857759257));
#131963=CARTESIAN_POINT('Ctrl Pts',(-16.9553391166104,-68.8399176416641,
-55.4404431349053));
#131964=CARTESIAN_POINT('Ctrl Pts',(-16.9845618032129,-69.2197419714937,
-55.4939038812302));
#131965=CARTESIAN_POINT('Ctrl Pts',(-17.1955506950046,-68.7655509085055,
-55.1267370897427));
#131966=CARTESIAN_POINT('Ctrl Pts',(-16.9005894152091,-68.8563914475931,
-55.377823329943));
#131967=CARTESIAN_POINT('Ctrl Pts',(-16.9464021983051,-69.2433762217045,
-55.4383435435979));
#131968=CARTESIAN_POINT('Ctrl Pts',(-17.0112333722604,-68.8220198533602,
-54.9445960314883));
#131969=CARTESIAN_POINT('Ctrl Pts',(-16.7737497934953,-68.8942921521941,
-55.2851829950906));
#131970=CARTESIAN_POINT('Ctrl Pts',(-16.8534543357224,-69.300328736023,
-55.3472730170175));
#131971=CARTESIAN_POINT('Ctrl Pts',(-16.9010650546211,-68.8555068833233,
-54.8720727600904));
#131972=CARTESIAN_POINT('Ctrl Pts',(-16.6998467063121,-68.9162473809411,
-55.2547261014823));
#131973=CARTESIAN_POINT('Ctrl Pts',(-16.7978984661854,-69.3341025322853,
-55.3110113805052));
#131974=CARTESIAN_POINT('Ctrl Pts',(-16.6652454739222,-68.9262786380983,
-54.7753009573657));
#131975=CARTESIAN_POINT('Ctrl Pts',(-16.5521913264397,-68.9598430749121,
-55.2279532590823));
#131976=CARTESIAN_POINT('Ctrl Pts',(-16.6789789583454,-69.4054803385803,
-55.2626254782229));
#131977=CARTESIAN_POINT('Ctrl Pts',(-16.5367871504596,-68.9643965824736,
-54.7499500149468));
#131978=CARTESIAN_POINT('Ctrl Pts',(-16.4764075692004,-68.9820786017848,
-55.2322379892913));
#131979=CARTESIAN_POINT('Ctrl Pts',(-16.6141964540128,-69.4439266482582,
-55.24995));
#131980=CARTESIAN_POINT('Ctrl Pts',(-16.4094778178732,-69.001678821881,
-54.74995));
#131981=CARTESIAN_POINT('Ctrl Pts',(-16.4094778178731,-69.001678821881,
-55.24995));
#131982=CARTESIAN_POINT('Ctrl Pts',(-16.55,-69.4815262104644,-55.24995));
#131983=CARTESIAN_POINT('',(-17.4009870515814,-68.7017426890012,-55.74995));
#131984=CARTESIAN_POINT('Ctrl Pts',(-16.4094778178732,-69.001678821881,
-54.74995));
#131985=CARTESIAN_POINT('Ctrl Pts',(-16.4504095598616,-68.9896920572568,
-54.7499500048056));
#131986=CARTESIAN_POINT('Ctrl Pts',(-16.4912475287742,-68.9776812452657,
-54.7525666780149));
#131987=CARTESIAN_POINT('Ctrl Pts',(-16.5317041745654,-68.965736321318,
-54.757667934043));
#131988=CARTESIAN_POINT('Ctrl Pts',(-16.5749366447117,-68.9529718284177,
-54.7631191990857));
#131989=CARTESIAN_POINT('Ctrl Pts',(-16.6177350648204,-68.9402821612408,
-54.771407370512));
#131990=CARTESIAN_POINT('Ctrl Pts',(-16.659758562013,-68.9277728443736,
-54.7824337221976));
#131991=CARTESIAN_POINT('Ctrl Pts',(-16.7017820592057,-68.9152635275064,
-54.7934600738833));
#131992=CARTESIAN_POINT('Ctrl Pts',(-16.7430322683556,-68.9029340622973,
-54.8072249335998));
#131993=CARTESIAN_POINT('Ctrl Pts',(-16.7831545131606,-68.8908929861314,
-54.8236888710244));
#131994=CARTESIAN_POINT('Ctrl Pts',(-16.7835975596796,-68.890760023559,
-54.8238706726708));
#131995=CARTESIAN_POINT('Ctrl Pts',(-16.7840405080022,-68.8906270844636,
-54.8240528195673));
#131996=CARTESIAN_POINT('Ctrl Pts',(-16.7844833577117,-68.8904941689839,
-54.8242353115275));
#131997=CARTESIAN_POINT('Ctrl Pts',(-16.8581304439988,-68.8683899706622,
-54.8545842106015));
#131998=CARTESIAN_POINT('Ctrl Pts',(-16.9287006566096,-68.8470438209494,
-54.8943416412349));
#131999=CARTESIAN_POINT('Ctrl Pts',(-16.9936792242025,-68.8272773402426,
-54.9420858838156));
#132000=CARTESIAN_POINT('Ctrl Pts',(-17.0324101749564,-68.815495384758,
-54.970544189018));
#132001=CARTESIAN_POINT('Ctrl Pts',(-17.0691551792516,-68.8042744590646,
-55.0018396382534));
#132002=CARTESIAN_POINT('Ctrl Pts',(-17.1033900455892,-68.7937859900155,
-55.0356687800906));
#132003=CARTESIAN_POINT('Ctrl Pts',(-17.103886172442,-68.7936339926019,
-55.0361590272412));
#132004=CARTESIAN_POINT('Ctrl Pts',(-17.1043818163765,-68.7934821358841,
-55.0366498500402));
#132005=CARTESIAN_POINT('Ctrl Pts',(-17.1048769761793,-68.7933304202781,
-55.0371412470353));
#132006=CARTESIAN_POINT('Ctrl Pts',(-17.1669690008271,-68.7743055941548,
-55.0987614233146));
#132007=CARTESIAN_POINT('Ctrl Pts',(-17.2214535479523,-68.7574981762719,
-55.1694239623158));
#132008=CARTESIAN_POINT('Ctrl Pts',(-17.2659841189476,-68.7437133283472,
-55.2463463516028));
#132009=CARTESIAN_POINT('Ctrl Pts',(-17.2871667241188,-68.7371560580403,
-55.2829373174196));
#132010=CARTESIAN_POINT('Ctrl Pts',(-17.3060972390716,-68.7312826257117,
-55.3209455236331));
#132011=CARTESIAN_POINT('Ctrl Pts',(-17.322524151481,-68.7261792841162,
-55.3600753258131));
#132012=CARTESIAN_POINT('Ctrl Pts',(-17.3227235277485,-68.7261173439796,
-55.3605502509672));
#132013=CARTESIAN_POINT('Ctrl Pts',(-17.3229225385083,-68.7260555164805,
-55.3610253536613));
#132014=CARTESIAN_POINT('Ctrl Pts',(-17.3231211835968,-68.7259938016769,
-55.3615006331605));
#132015=CARTESIAN_POINT('Ctrl Pts',(-17.3377397858477,-68.7214521129136,
-55.3964771936486));
#132016=CARTESIAN_POINT('Ctrl Pts',(-17.3503329508714,-68.717534766207,
-55.4322944098896));
#132017=CARTESIAN_POINT('Ctrl Pts',(-17.3608936617493,-68.7142467873541,
-55.4687543689715));
#132018=CARTESIAN_POINT('Ctrl Pts',(-17.3714744037536,-68.7109525719968,
-55.5052834838195));
#132019=CARTESIAN_POINT('Ctrl Pts',(-17.3800152474177,-68.70829001851,-55.5424589028238));
#132020=CARTESIAN_POINT('Ctrl Pts',(-17.3864625050711,-68.7062785938727,
-55.5800999366541));
#132021=CARTESIAN_POINT('Ctrl Pts',(-17.3927323721603,-68.7043225117965,
-55.6167053108928));
#132022=CARTESIAN_POINT('Ctrl Pts',(-17.3970223360455,-68.7029821923561,
-55.6537520599017));
#132023=CARTESIAN_POINT('Ctrl Pts',(-17.399236871165,-68.7022899564979,
-55.6910754862815));
#132024=CARTESIAN_POINT('Ctrl Pts',(-17.4003972743764,-68.7019272290316,
-55.7106327393814));
#132025=CARTESIAN_POINT('Ctrl Pts',(-17.4009870480798,-68.7017426900946,
-55.7302658927369));
#132026=CARTESIAN_POINT('Ctrl Pts',(-17.4009870515814,-68.7017426890013,
-55.74995));
#132027=CARTESIAN_POINT('',(-17.05,-69.1790215814778,-55.74995));
#132028=CARTESIAN_POINT('Origin',(-17.55,-69.1790215814778,-55.74995));
#132029=CARTESIAN_POINT('Ctrl Pts',(-17.05,-69.1790215814778,-55.74995));
#132030=CARTESIAN_POINT('Ctrl Pts',(-17.05,-69.1790215840141,-55.7273117036717));
#132031=CARTESIAN_POINT('Ctrl Pts',(-17.0484581724605,-69.1800068330463,
-55.704632518585));
#132032=CARTESIAN_POINT('Ctrl Pts',(-17.045383935534,-69.1819358319623,
-55.6821653674136));
#132033=CARTESIAN_POINT('Ctrl Pts',(-17.0423062744033,-69.183866979472,
-55.6596731914591));
#132034=CARTESIAN_POINT('Ctrl Pts',(-17.0376928923171,-69.1867439804066,
-55.6373943130373));
#132035=CARTESIAN_POINT('Ctrl Pts',(-17.0316050134448,-69.1905251993378,
-55.6155751101402));
#132036=CARTESIAN_POINT('Ctrl Pts',(-17.0258391557959,-69.1941064089108,
-55.5949100442681));
#132037=CARTESIAN_POINT('Ctrl Pts',(-17.0187512873944,-69.1984987083453,
-55.5746577770516));
#132038=CARTESIAN_POINT('Ctrl Pts',(-17.0104337397434,-69.2036667258726,
-55.555012134756));
#132039=CARTESIAN_POINT('Ctrl Pts',(-17.0013343801787,-69.2093205137066,
-55.5335198908125));
#132040=CARTESIAN_POINT('Ctrl Pts',(-16.9907376252434,-69.2159093376612,
-55.512693370794));
#132041=CARTESIAN_POINT('Ctrl Pts',(-16.9787804466987,-69.2233149929863,
-55.4927587705056));
#132042=CARTESIAN_POINT('Ctrl Pts',(-16.9667872973728,-69.2307429267449,
-55.4727642009576));
#132043=CARTESIAN_POINT('Ctrl Pts',(-16.9534260163454,-69.2389926138138,
-55.4536675252671));
#132044=CARTESIAN_POINT('Ctrl Pts',(-16.9388754710694,-69.2479447794443,
-55.4356637164931));
#132045=CARTESIAN_POINT('Ctrl Pts',(-16.9266858743886,-69.2554443807571,
-55.4205811774192));
#132046=CARTESIAN_POINT('Ctrl Pts',(-16.9136625469686,-69.2634369892112,
-55.4062651589592));
#132047=CARTESIAN_POINT('Ctrl Pts',(-16.8999282670137,-69.2718524788637,
-55.3928082803077));
#132048=CARTESIAN_POINT('Ctrl Pts',(-16.8836819568998,-69.2818071801734,
-55.3768901088086));
#132049=CARTESIAN_POINT('Ctrl Pts',(-16.8663408763305,-69.2924092697525,
-55.3620781535359));
#132050=CARTESIAN_POINT('Ctrl Pts',(-16.8481019051626,-69.3035142485201,
-55.3485334406276));
#132051=CARTESIAN_POINT('Ctrl Pts',(-16.8298276464078,-69.3146407124856,
-55.3349625222809));
#132052=CARTESIAN_POINT('Ctrl Pts',(-16.8106526893114,-69.3262720134373,
-55.3226641848208));
#132053=CARTESIAN_POINT('Ctrl Pts',(-16.7908030911076,-69.3382628119682,
-55.3117561258837));
#132054=CARTESIAN_POINT('Ctrl Pts',(-16.7737921641089,-69.3485388183827,
-55.3024080175557));
#132055=CARTESIAN_POINT('Ctrl Pts',(-16.7562864891711,-69.3590788518886,
-55.2940803227657));
#132056=CARTESIAN_POINT('Ctrl Pts',(-16.7384387122654,-69.3697914354328,
-55.286818429364));
#132057=CARTESIAN_POINT('Ctrl Pts',(-16.7180829214159,-69.3820093778262,
-55.2785360766634));
#132058=CARTESIAN_POINT('Ctrl Pts',(-16.6971109842387,-69.3945504898523,
-55.2715719188538));
#132059=CARTESIAN_POINT('Ctrl Pts',(-16.6757471551705,-69.407270161634,
-55.2660206115904));
#132060=CARTESIAN_POINT('Ctrl Pts',(-16.6543745545499,-69.4199950558536,
-55.2604670250734));
#132061=CARTESIAN_POINT('Ctrl Pts',(-16.6326105138126,-69.4328986564849,
-55.2563277011337));
#132062=CARTESIAN_POINT('Ctrl Pts',(-16.6106950449315,-69.4458361754561,
-55.2536475604324));
#132063=CARTESIAN_POINT('Ctrl Pts',(-16.590527650153,-69.4577417410619,
-55.251181199531));
#132064=CARTESIAN_POINT('Ctrl Pts',(-16.5702326710683,-69.4696760298565,
-55.24995));
#132065=CARTESIAN_POINT('Ctrl Pts',(-16.55,-69.4815262104643,-55.24995));
#132066=CARTESIAN_POINT('Origin',(-17.55,-69.1790215814778,-55.24995));
#132067=CARTESIAN_POINT('',(-17.05,-69.1790215814778,-60.42825533736));
#132068=CARTESIAN_POINT('',(-17.4009870515814,-68.7017426890012,-60.42825533736));
#132069=CARTESIAN_POINT('Origin',(-17.55,-69.1790215814778,-60.42825533736));
#132070=CARTESIAN_POINT('',(-17.05,-69.1790215814778,-55.24995));
#132071=CARTESIAN_POINT('',(-17.4009870515814,-68.7017426890012,-55.24995));
#132072=CARTESIAN_POINT('Origin',(0.,-12.9675000200281,-60.42825533736));
#132073=CARTESIAN_POINT('',(-23.0210431649761,-66.5230748737403,-60.8508735991007));
#132074=CARTESIAN_POINT('',(-17.4146253252297,-68.5993151180197,-60.8508735991007));
#132075=CARTESIAN_POINT('Origin',(0.,-12.9675000200281,-60.8508735991007));
#132076=CARTESIAN_POINT('Origin',(-17.5536315931459,-67.566484588888,-60.418466472047));
#132077=CARTESIAN_POINT('',(-23.0030142220336,-66.6327727106072,-60.42825533736));
#132078=CARTESIAN_POINT('Origin',(0.,-12.9675000200281,-60.42825533736));
#132079=CARTESIAN_POINT('Origin',(-23.206372880927,-65.3976857628708,-60.4139613002479));
#132080=CARTESIAN_POINT('Origin',(-23.2,-67.0923340267327,-55.24995));
#132081=CARTESIAN_POINT('',(-23.0030142220336,-66.6327727106072,-55.74995));
#132082=CARTESIAN_POINT('',(-23.7,-67.0923340267327,-55.74995));
#132083=CARTESIAN_POINT('Origin',(-23.2,-67.0923340267327,-55.74995));
#132084=CARTESIAN_POINT('',(-23.7,-67.0923340267327,-60.42825533736));
#132085=CARTESIAN_POINT('',(-23.7,-67.0923340267327,-55.24995));
#132086=CARTESIAN_POINT('Origin',(-23.2,-67.0923340267327,-60.42825533736));
#132087=CARTESIAN_POINT('',(-23.0030142220336,-66.6327727106072,-55.24995));
#132088=CARTESIAN_POINT('Ctrl Pts',(-23.9945234557419,-66.1968434349636,
-54.74995));
#132089=CARTESIAN_POINT('Ctrl Pts',(-23.9945234557419,-66.1968434349636,
-55.24995));
#132090=CARTESIAN_POINT('Ctrl Pts',(-24.2,-66.6526716808631,-55.24995));
#132091=CARTESIAN_POINT('Ctrl Pts',(-23.8699830688991,-66.2529832826787,
-54.7499500150097));
#132092=CARTESIAN_POINT('Ctrl Pts',(-23.9202432240961,-66.2303271978257,
-55.2764502978682));
#132093=CARTESIAN_POINT('Ctrl Pts',(-24.1371955572435,-66.7092931820382,
-55.24995));
#132094=CARTESIAN_POINT('Ctrl Pts',(-23.7474276190468,-66.3076948875735,
-54.7731313367517));
#132095=CARTESIAN_POINT('Ctrl Pts',(-23.8581370153758,-66.2582349963978,
-55.3179716549212));
#132096=CARTESIAN_POINT('Ctrl Pts',(-24.0753940809144,-66.764472406879,
-55.2615406660682));
#132097=CARTESIAN_POINT('Ctrl Pts',(-23.5121407959317,-66.4118256516783,
-54.867008414748));
#132098=CARTESIAN_POINT('Ctrl Pts',(-23.7601274312421,-66.3025641007665,
-55.4174636561498));
#132099=CARTESIAN_POINT('Ctrl Pts',(-23.9567432347527,-66.8694948932304,
-55.3084792096817));
#132100=CARTESIAN_POINT('Ctrl Pts',(-23.4042122584794,-66.4591215590598,
-54.9358182281615));
#132101=CARTESIAN_POINT('Ctrl Pts',(-23.7282344734586,-66.3172128520127,
-55.4737170925055));
#132102=CARTESIAN_POINT('Ctrl Pts',(-23.902316841733,-66.9171958169871,
-55.3428841126209));
#132103=CARTESIAN_POINT('Ctrl Pts',(-23.2156877780054,-66.5412115519831,
-55.117294361456));
#132104=CARTESIAN_POINT('Ctrl Pts',(-23.6919934707232,-66.3346728811278,
-55.5807863787511));
#132105=CARTESIAN_POINT('Ctrl Pts',(-23.8072473920369,-66.9999887868491,
-55.4336221821879));
#132106=CARTESIAN_POINT('Ctrl Pts',(-23.138673673191,-66.5744522205999,
-55.227252767375));
#132107=CARTESIAN_POINT('Ctrl Pts',(-23.6899497583265,-66.3364476351196,
-55.6278104638636));
#132108=CARTESIAN_POINT('Ctrl Pts',(-23.7684105820677,-67.0335141101085,
-55.4886013829516));
#132109=CARTESIAN_POINT('Ctrl Pts',(-23.0317566828166,-66.6204750325317,
-55.4753103039836));
#132110=CARTESIAN_POINT('Ctrl Pts',(-23.6944387661923,-66.3359499016387,
-55.7013955638849));
#132111=CARTESIAN_POINT('Ctrl Pts',(-23.7144942998795,-67.079931038232,
-55.6126301527277));
#132112=CARTESIAN_POINT('Ctrl Pts',(-23.0030142327697,-66.6327727060053,
-55.6101370134438));
#132113=CARTESIAN_POINT('Ctrl Pts',(-23.6999999982635,-66.3340176139022,
-55.7259208430489));
#132114=CARTESIAN_POINT('Ctrl Pts',(-23.7,-67.0923340220896,-55.6800435061715));
#132115=CARTESIAN_POINT('Ctrl Pts',(-23.0030142220336,-66.6327727106072,
-55.74995));
#132116=CARTESIAN_POINT('Ctrl Pts',(-23.6999999999999,-66.3340176133293,
-55.74995));
#132117=CARTESIAN_POINT('Ctrl Pts',(-23.7,-67.0923340267327,-55.74995));
#132118=CARTESIAN_POINT('',(-23.9945234557419,-66.1968434349636,-54.74995));
#132119=CARTESIAN_POINT('Ctrl Pts',(-23.0030142220336,-66.6327727106072,
-55.74995));
#132120=CARTESIAN_POINT('Ctrl Pts',(-23.0030142252181,-66.6327727092422,
-55.7084794961837));
#132121=CARTESIAN_POINT('Ctrl Pts',(-23.0055473075491,-66.6316889244747,
-55.6672305708314));
#132122=CARTESIAN_POINT('Ctrl Pts',(-23.01056277729,-66.6295393332012,-55.6264611420266));
#132123=CARTESIAN_POINT('Ctrl Pts',(-23.0156442349954,-66.62736146,-55.585155314488));
#132124=CARTESIAN_POINT('Ctrl Pts',(-23.0232736525723,-66.6240896154023,
-55.5443421797599));
#132125=CARTESIAN_POINT('Ctrl Pts',(-23.0333489722998,-66.6197635354293,
-55.5042845968467));
#132126=CARTESIAN_POINT('Ctrl Pts',(-23.0435966387887,-66.6153634542441,
-55.4635417955117));
#132127=CARTESIAN_POINT('Ctrl Pts',(-23.0563743830217,-66.6098728426923,
-55.4235811788329));
#132128=CARTESIAN_POINT('Ctrl Pts',(-23.0715270926203,-66.6033540441774,
-55.3846656949086));
#132129=CARTESIAN_POINT('Ctrl Pts',(-23.075698862771,-66.6015593203436,
-55.3739516735531));
#132130=CARTESIAN_POINT('Ctrl Pts',(-23.08005038839,-66.5996867754406,-55.3633167653533));
#132131=CARTESIAN_POINT('Ctrl Pts',(-23.0845778500673,-66.5977379631867,
-55.3527661917799));
#132132=CARTESIAN_POINT('Ctrl Pts',(-23.084790216786,-66.5976465515099,
-55.3522713028445));
#132133=CARTESIAN_POINT('Ctrl Pts',(-23.0850029782865,-66.5975549687209,
-55.3517765816013));
#132134=CARTESIAN_POINT('Ctrl Pts',(-23.0852161343291,-66.5974632149135,
-55.3512820284305));
#132135=CARTESIAN_POINT('Ctrl Pts',(-23.1225303099355,-66.5814011899271,
-55.2647076876699));
#132136=CARTESIAN_POINT('Ctrl Pts',(-23.171373896406,-66.560332705268,-55.1848774594358));
#132137=CARTESIAN_POINT('Ctrl Pts',(-23.2296539151234,-66.5350590387648,
-55.1136222625269));
#132138=CARTESIAN_POINT('Ctrl Pts',(-23.254282078481,-66.5243788090568,
-55.0835110053899));
#132139=CARTESIAN_POINT('Ctrl Pts',(-23.2805947528025,-66.5129478823944,
-55.0549311560836));
#132140=CARTESIAN_POINT('Ctrl Pts',(-23.3084314920874,-66.5008277482104,
-55.0280211962633));
#132141=CARTESIAN_POINT('Ctrl Pts',(-23.3089371697075,-66.5006075758495,
-55.0275323543663));
#132142=CARTESIAN_POINT('Ctrl Pts',(-23.3094433520675,-66.5003871752661,
-55.0270440618914));
#132143=CARTESIAN_POINT('Ctrl Pts',(-23.3099500382032,-66.5001665468298,
-55.0265563196877));
#132144=CARTESIAN_POINT('Ctrl Pts',(-23.3737418241132,-66.4723894260756,
-54.9651495748562));
#132145=CARTESIAN_POINT('Ctrl Pts',(-23.4438814283319,-66.4417108192545,
-54.913708537172));
#132146=CARTESIAN_POINT('Ctrl Pts',(-23.5191429186309,-66.4085890914567,
-54.8723032868967));
#132147=CARTESIAN_POINT('Ctrl Pts',(-23.5545073851492,-66.3930255910651,
-54.8528474592054));
#132148=CARTESIAN_POINT('Ctrl Pts',(-23.5910022261981,-66.3769228800001,
-54.8356069181204));
#132149=CARTESIAN_POINT('Ctrl Pts',(-23.6284978920678,-66.3603295348338,
-54.8205860088576));
#132150=CARTESIAN_POINT('Ctrl Pts',(-23.6289267193329,-66.360139761465,
-54.8204142189909));
#132151=CARTESIAN_POINT('Ctrl Pts',(-23.6293556721512,-66.359949926291,
-54.8202427216662));
#132152=CARTESIAN_POINT('Ctrl Pts',(-23.629784750377,-66.3597600293637,
-54.8200715168436));
#132153=CARTESIAN_POINT('Ctrl Pts',(-23.6783390158401,-66.3382713933413,
-54.8006980695173));
#132154=CARTESIAN_POINT('Ctrl Pts',(-23.7276801213798,-66.316354158209,
-54.7853871133686));
#132155=CARTESIAN_POINT('Ctrl Pts',(-23.7776797138645,-66.29405966747,-54.7740684617323));
#132156=CARTESIAN_POINT('Ctrl Pts',(-23.8282083296012,-66.2715292887286,
-54.7626300525221));
#132157=CARTESIAN_POINT('Ctrl Pts',(-23.8794098794654,-66.2486134489514,
-54.75526886116));
#132158=CARTESIAN_POINT('Ctrl Pts',(-23.9311587890205,-66.2253609159866,
-54.7519649331453));
#132159=CARTESIAN_POINT('Ctrl Pts',(-23.9521926643966,-66.2159096853276,
-54.7506220176962));
#132160=CARTESIAN_POINT('Ctrl Pts',(-23.97331701039,-66.2064027967322,-54.7499500025558));
#132161=CARTESIAN_POINT('Ctrl Pts',(-23.9945234557419,-66.1968434349636,
-54.74995));
#132162=CARTESIAN_POINT('',(-24.2,-66.6526716808631,-55.24995));
#132163=CARTESIAN_POINT('Origin',(-24.2,-66.6526716808631,-54.74995));
#132164=CARTESIAN_POINT('Ctrl Pts',(-24.2,-66.6526716808631,-55.24995));
#132165=CARTESIAN_POINT('Ctrl Pts',(-24.1371955572435,-66.7092931820382,
-55.24995));
#132166=CARTESIAN_POINT('Ctrl Pts',(-24.0753940809144,-66.764472406879,
-55.2615406660682));
#132167=CARTESIAN_POINT('Ctrl Pts',(-23.9567432347527,-66.8694948932304,
-55.3084792096817));
#132168=CARTESIAN_POINT('Ctrl Pts',(-23.902316841733,-66.9171958169871,
-55.3428841126209));
#132169=CARTESIAN_POINT('Ctrl Pts',(-23.8072473920369,-66.9999887868491,
-55.4336221821879));
#132170=CARTESIAN_POINT('Ctrl Pts',(-23.7684105820677,-67.0335141101085,
-55.4886013829516));
#132171=CARTESIAN_POINT('Ctrl Pts',(-23.7144942998795,-67.079931038232,
-55.6126301527277));
#132172=CARTESIAN_POINT('Ctrl Pts',(-23.7,-67.0923340220896,-55.6800435061715));
#132173=CARTESIAN_POINT('Ctrl Pts',(-23.7,-67.0923340267327,-55.74995));
#132174=CARTESIAN_POINT('Origin',(0.,-12.9675000200281,-54.74995));
#132175=CARTESIAN_POINT('Origin',(0.,-12.9675000200281,-54.74995));
#132176=CARTESIAN_POINT('Origin',(0.,-12.9675000200281,-55.24995));
#132177=CARTESIAN_POINT('Origin',(-25.8159964412441,44.9247229809868,-55.24995));
#132178=CARTESIAN_POINT('',(-25.3802177275058,39.9437494905281,-60.1097730249189));
#132179=CARTESIAN_POINT('',(-25.3802177275058,39.9437494905281,-52.64995));
#132180=CARTESIAN_POINT('',(-25.3802177275058,39.9437494905281,-52.64995));
#132181=CARTESIAN_POINT('',(-23.7796330855957,40.3581899105085,-52.64995));
#132182=CARTESIAN_POINT('Origin',(-25.8159964412441,44.9247229809868,-52.64995));
#132183=CARTESIAN_POINT('',(-23.7796330855957,40.3581899105085,-60.5010370523947));
#132184=CARTESIAN_POINT('',(-23.7796330855957,40.3581899105085,-55.24995));
#132185=CARTESIAN_POINT('Ctrl Pts',(-25.3802177275058,39.9437494905281,
-60.1097730249189));
#132186=CARTESIAN_POINT('Ctrl Pts',(-25.2914736937722,39.9515135874353,
-60.1414728066845));
#132187=CARTESIAN_POINT('Ctrl Pts',(-25.2032163472256,39.9616205609225,
-60.1731437386284));
#132188=CARTESIAN_POINT('Ctrl Pts',(-25.115294687975,39.9740647365747,-60.2040070978231));
#132189=CARTESIAN_POINT('Ctrl Pts',(-25.0249019722788,39.9868586583613,
-60.235737878121));
#132190=CARTESIAN_POINT('Ctrl Pts',(-24.9348634969356,40.0021228222354,
-60.2666150537668));
#132191=CARTESIAN_POINT('Ctrl Pts',(-24.8450231973729,40.0199079019358,
-60.2957923806914));
#132192=CARTESIAN_POINT('Ctrl Pts',(-24.7551828978101,40.0376929816362,
-60.324969707616));
#132193=CARTESIAN_POINT('Ctrl Pts',(-24.6655401952566,40.0579990530801,
-60.3524471858193));
#132194=CARTESIAN_POINT('Ctrl Pts',(-24.5759556726477,40.0809332567916,
-60.3773785712321));
#132195=CARTESIAN_POINT('Ctrl Pts',(-24.4871224941809,40.1036751116563,
-60.402100857463));
#132196=CARTESIAN_POINT('Ctrl Pts',(-24.3980209679472,40.1290938411118,
-60.4240895083655));
#132197=CARTESIAN_POINT('Ctrl Pts',(-24.3090165921686,40.157227649633,-60.442417337988));
#132198=CARTESIAN_POINT('Ctrl Pts',(-24.2201098694864,40.1853305905312,
-60.4607250588316));
#132199=CARTESIAN_POINT('Ctrl Pts',(-24.1313005324118,40.2161427128992,
-60.4753799870885));
#132200=CARTESIAN_POINT('Ctrl Pts',(-24.0429505749462,40.2496498953545,
-60.4854579853069));
#132201=CARTESIAN_POINT('Ctrl Pts',(-23.9546006174805,40.2831570778098,
-60.4955359835253));
#132202=CARTESIAN_POINT('Ctrl Pts',(-23.8667104997529,40.3193593025707,
-60.5010370517052));
#132203=CARTESIAN_POINT('Ctrl Pts',(-23.7796330855957,40.3581899105084,
-60.5010370523947));
#132204=CARTESIAN_POINT('Origin',(0.,-12.9675000200281,-60.5010370523947));
#132205=CARTESIAN_POINT('',(-22.3428990418278,40.7794755973209,-61.0754935261978));
#132206=CARTESIAN_POINT('',(-23.7057274034393,40.1924568448808,-61.0754935261973));
#132207=CARTESIAN_POINT('Origin',(0.,-12.9675000200281,-61.0754935261978));
#132208=CARTESIAN_POINT('Origin',(-23.372360414466,39.4448832964128,-60.5010370523947));
#132209=CARTESIAN_POINT('',(-22.3089577584378,40.9899884313956,-60.5010370523947));
#132210=CARTESIAN_POINT('Origin',(0.,-12.9675000200281,-60.5010370523947));
#132211=CARTESIAN_POINT('Ctrl Pts',(-22.3428990418278,40.7794755973209,
-61.0754935261978));
#132212=CARTESIAN_POINT('Ctrl Pts',(-22.3211558478618,40.913825471773,-60.9106181484486));
#132213=CARTESIAN_POINT('Ctrl Pts',(-22.3089577682091,40.9899884273556,
-60.7079658702078));
#132214=CARTESIAN_POINT('Ctrl Pts',(-22.3089577584378,40.9899884313956,
-60.5010370523947));
#132215=CARTESIAN_POINT('Origin',(-22.5,41.4520521304013,-55.24995));
#132216=CARTESIAN_POINT('',(-22.,41.4520521304013,-55.74995));
#132217=CARTESIAN_POINT('',(-22.3089577584378,40.9899884313956,-55.74995));
#132218=CARTESIAN_POINT('Origin',(-22.5,41.4520521304013,-55.74995));
#132219=CARTESIAN_POINT('',(-22.,41.4520521304013,-60.5010370523947));
#132220=CARTESIAN_POINT('',(-22.,41.4520521304013,-92.34995));
#132221=CARTESIAN_POINT('Origin',(-22.5,41.4520521304013,-60.5010370523947));
#132222=CARTESIAN_POINT('',(-22.3089577584378,40.9899884313956,-55.24995));
#132223=CARTESIAN_POINT('Ctrl Pts',(-21.3174485247294,41.3893444859658,
-54.74995));
#132224=CARTESIAN_POINT('Ctrl Pts',(-21.3174485247294,41.3893444859657,
-55.2499499999999));
#132225=CARTESIAN_POINT('Ctrl Pts',(-21.5,41.8548280612684,-55.24995));
#132226=CARTESIAN_POINT('Ctrl Pts',(-21.5685182080957,41.2908809879478,
-54.7499500358909));
#132227=CARTESIAN_POINT('Ctrl Pts',(-21.4527403558093,41.3362862814715,
-55.2057014819632));
#132228=CARTESIAN_POINT('Ctrl Pts',(-21.6265769007959,41.7555472214248,
-55.24995));
#132229=CARTESIAN_POINT('Ctrl Pts',(-21.8184932751815,41.1905485577301,
-54.8481958669544));
#132230=CARTESIAN_POINT('Ctrl Pts',(-21.6281820015964,41.2670053764725,
-55.2194033701588));
#132231=CARTESIAN_POINT('Ctrl Pts',(-21.7526677202179,41.6543297475467,
-55.2990729306864));
#132232=CARTESIAN_POINT('Ctrl Pts',(-22.1923090650992,41.0384468090859,
-55.2114532855809));
#132233=CARTESIAN_POINT('Ctrl Pts',(-21.9027572404762,41.1571860364011,
-55.4056848867362));
#132234=CARTESIAN_POINT('Ctrl Pts',(-21.9411761916919,41.5009254814558,
-55.4807016455813));
#132235=CARTESIAN_POINT('Ctrl Pts',(-22.3089577352982,40.9899884409628,
-55.4723235737238));
#132236=CARTESIAN_POINT('Ctrl Pts',(-21.9999999817668,41.117728364782,-55.5719557452777));
#132237=CARTESIAN_POINT('Ctrl Pts',(-22.,41.4520521400528,-55.6111367847502));
#132238=CARTESIAN_POINT('Ctrl Pts',(-22.3089577584378,40.9899884313956,
-55.74995));
#132239=CARTESIAN_POINT('Ctrl Pts',(-22.,41.1177283573993,-55.74995));
#132240=CARTESIAN_POINT('Ctrl Pts',(-22.,41.4520521304013,-55.74995));
#132241=CARTESIAN_POINT('',(-21.5,41.8548280612684,-55.24995));
#132242=CARTESIAN_POINT('',(-21.3174485247294,41.3893444859658,-54.74995));
#132243=CARTESIAN_POINT('Origin',(-21.5,41.8548280612684,-54.74995));
#132244=CARTESIAN_POINT('Ctrl Pts',(-21.5,41.8548280612684,-55.24995));
#132245=CARTESIAN_POINT('Ctrl Pts',(-21.6265769007959,41.7555472214248,
-55.24995));
#132246=CARTESIAN_POINT('Ctrl Pts',(-21.7526677202179,41.6543297475467,
-55.2990729306864));
#132247=CARTESIAN_POINT('Ctrl Pts',(-21.9411761916919,41.5009254814558,
-55.4807016455813));
#132248=CARTESIAN_POINT('Ctrl Pts',(-22.,41.4520521400528,-55.6111367847502));
#132249=CARTESIAN_POINT('Ctrl Pts',(-22.,41.4520521304013,-55.74995));
#132250=CARTESIAN_POINT('Ctrl Pts',(-22.3089577584378,40.9899884313956,
-55.74995));
#132251=CARTESIAN_POINT('Ctrl Pts',(-22.3089577352982,40.9899884409628,
-55.4723235737238));
#132252=CARTESIAN_POINT('Ctrl Pts',(-22.1923090650992,41.0384468090859,
-55.2114532855809));
#132253=CARTESIAN_POINT('Ctrl Pts',(-21.8184932751815,41.1905485577301,
-54.8481958669544));
#132254=CARTESIAN_POINT('Ctrl Pts',(-21.5685182080957,41.2908809879478,
-54.7499500358909));
#132255=CARTESIAN_POINT('Ctrl Pts',(-21.3174485247294,41.3893444859658,
-54.74995));
#132256=CARTESIAN_POINT('Origin',(0.,-12.9675000200281,-54.74995));
#132257=CARTESIAN_POINT('',(-21.,42.0482945870964,-55.24995));
#132258=CARTESIAN_POINT('',(-20.8216939078753,41.5811683327377,-54.74995));
#132259=CARTESIAN_POINT('Origin',(-21.,42.0482945870964,-54.74995));
#132260=CARTESIAN_POINT('Origin',(0.,-12.9675000200281,-55.24995));
#132261=CARTESIAN_POINT('Origin',(0.,-12.9675000200281,-54.74995));
#132262=CARTESIAN_POINT('Ctrl Pts',(-19.8301846741669,41.9493820112901,
-55.74995));
#132263=CARTESIAN_POINT('Ctrl Pts',(-20.5,41.7075153736088,-55.7499499999999));
#132264=CARTESIAN_POINT('Ctrl Pts',(-20.5,42.4196614549321,-55.74995));
#132265=CARTESIAN_POINT('Ctrl Pts',(-19.8301846986023,41.9493820024666,
-55.6149487156912));
#132266=CARTESIAN_POINT('Ctrl Pts',(-20.4999999995541,41.7075153734334,
-55.7174757167052));
#132267=CARTESIAN_POINT('Ctrl Pts',(-20.5,42.4196614460347,-55.6824493590803));
#132268=CARTESIAN_POINT('Ctrl Pts',(-19.8580536242861,41.939338788612,-55.4791792828035));
#132269=CARTESIAN_POINT('Ctrl Pts',(-20.4987004734351,41.7075927453749,
-55.6840485748926));
#132270=CARTESIAN_POINT('Ctrl Pts',(-20.514053798786,42.4095322277552,-55.614564639731));
#132271=CARTESIAN_POINT('Ctrl Pts',(-19.9624885940201,41.9014556000366,
-55.2332682431543));
#132272=CARTESIAN_POINT('Ctrl Pts',(-20.5049952302095,41.704035376344,-55.6029041515887));
#132273=CARTESIAN_POINT('Ctrl Pts',(-20.5667184545259,42.3713246265636,
-55.4916091232479));
#132274=CARTESIAN_POINT('Ctrl Pts',(-20.0393490386551,41.8734921844523,
-55.1219509819824));
#132275=CARTESIAN_POINT('Ctrl Pts',(-20.5131880407467,41.7002281457635,
-55.5554275272938));
#132276=CARTESIAN_POINT('Ctrl Pts',(-20.6054777681041,42.3431217478432,
-55.4359504896237));
#132277=CARTESIAN_POINT('Ctrl Pts',(-20.2250038078484,41.8052957533979,
-54.9407461359128));
#132278=CARTESIAN_POINT('Ctrl Pts',(-20.5562936263709,41.682844191329,-55.4545960701533));
#132279=CARTESIAN_POINT('Ctrl Pts',(-20.6991000803093,42.274341317199,-55.3453480693239));
#132280=CARTESIAN_POINT('Ctrl Pts',(-20.3351498160899,41.7645520870248,
-54.8693487992283));
#132281=CARTESIAN_POINT('Ctrl Pts',(-20.5906196334233,41.6694809696074,
-55.401758477076));
#132282=CARTESIAN_POINT('Ctrl Pts',(-20.7546446997872,42.233248744276,-55.3096493999238));
#132283=CARTESIAN_POINT('Ctrl Pts',(-20.569794123189,41.6767990021169,-54.774393519968));
#132284=CARTESIAN_POINT('Ctrl Pts',(-20.6877494411454,41.6322368154735,
-55.3113977742726));
#132285=CARTESIAN_POINT('Ctrl Pts',(-20.8729715384853,42.1447441871192,
-55.2621717596744));
#132286=CARTESIAN_POINT('Ctrl Pts',(-20.6965038706024,41.6289544421905,
-54.7499500128377));
#132287=CARTESIAN_POINT('Ctrl Pts',(-20.7498635250281,41.608586604298,-55.2730231656551));
#132288=CARTESIAN_POINT('Ctrl Pts',(-20.936865425116,42.0964926027484,-55.24995));
#132289=CARTESIAN_POINT('Ctrl Pts',(-20.8216939078753,41.5811683327377,
-54.74995));
#132290=CARTESIAN_POINT('Ctrl Pts',(-20.8216939078753,41.5811683327377,
-55.2499499999999));
#132291=CARTESIAN_POINT('Ctrl Pts',(-21.,42.0482945870964,-55.24995));
#132292=CARTESIAN_POINT('',(-20.5,42.4196614549321,-55.74995));
#132293=CARTESIAN_POINT('',(-19.8301846741669,41.9493820112901,-55.74995));
#132294=CARTESIAN_POINT('Origin',(-20.,42.4196614549321,-55.74995));
#132295=CARTESIAN_POINT('Ctrl Pts',(-20.5,42.4196614549321,-55.74995));
#132296=CARTESIAN_POINT('Ctrl Pts',(-20.5,42.4196614460347,-55.6824493590803));
#132297=CARTESIAN_POINT('Ctrl Pts',(-20.514053798786,42.4095322277552,-55.614564639731));
#132298=CARTESIAN_POINT('Ctrl Pts',(-20.5667184545259,42.3713246265636,
-55.4916091232479));
#132299=CARTESIAN_POINT('Ctrl Pts',(-20.6054777681041,42.3431217478432,
-55.4359504896237));
#132300=CARTESIAN_POINT('Ctrl Pts',(-20.6991000803093,42.274341317199,-55.3453480693239));
#132301=CARTESIAN_POINT('Ctrl Pts',(-20.7546446997872,42.233248744276,-55.3096493999238));
#132302=CARTESIAN_POINT('Ctrl Pts',(-20.8729715384853,42.1447441871192,
-55.2621717596744));
#132303=CARTESIAN_POINT('Ctrl Pts',(-20.936865425116,42.0964926027484,-55.24995));
#132304=CARTESIAN_POINT('Ctrl Pts',(-21.,42.0482945870964,-55.24995));
#132305=CARTESIAN_POINT('Ctrl Pts',(-20.8216939078753,41.5811683327377,
-54.74995));
#132306=CARTESIAN_POINT('Ctrl Pts',(-20.7819408740053,41.5963424062421,
-54.7499500040765));
#132307=CARTESIAN_POINT('Ctrl Pts',(-20.7422583702479,41.6114370651536,
-54.7524107511961));
#132308=CARTESIAN_POINT('Ctrl Pts',(-20.7028910580564,41.6263644244518,
-54.7572302478587));
#132309=CARTESIAN_POINT('Ctrl Pts',(-20.6627696815177,41.6415777110541,
-54.7621420599578));
#132310=CARTESIAN_POINT('Ctrl Pts',(-20.6229744854674,41.6566176734326,
-54.769503891898));
#132311=CARTESIAN_POINT('Ctrl Pts',(-20.5837549178886,41.6713937246249,
-54.7792610196498));
#132312=CARTESIAN_POINT('Ctrl Pts',(-20.5448758646519,41.6860414863519,
-54.7889334335166));
#132313=CARTESIAN_POINT('Ctrl Pts',(-20.5065612917295,41.7004303395792,
-54.8009599654575));
#132314=CARTESIAN_POINT('Ctrl Pts',(-20.4690629498571,41.7144677618963,
-54.8153366743301));
#132315=CARTESIAN_POINT('Ctrl Pts',(-20.4635146440737,41.716544758039,-54.8174638717741));
#132316=CARTESIAN_POINT('Ctrl Pts',(-20.4579842421572,41.7186140458698,
-54.8196426059304));
#132317=CARTESIAN_POINT('Ctrl Pts',(-20.452472600707,41.7206753085659,-54.8218729523577));
#132318=CARTESIAN_POINT('Ctrl Pts',(-20.4520370571492,41.7208381946492,
-54.8220491998562));
#132319=CARTESIAN_POINT('Ctrl Pts',(-20.4516016002718,41.7210010421259,
-54.8222257818663));
#132320=CARTESIAN_POINT('Ctrl Pts',(-20.451166230457,41.7211638508663,-54.8224026982642));
#132321=CARTESIAN_POINT('Ctrl Pts',(-20.3795793872674,41.7479341123136,
-54.851492648923));
#132322=CARTESIAN_POINT('Ctrl Pts',(-20.310713633462,41.7735197491881,-54.8894829736819));
#132323=CARTESIAN_POINT('Ctrl Pts',(-20.246890665183,41.797116806489,-54.9352464330119));
#132324=CARTESIAN_POINT('Ctrl Pts',(-20.2064337192093,41.8120748207916,
-54.9642555789606));
#132325=CARTESIAN_POINT('Ctrl Pts',(-20.1680024696344,41.8262340118398,
-54.9963875370302));
#132326=CARTESIAN_POINT('Ctrl Pts',(-20.1321785809257,41.8393931763607,
-55.0313510893754));
#132327=CARTESIAN_POINT('Ctrl Pts',(-20.1316789419887,41.8395767083895,
-55.0318387291252));
#132328=CARTESIAN_POINT('Ctrl Pts',(-20.1311797709301,41.8397600607401,
-55.0323269633832));
#132329=CARTESIAN_POINT('Ctrl Pts',(-20.1306810690887,41.839943232968,-55.0328157906737));
#132330=CARTESIAN_POINT('Ctrl Pts',(-20.0684907293798,41.8627856252243,
-55.0937747299283));
#132331=CARTESIAN_POINT('Ctrl Pts',(-20.0135863047507,41.8828310295763,
-55.16397742118));
#132332=CARTESIAN_POINT('Ctrl Pts',(-19.9685212499155,41.8992323516681,
-55.2406426510445));
#132333=CARTESIAN_POINT('Ctrl Pts',(-19.9467038340028,41.907172749542,-55.2777587094209));
#132334=CARTESIAN_POINT('Ctrl Pts',(-19.9271921606261,41.9142591786561,
-55.3163901520212));
#132335=CARTESIAN_POINT('Ctrl Pts',(-19.9102738131902,41.9203962134609,
-55.3562250735781));
#132336=CARTESIAN_POINT('Ctrl Pts',(-19.9100688061412,41.9204705786079,
-55.356707770824));
#132337=CARTESIAN_POINT('Ctrl Pts',(-19.9098641753246,41.9205448062603,
-55.3571906629275));
#132338=CARTESIAN_POINT('Ctrl Pts',(-19.9096599209391,41.9206188963538,
-55.3576737490625));
#132339=CARTESIAN_POINT('Ctrl Pts',(-19.8950560556066,41.9259162207946,
-55.3922136432421));
#132340=CARTESIAN_POINT('Ctrl Pts',(-19.8824223932141,41.9304937150683,
-55.4276284386808));
#132341=CARTESIAN_POINT('Ctrl Pts',(-19.8717730238587,41.934349206398,-55.4637108040148));
#132342=CARTESIAN_POINT('Ctrl Pts',(-19.8611060292098,41.9382110787784,
-55.499852887653));
#132343=CARTESIAN_POINT('Ctrl Pts',(-19.8524296011668,41.9413486539406,
-55.5366659074258));
#132344=CARTESIAN_POINT('Ctrl Pts',(-19.8458033807232,41.9437431691666,
-55.5739608322423));
#132345=CARTESIAN_POINT('Ctrl Pts',(-19.8393763220395,41.9460657133694,
-55.6101347978453));
#132346=CARTESIAN_POINT('Ctrl Pts',(-19.8348780094478,41.9476892093277,
-55.6467631869939));
#132347=CARTESIAN_POINT('Ctrl Pts',(-19.832407933269,41.9485802658015,-55.6836754313748));
#132348=CARTESIAN_POINT('Ctrl Pts',(-19.8309355210528,41.9491114244956,
-55.7056788173518));
#132349=CARTESIAN_POINT('Ctrl Pts',(-19.8301846781792,41.9493820098413,
-55.7277830320761));
#132350=CARTESIAN_POINT('Ctrl Pts',(-19.8301846741669,41.9493820112901,
-55.74995));
#132351=CARTESIAN_POINT('Origin',(-20.,42.4196614549321,-55.24995));
#132352=CARTESIAN_POINT('',(-19.8301846741669,41.9493820112901,-60.42825533736));
#132353=CARTESIAN_POINT('',(-19.8301846741669,41.9493820112901,-55.24995));
#132354=CARTESIAN_POINT('',(-20.5,42.4196614549321,-60.42825533736));
#132355=CARTESIAN_POINT('Origin',(-20.,42.4196614549321,-60.42825533736));
#132356=CARTESIAN_POINT('',(-20.5,42.4196614549321,-92.34995));
#132357=CARTESIAN_POINT('Origin',(0.,-12.9675000200281,-60.42825533736));
#132358=CARTESIAN_POINT('',(-13.8920088064511,43.6468101642065,-60.8508735991007));
#132359=CARTESIAN_POINT('',(-19.8457268663587,41.8441333387867,-60.8508735991007));
#132360=CARTESIAN_POINT('Origin',(0.,-12.9675000200281,-60.8508735991007));
#132361=CARTESIAN_POINT('Origin',(-20.0201720011615,40.6653127489884,-60.3953656913166));
#132362=CARTESIAN_POINT('',(-13.8811292719168,43.7459411239336,-60.42825533736));
#132363=CARTESIAN_POINT('Origin',(0.,-12.9675000200281,-60.42825533736));
#132364=CARTESIAN_POINT('Origin',(-14.0020199016113,42.6566962185633,-60.4209701665496));
#132365=CARTESIAN_POINT('Origin',(-14.,44.2316053598056,-55.24995));
#132366=CARTESIAN_POINT('',(-13.5,44.2316053598049,-55.7692503840784));
#132367=CARTESIAN_POINT('',(-13.8811292719168,43.7459411239337,-55.7692503840715));
#132368=CARTESIAN_POINT('Origin',(-14.,44.2316053598044,-55.7692503840718));
#132369=CARTESIAN_POINT('',(-13.5,44.2316053598056,-60.42825533736));
#132370=CARTESIAN_POINT('',(-13.5,44.2316053598056,-92.34995));
#132371=CARTESIAN_POINT('Origin',(-14.,44.2316053598056,-60.42825533736));
#132372=CARTESIAN_POINT('',(-13.8811292719168,43.7459411239336,-55.24995));
#132373=CARTESIAN_POINT('Ctrl Pts',(-12.8921600942007,43.978899026433,-54.7926966592038));
#132374=CARTESIAN_POINT('Ctrl Pts',(-12.9056883239205,43.9758363551094,
-55.2210744412793));
#132375=CARTESIAN_POINT('Ctrl Pts',(-13.0012809038513,44.3884784473357,
-55.2865609247418));
#132376=CARTESIAN_POINT('Ctrl Pts',(-13.0193597758081,43.9501021457404,
-54.7884376491597));
#132377=CARTESIAN_POINT('Ctrl Pts',(-12.9784387965694,43.9593348061506,
-55.2098637836594));
#132378=CARTESIAN_POINT('Ctrl Pts',(-13.0654243459864,44.3636027691474,
-55.2827944545873));
#132379=CARTESIAN_POINT('Ctrl Pts',(-13.1474090807614,43.9206427834081,
-54.8097712354121));
#132380=CARTESIAN_POINT('Ctrl Pts',(-13.0552570243808,43.9418365181403,
-55.2141810151918));
#132381=CARTESIAN_POINT('Ctrl Pts',(-13.1299983077116,44.3395152672781,
-55.2921354075477));
#132382=CARTESIAN_POINT('Ctrl Pts',(-13.3859583749986,43.8649843137035,
-54.9019989045167));
#132383=CARTESIAN_POINT('Ctrl Pts',(-13.2011715416027,43.9084021006501,
-55.25643129776));
#132384=CARTESIAN_POINT('Ctrl Pts',(-13.2502943581078,44.2958064353142,
-55.3361304655099));
#132385=CARTESIAN_POINT('Ctrl Pts',(-13.496053992198,43.8388872267122,-54.9728361666051));
#132386=CARTESIAN_POINT('Ctrl Pts',(-13.2704159548698,43.8924342454859,
-55.2940831522118));
#132387=CARTESIAN_POINT('Ctrl Pts',(-13.3058135696287,44.2762488685004,
-55.3707576859229));
#132388=CARTESIAN_POINT('Ctrl Pts',(-13.6800589131788,43.7948562869374,
-55.1530004401584));
#132389=CARTESIAN_POINT('Ctrl Pts',(-13.3860573147077,43.8656515577332,
-55.3967868701307));
#132390=CARTESIAN_POINT('Ctrl Pts',(-13.3986038888631,44.2453125071312,
-55.4597899571993));
#132391=CARTESIAN_POINT('Ctrl Pts',(-13.7547890917519,43.7767382792428,
-55.2636104102621));
#132392=CARTESIAN_POINT('Ctrl Pts',(-13.4334072964209,43.8546223828157,
-55.46277372953));
#132393=CARTESIAN_POINT('Ctrl Pts',(-13.4362889542451,44.2338103823362,
-55.514828855807));
#132394=CARTESIAN_POINT('Ctrl Pts',(-13.8547672339164,43.7524103115038,
-55.5042410247415));
#132395=CARTESIAN_POINT('Ctrl Pts',(-13.4931806941864,43.8407149886408,
-55.6082533108594));
#132396=CARTESIAN_POINT('Ctrl Pts',(-13.4867061057231,44.2229131048268,
-55.6353022097904));
#132397=CARTESIAN_POINT('Ctrl Pts',(-13.8811292609786,43.7459411266109,
-55.6370500544614));
#132398=CARTESIAN_POINT('Ctrl Pts',(-13.5063795391638,43.8376645208725,
-55.6900657479953));
#132399=CARTESIAN_POINT('Ctrl Pts',(-13.5,44.2234307110675,-55.7021231738993));
#132400=CARTESIAN_POINT('Ctrl Pts',(-13.8811292719168,43.7459411239336,
-55.7692503840715));
#132401=CARTESIAN_POINT('Ctrl Pts',(-13.5,43.83922597116,-55.7692503840715));
#132402=CARTESIAN_POINT('Ctrl Pts',(-13.5,44.2316053598055,-55.7692503840715));
#132403=CARTESIAN_POINT('',(-13.0012809040741,44.3884784473346,-55.2865609247422));
#132404=CARTESIAN_POINT('',(-12.8921600942007,43.978899026433,-54.7926966592038));
#132405=CARTESIAN_POINT('Origin',(-13.0025618077027,44.4665581918916,-54.7926966592038));
#132406=CARTESIAN_POINT('Ctrl Pts',(-13.0012809038513,44.3884784473357,
-55.2865609247418));
#132407=CARTESIAN_POINT('Ctrl Pts',(-13.0654243459864,44.3636027691474,
-55.2827944545873));
#132408=CARTESIAN_POINT('Ctrl Pts',(-13.1299983077116,44.3395152672781,
-55.2921354075477));
#132409=CARTESIAN_POINT('Ctrl Pts',(-13.2502943581078,44.2958064353142,
-55.3361304655099));
#132410=CARTESIAN_POINT('Ctrl Pts',(-13.3058135696287,44.2762488685004,
-55.3707576859229));
#132411=CARTESIAN_POINT('Ctrl Pts',(-13.3986038888631,44.2453125071312,
-55.4597899571993));
#132412=CARTESIAN_POINT('Ctrl Pts',(-13.4362889542451,44.2338103823362,
-55.514828855807));
#132413=CARTESIAN_POINT('Ctrl Pts',(-13.4867061057231,44.2229131048268,
-55.6353022097904));
#132414=CARTESIAN_POINT('Ctrl Pts',(-13.5,44.2234307110675,-55.7021231738993));
#132415=CARTESIAN_POINT('Ctrl Pts',(-13.5,44.2316053598049,-55.7692503840784));
#132416=CARTESIAN_POINT('Ctrl Pts',(-13.8811292719168,43.7459411239336,
-55.7692503840715));
#132417=CARTESIAN_POINT('Ctrl Pts',(-13.8811292682097,43.745941124841,-55.7244458157437));
#132418=CARTESIAN_POINT('Ctrl Pts',(-13.878105549578,43.7466831296689,-55.6797361384662));
#132419=CARTESIAN_POINT('Ctrl Pts',(-13.8722047277525,43.7481272051964,
-55.6355346293342));
#132420=CARTESIAN_POINT('Ctrl Pts',(-13.8662038608383,43.7495957642058,
-55.5905837086734));
#132421=CARTESIAN_POINT('Ctrl Pts',(-13.8572273197946,43.7517904587082,
-55.546156909735));
#132422=CARTESIAN_POINT('Ctrl Pts',(-13.8453776205414,43.7546819864356,
-55.5026858819472));
#132423=CARTESIAN_POINT('Ctrl Pts',(-13.8344632356935,43.7573452815742,
-55.4626460871073));
#132424=CARTESIAN_POINT('Ctrl Pts',(-13.8211106222446,43.7605999346755,
-55.42341623202));
#132425=CARTESIAN_POINT('Ctrl Pts',(-13.8053642538662,43.7644316776827,
-55.3853473456883));
#132426=CARTESIAN_POINT('Ctrl Pts',(-13.8051683359555,43.7644793526174,
-55.3848736887475));
#132427=CARTESIAN_POINT('Ctrl Pts',(-13.8049720511568,43.7645271159922,
-55.3844002212373));
#132428=CARTESIAN_POINT('Ctrl Pts',(-13.8047753996222,43.7645749677634,
-55.3839269439647));
#132429=CARTESIAN_POINT('Ctrl Pts',(-13.7718577708347,43.7725849069894,
-55.3047047522731));
#132430=CARTESIAN_POINT('Ctrl Pts',(-13.728178051491,43.7831849346495,-55.2296008411733));
#132431=CARTESIAN_POINT('Ctrl Pts',(-13.6758172364543,43.7957998172914,
-55.1617614773858));
#132432=CARTESIAN_POINT('Ctrl Pts',(-13.6492141753641,43.8022090852399,
-55.1272941999399));
#132433=CARTESIAN_POINT('Ctrl Pts',(-13.6203708268823,43.8091382966092,
-55.0947027771972));
#132434=CARTESIAN_POINT('Ctrl Pts',(-13.5895638615798,43.8165110245856,
-55.0644031256242));
#132435=CARTESIAN_POINT('Ctrl Pts',(-13.5890610147607,43.8166313659687,
-55.0639085594356));
#132436=CARTESIAN_POINT('Ctrl Pts',(-13.5885576424949,43.8167518260625,
-55.0634146006456));
#132437=CARTESIAN_POINT('Ctrl Pts',(-13.5880537459902,43.8168724045334,
-55.0629212511039));
#132438=CARTESIAN_POINT('Ctrl Pts',(-13.5330913533195,43.8300244728725,
-55.0091092659349));
#132439=CARTESIAN_POINT('Ctrl Pts',(-13.4715943783259,43.8446517471105,
-54.9620890033323));
#132440=CARTESIAN_POINT('Ctrl Pts',(-13.4054646975513,43.8602521578836,
-54.9231113264506));
#132441=CARTESIAN_POINT('Ctrl Pts',(-13.3615129962604,43.8706206427498,
-54.8972056334056));
#132442=CARTESIAN_POINT('Ctrl Pts',(-13.3155161569051,43.881418679702,-54.8748524249685));
#132443=CARTESIAN_POINT('Ctrl Pts',(-13.2680436044718,43.8924962435662,
-54.8564136580933));
#132444=CARTESIAN_POINT('Ctrl Pts',(-13.2675902582944,43.8926020304046,
-54.8562375743555));
#132445=CARTESIAN_POINT('Ctrl Pts',(-13.267136793244,43.89270783907,-54.8560618534164));
#132446=CARTESIAN_POINT('Ctrl Pts',(-13.2666832096553,43.8928136694707,
-54.8558864954404));
#132447=CARTESIAN_POINT('Ctrl Pts',(-13.2297963270863,43.9014201395016,
-54.8416258184039));
#132448=CARTESIAN_POINT('Ctrl Pts',(-13.1921658567097,43.9101602729064,
-54.82976688078));
#132449=CARTESIAN_POINT('Ctrl Pts',(-13.1539812007031,43.9189886853961,
-54.8202850097806));
#132450=CARTESIAN_POINT('Ctrl Pts',(-13.1156262419326,43.9278564724202,
-54.8107608498357));
#132451=CARTESIAN_POINT('Ctrl Pts',(-13.0767111408946,43.9368135671448,
-54.8036348844097));
#132452=CARTESIAN_POINT('Ctrl Pts',(-13.037416426663,43.9458157565233,-54.7989332461647));
#132453=CARTESIAN_POINT('Ctrl Pts',(-12.9988139657374,43.9546593547151,
-54.7943144364803));
#132454=CARTESIAN_POINT('Ctrl Pts',(-12.9598441948041,43.9635466980804,
-54.7920353122774));
#132455=CARTESIAN_POINT('Ctrl Pts',(-12.9206817922385,43.9724341406896,
-54.7921703301218));
#132456=CARTESIAN_POINT('Ctrl Pts',(-12.9111849603394,43.9745893340114,
-54.7922030717742));
#132457=CARTESIAN_POINT('Ctrl Pts',(-12.9016768542622,43.976744516291,-54.7923780107907));
#132458=CARTESIAN_POINT('Ctrl Pts',(-12.8921600942007,43.978899026433,-54.7926966592038));
#132459=CARTESIAN_POINT('Ctrl Pts',(-13.0012809038513,44.3884784473357,
-55.2865609247418));
#132460=CARTESIAN_POINT('Ctrl Pts',(-12.9056883239205,43.9758363551094,
-55.2210744412794));
#132461=CARTESIAN_POINT('Ctrl Pts',(-12.8921600942007,43.978899026433,-54.7926966592038));
#132462=CARTESIAN_POINT('Ctrl Pts',(-12.8359967737338,44.4202801831072,
-55.2911600797832));
#132463=CARTESIAN_POINT('Ctrl Pts',(-12.743502264335,44.012594228669,-55.2216770608656));
#132464=CARTESIAN_POINT('Ctrl Pts',(-12.7296669706488,44.015686029617,-54.798137418056));
#132465=CARTESIAN_POINT('Ctrl Pts',(-12.6706421628547,44.4514812651211,
-55.2954855956284));
#132466=CARTESIAN_POINT('Ctrl Pts',(-12.5803648873612,44.0488388411796,
-55.2222478741758));
#132467=CARTESIAN_POINT('Ctrl Pts',(-12.5670134373343,44.0517782170206,
-54.8033818322122));
#132468=CARTESIAN_POINT('Ctrl Pts',(-12.5052115625551,44.4820814550629,
-55.2995670619066));
#132469=CARTESIAN_POINT('Ctrl Pts',(-12.4164090892806,44.0845209580867,
-55.2227904669344));
#132470=CARTESIAN_POINT('Ctrl Pts',(-12.4042000461459,44.0871753139748,
-54.8084491013774));
#132471=CARTESIAN_POINT('',(-12.5052115622199,44.4820814550383,-55.2995670618994));
#132472=CARTESIAN_POINT('',(-12.4042000461459,44.0871753139748,-54.8084491013776));
#132473=CARTESIAN_POINT('Origin',(-12.5104231251106,44.5757617009068,-54.8084491013774));
#132474=CARTESIAN_POINT('Origin',(-1.07162825033821,-13.9448070428209,-29.8942234462249));
#132475=CARTESIAN_POINT('Origin',(-0.360052490448792,-9.26137067391203,
-40.4793207392782));
#132476=CARTESIAN_POINT('Ctrl Pts',(-11.402356187646,44.2958078622741,-55.9012688372262));
#132477=CARTESIAN_POINT('Ctrl Pts',(-12.,44.1768041254343,-55.9012688372262));
#132478=CARTESIAN_POINT('Ctrl Pts',(-12.,44.7861808691872,-55.9012688372262));
#132479=CARTESIAN_POINT('Ctrl Pts',(-11.4023562275606,44.2958078543263,
-55.6244035357895));
#132480=CARTESIAN_POINT('Ctrl Pts',(-11.9474030636527,44.1872773054367,
-55.780904033187));
#132481=CARTESIAN_POINT('Ctrl Pts',(-12.,44.7411652565669,-55.7461428048454));
#132482=CARTESIAN_POINT('Ctrl Pts',(-11.5065640898974,44.2752649070124,
-55.34818818067));
#132483=CARTESIAN_POINT('Ctrl Pts',(-11.9557714038036,44.1846647896565,
-55.6127743620011));
#132484=CARTESIAN_POINT('Ctrl Pts',(-12.0525501385771,44.690888206552,-55.5962799769554));
#132485=CARTESIAN_POINT('Ctrl Pts',(-11.8731403310981,44.2003553912551,
-54.9432617778679));
#132486=CARTESIAN_POINT('Ctrl Pts',(-12.1135094933846,44.1501114029528,
-55.3471606562964));
#132487=CARTESIAN_POINT('Ctrl Pts',(-12.2374078497883,44.5869769557055,
-55.3765885853276));
#132488=CARTESIAN_POINT('Ctrl Pts',(-12.1323033844902,44.146288095939,-54.8169114178557));
#132489=CARTESIAN_POINT('Ctrl Pts',(-12.2536090925735,44.1199772025877,
-55.2458645392504));
#132490=CARTESIAN_POINT('Ctrl Pts',(-12.3680985162645,44.5329923862803,
-55.3078232766261));
#132491=CARTESIAN_POINT('Ctrl Pts',(-12.4042000461455,44.0871753139749,
-54.8084491013774));
#132492=CARTESIAN_POINT('Ctrl Pts',(-12.4164090892808,44.0845209580867,
-55.2227904669341));
#132493=CARTESIAN_POINT('Ctrl Pts',(-12.5052115625553,44.4820814550625,
-55.2995670619065));
#132494=CARTESIAN_POINT('',(-12.0000000086793,44.7861491811712,-55.9011596426166));
#132495=CARTESIAN_POINT('',(-11.402356187646,44.2958078622741,-55.9012688372262));
#132496=CARTESIAN_POINT('Origin',(-11.5,44.7861808691872,-55.9012688372262));
#132497=CARTESIAN_POINT('Ctrl Pts',(-12.0000000086793,44.7861491811712,
-55.9011596426166));
#132498=CARTESIAN_POINT('Ctrl Pts',(-12.0000246627355,44.7411416626413,
-55.74607247996));
#132499=CARTESIAN_POINT('Ctrl Pts',(-12.0525718259175,44.6908760157775,
-55.596254202959));
#132500=CARTESIAN_POINT('Ctrl Pts',(-12.2374078497883,44.5869769557055,
-55.3765885853276));
#132501=CARTESIAN_POINT('Ctrl Pts',(-12.3680985162645,44.5329923862803,
-55.3078232766261));
#132502=CARTESIAN_POINT('Ctrl Pts',(-12.5052115625557,44.4820814550628,
-55.2995670619079));
#132503=CARTESIAN_POINT('Ctrl Pts',(-12.4042000461459,44.0871753139748,
-54.8084491013776));
#132504=CARTESIAN_POINT('Ctrl Pts',(-12.1323033844902,44.146288095939,-54.8169114178557));
#132505=CARTESIAN_POINT('Ctrl Pts',(-11.8731403310981,44.2003553912551,
-54.9432617778679));
#132506=CARTESIAN_POINT('Ctrl Pts',(-11.5065640898974,44.2752649070124,
-55.34818818067));
#132507=CARTESIAN_POINT('Ctrl Pts',(-11.4023562275606,44.2958078543263,
-55.6244035357895));
#132508=CARTESIAN_POINT('Ctrl Pts',(-11.402356187646,44.2958078622741,-55.9012688372262));
#132509=CARTESIAN_POINT('Origin',(-11.5,44.7861808691872,-55.24995));
#132510=CARTESIAN_POINT('',(-12.,44.7861808691872,-60.42825533736));
#132511=CARTESIAN_POINT('',(-11.402356187646,44.2958078622741,-60.42825533736));
#132512=CARTESIAN_POINT('Origin',(-11.5,44.7861808691872,-60.42825533736));
#132513=CARTESIAN_POINT('',(-12.,44.7861808691872,-92.34995));
#132514=CARTESIAN_POINT('',(-11.402356187646,44.2958078622741,-55.24995));
#132515=CARTESIAN_POINT('Origin',(0.,-12.9675000200281,-60.42825533736));
#132516=CARTESIAN_POINT('',(-5.45757488824865,45.0702713246265,-60.8508735991007));
#132517=CARTESIAN_POINT('',(-11.4112929481563,44.1984900402045,-60.8508735991007));
#132518=CARTESIAN_POINT('Origin',(0.,-12.9675000200281,-60.8508735991007));
#132519=CARTESIAN_POINT('Origin',(-11.5321619114544,42.885355037367,-60.3485867710543));
#132520=CARTESIAN_POINT('',(-5.4533007853959,45.1647773033082,-60.42825533736));
#132521=CARTESIAN_POINT('Origin',(0.,-12.9675000200281,-60.42825533736));
#132522=CARTESIAN_POINT('Origin',(-5.49875184992484,44.1739762304382,-60.4281300090422));
#132523=CARTESIAN_POINT('Origin',(-5.5,45.6625917098448,-55.24995));
#132524=CARTESIAN_POINT('',(-4.9999999999978,45.6625933174098,-56.1488938878456));
#132525=CARTESIAN_POINT('',(-5.4533007853959,45.1647773033082,-56.1488993661993));
#132526=CARTESIAN_POINT('Origin',(-5.5,45.6625917098448,-56.1488993661993));
#132527=CARTESIAN_POINT('',(-5.,45.6625917098448,-60.42825533736));
#132528=CARTESIAN_POINT('',(-5.,45.6625917098448,-92.34995));
#132529=CARTESIAN_POINT('Origin',(-5.5,45.6625917098448,-60.42825533736));
#132530=CARTESIAN_POINT('',(-5.4533007853959,45.1647773033082,-55.24995));
#132531=CARTESIAN_POINT('Ctrl Pts',(-4.40504871546089,45.2535845867532,
-54.9609750843567));
#132532=CARTESIAN_POINT('Ctrl Pts',(-4.4367234185141,45.2509948349534,-55.2414357815079));
#132533=CARTESIAN_POINT('Ctrl Pts',(-4.47139039164496,45.4906548448225,
-55.3863604038317));
#132534=CARTESIAN_POINT('Ctrl Pts',(-4.5746726100032,45.2407903510215,-54.9401638606374));
#132535=CARTESIAN_POINT('Ctrl Pts',(-4.55013513142196,45.2423482358409,
-55.222182383583));
#132536=CARTESIAN_POINT('Ctrl Pts',(-4.55693219186133,45.4776416184102,
-55.3719745613437));
#132537=CARTESIAN_POINT('Ctrl Pts',(-4.75204967627729,45.2264957449184,
-54.9756360521501));
#132538=CARTESIAN_POINT('Ctrl Pts',(-4.67148999584465,45.2327453727894,
-55.2479506024288));
#132539=CARTESIAN_POINT('Ctrl Pts',(-4.64632152753943,45.4720450292502,
-55.3906024673539));
#132540=CARTESIAN_POINT('Ctrl Pts',(-5.02768780679811,45.2032674062285,
-55.1236362709704));
#132541=CARTESIAN_POINT('Ctrl Pts',(-4.85155529671713,45.2181899234016,
-55.3600111127249));
#132542=CARTESIAN_POINT('Ctrl Pts',(-4.78526231654569,45.4785391935409,
-55.4758941943565));
#132543=CARTESIAN_POINT('Ctrl Pts',(-5.13603339661033,45.1937280671781,
-55.2216356337625));
#132544=CARTESIAN_POINT('Ctrl Pts',(-4.91960725641842,45.2125663061104,
-55.4362681462788));
#132545=CARTESIAN_POINT('Ctrl Pts',(-4.83987531604392,45.4877168692796,
-55.5336384447089));
#132546=CARTESIAN_POINT('Ctrl Pts',(-5.30411094495532,45.178640871319,-55.4541550621106));
#132547=CARTESIAN_POINT('Ctrl Pts',(-5.01304731809969,45.2048811773774,
-55.6156547787452));
#132548=CARTESIAN_POINT('Ctrl Pts',(-4.92459268013903,45.5188916935313,
-55.6761597789111));
#132549=CARTESIAN_POINT('Ctrl Pts',(-5.3635004865346,45.1731436419376,-55.5870891782066));
#132550=CARTESIAN_POINT('Ctrl Pts',(-5.03798355387793,45.2028686588533,
-55.7195028114066));
#132551=CARTESIAN_POINT('Ctrl Pts',(-4.95452456181636,45.5407314582523,
-55.7600334675643));
#132552=CARTESIAN_POINT('Ctrl Pts',(-5.44607043400789,45.165473055749,-55.892595119653));
#132553=CARTESIAN_POINT('Ctrl Pts',(-5.04892271004842,45.2022954662183,
-55.9561269088792));
#132554=CARTESIAN_POINT('Ctrl Pts',(-4.99613220506375,45.6005437839053,
-55.9629949137758));
#132555=CARTESIAN_POINT('Ctrl Pts',(-5.45934494047939,45.1642043041266,
-56.0648075138966));
#132556=CARTESIAN_POINT('Ctrl Pts',(-5.0236821379186,45.2047138612132,-56.09030865871));
#132557=CARTESIAN_POINT('Ctrl Pts',(-5.00281283901273,45.6402645497959,
-56.0837699876347));
#132558=CARTESIAN_POINT('Ctrl Pts',(-5.45177805579373,45.1649222445519,
-56.2401344498719));
#132559=CARTESIAN_POINT('Ctrl Pts',(-4.97691572104394,45.208981116778,-56.2185887282704));
#132560=CARTESIAN_POINT('Ctrl Pts',(-4.99898645253332,45.6858523253614,
-56.2175969723113));
#132561=CARTESIAN_POINT('',(-4.51630724703443,45.4845441383223,-55.3818234144838));
#132562=CARTESIAN_POINT('',(-4.49412912371054,45.2467848220337,-54.955514051414));
#132563=CARTESIAN_POINT('Origin',(-4.53261449406992,45.7453014980519,-54.955514051414));
#132564=CARTESIAN_POINT('Ctrl Pts',(-4.51630724703492,45.4845441383302,
-55.3818234144886));
#132565=CARTESIAN_POINT('Ctrl Pts',(-4.58764035252675,45.4759709740095,
-55.3793081773896));
#132566=CARTESIAN_POINT('Ctrl Pts',(-4.6595628053899,45.4726639334208,-55.3987309043929));
#132567=CARTESIAN_POINT('Ctrl Pts',(-4.78526231654569,45.4785391935409,
-55.4758941943565));
#132568=CARTESIAN_POINT('Ctrl Pts',(-4.83987531604392,45.4877168692796,
-55.5336384447089));
#132569=CARTESIAN_POINT('Ctrl Pts',(-4.92459268013903,45.5188916935313,
-55.6761597789111));
#132570=CARTESIAN_POINT('Ctrl Pts',(-4.95452456181636,45.5407314582523,
-55.7600334675643));
#132571=CARTESIAN_POINT('Ctrl Pts',(-4.99216667017373,45.5948431999328,
-55.9436510953457));
#132572=CARTESIAN_POINT('Ctrl Pts',(-4.99999978324149,45.6266502446907,
-56.0420243862498));
#132573=CARTESIAN_POINT('Ctrl Pts',(-4.9999999999955,45.6625902180274,-56.1488949301565));
#132574=CARTESIAN_POINT('Ctrl Pts',(-5.4533007853959,45.1647773033082,-56.1488993661993));
#132575=CARTESIAN_POINT('Ctrl Pts',(-5.4533007853959,45.1647773033082,-56.0055674620926));
#132576=CARTESIAN_POINT('Ctrl Pts',(-5.43788134491899,45.1662336319389,
-55.8645506073504));
#132577=CARTESIAN_POINT('Ctrl Pts',(-5.3637535993023,45.1731199385278,-55.5890146236025));
#132578=CARTESIAN_POINT('Ctrl Pts',(-5.30482297007121,45.1785752810591,
-55.4563513172782));
#132579=CARTESIAN_POINT('Ctrl Pts',(-5.13740816361988,45.1936060305266,
-55.2236271337424));
#132580=CARTESIAN_POINT('Ctrl Pts',(-5.02927744515326,45.2031302456007,
-55.1252272506259));
#132581=CARTESIAN_POINT('Ctrl Pts',(-4.8419870330226,45.2189180089433,-55.0241597383142));
#132582=CARTESIAN_POINT('Ctrl Pts',(-4.77441476074195,45.2245089469405,
-54.9977644123794));
#132583=CARTESIAN_POINT('Ctrl Pts',(-4.63647895825164,45.2356614644569,
-54.9633053694043));
#132584=CARTESIAN_POINT('Ctrl Pts',(-4.56605684297844,45.2412320189915,
-54.9548634767888));
#132585=CARTESIAN_POINT('Ctrl Pts',(-4.49412912371054,45.2467848220337,
-54.955514051414));
#132586=CARTESIAN_POINT('Ctrl Pts',(-4.51630724703493,45.4845441383302,
-55.3818234144886));
#132587=CARTESIAN_POINT('Ctrl Pts',(-4.49662538953713,45.2465921108978,
-55.2355242600995));
#132588=CARTESIAN_POINT('Ctrl Pts',(-4.49412912371062,45.2467848220336,
-54.955514051414));
#132589=CARTESIAN_POINT('Ctrl Pts',(-4.34919298261046,45.4956321595243,
-55.3822130600194));
#132590=CARTESIAN_POINT('Ctrl Pts',(-4.33057507588361,45.2594183143523,
-55.2356268020846));
#132591=CARTESIAN_POINT('Ctrl Pts',(-4.32798628668273,45.2596110100493,
-54.9570167865889));
#132592=CARTESIAN_POINT('Ctrl Pts',(-4.18205130859575,45.5061051687682,
-55.3825645302384));
#132593=CARTESIAN_POINT('Ctrl Pts',(-4.16425328466829,45.2715506006274,
-55.2357229472724));
#132594=CARTESIAN_POINT('Ctrl Pts',(-4.16179087919831,45.271725776299,-54.9584347299645));
#132595=CARTESIAN_POINT('Ctrl Pts',(-4.01487932239355,45.5159631499936,
-55.3828830175977));
#132596=CARTESIAN_POINT('Ctrl Pts',(-3.99772850678838,45.2829791869159,
-55.2358129028006));
#132597=CARTESIAN_POINT('Ctrl Pts',(-3.9955429059226,45.2831291022416,-54.9597685279837));
#132598=CARTESIAN_POINT('',(-4.01487932206326,45.5159631499916,-55.3828830175848));
#132599=CARTESIAN_POINT('',(-3.99554290592262,45.2831291022416,-54.9597685279837));
#132600=CARTESIAN_POINT('Origin',(-4.02975864478749,45.7819570116602,-54.9597685279843));
#132601=CARTESIAN_POINT('Origin',(0.00205740951117972,-22.4761263385902,
-51.448280968311));
#132602=CARTESIAN_POINT('Origin',(-0.000537877419798383,-12.1619648117072,
-48.1393127415158));
#132603=CARTESIAN_POINT('Ctrl Pts',(-2.97452770112504,45.3441826962898,
-56.3263223051814));
#132604=CARTESIAN_POINT('Ctrl Pts',(-3.49999999999616,45.3173779148746,
-56.3263223051846));
#132605=CARTESIAN_POINT('Ctrl Pts',(-3.5,45.8435334367382,-56.3263223051844));
#132606=CARTESIAN_POINT('Ctrl Pts',(-2.97452768320356,45.344182697204,-56.1669325210571));
#132607=CARTESIAN_POINT('Ctrl Pts',(-3.46044927957153,45.3193954300817,
-56.2062114458595));
#132608=CARTESIAN_POINT('Ctrl Pts',(-3.50000000000048,45.8043701107064,
-56.199422183327));
#132609=CARTESIAN_POINT('Ctrl Pts',(-2.98977292660286,45.3434149603554,
-56.0100642332945));
#132610=CARTESIAN_POINT('Ctrl Pts',(-3.43677818882601,45.3204789931111,
-56.08184534982));
#132611=CARTESIAN_POINT('Ctrl Pts',(-3.50768789429957,45.7667515939358,
-56.0829442465191));
#132612=CARTESIAN_POINT('Ctrl Pts',(-3.06428488995232,45.339546776353,-55.7037165501142));
#132613=CARTESIAN_POINT('Ctrl Pts',(-3.43477708310906,45.3200587327755,
-55.8400245162723));
#132614=CARTESIAN_POINT('Ctrl Pts',(-3.54526290572092,45.6961797895947,
-55.8659417020081));
#132615=CARTESIAN_POINT('Ctrl Pts',(-3.12473312373466,45.3363910645469,
-55.5532476192867));
#132616=CARTESIAN_POINT('Ctrl Pts',(-3.45484122335623,45.3186462559097,
-55.719311149436));
#132617=CARTESIAN_POINT('Ctrl Pts',(-3.57574585639141,45.6630233017381,
-55.7649226433931));
#132618=CARTESIAN_POINT('Ctrl Pts',(-3.2545824170552,45.329238556454,-55.3542910788838));
#132619=CARTESIAN_POINT('Ctrl Pts',(-3.52210194558877,45.3142897117584,
-55.5588309593355));
#132620=CARTESIAN_POINT('Ctrl Pts',(-3.64122647661092,45.619502323306,-55.6349498078453));
#132621=CARTESIAN_POINT('Ctrl Pts',(-3.30516068386241,45.3264035474275,
-55.2914116693877));
#132622=CARTESIAN_POINT('Ctrl Pts',(-3.55052601940425,45.3124719950673,
-55.508240833463));
#132623=CARTESIAN_POINT('Ctrl Pts',(-3.66673217579536,45.6057722112868,
-55.5945395207919));
#132624=CARTESIAN_POINT('Ctrl Pts',(-3.4167612791713,45.3199688102369,-55.1805611737224));
#132625=CARTESIAN_POINT('Ctrl Pts',(-3.61713920495138,45.3082025597939,
-55.418990846134));
#132626=CARTESIAN_POINT('Ctrl Pts',(-3.72301031701685,45.5810344345382,
-55.523890140111));
#132627=CARTESIAN_POINT('Ctrl Pts',(-3.47812992567118,45.3163517222977,
-55.1317622002044));
#132628=CARTESIAN_POINT('Ctrl Pts',(-3.65544514044212,45.3057432608012,
-55.3793555355223));
#132629=CARTESIAN_POINT('Ctrl Pts',(-3.75395740734289,45.5698505794225,
-55.4931090773944));
#132630=CARTESIAN_POINT('Ctrl Pts',(-3.68134449873891,45.3039876967517,
-55.0081141730616));
#132631=CARTESIAN_POINT('Ctrl Pts',(-3.78526119814061,45.2973112081201,
-55.2791383019779));
#132632=CARTESIAN_POINT('Ctrl Pts',(-3.85643479923312,45.5394893320724,
-55.41516737719));
#132633=CARTESIAN_POINT('Ctrl Pts',(-3.83550338599139,45.2941065762735,
-54.9610525310383));
#132634=CARTESIAN_POINT('Ctrl Pts',(-3.88948584507314,45.2904098439472,
-55.2390222324507));
#132635=CARTESIAN_POINT('Ctrl Pts',(-3.93416970441329,45.5245403614258,
-55.3854368917654));
#132636=CARTESIAN_POINT('Ctrl Pts',(-3.99554290592259,45.2831291022416,
-54.9597685279837));
#132637=CARTESIAN_POINT('Ctrl Pts',(-3.99772850678843,45.282979186916,-55.2358129028005));
#132638=CARTESIAN_POINT('Ctrl Pts',(-4.01487932239363,45.5159631499936,
-55.3828830175977));
#132639=CARTESIAN_POINT('',(-3.50000000126666,45.8435334367292,-56.3263223051815));
#132640=CARTESIAN_POINT('',(-2.97452770112504,45.3441826962898,-56.3263223051814));
#132641=CARTESIAN_POINT('Origin',(-3.,45.8435334367418,-56.3263223051791));
#132642=CARTESIAN_POINT('Ctrl Pts',(-3.5,45.8435334367294,-56.3263223051813));
#132643=CARTESIAN_POINT('Ctrl Pts',(-3.50000000000048,45.8043701107064,
-56.199422183327));
#132644=CARTESIAN_POINT('Ctrl Pts',(-3.50768789429957,45.7667515939358,
-56.0829442465191));
#132645=CARTESIAN_POINT('Ctrl Pts',(-3.54526290572092,45.6961797895947,
-55.8659417020081));
#132646=CARTESIAN_POINT('Ctrl Pts',(-3.57574585639141,45.6630233017381,
-55.7649226433931));
#132647=CARTESIAN_POINT('Ctrl Pts',(-3.64122647661092,45.619502323306,-55.6349498078453));
#132648=CARTESIAN_POINT('Ctrl Pts',(-3.66673217579536,45.6057722112868,
-55.5945395207919));
#132649=CARTESIAN_POINT('Ctrl Pts',(-3.72301031701685,45.5810344345382,
-55.523890140111));
#132650=CARTESIAN_POINT('Ctrl Pts',(-3.75395740734289,45.5698505794225,
-55.4931090773944));
#132651=CARTESIAN_POINT('Ctrl Pts',(-3.85643479923312,45.5394893320724,
-55.41516737719));
#132652=CARTESIAN_POINT('Ctrl Pts',(-3.93416970441329,45.5245403614258,
-55.3854368917654));
#132653=CARTESIAN_POINT('Ctrl Pts',(-4.01487932239371,45.5159631499936,
-55.3828830175977));
#132654=CARTESIAN_POINT('Ctrl Pts',(-3.99554290592259,45.2831291022416,
-54.9597685279837));
#132655=CARTESIAN_POINT('Ctrl Pts',(-3.94364694050566,45.2866887643361,
-54.9601848912554));
#132656=CARTESIAN_POINT('Ctrl Pts',(-3.89225569969733,45.290140860166,-54.9654203274235));
#132657=CARTESIAN_POINT('Ctrl Pts',(-3.84188163699223,45.2934612214908,
-54.9751546343629));
#132658=CARTESIAN_POINT('Ctrl Pts',(-3.78940342464011,45.2969202759591,
-54.9852955481435));
#132659=CARTESIAN_POINT('Ctrl Pts',(-3.73803006364864,45.3002363143352,
-55.0003187158492));
#132660=CARTESIAN_POINT('Ctrl Pts',(-3.68833368154021,45.3033833815736,
-55.0198046066587));
#132661=CARTESIAN_POINT('Ctrl Pts',(-3.63901329263832,45.3065066387106,
-55.0391430709906));
#132662=CARTESIAN_POINT('Ctrl Pts',(-3.59134547691493,45.3094634363257,
-55.0628761864965));
#132663=CARTESIAN_POINT('Ctrl Pts',(-3.54586890420048,45.3122303325377,
-55.0905475013328));
#132664=CARTESIAN_POINT('Ctrl Pts',(-3.54528805073115,45.3122656729596,
-55.0909009356016));
#132665=CARTESIAN_POINT('Ctrl Pts',(-3.5447076792751,45.3123009754724,-55.0912549191843));
#132666=CARTESIAN_POINT('Ctrl Pts',(-3.54412778939157,45.3123362401396,
-55.0916094513196));
#132667=CARTESIAN_POINT('Ctrl Pts',(-3.4770118322515,45.3164177424284,-55.1326426961998));
#132668=CARTESIAN_POINT('Ctrl Pts',(-3.41622114944532,45.3199999518618,
-55.181103831794));
#132669=CARTESIAN_POINT('Ctrl Pts',(-3.3609625888742,45.3231860861595,-55.2359880590722));
#132670=CARTESIAN_POINT('Ctrl Pts',(-3.360382416735,45.3232195381049,-55.2365643010014));
#132671=CARTESIAN_POINT('Ctrl Pts',(-3.35980281684021,45.3232529482704,
-55.2371413403592));
#132672=CARTESIAN_POINT('Ctrl Pts',(-3.35922379149642,45.3232863165813,
-55.2377191725325));
#132673=CARTESIAN_POINT('Ctrl Pts',(-3.30734351853376,45.3262760943052,
-55.2894925382397));
#132674=CARTESIAN_POINT('Ctrl Pts',(-3.26003938774077,45.3289319621743,
-55.347682131924));
#132675=CARTESIAN_POINT('Ctrl Pts',(-3.21898968010271,45.3311986016842,
-55.4089811023588));
#132676=CARTESIAN_POINT('Ctrl Pts',(-3.21640175023372,45.3313414992693,
-55.4128456228549));
#132677=CARTESIAN_POINT('Ctrl Pts',(-3.21383866111004,45.3314828508093,
-55.4167225044125));
#132678=CARTESIAN_POINT('Ctrl Pts',(-3.21130082579067,45.3316226428383,
-55.4206109203385));
#132679=CARTESIAN_POINT('Ctrl Pts',(-3.2108528415918,45.3316473192307,-55.4212973119574));
#132680=CARTESIAN_POINT('Ctrl Pts',(-3.21040556228037,45.3316719521366,
-55.4219841720788));
#132681=CARTESIAN_POINT('Ctrl Pts',(-3.20995898742772,45.3316965416118,
-55.4226714985032));
#132682=CARTESIAN_POINT('Ctrl Pts',(-3.15429853624867,45.3347613386447,
-55.5083388813912));
#132683=CARTESIAN_POINT('Ctrl Pts',(-3.10954127961322,45.337153729465,-55.6013158854464));
#132684=CARTESIAN_POINT('Ctrl Pts',(-3.07484642277075,45.338981720226,-55.6975623037685));
#132685=CARTESIAN_POINT('Ctrl Pts',(-3.05597305038912,45.3399761140203,
-55.7499186083827));
#132686=CARTESIAN_POINT('Ctrl Pts',(-3.04007792774141,45.34080344662,-55.8032432879277));
#132687=CARTESIAN_POINT('Ctrl Pts',(-3.02702981215949,45.3414808214313,
-55.8568906140328));
#132688=CARTESIAN_POINT('Ctrl Pts',(-3.0269130014781,45.3414868854957,-55.8573708811394));
#132689=CARTESIAN_POINT('Ctrl Pts',(-3.0267964073689,45.3414929380841,-55.8578511838465));
#132690=CARTESIAN_POINT('Ctrl Pts',(-3.02668002962044,45.3414989792089,
-55.8583315221214));
#132691=CARTESIAN_POINT('Ctrl Pts',(-2.9936294563398,45.3432146219472,-55.9947446729532));
#132692=CARTESIAN_POINT('Ctrl Pts',(-2.97802127132001,45.3440061056746,
-56.1340253985183));
#132693=CARTESIAN_POINT('Ctrl Pts',(-2.97505677856548,45.3441559820078,
-56.2753845134639));
#132694=CARTESIAN_POINT('Ctrl Pts',(-2.9747013176472,45.3441739531022,-56.2923343409611));
#132695=CARTESIAN_POINT('Ctrl Pts',(-2.97452770112514,45.3441826962898,
-56.3093140568238));
#132696=CARTESIAN_POINT('Ctrl Pts',(-2.97452770112504,45.3441826962898,
-56.3263223051814));
#132697=CARTESIAN_POINT('Origin',(-3.,45.8435334367418,-55.24995));
#132698=CARTESIAN_POINT('',(-3.5,45.8435334367418,-60.42825533736));
#132699=CARTESIAN_POINT('',(-2.97452770112504,45.3441826962898,-60.42825533736));
#132700=CARTESIAN_POINT('Origin',(-3.,45.8435334367418,-60.42825533736));
#132701=CARTESIAN_POINT('',(-3.5,45.8435334367418,-92.34995));
#132702=CARTESIAN_POINT('',(-2.97452770112504,45.3441826962898,-55.24995));
#132703=CARTESIAN_POINT('Ctrl Pts',(-53.4093468596021,-38.0856478194539,
-55.3542488214713));
#132704=CARTESIAN_POINT('Ctrl Pts',(-52.9364447521332,-38.0597348185281,
-55.3342330819689));
#132705=CARTESIAN_POINT('Ctrl Pts',(-52.9112495105562,-38.347717747534,
-54.9585476429427));
#132706=CARTESIAN_POINT('Ctrl Pts',(-53.4247544927353,-37.9975926380036,
-55.2862331725394));
#132707=CARTESIAN_POINT('Ctrl Pts',(-52.9572784319432,-37.9516014512281,
-55.2598937783695));
#132708=CARTESIAN_POINT('Ctrl Pts',(-52.9283556128915,-38.1521941031454,
-54.8226237570584));
#132709=CARTESIAN_POINT('Ctrl Pts',(-53.4555105552472,-37.889347597856,
-55.24995));
#132710=CARTESIAN_POINT('Ctrl Pts',(-52.9868771633111,-37.8051184700684,
-55.2259980552998));
#132711=CARTESIAN_POINT('Ctrl Pts',(-52.9626456126999,-37.9110442829472,
-54.7499500131212));
#132712=CARTESIAN_POINT('Ctrl Pts',(-53.5055391860638,-37.78000002,-55.24995));
#132713=CARTESIAN_POINT('Ctrl Pts',(-53.0181298732915,-37.6685004154141,
-55.2499499999999));
#132714=CARTESIAN_POINT('Ctrl Pts',(-53.0181298732915,-37.6685004154142,
-54.74995));
#132715=CARTESIAN_POINT('',(-53.4093468596018,-38.0856478194539,-55.3542488214713));
#132716=CARTESIAN_POINT('Origin',(-53.4093468596021,-38.3912956189078,-54.9585476429427));
#132717=CARTESIAN_POINT('',(-53.5055391860638,-37.78000002,-55.24995));
#132718=CARTESIAN_POINT('Origin',(-53.5055391860638,-37.78000002,-54.74995));
#132719=CARTESIAN_POINT('Ctrl Pts',(-53.5055391860638,-37.78000002,-55.24995));
#132720=CARTESIAN_POINT('Ctrl Pts',(-53.4555105552472,-37.889347597856,
-55.24995));
#132721=CARTESIAN_POINT('Ctrl Pts',(-53.4247544927353,-37.9975926380036,
-55.2862331725394));
#132722=CARTESIAN_POINT('Ctrl Pts',(-53.4093468596018,-38.0856478194539,
-55.3542488214713));
#132723=CARTESIAN_POINT('Origin',(-57.8922230010149,-38.7834964612722,-54.74995));
#132724=CARTESIAN_POINT('',(-53.65082011387,-37.28000002,-55.24995));
#132725=CARTESIAN_POINT('Origin',(-53.65082011387,-37.28000002,-54.74995));
#132726=CARTESIAN_POINT('Origin',(-57.8922230010149,-38.7834964612722,-55.24995));
#132727=CARTESIAN_POINT('Ctrl Pts',(-53.65082011387,-37.28000002,-55.24995));
#132728=CARTESIAN_POINT('Ctrl Pts',(-53.1795531264094,-37.1129448598586,
-55.24995));
#132729=CARTESIAN_POINT('Ctrl Pts',(-53.1795531264094,-37.1129448598586,
-54.74995));
#132730=CARTESIAN_POINT('Ctrl Pts',(-53.6913582052585,-37.222820517008,
-55.24995));
#132731=CARTESIAN_POINT('Ctrl Pts',(-53.2071047405196,-37.0352210513017,
-55.2694186883497));
#132732=CARTESIAN_POINT('Ctrl Pts',(-53.2245914375472,-36.9858906030954,
-54.74995002559));
#132733=CARTESIAN_POINT('Ctrl Pts',(-53.7354566371443,-37.1679561903806,
-55.2594951814958));
#132734=CARTESIAN_POINT('Ctrl Pts',(-53.233451048998,-36.9645829953838,
-55.3049428618926));
#132735=CARTESIAN_POINT('Ctrl Pts',(-53.2735999108999,-36.8639446739783,
-54.7690447340998));
#132736=CARTESIAN_POINT('Ctrl Pts',(-53.7823432375838,-37.115384730595,
-55.2778252214784));
#132737=CARTESIAN_POINT('Ctrl Pts',(-53.2549772028919,-36.90570598919,-55.3509337052282));
#132738=CARTESIAN_POINT('Ctrl Pts',(-53.3256899305359,-36.7471331056253,
-54.8057004429567));
#132739=CARTESIAN_POINT('',(-53.7823432375799,-37.1153847305994,-55.2778252214768));
#132740=CARTESIAN_POINT('Origin',(-53.7823432375799,-36.9507694411988,-54.8057004429536));
#132741=CARTESIAN_POINT('Ctrl Pts',(-53.7823432375799,-37.1153847305994,
-55.2778252214768));
#132742=CARTESIAN_POINT('Ctrl Pts',(-53.7654128825011,-37.1343678403332,
-55.271206398986));
#132743=CARTESIAN_POINT('Ctrl Pts',(-53.7488460686483,-37.1536518315554,
-55.265762135374));
#132744=CARTESIAN_POINT('Ctrl Pts',(-53.7326791511753,-37.1732333135577,
-55.261482119382));
#132745=CARTESIAN_POINT('Ctrl Pts',(-53.7167419269871,-37.1925365894685,
-55.2572629121949));
#132746=CARTESIAN_POINT('Ctrl Pts',(-53.7011933167552,-37.2121301535344,
-55.2541749669534));
#132747=CARTESIAN_POINT('Ctrl Pts',(-53.6860681479851,-37.2320179858152,
-55.2522576006252));
#132748=CARTESIAN_POINT('Ctrl Pts',(-53.6740454267308,-37.247826461575,
-55.2507335210425));
#132749=CARTESIAN_POINT('Ctrl Pts',(-53.662290251486,-37.2638212423203,
-55.24995));
#132750=CARTESIAN_POINT('Ctrl Pts',(-53.65082011387,-37.28000002,-55.24995));
#132751=CARTESIAN_POINT('Origin',(-57.8922230010151,12.8484964212155,-55.24995));
#132752=CARTESIAN_POINT('',(-53.3256899305368,10.8121330655672,-54.7553968408231));
#132753=CARTESIAN_POINT('',(-53.3256899305368,10.8121330655672,-52.64995));
#132754=CARTESIAN_POINT('',(-53.3256899305368,10.8121330655672,-55.24995));
#132755=CARTESIAN_POINT('',(-52.9112495105564,12.4127177074772,-52.64995));
#132756=CARTESIAN_POINT('Origin',(-57.8922230010151,12.8484964212155,-52.64995));
#132757=CARTESIAN_POINT('',(-52.9112495105564,12.4127177074773,-55.2016711737242));
#132758=CARTESIAN_POINT('',(-52.9112495105564,12.4127177074773,-55.24995));
#132759=CARTESIAN_POINT('',(-53.0821517130856,11.4835003754205,-54.74995));
#132760=CARTESIAN_POINT('Ctrl Pts',(-53.0821517130856,11.4835003754205,
-54.74995));
#132761=CARTESIAN_POINT('Ctrl Pts',(-53.0315209792098,11.6619165987151,
-54.7499500147364));
#132762=CARTESIAN_POINT('Ctrl Pts',(-52.9911015935698,11.8455806632674,
-54.7902878065788));
#132763=CARTESIAN_POINT('Ctrl Pts',(-52.9359691402844,12.1685120566519,
-54.9455502016771));
#132764=CARTESIAN_POINT('Ctrl Pts',(-52.9201323460278,12.3111864334412,
-55.062291149986));
#132765=CARTESIAN_POINT('Ctrl Pts',(-52.9112495105564,12.4127177074773,
-55.2016711737242));
#132766=CARTESIAN_POINT('',(-53.275786978871,10.927944819865,-54.74995));
#132767=CARTESIAN_POINT('Origin',(-57.8922230010151,12.8484964212155,-54.74995));
#132768=CARTESIAN_POINT('Origin',(-53.6419198431625,11.0805921128927,-56.1036535412916));
#132769=CARTESIAN_POINT('Origin',(0.,-12.9675000200281,-55.24995));
#132770=CARTESIAN_POINT('Origin',(0.,-12.9675000200281,-52.64995));
#132771=CARTESIAN_POINT('',(-53.7129480054761,9.92396941324122,-55.74995));
#132772=CARTESIAN_POINT('Ctrl Pts',(-53.7129480054761,9.92396941324122,
-55.74995));
#132773=CARTESIAN_POINT('Ctrl Pts',(-53.7129480039811,9.9239694167493,-55.6201514218302));
#132774=CARTESIAN_POINT('Ctrl Pts',(-53.702610379063,9.94826762670561,-55.4957569720976));
#132775=CARTESIAN_POINT('Ctrl Pts',(-53.6624100137865,10.0422483461928,
-55.2594857136242));
#132776=CARTESIAN_POINT('Ctrl Pts',(-53.633790842791,10.1090015716016,-55.1553271807471));
#132777=CARTESIAN_POINT('Ctrl Pts',(-53.5254458539065,10.3597364405483,
-54.885939939012));
#132778=CARTESIAN_POINT('Ctrl Pts',(-53.4285862862346,10.5813885818665,
-54.7797862992586));
#132779=CARTESIAN_POINT('Ctrl Pts',(-53.3256899305368,10.8121330655672,
-54.7553968408231));
#132780=CARTESIAN_POINT('',(-53.7129480054761,9.92396941324122,-60.42825533736));
#132781=CARTESIAN_POINT('',(-53.7129480054761,9.92396941324122,-55.24995));
#132782=CARTESIAN_POINT('',(-55.7689460407313,4.32194224278905,-60.42825533736));
#132783=CARTESIAN_POINT('Origin',(0.,-12.9675000200281,-60.42825533736));
#132784=CARTESIAN_POINT('',(-55.7689460407313,4.32194224278905,-55.74995));
#132785=CARTESIAN_POINT('',(-55.7689460407313,4.32194224278906,-55.24995));
#132786=CARTESIAN_POINT('',(-56.066723956657,3.33043300908072,-54.74995));
#132787=CARTESIAN_POINT('Ctrl Pts',(-56.0667239566569,3.33043300908083,
-54.74995));
#132788=CARTESIAN_POINT('Ctrl Pts',(-56.054810110711,3.37141798004119,-54.7499500048111));
#132789=CARTESIAN_POINT('Ctrl Pts',(-56.0428719096528,3.41230937921187,
-54.752573624799));
#132790=CARTESIAN_POINT('Ctrl Pts',(-56.0309991957517,3.45281789175014,
-54.7576881483825));
#132791=CARTESIAN_POINT('Ctrl Pts',(-56.0183308037643,3.4960411783501,-54.7631454338967));
#132792=CARTESIAN_POINT('Ctrl Pts',(-56.0057365602009,3.53882993079307,
-54.7714383768922));
#132793=CARTESIAN_POINT('Ctrl Pts',(-55.9933214348628,3.58084263808002,
-54.7824678791719));
#132794=CARTESIAN_POINT('Ctrl Pts',(-55.9809063095247,3.62285534536697,
-54.7934973814515));
#132795=CARTESIAN_POINT('Ctrl Pts',(-55.9686698102716,3.66409363256125,
-54.8072637702972));
#132796=CARTESIAN_POINT('Ctrl Pts',(-55.9567198801064,3.70420224798085,
-54.8237268632943));
#132797=CARTESIAN_POINT('Ctrl Pts',(-55.9565878111619,3.70464552274758,
-54.8239088110787));
#132798=CARTESIAN_POINT('Ctrl Pts',(-55.9564557655643,3.70508869905399,
-54.8240911044694));
#132799=CARTESIAN_POINT('Ctrl Pts',(-55.9563237434519,3.70553177648158,
-54.8242737432782));
#132800=CARTESIAN_POINT('Ctrl Pts',(-55.9343635745754,3.77923196927974,
-54.8546533441936));
#132801=CARTESIAN_POINT('Ctrl Pts',(-55.9131570003997,3.849848007421,-54.8944556864583));
#132802=CARTESIAN_POINT('Ctrl Pts',(-55.8935222184449,3.91485853316296,
-54.9422511775345));
#132803=CARTESIAN_POINT('Ctrl Pts',(-55.8818370634327,3.95354794017876,
-54.9706954823092));
#132804=CARTESIAN_POINT('Ctrl Pts',(-55.8707083955307,3.99025269895558,
-55.0019703122251));
#132805=CARTESIAN_POINT('Ctrl Pts',(-55.8603061323666,4.0244496930758,-55.0357720069019));
#132806=CARTESIAN_POINT('Ctrl Pts',(-55.8601552265094,4.02494578961079,
-55.0362623688193));
#132807=CARTESIAN_POINT('Ctrl Pts',(-55.8600044604701,4.02544140270094,
-55.0367533059883));
#132808=CARTESIAN_POINT('Ctrl Pts',(-55.859853834661,4.02593653113585,-55.0372448169564));
#132809=CARTESIAN_POINT('Ctrl Pts',(-55.8409688317124,4.08801421894894,
-55.0988689578539));
#132810=CARTESIAN_POINT('Ctrl Pts',(-55.8242867117939,4.14247853961694,
-55.1695258968662));
#132811=CARTESIAN_POINT('Ctrl Pts',(-55.8106050241011,4.1869905311095,-55.2464345690387));
#132812=CARTESIAN_POINT('Ctrl Pts',(-55.8040947258895,4.20817112995897,
-55.2830308137519));
#132813=CARTESIAN_POINT('Ctrl Pts',(-55.7982636966349,4.22709855295219,
-55.3210433783437));
#132814=CARTESIAN_POINT('Ctrl Pts',(-55.7931974644892,4.24352182478376,
-55.3601764970326));
#132815=CARTESIAN_POINT('Ctrl Pts',(-55.7931360049005,4.24372105914634,
-55.3606512295973));
#132816=CARTESIAN_POINT('Ctrl Pts',(-55.7930746570768,4.24391992824447,
-55.3611261391855));
#132817=CARTESIAN_POINT('Ctrl Pts',(-55.7930134210752,4.24411843191566,
-55.3616012250647));
#132818=CARTESIAN_POINT('Ctrl Pts',(-55.7885029443904,4.25873967037657,
-55.3965947538372));
#132819=CARTESIAN_POINT('Ctrl Pts',(-55.784613055677,4.27133328431392,-55.4324278680426));
#132820=CARTESIAN_POINT('Ctrl Pts',(-55.7813486835249,4.28189251196924,
-55.4689029452562));
#132821=CARTESIAN_POINT('Ctrl Pts',(-55.7780780325758,4.29247204957792,
-55.5054481797902));
#132822=CARTESIAN_POINT('Ctrl Pts',(-55.775435211876,4.30100963982809,-55.5426389688295));
#132823=CARTESIAN_POINT('Ctrl Pts',(-55.7734395025711,4.30745180750476,
-55.5802948673858));
#132824=CARTESIAN_POINT('Ctrl Pts',(-55.7714984886898,4.31371741785943,
-55.6169187492453));
#132825=CARTESIAN_POINT('Ctrl Pts',(-55.7701695736421,4.318000949421,-55.6539836247098));
#132826=CARTESIAN_POINT('Ctrl Pts',(-55.7694848260442,4.32020701122527,
-55.6913249513657));
#132827=CARTESIAN_POINT('Ctrl Pts',(-55.7691277073319,4.32135754604051,
-55.7107996987558));
#132828=CARTESIAN_POINT('Ctrl Pts',(-55.7689460418115,4.32194223930484,
-55.730349572429));
#132829=CARTESIAN_POINT('Ctrl Pts',(-55.7689460407313,4.32194224278905,
-55.74995));
#132830=CARTESIAN_POINT('',(-56.208463007634,2.83467839222654,-54.74995));
#132831=CARTESIAN_POINT('Origin',(0.,-12.9675000200281,-54.74995));
#132832=CARTESIAN_POINT('',(-56.4778207328943,1.8431691585182,-55.74995));
#132833=CARTESIAN_POINT('Ctrl Pts',(-56.4778207328943,1.8431691585182,-55.74995));
#132834=CARTESIAN_POINT('Ctrl Pts',(-56.4778207259178,1.84316918512194,
-55.479632471504));
#132835=CARTESIAN_POINT('Ctrl Pts',(-56.4486203895175,1.955305574271,-55.2191289705157));
#132836=CARTESIAN_POINT('Ctrl Pts',(-56.3494613434174,2.32547473937703,
-54.8529437484072));
#132837=CARTESIAN_POINT('Ctrl Pts',(-56.2799098403954,2.5805414908759,-54.7499500372609));
#132838=CARTESIAN_POINT('Ctrl Pts',(-56.208463007634,2.83467839222654,-54.74995));
#132839=CARTESIAN_POINT('',(-56.4778207328943,1.84316915851819,-60.42825533736));
#132840=CARTESIAN_POINT('',(-56.4778207328943,1.84316915851819,-55.24995));
#132841=CARTESIAN_POINT('',(-57.6567521511579,-3.75885801193397,-60.42825533736));
#132842=CARTESIAN_POINT('Origin',(0.,-12.9675000200281,-60.42825533736));
#132843=CARTESIAN_POINT('',(-57.6567521511579,-3.75885801193397,-55.9233081330105));
#132844=CARTESIAN_POINT('',(-57.6567521511579,-3.75885801193397,-55.24995));
#132845=CARTESIAN_POINT('',(-57.8012193907064,-4.71406478367238,-54.8923577774473));
#132846=CARTESIAN_POINT('Ctrl Pts',(-57.8012193907064,-4.71406478367238,
-54.8923577774473));
#132847=CARTESIAN_POINT('Ctrl Pts',(-57.7635403562534,-4.45018749203841,
-54.8876932766828));
#132848=CARTESIAN_POINT('Ctrl Pts',(-57.7251747303172,-4.19619393974228,
-55.0015199525886));
#132849=CARTESIAN_POINT('Ctrl Pts',(-57.6844132682985,-3.93331576897112,
-55.2955533951453));
#132850=CARTESIAN_POINT('Ctrl Pts',(-57.6739991030625,-3.86739163922285,
-55.4096956077557));
#132851=CARTESIAN_POINT('Ctrl Pts',(-57.6600305184041,-3.7792996685362,
-55.6597535514676));
#132852=CARTESIAN_POINT('Ctrl Pts',(-57.6567521506183,-3.75885800855547,
-55.7907772949108));
#132853=CARTESIAN_POINT('Ctrl Pts',(-57.6567521511579,-3.75885801193397,
-55.9233081330105));
#132854=CARTESIAN_POINT('',(-57.8697476022662,-5.20911947359366,-54.9007953984755));
#132855=CARTESIAN_POINT('Origin',(-1.16314418724182,-12.9460285170553,-46.7095980005158));
#132856=CARTESIAN_POINT('',(-57.9983536018174,-6.23763109620483,-56.1192785199305));
#132857=CARTESIAN_POINT('Ctrl Pts',(-57.9983536018174,-6.23763109620483,
-56.1192785199305));
#132858=CARTESIAN_POINT('Ctrl Pts',(-57.9983536018174,-6.23763109620483,
-56.0644455264786));
#132859=CARTESIAN_POINT('Ctrl Pts',(-57.9980221190057,-6.23475814249573,
-56.0098560074895));
#132860=CARTESIAN_POINT('Ctrl Pts',(-57.9973433490653,-6.22891039019456,
-55.9557040569574));
#132861=CARTESIAN_POINT('Ctrl Pts',(-57.9966909788379,-6.22329007722612,
-55.9036582632632));
#132862=CARTESIAN_POINT('Ctrl Pts',(-57.9957178277956,-6.21492191913586,
-55.8520157782166));
#132863=CARTESIAN_POINT('Ctrl Pts',(-57.9944044945626,-6.20366890587322,
-55.8009488806203));
#132864=CARTESIAN_POINT('Ctrl Pts',(-57.9933769792934,-6.19486486234419,
-55.7609955651094));
#132865=CARTESIAN_POINT('Ctrl Pts',(-57.9921411410287,-6.18429413978129,
-55.7213944424274));
#132866=CARTESIAN_POINT('Ctrl Pts',(-57.9906851268661,-6.17186945082616,
-55.682233037996));
#132867=CARTESIAN_POINT('Ctrl Pts',(-57.9906667712501,-6.17171281579784,
-55.6817393397059));
#132868=CARTESIAN_POINT('Ctrl Pts',(-57.9906483809946,-6.17155588913671,
-55.681245721757));
#132869=CARTESIAN_POINT('Ctrl Pts',(-57.9906299560812,-6.17139867071413,
-55.6807521844164));
#132870=CARTESIAN_POINT('Ctrl Pts',(-57.9875046150388,-6.14473036685058,
-55.5970355082689));
#132871=CARTESIAN_POINT('Ctrl Pts',(-57.9833865494891,-6.10971202599361,
-55.5161284707291));
#132872=CARTESIAN_POINT('Ctrl Pts',(-57.9782530724075,-6.06658854500577,
-55.4400802261805));
#132873=CARTESIAN_POINT('Ctrl Pts',(-57.9747553923278,-6.03720648329141,
-55.3882649700042));
#132874=CARTESIAN_POINT('Ctrl Pts',(-57.9707862300964,-6.00406098349662,
-55.3387057443247));
#132875=CARTESIAN_POINT('Ctrl Pts',(-57.9663371613776,-5.96722056379155,
-55.2920615727606));
#132876=CARTESIAN_POINT('Ctrl Pts',(-57.9662786111709,-5.96673574004027,
-55.2914477306162));
#132877=CARTESIAN_POINT('Ctrl Pts',(-57.9662199779913,-5.96625027756548,
-55.2908343949051));
#132878=CARTESIAN_POINT('Ctrl Pts',(-57.9661612618222,-5.96576417654625,
-55.290221567164));
#132879=CARTESIAN_POINT('Ctrl Pts',(-57.9589421887777,-5.90599871813408,
-55.2148752308619));
#132880=CARTESIAN_POINT('Ctrl Pts',(-57.9504117107847,-5.8361745051014,
-55.1470534422475));
#132881=CARTESIAN_POINT('Ctrl Pts',(-57.9407769623035,-5.75872949144323,
-55.0901422818152));
#132882=CARTESIAN_POINT('Ctrl Pts',(-57.9357443409803,-5.71827680833683,
-55.0604152660987));
#132883=CARTESIAN_POINT('Ctrl Pts',(-57.9304104809614,-5.67574542893252,
-55.0336657755841));
#132884=CARTESIAN_POINT('Ctrl Pts',(-57.9248052326105,-5.63148645921459,
-55.0103806480697));
#132885=CARTESIAN_POINT('Ctrl Pts',(-57.9247386150578,-5.63096044786508,
-55.0101039077518));
#132886=CARTESIAN_POINT('Ctrl Pts',(-57.9246719532792,-5.63043414597652,
-55.0098276317698));
#132887=CARTESIAN_POINT('Ctrl Pts',(-57.9246052474285,-5.62990755498803,
-55.0095518217287));
#132888=CARTESIAN_POINT('Ctrl Pts',(-57.9212703682263,-5.6035812685008,
-54.9957630286867));
#132889=CARTESIAN_POINT('Ctrl Pts',(-57.9178139721909,-5.57645251025529,
-54.9831217176361));
#132890=CARTESIAN_POINT('Ctrl Pts',(-57.9142675773717,-5.54877950578676,
-54.9717642717495));
#132891=CARTESIAN_POINT('Ctrl Pts',(-57.9135128174631,-5.54289001085238,
-54.9693471283529));
#132892=CARTESIAN_POINT('Ctrl Pts',(-57.9127539957424,-5.53697595914985,
-54.9669879747415));
#132893=CARTESIAN_POINT('Ctrl Pts',(-57.91199143806,-5.5310399789474,-54.9646878564231));
#132894=CARTESIAN_POINT('Ctrl Pts',(-57.9086784919242,-5.50525100176252,
-54.9546949493021));
#132895=CARTESIAN_POINT('Ctrl Pts',(-57.9052948080902,-5.47904671417076,
-54.9458177116981));
#132896=CARTESIAN_POINT('Ctrl Pts',(-57.9018664479803,-5.45263506176634,
-54.9381157197596));
#132897=CARTESIAN_POINT('Ctrl Pts',(-57.9006211279107,-5.44304127355402,
-54.9353180424943));
#132898=CARTESIAN_POINT('Ctrl Pts',(-57.8993701409321,-5.43342183598762,
-54.9326755439206));
#132899=CARTESIAN_POINT('Ctrl Pts',(-57.8981140995164,-5.42378169739181,
-54.9301886689189));
#132900=CARTESIAN_POINT('Ctrl Pts',(-57.8944762323974,-5.39586100721222,
-54.922985944005));
#132901=CARTESIAN_POINT('Ctrl Pts',(-57.8907870927058,-5.36769806592118,
-54.9170666561107));
#132902=CARTESIAN_POINT('Ctrl Pts',(-57.8870439982323,-5.33928354730618,
-54.9124555883765));
#132903=CARTESIAN_POINT('Ctrl Pts',(-57.883409887184,-5.31169634191705,
-54.9079787758579));
#132904=CARTESIAN_POINT('Ctrl Pts',(-57.8797247293364,-5.28387052582422,
-54.9047349097722));
#132905=CARTESIAN_POINT('Ctrl Pts',(-57.8759849933552,-5.25579526938797,
-54.9027947109811));
#132906=CARTESIAN_POINT('Ctrl Pts',(-57.8739226319616,-5.24031253871428,
-54.9017247447849));
#132907=CARTESIAN_POINT('Ctrl Pts',(-57.8718436840546,-5.22475414416997,
-54.9010521259367));
#132908=CARTESIAN_POINT('Ctrl Pts',(-57.8697476022663,-5.20911947359449,
-54.9007953984755));
#132909=CARTESIAN_POINT('',(-57.9983536018174,-6.23763109620483,-60.42825533736));
#132910=CARTESIAN_POINT('',(-57.9983536018174,-6.23763109620483,-55.24995));
#132911=CARTESIAN_POINT('',(-58.376606009879,-11.839658266657,-60.42825533736));
#132912=CARTESIAN_POINT('Origin',(0.,-12.9675000200281,-60.42825533736));
#132913=CARTESIAN_POINT('',(-58.376606009879,-11.839658266657,-56.2580153373943));
#132914=CARTESIAN_POINT('',(-58.376606009879,-11.839658266657,-55.24995));
#132915=CARTESIAN_POINT('',(-58.3873384184922,-12.8301367871357,-54.9623589764041));
#132916=CARTESIAN_POINT('Ctrl Pts',(-58.3873384184922,-12.8301367871357,
-54.9623589764041));
#132917=CARTESIAN_POINT('Ctrl Pts',(-58.3869791994405,-12.6774478623384,
-54.9623171132768));
#132918=CARTESIAN_POINT('Ctrl Pts',(-58.3859897562866,-12.527917508371,
-55.0050319539282));
#132919=CARTESIAN_POINT('Ctrl Pts',(-58.3840891453349,-12.3330632532853,
-55.1184352970832));
#132920=CARTESIAN_POINT('Ctrl Pts',(-58.3833791647681,-12.2716887773838,
-55.165249378439));
#132921=CARTESIAN_POINT('Ctrl Pts',(-58.3819811265814,-12.1628909733764,
-55.2698289416564));
#132922=CARTESIAN_POINT('Ctrl Pts',(-58.3812857230693,-12.1145902249729,
-55.3279498195379));
#132923=CARTESIAN_POINT('Ctrl Pts',(-58.3780124938151,-11.9012175869243,
-55.6452667274097));
#132924=CARTESIAN_POINT('Ctrl Pts',(-58.3766060091376,-11.8396582282804,
-55.955889104467));
#132925=CARTESIAN_POINT('Ctrl Pts',(-58.376606009879,-11.839658266657,-56.2580153373943));
#132926=CARTESIAN_POINT('',(-58.3863769436068,-13.3296376352283,-54.9622468511542));
#132927=CARTESIAN_POINT('Origin',(-0.783398267377109,-12.9675000260486,
-48.2446835017872));
#132928=CARTESIAN_POINT('',(-58.3718694303385,-14.3184313509278,-56.2531111209796));
#132929=CARTESIAN_POINT('Ctrl Pts',(-58.3718694303385,-14.3184313509278,
-56.2531111209796));
#132930=CARTESIAN_POINT('Ctrl Pts',(-58.3718694303385,-14.3184313509278,
-56.1315282681123));
#132931=CARTESIAN_POINT('Ctrl Pts',(-58.3720934589562,-14.3089057630787,
-56.0113829394871));
#132932=CARTESIAN_POINT('Ctrl Pts',(-58.372602521148,-14.2863749805017,
-55.8932001781189));
#132933=CARTESIAN_POINT('Ctrl Pts',(-58.3727280602367,-14.2808186968923,
-55.8640552987669));
#132934=CARTESIAN_POINT('Ctrl Pts',(-58.3728706983335,-14.274471486997,
-55.8350297744669));
#132935=CARTESIAN_POINT('Ctrl Pts',(-58.3730308041295,-14.2672811529287,
-55.8061314796515));
#132936=CARTESIAN_POINT('Ctrl Pts',(-58.3735850259137,-14.2423911122432,
-55.7060972215946));
#132937=CARTESIAN_POINT('Ctrl Pts',(-58.3743558983076,-14.2072301125135,
-55.6079785795892));
#132938=CARTESIAN_POINT('Ctrl Pts',(-58.3753143408088,-14.1603251811705,
-55.5154726363337));
#132939=CARTESIAN_POINT('Ctrl Pts',(-58.3757555226855,-14.138734313063,
-55.4728911089164));
#132940=CARTESIAN_POINT('Ctrl Pts',(-58.3762357928548,-14.114655053344,
-55.431498836353));
#132941=CARTESIAN_POINT('Ctrl Pts',(-58.3767484727564,-14.0879436829683,
-55.3916564088811));
#132942=CARTESIAN_POINT('Ctrl Pts',(-58.3783749205468,-14.0032033816892,
-55.2652585767906));
#132943=CARTESIAN_POINT('Ctrl Pts',(-58.3803191831255,-13.8924014500595,
-55.1564962213834));
#132944=CARTESIAN_POINT('Ctrl Pts',(-58.382091437956,-13.7622047346492,
-55.0806296262956));
#132945=CARTESIAN_POINT('Ctrl Pts',(-58.3829775653712,-13.6971063769441,
-55.0426963287517));
#132946=CARTESIAN_POINT('Ctrl Pts',(-58.3838281227637,-13.6263468744968,
-55.0125723550395));
#132947=CARTESIAN_POINT('Ctrl Pts',(-58.3845593996408,-13.5534863365101,
-54.9925162587396));
#132948=CARTESIAN_POINT('Ctrl Pts',(-58.385290676518,-13.4806257985234,
-54.9724601624396));
#132949=CARTESIAN_POINT('Ctrl Pts',(-58.3859030562338,-13.4060410952294,
-54.9621915864083));
#132950=CARTESIAN_POINT('Ctrl Pts',(-58.3863769436069,-13.3296376352283,
-54.9622468511542));
#132951=CARTESIAN_POINT('',(-58.3718694303385,-14.3184313509278,-60.42825533736));
#132952=CARTESIAN_POINT('',(-58.3718694303385,-14.3184313509278,-55.24995));
#132953=CARTESIAN_POINT('',(-57.9720322598041,-19.92045852138,-60.42825533736));
#132954=CARTESIAN_POINT('Origin',(0.,-12.9675000200281,-60.42825533736));
#132955=CARTESIAN_POINT('',(-57.9720322598041,-19.92045852138,-56.1088024963483));
#132956=CARTESIAN_POINT('',(-57.9720322598041,-19.92045852138,-55.24995));
#132957=CARTESIAN_POINT('',(-57.8394345625603,-20.9487258492221,-54.8970741880307));
#132958=CARTESIAN_POINT('Ctrl Pts',(-57.8394345625603,-20.948725849222,
-54.8970741880307));
#132959=CARTESIAN_POINT('Ctrl Pts',(-57.8483315717605,-20.8842497909763,
-54.8981689263727));
#132960=CARTESIAN_POINT('Ctrl Pts',(-57.8570330166385,-20.8203546606078,
-54.906184509473));
#132961=CARTESIAN_POINT('Ctrl Pts',(-57.8654251279101,-20.7580154570499,
-54.9205228428093));
#132962=CARTESIAN_POINT('Ctrl Pts',(-57.8742541462894,-20.6924307720817,
-54.9356076533483));
#132963=CARTESIAN_POINT('Ctrl Pts',(-57.8827409478708,-20.6285669203242,
-54.9576909614185));
#132964=CARTESIAN_POINT('Ctrl Pts',(-57.8907523071769,-20.5675574167388,
-54.9861327822154));
#132965=CARTESIAN_POINT('Ctrl Pts',(-57.8925393734151,-20.5539482375843,
-54.9924772009036));
#132966=CARTESIAN_POINT('Ctrl Pts',(-57.8943027736347,-20.5404811271335,
-54.9991382130806));
#132967=CARTESIAN_POINT('Ctrl Pts',(-57.8960410108923,-20.5271687639928,
-55.0061090485496));
#132968=CARTESIAN_POINT('Ctrl Pts',(-57.8961104580828,-20.5266368997638,
-55.0063875519222));
#132969=CARTESIAN_POINT('Ctrl Pts',(-57.8961798575478,-20.5261053444105,
-55.0066665020562));
#132970=CARTESIAN_POINT('Ctrl Pts',(-57.8962492093382,-20.5255740977204,
-55.0069458987164));
#132971=CARTESIAN_POINT('Ctrl Pts',(-57.9046540977694,-20.4611912009517,
-55.0408065639478));
#132972=CARTESIAN_POINT('Ctrl Pts',(-57.9123517927205,-20.4013952311835,
-55.0812026657775));
#132973=CARTESIAN_POINT('Ctrl Pts',(-57.9194238609353,-20.3458803213664,
-55.1276091020937));
#132974=CARTESIAN_POINT('Ctrl Pts',(-57.9194970031007,-20.3453061639072,
-55.1280890560674));
#132975=CARTESIAN_POINT('Ctrl Pts',(-57.9195700843622,-20.3447324149112,
-55.1285697353016));
#132976=CARTESIAN_POINT('Ctrl Pts',(-57.9196431043984,-20.3441590772921,
-55.1290511360631));
#132977=CARTESIAN_POINT('Ctrl Pts',(-57.9261585705979,-20.2930010380242,
-55.172005790074));
#132978=CARTESIAN_POINT('Ctrl Pts',(-57.9321919519937,-20.2450759632068,
-55.2207529417631));
#132979=CARTESIAN_POINT('Ctrl Pts',(-57.9375117382134,-20.2024766660004,
-55.2726481082449));
#132980=CARTESIAN_POINT('Ctrl Pts',(-57.9379542983796,-20.1989327732066,
-55.2769653368986));
#132981=CARTESIAN_POINT('Ctrl Pts',(-57.9383919237742,-20.1954257087619,
-55.2813043482872));
#132982=CARTESIAN_POINT('Ctrl Pts',(-57.938824483381,-20.1919566596153,
-55.2856636195628));
#132983=CARTESIAN_POINT('Ctrl Pts',(-57.938884960972,-20.1914716403672,
-55.2862731037146));
#132984=CARTESIAN_POINT('Ctrl Pts',(-57.9389453520762,-20.1909872680675,
-55.2868830674044));
#132985=CARTESIAN_POINT('Ctrl Pts',(-57.9390056567172,-20.1905035428318,
-55.2874935092313));
#132986=CARTESIAN_POINT('Ctrl Pts',(-57.9476291333812,-20.1213315320002,
-55.3747858097991));
#132987=CARTESIAN_POINT('Ctrl Pts',(-57.9544934737035,-20.0653204626856,
-55.4719393844644));
#132988=CARTESIAN_POINT('Ctrl Pts',(-57.9596779034765,-20.0227139410896,
-55.5751875387902));
#132989=CARTESIAN_POINT('Ctrl Pts',(-57.9612949610577,-20.0094246881199,
-55.607391313942));
#132990=CARTESIAN_POINT('Ctrl Pts',(-57.9627485647957,-19.9974396112336,
-55.6401883807122));
#132991=CARTESIAN_POINT('Ctrl Pts',(-57.964041058706,-19.9867663918423,
-55.6734654024398));
#132992=CARTESIAN_POINT('Ctrl Pts',(-57.9640600250566,-19.9866097705855,
-55.6739537170499));
#132993=CARTESIAN_POINT('Ctrl Pts',(-57.9640789558543,-19.9864534391018,
-55.6744420834267));
#132994=CARTESIAN_POINT('Ctrl Pts',(-57.964097851118,-19.9862973972617,
-55.6749305015429));
#132995=CARTESIAN_POINT('Ctrl Pts',(-57.9681300897667,-19.9529981564454,
-55.7791586525503));
#132996=CARTESIAN_POINT('Ctrl Pts',(-57.9705461679584,-19.9328724060777,
-55.8857647076465));
#132997=CARTESIAN_POINT('Ctrl Pts',(-57.9715251367094,-19.9246984926926,
-55.9945278474376));
#132998=CARTESIAN_POINT('Ctrl Pts',(-57.9718656735483,-19.9218551755562,
-56.0323613899052));
#132999=CARTESIAN_POINT('Ctrl Pts',(-57.9720322597889,-19.9204585215068,
-56.0704559927494));
#133000=CARTESIAN_POINT('Ctrl Pts',(-57.9720322598041,-19.92045852138,-56.1088024963483));
#133001=CARTESIAN_POINT('',(-57.7689991024637,-21.4435190710235,-54.8883584020537));
#133002=CARTESIAN_POINT('Origin',(-1.20679688010735,-12.992434491263,-46.5556728733189));
#133003=CARTESIAN_POINT('',(-57.6206785412152,-22.3992316056509,-55.9136064684106));
#133004=CARTESIAN_POINT('Ctrl Pts',(-57.6206785412152,-22.3992316056509,
-55.9136064684106));
#133005=CARTESIAN_POINT('Ctrl Pts',(-57.6206785412152,-22.3992316056506,
-55.8712576139305));
#133006=CARTESIAN_POINT('Ctrl Pts',(-57.6210388568449,-22.3970387396972,
-55.8289927265008));
#133007=CARTESIAN_POINT('Ctrl Pts',(-57.6217580713774,-22.3926459443346,
-55.7870504595468));
#133008=CARTESIAN_POINT('Ctrl Pts',(-57.6224751991257,-22.3882658945648,
-55.7452298870979));
#133009=CARTESIAN_POINT('Ctrl Pts',(-57.6235491311395,-22.3816988155788,
-55.7037286574054));
#133010=CARTESIAN_POINT('Ctrl Pts',(-57.6249866999782,-22.3728877575666,
-55.6627754268274));
#133011=CARTESIAN_POINT('Ctrl Pts',(-57.6263702144474,-22.3644080062531,
-55.6233620884627));
#133012=CARTESIAN_POINT('Ctrl Pts',(-57.6280905589435,-22.3538497499171,
-55.5844551760954));
#133013=CARTESIAN_POINT('Ctrl Pts',(-57.6301613121382,-22.3411160233781,
-55.5462695907392));
#133014=CARTESIAN_POINT('Ctrl Pts',(-57.6305151022056,-22.3389404546127,
-55.5397455487366));
#133015=CARTESIAN_POINT('Ctrl Pts',(-57.6308791385551,-22.3367012727077,
-55.533242612179));
#133016=CARTESIAN_POINT('Ctrl Pts',(-57.6312535111585,-22.3343978551758,
-55.5267619228708));
#133017=CARTESIAN_POINT('Ctrl Pts',(-57.631280295686,-22.3342330569249,
-55.5262982612688));
#133018=CARTESIAN_POINT('Ctrl Pts',(-57.6313071321696,-22.3340679357285,
-55.525834729741));
#133019=CARTESIAN_POINT('Ctrl Pts',(-57.6313340206222,-22.3339024914829,
-55.525371328865));
#133020=CARTESIAN_POINT('Ctrl Pts',(-57.6359864322557,-22.3052762724673,
-55.4451907525285));
#133021=CARTESIAN_POINT('Ctrl Pts',(-57.6422382498636,-22.2666955115369,
-55.3683025755968));
#133022=CARTESIAN_POINT('Ctrl Pts',(-57.6498495152227,-22.2192637924273,
-55.2978189119865));
#133023=CARTESIAN_POINT('Ctrl Pts',(-57.6538973328722,-22.194038689807,
-55.2603343408809));
#133024=CARTESIAN_POINT('Ctrl Pts',(-57.6583296672913,-22.1663100498317,
-55.2246619070075));
#133025=CARTESIAN_POINT('Ctrl Pts',(-57.6631104665852,-22.1362429894798,
-55.1912758544359));
#133026=CARTESIAN_POINT('Ctrl Pts',(-57.6631864482776,-22.1357651308643,
-55.1907452467652));
#133027=CARTESIAN_POINT('Ctrl Pts',(-57.663262518071,-22.1352866810589,
-55.1902152153126));
#133028=CARTESIAN_POINT('Ctrl Pts',(-57.6633386758179,-22.1348076407422,
-55.1896857620266));
#133029=CARTESIAN_POINT('Ctrl Pts',(-57.6719065247418,-22.0809149610439,
-55.1301215555107));
#133030=CARTESIAN_POINT('Ctrl Pts',(-57.68166029603,-22.0190502353757,-55.0773873317788));
#133031=CARTESIAN_POINT('Ctrl Pts',(-57.6921719467787,-21.9515533423688,
-55.0335672587637));
#133032=CARTESIAN_POINT('Ctrl Pts',(-57.6985643073566,-21.9105070321072,
-55.0069193312439));
#133033=CARTESIAN_POINT('Ctrl Pts',(-57.7052367391672,-21.8673790789986,
-54.983568141199));
#133034=CARTESIAN_POINT('Ctrl Pts',(-57.7120915003347,-21.8227047516213,
-54.9639818384176));
#133035=CARTESIAN_POINT('Ctrl Pts',(-57.7121639633474,-21.8222324906232,
-54.9637747878039));
#133036=CARTESIAN_POINT('Ctrl Pts',(-57.7122364434107,-21.8217600784835,
-54.9635681670512));
#133037=CARTESIAN_POINT('Ctrl Pts',(-57.7123089404443,-21.8212875156173,
-54.9633619764799));
#133038=CARTESIAN_POINT('Ctrl Pts',(-57.7175256896611,-21.7872827868695,
-54.9485248935223));
#133039=CARTESIAN_POINT('Ctrl Pts',(-57.7228431420999,-21.7524063113004,
-54.935873883604));
#133040=CARTESIAN_POINT('Ctrl Pts',(-57.7282261110468,-21.716879990905,
-54.9253981395351));
#133041=CARTESIAN_POINT('Ctrl Pts',(-57.7336334907216,-21.6811925654857,
-54.9148748899835));
#133042=CARTESIAN_POINT('Ctrl Pts',(-57.7391071704681,-21.6448481995525,
-54.9065464760172));
#133043=CARTESIAN_POINT('Ctrl Pts',(-57.7446130540745,-21.6080564477773,
-54.9004521188838));
#133044=CARTESIAN_POINT('Ctrl Pts',(-57.7499689591833,-21.5722668914813,
-54.8945237700776));
#133045=CARTESIAN_POINT('Ctrl Pts',(-57.7553555069844,-21.5360528976767,
-54.8907094534876));
#133046=CARTESIAN_POINT('Ctrl Pts',(-57.7607401663573,-21.4996096687902,
-54.8890935200766));
#133047=CARTESIAN_POINT('Ctrl Pts',(-57.7634952382929,-21.4809634165035,
-54.8882667244556));
#133048=CARTESIAN_POINT('Ctrl Pts',(-57.7662497818651,-21.4622572897839,
-54.8880162223889));
#133049=CARTESIAN_POINT('Ctrl Pts',(-57.7689991024637,-21.4435190710235,
-54.8883584020538));
#133050=CARTESIAN_POINT('',(-57.6206785412152,-22.3992316056509,-60.42825533736));
#133051=CARTESIAN_POINT('',(-57.6206785412152,-22.3992316056509,-55.24995));
#133052=CARTESIAN_POINT('',(-56.418846619879,-28.001258776103,-60.42825533736));
#133053=CARTESIAN_POINT('Origin',(0.,-12.9675000200281,-60.42825533736));
#133054=CARTESIAN_POINT('',(-56.418846619879,-28.0012587761031,-55.74995));
#133055=CARTESIAN_POINT('',(-56.418846619879,-28.0012587761031,-55.24995));
#133056=CARTESIAN_POINT('',(-56.1452664265556,-28.9927680098114,-54.74995));
#133057=CARTESIAN_POINT('Ctrl Pts',(-56.1452664265556,-28.9927680098114,
-54.74995));
#133058=CARTESIAN_POINT('Ctrl Pts',(-56.157135481805,-28.9511842266489,
-54.7499500043992));
#133059=CARTESIAN_POINT('Ctrl Pts',(-56.168934149989,-28.9096618081524,
-54.7526528441348));
#133060=CARTESIAN_POINT('Ctrl Pts',(-56.1805785937552,-28.8685154650404,
-54.7579280669059));
#133061=CARTESIAN_POINT('Ctrl Pts',(-56.192713707601,-28.825635309661,-54.7634255754322));
#133062=CARTESIAN_POINT('Ctrl Pts',(-56.204681702463,-28.7831622366754,
-54.7717167436039));
#133063=CARTESIAN_POINT('Ctrl Pts',(-56.2163892898623,-28.7414427179697,
-54.7827110993106));
#133064=CARTESIAN_POINT('Ctrl Pts',(-56.2280968772615,-28.6997231992639,
-54.7937054550174));
#133065=CARTESIAN_POINT('Ctrl Pts',(-56.239544464813,-28.6587557436148,
-54.8074032739245));
#133066=CARTESIAN_POINT('Ctrl Pts',(-56.2506343384323,-28.6188990877768,
-54.8237679977477));
#133067=CARTESIAN_POINT('Ctrl Pts',(-56.2507584702878,-28.618452961805,
-54.823951172381));
#133068=CARTESIAN_POINT('Ctrl Pts',(-56.2508825687622,-28.618006934334,
-54.8241346982876));
#133069=CARTESIAN_POINT('Ctrl Pts',(-56.2510066337442,-28.6175610058129,
-54.824318575259));
#133070=CARTESIAN_POINT('Ctrl Pts',(-56.2715808747846,-28.5436107200033,
-54.8548117012847));
#133071=CARTESIAN_POINT('Ctrl Pts',(-56.2911418613671,-28.472713004467,
-54.8948321838607));
#133072=CARTESIAN_POINT('Ctrl Pts',(-56.3090294712607,-28.4074824207921,
-54.9428936399892));
#133073=CARTESIAN_POINT('Ctrl Pts',(-56.3196152133156,-28.3688794918939,
-54.9713360188419));
#133074=CARTESIAN_POINT('Ctrl Pts',(-56.329615102025,-28.3322606012612,
-55.0025940679593));
#133075=CARTESIAN_POINT('Ctrl Pts',(-56.3388945722868,-28.2981593218029,
-55.0363576523063));
#133076=CARTESIAN_POINT('Ctrl Pts',(-56.339029993733,-28.2976616592801,
-55.036850386621));
#133077=CARTESIAN_POINT('Ctrl Pts',(-56.3391652743153,-28.297164488402,
-55.0373436962489));
#133078=CARTESIAN_POINT('Ctrl Pts',(-56.3393004137533,-28.2966678103585,
-55.037837579714));
#133079=CARTESIAN_POINT('Ctrl Pts',(-56.3561267590193,-28.2348259352618,
-55.0993314990908));
#133080=CARTESIAN_POINT('Ctrl Pts',(-56.3707655818803,-28.1806225233707,
-55.1697303039922));
#133081=CARTESIAN_POINT('Ctrl Pts',(-56.3826877315599,-28.1363072821442,
-55.2462670316835));
#133082=CARTESIAN_POINT('Ctrl Pts',(-56.388440528518,-28.1149238410887,
-55.2831983122062));
#133083=CARTESIAN_POINT('Ctrl Pts',(-56.3935608278346,-28.0958424992867,
-55.3215595430322));
#133084=CARTESIAN_POINT('Ctrl Pts',(-56.397989272594,-28.0793153399122,
-55.3610440111482));
#133085=CARTESIAN_POINT('Ctrl Pts',(-56.3980423761537,-28.0791171549869,
-55.3615174879381));
#133086=CARTESIAN_POINT('Ctrl Pts',(-56.3980953812291,-28.0789193343635,
-55.3619911356045));
#133087=CARTESIAN_POINT('Ctrl Pts',(-56.3981482877874,-28.0787218781893,
-55.3624649534454));
#133088=CARTESIAN_POINT('Ctrl Pts',(-56.4020846045284,-28.0640308820639,
-55.3977176169507));
#133089=CARTESIAN_POINT('Ctrl Pts',(-56.4054635861547,-28.051402110709,
-55.4337954284411));
#133090=CARTESIAN_POINT('Ctrl Pts',(-56.4082873243379,-28.0408381674741,
-55.4705044074017));
#133091=CARTESIAN_POINT('Ctrl Pts',(-56.4111187646799,-28.0302454095389,
-55.5073135154712));
#133092=CARTESIAN_POINT('Ctrl Pts',(-56.4133919882818,-28.0217284962733,
-55.5447583433606));
#133093=CARTESIAN_POINT('Ctrl Pts',(-56.4150963311521,-28.0153374570684,
-55.5826612239245));
#133094=CARTESIAN_POINT('Ctrl Pts',(-56.4167572958903,-28.0091090795837,
-55.6195994182216));
#133095=CARTESIAN_POINT('Ctrl Pts',(-56.4178779761682,-28.0048996781118,
-55.656973670175));
#133096=CARTESIAN_POINT('Ctrl Pts',(-56.4184359903581,-28.0028025535953,
-55.694620789627));
#133097=CARTESIAN_POINT('Ctrl Pts',(-56.4187084931304,-28.0017784358308,
-55.7130055271627));
#133098=CARTESIAN_POINT('Ctrl Pts',(-56.4188466190161,-28.0012587793416,
-55.7314552635407));
#133099=CARTESIAN_POINT('Ctrl Pts',(-56.418846619879,-28.0012587761031,
-55.74995));
#133100=CARTESIAN_POINT('',(-56.0013925566522,-29.4885226266656,-54.74995));
#133101=CARTESIAN_POINT('Origin',(0.,-12.9675000200281,-54.74995));
#133102=CARTESIAN_POINT('',(-55.6992942935022,-30.4800318603739,-55.74995));
#133103=CARTESIAN_POINT('Ctrl Pts',(-55.6992942935022,-30.4800318603739,
-55.74995));
#133104=CARTESIAN_POINT('Ctrl Pts',(-55.699294301712,-30.4800318342627,
-55.4780587856325));
#133105=CARTESIAN_POINT('Ctrl Pts',(-55.7350468385274,-30.3669899517508,
-55.2177384600888));
#133106=CARTESIAN_POINT('Ctrl Pts',(-55.8207323820705,-30.0892808127342,
-54.9437622390698));
#133107=CARTESIAN_POINT('Ctrl Pts',(-55.8541342694537,-29.9801791700519,
-54.8719723798496));
#133108=CARTESIAN_POINT('Ctrl Pts',(-55.9259713199402,-29.7425201026704,
-54.7747042862246));
#133109=CARTESIAN_POINT('Ctrl Pts',(-55.9637778607192,-29.6160253486821,
-54.7499500197391));
#133110=CARTESIAN_POINT('Ctrl Pts',(-56.0013925566522,-29.4885226266656,
-54.74995));
#133111=CARTESIAN_POINT('',(-55.6992942935022,-30.4800318603739,-60.42825533736));
#133112=CARTESIAN_POINT('',(-55.6992942935022,-30.4800318603739,-55.24995));
#133113=CARTESIAN_POINT('',(-53.6173229282256,-36.0820590308261,-60.42825533736));
#133114=CARTESIAN_POINT('Origin',(0.,-12.9675000200281,-60.42825533736));
#133115=CARTESIAN_POINT('',(-53.6173229282256,-36.0820590308261,-55.74995));
#133116=CARTESIAN_POINT('',(-53.6173229282256,-36.0820590308261,-55.24995));
#133117=CARTESIAN_POINT('Ctrl Pts',(-53.3256899305366,-36.7471331056238,
-54.8057004429536));
#133118=CARTESIAN_POINT('Ctrl Pts',(-53.4080974646291,-36.562334686105,
-54.8706857163843));
#133119=CARTESIAN_POINT('Ctrl Pts',(-53.481339980492,-36.3953483985127,
-54.9914263135601));
#133120=CARTESIAN_POINT('Ctrl Pts',(-53.587398316273,-36.1517305970246,
-55.3270423559178));
#133121=CARTESIAN_POINT('Ctrl Pts',(-53.6173229109667,-36.0820590708605,
-55.5352328299022));
#133122=CARTESIAN_POINT('Ctrl Pts',(-53.6173229282256,-36.0820590308261,
-55.74995));
#133123=CARTESIAN_POINT('Ctrl Pts',(-53.7823432375846,11.067884690566,-55.2526734204115));
#133124=CARTESIAN_POINT('Ctrl Pts',(-53.3054454943535,10.8575310968505,
-55.2747187747876));
#133125=CARTESIAN_POINT('Ctrl Pts',(-53.3256899305368,10.8121330655672,
-54.7553968408231));
#133126=CARTESIAN_POINT('Ctrl Pts',(-53.7669694165083,11.0851225427625,
-55.2508668691012));
#133127=CARTESIAN_POINT('Ctrl Pts',(-53.2957533879043,10.880281535778,-55.2650191833929));
#133128=CARTESIAN_POINT('Ctrl Pts',(-53.3086079255675,10.8504393631076,
-54.7517837407593));
#133129=CARTESIAN_POINT('Ctrl Pts',(-53.7519966717624,11.1024937011227,
-55.24995));
#133130=CARTESIAN_POINT('Ctrl Pts',(-53.2858304006402,10.9038034191885,
-55.2567197573796));
#133131=CARTESIAN_POINT('Ctrl Pts',(-53.2919715007789,10.8890420328302,
-54.7499500043796));
#133132=CARTESIAN_POINT('Ctrl Pts',(-53.7374305810854,11.11999998,-55.24995));
#133133=CARTESIAN_POINT('Ctrl Pts',(-53.275786978871,10.927944819865,-55.24995));
#133134=CARTESIAN_POINT('Ctrl Pts',(-53.275786978871,10.927944819865,-54.74995));
#133135=CARTESIAN_POINT('',(-53.7374305810854,11.11999998,-55.24995));
#133136=CARTESIAN_POINT('Origin',(-53.7374305810854,11.11999998,-54.74995));
#133137=CARTESIAN_POINT('',(-53.7823432375846,11.067884690566,-55.2526734204115));
#133138=CARTESIAN_POINT('Ctrl Pts',(-53.7374305810854,11.11999998,-55.24995));
#133139=CARTESIAN_POINT('Ctrl Pts',(-53.7521098206901,11.1023577124241,
-55.24995));
#133140=CARTESIAN_POINT('Ctrl Pts',(-53.7671137595184,11.084960698582,-55.2508838306004));
#133141=CARTESIAN_POINT('Ctrl Pts',(-53.7823432375846,11.067884690566,-55.2526734204115));
#133142=CARTESIAN_POINT('Origin',(-53.7823432375846,11.015769401132,-54.7553968408231));
#133143=CARTESIAN_POINT('Origin',(-57.8922230010151,12.8484964212155,-54.74995));
#133144=CARTESIAN_POINT('',(-53.5631588418786,11.61999998,-55.24995));
#133145=CARTESIAN_POINT('Origin',(-53.5631588418786,11.61999998,-54.74995));
#133146=CARTESIAN_POINT('Origin',(-57.8922230010151,12.8484964212155,-55.24995));
#133147=CARTESIAN_POINT('Ctrl Pts',(-53.5631588418786,11.61999998,-55.24995));
#133148=CARTESIAN_POINT('Ctrl Pts',(-53.0821517130855,11.4835003754205,
-55.24995));
#133149=CARTESIAN_POINT('Ctrl Pts',(-53.0821517130856,11.4835003754205,
-54.74995));
#133150=CARTESIAN_POINT('Ctrl Pts',(-53.5175339525391,11.7003881248737,
-55.24995));
#133151=CARTESIAN_POINT('Ctrl Pts',(-53.0531569518754,11.5856741846736,
-55.2284398184114));
#133152=CARTESIAN_POINT('Ctrl Pts',(-53.0315209792098,11.6619165987151,
-54.7499500147364));
#133153=CARTESIAN_POINT('Ctrl Pts',(-53.481213741953,11.782936109662,-55.2701189042654));
#133154=CARTESIAN_POINT('Ctrl Pts',(-53.0233020583897,11.6990374932301,
-55.2381992664208));
#133155=CARTESIAN_POINT('Ctrl Pts',(-52.9911015935698,11.8455806632674,
-54.7902878065788));
#133156=CARTESIAN_POINT('Ctrl Pts',(-53.4315945187188,11.9282552364233,
-55.3477500998626));
#133157=CARTESIAN_POINT('Ctrl Pts',(-52.976392393765,11.8900295415054,-55.3145394488894));
#133158=CARTESIAN_POINT('Ctrl Pts',(-52.9359691402844,12.1685120566519,
-54.9455502016771));
#133159=CARTESIAN_POINT('Ctrl Pts',(-53.4173436672944,11.9924457375215,
-55.4061007701193));
#133160=CARTESIAN_POINT('Ctrl Pts',(-52.9577221123402,11.9716892536029,
-55.3811617269574));
#133161=CARTESIAN_POINT('Ctrl Pts',(-52.9201323460278,12.3111864334412,
-55.062291149986));
#133162=CARTESIAN_POINT('Ctrl Pts',(-53.4093468596018,12.0381477794281,
-55.475810586866));
#133163=CARTESIAN_POINT('Ctrl Pts',(-52.9450883668935,12.0259378096739,
-55.4571865884944));
#133164=CARTESIAN_POINT('Ctrl Pts',(-52.9112495105559,12.4127177074828,
-55.2016711737319));
#133165=CARTESIAN_POINT('',(-53.4093468596018,12.0381477794281,-55.475810586866));
#133166=CARTESIAN_POINT('Origin',(-53.4093468596018,12.4562955788561,-55.2016711737319));
#133167=CARTESIAN_POINT('Ctrl Pts',(-53.4093468596018,12.0381477794281,
-55.475810586866));
#133168=CARTESIAN_POINT('Ctrl Pts',(-53.4173436672944,11.9924457375215,
-55.4061007701193));
#133169=CARTESIAN_POINT('Ctrl Pts',(-53.4315945187188,11.9282552364233,
-55.3477500998626));
#133170=CARTESIAN_POINT('Ctrl Pts',(-53.481213741953,11.782936109662,-55.2701189042654));
#133171=CARTESIAN_POINT('Ctrl Pts',(-53.5175339525391,11.7003881248737,
-55.24995));
#133172=CARTESIAN_POINT('Ctrl Pts',(-53.5631588418786,11.61999998,-55.24995));
#133173=CARTESIAN_POINT('Origin',(-48.3718238300661,29.8774509229704,-52.64995));
#133174=CARTESIAN_POINT('',(-51.3604079243413,30.1389181512134,-59.64995));
#133175=CARTESIAN_POINT('',(-51.3604079243413,30.1389181512134,-52.64995));
#133176=CARTESIAN_POINT('',(-51.3604079243413,30.1389181512134,-52.64995));
#133177=CARTESIAN_POINT('',(-50.4931441736257,31.9987712665301,-52.64995));
#133178=CARTESIAN_POINT('Origin',(-48.3718238300661,29.8774509229704,-52.64995));
#133179=CARTESIAN_POINT('',(-50.4931441736257,31.9987712665301,-59.64995));
#133180=CARTESIAN_POINT('',(-50.4931441736257,31.9987712665301,-52.64995));
#133181=CARTESIAN_POINT('Origin',(-48.3718238300661,29.8774509229704,-59.64995));
#133182=CARTESIAN_POINT('Origin',(-51.2652416360248,31.226673804131,-52.64995));
#133183=CARTESIAN_POINT('',(-52.1838946235503,20.7264221086262,-59.64995));
#133184=CARTESIAN_POINT('',(-51.6895836746288,26.3764221086262,-59.64995));
#133185=CARTESIAN_POINT('',(-51.2652416360248,31.226673804131,-59.64995));
#133186=CARTESIAN_POINT('',(-52.1838946235503,20.7264221086262,-55.74995));
#133187=CARTESIAN_POINT('',(-52.1838946235503,20.7264221086262,-52.64995));
#133188=CARTESIAN_POINT('',(-52.2713832870762,19.7264221086262,-54.74995));
#133189=CARTESIAN_POINT('Ctrl Pts',(-52.2713832870762,19.7264221086262,
-54.74995));
#133190=CARTESIAN_POINT('Ctrl Pts',(-52.2484144777976,19.9889568000129,
-54.7499500000658));
#133191=CARTESIAN_POINT('Ctrl Pts',(-52.2257153692336,20.2484087981252,
-54.8577231271255));
#133192=CARTESIAN_POINT('Ctrl Pts',(-52.2095194598201,20.4335288898127,
-55.0428432188135));
#133193=CARTESIAN_POINT('Ctrl Pts',(-52.1933235504066,20.6186489815003,
-55.2279633105015));
#133194=CARTESIAN_POINT('Ctrl Pts',(-52.1838946235561,20.7264221085606,
-55.487415308613));
#133195=CARTESIAN_POINT('Ctrl Pts',(-52.1838946235503,20.7264221086262,
-55.74995));
#133196=CARTESIAN_POINT('',(-52.3151276188392,19.2264221086262,-54.74995));
#133197=CARTESIAN_POINT('',(-51.2652416360248,31.226673804131,-54.74995));
#133198=CARTESIAN_POINT('',(-52.4026162823651,18.2264221086262,-55.74995));
#133199=CARTESIAN_POINT('Ctrl Pts',(-52.4026162823651,18.2264221086262,
-55.74995));
#133200=CARTESIAN_POINT('Ctrl Pts',(-52.4026162823594,18.2264221086918,
-55.4874153086129));
#133201=CARTESIAN_POINT('Ctrl Pts',(-52.3931873555089,18.334195235752,-55.2279633105015));
#133202=CARTESIAN_POINT('Ctrl Pts',(-52.3769914460954,18.5193153274396,
-55.0428432188135));
#133203=CARTESIAN_POINT('Ctrl Pts',(-52.3607955366818,18.7044354191273,
-54.8577231271254));
#133204=CARTESIAN_POINT('Ctrl Pts',(-52.3380964281178,18.9638874172394,
-54.7499500000658));
#133205=CARTESIAN_POINT('Ctrl Pts',(-52.3151276188392,19.2264221086262,
-54.74995));
#133206=CARTESIAN_POINT('',(-52.4026162823651,18.2264221086262,-59.64995));
#133207=CARTESIAN_POINT('',(-52.4026162823651,18.2264221086262,-52.64995));
#133208=CARTESIAN_POINT('',(-52.6206164493001,15.7346687985483,-59.64995));
#133209=CARTESIAN_POINT('',(-51.2652416360248,31.226673804131,-59.64995));
#133210=CARTESIAN_POINT('',(-52.8969272299346,12.5764221085064,-60.0627241236308));
#133211=CARTESIAN_POINT('Ctrl Pts',(-52.8969272285826,12.5764221083881,
-60.0627241236306));
#133212=CARTESIAN_POINT('Ctrl Pts',(-52.8810850690576,12.7574987008071,
-60.0124953264523));
#133213=CARTESIAN_POINT('Ctrl Pts',(-52.8651783101947,12.9393136629347,
-59.9676531117587));
#133214=CARTESIAN_POINT('Ctrl Pts',(-52.8492129207345,13.1217989910892,
-59.9276740961125));
#133215=CARTESIAN_POINT('Ctrl Pts',(-52.8424237249512,13.1993998929342,
-59.910673235274));
#133216=CARTESIAN_POINT('Ctrl Pts',(-52.8356239352219,13.2771218944156,
-59.8945524608641));
#133217=CARTESIAN_POINT('Ctrl Pts',(-52.8288140636153,13.354959116562,-59.8792742373811));
#133218=CARTESIAN_POINT('Ctrl Pts',(-52.8084063492458,13.5882204595985,
-59.8334887014819));
#133219=CARTESIAN_POINT('Ctrl Pts',(-52.7879062369248,13.822537779029,-59.7953375078724));
#133220=CARTESIAN_POINT('Ctrl Pts',(-52.7673307740641,14.0577163898014,
-59.7635551171396));
#133221=CARTESIAN_POINT('Ctrl Pts',(-52.7648947458015,14.0855603195582,
-59.7597922466466));
#133222=CARTESIAN_POINT('Ctrl Pts',(-52.7624575809797,14.1134172399927,
-59.7561214184401));
#133223=CARTESIAN_POINT('Ctrl Pts',(-52.7600192757782,14.1412871946384,
-59.7525428773024));
#133224=CARTESIAN_POINT('Ctrl Pts',(-52.7305287650648,14.4783652583491,
-59.7092615826991));
#133225=CARTESIAN_POINT('Ctrl Pts',(-52.7008776982776,14.8172785115587,
-59.6793561042853));
#133226=CARTESIAN_POINT('Ctrl Pts',(-52.6710582492635,15.1581163818776,
-59.6634323280936));
#133227=CARTESIAN_POINT('Ctrl Pts',(-52.6542978767186,15.3496883214284,
-59.6544821821278));
#133228=CARTESIAN_POINT('Ctrl Pts',(-52.6374843263042,15.541868082155,-59.6499500007379));
#133229=CARTESIAN_POINT('Ctrl Pts',(-52.6206164493001,15.7346687985483,
-59.64995));
#133230=CARTESIAN_POINT('',(-52.8969272312866,12.5764221086262,-55.74995));
#133231=CARTESIAN_POINT('',(-52.8969272312866,12.5764221086262,-52.64995));
#133232=CARTESIAN_POINT('Origin',(-52.9691152015747,11.7513098326049,-55.69773241533));
#133233=CARTESIAN_POINT('',(-51.2652416360248,31.226673804131,-52.64995));
#133234=CARTESIAN_POINT('',(-51.4708620158141,28.8764221086262,-59.64995));
#133235=CARTESIAN_POINT('',(-51.2652416360248,31.226673804131,-59.64995));
#133236=CARTESIAN_POINT('',(-51.4708620158141,28.8764221086262,-55.74995));
#133237=CARTESIAN_POINT('',(-51.4708620158141,28.8764221086262,-52.64995));
#133238=CARTESIAN_POINT('',(-51.55835067934,27.8764221086262,-54.74995));
#133239=CARTESIAN_POINT('Ctrl Pts',(-51.55835067934,27.8764221086262,-54.74995));
#133240=CARTESIAN_POINT('Ctrl Pts',(-51.5353818700614,28.1389568000129,
-54.7499500000658));
#133241=CARTESIAN_POINT('Ctrl Pts',(-51.5126827614974,28.3984087981251,
-54.8577231271254));
#133242=CARTESIAN_POINT('Ctrl Pts',(-51.4964868520838,28.5835288898127,
-55.0428432188135));
#133243=CARTESIAN_POINT('Ctrl Pts',(-51.4802909426703,28.7686489815003,
-55.2279633105015));
#133244=CARTESIAN_POINT('Ctrl Pts',(-51.4708620158198,28.8764221085606,
-55.4874153086129));
#133245=CARTESIAN_POINT('Ctrl Pts',(-51.4708620158141,28.8764221086262,
-55.74995));
#133246=CARTESIAN_POINT('',(-51.6020950111029,27.3764221086262,-54.74995));
#133247=CARTESIAN_POINT('',(-51.2652416360248,31.226673804131,-54.74995));
#133248=CARTESIAN_POINT('',(-51.6895836746288,26.3764221086262,-55.74995));
#133249=CARTESIAN_POINT('Ctrl Pts',(-51.6895836746288,26.3764221086262,
-55.74995));
#133250=CARTESIAN_POINT('Ctrl Pts',(-51.6895836746231,26.3764221086917,
-55.4874153086129));
#133251=CARTESIAN_POINT('Ctrl Pts',(-51.6801547477726,26.484195235752,-55.2279633105015));
#133252=CARTESIAN_POINT('Ctrl Pts',(-51.6639588383591,26.6693153274396,
-55.0428432188135));
#133253=CARTESIAN_POINT('Ctrl Pts',(-51.6477629289455,26.8544354191273,
-54.8577231271254));
#133254=CARTESIAN_POINT('Ctrl Pts',(-51.6250638203816,27.1138874172394,
-54.7499500000658));
#133255=CARTESIAN_POINT('Ctrl Pts',(-51.6020950111029,27.3764221086262,
-54.74995));
#133256=CARTESIAN_POINT('',(-51.6895836746288,26.3764221086262,-52.64995));
#133257=CARTESIAN_POINT('Origin',(-48.3718238300661,29.8774509229704,-59.64995));
#133258=CARTESIAN_POINT('',(-50.3642132262496,30.0517624084658,-60.64995));
#133259=CARTESIAN_POINT('Origin',(-50.3642132262496,30.0517624084658,-59.64995));
#133260=CARTESIAN_POINT('',(-49.7860373924392,31.2916644853436,-60.64995));
#133261=CARTESIAN_POINT('Origin',(-49.7860373924392,31.2916644853435,-59.64995));
#133262=CARTESIAN_POINT('Origin',(-48.3718238300661,29.8774509229704,-60.64995));
#133263=CARTESIAN_POINT('Origin',(-42.8449509429988,35.4043238100378,-52.64995));
#133264=CARTESIAN_POINT('',(-44.9662712865584,37.5256441535974,-59.64995));
#133265=CARTESIAN_POINT('',(-44.9662712865584,37.5256441535974,-52.64995));
#133266=CARTESIAN_POINT('',(-44.9662712865584,37.5256441535974,-52.64995));
#133267=CARTESIAN_POINT('',(-43.1064181712417,38.392907904313,-52.64995));
#133268=CARTESIAN_POINT('Origin',(-42.8449509429988,35.4043238100378,-52.64995));
#133269=CARTESIAN_POINT('',(-43.1064181712417,38.392907904313,-59.64995));
#133270=CARTESIAN_POINT('',(-43.1064181712417,38.392907904313,-52.64995));
#133271=CARTESIAN_POINT('Origin',(-42.8449509429988,35.4043238100378,-59.64995));
#133272=CARTESIAN_POINT('Origin',(-44.1941738241593,38.2977416159964,-52.64995));
#133273=CARTESIAN_POINT('',(-44.1941738241593,38.2977416159964,-52.64995));
#133274=CARTESIAN_POINT('',(-44.1941738241593,38.2977416159964,-59.64995));
#133275=CARTESIAN_POINT('Origin',(-42.8449509429988,35.4043238100378,-59.64995));
#133276=CARTESIAN_POINT('',(-44.2591645053719,36.8185373724109,-60.64995));
#133277=CARTESIAN_POINT('Origin',(-44.2591645053719,36.8185373724109,-59.64995));
#133278=CARTESIAN_POINT('',(-43.019262428494,37.3967132062212,-60.64995));
#133279=CARTESIAN_POINT('Origin',(-43.019262428494,37.3967132062212,-59.64995));
#133280=CARTESIAN_POINT('Origin',(-42.8449509429988,35.4043238100378,-60.64995));
#133281=CARTESIAN_POINT('Origin',(-24.5275331667447,40.0183497231583,-52.64995));
#133282=CARTESIAN_POINT('',(-36.9564221286262,38.9309628387712,-59.64995));
#133283=CARTESIAN_POINT('',(-30.9564221286262,39.4558948199267,-59.64995));
#133284=CARTESIAN_POINT('',(-24.5275331667447,40.0183497231583,-59.64995));
#133285=CARTESIAN_POINT('',(-36.9564221286262,38.9309628387712,-55.74995));
#133286=CARTESIAN_POINT('',(-36.9564221286262,38.9309628387712,-52.64995));
#133287=CARTESIAN_POINT('',(-37.9564221286262,38.8434741752452,-54.74995));
#133288=CARTESIAN_POINT('Ctrl Pts',(-37.9564221286262,38.8434741752452,
-54.74995));
#133289=CARTESIAN_POINT('Ctrl Pts',(-37.6938874372391,38.8664429845239,
-54.7499500000658));
#133290=CARTESIAN_POINT('Ctrl Pts',(-37.4344354391277,38.8891420930878,
-54.8577231271255));
#133291=CARTESIAN_POINT('Ctrl Pts',(-37.2493153474397,38.9053380025014,
-55.0428432188135));
#133292=CARTESIAN_POINT('Ctrl Pts',(-37.0641952557516,38.9215339119149,
-55.2279633105015));
#133293=CARTESIAN_POINT('Ctrl Pts',(-36.9564221286917,38.9309628387654,
-55.487415308613));
#133294=CARTESIAN_POINT('Ctrl Pts',(-36.9564221286262,38.9309628387712,
-55.74995));
#133295=CARTESIAN_POINT('',(-38.4564221286262,38.7997298434823,-54.74995));
#133296=CARTESIAN_POINT('',(-38.,38.8396616055195,-54.74995));
#133297=CARTESIAN_POINT('',(-39.4564221286262,38.7122411799564,-55.74995));
#133298=CARTESIAN_POINT('Ctrl Pts',(-39.4564221286262,38.7122411799564,
-55.74995));
#133299=CARTESIAN_POINT('Ctrl Pts',(-39.4564221285606,38.7122411799621,
-55.487415308613));
#133300=CARTESIAN_POINT('Ctrl Pts',(-39.3486490015007,38.7216701068126,
-55.2279633105015));
#133301=CARTESIAN_POINT('Ctrl Pts',(-39.1635289098127,38.7378660162261,
-55.0428432188135));
#133302=CARTESIAN_POINT('Ctrl Pts',(-38.9784088181247,38.7540619256397,
-54.8577231271255));
#133303=CARTESIAN_POINT('Ctrl Pts',(-38.7189568200132,38.7767610342036,
-54.7499500000658));
#133304=CARTESIAN_POINT('Ctrl Pts',(-38.4564221286262,38.7997298434823,
-54.74995));
#133305=CARTESIAN_POINT('',(-39.4564221286262,38.7122411799564,-59.64995));
#133306=CARTESIAN_POINT('',(-39.4564221286262,38.7122411799564,-55.74995));
#133307=CARTESIAN_POINT('',(-24.5275331667447,40.0183497231583,-59.64995));
#133308=CARTESIAN_POINT('',(-24.5275331667447,40.0183497231583,-52.64995));
#133309=CARTESIAN_POINT('',(-28.4564221286262,39.6746164787415,-59.6524466674074));
#133310=CARTESIAN_POINT('Ctrl Pts',(-28.4564221286157,39.6746164786217,
-59.6524466674074));
#133311=CARTESIAN_POINT('Ctrl Pts',(-28.131799882143,39.7030172440175,-59.6590182799318));
#133312=CARTESIAN_POINT('Ctrl Pts',(-27.8089020756434,39.7312671410702,
-59.6781506934662));
#133313=CARTESIAN_POINT('Ctrl Pts',(-27.4876982951987,39.759368830939,-59.7096215394405));
#133314=CARTESIAN_POINT('Ctrl Pts',(-27.3141484358439,39.7745524764041,
-59.7266255762083));
#133315=CARTESIAN_POINT('Ctrl Pts',(-27.1410937670819,39.7896927982217,
-59.7472310046319));
#133316=CARTESIAN_POINT('Ctrl Pts',(-26.9685328542776,39.8047899206072,
-59.7713974032318));
#133317=CARTESIAN_POINT('Ctrl Pts',(-26.9471826335434,39.8066578227303,
-59.7743874079558));
#133318=CARTESIAN_POINT('Ctrl Pts',(-26.9258394639526,39.8085251079323,
-59.7774303163423));
#133319=CARTESIAN_POINT('Ctrl Pts',(-26.904503506364,39.8103917621319,-59.7805271013239));
#133320=CARTESIAN_POINT('Ctrl Pts',(-26.5372951385281,39.8425183277711,
-59.8338251712089));
#133321=CARTESIAN_POINT('Ctrl Pts',(-26.1722508037018,39.8744555741516,
-59.9028698737186));
#133322=CARTESIAN_POINT('Ctrl Pts',(-25.8100560258455,39.9061435120041,
-59.9926952103956));
#133323=CARTESIAN_POINT('Ctrl Pts',(-25.6663124460746,39.9187194460069,
-60.0283440276549));
#133324=CARTESIAN_POINT('Ctrl Pts',(-25.5230181721787,39.9312560704728,
-60.0672655467087));
#133325=CARTESIAN_POINT('Ctrl Pts',(-25.3802177275058,39.9437494905281,
-60.1097730249189));
#133326=CARTESIAN_POINT('',(-28.4564221286262,39.6746164787415,-55.74995));
#133327=CARTESIAN_POINT('',(-28.4564221286262,39.6746164787415,-52.64995));
#133328=CARTESIAN_POINT('',(-29.4564221286262,39.5871278152156,-54.74995));
#133329=CARTESIAN_POINT('Ctrl Pts',(-29.4564221286262,39.5871278152156,
-54.74995));
#133330=CARTESIAN_POINT('Ctrl Pts',(-29.1938874372394,39.6100966244942,
-54.7499500000658));
#133331=CARTESIAN_POINT('Ctrl Pts',(-28.9344354391271,39.6327957330582,
-54.8577231271255));
#133332=CARTESIAN_POINT('Ctrl Pts',(-28.7493153474396,39.6489916424717,
-55.0428432188135));
#133333=CARTESIAN_POINT('Ctrl Pts',(-28.5641952557521,39.6651875518853,
-55.2279633105015));
#133334=CARTESIAN_POINT('Ctrl Pts',(-28.4564221286917,39.6746164787358,
-55.487415308613));
#133335=CARTESIAN_POINT('Ctrl Pts',(-28.4564221286262,39.6746164787415,
-55.74995));
#133336=CARTESIAN_POINT('',(-29.9564221286262,39.5433834834526,-54.74995));
#133337=CARTESIAN_POINT('',(-29.5,39.5833152454898,-54.74995));
#133338=CARTESIAN_POINT('',(-30.9564221286262,39.4558948199267,-55.74995));
#133339=CARTESIAN_POINT('Ctrl Pts',(-30.9564221286262,39.4558948199267,
-55.74995));
#133340=CARTESIAN_POINT('Ctrl Pts',(-30.9564221285606,39.4558948199325,
-55.4874153086129));
#133341=CARTESIAN_POINT('Ctrl Pts',(-30.8486490015003,39.4653237467829,
-55.2279633105015));
#133342=CARTESIAN_POINT('Ctrl Pts',(-30.6635289098127,39.4815196561965,
-55.0428432188135));
#133343=CARTESIAN_POINT('Ctrl Pts',(-30.4784088181251,39.4977155656101,
-54.8577231271254));
#133344=CARTESIAN_POINT('Ctrl Pts',(-30.218956820013,39.520414674174,-54.7499500000658));
#133345=CARTESIAN_POINT('Ctrl Pts',(-29.9564221286262,39.5433834834526,
-54.74995));
#133346=CARTESIAN_POINT('',(-30.9564221286262,39.4558948199267,-52.64995));
#133347=CARTESIAN_POINT('Ctrl Pts',(-53.6173229282256,-36.0820590308261,
-55.74995));
#133348=CARTESIAN_POINT('Ctrl Pts',(-53.3164388612999,-36.78000002,-55.7499499999999));
#133349=CARTESIAN_POINT('Ctrl Pts',(-54.076473627675,-36.78000002,-55.74995));
#133350=CARTESIAN_POINT('Ctrl Pts',(-53.6173229109667,-36.0820590708605,
-55.5352328299022));
#133351=CARTESIAN_POINT('Ctrl Pts',(-53.3164388632929,-36.7800000140484,
-55.7160682965194));
#133352=CARTESIAN_POINT('Ctrl Pts',(-54.07647361027,-36.78000002,-55.6425914202082));
#133353=CARTESIAN_POINT('Ctrl Pts',(-53.587398316273,-36.1517305970246,
-55.3270423559178));
#133354=CARTESIAN_POINT('Ctrl Pts',(-53.3223470981189,-36.7637806572682,
-55.672084159207));
#133355=CARTESIAN_POINT('Ctrl Pts',(-54.0462927577141,-36.8151341090744,
-55.5384961709319));
#133356=CARTESIAN_POINT('Ctrl Pts',(-53.481339980492,-36.3953483985127,
-54.9914263135601));
#133357=CARTESIAN_POINT('Ctrl Pts',(-53.3111802821853,-36.783202746029,
-55.5229519438579));
#133358=CARTESIAN_POINT('Ctrl Pts',(-53.939326192416,-36.9379861363991,
-55.370688163807));
#133359=CARTESIAN_POINT('Ctrl Pts',(-53.4080974646291,-36.562334686105,
-54.8706857163843));
#133360=CARTESIAN_POINT('Ctrl Pts',(-53.293833750711,-36.8201344622738,
-55.429912748872));
#133361=CARTESIAN_POINT('Ctrl Pts',(-53.8654589377065,-37.0221914881654,
-55.3103188190833));
#133362=CARTESIAN_POINT('Ctrl Pts',(-53.3256899305316,-36.747133105635,
-54.8057004429533));
#133363=CARTESIAN_POINT('Ctrl Pts',(-53.2549772028899,-36.9057059891941,
-55.3509337052243));
#133364=CARTESIAN_POINT('Ctrl Pts',(-53.7823432375794,-37.1153847305999,
-55.2778252214766));
#133365=CARTESIAN_POINT('',(-54.076473627675,-36.78000002,-55.74995));
#133366=CARTESIAN_POINT('Origin',(-54.076473627675,-36.28000002,-55.74995));
#133367=CARTESIAN_POINT('Ctrl Pts',(-54.076473627675,-36.78000002,-55.74995));
#133368=CARTESIAN_POINT('Ctrl Pts',(-54.07647361027,-36.78000002,-55.6425914202082));
#133369=CARTESIAN_POINT('Ctrl Pts',(-54.0462927577141,-36.8151341090744,
-55.5384961709319));
#133370=CARTESIAN_POINT('Ctrl Pts',(-53.939326192416,-36.9379861363991,
-55.370688163807));
#133371=CARTESIAN_POINT('Ctrl Pts',(-53.8654589377065,-37.0221914881654,
-55.3103188190833));
#133372=CARTESIAN_POINT('Ctrl Pts',(-53.7823432375799,-37.1153847305994,
-55.2778252214768));
#133373=CARTESIAN_POINT('Origin',(-54.076473627675,-36.28000002,-55.24995));
#133374=CARTESIAN_POINT('',(-54.076473627675,-36.78000002,-60.42825533736));
#133375=CARTESIAN_POINT('Origin',(-54.076473627675,-36.28000002,-60.42825533736));
#133376=CARTESIAN_POINT('',(-54.076473627675,-36.78000002,-55.24995));
#133377=CARTESIAN_POINT('Origin',(0.,-12.9675000200281,-60.42825533736));
#133378=CARTESIAN_POINT('',(-55.5967474138374,-30.4937575588533,-60.8508735991007));
#133379=CARTESIAN_POINT('',(-53.5074514076768,-36.1001753985996,-60.8508735991007));
#133380=CARTESIAN_POINT('Origin',(0.,-12.9675000200281,-60.8508735991007));
#133381=CARTESIAN_POINT('Origin',(-52.5655138039885,-36.2558013973473,-60.449477355207));
#133382=CARTESIAN_POINT('Origin',(-54.5663882978998,-30.6330498593666,-60.4192568707561));
#133383=CARTESIAN_POINT('Origin',(-56.1762739063772,-30.63000002,-55.24995));
#133384=CARTESIAN_POINT('',(-56.1762739063771,-30.13000002,-55.74995));
#133385=CARTESIAN_POINT('Origin',(-56.1762739063772,-30.63000002,-55.74995));
#133386=CARTESIAN_POINT('',(-56.1762739063772,-30.13000002,-60.42825533736));
#133387=CARTESIAN_POINT('',(-56.1762739063772,-30.13000002,-55.24995));
#133388=CARTESIAN_POINT('Origin',(-56.1762739063772,-30.63000002,-60.42825533736));
#133389=CARTESIAN_POINT('Ctrl Pts',(-56.0013925566522,-29.4885226266656,
-54.74995));
#133390=CARTESIAN_POINT('Ctrl Pts',(-56.0013925566522,-29.4885226266655,
-55.2499499999999));
#133391=CARTESIAN_POINT('Ctrl Pts',(-56.4809591809864,-29.63000002,-55.24995));
#133392=CARTESIAN_POINT('Ctrl Pts',(-55.9637778607192,-29.6160253486821,
-54.7499500197391));
#133393=CARTESIAN_POINT('Ctrl Pts',(-55.9815963325889,-29.5556259878439,
-55.2320894585059));
#133394=CARTESIAN_POINT('Ctrl Pts',(-56.4430235619105,-29.6942952977694,
-55.24995));
#133395=CARTESIAN_POINT('Ctrl Pts',(-55.9259713199402,-29.7425201026704,
-54.7747042862246));
#133396=CARTESIAN_POINT('Ctrl Pts',(-55.9595264494602,-29.6302973578872,
-55.2276198610214));
#133397=CARTESIAN_POINT('Ctrl Pts',(-56.4048920758008,-29.7580863098899,
-55.2623271401185));
#133398=CARTESIAN_POINT('Ctrl Pts',(-55.8541342694537,-29.9801791700519,
-54.8719723798496));
#133399=CARTESIAN_POINT('Ctrl Pts',(-55.9152124797534,-29.7792875750423,
-55.2543206061649));
#133400=CARTESIAN_POINT('Ctrl Pts',(-56.3324398513309,-29.877933435243,
-55.3109611929186));
#133401=CARTESIAN_POINT('Ctrl Pts',(-55.8207323820705,-30.0892808127342,
-54.9437622390698));
#133402=CARTESIAN_POINT('Ctrl Pts',(-55.8932648786607,-29.8526235485765,
-55.2844345178149));
#133403=CARTESIAN_POINT('Ctrl Pts',(-56.2987519266105,-29.9329514036474,
-55.3468561181883));
#133404=CARTESIAN_POINT('Ctrl Pts',(-55.7350468385274,-30.3669899517508,
-55.2177384600888));
#133405=CARTESIAN_POINT('Ctrl Pts',(-55.8363250868006,-30.0417896984651,
-55.4221362713026));
#133406=CARTESIAN_POINT('Ctrl Pts',(-56.2123326186624,-30.0729950473548,
-55.4838442327376));
#133407=CARTESIAN_POINT('Ctrl Pts',(-55.699294301712,-30.4800318342627,
-55.4780587856325));
#133408=CARTESIAN_POINT('Ctrl Pts',(-55.8093485438182,-30.1300000005986,
-55.5818806132723));
#133409=CARTESIAN_POINT('Ctrl Pts',(-56.1762739146114,-30.1300000200003,
-55.614004390749));
#133410=CARTESIAN_POINT('Ctrl Pts',(-55.6992942935022,-30.4800318603742,
-55.74995));
#133411=CARTESIAN_POINT('Ctrl Pts',(-55.8093485379488,-30.1300000200003,
-55.7499499999999));
#133412=CARTESIAN_POINT('Ctrl Pts',(-56.1762739063772,-30.1300000200003,
-55.74995));
#133413=CARTESIAN_POINT('',(-56.4809591809864,-29.63000002,-55.24995));
#133414=CARTESIAN_POINT('Origin',(-56.4809591809864,-29.63000002,-54.74995));
#133415=CARTESIAN_POINT('Ctrl Pts',(-56.4809591809864,-29.63000002,-55.24995));
#133416=CARTESIAN_POINT('Ctrl Pts',(-56.4430235619105,-29.6942952977694,
-55.24995));
#133417=CARTESIAN_POINT('Ctrl Pts',(-56.4048920758008,-29.7580863098899,
-55.2623271401185));
#133418=CARTESIAN_POINT('Ctrl Pts',(-56.3324398513309,-29.877933435243,
-55.3109611929186));
#133419=CARTESIAN_POINT('Ctrl Pts',(-56.2987519266105,-29.9329514036474,
-55.3468561181883));
#133420=CARTESIAN_POINT('Ctrl Pts',(-56.2123326186624,-30.0729950473548,
-55.4838442327376));
#133421=CARTESIAN_POINT('Ctrl Pts',(-56.1762739146114,-30.1300000200003,
-55.614004390749));
#133422=CARTESIAN_POINT('Ctrl Pts',(-56.1762739063771,-30.13000002,-55.74995));
#133423=CARTESIAN_POINT('Origin',(0.,-12.9675000200281,-54.74995));
#133424=CARTESIAN_POINT('',(-56.6260651114328,-29.13000002,-55.24995));
#133425=CARTESIAN_POINT('Origin',(-56.6260651114328,-29.13000002,-54.74995));
#133426=CARTESIAN_POINT('Origin',(0.,-12.9675000200281,-55.24995));
#133427=CARTESIAN_POINT('Ctrl Pts',(-56.418846619879,-28.0012587761031,
-55.74995));
#133428=CARTESIAN_POINT('Ctrl Pts',(-56.2513078496445,-28.6300000199999,
-55.74995));
#133429=CARTESIAN_POINT('Ctrl Pts',(-56.9019881023868,-28.63000002,-55.74995));
#133430=CARTESIAN_POINT('Ctrl Pts',(-56.4188466136678,-28.0012587994123,
-55.6168335059946));
#133431=CARTESIAN_POINT('Ctrl Pts',(-56.2513078484208,-28.6300000235388,
-55.7066092661189));
#133432=CARTESIAN_POINT('Ctrl Pts',(-56.9019880961229,-28.63000002,-55.6833917541491));
#133433=CARTESIAN_POINT('Ctrl Pts',(-56.4116877572674,-28.0281919581543,
-55.4831809085995));
#133434=CARTESIAN_POINT('Ctrl Pts',(-56.2500205046201,-28.6336048267405,
-55.662915181482));
#133435=CARTESIAN_POINT('Ctrl Pts',(-56.8947679354133,-28.6435819282218,
-55.6165654527396));
#133436=CARTESIAN_POINT('Ctrl Pts',(-56.3842918802123,-28.1304346451459,
-55.2389052692862));
#133437=CARTESIAN_POINT('Ctrl Pts',(-56.2435792593614,-28.6535512137473,
-55.5706051556274));
#133438=CARTESIAN_POINT('Ctrl Pts',(-56.8671374536179,-28.6951410554417,
-55.4944276362032));
#133439=CARTESIAN_POINT('Ctrl Pts',(-56.3639882171558,-28.2059422564823,
-55.1276612780425));
#133440=CARTESIAN_POINT('Ctrl Pts',(-56.2384193392041,-28.6700167701719,
-55.5221237308774));
#133441=CARTESIAN_POINT('Ctrl Pts',(-56.8466599215264,-28.733218160043,
-55.438805637664));
#133442=CARTESIAN_POINT('Ctrl Pts',(-56.313802009893,-28.3903724090483,
-54.9450496744345));
#133443=CARTESIAN_POINT('Ctrl Pts',(-56.2221065093684,-28.7248002564605,
-55.4263976661905));
#133444=CARTESIAN_POINT('Ctrl Pts',(-56.7960439448031,-28.8262229205127,
-55.3474998385745));
#133445=CARTESIAN_POINT('Ctrl Pts',(-56.2834891741183,-28.5008198383441,
-54.8722499675113));
#133446=CARTESIAN_POINT('Ctrl Pts',(-56.2109691262328,-28.7630648267862,
-55.3789982403422));
#133447=CARTESIAN_POINT('Ctrl Pts',(-56.7654715266632,-28.8819195410099,
-55.3110999839041));
#133448=CARTESIAN_POINT('Ctrl Pts',(-56.2177799652687,-28.7369766748766,
-54.7752816287617));
#133449=CARTESIAN_POINT('Ctrl Pts',(-56.1824656282838,-28.8623399510796,
-55.300226361809));
#133450=CARTESIAN_POINT('Ctrl Pts',(-56.6991996177705,-29.0010091208419,
-55.2626158142325));
#133451=CARTESIAN_POINT('Ctrl Pts',(-56.1815764992065,-28.8655539935311,
-54.749950013458));
#133452=CARTESIAN_POINT('Ctrl Pts',(-56.1650303807126,-28.9235240815735,
-55.2679072059029));
#133453=CARTESIAN_POINT('Ctrl Pts',(-56.6626879858136,-29.0658450537332,
-55.24995));
#133454=CARTESIAN_POINT('Ctrl Pts',(-56.1452664265556,-28.9927680098115,
-54.74995));
#133455=CARTESIAN_POINT('Ctrl Pts',(-56.1452664265556,-28.9927680098115,
-55.24995));
#133456=CARTESIAN_POINT('Ctrl Pts',(-56.6260651114328,-29.1300000200001,
-55.24995));
#133457=CARTESIAN_POINT('',(-56.9019881023868,-28.63000002,-55.74995));
#133458=CARTESIAN_POINT('Origin',(-56.9019881023868,-28.13000002,-55.74995));
#133459=CARTESIAN_POINT('Ctrl Pts',(-56.9019881023868,-28.63000002,-55.74995));
#133460=CARTESIAN_POINT('Ctrl Pts',(-56.9019880961229,-28.63000002,-55.6833917541491));
#133461=CARTESIAN_POINT('Ctrl Pts',(-56.8947679354133,-28.6435819282218,
-55.6165654527396));
#133462=CARTESIAN_POINT('Ctrl Pts',(-56.8671374536179,-28.6951410554417,
-55.4944276362032));
#133463=CARTESIAN_POINT('Ctrl Pts',(-56.8466599215264,-28.733218160043,
-55.438805637664));
#133464=CARTESIAN_POINT('Ctrl Pts',(-56.7960439448031,-28.8262229205127,
-55.3474998385745));
#133465=CARTESIAN_POINT('Ctrl Pts',(-56.7654715266632,-28.8819195410099,
-55.3110999839041));
#133466=CARTESIAN_POINT('Ctrl Pts',(-56.6991996177705,-29.0010091208419,
-55.2626158142325));
#133467=CARTESIAN_POINT('Ctrl Pts',(-56.6626879858136,-29.0658450537332,
-55.24995));
#133468=CARTESIAN_POINT('Ctrl Pts',(-56.6260651114328,-29.13000002,-55.24995));
#133469=CARTESIAN_POINT('Origin',(-56.9019881023868,-28.13000002,-55.24995));
#133470=CARTESIAN_POINT('',(-56.9019881023868,-28.63000002,-60.42825533736));
#133471=CARTESIAN_POINT('Origin',(-56.9019881023868,-28.13000002,-60.42825533736));
#133472=CARTESIAN_POINT('',(-56.9019881023868,-28.63000002,-55.24995));
#133473=CARTESIAN_POINT('Origin',(0.,-12.9675000200281,-60.42825533736));
#133474=CARTESIAN_POINT('',(-57.5245249214072,-22.4066238608121,-60.8508735991007));
#133475=CARTESIAN_POINT('',(-56.3187331343194,-28.0130417005584,-60.8508735991007));
#133476=CARTESIAN_POINT('Origin',(0.,-12.9675000200281,-60.8508735991007));
#133477=CARTESIAN_POINT('Origin',(-55.0588362446609,-28.1616614222003,-60.3670915993992));
#133478=CARTESIAN_POINT('Origin',(-56.5772574599055,-22.4805096121333,-60.4242148671621));
#133479=CARTESIAN_POINT('Origin',(-58.1141118834647,-22.48000002,-55.24995));
#133480=CARTESIAN_POINT('',(-58.1141118834647,-21.98000002,-60.42825533736));
#133481=CARTESIAN_POINT('Origin',(-58.1141118834647,-22.48000002,-60.42825533736));
#133482=CARTESIAN_POINT('',(-58.1141118834537,-21.9800000069849,-55.913606468422));
#133483=CARTESIAN_POINT('Origin',(-58.1141118834647,-22.48000002,-55.9136064684106));
#133484=CARTESIAN_POINT('',(-58.1141118834647,-21.98000002,-55.24995));
#133485=CARTESIAN_POINT('Ctrl Pts',(-57.7689991024638,-21.4435190710229,
-54.8883584020538));
#133486=CARTESIAN_POINT('Ctrl Pts',(-57.7681097820422,-21.4495803068843,
-55.2303260732311));
#133487=CARTESIAN_POINT('Ctrl Pts',(-58.0831736437665,-21.4980516416407,
-55.3542805420643));
#133488=CARTESIAN_POINT('Ctrl Pts',(-57.7500908600563,-21.5723897392102,
-54.8860050875463));
#133489=CARTESIAN_POINT('Ctrl Pts',(-57.7561082976293,-21.5312836766001,
-55.2240269539559));
#133490=CARTESIAN_POINT('Ctrl Pts',(-58.0674311963076,-21.5630475770342,
-55.3506990738629));
#133491=CARTESIAN_POINT('Ctrl Pts',(-57.7304928612488,-21.702757912867,
-54.9116382623115));
#133492=CARTESIAN_POINT('Ctrl Pts',(-57.7435735661121,-21.6157110452939,
-55.2378962877635));
#133493=CARTESIAN_POINT('Ctrl Pts',(-58.0543804972822,-21.6287810566872,
-55.3623310903062));
#133494=CARTESIAN_POINT('Ctrl Pts',(-57.6941246628956,-21.9398194436421,
-55.0150801896028));
#133495=CARTESIAN_POINT('Ctrl Pts',(-57.720944678806,-21.7667785312353,
-55.3041336540307));
#133496=CARTESIAN_POINT('Ctrl Pts',(-58.0368385085867,-21.7483268550824,
-55.4143541528288));
#133497=CARTESIAN_POINT('Ctrl Pts',(-57.6771952780886,-22.0476481665544,
-55.0933432841215));
#133498=CARTESIAN_POINT('Ctrl Pts',(-57.7106605173207,-21.8347350541072,
-55.3571283178239));
#133499=CARTESIAN_POINT('Ctrl Pts',(-58.0322828839583,-21.8027029130102,
-55.4549704742887));
#133500=CARTESIAN_POINT('Ctrl Pts',(-57.6494812249724,-22.2219724523816,
-55.2860232465006));
#133501=CARTESIAN_POINT('Ctrl Pts',(-57.695076042676,-21.9376161761805,
-55.488705776954));
#133502=CARTESIAN_POINT('Ctrl Pts',(-58.0344578164564,-21.8906114651791,
-55.5576238485917));
#133503=CARTESIAN_POINT('Ctrl Pts',(-57.6385084201743,-22.2897585279143,
-55.4017143890713));
#133504=CARTESIAN_POINT('Ctrl Pts',(-57.6896470027836,-21.9734580917706,
-55.5692031110363));
#133505=CARTESIAN_POINT('Ctrl Pts',(-58.0412481050148,-21.9247947465257,
-55.6203478572209));
#133506=CARTESIAN_POINT('Ctrl Pts',(-57.6241589914286,-22.3780503291714,
-55.6490268368888));
#133507=CARTESIAN_POINT('Ctrl Pts',(-57.6849292160896,-22.0058199931385,
-55.7382976471412));
#133508=CARTESIAN_POINT('Ctrl Pts',(-58.0678405993018,-21.9693186886025,
-55.7585030512593));
#133509=CARTESIAN_POINT('Ctrl Pts',(-57.6206785404325,-22.3992316104322,
-55.7821117710573));
#133510=CARTESIAN_POINT('Ctrl Pts',(-57.6857286259381,-22.0018252542719,
-55.8292768225565));
#133511=CARTESIAN_POINT('Ctrl Pts',(-58.0878569699436,-21.9800000199996,
-55.8347456438184));
#133512=CARTESIAN_POINT('Ctrl Pts',(-57.6206785412152,-22.3992316056509,
-55.9136064684106));
#133513=CARTESIAN_POINT('Ctrl Pts',(-57.6893011240825,-21.9800000200013,
-55.9136064684131));
#133514=CARTESIAN_POINT('Ctrl Pts',(-58.1141118834632,-21.98000002,-55.9136064684135));
#133515=CARTESIAN_POINT('',(-58.0831736436651,-21.4980516422417,-55.3542805420483));
#133516=CARTESIAN_POINT('Origin',(-58.2637025843942,-21.516103263282,-54.8883584020538));
#133517=CARTESIAN_POINT('Ctrl Pts',(-58.0831736437664,-21.4980516416407,
-55.3542805420642));
#133518=CARTESIAN_POINT('Ctrl Pts',(-58.0674311963076,-21.5630475770342,
-55.3506990738629));
#133519=CARTESIAN_POINT('Ctrl Pts',(-58.0543804972822,-21.6287810566872,
-55.3623310903062));
#133520=CARTESIAN_POINT('Ctrl Pts',(-58.0368385085867,-21.7483268550824,
-55.4143541528288));
#133521=CARTESIAN_POINT('Ctrl Pts',(-58.0322828839583,-21.8027029130102,
-55.4549704742887));
#133522=CARTESIAN_POINT('Ctrl Pts',(-58.0344578164564,-21.8906114651791,
-55.5576238485917));
#133523=CARTESIAN_POINT('Ctrl Pts',(-58.0412481050148,-21.9247947465257,
-55.6203478572209));
#133524=CARTESIAN_POINT('Ctrl Pts',(-58.0678405993018,-21.9693186886025,
-55.7585030512593));
#133525=CARTESIAN_POINT('Ctrl Pts',(-58.0878569699436,-21.9800000199996,
-55.8347456438184));
#133526=CARTESIAN_POINT('Ctrl Pts',(-58.1141118834578,-21.98000002,-55.9136064684144));
#133527=CARTESIAN_POINT('Ctrl Pts',(-57.8394345625603,-20.9487258492223,
-54.8970741880307));
#133528=CARTESIAN_POINT('Ctrl Pts',(-57.8386732172432,-20.9542432701794,
-55.231054762791));
#133529=CARTESIAN_POINT('Ctrl Pts',(-58.1440639002148,-20.9985364556095,
-55.3589167601806));
#133530=CARTESIAN_POINT('Ctrl Pts',(-57.8166617235658,-21.1137591610236,
-54.8942721021231));
#133531=CARTESIAN_POINT('Ctrl Pts',(-57.8158059697179,-21.1198442176538,
-55.2308230742677));
#133532=CARTESIAN_POINT('Ctrl Pts',(-58.124377168252,-21.1650956023415,
-55.357473843553));
#133533=CARTESIAN_POINT('Ctrl Pts',(-57.7931832180155,-21.2786902591483,
-54.8913683748515));
#133534=CARTESIAN_POINT('Ctrl Pts',(-57.7922771725925,-21.2849855841189,
-55.2305804544121));
#133535=CARTESIAN_POINT('Ctrl Pts',(-58.1040803997663,-21.3315995267041,
-55.3559321998119));
#133536=CARTESIAN_POINT('Ctrl Pts',(-57.7689991024637,-21.4435190710235,
-54.8883584020537));
#133537=CARTESIAN_POINT('Ctrl Pts',(-57.7681097820422,-21.4495803068845,
-55.2303260732311));
#133538=CARTESIAN_POINT('Ctrl Pts',(-58.0831736437665,-21.4980516416408,
-55.3542805420642));
#133539=CARTESIAN_POINT('',(-58.1440636542725,-20.9985364317146,-55.3589173554775));
#133540=CARTESIAN_POINT('Origin',(-58.3347412169172,-21.017072891219,-54.8970741880307));
#133541=CARTESIAN_POINT('Origin',(8.40472652016414,-13.0339084621842,-43.9483258606649));
#133542=CARTESIAN_POINT('Ctrl Pts',(-57.970850887931,-19.9304072883579,
-56.2895381767097));
#133543=CARTESIAN_POINT('Ctrl Pts',(-57.8976234932917,-20.54001496768,-56.2187331880681));
#133544=CARTESIAN_POINT('Ctrl Pts',(-58.5127149485701,-20.4849816559984,
-56.2328156683283));
#133545=CARTESIAN_POINT('Ctrl Pts',(-57.9735750287413,-19.9074135537666,
-56.0766526555005));
#133546=CARTESIAN_POINT('Ctrl Pts',(-57.9072350111286,-20.4617756146749,
-56.1016741619115));
#133547=CARTESIAN_POINT('Ctrl Pts',(-58.4599257443274,-20.4734298477889,
-56.0837094320831));
#133548=CARTESIAN_POINT('Ctrl Pts',(-57.9717019896149,-19.9235035634186,
-55.8706894656042));
#133549=CARTESIAN_POINT('Ctrl Pts',(-57.9119143840911,-20.421400833978,
-55.9614017711877));
#133550=CARTESIAN_POINT('Ctrl Pts',(-58.4131413827532,-20.4815791649057,
-55.9505952646837));
#133551=CARTESIAN_POINT('Ctrl Pts',(-57.9585693859923,-20.0319506515215,
-55.5325899309841));
#133552=CARTESIAN_POINT('Ctrl Pts',(-57.9099424206244,-20.4307035336697,
-55.7218311799895));
#133553=CARTESIAN_POINT('Ctrl Pts',(-58.337292873758,-20.5363048245876,
-55.740436199424));
#133554=CARTESIAN_POINT('Ctrl Pts',(-57.9502161720285,-20.1005973934661,
-55.4004673410398));
#133555=CARTESIAN_POINT('Ctrl Pts',(-57.9064615881784,-20.4555454071529,
-55.6247135460827));
#133556=CARTESIAN_POINT('Ctrl Pts',(-58.3079048908359,-20.5709315394046,
-55.6609486926888));
#133557=CARTESIAN_POINT('Ctrl Pts',(-57.9331286547812,-20.2376361665866,
-55.2282616560402));
#133558=CARTESIAN_POINT('Ctrl Pts',(-57.897198940496,-20.5238155454433,
-55.4956413947157));
#133559=CARTESIAN_POINT('Ctrl Pts',(-58.2667283591981,-20.6400407226598,
-55.5584509242662));
#133560=CARTESIAN_POINT('Ctrl Pts',(-57.9265619920107,-20.2898468150981,
-55.1744487967193));
#133561=CARTESIAN_POINT('Ctrl Pts',(-57.8934360858788,-20.5517279947688,
-55.4549818870893));
#133562=CARTESIAN_POINT('Ctrl Pts',(-58.2532825451019,-20.6663690401879,
-55.5266431857194));
#133563=CARTESIAN_POINT('Ctrl Pts',(-57.9122860844342,-20.4019110441904,
-55.0807659948788));
#133564=CARTESIAN_POINT('Ctrl Pts',(-57.8849186400004,-20.6149205916457,
-55.3834750893986));
#133565=CARTESIAN_POINT('Ctrl Pts',(-58.2280408271646,-20.7228767370785,
-55.4713148466751));
#133566=CARTESIAN_POINT('Ctrl Pts',(-57.9045197753069,-20.4622337862451,
-55.0401096877444));
#133567=CARTESIAN_POINT('Ctrl Pts',(-57.8801386015543,-20.6503866910324,
-55.3518324750308));
#133568=CARTESIAN_POINT('Ctrl Pts',(-58.2160717164706,-20.753292731466,
-55.4473281588797));
#133569=CARTESIAN_POINT('Ctrl Pts',(-57.8723006909993,-20.7089850131959,
-54.9109039511417));
#133570=CARTESIAN_POINT('Ctrl Pts',(-57.8601439921696,-20.7981658738856,
-55.250541365782));
#133571=CARTESIAN_POINT('Ctrl Pts',(-58.1723605376483,-20.8777067919942,
-55.3705177858243));
#133572=CARTESIAN_POINT('Ctrl Pts',(-57.8438584328939,-20.9197294286556,
-54.8734589342148));
#133573=CARTESIAN_POINT('Ctrl Pts',(-57.8415274164302,-20.9345476815752,
-55.214451085197));
#133574=CARTESIAN_POINT('Ctrl Pts',(-58.145173752928,-20.9839602690723,
-55.346687116762));
#133575=CARTESIAN_POINT('Ctrl Pts',(-57.8147273601029,-21.1255768370871,
-54.9117960309513));
#133576=CARTESIAN_POINT('Ctrl Pts',(-57.8228292490717,-21.0682703109648,
-55.236394534989));
#133577=CARTESIAN_POINT('Ctrl Pts',(-58.1259919089073,-21.0877309864276,
-55.3639580518367));
#133578=CARTESIAN_POINT('',(-58.4684744114517,-20.4800000236652,-56.1088024963483));
#133579=CARTESIAN_POINT('Origin',(-58.4684744114614,-19.98000002,-56.108802496345));
#133580=CARTESIAN_POINT('Ctrl Pts',(-58.4684744114466,-20.4800000273303,
-56.1088024963493));
#133581=CARTESIAN_POINT('Ctrl Pts',(-58.4560594229943,-20.4800036500033,
-56.0736749117289));
#133582=CARTESIAN_POINT('Ctrl Pts',(-58.4439350613241,-20.4813472561768,
-56.0394507359076));
#133583=CARTESIAN_POINT('Ctrl Pts',(-58.4320811979818,-20.4840487563327,
-56.0060462075256));
#133584=CARTESIAN_POINT('Ctrl Pts',(-58.421086555275,-20.4865544397651,
-55.9750629876465));
#133585=CARTESIAN_POINT('Ctrl Pts',(-58.4103249292896,-20.4902278471488,
-55.9447835971118));
#133586=CARTESIAN_POINT('Ctrl Pts',(-58.3997538039955,-20.4951176237352,
-55.9151358942012));
#133587=CARTESIAN_POINT('Ctrl Pts',(-58.3897209301719,-20.4997584268807,
-55.8869977675415));
#133588=CARTESIAN_POINT('Ctrl Pts',(-58.3798599201571,-20.5054949994344,
-55.8594274183296));
#133589=CARTESIAN_POINT('Ctrl Pts',(-58.3701054711661,-20.5124031604037,
-55.8323759729964));
#133590=CARTESIAN_POINT('Ctrl Pts',(-58.369582156849,-20.5127737748324,
-55.8309246958763));
#133591=CARTESIAN_POINT('Ctrl Pts',(-58.3690591414204,-20.5131477694283,
-55.8294749181168));
#133592=CARTESIAN_POINT('Ctrl Pts',(-58.3685364120709,-20.5135251586298,
-55.8280266343692));
#133593=CARTESIAN_POINT('Ctrl Pts',(-58.355322598113,-20.5230649916293,
-55.7914161933879));
#133594=CARTESIAN_POINT('Ctrl Pts',(-58.3424819682759,-20.5346544306425,
-55.7562349549661));
#133595=CARTESIAN_POINT('Ctrl Pts',(-58.3300197127882,-20.5482894757852,
-55.7226770371038));
#133596=CARTESIAN_POINT('Ctrl Pts',(-58.3189876225659,-20.5603597666202,
-55.6929702173479));
#133597=CARTESIAN_POINT('Ctrl Pts',(-58.3082519351362,-20.5740337277965,
-55.6645352898577));
#133598=CARTESIAN_POINT('Ctrl Pts',(-58.297793069529,-20.5892884176472,
-55.6375339573335));
#133599=CARTESIAN_POINT('Ctrl Pts',(-58.2918114955221,-20.5980127917543,
-55.622091511198));
#133600=CARTESIAN_POINT('Ctrl Pts',(-58.2859200261619,-20.6072537934279,
-55.6071185210319));
#133601=CARTESIAN_POINT('Ctrl Pts',(-58.2801113530785,-20.6170020227668,
-55.5926500177757));
#133602=CARTESIAN_POINT('Ctrl Pts',(-58.2739672932451,-20.6273131047414,
-55.5773461181711));
#133603=CARTESIAN_POINT('Ctrl Pts',(-58.2678869023947,-20.638271485625,
-55.562504370203));
#133604=CARTESIAN_POINT('Ctrl Pts',(-58.2619058079972,-20.6497784634518,
-55.5483031281744));
#133605=CARTESIAN_POINT('Ctrl Pts',(-58.2559442889337,-20.6612477804562,
-55.5341483649398));
#133606=CARTESIAN_POINT('Ctrl Pts',(-58.2500813442384,-20.6732615002889,
-55.5206307132331));
#133607=CARTESIAN_POINT('Ctrl Pts',(-58.2443734669305,-20.6856843380992,
-55.5078979452598));
#133608=CARTESIAN_POINT('Ctrl Pts',(-58.2430208618868,-20.6886281983423,
-55.5048806403578));
#133609=CARTESIAN_POINT('Ctrl Pts',(-58.2416770603513,-20.6915948918065,
-55.5019072550467));
#133610=CARTESIAN_POINT('Ctrl Pts',(-58.2403429914197,-20.6945823753937,
-55.4989794498912));
#133611=CARTESIAN_POINT('Ctrl Pts',(-58.2336464050011,-20.7095785585306,
-55.4842828328155));
#133612=CARTESIAN_POINT('Ctrl Pts',(-58.2271276542843,-20.7251842455087,
-55.4706315466689));
#133613=CARTESIAN_POINT('Ctrl Pts',(-58.2207713165789,-20.7414257608518,
-55.4580213750816));
#133614=CARTESIAN_POINT('Ctrl Pts',(-58.2151565865895,-20.7557723433489,
-55.4468824595826));
#133615=CARTESIAN_POINT('Ctrl Pts',(-58.2096680821563,-20.7706159767222,
-55.4365563660369));
#133616=CARTESIAN_POINT('Ctrl Pts',(-58.2042768588887,-20.7859705675371,
-55.4270685753685));
#133617=CARTESIAN_POINT('Ctrl Pts',(-58.1969328174058,-20.8068869247906,
-55.4141441007564));
#133618=CARTESIAN_POINT('Ctrl Pts',(-58.1898412601343,-20.828523501731,
-55.40291734747));
#133619=CARTESIAN_POINT('Ctrl Pts',(-58.1830505367822,-20.8507355057842,
-55.3934981904853));
#133620=CARTESIAN_POINT('Ctrl Pts',(-58.1765582690219,-20.871971281464,
-55.3844930100279));
#133621=CARTESIAN_POINT('Ctrl Pts',(-58.1703405182628,-20.8937334832869,
-55.3771411838376));
#133622=CARTESIAN_POINT('Ctrl Pts',(-58.164427550618,-20.9158503556191,
-55.3715356173205));
#133623=CARTESIAN_POINT('Ctrl Pts',(-58.1587702929555,-20.937010769981,
-55.3661724670316));
#133624=CARTESIAN_POINT('Ctrl Pts',(-58.1533916071063,-20.9584955938527,
-55.3624089485159));
#133625=CARTESIAN_POINT('Ctrl Pts',(-58.1483130703003,-20.9801107627175,
-55.3603068684826));
#133626=CARTESIAN_POINT('Ctrl Pts',(-58.1468720340706,-20.9862440728885,
-55.3597104026891));
#133627=CARTESIAN_POINT('Ctrl Pts',(-58.1454551536744,-20.9923876162956,
-55.3592475231078));
#133628=CARTESIAN_POINT('Ctrl Pts',(-58.1440629164629,-20.9985363600311,
-55.358919141335));
#133629=CARTESIAN_POINT('Origin',(-58.4684744114614,-19.98000002,-55.24995));
#133630=CARTESIAN_POINT('',(-58.4684744114614,-20.48000002,-60.42825533736));
#133631=CARTESIAN_POINT('Origin',(-58.4684744114614,-19.98000002,-60.42825533736));
#133632=CARTESIAN_POINT('',(-58.4684744114614,-20.48000002,-55.24995));
#133633=CARTESIAN_POINT('Origin',(0.,-12.9675000200281,-60.42825533736));
#133634=CARTESIAN_POINT('',(-58.2781275348581,-14.3194901627709,-60.8508735991007));
#133635=CARTESIAN_POINT('',(-57.8770125754992,-19.9259080025173,-60.8508735991007));
#133636=CARTESIAN_POINT('Origin',(0.,-12.9675000200281,-60.8508735991007));
#133637=CARTESIAN_POINT('Origin',(-56.5152414274053,-20.0041958453797,-60.331554578498));
#133638=CARTESIAN_POINT('Origin',(-57.3724390589806,-14.3298873277334,-60.4282477713549));
#133639=CARTESIAN_POINT('Origin',(-58.871735578318,-14.33000002,-55.24995));
#133640=CARTESIAN_POINT('',(-58.871735578318,-13.83000002,-60.42825533736));
#133641=CARTESIAN_POINT('Origin',(-58.871735578318,-14.33000002,-60.42825533736));
#133642=CARTESIAN_POINT('',(-58.871735578318,-13.83000002,-56.2531111209796));
#133643=CARTESIAN_POINT('Origin',(-58.871735578318,-14.33000002,-56.2531111209796));
#133644=CARTESIAN_POINT('',(-58.871735578318,-13.83000002,-55.24995));
#133645=CARTESIAN_POINT('Ctrl Pts',(-58.3870336823786,-13.1950672036472,
-54.9735905576542));
#133646=CARTESIAN_POINT('Ctrl Pts',(-58.386666124584,-13.2389284460928,
-55.245469113786));
#133647=CARTESIAN_POINT('Ctrl Pts',(-58.6192838059339,-13.2635419343739,
-55.3905548168058));
#133648=CARTESIAN_POINT('Ctrl Pts',(-58.3863638568524,-13.3879941755922,
-54.9394842857217));
#133649=CARTESIAN_POINT('Ctrl Pts',(-58.3860638311514,-13.3687276186212,
-55.2176214035434));
#133650=CARTESIAN_POINT('Ctrl Pts',(-58.613439068509,-13.3607847257335,
-55.3701021803697));
#133651=CARTESIAN_POINT('Ctrl Pts',(-58.3844076455848,-13.5917447402541,
-54.9813451387709));
#133652=CARTESIAN_POINT('Ctrl Pts',(-58.3849151617365,-13.5088631788445,
-55.251799877981));
#133653=CARTESIAN_POINT('Ctrl Pts',(-58.6183088754593,-13.4634772759073,
-55.3945154239426));
#133654=CARTESIAN_POINT('Ctrl Pts',(-58.3803446492905,-13.8907806579908,
-55.1547248800286));
#133655=CARTESIAN_POINT('Ctrl Pts',(-58.3829868535489,-13.7025366763559,
-55.3887548371216));
#133656=CARTESIAN_POINT('Ctrl Pts',(-58.6446085400692,-13.614195445683,
-55.5000130596728));
#133657=CARTESIAN_POINT('Ctrl Pts',(-58.3784003210709,-14.0018139117568,
-55.2630289365479));
#133658=CARTESIAN_POINT('Ctrl Pts',(-58.3821831638283,-13.7708280924458,
-55.4756863263615));
#133659=CARTESIAN_POINT('Ctrl Pts',(-58.6620402598172,-13.6701578227605,
-55.566624268873));
#133660=CARTESIAN_POINT('Ctrl Pts',(-58.3751346753983,-14.1721093492982,
-55.5158238508396));
#133661=CARTESIAN_POINT('Ctrl Pts',(-58.3811829168127,-13.8615332852492,
-55.675485688548));
#133662=CARTESIAN_POINT('Ctrl Pts',(-58.7077104063222,-13.7559878496911,
-55.7281943165199));
#133663=CARTESIAN_POINT('Ctrl Pts',(-58.3738439529203,-14.2307758203948,
-55.6580834410202));
#133664=CARTESIAN_POINT('Ctrl Pts',(-58.3810074666823,-13.8830868568037,
-55.788873845676));
#133665=CARTESIAN_POINT('Ctrl Pts',(-58.7356377641522,-13.7855551979282,
-55.8218169965321));
#133666=CARTESIAN_POINT('Ctrl Pts',(-58.371968604942,-14.3149917907957,
-55.9950091948521));
#133667=CARTESIAN_POINT('Ctrl Pts',(-58.3813969201454,-13.8862626584142,
-56.0560043903553));
#133668=CARTESIAN_POINT('Ctrl Pts',(-58.8084294771009,-13.8279974118869,
-56.0558032453046));
#133669=CARTESIAN_POINT('Ctrl Pts',(-58.371685997399,-14.3259563616536,
-56.1910588010128));
#133670=CARTESIAN_POINT('Ctrl Pts',(-58.3822444492649,-13.8506911564217,
-56.212199449184));
#133671=CARTESIAN_POINT('Ctrl Pts',(-58.855449162814,-13.8335191345168,
-56.2004791098763));
#133672=CARTESIAN_POINT('Ctrl Pts',(-58.3719493412616,-14.3151650612744,
-56.3903791996399));
#133673=CARTESIAN_POINT('Ctrl Pts',(-58.3834300043284,-13.791901460541,
-56.360880747514));
#133674=CARTESIAN_POINT('Ctrl Pts',(-58.9064235376792,-13.8280751907923,
-56.3623652529328));
#133675=CARTESIAN_POINT('',(-58.6168863951182,-13.3313694067285,-55.3834094543327));
#133676=CARTESIAN_POINT('Origin',(-58.8863673263393,-13.3327387922841,-54.9622468511542));
#133677=CARTESIAN_POINT('Ctrl Pts',(-58.6168867413708,-13.3313694084883,
-55.383408913088));
#133678=CARTESIAN_POINT('Ctrl Pts',(-58.6166911469594,-13.3517892137721,
-55.3833501769659));
#133679=CARTESIAN_POINT('Ctrl Pts',(-58.6169551454442,-13.3722412722744,
-55.3850753059523));
#133680=CARTESIAN_POINT('Ctrl Pts',(-58.6176634841287,-13.3924918963401,
-55.3885601063615));
#133681=CARTESIAN_POINT('Ctrl Pts',(-58.6183725932892,-13.4127645474659,
-55.3920486972666));
#133682=CARTESIAN_POINT('Ctrl Pts',(-58.6195270688617,-13.4328341668126,
-55.3973004085694));
#133683=CARTESIAN_POINT('Ctrl Pts',(-58.6211188739901,-13.4524818769443,
-55.4042414350838));
#133684=CARTESIAN_POINT('Ctrl Pts',(-58.6227236599655,-13.4722898101543,
-55.4112390642571));
#133685=CARTESIAN_POINT('Ctrl Pts',(-58.6247730789981,-13.4916679682566,
-55.4199529583737));
#133686=CARTESIAN_POINT('Ctrl Pts',(-58.627264754533,-13.5104240755455,
-55.4302654575736));
#133687=CARTESIAN_POINT('Ctrl Pts',(-58.6290008545194,-13.5234925819195,
-55.4374507950986));
#133688=CARTESIAN_POINT('Ctrl Pts',(-58.6309517906365,-13.536259812243,
-55.4454112967302));
#133689=CARTESIAN_POINT('Ctrl Pts',(-58.6331177534659,-13.548672905394,
-55.4540985105411));
#133690=CARTESIAN_POINT('Ctrl Pts',(-58.6364466735685,-13.567750885295,
-55.4674500973265));
#133691=CARTESIAN_POINT('Ctrl Pts',(-58.6402780389743,-13.5860620622833,
-55.4825567103882));
#133692=CARTESIAN_POINT('Ctrl Pts',(-58.6446041270825,-13.6034603706004,
-55.499260499199));
#133693=CARTESIAN_POINT('Ctrl Pts',(-58.6489851274684,-13.6210795206375,
-55.5161763139942));
#133694=CARTESIAN_POINT('Ctrl Pts',(-58.6538736776085,-13.6377624792879,
-55.5347290400659));
#133695=CARTESIAN_POINT('Ctrl Pts',(-58.6592563987165,-13.6534107023946,
-55.5547469245073));
#133696=CARTESIAN_POINT('Ctrl Pts',(-58.6647747031922,-13.6694530827954,
-55.5752690320232));
#133697=CARTESIAN_POINT('Ctrl Pts',(-58.670812549364,-13.6844082085566,
-55.5973300534321));
#133698=CARTESIAN_POINT('Ctrl Pts',(-58.6773471776121,-13.6982235274118,
-55.6207527017991));
#133699=CARTESIAN_POINT('Ctrl Pts',(-58.6797711272743,-13.7033481704979,
-55.629441079843));
#133700=CARTESIAN_POINT('Ctrl Pts',(-58.6822633392963,-13.7083164773331,
-55.6383169613905));
#133701=CARTESIAN_POINT('Ctrl Pts',(-58.6848223131132,-13.7131274153225,
-55.6473719395789));
#133702=CARTESIAN_POINT('Ctrl Pts',(-58.6917189083808,-13.7260931955708,
-55.6717756749011));
#133703=CARTESIAN_POINT('Ctrl Pts',(-58.6990713849487,-13.7378634833018,
-55.697382248317));
#133704=CARTESIAN_POINT('Ctrl Pts',(-58.706853591563,-13.7484649343429,
-55.7240191465997));
#133705=CARTESIAN_POINT('Ctrl Pts',(-58.7148369504267,-13.7593404086564,
-55.7513445478056));
#133706=CARTESIAN_POINT('Ctrl Pts',(-58.7232726197845,-13.7689867245339,
-55.7797537951109));
#133707=CARTESIAN_POINT('Ctrl Pts',(-58.7321217354356,-13.7774700892654,
-55.8091004361974));
#133708=CARTESIAN_POINT('Ctrl Pts',(-58.7413560701509,-13.7863227512184,
-55.8397245931469));
#133709=CARTESIAN_POINT('Ctrl Pts',(-58.7510406560465,-13.7939099084487,
-55.8713692899863));
#133710=CARTESIAN_POINT('Ctrl Pts',(-58.7611190114348,-13.8003330673419,
-55.9039164111607));
#133711=CARTESIAN_POINT('Ctrl Pts',(-58.7631356097838,-13.8016182900911,
-55.9104288299332));
#133712=CARTESIAN_POINT('Ctrl Pts',(-58.7651679353576,-13.802856965918,
-55.9169775323731));
#133713=CARTESIAN_POINT('Ctrl Pts',(-58.7672154801736,-13.804049979403,
-55.9235617984596));
#133714=CARTESIAN_POINT('Ctrl Pts',(-58.7772438220828,-13.80989304913,-55.955809821077));
#133715=CARTESIAN_POINT('Ctrl Pts',(-58.787591444619,-13.8146310037254,
-55.9888239184914));
#133716=CARTESIAN_POINT('Ctrl Pts',(-58.7982713308712,-13.8183831216517,
-56.0226328969941));
#133717=CARTESIAN_POINT('Ctrl Pts',(-58.8094011606195,-13.8222933162669,
-56.057866247407));
#133718=CARTESIAN_POINT('Ctrl Pts',(-58.8208917803897,-13.8251334049964,
-56.0939631676213));
#133719=CARTESIAN_POINT('Ctrl Pts',(-58.8327267583728,-13.8270283739072,
-56.1310025459061));
#133720=CARTESIAN_POINT('Ctrl Pts',(-58.8368443754292,-13.8276876701324,
-56.1438892598484));
#133721=CARTESIAN_POINT('Ctrl Pts',(-58.841003414625,-13.828232439654,-56.1568904311276));
#133722=CARTESIAN_POINT('Ctrl Pts',(-58.8452023822018,-13.8286675259685,
-56.1700105135303));
#133723=CARTESIAN_POINT('Ctrl Pts',(-58.8538987623764,-13.8295686227095,
-56.197183198818));
#133724=CARTESIAN_POINT('Ctrl Pts',(-58.8627548931133,-13.829999537714,
-56.2248738007663));
#133725=CARTESIAN_POINT('Ctrl Pts',(-58.871735578318,-13.8300000195957,
-56.2531111209796));
#133726=CARTESIAN_POINT('Ctrl Pts',(-58.3873384184922,-12.8301367871357,
-54.9623589764042));
#133727=CARTESIAN_POINT('Ctrl Pts',(-58.3873382434228,-12.8300623725117,
-55.2359199480943));
#133728=CARTESIAN_POINT('Ctrl Pts',(-58.6177174583935,-12.8294802501408,
-55.3834349955049));
#133729=CARTESIAN_POINT('Ctrl Pts',(-58.3877301336919,-12.9966384589807,
-54.9624046566442));
#133730=CARTESIAN_POINT('Ctrl Pts',(-58.3877303689833,-12.9966482737696,
-55.2359230050537));
#133731=CARTESIAN_POINT('Ctrl Pts',(-58.6180560895148,-12.9967778686954,
-55.3834453150663));
#133732=CARTESIAN_POINT('Ctrl Pts',(-58.3874096419063,-13.1631387418538,
-54.9623672844226));
#133733=CARTESIAN_POINT('Ctrl Pts',(-58.387409446605,-13.1632604597673,
-55.2359205047867));
#133734=CARTESIAN_POINT('Ctrl Pts',(-58.6177790296338,-13.16407332507,-55.3834369074594));
#133735=CARTESIAN_POINT('Ctrl Pts',(-58.3863769436068,-13.3296376352283,
-54.9622468511542));
#133736=CARTESIAN_POINT('Ctrl Pts',(-58.3863757263072,-13.3298338968435,
-55.2359124429054));
#133737=CARTESIAN_POINT('Ctrl Pts',(-58.6168862797201,-13.3313694061415,
-55.3834096347601));
#133738=CARTESIAN_POINT('',(-58.6177175690985,-12.8294802499273,-55.3834348225703));
#133739=CARTESIAN_POINT('Origin',(-58.8873370347925,-12.8289604802815,-54.9623589764042));
#133740=CARTESIAN_POINT('Origin',(9.50671311766895,-12.9674995491444,-53.303688922601));
#133741=CARTESIAN_POINT('Ctrl Pts',(-58.3767309587969,-11.8448446071682,
-56.4122977393942));
#133742=CARTESIAN_POINT('Ctrl Pts',(-58.3869014365542,-12.3742451521447,
-56.3787762146875));
#133743=CARTESIAN_POINT('Ctrl Pts',(-58.9159388499761,-12.33260651506,-56.3821256036996));
#133744=CARTESIAN_POINT('Ctrl Pts',(-58.3761594576374,-11.8217613269723,
-56.0640428959811));
#133745=CARTESIAN_POINT('Ctrl Pts',(-58.3850096805969,-12.2694751488998,
-56.131480723907));
#133746=CARTESIAN_POINT('Ctrl Pts',(-58.8249733980819,-12.3209870158311,
-56.0943527415187));
#133747=CARTESIAN_POINT('Ctrl Pts',(-58.3775636494613,-11.8719586819063,
-55.6887790791007));
#133748=CARTESIAN_POINT('Ctrl Pts',(-58.3840763820856,-12.2332797983991,
-55.8207298766612));
#133749=CARTESIAN_POINT('Ctrl Pts',(-58.7426223732974,-12.3463167916318,
-55.8395053228666));
#133750=CARTESIAN_POINT('Ctrl Pts',(-58.3812857230693,-12.1145902249729,
-55.3279498195379));
#133751=CARTESIAN_POINT('Ctrl Pts',(-58.3849523847638,-12.3664682018911,
-55.5261704685903));
#133752=CARTESIAN_POINT('Ctrl Pts',(-58.6766505662879,-12.4686699842847,
-55.6084539884381));
#133753=CARTESIAN_POINT('Ctrl Pts',(-58.3819811265814,-12.1628909733764,
-55.2698289416564));
#133754=CARTESIAN_POINT('Ctrl Pts',(-58.3851526533159,-12.3943556730011,
-55.4799801456162));
#133755=CARTESIAN_POINT('Ctrl Pts',(-58.6665193417984,-12.4930264323153,
-55.5718937149656));
#133756=CARTESIAN_POINT('Ctrl Pts',(-58.3833791647681,-12.2716887773838,
-55.165249378439));
#133757=CARTESIAN_POINT('Ctrl Pts',(-58.3856109002795,-12.4605296876876,
-55.3971016982864));
#133758=CARTESIAN_POINT('Ctrl Pts',(-58.6488938487369,-12.5478884692595,
-55.5067940385222));
#133759=CARTESIAN_POINT('Ctrl Pts',(-58.3840891453349,-12.3330632532853,
-55.1184352970832));
#133760=CARTESIAN_POINT('Ctrl Pts',(-58.3858723799976,-12.4994236383624,
-55.3598423864862));
#133761=CARTESIAN_POINT('Ctrl Pts',(-58.6413490671682,-12.5788364831875,
-55.4780465670558));
#133762=CARTESIAN_POINT('Ctrl Pts',(-58.3864241277835,-12.5724501016325,
-54.9791144036392));
#133763=CARTESIAN_POINT('Ctrl Pts',(-58.3867921906799,-12.6537459867802,
-55.2500592167191));
#133764=CARTESIAN_POINT('Ctrl Pts',(-58.6194845317821,-12.6995460488039,
-55.3930474481988));
#133765=CARTESIAN_POINT('Ctrl Pts',(-58.3876249629302,-12.7822769116689,
-54.9368955558876));
#133766=CARTESIAN_POINT('Ctrl Pts',(-58.3874149873687,-12.798358027374,
-55.2152912072037));
#133767=CARTESIAN_POINT('Ctrl Pts',(-58.6140349181668,-12.8053471169491,
-55.3683568445872));
#133768=CARTESIAN_POINT('Ctrl Pts',(-58.3874714544294,-12.9876188791411,
-54.9778741910769));
#133769=CARTESIAN_POINT('Ctrl Pts',(-58.3874999658154,-12.9364675110246,
-55.2486081571874));
#133770=CARTESIAN_POINT('Ctrl Pts',(-58.6203209684042,-12.9088882648831,
-55.3927678988426));
#133771=CARTESIAN_POINT('',(-58.8765127194368,-12.33000002,-56.2580153373943));
#133772=CARTESIAN_POINT('Origin',(-58.8765127194474,-11.83000002,-56.2580153373923));
#133773=CARTESIAN_POINT('Ctrl Pts',(-58.8765127194368,-12.330000020523,
-56.2580153373943));
#133774=CARTESIAN_POINT('Ctrl Pts',(-58.8668469571914,-12.3300006089033,
-56.2275462744181));
#133775=CARTESIAN_POINT('Ctrl Pts',(-58.8572724827484,-12.3304973506903,
-56.1976030412555));
#133776=CARTESIAN_POINT('Ctrl Pts',(-58.8478488263232,-12.3315471370039,
-56.1681943340671));
#133777=CARTESIAN_POINT('Ctrl Pts',(-58.8351276172195,-12.3329642675325,
-56.1284948483541));
#133778=CARTESIAN_POINT('Ctrl Pts',(-58.8227077416393,-12.3353891641161,
-56.0897498595506));
#133779=CARTESIAN_POINT('Ctrl Pts',(-58.8106737837062,-12.3389698977987,
-56.0519640291567));
#133780=CARTESIAN_POINT('Ctrl Pts',(-58.798585967488,-12.3425666571462,
-56.0140090873166));
#133781=CARTESIAN_POINT('Ctrl Pts',(-58.7868877399643,-12.3473304320438,
-55.9770211857099));
#133782=CARTESIAN_POINT('Ctrl Pts',(-58.7756496355396,-12.3534118638669,
-55.9410597318365));
#133783=CARTESIAN_POINT('Ctrl Pts',(-58.7654551148452,-12.3589285667047,
-55.9084377013004));
#133784=CARTESIAN_POINT('Ctrl Pts',(-58.7556391095688,-12.3655302748636,
-55.8766607416699));
#133785=CARTESIAN_POINT('Ctrl Pts',(-58.7462416806977,-12.3733192924399,
-55.8458185837666));
#133786=CARTESIAN_POINT('Ctrl Pts',(-58.7370890065606,-12.3809054461317,
-55.8157797055964));
#133787=CARTESIAN_POINT('Ctrl Pts',(-58.7283333473674,-12.3896186806531,
-55.7866276816044));
#133788=CARTESIAN_POINT('Ctrl Pts',(-58.7200001112973,-12.3995324607904,
-55.7584877378961));
#133789=CARTESIAN_POINT('Ctrl Pts',(-58.7119333700456,-12.4091292007029,
-55.7312477025938));
#133790=CARTESIAN_POINT('Ctrl Pts',(-58.7042623453504,-12.4198516550861,
-55.7049564664655));
#133791=CARTESIAN_POINT('Ctrl Pts',(-58.6970002769998,-12.4317352917216,
-55.679763891269));
#133792=CARTESIAN_POINT('Ctrl Pts',(-58.693993662897,-12.4366553100656,
-55.6693337564626));
#133793=CARTESIAN_POINT('Ctrl Pts',(-58.6910570395936,-12.4417739272228,
-55.6590923450502));
#133794=CARTESIAN_POINT('Ctrl Pts',(-58.688190921677,-12.4470915758791,
-55.6490518746812));
#133795=CARTESIAN_POINT('Ctrl Pts',(-58.6819688096681,-12.4586357644038,
-55.6272548191955));
#133796=CARTESIAN_POINT('Ctrl Pts',(-58.676161566562,-12.4709976964519,
-55.6066383301269));
#133797=CARTESIAN_POINT('Ctrl Pts',(-58.6707625823114,-12.4842111874128,
-55.5871773541376));
#133798=CARTESIAN_POINT('Ctrl Pts',(-58.6660950833367,-12.4956344390189,
-55.570353062519));
#133799=CARTESIAN_POINT('Ctrl Pts',(-58.6617321827839,-12.5076948684914,
-55.5543925885353));
#133800=CARTESIAN_POINT('Ctrl Pts',(-58.6576458797968,-12.5204167509595,
-55.5393004504467));
#133801=CARTESIAN_POINT('Ctrl Pts',(-58.6538203633614,-12.5323267269511,
-55.5251714877913));
#133802=CARTESIAN_POINT('Ctrl Pts',(-58.6502422277945,-12.5448868051958,
-55.5117483046152));
#133803=CARTESIAN_POINT('Ctrl Pts',(-58.6469241897868,-12.5579798460549,
-55.4992040857469));
#133804=CARTESIAN_POINT('Ctrl Pts',(-58.6436008912601,-12.5710936450212,
-55.4866399788907));
#133805=CARTESIAN_POINT('Ctrl Pts',(-58.640538399124,-12.5847413788212,
-55.4749584070027));
#133806=CARTESIAN_POINT('Ctrl Pts',(-58.6377735166986,-12.5987697559786,
-55.4643034363389));
#133807=CARTESIAN_POINT('Ctrl Pts',(-58.636939408858,-12.6030018272128,
-55.4610890520705));
#133808=CARTESIAN_POINT('Ctrl Pts',(-58.6361325568626,-12.6072683399031,
-55.4579678510716));
#133809=CARTESIAN_POINT('Ctrl Pts',(-58.6353544099234,-12.6115646261654,
-55.4549431101388));
#133810=CARTESIAN_POINT('Ctrl Pts',(-58.6319384747262,-12.6304246058457,
-55.4416650022455));
#133811=CARTESIAN_POINT('Ctrl Pts',(-58.6289958183114,-12.6500604145187,
-55.4300757823933));
#133812=CARTESIAN_POINT('Ctrl Pts',(-58.6265511922013,-12.6703334806547,
-55.4203199554195));
#133813=CARTESIAN_POINT('Ctrl Pts',(-58.6241562833628,-12.6901942458945,
-55.4107625363323));
#133814=CARTESIAN_POINT('Ctrl Pts',(-58.6222390524072,-12.7106665739421,
-55.4029656961182));
#133815=CARTESIAN_POINT('Ctrl Pts',(-58.6208117373686,-12.7315745389804,
-55.3970503586626));
#133816=CARTESIAN_POINT('Ctrl Pts',(-58.6194133085358,-12.7520593656347,
-55.3912547366517));
#133817=CARTESIAN_POINT('Ctrl Pts',(-58.6184848265338,-12.77296187318,-55.387266165696));
#133818=CARTESIAN_POINT('Ctrl Pts',(-58.6180318547009,-12.7940763452495,
-55.3851695450414));
#133819=CARTESIAN_POINT('Ctrl Pts',(-58.6177797881602,-12.805825976342,
-55.3840028325064));
#133820=CARTESIAN_POINT('Ctrl Pts',(-58.6176748911857,-12.8176405504773,
-55.3834213832906));
#133821=CARTESIAN_POINT('Ctrl Pts',(-58.617717901229,-12.8294802492869,
-55.3834343037763));
#133822=CARTESIAN_POINT('Origin',(-58.8765127194474,-11.83000002,-55.24995));
#133823=CARTESIAN_POINT('',(-58.8765127194474,-12.33000002,-60.42825533736));
#133824=CARTESIAN_POINT('Origin',(-58.8765127194474,-11.83000002,-60.42825533736));
#133825=CARTESIAN_POINT('',(-58.8765127194474,-12.33000002,-55.24995));
#133826=CARTESIAN_POINT('Origin',(0.,-12.9675000200281,-60.42825533736));
#133827=CARTESIAN_POINT('',(-57.9034184448965,-6.23235646472971,-60.8508735991007));
#133828=CARTESIAN_POINT('',(-58.2828791719688,-11.838774304476,-60.8508735991007));
#133829=CARTESIAN_POINT('Origin',(0.,-12.9675000200281,-60.8508735991007));
#133830=CARTESIAN_POINT('Origin',(-57.3770031434005,-11.8300849588959,-60.4282500608777));
#133831=CARTESIAN_POINT('Origin',(-56.5400850853955,-6.15642395592187,-60.3303328953569));
#133832=CARTESIAN_POINT('Origin',(-58.4950211556756,-6.18000001999999,-55.24995));
#133833=CARTESIAN_POINT('',(-58.4950211556756,-5.68000001999999,-60.42825533736));
#133834=CARTESIAN_POINT('Origin',(-58.4950211556756,-6.18000001999999,-60.42825533736));
#133835=CARTESIAN_POINT('',(-58.4950211556755,-5.6800000188644,-56.1192785199307));
#133836=CARTESIAN_POINT('Origin',(-58.4950211556756,-6.18000001999999,-56.1192785199305));
#133837=CARTESIAN_POINT('',(-58.4950211556756,-5.68000001999999,-55.24995));
#133838=CARTESIAN_POINT('Ctrl Pts',(-57.8697476022663,-5.20911947359449,
-54.9007953984755));
#133839=CARTESIAN_POINT('Ctrl Pts',(-57.8690388195133,-5.20383266421795,
-55.2313599550619));
#133840=CARTESIAN_POINT('Ctrl Pts',(-58.1702690071154,-5.16134039100007,
-55.3608055405082));
#133841=CARTESIAN_POINT('Ctrl Pts',(-57.8892576239528,-5.35464469293038,
-54.9031849800101));
#133842=CARTESIAN_POINT('Ctrl Pts',(-57.8816711167897,-5.29795553030126,
-55.2377699288152));
#133843=CARTESIAN_POINT('Ctrl Pts',(-58.1863681399526,-5.2347113163298,
-55.3646554087878));
#133844=CARTESIAN_POINT('Ctrl Pts',(-57.9082088324435,-5.50047055831863,
-54.9417550134773));
#133845=CARTESIAN_POINT('Ctrl Pts',(-57.8939857420187,-5.39104663027327,
-55.2713483619941));
#133846=CARTESIAN_POINT('Ctrl Pts',(-58.206532806921,-5.30826342386473,
-55.3884755439432));
#133847=CARTESIAN_POINT('Ctrl Pts',(-57.9410017896518,-5.75934555612452,
-55.0773466647676));
#133848=CARTESIAN_POINT('Ctrl Pts',(-57.9146461968408,-5.54837256073304,
-55.3788933751119));
#133849=CARTESIAN_POINT('Ctrl Pts',(-58.2517768983759,-5.43880935502387,
-55.4693790307482));
#133850=CARTESIAN_POINT('Ctrl Pts',(-57.9551095363294,-5.87426883806545,
-55.1748695369358));
#133851=CARTESIAN_POINT('Ctrl Pts',(-57.9231956882672,-5.61406051834577,
-55.4547002829484));
#133852=CARTESIAN_POINT('Ctrl Pts',(-58.2772082041435,-5.49676306934017,
-55.5268083141558));
#133853=CARTESIAN_POINT('Ctrl Pts',(-57.9772132186836,-6.05726143051376,
-55.4055720426652));
#133854=CARTESIAN_POINT('Ctrl Pts',(-57.9351757774934,-5.70509939430376,
-55.6270222213536));
#133855=CARTESIAN_POINT('Ctrl Pts',(-58.3321412809957,-5.58904289089475,
-55.6647824032721));
#133856=CARTESIAN_POINT('Ctrl Pts',(-57.9853419314568,-6.12627634754757,
-55.5391049776385));
#133857=CARTESIAN_POINT('Ctrl Pts',(-57.9385982402169,-5.73028333208738,
-55.725786817627));
#133858=CARTESIAN_POINT('Ctrl Pts',(-58.3618432600141,-5.62384585378313,
-55.7455542887996));
#133859=CARTESIAN_POINT('Ctrl Pts',(-57.9959179918116,-6.21652108864807,
-55.822399360329));
#133860=CARTESIAN_POINT('Ctrl Pts',(-57.9401928503808,-5.73799842569994,
-55.9259333604635));
#133861=CARTESIAN_POINT('Ctrl Pts',(-58.4256102669737,-5.66935462867838,
-55.922812372103));
#133862=CARTESIAN_POINT('Ctrl Pts',(-57.9983536021903,-6.2376310994186,
-55.9707502487912));
#133863=CARTESIAN_POINT('Ctrl Pts',(-57.9381116944449,-5.71846326962232,
-56.0282143296093));
#133864=CARTESIAN_POINT('Ctrl Pts',(-58.4594118188676,-5.68000001999999,
-56.0184103401194));
#133865=CARTESIAN_POINT('Ctrl Pts',(-57.9983536018174,-6.23763109620483,
-56.1192785199305));
#133866=CARTESIAN_POINT('Ctrl Pts',(-57.9336485918015,-5.68000002,-56.1192785199305));
#133867=CARTESIAN_POINT('Ctrl Pts',(-58.4950211556756,-5.68000001999999,
-56.1192785199305));
#133868=CARTESIAN_POINT('',(-58.1702690070839,-5.16134039099922,-55.3608055404948));
#133869=CARTESIAN_POINT('Origin',(-58.3653138416346,-5.14268076199931,-54.9007953984755));
#133870=CARTESIAN_POINT('Ctrl Pts',(-58.1702690071152,-5.16134039100008,
-55.3608055405081));
#133871=CARTESIAN_POINT('Ctrl Pts',(-58.1863681399526,-5.2347113163298,
-55.3646554087878));
#133872=CARTESIAN_POINT('Ctrl Pts',(-58.206532806921,-5.30826342386473,
-55.3884755439432));
#133873=CARTESIAN_POINT('Ctrl Pts',(-58.2517768983759,-5.43880935502387,
-55.4693790307482));
#133874=CARTESIAN_POINT('Ctrl Pts',(-58.2772082041435,-5.49676306934017,
-55.5268083141558));
#133875=CARTESIAN_POINT('Ctrl Pts',(-58.3321412809957,-5.58904289089475,
-55.6647824032721));
#133876=CARTESIAN_POINT('Ctrl Pts',(-58.3618432600141,-5.62384585378313,
-55.7455542887996));
#133877=CARTESIAN_POINT('Ctrl Pts',(-58.4256102669737,-5.66935462867838,
-55.922812372103));
#133878=CARTESIAN_POINT('Ctrl Pts',(-58.4594118188676,-5.68000001999999,
-56.0184103401194));
#133879=CARTESIAN_POINT('Ctrl Pts',(-58.4950211556756,-5.68000001999999,
-56.1192785199305));
#133880=CARTESIAN_POINT('Ctrl Pts',(-57.8012193907063,-4.71406478367217,
-54.8923577774473));
#133881=CARTESIAN_POINT('Ctrl Pts',(-57.8003896508712,-4.70825387307828,
-55.2306628708486));
#133882=CARTESIAN_POINT('Ctrl Pts',(-58.1110275345658,-4.66169335137012,
-55.3564444847807));
#133883=CARTESIAN_POINT('Ctrl Pts',(-57.8247681406176,-4.8789835624615,
-54.8952730204543));
#133884=CARTESIAN_POINT('Ctrl Pts',(-57.8239228782473,-4.87294575633325,
-55.2309062620395));
#133885=CARTESIAN_POINT('Ctrl Pts',(-58.13138502781,-4.82819068711566,-55.3579993904125));
#133886=CARTESIAN_POINT('Ctrl Pts',(-57.8476108954267,-5.04400181406656,
-54.8980841413334));
#133887=CARTESIAN_POINT('Ctrl Pts',(-57.8468132839757,-5.03816723372008,
-55.2311383656919));
#133888=CARTESIAN_POINT('Ctrl Pts',(-58.1511322005955,-4.99473857781996,
-55.3594494677196));
#133889=CARTESIAN_POINT('Ctrl Pts',(-57.8697476022662,-5.20911947359366,
-54.9007953984755));
#133890=CARTESIAN_POINT('Ctrl Pts',(-57.8690388195133,-5.20383266421771,
-55.2313599550618));
#133891=CARTESIAN_POINT('Ctrl Pts',(-58.1702690071153,-5.16134039100007,
-55.3608055405081));
#133892=CARTESIAN_POINT('',(-58.1110275344741,-4.66169335080973,-55.3564444847662));
#133893=CARTESIAN_POINT('Origin',(-58.2961987903268,-4.64338668274023,-54.8923577774473));
#133894=CARTESIAN_POINT('Origin',(8.5361523961935,-12.9121665737653,-44.4738563732989));
#133895=CARTESIAN_POINT('Ctrl Pts',(-57.6567521511579,-3.75885801193397,
-55.9233081330105));
#133896=CARTESIAN_POINT('Ctrl Pts',(-57.7240148019691,-4.18000001999999,
-55.9233081330106));
#133897=CARTESIAN_POINT('Ctrl Pts',(-58.1504944089282,-4.18000001999999,
-55.9233081330105));
#133898=CARTESIAN_POINT('Ctrl Pts',(-57.6567521506183,-3.75885800855547,
-55.7907772949108));
#133899=CARTESIAN_POINT('Ctrl Pts',(-57.720407107403,-4.15741168017902,
-55.8378278694331));
#133900=CARTESIAN_POINT('Ctrl Pts',(-58.1234127965435,-4.18000001999999,
-55.8430054684059));
#133901=CARTESIAN_POINT('Ctrl Pts',(-57.6600305184041,-3.7792996685362,
-55.6597535514676));
#133902=CARTESIAN_POINT('Ctrl Pts',(-57.7195075819602,-4.152660660194,-55.7476211206603));
#133903=CARTESIAN_POINT('Ctrl Pts',(-58.1029269769243,-4.19030837229928,
-55.7671861383685));
#133904=CARTESIAN_POINT('Ctrl Pts',(-57.6739991030625,-3.86739163922285,
-55.4096956077557));
#133905=CARTESIAN_POINT('Ctrl Pts',(-57.7239127922735,-4.18385080200108,
-55.5755351032824));
#133906=CARTESIAN_POINT('Ctrl Pts',(-58.0744257289554,-4.23473154807011,
-55.6263252797207));
#133907=CARTESIAN_POINT('Ctrl Pts',(-57.6844132682985,-3.93331576897112,
-55.2955533951453));
#133908=CARTESIAN_POINT('Ctrl Pts',(-57.7289974028628,-4.21833224283565,
-55.4955276754143));
#133909=CARTESIAN_POINT('Ctrl Pts',(-58.0668966730084,-4.26797587839126,
-55.5640071328243));
#133910=CARTESIAN_POINT('Ctrl Pts',(-57.7251747303172,-4.19619393974228,
-55.0015199525886));
#133911=CARTESIAN_POINT('Ctrl Pts',(-57.7516721739213,-4.37202128884096,
-55.2943853542448));
#133912=CARTESIAN_POINT('Ctrl Pts',(-58.0611013349386,-4.40054054713837,
-55.4063183641287));
#133913=CARTESIAN_POINT('Ctrl Pts',(-57.7635403562534,-4.45018749203841,
-54.8876932766828));
#133914=CARTESIAN_POINT('Ctrl Pts',(-57.7764802977889,-4.54099770957247,
-55.2182493155612));
#133915=CARTESIAN_POINT('Ctrl Pts',(-58.0797561993292,-4.52867484626318,
-55.3492143127724));
#133916=CARTESIAN_POINT('Ctrl Pts',(-57.8012193907063,-4.71406478367227,
-54.8923577774466));
#133917=CARTESIAN_POINT('Ctrl Pts',(-57.8003896508711,-4.70825387307822,
-55.2306628708477));
#133918=CARTESIAN_POINT('Ctrl Pts',(-58.1110275345655,-4.66169335137004,
-55.3564444847799));
#133919=CARTESIAN_POINT('',(-58.1504944089236,-4.18000003396406,-55.9233081330193));
#133920=CARTESIAN_POINT('Origin',(-58.1504944089282,-3.68000001999999,-55.9233081330105));
#133921=CARTESIAN_POINT('Ctrl Pts',(-58.1504944089282,-4.18000001999999,
-55.9233081330105));
#133922=CARTESIAN_POINT('Ctrl Pts',(-58.1234127965435,-4.18000001999999,
-55.8430054684059));
#133923=CARTESIAN_POINT('Ctrl Pts',(-58.1029269769243,-4.19030837229928,
-55.7671861383685));
#133924=CARTESIAN_POINT('Ctrl Pts',(-58.0744257289554,-4.23473154807011,
-55.6263252797207));
#133925=CARTESIAN_POINT('Ctrl Pts',(-58.0668966730084,-4.26797587839126,
-55.5640071328243));
#133926=CARTESIAN_POINT('Ctrl Pts',(-58.0611013349386,-4.40054054713837,
-55.4063183641287));
#133927=CARTESIAN_POINT('Ctrl Pts',(-58.0797561993292,-4.52867484626318,
-55.3492143127724));
#133928=CARTESIAN_POINT('Ctrl Pts',(-58.1110275345658,-4.6616933513699,
-55.3564444847807));
#133929=CARTESIAN_POINT('Origin',(-58.1504944089282,-3.68000001999999,-55.24995));
#133930=CARTESIAN_POINT('',(-58.1504944089282,-4.18000001999999,-60.42825533736));
#133931=CARTESIAN_POINT('Origin',(-58.1504944089282,-3.68000001999999,-60.42825533736));
#133932=CARTESIAN_POINT('',(-58.1504944089282,-4.18000001999999,-55.24995));
#133933=CARTESIAN_POINT('Origin',(0.,-12.9675000200281,-60.42825533736));
#133934=CARTESIAN_POINT('',(-56.377904566775,1.85477723331148,-60.8508735991007));
#133935=CARTESIAN_POINT('',(-57.5607154366947,-3.75164060643487,-60.8508735991007));
#133936=CARTESIAN_POINT('Origin',(0.,-12.9675000200281,-60.8508735991007));
#133937=CARTESIAN_POINT('Origin',(-56.6143043465388,-3.67942422979871,-60.4241466659414));
#133938=CARTESIAN_POINT('Origin',(-55.1148638636367,2.00185121638848,-60.365292836485));
#133939=CARTESIAN_POINT('Origin',(-56.9614672388491,1.96999998000001,-55.24995));
#133940=CARTESIAN_POINT('',(-56.9614672388491,2.46999998000001,-55.74995));
#133941=CARTESIAN_POINT('Origin',(-56.9614672388491,1.96999998000001,-55.74995));
#133942=CARTESIAN_POINT('',(-56.9614672388491,2.46999998000001,-60.42825533736));
#133943=CARTESIAN_POINT('',(-56.9614672388491,2.46999998000001,-55.24995));
#133944=CARTESIAN_POINT('Origin',(-56.9614672388491,1.96999998000001,-60.42825533736));
#133945=CARTESIAN_POINT('Ctrl Pts',(-56.208463007634,2.83467839222654,-54.74995));
#133946=CARTESIAN_POINT('Ctrl Pts',(-56.2084630076339,2.83467839222653,
-55.2499499999999));
#133947=CARTESIAN_POINT('Ctrl Pts',(-56.6898028749653,2.96999998000001,
-55.24995));
#133948=CARTESIAN_POINT('Ctrl Pts',(-56.2799098403954,2.5805414908759,-54.7499500372609));
#133949=CARTESIAN_POINT('Ctrl Pts',(-56.2484819268069,2.69233080251842,
-55.2864232478283));
#133950=CARTESIAN_POINT('Ctrl Pts',(-56.761879333771,2.84181173581483,-55.24995));
#133951=CARTESIAN_POINT('Ctrl Pts',(-56.3494613434174,2.32547473937703,
-54.8529437484072));
#133952=CARTESIAN_POINT('Ctrl Pts',(-56.2763245403096,2.59340567144111,
-55.3787800334104));
#133953=CARTESIAN_POINT('Ctrl Pts',(-56.8320086455423,2.71321787394558,
-55.3014468715073));
#133954=CARTESIAN_POINT('Ctrl Pts',(-56.4486203895175,1.955305574271,-55.2191289705157));
#133955=CARTESIAN_POINT('Ctrl Pts',(-56.3089306288004,2.48216937222065,
-55.5705782077274));
#133956=CARTESIAN_POINT('Ctrl Pts',(-56.9320168401896,2.52654832947528,
-55.4845394879542));
#133957=CARTESIAN_POINT('Ctrl Pts',(-56.4778207259178,1.84316918512194,
-55.479632471504));
#133958=CARTESIAN_POINT('Ctrl Pts',(-56.313441444092,2.46999998405909,-55.6636097943426));
#133959=CARTESIAN_POINT('Ctrl Pts',(-56.9614672318199,2.46999998000001,
-55.614791233664));
#133960=CARTESIAN_POINT('Ctrl Pts',(-56.4778207328943,1.8431691585182,-55.74995));
#133961=CARTESIAN_POINT('Ctrl Pts',(-56.3134414454605,2.46999998000001,
-55.74995));
#133962=CARTESIAN_POINT('Ctrl Pts',(-56.9614672388491,2.46999998000001,
-55.74995));
#133963=CARTESIAN_POINT('',(-56.6898028749653,2.96999998000001,-55.24995));
#133964=CARTESIAN_POINT('Origin',(-56.6898028749653,2.96999998000001,-54.74995));
#133965=CARTESIAN_POINT('Ctrl Pts',(-56.6898028749653,2.96999998000001,
-55.24995));
#133966=CARTESIAN_POINT('Ctrl Pts',(-56.761879333771,2.84181173581483,-55.24995));
#133967=CARTESIAN_POINT('Ctrl Pts',(-56.8320086455423,2.71321787394558,
-55.3014468715073));
#133968=CARTESIAN_POINT('Ctrl Pts',(-56.9320168401896,2.52654832947528,
-55.4845394879542));
#133969=CARTESIAN_POINT('Ctrl Pts',(-56.9614672318199,2.46999998000001,
-55.614791233664));
#133970=CARTESIAN_POINT('Ctrl Pts',(-56.9614672388491,2.46999998000001,
-55.74995));
#133971=CARTESIAN_POINT('Origin',(0.,-12.9675000200281,-54.74995));
#133972=CARTESIAN_POINT('',(-56.5468500449175,3.46999998000001,-55.24995));
#133973=CARTESIAN_POINT('Origin',(-56.5468500449175,3.46999998000001,-54.74995));
#133974=CARTESIAN_POINT('Origin',(0.,-12.9675000200281,-55.24995));
#133975=CARTESIAN_POINT('Ctrl Pts',(-55.7689460407313,4.32194224278906,
-55.74995));
#133976=CARTESIAN_POINT('Ctrl Pts',(-55.8780548882949,3.96999998000002,
-55.74995));
#133977=CARTESIAN_POINT('Ctrl Pts',(-56.2465221147258,3.96999998000001,
-55.74995));
#133978=CARTESIAN_POINT('Ctrl Pts',(-55.7689460480881,4.32194221905895,
-55.6164566007256));
#133979=CARTESIAN_POINT('Ctrl Pts',(-55.8780548935443,3.96999996254405,
-55.6679224120286));
#133980=CARTESIAN_POINT('Ctrl Pts',(-56.2465221221473,3.96999998000001,
-55.683203301545));
#133981=CARTESIAN_POINT('Ctrl Pts',(-55.777377389072,4.29480596539276,-55.4823754218786));
#133982=CARTESIAN_POINT('Ctrl Pts',(-55.8841708256374,3.94968459977806,
-55.5852103705331));
#133983=CARTESIAN_POINT('Ctrl Pts',(-56.2550256651168,3.95631565470027,
-55.6161627093404));
#133984=CARTESIAN_POINT('Ctrl Pts',(-55.8090161453349,4.19224220492976,
-55.2379754767005));
#133985=CARTESIAN_POINT('Ctrl Pts',(-55.9063784289296,3.87553573797955,
-55.4407856273786));
#133986=CARTESIAN_POINT('Ctrl Pts',(-56.2869353583447,3.90459461560065,
-55.4939627399492));
#133987=CARTESIAN_POINT('Ctrl Pts',(-55.832275617124,4.11659879830721,-55.1268557913785));
#133988=CARTESIAN_POINT('Ctrl Pts',(-55.9226989367341,3.8208945781902,-55.3782063812366));
#133989=CARTESIAN_POINT('Ctrl Pts',(-56.3103940129914,3.86644903217756,
-55.4384028944151));
#133990=CARTESIAN_POINT('Ctrl Pts',(-55.888335440433,3.9323045563208,-54.9446837986715));
#133991=CARTESIAN_POINT('Ctrl Pts',(-55.9602568779234,3.69427053570811,
-55.285569160897));
#133992=CARTESIAN_POINT('Ctrl Pts',(-56.366933902262,3.77351280880021,-55.3473169006099));
#133993=CARTESIAN_POINT('Ctrl Pts',(-55.9215848671782,3.82212901679781,
-54.8721313715614));
#133994=CARTESIAN_POINT('Ctrl Pts',(-55.9820168525955,3.62048086904919,
-55.2550739756198));
#133995=CARTESIAN_POINT('Ctrl Pts',(-56.4004680605965,3.71795329740048,
-55.3110406862353));
#133996=CARTESIAN_POINT('Ctrl Pts',(-55.9918544429005,3.58627698995622,
-54.7753183134609));
#133997=CARTESIAN_POINT('Ctrl Pts',(-56.0252324832575,3.47302446308311,
-55.2281701114017));
#133998=CARTESIAN_POINT('Ctrl Pts',(-56.4713393874401,3.59901742755992,
-55.262634156276));
#133999=CARTESIAN_POINT('Ctrl Pts',(-56.0297048503836,3.4577829011709,-54.7499500149493));
#134000=CARTESIAN_POINT('Ctrl Pts',(-56.047279588089,3.39732382739444,-55.2323508865986));
#134001=CARTESIAN_POINT('Ctrl Pts',(-56.50951584811,3.5342168990206,-55.24995));
#134002=CARTESIAN_POINT('Ctrl Pts',(-56.0667239566569,3.33043300908083,
-54.74995));
#134003=CARTESIAN_POINT('Ctrl Pts',(-56.066723956657,3.33043300908077,-55.24995));
#134004=CARTESIAN_POINT('Ctrl Pts',(-56.5468500449175,3.46999998000007,
-55.24995));
#134005=CARTESIAN_POINT('',(-56.2465221147258,3.96999998000001,-55.74995));
#134006=CARTESIAN_POINT('Origin',(-56.2465221147258,4.46999998000001,-55.74995));
#134007=CARTESIAN_POINT('Ctrl Pts',(-56.2465221147258,3.96999998000007,
-55.74995));
#134008=CARTESIAN_POINT('Ctrl Pts',(-56.2465221172463,3.96999998000007,
-55.7272812089341));
#134009=CARTESIAN_POINT('Ctrl Pts',(-56.24750295639,3.96845400764675,-55.7045717667832));
#134010=CARTESIAN_POINT('Ctrl Pts',(-56.2494234122338,3.96537155503915,
-55.6820750956295));
#134011=CARTESIAN_POINT('Ctrl Pts',(-56.2513459831365,3.96228570762857,
-55.6595536481773));
#134012=CARTESIAN_POINT('Ctrl Pts',(-56.2542102415385,3.95766009770567,
-55.6372462305913));
#134013=CARTESIAN_POINT('Ctrl Pts',(-56.2579748311759,3.95155602091719,
-55.615399714024));
#134014=CARTESIAN_POINT('Ctrl Pts',(-56.2615221746811,3.9458041968841,-55.5948139115537));
#134015=CARTESIAN_POINT('Ctrl Pts',(-56.2658689354504,3.9387402676577,-55.5746377942181));
#134016=CARTESIAN_POINT('Ctrl Pts',(-56.2709805117308,3.93045513515051,
-55.5550627246448));
#134017=CARTESIAN_POINT('Ctrl Pts',(-56.2765960817443,3.92135310103939,
-55.5335575826534));
#134018=CARTESIAN_POINT('Ctrl Pts',(-56.2831412261279,3.91075174977411,
-55.5127182769628));
#134019=CARTESIAN_POINT('Ctrl Pts',(-56.2904985464591,3.89878795974976,
-55.4927713297682));
#134020=CARTESIAN_POINT('Ctrl Pts',(-56.2978778612356,3.88678840440414,
-55.4727647518903));
#134021=CARTESIAN_POINT('Ctrl Pts',(-56.3060742151598,3.87341874044962,
-55.4536564757209));
#134022=CARTESIAN_POINT('Ctrl Pts',(-56.3149691537834,3.85885777178856,
-55.4356418426681));
#134023=CARTESIAN_POINT('Ctrl Pts',(-56.3224025873938,3.84668927929807,
-55.4205871487034));
#134024=CARTESIAN_POINT('Ctrl Pts',(-56.330323899967,3.8336897103653,-55.4062957646521));
#134025=CARTESIAN_POINT('Ctrl Pts',(-56.3386639576267,3.81998092048891,
-55.3928598975125));
#134026=CARTESIAN_POINT('Ctrl Pts',(-56.3485367757166,3.80375268871842,
-55.3769547470254));
#134027=CARTESIAN_POINT('Ctrl Pts',(-56.3590516393933,3.78643081276152,
-55.3621527091661));
#134028=CARTESIAN_POINT('Ctrl Pts',(-56.3700653174119,3.76821160325647,
-55.3486149432771));
#134029=CARTESIAN_POINT('Ctrl Pts',(-56.3811000400428,3.74995758102126,
-55.3350513098229));
#134030=CARTESIAN_POINT('Ctrl Pts',(-56.3926354850762,3.73080346228537,
-55.3227572166925));
#134031=CARTESIAN_POINT('Ctrl Pts',(-56.404527598651,3.7109748182806,-55.3118505508841));
#134032=CARTESIAN_POINT('Ctrl Pts',(-56.414753129079,3.69392499771326,-55.3024723657204));
#134033=CARTESIAN_POINT('Ctrl Pts',(-56.4252423645287,3.67637719717626,
-55.2941193424573));
#134034=CARTESIAN_POINT('Ctrl Pts',(-56.4359037240183,3.65848536248023,
-55.2868374212556));
#134035=CARTESIAN_POINT('Ctrl Pts',(-56.4480269746482,3.63814019013509,
-55.2785569992435));
#134036=CARTESIAN_POINT('Ctrl Pts',(-56.4604710249688,3.61717859047507,
-55.2715931459213));
#134037=CARTESIAN_POINT('Ctrl Pts',(-56.4730923955105,3.59582457403251,
-55.2660407403897));
#134038=CARTESIAN_POINT('Ctrl Pts',(-56.485718783795,3.57446206810312,-55.2604861274479));
#134039=CARTESIAN_POINT('Ctrl Pts',(-56.4985226333192,3.55270760676572,
-55.2563443375913));
#134040=CARTESIAN_POINT('Ctrl Pts',(-56.511360293421,3.53080101674991,-55.2536605341334));
#134041=CARTESIAN_POINT('Ctrl Pts',(-56.5231990099542,3.51059905569539,
-55.2511855668795));
#134042=CARTESIAN_POINT('Ctrl Pts',(-56.5350664799457,3.49026837472315,
-55.24995));
#134043=CARTESIAN_POINT('Ctrl Pts',(-56.5468500449175,3.46999998000001,
-55.24995));
#134044=CARTESIAN_POINT('Origin',(-56.2465221147258,4.46999998000001,-55.24995));
#134045=CARTESIAN_POINT('',(-56.2465221147258,3.96999998000001,-60.42825533736));
#134046=CARTESIAN_POINT('Origin',(-56.2465221147258,4.46999998000001,-60.42825533736));
#134047=CARTESIAN_POINT('',(-56.2465221147258,3.96999998000001,-55.24995));
#134048=CARTESIAN_POINT('Origin',(0.,-12.9675000200281,-60.42825533736));
#134049=CARTESIAN_POINT('',(-53.6034226162473,9.94191093135268,-60.8508735991007));
#134050=CARTESIAN_POINT('',(-55.6666368275827,4.33549309160632,-60.8508735991007));
#134051=CARTESIAN_POINT('Origin',(0.,-12.9675000200281,-60.8508735991007));
#134052=CARTESIAN_POINT('Origin',(-54.6351094353318,4.47360462069243,-60.4185055563343));
#134053=CARTESIAN_POINT('Origin',(-52.4761756351917,10.1269382012971,-60.4132827620456));
#134054=CARTESIAN_POINT('Origin',(-54.1729175880533,10.11999998,-55.24995));
#134055=CARTESIAN_POINT('',(-54.1729175880533,10.61999998,-55.74995));
#134056=CARTESIAN_POINT('Origin',(-54.1729175880533,10.11999998,-55.74995));
#134057=CARTESIAN_POINT('',(-54.1729175880533,10.61999998,-60.42825533736));
#134058=CARTESIAN_POINT('',(-54.1729175880533,10.61999998,-55.24995));
#134059=CARTESIAN_POINT('Origin',(-54.1729175880533,10.11999998,-60.42825533736));
#134060=CARTESIAN_POINT('Ctrl Pts',(-53.3256899305368,10.8121330655672,
-54.7553968408231));
#134061=CARTESIAN_POINT('Ctrl Pts',(-53.3054454943535,10.8575310968505,
-55.2747187747876));
#134062=CARTESIAN_POINT('Ctrl Pts',(-53.7823432375846,11.067884690566,-55.2526734204115));
#134063=CARTESIAN_POINT('Ctrl Pts',(-53.4285862862346,10.5813885818665,
-54.7797862992586));
#134064=CARTESIAN_POINT('Ctrl Pts',(-53.3650311600591,10.7244739426765,
-55.3417466734359));
#134065=CARTESIAN_POINT('Ctrl Pts',(-53.8861362179292,10.9515071084652,
-55.2648699557477));
#134066=CARTESIAN_POINT('Ctrl Pts',(-53.5254458539065,10.3597364405483,
-54.885939939012));
#134067=CARTESIAN_POINT('Ctrl Pts',(-53.3983781597441,10.6502596450882,
-55.4540676493459));
#134068=CARTESIAN_POINT('Ctrl Pts',(-53.9838097653667,10.83974934456,-55.3179449795228));
#134069=CARTESIAN_POINT('Ctrl Pts',(-53.633790842791,10.1090015716016,-55.1553271807471));
#134070=CARTESIAN_POINT('Ctrl Pts',(-53.4176451441909,10.6111056725941,
-55.596678279911));
#134071=CARTESIAN_POINT('Ctrl Pts',(-54.0930825652429,10.7133083132261,
-55.4526385853652));
#134072=CARTESIAN_POINT('Ctrl Pts',(-53.6624100137865,10.0422483461928,
-55.2594857136242));
#134073=CARTESIAN_POINT('Ctrl Pts',(-53.4186534680994,10.6106295502708,
-55.6378844781733));
#134074=CARTESIAN_POINT('Ctrl Pts',(-54.1219468150851,10.6796458924645,
-55.5047178594674));
#134075=CARTESIAN_POINT('Ctrl Pts',(-53.702610379063,9.94826762670561,-55.4957569720976));
#134076=CARTESIAN_POINT('Ctrl Pts',(-53.4178589543304,10.6154785181549,
-55.7046481866627));
#134077=CARTESIAN_POINT('Ctrl Pts',(-54.1624914359772,10.6322531187842,
-55.6228534833935));
#134078=CARTESIAN_POINT('Ctrl Pts',(-53.7129480039811,9.9239694167493,-55.6201514218302));
#134079=CARTESIAN_POINT('Ctrl Pts',(-53.4163125940233,10.619999979359,-55.7271468411276));
#134080=CARTESIAN_POINT('Ctrl Pts',(-54.172917586547,10.61999998,-55.685050712911));
#134081=CARTESIAN_POINT('Ctrl Pts',(-53.7129480054761,9.92396941324122,
-55.74995));
#134082=CARTESIAN_POINT('Ctrl Pts',(-53.4163125938068,10.61999998,-55.74995));
#134083=CARTESIAN_POINT('Ctrl Pts',(-54.1729175880533,10.61999998,-55.74995));
#134084=CARTESIAN_POINT('Ctrl Pts',(-53.7823432375846,11.067884690566,-55.2526734204115));
#134085=CARTESIAN_POINT('Ctrl Pts',(-53.8861362179292,10.9515071084652,
-55.2648699557477));
#134086=CARTESIAN_POINT('Ctrl Pts',(-53.9838097653667,10.83974934456,-55.3179449795228));
#134087=CARTESIAN_POINT('Ctrl Pts',(-54.0930825652429,10.7133083132261,
-55.4526385853652));
#134088=CARTESIAN_POINT('Ctrl Pts',(-54.1219468150851,10.6796458924645,
-55.5047178594674));
#134089=CARTESIAN_POINT('Ctrl Pts',(-54.1624914359772,10.6322531187842,
-55.6228534833935));
#134090=CARTESIAN_POINT('Ctrl Pts',(-54.172917586547,10.61999998,-55.685050712911));
#134091=CARTESIAN_POINT('Ctrl Pts',(-54.1729175880533,10.61999998,-55.74995));
#134092=CARTESIAN_POINT('Origin',(-4.6996065532056,-66.6842487255793,-59.64995));
#134093=CARTESIAN_POINT('',(-39.5,-63.6396088127436,-60.64995));
#134094=CARTESIAN_POINT('',(-33.85,-64.1339197616649,-60.64995));
#134095=CARTESIAN_POINT('',(-4.6996065532056,-66.6842487255793,-60.64995));
#134096=CARTESIAN_POINT('Ctrl Pts',(-33.8064221286261,-65.1415521689341,
-59.64995));
#134097=CARTESIAN_POINT('Ctrl Pts',(-33.8064221286289,-65.1415521689339,
-59.7808732880372));
#134098=CARTESIAN_POINT('Ctrl Pts',(-33.8075563441358,-65.1153261907357,
-59.9116978933078));
#134099=CARTESIAN_POINT('Ctrl Pts',(-33.8119222489988,-65.0143752473362,
-60.1535689714224));
#134100=CARTESIAN_POINT('Ctrl Pts',(-33.8151522214979,-64.9396899802014,
-60.2644967268053));
#134101=CARTESIAN_POINT('Ctrl Pts',(-33.8232193617858,-64.7531569593752,
-60.4496168355678));
#134102=CARTESIAN_POINT('Ctrl Pts',(-33.8280533572402,-64.6413825582346,
-60.5237363920407));
#134103=CARTESIAN_POINT('Ctrl Pts',(-33.8385935839748,-64.3976654214474,
-60.6239226729819));
#134104=CARTESIAN_POINT('Ctrl Pts',(-33.8442946417933,-64.2658423095942,
-60.64995));
#134105=CARTESIAN_POINT('Ctrl Pts',(-33.85,-64.1339197616649,-60.64995));
#134106=CARTESIAN_POINT('Ctrl Pts',(-39.5,-63.6396088127436,-60.64995));
#134107=CARTESIAN_POINT('Ctrl Pts',(-39.4942946417933,-63.771531360673,
-60.64995));
#134108=CARTESIAN_POINT('Ctrl Pts',(-39.4885935839748,-63.9033544725257,
-60.623922672982));
#134109=CARTESIAN_POINT('Ctrl Pts',(-39.4780533572402,-64.1470716093135,
-60.5237363920406));
#134110=CARTESIAN_POINT('Ctrl Pts',(-39.4732193617865,-64.2588460104538,
-60.4496168355678));
#134111=CARTESIAN_POINT('Ctrl Pts',(-39.4651522214972,-64.4453790312801,
-60.2644967268053));
#134112=CARTESIAN_POINT('Ctrl Pts',(-39.4619222489981,-64.5200642984147,
-60.153568971423));
#134113=CARTESIAN_POINT('Ctrl Pts',(-39.4575563441365,-64.6210152418146,
-59.9116978933072));
#134114=CARTESIAN_POINT('Ctrl Pts',(-39.4564221286269,-64.6472412200127,
-59.7808732880376));
#134115=CARTESIAN_POINT('Ctrl Pts',(-39.4564221286262,-64.6472412200127,
-59.64995));
#134116=CARTESIAN_POINT('Origin',(-39.5,-65.1453385690586,-52.64995));
#134117=CARTESIAN_POINT('',(-40.,-65.1453385690586,-59.64995));
#134118=CARTESIAN_POINT('Origin',(-39.5,-65.1453385690586,-59.64995));
#134119=CARTESIAN_POINT('',(-40.,-65.1453385690586,-55.74995));
#134120=CARTESIAN_POINT('Origin',(-39.5,-65.1453385690586,-55.74995));
#134121=CARTESIAN_POINT('',(-40.,-65.1453385690586,-55.24995));
#134122=CARTESIAN_POINT('Ctrl Pts',(-40.4564221286262,-64.5597525564868,
-54.74995));
#134123=CARTESIAN_POINT('Ctrl Pts',(-40.4564221286261,-64.5597525564868,
-55.24995));
#134124=CARTESIAN_POINT('Ctrl Pts',(-40.5,-65.0578499055327,-55.24995));
#134125=CARTESIAN_POINT('Ctrl Pts',(-40.1938874372398,-64.5827213657654,
-54.7499500000659));
#134126=CARTESIAN_POINT('Ctrl Pts',(-40.322075011829,-64.5715064061754,
-55.2615708605686));
#134127=CARTESIAN_POINT('Ctrl Pts',(-40.3687326543062,-65.0808187148095,
-55.24995));
#134128=CARTESIAN_POINT('Ctrl Pts',(-39.9344354391268,-64.6054204743294,
-54.8577231271254));
#134129=CARTESIAN_POINT('Ctrl Pts',(-40.2033393021413,-64.581894434738,
-55.3274496218431));
#134130=CARTESIAN_POINT('Ctrl Pts',(-40.2390066552503,-65.1035178233753,
-55.3038365635632));
#134131=CARTESIAN_POINT('Ctrl Pts',(-39.5641952557525,-64.6378122931564,
-55.2279633105016));
#134132=CARTESIAN_POINT('Ctrl Pts',(-40.0417246342956,-64.5960338860327,
-55.5133819370971));
#134133=CARTESIAN_POINT('Ctrl Pts',(-40.0538865635631,-65.1359096422023,
-55.4889566552503));
#134134=CARTESIAN_POINT('Ctrl Pts',(-39.4564221286917,-64.647241220007,
-55.4874153086129));
#134135=CARTESIAN_POINT('Ctrl Pts',(-40.0000000000045,-64.5996843185185,
-55.6317784220497));
#134136=CARTESIAN_POINT('Ctrl Pts',(-40.,-65.1453385690531,-55.6186826543065));
#134137=CARTESIAN_POINT('Ctrl Pts',(-39.4564221286262,-64.6472412200127,
-55.74995));
#134138=CARTESIAN_POINT('Ctrl Pts',(-40.,-64.5996843185239,-55.74995));
#134139=CARTESIAN_POINT('Ctrl Pts',(-40.,-65.1453385690586,-55.74995));
#134140=CARTESIAN_POINT('',(-40.5,-65.0578499055327,-55.24995));
#134141=CARTESIAN_POINT('Origin',(-40.5,-65.0578499055327,-54.74995));
#134142=CARTESIAN_POINT('Ctrl Pts',(-40.5,-65.0578499055327,-55.24995));
#134143=CARTESIAN_POINT('Ctrl Pts',(-40.3687326543062,-65.0808187148095,
-55.24995));
#134144=CARTESIAN_POINT('Ctrl Pts',(-40.2390066552503,-65.1035178233753,
-55.3038365635632));
#134145=CARTESIAN_POINT('Ctrl Pts',(-40.0538865635631,-65.1359096422023,
-55.4889566552503));
#134146=CARTESIAN_POINT('Ctrl Pts',(-40.,-65.1453385690531,-55.6186826543065));
#134147=CARTESIAN_POINT('Ctrl Pts',(-40.,-65.1453385690586,-55.74995));
#134148=CARTESIAN_POINT('Origin',(-44.2377516955329,-64.7308390050988,-54.74995));
#134149=CARTESIAN_POINT('',(-41.,-65.0141055737697,-55.24995));
#134150=CARTESIAN_POINT('Origin',(-41.,-65.0141055737697,-54.74995));
#134151=CARTESIAN_POINT('',(-40.7958880023324,-65.0319630596553,-55.24995));
#134152=CARTESIAN_POINT('Ctrl Pts',(-41.9564221286262,-64.428519561198,
-55.74995));
#134153=CARTESIAN_POINT('Ctrl Pts',(-41.5,-64.4684513232351,-55.74995));
#134154=CARTESIAN_POINT('Ctrl Pts',(-41.5,-64.9266169102438,-55.74995));
#134155=CARTESIAN_POINT('Ctrl Pts',(-41.9564221285606,-64.4285195612037,
-55.487415308613));
#134156=CARTESIAN_POINT('Ctrl Pts',(-41.4999999999489,-64.4684513232351,
-55.6078478088783));
#134157=CARTESIAN_POINT('Ctrl Pts',(-41.5,-64.9266169102493,-55.6186826543063));
#134158=CARTESIAN_POINT('Ctrl Pts',(-41.8486490015007,-64.4379484880542,
-55.2279633105015));
#134159=CARTESIAN_POINT('Ctrl Pts',(-41.4358662151155,-64.4740623023634,
-55.4680441063688));
#134160=CARTESIAN_POINT('Ctrl Pts',(-41.4461134364372,-64.9360458371002,
-55.4889566552508));
#134161=CARTESIAN_POINT('Ctrl Pts',(-41.4784088181247,-64.4703403068813,
-54.8577231271255));
#134162=CARTESIAN_POINT('Ctrl Pts',(-41.2286175782531,-64.4921942086162,
-55.2822894538775));
#134163=CARTESIAN_POINT('Ctrl Pts',(-41.2609933447493,-64.9684376559271,
-55.3038365635627));
#134164=CARTESIAN_POINT('Ctrl Pts',(-41.2189568200132,-64.4930394154452,
-54.7499500000659));
#134165=CARTESIAN_POINT('Ctrl Pts',(-41.0869589695398,-64.5045877309693,
-55.2386587236917));
#134166=CARTESIAN_POINT('Ctrl Pts',(-41.1312673456941,-64.991136764493,
-55.24995));
#134167=CARTESIAN_POINT('Ctrl Pts',(-40.9564221286262,-64.5160082247239,
-54.74995));
#134168=CARTESIAN_POINT('Ctrl Pts',(-40.9564221286262,-64.5160082247238,
-55.24995));
#134169=CARTESIAN_POINT('Ctrl Pts',(-41.,-65.0141055737697,-55.24995));
#134170=CARTESIAN_POINT('',(-41.5,-64.9266169102438,-55.74995));
#134171=CARTESIAN_POINT('Origin',(-42.,-64.9266169102438,-55.74995));
#134172=CARTESIAN_POINT('Ctrl Pts',(-41.5,-64.9266169102438,-55.74995));
#134173=CARTESIAN_POINT('Ctrl Pts',(-41.5,-64.9266169102493,-55.6186826543063));
#134174=CARTESIAN_POINT('Ctrl Pts',(-41.4461134364372,-64.9360458371002,
-55.4889566552508));
#134175=CARTESIAN_POINT('Ctrl Pts',(-41.2609933447493,-64.9684376559271,
-55.3038365635627));
#134176=CARTESIAN_POINT('Ctrl Pts',(-41.1312673456941,-64.991136764493,
-55.24995));
#134177=CARTESIAN_POINT('Ctrl Pts',(-41.,-65.0141055737697,-55.24995));
#134178=CARTESIAN_POINT('Origin',(-42.,-64.9266169102438,-52.64995));
#134179=CARTESIAN_POINT('',(-41.5,-64.9266169102438,-59.64995));
#134180=CARTESIAN_POINT('Origin',(-42.,-64.9266169102438,-59.64995));
#134181=CARTESIAN_POINT('',(-41.5,-64.9266169102438,-177.34995));
#134182=CARTESIAN_POINT('Origin',(-4.6996065532056,-66.6842487255793,-59.64995));
#134183=CARTESIAN_POINT('',(-42.,-63.4208871539288,-60.64995));
#134184=CARTESIAN_POINT('',(-4.6996065532056,-66.6842487255793,-60.64995));
#134185=CARTESIAN_POINT('Ctrl Pts',(-41.9564221286262,-64.428519561198,
-59.64995));
#134186=CARTESIAN_POINT('Ctrl Pts',(-41.9564221286289,-64.4285195611977,
-59.7808732880376));
#134187=CARTESIAN_POINT('Ctrl Pts',(-41.9575563441358,-64.4022935829999,
-59.9116978933072));
#134188=CARTESIAN_POINT('Ctrl Pts',(-41.9619222489988,-64.3013426395998,
-60.153568971423));
#134189=CARTESIAN_POINT('Ctrl Pts',(-41.9651522214979,-64.2266573724653,
-60.2644967268053));
#134190=CARTESIAN_POINT('Ctrl Pts',(-41.9732193617859,-64.0401243516391,
-60.4496168355678));
#134191=CARTESIAN_POINT('Ctrl Pts',(-41.9780533572395,-63.9283499504973,
-60.5237363920413));
#134192=CARTESIAN_POINT('Ctrl Pts',(-41.9885935839755,-63.6846328137124,
-60.6239226729814));
#134193=CARTESIAN_POINT('Ctrl Pts',(-41.9942946417934,-63.5528097018572,
-60.64995));
#134194=CARTESIAN_POINT('Ctrl Pts',(-42.,-63.4208871539288,-60.64995));
#134195=CARTESIAN_POINT('Ctrl Pts',(-25.6564221286262,-65.8545847766702,
-55.74995));
#134196=CARTESIAN_POINT('Ctrl Pts',(-25.2,-65.8945165387074,-55.74995));
#134197=CARTESIAN_POINT('Ctrl Pts',(-25.2,-66.3526821257161,-55.74995));
#134198=CARTESIAN_POINT('Ctrl Pts',(-25.6564221285773,-65.8545847766745,
-55.5542114975488));
#134199=CARTESIAN_POINT('Ctrl Pts',(-25.1999999999616,-65.8945165387115,
-55.6441589529833));
#134200=CARTESIAN_POINT('Ctrl Pts',(-25.2,-66.3526821257202,-55.6520807487743));
#134201=CARTESIAN_POINT('Ctrl Pts',(-25.5974642419416,-65.8597429233806,
-55.3592003264656));
#134202=CARTESIAN_POINT('Ctrl Pts',(-25.1652351487286,-65.8975580690824,
-55.5387129880067));
#134203=CARTESIAN_POINT('Ctrl Pts',(-25.1705210566577,-66.3578402724271,
-55.5545751632329));
#134204=CARTESIAN_POINT('Ctrl Pts',(-25.3809306020242,-65.8786871621453,
-55.033477363834));
#134205=CARTESIAN_POINT('Ctrl Pts',(-25.0420941082282,-65.9083315141418,
-55.3693682972756));
#134206=CARTESIAN_POINT('Ctrl Pts',(-25.062254236699,-66.3767845111906,
-55.391713681917));
#134207=CARTESIAN_POINT('Ctrl Pts',(-25.2239370702218,-65.892422316425,
-54.9036397860402));
#134208=CARTESIAN_POINT('Ctrl Pts',(-24.9535760611327,-65.9160758397827,
-55.3059410651653));
#134209=CARTESIAN_POINT('Ctrl Pts',(-24.9837596261582,-66.3905192883359,
-55.3267957976874));
#134210=CARTESIAN_POINT('Ctrl Pts',(-25.043451507077,-65.9082127571302,
-54.8278826162281));
#134211=CARTESIAN_POINT('Ctrl Pts',(-24.8576734148988,-65.9244662341272,
-55.273872259957));
#134212=CARTESIAN_POINT('Ctrl Pts',(-24.8935146892254,-66.4063101061761,
-55.2889163081141));
#134213=CARTESIAN_POINT('',(-25.2,-66.3526821257161,-55.74995));
#134214=CARTESIAN_POINT('Origin',(-25.7,-66.3526821257161,-55.74995));
#134215=CARTESIAN_POINT('Ctrl Pts',(-25.2,-66.3526821257161,-55.74995));
#134216=CARTESIAN_POINT('Ctrl Pts',(-25.2,-66.3526821257202,-55.6520807487743));
#134217=CARTESIAN_POINT('Ctrl Pts',(-25.1705210566577,-66.3578402724271,
-55.5545751632329));
#134218=CARTESIAN_POINT('Ctrl Pts',(-25.062254236699,-66.3767845111906,
-55.391713681917));
#134219=CARTESIAN_POINT('Ctrl Pts',(-24.9837596261582,-66.3905192883359,
-55.3267957976874));
#134220=CARTESIAN_POINT('Ctrl Pts',(-24.8935146892254,-66.4063101061761,
-55.2889163081141));
#134221=CARTESIAN_POINT('Origin',(-25.7,-66.3526821257161,-52.64995));
#134222=CARTESIAN_POINT('',(-25.2,-66.3526821257161,-60.0322609860583));
#134223=CARTESIAN_POINT('Origin',(-25.7,-66.3526821257161,-60.0322609860583));
#134224=CARTESIAN_POINT('',(-25.2,-66.3526821257161,-55.24995));
#134225=CARTESIAN_POINT('Ctrl Pts',(-28.6150130758292,-64.5919217712362,
-60.64995));
#134226=CARTESIAN_POINT('Ctrl Pts',(-28.7021688185769,-65.588116469328,
-60.64995));
#134227=CARTESIAN_POINT('Ctrl Pts',(-28.7021688185769,-65.588116469328,
-59.64995));
#134228=CARTESIAN_POINT('Ctrl Pts',(-28.0991390263463,-64.7442358506513,
-60.64995));
#134229=CARTESIAN_POINT('Ctrl Pts',(-28.2033028175763,-65.6317615890315,
-60.5485267380177));
#134230=CARTESIAN_POINT('Ctrl Pts',(-28.1296330247306,-65.6382068607523,
-59.649950002333));
#134231=CARTESIAN_POINT('Ctrl Pts',(-27.584859681119,-64.89321892758,-60.6698497986403));
#134232=CARTESIAN_POINT('Ctrl Pts',(-27.6612478839793,-65.6791852507322,
-60.4928259381272));
#134233=CARTESIAN_POINT('Ctrl Pts',(-27.5637794550765,-65.6877126333127,
-59.6897495968387));
#134234=CARTESIAN_POINT('Ctrl Pts',(-26.5596543334024,-65.1843117452004,
-60.7464752559987));
#134235=CARTESIAN_POINT('Ctrl Pts',(-26.5839609508645,-65.7734356447442,
-60.477600868097));
#134236=CARTESIAN_POINT('Ctrl Pts',(-26.4448676457179,-65.7856047321169,
-59.8430005124393));
#134237=CARTESIAN_POINT('Ctrl Pts',(-26.0485518825385,-65.3264611076661,
-60.802611641644));
#134238=CARTESIAN_POINT('Ctrl Pts',(-26.0406038710994,-65.8209732294689,
-60.5097186566584));
#134239=CARTESIAN_POINT('Ctrl Pts',(-25.8914156146746,-65.8340255106386,
-59.9553384305595));
#134240=CARTESIAN_POINT('Ctrl Pts',(-25.5416884892005,-65.4644312001072,
-60.8848189055469));
#134241=CARTESIAN_POINT('Ctrl Pts',(-25.4903329393053,-65.86911569787,-60.5974971539929));
#134242=CARTESIAN_POINT('Ctrl Pts',(-25.3471476467368,-65.8816427877534,
-60.1196878110938));
#134243=CARTESIAN_POINT('',(-28.6150130758292,-64.5919217712362,-60.64995));
#134244=CARTESIAN_POINT('Origin',(-28.6150130758292,-64.5919217712362,-59.64995));
#134245=CARTESIAN_POINT('',(-25.559825688613,-65.4594929016036,-60.8818893816079));
#134246=CARTESIAN_POINT('Ctrl Pts',(-28.6150130758292,-64.5919217712362,
-60.64995));
#134247=CARTESIAN_POINT('Ctrl Pts',(-28.0991390263463,-64.7442358506513,
-60.64995));
#134248=CARTESIAN_POINT('Ctrl Pts',(-27.584859681119,-64.89321892758,-60.6698497986403));
#134249=CARTESIAN_POINT('Ctrl Pts',(-26.5657678476125,-65.1825758977617,
-60.7460183223478));
#134250=CARTESIAN_POINT('Ctrl Pts',(-26.0607433397739,-65.32306995879,-60.8012751647717));
#134251=CARTESIAN_POINT('Ctrl Pts',(-25.5598256882386,-65.4594929016689,
-60.8818893816956));
#134252=CARTESIAN_POINT('Ctrl Pts',(-25.6564221286262,-65.8545847766702,
-60.0322609860583));
#134253=CARTESIAN_POINT('Ctrl Pts',(-25.6369719721911,-65.8562864448621,
-60.1960022731895));
#134254=CARTESIAN_POINT('Ctrl Pts',(-25.6175094928883,-65.8217787894205,
-60.3603674876955));
#134255=CARTESIAN_POINT('Ctrl Pts',(-25.5836282597575,-65.6869336598766,
-60.6533188274199));
#134256=CARTESIAN_POINT('Ctrl Pts',(-25.5689423412454,-65.58489046904,-60.7845618642934));
#134257=CARTESIAN_POINT('Ctrl Pts',(-25.5598256882386,-65.4594929016689,
-60.8818893816956));
#134258=CARTESIAN_POINT('Origin',(-4.6996065532056,-66.6842487255793,-59.64995));
#134259=CARTESIAN_POINT('',(-31.35,-64.3526414204797,-60.64995));
#134260=CARTESIAN_POINT('',(-4.6996065532056,-66.6842487255793,-60.64995));
#134261=CARTESIAN_POINT('Ctrl Pts',(-31.35,-64.3526414204797,-60.64995));
#134262=CARTESIAN_POINT('Ctrl Pts',(-31.3442946417934,-64.4845639684081,
-60.64995));
#134263=CARTESIAN_POINT('Ctrl Pts',(-31.3385935839747,-64.6163870802633,
-60.6239226729814));
#134264=CARTESIAN_POINT('Ctrl Pts',(-31.3280533572402,-64.8601042170482,
-60.5237363920412));
#134265=CARTESIAN_POINT('Ctrl Pts',(-31.3232193617865,-64.9718786181899,
-60.4496168355678));
#134266=CARTESIAN_POINT('Ctrl Pts',(-31.3151522214972,-65.1584116390162,
-60.2644967268053));
#134267=CARTESIAN_POINT('Ctrl Pts',(-31.3119222489988,-65.2330969061508,
-60.1535689714229));
#134268=CARTESIAN_POINT('Ctrl Pts',(-31.3075563441358,-65.3340478495507,
-59.9116978933073));
#134269=CARTESIAN_POINT('Ctrl Pts',(-31.3064221286269,-65.3602738277488,
-59.7808732880376));
#134270=CARTESIAN_POINT('Ctrl Pts',(-31.3064221286262,-65.3602738277489,
-59.64995));
#134271=CARTESIAN_POINT('Origin',(-31.35,-65.8583711767947,-52.64995));
#134272=CARTESIAN_POINT('',(-31.85,-65.8583711767947,-59.64995));
#134273=CARTESIAN_POINT('Origin',(-31.35,-65.8583711767947,-59.64995));
#134274=CARTESIAN_POINT('',(-31.85,-65.8583711767947,-55.74995));
#134275=CARTESIAN_POINT('Origin',(-31.35,-65.8583711767947,-55.74995));
#134276=CARTESIAN_POINT('',(-31.85,-65.8583711767947,-55.24995));
#134277=CARTESIAN_POINT('Ctrl Pts',(-32.3064221286262,-65.2727851642229,
-54.74995));
#134278=CARTESIAN_POINT('Ctrl Pts',(-32.3064221286261,-65.2727851642229,
-55.24995));
#134279=CARTESIAN_POINT('Ctrl Pts',(-32.35,-65.7708825132688,-55.24995));
#134280=CARTESIAN_POINT('Ctrl Pts',(-32.0438874372397,-65.2957539735015,
-54.7499500000659));
#134281=CARTESIAN_POINT('Ctrl Pts',(-32.172075011829,-65.2845390139115,
-55.2615708605686));
#134282=CARTESIAN_POINT('Ctrl Pts',(-32.2187326543062,-65.7938513225456,
-55.24995));
#134283=CARTESIAN_POINT('Ctrl Pts',(-31.7844354391267,-65.3184530820656,
-54.8577231271254));
#134284=CARTESIAN_POINT('Ctrl Pts',(-32.0533393021413,-65.2949270424741,
-55.3274496218431));
#134285=CARTESIAN_POINT('Ctrl Pts',(-32.0890066552503,-65.8165504311115,
-55.3038365635632));
#134286=CARTESIAN_POINT('Ctrl Pts',(-31.4141952557525,-65.3508449008926,
-55.2279633105016));
#134287=CARTESIAN_POINT('Ctrl Pts',(-31.8917246342956,-65.3090664937689,
-55.5133819370971));
#134288=CARTESIAN_POINT('Ctrl Pts',(-31.9038865635631,-65.8489422499384,
-55.4889566552503));
#134289=CARTESIAN_POINT('Ctrl Pts',(-31.3064221286917,-65.3602738277431,
-55.4874153086129));
#134290=CARTESIAN_POINT('Ctrl Pts',(-31.8500000000045,-65.3127169262546,
-55.6317784220497));
#134291=CARTESIAN_POINT('Ctrl Pts',(-31.85,-65.8583711767893,-55.6186826543066));
#134292=CARTESIAN_POINT('Ctrl Pts',(-31.3064221286262,-65.3602738277489,
-55.74995));
#134293=CARTESIAN_POINT('Ctrl Pts',(-31.85,-65.3127169262601,-55.74995));
#134294=CARTESIAN_POINT('Ctrl Pts',(-31.85,-65.8583711767947,-55.74995));
#134295=CARTESIAN_POINT('',(-32.35,-65.7708825132688,-55.24995));
#134296=CARTESIAN_POINT('Origin',(-32.35,-65.7708825132688,-54.74995));
#134297=CARTESIAN_POINT('Ctrl Pts',(-32.35,-65.7708825132688,-55.24995));
#134298=CARTESIAN_POINT('Ctrl Pts',(-32.2187326543062,-65.7938513225456,
-55.24995));
#134299=CARTESIAN_POINT('Ctrl Pts',(-32.0890066552503,-65.8165504311115,
-55.3038365635632));
#134300=CARTESIAN_POINT('Ctrl Pts',(-31.9038865635631,-65.8489422499384,
-55.4889566552503));
#134301=CARTESIAN_POINT('Ctrl Pts',(-31.85,-65.8583711767893,-55.6186826543066));
#134302=CARTESIAN_POINT('Ctrl Pts',(-31.85,-65.8583711767947,-55.74995));
#134303=CARTESIAN_POINT('Origin',(-44.2377516955329,-64.7308390050988,-54.74995));
#134304=CARTESIAN_POINT('',(-32.85,-65.7271381815059,-55.24995));
#134305=CARTESIAN_POINT('Origin',(-32.85,-65.7271381815059,-54.74995));
#134306=CARTESIAN_POINT('',(-40.7958880023324,-65.0319630596553,-55.24995));
#134307=CARTESIAN_POINT('Ctrl Pts',(-33.8064221286261,-65.1415521689341,
-55.74995));
#134308=CARTESIAN_POINT('Ctrl Pts',(-33.3499999999999,-65.1814839309712,
-55.74995));
#134309=CARTESIAN_POINT('Ctrl Pts',(-33.35,-65.63964951798,-55.74995));
#134310=CARTESIAN_POINT('Ctrl Pts',(-33.8064221285606,-65.1415521689398,
-55.487415308613));
#134311=CARTESIAN_POINT('Ctrl Pts',(-33.3499999999488,-65.1814839309712,
-55.607847808877));
#134312=CARTESIAN_POINT('Ctrl Pts',(-33.35,-65.6396495179854,-55.6186826543062));
#134313=CARTESIAN_POINT('Ctrl Pts',(-33.6986490015007,-65.1509810957903,
-55.2279633105015));
#134314=CARTESIAN_POINT('Ctrl Pts',(-33.2858662151155,-65.1870949100978,
-55.4680441063706));
#134315=CARTESIAN_POINT('Ctrl Pts',(-33.2961134364373,-65.6490784448363,
-55.4889566552507));
#134316=CARTESIAN_POINT('Ctrl Pts',(-33.3284088181247,-65.1833729146174,
-54.8577231271255));
#134317=CARTESIAN_POINT('Ctrl Pts',(-33.0786175782532,-65.2052268163542,
-55.2822894538758));
#134318=CARTESIAN_POINT('Ctrl Pts',(-33.1109933447493,-65.6814702636632,
-55.3038365635628));
#134319=CARTESIAN_POINT('Ctrl Pts',(-33.0689568200132,-65.2060720231813,
-54.7499500000659));
#134320=CARTESIAN_POINT('Ctrl Pts',(-32.9369589695398,-65.2176203387053,
-55.2386587236917));
#134321=CARTESIAN_POINT('Ctrl Pts',(-32.981267345694,-65.704169372229,-55.24995));
#134322=CARTESIAN_POINT('Ctrl Pts',(-32.8064221286262,-65.22904083246,-54.74995));
#134323=CARTESIAN_POINT('Ctrl Pts',(-32.8064221286261,-65.22904083246,-55.24995));
#134324=CARTESIAN_POINT('Ctrl Pts',(-32.85,-65.7271381815059,-55.24995));
#134325=CARTESIAN_POINT('',(-33.35,-65.63964951798,-55.74995));
#134326=CARTESIAN_POINT('Origin',(-33.85,-65.63964951798,-55.74995));
#134327=CARTESIAN_POINT('Ctrl Pts',(-33.35,-65.63964951798,-55.74995));
#134328=CARTESIAN_POINT('Ctrl Pts',(-33.35,-65.6396495179854,-55.6186826543062));
#134329=CARTESIAN_POINT('Ctrl Pts',(-33.2961134364373,-65.6490784448363,
-55.4889566552507));
#134330=CARTESIAN_POINT('Ctrl Pts',(-33.1109933447493,-65.6814702636632,
-55.3038365635628));
#134331=CARTESIAN_POINT('Ctrl Pts',(-32.981267345694,-65.704169372229,-55.24995));
#134332=CARTESIAN_POINT('Ctrl Pts',(-32.85,-65.7271381815059,-55.24995));
#134333=CARTESIAN_POINT('Origin',(-33.85,-65.63964951798,-52.64995));
#134334=CARTESIAN_POINT('',(-33.35,-65.63964951798,-59.64995));
#134335=CARTESIAN_POINT('Origin',(-33.85,-65.63964951798,-59.64995));
#134336=CARTESIAN_POINT('',(-33.35,-65.63964951798,-55.24995));
#134337=CARTESIAN_POINT('Origin',(-47.0226009489055,-59.9901009689335,-59.64995));
#134338=CARTESIAN_POINT('',(-47.0226009489055,-59.9901009689335,-60.64995));
#134339=CARTESIAN_POINT('Ctrl Pts',(-25.3802177275058,39.943749490528,-60.1097730249189));
#134340=CARTESIAN_POINT('Ctrl Pts',(-25.5227862062494,39.9312763648619,
-60.5923862926587));
#134341=CARTESIAN_POINT('Ctrl Pts',(-25.572468850428,39.5210489290882,-60.8798615124595));
#134342=CARTESIAN_POINT('Ctrl Pts',(-25.1089972874034,39.9674782043536,
-60.2066542280814));
#134343=CARTESIAN_POINT('Ctrl Pts',(-25.2414738675095,39.9482243711148,
-60.6373384822398));
#134344=CARTESIAN_POINT('Ctrl Pts',(-25.2694477113958,39.6036052974814,
-60.9283242463865));
#134345=CARTESIAN_POINT('Ctrl Pts',(-24.8422602775208,40.0127575956439,
-60.3032659617329));
#134346=CARTESIAN_POINT('Ctrl Pts',(-24.9493186357974,39.9900159541718,
-60.6937268873635));
#134347=CARTESIAN_POINT('Ctrl Pts',(-24.9650212889786,39.6997861053784,
-60.9766079791613));
#134348=CARTESIAN_POINT('Ctrl Pts',(-24.3096510677746,40.1491089179394,
-60.4514911807313));
#134349=CARTESIAN_POINT('Ctrl Pts',(-24.3665512677474,40.1299777240875,
-60.7838744940585));
#134350=CARTESIAN_POINT('Ctrl Pts',(-24.3438778196125,39.9224728282123,
-61.0507205920708));
#134351=CARTESIAN_POINT('Ctrl Pts',(-24.0409609718932,40.24165543605,-60.5010370503254));
#134352=CARTESIAN_POINT('Ctrl Pts',(-24.0669512606435,40.2300655352942,
-60.8169267274199));
#134353=CARTESIAN_POINT('Ctrl Pts',(-24.0238031468177,40.0506166841414,
-61.0754935252291));
#134354=CARTESIAN_POINT('Ctrl Pts',(-23.7796330855957,40.3581899105085,
-60.5010370523946));
#134355=CARTESIAN_POINT('Ctrl Pts',(-23.7796330855957,40.3581899105084,
-60.8169267287601));
#134356=CARTESIAN_POINT('Ctrl Pts',(-23.7057274034393,40.1924568448808,
-61.0754935261973));
#134357=CARTESIAN_POINT('',(-25.572468850428,39.5210489290882,-60.8798615124594));
#134358=CARTESIAN_POINT('Origin',(-25.2930619847582,38.9475547924363,-60.1097730249189));
#134359=CARTESIAN_POINT('Ctrl Pts',(-23.7057274034393,40.1924568448808,
-61.0754935261973));
#134360=CARTESIAN_POINT('Ctrl Pts',(-24.0238031468177,40.0506166841414,
-61.0754935252291));
#134361=CARTESIAN_POINT('Ctrl Pts',(-24.3438778196125,39.9224728282123,
-61.0507205920708));
#134362=CARTESIAN_POINT('Ctrl Pts',(-24.9650212889786,39.6997861053784,
-60.9766079791613));
#134363=CARTESIAN_POINT('Ctrl Pts',(-25.2694477113958,39.6036052974814,
-60.9283242463865));
#134364=CARTESIAN_POINT('Ctrl Pts',(-25.572468850428,39.5210489290882,-60.8798615124594));
#134365=CARTESIAN_POINT('Origin',(-4.69960655320655,40.7492486855235,-59.64995));
#134366=CARTESIAN_POINT('',(-31.,38.4482624126576,-60.64995));
#134367=CARTESIAN_POINT('',(-37.,37.923330431502,-60.64995));
#134368=CARTESIAN_POINT('',(-4.69960655320655,40.7492486855235,-60.64995));
#134369=CARTESIAN_POINT('Ctrl Pts',(-36.9564221286262,38.9309628387712,
-59.64995));
#134370=CARTESIAN_POINT('Ctrl Pts',(-36.9564221286271,38.9309628387711,
-59.7808732880376));
#134371=CARTESIAN_POINT('Ctrl Pts',(-36.9575563441365,38.904736860573,-59.9116978933072));
#134372=CARTESIAN_POINT('Ctrl Pts',(-36.9619222489981,38.8037859171731,
-60.153568971423));
#134373=CARTESIAN_POINT('Ctrl Pts',(-36.9651522214979,38.7291006500388,
-60.2644967268049));
#134374=CARTESIAN_POINT('Ctrl Pts',(-36.9732193617859,38.5425676292119,
-60.4496168355682));
#134375=CARTESIAN_POINT('Ctrl Pts',(-36.9780533572402,38.4307932280718,
-60.5237363920407));
#134376=CARTESIAN_POINT('Ctrl Pts',(-36.9885935839748,38.1870760912844,
-60.6239226729819));
#134377=CARTESIAN_POINT('Ctrl Pts',(-36.9942946417934,38.0552529794313,
-60.64995));
#134378=CARTESIAN_POINT('Ctrl Pts',(-37.,37.923330431502,-60.64995));
#134379=CARTESIAN_POINT('Ctrl Pts',(-31.,38.4482624126576,-60.64995));
#134380=CARTESIAN_POINT('Ctrl Pts',(-30.994294641792,38.5801849605867,-60.64995));
#134381=CARTESIAN_POINT('Ctrl Pts',(-30.9885935839752,38.71200807244,-60.6239226729818));
#134382=CARTESIAN_POINT('Ctrl Pts',(-30.9780533572398,38.9557252092273,
-60.5237363920407));
#134383=CARTESIAN_POINT('Ctrl Pts',(-30.9732193617862,39.0674996103677,
-60.4496168355678));
#134384=CARTESIAN_POINT('Ctrl Pts',(-30.9651522214976,39.2540326311941,
-60.2644967268053));
#134385=CARTESIAN_POINT('Ctrl Pts',(-30.9619222489984,39.3287178983286,
-60.153568971423));
#134386=CARTESIAN_POINT('Ctrl Pts',(-30.9575563441362,39.4296688417285,
-59.9116978933072));
#134387=CARTESIAN_POINT('Ctrl Pts',(-30.9564221286278,39.4558948199266,
-59.7808732880376));
#134388=CARTESIAN_POINT('Ctrl Pts',(-30.9564221286262,39.4558948199267,
-59.64995));
#134389=CARTESIAN_POINT('Origin',(-31.,39.9539921689726,-52.64995));
#134390=CARTESIAN_POINT('',(-30.5,39.9539921689726,-55.74995));
#134391=CARTESIAN_POINT('Origin',(-31.,39.9539921689726,-55.74995));
#134392=CARTESIAN_POINT('',(-30.5,39.9539921689726,-59.64995));
#134393=CARTESIAN_POINT('',(-30.5,39.9539921689726,-92.34995));
#134394=CARTESIAN_POINT('Origin',(-31.,39.9539921689726,-59.64995));
#134395=CARTESIAN_POINT('Ctrl Pts',(-29.9564221286262,39.5433834834526,
-54.74995));
#134396=CARTESIAN_POINT('Ctrl Pts',(-29.9564221286262,39.5433834834526,
-55.24995));
#134397=CARTESIAN_POINT('Ctrl Pts',(-30.,40.0414808324985,-55.24995));
#134398=CARTESIAN_POINT('Ctrl Pts',(-30.218956820013,39.520414674174,-54.7499500000658));
#134399=CARTESIAN_POINT('Ctrl Pts',(-30.0869589695403,39.5319629897042,
-55.2386587236916));
#134400=CARTESIAN_POINT('Ctrl Pts',(-30.131267345694,40.0185120232214,-55.24995));
#134401=CARTESIAN_POINT('Ctrl Pts',(-30.4784088181251,39.4977155656101,
-54.8577231271254));
#134402=CARTESIAN_POINT('Ctrl Pts',(-30.2286175782536,39.5195694673468,
-55.2822894538777));
#134403=CARTESIAN_POINT('Ctrl Pts',(-30.2609933447492,39.9958129146559,
-55.3038365635627));
#134404=CARTESIAN_POINT('Ctrl Pts',(-30.8486490015003,39.4653237467829,
-55.2279633105015));
#134405=CARTESIAN_POINT('Ctrl Pts',(-30.4358662151152,39.5014375610904,
-55.4680441063689));
#134406=CARTESIAN_POINT('Ctrl Pts',(-30.4461134364373,39.9634210958289,
-55.4889566552508));
#134407=CARTESIAN_POINT('Ctrl Pts',(-30.9564221285606,39.4558948199325,
-55.4874153086129));
#134408=CARTESIAN_POINT('Ctrl Pts',(-30.4999999999484,39.4958265819666,
-55.6078478088783));
#134409=CARTESIAN_POINT('Ctrl Pts',(-30.5,39.9539921689781,-55.6186826543063));
#134410=CARTESIAN_POINT('Ctrl Pts',(-30.9564221286262,39.4558948199267,
-55.74995));
#134411=CARTESIAN_POINT('Ctrl Pts',(-30.5,39.4958265819639,-55.74995));
#134412=CARTESIAN_POINT('Ctrl Pts',(-30.5,39.9539921689726,-55.74995));
#134413=CARTESIAN_POINT('',(-30.,40.0414808324985,-55.24995));
#134414=CARTESIAN_POINT('Origin',(-30.,40.0414808324985,-54.74995));
#134415=CARTESIAN_POINT('Ctrl Pts',(-30.,40.0414808324985,-55.24995));
#134416=CARTESIAN_POINT('Ctrl Pts',(-30.131267345694,40.0185120232214,-55.24995));
#134417=CARTESIAN_POINT('Ctrl Pts',(-30.2609933447492,39.9958129146559,
-55.3038365635627));
#134418=CARTESIAN_POINT('Ctrl Pts',(-30.4461134364373,39.9634210958289,
-55.4889566552508));
#134419=CARTESIAN_POINT('Ctrl Pts',(-30.5,39.9539921689781,-55.6186826543063));
#134420=CARTESIAN_POINT('Ctrl Pts',(-30.5,39.9539921689726,-55.74995));
#134421=CARTESIAN_POINT('Origin',(-3.70444879364117,42.3420434642203,-54.74995));
#134422=CARTESIAN_POINT('',(-29.5,40.0852251642615,-55.24995));
#134423=CARTESIAN_POINT('Origin',(-29.5,40.0852251642615,-54.74995));
#134424=CARTESIAN_POINT('',(-30.0435778713739,40.0376682627727,-55.24995));
#134425=CARTESIAN_POINT('Ctrl Pts',(-28.4564221286262,39.6746164787415,
-55.74995));
#134426=CARTESIAN_POINT('Ctrl Pts',(-29.,39.6270595772528,-55.74995));
#134427=CARTESIAN_POINT('Ctrl Pts',(-29.,40.1727138277873,-55.74995));
#134428=CARTESIAN_POINT('Ctrl Pts',(-28.4564221286917,39.6746164787358,
-55.487415308613));
#134429=CARTESIAN_POINT('Ctrl Pts',(-29.0000000000046,39.6270595772536,
-55.6317784220498));
#134430=CARTESIAN_POINT('Ctrl Pts',(-29.,40.1727138277819,-55.6186826543062));
#134431=CARTESIAN_POINT('Ctrl Pts',(-28.5641952557521,39.6651875518853,
-55.2279633105015));
#134432=CARTESIAN_POINT('Ctrl Pts',(-29.0417246342951,39.6234091447624,
-55.5133819370971));
#134433=CARTESIAN_POINT('Ctrl Pts',(-29.0538865635627,40.163284900931,-55.4889566552507));
#134434=CARTESIAN_POINT('Ctrl Pts',(-28.9344354391272,39.6327957330582,
-54.8577231271255));
#134435=CARTESIAN_POINT('Ctrl Pts',(-29.2033393021417,39.6092696934658,
-55.3274496218431));
#134436=CARTESIAN_POINT('Ctrl Pts',(-29.2390066552507,40.1308930821041,
-55.3038365635627));
#134437=CARTESIAN_POINT('Ctrl Pts',(-29.1938874372395,39.6100966244942,
-54.7499500000658));
#134438=CARTESIAN_POINT('Ctrl Pts',(-29.3220750118295,39.5988816649146,
-55.2615708605689));
#134439=CARTESIAN_POINT('Ctrl Pts',(-29.368732654306,40.1081939735386,-55.24995));
#134440=CARTESIAN_POINT('Ctrl Pts',(-29.4564221286262,39.5871278152156,
-54.74995));
#134441=CARTESIAN_POINT('Ctrl Pts',(-29.4564221286262,39.5871278152156,
-55.24995));
#134442=CARTESIAN_POINT('Ctrl Pts',(-29.5,40.0852251642615,-55.24995));
#134443=CARTESIAN_POINT('',(-29.,40.1727138277873,-55.74995));
#134444=CARTESIAN_POINT('Origin',(-28.5,40.1727138277873,-55.74995));
#134445=CARTESIAN_POINT('Ctrl Pts',(-29.,40.1727138277873,-55.74995));
#134446=CARTESIAN_POINT('Ctrl Pts',(-29.,40.1727138277819,-55.6186826543062));
#134447=CARTESIAN_POINT('Ctrl Pts',(-29.0538865635627,40.163284900931,-55.4889566552507));
#134448=CARTESIAN_POINT('Ctrl Pts',(-29.2390066552507,40.1308930821041,
-55.3038365635627));
#134449=CARTESIAN_POINT('Ctrl Pts',(-29.368732654306,40.1081939735386,-55.24995));
#134450=CARTESIAN_POINT('Ctrl Pts',(-29.5,40.0852251642615,-55.24995));
#134451=CARTESIAN_POINT('Origin',(-28.5,40.1727138277873,-52.64995));
#134452=CARTESIAN_POINT('',(-29.,40.1727138277873,-59.6524466674074));
#134453=CARTESIAN_POINT('Origin',(-28.5,40.1727138277873,-59.6524466674074));
#134454=CARTESIAN_POINT('',(-29.,40.1727138277874,-92.34995));
#134455=CARTESIAN_POINT('Ctrl Pts',(-25.572468850428,39.5210489290882,-60.8798615124595));
#134456=CARTESIAN_POINT('Ctrl Pts',(-25.5227862062494,39.9312763648619,
-60.5923862926587));
#134457=CARTESIAN_POINT('Ctrl Pts',(-25.3802177275058,39.9437494905281,
-60.1097730249189));
#134458=CARTESIAN_POINT('Ctrl Pts',(-26.059719336348,39.3883003271754,-60.8019346414671));
#134459=CARTESIAN_POINT('Ctrl Pts',(-26.0512576071349,39.8850411082851,
-60.5102318318317));
#134460=CARTESIAN_POINT('Ctrl Pts',(-25.9036128690389,39.8979583490994,
-59.9539737371434));
#134461=CARTESIAN_POINT('Ctrl Pts',(-26.5494003841727,39.2520983829515,
-60.748049450926));
#134462=CARTESIAN_POINT('Ctrl Pts',(-26.5712796028832,39.8395450788764,
-60.4792397999495));
#134463=CARTESIAN_POINT('Ctrl Pts',(-26.4338688782163,39.8515669595299,
-59.8461489023585));
#134464=CARTESIAN_POINT('Ctrl Pts',(-27.529498834359,38.9740545371747,-60.6732320595124));
#134465=CARTESIAN_POINT('Ctrl Pts',(-27.601298997848,39.7494300586015,-60.4901498725136));
#134466=CARTESIAN_POINT('Ctrl Pts',(-27.5031785292772,39.7580144872632,
-59.6965141185183));
#134467=CARTESIAN_POINT('Ctrl Pts',(-28.0200529940657,38.8321810243987,
-60.6528294999755));
#134468=CARTESIAN_POINT('Ctrl Pts',(-28.1179039179461,39.7042329845701,
-60.5392590138154));
#134469=CARTESIAN_POINT('Ctrl Pts',(-28.0425516254864,39.710825455934,-59.6557090289434));
#134470=CARTESIAN_POINT('Ctrl Pts',(-28.5109323535812,38.6876131939284,
-60.6502266229092));
#134471=CARTESIAN_POINT('Ctrl Pts',(-28.5960141520618,39.6624037591722,
-60.6291816703115));
#134472=CARTESIAN_POINT('Ctrl Pts',(-28.5867228014573,39.663216647019,-59.6505032458185));
#134473=CARTESIAN_POINT('',(-28.4933647440941,38.6927858841383,-60.6503275731476));
#134474=CARTESIAN_POINT('Ctrl Pts',(-25.572468850428,39.5210489290882,-60.8798615124594));
#134475=CARTESIAN_POINT('Ctrl Pts',(-26.059719336348,39.3883003271754,-60.8019346414671));
#134476=CARTESIAN_POINT('Ctrl Pts',(-26.5494003841727,39.2520983829515,
-60.748049450926));
#134477=CARTESIAN_POINT('Ctrl Pts',(-27.5236528204355,38.9757129911733,
-60.673678324387));
#134478=CARTESIAN_POINT('Ctrl Pts',(-28.0083489909001,38.8355655623354,
-60.6533187024567));
#134479=CARTESIAN_POINT('Ctrl Pts',(-28.4933647440612,38.6927858841383,
-60.650327573148));
#134480=CARTESIAN_POINT('Ctrl Pts',(-28.4564221286262,39.6746164787415,
-59.6524466674074));
#134481=CARTESIAN_POINT('Ctrl Pts',(-28.4551199545093,39.6747304042147,
-59.7821590925224));
#134482=CARTESIAN_POINT('Ctrl Pts',(-28.4548707416055,39.6494517959669,
-59.9101257001469));
#134483=CARTESIAN_POINT('Ctrl Pts',(-28.4563005932054,39.5761796095201,
-60.0890325252997));
#134484=CARTESIAN_POINT('Ctrl Pts',(-28.4570887248156,39.5455314661108,
-60.1469471546371));
#134485=CARTESIAN_POINT('Ctrl Pts',(-28.4592438293891,39.4746917169037,
-60.2541491598715));
#134486=CARTESIAN_POINT('Ctrl Pts',(-28.4606134496588,39.434276061177,-60.3041245704241));
#134487=CARTESIAN_POINT('Ctrl Pts',(-28.465656656414,39.2976315760154,-60.4428805969007));
#134488=CARTESIAN_POINT('Ctrl Pts',(-28.4702284641343,39.1877232210837,
-60.5175376561534));
#134489=CARTESIAN_POINT('Ctrl Pts',(-28.4808526630789,38.9512642676271,
-60.6191174333591));
#134490=CARTESIAN_POINT('Ctrl Pts',(-28.4870505338491,38.8213938162437,
-60.647315885492));
#134491=CARTESIAN_POINT('Ctrl Pts',(-28.4933647440612,38.6927858841383,
-60.650327573148));
#134492=CARTESIAN_POINT('Origin',(-4.69960655320655,40.7492486855235,-59.64995));
#134493=CARTESIAN_POINT('',(-39.5,37.7046087726872,-60.64995));
#134494=CARTESIAN_POINT('',(-4.69960655320655,40.7492486855235,-60.64995));
#134495=CARTESIAN_POINT('Ctrl Pts',(-39.5,37.7046087726872,-60.64995));
#134496=CARTESIAN_POINT('Ctrl Pts',(-39.4942946417934,37.8365313206165,
-60.64995));
#134497=CARTESIAN_POINT('Ctrl Pts',(-39.4885935839755,37.9683544324696,
-60.6239226729818));
#134498=CARTESIAN_POINT('Ctrl Pts',(-39.4780533572395,38.2120715692569,
-60.5237363920407));
#134499=CARTESIAN_POINT('Ctrl Pts',(-39.4732193617859,38.3238459703974,
-60.4496168355678));
#134500=CARTESIAN_POINT('Ctrl Pts',(-39.4651522214979,38.5103789912237,
-60.2644967268053));
#134501=CARTESIAN_POINT('Ctrl Pts',(-39.4619222489988,38.5850642583582,
-60.153568971423));
#134502=CARTESIAN_POINT('Ctrl Pts',(-39.4575563441359,38.6860152017583,
-59.9116978933072));
#134503=CARTESIAN_POINT('Ctrl Pts',(-39.4564221286291,38.7122411799561,
-59.7808732880376));
#134504=CARTESIAN_POINT('Ctrl Pts',(-39.4564221286262,38.7122411799564,
-59.64995));
#134505=CARTESIAN_POINT('Origin',(-39.5,39.2103385290023,-129.34995));
#134506=CARTESIAN_POINT('',(-39.,39.2103385290022,-59.64995));
#134507=CARTESIAN_POINT('Origin',(-39.5,39.2103385290022,-59.64995));
#134508=CARTESIAN_POINT('',(-39.,39.2103385290022,-55.74995));
#134509=CARTESIAN_POINT('Origin',(-39.5,39.2103385290022,-55.74995));
#134510=CARTESIAN_POINT('',(-39.,39.2103385290022,-59.64995));
#134511=CARTESIAN_POINT('Ctrl Pts',(-38.4564221286262,38.7997298434823,
-54.74995));
#134512=CARTESIAN_POINT('Ctrl Pts',(-38.4564221286261,38.7997298434823,
-55.2499499999999));
#134513=CARTESIAN_POINT('Ctrl Pts',(-38.5,39.2978271925282,-55.24995));
#134514=CARTESIAN_POINT('Ctrl Pts',(-38.7189568200132,38.7767610342036,
-54.7499500000658));
#134515=CARTESIAN_POINT('Ctrl Pts',(-38.5869589695399,38.788309349734,-55.2386587236917));
#134516=CARTESIAN_POINT('Ctrl Pts',(-38.6312673456941,39.2748583832512,
-55.24995));
#134517=CARTESIAN_POINT('Ctrl Pts',(-38.9784088181247,38.7540619256397,
-54.8577231271255));
#134518=CARTESIAN_POINT('Ctrl Pts',(-38.7286175782541,38.7759158273764,
-55.2822894538767));
#134519=CARTESIAN_POINT('Ctrl Pts',(-38.7609933447493,39.2521592746855,
-55.3038365635627));
#134520=CARTESIAN_POINT('Ctrl Pts',(-39.3486490015007,38.7216701068126,
-55.2279633105015));
#134521=CARTESIAN_POINT('Ctrl Pts',(-38.9358662151147,38.7577839211201,
-55.4680441063697));
#134522=CARTESIAN_POINT('Ctrl Pts',(-38.9461134364373,39.2197674558585,
-55.4889566552507));
#134523=CARTESIAN_POINT('Ctrl Pts',(-39.4564221285606,38.7122411799621,
-55.487415308613));
#134524=CARTESIAN_POINT('Ctrl Pts',(-38.9999999999489,38.7521729419962,
-55.6078478088777));
#134525=CARTESIAN_POINT('Ctrl Pts',(-39.,39.2103385290077,-55.6186826543063));
#134526=CARTESIAN_POINT('Ctrl Pts',(-39.4564221286262,38.7122411799564,
-55.74995));
#134527=CARTESIAN_POINT('Ctrl Pts',(-39.,38.7521729419935,-55.74995));
#134528=CARTESIAN_POINT('Ctrl Pts',(-39.,39.2103385290022,-55.74995));
#134529=CARTESIAN_POINT('',(-38.5,39.2978271925282,-55.24995));
#134530=CARTESIAN_POINT('Origin',(-38.5,39.2978271925282,-54.74995));
#134531=CARTESIAN_POINT('Ctrl Pts',(-38.5,39.2978271925282,-55.24995));
#134532=CARTESIAN_POINT('Ctrl Pts',(-38.6312673456941,39.2748583832512,
-55.24995));
#134533=CARTESIAN_POINT('Ctrl Pts',(-38.7609933447493,39.2521592746855,
-55.3038365635627));
#134534=CARTESIAN_POINT('Ctrl Pts',(-38.9461134364373,39.2197674558585,
-55.4889566552507));
#134535=CARTESIAN_POINT('Ctrl Pts',(-39.,39.2103385290077,-55.6186826543063));
#134536=CARTESIAN_POINT('Ctrl Pts',(-39.,39.2103385290022,-55.74995));
#134537=CARTESIAN_POINT('Origin',(-3.70444879364117,42.3420434642203,-54.74995));
#134538=CARTESIAN_POINT('',(-38.,39.3415715242911,-55.24995));
#134539=CARTESIAN_POINT('Origin',(-38.,39.3415715242911,-54.74995));
#134540=CARTESIAN_POINT('',(-38.5435778713738,39.2940146228024,-55.24995));
#134541=CARTESIAN_POINT('Ctrl Pts',(-36.9564221286262,38.9309628387712,
-55.74995));
#134542=CARTESIAN_POINT('Ctrl Pts',(-37.5000000000001,38.8834059372824,
-55.74995));
#134543=CARTESIAN_POINT('Ctrl Pts',(-37.5,39.4290601878171,-55.74995));
#134544=CARTESIAN_POINT('Ctrl Pts',(-36.9564221286917,38.9309628387654,
-55.487415308613));
#134545=CARTESIAN_POINT('Ctrl Pts',(-37.5000000000036,38.8834059372834,
-55.6317784220504));
#134546=CARTESIAN_POINT('Ctrl Pts',(-37.5,39.4290601878116,-55.6186826543065));
#134547=CARTESIAN_POINT('Ctrl Pts',(-37.0641952557516,38.9215339119149,
-55.2279633105015));
#134548=CARTESIAN_POINT('Ctrl Pts',(-37.5417246342956,38.879755504792,-55.5133819370962));
#134549=CARTESIAN_POINT('Ctrl Pts',(-37.5538865635632,39.4196312609607,
-55.4889566552503));
#134550=CARTESIAN_POINT('Ctrl Pts',(-37.4344354391277,38.8891420930878,
-54.8577231271255));
#134551=CARTESIAN_POINT('Ctrl Pts',(-37.7033393021412,38.8656160534955,
-55.3274496218441));
#134552=CARTESIAN_POINT('Ctrl Pts',(-37.7390066552503,39.3872394421337,
-55.3038365635632));
#134553=CARTESIAN_POINT('Ctrl Pts',(-37.6938874372391,38.8664429845239,
-54.7499500000658));
#134554=CARTESIAN_POINT('Ctrl Pts',(-37.8220750118298,38.855228024944,-55.2615708605686));
#134555=CARTESIAN_POINT('Ctrl Pts',(-37.8687326543062,39.3645403335679,
-55.24995));
#134556=CARTESIAN_POINT('Ctrl Pts',(-37.9564221286262,38.8434741752452,
-54.74995));
#134557=CARTESIAN_POINT('Ctrl Pts',(-37.9564221286261,38.8434741752452,
-55.2499499999999));
#134558=CARTESIAN_POINT('Ctrl Pts',(-38.,39.3415715242911,-55.24995));
#134559=CARTESIAN_POINT('',(-37.5,39.4290601878171,-55.74995));
#134560=CARTESIAN_POINT('Origin',(-37.,39.4290601878171,-55.74995));
#134561=CARTESIAN_POINT('Ctrl Pts',(-37.5,39.4290601878171,-55.74995));
#134562=CARTESIAN_POINT('Ctrl Pts',(-37.5,39.4290601878116,-55.6186826543065));
#134563=CARTESIAN_POINT('Ctrl Pts',(-37.5538865635632,39.4196312609607,
-55.4889566552503));
#134564=CARTESIAN_POINT('Ctrl Pts',(-37.7390066552503,39.3872394421337,
-55.3038365635632));
#134565=CARTESIAN_POINT('Ctrl Pts',(-37.8687326543062,39.3645403335679,
-55.24995));
#134566=CARTESIAN_POINT('Ctrl Pts',(-38.,39.3415715242911,-55.24995));
#134567=CARTESIAN_POINT('Origin',(-37.,39.4290601878171,-92.34995));
#134568=CARTESIAN_POINT('',(-37.5,39.429060187817,-59.64995));
#134569=CARTESIAN_POINT('Origin',(-37.,39.4290601878171,-59.64995));
#134570=CARTESIAN_POINT('',(-37.5,39.4290601878171,-92.34995));
#134571=CARTESIAN_POINT('Origin',(-47.0226009489055,34.0551009288773,-59.64995));
#134572=CARTESIAN_POINT('',(-47.0226009489055,34.0551009288773,-60.64995));
#134573=CARTESIAN_POINT('Origin',(-53.7167487055517,-8.26789346682159,-59.64995));
#134574=CARTESIAN_POINT('',(-50.6819512673597,26.41999998,-60.64995));
#134575=CARTESIAN_POINT('',(-51.1762622162812,20.76999998,-60.64995));
#134576=CARTESIAN_POINT('',(-53.7167487055517,-8.26789346682159,-60.64995));
#134577=CARTESIAN_POINT('Ctrl Pts',(-52.1838946235503,20.7264221086262,
-59.64995));
#134578=CARTESIAN_POINT('Ctrl Pts',(-52.1838946235501,20.7264221086281,
-59.7808732880376));
#134579=CARTESIAN_POINT('Ctrl Pts',(-52.1576686453522,20.7275563241362,
-59.9116978933072));
#134580=CARTESIAN_POINT('Ctrl Pts',(-52.0567177019522,20.7319222289985,
-60.153568971423));
#134581=CARTESIAN_POINT('Ctrl Pts',(-51.9820324348179,20.7351522014979,
-60.264496726805));
#134582=CARTESIAN_POINT('Ctrl Pts',(-51.7954994139911,20.7432193417859,
-60.4496168355681));
#134583=CARTESIAN_POINT('Ctrl Pts',(-51.6837250128509,20.7480533372398,
-60.5237363920407));
#134584=CARTESIAN_POINT('Ctrl Pts',(-51.4400078760636,20.7585935639752,
-60.6239226729818));
#134585=CARTESIAN_POINT('Ctrl Pts',(-51.3081847642104,20.764294621792,-60.64995));
#134586=CARTESIAN_POINT('Ctrl Pts',(-51.1762622162812,20.76999998,-60.64995));
#134587=CARTESIAN_POINT('Ctrl Pts',(-50.6819512673597,26.41999998,-60.64995));
#134588=CARTESIAN_POINT('Ctrl Pts',(-50.8138738152888,26.4142946217921,
-60.64995));
#134589=CARTESIAN_POINT('Ctrl Pts',(-50.9456969271423,26.4085935639752,
-60.6239226729817));
#134590=CARTESIAN_POINT('Ctrl Pts',(-51.1894140639292,26.3980533372399,
-60.5237363920408));
#134591=CARTESIAN_POINT('Ctrl Pts',(-51.3011884650699,26.3932193417862,
-60.4496168355678));
#134592=CARTESIAN_POINT('Ctrl Pts',(-51.4877214858962,26.3851522014976,
-60.2644967268053));
#134593=CARTESIAN_POINT('Ctrl Pts',(-51.5624067530308,26.3819222289988,
-60.1535689714229));
#134594=CARTESIAN_POINT('Ctrl Pts',(-51.6633576964307,26.3775563241358,
-59.9116978933072));
#134595=CARTESIAN_POINT('Ctrl Pts',(-51.6895836746287,26.3764221086278,
-59.7808732880375));
#134596=CARTESIAN_POINT('Ctrl Pts',(-51.6895836746288,26.3764221086262,
-59.64995));
#134597=CARTESIAN_POINT('Origin',(-52.1876810236747,26.41999998,-52.64995));
#134598=CARTESIAN_POINT('',(-52.1876810236747,26.91999998,-55.74995));
#134599=CARTESIAN_POINT('Origin',(-52.1876810236747,26.41999998,-55.74995));
#134600=CARTESIAN_POINT('',(-52.1876810236747,26.91999998,-59.64995));
#134601=CARTESIAN_POINT('',(-52.1876810236747,26.91999998,-55.24995));
#134602=CARTESIAN_POINT('Origin',(-52.1876810236747,26.41999998,-59.64995));
#134603=CARTESIAN_POINT('Ctrl Pts',(-51.6020950111029,27.3764221086262,
-54.74995));
#134604=CARTESIAN_POINT('Ctrl Pts',(-51.6020950111029,27.3764221086262,
-55.2499499999999));
#134605=CARTESIAN_POINT('Ctrl Pts',(-52.1001923601488,27.41999998,-55.24995));
#134606=CARTESIAN_POINT('Ctrl Pts',(-51.6250638203816,27.1138874172394,
-54.7499500000658));
#134607=CARTESIAN_POINT('Ctrl Pts',(-51.6138488608016,27.2420749918296,
-55.2615708605686));
#134608=CARTESIAN_POINT('Ctrl Pts',(-52.1231611694256,27.2887326343059,
-55.24995));
#134609=CARTESIAN_POINT('Ctrl Pts',(-51.6477629289455,26.8544354191273,
-54.8577231271254));
#134610=CARTESIAN_POINT('Ctrl Pts',(-51.6242368893532,27.1233392821413,
-55.3274496218423));
#134611=CARTESIAN_POINT('Ctrl Pts',(-52.1458602779915,27.1590066352508,
-55.3038365635627));
#134612=CARTESIAN_POINT('Ctrl Pts',(-51.6801547477726,26.484195235752,-55.2279633105015));
#134613=CARTESIAN_POINT('Ctrl Pts',(-51.6383763406497,26.9617246142954,
-55.5133819370981));
#134614=CARTESIAN_POINT('Ctrl Pts',(-52.1782520968184,26.9738865435627,
-55.4889566552508));
#134615=CARTESIAN_POINT('Ctrl Pts',(-51.6895836746231,26.3764221086917,
-55.4874153086129));
#134616=CARTESIAN_POINT('Ctrl Pts',(-51.6420267731401,26.9199999800045,
-55.6317784220491));
#134617=CARTESIAN_POINT('Ctrl Pts',(-52.1876810236693,26.91999998,-55.6186826543062));
#134618=CARTESIAN_POINT('Ctrl Pts',(-51.6895836746288,26.3764221086262,
-55.74995));
#134619=CARTESIAN_POINT('Ctrl Pts',(-51.6420267731401,26.91999998,-55.74995));
#134620=CARTESIAN_POINT('Ctrl Pts',(-52.1876810236747,26.91999998,-55.74995));
#134621=CARTESIAN_POINT('',(-52.1001923601488,27.41999998,-55.24995));
#134622=CARTESIAN_POINT('Origin',(-52.1001923601488,27.41999998,-54.74995));
#134623=CARTESIAN_POINT('Ctrl Pts',(-52.1001923601488,27.41999998,-55.24995));
#134624=CARTESIAN_POINT('Ctrl Pts',(-52.1231611694256,27.2887326343059,
-55.24995));
#134625=CARTESIAN_POINT('Ctrl Pts',(-52.1458602779915,27.1590066352508,
-55.3038365635627));
#134626=CARTESIAN_POINT('Ctrl Pts',(-52.1782520968184,26.9738865435627,
-55.4889566552508));
#134627=CARTESIAN_POINT('Ctrl Pts',(-52.1876810236693,26.91999998,-55.6186826543062));
#134628=CARTESIAN_POINT('Ctrl Pts',(-52.1876810236747,26.91999998,-55.74995));
#134629=CARTESIAN_POINT('Origin',(-51.7633389850707,31.2702516755049,-54.74995));
#134630=CARTESIAN_POINT('',(-52.0564480283858,27.91999998,-55.24995));
#134631=CARTESIAN_POINT('Origin',(-52.0564480283858,27.91999998,-54.74995));
#134632=CARTESIAN_POINT('',(-52.0733761857257,27.7265102562164,-55.24995));
#134633=CARTESIAN_POINT('Ctrl Pts',(-51.4708620158141,28.8764221086262,
-55.74995));
#134634=CARTESIAN_POINT('Ctrl Pts',(-51.5107937778512,28.41999998,-55.74995));
#134635=CARTESIAN_POINT('Ctrl Pts',(-51.9689593648599,28.41999998,-55.74995));
#134636=CARTESIAN_POINT('Ctrl Pts',(-51.4708620158198,28.8764221085606,
-55.4874153086129));
#134637=CARTESIAN_POINT('Ctrl Pts',(-51.5107937778567,28.4199999799462,
-55.6078478088784));
#134638=CARTESIAN_POINT('Ctrl Pts',(-51.9689593648654,28.41999998,-55.6186826543062));
#134639=CARTESIAN_POINT('Ctrl Pts',(-51.4802909426703,28.7686489815003,
-55.2279633105015));
#134640=CARTESIAN_POINT('Ctrl Pts',(-51.5164047569777,28.3558661951151,
-55.4680441063688));
#134641=CARTESIAN_POINT('Ctrl Pts',(-51.9783882917162,28.3661134164373,
-55.4889566552507));
#134642=CARTESIAN_POINT('Ctrl Pts',(-51.5126827614974,28.3984087981251,
-54.8577231271254));
#134643=CARTESIAN_POINT('Ctrl Pts',(-51.5345366632341,28.1486175582537,
-55.2822894538777));
#134644=CARTESIAN_POINT('Ctrl Pts',(-52.0107801105432,28.1809933247493,
-55.3038365635627));
#134645=CARTESIAN_POINT('Ctrl Pts',(-51.5353818700614,28.1389568000129,
-54.7499500000658));
#134646=CARTESIAN_POINT('Ctrl Pts',(-51.5469301855916,28.0069589495408,
-55.2386587236988));
#134647=CARTESIAN_POINT('Ctrl Pts',(-52.033479219109,28.0512673256941,-55.24995));
#134648=CARTESIAN_POINT('Ctrl Pts',(-51.55835067934,27.8764221086262,-54.74995));
#134649=CARTESIAN_POINT('Ctrl Pts',(-51.5583506793399,27.8764221086261,
-55.24995));
#134650=CARTESIAN_POINT('Ctrl Pts',(-52.0564480283858,27.91999998,-55.24995));
#134651=CARTESIAN_POINT('',(-51.9689593648599,28.41999998,-55.74995));
#134652=CARTESIAN_POINT('Origin',(-51.9689593648599,28.91999998,-55.74995));
#134653=CARTESIAN_POINT('Ctrl Pts',(-51.9689593648599,28.41999998,-55.74995));
#134654=CARTESIAN_POINT('Ctrl Pts',(-51.9689593648654,28.41999998,-55.6186826543062));
#134655=CARTESIAN_POINT('Ctrl Pts',(-51.9783882917162,28.3661134164373,
-55.4889566552507));
#134656=CARTESIAN_POINT('Ctrl Pts',(-52.0107801105432,28.1809933247493,
-55.3038365635627));
#134657=CARTESIAN_POINT('Ctrl Pts',(-52.033479219109,28.0512673256941,-55.24995));
#134658=CARTESIAN_POINT('Ctrl Pts',(-52.0564480283858,27.91999998,-55.24995));
#134659=CARTESIAN_POINT('Origin',(-51.9689593648599,28.91999998,-52.64995));
#134660=CARTESIAN_POINT('',(-51.9689593648599,28.41999998,-59.64995));
#134661=CARTESIAN_POINT('Origin',(-51.9689593648599,28.91999998,-59.64995));
#134662=CARTESIAN_POINT('',(-51.9689593648599,28.41999998,-55.24995));
#134663=CARTESIAN_POINT('Origin',(-53.7167487055517,-8.26789346682159,-59.64995));
#134664=CARTESIAN_POINT('',(-50.4632296085449,28.91999998,-60.64995));
#134665=CARTESIAN_POINT('',(-53.7167487055517,-8.26789346682159,-60.64995));
#134666=CARTESIAN_POINT('Ctrl Pts',(-51.4708620158141,28.8764221086262,
-59.64995));
#134667=CARTESIAN_POINT('Ctrl Pts',(-51.4708620158139,28.8764221086278,
-59.7808732880376));
#134668=CARTESIAN_POINT('Ctrl Pts',(-51.4446360376159,28.8775563241362,
-59.9116978933072));
#134669=CARTESIAN_POINT('Ctrl Pts',(-51.343685094216,28.8819222289984,-60.153568971423));
#134670=CARTESIAN_POINT('Ctrl Pts',(-51.2689998270813,28.8851522014976,
-60.2644967268053));
#134671=CARTESIAN_POINT('Ctrl Pts',(-51.0824668062551,28.8932193417862,
-60.4496168355678));
#134672=CARTESIAN_POINT('Ctrl Pts',(-50.9706924051143,28.8980533372399,
-60.5237363920408));
#134673=CARTESIAN_POINT('Ctrl Pts',(-50.7269752683276,28.9085935639752,
-60.6239226729817));
#134674=CARTESIAN_POINT('Ctrl Pts',(-50.5951521564739,28.9142946217921,
-60.64995));
#134675=CARTESIAN_POINT('Ctrl Pts',(-50.4632296085449,28.91999998,-60.64995));
#134676=CARTESIAN_POINT('Ctrl Pts',(-52.8969272312866,12.5764221086262,
-55.74995));
#134677=CARTESIAN_POINT('Ctrl Pts',(-52.9368589933237,12.11999998,-55.74995));
#134678=CARTESIAN_POINT('Ctrl Pts',(-53.3950245803324,12.11999998,-55.74995));
#134679=CARTESIAN_POINT('Ctrl Pts',(-52.8969272312908,12.5764221085778,
-55.5560711921817));
#134680=CARTESIAN_POINT('Ctrl Pts',(-52.9368589933258,12.1199999799653,
-55.6451138110298));
#134681=CARTESIAN_POINT('Ctrl Pts',(-53.3950245803365,12.11999998,-55.6530085475485));
#134682=CARTESIAN_POINT('Ctrl Pts',(-52.9019494572905,12.5190178027248,
-55.3638118539785));
#134683=CARTESIAN_POINT('Ctrl Pts',(-52.9398152308639,12.0862100303001,
-55.5412722521129));
#134684=CARTESIAN_POINT('Ctrl Pts',(-53.4000464934415,12.0912996152796,
-55.5568836545521));
#134685=CARTESIAN_POINT('Ctrl Pts',(-52.9112495105564,12.4127177074772,
-55.2016711737242));
#134686=CARTESIAN_POINT('Ctrl Pts',(-52.9450883668941,12.0259378096709,
-55.4571865884902));
#134687=CARTESIAN_POINT('Ctrl Pts',(-53.4093468596023,12.0381477794255,
-55.4758105868621));
#134688=CARTESIAN_POINT('',(-53.3950245803324,12.11999998,-55.74995));
#134689=CARTESIAN_POINT('Origin',(-53.3950245803325,12.61999998,-55.74995));
#134690=CARTESIAN_POINT('Origin',(-53.4672819406082,11.7070472760343,-55.7239598691462));
#134691=CARTESIAN_POINT('Origin',(-53.3950245803324,12.61999998,-55.24995));
#134692=CARTESIAN_POINT('',(-53.3950245803324,12.11999998,-60.0627241236309));
#134693=CARTESIAN_POINT('Origin',(-53.3950245803325,12.61999998,-60.0627241236309));
#134694=CARTESIAN_POINT('',(-53.3950245803324,12.11999998,-55.24995));
#134695=CARTESIAN_POINT('Ctrl Pts',(-51.6244217512084,15.6475130558006,
-60.64995));
#134696=CARTESIAN_POINT('Ctrl Pts',(-52.6206164493002,15.7346687985482,
-60.64995));
#134697=CARTESIAN_POINT('Ctrl Pts',(-52.6206164493001,15.7346687985483,
-59.64995));
#134698=CARTESIAN_POINT('Ctrl Pts',(-51.7744992817202,15.1392139958173,
-60.64995));
#134699=CARTESIAN_POINT('Ctrl Pts',(-52.6636514122595,15.2427769209991,
-60.5499446302911));
#134700=CARTESIAN_POINT('Ctrl Pts',(-52.6699713539896,15.1705396565499,
-59.6499500021592));
#134701=CARTESIAN_POINT('Ctrl Pts',(-51.921686259274,14.6313008059217,-60.6692877368673));
#134702=CARTESIAN_POINT('Ctrl Pts',(-52.7104450878319,14.7079227618566,
-60.4941916839025));
#134703=CARTESIAN_POINT('Ctrl Pts',(-52.7188714030742,14.6116095379051,
-59.6886254732604));
#134704=CARTESIAN_POINT('Ctrl Pts',(-52.209973495227,13.6164898397673,-60.7441942307015));
#134705=CARTESIAN_POINT('Ctrl Pts',(-52.8037229951722,13.64175140224,-60.4769182500017));
#134706=CARTESIAN_POINT('Ctrl Pts',(-52.8157906892286,13.5038170280144,
-59.8384384618772));
#134707=CARTESIAN_POINT('Ctrl Pts',(-52.3511088881553,13.109439201609,-60.799180633384));
#134708=CARTESIAN_POINT('Ctrl Pts',(-52.850859560631,13.1029779936029,-60.5072438893719));
#134709=CARTESIAN_POINT('Ctrl Pts',(-52.8638414531199,12.954594283549,-59.9484723594913));
#134710=CARTESIAN_POINT('Ctrl Pts',(-52.4885489491165,12.6049688303995,
-60.8798615124595));
#134711=CARTESIAN_POINT('Ctrl Pts',(-52.8987763848902,12.5552861862208,
-60.5923862926586));
#134712=CARTESIAN_POINT('Ctrl Pts',(-52.9112495105564,12.4127177074772,
-60.1097730249189));
#134713=CARTESIAN_POINT('',(-51.6244217512084,15.6475130558006,-60.64995));
#134714=CARTESIAN_POINT('Origin',(-51.6244217512084,15.6475130558006,-59.64995));
#134715=CARTESIAN_POINT('',(-52.4885489491165,12.6049688303995,-60.8798615124595));
#134716=CARTESIAN_POINT('Ctrl Pts',(-51.6244217512084,15.6475130558006,
-60.64995));
#134717=CARTESIAN_POINT('Ctrl Pts',(-51.7744993530724,15.1392140041279,
-60.6499499919748));
#134718=CARTESIAN_POINT('Ctrl Pts',(-51.9216863254076,14.6313008123461,
-60.6692877221863));
#134719=CARTESIAN_POINT('Ctrl Pts',(-52.2099735489448,13.6164898420528,
-60.7441942065205));
#134720=CARTESIAN_POINT('Ctrl Pts',(-52.3511089348818,13.1094392010049,
-60.799180606088));
#134721=CARTESIAN_POINT('Ctrl Pts',(-52.4885489491165,12.6049688303995,
-60.8798615124595));
#134722=CARTESIAN_POINT('',(-52.81219032515,12.5218539749099,-60.5055220850798));
#134723=CARTESIAN_POINT('Origin',(-51.9150548124647,12.3255619647296,-60.1097730249189));
#134724=CARTESIAN_POINT('Ctrl Pts',(-52.8969272285826,12.5764221083876,
-60.0627241236307));
#134725=CARTESIAN_POINT('Ctrl Pts',(-52.8973718975191,12.5713069363321,
-60.1041418566377));
#134726=CARTESIAN_POINT('Ctrl Pts',(-52.895580098221,12.5662216141313,-60.1452630246831));
#134727=CARTESIAN_POINT('Ctrl Pts',(-52.8916250763018,12.5611890572108,
-60.1859586821439));
#134728=CARTESIAN_POINT('Ctrl Pts',(-52.8875910253699,12.5560559400376,
-60.2274675178095));
#134729=CARTESIAN_POINT('Ctrl Pts',(-52.8813073672434,12.550978356838,-60.2685357471677));
#134730=CARTESIAN_POINT('Ctrl Pts',(-52.872806509014,12.5459803352207,-60.3090583620907));
#134731=CARTESIAN_POINT('Ctrl Pts',(-52.8644535955316,12.5410692967085,
-60.3488757413946));
#134732=CARTESIAN_POINT('Ctrl Pts',(-52.8539596832267,12.5362356727488,
-60.3881685164046));
#134733=CARTESIAN_POINT('Ctrl Pts',(-52.8413080863257,12.5314926818733,
-60.4268350961324));
#134734=CARTESIAN_POINT('Ctrl Pts',(-52.8326250159684,12.5282374624889,
-60.4533728237313));
#134735=CARTESIAN_POINT('Ctrl Pts',(-52.8229245067539,12.5250247275077,
-60.4796155210117));
#134736=CARTESIAN_POINT('Ctrl Pts',(-52.81219032515,12.5218539749099,-60.5055220850798));
#134737=CARTESIAN_POINT('Origin',(-53.7167487055517,-8.26789346682159,-59.64995));
#134738=CARTESIAN_POINT('',(-51.394983875096,18.26999998,-60.64995));
#134739=CARTESIAN_POINT('',(-53.7167487055517,-8.26789346682159,-60.64995));
#134740=CARTESIAN_POINT('Ctrl Pts',(-51.394983875096,18.26999998,-60.64995));
#134741=CARTESIAN_POINT('Ctrl Pts',(-51.5269064230252,18.264294621793,-60.64995));
#134742=CARTESIAN_POINT('Ctrl Pts',(-51.6587295348784,18.2585935639752,
-60.6239226729819));
#134743=CARTESIAN_POINT('Ctrl Pts',(-51.9024466716657,18.2480533372399,
-60.5237363920407));
#134744=CARTESIAN_POINT('Ctrl Pts',(-52.0142210728062,18.2432193417862,
-60.4496168355678));
#134745=CARTESIAN_POINT('Ctrl Pts',(-52.2007540936325,18.2351522014976,
-60.2644967268053));
#134746=CARTESIAN_POINT('Ctrl Pts',(-52.2754393607673,18.2319222289985,
-60.1535689714224));
#134747=CARTESIAN_POINT('Ctrl Pts',(-52.3763903041667,18.2275563241362,
-59.9116978933078));
#134748=CARTESIAN_POINT('Ctrl Pts',(-52.402616282365,18.2264221086281,-59.7808732880371));
#134749=CARTESIAN_POINT('Ctrl Pts',(-52.4026162823651,18.2264221086262,
-59.64995));
#134750=CARTESIAN_POINT('Origin',(-52.900713631411,18.26999998,-52.64995));
#134751=CARTESIAN_POINT('',(-52.900713631411,18.76999998,-59.64995));
#134752=CARTESIAN_POINT('Origin',(-52.900713631411,18.26999998,-59.64995));
#134753=CARTESIAN_POINT('',(-52.900713631411,18.76999998,-55.74995));
#134754=CARTESIAN_POINT('Origin',(-52.900713631411,18.26999998,-55.74995));
#134755=CARTESIAN_POINT('',(-52.900713631411,18.76999998,-55.24995));
#134756=CARTESIAN_POINT('Ctrl Pts',(-52.3151276188392,19.2264221086262,
-54.74995));
#134757=CARTESIAN_POINT('Ctrl Pts',(-52.3151276188392,19.2264221086262,
-55.2499499999999));
#134758=CARTESIAN_POINT('Ctrl Pts',(-52.8132249678851,19.26999998,-55.24995));
#134759=CARTESIAN_POINT('Ctrl Pts',(-52.3380964281178,18.9638874172394,
-54.7499500000658));
#134760=CARTESIAN_POINT('Ctrl Pts',(-52.3268814685379,19.09207499183,-55.2615708605685));
#134761=CARTESIAN_POINT('Ctrl Pts',(-52.8361937771619,19.1387326343059,
-55.24995));
#134762=CARTESIAN_POINT('Ctrl Pts',(-52.3607955366818,18.7044354191273,
-54.8577231271254));
#134763=CARTESIAN_POINT('Ctrl Pts',(-52.3372694970894,18.9733392821407,
-55.3274496218431));
#134764=CARTESIAN_POINT('Ctrl Pts',(-52.8588928857277,19.0090066352508,
-55.3038365635627));
#134765=CARTESIAN_POINT('Ctrl Pts',(-52.3931873555089,18.334195235752,-55.2279633105015));
#134766=CARTESIAN_POINT('Ctrl Pts',(-52.351408948386,18.8117246142959,-55.5133819370972));
#134767=CARTESIAN_POINT('Ctrl Pts',(-52.8912847045547,18.8238865435627,
-55.4889566552508));
#134768=CARTESIAN_POINT('Ctrl Pts',(-52.4026162823594,18.2264221086918,
-55.4874153086129));
#134769=CARTESIAN_POINT('Ctrl Pts',(-52.3550593808763,18.7699999800045,
-55.6317784220498));
#134770=CARTESIAN_POINT('Ctrl Pts',(-52.9007136314055,18.76999998,-55.6186826543062));
#134771=CARTESIAN_POINT('Ctrl Pts',(-52.4026162823651,18.2264221086262,
-55.74995));
#134772=CARTESIAN_POINT('Ctrl Pts',(-52.3550593808763,18.76999998,-55.74995));
#134773=CARTESIAN_POINT('Ctrl Pts',(-52.900713631411,18.76999998,-55.74995));
#134774=CARTESIAN_POINT('',(-52.8132249678851,19.26999998,-55.24995));
#134775=CARTESIAN_POINT('Origin',(-52.8132249678851,19.26999998,-54.74995));
#134776=CARTESIAN_POINT('Ctrl Pts',(-52.8132249678851,19.26999998,-55.24995));
#134777=CARTESIAN_POINT('Ctrl Pts',(-52.8361937771619,19.1387326343059,
-55.24995));
#134778=CARTESIAN_POINT('Ctrl Pts',(-52.8588928857277,19.0090066352508,
-55.3038365635627));
#134779=CARTESIAN_POINT('Ctrl Pts',(-52.8912847045547,18.8238865435627,
-55.4889566552508));
#134780=CARTESIAN_POINT('Ctrl Pts',(-52.9007136314055,18.76999998,-55.6186826543062));
#134781=CARTESIAN_POINT('Ctrl Pts',(-52.900713631411,18.76999998,-55.74995));
#134782=CARTESIAN_POINT('Origin',(-51.7633389850707,31.2702516755049,-54.74995));
#134783=CARTESIAN_POINT('',(-52.7694806361221,19.76999998,-55.24995));
#134784=CARTESIAN_POINT('Origin',(-52.7694806361221,19.76999998,-54.74995));
#134785=CARTESIAN_POINT('',(-52.0733761857257,27.7265102562164,-55.24995));
#134786=CARTESIAN_POINT('Ctrl Pts',(-52.1838946235503,20.7264221086262,
-55.74995));
#134787=CARTESIAN_POINT('Ctrl Pts',(-52.2238263855875,20.26999998,-55.74995));
#134788=CARTESIAN_POINT('Ctrl Pts',(-52.6819919725962,20.26999998,-55.74995));
#134789=CARTESIAN_POINT('Ctrl Pts',(-52.1838946235561,20.7264221085606,
-55.487415308613));
#134790=CARTESIAN_POINT('Ctrl Pts',(-52.2238263855902,20.2699999799516,
-55.6078478088784));
#134791=CARTESIAN_POINT('Ctrl Pts',(-52.6819919726017,20.26999998,-55.6186826543063));
#134792=CARTESIAN_POINT('Ctrl Pts',(-52.1933235504066,20.6186489815003,
-55.2279633105015));
#134793=CARTESIAN_POINT('Ctrl Pts',(-52.229437364714,20.2058661951152,-55.4680441063689));
#134794=CARTESIAN_POINT('Ctrl Pts',(-52.6914208994525,20.2161134164373,
-55.4889566552507));
#134795=CARTESIAN_POINT('Ctrl Pts',(-52.2257153692336,20.2484087981252,
-54.8577231271255));
#134796=CARTESIAN_POINT('Ctrl Pts',(-52.2475692709704,19.9986175582537,
-55.2822894538776));
#134797=CARTESIAN_POINT('Ctrl Pts',(-52.7238127182794,20.0309933247493,
-55.3038365635627));
#134798=CARTESIAN_POINT('Ctrl Pts',(-52.2484144777976,19.9889568000129,
-54.7499500000658));
#134799=CARTESIAN_POINT('Ctrl Pts',(-52.2599627933277,19.8569589495402,
-55.2386587236914));
#134800=CARTESIAN_POINT('Ctrl Pts',(-52.746511826845,19.901267325694,-55.24995));
#134801=CARTESIAN_POINT('Ctrl Pts',(-52.2713832870762,19.7264221086262,
-54.74995));
#134802=CARTESIAN_POINT('Ctrl Pts',(-52.2713832870762,19.7264221086262,
-55.2499499999999));
#134803=CARTESIAN_POINT('Ctrl Pts',(-52.7694806361221,19.76999998,-55.24995));
#134804=CARTESIAN_POINT('',(-52.6819919725962,20.26999998,-55.74995));
#134805=CARTESIAN_POINT('Origin',(-52.6819919725962,20.76999998,-55.74995));
#134806=CARTESIAN_POINT('Ctrl Pts',(-52.6819919725962,20.26999998,-55.74995));
#134807=CARTESIAN_POINT('Ctrl Pts',(-52.6819919726017,20.26999998,-55.6186826543063));
#134808=CARTESIAN_POINT('Ctrl Pts',(-52.6914208994525,20.2161134164373,
-55.4889566552507));
#134809=CARTESIAN_POINT('Ctrl Pts',(-52.7238127182794,20.0309933247493,
-55.3038365635627));
#134810=CARTESIAN_POINT('Ctrl Pts',(-52.746511826845,19.901267325694,-55.24995));
#134811=CARTESIAN_POINT('Ctrl Pts',(-52.7694806361221,19.76999998,-55.24995));
#134812=CARTESIAN_POINT('Origin',(-52.6819919725962,20.76999998,-52.64995));
#134813=CARTESIAN_POINT('',(-52.6819919725962,20.26999998,-59.64995));
#134814=CARTESIAN_POINT('Origin',(-52.6819919725962,20.76999998,-59.64995));
#134815=CARTESIAN_POINT('',(-52.6819919725962,20.26999998,-55.24995));
#134816=CARTESIAN_POINT('Ctrl Pts',(-52.4648996019023,-38.6266655296175,
-60.866265313415));
#134817=CARTESIAN_POINT('Ctrl Pts',(-52.8907789702838,-38.5816970935142,
-60.5786901973488));
#134818=CARTESIAN_POINT('Ctrl Pts',(-52.903095448475,-38.4409191036023,
-60.08258062683));
#134819=CARTESIAN_POINT('Ctrl Pts',(-52.3309754745585,-39.1170130132287,
-60.7908684306025));
#134820=CARTESIAN_POINT('Ctrl Pts',(-52.8442212423788,-39.1138543585791,
-60.5019204415683));
#134821=CARTESIAN_POINT('Ctrl Pts',(-52.8569709369232,-38.9681246830787,
-59.9318336272105));
#134822=CARTESIAN_POINT('Ctrl Pts',(-52.1936254351686,-39.6095793654924,
-60.7389129305601));
#134823=CARTESIAN_POINT('Ctrl Pts',(-52.7984570004479,-39.6369420374376,
-60.4756484953684));
#134824=CARTESIAN_POINT('Ctrl Pts',(-52.8102637225239,-39.5019905865797,
-59.8278758615346));
#134825=CARTESIAN_POINT('Ctrl Pts',(-51.9132529272684,-40.5953951229239,
-60.6682257074536));
#134826=CARTESIAN_POINT('Ctrl Pts',(-52.7078841622538,-40.6721943151964,
-60.4973085875933));
#134827=CARTESIAN_POINT('Ctrl Pts',(-52.7160699755127,-40.5786300415107,
-59.6865014144928));
#134828=CARTESIAN_POINT('Ctrl Pts',(-51.7702028983306,-41.0887654988916,
-60.64995));
#134829=CARTESIAN_POINT('Ctrl Pts',(-52.662477767809,-41.1911917785403,
-60.5526719649898));
#134830=CARTESIAN_POINT('Ctrl Pts',(-52.6685584273161,-41.1216895223836,
-59.6499500020974));
#134831=CARTESIAN_POINT('Ctrl Pts',(-51.6244217512083,-41.5825130958571,
-60.64995));
#134832=CARTESIAN_POINT('Ctrl Pts',(-52.6206164493,-41.6696688386047,-60.64995));
#134833=CARTESIAN_POINT('Ctrl Pts',(-52.6206164493,-41.6696688386047,-59.64995));
#134834=CARTESIAN_POINT('',(-52.4601060488076,-38.6442121690347,-60.8635779995146));
#134835=CARTESIAN_POINT('',(-51.6244217512083,-41.5825130958571,-60.64995));
#134836=CARTESIAN_POINT('Ctrl Pts',(-52.4601060488526,-38.6442121687577,
-60.8635779995784));
#134837=CARTESIAN_POINT('Ctrl Pts',(-52.327698644121,-39.1287630233132,
-60.7896314173872));
#134838=CARTESIAN_POINT('Ctrl Pts',(-52.1919533933421,-39.6154584197261,
-60.7384913771257));
#134839=CARTESIAN_POINT('Ctrl Pts',(-51.9132529272684,-40.5953951229239,
-60.6682257074536));
#134840=CARTESIAN_POINT('Ctrl Pts',(-51.7702028983306,-41.0887654988916,
-60.64995));
#134841=CARTESIAN_POINT('Ctrl Pts',(-51.6244217512083,-41.5825130958571,
-60.64995));
#134842=CARTESIAN_POINT('Origin',(-51.6244217512083,-41.5825130958571,-59.64995));
#134843=CARTESIAN_POINT('Ctrl Pts',(-52.4601060488526,-38.6442121687577,
-60.8635779995784));
#134844=CARTESIAN_POINT('Ctrl Pts',(-52.5917711956707,-38.6521075044106,
-60.7679496692827));
#134845=CARTESIAN_POINT('Ctrl Pts',(-52.6988044737759,-38.6656865171052,
-60.6372698562504));
#134846=CARTESIAN_POINT('Ctrl Pts',(-52.8422535332614,-38.6982739394415,
-60.3389622441799));
#134847=CARTESIAN_POINT('Ctrl Pts',(-52.8788986395818,-38.7174898948119,
-60.1690974501184));
#134848=CARTESIAN_POINT('Ctrl Pts',(-52.877242281998,-38.7364221486262,
-60.0032396521562));
#134849=CARTESIAN_POINT('Origin',(-53.3753396310439,-38.78000002,-55.2499500000007));
#134850=CARTESIAN_POINT('',(-53.3753396310439,-38.28000002,-55.74995));
#134851=CARTESIAN_POINT('Origin',(-53.3753396310439,-38.78000002,-55.74995));
#134852=CARTESIAN_POINT('',(-53.3753396310439,-38.28000002,-60.0032396521563));
#134853=CARTESIAN_POINT('',(-53.3753396310439,-38.28000002,-55.2499500000007));
#134854=CARTESIAN_POINT('Origin',(-53.3753396310439,-38.78000002,-60.0032396521563));
#134855=CARTESIAN_POINT('Ctrl Pts',(-52.9112502355242,-38.3477094636814,
-54.9585223635782));
#134856=CARTESIAN_POINT('Ctrl Pts',(-52.9364314216307,-38.0597244105783,
-55.3342259538136));
#134857=CARTESIAN_POINT('Ctrl Pts',(-53.4093483797613,-38.0856391317044,
-55.3542421110299));
#134858=CARTESIAN_POINT('Ctrl Pts',(-52.889976625843,-38.5908679349475,
-55.1463344612842));
#134859=CARTESIAN_POINT('Ctrl Pts',(-52.9247563553464,-38.1931762538392,
-55.4246794702588));
#134860=CARTESIAN_POINT('Ctrl Pts',(-53.3880736387225,-38.2072248331335,
-55.448153047952));
#134861=CARTESIAN_POINT('Ctrl Pts',(-52.87724039479,-38.7364437219894,-55.4427310705271));
#134862=CARTESIAN_POINT('Ctrl Pts',(-52.9171601694684,-38.2800041317283,
-55.5832548498195));
#134863=CARTESIAN_POINT('Ctrl Pts',(-53.375339024416,-38.2800034869308,
-55.5963379967406));
#134864=CARTESIAN_POINT('Ctrl Pts',(-52.8772410016055,-38.736436786057,
-55.7499719536926));
#134865=CARTESIAN_POINT('Ctrl Pts',(-52.9171605282557,-38.2800000198531,
-55.7499619127669));
#134866=CARTESIAN_POINT('Ctrl Pts',(-53.3753396310656,-38.2800000198761,
-55.7499609770277));
#134867=CARTESIAN_POINT('Origin',(-53.4522675625606,-37.8403548794211,-55.7203077484906));
#134868=CARTESIAN_POINT('Origin',(-53.7167487055513,-17.6671065732338,-59.64995));
#134869=CARTESIAN_POINT('',(-50.4435446592566,-55.08000002,-60.64995));
#134870=CARTESIAN_POINT('',(-53.7167487055513,-17.6671065732338,-60.64995));
#134871=CARTESIAN_POINT('Ctrl Pts',(-50.4435446592566,-55.08000002,-60.64995));
#134872=CARTESIAN_POINT('Ctrl Pts',(-50.5754672071858,-55.0742946617933,
-60.64995));
#134873=CARTESIAN_POINT('Ctrl Pts',(-50.707290319039,-55.0685936039748,
-60.6239226729819));
#134874=CARTESIAN_POINT('Ctrl Pts',(-50.9510074558263,-55.0580533772402,
-60.5237363920407));
#134875=CARTESIAN_POINT('Ctrl Pts',(-51.0627818569665,-55.0532193817859,
-60.4496168355682));
#134876=CARTESIAN_POINT('Ctrl Pts',(-51.2493148777934,-55.0451522414979,
-60.2644967268049));
#134877=CARTESIAN_POINT('Ctrl Pts',(-51.3240001449277,-55.0419222689988,
-60.153568971423));
#134878=CARTESIAN_POINT('Ctrl Pts',(-51.4249510883276,-55.0375563641359,
-59.9116978933072));
#134879=CARTESIAN_POINT('Ctrl Pts',(-51.4511770665255,-55.0364221486294,
-59.7808732880376));
#134880=CARTESIAN_POINT('Ctrl Pts',(-51.4511770665258,-55.0364221486262,
-59.64995));
#134881=CARTESIAN_POINT('Origin',(-51.9492744155716,-55.08000002,-52.64995));
#134882=CARTESIAN_POINT('',(-51.9492744155716,-54.58000002,-59.64995));
#134883=CARTESIAN_POINT('Origin',(-51.9492744155716,-55.08000002,-59.64995));
#134884=CARTESIAN_POINT('',(-51.9492744155716,-54.58000002,-55.74995));
#134885=CARTESIAN_POINT('Origin',(-51.9492744155716,-55.08000002,-55.74995));
#134886=CARTESIAN_POINT('',(-51.9492744155716,-54.58000002,-55.24995));
#134887=CARTESIAN_POINT('Ctrl Pts',(-51.5386657300517,-54.0364221486262,
-54.74995));
#134888=CARTESIAN_POINT('Ctrl Pts',(-51.5386657300516,-54.0364221486262,
-55.24995));
#134889=CARTESIAN_POINT('Ctrl Pts',(-52.0367630790975,-54.08000002,-55.24995));
#134890=CARTESIAN_POINT('Ctrl Pts',(-51.5156969207731,-54.2989568400126,
-54.7499500000658));
#134891=CARTESIAN_POINT('Ctrl Pts',(-51.5272452363036,-54.1669589895393,
-55.2386587236848));
#134892=CARTESIAN_POINT('Ctrl Pts',(-52.0137942698207,-54.2112673656937,
-55.24995));
#134893=CARTESIAN_POINT('Ctrl Pts',(-51.4929978122091,-54.5584088381255,
-54.8577231271254));
#134894=CARTESIAN_POINT('Ctrl Pts',(-51.5148517139458,-54.308617598254,
-55.2822894538766));
#134895=CARTESIAN_POINT('Ctrl Pts',(-51.9910951612549,-54.3409933647497,
-55.3038365635632));
#134896=CARTESIAN_POINT('Ctrl Pts',(-51.460605993382,-54.9286490214999,
-55.2279633105015));
#134897=CARTESIAN_POINT('Ctrl Pts',(-51.4967198076894,-54.5158662351146,
-55.4680441063697));
#134898=CARTESIAN_POINT('Ctrl Pts',(-51.958703342428,-54.5261134564368,
-55.4889566552503));
#134899=CARTESIAN_POINT('Ctrl Pts',(-51.4511770665315,-55.0364221485606,
-55.4874153086129));
#134900=CARTESIAN_POINT('Ctrl Pts',(-51.491108828562,-54.5800000199489,
-55.6078478088776));
#134901=CARTESIAN_POINT('Ctrl Pts',(-51.9492744155771,-54.58000002,-55.6186826543065));
#134902=CARTESIAN_POINT('Ctrl Pts',(-51.4511770665258,-55.0364221486262,
-55.74995));
#134903=CARTESIAN_POINT('Ctrl Pts',(-51.491108828563,-54.58000002,-55.74995));
#134904=CARTESIAN_POINT('Ctrl Pts',(-51.9492744155716,-54.58000002,-55.74995));
#134905=CARTESIAN_POINT('',(-52.0367630790975,-54.08000002,-55.24995));
#134906=CARTESIAN_POINT('Origin',(-52.0367630790975,-54.08000002,-54.74995));
#134907=CARTESIAN_POINT('Ctrl Pts',(-52.0367630790975,-54.08000002,-55.24995));
#134908=CARTESIAN_POINT('Ctrl Pts',(-52.0137942698207,-54.2112673656937,
-55.24995));
#134909=CARTESIAN_POINT('Ctrl Pts',(-51.9910951612549,-54.3409933647497,
-55.3038365635632));
#134910=CARTESIAN_POINT('Ctrl Pts',(-51.958703342428,-54.5261134564368,
-55.4889566552503));
#134911=CARTESIAN_POINT('Ctrl Pts',(-51.9492744155771,-54.58000002,-55.6186826543065));
#134912=CARTESIAN_POINT('Ctrl Pts',(-51.9492744155716,-54.58000002,-55.74995));
#134913=CARTESIAN_POINT('Origin',(-53.4839470922323,-37.5386110581466,-54.74995));
#134914=CARTESIAN_POINT('',(-52.0805074108605,-53.58000002,-55.24995));
#134915=CARTESIAN_POINT('Origin',(-52.0805074108605,-53.58000002,-54.74995));
#134916=CARTESIAN_POINT('',(-59.2602401389193,28.4847205815761,-55.24995));
#134917=CARTESIAN_POINT('Ctrl Pts',(-51.6698987253405,-52.5364221486262,
-55.74995));
#134918=CARTESIAN_POINT('Ctrl Pts',(-51.6223418238518,-53.08000002,-55.74995));
#134919=CARTESIAN_POINT('Ctrl Pts',(-52.1679960743864,-53.08000002,-55.74995));
#134920=CARTESIAN_POINT('Ctrl Pts',(-51.6698987253348,-52.5364221486917,
-55.4874153086129));
#134921=CARTESIAN_POINT('Ctrl Pts',(-51.6223418238527,-53.0800000200045,
-55.6317784220505));
#134922=CARTESIAN_POINT('Ctrl Pts',(-52.1679960743809,-53.08000002,-55.6186826543066));
#134923=CARTESIAN_POINT('Ctrl Pts',(-51.6604697984843,-52.6441952757516,
-55.2279633105015));
#134924=CARTESIAN_POINT('Ctrl Pts',(-51.6186913913614,-53.1217246542964,
-55.5133819370962));
#134925=CARTESIAN_POINT('Ctrl Pts',(-52.1585671475301,-53.1338865835632,
-55.4889566552503));
#134926=CARTESIAN_POINT('Ctrl Pts',(-51.6280779796571,-53.0144354591276,
-54.8577231271254));
#134927=CARTESIAN_POINT('Ctrl Pts',(-51.6045519400649,-53.2833393221403,
-55.327449621844));
#134928=CARTESIAN_POINT('Ctrl Pts',(-52.1261753287031,-53.3190066752503,
-55.3038365635632));
#134929=CARTESIAN_POINT('Ctrl Pts',(-51.6053788710933,-53.2738874572391,
-54.7499500000658));
#134930=CARTESIAN_POINT('Ctrl Pts',(-51.5941639115132,-53.4020750318305,
-55.2615708605685));
#134931=CARTESIAN_POINT('Ctrl Pts',(-52.1034762201372,-53.4487326743062,
-55.24995));
#134932=CARTESIAN_POINT('Ctrl Pts',(-51.5824100618146,-53.5364221486262,
-54.74995));
#134933=CARTESIAN_POINT('Ctrl Pts',(-51.5824100618146,-53.5364221486261,
-55.2499499999999));
#134934=CARTESIAN_POINT('Ctrl Pts',(-52.0805074108605,-53.58000002,-55.24995));
#134935=CARTESIAN_POINT('',(-52.1679960743864,-53.08000002,-55.74995));
#134936=CARTESIAN_POINT('Origin',(-52.1679960743864,-52.58000002,-55.74995));
#134937=CARTESIAN_POINT('Ctrl Pts',(-52.1679960743864,-53.08000002,-55.74995));
#134938=CARTESIAN_POINT('Ctrl Pts',(-52.1679960743809,-53.08000002,-55.6186826543066));
#134939=CARTESIAN_POINT('Ctrl Pts',(-52.1585671475301,-53.1338865835632,
-55.4889566552503));
#134940=CARTESIAN_POINT('Ctrl Pts',(-52.1261753287031,-53.3190066752503,
-55.3038365635632));
#134941=CARTESIAN_POINT('Ctrl Pts',(-52.1034762201372,-53.4487326743062,
-55.24995));
#134942=CARTESIAN_POINT('Ctrl Pts',(-52.0805074108605,-53.58000002,-55.24995));
#134943=CARTESIAN_POINT('Origin',(-52.1679960743864,-52.58000002,-55.2499500000008));
#134944=CARTESIAN_POINT('',(-52.1679960743864,-53.08000002,-59.64995));
#134945=CARTESIAN_POINT('Origin',(-52.1679960743864,-52.58000002,-59.64995));
#134946=CARTESIAN_POINT('',(-52.1679960743864,-53.08000002,-55.2499500000008));
#134947=CARTESIAN_POINT('Origin',(-53.7167487055513,-17.6671065732338,-59.64995));
#134948=CARTESIAN_POINT('',(-51.1565772669927,-46.93000002,-60.64995));
#134949=CARTESIAN_POINT('',(-50.6622663180714,-52.58000002,-60.64995));
#134950=CARTESIAN_POINT('',(-53.7167487055513,-17.6671065732338,-60.64995));
#134951=CARTESIAN_POINT('Ctrl Pts',(-51.6698987253405,-52.5364221486262,
-59.64995));
#134952=CARTESIAN_POINT('Ctrl Pts',(-51.6698987253403,-52.5364221486294,
-59.7808732880376));
#134953=CARTESIAN_POINT('Ctrl Pts',(-51.6436727471424,-52.5375563641358,
-59.9116978933072));
#134954=CARTESIAN_POINT('Ctrl Pts',(-51.5427218037424,-52.5419222689988,
-60.153568971423));
#134955=CARTESIAN_POINT('Ctrl Pts',(-51.4680365366082,-52.5451522414979,
-60.2644967268049));
#134956=CARTESIAN_POINT('Ctrl Pts',(-51.2815035157812,-52.5532193817859,
-60.4496168355682));
#134957=CARTESIAN_POINT('Ctrl Pts',(-51.1697291146411,-52.5580533772395,
-60.5237363920407));
#134958=CARTESIAN_POINT('Ctrl Pts',(-50.9260119778537,-52.5685936039755,
-60.6239226729819));
#134959=CARTESIAN_POINT('Ctrl Pts',(-50.7941888660007,-52.5742946617934,
-60.64995));
#134960=CARTESIAN_POINT('Ctrl Pts',(-50.6622663180714,-52.58000002,-60.64995));
#134961=CARTESIAN_POINT('Ctrl Pts',(-51.1565772669927,-46.93000002,-60.64995));
#134962=CARTESIAN_POINT('Ctrl Pts',(-51.288499814922,-46.9242946617933,
-60.64995));
#134963=CARTESIAN_POINT('Ctrl Pts',(-51.4203229267752,-46.9185936039748,
-60.6239226729819));
#134964=CARTESIAN_POINT('Ctrl Pts',(-51.6640400635624,-46.9080533772402,
-60.5237363920407));
#134965=CARTESIAN_POINT('Ctrl Pts',(-51.7758144647026,-46.9032193817865,
-60.4496168355682));
#134966=CARTESIAN_POINT('Ctrl Pts',(-51.9623474855296,-46.8951522414972,
-60.264496726805));
#134967=CARTESIAN_POINT('Ctrl Pts',(-52.0370327526638,-46.8919222689988,
-60.153568971423));
#134968=CARTESIAN_POINT('Ctrl Pts',(-52.1379836960638,-46.8875563641358,
-59.9116978933072));
#134969=CARTESIAN_POINT('Ctrl Pts',(-52.1642096742618,-46.8864221486274,
-59.7808732880376));
#134970=CARTESIAN_POINT('Ctrl Pts',(-52.1642096742619,-46.8864221486262,
-59.64995));
#134971=CARTESIAN_POINT('Origin',(-52.6623070233078,-46.93000002,-52.64995));
#134972=CARTESIAN_POINT('',(-52.6623070233077,-46.43000002,-59.64995));
#134973=CARTESIAN_POINT('Origin',(-52.6623070233077,-46.93000002,-59.64995));
#134974=CARTESIAN_POINT('',(-52.6623070233078,-46.43000002,-55.74995));
#134975=CARTESIAN_POINT('Origin',(-52.6623070233078,-46.93000002,-55.74995));
#134976=CARTESIAN_POINT('',(-52.6623070233078,-46.43000002,-55.2499500000008));
#134977=CARTESIAN_POINT('Ctrl Pts',(-52.2516983377878,-45.8864221486262,
-54.74995));
#134978=CARTESIAN_POINT('Ctrl Pts',(-52.2516983377878,-45.8864221486262,
-55.24995));
#134979=CARTESIAN_POINT('Ctrl Pts',(-52.7497956868337,-45.93000002,-55.24995));
#134980=CARTESIAN_POINT('Ctrl Pts',(-52.2287295285091,-46.1489568400132,
-54.7499500000658));
#134981=CARTESIAN_POINT('Ctrl Pts',(-52.2402778440398,-46.0169589895406,
-55.2386587236919));
#134982=CARTESIAN_POINT('Ctrl Pts',(-52.7268268775569,-46.0612673656941,
-55.24995));
#134983=CARTESIAN_POINT('Ctrl Pts',(-52.2060304199453,-46.4084088381247,
-54.8577231271255));
#134984=CARTESIAN_POINT('Ctrl Pts',(-52.227884321682,-46.1586175982532,
-55.2822894538777));
#134985=CARTESIAN_POINT('Ctrl Pts',(-52.704127768991,-46.1909933647493,
-55.3038365635627));
#134986=CARTESIAN_POINT('Ctrl Pts',(-52.1736386011181,-46.7786490215007,
-55.2279633105015));
#134987=CARTESIAN_POINT('Ctrl Pts',(-52.2097524154255,-46.3658662351156,
-55.4680441063688));
#134988=CARTESIAN_POINT('Ctrl Pts',(-52.6717359501641,-46.3761134564373,
-55.4889566552507));
#134989=CARTESIAN_POINT('Ctrl Pts',(-52.1642096742676,-46.8864221485606,
-55.487415308613));
#134990=CARTESIAN_POINT('Ctrl Pts',(-52.2041414362981,-46.4300000199443,
-55.6078478088784));
#134991=CARTESIAN_POINT('Ctrl Pts',(-52.6623070233132,-46.43000002,-55.6186826543062));
#134992=CARTESIAN_POINT('Ctrl Pts',(-52.1642096742619,-46.8864221486262,
-55.74995));
#134993=CARTESIAN_POINT('Ctrl Pts',(-52.2041414362991,-46.43000002,-55.74995));
#134994=CARTESIAN_POINT('Ctrl Pts',(-52.6623070233078,-46.43000002,-55.74995));
#134995=CARTESIAN_POINT('',(-52.7497956868337,-45.93000002,-55.24995));
#134996=CARTESIAN_POINT('Origin',(-52.7497956868337,-45.93000002,-54.74995));
#134997=CARTESIAN_POINT('Ctrl Pts',(-52.7497956868337,-45.93000002,-55.24995));
#134998=CARTESIAN_POINT('Ctrl Pts',(-52.7268268775569,-46.0612673656941,
-55.24995));
#134999=CARTESIAN_POINT('Ctrl Pts',(-52.704127768991,-46.1909933647493,
-55.3038365635627));
#135000=CARTESIAN_POINT('Ctrl Pts',(-52.6717359501641,-46.3761134564373,
-55.4889566552507));
#135001=CARTESIAN_POINT('Ctrl Pts',(-52.6623070233132,-46.43000002,-55.6186826543062));
#135002=CARTESIAN_POINT('Ctrl Pts',(-52.6623070233078,-46.43000002,-55.74995));
#135003=CARTESIAN_POINT('Origin',(-53.4839470922323,-37.5386110581466,-54.74995));
#135004=CARTESIAN_POINT('',(-52.7935400185966,-45.43000002,-55.24995));
#135005=CARTESIAN_POINT('Origin',(-52.7935400185966,-45.43000002,-54.74995));
#135006=CARTESIAN_POINT('',(-59.2602401389193,28.4847205815761,-55.24995));
#135007=CARTESIAN_POINT('Ctrl Pts',(-52.3829313330767,-44.3864221486262,
-55.74995));
#135008=CARTESIAN_POINT('Ctrl Pts',(-52.3353744315879,-44.93000002,-55.74995));
#135009=CARTESIAN_POINT('Ctrl Pts',(-52.8810286821225,-44.93000002,-55.74995));
#135010=CARTESIAN_POINT('Ctrl Pts',(-52.3829313330709,-44.3864221486917,
-55.4874153086129));
#135011=CARTESIAN_POINT('Ctrl Pts',(-52.3353744315888,-44.9300000200045,
-55.6317784220498));
#135012=CARTESIAN_POINT('Ctrl Pts',(-52.8810286821171,-44.93000002,-55.6186826543063));
#135013=CARTESIAN_POINT('Ctrl Pts',(-52.3735024062205,-44.4941952757516,
-55.2279633105015));
#135014=CARTESIAN_POINT('Ctrl Pts',(-52.3317239990966,-44.9717246542945,
-55.5133819370972));
#135015=CARTESIAN_POINT('Ctrl Pts',(-52.8715997552662,-44.9838865835627,
-55.4889566552507));
#135016=CARTESIAN_POINT('Ctrl Pts',(-52.3411105873933,-44.8644354591276,
-54.8577231271254));
#135017=CARTESIAN_POINT('Ctrl Pts',(-52.317584547802,-45.1333393221421,
-55.3274496218433));
#135018=CARTESIAN_POINT('Ctrl Pts',(-52.8392079364393,-45.1690066752507,
-55.3038365635627));
#135019=CARTESIAN_POINT('Ctrl Pts',(-52.3184114788294,-45.1238874572391,
-54.7499500000658));
#135020=CARTESIAN_POINT('Ctrl Pts',(-52.3071965192496,-45.252075031829,
-55.2615708605687));
#135021=CARTESIAN_POINT('Ctrl Pts',(-52.8165088278734,-45.2987326743059,
-55.24995));
#135022=CARTESIAN_POINT('Ctrl Pts',(-52.2954426695508,-45.3864221486262,
-54.74995));
#135023=CARTESIAN_POINT('Ctrl Pts',(-52.2954426695507,-45.3864221486261,
-55.2499499999999));
#135024=CARTESIAN_POINT('Ctrl Pts',(-52.7935400185966,-45.43000002,-55.24995));
#135025=CARTESIAN_POINT('',(-52.3810286821225,-44.43000002,-55.74995));
#135026=CARTESIAN_POINT('Origin',(-52.8810286821225,-44.43000002,-55.74995));
#135027=CARTESIAN_POINT('',(-52.8810286821225,-44.93000002,-55.74995));
#135028=CARTESIAN_POINT('Origin',(-52.8810286821225,-44.43000002,-55.74995));
#135029=CARTESIAN_POINT('Ctrl Pts',(-52.8810286821225,-44.93000002,-55.74995));
#135030=CARTESIAN_POINT('Ctrl Pts',(-52.8810286821171,-44.93000002,-55.6186826543063));
#135031=CARTESIAN_POINT('Ctrl Pts',(-52.8715997552662,-44.9838865835627,
-55.4889566552507));
#135032=CARTESIAN_POINT('Ctrl Pts',(-52.8392079364393,-45.1690066752507,
-55.3038365635627));
#135033=CARTESIAN_POINT('Ctrl Pts',(-52.8165088278734,-45.2987326743059,
-55.24995));
#135034=CARTESIAN_POINT('Ctrl Pts',(-52.7935400185966,-45.43000002,-55.24995));
#135035=CARTESIAN_POINT('Origin',(-52.8810286821225,-44.43000002,-52.64995));
#135036=CARTESIAN_POINT('',(-52.3810286821225,-44.43000002,-59.64995));
#135037=CARTESIAN_POINT('Origin',(-52.8810286821225,-44.43000002,-59.64995));
#135038=CARTESIAN_POINT('',(-52.8810286821225,-44.93000002,-59.64995));
#135039=CARTESIAN_POINT('Origin',(-52.8810286821225,-44.43000002,-59.64995));
#135040=CARTESIAN_POINT('',(-52.8810286821225,-44.93000002,-55.2499500000007));
#135041=CARTESIAN_POINT('Origin',(-53.7167487055513,-17.6671065732338,-59.64995));
#135042=CARTESIAN_POINT('',(-51.3752989258075,-44.43000002,-60.64995));
#135043=CARTESIAN_POINT('',(-53.7167487055513,-17.6671065732338,-60.64995));
#135044=CARTESIAN_POINT('Ctrl Pts',(-52.3829313330767,-44.3864221486262,
-59.64995));
#135045=CARTESIAN_POINT('Ctrl Pts',(-52.3829313330764,-44.3864221486294,
-59.7808732880376));
#135046=CARTESIAN_POINT('Ctrl Pts',(-52.3567053548786,-44.3875563641358,
-59.9116978933072));
#135047=CARTESIAN_POINT('Ctrl Pts',(-52.2557544114786,-44.3919222689988,
-60.153568971423));
#135048=CARTESIAN_POINT('Ctrl Pts',(-52.1810691443443,-44.3951522414979,
-60.2644967268049));
#135049=CARTESIAN_POINT('Ctrl Pts',(-51.9945361235173,-44.4032193817859,
-60.4496168355682));
#135050=CARTESIAN_POINT('Ctrl Pts',(-51.8827617223772,-44.4080533772395,
-60.5237363920407));
#135051=CARTESIAN_POINT('Ctrl Pts',(-51.6390445855899,-44.4185936039755,
-60.6239226729819));
#135052=CARTESIAN_POINT('Ctrl Pts',(-51.5072214737368,-44.4242946617934,
-60.64995));
#135053=CARTESIAN_POINT('Ctrl Pts',(-51.3752989258075,-44.43000002,-60.64995));
#135054=CARTESIAN_POINT('Origin',(0.,-12.9675000200281,-60.64995));
#135055=CARTESIAN_POINT('',(-39.5,31.080768958446,-60.64995));
#135056=CARTESIAN_POINT('',(-39.5,37.7483531044501,-60.64995));
#135057=CARTESIAN_POINT('',(-39.6638655462185,30.7106154376184,-60.64995));
#135058=CARTESIAN_POINT('Origin',(-40.,31.080768958446,-60.64995));
#135059=CARTESIAN_POINT('',(-41.4049466656476,29.0638025010082,-60.64995));
#135060=CARTESIAN_POINT('Origin',(0.,-12.9675000200281,-60.64995));
#135061=CARTESIAN_POINT('',(-41.7558360441701,28.91999998,-60.64995));
#135062=CARTESIAN_POINT('Origin',(-41.7558360441701,29.41999998,-60.64995));
#135063=CARTESIAN_POINT('',(-43.6738487993976,28.91999998,-60.64995));
#135064=CARTESIAN_POINT('',(-1.8346904061005E-14,28.9199999800001,-60.64995));
#135065=CARTESIAN_POINT('',(-45.342056117244,28.91999998,-60.64995));
#135066=CARTESIAN_POINT('Origin',(-44.5079524583208,31.5404524382925,-60.64995));
#135067=CARTESIAN_POINT('',(-1.8346904061005E-14,28.9199999800001,-60.64995));
#135068=CARTESIAN_POINT('Origin',(0.,-12.9675000200281,-60.64995));
#135069=CARTESIAN_POINT('',(-45.8586217441897,-55.08000002,-60.64995));
#135070=CARTESIAN_POINT('',(1.8445455022812E-14,-55.08000002,-60.64995));
#135071=CARTESIAN_POINT('',(-44.5079524583206,-60.2254524783489,-60.64995));
#135072=CARTESIAN_POINT('Origin',(-44.5079524583206,-57.4754524783489,-60.64995));
#135073=CARTESIAN_POINT('',(-42.,-58.6035812240174,-60.64995));
#135074=CARTESIAN_POINT('Origin',(-44.5079524583206,-57.4754524783489,-60.64995));
#135075=CARTESIAN_POINT('',(-42.,-12.9675000200281,-60.64995));
#135076=CARTESIAN_POINT('Origin',(-41.5,-73.08000002,-55.24995));
#135077=CARTESIAN_POINT('',(-24.7,-70.08000002,-55.24995));
#135078=CARTESIAN_POINT('',(-24.7,-73.08000002,-55.24995));
#135079=CARTESIAN_POINT('',(-24.2,-70.08000002,-55.24995));
#135080=CARTESIAN_POINT('',(-41.5,-70.08000002,-55.24995));
#135081=CARTESIAN_POINT('',(-24.2,-73.08000002,-55.24995));
#135082=CARTESIAN_POINT('Origin',(-24.7,67.7009572055632,-55.74995));
#135083=CARTESIAN_POINT('',(-25.2,-70.08000002,-55.74995));
#135084=CARTESIAN_POINT('',(-25.2,67.7009572055632,-55.74995));
#135085=CARTESIAN_POINT('Origin',(-24.7,-70.08000002,-55.74995));
#135086=CARTESIAN_POINT('Ctrl Pts',(-2.97685902995381,45.2502493063675,
-60.8508735991007));
#135087=CARTESIAN_POINT('Ctrl Pts',(-3.50000000000001,45.2282873890497,
-60.8406192095206));
#135088=CARTESIAN_POINT('Ctrl Pts',(-3.5,45.7028119503364,-61.0621827299711));
#135089=CARTESIAN_POINT('Ctrl Pts',(-2.97532164922327,45.3120457868827,
-60.7186918897092));
#135090=CARTESIAN_POINT('Ctrl Pts',(-3.49999999999858,45.2871516612883,
-60.7107288313429));
#135091=CARTESIAN_POINT('Ctrl Pts',(-3.5,45.7953890262578,-60.8639095446885));
#135092=CARTESIAN_POINT('Ctrl Pts',(-2.97452770132487,45.3441826962796,
-60.5756208725641));
#135093=CARTESIAN_POINT('Ctrl Pts',(-3.50000000000077,45.317377912702,-60.5716465029099));
#135094=CARTESIAN_POINT('Ctrl Pts',(-3.5,45.8435334327792,-60.6493041067215));
#135095=CARTESIAN_POINT('Ctrl Pts',(-2.97452770112504,45.3441826962898,
-60.42825533736));
#135096=CARTESIAN_POINT('Ctrl Pts',(-3.5,45.3173779148743,-60.42825533736));
#135097=CARTESIAN_POINT('Ctrl Pts',(-3.5,45.8435334367418,-60.42825533736));
#135098=CARTESIAN_POINT('',(-2.97685902995381,45.2502493063675,-60.8508735991007));
#135099=CARTESIAN_POINT('',(-3.5,45.7028119503364,-61.0621827299711));
#135100=CARTESIAN_POINT('Origin',(-3.,45.7028119503364,-61.0621827299711));
#135101=CARTESIAN_POINT('Origin',(-3.5,43.6249324139852,-60.2700376788023));
#135102=CARTESIAN_POINT('Origin',(-3.01135515498232,43.8637384804388,-60.3228490285208));
#135103=CARTESIAN_POINT('Ctrl Pts',(-2.96960200166493,31.2017108282785,
-90.9273317382593));
#135104=CARTESIAN_POINT('Ctrl Pts',(-3.5,31.1724436113174,-90.9136534008893));
#135105=CARTESIAN_POINT('Ctrl Pts',(-3.5,31.6538440087773,-91.1386408691297));
#135106=CARTESIAN_POINT('Ctrl Pts',(-2.97277930784816,35.8865598281193,
-80.9028133775132));
#135107=CARTESIAN_POINT('Ctrl Pts',(-3.50000000000001,35.8447898541155,
-80.9243218897256));
#135108=CARTESIAN_POINT('Ctrl Pts',(-3.5,36.338906312512,-81.114123180147));
#135109=CARTESIAN_POINT('Ctrl Pts',(-2.97501738453455,40.5689313038002,
-70.8770956617078));
#135110=CARTESIAN_POINT('Ctrl Pts',(-3.49999999995192,40.5360321489106,
-70.8854859061211));
#135111=CARTESIAN_POINT('Ctrl Pts',(-3.5,41.0213995348936,-71.0884053145847));
#135112=CARTESIAN_POINT('Ctrl Pts',(-2.97685902995381,45.2502493063675,
-60.8508735991007));
#135113=CARTESIAN_POINT('Ctrl Pts',(-3.5,45.2282873890496,-60.8406192095206));
#135114=CARTESIAN_POINT('Ctrl Pts',(-3.5,45.7028119503364,-61.0621827299711));
#135115=CARTESIAN_POINT('',(-2.96960200166493,31.2017108282785,-90.9273317382593));
#135116=CARTESIAN_POINT('Ctrl Pts',(-2.97685902995381,45.2502493063675,
-60.8508735991007));
#135117=CARTESIAN_POINT('Ctrl Pts',(-2.97501738453455,40.5689313038002,
-70.8770956617078));
#135118=CARTESIAN_POINT('Ctrl Pts',(-2.97277930784816,35.8865598281193,
-80.9028133775132));
#135119=CARTESIAN_POINT('Ctrl Pts',(-2.96960200166493,31.2017108282785,
-90.9273317382593));
#135120=CARTESIAN_POINT('',(-3.5,31.6538440087773,-91.1386408691296));
#135121=CARTESIAN_POINT('Origin',(-3.,31.6538440087773,-91.1386408691297));
#135122=CARTESIAN_POINT('Ctrl Pts',(-3.5,31.6538440087773,-91.1386408691296));
#135123=CARTESIAN_POINT('Ctrl Pts',(-3.5,36.3389063125119,-81.1141231801469));
#135124=CARTESIAN_POINT('Ctrl Pts',(-3.5,41.0213995348935,-71.0884053145847));
#135125=CARTESIAN_POINT('Ctrl Pts',(-3.5,45.7028119503364,-61.0621827299711));
#135126=CARTESIAN_POINT('Ctrl Pts',(-3.49999922403526,31.7061080469582,
-91.0538938313493));
#135127=CARTESIAN_POINT('Ctrl Pts',(-3.50093050801352,31.2817393765698,
-90.7398753859638));
#135128=CARTESIAN_POINT('Ctrl Pts',(-2.97306337601761,31.3045907584141,
-90.7567937156446));
#135129=CARTESIAN_POINT('Ctrl Pts',(-3.49999921701682,31.6355825669373,
-91.145911917233));
#135130=CARTESIAN_POINT('Ctrl Pts',(-3.50094379952756,31.1316678238861,
-90.9272671499976));
#135131=CARTESIAN_POINT('Ctrl Pts',(-2.96829288576189,31.1636053620749,
-90.9411478319373));
#135132=CARTESIAN_POINT('Ctrl Pts',(-3.49999921357759,31.6011902598928,
-91.2666067024717));
#135133=CARTESIAN_POINT('Ctrl Pts',(-3.5009502924524,31.0578568420018,-91.1768604568285));
#135134=CARTESIAN_POINT('Ctrl Pts',(-2.96595524421095,31.0948516197048,
-91.1829668200116));
#135135=CARTESIAN_POINT('Ctrl Pts',(-3.49999921461707,31.6116002328841,
-91.4242502749333));
#135136=CARTESIAN_POINT('Ctrl Pts',(-3.500948315334,31.0802325137817,-91.5041422369424));
#135137=CARTESIAN_POINT('Ctrl Pts',(-2.96666178933019,31.1156621951816,
-91.4988147743607));
#135138=CARTESIAN_POINT('Ctrl Pts',(-3.49999921542421,31.6196822275484,
-91.4659533973627));
#135139=CARTESIAN_POINT('Ctrl Pts',(-3.50094678207594,31.0975814779846,
-91.5905416925536));
#135140=CARTESIAN_POINT('Ctrl Pts',(-2.96721040786793,31.131818851425,-91.5823690954228));
#135141=CARTESIAN_POINT('Ctrl Pts',(-3.49999921802616,31.6457674414273,
-91.5452519327685));
#135142=CARTESIAN_POINT('Ctrl Pts',(-3.50094185515329,31.1534209463481,
-91.7542131679878));
#135143=CARTESIAN_POINT('Ctrl Pts',(-2.96897896666049,31.1839656512662,
-91.7412467109364));
#135144=CARTESIAN_POINT('Ctrl Pts',(-3.49999921980098,31.6635702854767,
-91.582854393305));
#135145=CARTESIAN_POINT('Ctrl Pts',(-3.50093850621097,31.1914043311977,
-91.8314070942134));
#135146=CARTESIAN_POINT('Ctrl Pts',(-2.97018531781006,31.2195550726727,
-91.8165839823916));
#135147=CARTESIAN_POINT('Ctrl Pts',(-3.49999922431731,31.7089557758124,
-91.6538544608224));
#135148=CARTESIAN_POINT('Ctrl Pts',(-3.50093003210323,31.2877585223428,
-91.9760692084669));
#135149=CARTESIAN_POINT('Ctrl Pts',(-2.97325503421203,31.3102843159908,
-91.9588322867574));
#135150=CARTESIAN_POINT('Ctrl Pts',(-3.4999992269732,31.7356790255681,-91.6858710465136));
#135151=CARTESIAN_POINT('Ctrl Pts',(-3.50092507815379,31.344184586453,-92.0406734083645));
#135152=CARTESIAN_POINT('Ctrl Pts',(-2.9750602060129,31.3637060404082,-92.0229763012619));
#135153=CARTESIAN_POINT('Ctrl Pts',(-3.49999923301664,31.7966270247391,
-91.7428001834818));
#135154=CARTESIAN_POINT('Ctrl Pts',(-3.50091389005982,31.4720263066748,
-92.1541680580386));
#135155=CARTESIAN_POINT('Ctrl Pts',(-2.97916779726235,31.4855450265412,
-92.1370294700019));
#135156=CARTESIAN_POINT('Ctrl Pts',(-3.49999923642963,31.8311111796843,
-91.7677027010548));
#135157=CARTESIAN_POINT('Ctrl Pts',(-3.50090762073163,31.5438509901872,
-92.2030328175872));
#135158=CARTESIAN_POINT('Ctrl Pts',(-2.98148749783816,31.5544807156723,
-92.1869184533145));
#135159=CARTESIAN_POINT('Ctrl Pts',(-3.49999925011377,31.9697383525658,
-91.8435168239899));
#135160=CARTESIAN_POINT('Ctrl Pts',(-3.50088282112773,31.8290423663707,
-92.3480552642004));
#135161=CARTESIAN_POINT('Ctrl Pts',(-2.99078795925646,31.831600651801,-92.3387960611338));
#135162=CARTESIAN_POINT('Ctrl Pts',(-3.49999926225773,32.0935311034211,
-91.8633729799761));
#135163=CARTESIAN_POINT('Ctrl Pts',(-3.50086127365168,32.0791885144776,
-92.3794664923917));
#135164=CARTESIAN_POINT('Ctrl Pts',(-2.99904131966573,32.0790639293044,
-92.3785629066546));
#135165=CARTESIAN_POINT('Ctrl Pts',(-3.49999927329452,32.2071461725455,
-91.8385626593204));
#135166=CARTESIAN_POINT('Ctrl Pts',(-3.50084210619723,32.3047109063527,
-92.3225314465932));
#135167=CARTESIAN_POINT('Ctrl Pts',(-3.00654191745144,32.3061822047335,
-92.3288444828576));
#135168=CARTESIAN_POINT('',(-2.96642434956618,31.1080206316559,-91.3499499999828));
#135169=CARTESIAN_POINT('Ctrl Pts',(-2.96960200166493,31.2017108282784,
-90.9273317382593));
#135170=CARTESIAN_POINT('Ctrl Pts',(-2.96907626063775,31.1861935567743,
-90.9606093101452));
#135171=CARTESIAN_POINT('Ctrl Pts',(-2.96861263948861,31.1725578229795,
-90.9946439154509));
#135172=CARTESIAN_POINT('Ctrl Pts',(-2.968215225744,31.1608577587541,-91.0291939475198));
#135173=CARTESIAN_POINT('Ctrl Pts',(-2.96801651887169,31.1550077266415,
-91.0464689635542));
#135174=CARTESIAN_POINT('Ctrl Pts',(-2.96783433959547,31.1496412337337,
-91.0638723528608));
#135175=CARTESIAN_POINT('Ctrl Pts',(-2.9676690065049,31.144762087643,-91.0813717845137));
#135176=CARTESIAN_POINT('Ctrl Pts',(-2.9675863399596,31.1423225145976,-91.0901215003401));
#135177=CARTESIAN_POINT('Ctrl Pts',(-2.96750788278562,31.1400047458653,
-91.0988951964481));
#135178=CARTESIAN_POINT('Ctrl Pts',(-2.9674336594212,31.1378090219179,-91.1076887806881));
#135179=CARTESIAN_POINT('Ctrl Pts',(-2.96739654773899,31.1367111599442,
-91.1120855728081));
#135180=CARTESIAN_POINT('Ctrl Pts',(-2.96736049435837,31.1356438069241,
-91.1164873356036));
#135181=CARTESIAN_POINT('Ctrl Pts',(-2.96732550136397,31.1346069783171,
-91.1208935530637));
#135182=CARTESIAN_POINT('Ctrl Pts',(-2.96730800486679,31.1340885640136,
-91.1230966617938));
#135183=CARTESIAN_POINT('Ctrl Pts',(-2.96729077345614,31.1335777806645,
-91.1253008841207));
#135184=CARTESIAN_POINT('Ctrl Pts',(-2.96727380732783,31.1330746292164,
-91.1275061555234));
#135185=CARTESIAN_POINT('Ctrl Pts',(-2.96726030613665,31.1326742347498,
-91.1292610515298));
#135186=CARTESIAN_POINT('Ctrl Pts',(-2.96723992575453,31.1320713979023,
-91.131945205737));
#135187=CARTESIAN_POINT('Ctrl Pts',(-2.96722952789365,31.1317615130644,
-91.1333418601676));
#135188=CARTESIAN_POINT('Ctrl Pts',(-2.96722685939323,31.1316819844165,
-91.1337002966734));
#135189=CARTESIAN_POINT('Ctrl Pts',(-2.96722483060121,31.1316214861816,
-91.1339738745067));
#135190=CARTESIAN_POINT('Ctrl Pts',(-2.96722370494375,31.1315880708905,
-91.1341250523127));
#135191=CARTESIAN_POINT('Ctrl Pts',(-2.96719059076607,31.1306050721212,
-91.1385723455124));
#135192=CARTESIAN_POINT('Ctrl Pts',(-2.96714968507035,31.1292784394994,
-91.1446972176635));
#135193=CARTESIAN_POINT('Ctrl Pts',(-2.96710052166565,31.127704189862,-91.1525124220698));
#135194=CARTESIAN_POINT('Ctrl Pts',(-2.9670513411666,31.1261293928509,-91.160330343858));
#135195=CARTESIAN_POINT('Ctrl Pts',(-2.96699389511064,31.1243067798829,
-91.1698401921196));
#135196=CARTESIAN_POINT('Ctrl Pts',(-2.96693120584415,31.1223842739554,
-91.1810590360774));
#135197=CARTESIAN_POINT('Ctrl Pts',(-2.96686889195463,31.1204732797982,
-91.1922107027374));
#135198=CARTESIAN_POINT('Ctrl Pts',(-2.96680140002913,31.1184636257961,
-91.2050515373047));
#135199=CARTESIAN_POINT('Ctrl Pts',(-2.96673513845011,31.1165516198435,
-91.2195950992161));
#135200=CARTESIAN_POINT('Ctrl Pts',(-2.96666947809326,31.1146569624116,
-91.2340067006156));
#135201=CARTESIAN_POINT('Ctrl Pts',(-2.96660503372642,31.112858304374,-91.2500909687296));
#135202=CARTESIAN_POINT('Ctrl Pts',(-2.96655135114763,31.1113957530503,
-91.2678484443061));
#135203=CARTESIAN_POINT('Ctrl Pts',(-2.96649881526904,31.109964442921,-91.2852266068699));
#135204=CARTESIAN_POINT('Ctrl Pts',(-2.96645660610933,31.1088553216018,
-91.3042079708774));
#135205=CARTESIAN_POINT('Ctrl Pts',(-2.96643664336358,31.1083375749915,
-91.3247705156409));
#135206=CARTESIAN_POINT('Ctrl Pts',(-2.96642873475368,31.1081324601229,
-91.3329167469847));
#135207=CARTESIAN_POINT('Ctrl Pts',(-2.96642434935722,31.1080206316701,
-91.3413108330902));
#135208=CARTESIAN_POINT('Ctrl Pts',(-2.96642434956618,31.1080206316559,
-91.3499499999828));
#135209=CARTESIAN_POINT('',(-3.,32.1080106234021,-92.34995));
#135210=CARTESIAN_POINT('Ctrl Pts',(-2.96642434956619,31.1080206316559,
-91.3499499999828));
#135211=CARTESIAN_POINT('Ctrl Pts',(-2.9664271070228,31.108045768609,-91.37190912875));
#135212=CARTESIAN_POINT('Ctrl Pts',(-2.96645079020869,31.1087442225408,
-91.3938431330336));
#135213=CARTESIAN_POINT('Ctrl Pts',(-2.96668560519294,31.1156606164675,
-91.4988150117475));
#135214=CARTESIAN_POINT('Ctrl Pts',(-2.96723421322274,31.1318173249492,
-91.5823694597986));
#135215=CARTESIAN_POINT('Ctrl Pts',(-2.96900273785673,31.1839642868761,
-91.7412472901304));
#135216=CARTESIAN_POINT('Ctrl Pts',(-2.97020906550757,31.2195538136165,
-91.8165846453629));
#135217=CARTESIAN_POINT('Ctrl Pts',(-2.97327872125958,31.3102833052691,
-91.95883306017));
#135218=CARTESIAN_POINT('Ctrl Pts',(-2.97508385688375,31.3637051628446,
-92.0229770968143));
#135219=CARTESIAN_POINT('Ctrl Pts',(-2.97919136429243,31.485544416253,-92.1370302437053));
#135220=CARTESIAN_POINT('Ctrl Pts',(-2.98151101664575,31.5544802346756,
-92.1869191824921));
#135221=CARTESIAN_POINT('Ctrl Pts',(-2.98885332885225,31.7732594207181,
-92.3068223160387));
#135222=CARTESIAN_POINT('Ctrl Pts',(-2.99446266807111,31.9411884844373,
-92.349950020068));
#135223=CARTESIAN_POINT('Ctrl Pts',(-3.,32.1080106234021,-92.34995));
#135224=CARTESIAN_POINT('',(-3.5,32.1080106234021,-91.84995));
#135225=CARTESIAN_POINT('Origin',(-3.,32.1080106234021,-91.84995));
#135226=CARTESIAN_POINT('Ctrl Pts',(-3.5,32.1080106234021,-91.84995));
#135227=CARTESIAN_POINT('Ctrl Pts',(-3.5,31.9390236361236,-91.84995));
#135228=CARTESIAN_POINT('Ctrl Pts',(-3.5,31.7764555346939,-91.7610777969008));
#135229=CARTESIAN_POINT('Ctrl Pts',(-3.5,31.5945841314222,-91.476580999558));
#135230=CARTESIAN_POINT('Ctrl Pts',(-3.5,31.5822909477801,-91.2917412718895));
#135231=CARTESIAN_POINT('Ctrl Pts',(-3.5,31.6538440087773,-91.1386408691296));
#135232=CARTESIAN_POINT('Origin',(-38.,46.41999998,-91.84995));
#135233=CARTESIAN_POINT('',(-37.,46.41999998,-92.34995));
#135234=CARTESIAN_POINT('',(-37.5,46.41999998,-91.84995));
#135235=CARTESIAN_POINT('Origin',(-37.,46.41999998,-91.84995));
#135236=CARTESIAN_POINT('',(-38.,47.41999998,-92.34995));
#135237=CARTESIAN_POINT('Origin',(-38.,46.41999998,-92.34995));
#135238=CARTESIAN_POINT('',(-38.,46.91999998,-91.84995));
#135239=CARTESIAN_POINT('Origin',(-38.,47.41999998,-91.84995));
#135240=CARTESIAN_POINT('Origin',(-38.,46.41999998,-91.84995));
#135241=CARTESIAN_POINT('Origin',(41.5,47.41999998,-91.84995));
#135242=CARTESIAN_POINT('',(-38.5,47.41999998,-92.34995));
#135243=CARTESIAN_POINT('',(41.5,47.41999998,-92.34995));
#135244=CARTESIAN_POINT('',(-38.5,46.91999998,-91.84995));
#135245=CARTESIAN_POINT('Origin',(-38.5,47.41999998,-91.84995));
#135246=CARTESIAN_POINT('',(39.,46.91999998,-91.84995));
#135247=CARTESIAN_POINT('Origin',(-38.5,58.91999998,-95.34995));
#135248=CARTESIAN_POINT('',(-40.9899542848408,29.0638025010082,-93.6765918018241));
#135249=CARTESIAN_POINT('',(-41.2907166092886,28.91999998,-94.2490863360338));
#135250=CARTESIAN_POINT('Ctrl Pts',(-40.9899542848408,29.0638025010082,
-93.6765918018241));
#135251=CARTESIAN_POINT('Ctrl Pts',(-41.0445777715999,29.0010249744694,
-93.7578714615268));
#135252=CARTESIAN_POINT('Ctrl Pts',(-41.1012013116007,28.9670983124193,
-93.8513385014916));
#135253=CARTESIAN_POINT('Ctrl Pts',(-41.203906529354,28.9262911739198,-94.0457359962981));
#135254=CARTESIAN_POINT('Ctrl Pts',(-41.2500626594833,28.9199999557335,
-94.1460275680244));
#135255=CARTESIAN_POINT('Ctrl Pts',(-41.2907166092886,28.91999998,-94.2490863360338));
#135256=CARTESIAN_POINT('',(-39.4975990396159,30.7106154376184,-92.5206751536556));
#135257=CARTESIAN_POINT('Ctrl Pts',(-39.4975990396159,30.7106154376184,
-92.5206751536556));
#135258=CARTESIAN_POINT('Ctrl Pts',(-39.7830757934441,30.4081688522969,
-92.6213339269874));
#135259=CARTESIAN_POINT('Ctrl Pts',(-40.0606440851126,30.1068692044787,
-92.7683994467215));
#135260=CARTESIAN_POINT('Ctrl Pts',(-40.5646325235533,29.548843193136,-93.1505624120075));
#135261=CARTESIAN_POINT('Ctrl Pts',(-40.7930602005308,29.2900891143653,
-93.3836137237161));
#135262=CARTESIAN_POINT('Ctrl Pts',(-40.9899542848408,29.0638025010082,
-93.6765918018241));
#135263=CARTESIAN_POINT('',(-39.3571428571429,31.080768958446,-92.4750054575003));
#135264=CARTESIAN_POINT('Ctrl Pts',(-39.3571428571429,31.080768958446,-92.4750054575003));
#135265=CARTESIAN_POINT('Ctrl Pts',(-39.3571429430277,30.9391538899445,
-92.4750054831062));
#135266=CARTESIAN_POINT('Ctrl Pts',(-39.410274588038,30.8031308123719,-92.4898846529936));
#135267=CARTESIAN_POINT('Ctrl Pts',(-39.4975990396159,30.7106154376184,
-92.5206751536556));
#135268=CARTESIAN_POINT('',(-39.3571428571429,46.41999998,-92.4750054575003));
#135269=CARTESIAN_POINT('',(-39.3571428571429,58.91999998,-92.4750054575003));
#135270=CARTESIAN_POINT('Ctrl Pts',(-38.5,47.41999998,-92.34995));
#135271=CARTESIAN_POINT('Ctrl Pts',(-38.6117163199788,47.4199999701223,
-92.34995));
#135272=CARTESIAN_POINT('Ctrl Pts',(-38.7257728904125,47.3934379073013,
-92.3566603033275));
#135273=CARTESIAN_POINT('Ctrl Pts',(-38.9319509445986,47.2935007246494,
-92.3793987064332));
#135274=CARTESIAN_POINT('Ctrl Pts',(-39.0271570378558,47.2191189043121,
-92.3955365750638));
#135275=CARTESIAN_POINT('Ctrl Pts',(-39.1845108402481,47.0356954006484,
-92.4279818041452));
#135276=CARTESIAN_POINT('Ctrl Pts',(-39.2481885236226,46.925205464765,-92.444400991043));
#135277=CARTESIAN_POINT('Ctrl Pts',(-39.3344873999803,46.6833015096169,
-92.4680006788624));
#135278=CARTESIAN_POINT('Ctrl Pts',(-39.3571428368889,46.5515558031783,
-92.4750054514617));
#135279=CARTESIAN_POINT('Ctrl Pts',(-39.3571428571429,46.41999998,-92.4750054575003));
#135280=CARTESIAN_POINT('',(-38.5,58.91999998,-92.34995));
#135281=CARTESIAN_POINT('',(-38.5,58.91999998,-92.34995));
#135282=CARTESIAN_POINT('',(-41.5,58.91999998,-95.34995));
#135283=CARTESIAN_POINT('Origin',(-38.5,58.91999998,-95.34995));
#135284=CARTESIAN_POINT('',(-41.5,28.91999998,-95.34995));
#135285=CARTESIAN_POINT('',(-41.5,58.91999998,-95.34995));
#135286=CARTESIAN_POINT('Origin',(-38.5,28.91999998,-95.34995));
#135287=CARTESIAN_POINT('Origin',(-3.,58.91999998,-91.84995));
#135288=CARTESIAN_POINT('',(-3.,46.41999998,-92.34995));
#135289=CARTESIAN_POINT('',(-3.,46.41999998,-92.34995));
#135290=CARTESIAN_POINT('',(-3.5,46.41999998,-91.84995));
#135291=CARTESIAN_POINT('Origin',(-3.,46.41999998,-91.84995));
#135292=CARTESIAN_POINT('',(-3.5,32.0719455778696,-91.84995));
#135293=CARTESIAN_POINT('Origin',(-4.,46.41999998,-91.84995));
#135294=CARTESIAN_POINT('',(-4.,47.41999998,-92.34995));
#135295=CARTESIAN_POINT('Origin',(-4.,46.41999998,-92.34995));
#135296=CARTESIAN_POINT('',(-4.,46.91999998,-91.84995));
#135297=CARTESIAN_POINT('Origin',(-4.,47.41999998,-91.84995));
#135298=CARTESIAN_POINT('Origin',(-4.,46.41999998,-91.84995));
#135299=CARTESIAN_POINT('Origin',(41.5,47.41999998,-91.84995));
#135300=CARTESIAN_POINT('',(-4.5,47.41999998,-92.34995));
#135301=CARTESIAN_POINT('',(41.5,47.41999998,-92.34995));
#135302=CARTESIAN_POINT('',(-4.5,46.91999998,-91.84995));
#135303=CARTESIAN_POINT('Origin',(-4.5,47.41999998,-91.84995));
#135304=CARTESIAN_POINT('',(39.,46.91999998,-91.84995));
#135305=CARTESIAN_POINT('Origin',(-4.5,46.41999998,-91.84995));
#135306=CARTESIAN_POINT('',(-5.5,46.41999998,-92.34995));
#135307=CARTESIAN_POINT('Origin',(-4.5,46.41999998,-92.34995));
#135308=CARTESIAN_POINT('',(-5.,46.41999998,-91.84995));
#135309=CARTESIAN_POINT('Origin',(-5.5,46.41999998,-91.84995));
#135310=CARTESIAN_POINT('Origin',(-4.5,46.41999998,-91.84995));
#135311=CARTESIAN_POINT('Origin',(-5.5,-9.33460238845303,-91.84995));
#135312=CARTESIAN_POINT('',(-5.5,31.8716754827171,-92.34995));
#135313=CARTESIAN_POINT('',(-5.5,31.9301798728793,-92.34995));
#135314=CARTESIAN_POINT('',(-5.,31.8716754827171,-91.84995));
#135315=CARTESIAN_POINT('Origin',(-5.5,31.8716754827171,-91.84995));
#135316=CARTESIAN_POINT('',(-5.,46.41999998,-91.84995));
#135317=CARTESIAN_POINT('Origin',(-1.1373643128445E-15,-12.9675000200281,
-91.34995));
#135318=CARTESIAN_POINT('',(-11.3834743397155,29.812801930373,-90.9273317382593));
#135319=CARTESIAN_POINT('',(-11.3712933400039,29.7190889970661,-91.3499500007659));
#135320=CARTESIAN_POINT('Origin',(-11.4527257127636,30.3470007156979,-91.2823260948233));
#135321=CARTESIAN_POINT('',(-5.44427033638568,30.9653765476951,-90.9273317382593));
#135322=CARTESIAN_POINT('Origin',(-1.1373643128445E-15,-12.9675000200281,
-90.9273317382593));
#135323=CARTESIAN_POINT('',(-5.43844464087133,30.8716892291688,-91.34995));
#135324=CARTESIAN_POINT('Origin',(-5.47960007965946,31.5342994497431,-91.2881238021625));
#135325=CARTESIAN_POINT('Ctrl Pts',(-5.5,31.8716754827171,-92.34995));
#135326=CARTESIAN_POINT('Ctrl Pts',(-5.48989377680063,31.7056523166615,
-92.34995));
#135327=CARTESIAN_POINT('Ctrl Pts',(-5.47963373781052,31.538103809625,-92.3071746231476));
#135328=CARTESIAN_POINT('Ctrl Pts',(-5.46619042199875,31.3196047327668,
-92.1878686007335));
#135329=CARTESIAN_POINT('Ctrl Pts',(-5.46194839019336,31.2508398250121,
-92.1383294170381));
#135330=CARTESIAN_POINT('Ctrl Pts',(-5.45439667136824,31.1286541135227,
-92.0244078521253));
#135331=CARTESIAN_POINT('Ctrl Pts',(-5.45108997919633,31.0752759499814,
-91.9605552262364));
#135332=CARTESIAN_POINT('Ctrl Pts',(-5.44262999595016,30.938884482232,-91.7477840212027));
#135333=CARTESIAN_POINT('Ctrl Pts',(-5.43928039898085,30.8851161679224,
-91.5835323055617));
#135334=CARTESIAN_POINT('Ctrl Pts',(-5.43849137201243,30.8724399372431,
-91.3946568152791));
#135335=CARTESIAN_POINT('Ctrl Pts',(-5.43844622689811,30.8717137358109,
-91.3723154432813));
#135336=CARTESIAN_POINT('Ctrl Pts',(-5.43844464087133,30.8716892291688,
-91.34995));
#135337=CARTESIAN_POINT('',(-11.5,30.7194735506599,-92.34995));
#135338=CARTESIAN_POINT('Origin',(-1.1373643128445E-15,-12.9675000200281,
-92.34995));
#135339=CARTESIAN_POINT('Ctrl Pts',(-11.3712933400038,29.719088997066,-91.3499500007659));
#135340=CARTESIAN_POINT('Ctrl Pts',(-11.3713013356712,29.7190868671284,
-91.3885031985189));
#135341=CARTESIAN_POINT('Ctrl Pts',(-11.3715900563149,29.7213217313681,
-91.4271147023396));
#135342=CARTESIAN_POINT('Ctrl Pts',(-11.3721684286715,29.7257851411112,
-91.4654778746805));
#135343=CARTESIAN_POINT('Ctrl Pts',(-11.3727466124145,29.7302470952876,
-91.5038285363716));
#135344=CARTESIAN_POINT('Ctrl Pts',(-11.373614238183,29.736936078301,-91.5419303731955));
#135345=CARTESIAN_POINT('Ctrl Pts',(-11.3747663901512,29.7457936995826,
-91.579482237));
#135346=CARTESIAN_POINT('Ctrl Pts',(-11.3759196281462,29.7546596701221,
-91.6170694974632));
#135347=CARTESIAN_POINT('Ctrl Pts',(-11.3773578751843,29.7656981886916,
-91.654105115319));
#135348=CARTESIAN_POINT('Ctrl Pts',(-11.3790628963733,29.7788024661424,
-91.6903019838639));
#135349=CARTESIAN_POINT('Ctrl Pts',(-11.3798254998803,29.7846636061715,
-91.7064917292316));
#135350=CARTESIAN_POINT('Ctrl Pts',(-11.3806412991493,29.7909373746637,
-91.7225139392306));
#135351=CARTESIAN_POINT('Ctrl Pts',(-11.3815078564561,29.7976112818844,
-91.7383443849165));
#135352=CARTESIAN_POINT('Ctrl Pts',(-11.3834559407968,29.8126147144873,
-91.7739323871261));
#135353=CARTESIAN_POINT('Ctrl Pts',(-11.3856671264025,29.8296923799048,
-91.8086655197473));
#135354=CARTESIAN_POINT('Ctrl Pts',(-11.388129442384,29.8487050388042,-91.8422692512968));
#135355=CARTESIAN_POINT('Ctrl Pts',(-11.3905921149091,29.8677204507392,
-91.875877848671));
#135356=CARTESIAN_POINT('Ctrl Pts',(-11.3933058886042,29.8886710747684,
-91.9083561622676));
#135357=CARTESIAN_POINT('Ctrl Pts',(-11.3962472964129,29.911374995788,-91.9394573269113));
#135358=CARTESIAN_POINT('Ctrl Pts',(-11.3991934464272,29.9341155205936,
-91.9706086335712));
#135359=CARTESIAN_POINT('Ctrl Pts',(-11.4023678382941,29.9586145652146,
-92.0003778665942));
#135360=CARTESIAN_POINT('Ctrl Pts',(-11.4057370832413,29.9846524195957,
-92.0285526540719));
#135361=CARTESIAN_POINT('Ctrl Pts',(-11.4071664410782,29.9956986367154,
-92.0405054369404));
#135362=CARTESIAN_POINT('Ctrl Pts',(-11.408630758751,30.0070213892768,-92.0521717366627));
#135363=CARTESIAN_POINT('Ctrl Pts',(-11.410127046267,30.0186022152685,-92.0635375721449));
#135364=CARTESIAN_POINT('Ctrl Pts',(-11.4142954954677,30.0508647880247,
-92.0952012112017));
#135365=CARTESIAN_POINT('Ctrl Pts',(-11.4187247812978,30.0852050202082,
-92.1246026482632));
#135366=CARTESIAN_POINT('Ctrl Pts',(-11.4233738906191,30.1212889057877,
-92.1515089998868));
#135367=CARTESIAN_POINT('Ctrl Pts',(-11.4280432727768,30.157530138217,-92.1785326789434));
#135368=CARTESIAN_POINT('Ctrl Pts',(-11.432934281018,30.1955298850529,-92.2030393156081));
#135369=CARTESIAN_POINT('Ctrl Pts',(-11.438000215523,30.2349279316181,-92.2248405680941));
#135370=CARTESIAN_POINT('Ctrl Pts',(-11.4430983663307,30.2745765261115,
-92.2467804634601));
#135371=CARTESIAN_POINT('Ctrl Pts',(-11.4483735571548,30.3156408743999,
-92.265980333651));
#135372=CARTESIAN_POINT('Ctrl Pts',(-11.4537747777112,30.3577375734027,
-92.2822984029973));
#135373=CARTESIAN_POINT('Ctrl Pts',(-11.4591922473244,30.3999609163087,
-92.2986655636985));
#135374=CARTESIAN_POINT('Ctrl Pts',(-11.4647363885862,30.4432224293095,
-92.3121335087565));
#135375=CARTESIAN_POINT('Ctrl Pts',(-11.4703540873708,30.4871248827319,
-92.3226107580528));
#135376=CARTESIAN_POINT('Ctrl Pts',(-11.4759973775821,30.5312273337798,
-92.3331357364579));
#135377=CARTESIAN_POINT('Ctrl Pts',(-11.4817147834776,30.5759761761234,
-92.3406426903389));
#135378=CARTESIAN_POINT('Ctrl Pts',(-11.4874525496363,30.6209643473028,
-92.3450913875843));
#135379=CARTESIAN_POINT('Ctrl Pts',(-11.4916309796454,30.6537262130378,
-92.3483310752184));
#135380=CARTESIAN_POINT('Ctrl Pts',(-11.495820204077,30.6866148885679,-92.34995));
#135381=CARTESIAN_POINT('Ctrl Pts',(-11.5,30.7194735506599,-92.34995));
#135382=CARTESIAN_POINT('Origin',(-11.5,58.91999998,-91.84995));
#135383=CARTESIAN_POINT('',(-12.,30.7194735506599,-91.84995));
#135384=CARTESIAN_POINT('Origin',(-11.5,30.7194735506599,-91.84995));
#135385=CARTESIAN_POINT('',(-11.5,46.41999998,-92.34995));
#135386=CARTESIAN_POINT('',(-11.5,46.41999998,-92.34995));
#135387=CARTESIAN_POINT('',(-12.,46.41999998,-91.84995));
#135388=CARTESIAN_POINT('Origin',(-11.5,46.41999998,-91.84995));
#135389=CARTESIAN_POINT('',(-12.,30.5847864844252,-91.84995));
#135390=CARTESIAN_POINT('Origin',(-12.5,46.41999998,-91.84995));
#135391=CARTESIAN_POINT('',(-12.5,47.41999998,-92.34995));
#135392=CARTESIAN_POINT('Origin',(-12.5,46.41999998,-92.34995));
#135393=CARTESIAN_POINT('',(-12.5,46.91999998,-91.84995));
#135394=CARTESIAN_POINT('Origin',(-12.5,47.41999998,-91.84995));
#135395=CARTESIAN_POINT('Origin',(-12.5,46.41999998,-91.84995));
#135396=CARTESIAN_POINT('Origin',(41.5,47.41999998,-91.84995));
#135397=CARTESIAN_POINT('',(-13.,47.41999998,-92.34995));
#135398=CARTESIAN_POINT('',(41.5,47.41999998,-92.34995));
#135399=CARTESIAN_POINT('',(-13.,46.91999998,-91.84995));
#135400=CARTESIAN_POINT('Origin',(-13.,47.41999998,-91.84995));
#135401=CARTESIAN_POINT('',(39.,46.91999998,-91.84995));
#135402=CARTESIAN_POINT('Origin',(-13.,46.41999998,-91.84995));
#135403=CARTESIAN_POINT('',(-14.,46.41999998,-92.34995));
#135404=CARTESIAN_POINT('Origin',(-13.,46.41999998,-92.34995));
#135405=CARTESIAN_POINT('',(-13.5,46.41999998,-91.84995));
#135406=CARTESIAN_POINT('Origin',(-14.,46.41999998,-91.84995));
#135407=CARTESIAN_POINT('Origin',(-13.,46.41999998,-91.84995));
#135408=CARTESIAN_POINT('Origin',(-14.,-9.33460238845303,-91.84995));
#135409=CARTESIAN_POINT('',(-14.,29.9836543272765,-92.34995));
#135410=CARTESIAN_POINT('',(-14.,30.1434227231235,-92.34995));
#135411=CARTESIAN_POINT('',(-13.5,29.9836543272765,-91.84995));
#135412=CARTESIAN_POINT('Origin',(-14.,29.9836543272765,-91.84995));
#135413=CARTESIAN_POINT('',(-13.5,46.41999998,-91.84995));
#135414=CARTESIAN_POINT('Origin',(-1.1373643128445E-15,-12.9675000200281,
-91.34995));
#135415=CARTESIAN_POINT('',(-14.0295223410747,29.9740202447141,-92.34995));
#135416=CARTESIAN_POINT('Origin',(-1.1373643128445E-15,-12.9675000200281,
-92.34995));
#135417=CARTESIAN_POINT('',(-13.9704776589253,29.7932964571609,-92.3317099697081));
#135418=CARTESIAN_POINT('Origin',(-14.0295223410747,29.9740202447144,-91.34995));
#135419=CARTESIAN_POINT('Origin',(-13.9965098969202,29.9839599889458,-91.3260842600189));
#135420=CARTESIAN_POINT('Ctrl Pts',(-17.5283605562717,29.4199999800001,
-92.34995));
#135421=CARTESIAN_POINT('Ctrl Pts',(-17.5283605562716,28.41999998,-92.34995));
#135422=CARTESIAN_POINT('Ctrl Pts',(-17.5283605562717,28.4199999800001,
-91.34995));
#135423=CARTESIAN_POINT('Ctrl Pts',(-16.9294484484718,29.4199999819522,
-92.34995));
#135424=CARTESIAN_POINT('Ctrl Pts',(-16.8501904102942,28.3452044605545,
-92.3499500000001));
#135425=CARTESIAN_POINT('Ctrl Pts',(-16.8748117549663,28.4199999800001,
-91.2778699709694));
#135426=CARTESIAN_POINT('Ctrl Pts',(-16.3387077693293,29.4682775272991,
-92.34995));
#135427=CARTESIAN_POINT('Ctrl Pts',(-16.1934854928648,28.3221299458475,
-92.34995));
#135428=CARTESIAN_POINT('Ctrl Pts',(-16.233134779349,28.4803469141606,-91.2065756291954));
#135429=CARTESIAN_POINT('Ctrl Pts',(-15.1723882243972,29.6527167118161,
-92.34995));
#135430=CARTESIAN_POINT('Ctrl Pts',(-14.8701093399109,28.3452025116243,
-92.34995));
#135431=CARTESIAN_POINT('Ctrl Pts',(-14.9727946058278,28.7108958947333,
-91.0656179778369));
#135432=CARTESIAN_POINT('Ctrl Pts',(-14.5966754937866,29.7887243470281,
-92.34995));
#135433=CARTESIAN_POINT('Ctrl Pts',(-14.194875318369,28.3987342821361,-92.3499499999805));
#135434=CARTESIAN_POINT('Ctrl Pts',(-14.3539522178783,28.8809201843631,
-90.9959326732687));
#135435=CARTESIAN_POINT('Ctrl Pts',(-14.0295223410746,29.9740202447142,
-92.34995));
#135436=CARTESIAN_POINT('Ctrl Pts',(-13.5420441920761,28.4819485757734,
-92.3499500000002));
#135437=CARTESIAN_POINT('Ctrl Pts',(-13.7480613600421,29.1125253108927,
-90.92733173826));
#135438=CARTESIAN_POINT('',(-17.5283605562717,29.41999998,-92.34995));
#135439=CARTESIAN_POINT('Ctrl Pts',(-14.0295223410747,29.9740202447141,
-92.34995));
#135440=CARTESIAN_POINT('Ctrl Pts',(-14.5967291533814,29.7887068092282,
-92.34995));
#135441=CARTESIAN_POINT('Ctrl Pts',(-15.1723882243932,29.6527167117912,
-92.34995));
#135442=CARTESIAN_POINT('Ctrl Pts',(-16.3387077693334,29.4682775273239,
-92.34995));
#135443=CARTESIAN_POINT('Ctrl Pts',(-16.9293976390415,29.4199999800001,
-92.34995));
#135444=CARTESIAN_POINT('Ctrl Pts',(-17.5283605562717,29.41999998,-92.34995));
#135445=CARTESIAN_POINT('',(-17.5283474636365,28.4199999800081,-91.3499485560105));
#135446=CARTESIAN_POINT('Origin',(-17.5283605562717,29.41999998,-91.34995));
#135447=CARTESIAN_POINT('',(-13.862967014578,29.069410410554,-90.9403371832688));
#135448=CARTESIAN_POINT('Ctrl Pts',(-17.5283474636365,28.4199999800081,
-91.3499485560106));
#135449=CARTESIAN_POINT('Ctrl Pts',(-16.8748031850957,28.4200007859617,
-91.2778690188029));
#135450=CARTESIAN_POINT('Ctrl Pts',(-16.2331305712531,28.4803476839308,
-91.2065751585579));
#135451=CARTESIAN_POINT('Ctrl Pts',(-15.0125763307461,28.7036187831106,
-91.0700672040294));
#135452=CARTESIAN_POINT('Ctrl Pts',(-14.4321306085786,28.8596715997071,
-91.0047341003281));
#135453=CARTESIAN_POINT('Ctrl Pts',(-13.8629670146618,29.0694104105324,
-90.9403371832586));
#135454=CARTESIAN_POINT('Ctrl Pts',(-13.9704776589253,29.7932964571609,
-92.3317099697081));
#135455=CARTESIAN_POINT('Ctrl Pts',(-13.9485824763266,29.6507732526529,
-92.3041572803908));
#135456=CARTESIAN_POINT('Ctrl Pts',(-13.9277414892694,29.5120300570818,
-92.2444171371624));
#135457=CARTESIAN_POINT('Ctrl Pts',(-13.8924131672203,29.2732201982241,
-92.0703719609639));
#135458=CARTESIAN_POINT('Ctrl Pts',(-13.8776710606793,29.1715523493698,
-91.9547463954628));
#135459=CARTESIAN_POINT('Ctrl Pts',(-13.8571693529918,29.0291974882966,
-91.6899374203782));
#135460=CARTESIAN_POINT('Ctrl Pts',(-13.851254772454,28.9875557647693,-91.5391474846049));
#135461=CARTESIAN_POINT('Ctrl Pts',(-13.8496827900737,28.9765232161018,
-91.2324126084916));
#135462=CARTESIAN_POINT('Ctrl Pts',(-13.8539744318671,29.0067940350096,
-91.0793665022882));
#135463=CARTESIAN_POINT('Ctrl Pts',(-13.8629670146618,29.0694104105324,
-90.9403371832586));
#135464=CARTESIAN_POINT('Origin',(-60.,29.41999998,-91.34995));
#135465=CARTESIAN_POINT('',(-20.,28.4199999800001,-91.34995));
#135466=CARTESIAN_POINT('',(-16.1621051845127,28.4199999800001,-91.34995));
#135467=CARTESIAN_POINT('',(-20.,29.41999998,-92.34995));
#135468=CARTESIAN_POINT('',(-20.5,29.41999998,-92.34995));
#135469=CARTESIAN_POINT('Origin',(-20.,29.41999998,-91.34995));
#135470=CARTESIAN_POINT('Origin',(-20.,58.91999998,-91.84995));
#135471=CARTESIAN_POINT('',(-20.5,29.41999998,-91.84995));
#135472=CARTESIAN_POINT('Origin',(-20.,29.41999998,-91.84995));
#135473=CARTESIAN_POINT('',(-20.,46.41999998,-92.34995));
#135474=CARTESIAN_POINT('',(-20.,46.41999998,-92.34995));
#135475=CARTESIAN_POINT('',(-20.5,46.41999998,-91.84995));
#135476=CARTESIAN_POINT('Origin',(-20.,46.41999998,-91.84995));
#135477=CARTESIAN_POINT('',(-20.5,29.41999998,-91.84995));
#135478=CARTESIAN_POINT('Origin',(-21.,46.41999998,-91.84995));
#135479=CARTESIAN_POINT('',(-21.,47.41999998,-92.34995));
#135480=CARTESIAN_POINT('Origin',(-21.,46.41999998,-92.34995));
#135481=CARTESIAN_POINT('',(-21.,46.91999998,-91.84995));
#135482=CARTESIAN_POINT('Origin',(-21.,47.41999998,-91.84995));
#135483=CARTESIAN_POINT('Origin',(-21.,46.41999998,-91.84995));
#135484=CARTESIAN_POINT('Origin',(41.5,47.41999998,-91.84995));
#135485=CARTESIAN_POINT('',(-21.5,47.41999998,-92.34995));
#135486=CARTESIAN_POINT('',(41.5,47.41999998,-92.34995));
#135487=CARTESIAN_POINT('',(-21.5,46.91999998,-91.84995));
#135488=CARTESIAN_POINT('Origin',(-21.5,47.41999998,-91.84995));
#135489=CARTESIAN_POINT('',(39.,46.91999998,-91.84995));
#135490=CARTESIAN_POINT('Origin',(-21.5,46.41999998,-91.84995));
#135491=CARTESIAN_POINT('',(-22.5,46.41999998,-92.34995));
#135492=CARTESIAN_POINT('Origin',(-21.5,46.41999998,-92.34995));
#135493=CARTESIAN_POINT('',(-22.,46.41999998,-91.84995));
#135494=CARTESIAN_POINT('Origin',(-22.5,46.41999998,-91.84995));
#135495=CARTESIAN_POINT('Origin',(-21.5,46.41999998,-91.84995));
#135496=CARTESIAN_POINT('Origin',(-22.5,-9.33460238845303,-91.84995));
#135497=CARTESIAN_POINT('',(-22.5,29.41999998,-92.34995));
#135498=CARTESIAN_POINT('',(-22.5,29.41999998,-92.34995));
#135499=CARTESIAN_POINT('',(-22.,29.41999998,-91.84995));
#135500=CARTESIAN_POINT('Origin',(-22.5,29.41999998,-91.84995));
#135501=CARTESIAN_POINT('',(-22.,46.41999998,-91.84995));
#135502=CARTESIAN_POINT('Origin',(-60.,29.41999998,-91.34995));
#135503=CARTESIAN_POINT('',(-28.5,29.41999998,-92.34995));
#135504=CARTESIAN_POINT('',(-29.,29.41999998,-92.34995));
#135505=CARTESIAN_POINT('',(-28.5,28.41999998,-91.34995));
#135506=CARTESIAN_POINT('Origin',(-28.5,29.41999998,-91.34995));
#135507=CARTESIAN_POINT('',(-22.5,28.4199999800001,-91.34995));
#135508=CARTESIAN_POINT('',(-22.,28.4199999800001,-91.34995));
#135509=CARTESIAN_POINT('Origin',(-22.5,29.41999998,-91.34995));
#135510=CARTESIAN_POINT('Origin',(-28.5,58.91999998,-91.84995));
#135511=CARTESIAN_POINT('',(-29.,29.41999998,-91.84995));
#135512=CARTESIAN_POINT('Origin',(-28.5,29.41999998,-91.84995));
#135513=CARTESIAN_POINT('',(-28.5,46.41999998,-92.34995));
#135514=CARTESIAN_POINT('',(-28.5,46.41999998,-92.34995));
#135515=CARTESIAN_POINT('',(-29.,46.41999998,-91.84995));
#135516=CARTESIAN_POINT('Origin',(-28.5,46.41999998,-91.84995));
#135517=CARTESIAN_POINT('',(-29.,29.41999998,-91.84995));
#135518=CARTESIAN_POINT('Origin',(-29.5,46.41999998,-91.84995));
#135519=CARTESIAN_POINT('',(-29.5,47.41999998,-92.34995));
#135520=CARTESIAN_POINT('Origin',(-29.5,46.41999998,-92.34995));
#135521=CARTESIAN_POINT('',(-29.5,46.91999998,-91.84995));
#135522=CARTESIAN_POINT('Origin',(-29.5,47.41999998,-91.84995));
#135523=CARTESIAN_POINT('Origin',(-29.5,46.41999998,-91.84995));
#135524=CARTESIAN_POINT('Origin',(41.5,47.41999998,-91.84995));
#135525=CARTESIAN_POINT('',(-30.,47.41999998,-92.34995));
#135526=CARTESIAN_POINT('',(41.5,47.41999998,-92.34995));
#135527=CARTESIAN_POINT('',(-30.,46.91999998,-91.84995));
#135528=CARTESIAN_POINT('Origin',(-30.,47.41999998,-91.84995));
#135529=CARTESIAN_POINT('',(39.,46.91999998,-91.84995));
#135530=CARTESIAN_POINT('Origin',(-30.,46.41999998,-91.84995));
#135531=CARTESIAN_POINT('',(-31.,46.41999998,-92.34995));
#135532=CARTESIAN_POINT('Origin',(-30.,46.41999998,-92.34995));
#135533=CARTESIAN_POINT('',(-30.5,46.41999998,-91.84995));
#135534=CARTESIAN_POINT('Origin',(-31.,46.41999998,-91.84995));
#135535=CARTESIAN_POINT('Origin',(-30.,46.41999998,-91.84995));
#135536=CARTESIAN_POINT('Origin',(-31.,-9.33460238845303,-91.84995));
#135537=CARTESIAN_POINT('',(-31.,29.41999998,-92.34995));
#135538=CARTESIAN_POINT('',(-31.,29.41999998,-92.34995));
#135539=CARTESIAN_POINT('',(-30.5,29.41999998,-91.84995));
#135540=CARTESIAN_POINT('Origin',(-31.,29.41999998,-91.84995));
#135541=CARTESIAN_POINT('',(-30.5,46.41999998,-91.84995));
#135542=CARTESIAN_POINT('Origin',(-60.,29.41999998,-91.34995));
#135543=CARTESIAN_POINT('',(-37.,29.41999998,-92.34995));
#135544=CARTESIAN_POINT('',(-37.5,29.41999998,-92.34995));
#135545=CARTESIAN_POINT('',(-37.,28.41999998,-91.34995));
#135546=CARTESIAN_POINT('Origin',(-37.,29.41999998,-91.34995));
#135547=CARTESIAN_POINT('',(-31.,28.41999998,-91.34995));
#135548=CARTESIAN_POINT('',(-30.5,28.41999998,-91.34995));
#135549=CARTESIAN_POINT('Origin',(-31.,29.41999998,-91.34995));
#135550=CARTESIAN_POINT('Origin',(-37.,58.91999998,-91.84995));
#135551=CARTESIAN_POINT('',(-37.5,29.41999998,-91.84995));
#135552=CARTESIAN_POINT('Origin',(-37.,29.41999998,-91.84995));
#135553=CARTESIAN_POINT('',(-37.,46.41999998,-92.34995));
#135554=CARTESIAN_POINT('',(-37.5,29.41999998,-91.84995));
#135555=CARTESIAN_POINT('Origin',(-41.5,58.91999998,-92.34995));
#135556=CARTESIAN_POINT('',(-41.5,28.91999998,-171.14995));
#135557=CARTESIAN_POINT('',(-41.5,28.91999998,-171.64995));
#135558=CARTESIAN_POINT('',(-41.5,58.91999998,-174.34995));
#135559=CARTESIAN_POINT('',(-41.5,58.91999998,-92.34995));
#135560=CARTESIAN_POINT('',(-41.5,37.8417754273786,-174.34995));
#135561=CARTESIAN_POINT('',(-41.5,58.91999998,-174.34995));
#135562=CARTESIAN_POINT('',(-41.5,37.8417754273786,-172.64995));
#135563=CARTESIAN_POINT('',(-41.5,37.8417754273786,-92.34995));
#135564=CARTESIAN_POINT('',(-41.5,36.3270340686007,-171.14995));
#135565=CARTESIAN_POINT('Ctrl Pts',(-41.5,36.3270340686007,-171.14995));
#135566=CARTESIAN_POINT('Ctrl Pts',(-41.5,36.5253489879757,-171.149950000016));
#135567=CARTESIAN_POINT('Ctrl Pts',(-41.5,36.7235144279567,-171.18899099047));
#135568=CARTESIAN_POINT('Ctrl Pts',(-41.5,37.0898865538897,-171.339270411997));
#135569=CARTESIAN_POINT('Ctrl Pts',(-41.5,37.2579134125323,-171.450449746589));
#135570=CARTESIAN_POINT('Ctrl Pts',(-41.5,37.5383224977403,-171.728129909852));
#135571=CARTESIAN_POINT('Ctrl Pts',(-41.5,37.6505944553831,-171.894521542842));
#135572=CARTESIAN_POINT('Ctrl Pts',(-41.5,37.8023507586648,-172.257328160063));
#135573=CARTESIAN_POINT('Ctrl Pts',(-41.5,37.8417754273637,-172.453565067926));
#135574=CARTESIAN_POINT('Ctrl Pts',(-41.5,37.8417754273786,-172.64995));
#135575=CARTESIAN_POINT('',(-41.5,32.6685811839606,-171.14995));
#135576=CARTESIAN_POINT('',(-41.5,36.3973044859519,-171.14995));
#135577=CARTESIAN_POINT('',(-41.5,30.4123236926243,-171.14995));
#135578=CARTESIAN_POINT('Ctrl Pts',(-41.5,30.4123236926243,-171.14995));
#135579=CARTESIAN_POINT('Ctrl Pts',(-41.5,30.6002475127106,-171.149950044596));
#135580=CARTESIAN_POINT('Ctrl Pts',(-41.4999999999992,30.7880947817855,
-171.167358426712));
#135581=CARTESIAN_POINT('Ctrl Pts',(-41.5000000000009,30.9759786884911,
-171.183208448531));
#135582=CARTESIAN_POINT('Ctrl Pts',(-41.5000000000009,30.976120931185,-171.183220448228));
#135583=CARTESIAN_POINT('Ctrl Pts',(-41.5000000000009,30.9762631739402,
-171.183232446501));
#135584=CARTESIAN_POINT('Ctrl Pts',(-41.5000000000009,30.9764054167567,
-171.183244443348));
#135585=CARTESIAN_POINT('Ctrl Pts',(-41.5000000000023,31.1369344019092,
-171.196783556864));
#135586=CARTESIAN_POINT('Ctrl Pts',(-41.4999999999993,31.2974626498935,
-171.208492413821));
#135587=CARTESIAN_POINT('Ctrl Pts',(-41.500000000002,31.4579880082369,-171.211623701833));
#135588=CARTESIAN_POINT('Ctrl Pts',(-41.5000000000025,31.4852425169035,
-171.212155341925));
#135589=CARTESIAN_POINT('Ctrl Pts',(-41.5000000000032,31.5124969442739,
-171.212439843791));
#135590=CARTESIAN_POINT('Ctrl Pts',(-41.5000000000045,31.5397512823877,
-171.212444366369));
#135591=CARTESIAN_POINT('Ctrl Pts',(-41.5000000000045,31.5399934772056,
-171.212444406558));
#135592=CARTESIAN_POINT('Ctrl Pts',(-41.5000000000045,31.5402356720169,
-171.212444424596));
#135593=CARTESIAN_POINT('Ctrl Pts',(-41.5000000000045,31.5404778668211,
-171.212444420506));
#135594=CARTESIAN_POINT('Ctrl Pts',(-41.5000000000123,31.7017281895667,
-171.21244169735));
#135595=CARTESIAN_POINT('Ctrl Pts',(-41.5000000000007,31.8629751163933,
-171.202628065385));
#135596=CARTESIAN_POINT('Ctrl Pts',(-41.5000000000001,32.0242208996094,
-171.189830777503));
#135597=CARTESIAN_POINT('Ctrl Pts',(-41.5,32.0508620129899,-171.187716402848));
#135598=CARTESIAN_POINT('Ctrl Pts',(-41.5,32.0775031023629,-171.185520466759));
#135599=CARTESIAN_POINT('Ctrl Pts',(-41.5,32.1041441836616,-171.183273657173));
#135600=CARTESIAN_POINT('Ctrl Pts',(-41.5,32.1042728698424,-171.18326280426));
#135601=CARTESIAN_POINT('Ctrl Pts',(-41.5,32.1044015560177,-171.183251950612));
#135602=CARTESIAN_POINT('Ctrl Pts',(-41.5,32.1045302421874,-171.183241096235));
#135603=CARTESIAN_POINT('Ctrl Pts',(-41.5000000000001,32.2434923963757,
-171.171519963656));
#135604=CARTESIAN_POINT('Ctrl Pts',(-41.5,32.3824542184576,-171.158942972389));
#135605=CARTESIAN_POINT('Ctrl Pts',(-41.5,32.5214184450654,-171.153174108104));
#135606=CARTESIAN_POINT('Ctrl Pts',(-41.5,32.5704723625825,-171.151137717878));
#135607=CARTESIAN_POINT('Ctrl Pts',(-41.5,32.6195265765183,-171.149950012104));
#135608=CARTESIAN_POINT('Ctrl Pts',(-41.5,32.6685811839606,-171.14995));
#135609=CARTESIAN_POINT('',(-41.5,36.3973044859519,-171.14995));
#135610=CARTESIAN_POINT('Origin',(-38.5,58.91999998,-174.34995));
#135611=CARTESIAN_POINT('',(-38.5,58.91999998,-177.34995));
#135612=CARTESIAN_POINT('Origin',(-38.5,58.91999998,-174.34995));
#135613=CARTESIAN_POINT('',(-38.5,38.333668348837,-177.34995));
#135614=CARTESIAN_POINT('',(-38.5,58.91999998,-177.34995));
#135615=CARTESIAN_POINT('Ctrl Pts',(-41.5,37.8417754273786,-174.34995));
#135616=CARTESIAN_POINT('Ctrl Pts',(-41.5,37.8417754273818,-174.742719880575));
#135617=CARTESIAN_POINT('Ctrl Pts',(-41.4219180279654,37.8545780838243,
-175.135193658002));
#135618=CARTESIAN_POINT('Ctrl Pts',(-41.1213591671024,37.9038590092046,
-175.860806936189));
#135619=CARTESIAN_POINT('Ctrl Pts',(-40.8990005234543,37.9403178901501,
-176.193590163665));
#135620=CARTESIAN_POINT('Ctrl Pts',(-40.343640163665,38.0313771667621,-176.748950523454));
#135621=CARTESIAN_POINT('Ctrl Pts',(-40.0108569362568,38.0859417380754,
-176.971309167074));
#135622=CARTESIAN_POINT('Ctrl Pts',(-39.2852436579338,38.204916416519,-177.271868027993));
#135623=CARTESIAN_POINT('Ctrl Pts',(-38.8927698806272,38.2692681074913,
-177.34995));
#135624=CARTESIAN_POINT('Ctrl Pts',(-38.5,38.333668348837,-177.34995));
#135625=CARTESIAN_POINT('Origin',(-27.0372992073901,44.4888699625078,-177.84995));
#135626=CARTESIAN_POINT('',(-26.4110202530699,40.0326636531708,-177.34995));
#135627=CARTESIAN_POINT('',(-26.3414337025898,39.5375296188,-177.84995));
#135628=CARTESIAN_POINT('Origin',(-26.4110202530699,40.0326636531708,-177.84995));
#135629=CARTESIAN_POINT('',(-25.121270129701,40.4171587039029,-177.34995));
#135630=CARTESIAN_POINT('Origin',(-27.0372992073901,44.4888699625078,-177.34995));
#135631=CARTESIAN_POINT('',(-24.9083780099579,39.9647463418357,-177.84995));
#135632=CARTESIAN_POINT('Origin',(-25.121270129701,40.4171587039029,-177.84995));
#135633=CARTESIAN_POINT('Origin',(-27.0372992073901,44.4888699625078,-177.84995));
#135634=CARTESIAN_POINT('Origin',(-45.6308101826775,37.3314983336592,-177.84995));
#135635=CARTESIAN_POINT('',(-38.43041344952,37.8385343144662,-177.84995));
#135636=CARTESIAN_POINT('Origin',(-38.5,38.333668348837,-177.84995));
#135637=CARTESIAN_POINT('',(42.7876488459256,49.7579023686377,-177.34995));
#135638=CARTESIAN_POINT('',(-45.5612236321975,36.8363642992885,-177.84995));
#135639=CARTESIAN_POINT('Origin',(-27.0372992073901,44.4888699625078,-179.64995));
#135640=CARTESIAN_POINT('',(-24.9083780099579,39.9647463418357,-179.39995));
#135641=CARTESIAN_POINT('',(-24.9083780099579,39.9647463418357,-179.64995));
#135642=CARTESIAN_POINT('',(-26.3414337025898,39.5375296188,-179.39995));
#135643=CARTESIAN_POINT('Origin',(-27.0372992073901,44.4888699625078,-179.39995));
#135644=CARTESIAN_POINT('',(-26.3414337025898,39.5375296188,-171.64995));
#135645=CARTESIAN_POINT('Origin',(-27.0372992073901,44.4888699625078,-179.39995));
#135646=CARTESIAN_POINT('',(-26.3066404273498,39.2899626016146,-179.64995));
#135647=CARTESIAN_POINT('Origin',(-26.3066404273498,39.2899626016146,-179.39995));
#135648=CARTESIAN_POINT('',(-24.8019319500862,39.7385401608021,-179.64995));
#135649=CARTESIAN_POINT('Origin',(-24.8019319500862,39.7385401608021,-179.39995));
#135650=CARTESIAN_POINT('Origin',(-27.0372992073901,44.4888699625078,-179.64995));
#135651=CARTESIAN_POINT('Origin',(-62.8299850317005,34.1569412647963,-179.39995));
#135652=CARTESIAN_POINT('',(-44.628608857647,36.9674347581595,-179.39995));
#135653=CARTESIAN_POINT('',(-44.593815582407,36.7198677409741,-179.64995));
#135654=CARTESIAN_POINT('Origin',(-44.593815582407,36.7198677409741,-179.39995));
#135655=CARTESIAN_POINT('',(-26.3414337025898,39.5375296188,-179.39995));
#135656=CARTESIAN_POINT('',(-44.593815582407,36.7198677409741,-179.64995));
#135657=CARTESIAN_POINT('Origin',(-44.2110895547669,33.9966305519348,-179.39995));
#135658=CARTESIAN_POINT('',(-46.2674193015002,36.1810087180727,-179.39995));
#135659=CARTESIAN_POINT('',(-46.0960584892724,35.9989772042278,-179.64995));
#135660=CARTESIAN_POINT('Origin',(-46.0960584892724,35.9989772042278,-179.39995));
#135661=CARTESIAN_POINT('Origin',(-44.2110895547669,33.9966305519348,-179.39995));
#135662=CARTESIAN_POINT('Origin',(-44.2110895547669,33.9966305519348,-179.64995));
#135663=CARTESIAN_POINT('Origin',(0.,-12.9675000200281,-179.39995));
#135664=CARTESIAN_POINT('',(-49.1485087381009,33.2999192814719,-179.39995));
#135665=CARTESIAN_POINT('',(-48.9664772242561,33.1285584692441,-179.64995));
#135666=CARTESIAN_POINT('Origin',(-48.9664772242561,33.1285584692441,-179.39995));
#135667=CARTESIAN_POINT('Origin',(0.,-12.9675000200281,-179.39995));
#135668=CARTESIAN_POINT('Origin',(0.,-12.9675000200281,-179.64995));
#135669=CARTESIAN_POINT('Origin',(-46.9641305719631,31.2435895347386,-179.39995));
#135670=CARTESIAN_POINT('',(-49.9349347781878,31.6611088376188,-179.39995));
#135671=CARTESIAN_POINT('',(-49.6873677610025,31.6263155623787,-179.64995));
#135672=CARTESIAN_POINT('Origin',(-49.6873677610024,31.6263155623787,-179.39995));
#135673=CARTESIAN_POINT('Origin',(-46.9641305719631,31.2435895347386,-179.39995));
#135674=CARTESIAN_POINT('Origin',(-46.9641305719631,31.2435895347386,-179.64995));
#135675=CARTESIAN_POINT('Origin',(-61.3785689046687,-51.5609030735669,-179.39995));
#135676=CARTESIAN_POINT('',(-52.5050296388285,13.3739336825608,-179.39995));
#135677=CARTESIAN_POINT('',(-52.2574626216432,13.3391404073208,-179.64995));
#135678=CARTESIAN_POINT('Origin',(-52.2574626216431,13.3391404073208,-179.39995));
#135679=CARTESIAN_POINT('',(-49.9349347781878,31.6611088376188,-179.39995));
#135680=CARTESIAN_POINT('',(-52.2574626216432,13.3391404073208,-179.64995));
#135681=CARTESIAN_POINT('Origin',(-57.4563699825364,14.0697991873612,-179.39995));
#135682=CARTESIAN_POINT('',(-52.9322463618642,11.9408779899289,-179.39995));
#135683=CARTESIAN_POINT('',(-52.7060401808306,11.8344319300573,-179.64995));
#135684=CARTESIAN_POINT('Origin',(-52.7060401808306,11.8344319300573,-179.39995));
#135685=CARTESIAN_POINT('Origin',(-57.4563699825364,14.0697991873612,-179.39995));
#135686=CARTESIAN_POINT('Origin',(-57.4563699825364,14.0697991873612,-179.64995));
#135687=CARTESIAN_POINT('Origin',(0.,-12.9675000200281,-179.39995));
#135688=CARTESIAN_POINT('',(-52.9322463618642,-37.8758780299853,-179.39995));
#135689=CARTESIAN_POINT('',(-52.7060401808306,-37.7694319701137,-179.64995));
#135690=CARTESIAN_POINT('Origin',(-52.7060401808306,-37.7694319701137,-179.39995));
#135691=CARTESIAN_POINT('Origin',(0.,-12.9675000200281,-179.39995));
#135692=CARTESIAN_POINT('Origin',(0.,-12.9675000200281,-179.64995));
#135693=CARTESIAN_POINT('Origin',(-57.4563699825363,-40.0047992274175,-179.39995));
#135694=CARTESIAN_POINT('',(-52.5050296388285,-39.3089337226171,-179.39995));
#135695=CARTESIAN_POINT('',(-52.2574626216431,-39.2741404473771,-179.64995));
#135696=CARTESIAN_POINT('Origin',(-52.2574626216431,-39.2741404473771,-179.39995));
#135697=CARTESIAN_POINT('Origin',(-57.4563699825363,-40.0047992274175,-179.39995));
#135698=CARTESIAN_POINT('Origin',(-57.4563699825363,-40.0047992274175,-179.64995));
#135699=CARTESIAN_POINT('Origin',(-50.3220654694669,-53.04520674476,-179.39995));
#135700=CARTESIAN_POINT('',(-49.9349347781878,-57.596108877675,-179.39995));
#135701=CARTESIAN_POINT('',(-49.6873677610024,-57.561315602435,-179.64995));
#135702=CARTESIAN_POINT('Origin',(-49.6873677610024,-57.561315602435,-179.39995));
#135703=CARTESIAN_POINT('',(-52.5050296388285,-39.3089337226171,-179.39995));
#135704=CARTESIAN_POINT('',(-49.6873677610024,-57.561315602435,-179.64995));
#135705=CARTESIAN_POINT('Origin',(-46.9641305719631,-57.1785895747948,-179.39995));
#135706=CARTESIAN_POINT('',(-49.148508738101,-59.2349193215281,-179.39995));
#135707=CARTESIAN_POINT('',(-48.9664772242561,-59.0635585093003,-179.64995));
#135708=CARTESIAN_POINT('Origin',(-48.9664772242561,-59.0635585093003,-179.39995));
#135709=CARTESIAN_POINT('Origin',(-46.9641305719631,-57.1785895747948,-179.39995));
#135710=CARTESIAN_POINT('Origin',(-46.9641305719631,-57.1785895747948,-179.64995));
#135711=CARTESIAN_POINT('Origin',(0.,-12.9675000200281,-179.39995));
#135712=CARTESIAN_POINT('',(-46.2674193015002,-62.1160087581289,-179.39995));
#135713=CARTESIAN_POINT('',(-46.0960584892725,-61.9339772442841,-179.64995));
#135714=CARTESIAN_POINT('Origin',(-46.0960584892725,-61.9339772442841,-179.39995));
#135715=CARTESIAN_POINT('Origin',(0.,-12.9675000200281,-179.39995));
#135716=CARTESIAN_POINT('Origin',(0.,-12.9675000200281,-179.64995));
#135717=CARTESIAN_POINT('Origin',(-44.2110895547669,-59.9316305919911,-179.39995));
#135718=CARTESIAN_POINT('',(-44.628608857647,-62.9024347982158,-179.39995));
#135719=CARTESIAN_POINT('',(-44.5938155824071,-62.6548677810304,-179.64995));
#135720=CARTESIAN_POINT('Origin',(-44.5938155824071,-62.6548677810303,-179.39995));
#135721=CARTESIAN_POINT('Origin',(-44.2110895547669,-59.9316305919911,-179.39995));
#135722=CARTESIAN_POINT('Origin',(-44.2110895547669,-59.9316305919911,-179.64995));
#135723=CARTESIAN_POINT('Origin',(-51.7734815964994,-61.6458315265255,-179.39995));
#135724=CARTESIAN_POINT('',(-26.0394480946395,-65.5149709682656,-179.39995));
#135725=CARTESIAN_POINT('',(-26.0046548193995,-65.2674039510802,-179.64995));
#135726=CARTESIAN_POINT('Origin',(-26.0046548193995,-65.2674039510803,-179.39995));
#135727=CARTESIAN_POINT('',(-44.628608857647,-62.9024347982158,-179.39995));
#135728=CARTESIAN_POINT('',(-26.0046548193995,-65.2674039510802,-179.64995));
#135729=CARTESIAN_POINT('Origin',(-26.4569673975197,-68.4857751744904,-179.39995));
#135730=CARTESIAN_POINT('',(-25.166383622031,-65.7775666303703,-179.39995));
#135731=CARTESIAN_POINT('',(-25.0588349740736,-65.5518825850269,-179.64995));
#135732=CARTESIAN_POINT('Origin',(-25.0588349740736,-65.5518825850269,-179.39995));
#135733=CARTESIAN_POINT('Origin',(-26.4569673975197,-68.4857751744904,-179.39995));
#135734=CARTESIAN_POINT('Origin',(-26.4569673975197,-68.4857751744904,-179.64995));
#135735=CARTESIAN_POINT('Origin',(-44.5079524583208,-57.4754524783487,-171.64995));
#135736=CARTESIAN_POINT('',(-43.1572831724514,-55.08000002,-171.64995));
#135737=CARTESIAN_POINT('',(-45.8586217441902,-55.08000002,-171.64995));
#135738=CARTESIAN_POINT('Ctrl Pts',(-45.8586217441902,-55.08000002,-171.64995));
#135739=CARTESIAN_POINT('Ctrl Pts',(-45.7689536596569,-55.0294409169463,
-171.64995));
#135740=CARTESIAN_POINT('Ctrl Pts',(-45.6765174633176,-54.9839564622376,
-171.649937574984));
#135741=CARTESIAN_POINT('Ctrl Pts',(-45.4778485953858,-54.8996925932595,
-171.64992638429));
#135742=CARTESIAN_POINT('Ctrl Pts',(-45.371333860312,-54.8620619965585,
-171.649947040217));
#135743=CARTESIAN_POINT('Ctrl Pts',(-45.1857602021761,-54.8090884744686,
-171.649951805482));
#135744=CARTESIAN_POINT('Ctrl Pts',(-45.1077985401449,-54.7904750984752,
-171.649838856786));
#135745=CARTESIAN_POINT('Ctrl Pts',(-44.9203791059924,-54.7542997329157,
-171.649614268465));
#135746=CARTESIAN_POINT('Ctrl Pts',(-44.8104650288131,-54.73989862651,-171.649606832116));
#135747=CARTESIAN_POINT('Ctrl Pts',(-44.6361116415896,-54.7276946232682,
-171.649829887348));
#135748=CARTESIAN_POINT('Ctrl Pts',(-44.572121425011,-54.7254562445457,
-171.649942496644));
#135749=CARTESIAN_POINT('Ctrl Pts',(-44.4919713617221,-54.7254515344574,
-171.649951467562));
#135750=CARTESIAN_POINT('Ctrl Pts',(-44.4758287519422,-54.7255927281285,
-171.649946189807));
#135751=CARTESIAN_POINT('Ctrl Pts',(-44.3973353016952,-54.7269705335247,
-171.649899299462));
#135752=CARTESIAN_POINT('Ctrl Pts',(-44.3350361171979,-54.7301856687744,
-171.649800793763));
#135753=CARTESIAN_POINT('Ctrl Pts',(-44.24589448532,-54.7378330706293,-171.64971310718));
#135754=CARTESIAN_POINT('Ctrl Pts',(-44.2189296557681,-54.7405484163111,
-171.649692645932));
#135755=CARTESIAN_POINT('Ctrl Pts',(-44.1669378685671,-54.7465614902616,
-171.649670825756));
#135756=CARTESIAN_POINT('Ctrl Pts',(-44.141907947472,-54.7498060612266,
-171.649668207626));
#135757=CARTESIAN_POINT('Ctrl Pts',(-44.0251905251421,-54.7665726407083,
-171.649692857457));
#135758=CARTESIAN_POINT('Ctrl Pts',(-43.9341908339778,-54.7843774385806,
-171.64983557602));
#135759=CARTESIAN_POINT('Ctrl Pts',(-43.7178584587823,-54.8381778103583,
-171.650016020842));
#135760=CARTESIAN_POINT('Ctrl Pts',(-43.5938526567541,-54.8785531161362,
-171.649916571135));
#135761=CARTESIAN_POINT('Ctrl Pts',(-43.3647423777249,-54.9716018333704,
-171.649923778305));
#135762=CARTESIAN_POINT('Ctrl Pts',(-43.2592299860174,-55.0225175893235,
-171.64995));
#135763=CARTESIAN_POINT('Ctrl Pts',(-43.1572831724514,-55.08000002,-171.64995));
#135764=CARTESIAN_POINT('',(-44.5079524583208,-60.2254524783487,-171.64995));
#135765=CARTESIAN_POINT('Origin',(-44.5079524583208,-57.4754524783487,-171.64995));
#135766=CARTESIAN_POINT('',(-44.5079524583208,-60.2254524783487,-179.64995));
#135767=CARTESIAN_POINT('',(-44.5079524583208,-60.2254524783487,-171.64995));
#135768=CARTESIAN_POINT('Origin',(-44.5079524583208,-57.4754524783487,-179.64995));
#135769=CARTESIAN_POINT('',(-42.,-58.6035812240168,-171.64995));
#135770=CARTESIAN_POINT('Origin',(-44.5079524583208,-57.4754524783487,-171.64995));
#135771=CARTESIAN_POINT('',(-42.,-56.3473237326807,-171.64995));
#135772=CARTESIAN_POINT('Ctrl Pts',(-42.,-58.6035812240168,-171.64995));
#135773=CARTESIAN_POINT('Ctrl Pts',(-41.9586127577212,-58.5115728992446,
-171.64995));
#135774=CARTESIAN_POINT('Ctrl Pts',(-41.9223200866005,-58.4173567491321,
-171.649936040447));
#135775=CARTESIAN_POINT('Ctrl Pts',(-41.8579031946499,-58.2180944893019,
-171.649932806722));
#135776=CARTESIAN_POINT('Ctrl Pts',(-41.8306620008006,-58.1129431414185,
-171.649968769067));
#135777=CARTESIAN_POINT('Ctrl Pts',(-41.7951274186659,-57.9323775711287,
-171.649917110529));
#135778=CARTESIAN_POINT('Ctrl Pts',(-41.7836058362705,-57.8577298063974,
-171.649879920008));
#135779=CARTESIAN_POINT('Ctrl Pts',(-41.7636999883713,-57.6806798505216,
-171.649872834512));
#135780=CARTESIAN_POINT('Ctrl Pts',(-41.7579524619681,-57.5781054625683,
-171.649950538122));
#135781=CARTESIAN_POINT('Ctrl Pts',(-41.7579524619681,-57.3728595819388,
-171.649949462193));
#135782=CARTESIAN_POINT('Ctrl Pts',(-41.7636932451378,-57.2703453579385,
-171.649869923244));
#135783=CARTESIAN_POINT('Ctrl Pts',(-41.7835828980498,-57.09333489844,-171.649877908044));
#135784=CARTESIAN_POINT('Ctrl Pts',(-41.7951032511141,-57.0186677636544,
-171.649916441382));
#135785=CARTESIAN_POINT('Ctrl Pts',(-41.8306429216695,-56.8380335332052,
-171.649969369358));
#135786=CARTESIAN_POINT('Ctrl Pts',(-41.857894634129,-56.7328337987611,
-171.64993233013));
#135787=CARTESIAN_POINT('Ctrl Pts',(-41.9223259722371,-56.5335329279264,
-171.649935735269));
#135788=CARTESIAN_POINT('Ctrl Pts',(-41.9586161144824,-56.4393245950087,
-171.64995));
#135789=CARTESIAN_POINT('Ctrl Pts',(-42.,-56.3473237326807,-171.64995));
#135790=CARTESIAN_POINT('Origin',(-44.5079524583208,-57.4754524783487,-171.64995));
#135791=CARTESIAN_POINT('Origin',(-44.5079524583208,31.5404524382925,-171.64995));
#135792=CARTESIAN_POINT('',(-42.,32.6685811839606,-171.64995));
#135793=CARTESIAN_POINT('',(-45.342056117244,28.91999998,-171.64995));
#135794=CARTESIAN_POINT('Origin',(-44.5079524583208,31.5404524382925,-171.64995));
#135795=CARTESIAN_POINT('',(-44.507948362235,28.7904524382955,-171.649949999922));
#135796=CARTESIAN_POINT('Ctrl Pts',(-45.342056117244,28.91999998,-171.64995));
#135797=CARTESIAN_POINT('Ctrl Pts',(-45.2444197705179,28.8889218225657,
-171.64995));
#135798=CARTESIAN_POINT('Ctrl Pts',(-45.145122736077,28.8633247324813,-171.649944548176));
#135799=CARTESIAN_POINT('Ctrl Pts',(-44.9394245210704,28.8223946394273,
-171.649950242553));
#135800=CARTESIAN_POINT('Ctrl Pts',(-44.8330844822692,28.8076342035681,
-171.649941034682));
#135801=CARTESIAN_POINT('Ctrl Pts',(-44.6535626787428,28.7933447394312,
-171.649939912182));
#135802=CARTESIAN_POINT('Ctrl Pts',(-44.5807739260493,28.7904524382925,
-171.649950037878));
#135803=CARTESIAN_POINT('Ctrl Pts',(-44.5079524583208,28.7904524382925,
-171.649949999924));
#135804=CARTESIAN_POINT('',(-44.5079524583208,28.7904524382925,-179.64995));
#135805=CARTESIAN_POINT('',(-44.5079524583208,28.7904524382925,-171.64995));
#135806=CARTESIAN_POINT('Origin',(-44.5079524583208,31.5404524382925,-179.64995));
#135807=CARTESIAN_POINT('',(-43.6738487993976,28.91999998,-171.64995));
#135808=CARTESIAN_POINT('Ctrl Pts',(-44.507948362235,28.7904524382955,-171.649949999922));
#135809=CARTESIAN_POINT('Ctrl Pts',(-44.4351555237766,28.7904525467194,
-171.64994996145));
#135810=CARTESIAN_POINT('Ctrl Pts',(-44.3623912990527,28.7933428984961,
-171.649939477139));
#135811=CARTESIAN_POINT('Ctrl Pts',(-44.1829187602443,28.8076233386202,
-171.649940713495));
#135812=CARTESIAN_POINT('Ctrl Pts',(-44.0765991739455,28.8223766210747,
-171.649950205311));
#135813=CARTESIAN_POINT('Ctrl Pts',(-43.8708734141959,28.8633012176256,
-171.649945186597));
#135814=CARTESIAN_POINT('Ctrl Pts',(-43.7715300191675,28.8889075392422,
-171.64995));
#135815=CARTESIAN_POINT('Ctrl Pts',(-43.6738487993977,28.91999998,-171.64995));
#135816=CARTESIAN_POINT('',(-42.,30.4123236926243,-171.64995));
#135817=CARTESIAN_POINT('Origin',(-44.5079524583208,31.5404524382925,-171.64995));
#135818=CARTESIAN_POINT('Ctrl Pts',(-42.,30.4123236926244,-171.64995));
#135819=CARTESIAN_POINT('Ctrl Pts',(-41.9586127577212,30.5043320173966,
-171.64995));
#135820=CARTESIAN_POINT('Ctrl Pts',(-41.9223200866006,30.5985481675089,
-171.649936040447));
#135821=CARTESIAN_POINT('Ctrl Pts',(-41.85790319465,30.7978104273388,-171.649932806722));
#135822=CARTESIAN_POINT('Ctrl Pts',(-41.8306620008007,30.902961775222,-171.649968769066));
#135823=CARTESIAN_POINT('Ctrl Pts',(-41.7951274186661,31.0835273455116,
-171.649917110529));
#135824=CARTESIAN_POINT('Ctrl Pts',(-41.7836058362707,31.1581751102429,
-171.649879920008));
#135825=CARTESIAN_POINT('Ctrl Pts',(-41.7636999883716,31.3352250661166,
-171.649872834512));
#135826=CARTESIAN_POINT('Ctrl Pts',(-41.7579524619681,31.4377994540703,
-171.649950538122));
#135827=CARTESIAN_POINT('Ctrl Pts',(-41.7579524619681,31.6430453346998,
-171.649949462193));
#135828=CARTESIAN_POINT('Ctrl Pts',(-41.7636932451375,31.7455595586996,
-171.649869923244));
#135829=CARTESIAN_POINT('Ctrl Pts',(-41.7835828980496,31.9225700182004,
-171.649877908044));
#135830=CARTESIAN_POINT('Ctrl Pts',(-41.795103251114,31.9972371529859,-171.649916441382));
#135831=CARTESIAN_POINT('Ctrl Pts',(-41.8306429216694,32.1778713834354,
-171.649969369358));
#135832=CARTESIAN_POINT('Ctrl Pts',(-41.8578946341289,32.2830711178797,
-171.64993233013));
#135833=CARTESIAN_POINT('Ctrl Pts',(-41.922325972237,32.4823719887145,-171.649935735269));
#135834=CARTESIAN_POINT('Ctrl Pts',(-41.9586161144823,32.5765803216321,
-171.64995));
#135835=CARTESIAN_POINT('Ctrl Pts',(-42.,32.6685811839606,-171.64995));
#135836=CARTESIAN_POINT('Ctrl Pts',(-24.2000000000011,-66.7760495265879,
-177.34995));
#135837=CARTESIAN_POINT('Ctrl Pts',(-23.9949152542386,-66.320044869753,
-177.34995));
#135838=CARTESIAN_POINT('Ctrl Pts',(-23.9949152542395,-66.3200448697526,
-177.84995));
#135839=CARTESIAN_POINT('Ctrl Pts',(-24.1371859654851,-66.8325498277328,
-177.34995));
#135840=CARTESIAN_POINT('Ctrl Pts',(-23.9206657457682,-66.3534380400361,
-177.323497139763));
#135841=CARTESIAN_POINT('Ctrl Pts',(-23.8703538324233,-66.3760654545035,
-177.849949984965));
#135842=CARTESIAN_POINT('Ctrl Pts',(-24.0753687900163,-66.8876168115863,
-177.338353763422));
#135843=CARTESIAN_POINT('Ctrl Pts',(-23.85857311611,-66.3812761568117,-177.28202856183));
#135844=CARTESIAN_POINT('Ctrl Pts',(-23.7477652296632,-66.4306666697135,
-177.82675752222));
#135845=CARTESIAN_POINT('Ctrl Pts',(-23.9567084144264,-66.9924080535444,
-177.291402578445));
#135846=CARTESIAN_POINT('Ctrl Pts',(-23.7605684693856,-66.4255018631538,
-177.182659406882));
#135847=CARTESIAN_POINT('Ctrl Pts',(-23.5124556672824,-66.534569849442,
-177.732855161513));
#135848=CARTESIAN_POINT('Ctrl Pts',(-23.9022748831747,-67.0400066306863,
-177.256984676403));
#135849=CARTESIAN_POINT('Ctrl Pts',(-23.728650188117,-66.4401283754592,
-177.126465197113));
#135850=CARTESIAN_POINT('Ctrl Pts',(-23.4045112120254,-66.5817650498296,
-177.66401934989));
#135851=CARTESIAN_POINT('Ctrl Pts',(-23.8072189577995,-67.1225998569154,
-177.166241836555));
#135852=CARTESIAN_POINT('Ctrl Pts',(-23.6923095199098,-66.4575908379652,
-177.01948600884));
#135853=CARTESIAN_POINT('Ctrl Pts',(-23.2160104726183,-66.6636583322845,
-177.482533676026));
#135854=CARTESIAN_POINT('Ctrl Pts',(-23.7683864506384,-67.1560455904002,
-177.111255395708));
#135855=CARTESIAN_POINT('Ctrl Pts',(-23.6901782519314,-66.4593985440301,
-176.972463316884));
#135856=CARTESIAN_POINT('Ctrl Pts',(-23.1390036429345,-66.6968206283899,
-177.372560789955));
#135857=CARTESIAN_POINT('Ctrl Pts',(-23.7144895325829,-67.2023409665867,
-176.987246583524));
#135858=CARTESIAN_POINT('Ctrl Pts',(-23.6945043498585,-66.4589699067553,
-176.898771091495));
#135859=CARTESIAN_POINT('Ctrl Pts',(-23.0321233068433,-66.742723669979,
-177.12454316851));
#135860=CARTESIAN_POINT('Ctrl Pts',(-23.7,-67.2147119253083,-176.919839157335));
#135861=CARTESIAN_POINT('Ctrl Pts',(-23.6999999982817,-66.4570693060762,
-176.874118380146));
#135862=CARTESIAN_POINT('Ctrl Pts',(-23.0033898412675,-66.7549897905191,
-176.989728313577));
#135863=CARTESIAN_POINT('Ctrl Pts',(-23.7,-67.2147119299503,-176.84995));
#135864=CARTESIAN_POINT('Ctrl Pts',(-23.6999999999999,-66.45706930551,-176.84995));
#135865=CARTESIAN_POINT('Ctrl Pts',(-23.0033898305084,-66.7549897951205,
-176.84995));
#135866=CARTESIAN_POINT('',(-23.0033898305085,-66.7549897951205,-176.84995));
#135867=CARTESIAN_POINT('',(-23.7,-67.2147119299503,-176.84995));
#135868=CARTESIAN_POINT('Origin',(-23.2,-67.2147119299503,-176.84995));
#135869=CARTESIAN_POINT('',(-24.2,-66.7760495265873,-177.34995));
#135870=CARTESIAN_POINT('Ctrl Pts',(-23.7,-67.2147119299503,-176.84995));
#135871=CARTESIAN_POINT('Ctrl Pts',(-23.7,-67.2147119253083,-176.919839157335));
#135872=CARTESIAN_POINT('Ctrl Pts',(-23.7144895325829,-67.2023409665867,
-176.987246583524));
#135873=CARTESIAN_POINT('Ctrl Pts',(-23.7683864506384,-67.1560455904002,
-177.111255395708));
#135874=CARTESIAN_POINT('Ctrl Pts',(-23.8072189577995,-67.1225998569154,
-177.166241836555));
#135875=CARTESIAN_POINT('Ctrl Pts',(-23.9022748831747,-67.0400066306863,
-177.256984676403));
#135876=CARTESIAN_POINT('Ctrl Pts',(-23.9567084144264,-66.9924080535444,
-177.291402578445));
#135877=CARTESIAN_POINT('Ctrl Pts',(-24.0753687900163,-66.8876168115863,
-177.338353763422));
#135878=CARTESIAN_POINT('Ctrl Pts',(-24.1371859654851,-66.8325498277328,
-177.34995));
#135879=CARTESIAN_POINT('Ctrl Pts',(-24.2,-66.7760495265873,-177.34995));
#135880=CARTESIAN_POINT('',(-23.9949152542395,-66.3200448697526,-177.84995));
#135881=CARTESIAN_POINT('Origin',(-24.200000000006,-66.7760495265862,-177.84995));
#135882=CARTESIAN_POINT('Ctrl Pts',(-23.9949152542395,-66.3200448697526,
-177.84995));
#135883=CARTESIAN_POINT('Ctrl Pts',(-23.9428551887952,-66.3434585018855,
-177.849949993716));
#135884=CARTESIAN_POINT('Ctrl Pts',(-23.8912891629459,-66.3665571088585,
-177.845903065055));
#135885=CARTESIAN_POINT('Ctrl Pts',(-23.8403424606444,-66.3892926538626,
-177.83781160242));
#135886=CARTESIAN_POINT('Ctrl Pts',(-23.7898936124076,-66.4118060258313,
-177.829799210017));
#135887=CARTESIAN_POINT('Ctrl Pts',(-23.7400516011853,-66.4339635775754,
-177.817820923568));
#135888=CARTESIAN_POINT('Ctrl Pts',(-23.6909420374961,-66.4557157061562,
-177.80182839125));
#135889=CARTESIAN_POINT('Ctrl Pts',(-23.6705352998627,-66.4647544747293,
-177.795182935934));
#135890=CARTESIAN_POINT('Ctrl Pts',(-23.6502551185152,-66.4737231883063,
-177.787843738039));
#135891=CARTESIAN_POINT('Ctrl Pts',(-23.6301109846052,-66.4826180228466,
-177.779804722709));
#135892=CARTESIAN_POINT('Ctrl Pts',(-23.6296825902114,-66.4828071844789,
-177.779633761321));
#135893=CARTESIAN_POINT('Ctrl Pts',(-23.6292543206867,-66.4829962847601,
-177.77946250822));
#135894=CARTESIAN_POINT('Ctrl Pts',(-23.6288261761769,-66.4831853236383,
-177.779290963367));
#135895=CARTESIAN_POINT('Ctrl Pts',(-23.5490836050341,-66.5183941044508,
-177.747340471671));
#135896=CARTESIAN_POINT('Ctrl Pts',(-23.4738664381495,-66.551389542848,
-177.705344056616));
#135897=CARTESIAN_POINT('Ctrl Pts',(-23.4044230513275,-66.5817044398146,
-177.653364341176));
#135898=CARTESIAN_POINT('Ctrl Pts',(-23.3717123604324,-66.5959840029173,
-177.628879757656));
#135899=CARTESIAN_POINT('Ctrl Pts',(-23.3402823397949,-66.6096689890227,
-177.60218062654));
#135900=CARTESIAN_POINT('Ctrl Pts',(-23.3102608826734,-66.6227116735265,
-177.57327646271));
#135901=CARTESIAN_POINT('Ctrl Pts',(-23.3097552045839,-66.6229313630558,
-177.572789604185));
#135902=CARTESIAN_POINT('Ctrl Pts',(-23.3092500282568,-66.6231508261632,
-177.572302197161));
#135903=CARTESIAN_POINT('Ctrl Pts',(-23.3087453546535,-66.6233700624813,
-177.571814242488));
#135904=CARTESIAN_POINT('Ctrl Pts',(-23.2428791470164,-66.6519831398301,
-177.508130064148));
#135905=CARTESIAN_POINT('Ctrl Pts',(-23.1855484931334,-66.6767452815916,
-177.435089847605));
#135906=CARTESIAN_POINT('Ctrl Pts',(-23.1388722340375,-66.6968462861646,
-177.354542469169));
#135907=CARTESIAN_POINT('Ctrl Pts',(-23.1191486795941,-66.7053401814712,
-177.320506309575));
#135908=CARTESIAN_POINT('Ctrl Pts',(-23.1013269939373,-66.7130020216597,
-177.285129627946));
#135909=CARTESIAN_POINT('Ctrl Pts',(-23.0855644128598,-66.7197717463454,
-177.248551496375));
#135910=CARTESIAN_POINT('Ctrl Pts',(-23.0853517691174,-66.7198630727333,
-177.248058042242));
#135911=CARTESIAN_POINT('Ctrl Pts',(-23.0851395181392,-66.7199542292592,
-177.24756442059));
#135912=CARTESIAN_POINT('Ctrl Pts',(-23.0849276601638,-66.7200452158304,
-177.247070631801));
#135913=CARTESIAN_POINT('Ctrl Pts',(-23.0685067964826,-66.7270974784524,
-177.208797640755));
#135914=CARTESIAN_POINT('Ctrl Pts',(-23.0544044796131,-66.7331469401741,
-177.169412579499));
#135915=CARTESIAN_POINT('Ctrl Pts',(-23.04278734195,-66.738126397354,-177.129172865924));
#135916=CARTESIAN_POINT('Ctrl Pts',(-23.0313107069198,-66.7430456308484,
-177.089419828659));
#135917=CARTESIAN_POINT('Ctrl Pts',(-23.0222597634207,-66.7469204858851,
-177.048833228894));
#135918=CARTESIAN_POINT('Ctrl Pts',(-23.0157509005018,-66.7497052241092,
-177.007676413083));
#135919=CARTESIAN_POINT('Ctrl Pts',(-23.0093646056921,-66.7524375230512,
-176.967294619447));
#135920=CARTESIAN_POINT('Ctrl Pts',(-23.0054256948344,-66.7541203250939,
-176.926364378223));
#135921=CARTESIAN_POINT('Ctrl Pts',(-23.0039983429947,-66.7547299427615,
-176.885141466357));
#135922=CARTESIAN_POINT('Ctrl Pts',(-23.0035929213886,-66.7549030971072,
-176.873432608966));
#135923=CARTESIAN_POINT('Ctrl Pts',(-23.0033898314129,-66.7549897947337,
-176.861700158873));
#135924=CARTESIAN_POINT('Ctrl Pts',(-23.0033898305084,-66.7549897951205,
-176.84995));
#135925=CARTESIAN_POINT('Origin',(-23.2,-67.2147119299503,-179.64995));
#135926=CARTESIAN_POINT('',(-23.0033898305084,-66.7549897951204,-171.871644662643));
#135927=CARTESIAN_POINT('',(-23.0033898305085,-66.7549897951205,-179.64995));
#135928=CARTESIAN_POINT('',(-23.7,-67.2147119299503,-171.871644662643));
#135929=CARTESIAN_POINT('Origin',(-23.2,-67.2147119299503,-171.871644662643));
#135930=CARTESIAN_POINT('',(-23.7,-67.2147119299503,-176.84995));
#135931=CARTESIAN_POINT('Origin',(0.,-12.9675000200281,-171.871644662643));
#135932=CARTESIAN_POINT('',(-17.4012711864406,-68.8194987407181,-171.871644662643));
#135933=CARTESIAN_POINT('Origin',(0.,-12.9675000200281,-171.871644662643));
#135934=CARTESIAN_POINT('',(-17.4148840712406,-68.7171063154928,-171.449026400902));
#135935=CARTESIAN_POINT('Origin',(-17.5530339837215,-67.6883802890115,-171.880603003797));
#135936=CARTESIAN_POINT('',(-23.0213852109847,-66.6453596297547,-171.449026400902));
#135937=CARTESIAN_POINT('Origin',(0.,-12.9675000200281,-171.449026400902));
#135938=CARTESIAN_POINT('Origin',(-23.2064336390783,-65.5202502275577,-171.885329893835));
#135939=CARTESIAN_POINT('Origin',(-17.55,-69.2968662511513,-179.64995));
#135940=CARTESIAN_POINT('',(-17.05,-69.2968662511513,-176.84995));
#135941=CARTESIAN_POINT('',(-17.4012711864406,-68.8194987407181,-176.84995));
#135942=CARTESIAN_POINT('Origin',(-17.55,-69.2968662511513,-176.84995));
#135943=CARTESIAN_POINT('',(-17.05,-69.2968662511513,-171.871644662643));
#135944=CARTESIAN_POINT('',(-17.05,-69.2968662511513,-171.871644662643));
#135945=CARTESIAN_POINT('Origin',(-17.55,-69.2968662511513,-171.871644662643));
#135946=CARTESIAN_POINT('',(-17.4012711864406,-68.8194987407181,-179.64995));
#135947=CARTESIAN_POINT('Ctrl Pts',(-17.0492479950133,-69.297368111594,
-176.822948722429));
#135948=CARTESIAN_POINT('Ctrl Pts',(-17.0488576004114,-68.9292870000689,
-176.816737185091));
#135949=CARTESIAN_POINT('Ctrl Pts',(-17.3997798690686,-68.8199646773016,
-176.79594636526));
#135950=CARTESIAN_POINT('Ctrl Pts',(-17.053474034057,-69.2947264864225,
-176.89849934037));
#135951=CARTESIAN_POINT('Ctrl Pts',(-17.0551529338767,-68.9273807085645,
-176.909574260456));
#135952=CARTESIAN_POINT('Ctrl Pts',(-17.4081606356245,-68.8173454677221,
-176.947050609194));
#135953=CARTESIAN_POINT('Ctrl Pts',(-17.0398006752804,-69.3032834461013,
-176.975516985737));
#135954=CARTESIAN_POINT('Ctrl Pts',(-17.0345718967367,-68.933617729428,
-177.005206223573));
#135955=CARTESIAN_POINT('Ctrl Pts',(-17.3810445025101,-68.8258298172436,
-177.101089109421));
#135956=CARTESIAN_POINT('Ctrl Pts',(-16.984573721817,-69.3375281363239,
-177.105974674662));
#135957=CARTESIAN_POINT('Ctrl Pts',(-16.9553753472294,-68.9574616796934,
-177.159342510638));
#135958=CARTESIAN_POINT('Ctrl Pts',(-17.271522613636,-68.8597838444499,
-177.362008470827));
#135959=CARTESIAN_POINT('Ctrl Pts',(-16.9464194670572,-69.3611108992158,
-177.16153439432));
#135960=CARTESIAN_POINT('Ctrl Pts',(-16.9006584936516,-68.9738907873115,
-177.221947407359));
#135961=CARTESIAN_POINT('Ctrl Pts',(-17.1958580434816,-68.8831664553272,
-177.473129011102));
#135962=CARTESIAN_POINT('Ctrl Pts',(-16.8534774852002,-69.4179436363549,
-177.252609444331));
#135963=CARTESIAN_POINT('Ctrl Pts',(-16.7738840954457,-69.0116922167351,
-177.31458111062));
#135964=CARTESIAN_POINT('Ctrl Pts',(-17.0115440055365,-68.9395167543114,
-177.65527913718));
#135965=CARTESIAN_POINT('Ctrl Pts',(-16.7979218519985,-69.4516483772983,
-177.28887581796));
#135966=CARTESIAN_POINT('Ctrl Pts',(-16.7000151738869,-69.0335912458224,
-177.345046470341));
#135967=CARTESIAN_POINT('Ctrl Pts',(-16.901371584146,-68.9729353808306,
-177.727810792065));
#135968=CARTESIAN_POINT('Ctrl Pts',(-16.6709738473584,-69.5276893376271,
-177.340535368617));
#135969=CARTESIAN_POINT('Ctrl Pts',(-16.5421185639685,-69.0801133097091,
-177.373722750586));
#135970=CARTESIAN_POINT('Ctrl Pts',(-16.6496229232295,-69.0483307385377,
-177.831125967842));
#135971=CARTESIAN_POINT('Ctrl Pts',(-16.5966263844035,-69.5716604942096,
-177.353161582598));
#135972=CARTESIAN_POINT('Ctrl Pts',(-16.4557762619242,-69.1053726143953,
-177.36608299368));
#135973=CARTESIAN_POINT('Ctrl Pts',(-16.5021951424801,-69.091926058946,
-177.856375144043));
#135974=CARTESIAN_POINT('Ctrl Pts',(-16.5240599846146,-69.6139181916527,
-177.349254788131));
#135975=CARTESIAN_POINT('Ctrl Pts',(-16.3826215477911,-69.1267402936733,
-177.341852229526));
#135976=CARTESIAN_POINT('Ctrl Pts',(-16.3582807548912,-69.1338282608016,
-177.848558467037));
#135977=CARTESIAN_POINT('',(-16.55,-69.5987413979107,-177.34995));
#135978=CARTESIAN_POINT('',(-16.4097457627119,-69.1188156235219,-177.84995));
#135979=CARTESIAN_POINT('Origin',(-16.55,-69.5987413979107,-177.84995));
#135980=CARTESIAN_POINT('Ctrl Pts',(-16.55,-69.5987413979107,-177.34995));
#135981=CARTESIAN_POINT('Ctrl Pts',(-16.571974857016,-69.5858974666297,
-177.34995));
#135982=CARTESIAN_POINT('Ctrl Pts',(-16.5940231568532,-69.5729545882568,
-177.348496976456));
#135983=CARTESIAN_POINT('Ctrl Pts',(-16.6159015410091,-69.5600570385675,
-177.345587959495));
#135984=CARTESIAN_POINT('Ctrl Pts',(-16.637789232771,-69.5471540019415,
-177.342677704967));
#135985=CARTESIAN_POINT('Ctrl Pts',(-16.6595060527741,-69.5342963325752,
-177.338310277277));
#135986=CARTESIAN_POINT('Ctrl Pts',(-16.6808128321261,-69.521628490458,
-177.332534710648));
#135987=CARTESIAN_POINT('Ctrl Pts',(-16.7004320836829,-69.5099639597905,
-177.327216577264));
#135988=CARTESIAN_POINT('Ctrl Pts',(-16.7197032679559,-69.4984603779473,
-177.320705253509));
#135989=CARTESIAN_POINT('Ctrl Pts',(-16.7384517689056,-69.4872305273618,
-177.313076257943));
#135990=CARTESIAN_POINT('Ctrl Pts',(-16.7592707344465,-69.4747605238669,
-177.304604764877));
#135991=CARTESIAN_POINT('Ctrl Pts',(-16.7796238303514,-69.4625248975477,
-177.294681953488));
#135992=CARTESIAN_POINT('Ctrl Pts',(-16.7992696834622,-69.4506685598544,
-177.283383529975));
#135993=CARTESIAN_POINT('Ctrl Pts',(-16.8188916910297,-69.4388266130258,
-177.272098820148));
#135994=CARTESIAN_POINT('Ctrl Pts',(-16.8378074309329,-69.4273630346438,
-177.259442107775));
#135995=CARTESIAN_POINT('Ctrl Pts',(-16.8557951920564,-69.4164222091315,
-177.245537285583));
#135996=CARTESIAN_POINT('Ctrl Pts',(-16.8712360041473,-69.4070305327747,
-177.233601295042));
#135997=CARTESIAN_POINT('Ctrl Pts',(-16.8859930975071,-69.3980240530471,
-177.22074657705));
#135998=CARTESIAN_POINT('Ctrl Pts',(-16.8999432516754,-69.389494096997,
-177.207077037071));
#135999=CARTESIAN_POINT('Ctrl Pts',(-16.91634277459,-69.3794664508494,-177.191007398598));
#136000=CARTESIAN_POINT('Ctrl Pts',(-16.9317275329241,-69.3700407193404,
-177.17371192959));
#136001=CARTESIAN_POINT('Ctrl Pts',(-16.9458910222967,-69.3613359641857,
-177.155351863886));
#136002=CARTESIAN_POINT('Ctrl Pts',(-16.9600211165384,-69.3526517333829,
-177.137035088135));
#136003=CARTESIAN_POINT('Ctrl Pts',(-16.9729351002459,-69.3446850830602,
-177.117659209345));
#136004=CARTESIAN_POINT('Ctrl Pts',(-16.9844613282345,-69.3375542347348,
-177.097423946646));
#136005=CARTESIAN_POINT('Ctrl Pts',(-16.9941214124636,-69.3315779001078,
-177.080464856278));
#136006=CARTESIAN_POINT('Ctrl Pts',(-17.0028071808333,-69.3261886367402,
-177.062903012023));
#136007=CARTESIAN_POINT('Ctrl Pts',(-17.0104398994491,-69.32145603957,-177.044873315679));
#136008=CARTESIAN_POINT('Ctrl Pts',(-17.0192225481519,-69.3160104387965,
-177.024127301425));
#136009=CARTESIAN_POINT('Ctrl Pts',(-17.0266333838746,-69.3114281239145,
-177.002705007449));
#136010=CARTESIAN_POINT('Ctrl Pts',(-17.0325650959538,-69.3077506027218,
-176.980835171685));
#136011=CARTESIAN_POINT('Ctrl Pts',(-17.0384951751614,-69.3040740938709,
-176.958971356213));
#136012=CARTESIAN_POINT('Ctrl Pts',(-17.0429466552163,-69.3013018806378,
-176.936660984636));
#136013=CARTESIAN_POINT('Ctrl Pts',(-17.0458611190542,-69.2994754365511,
-176.914150861446));
#136014=CARTESIAN_POINT('Ctrl Pts',(-17.0486180997703,-69.2977476844135,
-176.892857073289));
#136015=CARTESIAN_POINT('Ctrl Pts',(-17.05,-69.2968662535477,-176.871385242631));
#136016=CARTESIAN_POINT('Ctrl Pts',(-17.05,-69.2968662511513,-176.84995));
#136017=CARTESIAN_POINT('Ctrl Pts',(-17.4012711864406,-68.8194987407181,
-176.84995));
#136018=CARTESIAN_POINT('Ctrl Pts',(-17.4012711797275,-68.8194987428096,
-176.887694684675));
#136019=CARTESIAN_POINT('Ctrl Pts',(-17.3991058038741,-68.8201748588276,
-176.925251096234));
#136020=CARTESIAN_POINT('Ctrl Pts',(-17.3948976591097,-68.8214863041692,
-176.962447012708));
#136021=CARTESIAN_POINT('Ctrl Pts',(-17.3906053585138,-68.8228239762163,
-177.000386785074));
#136022=CARTESIAN_POINT('Ctrl Pts',(-17.3841876175728,-68.8248226995135,
-177.037952567699));
#136023=CARTESIAN_POINT('Ctrl Pts',(-17.3757224555706,-68.8274555088436,
-177.074968429999));
#136024=CARTESIAN_POINT('Ctrl Pts',(-17.3672590966796,-68.8300877573754,
-177.11197640778));
#136025=CARTESIAN_POINT('Ctrl Pts',(-17.356748909814,-68.8333539190401,
-177.148435801525));
#136026=CARTESIAN_POINT('Ctrl Pts',(-17.3442218215212,-68.837241948804,
-177.184161144092));
#136027=CARTESIAN_POINT('Ctrl Pts',(-17.3378147381211,-68.839230513934,
-177.202433167405));
#136028=CARTESIAN_POINT('Ctrl Pts',(-17.3308793073379,-68.8413819840089,
-177.22051291325));
#136029=CARTESIAN_POINT('Ctrl Pts',(-17.3234150119905,-68.84369613616,-177.238373157981));
#136030=CARTESIAN_POINT('Ctrl Pts',(-17.323216781765,-68.8437575933882,
-177.238847474735));
#136031=CARTESIAN_POINT('Ctrl Pts',(-17.3230181873272,-68.8438191626283,
-177.239321615502));
#136032=CARTESIAN_POINT('Ctrl Pts',(-17.3228192288394,-68.8438808438229,
-177.23979557955));
#136033=CARTESIAN_POINT('Ctrl Pts',(-17.2882744024226,-68.8545904455368,
-177.322089157366));
#136034=CARTESIAN_POINT('Ctrl Pts',(-17.24265513348,-68.868699441709,-177.399426405929));
#136035=CARTESIAN_POINT('Ctrl Pts',(-17.1883023464399,-68.8854065190392,
-177.469044916629));
#136036=CARTESIAN_POINT('Ctrl Pts',(-17.1624825557968,-68.8933430621755,
-177.502116548628));
#136037=CARTESIAN_POINT('Ctrl Pts',(-17.1346920798658,-68.9018658361705,
-177.533445664935));
#136038=CARTESIAN_POINT('Ctrl Pts',(-17.1051831298931,-68.9108884594799,
-177.562732114831));
#136039=CARTESIAN_POINT('Ctrl Pts',(-17.104688915706,-68.9110395698531,
-177.5632226026));
#136040=CARTESIAN_POINT('Ctrl Pts',(-17.1041942190907,-68.9111908205538,
-177.563712518466));
#136041=CARTESIAN_POINT('Ctrl Pts',(-17.1036990412529,-68.9113422111695,
-177.564201860987));
#136042=CARTESIAN_POINT('Ctrl Pts',(-17.0462278720989,-68.9289128595717,
-177.620995773434));
#136043=CARTESIAN_POINT('Ctrl Pts',(-16.9816775189031,-68.9485450280228,
-177.67064989156));
#136044=CARTESIAN_POINT('Ctrl Pts',(-16.9125398584879,-68.9694257059549,
-177.711729306558));
#136045=CARTESIAN_POINT('Ctrl Pts',(-16.8713991530587,-68.9818508562248,
-177.736173814827));
#136046=CARTESIAN_POINT('Ctrl Pts',(-16.8286352683543,-68.9947177370478,
-177.7575822379));
#136047=CARTESIAN_POINT('Ctrl Pts',(-16.7847809634131,-69.007852694924,
-177.775654990622));
#136048=CARTESIAN_POINT('Ctrl Pts',(-16.78433889104,-69.007985101583,-177.775837172615));
#136049=CARTESIAN_POINT('Ctrl Pts',(-16.7838967203631,-69.008117531739,
-177.776019010763));
#136050=CARTESIAN_POINT('Ctrl Pts',(-16.7834544517973,-69.0082499852542,
-177.776200504879));
#136051=CARTESIAN_POINT('Ctrl Pts',(-16.7449698092192,-69.0197756205532,
-177.791993479437));
#136052=CARTESIAN_POINT('Ctrl Pts',(-16.7054466746896,-69.031566259125,
-177.805303057386));
#136053=CARTESIAN_POINT('Ctrl Pts',(-16.6651986963189,-69.0435261398609,
-177.816095296664));
#136054=CARTESIAN_POINT('Ctrl Pts',(-16.6237252999666,-69.0558501594555,
-177.827216123976));
#136055=CARTESIAN_POINT('Ctrl Pts',(-16.5814808439819,-69.0683543171784,
-177.835664557351));
#136056=CARTESIAN_POINT('Ctrl Pts',(-16.5387947985049,-69.0809368867564,
-177.841347934728));
#136057=CARTESIAN_POINT('Ctrl Pts',(-16.4988275773255,-69.0927180282444,
-177.84666931782));
#136058=CARTESIAN_POINT('Ctrl Pts',(-16.4584720658829,-69.1045682551434,
-177.849566394706));
#136059=CARTESIAN_POINT('Ctrl Pts',(-16.4180055598672,-69.1164010707452,
-177.849914459328));
#136060=CARTESIAN_POINT('Ctrl Pts',(-16.415252771043,-69.1172060140367,
-177.849938136895));
#136061=CARTESIAN_POINT('Ctrl Pts',(-16.41249947515,-69.1180108744163,-177.849949999677));
#136062=CARTESIAN_POINT('Ctrl Pts',(-16.4097457627119,-69.1188156235219,
-177.84995));
#136063=CARTESIAN_POINT('Origin',(0.,-12.9675000200281,-177.84995));
#136064=CARTESIAN_POINT('',(-16.05,-69.7424724991055,-177.34995));
#136065=CARTESIAN_POINT('',(-15.9139830508475,-69.2613286645371,-177.84995));
#136066=CARTESIAN_POINT('Origin',(-16.0500000000002,-69.7424724991055,-177.84995));
#136067=CARTESIAN_POINT('Origin',(0.,-12.9675000200281,-177.34995));
#136068=CARTESIAN_POINT('Origin',(0.,-12.9675000200281,-177.84995));
#136069=CARTESIAN_POINT('Ctrl Pts',(-16.05,-69.7424724991056,-177.34995));
#136070=CARTESIAN_POINT('Ctrl Pts',(-15.9139830508475,-69.2613286645371,
-177.34995));
#136071=CARTESIAN_POINT('Ctrl Pts',(-15.9139830508475,-69.2613286645371,
-177.84995));
#136072=CARTESIAN_POINT('Ctrl Pts',(-15.9218377669144,-69.8149341395249,
-177.34995));
#136073=CARTESIAN_POINT('Ctrl Pts',(-15.7715232212968,-69.3016013426613,
-177.313287744377));
#136074=CARTESIAN_POINT('Ctrl Pts',(-15.6598936117711,-69.3331584747352,
-177.849949962799));
#136075=CARTESIAN_POINT('Ctrl Pts',(-15.7932661099729,-69.8854545791845,
-177.298481825532));
#136076=CARTESIAN_POINT('Ctrl Pts',(-15.6726841471448,-69.3295726985644,
-177.220678605763));
#136077=CARTESIAN_POINT('Ctrl Pts',(-15.4048666982144,-69.4030990332408,
-177.747013645666));
#136078=CARTESIAN_POINT('Ctrl Pts',(-15.6065726131672,-69.9860620159006,
-177.115402898665));
#136079=CARTESIAN_POINT('Ctrl Pts',(-15.5618471106836,-69.3622450871995,
-177.028739897256));
#136080=CARTESIAN_POINT('Ctrl Pts',(-15.0346439900464,-69.5028538622254,
-177.380855802727));
#136081=CARTESIAN_POINT('Ctrl Pts',(-15.55,-70.0157033150841,-176.985144891356));
#136082=CARTESIAN_POINT('Ctrl Pts',(-15.5500000039846,-69.3666907690031,
-176.935931672441));
#136083=CARTESIAN_POINT('Ctrl Pts',(-14.922457653694,-69.5322439651191,
-177.120339778533));
#136084=CARTESIAN_POINT('Ctrl Pts',(-15.55,-70.015703322148,-176.84995));
#136085=CARTESIAN_POINT('Ctrl Pts',(-15.5499999999999,-69.3666907703604,
-176.84995));
#136086=CARTESIAN_POINT('Ctrl Pts',(-14.9224576271186,-69.53224397213,-176.84995));
#136087=CARTESIAN_POINT('',(-14.9224576271186,-69.53224397213,-176.84995));
#136088=CARTESIAN_POINT('Ctrl Pts',(-15.9139830508475,-69.2613286645371,
-177.84995));
#136089=CARTESIAN_POINT('Ctrl Pts',(-15.6598936117711,-69.3331584747352,
-177.849949962799));
#136090=CARTESIAN_POINT('Ctrl Pts',(-15.4048666982144,-69.4030990332408,
-177.747013645666));
#136091=CARTESIAN_POINT('Ctrl Pts',(-15.0346439900464,-69.5028538622254,
-177.380855802727));
#136092=CARTESIAN_POINT('Ctrl Pts',(-14.922457653694,-69.5322439651191,
-177.120339778533));
#136093=CARTESIAN_POINT('Ctrl Pts',(-14.9224576271186,-69.53224397213,-176.84995));
#136094=CARTESIAN_POINT('',(-15.55,-70.015703322148,-176.84995));
#136095=CARTESIAN_POINT('Origin',(-15.05,-70.015703322148,-176.84995));
#136096=CARTESIAN_POINT('Ctrl Pts',(-15.55,-70.015703322148,-176.84995));
#136097=CARTESIAN_POINT('Ctrl Pts',(-15.55,-70.0157033150841,-176.985144891356));
#136098=CARTESIAN_POINT('Ctrl Pts',(-15.6065726131672,-69.9860620159006,
-177.115402898665));
#136099=CARTESIAN_POINT('Ctrl Pts',(-15.7932661099729,-69.8854545791845,
-177.298481825532));
#136100=CARTESIAN_POINT('Ctrl Pts',(-15.9218377669144,-69.8149341395249,
-177.34995));
#136101=CARTESIAN_POINT('Ctrl Pts',(-16.05,-69.7424724991055,-177.34995));
#136102=CARTESIAN_POINT('Origin',(-15.05,-70.015703322148,-179.64995));
#136103=CARTESIAN_POINT('',(-14.9224576271186,-69.5322439721301,-171.871644662643));
#136104=CARTESIAN_POINT('',(-14.9224576271186,-69.5322439721301,-179.64995));
#136105=CARTESIAN_POINT('',(-15.55,-70.015703322148,-171.871644662643));
#136106=CARTESIAN_POINT('Origin',(-15.05,-70.015703322148,-171.871644662643));
#136107=CARTESIAN_POINT('',(-15.55,-70.015703322148,-176.84995));
#136108=CARTESIAN_POINT('Origin',(0.,-12.9675000200281,-171.871644662643));
#136109=CARTESIAN_POINT('',(-9.32033898305081,-70.7202599648223,-171.871644662643));
#136110=CARTESIAN_POINT('Origin',(0.,-12.9675000200281,-171.871644662643));
#136111=CARTESIAN_POINT('',(-9.3276302147955,-70.6241744288951,-171.449026400902));
#136112=CARTESIAN_POINT('Origin',(-9.40047870352405,-69.677975233741,-171.875589094873));
#136113=CARTESIAN_POINT('',(-14.9341313545396,-69.4322546019744,-171.449026400902));
#136114=CARTESIAN_POINT('Origin',(0.,-12.9675000200281,-171.449026400902));
#136115=CARTESIAN_POINT('Origin',(-15.0818193009629,-68.1701112854949,-171.933582810381));
#136116=CARTESIAN_POINT('Origin',(-9.4,-71.2138732976838,-179.64995));
#136117=CARTESIAN_POINT('',(-8.89999998637947,-71.2138732976795,-176.681036188732));
#136118=CARTESIAN_POINT('',(-9.32033898305081,-70.7202599648223,-176.681036188741));
#136119=CARTESIAN_POINT('Origin',(-9.4,-71.2138732976838,-176.681036188741));
#136120=CARTESIAN_POINT('',(-8.9,-71.2138732976838,-171.871644662643));
#136121=CARTESIAN_POINT('',(-8.9,-71.2138732976838,-171.871644662643));
#136122=CARTESIAN_POINT('Origin',(-9.4,-71.2138732976838,-171.871644662643));
#136123=CARTESIAN_POINT('',(-9.32033898305081,-70.7202599648223,-179.64995));
#136124=CARTESIAN_POINT('Ctrl Pts',(-8.9,-71.2138732976838,-176.681036188741));
#136125=CARTESIAN_POINT('Ctrl Pts',(-8.89999999999995,-70.7880957152449,
-176.681036188741));
#136126=CARTESIAN_POINT('Ctrl Pts',(-9.32033898305081,-70.7202599648223,
-176.681036188741));
#136127=CARTESIAN_POINT('Ctrl Pts',(-8.9,-71.1871171480823,-176.760825627325));
#136128=CARTESIAN_POINT('Ctrl Pts',(-8.92228717603221,-70.7844989338608,
-176.766146975383));
#136129=CARTESIAN_POINT('Ctrl Pts',(-9.32033898600605,-70.7202599643454,
-176.813381110627));
#136130=CARTESIAN_POINT('Ctrl Pts',(-8.88962568872291,-71.1669786363603,
-176.836281093745));
#136131=CARTESIAN_POINT('Ctrl Pts',(-8.92671149441355,-70.7836436470507,
-176.856038553599));
#136132=CARTESIAN_POINT('Ctrl Pts',(-9.29976619260072,-70.7235936461789,
-176.944341025131));
#136133=CARTESIAN_POINT('Ctrl Pts',(-8.84506581279844,-71.1392355158483,
-176.976329963003));
#136134=CARTESIAN_POINT('Ctrl Pts',(-8.89496802003281,-70.7881886691942,
-177.027264022804));
#136135=CARTESIAN_POINT('Ctrl Pts',(-9.21140170024677,-70.7377525805495,
-177.193900303459));
#136136=CARTESIAN_POINT('Ctrl Pts',(-8.81169873029936,-71.1320753660863,
-177.038360991276));
#136137=CARTESIAN_POINT('Ctrl Pts',(-8.86020506502259,-70.7933743404483,
-177.1069029419));
#136138=CARTESIAN_POINT('Ctrl Pts',(-9.14523307029305,-70.748315066844,
-177.307880650604));
#136139=CARTESIAN_POINT('Ctrl Pts',(-8.67906488297454,-71.1273471571499,
-177.195002198461));
#136140=CARTESIAN_POINT('Ctrl Pts',(-8.70620726441098,-70.816353148992,
-177.306646407394));
#136141=CARTESIAN_POINT('Ctrl Pts',(-8.88221342209322,-70.789535493208,
-177.600825160592));
#136142=CARTESIAN_POINT('Ctrl Pts',(-8.55095696965989,-71.1465765189117,
-177.251701888337));
#136143=CARTESIAN_POINT('Ctrl Pts',(-8.53744099317464,-70.8414090832674,
-177.381970537377));
#136144=CARTESIAN_POINT('Ctrl Pts',(-8.62826388004552,-70.8283148356172,
-177.714106286858));
#136145=CARTESIAN_POINT('Ctrl Pts',(-8.41817827172749,-71.1781985203564,
-177.244444626905));
#136146=CARTESIAN_POINT('Ctrl Pts',(-8.37078242155037,-70.8655141261624,
-177.369392503913));
#136147=CARTESIAN_POINT('Ctrl Pts',(-8.36486199647655,-70.8663694716841,
-177.709383806606));
#136148=CARTESIAN_POINT('',(-8.41817827230434,-71.1781985202609,-177.244444626919));
#136149=CARTESIAN_POINT('',(-8.36486199647649,-70.8663694716841,-177.709383806605));
#136150=CARTESIAN_POINT('Origin',(-8.43635654345535,-71.3612316037495,-177.709383806605));
#136151=CARTESIAN_POINT('Ctrl Pts',(-8.4181782717274,-71.1781985203566,
-177.244444626904));
#136152=CARTESIAN_POINT('Ctrl Pts',(-8.55095696965989,-71.1465765189117,
-177.251701888337));
#136153=CARTESIAN_POINT('Ctrl Pts',(-8.67906488297454,-71.1273471571499,
-177.195002198461));
#136154=CARTESIAN_POINT('Ctrl Pts',(-8.81169873029936,-71.1320753660863,
-177.038360991276));
#136155=CARTESIAN_POINT('Ctrl Pts',(-8.84506581279844,-71.1392355158483,
-176.976329963003));
#136156=CARTESIAN_POINT('Ctrl Pts',(-8.88962568872291,-71.1669786363603,
-176.836281093745));
#136157=CARTESIAN_POINT('Ctrl Pts',(-8.9,-71.1871171480823,-176.760825627325));
#136158=CARTESIAN_POINT('Ctrl Pts',(-8.9,-71.2138732976838,-176.681036188741));
#136159=CARTESIAN_POINT('Ctrl Pts',(-9.32033898305081,-70.7202599648223,
-176.681036188741));
#136160=CARTESIAN_POINT('Ctrl Pts',(-9.32033898600605,-70.7202599643454,
-176.813381110627));
#136161=CARTESIAN_POINT('Ctrl Pts',(-9.29976619260072,-70.7235936461789,
-176.944341025131));
#136162=CARTESIAN_POINT('Ctrl Pts',(-9.21140170024677,-70.7377525805495,
-177.193900303459));
#136163=CARTESIAN_POINT('Ctrl Pts',(-9.14523307029305,-70.748315066844,
-177.307880650604));
#136164=CARTESIAN_POINT('Ctrl Pts',(-8.88221342209322,-70.789535493208,
-177.600825160592));
#136165=CARTESIAN_POINT('Ctrl Pts',(-8.62826388004552,-70.8283148356172,
-177.714106286858));
#136166=CARTESIAN_POINT('Ctrl Pts',(-8.36486199647649,-70.8663694716841,
-177.709383806605));
#136167=CARTESIAN_POINT('Ctrl Pts',(-7.86991817520098,-70.935718794764,
-177.700825662763));
#136168=CARTESIAN_POINT('Ctrl Pts',(-7.87530650495358,-70.9349872609141,
-177.368681451894));
#136169=CARTESIAN_POINT('Ctrl Pts',(-7.91859121655416,-71.2381488509313,
-177.239961484006));
#136170=CARTESIAN_POINT('Ctrl Pts',(-8.03499989482399,-70.9133068653807,
-177.703576433696));
#136171=CARTESIAN_POINT('Ctrl Pts',(-8.04094447940713,-70.9124841487064,
-177.368907517599));
#136172=CARTESIAN_POINT('Ctrl Pts',(-8.08517348178868,-71.21877443556,-177.241356202481));
#136173=CARTESIAN_POINT('Ctrl Pts',(-8.19998119128136,-70.8901904062617,
-177.706427680957));
#136174=CARTESIAN_POINT('Ctrl Pts',(-8.20613182703653,-70.889318969813,
-177.369144269326));
#136175=CARTESIAN_POINT('Ctrl Pts',(-8.25170137526425,-71.1987909763519,
-177.242846915875));
#136176=CARTESIAN_POINT('Ctrl Pts',(-8.36486199647703,-70.866369471684,
-177.709383806605));
#136177=CARTESIAN_POINT('Ctrl Pts',(-8.3707824215504,-70.8655141261623,
-177.369392503912));
#136178=CARTESIAN_POINT('Ctrl Pts',(-8.41817827172741,-71.1781985203567,
-177.244444626904));
#136179=CARTESIAN_POINT('',(-7.91859121655529,-71.238148850898,-177.239961484019));
#136180=CARTESIAN_POINT('',(-7.86991817520075,-70.935718794764,-177.700825662763));
#136181=CARTESIAN_POINT('Origin',(-7.93718243310846,-71.4311736560866,-177.700825662763));
#136182=CARTESIAN_POINT('Origin',(-0.0604498207115989,-4.47548892910441,
-188.389030577756));
#136183=CARTESIAN_POINT('Origin',(-0.0230368112449109,-14.1525797482743,
-185.975887614352));
#136184=CARTESIAN_POINT('Ctrl Pts',(-7.91859121655422,-71.2381488509314,
-177.239961484007));
#136185=CARTESIAN_POINT('Ctrl Pts',(-7.87530650495354,-70.9349872609141,
-177.368681451895));
#136186=CARTESIAN_POINT('Ctrl Pts',(-7.86991817520074,-70.935718794764,
-177.700825662764));
#136187=CARTESIAN_POINT('Ctrl Pts',(-7.84535391894273,-71.2544423085659,
-177.236091643156));
#136188=CARTESIAN_POINT('Ctrl Pts',(-7.78148695261579,-70.9477382671599,
-177.362180852783));
#136189=CARTESIAN_POINT('Ctrl Pts',(-7.72465595207765,-70.9554399770617,
-177.698405110518));
#136190=CARTESIAN_POINT('Ctrl Pts',(-7.77193648886645,-71.274739088698,
-177.212399058377));
#136191=CARTESIAN_POINT('Ctrl Pts',(-7.68873678647519,-70.9601668953933,
-177.328725158091));
#136192=CARTESIAN_POINT('Ctrl Pts',(-7.57909439591914,-70.9746058127342,
-177.660005031717));
#136193=CARTESIAN_POINT('Ctrl Pts',(-7.64153051403658,-71.3201342851139,
-177.131947985374));
#136194=CARTESIAN_POINT('Ctrl Pts',(-7.53187921075035,-70.98103712284,-177.221702886533));
#136195=CARTESIAN_POINT('Ctrl Pts',(-7.32049271153216,-71.0078082615326,
-177.524965998388));
#136196=CARTESIAN_POINT('Ctrl Pts',(-7.58359051438092,-71.3455846992379,
-177.074841178091));
#136197=CARTESIAN_POINT('Ctrl Pts',(-7.46634030528468,-70.9896817811965,
-177.14630380948));
#136198=CARTESIAN_POINT('Ctrl Pts',(-7.20559474882705,-71.0221114770482,
-177.427818678983));
#136199=CARTESIAN_POINT('Ctrl Pts',(-7.49125858243999,-71.4004398176271,
-176.937641167035));
#136200=CARTESIAN_POINT('Ctrl Pts',(-7.3754100247025,-71.0018071186815,
-176.974926941462));
#136201=CARTESIAN_POINT('Ctrl Pts',(-7.0224958330043,-71.0445441888331,
-177.19789774704));
#136202=CARTESIAN_POINT('Ctrl Pts',(-7.45636610731683,-71.4300660132009,
-176.85726439743));
#136203=CARTESIAN_POINT('Ctrl Pts',(-7.35016748493995,-71.0052818262832,
-176.876651794266));
#136204=CARTESIAN_POINT('Ctrl Pts',(-6.95330228061017,-71.0528136932555,
-177.064676392973));
#136205=CARTESIAN_POINT('Ctrl Pts',(-7.41072271257901,-71.4935573295699,
-176.680998879949));
#136206=CARTESIAN_POINT('Ctrl Pts',(-7.34226626007839,-71.0069144630253,
-176.677678014477));
#136207=CARTESIAN_POINT('Ctrl Pts',(-6.86278910799687,-71.0635773642165,
-176.782076502575));
#136208=CARTESIAN_POINT('Ctrl Pts',(-7.4,-71.5272255526701,-176.585813210379));
#136209=CARTESIAN_POINT('Ctrl Pts',(-7.36167840976143,-71.0048156182876,
-176.575906600101));
#136210=CARTESIAN_POINT('Ctrl Pts',(-6.8415254209523,-71.06606738545,-176.633819401763));
#136211=CARTESIAN_POINT('Ctrl Pts',(-7.4,-71.5626363369615,-176.485569595297));
#136212=CARTESIAN_POINT('Ctrl Pts',(-7.40000000000002,-71.0003029749946,
-176.485569595297));
#136213=CARTESIAN_POINT('Ctrl Pts',(-6.84152542372878,-71.066067385123,
-176.485569595297));
#136214=CARTESIAN_POINT('',(-6.84152542372878,-71.066067385123,-176.485569595297));
#136215=CARTESIAN_POINT('Ctrl Pts',(-7.86991817520075,-70.935718794764,
-177.700825662763));
#136216=CARTESIAN_POINT('Ctrl Pts',(-7.84145915028904,-70.9395824669992,
-177.700351440663));
#136217=CARTESIAN_POINT('Ctrl Pts',(-7.81325306985418,-70.9433890026599,
-177.698505055736));
#136218=CARTESIAN_POINT('Ctrl Pts',(-7.78529419147434,-70.9471417642783,
-177.695385832037));
#136219=CARTESIAN_POINT('Ctrl Pts',(-7.77696163598821,-70.9482601959259,
-177.694456213038));
#136220=CARTESIAN_POINT('Ctrl Pts',(-7.76865098308068,-70.9493738524319,
-177.693413186647));
#136221=CARTESIAN_POINT('Ctrl Pts',(-7.76036198762536,-70.9504828203398,
-177.692258509338));
#136222=CARTESIAN_POINT('Ctrl Pts',(-7.73171720388245,-70.9543151479204,
-177.688268221013));
#136223=CARTESIAN_POINT('Ctrl Pts',(-7.7033289936209,-70.9580918229642,
-177.682948350417));
#136224=CARTESIAN_POINT('Ctrl Pts',(-7.67518610521715,-70.9618160028387,
-177.676335993945));
#136225=CARTESIAN_POINT('Ctrl Pts',(-7.66343218081719,-70.9633714127906,
-177.673574332209));
#136226=CARTESIAN_POINT('Ctrl Pts',(-7.65172493396012,-70.9649171451445,
-177.670587723936));
#136227=CARTESIAN_POINT('Ctrl Pts',(-7.64004659109474,-70.9664556187744,
-177.667371199654));
#136228=CARTESIAN_POINT('Ctrl Pts',(-7.60920468563951,-70.9705186488451,
-177.658876523743));
#136229=CARTESIAN_POINT('Ctrl Pts',(-7.57859346492051,-70.9745271017095,
-177.64877837365));
#136230=CARTESIAN_POINT('Ctrl Pts',(-7.54854310099584,-70.9784389453262,
-177.637166030246));
#136231=CARTESIAN_POINT('Ctrl Pts',(-7.52067144326531,-70.9820671731458,
-177.626395602919));
#136232=CARTESIAN_POINT('Ctrl Pts',(-7.49328227206125,-70.9856123005525,
-177.614321694518));
#136233=CARTESIAN_POINT('Ctrl Pts',(-7.4666388775123,-70.9890415496571,
-177.601070367657));
#136234=CARTESIAN_POINT('Ctrl Pts',(-7.46098971645269,-70.9897686484684,
-177.598260707666));
#136235=CARTESIAN_POINT('Ctrl Pts',(-7.45537399181997,-70.9904905521545,
-177.595398277761));
#136236=CARTESIAN_POINT('Ctrl Pts',(-7.44979405295274,-70.9912069730377,
-177.59248453496));
#136237=CARTESIAN_POINT('Ctrl Pts',(-7.44926963945517,-70.9912743036645,
-177.59221069575));
#136238=CARTESIAN_POINT('Ctrl Pts',(-7.44874551143164,-70.9913415902563,
-177.591936395013));
#136239=CARTESIAN_POINT('Ctrl Pts',(-7.44822167031191,-70.9914088326578,
-177.591661634332));
#136240=CARTESIAN_POINT('Ctrl Pts',(-7.36341668567551,-71.0022947494168,
-177.547180446307));
#136241=CARTESIAN_POINT('Ctrl Pts',(-7.2849205420624,-71.0121779828215,
-177.489997024843));
#136242=CARTESIAN_POINT('Ctrl Pts',(-7.21521422000437,-71.0208423096892,
-177.423514614708));
#136243=CARTESIAN_POINT('Ctrl Pts',(-7.17900585545438,-71.0253429216357,
-177.388980884176));
#136244=CARTESIAN_POINT('Ctrl Pts',(-7.14516858275053,-71.029514703104,
-177.351937503402));
#136245=CARTESIAN_POINT('Ctrl Pts',(-7.1140463350679,-71.0333277050162,
-177.3128573618));
#136246=CARTESIAN_POINT('Ctrl Pts',(-7.11356074608129,-71.0333871978829,
-177.312247608721));
#136247=CARTESIAN_POINT('Ctrl Pts',(-7.11307579006789,-71.0334466073515,
-177.311637347152));
#136248=CARTESIAN_POINT('Ctrl Pts',(-7.11259146723154,-71.0335059334348,
-177.311026578643));
#136249=CARTESIAN_POINT('Ctrl Pts',(-7.05806005588037,-71.0401856412925,
-177.242258256475));
#136250=CARTESIAN_POINT('Ctrl Pts',(-7.01156780676673,-71.0458068303072,
-177.1670831198));
#136251=CARTESIAN_POINT('Ctrl Pts',(-6.97337953736936,-71.0503909874129,
-177.087652956333));
#136252=CARTESIAN_POINT('Ctrl Pts',(-6.94786514373973,-71.0534537601099,
-177.034583977593));
#136253=CARTESIAN_POINT('Ctrl Pts',(-6.9260581499733,-71.0560535184276,
-176.97961441076));
#136254=CARTESIAN_POINT('Ctrl Pts',(-6.90804579110999,-71.058195517224,
-176.923376416061));
#136255=CARTESIAN_POINT('Ctrl Pts',(-6.90788807893848,-71.0582142720847,
-176.922884008801));
#136256=CARTESIAN_POINT('Ctrl Pts',(-6.90773065840123,-71.0582329917957,
-176.922391517884));
#136257=CARTESIAN_POINT('Ctrl Pts',(-6.90757352937676,-71.0582516763749,
-176.921898943596));
#136258=CARTESIAN_POINT('Ctrl Pts',(-6.89200677785444,-71.0601027551398,
-176.873099674503));
#136259=CARTESIAN_POINT('Ctrl Pts',(-6.87933106860593,-71.0616054747708,
-176.82359063585));
#136260=CARTESIAN_POINT('Ctrl Pts',(-6.86938539001926,-71.0627821611453,
-176.773553029938));
#136261=CARTESIAN_POINT('Ctrl Pts',(-6.85903549341789,-71.0640066710871,
-176.72148176674));
#136262=CARTESIAN_POINT('Ctrl Pts',(-6.85164206564099,-71.0648780949575,
-176.668837206011));
#136263=CARTESIAN_POINT('Ctrl Pts',(-6.84707944646844,-71.065414925157,
-176.615812182358));
#136264=CARTESIAN_POINT('Ctrl Pts',(-6.84336254226504,-71.0658522499369,
-176.572615736228));
#136265=CARTESIAN_POINT('Ctrl Pts',(-6.84152542372878,-71.066067385123,
-176.529166339213));
#136266=CARTESIAN_POINT('Ctrl Pts',(-6.84152542372878,-71.066067385123,
-176.485569595297));
#136267=CARTESIAN_POINT('',(-7.40000000143918,-71.5626363369615,-176.485569595296));
#136268=CARTESIAN_POINT('Origin',(-6.9,-71.5626363369615,-176.485569595297));
#136269=CARTESIAN_POINT('Ctrl Pts',(-7.4,-71.5626363369618,-176.485569595297));
#136270=CARTESIAN_POINT('Ctrl Pts',(-7.4,-71.5272255526701,-176.585813210379));
#136271=CARTESIAN_POINT('Ctrl Pts',(-7.41072271257901,-71.4935573295699,
-176.680998879949));
#136272=CARTESIAN_POINT('Ctrl Pts',(-7.45636610731683,-71.4300660132009,
-176.85726439743));
#136273=CARTESIAN_POINT('Ctrl Pts',(-7.49125858243999,-71.4004398176271,
-176.937641167035));
#136274=CARTESIAN_POINT('Ctrl Pts',(-7.58359051438092,-71.3455846992379,
-177.074841178091));
#136275=CARTESIAN_POINT('Ctrl Pts',(-7.64153051403658,-71.3201342851139,
-177.131947985374));
#136276=CARTESIAN_POINT('Ctrl Pts',(-7.77193648886645,-71.274739088698,
-177.212399058377));
#136277=CARTESIAN_POINT('Ctrl Pts',(-7.84535391894273,-71.2544423085659,
-177.236091643156));
#136278=CARTESIAN_POINT('Ctrl Pts',(-7.91859121655449,-71.2381488509313,
-177.239961484006));
#136279=CARTESIAN_POINT('Origin',(-6.9,-71.5626363369615,-179.64995));
#136280=CARTESIAN_POINT('',(-6.84152542372877,-71.066067385123,-171.871644662643));
#136281=CARTESIAN_POINT('',(-6.84152542372878,-71.066067385123,-179.64995));
#136282=CARTESIAN_POINT('',(-7.4,-71.5626363369615,-171.871644662643));
#136283=CARTESIAN_POINT('Origin',(-6.9,-71.5626363369615,-171.871644662643));
#136284=CARTESIAN_POINT('',(-7.4,-71.5626363369615,-176.798439391084));
#136285=CARTESIAN_POINT('Origin',(0.,-12.9675000200281,-171.871644662643));
#136286=CARTESIAN_POINT('',(-1.23940677966098,-71.4543692372681,-171.871644662643));
#136287=CARTESIAN_POINT('Origin',(0.,-12.9675000200281,-171.871644662643));
#136288=CARTESIAN_POINT('',(-1.24037635835043,-71.360635368318,-171.449026400902));
#136289=CARTESIAN_POINT('Origin',(-1.24989913208291,-70.4548469135707,-171.87165100631));
#136290=CARTESIAN_POINT('',(-6.84687749809456,-70.9710952348089,-171.449026400902));
#136291=CARTESIAN_POINT('Origin',(0.,-12.9675000200281,-171.449026400902));
#136292=CARTESIAN_POINT('Origin',(-6.92386407101644,-69.6082647247615,-171.968716884213));
#136293=CARTESIAN_POINT('Origin',(-1.24999999999996,-71.9542570083556,-179.64995));
#136294=CARTESIAN_POINT('',(-0.749999999999965,-71.9542570083556,-176.344247731786));
#136295=CARTESIAN_POINT('',(-1.23940677966098,-71.4543692372681,-176.344247731786));
#136296=CARTESIAN_POINT('Origin',(-1.24999999999996,-71.9542570083556,-176.344247731786));
#136297=CARTESIAN_POINT('',(-0.749999999999965,-71.9542570083556,-171.871644662643));
#136298=CARTESIAN_POINT('',(-0.749999999999965,-71.9542570083556,-171.871644662643));
#136299=CARTESIAN_POINT('Origin',(-1.24999999999996,-71.9542570083556,-171.871644662643));
#136300=CARTESIAN_POINT('',(-1.23940677966098,-71.4543692372681,-179.64995));
#136301=CARTESIAN_POINT('Ctrl Pts',(-0.747421739247287,-71.9934178165856,
-176.221164796295));
#136302=CARTESIAN_POINT('Ctrl Pts',(-0.70616503121794,-71.4656369062186,
-176.224399921719));
#136303=CARTESIAN_POINT('Ctrl Pts',(-1.23427661107857,-71.4545023028019,
-176.191083684094));
#136304=CARTESIAN_POINT('Ctrl Pts',(-0.758975746064385,-71.9025894407889,
-176.507953684521));
#136305=CARTESIAN_POINT('Ctrl Pts',(-0.81048947165755,-71.4635573472225,
-176.471174785183));
#136306=CARTESIAN_POINT('Ctrl Pts',(-1.25722997205992,-71.45389181123,-176.53857099329));
#136307=CARTESIAN_POINT('Ctrl Pts',(-0.733576267199836,-71.8205532116895,
-176.762007115851));
#136308=CARTESIAN_POINT('Ctrl Pts',(-0.846229070149368,-71.4625657314852,
-176.781098235956));
#136309=CARTESIAN_POINT('Ctrl Pts',(-1.20689317142187,-71.4553901565039,
-176.912968106426));
#136310=CARTESIAN_POINT('Ctrl Pts',(-0.61137645617211,-71.7551248751779,
-176.992297889673));
#136311=CARTESIAN_POINT('Ctrl Pts',(-0.713096236824655,-71.463696805273,
-177.074741700705));
#136312=CARTESIAN_POINT('Ctrl Pts',(-0.964561766455219,-71.4595630740809,
-177.27289534809));
#136313=CARTESIAN_POINT('Ctrl Pts',(-0.587032103695945,-71.7450861570452,
-177.028762667147));
#136314=CARTESIAN_POINT('Ctrl Pts',(-0.685202146366885,-71.4639504420806,
-177.120826376552));
#136315=CARTESIAN_POINT('Ctrl Pts',(-0.916284213905676,-71.4603489737626,
-177.330911863332));
#136316=CARTESIAN_POINT('Ctrl Pts',(-0.532211729471667,-71.7276623467411,
-177.093668859127));
#136317=CARTESIAN_POINT('Ctrl Pts',(-0.619044665129952,-71.4645348847711,
-177.203483227351));
#136318=CARTESIAN_POINT('Ctrl Pts',(-0.807567270427997,-71.4619509584614,
-177.435272175182));
#136319=CARTESIAN_POINT('Ctrl Pts',(-0.501290424235228,-71.7202266627171,
-177.122322890028));
#136320=CARTESIAN_POINT('Ctrl Pts',(-0.580169914453843,-71.4648703870088,
-177.240630878936));
#136321=CARTESIAN_POINT('Ctrl Pts',(-0.746244778353079,-71.4627761544078,
-177.481978941987));
#136322=CARTESIAN_POINT('Ctrl Pts',(-0.380827972894088,-71.6987946446081,
-177.206922015165));
#136323=CARTESIAN_POINT('Ctrl Pts',(-0.426114111673254,-71.4660826321625,
-177.349931905848));
#136324=CARTESIAN_POINT('Ctrl Pts',(-0.507344188737427,-71.4655588391503,
-177.620801033149));
#136325=CARTESIAN_POINT('Ctrl Pts',(-0.275357886911095,-71.6936685153208,
-177.231454787208));
#136326=CARTESIAN_POINT('Ctrl Pts',(-0.28195822162906,-71.4669790634829,
-177.384469640037));
#136327=CARTESIAN_POINT('Ctrl Pts',(-0.298170239974036,-71.4671552685673,
-177.662854386168));
#136328=CARTESIAN_POINT('Ctrl Pts',(-0.17210844915256,-71.7001976451323,
-177.207208612955));
#136329=CARTESIAN_POINT('Ctrl Pts',(-0.144256214768473,-71.4673303402777,
-177.351394652173));
#136330=CARTESIAN_POINT('Ctrl Pts',(-0.093404169259408,-71.4674008940711,
-177.622262820987));
#136331=CARTESIAN_POINT('',(-0.250942966392183,-71.6973964039529,-177.216474976116));
#136332=CARTESIAN_POINT('',(-0.249751305446096,-71.4669668918333,-177.637584354353));
#136333=CARTESIAN_POINT('Origin',(-0.25188593198836,-71.966962335182,-177.637584354353));
#136334=CARTESIAN_POINT('Ctrl Pts',(-0.250942967586682,-71.6973967453598,
-177.21647550955));
#136335=CARTESIAN_POINT('Ctrl Pts',(-0.272289386377385,-71.6972560147929,
-177.21651778088));
#136336=CARTESIAN_POINT('Ctrl Pts',(-0.29355234382452,-71.6975963514289,
-177.214625541668));
#136337=CARTESIAN_POINT('Ctrl Pts',(-0.314505400471286,-71.6984140417121,
-177.210861644173));
#136338=CARTESIAN_POINT('Ctrl Pts',(-0.335712123041887,-71.6992416312746,
-177.207052179459));
#136339=CARTESIAN_POINT('Ctrl Pts',(-0.356600655403705,-71.7005585587564,
-177.201326394673));
#136340=CARTESIAN_POINT('Ctrl Pts',(-0.376973851059467,-71.7023574770162,
-177.193788200059));
#136341=CARTESIAN_POINT('Ctrl Pts',(-0.397939430005541,-71.7042087017054,
-177.186030820365));
#136342=CARTESIAN_POINT('Ctrl Pts',(-0.418358881240999,-71.7065707314756,
-177.176355157432));
#136343=CARTESIAN_POINT('Ctrl Pts',(-0.438065962998032,-71.7094261265985,
-177.164899868662));
#136344=CARTESIAN_POINT('Ctrl Pts',(-0.448444784692127,-71.7109299330581,
-177.15886689021));
#136345=CARTESIAN_POINT('Ctrl Pts',(-0.458626866764958,-71.7125703880655,
-177.152340621388));
#136346=CARTESIAN_POINT('Ctrl Pts',(-0.468593349490525,-71.7143434487124,
-177.145342538011));
#136347=CARTESIAN_POINT('Ctrl Pts',(-0.482831780147209,-71.7168764989135,
-177.135344856017));
#136348=CARTESIAN_POINT('Ctrl Pts',(-0.49674155482062,-71.7197238945552,
-177.124284610517));
#136349=CARTESIAN_POINT('Ctrl Pts',(-0.510160832381796,-71.7228419069474,
-177.112294550298));
#136350=CARTESIAN_POINT('Ctrl Pts',(-0.523556614986982,-71.7259544602108,
-177.100325482711));
#136351=CARTESIAN_POINT('Ctrl Pts',(-0.536462801325541,-71.7293367437336,
-177.087430553005));
#136352=CARTESIAN_POINT('Ctrl Pts',(-0.548750322054646,-71.7329694869921,
-177.073774966279));
#136353=CARTESIAN_POINT('Ctrl Pts',(-0.552444173025322,-71.7340615553196,
-177.069669849926));
#136354=CARTESIAN_POINT('Ctrl Pts',(-0.556082376451407,-71.7351764190293,
-177.065496177473));
#136355=CARTESIAN_POINT('Ctrl Pts',(-0.559662137354108,-71.7363139575646,
-177.061258859581));
#136356=CARTESIAN_POINT('Ctrl Pts',(-0.574421398896868,-71.7410039995011,
-177.043788507593));
#136357=CARTESIAN_POINT('Ctrl Pts',(-0.588291608237107,-71.746070304877,
-177.025148207316));
#136358=CARTESIAN_POINT('Ctrl Pts',(-0.601309402288751,-71.7515531186499,
-177.005343891899));
#136359=CARTESIAN_POINT('Ctrl Pts',(-0.612473327545254,-71.7562551229153,
-176.988359916258));
#136360=CARTESIAN_POINT('Ctrl Pts',(-0.623010909387807,-71.7612627209243,
-176.97051897202));
#136361=CARTESIAN_POINT('Ctrl Pts',(-0.632942561425503,-71.7665782772395,
-176.951804930916));
#136362=CARTESIAN_POINT('Ctrl Pts',(-0.645798430805969,-71.7734589147622,
-176.927580837371));
#136363=CARTESIAN_POINT('Ctrl Pts',(-0.657488093972069,-71.7807562798892,
-176.902183776764));
#136364=CARTESIAN_POINT('Ctrl Pts',(-0.66803034729961,-71.7884603514116,
-176.875777760919));
#136365=CARTESIAN_POINT('Ctrl Pts',(-0.67883683320761,-71.7963575189103,
-176.848709900827));
#136366=CARTESIAN_POINT('Ctrl Pts',(-0.688438466109612,-71.8046821807652,
-176.820582401159));
#136367=CARTESIAN_POINT('Ctrl Pts',(-0.696894970215001,-71.8134135310904,
-176.791534794693));
#136368=CARTESIAN_POINT('Ctrl Pts',(-0.705747603657008,-71.8225538854166,
-176.761126506682));
#136369=CARTESIAN_POINT('Ctrl Pts',(-0.713346151475314,-71.8321400413436,
-176.729710293235));
#136370=CARTESIAN_POINT('Ctrl Pts',(-0.719789108725433,-71.8421351271434,
-176.69739845248));
#136371=CARTESIAN_POINT('Ctrl Pts',(-0.726420722863542,-71.8524228800694,
-176.664140485421));
#136372=CARTESIAN_POINT('Ctrl Pts',(-0.731829007749542,-71.8631438606517,
-176.629933637363));
#136373=CARTESIAN_POINT('Ctrl Pts',(-0.736138331198896,-71.8742435001081,
-176.594848190457));
#136374=CARTESIAN_POINT('Ctrl Pts',(-0.740663192872281,-71.8858983071225,
-176.55800788458));
#136375=CARTESIAN_POINT('Ctrl Pts',(-0.743977251576075,-71.8979705598559,
-176.520198759072));
#136376=CARTESIAN_POINT('Ctrl Pts',(-0.746228912135858,-71.9103817043686,
-176.481446564245));
#136377=CARTESIAN_POINT('Ctrl Pts',(-0.747198200169345,-71.9157244163533,
-176.464764636522));
#136378=CARTESIAN_POINT('Ctrl Pts',(-0.747970592530854,-71.9211297455964,
-176.447907285908));
#136379=CARTESIAN_POINT('Ctrl Pts',(-0.748557632300597,-71.9265906597324,
-176.430873773194));
#136380=CARTESIAN_POINT('Ctrl Pts',(-0.749535729765846,-71.9356893725448,
-176.402493352533));
#136381=CARTESIAN_POINT('Ctrl Pts',(-0.749999463873935,-71.9449293580282,
-176.373615401923));
#136382=CARTESIAN_POINT('Ctrl Pts',(-0.749999999535633,-71.9542570083556,
-176.344247731786));
#136383=CARTESIAN_POINT('Ctrl Pts',(-1.23940677966098,-71.4543692372681,
-176.344247731786));
#136384=CARTESIAN_POINT('Ctrl Pts',(-1.23940681800414,-71.4543692364556,
-176.64594121493));
#136385=CARTESIAN_POINT('Ctrl Pts',(-1.17782106642746,-71.4558907746468,
-176.956147992919));
#136386=CARTESIAN_POINT('Ctrl Pts',(-0.964561766455219,-71.4595630740809,
-177.27289534809));
#136387=CARTESIAN_POINT('Ctrl Pts',(-0.916284213905676,-71.4603489737626,
-177.330911863332));
#136388=CARTESIAN_POINT('Ctrl Pts',(-0.807567270427997,-71.4619509584614,
-177.435272175182));
#136389=CARTESIAN_POINT('Ctrl Pts',(-0.746244778353079,-71.4627761544078,
-177.481978941987));
#136390=CARTESIAN_POINT('Ctrl Pts',(-0.55157424298232,-71.4650436529077,
-177.595099511724));
#136391=CARTESIAN_POINT('Ctrl Pts',(-0.402234283661645,-71.4663158974755,
-177.637660247068));
#136392=CARTESIAN_POINT('Ctrl Pts',(-0.249751305446096,-71.4669668918333,
-177.637584354353));
#136393=CARTESIAN_POINT('Origin',(-26.4569673975197,-68.4857751744904,-179.64995));
#136394=CARTESIAN_POINT('',(-25.548606520418,-65.6266003779886,-171.854014632027));
#136395=CARTESIAN_POINT('',(-25.548606520496,-65.6266003779638,-176.84995));
#136396=CARTESIAN_POINT('',(-25.548606520496,-65.6266003779638,-179.64995));
#136397=CARTESIAN_POINT('',(-26.0394480946395,-65.5149709682656,-172.038055421481));
#136398=CARTESIAN_POINT('Ctrl Pts',(-26.0394480946395,-65.5149709682656,
-172.038055421481));
#136399=CARTESIAN_POINT('Ctrl Pts',(-25.8744525829839,-65.5381595751959,
-171.964276677778));
#136400=CARTESIAN_POINT('Ctrl Pts',(-25.7113823551758,-65.5748168753238,
-171.898042693471));
#136401=CARTESIAN_POINT('Ctrl Pts',(-25.5486065204936,-65.6266003779646,
-171.854014632593));
#136402=CARTESIAN_POINT('',(-26.0394480946395,-65.5149709682656,-171.64995));
#136403=CARTESIAN_POINT('',(-25.166383622031,-65.7775666303703,-177.581785882201));
#136404=CARTESIAN_POINT('',(-25.166383622031,-65.7775666303703,-179.64995));
#136405=CARTESIAN_POINT('Ctrl Pts',(-25.548606520496,-65.6266003779638,
-176.84995));
#136406=CARTESIAN_POINT('Ctrl Pts',(-25.5486064910184,-65.6266003873288,
-176.988420898571));
#136407=CARTESIAN_POINT('Ctrl Pts',(-25.5128982512925,-65.6373177084965,
-177.128208340634));
#136408=CARTESIAN_POINT('Ctrl Pts',(-25.3800542465628,-65.6848405887261,
-177.37909156612));
#136409=CARTESIAN_POINT('Ctrl Pts',(-25.2828559308331,-65.7220623109706,
-177.491403988801));
#136410=CARTESIAN_POINT('Ctrl Pts',(-25.166383622031,-65.7775666303703,
-177.581785882201));
#136411=CARTESIAN_POINT('Ctrl Pts',(-25.0407404589729,-66.228934721057,
-177.2158679411));
#136412=CARTESIAN_POINT('Ctrl Pts',(-24.9516549782085,-65.8798945343463,
-177.298823774072));
#136413=CARTESIAN_POINT('Ctrl Pts',(-25.166383622031,-65.7775666303703,
-177.581785882201));
#136414=CARTESIAN_POINT('Ctrl Pts',(-24.9465334973015,-66.3187224932389,
-177.303592864513));
#136415=CARTESIAN_POINT('Ctrl Pts',(-24.8039770572177,-65.9493003143299,
-177.391803085524));
#136416=CARTESIAN_POINT('Ctrl Pts',(-24.9795558812766,-65.8665984929838,
-177.757245548006));
#136417=CARTESIAN_POINT('Ctrl Pts',(-24.8237985595108,-66.4342348178924,
-177.34995));
#136418=CARTESIAN_POINT('Ctrl Pts',(-24.6278738771108,-66.0310529650264,
-177.399536111675));
#136419=CARTESIAN_POINT('Ctrl Pts',(-24.7362442762044,-65.9810957924573,
-177.84994999494));
#136420=CARTESIAN_POINT('Ctrl Pts',(-24.7,-66.548373473155,-177.34995));
#136421=CARTESIAN_POINT('Ctrl Pts',(-24.4906779661017,-66.0942982743998,
-177.34995));
#136422=CARTESIAN_POINT('Ctrl Pts',(-24.4906779661017,-66.0942982743997,
-177.84995));
#136423=CARTESIAN_POINT('',(-24.7,-66.5483734731532,-177.34995));
#136424=CARTESIAN_POINT('',(-24.4906779661044,-66.0942982743985,-177.84995));
#136425=CARTESIAN_POINT('Origin',(-24.7000000000027,-66.5483734731538,-177.84995));
#136426=CARTESIAN_POINT('',(-25.0407404589729,-66.228934721057,-177.2158679411));
#136427=CARTESIAN_POINT('Ctrl Pts',(-24.7,-66.5483734731532,-177.34995));
#136428=CARTESIAN_POINT('Ctrl Pts',(-24.8237985595108,-66.4342348178924,
-177.34995));
#136429=CARTESIAN_POINT('Ctrl Pts',(-24.9465334973015,-66.3187224932389,
-177.303592864513));
#136430=CARTESIAN_POINT('Ctrl Pts',(-25.0407404589729,-66.228934721057,
-177.2158679411));
#136431=CARTESIAN_POINT('Origin',(-25.3814809179458,-66.228934721057,-177.581785882201));
#136432=CARTESIAN_POINT('Ctrl Pts',(-25.166383622031,-65.7775666303703,
-177.581785882201));
#136433=CARTESIAN_POINT('Ctrl Pts',(-24.9795558812766,-65.8665984929838,
-177.757245548006));
#136434=CARTESIAN_POINT('Ctrl Pts',(-24.7362442762044,-65.9810957924573,
-177.84994999494));
#136435=CARTESIAN_POINT('Ctrl Pts',(-24.4906779661044,-66.0942982743985,
-177.84995));
#136436=CARTESIAN_POINT('Origin',(0.,-12.9675000200281,-177.84995));
#136437=CARTESIAN_POINT('Origin',(0.,-12.9675000200281,-177.34995));
#136438=CARTESIAN_POINT('Origin',(0.,-12.9675000200281,-177.84995));
#136439=CARTESIAN_POINT('Ctrl Pts',(-0.749999999999964,-72.58000002,-174.689806803097));
#136440=CARTESIAN_POINT('Ctrl Pts',(-0.749999999999964,-73.08000002,-174.689806803097));
#136441=CARTESIAN_POINT('Ctrl Pts',(-0.249999999999964,-73.08000002,-174.689806803097));
#136442=CARTESIAN_POINT('Ctrl Pts',(-0.749999999999964,-72.5800000142362,
-174.901707787501));
#136443=CARTESIAN_POINT('Ctrl Pts',(-0.749999999999999,-73.0799033011073,
-174.944063234271));
#136444=CARTESIAN_POINT('Ctrl Pts',(-0.250096721285987,-73.08000002,-174.944087763949));
#136445=CARTESIAN_POINT('Ctrl Pts',(-0.749999999999964,-72.5534802154039,
-175.109145968138));
#136446=CARTESIAN_POINT('Ctrl Pts',(-0.749999999999976,-73.047991321912,
-175.192966486363));
#136447=CARTESIAN_POINT('Ctrl Pts',(-0.25019084538922,-73.0481762528639,
-175.193013365813));
#136448=CARTESIAN_POINT('Ctrl Pts',(-0.749999999999964,-72.4491003622499,
-175.515225349862));
#136449=CARTESIAN_POINT('Ctrl Pts',(-0.749999999999953,-72.9225699879354,
-175.680169902411));
#136450=CARTESIAN_POINT('Ctrl Pts',(-0.250374112266224,-72.9229204323206,
-175.680308208816));
#136451=CARTESIAN_POINT('Ctrl Pts',(-0.749999999999965,-72.3702407172373,
-175.713745513771));
#136452=CARTESIAN_POINT('Ctrl Pts',(-0.750000000001358,-72.8278715101479,
-175.918330718485));
#136453=CARTESIAN_POINT('Ctrl Pts',(-0.250463183534996,-72.8282888567225,
-175.918532203572));
#136454=CARTESIAN_POINT('Ctrl Pts',(-0.749999999999965,-72.1685246628573,
-176.079670924798));
#136455=CARTESIAN_POINT('Ctrl Pts',(-0.749999999998571,-72.5857133666792,
-176.357282462775));
#136456=CARTESIAN_POINT('Ctrl Pts',(-0.25062659166413,-72.5862295913911,
-176.357642327882));
#136457=CARTESIAN_POINT('Ctrl Pts',(-0.749999999999965,-72.0428483696925,
-176.252247715791));
#136458=CARTESIAN_POINT('Ctrl Pts',(-0.749999999997964,-72.4348744309047,
-176.56428717754));
#136459=CARTESIAN_POINT('Ctrl Pts',(-0.250703242845797,-72.4354180409157,
-176.564734305741));
#136460=CARTESIAN_POINT('Ctrl Pts',(-0.749999999999965,-71.7551070954922,
-176.557430126179));
#136461=CARTESIAN_POINT('Ctrl Pts',(-0.750000000001966,-72.0895755229708,
-176.930319469104));
#136462=CARTESIAN_POINT('Ctrl Pts',(-0.250838284668646,-72.090128509306,
-176.930952892336));
#136463=CARTESIAN_POINT('Ctrl Pts',(-0.749999999999965,-71.5938796749303,
-176.690562238895));
#136464=CARTESIAN_POINT('Ctrl Pts',(-0.749999999997485,-71.8961205198801,
-177.08999030776));
#136465=CARTESIAN_POINT('Ctrl Pts',(-0.250896921774036,-71.8966556096658,
-177.090711302921));
#136466=CARTESIAN_POINT('Ctrl Pts',(-0.749999999999965,-71.414849447251,
-176.803618488051));
#136467=CARTESIAN_POINT('Ctrl Pts',(-0.749999999999965,-71.6813148644928,
-177.225579834422));
#136468=CARTESIAN_POINT('Ctrl Pts',(-0.250946592270043,-71.6818193327012,
-177.226378685119));
#136469=CARTESIAN_POINT('',(-0.249999999999962,-73.08000002,-174.689806803098));
#136470=CARTESIAN_POINT('Ctrl Pts',(-0.250942965994136,-71.6973962901632,
-177.216474798313));
#136471=CARTESIAN_POINT('Ctrl Pts',(-0.250894093572665,-71.906018225657,
-177.082956409594));
#136472=CARTESIAN_POINT('Ctrl Pts',(-0.250836667095525,-72.0943113105341,
-176.926516558683));
#136473=CARTESIAN_POINT('Ctrl Pts',(-0.250703261157637,-72.4354180408958,
-176.564734305724));
#136474=CARTESIAN_POINT('Ctrl Pts',(-0.250626609977381,-72.5862295913722,
-176.357642327869));
#136475=CARTESIAN_POINT('Ctrl Pts',(-0.250463201851249,-72.8282888567072,
-175.918532203564));
#136476=CARTESIAN_POINT('Ctrl Pts',(-0.250374130584112,-72.9229204323078,
-175.680308208811));
#136477=CARTESIAN_POINT('Ctrl Pts',(-0.250190863710472,-73.0481762528571,
-175.193013365811));
#136478=CARTESIAN_POINT('Ctrl Pts',(-0.250096739608965,-73.0800000199965,
-174.944087763948));
#136479=CARTESIAN_POINT('Ctrl Pts',(-0.249999999999962,-73.08000002,-174.689806803098));
#136480=CARTESIAN_POINT('',(-0.749999999999964,-72.58000002,-174.689806803098));
#136481=CARTESIAN_POINT('Origin',(-0.249999999999964,-72.58000002,-174.689806803098));
#136482=CARTESIAN_POINT('Ctrl Pts',(-0.749999999999964,-72.58000002,-174.689806803098));
#136483=CARTESIAN_POINT('Ctrl Pts',(-0.749999999999964,-72.58000002,-174.831376286945));
#136484=CARTESIAN_POINT('Ctrl Pts',(-0.750000000181377,-72.5681788618565,
-174.970941599173));
#136485=CARTESIAN_POINT('Ctrl Pts',(-0.749999999141365,-72.5447649315039,
-175.108599805088));
#136486=CARTESIAN_POINT('Ctrl Pts',(-0.749999998625103,-72.5331422713358,
-175.176933251143));
#136487=CARTESIAN_POINT('Ctrl Pts',(-0.749999997778457,-72.5186622030691,
-175.244796569616));
#136488=CARTESIAN_POINT('Ctrl Pts',(-0.749999996441189,-72.501348066122,
-175.312200510247));
#136489=CARTESIAN_POINT('Ctrl Pts',(-0.749999994685787,-72.4786201957877,
-175.400680116672));
#136490=CARTESIAN_POINT('Ctrl Pts',(-0.749999992058193,-72.4508191867992,
-175.488345833607));
#136491=CARTESIAN_POINT('Ctrl Pts',(-0.749999988588697,-72.4183069147095,
-175.574298130555));
#136492=CARTESIAN_POINT('Ctrl Pts',(-0.749999986546665,-72.3991712571468,
-175.624886834925));
#136493=CARTESIAN_POINT('Ctrl Pts',(-0.749999987460588,-72.3784930875005,
-175.674621364586));
#136494=CARTESIAN_POINT('Ctrl Pts',(-0.749999990785369,-72.3562980983182,
-175.723514264023));
#136495=CARTESIAN_POINT('Ctrl Pts',(-0.749999992115961,-72.347415567763,
-175.7430814136));
#136496=CARTESIAN_POINT('Ctrl Pts',(-0.749999993758535,-72.3382895360997,
-175.762513592358));
#136497=CARTESIAN_POINT('Ctrl Pts',(-0.749999995341683,-72.3289194940821,
-175.781810711456));
#136498=CARTESIAN_POINT('Ctrl Pts',(-0.749999998527987,-72.3100609827057,
-175.820648844665));
#136499=CARTESIAN_POINT('Ctrl Pts',(-0.749999999364237,-72.2901904086323,
-175.8590152493));
#136500=CARTESIAN_POINT('Ctrl Pts',(-0.749999999592108,-72.2694003762988,
-175.896717968815));
#136501=CARTESIAN_POINT('Ctrl Pts',(-0.749999999760363,-72.2540495109209,
-175.924556760134));
#136502=CARTESIAN_POINT('Ctrl Pts',(-0.749999999832536,-72.2381324361931,
-175.952153763115));
#136503=CARTESIAN_POINT('Ctrl Pts',(-0.749999998887563,-72.22169996255,
-175.979441154676));
#136504=CARTESIAN_POINT('Ctrl Pts',(-0.749999996495687,-72.1801067750961,
-176.048509854675));
#136505=CARTESIAN_POINT('Ctrl Pts',(-0.749999993208358,-72.1348499287488,
-176.116013152087));
#136506=CARTESIAN_POINT('Ctrl Pts',(-0.749999994093549,-72.0863465370676,
-176.181265394643));
#136507=CARTESIAN_POINT('Ctrl Pts',(-0.749999994855056,-72.0446203524745,
-176.237400172514));
#136508=CARTESIAN_POINT('Ctrl Pts',(-0.749999998190332,-72.0004927389796,
-176.291868658539));
#136509=CARTESIAN_POINT('Ctrl Pts',(-0.749999999535633,-71.9542570083556,
-176.344247731786));
#136510=CARTESIAN_POINT('Origin',(-0.249999999999964,-72.58000002,-55.24995));
#136511=CARTESIAN_POINT('',(-0.249999999999964,-73.08000002,-57.9657868813819));
#136512=CARTESIAN_POINT('',(-0.249999999999964,-73.08000002,-57.9678366169137));
#136513=CARTESIAN_POINT('',(-0.749999999999964,-72.58000002,-57.9657868813819));
#136514=CARTESIAN_POINT('Origin',(-0.249999999999964,-72.58000002,-57.9657868813819));
#136515=CARTESIAN_POINT('',(-0.749999999999964,-72.58000002,-174.687529226493));
#136516=CARTESIAN_POINT('Ctrl Pts',(-0.249999999999964,-73.08000002,-57.9657868813819));
#136517=CARTESIAN_POINT('Ctrl Pts',(-0.749999999999964,-73.08000002,-57.9657868813819));
#136518=CARTESIAN_POINT('Ctrl Pts',(-0.749999999999964,-72.58000002,-57.9657868813819));
#136519=CARTESIAN_POINT('Ctrl Pts',(-0.250090304006367,-73.08000002,-57.7020110302663));
#136520=CARTESIAN_POINT('Ctrl Pts',(-0.749999999999964,-73.0799097169388,
-57.7020347823602));
#136521=CARTESIAN_POINT('Ctrl Pts',(-0.749999999999964,-72.5800000140225,
-57.7459735178474));
#136522=CARTESIAN_POINT('Ctrl Pts',(-0.250178150913126,-73.0457949912512,
-57.4439860415223));
#136523=CARTESIAN_POINT('Ctrl Pts',(-0.749999999999964,-73.0456227684187,
-57.4440313928443));
#136524=CARTESIAN_POINT('Ctrl Pts',(-0.749999999999964,-72.5514958309333,
-57.5309525432158));
#136525=CARTESIAN_POINT('Ctrl Pts',(-0.250306370454135,-72.9447005728246,
-57.0654831530319));
#136526=CARTESIAN_POINT('Ctrl Pts',(-0.749999999999965,-72.9444091558477,
-57.0655786327141));
#136527=CARTESIAN_POINT('Ctrl Pts',(-0.749999999999964,-72.4672504799085,
-57.2155332517716));
#136528=CARTESIAN_POINT('Ctrl Pts',(-0.25034879630597,-72.9021819864826,
-56.9399108365871));
#136529=CARTESIAN_POINT('Ctrl Pts',(-0.749999999999971,-72.9018554492066,
-56.9400333127282));
#136530=CARTESIAN_POINT('Ctrl Pts',(-0.749999999999964,-72.4318183244811,
-57.1108895827629));
#136531=CARTESIAN_POINT('Ctrl Pts',(-0.250430320614374,-72.8021179994285,
-56.6980298209841));
#136532=CARTESIAN_POINT('Ctrl Pts',(-0.749999999999958,-72.8017292323873,
-56.6982147960383));
#136533=CARTESIAN_POINT('Ctrl Pts',(-0.749999999999964,-72.3484316704448,
-56.9093219305338));
#136534=CARTESIAN_POINT('Ctrl Pts',(-0.250469580226035,-72.744578160532,
-56.5812500750007));
#136535=CARTESIAN_POINT('Ctrl Pts',(-0.74999999999997,-72.7441631076294,
-56.581469426742));
#136536=CARTESIAN_POINT('Ctrl Pts',(-0.749999999999965,-72.300481803901,
-56.8120054092621));
#136537=CARTESIAN_POINT('Ctrl Pts',(-0.250582991914968,-72.5498603521484,
-56.2431574556907));
#136538=CARTESIAN_POINT('Ctrl Pts',(-0.749999999999952,-72.5493874743356,
-56.2435031793822));
#136539=CARTESIAN_POINT('Ctrl Pts',(-0.749999999999965,-72.1382169632082,
-56.5302613678863));
#136540=CARTESIAN_POINT('Ctrl Pts',(-0.250653625589273,-72.3879279481205,
-56.0315291953545));
#136541=CARTESIAN_POINT('Ctrl Pts',(-0.749999999999435,-72.3874332788213,
-56.0319576106046));
#136542=CARTESIAN_POINT('Ctrl Pts',(-0.749999999999965,-72.0032732927043,
-56.3539043654751));
#136543=CARTESIAN_POINT('Ctrl Pts',(-0.250776334581247,-72.0199436379809,
-55.6626353009023));
#136544=CARTESIAN_POINT('Ctrl Pts',(-0.750000000000494,-72.0194499168863,
-55.6632379181992));
#136545=CARTESIAN_POINT('Ctrl Pts',(-0.749999999999965,-71.6966197023802,
-56.0464925782632));
#136546=CARTESIAN_POINT('Ctrl Pts',(-0.250829232083772,-71.8132859417639,
-55.5029329728744));
#136547=CARTESIAN_POINT('Ctrl Pts',(-0.749999999997384,-71.8128142650138,
-55.5036164406727));
#136548=CARTESIAN_POINT('Ctrl Pts',(-0.749999999999965,-71.5244049571092,
-55.9134072123415));
#136549=CARTESIAN_POINT('Ctrl Pts',(-0.250873059487692,-71.5845312649516,
-55.3703284570208));
#136550=CARTESIAN_POINT('Ctrl Pts',(-0.749999999999965,-71.5840941797283,
-55.3710824677091));
#136551=CARTESIAN_POINT('Ctrl Pts',(-0.749999999999965,-71.3337760574596,
-55.8029033796444));
#136552=CARTESIAN_POINT('Ctrl Pts',(-0.749999999999965,-71.8417319269067,
-56.1920012792715));
#136553=CARTESIAN_POINT('Ctrl Pts',(-0.749999999999965,-71.8444758759865,
-56.1947266143563));
#136554=CARTESIAN_POINT('Ctrl Pts',(-0.749999999999854,-71.8472142189877,
-56.1974588803415));
#136555=CARTESIAN_POINT('Ctrl Pts',(-0.749999999999599,-71.849946925556,
-56.200198044911));
#136556=CARTESIAN_POINT('Ctrl Pts',(-0.749999999995322,-71.895797123968,
-56.246156597672));
#136557=CARTESIAN_POINT('Ctrl Pts',(-0.750000000361229,-71.9401028597185,
-56.2942420626362));
#136558=CARTESIAN_POINT('Ctrl Pts',(-0.74999999895657,-71.982527737009,
-56.344035893725));
#136559=CARTESIAN_POINT('Ctrl Pts',(-0.749999998672542,-71.9911062235921,
-56.3541044134048));
#136560=CARTESIAN_POINT('Ctrl Pts',(-0.749999998292393,-71.999607928201,
-56.3642426607214));
#136561=CARTESIAN_POINT('Ctrl Pts',(-0.749999997746176,-72.0080302616703,
-56.3744470046658));
#136562=CARTESIAN_POINT('Ctrl Pts',(-0.74999999604191,-72.0343090036282,
-56.4062858439066));
#136563=CARTESIAN_POINT('Ctrl Pts',(-0.749999992814762,-72.0598149071135,
-56.4387765753063));
#136564=CARTESIAN_POINT('Ctrl Pts',(-0.749999990764931,-72.0844669777911,
-56.471823595159));
#136565=CARTESIAN_POINT('Ctrl Pts',(-0.7499999887151,-72.1091190484687,
-56.5048706150117));
#136566=CARTESIAN_POINT('Ctrl Pts',(-0.74999998878556,-72.1329172515315,
-56.5384738714876));
#136567=CARTESIAN_POINT('Ctrl Pts',(-0.749999992523647,-72.1557838559918,
-56.5725357961293));
#136568=CARTESIAN_POINT('Ctrl Pts',(-0.749999997741391,-72.1877018007307,
-56.6200805302109));
#136569=CARTESIAN_POINT('Ctrl Pts',(-0.749999998819484,-72.2179714721241,
-56.6686674551481));
#136570=CARTESIAN_POINT('Ctrl Pts',(-0.749999999429074,-72.2464142286222,
-56.7180788042009));
#136571=CARTESIAN_POINT('Ctrl Pts',(-0.750000000419556,-72.2926289656521,
-56.7983640080249));
#136572=CARTESIAN_POINT('Ctrl Pts',(-0.749999999999578,-72.3344223494509,
-56.8812169184746));
#136573=CARTESIAN_POINT('Ctrl Pts',(-0.749999999999555,-72.3716419026398,
-56.9665912683841));
#136574=CARTESIAN_POINT('Ctrl Pts',(-0.749999999999551,-72.3771587620856,
-56.9792458611551));
#136575=CARTESIAN_POINT('Ctrl Pts',(-0.749999999999476,-72.382575206817,
-56.991955795638));
#136576=CARTESIAN_POINT('Ctrl Pts',(-0.749999999999378,-72.3878908196251,
-57.0047208623372));
#136577=CARTESIAN_POINT('Ctrl Pts',(-0.749999999999364,-72.3886377760633,
-57.0065146251825));
#136578=CARTESIAN_POINT('Ctrl Pts',(-0.749999999999346,-72.389382748593,
-57.0083094879105));
#136579=CARTESIAN_POINT('Ctrl Pts',(-0.749999999999324,-72.3901257364801,
-57.0101054509239));
#136580=CARTESIAN_POINT('Ctrl Pts',(-0.749999999998099,-72.4318199510488,
-57.1108894186501));
#136581=CARTESIAN_POINT('Ctrl Pts',(-0.749999999915445,-72.4672597866091,
-57.2155313871763));
#136582=CARTESIAN_POINT('Ctrl Pts',(-0.749999999861768,-72.4953436211357,
-57.3206699820974));
#136583=CARTESIAN_POINT('Ctrl Pts',(-0.749999999835408,-72.5091351036103,
-57.3723017166415));
#136584=CARTESIAN_POINT('Ctrl Pts',(-0.749999999849788,-72.5212576085903,
-57.4242193465116));
#136585=CARTESIAN_POINT('Ctrl Pts',(-0.749999999908996,-72.53169711994,
-57.4764233217448));
#136586=CARTESIAN_POINT('Ctrl Pts',(-0.75000000009092,-72.5637736078163,
-57.6368254825897));
#136587=CARTESIAN_POINT('Ctrl Pts',(-0.749999999999964,-72.58000002,-57.7999242188348));
#136588=CARTESIAN_POINT('Ctrl Pts',(-0.749999999999964,-72.58000002,-57.9657868813819));
#136589=CARTESIAN_POINT('Ctrl Pts',(-0.249999999999964,-73.08000002,-57.9657868813819));
#136590=CARTESIAN_POINT('Ctrl Pts',(-0.250090304006367,-73.08000002,-57.7020110302663));
#136591=CARTESIAN_POINT('Ctrl Pts',(-0.250178150913126,-73.0457949912512,
-57.4439860415223));
#136592=CARTESIAN_POINT('Ctrl Pts',(-0.250306370454135,-72.9447005728246,
-57.0654831530319));
#136593=CARTESIAN_POINT('Ctrl Pts',(-0.25034879630597,-72.9021819864826,
-56.9399108365871));
#136594=CARTESIAN_POINT('Ctrl Pts',(-0.250430320614374,-72.8021179994285,
-56.6980298209841));
#136595=CARTESIAN_POINT('Ctrl Pts',(-0.250469580226035,-72.744578160532,
-56.5812500750007));
#136596=CARTESIAN_POINT('Ctrl Pts',(-0.250582991914968,-72.5498603521484,
-56.2431574556907));
#136597=CARTESIAN_POINT('Ctrl Pts',(-0.250653625589273,-72.3879279481205,
-56.0315291953545));
#136598=CARTESIAN_POINT('Ctrl Pts',(-0.250774861685046,-72.0243606141434,
-55.6670631949548));
#136599=CARTESIAN_POINT('Ctrl Pts',(-0.250826687460303,-71.8231950647151,
-55.5106149664713));
#136600=CARTESIAN_POINT('Ctrl Pts',(-0.250869887203096,-71.6009673739964,
-55.3799259279342));
#136601=CARTESIAN_POINT('Ctrl Pts',(-1.24035792914739,-71.2481103336038,
-60.8508735991007));
#136602=CARTESIAN_POINT('Ctrl Pts',(-0.749999999999965,-71.2566817467534,
-60.8548714197835));
#136603=CARTESIAN_POINT('Ctrl Pts',(-0.749999999999965,-71.701161634982,
-61.0621827299711));
#136604=CARTESIAN_POINT('Ctrl Pts',(-1.23971725581624,-71.3097847042778,
-60.7186716617645));
#136605=CARTESIAN_POINT('Ctrl Pts',(-0.74999999999993,-71.3194598672011,
-60.7217601410269));
#136606=CARTESIAN_POINT('Ctrl Pts',(-0.749999999999965,-71.7936527766986,
-60.8638797025928));
#136607=CARTESIAN_POINT('Ctrl Pts',(-1.23938654221847,-71.3418443611191,
-60.5756111021815));
#136608=CARTESIAN_POINT('Ctrl Pts',(-0.749999999999964,-71.3522348667501,
-60.5771488614746));
#136609=CARTESIAN_POINT('Ctrl Pts',(-0.749999999999965,-71.8417316989903,
-60.6492890757558));
#136610=CARTESIAN_POINT('Ctrl Pts',(-1.2393865421354,-71.3418443611208,
-60.42825533736));
#136611=CARTESIAN_POINT('Ctrl Pts',(-0.749999999999964,-71.3522348691612,
-60.4282553373599));
#136612=CARTESIAN_POINT('Ctrl Pts',(-0.749999999999965,-71.8417317029411,
-60.42825533736));
#136613=CARTESIAN_POINT('',(-0.749999999999965,-71.701161634982,-61.0621827299711));
#136614=CARTESIAN_POINT('Origin',(-1.24999999999996,-71.701161634982,-61.0621827299711));
#136615=CARTESIAN_POINT('Origin',(-0.749999999999965,-69.6146150315905,
-60.2676349698354));
#136616=CARTESIAN_POINT('Origin',(-0.750000000000035,67.7009572055632,-55.24995));
#136617=CARTESIAN_POINT('',(-0.749999999999973,-55.5033748716332,-95.7875912885257));
#136618=CARTESIAN_POINT('Ctrl Pts',(-0.749999999999971,-55.5033748716332,
-95.7875912885257));
#136619=CARTESIAN_POINT('Ctrl Pts',(-0.749999999999969,-60.9031648374056,
-84.2127012585751));
#136620=CARTESIAN_POINT('Ctrl Pts',(-0.749999999999967,-66.3022815738571,
-72.6374971882577));
#136621=CARTESIAN_POINT('Ctrl Pts',(-0.749999999999965,-71.701161634982,
-61.062182729971));
#136622=CARTESIAN_POINT('',(-0.749999999999973,-55.08000002,-97.6965903014517));
#136623=CARTESIAN_POINT('Origin',(-0.749999999999973,-61.7707294446428,
-98.17800342417));
#136624=CARTESIAN_POINT('',(-0.749999999999973,-55.08000002,-134.362052670054));
#136625=CARTESIAN_POINT('',(-0.749999999999973,-55.08000002,-97.7195882395211));
#136626=CARTESIAN_POINT('',(-0.749999999999973,-55.5033748716332,-136.27105168298));
#136627=CARTESIAN_POINT('Origin',(-0.749999999999977,-61.7710312680802,
-133.877753475464));
#136628=CARTESIAN_POINT('',(-0.749999999999965,-71.813687061541,-171.237717270032));
#136629=CARTESIAN_POINT('Ctrl Pts',(-0.749999999999965,-71.813687061541,
-171.237717270032));
#136630=CARTESIAN_POINT('Ctrl Pts',(-0.749999999999967,-66.3773023734559,
-159.58198200727));
#136631=CARTESIAN_POINT('Ctrl Pts',(-0.74999999999997,-60.9406796476674,
-147.926357767621));
#136632=CARTESIAN_POINT('Ctrl Pts',(-0.749999999999973,-55.5033748716332,
-136.27105168298));
#136633=CARTESIAN_POINT('Origin',(-0.749999999999965,-69.7273331732481,
-172.033160909053));
#136634=CARTESIAN_POINT('Origin',(0.,-12.9675000200281,-60.64995));
#136635=CARTESIAN_POINT('',(-1.23668888567854,-55.0504149642627,-95.576281431058));
#136636=CARTESIAN_POINT('',(-6.82752391182554,-55.1067946037879,-94.3158809919512));
#136637=CARTESIAN_POINT('Ctrl Pts',(-1.23668874794468,-55.0504102916018,
-95.5762792512635));
#136638=CARTESIAN_POINT('Ctrl Pts',(-2.16407513351987,-55.0533526605647,
-95.5113527668491));
#136639=CARTESIAN_POINT('Ctrl Pts',(-3.10799502527407,-55.0597210848585,
-95.3707630380922));
#136640=CARTESIAN_POINT('Ctrl Pts',(-4.02669441069485,-55.0690422663978,
-95.16328981846));
#136641=CARTESIAN_POINT('Ctrl Pts',(-4.98118226589344,-55.0787265599944,
-94.9477343586866));
#136642=CARTESIAN_POINT('Ctrl Pts',(-5.91348766496874,-55.0915160415816,
-94.6617302601372));
#136643=CARTESIAN_POINT('Ctrl Pts',(-6.82752392642188,-55.1067946087991,
-94.3158810345077));
#136644=CARTESIAN_POINT('Ctrl Pts',(-1.24035792914739,-71.2481103336038,
-60.8508735991007));
#136645=CARTESIAN_POINT('Ctrl Pts',(-1.24033480878609,-71.1072117831156,
-61.1529641634137));
#136646=CARTESIAN_POINT('Ctrl Pts',(-1.24031152212174,-70.9663130484708,
-61.4550546418214));
#136647=CARTESIAN_POINT('Ctrl Pts',(-1.24019423907957,-70.2618184344542,
-62.9655065950025));
#136648=CARTESIAN_POINT('Ctrl Pts',(-1.2400976958218,-69.6982197351968,
-64.1738667543558));
#136649=CARTESIAN_POINT('Ctrl Pts',(-1.23999818500278,-69.1346177525067,
-65.3822253820002));
#136650=CARTESIAN_POINT('Ctrl Pts',(-1.23960014172664,-66.8802098214716,
-70.2156598931668));
#136651=CARTESIAN_POINT('Ctrl Pts',(-1.23915545083688,-64.6257502610154,
-75.0490703206921));
#136652=CARTESIAN_POINT('Ctrl Pts',(-1.23864216610312,-62.3712150282457,
-79.8824454429464));
#136653=CARTESIAN_POINT('Ctrl Pts',(-1.23808662039688,-59.9310540692955,
-85.1137734354556));
#136654=CARTESIAN_POINT('Ctrl Pts',(-1.23745196892516,-57.4908058054248,
-90.3450606997508));
#136655=CARTESIAN_POINT('Ctrl Pts',(-1.23668893165476,-55.0504165218147,
-95.5762821576554));
#136656=CARTESIAN_POINT('Ctrl Pts',(-6.82752390105444,-55.106794611208,
-94.3158809605474));
#136657=CARTESIAN_POINT('Ctrl Pts',(-6.83625690025051,-60.3715570323219,
-83.1679040708394));
#136658=CARTESIAN_POINT('Ctrl Pts',(-6.84206094040904,-65.61805576689,-72.0110063808198));
#136659=CARTESIAN_POINT('Ctrl Pts',(-6.84677576889373,-70.8578246683297,
-60.8508735991007));
#136660=CARTESIAN_POINT('Ctrl Pts',(-6.84141371258755,-70.9528017323285,
-60.42825533736));
#136661=CARTESIAN_POINT('Ctrl Pts',(-7.39999999999997,-70.886896756869,
-60.42825533736));
#136662=CARTESIAN_POINT('Ctrl Pts',(-7.4,-71.449357516634,-60.42825533736));
#136663=CARTESIAN_POINT('Ctrl Pts',(-6.84141371452047,-70.9528017321005,
-60.574175588166));
#136664=CARTESIAN_POINT('Ctrl Pts',(-7.39999999999996,-70.8868967471692,
-60.5644399462782));
#136665=CARTESIAN_POINT('Ctrl Pts',(-7.4,-71.4493574998816,-60.6471383113761));
#136666=CARTESIAN_POINT('Ctrl Pts',(-6.84320633698782,-70.9209010052172,
-60.7174412822399));
#136667=CARTESIAN_POINT('Ctrl Pts',(-7.39999999999997,-70.85979500338,-60.6978441698658));
#136668=CARTESIAN_POINT('Ctrl Pts',(-7.4,-71.4018249198588,-60.8620307958147));
#136669=CARTESIAN_POINT('Ctrl Pts',(-6.84677576889373,-70.8578246683297,
-60.8508735991007));
#136670=CARTESIAN_POINT('Ctrl Pts',(-7.39999999999996,-70.8042142666047,
-60.8257004209668));
#136671=CARTESIAN_POINT('Ctrl Pts',(-7.4,-71.3078420373655,-61.0621827299711));
#136672=CARTESIAN_POINT('',(-7.4,-71.3078420373655,-61.0621827299711));
#136673=CARTESIAN_POINT('Origin',(-6.9,-71.3078420373655,-61.0621827299711));
#136674=CARTESIAN_POINT('Origin',(-7.4,-69.2744516168521,-60.2813964156253));
#136675=CARTESIAN_POINT('Origin',(-7.4,67.7009572055632,-55.24995));
#136676=CARTESIAN_POINT('',(-7.4,-72.58000002,-58.1594740865074));
#136677=CARTESIAN_POINT('Ctrl Pts',(-7.4,-72.58000002,-58.1594740865074));
#136678=CARTESIAN_POINT('Ctrl Pts',(-7.4,-72.58000002,-58.0551776270551));
#136679=CARTESIAN_POINT('Ctrl Pts',(-7.4,-72.5736287847411,-57.9519715312753));
#136680=CARTESIAN_POINT('Ctrl Pts',(-7.4,-72.5609286762394,-57.8498358231105));
#136681=CARTESIAN_POINT('Ctrl Pts',(-7.4,-72.5482285677376,-57.7477001149457));
#136682=CARTESIAN_POINT('Ctrl Pts',(-7.39999999935597,-72.529198463361,
-57.6466357793308));
#136683=CARTESIAN_POINT('Ctrl Pts',(-7.40000000064314,-72.5039045953935,
-57.5466462680235));
#136684=CARTESIAN_POINT('Ctrl Pts',(-7.40000000122792,-72.4924131270627,
-57.5012191983453));
#136685=CARTESIAN_POINT('Ctrl Pts',(-7.40000000179748,-72.4796171505751,
-57.4560136230692));
#136686=CARTESIAN_POINT('Ctrl Pts',(-7.40000000193861,-72.4655224562879,
-57.4110306599075));
#136687=CARTESIAN_POINT('Ctrl Pts',(-7.40000000231984,-72.4274510918893,
-57.2895265855827));
#136688=CARTESIAN_POINT('Ctrl Pts',(-7.4000000004226,-72.3798384459848,
-57.1705512406855));
#136689=CARTESIAN_POINT('Ctrl Pts',(-7.40000000013593,-72.3241837880397,
-57.0571398660674));
#136690=CARTESIAN_POINT('Ctrl Pts',(-7.40000000006153,-72.3097383663643,
-57.0277034237349));
#136691=CARTESIAN_POINT('Ctrl Pts',(-7.40000000003645,-72.2947325387355,
-56.9985778271777));
#136692=CARTESIAN_POINT('Ctrl Pts',(-7.40000000002765,-72.279165204543,
-56.9697637092871));
#136693=CARTESIAN_POINT('Ctrl Pts',(-7.40000000000257,-72.2347715487634,
-56.8875939546328));
#136694=CARTESIAN_POINT('Ctrl Pts',(-7.40000000007907,-72.1857795264399,
-56.8079051030792));
#136695=CARTESIAN_POINT('Ctrl Pts',(-7.40000000044821,-72.1321711779398,
-56.7307944085666));
#136696=CARTESIAN_POINT('Ctrl Pts',(-7.40000000085049,-72.0737492661558,
-56.6467598445767));
#136697=CARTESIAN_POINT('Ctrl Pts',(-7.40000000144702,-72.0094938737877,
-56.565563603203));
#136698=CARTESIAN_POINT('Ctrl Pts',(-7.40000000089367,-71.9411026567194,
-56.4892360541678));
#136699=CARTESIAN_POINT('Ctrl Pts',(-7.40000000083676,-71.9340690507491,
-56.481386246435));
#136700=CARTESIAN_POINT('Ctrl Pts',(-7.40000000077119,-71.926991725805,
-56.4735878952515));
#136701=CARTESIAN_POINT('Ctrl Pts',(-7.4000000007,-71.9198725431757,-56.465843179204));
#136702=CARTESIAN_POINT('Ctrl Pts',(-7.40000000060499,-71.9103706657815,
-56.4555064107617));
#136703=CARTESIAN_POINT('Ctrl Pts',(-7.40000000052617,-71.9007927917902,
-56.4452629042245));
#136704=CARTESIAN_POINT('Ctrl Pts',(-7.40000000046129,-71.8911429761284,
-56.4351175107121));
#136705=CARTESIAN_POINT('Ctrl Pts',(-7.39999999996768,-71.8177272070187,
-56.3579313867758));
#136706=CARTESIAN_POINT('Ctrl Pts',(-7.39999999939412,-71.7397944141598,
-56.2857954012954));
#136707=CARTESIAN_POINT('Ctrl Pts',(-7.40000000114364,-71.6572752456072,
-56.2186315211966));
#136708=CARTESIAN_POINT('Ctrl Pts',(-7.40000000147217,-71.641779599927,
-56.2060193280932));
#136709=CARTESIAN_POINT('Ctrl Pts',(-7.40000000193345,-71.6261221119207,
-56.1935825531791));
#136710=CARTESIAN_POINT('Ctrl Pts',(-7.40000000264863,-71.6103021593138,
-56.1813208069962));
#136711=CARTESIAN_POINT('Ctrl Pts',(-7.40000000499281,-71.558447829008,
-56.1411294959033));
#136712=CARTESIAN_POINT('Ctrl Pts',(-7.40000000927177,-71.5046891439978,
-56.1028356287387));
#136713=CARTESIAN_POINT('Ctrl Pts',(-7.40000002552836,-71.4493575166296,
-56.0666111687568));
#136714=CARTESIAN_POINT('',(-7.4,-72.58000002,-174.471034982976));
#136715=CARTESIAN_POINT('',(-7.4,-72.58000002,-58.1419820049528));
#136716=CARTESIAN_POINT('Ctrl Pts',(-7.40000000575672,-71.5626363369612,
-176.485569595296));
#136717=CARTESIAN_POINT('Ctrl Pts',(-7.39999999964314,-71.5963334703268,
-176.460729295267));
#136718=CARTESIAN_POINT('Ctrl Pts',(-7.40000000050213,-71.6293602055438,
-176.435105116127));
#136719=CARTESIAN_POINT('Ctrl Pts',(-7.40000000080687,-71.6616524595397,
-176.408710325206));
#136720=CARTESIAN_POINT('Ctrl Pts',(-7.40000000085713,-71.6669782225453,
-176.404357194544));
#136721=CARTESIAN_POINT('Ctrl Pts',(-7.40000000093686,-71.6722864874059,
-176.399982537289));
#136722=CARTESIAN_POINT('Ctrl Pts',(-7.40000000105475,-71.6775773354997,
-176.395586157876));
#136723=CARTESIAN_POINT('Ctrl Pts',(-7.40000000288459,-71.7597041196625,
-176.327343695267));
#136724=CARTESIAN_POINT('Ctrl Pts',(-7.40000000086288,-71.8372393620123,
-176.253983607122));
#136725=CARTESIAN_POINT('Ctrl Pts',(-7.40000000055521,-71.9102228395748,
-176.175469994329));
#136726=CARTESIAN_POINT('Ctrl Pts',(-7.40000000052935,-71.916356742894,
-176.168871310268));
#136727=CARTESIAN_POINT('Ctrl Pts',(-7.40000000051231,-71.9224585008182,
-176.162236193811));
#136728=CARTESIAN_POINT('Ctrl Pts',(-7.40000000050508,-71.9285281400417,
-176.15556460665));
#136729=CARTESIAN_POINT('Ctrl Pts',(-7.40000000048088,-71.9488281698803,
-176.133251349886));
#136730=CARTESIAN_POINT('Ctrl Pts',(-7.4000000005302,-71.9687792955913,
-176.110498872159));
#136731=CARTESIAN_POINT('Ctrl Pts',(-7.40000000090086,-71.9883433756989,
-176.087359845977));
#136732=CARTESIAN_POINT('Ctrl Pts',(-7.40000000204431,-72.0486965657351,
-176.01597831223));
#136733=CARTESIAN_POINT('Ctrl Pts',(-7.40000000174205,-72.1052822109679,
-175.940916275219));
#136734=CARTESIAN_POINT('Ctrl Pts',(-7.40000000104438,-72.1569369843104,
-175.863739490819));
#136735=CARTESIAN_POINT('Ctrl Pts',(-7.40000000027758,-72.2137093550038,
-175.778916564894));
#136736=CARTESIAN_POINT('Ctrl Pts',(-7.39999999999849,-72.2650200455803,
-175.691076839899));
#136737=CARTESIAN_POINT('Ctrl Pts',(-7.40000000003311,-72.3109220293856,
-175.600232860702));
#136738=CARTESIAN_POINT('Ctrl Pts',(-7.4000000000402,-72.3203292671906,
-175.5816151269));
#136739=CARTESIAN_POINT('Ctrl Pts',(-7.40000000005342,-72.3295088745487,
-175.562871130851));
#136740=CARTESIAN_POINT('Ctrl Pts',(-7.40000000007737,-72.3384609015072,
-175.544000911756));
#136741=CARTESIAN_POINT('Ctrl Pts',(-7.40000000021819,-72.3910932309574,
-175.433055804823));
#136742=CARTESIAN_POINT('Ctrl Pts',(-7.4000000012263,-72.436127459958,-175.316747505601));
#136743=CARTESIAN_POINT('Ctrl Pts',(-7.40000000110901,-72.4720179137164,
-175.198544593051));
#136744=CARTESIAN_POINT('Ctrl Pts',(-7.40000000106035,-72.4869106518372,
-175.14949631315));
#136745=CARTESIAN_POINT('Ctrl Pts',(-7.40000000071105,-72.5002693294562,
-175.100185099317));
#136746=CARTESIAN_POINT('Ctrl Pts',(-7.4000000003472,-72.5120857612517,
-175.050611983827));
#136747=CARTESIAN_POINT('Ctrl Pts',(-7.39999999965227,-72.534654114155,
-174.955931662031));
#136748=CARTESIAN_POINT('Ctrl Pts',(-7.4,-72.5516373021817,-174.860293425931));
#136749=CARTESIAN_POINT('Ctrl Pts',(-7.4,-72.5629735391251,-174.763699740561));
#136750=CARTESIAN_POINT('Ctrl Pts',(-7.4,-72.5743097760684,-174.667106055192));
#136751=CARTESIAN_POINT('Ctrl Pts',(-7.4,-72.58000002,-174.569557605373));
#136752=CARTESIAN_POINT('Ctrl Pts',(-7.4,-72.58000002,-174.471034982976));
#136753=CARTESIAN_POINT('',(-7.4,-71.4211246238516,-171.237717270032));
#136754=CARTESIAN_POINT('Origin',(-7.4,-69.3873379576789,-172.017654079519));
#136755=CARTESIAN_POINT('',(-7.4,-55.5541151520872,-137.531452880088));
#136756=CARTESIAN_POINT('Ctrl Pts',(-7.4,-55.5541151520872,-137.531452880088));
#136757=CARTESIAN_POINT('Ctrl Pts',(-7.4,-60.858236996045,-148.759754479668));
#136758=CARTESIAN_POINT('Ctrl Pts',(-7.4,-66.1431501582269,-159.997106821727));
#136759=CARTESIAN_POINT('Ctrl Pts',(-7.4,-71.4211246238516,-171.237717270032));
#136760=CARTESIAN_POINT('',(-7.4,-55.08000002,-135.415380765739));
#136761=CARTESIAN_POINT('Ctrl Pts',(-7.4,-55.08000002,-135.415380765739));
#136762=CARTESIAN_POINT('Ctrl Pts',(-7.4,-55.08000002,-135.642528198476));
#136763=CARTESIAN_POINT('Ctrl Pts',(-7.4,-55.0958102967125,-135.869567477787));
#136764=CARTESIAN_POINT('Ctrl Pts',(-7.4,-55.1266901212419,-136.093433076237));
#136765=CARTESIAN_POINT('Ctrl Pts',(-7.4,-55.1457148268974,-136.231354103373));
#136766=CARTESIAN_POINT('Ctrl Pts',(-7.4,-55.170458313014,-136.368070310456));
#136767=CARTESIAN_POINT('Ctrl Pts',(-7.4,-55.2007376448274,-136.502866089854));
#136768=CARTESIAN_POINT('Ctrl Pts',(-7.4,-55.2691608068266,-136.807468367981));
#136769=CARTESIAN_POINT('Ctrl Pts',(-7.4,-55.3655723350956,-137.104245532218));
#136770=CARTESIAN_POINT('Ctrl Pts',(-7.4,-55.4912205286389,-137.392848584318));
#136771=CARTESIAN_POINT('Ctrl Pts',(-7.4,-55.511427368581,-137.439261951006));
#136772=CARTESIAN_POINT('Ctrl Pts',(-7.4,-55.5323904712551,-137.485463878382));
#136773=CARTESIAN_POINT('Ctrl Pts',(-7.4,-55.5541151520872,-137.531452880088));
#136774=CARTESIAN_POINT('',(-7.4,-55.08000002,-96.6432622057672));
#136775=CARTESIAN_POINT('',(-7.4,-55.08000002,-135.57795249279));
#136776=CARTESIAN_POINT('',(-7.4,-55.5541151520872,-94.5271900914178));
#136777=CARTESIAN_POINT('Ctrl Pts',(-7.4,-55.5541151520872,-94.5271900914178));
#136778=CARTESIAN_POINT('Ctrl Pts',(-7.4,-55.4646684466484,-94.7165399244892));
#136779=CARTESIAN_POINT('Ctrl Pts',(-7.4,-55.3874966670382,-94.9115657139063));
#136780=CARTESIAN_POINT('Ctrl Pts',(-7.4,-55.3230550301945,-95.1098279145052));
#136781=CARTESIAN_POINT('Ctrl Pts',(-7.4,-55.2745243397284,-95.2591382355908));
#136782=CARTESIAN_POINT('Ctrl Pts',(-7.4,-55.2332126733285,-95.410283167727));
#136783=CARTESIAN_POINT('Ctrl Pts',(-7.4,-55.199296044664,-95.5622145003849));
#136784=CARTESIAN_POINT('Ctrl Pts',(-7.4,-55.1306219000049,-95.8698439649878));
#136785=CARTESIAN_POINT('Ctrl Pts',(-7.4,-55.0911602505268,-96.1824496093173));
#136786=CARTESIAN_POINT('Ctrl Pts',(-7.4,-55.0820478268083,-96.500225074923));
#136787=CARTESIAN_POINT('Ctrl Pts',(-7.4,-55.0806839263472,-96.5477880633723));
#136788=CARTESIAN_POINT('Ctrl Pts',(-7.4,-55.08000002,-96.595466884908));
#136789=CARTESIAN_POINT('Ctrl Pts',(-7.4,-55.08000002,-96.6432622057672));
#136790=CARTESIAN_POINT('Ctrl Pts',(-7.4,-71.3078420373655,-61.0621827299711));
#136791=CARTESIAN_POINT('Ctrl Pts',(-7.4,-66.0675133276181,-72.2223201517098));
#136792=CARTESIAN_POINT('Ctrl Pts',(-7.4,-60.8202894597531,-83.3792196747323));
#136793=CARTESIAN_POINT('Ctrl Pts',(-7.4,-55.5541151520872,-94.5271900914177));
#136794=CARTESIAN_POINT('Ctrl Pts',(-7.4,-72.58000002,-58.1594740865074));
#136795=CARTESIAN_POINT('Ctrl Pts',(-7.39999999999995,-73.0800000199999,
-58.1594740865073));
#136796=CARTESIAN_POINT('Ctrl Pts',(-7.9,-73.08000002,-58.1594740865074));
#136797=CARTESIAN_POINT('Ctrl Pts',(-7.4,-72.5800000130548,-57.9035537157173));
#136798=CARTESIAN_POINT('Ctrl Pts',(-7.39999999999997,-73.0817635435305,
-57.8518911502671));
#136799=CARTESIAN_POINT('Ctrl Pts',(-7.9017604405896,-73.08000002,-57.8524302618023));
#136800=CARTESIAN_POINT('Ctrl Pts',(-7.4,-72.5416326919704,-57.6540534055839));
#136801=CARTESIAN_POINT('Ctrl Pts',(-7.39999999999995,-73.0373043377172,
-57.5520537815894));
#136802=CARTESIAN_POINT('Ctrl Pts',(-7.90348019558611,-73.0339592231946,
-57.5530891712348));
#136803=CARTESIAN_POINT('Ctrl Pts',(-7.4,-72.42740431593,-57.2895390365225));
#136804=CARTESIAN_POINT('Ctrl Pts',(-7.39999999999995,-72.9025581822962,
-57.1135670536862));
#136805=CARTESIAN_POINT('Ctrl Pts',(-7.90599716341333,-72.896885176701,
-57.1157587646024));
#136806=CARTESIAN_POINT('Ctrl Pts',(-7.4,-72.3798159344887,-57.1705597381646));
#136807=CARTESIAN_POINT('Ctrl Pts',(-7.39999999999996,-72.846103402619,
-56.9702086770063));
#136808=CARTESIAN_POINT('Ctrl Pts',(-7.90681948691283,-72.8397791179241,
-56.9730119912525));
#136809=CARTESIAN_POINT('Ctrl Pts',(-7.4,-72.2685307073729,-56.9437302645456));
#136810=CARTESIAN_POINT('Ctrl Pts',(-7.39999999999997,-72.7136696095191,
-56.6966550709085));
#136811=CARTESIAN_POINT('Ctrl Pts',(-7.9083884819823,-72.7062368443098,
-56.70087080336));
#136812=CARTESIAN_POINT('Ctrl Pts',(-7.4,-72.2045576741781,-56.8349322106875));
#136813=CARTESIAN_POINT('Ctrl Pts',(-7.40000000000002,-72.6373398680779,
-56.5653507289509));
#136814=CARTESIAN_POINT('Ctrl Pts',(-7.90914169806791,-72.6294692039913,
-56.5703391604345));
#136815=CARTESIAN_POINT('Ctrl Pts',(-7.4,-72.0597499182548,-56.6266807792285));
#136816=CARTESIAN_POINT('Ctrl Pts',(-7.39999999999991,-72.4642201336178,
-56.3138046122562));
#136817=CARTESIAN_POINT('Ctrl Pts',(-7.91058447423394,-72.4556998989282,
-56.3204873030743));
#136818=CARTESIAN_POINT('Ctrl Pts',(-7.4,-71.9783757021874,-56.5268811589555));
#136819=CARTESIAN_POINT('Ctrl Pts',(-7.39999999999996,-72.366765643856,
-56.1931795440353));
#136820=CARTESIAN_POINT('Ctrl Pts',(-7.91127644455456,-72.3580508393546,
-56.2007516828216));
#136821=CARTESIAN_POINT('Ctrl Pts',(-7.4,-71.8038791222482,-56.3433834633767));
#136822=CARTESIAN_POINT('Ctrl Pts',(-7.39999999999996,-72.1574857101496,
-55.9712111947932));
#136823=CARTESIAN_POINT('Ctrl Pts',(-7.91254952666346,-72.1486549419682,
-55.9805984788111));
#136824=CARTESIAN_POINT('Ctrl Pts',(-7.4,-71.710253472938,-56.2588007503857));
#136825=CARTESIAN_POINT('Ctrl Pts',(-7.39999999999963,-72.0450577059424,
-55.8688410357779));
#136826=CARTESIAN_POINT('Ctrl Pts',(-7.91313676360239,-72.0363041630141,
-55.879119540041));
#136827=CARTESIAN_POINT('Ctrl Pts',(-7.4,-71.4103049905956,-56.0264829839341));
#136828=CARTESIAN_POINT('Ctrl Pts',(-7.40000000000062,-71.6842770741658,
-55.5873067274671));
#136829=CARTESIAN_POINT('Ctrl Pts',(-7.9147504864484,-71.6763659857377,
-55.6003940631938));
#136830=CARTESIAN_POINT('Ctrl Pts',(-7.4,-71.1825473819866,-55.9004387386915));
#136831=CARTESIAN_POINT('Ctrl Pts',(-7.39999999999996,-71.4100611802463,
-55.4345719679896));
#136832=CARTESIAN_POINT('Ctrl Pts',(-7.91562717321909,-71.4030569333749,
-55.449171357324));
#136833=CARTESIAN_POINT('Ctrl Pts',(-7.4,-70.9475727253686,-55.8134402200258));
#136834=CARTESIAN_POINT('Ctrl Pts',(-7.39999999999996,-71.1269094387434,
-55.3290689454198));
#136835=CARTESIAN_POINT('Ctrl Pts',(-7.91623251645313,-71.1210872664424,
-55.3447940747887));
#136836=CARTESIAN_POINT('',(-7.9,-73.08000002,-58.1594740865074));
#136837=CARTESIAN_POINT('Ctrl Pts',(-7.91618843693208,-71.1413940909408,
-55.3523946663949));
#136838=CARTESIAN_POINT('Ctrl Pts',(-7.91558486059001,-71.4161690172318,
-55.4564569226562));
#136839=CARTESIAN_POINT('Ctrl Pts',(-7.91472456568273,-71.6821304827593,
-55.6048579163084));
#136840=CARTESIAN_POINT('Ctrl Pts',(-7.91313668710487,-72.036304164319,
-55.8791195385087));
#136841=CARTESIAN_POINT('Ctrl Pts',(-7.91254945020742,-72.1486549432855,
-55.9805984774108));
#136842=CARTESIAN_POINT('Ctrl Pts',(-7.91127636818889,-72.3580508406563,
-56.2007516816906));
#136843=CARTESIAN_POINT('Ctrl Pts',(-7.91058439791765,-72.4556999002017,
-56.3204873020754));
#136844=CARTESIAN_POINT('Ctrl Pts',(-7.90914162185518,-72.6294692051695,
-56.5703391596878));
#136845=CARTESIAN_POINT('Ctrl Pts',(-7.90838840582395,-72.7062368454232,
-56.7008708027285));
#136846=CARTESIAN_POINT('Ctrl Pts',(-7.90681941086846,-72.839779118873,
-56.9730119908319));
#136847=CARTESIAN_POINT('Ctrl Pts',(-7.90599708742908,-72.8968851775529,
-57.1157587642733));
#136848=CARTESIAN_POINT('Ctrl Pts',(-7.90348011978738,-73.0339592236982,
-57.5530891710789));
#136849=CARTESIAN_POINT('Ctrl Pts',(-7.90176036491906,-73.0800000202659,
-57.852430261721));
#136850=CARTESIAN_POINT('Ctrl Pts',(-7.9,-73.08000002,-58.1594740865074));
#136851=CARTESIAN_POINT('Origin',(-7.9,-72.58000002,-58.1594740865074));
#136852=CARTESIAN_POINT('Ctrl Pts',(-7.91297989639778,-71.1218111846181,
-55.3449495350315));
#136853=CARTESIAN_POINT('Ctrl Pts',(-7.88787222497776,-73.08000002,-56.0696654600803));
#136854=CARTESIAN_POINT('Ctrl Pts',(-7.81557216061084,-73.08000002,-58.1565578346149));
#136855=CARTESIAN_POINT('Ctrl Pts',(-8.10803398103311,-71.097847913879,
-55.3428278238724));
#136856=CARTESIAN_POINT('Ctrl Pts',(-8.08415144386284,-73.08000002,-56.0574351382547));
#136857=CARTESIAN_POINT('Ctrl Pts',(-8.01154341310344,-73.08000002,-58.1633472285775));
#136858=CARTESIAN_POINT('Ctrl Pts',(-8.30261637240508,-71.0730051020417,
-55.3405756034006));
#136859=CARTESIAN_POINT('Ctrl Pts',(-8.27957773898596,-73.0800000199964,
-56.044305254623));
#136860=CARTESIAN_POINT('Ctrl Pts',(-8.20751459242944,-73.08000002,-58.1699994619964));
#136861=CARTESIAN_POINT('Ctrl Pts',(-8.49667612019033,-71.047290072049,
-55.338183503385));
#136862=CARTESIAN_POINT('Ctrl Pts',(-8.47395476319521,-73.08000002,-56.030195271658));
#136863=CARTESIAN_POINT('Ctrl Pts',(-8.40348565122521,-73.08000002,-58.176433931325));
#136864=CARTESIAN_POINT('',(-8.4,-73.08000002,-58.1763194612681));
#136865=CARTESIAN_POINT('Ctrl Pts',(-8.4,-73.08000002,-58.1763194612681));
#136866=CARTESIAN_POINT('Ctrl Pts',(-8.40172135040051,-73.08000002,-57.8616056776356));
#136867=CARTESIAN_POINT('Ctrl Pts',(-8.40340362484077,-73.0316819589995,
-57.5549684855522));
#136868=CARTESIAN_POINT('Ctrl Pts',(-8.40668695336401,-72.8395715451724,
-56.9580994114807));
#136869=CARTESIAN_POINT('Ctrl Pts',(-8.40822820346396,-72.6984881279278,
-56.6787458682451));
#136870=CARTESIAN_POINT('Ctrl Pts',(-8.41033280652841,-72.4250329770282,
-56.2980850295082));
#136871=CARTESIAN_POINT('Ctrl Pts',(-8.41100144942456,-72.322979355276,
-56.1772949390326));
#136872=CARTESIAN_POINT('Ctrl Pts',(-8.41222718544652,-72.1044079319076,
-55.9560708595913));
#136873=CARTESIAN_POINT('Ctrl Pts',(-8.41279083164671,-71.9871179192065,
-55.8544512596825));
#136874=CARTESIAN_POINT('Ctrl Pts',(-8.41427813867351,-71.6242920428588,
-55.5865039897334));
#136875=CARTESIAN_POINT('Ctrl Pts',(-8.41506374698045,-71.3572532546422,
-55.4452391148706));
#136876=CARTESIAN_POINT('Ctrl Pts',(-8.41560835021378,-71.0814043774777,
-55.3473655916165));
#136877=CARTESIAN_POINT('Ctrl Pts',(-8.4,-73.08000002,-58.1763194612681));
#136878=CARTESIAN_POINT('Ctrl Pts',(-8.23332974561635,-73.08000002,-58.1708448514923));
#136879=CARTESIAN_POINT('Ctrl Pts',(-8.06666350196851,-73.08000002,-58.1652131587787));
#136880=CARTESIAN_POINT('Ctrl Pts',(-7.9,-73.08000002,-58.1594740865074));
#136881=CARTESIAN_POINT('Ctrl Pts',(-8.4,-73.08000002,-58.1763194612681));
#136882=CARTESIAN_POINT('Ctrl Pts',(-8.89999999999996,-73.0800000199999,
-58.1763194612681));
#136883=CARTESIAN_POINT('Ctrl Pts',(-8.9,-72.58000002,-58.1763194612681));
#136884=CARTESIAN_POINT('Ctrl Pts',(-8.40172135040051,-73.08000002,-57.8616056776356));
#136885=CARTESIAN_POINT('Ctrl Pts',(-8.89999999999996,-73.0782816065607,
-57.8621442504892));
#136886=CARTESIAN_POINT('Ctrl Pts',(-8.9,-72.5800000128814,-57.9140108579591));
#136887=CARTESIAN_POINT('Ctrl Pts',(-8.40340362484077,-73.0316819589995,
-57.5549684855522));
#136888=CARTESIAN_POINT('Ctrl Pts',(-8.89999999999997,-73.0284577192567,
-57.5559934180811));
#136889=CARTESIAN_POINT('Ctrl Pts',(-8.9,-72.5397349720259,-57.6584337450815));
#136890=CARTESIAN_POINT('Ctrl Pts',(-8.40668695336401,-72.8395715451724,
-56.9580994114807));
#136891=CARTESIAN_POINT('Ctrl Pts',(-8.89999999999997,-72.8336034512039,
-56.9611013895289));
#136892=CARTESIAN_POINT('Ctrl Pts',(-8.9,-72.3796429547841,-57.1609527205255));
#136893=CARTESIAN_POINT('Ctrl Pts',(-8.40822820346396,-72.6984881279278,
-56.6787458682451));
#136894=CARTESIAN_POINT('Ctrl Pts',(-8.89999999999995,-72.6915892789857,
-56.6830185073362));
#136895=CARTESIAN_POINT('Ctrl Pts',(-8.9,-72.262073445265,-56.9281157265161));
#136896=CARTESIAN_POINT('Ctrl Pts',(-8.41033280652841,-72.4250329770282,
-56.2980850295082));
#136897=CARTESIAN_POINT('Ctrl Pts',(-8.89999999999996,-72.4171612181699,
-56.3044762227344));
#136898=CARTESIAN_POINT('Ctrl Pts',(-8.9,-72.0341941498609,-56.6108404408522));
#136899=CARTESIAN_POINT('Ctrl Pts',(-8.41100144942456,-72.322979355276,
-56.1772949390326));
#136900=CARTESIAN_POINT('Ctrl Pts',(-8.9000000000003,-72.3149747479787,
-56.1845060329552));
#136901=CARTESIAN_POINT('Ctrl Pts',(-8.9,-71.9491494655935,-56.5101636182542));
#136902=CARTESIAN_POINT('Ctrl Pts',(-8.41222718544652,-72.1044079319076,
-55.9560708595913));
#136903=CARTESIAN_POINT('Ctrl Pts',(-8.89999999999963,-72.0963975739119,
-55.9649406347444));
#136904=CARTESIAN_POINT('Ctrl Pts',(-8.9,-71.7670066137261,-56.3257764465383));
#136905=CARTESIAN_POINT('Ctrl Pts',(-8.41279083164671,-71.9871179192065,
-55.8544512596825));
#136906=CARTESIAN_POINT('Ctrl Pts',(-8.89999999999951,-71.9792314944188,
-55.8641264120645));
#136907=CARTESIAN_POINT('Ctrl Pts',(-8.9,-71.6692649365715,-56.2410779083558));
#136908=CARTESIAN_POINT('Ctrl Pts',(-8.41433230457371,-71.6110783688472,
-55.5767456783554));
#136909=CARTESIAN_POINT('Ctrl Pts',(-8.90000000000086,-71.6041352856071,
-55.588933048404));
#136910=CARTESIAN_POINT('Ctrl Pts',(-8.9,-71.3558986429072,-56.0096140831459));
#136911=CARTESIAN_POINT('Ctrl Pts',(-8.41515058995443,-71.3274449382984,
-55.429624391176));
#136912=CARTESIAN_POINT('Ctrl Pts',(-8.89999999999818,-71.3214288330036,
-55.443108937543));
#136913=CARTESIAN_POINT('Ctrl Pts',(-8.9,-71.1195373961099,-55.8869904035305));
#136914=CARTESIAN_POINT('Ctrl Pts',(-8.41569693570581,-71.0352755960629,
-55.3314460318215));
#136915=CARTESIAN_POINT('Ctrl Pts',(-8.89999999999995,-71.0304294360218,
-55.3458650785795));
#136916=CARTESIAN_POINT('Ctrl Pts',(-8.9,-70.8760630000525,-55.8051600336001));
#136917=CARTESIAN_POINT('',(-8.9,-72.58000002,-58.1763194612681));
#136918=CARTESIAN_POINT('Ctrl Pts',(-8.89999996628377,-71.0999148696861,
-55.8925850873112));
#136919=CARTESIAN_POINT('Ctrl Pts',(-8.89999995709263,-71.1271912455156,
-55.9047800168435));
#136920=CARTESIAN_POINT('Ctrl Pts',(-8.89999995405378,-71.1542893399126,
-55.9174976277302));
#136921=CARTESIAN_POINT('Ctrl Pts',(-8.89999995711454,-71.1811814737311,
-55.9307199810309));
#136922=CARTESIAN_POINT('Ctrl Pts',(-8.89999996594249,-71.2587447432665,
-55.9688563728797));
#136923=CARTESIAN_POINT('Ctrl Pts',(-8.89999997989509,-71.3347385769612,
-56.0111644614659));
#136924=CARTESIAN_POINT('Ctrl Pts',(-8.89999998822403,-71.4082909897931,
-56.0572656901905));
#136925=CARTESIAN_POINT('Ctrl Pts',(-8.89999999429182,-71.4618752880513,
-56.0908512911917));
#136926=CARTESIAN_POINT('Ctrl Pts',(-8.89999999762151,-71.5141639062437,
-56.1264488763503));
#136927=CARTESIAN_POINT('Ctrl Pts',(-8.89999999894661,-71.5648287885728,
-56.1638971934456));
#136928=CARTESIAN_POINT('Ctrl Pts',(-8.90000000021706,-71.6134037334432,
-56.1998007592839));
#136929=CARTESIAN_POINT('Ctrl Pts',(-8.9,-71.6605183672425,-56.2373236964706));
#136930=CARTESIAN_POINT('Ctrl Pts',(-8.9,-71.7061534805117,-56.276424902386));
#136931=CARTESIAN_POINT('Ctrl Pts',(-8.9,-71.7586958576709,-56.3214444095464));
#136932=CARTESIAN_POINT('Ctrl Pts',(-8.90000000000525,-71.8093442969672,
-56.3686312342462));
#136933=CARTESIAN_POINT('Ctrl Pts',(-8.89999999994877,-71.8580831316161,
-56.4179650024181));
#136934=CARTESIAN_POINT('Ctrl Pts',(-8.89999999986101,-71.9338178277776,
-56.4946241587137));
#136935=CARTESIAN_POINT('Ctrl Pts',(-8.89999999955086,-72.0053843762033,
-56.5771518376495));
#136936=CARTESIAN_POINT('Ctrl Pts',(-8.89999999953632,-72.0709679837644,
-56.6635131964772));
#136937=CARTESIAN_POINT('Ctrl Pts',(-8.89999999953336,-72.084287167389,
-56.6810520730208));
#136938=CARTESIAN_POINT('Ctrl Pts',(-8.89999999954423,-72.0973597365665,
-56.6987489820051));
#136939=CARTESIAN_POINT('Ctrl Pts',(-8.89999999957055,-72.1101707466964,
-56.7165867802331));
#136940=CARTESIAN_POINT('Ctrl Pts',(-8.89999999961887,-72.1337005884472,
-56.7493492685329));
#136941=CARTESIAN_POINT('Ctrl Pts',(-8.89999999972697,-72.1563957720432,
-56.7826109127347));
#136942=CARTESIAN_POINT('Ctrl Pts',(-8.89999999983668,-72.1782434639423,
-56.8163461536645));
#136943=CARTESIAN_POINT('Ctrl Pts',(-8.90000000003969,-72.2186712712158,
-56.8787711377289));
#136944=CARTESIAN_POINT('Ctrl Pts',(-8.89999999999795,-72.2562052259131,
-56.9428012878323));
#136945=CARTESIAN_POINT('Ctrl Pts',(-8.89999999999952,-72.2908444043662,
-57.0084360093237));
#136946=CARTESIAN_POINT('Ctrl Pts',(-8.90000000000048,-72.311901730162,
-57.0483356771474));
#136947=CARTESIAN_POINT('Ctrl Pts',(-8.9,-72.3318884210689,-57.0888288165436));
#136948=CARTESIAN_POINT('Ctrl Pts',(-8.9,-72.3507957900478,-57.1299193914404));
#136949=CARTESIAN_POINT('Ctrl Pts',(-8.9,-72.3746230901592,-57.1817022418682));
#136950=CARTESIAN_POINT('Ctrl Pts',(-8.89999999998365,-72.3967864402965,
-57.2345342704724));
#136951=CARTESIAN_POINT('Ctrl Pts',(-8.89999999972024,-72.4171503424455,
-57.2881976322959));
#136952=CARTESIAN_POINT('Ctrl Pts',(-8.89999999952357,-72.4323543754486,
-57.3282636038495));
#136953=CARTESIAN_POINT('Ctrl Pts',(-8.89999999921991,-72.4465562092313,
-57.3687924002643));
#136954=CARTESIAN_POINT('Ctrl Pts',(-8.89999999918092,-72.4597162071225,
-57.4096844656319));
#136955=CARTESIAN_POINT('Ctrl Pts',(-8.89999999916252,-72.4659246935418,
-57.428976097332));
#136956=CARTESIAN_POINT('Ctrl Pts',(-8.89999999920802,-72.4718879323416,
-57.4482939264422));
#136957=CARTESIAN_POINT('Ctrl Pts',(-8.89999999932168,-72.4776042453442,
-57.4676297862024));
#136958=CARTESIAN_POINT('Ctrl Pts',(-8.90000000038933,-72.5312977767194,
-57.6492522047483));
#136959=CARTESIAN_POINT('Ctrl Pts',(-8.89999999999947,-72.5639591690306,
-57.834465787063));
#136960=CARTESIAN_POINT('Ctrl Pts',(-8.89999999999994,-72.5753897578134,
-58.0232925565627));
#136961=CARTESIAN_POINT('Ctrl Pts',(-8.90000000000006,-72.5784617700053,
-58.0740404357044));
#136962=CARTESIAN_POINT('Ctrl Pts',(-8.9,-72.58000002,-58.1250492743192));
#136963=CARTESIAN_POINT('Ctrl Pts',(-8.9,-72.58000002,-58.1763194612681));
#136964=CARTESIAN_POINT('Origin',(-8.4,-72.58000002,-58.1763194612681));
#136965=CARTESIAN_POINT('Ctrl Pts',(-9.32900358361251,-70.4903946571405,
-60.8901185898343));
#136966=CARTESIAN_POINT('Ctrl Pts',(-8.89988778396231,-70.5448235085214,
-60.918842206156));
#136967=CARTESIAN_POINT('Ctrl Pts',(-8.90000001675659,-70.9282729174771,
-61.1211126854556));
#136968=CARTESIAN_POINT('Ctrl Pts',(-9.32267960676823,-70.5733355012344,
-60.7345408641471));
#136969=CARTESIAN_POINT('Ctrl Pts',(-8.89989004681883,-70.6365947859941,
-60.7567344379852));
#136970=CARTESIAN_POINT('Ctrl Pts',(-8.90000001650961,-71.0511602413471,
-60.887714756578));
#136971=CARTESIAN_POINT('Ctrl Pts',(-9.31966069353146,-70.6132825269153,
-60.5618033393074));
#136972=CARTESIAN_POINT('Ctrl Pts',(-8.89989111303311,-70.682184857852,
-60.5709595618158));
#136973=CARTESIAN_POINT('Ctrl Pts',(-8.9000000163917,-71.1103503405761,
-60.6286014156989));
#136974=CARTESIAN_POINT('Ctrl Pts',(-9.32026185019719,-70.6053339699646,
-60.3838922942772));
#136975=CARTESIAN_POINT('Ctrl Pts',(-8.89989090319396,-70.6731622220975,
-60.380823819096));
#136976=CARTESIAN_POINT('Ctrl Pts',(-8.90000001641518,-71.0985729052349,
-60.3617033877878));
#136977=CARTESIAN_POINT('',(-8.9,-70.9575466375288,-61.0621827299711));
#136978=CARTESIAN_POINT('Origin',(-9.4,-70.9575466375288,-61.0621827299711));
#136979=CARTESIAN_POINT('Origin',(-8.89999938777026,-69.7158521499215,-60.4580628686544));
#136980=CARTESIAN_POINT('Origin',(-8.9,67.7009572055632,-55.24995));
#136981=CARTESIAN_POINT('',(-8.9,-72.58000002,-174.451268889151));
#136982=CARTESIAN_POINT('Ctrl Pts',(-8.9,-72.58000002,-174.451268889151));
#136983=CARTESIAN_POINT('Ctrl Pts',(-8.9,-72.58000002,-174.643662890522));
#136984=CARTESIAN_POINT('Ctrl Pts',(-8.90000000018189,-72.5583230934377,
-174.832372832512));
#136985=CARTESIAN_POINT('Ctrl Pts',(-8.89999999981754,-72.5152520259488,
-175.017431778767));
#136986=CARTESIAN_POINT('Ctrl Pts',(-8.89999999974365,-72.5065182587111,
-175.054957242055));
#136987=CARTESIAN_POINT('Ctrl Pts',(-8.89999999963418,-72.4969046367721,
-175.09233259596));
#136988=CARTESIAN_POINT('Ctrl Pts',(-8.89999999944856,-72.4864132528962,
-175.129558133433));
#136989=CARTESIAN_POINT('Ctrl Pts',(-8.89999999933697,-72.4801056624026,
-175.151938731556));
#136990=CARTESIAN_POINT('Ctrl Pts',(-8.89999999923514,-72.4734752856604,
-175.174281489137));
#136991=CARTESIAN_POINT('Ctrl Pts',(-8.8999999991621,-72.4665241218154,
-175.196577428232));
#136992=CARTESIAN_POINT('Ctrl Pts',(-8.89999999896656,-72.4479148757584,
-175.256266801974));
#136993=CARTESIAN_POINT('Ctrl Pts',(-8.89999999902277,-72.4269795805932,
-175.315421893863));
#136994=CARTESIAN_POINT('Ctrl Pts',(-8.89999999928889,-72.4039589917986,
-175.373505006315));
#136995=CARTESIAN_POINT('Ctrl Pts',(-8.89999999941373,-72.3931602367398,
-175.400751281813));
#136996=CARTESIAN_POINT('Ctrl Pts',(-8.8999999995758,-72.3819033245036,
-175.427761928544));
#136997=CARTESIAN_POINT('Ctrl Pts',(-8.899999999719,-72.3702165277834,-175.454483443826));
#136998=CARTESIAN_POINT('Ctrl Pts',(-8.89999999989012,-72.356250141463,
-175.486417173351));
#136999=CARTESIAN_POINT('Ctrl Pts',(-8.89999999994017,-72.3416346359546,
-175.518026103028));
#137000=CARTESIAN_POINT('Ctrl Pts',(-8.89999999996783,-72.3264029998066,
-175.549231269472));
#137001=CARTESIAN_POINT('Ctrl Pts',(-8.90000000003108,-72.2915692635033,
-175.620595404528));
#137002=CARTESIAN_POINT('Ctrl Pts',(-8.90000000000045,-72.2533993434512,
-175.690229109067));
#137003=CARTESIAN_POINT('Ctrl Pts',(-8.89999999999886,-72.2119321367876,
-175.757979856507));
#137004=CARTESIAN_POINT('Ctrl Pts',(-8.89999999999793,-72.1877543610133,
-175.797482454149));
#137005=CARTESIAN_POINT('Ctrl Pts',(-8.89999999999706,-72.1624481423419,
-175.836359594911));
#137006=CARTESIAN_POINT('Ctrl Pts',(-8.89999999999683,-72.1360090283531,
-175.874608824138));
#137007=CARTESIAN_POINT('Ctrl Pts',(-8.8999999999962,-72.0642253375692,
-175.978457646179));
#137008=CARTESIAN_POINT('Ctrl Pts',(-8.89999999999926,-71.9835064480419,
-176.078093573446));
#137009=CARTESIAN_POINT('Ctrl Pts',(-8.89999999999979,-71.8969230956058,
-176.169773703533));
#137010=CARTESIAN_POINT('Ctrl Pts',(-8.90000000000003,-71.8581752387953,
-176.210802474689));
#137011=CARTESIAN_POINT('Ctrl Pts',(-8.9,-71.8181601276395,-176.250407223135));
#137012=CARTESIAN_POINT('Ctrl Pts',(-8.9,-71.7768804944358,-176.288591148433));
#137013=CARTESIAN_POINT('Ctrl Pts',(-8.9,-71.7350069729775,-176.327324424174));
#137014=CARTESIAN_POINT('Ctrl Pts',(-8.9,-71.6916833325441,-176.364727207912));
#137015=CARTESIAN_POINT('Ctrl Pts',(-8.9,-71.6470438920773,-176.40066126947));
#137016=CARTESIAN_POINT('Ctrl Pts',(-8.9,-71.6374948625339,-176.408348091075));
#137017=CARTESIAN_POINT('Ctrl Pts',(-8.9,-71.6278871345229,-176.415966736531));
#137018=CARTESIAN_POINT('Ctrl Pts',(-8.9,-71.6182220181434,-176.423516347907));
#137019=CARTESIAN_POINT('Ctrl Pts',(-8.9,-71.5940005454252,-176.442436213824));
#137020=CARTESIAN_POINT('Ctrl Pts',(-8.9,-71.5693801206575,-176.460921216669));
#137021=CARTESIAN_POINT('Ctrl Pts',(-8.9,-71.5444197215458,-176.478940580039));
#137022=CARTESIAN_POINT('Ctrl Pts',(-8.9,-71.4920391665984,-176.516755049627));
#137023=CARTESIAN_POINT('Ctrl Pts',(-8.89999999451621,-71.4381757456861,
-176.552638667358));
#137024=CARTESIAN_POINT('Ctrl Pts',(-8.89999997064355,-71.3830164241513,
-176.586384312661));
#137025=CARTESIAN_POINT('Ctrl Pts',(-8.89999995870723,-71.3554367633839,
-176.603257135313));
#137026=CARTESIAN_POINT('Ctrl Pts',(-8.89999994562374,-71.3275333910231,
-176.61959527903));
#137027=CARTESIAN_POINT('Ctrl Pts',(-8.89999993949196,-71.299333729225,
-176.635377629733));
#137028=CARTESIAN_POINT('Ctrl Pts',(-8.89999993336017,-71.2711340674268,
-176.651159980436));
#137029=CARTESIAN_POINT('Ctrl Pts',(-8.89999993496576,-71.242638116192,
-176.666386538126));
#137030=CARTESIAN_POINT('Ctrl Pts',(-8.89999994551797,-71.2138732976723,
-176.681036188718));
#137031=CARTESIAN_POINT('',(-8.9,-72.58000002,-174.432329119515));
#137032=CARTESIAN_POINT('',(-8.9,-55.5972887473416,-93.4294586200098));
#137033=CARTESIAN_POINT('Ctrl Pts',(-8.9,-55.5972887473416,-93.4294586200098));
#137034=CARTESIAN_POINT('Ctrl Pts',(-8.9,-60.7433024895534,-82.6526792495127));
#137035=CARTESIAN_POINT('Ctrl Pts',(-8.9,-65.8565639782118,-71.8603324984455));
#137036=CARTESIAN_POINT('Ctrl Pts',(-8.9,-70.9575466375288,-61.0621827299711));
#137037=CARTESIAN_POINT('',(-8.9,-55.08000002,-95.7201877838351));
#137038=CARTESIAN_POINT('Ctrl Pts',(-8.9,-55.08000002,-95.7201877838351));
#137039=CARTESIAN_POINT('Ctrl Pts',(-8.9,-55.08000002,-95.3987883664371));
#137040=CARTESIAN_POINT('Ctrl Pts',(-8.9,-55.109467211452,-95.0775170946566));
#137041=CARTESIAN_POINT('Ctrl Pts',(-8.9,-55.1665218943413,-94.7639046607142));
#137042=CARTESIAN_POINT('Ctrl Pts',(-8.9,-55.1800381380422,-94.6896099337934));
#137043=CARTESIAN_POINT('Ctrl Pts',(-8.9,-55.1951028648176,-94.6157450444869));
#137044=CARTESIAN_POINT('Ctrl Pts',(-8.9,-55.2116915002618,-94.5424101933588));
#137045=CARTESIAN_POINT('Ctrl Pts',(-8.9,-55.2822535698941,-94.2304701975012));
#137046=CARTESIAN_POINT('Ctrl Pts',(-8.9,-55.3800515517497,-93.9262693259458));
#137047=CARTESIAN_POINT('Ctrl Pts',(-8.9,-55.5065195348463,-93.6302150671016));
#137048=CARTESIAN_POINT('Ctrl Pts',(-8.9,-55.5352865893775,-93.5628730505705));
#137049=CARTESIAN_POINT('Ctrl Pts',(-8.9,-55.5655372445571,-93.4959526010439));
#137050=CARTESIAN_POINT('Ctrl Pts',(-8.9,-55.5972887473416,-93.4294586200098));
#137051=CARTESIAN_POINT('',(-8.9,-55.08000002,-136.338455187671));
#137052=CARTESIAN_POINT('',(-8.9,-55.08000002,-95.926725859984));
#137053=CARTESIAN_POINT('',(-8.9,-55.5972887473373,-138.629184351487));
#137054=CARTESIAN_POINT('Ctrl Pts',(-8.9,-55.5972887473373,-138.629184351487));
#137055=CARTESIAN_POINT('Ctrl Pts',(-8.9,-55.4856871847905,-138.39546841578));
#137056=CARTESIAN_POINT('Ctrl Pts',(-8.9,-55.3917128230604,-138.153503053561));
#137057=CARTESIAN_POINT('Ctrl Pts',(-8.9,-55.3159696737979,-137.907364658656));
#137058=CARTESIAN_POINT('Ctrl Pts',(-8.9,-55.275425284041,-137.775609759179));
#137059=CARTESIAN_POINT('Ctrl Pts',(-8.9,-55.240103934472,-137.642659649441));
#137060=CARTESIAN_POINT('Ctrl Pts',(-8.9,-55.2100924708571,-137.509141392841));
#137061=CARTESIAN_POINT('Ctrl Pts',(-8.9,-55.1385732376637,-137.190958865929));
#137062=CARTESIAN_POINT('Ctrl Pts',(-8.9,-55.0960936141251,-136.867828326659));
#137063=CARTESIAN_POINT('Ctrl Pts',(-8.9,-55.0837682332387,-136.53955984602));
#137064=CARTESIAN_POINT('Ctrl Pts',(-8.9,-55.0812593131255,-136.472738430829));
#137065=CARTESIAN_POINT('Ctrl Pts',(-8.9,-55.08000002,-136.405704093546));
#137066=CARTESIAN_POINT('Ctrl Pts',(-8.9,-55.08000002,-136.338455187671));
#137067=CARTESIAN_POINT('',(-8.9,-71.0715121820529,-171.237717270032));
#137068=CARTESIAN_POINT('Ctrl Pts',(-8.9,-71.0715121820529,-171.237717270032));
#137069=CARTESIAN_POINT('Ctrl Pts',(-8.9,-65.932751045448,-160.359049360718));
#137070=CARTESIAN_POINT('Ctrl Pts',(-8.9,-60.7816272203214,-149.486223352848));
#137071=CARTESIAN_POINT('Ctrl Pts',(-8.9,-55.5972887473373,-138.629184351487));
#137072=CARTESIAN_POINT('Origin',(-8.9,-69.0831852719725,-172.006057477089));
#137073=CARTESIAN_POINT('Origin',(0.,-12.9675000200281,-60.64995));
#137074=CARTESIAN_POINT('',(-9.30242220813418,-55.1547652725561,-93.2181494891177));
#137075=CARTESIAN_POINT('',(-14.8995694557399,-55.305434517314,-89.6101049856477));
#137076=CARTESIAN_POINT('Ctrl Pts',(-9.30242220787995,-55.1547652726018,
-93.2181494891395));
#137077=CARTESIAN_POINT('Ctrl Pts',(-10.1477584234389,-55.1733150950176,
-92.7890451196444));
#137078=CARTESIAN_POINT('Ctrl Pts',(-10.9772737219349,-55.1936535277891,
-92.3131807748197));
#137079=CARTESIAN_POINT('Ctrl Pts',(-12.8655985312176,-55.243800840887,
-91.1207823248442));
#137080=CARTESIAN_POINT('Ctrl Pts',(-13.8974380553098,-55.2740994408045,
-90.3869238925609));
#137081=CARTESIAN_POINT('Ctrl Pts',(-14.8995694550283,-55.3054345175152,
-89.6101049857472));
#137082=CARTESIAN_POINT('Ctrl Pts',(-9.32749162718857,-70.5102313269446,
-60.8508735991008));
#137083=CARTESIAN_POINT('Ctrl Pts',(-9.32127686111114,-65.4102595348795,
-71.6490160142261));
#137084=CARTESIAN_POINT('Ctrl Pts',(-9.31365506232303,-60.2983072126764,
-82.4413594866477));
#137085=CARTESIAN_POINT('Ctrl Pts',(-9.30242220787995,-55.1547652726018,
-93.2181494891395));
#137086=CARTESIAN_POINT('Ctrl Pts',(-14.8995694550283,-55.3054345175152,
-89.6101049857472));
#137087=CARTESIAN_POINT('Ctrl Pts',(-14.9143624117001,-60.0265024281888,
-80.0493410623047));
#137088=CARTESIAN_POINT('Ctrl Pts',(-14.9250579803326,-64.6843968356381,
-70.4566455899725));
#137089=CARTESIAN_POINT('Ctrl Pts',(-14.9339094669349,-69.3159372152925,
-60.8508735991008));
#137090=CARTESIAN_POINT('Ctrl Pts',(-14.9223321947707,-69.4149357692034,
-60.3843514923986));
#137091=CARTESIAN_POINT('Ctrl Pts',(-15.5501315664229,-69.2493490991427,
-60.3919718313355));
#137092=CARTESIAN_POINT('Ctrl Pts',(-15.5499999897346,-69.8979710840161,
-60.3623910423524));
#137093=CARTESIAN_POINT('Ctrl Pts',(-14.9213859066283,-69.4230681799894,
-60.5602124639497));
#137094=CARTESIAN_POINT('Ctrl Pts',(-15.5501319338923,-69.254225424885,
-60.5374367820963));
#137095=CARTESIAN_POINT('Ctrl Pts',(-15.5499999897191,-69.909794297014,
-60.6262209796107));
#137096=CARTESIAN_POINT('Ctrl Pts',(-14.9261257169452,-69.3823033916894,
-60.7335097961699));
#137097=CARTESIAN_POINT('Ctrl Pts',(-15.5501300981793,-69.2303831032415,
-60.678769908775));
#137098=CARTESIAN_POINT('Ctrl Pts',(-15.5499999897966,-69.8505276805174,
-60.8861498986541));
#137099=CARTESIAN_POINT('Ctrl Pts',(-14.9363515075123,-69.2951068303029,
-60.89043888838));
#137100=CARTESIAN_POINT('Ctrl Pts',(-15.5501262723864,-69.1690548338264,
-60.822436019398));
#137101=CARTESIAN_POINT('Ctrl Pts',(-15.5499999899638,-69.7237798948102,
-61.1215831761309));
#137102=CARTESIAN_POINT('',(-15.55,-69.7539685376239,-61.0621827299711));
#137103=CARTESIAN_POINT('Origin',(-15.05,-69.753968537624,-61.0621827299711));
#137104=CARTESIAN_POINT('Origin',(-15.5500003881169,-68.4591876507942,-60.4515855208217));
#137105=CARTESIAN_POINT('Origin',(-15.55,67.7009572055632,-55.24995));
#137106=CARTESIAN_POINT('',(-15.55,-70.08000002,-55.74995));
#137107=CARTESIAN_POINT('',(-15.55,67.7009572055632,-55.74995));
#137108=CARTESIAN_POINT('',(-15.55,-72.58000002,-58.24995));
#137109=CARTESIAN_POINT('Origin',(-15.55,-70.08000002,-58.24995));
#137110=CARTESIAN_POINT('',(-15.55,-72.58000002,-174.34995));
#137111=CARTESIAN_POINT('',(-15.55,-72.58000002,-58.24995));
#137112=CARTESIAN_POINT('',(-15.55,-70.08000002,-176.84995));
#137113=CARTESIAN_POINT('Origin',(-15.55,-70.08000002,-174.34995));
#137114=CARTESIAN_POINT('',(-15.55,67.7009572055632,-176.84995));
#137115=CARTESIAN_POINT('',(-15.55,-69.870344670579,-171.237717270032));
#137116=CARTESIAN_POINT('Origin',(-15.5500003878738,-68.5755848712236,-171.847853238442));
#137117=CARTESIAN_POINT('',(-15.55,-55.7328910677637,-142.237228854888));
#137118=CARTESIAN_POINT('Ctrl Pts',(-15.55,-55.7328910677637,-142.237228854888));
#137119=CARTESIAN_POINT('Ctrl Pts',(-15.55,-60.4987378575172,-151.878044750548));
#137120=CARTESIAN_POINT('Ctrl Pts',(-15.55,-65.1981545194713,-161.551244681819));
#137121=CARTESIAN_POINT('Ctrl Pts',(-15.55,-69.870344670579,-171.237717270032));
#137122=CARTESIAN_POINT('',(-15.55,-55.08000002,-139.407335470919));
#137123=CARTESIAN_POINT('Ctrl Pts',(-15.55,-55.08000002,-139.407335470919));
#137124=CARTESIAN_POINT('Ctrl Pts',(-15.55,-55.08000002,-139.59083822256));
#137125=CARTESIAN_POINT('Ctrl Pts',(-15.55,-55.0879005396309,-139.774357162878));
#137126=CARTESIAN_POINT('Ctrl Pts',(-15.55,-55.1034481519512,-139.956947178511));
#137127=CARTESIAN_POINT('Ctrl Pts',(-15.55,-55.1192595423617,-140.142634984636));
#137128=CARTESIAN_POINT('Ctrl Pts',(-15.55,-55.1429798052606,-140.327363292663));
#137129=CARTESIAN_POINT('Ctrl Pts',(-15.55,-55.1743956555241,-140.510141133111));
#137130=CARTESIAN_POINT('Ctrl Pts',(-15.55,-55.1948438531121,-140.629109022404));
#137131=CARTESIAN_POINT('Ctrl Pts',(-15.55,-55.2185534084275,-140.747250607227));
#137132=CARTESIAN_POINT('Ctrl Pts',(-15.55,-55.2454769784191,-140.864289524316));
#137133=CARTESIAN_POINT('Ctrl Pts',(-15.55,-55.3211274089245,-141.193148010259));
#137134=CARTESIAN_POINT('Ctrl Pts',(-15.55,-55.4215956233193,-141.514575802571));
#137135=CARTESIAN_POINT('Ctrl Pts',(-15.55,-55.5489107707142,-141.827965375896));
#137136=CARTESIAN_POINT('Ctrl Pts',(-15.55,-55.6049725527698,-141.965962922282));
#137137=CARTESIAN_POINT('Ctrl Pts',(-15.55,-55.666240524002,-142.102401687737));
#137138=CARTESIAN_POINT('Ctrl Pts',(-15.55,-55.7328910677637,-142.237228854888));
#137139=CARTESIAN_POINT('',(-15.55,-55.08000002,-92.6513075005872));
#137140=CARTESIAN_POINT('',(-15.55,-55.08000002,-139.74173251362));
#137141=CARTESIAN_POINT('',(-15.55,-55.7328910677637,-89.8214141166176));
#137142=CARTESIAN_POINT('Ctrl Pts',(-15.55,-55.7328910677637,-89.8214141166176));
#137143=CARTESIAN_POINT('Ctrl Pts',(-15.55,-55.6023063246601,-90.085573566672));
#137144=CARTESIAN_POINT('Ctrl Pts',(-15.55,-55.4913767816585,-90.3592181628692));
#137145=CARTESIAN_POINT('Ctrl Pts',(-15.55,-55.4001499318839,-90.6379301892029));
#137146=CARTESIAN_POINT('Ctrl Pts',(-15.55,-55.3390449811731,-90.824615191192));
#137147=CARTESIAN_POINT('Ctrl Pts',(-15.55,-55.2867806294645,-91.0135745317695));
#137148=CARTESIAN_POINT('Ctrl Pts',(-15.55,-55.2433833364682,-91.2034849476131));
#137149=CARTESIAN_POINT('Ctrl Pts',(-15.55,-55.1636960311292,-91.5522036867216));
#137150=CARTESIAN_POINT('Ctrl Pts',(-15.55,-55.1127619110561,-91.9058298380985));
#137151=CARTESIAN_POINT('Ctrl Pts',(-15.55,-55.0914526404125,-92.2645121879592));
#137152=CARTESIAN_POINT('Ctrl Pts',(-15.55,-55.0838313896103,-92.3927947647004));
#137153=CARTESIAN_POINT('Ctrl Pts',(-15.55,-55.08000002,-92.5217241762754));
#137154=CARTESIAN_POINT('Ctrl Pts',(-15.55,-55.08000002,-92.6513075005872));
#137155=CARTESIAN_POINT('Ctrl Pts',(-15.55,-69.7539685376239,-61.0621827299711));
#137156=CARTESIAN_POINT('Ctrl Pts',(-15.55,-65.1200645664474,-70.6679914124205));
#137157=CARTESIAN_POINT('Ctrl Pts',(-15.55,-60.459169452046,-80.2606410189155));
#137158=CARTESIAN_POINT('Ctrl Pts',(-15.55,-55.7328910677637,-89.8214141166175));
#137159=CARTESIAN_POINT('Origin',(-16.05,-73.08000002,-55.74995));
#137160=CARTESIAN_POINT('',(-16.05,-70.08000002,-55.24995));
#137161=CARTESIAN_POINT('',(-16.05,-73.08000002,-55.24995));
#137162=CARTESIAN_POINT('Origin',(-16.05,-70.08000002,-55.74995));
#137163=CARTESIAN_POINT('Origin',(-41.5,-73.08000002,-55.24995));
#137164=CARTESIAN_POINT('',(-16.55,-70.08000002,-55.24995));
#137165=CARTESIAN_POINT('',(-16.55,-73.08000002,-55.24995));
#137166=CARTESIAN_POINT('',(-41.5,-70.08000002,-55.24995));
#137167=CARTESIAN_POINT('Origin',(-16.55,67.7009572055632,-55.74995));
#137168=CARTESIAN_POINT('',(-17.05,-70.08000002,-55.74995));
#137169=CARTESIAN_POINT('',(-17.05,67.7009572055632,-55.74995));
#137170=CARTESIAN_POINT('Origin',(-16.55,-70.08000002,-55.74995));
#137171=CARTESIAN_POINT('Ctrl Pts',(-17.4174322081753,-68.5782862263167,
-60.8898940315426));
#137172=CARTESIAN_POINT('Ctrl Pts',(-17.0499351254479,-68.6669792326861,
-60.938279139678));
#137173=CARTESIAN_POINT('Ctrl Pts',(-17.0500000072447,-69.0016232241721,
-61.1207587448991));
#137174=CARTESIAN_POINT('Ctrl Pts',(-17.4057007122192,-68.6661491518679,
-60.7353408116852));
#137175=CARTESIAN_POINT('Ctrl Pts',(-17.0499377736316,-68.768366090799,
-60.7724682610327));
#137176=CARTESIAN_POINT('Ctrl Pts',(-17.0500000070135,-69.1279231312629,
-60.8888915170785));
#137177=CARTESIAN_POINT('Ctrl Pts',(-17.3999941136478,-68.7092345420341,
-60.5620638496915));
#137178=CARTESIAN_POINT('Ctrl Pts',(-17.0499390370914,-68.8203021885316,
-60.5773600099809));
#137179=CARTESIAN_POINT('Ctrl Pts',(-17.0500000069009,-69.1898773189587,
-60.6289947788348));
#137180=CARTESIAN_POINT('Ctrl Pts',(-17.4011286297274,-68.7006746954154,
-60.3838015812945));
#137181=CARTESIAN_POINT('Ctrl Pts',(-17.0499387884128,-68.8100686727309,
-60.3786737910309));
#137182=CARTESIAN_POINT('Ctrl Pts',(-17.0500000069233,-69.1775691162164,
-60.3615671969807));
#137183=CARTESIAN_POINT('',(-17.05,-69.0317756926871,-61.0621827299711));
#137184=CARTESIAN_POINT('Origin',(-17.55,-69.0317756926871,-61.0621827299711));
#137185=CARTESIAN_POINT('Origin',(-17.0499997344964,-67.7007635583902,-60.4478804500804));
#137186=CARTESIAN_POINT('Origin',(-17.05,67.7009572055632,-55.24995));
#137187=CARTESIAN_POINT('',(-17.05,-70.08000002,-176.84995));
#137188=CARTESIAN_POINT('',(-17.05,67.7009572055632,-176.84995));
#137189=CARTESIAN_POINT('',(-17.05,-72.58000002,-174.34995));
#137190=CARTESIAN_POINT('Origin',(-17.05,-70.08000002,-174.34995));
#137191=CARTESIAN_POINT('',(-17.05,-72.58000002,-58.24995));
#137192=CARTESIAN_POINT('',(-17.05,-72.58000002,-174.34995));
#137193=CARTESIAN_POINT('Origin',(-17.05,-70.08000002,-58.24995));
#137194=CARTESIAN_POINT('',(-17.05,-55.8060398696737,-87.7674469593951));
#137195=CARTESIAN_POINT('Ctrl Pts',(-17.05,-55.8060398696737,-87.7674469593951));
#137196=CARTESIAN_POINT('Ctrl Pts',(-17.05,-60.2764102501238,-78.896294484622));
#137197=CARTESIAN_POINT('Ctrl Pts',(-17.05,-64.6707000732441,-69.9874632456984));
#137198=CARTESIAN_POINT('Ctrl Pts',(-17.05,-69.0317756926871,-61.0621827299711));
#137199=CARTESIAN_POINT('',(-17.05,-55.08000002,-90.8821060618472));
#137200=CARTESIAN_POINT('Ctrl Pts',(-17.05,-55.08000002,-90.8821060618472));
#137201=CARTESIAN_POINT('Ctrl Pts',(-17.05,-55.0800000198976,-90.704401128278));
#137202=CARTESIAN_POINT('Ctrl Pts',(-17.05,-55.0867609195444,-90.5266735432516));
#137203=CARTESIAN_POINT('Ctrl Pts',(-17.05,-55.1000918811982,-90.3496297314767));
#137204=CARTESIAN_POINT('Ctrl Pts',(-17.05,-55.1137303582781,-90.1685019155126));
#137205=CARTESIAN_POINT('Ctrl Pts',(-17.05,-55.1342455055613,-89.9880886440527));
#137206=CARTESIAN_POINT('Ctrl Pts',(-17.05,-55.1614876321832,-89.8091398363497));
#137207=CARTESIAN_POINT('Ctrl Pts',(-17.05,-55.1887297588051,-89.6301910286466));
#137208=CARTESIAN_POINT('Ctrl Pts',(-17.05,-55.2226990580678,-89.4527054855484));
#137209=CARTESIAN_POINT('Ctrl Pts',(-17.05,-55.2632981110657,-89.2774444065539));
#137210=CARTESIAN_POINT('Ctrl Pts',(-17.05,-55.3408916382115,-88.9424827686241));
#137211=CARTESIAN_POINT('Ctrl Pts',(-17.05,-55.4420234811604,-88.614774521522));
#137212=CARTESIAN_POINT('Ctrl Pts',(-17.05,-55.5689958159337,-88.2950290565654));
#137213=CARTESIAN_POINT('Ctrl Pts',(-17.05,-55.6398317020692,-88.1166480463363));
#137214=CARTESIAN_POINT('Ctrl Pts',(-17.05,-55.7187108542616,-87.9407455779088));
#137215=CARTESIAN_POINT('Ctrl Pts',(-17.05,-55.8060398696737,-87.7674469593951));
#137216=CARTESIAN_POINT('',(-17.05,-55.08000002,-141.176536909659));
#137217=CARTESIAN_POINT('',(-17.05,-55.08000002,-91.2551956845905));
#137218=CARTESIAN_POINT('',(-17.05,-55.8060398696787,-144.291196012121));
#137219=CARTESIAN_POINT('Ctrl Pts',(-17.05,-55.8060398696787,-144.291196012121));
#137220=CARTESIAN_POINT('Ctrl Pts',(-17.05,-55.6831540655477,-144.047337313036));
#137221=CARTESIAN_POINT('Ctrl Pts',(-17.05,-55.5762002500337,-143.795681932952));
#137222=CARTESIAN_POINT('Ctrl Pts',(-17.05,-55.4849662480647,-143.539333784836));
#137223=CARTESIAN_POINT('Ctrl Pts',(-17.05,-55.3950897214903,-143.286799853964));
#137224=CARTESIAN_POINT('Ctrl Pts',(-17.05,-55.3204688827058,-143.029710172843));
#137225=CARTESIAN_POINT('Ctrl Pts',(-17.05,-55.2609467896032,-142.77101380861));
#137226=CARTESIAN_POINT('Ctrl Pts',(-17.05,-55.1772261529236,-142.407145147557));
#137227=CARTESIAN_POINT('Ctrl Pts',(-17.05,-55.1222258452589,-142.038367265734));
#137228=CARTESIAN_POINT('Ctrl Pts',(-17.05,-55.0966366319634,-141.664562069113));
#137229=CARTESIAN_POINT('Ctrl Pts',(-17.05,-55.0855652067498,-141.502831568412));
#137230=CARTESIAN_POINT('Ctrl Pts',(-17.05,-55.0800000200001,-141.340159872037));
#137231=CARTESIAN_POINT('Ctrl Pts',(-17.05,-55.08000002,-141.176536909659));
#137232=CARTESIAN_POINT('',(-17.05,-69.1496478013716,-171.237717270032));
#137233=CARTESIAN_POINT('Ctrl Pts',(-17.05,-69.1496478013716,-171.237717270032));
#137234=CARTESIAN_POINT('Ctrl Pts',(-17.05,-64.7499424271364,-162.231693289135));
#137235=CARTESIAN_POINT('Ctrl Pts',(-17.05,-60.3166901832211,-153.242281332924));
#137236=CARTESIAN_POINT('Ctrl Pts',(-17.05,-55.8060398696787,-144.291196012121));
#137237=CARTESIAN_POINT('Origin',(-17.0499997303009,-67.8195562478302,-171.852380930964));
#137238=CARTESIAN_POINT('Origin',(0.,-12.9675000200281,-60.64995));
#137239=CARTESIAN_POINT('',(-17.3782102443508,-55.3867109640818,-87.5561378285247));
#137240=CARTESIAN_POINT('',(-22.9849163801915,-55.5914230811224,-82.0118419126005));
#137241=CARTESIAN_POINT('Ctrl Pts',(-17.3782874559398,-55.3867051038986,
-87.5562252660302));
#137242=CARTESIAN_POINT('Ctrl Pts',(-18.121577867119,-55.4121156870237,
-86.9015665730796));
#137243=CARTESIAN_POINT('Ctrl Pts',(-18.8518378359084,-55.4379479436565,
-86.2242613702274));
#137244=CARTESIAN_POINT('Ctrl Pts',(-19.5713894980264,-55.4639865475406,
-85.5280522873859));
#137245=CARTESIAN_POINT('Ctrl Pts',(-20.7455454946912,-55.5064760371838,
-84.3919864389039));
#137246=CARTESIAN_POINT('Ctrl Pts',(-21.8822352961522,-55.5492052310813,
-83.2139191382355));
#137247=CARTESIAN_POINT('Ctrl Pts',(-22.9849164160517,-55.5914231002813,
-82.0118419843783));
#137248=CARTESIAN_POINT('Ctrl Pts',(-17.4146253252297,-68.5993151180197,
-60.8508735991007));
#137249=CARTESIAN_POINT('Ctrl Pts',(-17.4050346480916,-64.2412639468132,
-69.7761085955077));
#137250=CARTESIAN_POINT('Ctrl Pts',(-17.3935606665343,-59.8507835974011,
-78.6850032438638));
#137251=CARTESIAN_POINT('Ctrl Pts',(-17.3782102443508,-55.3867109640818,
-87.5561378285247));
#137252=CARTESIAN_POINT('Ctrl Pts',(-22.9849163103247,-55.591423110293,
-82.011841880507));
#137253=CARTESIAN_POINT('Ctrl Pts',(-22.9993168926453,-59.3018045077389,
-74.9936336228867));
#137254=CARTESIAN_POINT('Ctrl Pts',(-23.0109831737233,-62.9327835325611,
-67.9329755599233));
#137255=CARTESIAN_POINT('Ctrl Pts',(-23.0210431649761,-66.5230748737403,
-60.8508735991007));
#137256=CARTESIAN_POINT('Ctrl Pts',(-23.0030676793156,-66.6324461755808,
-60.4045898193565));
#137257=CARTESIAN_POINT('Ctrl Pts',(-23.7000444961004,-66.3339120499585,
-60.4123961703627));
#137258=CARTESIAN_POINT('Ctrl Pts',(-23.6999999991391,-67.091907941907,
-60.3927543614167));
#137259=CARTESIAN_POINT('Ctrl Pts',(-23.0023333098327,-66.6369323384221,
-60.5671687383203));
#137260=CARTESIAN_POINT('Ctrl Pts',(-23.7000445996745,-66.3350862497419,
-60.5213661743307));
#137261=CARTESIAN_POINT('Ctrl Pts',(-23.6999999991382,-67.0981649919418,
-60.6366434264749));
#137262=CARTESIAN_POINT('Ctrl Pts',(-23.0091746715062,-66.5951265090932,
-60.7272889592981));
#137263=CARTESIAN_POINT('Ctrl Pts',(-23.7000436587853,-66.3247262225065,
-60.6279370962779));
#137264=CARTESIAN_POINT('Ctrl Pts',(-23.6999999991466,-67.0398545336995,
-60.8767984170799));
#137265=CARTESIAN_POINT('Ctrl Pts',(-23.0230090051547,-66.5111384208438,
-60.8720725996219));
#137266=CARTESIAN_POINT('Ctrl Pts',(-23.7000418676227,-66.2856006591993,
-60.7504731407162));
#137267=CARTESIAN_POINT('Ctrl Pts',(-23.6999999991637,-66.9227827756709,
-61.0939974638476));
#137268=CARTESIAN_POINT('',(-23.7,-66.9393955463102,-61.0621827299711));
#137269=CARTESIAN_POINT('Origin',(-23.2,-66.9393955463102,-61.0621827299711));
#137270=CARTESIAN_POINT('Origin',(-23.7000000338414,-65.5006105045681,-60.4353544160189));
#137271=CARTESIAN_POINT('Origin',(-23.7,67.7009572055632,-55.24995));
#137272=CARTESIAN_POINT('',(-23.7,-70.08000002,-55.74995));
#137273=CARTESIAN_POINT('',(-23.7,67.7009572055632,-55.74995));
#137274=CARTESIAN_POINT('',(-23.7,-72.58000002,-58.24995));
#137275=CARTESIAN_POINT('Origin',(-23.7,-70.08000002,-58.24995));
#137276=CARTESIAN_POINT('',(-23.7,-72.58000002,-174.34995));
#137277=CARTESIAN_POINT('',(-23.7,-72.58000002,-58.24995));
#137278=CARTESIAN_POINT('',(-23.7,-70.08000002,-176.84995));
#137279=CARTESIAN_POINT('Origin',(-23.7,-70.08000002,-174.34995));
#137280=CARTESIAN_POINT('',(-23.7,67.7009572055632,-176.84995));
#137281=CARTESIAN_POINT('',(-23.7,-67.0618271655313,-171.237717270032));
#137282=CARTESIAN_POINT('Origin',(-23.7000000319865,-65.6225360751686,-171.864194562605));
#137283=CARTESIAN_POINT('',(-23.7,-55.9902808012637,-149.835491960129));
#137284=CARTESIAN_POINT('Ctrl Pts',(-23.7,-55.9902808012637,-149.835491960129));
#137285=CARTESIAN_POINT('Ctrl Pts',(-23.7,-59.7506641394806,-156.933423835337));
#137286=CARTESIAN_POINT('Ctrl Pts',(-23.7,-63.4273897219659,-164.074632552453));
#137287=CARTESIAN_POINT('Ctrl Pts',(-23.7,-67.0618271655313,-171.237717270032));
#137288=CARTESIAN_POINT('',(-23.7,-55.08000002,-146.023178055809));
#137289=CARTESIAN_POINT('Ctrl Pts',(-23.7,-55.08000002,-146.023178055809));
#137290=CARTESIAN_POINT('Ctrl Pts',(-23.7,-55.08000002,-146.158053606653));
#137291=CARTESIAN_POINT('Ctrl Pts',(-23.7000000000707,-55.0831707493112,
-146.292669951121));
#137292=CARTESIAN_POINT('Ctrl Pts',(-23.6999999992499,-55.0894565008802,
-146.427026468199));
#137293=CARTESIAN_POINT('Ctrl Pts',(-23.6999999984213,-55.0958009827676,
-146.562638332538));
#137294=CARTESIAN_POINT('Ctrl Pts',(-23.6999999964552,-55.1053189899911,
-146.697986218052));
#137295=CARTESIAN_POINT('Ctrl Pts',(-23.6999999951529,-55.1180059197239,
-146.833072917223));
#137296=CARTESIAN_POINT('Ctrl Pts',(-23.6999999945721,-55.1236634789143,
-146.893312944754));
#137297=CARTESIAN_POINT('Ctrl Pts',(-23.6999999941814,-55.1299519000527,
-146.953501011813));
#137298=CARTESIAN_POINT('Ctrl Pts',(-23.6999999942164,-55.1368740952971,
-147.013636993293));
#137299=CARTESIAN_POINT('Ctrl Pts',(-23.6999999943017,-55.1537261451255,
-147.160037740543));
#137300=CARTESIAN_POINT('Ctrl Pts',(-23.6999999965898,-55.1743560689035,
-147.306288458156));
#137301=CARTESIAN_POINT('Ctrl Pts',(-23.6999999980531,-55.1987232126615,
-147.451788749127));
#137302=CARTESIAN_POINT('Ctrl Pts',(-23.6999999995039,-55.2228814172672,
-147.596041429472));
#137303=CARTESIAN_POINT('Ctrl Pts',(-23.699999999956,-55.2507128773882,
-147.73955572536));
#137304=CARTESIAN_POINT('Ctrl Pts',(-23.6999999999927,-55.2821282400235,
-147.881757850267));
#137305=CARTESIAN_POINT('Ctrl Pts',(-23.700000000002,-55.2901469859131,
-147.918054827572));
#137306=CARTESIAN_POINT('Ctrl Pts',(-23.7,-55.2983989829638,-147.954266404712));
#137307=CARTESIAN_POINT('Ctrl Pts',(-23.7,-55.3068822390434,-147.990383251025));
#137308=CARTESIAN_POINT('Ctrl Pts',(-23.7,-55.3875157587021,-148.333674601646));
#137309=CARTESIAN_POINT('Ctrl Pts',(-23.7,-55.4886143890992,-148.670181748614));
#137310=CARTESIAN_POINT('Ctrl Pts',(-23.7,-55.6129610034727,-148.998982220287));
#137311=CARTESIAN_POINT('Ctrl Pts',(-23.7,-55.7206760510249,-149.283805081125));
#137312=CARTESIAN_POINT('Ctrl Pts',(-23.7,-55.8458362712923,-149.562844907631));
#137313=CARTESIAN_POINT('Ctrl Pts',(-23.7,-55.9902808012637,-149.835491960129));
#137314=CARTESIAN_POINT('',(-23.7,-55.08000002,-86.035464915697));
#137315=CARTESIAN_POINT('',(-23.7,-55.08000002,-146.505061715151));
#137316=CARTESIAN_POINT('',(-23.7,-55.9902808012638,-82.2231510113773));
#137317=CARTESIAN_POINT('Ctrl Pts',(-23.7,-55.9902808012637,-82.2231510113773));
#137318=CARTESIAN_POINT('Ctrl Pts',(-23.7,-55.895308966207,-82.4024156114538));
#137319=CARTESIAN_POINT('Ctrl Pts',(-23.7,-55.8083129339554,-82.5857246305521));
#137320=CARTESIAN_POINT('Ctrl Pts',(-23.7,-55.7290034297554,-82.7720704820173));
#137321=CARTESIAN_POINT('Ctrl Pts',(-23.7,-55.6467059711238,-82.9654368402719));
#137322=CARTESIAN_POINT('Ctrl Pts',(-23.7,-55.5726850268912,-83.1620740930088));
#137323=CARTESIAN_POINT('Ctrl Pts',(-23.7,-55.5066653875374,-83.3608873091131));
#137324=CARTESIAN_POINT('Ctrl Pts',(-23.7,-55.4379479535128,-83.5678247325012));
#137325=CARTESIAN_POINT('Ctrl Pts',(-23.7,-55.3778989830438,-83.7771208288598));
#137326=CARTESIAN_POINT('Ctrl Pts',(-23.7,-55.326260979212,-83.9875567996247));
#137327=CARTESIAN_POINT('Ctrl Pts',(-23.7,-55.3186643927326,-84.0185145232327));
#137328=CARTESIAN_POINT('Ctrl Pts',(-23.7,-55.3112499282573,-84.0494969228628));
#137329=CARTESIAN_POINT('Ctrl Pts',(-23.7,-55.304016859788,-84.0805001191198));
#137330=CARTESIAN_POINT('Ctrl Pts',(-23.7,-55.2100486983101,-84.4832770822498));
#137331=CARTESIAN_POINT('Ctrl Pts',(-23.7,-55.1455757138289,-84.8909305418239));
#137332=CARTESIAN_POINT('Ctrl Pts',(-23.7,-55.1107223807414,-85.3034811063171));
#137333=CARTESIAN_POINT('Ctrl Pts',(-23.7,-55.090251973458,-85.5457844194304));
#137334=CARTESIAN_POINT('Ctrl Pts',(-23.7,-55.0800000200001,-85.7897771817878));
#137335=CARTESIAN_POINT('Ctrl Pts',(-23.7,-55.08000002,-86.035464915697));
#137336=CARTESIAN_POINT('Ctrl Pts',(-23.7,-66.9393955463102,-61.0621827299711));
#137337=CARTESIAN_POINT('Ctrl Pts',(-23.7,-63.3447563953728,-68.1443309684329));
#137338=CARTESIAN_POINT('Ctrl Pts',(-23.7,-59.7084420726901,-75.2049156266561));
#137339=CARTESIAN_POINT('Ctrl Pts',(-23.7,-55.9902808012637,-82.2231510113772));
#137340=CARTESIAN_POINT('Origin',(-24.2,-73.08000002,-55.74995));
#137341=CARTESIAN_POINT('Origin',(-24.2,-70.08000002,-55.74995));
#137342=CARTESIAN_POINT('Origin',(0.,-12.9675000200281,-61.64995));
#137343=CARTESIAN_POINT('',(-22.3259225534138,40.6914751389564,-61.2273317382593));
#137344=CARTESIAN_POINT('',(-28.2795019009908,37.8065307949999,-61.2273317382593));
#137345=CARTESIAN_POINT('Origin',(0.,-12.9675000200281,-61.2273317382593));
#137346=CARTESIAN_POINT('Ctrl Pts',(-28.4933647440612,38.6927858841383,
-60.650327573148));
#137347=CARTESIAN_POINT('Ctrl Pts',(-28.4508217728044,38.5151017970219,
-60.6551690977179));
#137348=CARTESIAN_POINT('Ctrl Pts',(-28.4075947879363,38.335472514688,-60.707925961796));
#137349=CARTESIAN_POINT('Ctrl Pts',(-28.3514280416523,38.1029959208976,
-60.8540715547449));
#137350=CARTESIAN_POINT('Ctrl Pts',(-28.3338483525148,38.0303960306507,
-60.9145171861254));
#137351=CARTESIAN_POINT('Ctrl Pts',(-28.302912455342,37.9028346914031,-61.0569005178125));
#137352=CARTESIAN_POINT('Ctrl Pts',(-28.28982523324,37.8489775515987,-61.1370349799883));
#137353=CARTESIAN_POINT('Ctrl Pts',(-28.2795019009908,37.8065307949999,
-61.2273317382593));
#137354=CARTESIAN_POINT('Origin',(-22.4949668999609,41.5737931892869,-61.6552254095787));
#137355=CARTESIAN_POINT('Ctrl Pts',(-22.3089577584378,40.9899884313956,
-60.5010370523947));
#137356=CARTESIAN_POINT('Ctrl Pts',(-22.,41.1177283573993,-60.5010370523946));
#137357=CARTESIAN_POINT('Ctrl Pts',(-22.,41.4520521304013,-60.5010370523947));
#137358=CARTESIAN_POINT('Ctrl Pts',(-22.3089577682091,40.9899884273556,
-60.7079658702078));
#137359=CARTESIAN_POINT('Ctrl Pts',(-22.,41.1177283336776,-60.7368788147381));
#137360=CARTESIAN_POINT('Ctrl Pts',(-22.,41.4520521024983,-60.811367390836));
#137361=CARTESIAN_POINT('Ctrl Pts',(-22.3211558478618,40.913825471773,-60.9106181484486));
#137362=CARTESIAN_POINT('Ctrl Pts',(-21.9999999999979,41.0241336396768,
-60.969503986646));
#137363=CARTESIAN_POINT('Ctrl Pts',(-22.,41.345292929857,-61.115492429943));
#137364=CARTESIAN_POINT('Ctrl Pts',(-22.3428990418276,40.7794755973204,
-61.0754935261973));
#137365=CARTESIAN_POINT('Ctrl Pts',(-22.,40.8698280768405,-61.1441646043173));
#137366=CARTESIAN_POINT('Ctrl Pts',(-22.,41.1573899115079,-61.3627217630986));
#137367=CARTESIAN_POINT('',(-22.,41.1573899115079,-61.3627217630986));
#137368=CARTESIAN_POINT('Origin',(-22.,40.1816528161032,-60.6046736522198));
#137369=CARTESIAN_POINT('Origin',(-22.5,41.1573899115079,-61.3627217630986));
#137370=CARTESIAN_POINT('Origin',(-22.,-9.33460238845303,-92.34995));
#137371=CARTESIAN_POINT('',(-22.,43.91999998,-55.74995));
#137372=CARTESIAN_POINT('',(-22.,41.1166950488946,-55.74995));
#137373=CARTESIAN_POINT('',(-22.,46.41999998,-58.24995));
#137374=CARTESIAN_POINT('Origin',(-22.,43.91999998,-58.24995));
#137375=CARTESIAN_POINT('',(-22.,46.41999998,-58.24995));
#137376=CARTESIAN_POINT('',(-22.,28.9199999800001,-91.34995));
#137377=CARTESIAN_POINT('Origin',(-22.,29.41999998,-91.34995));
#137378=CARTESIAN_POINT('',(-22.,28.9199999800001,-87.1305533863517));
#137379=CARTESIAN_POINT('',(-22.,28.9199999800001,-91.34995));
#137380=CARTESIAN_POINT('',(-22.,29.8104512658091,-83.3922397161652));
#137381=CARTESIAN_POINT('Ctrl Pts',(-22.,29.8104512658092,-83.3922397161652));
#137382=CARTESIAN_POINT('Ctrl Pts',(-22.,29.7130107699212,-83.5771800425296));
#137383=CARTESIAN_POINT('Ctrl Pts',(-22.,29.6241027734271,-83.7664339874128));
#137384=CARTESIAN_POINT('Ctrl Pts',(-22.,29.5434345930966,-83.9588738468729));
#137385=CARTESIAN_POINT('Ctrl Pts',(-22.,29.4578017187799,-84.1631573478911));
#137386=CARTESIAN_POINT('Ctrl Pts',(-22.,29.3814538044553,-84.3710319263885));
#137387=CARTESIAN_POINT('Ctrl Pts',(-22.,29.3140928258487,-84.5811807101613));
#137388=CARTESIAN_POINT('Ctrl Pts',(-22.,29.2470690502147,-84.7902775081102));
#137389=CARTESIAN_POINT('Ctrl Pts',(-22.,29.1889427079809,-85.0016271465761));
#137390=CARTESIAN_POINT('Ctrl Pts',(-22.,29.1394698146751,-85.2139452109128));
#137391=CARTESIAN_POINT('Ctrl Pts',(-22.,29.0466872110909,-85.6121313989602));
#137392=CARTESIAN_POINT('Ctrl Pts',(-22.,28.9832164657706,-86.0152044949726));
#137393=CARTESIAN_POINT('Ctrl Pts',(-22.,28.9492578229232,-86.4231979120772));
#137394=CARTESIAN_POINT('Ctrl Pts',(-22.,28.9297677681886,-86.6573596265608));
#137395=CARTESIAN_POINT('Ctrl Pts',(-22.,28.9199999800002,-86.893142259867));
#137396=CARTESIAN_POINT('Ctrl Pts',(-22.,28.91999998,-87.1305533863517));
#137397=CARTESIAN_POINT('',(-22.,41.1098595241823,-61.4386408691296));
#137398=CARTESIAN_POINT('Ctrl Pts',(-22.,41.1098595241823,-61.4386408691296));
#137399=CARTESIAN_POINT('Ctrl Pts',(-22.,37.3993520818416,-68.7853105030709));
#137400=CARTESIAN_POINT('Ctrl Pts',(-22.,33.6470396305176,-76.1104633065809));
#137401=CARTESIAN_POINT('Ctrl Pts',(-22.,29.8104512658091,-83.3922397161652));
#137402=CARTESIAN_POINT('Origin',(-22.,41.5483105744971,-61.66030212062));
#137403=CARTESIAN_POINT('Origin',(-21.5,0.,-55.74995));
#137404=CARTESIAN_POINT('',(-21.5,43.91999998,-55.24995));
#137405=CARTESIAN_POINT('',(-21.5,43.91999998,-55.24995));
#137406=CARTESIAN_POINT('Origin',(-21.5,43.91999998,-55.74995));
#137407=CARTESIAN_POINT('Origin',(0.,0.,-55.24995));
#137408=CARTESIAN_POINT('',(-21.,43.91999998,-55.24995));
#137409=CARTESIAN_POINT('',(-21.,41.7028772994424,-55.24995));
#137410=CARTESIAN_POINT('',(0.,43.91999998,-55.24995));
#137411=CARTESIAN_POINT('Origin',(-21.,-9.33460238845303,-55.74995));
#137412=CARTESIAN_POINT('',(-20.5,43.91999998,-55.74995));
#137413=CARTESIAN_POINT('',(-20.5,43.91999998,-55.74995));
#137414=CARTESIAN_POINT('Origin',(-21.,43.91999998,-55.74995));
#137415=CARTESIAN_POINT('Origin',(-20.5,-9.33460238845303,-92.34995));
#137416=CARTESIAN_POINT('',(-20.5,42.270218132516,-61.0621827299711));
#137417=CARTESIAN_POINT('Origin',(-20.5000001497348,40.8982420778451,-60.4432551283365));
#137418=CARTESIAN_POINT('',(-20.5,29.726759920701,-85.9392854774869));
#137419=CARTESIAN_POINT('Ctrl Pts',(-20.5,29.726759920701,-85.9392854774869));
#137420=CARTESIAN_POINT('Ctrl Pts',(-20.5,33.9784770268254,-77.682497649623));
#137421=CARTESIAN_POINT('Ctrl Pts',(-20.5,38.1440239783714,-69.3822613645965));
#137422=CARTESIAN_POINT('Ctrl Pts',(-20.5,42.270218132516,-61.0621827299711));
#137423=CARTESIAN_POINT('',(-20.5,28.9199999800001,-89.3628471840452));
#137424=CARTESIAN_POINT('Ctrl Pts',(-20.5,28.9199999800001,-89.3628471840452));
#137425=CARTESIAN_POINT('Ctrl Pts',(-20.5,28.9199999800001,-89.0651820878934));
#137426=CARTESIAN_POINT('Ctrl Pts',(-20.5,28.93706429112,-88.7687961767652));
#137427=CARTESIAN_POINT('Ctrl Pts',(-20.5,29.004819730958,-88.1785451079783));
#137428=CARTESIAN_POINT('Ctrl Pts',(-20.5,29.0556764864843,-87.8849108068938));
#137429=CARTESIAN_POINT('Ctrl Pts',(-20.5,29.2565698843866,-87.0234827289138));
#137430=CARTESIAN_POINT('Ctrl Pts',(-20.5,29.453814841029,-86.4693418183145));
#137431=CARTESIAN_POINT('Ctrl Pts',(-20.5,29.726759920701,-85.9392854774869));
#137432=CARTESIAN_POINT('',(-20.5,28.9199999800001,-91.34995));
#137433=CARTESIAN_POINT('',(-20.5,28.9199999800001,-88.9338641536579));
#137434=CARTESIAN_POINT('Origin',(-20.5,29.41999998,-91.34995));
#137435=CARTESIAN_POINT('',(-20.5,46.41999998,-58.24995));
#137436=CARTESIAN_POINT('',(-20.5,46.41999998,-92.34995));
#137437=CARTESIAN_POINT('Origin',(-20.5,43.91999998,-58.24995));
#137438=CARTESIAN_POINT('Ctrl Pts',(-19.8489174898872,41.8225779837155,
-60.8897941554007));
#137439=CARTESIAN_POINT('Ctrl Pts',(-20.5000844423968,41.6420275017582,
-60.7898798297297));
#137440=CARTESIAN_POINT('Ctrl Pts',(-20.4999999961793,42.2396703210244,
-61.1205979678028));
#137441=CARTESIAN_POINT('Ctrl Pts',(-19.8355865710622,41.9126116301234,
-60.7356962259096));
#137442=CARTESIAN_POINT('Ctrl Pts',(-20.5000878549352,41.6934063086951,
-60.6536629857367));
#137443=CARTESIAN_POINT('Ctrl Pts',(-20.4999999961011,42.3674932175841,
-60.8894198661636));
#137444=CARTESIAN_POINT('Ctrl Pts',(-19.8290476963325,41.9571155016239,
-60.5621838877489));
#137445=CARTESIAN_POINT('Ctrl Pts',(-20.5000896090863,41.710625264557,-60.5273413240715));
#137446=CARTESIAN_POINT('Ctrl Pts',(-20.4999999960627,42.4307087138456,
-60.6291716490909));
#137447=CARTESIAN_POINT('Ctrl Pts',(-19.8303467534611,41.9482798096484,
-60.383760106758));
#137448=CARTESIAN_POINT('Ctrl Pts',(-20.5000892602552,41.7070302221805,
-60.3953720501034));
#137449=CARTESIAN_POINT('Ctrl Pts',(-20.4999999960704,42.4181586164624,
-60.3615059809689));
#137450=CARTESIAN_POINT('Origin',(-20.,42.270218132516,-61.0621827299711));
#137451=CARTESIAN_POINT('Origin',(0.,-12.9675000200281,-60.64995));
#137452=CARTESIAN_POINT('',(-19.8077681423597,29.3163998849126,-85.7279763868962));
#137453=CARTESIAN_POINT('',(-13.8582614853459,29.115831713372,-90.8469388041467));
#137454=CARTESIAN_POINT('Ctrl Pts',(-19.8077680666401,29.3163999141123,
-85.7279763466165));
#137455=CARTESIAN_POINT('Ctrl Pts',(-18.8664797933811,29.281909340585,-86.6512762314539));
#137456=CARTESIAN_POINT('Ctrl Pts',(-17.899945936779,29.2474791030901,-87.5495367943307));
#137457=CARTESIAN_POINT('Ctrl Pts',(-15.9119634012864,29.1799677018946,
-89.269473055814));
#137458=CARTESIAN_POINT('Ctrl Pts',(-14.8954908494031,29.1470358100342,
-90.0876330868643));
#137459=CARTESIAN_POINT('Ctrl Pts',(-13.8582614853459,29.115831713372,-90.8469388041467));
#137460=CARTESIAN_POINT('Ctrl Pts',(-19.8457268663587,41.8441333387867,
-60.8508735991007));
#137461=CARTESIAN_POINT('Ctrl Pts',(-19.8355385600285,37.7216554195719,
-69.1708971047811));
#137462=CARTESIAN_POINT('Ctrl Pts',(-19.8234665452012,33.5607487699413,
-77.4712163753771));
#137463=CARTESIAN_POINT('Ctrl Pts',(-19.8077680666401,29.3163999141123,
-85.7279763466165));
#137464=CARTESIAN_POINT('Ctrl Pts',(-13.8582614853459,29.115831713372,-90.8469388041467));
#137465=CARTESIAN_POINT('Ctrl Pts',(-13.8729899561679,34.0078013158341,
-80.8725774674286));
#137466=CARTESIAN_POINT('Ctrl Pts',(-13.8834224238665,38.8394159067996,
-70.867726207482));
#137467=CARTESIAN_POINT('Ctrl Pts',(-13.8920088064511,43.6468101642065,
-60.8508735991007));
#137468=CARTESIAN_POINT('Ctrl Pts',(-13.8812391026075,43.7449355503387,
-60.3843616038035));
#137469=CARTESIAN_POINT('Ctrl Pts',(-13.4999161431562,43.8380646295733,
-60.380129448632));
#137470=CARTESIAN_POINT('Ctrl Pts',(-13.5000000114112,44.2302441743789,
-60.3624063574045));
#137471=CARTESIAN_POINT('Ctrl Pts',(-13.8803600752771,43.7529853273083,
-60.5601847150614));
#137472=CARTESIAN_POINT('Ctrl Pts',(-13.4999163945295,43.8475317166231,
-60.5727811392321));
#137473=CARTESIAN_POINT('Ctrl Pts',(-13.5000000113849,44.2419957581614,
-60.6261785981702));
#137474=CARTESIAN_POINT('Ctrl Pts',(-13.884762026428,43.7126430688856,-60.7334063315744));
#137475=CARTESIAN_POINT('Ctrl Pts',(-13.4999151269544,43.7997377261502,
-60.7643333157514));
#137476=CARTESIAN_POINT('Ctrl Pts',(-13.5000000115167,44.1831007301226,
-60.8859969728056));
#137477=CARTESIAN_POINT('Ctrl Pts',(-13.8942821039575,43.6261495705425,
-60.8904677863889));
#137478=CARTESIAN_POINT('Ctrl Pts',(-13.4999123453879,43.7012956163656,
-60.9308210213385));
#137479=CARTESIAN_POINT('Ctrl Pts',(-13.5000000118016,44.0568479860271,
-61.1216298968641));
#137480=CARTESIAN_POINT('',(-13.5,44.086908282047,-61.0621827299711));
#137481=CARTESIAN_POINT('Origin',(-13.4999995641033,42.8035277780889,-60.452854070096));
#137482=CARTESIAN_POINT('Origin',(-14.,44.086908282047,-61.0621827299711));
#137483=CARTESIAN_POINT('Origin',(-13.5,-9.33460238845303,-92.34995));
#137484=CARTESIAN_POINT('',(-13.5,46.41999998,-58.2497627936531));
#137485=CARTESIAN_POINT('Ctrl Pts',(-13.5,46.41999998,-58.2497627936531));
#137486=CARTESIAN_POINT('Ctrl Pts',(-13.5,46.41999998,-58.1672776827351));
#137487=CARTESIAN_POINT('Ctrl Pts',(-13.5,46.4159357655689,-58.0853150765278));
#137488=CARTESIAN_POINT('Ctrl Pts',(-13.5,46.4079129436513,-58.0040039069954));
#137489=CARTESIAN_POINT('Ctrl Pts',(-13.5,46.3998480609524,-57.9222664521287));
#137490=CARTESIAN_POINT('Ctrl Pts',(-13.5,46.3877828714201,-57.8411867135011));
#137491=CARTESIAN_POINT('Ctrl Pts',(-13.4999999999999,46.371771733687,-57.7608954152445));
#137492=CARTESIAN_POINT('Ctrl Pts',(-13.4999999999999,46.3557907741679,
-57.6807554521414));
#137493=CARTESIAN_POINT('Ctrl Pts',(-13.4999999999998,46.3358786103981,
-57.6014003971059));
#137494=CARTESIAN_POINT('Ctrl Pts',(-13.4999999999993,46.3120383093697,
-57.5229684754948));
#137495=CARTESIAN_POINT('Ctrl Pts',(-13.499999999999,46.2959527721241,-57.4700488586319));
#137496=CARTESIAN_POINT('Ctrl Pts',(-13.4999999999985,46.2780779115088,
-57.4175496722019));
#137497=CARTESIAN_POINT('Ctrl Pts',(-13.4999999999976,46.2584018781846,
-57.3655174652213));
#137498=CARTESIAN_POINT('Ctrl Pts',(-13.4999999999975,46.2569427240896,
-57.361658811059));
#137499=CARTESIAN_POINT('Ctrl Pts',(-13.4999999999974,46.2554739003334,
-57.3578033707196));
#137500=CARTESIAN_POINT('Ctrl Pts',(-13.4999999999974,46.2539954124749,
-57.3539511680007));
#137501=CARTESIAN_POINT('Ctrl Pts',(-13.4999999999961,46.2196721389242,
-57.264521818319));
#137502=CARTESIAN_POINT('Ctrl Pts',(-13.4999999999986,46.1805716042443,
-57.1778714284216));
#137503=CARTESIAN_POINT('Ctrl Pts',(-13.4999999999971,46.1367457679121,
-57.0938423224747));
#137504=CARTESIAN_POINT('Ctrl Pts',(-13.4999999999963,46.1131655316067,
-57.048630950814));
#137505=CARTESIAN_POINT('Ctrl Pts',(-13.4999999999953,46.0882165583818,
-57.0041788421782));
#137506=CARTESIAN_POINT('Ctrl Pts',(-13.4999999999852,46.0619014378574,
-56.9604643403199));
#137507=CARTESIAN_POINT('Ctrl Pts',(-13.499999999984,46.0587398032398,-56.9552122540816));
#137508=CARTESIAN_POINT('Ctrl Pts',(-13.4999999999826,46.0555586143243,
-56.9499710767904));
#137509=CARTESIAN_POINT('Ctrl Pts',(-13.4999999999808,46.0523578866491,
-56.9447407904478));
#137510=CARTESIAN_POINT('Ctrl Pts',(-13.4999999999437,45.9841670777506,
-56.8333106743423));
#137511=CARTESIAN_POINT('Ctrl Pts',(-13.4999999995698,45.9062654719925,
-56.7259689765242));
#137512=CARTESIAN_POINT('Ctrl Pts',(-13.4999999997703,45.8207975744209,
-56.6258771140548));
#137513=CARTESIAN_POINT('Ctrl Pts',(-13.4999999997905,45.8121551558504,
-56.6157559364485));
#137514=CARTESIAN_POINT('Ctrl Pts',(-13.4999999998158,45.803435351972,-56.6057089285391));
#137515=CARTESIAN_POINT('Ctrl Pts',(-13.4999999998434,45.7946403691178,
-56.5957393884661));
#137516=CARTESIAN_POINT('Ctrl Pts',(-13.4999999998604,45.7891977407958,
-56.5895699050165));
#137517=CARTESIAN_POINT('Ctrl Pts',(-13.4999999998752,45.7837267069276,
-56.5834303340926));
#137518=CARTESIAN_POINT('Ctrl Pts',(-13.4999999998881,45.7782278023011,
-56.5773214434301));
#137519=CARTESIAN_POINT('Ctrl Pts',(-13.5000000001116,45.6828400874147,
-56.4713524986363));
#137520=CARTESIAN_POINT('Ctrl Pts',(-13.5000000000272,45.5794120988332,
-56.3745067808491));
#137521=CARTESIAN_POINT('Ctrl Pts',(-13.4999999999695,45.4679575974401,
-56.2866310284186));
#137522=CARTESIAN_POINT('Ctrl Pts',(-13.4999999999653,45.4599257124734,
-56.2802983282937));
#137523=CARTESIAN_POINT('Ctrl Pts',(-13.4999999999594,45.4518518043016,
-56.2740118496438));
#137524=CARTESIAN_POINT('Ctrl Pts',(-13.4999999999509,45.443735968515,-56.2677716701563));
#137525=CARTESIAN_POINT('Ctrl Pts',(-13.4999999998703,45.3663292591539,
-56.2082544777619));
#137526=CARTESIAN_POINT('Ctrl Pts',(-13.4999999992365,45.2845712727005,
-56.1527648487186));
#137527=CARTESIAN_POINT('Ctrl Pts',(-13.4999999991445,45.2001155591245,
-56.1023854625873));
#137528=CARTESIAN_POINT('Ctrl Pts',(-13.4999999991047,45.1634675983669,
-56.0805242801078));
#137529=CARTESIAN_POINT('Ctrl Pts',(-13.4999999992486,45.1263121785351,
-56.0596248906736));
#137530=CARTESIAN_POINT('Ctrl Pts',(-13.4999999995196,45.0887860427418,
-56.0397731680737));
#137531=CARTESIAN_POINT('Ctrl Pts',(-13.4999999995982,45.0778983802498,
-56.0340134794998));
#137532=CARTESIAN_POINT('Ctrl Pts',(-13.4999999996575,45.0669811451102,
-56.0283421588346));
#137533=CARTESIAN_POINT('Ctrl Pts',(-13.4999999997046,45.0560369222135,
-56.022760797256));
#137534=CARTESIAN_POINT('Ctrl Pts',(-13.4999999999911,44.9893496905534,
-55.9887514796382));
#137535=CARTESIAN_POINT('Ctrl Pts',(-13.4999999999377,44.9212851553075,
-55.9578058140964));
#137536=CARTESIAN_POINT('Ctrl Pts',(-13.4999999999181,44.8519312666028,
-55.929946672226));
#137537=CARTESIAN_POINT('Ctrl Pts',(-13.4999999999016,44.7935541183746,
-55.9064968371143));
#137538=CARTESIAN_POINT('Ctrl Pts',(-13.4999999998496,44.7342628547594,
-55.8852345670545));
#137539=CARTESIAN_POINT('Ctrl Pts',(-13.4999999998385,44.6741009867898,
-55.8662006918549));
#137540=CARTESIAN_POINT('Ctrl Pts',(-13.4999999998288,44.62199348368,-55.8497150383234));
#137541=CARTESIAN_POINT('Ctrl Pts',(-13.4999999998617,44.5690884019707,
-55.834861773659));
#137542=CARTESIAN_POINT('Ctrl Pts',(-13.4999999998979,44.5156559887649,
-55.8217533863187));
#137543=CARTESIAN_POINT('Ctrl Pts',(-13.4999999999339,44.4624243034299,
-55.808694242846));
#137544=CARTESIAN_POINT('Ctrl Pts',(-13.4999999999687,44.4086696615078,
-55.7973670287965));
#137545=CARTESIAN_POINT('Ctrl Pts',(-13.4999999999845,44.3546736478475,
-55.7878333559404));
#137546=CARTESIAN_POINT('Ctrl Pts',(-13.4999999999965,44.3137472492199,
-55.7806072873986));
#137547=CARTESIAN_POINT('Ctrl Pts',(-13.4999999999993,44.27268252233,-55.7744105877407));
#137548=CARTESIAN_POINT('Ctrl Pts',(-13.4999999999998,44.2316053598049,
-55.7692503840784));
#137549=CARTESIAN_POINT('',(-13.5,46.41999998,-58.24995));
#137550=CARTESIAN_POINT('',(-13.5,29.8836583509375,-91.8408299848543));
#137551=CARTESIAN_POINT('Origin',(-13.5,29.9835150560362,-91.2987164399481));
#137552=CARTESIAN_POINT('',(-13.5,29.5044693674792,-91.1451435916293));
#137553=CARTESIAN_POINT('Ctrl Pts',(-13.5,29.5044693674792,-91.1451435916293));
#137554=CARTESIAN_POINT('Ctrl Pts',(-13.5,29.4871798972865,-91.1818706195726));
#137555=CARTESIAN_POINT('Ctrl Pts',(-13.5,29.4746493543107,-91.2204653406996));
#137556=CARTESIAN_POINT('Ctrl Pts',(-13.5,29.4670724885977,-91.259957519387));
#137557=CARTESIAN_POINT('Ctrl Pts',(-13.5,29.4602667842095,-91.2954302470261));
#137558=CARTESIAN_POINT('Ctrl Pts',(-13.5,29.4574580326191,-91.3316285116295));
#137559=CARTESIAN_POINT('Ctrl Pts',(-13.5000000000001,29.4588194335385,
-91.3678650371612));
#137560=CARTESIAN_POINT('Ctrl Pts',(-13.5000000000001,29.4588222728777,
-91.367940612098));
#137561=CARTESIAN_POINT('Ctrl Pts',(-13.5000000000001,29.4588251305407,
-91.3680161857943));
#137562=CARTESIAN_POINT('Ctrl Pts',(-13.5000000000001,29.4588280065244,
-91.3680917582431));
#137563=CARTESIAN_POINT('Ctrl Pts',(-13.5000000000004,29.4617431600592,
-91.4446934778138));
#137564=CARTESIAN_POINT('Ctrl Pts',(-13.4999999999999,29.483485076552,-91.5200098118263));
#137565=CARTESIAN_POINT('Ctrl Pts',(-13.5000000000001,29.5206532241076,
-91.5861460983069));
#137566=CARTESIAN_POINT('Ctrl Pts',(-13.5000000000001,29.5206776694618,
-91.5861895958997));
#137567=CARTESIAN_POINT('Ctrl Pts',(-13.5000000000001,29.5207021217052,
-91.5862330898687));
#137568=CARTESIAN_POINT('Ctrl Pts',(-13.5000000000001,29.5207265808359,
-91.5862765802124));
#137569=CARTESIAN_POINT('Ctrl Pts',(-13.5000000000003,29.5579279046594,
-91.6524235901087));
#137570=CARTESIAN_POINT('Ctrl Pts',(-13.5,29.6110672833213,-91.710189265371));
#137571=CARTESIAN_POINT('Ctrl Pts',(-13.5,29.6735560708361,-91.7536723853085));
#137572=CARTESIAN_POINT('Ctrl Pts',(-13.5,29.6735766131945,-91.7536866798063));
#137573=CARTESIAN_POINT('Ctrl Pts',(-13.5,29.6735971566538,-91.7537009728318));
#137574=CARTESIAN_POINT('Ctrl Pts',(-13.5,29.6736177012137,-91.753715264385));
#137575=CARTESIAN_POINT('Ctrl Pts',(-13.5,29.6935761704139,-91.7675991112376));
#137576=CARTESIAN_POINT('Ctrl Pts',(-13.5,29.7144903240442,-91.7800410703758));
#137577=CARTESIAN_POINT('Ctrl Pts',(-13.5,29.7361680987988,-91.7910278638481));
#137578=CARTESIAN_POINT('Ctrl Pts',(-13.5,29.7580697930564,-91.8021281448607));
#137579=CARTESIAN_POINT('Ctrl Pts',(-13.5,29.7807523109198,-91.8117435399084));
#137580=CARTESIAN_POINT('Ctrl Pts',(-13.5,29.8040427282676,-91.8198138783841));
#137581=CARTESIAN_POINT('Ctrl Pts',(-13.5,29.826683860785,-91.8276592338433));
#137582=CARTESIAN_POINT('Ctrl Pts',(-13.5,29.8499007708162,-91.8340446948145));
#137583=CARTESIAN_POINT('Ctrl Pts',(-13.5,29.8735386060562,-91.8388665069537));
#137584=CARTESIAN_POINT('Ctrl Pts',(-13.5,29.8769034909808,-91.8395528998831));
#137585=CARTESIAN_POINT('Ctrl Pts',(-13.5,29.88027689369,-91.8402075213397));
#137586=CARTESIAN_POINT('Ctrl Pts',(-13.5,29.8836583509375,-91.8408299848543));
#137587=CARTESIAN_POINT('',(-13.5,29.5462485400348,-91.058247935017));
#137588=CARTESIAN_POINT('Ctrl Pts',(-13.5,29.5462485400348,-91.058247935017));
#137589=CARTESIAN_POINT('Ctrl Pts',(-13.5,29.5320849211775,-91.0870978945881));
#137590=CARTESIAN_POINT('Ctrl Pts',(-13.5,29.5181581265359,-91.1160653155134));
#137591=CARTESIAN_POINT('Ctrl Pts',(-13.5,29.5044693674783,-91.1451435916289));
#137592=CARTESIAN_POINT('Ctrl Pts',(-13.5,44.086908282047,-61.0621827299711));
#137593=CARTESIAN_POINT('Ctrl Pts',(-13.5,39.2774232822218,-71.079001631676));
#137594=CARTESIAN_POINT('Ctrl Pts',(-13.5,34.4431166252676,-81.0837881795346));
#137595=CARTESIAN_POINT('Ctrl Pts',(-13.5,29.5462485400348,-91.058247935017));
#137596=CARTESIAN_POINT('Ctrl Pts',(-13.5,46.41999998,-58.2497627936531));
#137597=CARTESIAN_POINT('Ctrl Pts',(-13.5,46.9199999800001,-58.2497627936531));
#137598=CARTESIAN_POINT('Ctrl Pts',(-13.,46.91999998,-58.2497627936531));
#137599=CARTESIAN_POINT('Ctrl Pts',(-13.5,46.4199999716718,-57.9435058971265));
#137600=CARTESIAN_POINT('Ctrl Pts',(-13.5,46.9198475451862,-57.8823102041449));
#137601=CARTESIAN_POINT('Ctrl Pts',(-13.0001524477397,46.91999998,-57.8822548982638));
#137602=CARTESIAN_POINT('Ctrl Pts',(-13.5,46.363911922201,-57.6403398562409));
#137603=CARTESIAN_POINT('Ctrl Pts',(-13.5000000000013,46.8524085179432,
-57.5185641386525));
#137604=CARTESIAN_POINT('Ctrl Pts',(-13.0003057176052,46.8526943145044,
-57.5184560311191));
#137605=CARTESIAN_POINT('Ctrl Pts',(-13.5,46.1990348882699,-57.2107576948721));
#137606=CARTESIAN_POINT('Ctrl Pts',(-13.4999999999993,46.6543661205181,
-57.0031847607698));
#137607=CARTESIAN_POINT('Ctrl Pts',(-13.0005259614006,46.6548418679923,
-57.0029579960184));
#137608=CARTESIAN_POINT('Ctrl Pts',(-13.5,46.1317137634759,-57.0744145874655));
#137609=CARTESIAN_POINT('Ctrl Pts',(-13.5000000000001,46.5735338055633,
-56.8396334804064));
#137610=CARTESIAN_POINT('Ctrl Pts',(-13.0005963858014,46.5740565196337,
-56.8393464452647));
#137611=CARTESIAN_POINT('Ctrl Pts',(-13.5,45.9729945411748,-56.8150715642796));
#137612=CARTESIAN_POINT('Ctrl Pts',(-13.4999999999999,46.3829981626758,
-56.5285611340859));
#137613=CARTESIAN_POINT('Ctrl Pts',(-13.0007311732941,46.3835934539471,
-56.5281351595755));
#137614=CARTESIAN_POINT('Ctrl Pts',(-13.5,45.8804524549659,-56.6909184744131));
#137615=CARTESIAN_POINT('Ctrl Pts',(-13.4999999999992,46.2719244986749,
-56.3796526797414));
#137616=CARTESIAN_POINT('Ctrl Pts',(-13.0007961467471,46.2725429511699,
-56.3791516167841));
#137617=CARTESIAN_POINT('Ctrl Pts',(-13.5,45.6759874229978,-56.4637385666375));
#137618=CARTESIAN_POINT('Ctrl Pts',(-13.5000000000008,46.0265477969208,
-56.1071944318285));
#137619=CARTESIAN_POINT('Ctrl Pts',(-13.0009156805798,46.0271849103864,
-56.1065360355095));
#137620=CARTESIAN_POINT('Ctrl Pts',(-13.5,45.5644586309065,-56.3605915480362));
#137621=CARTESIAN_POINT('Ctrl Pts',(-13.5,45.892718112414,-55.9834952073023));
#137622=CARTESIAN_POINT('Ctrl Pts',(-13.0009702923331,45.8933503604458,
-55.9827597531144));
#137623=CARTESIAN_POINT('Ctrl Pts',(-13.5,45.3230047666778,-56.1749628998404));
#137624=CARTESIAN_POINT('Ctrl Pts',(-13.5,45.6030118434335,-55.7608945639374));
#137625=CARTESIAN_POINT('Ctrl Pts',(-13.0010689871371,45.6036057246554,
-55.7600056274797));
#137626=CARTESIAN_POINT('Ctrl Pts',(-13.5,45.1917816064929,-56.0920265457655));
#137627=CARTESIAN_POINT('Ctrl Pts',(-13.5,45.4455768559353,-55.6614429290966));
#137628=CARTESIAN_POINT('Ctrl Pts',(-13.0011133171869,45.4461379323356,
-55.6604821166903));
#137629=CARTESIAN_POINT('Ctrl Pts',(-13.5,44.7845241217188,-55.8842752341532));
#137630=CARTESIAN_POINT('Ctrl Pts',(-13.5,44.9570225707288,-55.4123450088757));
#137631=CARTESIAN_POINT('Ctrl Pts',(-13.0012246935303,44.9574289489744,
-55.4111808336381));
#137632=CARTESIAN_POINT('Ctrl Pts',(-13.5,44.4886526268701,-55.795999572546));
#137633=CARTESIAN_POINT('Ctrl Pts',(-13.4999999999989,44.6020983302816,
-55.3064963379004));
#137634=CARTESIAN_POINT('Ctrl Pts',(-13.0012724779463,44.6023831565444,
-55.3052501647884));
#137635=CARTESIAN_POINT('Ctrl Pts',(-13.5,44.1833084789809,-55.7636597096568));
#137636=CARTESIAN_POINT('Ctrl Pts',(-13.5,44.2358346644988,-55.2677218601875));
#137637=CARTESIAN_POINT('Ctrl Pts',(-13.0012899687735,44.235970178777,-55.2664423715086));
#137638=CARTESIAN_POINT('',(-13.,46.91999998,-58.2497627936531));
#137639=CARTESIAN_POINT('Ctrl Pts',(-13.0012809038513,44.3884784473357,
-55.2865609247418));
#137640=CARTESIAN_POINT('Ctrl Pts',(-13.0012586427657,44.7007920382812,
-55.3359516716537));
#137641=CARTESIAN_POINT('Ctrl Pts',(-13.0012143439801,45.00284180769,-55.4343469392968));
#137642=CARTESIAN_POINT('Ctrl Pts',(-13.0011133171869,45.4461379323356,
-55.6604821166903));
#137643=CARTESIAN_POINT('Ctrl Pts',(-13.0010689871371,45.6036057246554,
-55.7600056274797));
#137644=CARTESIAN_POINT('Ctrl Pts',(-13.0009702923331,45.8933503604458,
-55.9827597531144));
#137645=CARTESIAN_POINT('Ctrl Pts',(-13.0009156805798,46.0271849103864,
-56.1065360355095));
#137646=CARTESIAN_POINT('Ctrl Pts',(-13.0007961467471,46.2725429511699,
-56.3791516167841));
#137647=CARTESIAN_POINT('Ctrl Pts',(-13.0007311732941,46.3835934539471,
-56.5281351595755));
#137648=CARTESIAN_POINT('Ctrl Pts',(-13.0005963858014,46.5740565196337,
-56.8393464452647));
#137649=CARTESIAN_POINT('Ctrl Pts',(-13.0005259614006,46.6548418679923,
-57.0029579960184));
#137650=CARTESIAN_POINT('Ctrl Pts',(-13.0003057176052,46.8526943145044,
-57.5184560311191));
#137651=CARTESIAN_POINT('Ctrl Pts',(-13.0001524477397,46.91999998,-57.8822548982638));
#137652=CARTESIAN_POINT('Ctrl Pts',(-13.,46.91999998,-58.2497627936531));
#137653=CARTESIAN_POINT('Origin',(-13.,46.41999998,-58.2497627936531));
#137654=CARTESIAN_POINT('Ctrl Pts',(-12.4707855792057,46.91999998,-58.2462412559184));
#137655=CARTESIAN_POINT('Ctrl Pts',(-12.4974463012635,46.91999998,-55.7446487532608));
#137656=CARTESIAN_POINT('Ctrl Pts',(-12.5022360800201,44.4589702388884,
-55.2952207669972));
#137657=CARTESIAN_POINT('Ctrl Pts',(-12.6482571751841,46.91999998,-58.2481326596478));
#137658=CARTESIAN_POINT('Ctrl Pts',(-12.669673221037,46.9199999799984,-55.7170654011474));
#137659=CARTESIAN_POINT('Ctrl Pts',(-12.6722965314191,44.424983519038,-55.2908259090656));
#137660=CARTESIAN_POINT('Ctrl Pts',(-12.8257146119078,46.91999998,-58.2493381002745));
#137661=CARTESIAN_POINT('Ctrl Pts',(-12.840428652506,46.9199999800016,-55.6879841619109));
#137662=CARTESIAN_POINT('Ctrl Pts',(-12.841697295306,44.3903034748056,-55.2862462023721));
#137663=CARTESIAN_POINT('Ctrl Pts',(-13.0031560751435,46.91999998,-58.2497705672942));
#137664=CARTESIAN_POINT('Ctrl Pts',(-13.0094744794619,46.91999998,-55.6573244385171));
#137665=CARTESIAN_POINT('Ctrl Pts',(-13.0103905133279,44.3549359954418,
-55.2814750420178));
#137666=CARTESIAN_POINT('',(-12.5,46.91999998,-58.2465463958495));
#137667=CARTESIAN_POINT('Ctrl Pts',(-12.5,46.91999998,-58.2465463958495));
#137668=CARTESIAN_POINT('Ctrl Pts',(-12.5005968089278,46.91999998,-57.8965394261518));
#137669=CARTESIAN_POINT('Ctrl Pts',(-12.5011890520215,46.8598614514991,
-57.5537408849781));
#137670=CARTESIAN_POINT('Ctrl Pts',(-12.5023407943396,46.6211347792778,
-56.8949802448316));
#137671=CARTESIAN_POINT('Ctrl Pts',(-12.5028756040753,46.4475853737583,
-56.5931100772464));
#137672=CARTESIAN_POINT('Ctrl Pts',(-12.503595797933,46.111455620038,-56.190236748787));
#137673=CARTESIAN_POINT('Ctrl Pts',(-12.5038165641686,45.9892097344963,
-56.0674068194903));
#137674=CARTESIAN_POINT('Ctrl Pts',(-12.5042197091625,45.7249560267766,
-55.8439466125607));
#137675=CARTESIAN_POINT('Ctrl Pts',(-12.5044033037043,45.5817611915078,
-55.7426504905235));
#137676=CARTESIAN_POINT('Ctrl Pts',(-12.5048753578165,45.1362912829311,
-55.482949899381));
#137677=CARTESIAN_POINT('Ctrl Pts',(-12.5050937333589,44.8192497088676,
-55.3638128672415));
#137678=CARTESIAN_POINT('Ctrl Pts',(-12.5052115625557,44.4820814550628,
-55.2995670619079));
#137679=CARTESIAN_POINT('Origin',(-13.1654225534,46.91999998,6.33069708304167));
#137680=CARTESIAN_POINT('Ctrl Pts',(-12.5,46.91999998,-58.2465463958495));
#137681=CARTESIAN_POINT('Ctrl Pts',(-12.,46.91999998,-58.2465463958495));
#137682=CARTESIAN_POINT('Ctrl Pts',(-12.,46.41999998,-58.2465463958495));
#137683=CARTESIAN_POINT('Ctrl Pts',(-12.5005968089278,46.91999998,-57.8965394261518));
#137684=CARTESIAN_POINT('Ctrl Pts',(-12.0000000000051,46.9205971329195,
-57.8963321594437));
#137685=CARTESIAN_POINT('Ctrl Pts',(-12.,46.4199999720693,-57.9548688319462));
#137686=CARTESIAN_POINT('Ctrl Pts',(-12.5011890520215,46.8598614514991,
-57.5537408849781));
#137687=CARTESIAN_POINT('Ctrl Pts',(-12.,46.8609831927853,-57.553339017633));
#137688=CARTESIAN_POINT('Ctrl Pts',(-12.,46.3698845360764,-57.6691983000707));
#137689=CARTESIAN_POINT('Ctrl Pts',(-12.5023407943396,46.6211347792778,
-56.8949802448316));
#137690=CARTESIAN_POINT('Ctrl Pts',(-12.,46.6232060214067,-56.8937940810153));
#137691=CARTESIAN_POINT('Ctrl Pts',(-12.,46.170945649571,-57.1202211534365));
#137692=CARTESIAN_POINT('Ctrl Pts',(-12.5028756040753,46.4475853737583,
-56.5931100772464));
#137693=CARTESIAN_POINT('Ctrl Pts',(-11.9999999999992,46.4499499105921,
-56.5914299423666));
#137694=CARTESIAN_POINT('Ctrl Pts',(-12.,46.0263211387953,-56.8686580359845));
#137695=CARTESIAN_POINT('Ctrl Pts',(-12.503595797933,46.111455620038,-56.190236748787));
#137696=CARTESIAN_POINT('Ctrl Pts',(-12.0000000000004,46.1140832559457,
-56.187732860667));
#137697=CARTESIAN_POINT('Ctrl Pts',(-12.,45.7462130147,-56.5329239712738));
#137698=CARTESIAN_POINT('Ctrl Pts',(-12.5038165641686,45.9892097344963,
-56.0674068194903));
#137699=CARTESIAN_POINT('Ctrl Pts',(-12.0000000000004,45.9918445187629,
-56.0645984007596));
#137700=CARTESIAN_POINT('Ctrl Pts',(-12.,45.64434144227,-56.430563765138));
#137701=CARTESIAN_POINT('Ctrl Pts',(-12.5042197091625,45.7249560267766,
-55.8439466125607));
#137702=CARTESIAN_POINT('Ctrl Pts',(-11.9999999999996,45.7274985396918,
-55.840523660562));
#137703=CARTESIAN_POINT('Ctrl Pts',(-12.,45.4241300187908,-56.2443433906185));
#137704=CARTESIAN_POINT('Ctrl Pts',(-12.5044033037043,45.5817611915078,
-55.7426504905235));
#137705=CARTESIAN_POINT('Ctrl Pts',(-12.,45.584205738319,-55.7389336239012));
#137706=CARTESIAN_POINT('Ctrl Pts',(-12.,45.3048009887765,-56.159928342783));
#137707=CARTESIAN_POINT('Ctrl Pts',(-12.5048829251119,45.1291501474361,
-55.4787867514921));
#137708=CARTESIAN_POINT('Ctrl Pts',(-12.,45.1310727951979,-55.4742001436884));
#137709=CARTESIAN_POINT('Ctrl Pts',(-12.,44.9276251211566,-55.9400376669437));
#137710=CARTESIAN_POINT('Ctrl Pts',(-12.5051042651495,44.8038662560613,
-55.3580679820572));
#137711=CARTESIAN_POINT('Ctrl Pts',(-12.0000000000043,44.8053592277238,
-55.3530984350278));
#137712=CARTESIAN_POINT('Ctrl Pts',(-12.,44.6565552133068,-55.8394367317102));
#137713=CARTESIAN_POINT('Ctrl Pts',(-12.5052199580625,44.4575274683141,
-55.2949893590463));
#137714=CARTESIAN_POINT('Ctrl Pts',(-12.,44.4584726259965,-55.289799987766));
#137715=CARTESIAN_POINT('Ctrl Pts',(-12.,44.367939553595,-55.7868701958087));
#137716=CARTESIAN_POINT('',(-12.,46.41999998,-58.2465463958495));
#137717=CARTESIAN_POINT('Ctrl Pts',(-12.,44.7862606093016,-55.9010529569358));
#137718=CARTESIAN_POINT('Ctrl Pts',(-12.,44.8788753121625,-55.9352619713505));
#137719=CARTESIAN_POINT('Ctrl Pts',(-11.9999999998966,44.9692347958817,
-55.97494450417));
#137720=CARTESIAN_POINT('Ctrl Pts',(-12.0000000001034,45.0573639465272,
-56.0200426809306));
#137721=CARTESIAN_POINT('Ctrl Pts',(-12.0000000001611,45.0819593060305,
-56.0326288214102));
#137722=CARTESIAN_POINT('Ctrl Pts',(-12.0000000002553,45.106380862283,-56.0456370713463));
#137723=CARTESIAN_POINT('Ctrl Pts',(-12.0000000004528,45.1306289434624,
-56.0590668658914));
#137724=CARTESIAN_POINT('Ctrl Pts',(-12.0000000005851,45.1468544406639,
-56.0680533540261));
#137725=CARTESIAN_POINT('Ctrl Pts',(-12.0000000007159,45.1630095639554,
-56.0772339702066));
#137726=CARTESIAN_POINT('Ctrl Pts',(-12.0000000008214,45.179090134652,-56.0866066905108));
#137727=CARTESIAN_POINT('Ctrl Pts',(-12.0000000011901,45.2352779195468,
-56.1193562988592));
#137728=CARTESIAN_POINT('Ctrl Pts',(-12.0000000011541,45.2902554021734,
-56.1543787808436));
#137729=CARTESIAN_POINT('Ctrl Pts',(-12.0000000008796,45.3436294771403,
-56.1913642361009));
#137730=CARTESIAN_POINT('Ctrl Pts',(-12.0000000006945,45.3796048513584,
-56.2162932975288));
#137731=CARTESIAN_POINT('Ctrl Pts',(-12.0000000004393,45.4148522843585,
-56.242113151159));
#137732=CARTESIAN_POINT('Ctrl Pts',(-12.0000000002603,45.4492603972454,
-56.268719019813));
#137733=CARTESIAN_POINT('Ctrl Pts',(-12.0000000001101,45.478118138608,-56.2910330966957));
#137734=CARTESIAN_POINT('Ctrl Pts',(-12.0000000000612,45.5064639161954,
-56.3139578240496));
#137735=CARTESIAN_POINT('Ctrl Pts',(-12.0000000000338,45.5342394837982,
-56.3374491395215));
#137736=CARTESIAN_POINT('Ctrl Pts',(-11.9999999999739,45.5949303219838,
-56.3887786981631));
#137737=CARTESIAN_POINT('Ctrl Pts',(-12.,45.653197014408,-56.4429844895127));
#137738=CARTESIAN_POINT('Ctrl Pts',(-12.,45.7088856859487,-56.5000343749642));
#137739=CARTESIAN_POINT('Ctrl Pts',(-12.,45.7160867166438,-56.5074114224843));
#137740=CARTESIAN_POINT('Ctrl Pts',(-12.,45.7232446868776,-56.5148359705652));
#137741=CARTESIAN_POINT('Ctrl Pts',(-12.,45.7303593052335,-56.522307900516));
#137742=CARTESIAN_POINT('Ctrl Pts',(-12.,45.7679171901077,-56.5617520239876));
#137743=CARTESIAN_POINT('Ctrl Pts',(-12.,45.8043465692001,-56.6026021164951));
#137744=CARTESIAN_POINT('Ctrl Pts',(-12.,45.8395823893984,-56.6448353261774));
#137745=CARTESIAN_POINT('Ctrl Pts',(-12.,45.8717319797964,-56.6833694197455));
#137746=CARTESIAN_POINT('Ctrl Pts',(-12.,45.9026476453863,-56.7227444562638));
#137747=CARTESIAN_POINT('Ctrl Pts',(-12.,45.9322838293524,-56.7628973708158));
#137748=CARTESIAN_POINT('Ctrl Pts',(-12.,45.9443118404255,-56.7791936558369));
#137749=CARTESIAN_POINT('Ctrl Pts',(-12.,45.9561292093552,-56.7956179994232));
#137750=CARTESIAN_POINT('Ctrl Pts',(-12.,45.9677333561082,-56.8121658958829));
#137751=CARTESIAN_POINT('Ctrl Pts',(-12.,45.9798251441557,-56.8294091849313));
#137752=CARTESIAN_POINT('Ctrl Pts',(-12.,45.9916897000447,-56.846792620521));
#137753=CARTESIAN_POINT('Ctrl Pts',(-12.,46.003328510704,-56.8643184852464));
#137754=CARTESIAN_POINT('Ctrl Pts',(-12.,46.0482762655415,-56.9320013691808));
#137755=CARTESIAN_POINT('Ctrl Pts',(-12.,46.0898342762661,-57.0017828739964));
#137756=CARTESIAN_POINT('Ctrl Pts',(-12.,46.1278764894281,-57.0734367367413));
#137757=CARTESIAN_POINT('Ctrl Pts',(-12.,46.1404078986294,-57.0970400920742));
#137758=CARTESIAN_POINT('Ctrl Pts',(-12.,46.1525581757035,-57.1208464092072));
#137759=CARTESIAN_POINT('Ctrl Pts',(-12.,46.164323905515,-57.144847012895));
#137760=CARTESIAN_POINT('Ctrl Pts',(-12.,46.1884069401606,-57.193973363694));
#137761=CARTESIAN_POINT('Ctrl Pts',(-12.0000000000007,46.2108248057518,
-57.2437789527952));
#137762=CARTESIAN_POINT('Ctrl Pts',(-12.0000000001545,46.2316525803282,
-57.2944049984523));
#137763=CARTESIAN_POINT('Ctrl Pts',(-12.000000000255,46.2452564476152,-57.3274719016808));
#137764=CARTESIAN_POINT('Ctrl Pts',(-12.0000000004148,46.258181019402,-57.3608893383372));
#137765=CARTESIAN_POINT('Ctrl Pts',(-12.0000000005167,46.2704364630794,
-57.3947019825787));
#137766=CARTESIAN_POINT('Ctrl Pts',(-12.0000000006197,46.2828321131732,
-57.4289014548942));
#137767=CARTESIAN_POINT('Ctrl Pts',(-12.0000000006374,46.2944781423923,
-57.4633231278189));
#137768=CARTESIAN_POINT('Ctrl Pts',(-12.0000000004958,46.3053795309571,
-57.4980138584003));
#137769=CARTESIAN_POINT('Ctrl Pts',(-12.0000000001659,46.330773911604,-57.5788246296214));
#137770=CARTESIAN_POINT('Ctrl Pts',(-12.0000000000875,46.3519200542249,
-57.660361761354));
#137771=CARTESIAN_POINT('Ctrl Pts',(-12.0000000000438,46.3688636122319,
-57.7426155626072));
#137772=CARTESIAN_POINT('Ctrl Pts',(-12.,46.3858667849632,-57.8251587681094));
#137773=CARTESIAN_POINT('Ctrl Pts',(-12.0000000000021,46.3986378015382,
-57.9084239530159));
#137774=CARTESIAN_POINT('Ctrl Pts',(-12.0000000000007,46.4071710877912,
-57.9924112496631));
#137775=CARTESIAN_POINT('Ctrl Pts',(-11.9999999999993,46.4157043740442,
-58.0763985463103));
#137776=CARTESIAN_POINT('Ctrl Pts',(-12.,46.41999998,-58.1611082160511));
#137777=CARTESIAN_POINT('Ctrl Pts',(-12.,46.41999998,-58.2465463958495));
#137778=CARTESIAN_POINT('Origin',(-12.5,46.41999998,-58.2465463958495));
#137779=CARTESIAN_POINT('Ctrl Pts',(-11.4131406659365,44.1784219329664,
-60.890075338912));
#137780=CARTESIAN_POINT('Ctrl Pts',(-12.0001420550745,44.0869928457662,
-60.8415158913113));
#137781=CARTESIAN_POINT('Ctrl Pts',(-11.9999999857978,44.6134318801692,
-61.1210441133877));
#137782=CARTESIAN_POINT('Ctrl Pts',(-11.4054134166098,44.2623189763507,
-60.7346949078221));
#137783=CARTESIAN_POINT('Ctrl Pts',(-12.000145286376,44.1531002254807,-60.6958383983959));
#137784=CARTESIAN_POINT('Ctrl Pts',(-11.9999999856108,44.7369792722067,
-60.8879413106956));
#137785=CARTESIAN_POINT('Ctrl Pts',(-11.4017112009619,44.3028668820624,
-60.5618538448931));
#137786=CARTESIAN_POINT('Ctrl Pts',(-12.0001468655555,44.1818517612737,
-60.5455762622013));
#137787=CARTESIAN_POINT('Ctrl Pts',(-11.9999999855212,44.7966973993881,
-60.6286788556915));
#137788=CARTESIAN_POINT('Ctrl Pts',(-11.4024481915019,44.294801171802,-60.3838747332568));
#137789=CARTESIAN_POINT('Ctrl Pts',(-12.0001465537004,44.1760490867645,
-60.3893137401235));
#137790=CARTESIAN_POINT('Ctrl Pts',(-11.9999999855391,44.7848185198866,
-60.3616767025499));
#137791=CARTESIAN_POINT('',(-12.,44.6428767076058,-61.062182729971));
#137792=CARTESIAN_POINT('Origin',(-11.5,44.6428767076058,-61.062182729971));
#137793=CARTESIAN_POINT('Origin',(-12.0000005388085,43.3853963400589,-60.4562959717164));
#137794=CARTESIAN_POINT('Origin',(-12.,-9.33460238845303,-92.34995));
#137795=CARTESIAN_POINT('',(-12.,30.2507177004773,-91.1386408691297));
#137796=CARTESIAN_POINT('Ctrl Pts',(-12.,30.2507177004773,-91.1386408691297));
#137797=CARTESIAN_POINT('Ctrl Pts',(-12.,35.0808027196733,-81.1288017666048));
#137798=CARTESIAN_POINT('Ctrl Pts',(-12.,39.8700874953717,-71.0994389691951));
#137799=CARTESIAN_POINT('Ctrl Pts',(-12.,44.6428767076058,-61.062182729971));
#137800=CARTESIAN_POINT('Ctrl Pts',(-12.,30.7194735506599,-91.84995));
#137801=CARTESIAN_POINT('Ctrl Pts',(-12.,30.6947425199752,-91.84995));
#137802=CARTESIAN_POINT('Ctrl Pts',(-12.,30.6701386971986,-91.8481899526742));
#137803=CARTESIAN_POINT('Ctrl Pts',(-12.,30.6458464406133,-91.8447815200538));
#137804=CARTESIAN_POINT('Ctrl Pts',(-12.,30.6209700785576,-91.841291131929));
#137805=CARTESIAN_POINT('Ctrl Pts',(-12.,30.5964191072391,-91.8360720015142));
#137806=CARTESIAN_POINT('Ctrl Pts',(-12.,30.5723817191875,-91.8291895987897));
#137807=CARTESIAN_POINT('Ctrl Pts',(-12.,30.5485535835649,-91.8223671093754));
#137808=CARTESIAN_POINT('Ctrl Pts',(-12.,30.5252287940053,-91.8139098291041));
#137809=CARTESIAN_POINT('Ctrl Pts',(-12.,30.5026013041074,-91.8038327530221));
#137810=CARTESIAN_POINT('Ctrl Pts',(-12.,30.4932234054493,-91.7996563375783));
#137811=CARTESIAN_POINT('Ctrl Pts',(-12.,30.4839655197029,-91.7952011432061));
#137812=CARTESIAN_POINT('Ctrl Pts',(-12.,30.4748428234451,-91.7904659511164));
#137813=CARTESIAN_POINT('Ctrl Pts',(-12.,30.3998197342529,-91.7515247512294));
#137814=CARTESIAN_POINT('Ctrl Pts',(-12.,30.3342288071963,-91.6940226895201));
#137815=CARTESIAN_POINT('Ctrl Pts',(-12.,30.2865222597932,-91.6234713302197));
#137816=CARTESIAN_POINT('Ctrl Pts',(-12.,30.2626689858469,-91.5881956502075));
#137817=CARTESIAN_POINT('Ctrl Pts',(-12.,30.2434629741256,-91.5500105562497));
#137818=CARTESIAN_POINT('Ctrl Pts',(-12.,30.2294961429083,-91.5100899134078));
#137819=CARTESIAN_POINT('Ctrl Pts',(-12.,30.2155293119778,-91.4701692713854));
#137820=CARTESIAN_POINT('Ctrl Pts',(-12.,30.2066913177853,-91.427825927269));
#137821=CARTESIAN_POINT('Ctrl Pts',(-12.,30.20356593057,-91.3857257541517));
#137822=CARTESIAN_POINT('Ctrl Pts',(-12.,30.2016706004034,-91.360194924649));
#137823=CARTESIAN_POINT('Ctrl Pts',(-12.,30.2018789661756,-91.3345298932575));
#137824=CARTESIAN_POINT('Ctrl Pts',(-12.,30.20409423165,-91.309005170562));
#137825=CARTESIAN_POINT('Ctrl Pts',(-12.,30.2063233672374,-91.2833206337071));
#137826=CARTESIAN_POINT('Ctrl Pts',(-12.,30.2105848815978,-91.2577766407636));
#137827=CARTESIAN_POINT('Ctrl Pts',(-12.,30.2168325161083,-91.232654980275));
#137828=CARTESIAN_POINT('Ctrl Pts',(-12.,30.2228393598885,-91.2085015363114));
#137829=CARTESIAN_POINT('Ctrl Pts',(-12.,30.2306827015458,-91.1847372739699));
#137830=CARTESIAN_POINT('Ctrl Pts',(-12.,30.2403633283693,-91.1616344702758));
#137831=CARTESIAN_POINT('Ctrl Pts',(-12.,30.24360775786,-91.1538916433916));
#137832=CARTESIAN_POINT('Ctrl Pts',(-12.,30.2470588833976,-91.1462233796087));
#137833=CARTESIAN_POINT('Ctrl Pts',(-12.,30.2507177004773,-91.1386408691297));
#137834=CARTESIAN_POINT('',(-12.,46.41999998,-92.34995));
#137835=CARTESIAN_POINT('Origin',(0.,-12.9675000200281,-60.64995));
#137836=CARTESIAN_POINT('Ctrl Pts',(-11.4112929481563,44.1984900402045,
-60.8508735991007));
#137837=CARTESIAN_POINT('Ctrl Pts',(-11.4042255504145,39.4271199662976,
-70.8881122426161));
#137838=CARTESIAN_POINT('Ctrl Pts',(-11.3956361798112,34.6396513996494,
-80.9174913671817));
#137839=CARTESIAN_POINT('Ctrl Pts',(-11.3834743397155,29.812801930373,-90.9273317382593));
#137840=CARTESIAN_POINT('Ctrl Pts',(-5.44427033638568,30.9653765476951,
-90.9273317382593));
#137841=CARTESIAN_POINT('Ctrl Pts',(-5.4500940393161,35.6738220550387,-80.9051511012611));
#137842=CARTESIAN_POINT('Ctrl Pts',(-5.45419794131935,40.3738290579191,
-70.8788685457756));
#137843=CARTESIAN_POINT('Ctrl Pts',(-5.45757488824865,45.0702713246265,
-60.8508735991007));
#137844=CARTESIAN_POINT('Ctrl Pts',(-5.4533007853959,45.1647773033082,-60.42825533736));
#137845=CARTESIAN_POINT('Ctrl Pts',(-5.,45.2073007626125,-60.42825533736));
#137846=CARTESIAN_POINT('Ctrl Pts',(-5.,45.6625917098448,-60.42825533736));
#137847=CARTESIAN_POINT('Ctrl Pts',(-5.45330078693253,45.1647773031641,
-60.574158272758));
#137848=CARTESIAN_POINT('Ctrl Pts',(-5.00000000000228,45.2073007505585,
-60.5804098497461));
#137849=CARTESIAN_POINT('Ctrl Pts',(-5.,45.6625916931772,-60.6471114271654));
#137850=CARTESIAN_POINT('Ctrl Pts',(-5.45472878287372,45.1330538591303,
-60.717398791161));
#137851=CARTESIAN_POINT('Ctrl Pts',(-4.99999999999914,45.1727790578482,
-60.730071400192));
#137852=CARTESIAN_POINT('Ctrl Pts',(-5.,45.6152082879987,-60.8619682722934));
#137853=CARTESIAN_POINT('Ctrl Pts',(-5.45757488824865,45.0702713246265,
-60.8508735991007));
#137854=CARTESIAN_POINT('Ctrl Pts',(-4.99999999999999,45.1055585268382,
-60.8674008824012));
#137855=CARTESIAN_POINT('Ctrl Pts',(-5.,45.5214348882082,-61.0621827299711));
#137856=CARTESIAN_POINT('',(-5.,45.5214348882082,-61.062182729971));
#137857=CARTESIAN_POINT('Origin',(-5.00000000000003,43.4682849809988,-60.27593181757));
#137858=CARTESIAN_POINT('Origin',(-5.5,45.5214348882082,-61.062182729971));
#137859=CARTESIAN_POINT('Origin',(-5.,-9.33460238845303,-92.34995));
#137860=CARTESIAN_POINT('',(-5.,46.41999998,-57.9428177527387));
#137861=CARTESIAN_POINT('Ctrl Pts',(-5.,46.41999998,-57.9428177527387));
#137862=CARTESIAN_POINT('Ctrl Pts',(-5.,46.41999998,-57.7745740624592));
#137863=CARTESIAN_POINT('Ctrl Pts',(-5.00000000017611,46.4033211412152,
-57.6091706164621));
#137864=CARTESIAN_POINT('Ctrl Pts',(-4.99999999982344,46.3703757696924,
-57.4465347800693));
#137865=CARTESIAN_POINT('Ctrl Pts',(-4.99999999972182,46.3608819639002,
-57.3996683167638));
#137866=CARTESIAN_POINT('Ctrl Pts',(-4.9999999996722,46.3500332431698,-57.3530322594102));
#137867=CARTESIAN_POINT('Ctrl Pts',(-4.99999999969245,46.3378403217705,
-57.3066263304899));
#137868=CARTESIAN_POINT('Ctrl Pts',(-4.99999999973771,46.3105877995303,
-57.202903968263));
#137869=CARTESIAN_POINT('Ctrl Pts',(-4.99999999996081,46.2762003337234,
-57.0996231221188));
#137870=CARTESIAN_POINT('Ctrl Pts',(-4.9999999999857,46.2356732197596,-56.9999496853278));
#137871=CARTESIAN_POINT('Ctrl Pts',(-4.99999999998832,46.2314106238701,
-56.9894661462744));
#137872=CARTESIAN_POINT('Ctrl Pts',(-4.99999999999009,46.2270807552915,
-56.9790199139327));
#137873=CARTESIAN_POINT('Ctrl Pts',(-4.99999999999128,46.2226837784916,
-56.9686108996226));
#137874=CARTESIAN_POINT('Ctrl Pts',(-5.00000000000135,46.1852595852369,
-56.8800161717309));
#137875=CARTESIAN_POINT('Ctrl Pts',(-5.00000000035917,46.1429808775709,
-56.7941365878385));
#137876=CARTESIAN_POINT('Ctrl Pts',(-4.99999999927331,46.0959886291946,
-56.7109637993559));
#137877=CARTESIAN_POINT('Ctrl Pts',(-4.99999999847595,46.061481441272,-56.6498886403374));
#137878=CARTESIAN_POINT('Ctrl Pts',(-4.9999999969677,46.0241995329013,-56.5900309298165));
#137879=CARTESIAN_POINT('Ctrl Pts',(-4.9999999904409,45.9844424230139,-56.5317775549116));
#137880=CARTESIAN_POINT('Ctrl Pts',(-4.99999998658713,45.9609677338277,
-56.4973816978229));
#137881=CARTESIAN_POINT('Ctrl Pts',(-4.99999998917526,45.9365437147868,
-56.4634809785609));
#137882=CARTESIAN_POINT('Ctrl Pts',(-4.99999999269503,45.9112549501108,
-56.4301707952614));
#137883=CARTESIAN_POINT('Ctrl Pts',(-4.99999999800588,45.8730976568612,
-56.379910276464));
#137884=CARTESIAN_POINT('Ctrl Pts',(-4.99999999856442,45.8329742633927,
-56.3309419284987));
#137885=CARTESIAN_POINT('Ctrl Pts',(-4.99999999917036,45.7911678591844,
-56.2836825816832));
#137886=CARTESIAN_POINT('Ctrl Pts',(-4.99999999955207,45.7648322159121,
-56.2539118964834));
#137887=CARTESIAN_POINT('Ctrl Pts',(-4.99999999973279,45.7378296447701,
-56.2248189288369));
#137888=CARTESIAN_POINT('Ctrl Pts',(-4.99999999986749,45.7102390019053,
-56.1965009486372));
#137889=CARTESIAN_POINT('Ctrl Pts',(-4.99999999994411,45.6945455669802,
-56.1803938074714));
#137890=CARTESIAN_POINT('Ctrl Pts',(-5.,45.6786637148754,-56.1645219339327));
#137891=CARTESIAN_POINT('Ctrl Pts',(-5.,45.6625994185597,-56.1488914421297));
#137892=CARTESIAN_POINT('',(-5.,46.41999998,-57.9628508566217));
#137893=CARTESIAN_POINT('',(-5.,31.415090518797,-91.1386408691297));
#137894=CARTESIAN_POINT('Ctrl Pts',(-5.,31.415090518797,-91.1386408691297));
#137895=CARTESIAN_POINT('Ctrl Pts',(-5.,31.3430615709327,-91.2919348798756));
#137896=CARTESIAN_POINT('Ctrl Pts',(-5.,31.355929990322,-91.4779432828738));
#137897=CARTESIAN_POINT('Ctrl Pts',(-5.,31.5391820921123,-91.7616382083514));
#137898=CARTESIAN_POINT('Ctrl Pts',(-5.,31.7023337675853,-91.84995));
#137899=CARTESIAN_POINT('Ctrl Pts',(-5.,31.8716754827171,-91.84995));
#137900=CARTESIAN_POINT('Ctrl Pts',(-5.,45.5214348882082,-61.0621827299711));
#137901=CARTESIAN_POINT('Ctrl Pts',(-5.,40.8246742459034,-71.0901794372786));
#137902=CARTESIAN_POINT('Ctrl Pts',(-5.,36.1242566254946,-81.1164625478583));
#137903=CARTESIAN_POINT('Ctrl Pts',(-5.,31.4150905187971,-91.1386408691297));
#137904=CARTESIAN_POINT('Ctrl Pts',(-5.,46.41999998,-57.9428177527387));
#137905=CARTESIAN_POINT('Ctrl Pts',(-4.99999999999999,46.91999998,-57.9428177527387));
#137906=CARTESIAN_POINT('Ctrl Pts',(-4.5,46.91999998,-57.9428177527387));
#137907=CARTESIAN_POINT('Ctrl Pts',(-5.,46.4199999741246,-57.7261203908743));
#137908=CARTESIAN_POINT('Ctrl Pts',(-4.99999999999699,46.9183271035242,
-57.6832796231231));
#137909=CARTESIAN_POINT('Ctrl Pts',(-4.50167566539267,46.91999998,-57.6828458026853));
#137910=CARTESIAN_POINT('Ctrl Pts',(-5.,46.3923260879484,-57.5140768479069));
#137911=CARTESIAN_POINT('Ctrl Pts',(-4.99999999999981,46.8836068729329,
-57.4292829235226));
#137912=CARTESIAN_POINT('Ctrl Pts',(-4.50330917749558,46.8867913077729,
-57.4284566847483));
#137913=CARTESIAN_POINT('Ctrl Pts',(-5.,46.310571996574,-57.2029077562381));
#137914=CARTESIAN_POINT('Ctrl Pts',(-5.00000000000009,46.7833158134961,
-57.0568766116336));
#137915=CARTESIAN_POINT('Ctrl Pts',(-4.50569802055499,46.7886864007714,
-57.055145939945));
#137916=CARTESIAN_POINT('Ctrl Pts',(-5.,46.2761936631225,-57.0996254934279));
#137917=CARTESIAN_POINT('Ctrl Pts',(-4.99999999999935,46.7414185265942,
-56.9334556299756));
#137918=CARTESIAN_POINT('Ctrl Pts',(-4.50648947498932,46.7474324008918,
-56.931237732302));
#137919=CARTESIAN_POINT('Ctrl Pts',(-5.,46.1951457708619,-56.9002767254212));
#137920=CARTESIAN_POINT('Ctrl Pts',(-5.00000000000066,46.6430202500091,
-56.6954228782697));
#137921=CARTESIAN_POINT('Ctrl Pts',(-4.50801451396916,46.6501749278894,
-56.6920779475246));
#137922=CARTESIAN_POINT('Ctrl Pts',(-5.,46.1485348528389,-56.8039757263989));
#137923=CARTESIAN_POINT('Ctrl Pts',(-4.99999999999985,46.5866051720245,
-56.5805088850576));
#137924=CARTESIAN_POINT('Ctrl Pts',(-4.50874992208284,46.5942418273256,
-56.5765450470161));
#137925=CARTESIAN_POINT('Ctrl Pts',(-5.,45.9908257800341,-56.5249797415912));
#137926=CARTESIAN_POINT('Ctrl Pts',(-5.00000000000027,46.3962887395937,
-56.2480691534848));
#137927=CARTESIAN_POINT('Ctrl Pts',(-4.51087720078722,46.404990940203,-56.2418316606537));
#137928=CARTESIAN_POINT('Ctrl Pts',(-5.,45.859682945468,-56.349946411749));
#137929=CARTESIAN_POINT('Ctrl Pts',(-4.99999999999943,46.2385095854938,
-56.0395648256266));
#137930=CARTESIAN_POINT('Ctrl Pts',(-4.51220710564129,46.2476195396021,
-56.0318427103247));
#137931=CARTESIAN_POINT('Ctrl Pts',(-5.,45.5607785663138,-56.0430715492057));
#137932=CARTESIAN_POINT('Ctrl Pts',(-5.00000000000056,45.8798007876186,
-55.6745387763548));
#137933=CARTESIAN_POINT('Ctrl Pts',(-4.51453310829638,45.888934282536,-55.6636820506581));
#137934=CARTESIAN_POINT('Ctrl Pts',(-5.,45.3931752587345,-55.909838595577));
#137935=CARTESIAN_POINT('Ctrl Pts',(-5.,45.6790509243108,-55.5161529972778));
#137936=CARTESIAN_POINT('Ctrl Pts',(-4.51553991135993,45.6878102784858,
-55.5038410313454));
#137937=CARTESIAN_POINT('Ctrl Pts',(-5.,45.207055184053,-55.7979884638099));
#137938=CARTESIAN_POINT('Ctrl Pts',(-5.00000000000001,45.4562991060438,
-55.383243356978));
#137939=CARTESIAN_POINT('Ctrl Pts',(-4.51638378732469,45.4644662248635,
-55.3696531657294));
#137940=CARTESIAN_POINT('',(-4.5,46.91999998,-57.9428177527387));
#137941=CARTESIAN_POINT('Ctrl Pts',(-4.51630724703492,45.4845441383302,
-55.3818234144886));
#137942=CARTESIAN_POINT('Ctrl Pts',(-4.51547928405129,45.699880758685,-55.5134714456491));
#137943=CARTESIAN_POINT('Ctrl Pts',(-4.51449818831776,45.8943246894343,
-55.6692148576343));
#137944=CARTESIAN_POINT('Ctrl Pts',(-4.51220714147383,46.2476195389329,
-56.031842710892));
#137945=CARTESIAN_POINT('Ctrl Pts',(-4.51087723667079,46.4049909395646,
-56.2418316611113));
#137946=CARTESIAN_POINT('Ctrl Pts',(-4.50874995804734,46.5942418267665,
-56.5765450473063));
#137947=CARTESIAN_POINT('Ctrl Pts',(-4.50801454996146,46.650174927366,-56.6920779477693));
#137948=CARTESIAN_POINT('Ctrl Pts',(-4.50648951103895,46.7474324004525,
-56.931237732464));
#137949=CARTESIAN_POINT('Ctrl Pts',(-4.50569805663421,46.7886864003794,
-57.0551459400713));
#137950=CARTESIAN_POINT('Ctrl Pts',(-4.50330921366347,46.886791307541,-57.4284566848085));
#137951=CARTESIAN_POINT('Ctrl Pts',(-4.50167570162058,46.9199999798784,
-57.6828458027168));
#137952=CARTESIAN_POINT('Ctrl Pts',(-4.5,46.91999998,-57.9428177527387));
#137953=CARTESIAN_POINT('Origin',(-4.5,46.41999998,-57.9428177527387));
#137954=CARTESIAN_POINT('Ctrl Pts',(-3.92215684205867,46.91999998,-57.921448793088));
#137955=CARTESIAN_POINT('Ctrl Pts',(-3.98080144737804,46.91999998,-56.25271405939));
#137956=CARTESIAN_POINT('Ctrl Pts',(-4.0117049092053,45.5008851266717,-55.3733547413106));
#137957=CARTESIAN_POINT('Ctrl Pts',(-4.11592937444032,46.91999998,-57.928258571556));
#137958=CARTESIAN_POINT('Ctrl Pts',(-4.17733814927362,46.9199999800019,
-56.2502970131512));
#137959=CARTESIAN_POINT('Ctrl Pts',(-4.20907605864164,45.4888071699388,
-55.3727975967628));
#137960=CARTESIAN_POINT('Ctrl Pts',(-4.30969200192382,46.91999998,-57.9354449440051));
#137961=CARTESIAN_POINT('Ctrl Pts',(-4.37353389556205,46.9199999800001,
-56.2475777730216));
#137962=CARTESIAN_POINT('Ctrl Pts',(-4.40621163658902,45.4758414047932,
-55.3721833857804));
#137963=CARTESIAN_POINT('Ctrl Pts',(-4.50344622215482,46.91999998,-57.9429512300502));
#137964=CARTESIAN_POINT('Ctrl Pts',(-4.56924626651609,46.91999998,-56.2445032348437));
#137965=CARTESIAN_POINT('Ctrl Pts',(-4.60306732532639,45.461992503193,-55.3715051982969));
#137966=CARTESIAN_POINT('',(-4.,46.91999998,-57.9242045702762));
#137967=CARTESIAN_POINT('Ctrl Pts',(-4.,46.91999998,-57.9242045702762));
#137968=CARTESIAN_POINT('Ctrl Pts',(-4.00152248707584,46.91999998,-57.6677551135179));
#137969=CARTESIAN_POINT('Ctrl Pts',(-4.00300631304518,46.8876664373662,
-57.4167435210981));
#137970=CARTESIAN_POINT('Ctrl Pts',(-4.00589913432669,46.76036485013,-56.9254492364038));
#137971=CARTESIAN_POINT('Ctrl Pts',(-4.00730581971222,46.6642417866207,
-56.6855258491379));
#137972=CARTESIAN_POINT('Ctrl Pts',(-4.00988782131373,46.4183727996822,
-56.2436081635303));
#137973=CARTESIAN_POINT('Ctrl Pts',(-4.01109981373647,46.2651121552776,
-56.0353451211632));
#137974=CARTESIAN_POINT('Ctrl Pts',(-4.01320487516091,45.9189819724219,
-55.6726195336341));
#137975=CARTESIAN_POINT('Ctrl Pts',(-4.01411057746497,45.7278522136539,
-55.5160338046631));
#137976=CARTESIAN_POINT('Ctrl Pts',(-4.01487932239371,45.5159631499936,
-55.3828830175977));
#137977=CARTESIAN_POINT('Ctrl Pts',(-4.,46.91999998,-57.9242045702762));
#137978=CARTESIAN_POINT('Ctrl Pts',(-4.16667353124555,46.91999998,-57.9301478976981));
#137979=CARTESIAN_POINT('Ctrl Pts',(-4.33333987978916,46.91999998,-57.9363643903873));
#137980=CARTESIAN_POINT('Ctrl Pts',(-4.5,46.91999998,-57.9428177527387));
#137981=CARTESIAN_POINT('Ctrl Pts',(-4.,46.91999998,-57.9242045702762));
#137982=CARTESIAN_POINT('Ctrl Pts',(-3.5,46.91999998,-57.9242045702762));
#137983=CARTESIAN_POINT('Ctrl Pts',(-3.5,46.41999998,-57.9242045702762));
#137984=CARTESIAN_POINT('Ctrl Pts',(-4.00152248707584,46.91999998,-57.6677551135179));
#137985=CARTESIAN_POINT('Ctrl Pts',(-3.49999999999684,46.9215247752432,
-57.6673651906402));
#137986=CARTESIAN_POINT('Ctrl Pts',(-3.5,46.4199999742014,-57.7104514486517));
#137987=CARTESIAN_POINT('Ctrl Pts',(-4.00300631304518,46.8876664373662,
-57.4167435210981));
#137988=CARTESIAN_POINT('Ctrl Pts',(-3.50000000000037,46.8905945241102,
-57.4159945765447));
#137989=CARTESIAN_POINT('Ctrl Pts',(-3.5,46.3930553625334,-57.5012311233074));
#137990=CARTESIAN_POINT('Ctrl Pts',(-4.00589913432669,46.76036485013,-56.9254492364038));
#137991=CARTESIAN_POINT('Ctrl Pts',(-3.49999999999963,46.7659528393486,
-56.9232257271801));
#137992=CARTESIAN_POINT('Ctrl Pts',(-3.5,46.2869707037134,-57.0917336115785));
#137993=CARTESIAN_POINT('Ctrl Pts',(-4.00730581971222,46.6642417866207,
-56.6855258491379));
#137994=CARTESIAN_POINT('Ctrl Pts',(-3.50000000000004,46.6709152176612,
-56.6822760272594));
#137995=CARTESIAN_POINT('Ctrl Pts',(-3.5,46.2068681522152,-56.8917559154199));
#137996=CARTESIAN_POINT('Ctrl Pts',(-4.00988782131373,46.4183727996822,
-56.2436081635303));
#137997=CARTESIAN_POINT('Ctrl Pts',(-3.49999999999995,46.4266646204127,
-56.237771148346));
#137998=CARTESIAN_POINT('Ctrl Pts',(-3.5,46.0019773297039,-56.5234150618225));
#137999=CARTESIAN_POINT('Ctrl Pts',(-4.01109981373647,46.2651121552776,
-56.0353451211632));
#138000=CARTESIAN_POINT('Ctrl Pts',(-3.50000000000055,46.2738584100651,
-56.0280733151404));
#138001=CARTESIAN_POINT('Ctrl Pts',(-3.5,45.8742601250717,-56.3498268696058));
#138002=CARTESIAN_POINT('Ctrl Pts',(-4.01323028458345,45.9148039622378,
-55.6682412064214));
#138003=CARTESIAN_POINT('Ctrl Pts',(-3.49999999999944,45.923712698628,-55.6579003398743));
#138004=CARTESIAN_POINT('Ctrl Pts',(-3.5,45.5823366328578,-56.0438443443254));
#138005=CARTESIAN_POINT('Ctrl Pts',(-4.01415476126711,45.7184991995766,
-55.5083945642206));
#138006=CARTESIAN_POINT('Ctrl Pts',(-3.50000000000342,45.7271164793515,
-55.4966052387911));
#138007=CARTESIAN_POINT('Ctrl Pts',(-3.5,45.4187493558633,-55.9106117044594));
#138008=CARTESIAN_POINT('Ctrl Pts',(-4.01493543718735,45.5003931325255,
-55.3731631297134));
#138009=CARTESIAN_POINT('Ctrl Pts',(-3.49999999999999,45.5085033459109,
-55.3600853439128));
#138010=CARTESIAN_POINT('Ctrl Pts',(-3.5,45.2369942737712,-55.7978959562326));
#138011=CARTESIAN_POINT('',(-3.5,46.41999998,-57.9242045702762));
#138012=CARTESIAN_POINT('Ctrl Pts',(-3.50000000506663,45.8435334367288,
-56.3263223051818));
#138013=CARTESIAN_POINT('Ctrl Pts',(-3.50000001032463,45.8894626566105,
-56.3816811876747));
#138014=CARTESIAN_POINT('Ctrl Pts',(-3.50000001775255,45.9328922004512,
-56.4388763829609));
#138015=CARTESIAN_POINT('Ctrl Pts',(-3.50000002291889,45.9736813029623,
-56.4976009415834));
#138016=CARTESIAN_POINT('Ctrl Pts',(-3.50000002818049,46.0152224330362,
-56.5574082032807));
#138017=CARTESIAN_POINT('Ctrl Pts',(-3.50000003120722,46.0540257195003,
-56.6188027368888));
#138018=CARTESIAN_POINT('Ctrl Pts',(-3.50000003122783,46.0899059446863,
-56.6814984159273));
#138019=CARTESIAN_POINT('Ctrl Pts',(-3.50000003123068,46.0948520295369,
-56.6901410079592));
#138020=CARTESIAN_POINT('Ctrl Pts',(-3.50000003118087,46.0997425008543,
-56.6988083694207));
#138021=CARTESIAN_POINT('Ctrl Pts',(-3.5000000310803,46.1045768057904,-56.7074997895477));
#138022=CARTESIAN_POINT('Ctrl Pts',(-3.50000003035461,46.1394632249472,
-56.7702208072801));
#138023=CARTESIAN_POINT('Ctrl Pts',(-3.50000002687238,46.1717681199833,
-56.8347988963915));
#138024=CARTESIAN_POINT('Ctrl Pts',(-3.50000002225516,46.2013495572015,
-56.9009409523226));
#138025=CARTESIAN_POINT('Ctrl Pts',(-3.5000000182853,46.2267835376252,-56.957809580555));
#138026=CARTESIAN_POINT('Ctrl Pts',(-3.50000001353393,46.2502037235481,
-57.0158352648144));
#138027=CARTESIAN_POINT('Ctrl Pts',(-3.50000000945277,46.2714898142467,
-57.0748386052854));
#138028=CARTESIAN_POINT('Ctrl Pts',(-3.50000000440193,46.2978334233143,
-57.1478609820601));
#138029=CARTESIAN_POINT('Ctrl Pts',(-3.5000000025334,46.3207458812431,-57.221900953307));
#138030=CARTESIAN_POINT('Ctrl Pts',(-3.50000000146594,46.3400500971326,
-57.2964727656199));
#138031=CARTESIAN_POINT('Ctrl Pts',(-3.50000000013692,46.3640841940101,
-57.3893160166336));
#138032=CARTESIAN_POINT('Ctrl Pts',(-3.5000000001043,46.3827251371296,-57.4829234266614));
#138033=CARTESIAN_POINT('Ctrl Pts',(-3.50000000003929,46.3959468792823,
-57.5774099701229));
#138034=CARTESIAN_POINT('Ctrl Pts',(-3.49999999997472,46.4090811642661,
-57.6712715183691));
#138035=CARTESIAN_POINT('Ctrl Pts',(-3.50000000000001,46.4168677320184,
-57.7660006115246));
#138036=CARTESIAN_POINT('Ctrl Pts',(-3.5,46.4192300563852,-57.8617170363508));
#138037=CARTESIAN_POINT('Ctrl Pts',(-3.5,46.4197429699982,-57.882499219346));
#138038=CARTESIAN_POINT('Ctrl Pts',(-3.5,46.41999998,-57.9033279738498));
#138039=CARTESIAN_POINT('Ctrl Pts',(-3.5,46.41999998,-57.9242045702762));
#138040=CARTESIAN_POINT('Origin',(-4.,46.41999998,-57.9242045702762));
#138041=CARTESIAN_POINT('Origin',(-3.5,-9.33460238845303,-92.34995));
#138042=CARTESIAN_POINT('',(-3.5,46.41999998,-92.34995));
#138043=CARTESIAN_POINT('Origin',(-60.,11.11999998,-55.74995));
#138044=CARTESIAN_POINT('',(-57.,11.11999998,-55.24995));
#138045=CARTESIAN_POINT('',(-60.,11.11999998,-55.24995));
#138046=CARTESIAN_POINT('',(-57.,10.61999998,-55.74995));
#138047=CARTESIAN_POINT('Origin',(-57.,11.11999998,-55.74995));
#138048=CARTESIAN_POINT('',(83.2809572255632,10.6199999800001,-55.74995));
#138049=CARTESIAN_POINT('Origin',(-60.,28.41999998,-55.24995));
#138050=CARTESIAN_POINT('',(-57.,11.61999998,-55.24995));
#138051=CARTESIAN_POINT('',(-60.,11.61999998,-55.24995));
#138052=CARTESIAN_POINT('',(-57.,28.41999998,-55.24995));
#138053=CARTESIAN_POINT('Origin',(83.2809572255632,11.6199999800001,-55.74995));
#138054=CARTESIAN_POINT('',(-57.,12.11999998,-55.74995));
#138055=CARTESIAN_POINT('',(83.2809572255632,12.1199999800001,-55.74995));
#138056=CARTESIAN_POINT('Origin',(-57.,11.61999998,-55.74995));
#138057=CARTESIAN_POINT('Origin',(-60.,-37.78000002,-55.74995));
#138058=CARTESIAN_POINT('',(-57.,-37.78000002,-55.24995));
#138059=CARTESIAN_POINT('',(-60.,-37.78000002,-55.24995));
#138060=CARTESIAN_POINT('',(-57.,-38.28000002,-55.74995));
#138061=CARTESIAN_POINT('Origin',(-57.,-37.78000002,-55.74995));
#138062=CARTESIAN_POINT('',(83.2809572255632,-38.28000002,-55.74995));
#138063=CARTESIAN_POINT('Origin',(-60.,28.41999998,-55.24995));
#138064=CARTESIAN_POINT('',(-57.,-37.28000002,-55.24995));
#138065=CARTESIAN_POINT('',(-60.,-37.28000002,-55.24995));
#138066=CARTESIAN_POINT('',(-57.,28.41999998,-55.24995));
#138067=CARTESIAN_POINT('Origin',(83.2809572255632,-37.28000002,-55.74995));
#138068=CARTESIAN_POINT('',(-57.,-36.78000002,-55.74995));
#138069=CARTESIAN_POINT('',(83.2809572255632,-36.78000002,-55.74995));
#138070=CARTESIAN_POINT('Origin',(-57.,-37.28000002,-55.74995));
#138071=CARTESIAN_POINT('Origin',(83.2809572255632,-36.78000002,-55.24995));
#138072=CARTESIAN_POINT('',(-57.,-36.78000002,-176.84995));
#138073=CARTESIAN_POINT('',(-54.1989607257493,-36.78000002,-176.84995));
#138074=CARTESIAN_POINT('',(83.2809572255632,-36.78000002,-176.84995));
#138075=CARTESIAN_POINT('',(-59.5,-36.78000002,-174.34995));
#138076=CARTESIAN_POINT('Origin',(-57.,-36.78000002,-174.34995));
#138077=CARTESIAN_POINT('',(-59.5,-36.78000002,-58.24995));
#138078=CARTESIAN_POINT('',(-59.5,-36.78000002,-174.34995));
#138079=CARTESIAN_POINT('Origin',(-57.,-36.78000002,-58.24995));
#138080=CARTESIAN_POINT('',(-53.9233979868778,-36.78000002,-61.0621827299711));
#138081=CARTESIAN_POINT('Origin',(-52.6143300187798,-36.78000002,-60.4624709867148));
#138082=CARTESIAN_POINT('',(-40.4661024946855,-36.78000002,-86.8949524600738));
#138083=CARTESIAN_POINT('Ctrl Pts',(-40.4661024946855,-36.78000002,-86.8949524600738));
#138084=CARTESIAN_POINT('Ctrl Pts',(-42.7668758174593,-36.78000002,-82.6196483790844));
#138085=CARTESIAN_POINT('Ctrl Pts',(-45.0302107640621,-36.78000002,-78.3248411901957));
#138086=CARTESIAN_POINT('Ctrl Pts',(-47.2696870908413,-36.78000002,-74.0176051177503));
#138087=CARTESIAN_POINT('Ctrl Pts',(-49.5091634176204,-36.78000002,-69.7103690453049));
#138088=CARTESIAN_POINT('Ctrl Pts',(-51.7244980141576,-36.78000002,-65.3905566052077));
#138089=CARTESIAN_POINT('Ctrl Pts',(-53.9233979868778,-36.78000002,-61.0621827299711));
#138090=CARTESIAN_POINT('',(-39.5,-36.78000002,-90.9091273827666));
#138091=CARTESIAN_POINT('Ctrl Pts',(-39.5,-36.78000002,-90.9091273827666));
#138092=CARTESIAN_POINT('Ctrl Pts',(-39.5,-36.78000002,-90.7679100061195));
#138093=CARTESIAN_POINT('Ctrl Pts',(-39.5033096444594,-36.7800000200224,
-90.6269761431622));
#138094=CARTESIAN_POINT('Ctrl Pts',(-39.5098707684965,-36.7800000197587,
-90.4863271086497));
#138095=CARTESIAN_POINT('Ctrl Pts',(-39.5164908621435,-36.7800000194927,
-90.3444139586223));
#138096=CARTESIAN_POINT('Ctrl Pts',(-39.5264211472601,-36.7800000188623,
-90.2027900769894));
#138097=CARTESIAN_POINT('Ctrl Pts',(-39.5396544427957,-36.7800000184551,
-90.0614520511805));
#138098=CARTESIAN_POINT('Ctrl Pts',(-39.5457621647725,-36.7800000182671,
-89.9962186129895));
#138099=CARTESIAN_POINT('Ctrl Pts',(-39.5525742276006,-36.780000018147,
-89.931046067388));
#138100=CARTESIAN_POINT('Ctrl Pts',(-39.5600936571067,-36.7800000181768,
-89.8659343821325));
#138101=CARTESIAN_POINT('Ctrl Pts',(-39.5772069508046,-36.7800000182445,
-89.7177482209288));
#138102=CARTESIAN_POINT('Ctrl Pts',(-39.5980137125873,-36.7800000189104,
-89.569651212334));
#138103=CARTESIAN_POINT('Ctrl Pts',(-39.6224903903717,-36.7800000193564,
-89.4222267568288));
#138104=CARTESIAN_POINT('Ctrl Pts',(-39.6467595279693,-36.7800000197985,
-89.2760523279532));
#138105=CARTESIAN_POINT('Ctrl Pts',(-39.6746364995126,-36.780000019972,
-89.1305398192676));
#138106=CARTESIAN_POINT('Ctrl Pts',(-39.7060481712982,-36.780000019994,
-88.9862487847464));
#138107=CARTESIAN_POINT('Ctrl Pts',(-39.716927298473,-36.7800000200016,
-88.9362749875714));
#138108=CARTESIAN_POINT('Ctrl Pts',(-39.7282299820617,-36.78000002,-88.8864475773876));
#138109=CARTESIAN_POINT('Ctrl Pts',(-39.7399518035734,-36.78000002,-88.8367893012138));
#138110=CARTESIAN_POINT('Ctrl Pts',(-39.8212039955528,-36.78000002,-88.492572851151));
#138111=CARTESIAN_POINT('Ctrl Pts',(-39.9220601466534,-36.78000002,-88.1550003033698));
#138112=CARTESIAN_POINT('Ctrl Pts',(-40.0453748819469,-36.78000002,-87.8250390461022));
#138113=CARTESIAN_POINT('Ctrl Pts',(-40.1639808073533,-36.78000002,-87.5076774576977));
#138114=CARTESIAN_POINT('Ctrl Pts',(-40.3033623182004,-36.78000002,-87.1973567576838));
#138115=CARTESIAN_POINT('Ctrl Pts',(-40.4661024946855,-36.78000002,-86.8949524600738));
#138116=CARTESIAN_POINT('',(-39.5,-36.78000002,-141.149515588739));
#138117=CARTESIAN_POINT('',(-39.5,-36.78000002,-55.24995));
#138118=CARTESIAN_POINT('',(-40.4661024946856,-36.78000002,-145.163690511432));
#138119=CARTESIAN_POINT('Ctrl Pts',(-40.4661024946855,-36.78000002,-145.163690511432));
#138120=CARTESIAN_POINT('Ctrl Pts',(-40.4051245273349,-36.78000002,-145.05038106453));
#138121=CARTESIAN_POINT('Ctrl Pts',(-40.3473970436743,-36.78000002,-144.935666150371));
#138122=CARTESIAN_POINT('Ctrl Pts',(-40.2927291183484,-36.78000002,-144.819632460353));
#138123=CARTESIAN_POINT('Ctrl Pts',(-40.2359907375983,-36.78000002,-144.699204190122));
#138124=CARTESIAN_POINT('Ctrl Pts',(-40.1825479091664,-36.78000002,-144.57735479297));
#138125=CARTESIAN_POINT('Ctrl Pts',(-40.1322366185216,-36.78000002,-144.454153170973));
#138126=CARTESIAN_POINT('Ctrl Pts',(-40.0991220934984,-36.78000002,-144.373062760805));
#138127=CARTESIAN_POINT('Ctrl Pts',(-40.0673652289499,-36.78000002,-144.291385980202));
#138128=CARTESIAN_POINT('Ctrl Pts',(-40.0369306905871,-36.78000002,-144.209138150939));
#138129=CARTESIAN_POINT('Ctrl Pts',(-39.9567208320419,-36.78000002,-143.992374989553));
#138130=CARTESIAN_POINT('Ctrl Pts',(-39.8859370925007,-36.78000002,-143.772269498048));
#138131=CARTESIAN_POINT('Ctrl Pts',(-39.8243406671268,-36.78000002,-143.550546349417));
#138132=CARTESIAN_POINT('Ctrl Pts',(-39.7928424603828,-36.78000002,-143.43716506904));
#138133=CARTESIAN_POINT('Ctrl Pts',(-39.7637458267523,-36.78000002,-143.323361070994));
#138134=CARTESIAN_POINT('Ctrl Pts',(-39.737013701299,-36.78000002,-143.209365754044));
#138135=CARTESIAN_POINT('Ctrl Pts',(-39.639900448195,-36.78000002,-142.795240207349));
#138136=CARTESIAN_POINT('Ctrl Pts',(-39.5726401857973,-36.78000002,-142.376286688263));
#138137=CARTESIAN_POINT('Ctrl Pts',(-39.5352116792783,-36.78000002,-141.952508599961));
#138138=CARTESIAN_POINT('Ctrl Pts',(-39.5117389237074,-36.78000002,-141.686742198676));
#138139=CARTESIAN_POINT('Ctrl Pts',(-39.5000000000007,-36.78000002,-141.419078129349));
#138140=CARTESIAN_POINT('Ctrl Pts',(-39.5,-36.78000002,-141.149515588739));
#138141=CARTESIAN_POINT('',(-54.0459394689003,-36.78000002,-171.237717270032));
#138142=CARTESIAN_POINT('Ctrl Pts',(-54.0459394689003,-36.78000002,-171.237717270032));
#138143=CARTESIAN_POINT('Ctrl Pts',(-51.8272412193298,-36.78000002,-166.868813514854));
#138144=CARTESIAN_POINT('Ctrl Pts',(-49.5919157423625,-36.78000002,-162.508569528244));
#138145=CARTESIAN_POINT('Ctrl Pts',(-47.3320947234338,-36.78000002,-158.161083274436));
#138146=CARTESIAN_POINT('Ctrl Pts',(-45.0722737045051,-36.78000002,-153.813597020627));
#138147=CARTESIAN_POINT('Ctrl Pts',(-42.7882516015473,-36.78000002,-149.478715140467));
#138148=CARTESIAN_POINT('Ctrl Pts',(-40.4661024946855,-36.78000002,-145.163690511432));
#138149=CARTESIAN_POINT('',(-54.1989607257493,-36.78000002,-171.871644662643));
#138150=CARTESIAN_POINT('Origin',(-52.6055188872069,-36.7800000520242,-171.864725026464));
#138151=CARTESIAN_POINT('',(-54.1989607257493,-36.78000002,-171.871644662643));
#138152=CARTESIAN_POINT('Ctrl Pts',(-53.5074514076768,-36.1001753985996,
-60.8508735991007));
#138153=CARTESIAN_POINT('Ctrl Pts',(-53.2738374538032,-36.78000002,-60.732193066502));
#138154=CARTESIAN_POINT('Ctrl Pts',(-53.9233979868778,-36.78000002,-61.0621827299711));
#138155=CARTESIAN_POINT('Ctrl Pts',(-53.5793517884845,-36.0882972935914,
-60.7194512531293));
#138156=CARTESIAN_POINT('Ctrl Pts',(-53.3063595996785,-36.7800000199961,
-60.6234805422192));
#138157=CARTESIAN_POINT('Ctrl Pts',(-54.0235433277796,-36.78000002,-60.8650539582955));
#138158=CARTESIAN_POINT('Ctrl Pts',(-53.6173229302591,-36.0820590261091,
-60.5748771537519));
#138159=CARTESIAN_POINT('Ctrl Pts',(-53.3164388644065,-36.7800000200045,
-60.5261947762596));
#138160=CARTESIAN_POINT('Ctrl Pts',(-54.0764736407615,-36.78000002,-60.6481844964965));
#138161=CARTESIAN_POINT('Ctrl Pts',(-53.6173229282256,-36.0820590308261,
-60.42825533736));
#138162=CARTESIAN_POINT('Ctrl Pts',(-53.3164388612998,-36.78000002,-60.42825533736));
#138163=CARTESIAN_POINT('Ctrl Pts',(-54.076473627675,-36.78000002,-60.42825533736));
#138164=CARTESIAN_POINT('Origin',(-53.9233979868778,-36.28000002,-61.0621827299711));
#138165=CARTESIAN_POINT('Origin',(0.,-12.9675000200281,-60.64995));
#138166=CARTESIAN_POINT('',(-40.0734472026555,-36.0537916247009,-86.6836434020945));
#138167=CARTESIAN_POINT('',(-39.850159149164,-30.447965242174,-92.5429803300057));
#138168=CARTESIAN_POINT('Ctrl Pts',(-40.0734472049734,-36.0537916894494,
-86.683643483585));
#138169=CARTESIAN_POINT('Ctrl Pts',(-40.0273699242565,-34.9400863872175,
-87.9615139033166));
#138170=CARTESIAN_POINT('Ctrl Pts',(-39.9805444369969,-33.7936306360731,
-89.2147954597336));
#138171=CARTESIAN_POINT('Ctrl Pts',(-39.9335716691851,-32.6056714694524,
-90.4294303486513));
#138172=CARTESIAN_POINT('Ctrl Pts',(-39.9055799708467,-31.8977507702987,
-91.1532474662255));
#138173=CARTESIAN_POINT('Ctrl Pts',(-39.8776986413925,-31.1793505068417,
-91.8590535072933));
#138174=CARTESIAN_POINT('Ctrl Pts',(-39.8501516349657,-30.4480624602042,
-92.5430839619263));
#138175=CARTESIAN_POINT('Ctrl Pts',(-53.5074514076768,-36.1001753985996,
-60.8508735991007));
#138176=CARTESIAN_POINT('Ctrl Pts',(-51.3114449995927,-36.0939978420838,
-65.1788088203991));
#138177=CARTESIAN_POINT('Ctrl Pts',(-49.0993449598848,-36.0872029674615,
-69.4983516680729));
#138178=CARTESIAN_POINT('Ctrl Pts',(-44.6279666678641,-36.07192692476,-78.1127593263175));
#138179=CARTESIAN_POINT('Ctrl Pts',(-42.3689613386823,-36.0634493757596,
-82.407773086312));
#138180=CARTESIAN_POINT('Ctrl Pts',(-40.0734472163172,-36.0537915241817,
-86.6836433292035));
#138181=CARTESIAN_POINT('Ctrl Pts',(-39.850159149164,-30.447965242174,-92.5429803300057));
#138182=CARTESIAN_POINT('Ctrl Pts',(-42.5227129344255,-30.4581147715466,
-87.2856833539494));
#138183=CARTESIAN_POINT('Ctrl Pts',(-45.1629315870884,-30.4666308723541,
-82.01174695052));
#138184=CARTESIAN_POINT('Ctrl Pts',(-50.405384759569,-30.4815921581836,
-71.4443972343972));
#138185=CARTESIAN_POINT('Ctrl Pts',(-53.0072677069205,-30.4880260434848,
-66.1508000801069));
#138186=CARTESIAN_POINT('Ctrl Pts',(-55.5967474138374,-30.4937575588533,
-60.8508735991007));
#138187=CARTESIAN_POINT('Ctrl Pts',(-55.6982488612463,-30.4801711525811,
-60.3843213671005));
#138188=CARTESIAN_POINT('Ctrl Pts',(-55.8081167820838,-30.1299397177969,
-60.3792327034747));
#138189=CARTESIAN_POINT('Ctrl Pts',(-56.1748536617521,-30.1300000267474,
-60.3623460050376));
#138190=CARTESIAN_POINT('Ctrl Pts',(-55.7066195808876,-30.47905606799,-60.5602959714918));
#138191=CARTESIAN_POINT('Ctrl Pts',(-55.8181378939596,-30.1299399603517,
-60.5754394884542));
#138192=CARTESIAN_POINT('Ctrl Pts',(-56.1868831687146,-30.1300000267259,
-60.6263466339184));
#138193=CARTESIAN_POINT('Ctrl Pts',(-55.6646352974887,-30.4846448609915,
-60.733808800051));
#138194=CARTESIAN_POINT('Ctrl Pts',(-55.7674480546492,-30.1299387371113,
-60.7710090719053));
#138195=CARTESIAN_POINT('Ctrl Pts',(-56.1265462537084,-30.1300000268336,
-60.8865882025091));
#138196=CARTESIAN_POINT('Ctrl Pts',(-55.5754321736229,-30.4966175475299,
-60.8903552940655));
#138197=CARTESIAN_POINT('Ctrl Pts',(-55.6644710959107,-30.1299360711904,
-60.9390296786082));
#138198=CARTESIAN_POINT('Ctrl Pts',(-55.9983862620519,-30.1300000270643,
-61.1214514057001));
#138199=CARTESIAN_POINT('',(-56.0289353856639,-30.13000002,-61.0621827299711));
#138200=CARTESIAN_POINT('Origin',(-54.6965997031483,-30.1299997573522,-60.447263207802));
#138201=CARTESIAN_POINT('Origin',(-56.0289353856639,-30.63000002,-61.0621827299711));
#138202=CARTESIAN_POINT('Origin',(83.2809572255632,-30.13000002,-55.24995));
#138203=CARTESIAN_POINT('',(-57.,-30.13000002,-55.74995));
#138204=CARTESIAN_POINT('',(83.2809572255632,-30.13000002,-55.74995));
#138205=CARTESIAN_POINT('',(-59.5,-30.13000002,-58.24995));
#138206=CARTESIAN_POINT('Origin',(-57.,-30.13000002,-58.24995));
#138207=CARTESIAN_POINT('',(-59.5,-30.13000002,-174.34995));
#138208=CARTESIAN_POINT('',(-59.5,-30.13000002,-58.24995));
#138209=CARTESIAN_POINT('',(-57.,-30.13000002,-176.84995));
#138210=CARTESIAN_POINT('Origin',(-57.,-30.13000002,-174.34995));
#138211=CARTESIAN_POINT('',(-56.294192362543,-30.13000002,-176.84995));
#138212=CARTESIAN_POINT('',(83.2809572255632,-30.13000002,-176.84995));
#138213=CARTESIAN_POINT('',(-56.294192362543,-30.13000002,-171.871644662643));
#138214=CARTESIAN_POINT('',(-56.294192362543,-30.13000002,-176.84995));
#138215=CARTESIAN_POINT('',(-56.1468816861249,-30.13000002,-171.237717270032));
#138216=CARTESIAN_POINT('Origin',(-54.8146431262804,-30.1299997583388,-171.852158294274));
#138217=CARTESIAN_POINT('',(-40.2651432342477,-30.13000002,-139.30435351063));
#138218=CARTESIAN_POINT('Ctrl Pts',(-40.2651432342477,-30.13000002,-139.30435351063));
#138219=CARTESIAN_POINT('Ctrl Pts',(-42.96245845912,-30.13000002,-144.601535351275));
#138220=CARTESIAN_POINT('Ctrl Pts',(-45.6258101137032,-30.13000002,-149.915608633243));
#138221=CARTESIAN_POINT('Ctrl Pts',(-48.2693741701893,-30.13000002,-155.239523078828));
#138222=CARTESIAN_POINT('Ctrl Pts',(-50.9129382266755,-30.13000002,-160.563437524412));
#138223=CARTESIAN_POINT('Ctrl Pts',(-53.5363337714711,-30.13000002,-165.897382577172));
#138224=CARTESIAN_POINT('Ctrl Pts',(-56.1468816861249,-30.13000002,-171.237717270032));
#138225=CARTESIAN_POINT('',(-39.5,-30.13000002,-136.04214564125));
#138226=CARTESIAN_POINT('Ctrl Pts',(-39.5,-30.13000002,-136.04214564125));
#138227=CARTESIAN_POINT('Ctrl Pts',(-39.5,-30.13000002,-136.325718326755));
#138228=CARTESIAN_POINT('Ctrl Pts',(-39.5162728499327,-30.13000002,-136.608122039194));
#138229=CARTESIAN_POINT('Ctrl Pts',(-39.5808560770791,-30.13000002,-137.170628022919));
#138230=CARTESIAN_POINT('Ctrl Pts',(-39.6292470494507,-30.13000002,-137.450036957971));
#138231=CARTESIAN_POINT('Ctrl Pts',(-39.8201451199495,-30.13000002,-138.270288236609));
#138232=CARTESIAN_POINT('Ctrl Pts',(-40.0074751366267,-30.13000002,-138.798326348879));
#138233=CARTESIAN_POINT('Ctrl Pts',(-40.2651432342477,-30.13000002,-139.30435351063));
#138234=CARTESIAN_POINT('',(-39.5,-30.13000002,-96.0164973302555));
#138235=CARTESIAN_POINT('',(-39.5,-30.13000002,-55.24995));
#138236=CARTESIAN_POINT('',(-40.2651432342477,-30.13000002,-92.754289460876));
#138237=CARTESIAN_POINT('Ctrl Pts',(-40.2651432342476,-30.13000002,-92.7542894608761));
#138238=CARTESIAN_POINT('Ctrl Pts',(-40.1497681189566,-30.13000002,-92.980871419087));
#138239=CARTESIAN_POINT('Ctrl Pts',(-40.0478331438212,-30.13000002,-93.2140840893041));
#138240=CARTESIAN_POINT('Ctrl Pts',(-39.9590875376232,-30.13000002,-93.4515644892626));
#138241=CARTESIAN_POINT('Ctrl Pts',(-39.8658509560187,-30.13000002,-93.7010625955778));
#138242=CARTESIAN_POINT('Ctrl Pts',(-39.7871721235835,-30.13000002,-93.9552726783301));
#138243=CARTESIAN_POINT('Ctrl Pts',(-39.7228113496722,-30.13000002,-94.2114776823651));
#138244=CARTESIAN_POINT('Ctrl Pts',(-39.7115691395802,-30.13000002,-94.2562302592367));
#138245=CARTESIAN_POINT('Ctrl Pts',(-39.700763918709,-30.13000002,-94.3010437266483));
#138246=CARTESIAN_POINT('Ctrl Pts',(-39.6903945692724,-30.13000002,-94.3459036197334));
#138247=CARTESIAN_POINT('Ctrl Pts',(-39.604671908225,-30.13000002,-94.7167571079927));
#138248=CARTESIAN_POINT('Ctrl Pts',(-39.5475807634113,-30.13000002,-95.0925075650422));
#138249=CARTESIAN_POINT('Ctrl Pts',(-39.5197593574043,-30.13000002,-95.4732641712576));
#138250=CARTESIAN_POINT('Ctrl Pts',(-39.506610251674,-30.13000002,-95.6532194499864));
#138251=CARTESIAN_POINT('Ctrl Pts',(-39.5000000000002,-30.13000002,-95.8342931017841));
#138252=CARTESIAN_POINT('Ctrl Pts',(-39.5,-30.13000002,-96.0164973302556));
#138253=CARTESIAN_POINT('Ctrl Pts',(-56.0289353856639,-30.13000002,-61.0621827299711));
#138254=CARTESIAN_POINT('Ctrl Pts',(-53.4376473376604,-30.13000002,-66.3621123698348));
#138255=CARTESIAN_POINT('Ctrl Pts',(-50.8336218773754,-30.13000002,-71.6557063652599));
#138256=CARTESIAN_POINT('Ctrl Pts',(-48.2096546190285,-30.13000002,-76.9393812233288));
#138257=CARTESIAN_POINT('Ctrl Pts',(-45.5856873606815,-30.13000002,-82.2230560813977));
#138258=CARTESIAN_POINT('Ctrl Pts',(-42.9421476228591,-30.13000002,-87.4969955027855));
#138259=CARTESIAN_POINT('Ctrl Pts',(-40.2651432342477,-30.13000002,-92.754289460876));
#138260=CARTESIAN_POINT('Origin',(-60.,-29.63000002,-55.74995));
#138261=CARTESIAN_POINT('',(-57.,-29.63000002,-55.24995));
#138262=CARTESIAN_POINT('',(-60.,-29.63000002,-55.24995));
#138263=CARTESIAN_POINT('Origin',(-57.,-29.63000002,-55.74995));
#138264=CARTESIAN_POINT('Origin',(-60.,28.41999998,-55.24995));
#138265=CARTESIAN_POINT('',(-57.,-29.13000002,-55.24995));
#138266=CARTESIAN_POINT('',(-60.,-29.13000002,-55.24995));
#138267=CARTESIAN_POINT('',(-57.,28.41999998,-55.24995));
#138268=CARTESIAN_POINT('Origin',(83.2809572255632,-29.13000002,-55.74995));
#138269=CARTESIAN_POINT('',(-57.,-28.63000002,-55.74995));
#138270=CARTESIAN_POINT('',(83.2809572255632,-28.6300000199999,-55.74995));
#138271=CARTESIAN_POINT('Origin',(-57.,-29.13000002,-55.74995));
#138272=CARTESIAN_POINT('Ctrl Pts',(-56.2981381510249,-28.0154717851087,
-60.8899762078857));
#138273=CARTESIAN_POINT('Ctrl Pts',(-56.1708458184293,-28.6301256542592,
-60.8213741500007));
#138274=CARTESIAN_POINT('Ctrl Pts',(-56.7267007677588,-28.6300000101017,
-61.1208879979441));
#138275=CARTESIAN_POINT('Ctrl Pts',(-56.3842107337159,-28.0053123694987,
-60.7350480688662));
#138276=CARTESIAN_POINT('Ctrl Pts',(-56.231166166104,-28.630129440528,-60.6796100628425));
#138277=CARTESIAN_POINT('Ctrl Pts',(-56.8517546922174,-28.6300000099381,
-60.8884604222472));
#138278=CARTESIAN_POINT('Ctrl Pts',(-56.4261416440025,-28.000404297649,
-60.56196856935));
#138279=CARTESIAN_POINT('Ctrl Pts',(-56.2556311178187,-28.6301313253205,
-60.5386217481864));
#138280=CARTESIAN_POINT('Ctrl Pts',(-56.9126898510831,-28.630000009859,
-60.6288526395369));
#138281=CARTESIAN_POINT('Ctrl Pts',(-56.4178064988838,-28.0013806349218,
-60.3838347631883));
#138282=CARTESIAN_POINT('Ctrl Pts',(-56.25064863923,-28.6301309522558,-60.3916281028846));
#138283=CARTESIAN_POINT('Ctrl Pts',(-56.900577244494,-28.6300000098747,
-60.3616165536491));
#138284=CARTESIAN_POINT('',(-56.7565335485771,-28.63000002,-61.0621827299711));
#138285=CARTESIAN_POINT('Origin',(-56.7565335485771,-28.13000002,-61.0621827299711));
#138286=CARTESIAN_POINT('Origin',(-55.4600042524658,-28.6300004012304,-60.4518437845537));
#138287=CARTESIAN_POINT('Origin',(83.2809572255632,-28.6300000199999,-55.24995));
#138288=CARTESIAN_POINT('',(-40.1842134716234,-28.63000002,-94.9396273673639));
#138289=CARTESIAN_POINT('Ctrl Pts',(-40.1842134716234,-28.63000002,-94.9396273673639));
#138290=CARTESIAN_POINT('Ctrl Pts',(-42.9880935290232,-28.63000002,-89.3138475723767));
#138291=CARTESIAN_POINT('Ctrl Pts',(-45.7634210292107,-28.63000002,-83.6741003095903));
#138292=CARTESIAN_POINT('Ctrl Pts',(-48.5225556597151,-28.63000002,-78.026431746297));
#138293=CARTESIAN_POINT('Ctrl Pts',(-51.2816902902195,-28.63000002,-72.3787631830038));
#138294=CARTESIAN_POINT('Ctrl Pts',(-54.0242783838037,-28.63000002,-66.7230003106817));
#138295=CARTESIAN_POINT('Ctrl Pts',(-56.7565335485771,-28.63000002,-61.0621827299711));
#138296=CARTESIAN_POINT('',(-39.5,-28.63000002,-97.8896208912436));
#138297=CARTESIAN_POINT('Ctrl Pts',(-39.5,-28.63000002,-97.8896208912436));
#138298=CARTESIAN_POINT('Ctrl Pts',(-39.5,-28.63000002,-97.7089321417027));
#138299=CARTESIAN_POINT('Ctrl Pts',(-39.50738071193,-28.63000002,-97.5282244682258));
#138300=CARTESIAN_POINT('Ctrl Pts',(-39.5219120167721,-28.63000002,-97.3483295034428));
#138301=CARTESIAN_POINT('Ctrl Pts',(-39.5366966813148,-28.63000002,-97.1652979907105));
#138302=CARTESIAN_POINT('Ctrl Pts',(-39.5588835421167,-28.63000002,-96.9831066045018));
#138303=CARTESIAN_POINT('Ctrl Pts',(-39.5882836977188,-28.63000002,-96.802626732815));
#138304=CARTESIAN_POINT('Ctrl Pts',(-39.6119618388165,-28.63000002,-96.6572728127559));
#138305=CARTESIAN_POINT('Ctrl Pts',(-39.6403197974461,-28.63000002,-96.5130286888782));
#138306=CARTESIAN_POINT('Ctrl Pts',(-39.6732827765156,-28.63000002,-96.3703554408507));
#138307=CARTESIAN_POINT('Ctrl Pts',(-39.7499154654027,-28.63000002,-96.0386671366605));
#138308=CARTESIAN_POINT('Ctrl Pts',(-39.8508333618867,-28.63000002,-95.7143394136885));
#138309=CARTESIAN_POINT('Ctrl Pts',(-39.9781561959401,-28.63000002,-95.3980147135165));
#138310=CARTESIAN_POINT('Ctrl Pts',(-40.0404386993086,-28.63000002,-95.243278178232));
#138311=CARTESIAN_POINT('Ctrl Pts',(-40.1090402739363,-28.63000002,-95.0904568779003));
#138312=CARTESIAN_POINT('Ctrl Pts',(-40.1842134716234,-28.63000002,-94.9396273673639));
#138313=CARTESIAN_POINT('',(-39.5,-28.63000002,-134.169022080262));
#138314=CARTESIAN_POINT('',(-39.5,-28.63000002,-55.24995));
#138315=CARTESIAN_POINT('',(-40.1842134716234,-28.63000002,-137.119015604142));
#138316=CARTESIAN_POINT('Ctrl Pts',(-40.1842134716234,-28.63000002,-137.119015604142));
#138317=CARTESIAN_POINT('Ctrl Pts',(-40.063259300405,-28.63000002,-136.876329926221));
#138318=CARTESIAN_POINT('Ctrl Pts',(-39.9584937855378,-28.63000002,-136.625775901222));
#138319=CARTESIAN_POINT('Ctrl Pts',(-39.8698562579308,-28.63000002,-136.370603923321));
#138320=CARTESIAN_POINT('Ctrl Pts',(-39.7907547390424,-28.63000002,-136.142884450829));
#138321=CARTESIAN_POINT('Ctrl Pts',(-39.7244982953546,-28.63000002,-135.911485835381));
#138322=CARTESIAN_POINT('Ctrl Pts',(-39.6710763875084,-28.63000002,-135.678705638911));
#138323=CARTESIAN_POINT('Ctrl Pts',(-39.5896852679394,-28.63000002,-135.324052621675));
#138324=CARTESIAN_POINT('Ctrl Pts',(-39.5369428910349,-28.63000002,-134.964508495217));
#138325=CARTESIAN_POINT('Ctrl Pts',(-39.5136924175149,-28.63000002,-134.599929291455));
#138326=CARTESIAN_POINT('Ctrl Pts',(-39.5045817727589,-28.63000002,-134.457069766118));
#138327=CARTESIAN_POINT('Ctrl Pts',(-39.5,-28.63000002,-134.313437038192));
#138328=CARTESIAN_POINT('Ctrl Pts',(-39.5,-28.63000002,-134.169022080262));
#138329=CARTESIAN_POINT('',(-56.8729709358987,-28.63000002,-171.237717270032));
#138330=CARTESIAN_POINT('Ctrl Pts',(-56.8729709358987,-28.63000002,-171.237717270032));
#138331=CARTESIAN_POINT('Ctrl Pts',(-54.1216123272523,-28.63000002,-165.536543461238));
#138332=CARTESIAN_POINT('Ctrl Pts',(-51.3598402340142,-28.63000002,-159.840463284682));
#138333=CARTESIAN_POINT('Ctrl Pts',(-48.5813487526192,-28.63000002,-154.152561198155));
#138334=CARTESIAN_POINT('Ctrl Pts',(-45.8028572712242,-28.63000002,-148.464659111628));
#138335=CARTESIAN_POINT('Ctrl Pts',(-43.0080103715946,-28.63000002,-142.784757083568));
#138336=CARTESIAN_POINT('Ctrl Pts',(-40.1842134716234,-28.63000002,-137.119015604142));
#138337=CARTESIAN_POINT('',(-57.0184057454332,-28.63000002,-171.871644662643));
#138338=CARTESIAN_POINT('Origin',(-55.5771425539593,-28.6300004042112,-171.848433760986));
#138339=CARTESIAN_POINT('',(-57.0184057454332,-28.63000002,-176.849882244789));
#138340=CARTESIAN_POINT('',(-57.0184057454332,-28.63000002,-171.871644662643));
#138341=CARTESIAN_POINT('',(-59.5,-28.63000002,-174.34995));
#138342=CARTESIAN_POINT('Origin',(-57.,-28.63000002,-174.34995));
#138343=CARTESIAN_POINT('',(-59.5,-28.63000002,-58.24995));
#138344=CARTESIAN_POINT('',(-59.5,-28.63000002,-174.34995));
#138345=CARTESIAN_POINT('Origin',(-57.,-28.63000002,-58.24995));
#138346=CARTESIAN_POINT('Origin',(0.,-12.9675000200281,-60.64995));
#138347=CARTESIAN_POINT('',(-39.7602371875712,-27.9700232835192,-94.7283182633411));
#138348=CARTESIAN_POINT('',(-39.5912209089345,-22.3752378108151,-98.5946087902607));
#138349=CARTESIAN_POINT('Ctrl Pts',(-39.760237187334,-27.9700232996177,
-94.7283182916262));
#138350=CARTESIAN_POINT('Ctrl Pts',(-39.7429528415391,-27.4727630876175,
-95.1394632520645));
#138351=CARTESIAN_POINT('Ctrl Pts',(-39.725890220247,-26.9675166669193,
-95.540293140202));
#138352=CARTESIAN_POINT('Ctrl Pts',(-39.7091463075091,-26.4529290005184,
-95.9291550328498));
#138353=CARTESIAN_POINT('Ctrl Pts',(-39.6919956601185,-25.9258412309992,
-96.3274629617598));
#138354=CARTESIAN_POINT('Ctrl Pts',(-39.6751334260609,-25.3873798477127,
-96.7142461865699));
#138355=CARTESIAN_POINT('Ctrl Pts',(-39.6588811036972,-24.8421814727703,
-97.0830011825413));
#138356=CARTESIAN_POINT('Ctrl Pts',(-39.6348426135811,-24.0357892874514,
-97.6284194389328));
#138357=CARTESIAN_POINT('Ctrl Pts',(-39.6121111132943,-23.2146690372305,
-98.1350071075587));
#138358=CARTESIAN_POINT('Ctrl Pts',(-39.5912173600306,-22.3752713037076,
-98.5946697908795));
#138359=CARTESIAN_POINT('Ctrl Pts',(-56.3187331343194,-28.0130417005584,
-60.8508735991007));
#138360=CARTESIAN_POINT('Ctrl Pts',(-53.5878832423519,-28.007786404225,
-66.5116884426402));
#138361=CARTESIAN_POINT('Ctrl Pts',(-50.8469740031282,-28.0018438144749,
-72.167454052164));
#138362=CARTESIAN_POINT('Ctrl Pts',(-45.3330806261693,-27.9878402480257,
-83.4627911786916));
#138363=CARTESIAN_POINT('Ctrl Pts',(-42.560432140096,-27.9797945689747,
-89.1025347299149));
#138364=CARTESIAN_POINT('Ctrl Pts',(-39.7602371906927,-27.9700232578782,
-94.7283182364936));
#138365=CARTESIAN_POINT('Ctrl Pts',(-39.5912209089345,-22.3752378108151,
-98.5946087902606));
#138366=CARTESIAN_POINT('Ctrl Pts',(-45.6084483277559,-22.3901517769159,
-86.0327992158248));
#138367=CARTESIAN_POINT('Ctrl Pts',(-51.5741970786256,-22.399288356509,
-73.4455439777502));
#138368=CARTESIAN_POINT('Ctrl Pts',(-57.5245249214072,-22.4066238608121,
-60.8508735991007));
#138369=CARTESIAN_POINT('Ctrl Pts',(-57.6206785412152,-22.3992316056509,
-60.42825533736));
#138370=CARTESIAN_POINT('Ctrl Pts',(-57.6893011240826,-21.98000002,-60.42825533736));
#138371=CARTESIAN_POINT('Ctrl Pts',(-58.1141118834647,-21.98000002,-60.42825533736));
#138372=CARTESIAN_POINT('Ctrl Pts',(-57.6206785407758,-22.3992316083349,
-60.574219492927));
#138373=CARTESIAN_POINT('Ctrl Pts',(-57.6893011111963,-21.9800000199989,
-60.5843987403017));
#138374=CARTESIAN_POINT('Ctrl Pts',(-58.1141118664761,-21.98000002,-60.6472062522327));
#138375=CARTESIAN_POINT('Ctrl Pts',(-57.5883338458808,-22.4017068994087,
-60.7175481239357));
#138376=CARTESIAN_POINT('Ctrl Pts',(-57.6525421683829,-21.98000002,-60.7382102053579));
#138377=CARTESIAN_POINT('Ctrl Pts',(-58.0662048046675,-21.98000002,-60.8621882839625));
#138378=CARTESIAN_POINT('Ctrl Pts',(-57.5245249214072,-22.4066238608121,
-60.8508735991007));
#138379=CARTESIAN_POINT('Ctrl Pts',(-57.5817506954797,-21.98000002,-60.8779152752782));
#138380=CARTESIAN_POINT('Ctrl Pts',(-57.9716987024741,-21.98000002,-61.0621827299711));
#138381=CARTESIAN_POINT('',(-57.9716987024741,-21.98000002,-61.0621827299711));
#138382=CARTESIAN_POINT('Origin',(-57.9716987024741,-22.48000002,-61.0621827299711));
#138383=CARTESIAN_POINT('Origin',(-55.9860799622262,-21.98000002,-60.2945890942193));
#138384=CARTESIAN_POINT('Origin',(83.2809572255632,-21.9800000199999,-55.24995));
#138385=CARTESIAN_POINT('',(-59.5,-21.98000002,-58.1532962439713));
#138386=CARTESIAN_POINT('Ctrl Pts',(-59.5,-21.98000002,-58.1532962439713));
#138387=CARTESIAN_POINT('Ctrl Pts',(-59.5,-21.98000002,-57.9611810443356));
#138388=CARTESIAN_POINT('Ctrl Pts',(-59.4783898617064,-21.9800000201789,
-57.7727385086896));
#138389=CARTESIAN_POINT('Ctrl Pts',(-59.435440674215,-21.9800000198205,
-57.587937528972));
#138390=CARTESIAN_POINT('Ctrl Pts',(-59.4262406555698,-21.9800000197437,
-57.5483518567313));
#138391=CARTESIAN_POINT('Ctrl Pts',(-59.4160613127736,-21.9800000196281,
-57.5089332628346));
#138392=CARTESIAN_POINT('Ctrl Pts',(-59.4049049949538,-21.9800000194259,
-57.469681421663));
#138393=CARTESIAN_POINT('Ctrl Pts',(-59.3987196130206,-21.9800000193138,
-57.4479190773891));
#138394=CARTESIAN_POINT('Ctrl Pts',(-59.3922287663824,-21.9800000192153,
-57.4261931844644));
#138395=CARTESIAN_POINT('Ctrl Pts',(-59.3854342581924,-21.9800000191476,
-57.4045116647966));
#138396=CARTESIAN_POINT('Ctrl Pts',(-59.366537060127,-21.9800000189591,
-57.3442100270524));
#138397=CARTESIAN_POINT('Ctrl Pts',(-59.3452714576318,-21.9800000190536,
-57.2844762659556));
#138398=CARTESIAN_POINT('Ctrl Pts',(-59.3218795388589,-21.9800000193212,
-57.2258422130826));
#138399=CARTESIAN_POINT('Ctrl Pts',(-59.3106878533869,-21.9800000194493,
-57.1977891968217));
#138400=CARTESIAN_POINT('Ctrl Pts',(-59.2990101624398,-21.9800000196077,
-57.1699876439618));
#138401=CARTESIAN_POINT('Ctrl Pts',(-59.2868766202345,-21.9800000197421,
-57.1424936459686));
#138402=CARTESIAN_POINT('Ctrl Pts',(-59.2731919149499,-21.9800000198936,
-57.1114847902475));
#138403=CARTESIAN_POINT('Ctrl Pts',(-59.2588942022727,-21.9800000199412,
-57.0807856309711));
#138404=CARTESIAN_POINT('Ctrl Pts',(-59.2440132425671,-21.9800000199676,
-57.0504664636976));
#138405=CARTESIAN_POINT('Ctrl Pts',(-59.2100364625762,-21.9800000200278,
-56.981240573947));
#138406=CARTESIAN_POINT('Ctrl Pts',(-59.1729132668602,-21.9800000200007,
-56.9136446874655));
#138407=CARTESIAN_POINT('Ctrl Pts',(-59.1326772603361,-21.9800000199982,
-56.8478208127099));
#138408=CARTESIAN_POINT('Ctrl Pts',(-59.1305108981493,-21.9800000199981,
-56.8442767643418));
#138409=CARTESIAN_POINT('Ctrl Pts',(-59.1283355234414,-21.9800000199979,
-56.8407378470944));
#138410=CARTESIAN_POINT('Ctrl Pts',(-59.1261511452891,-21.9800000199978,
-56.8372040811614));
#138411=CARTESIAN_POINT('Ctrl Pts',(-59.1024586951323,-21.980000019996,
-56.7988757481558));
#138412=CARTESIAN_POINT('Ctrl Pts',(-59.0776978833329,-21.9800000199944,
-56.7611395583364));
#138413=CARTESIAN_POINT('Ctrl Pts',(-59.051864196737,-21.9800000199939,
-56.7239980129523));
#138414=CARTESIAN_POINT('Ctrl Pts',(-58.9794118018617,-21.9800000199925,
-56.6198319311016));
#138415=CARTESIAN_POINT('Ctrl Pts',(-58.897983005211,-21.9800000199984,
-56.5200000236488));
#138416=CARTESIAN_POINT('Ctrl Pts',(-58.8106774361301,-21.9800000199995,
-56.4282264859168));
#138417=CARTESIAN_POINT('Ctrl Pts',(-58.7700668687888,-21.9800000200001,
-56.3855376234141));
#138418=CARTESIAN_POINT('Ctrl Pts',(-58.7280754192644,-21.98000002,-56.3444004714051));
#138419=CARTESIAN_POINT('Ctrl Pts',(-58.6847050658881,-21.98000002,-56.3048126520436));
#138420=CARTESIAN_POINT('Ctrl Pts',(-58.6494885520011,-21.98000002,-56.2726675371952));
#138421=CARTESIAN_POINT('Ctrl Pts',(-58.6132573779918,-21.98000002,-56.2414509676698));
#138422=CARTESIAN_POINT('Ctrl Pts',(-58.5760924792892,-21.98000002,-56.2112492084164));
#138423=CARTESIAN_POINT('Ctrl Pts',(-58.5607621926284,-21.98000002,-56.1987911729265));
#138424=CARTESIAN_POINT('Ctrl Pts',(-58.5452724940588,-21.98000002,-56.1865050278631));
#138425=CARTESIAN_POINT('Ctrl Pts',(-58.5296351858009,-21.98000002,-56.174399760192));
#138426=CARTESIAN_POINT('Ctrl Pts',(-58.50318856599,-21.98000002,-56.1539267090422));
#138427=CARTESIAN_POINT('Ctrl Pts',(-58.4762743935287,-21.98000002,-56.1339724230775));
#138428=CARTESIAN_POINT('Ctrl Pts',(-58.4489601509993,-21.98000002,-56.1145700874369));
#138429=CARTESIAN_POINT('Ctrl Pts',(-58.3958489442448,-21.98000002,-56.0768431961047));
#138430=CARTESIAN_POINT('Ctrl Pts',(-58.3412467373532,-21.9800000154289,
-56.0410944834472));
#138431=CARTESIAN_POINT('Ctrl Pts',(-58.2853645640813,-21.9799999916842,
-56.0075334770553));
#138432=CARTESIAN_POINT('Ctrl Pts',(-58.2574234774454,-21.9799999798118,
-55.9907529738594));
#138433=CARTESIAN_POINT('Ctrl Pts',(-58.2291619777336,-21.9799999666902,
-55.9745206253323));
#138434=CARTESIAN_POINT('Ctrl Pts',(-58.2006099144576,-21.9799999607144,
-55.9588587007899));
#138435=CARTESIAN_POINT('Ctrl Pts',(-58.1720578511817,-21.9799999547386,
-55.9431967762476));
#138436=CARTESIAN_POINT('Ctrl Pts',(-58.1432152243425,-21.9799999567774,
-55.9281052756887));
#138437=CARTESIAN_POINT('Ctrl Pts',(-58.1141118834472,-21.9799999679397,
-55.9136064684357));
#138438=CARTESIAN_POINT('',(-59.5,-21.98000002,-174.47822483969));
#138439=CARTESIAN_POINT('',(-59.5,-21.98000002,-58.1720074546108));
#138440=CARTESIAN_POINT('',(-58.2281061322626,-21.9800000072249,-176.657965001847));
#138441=CARTESIAN_POINT('Ctrl Pts',(-58.2281061322555,-21.9799999688995,
-176.657965001835));
#138442=CARTESIAN_POINT('Ctrl Pts',(-58.276338147052,-21.9799999587489,
-176.630735497029));
#138443=CARTESIAN_POINT('Ctrl Pts',(-58.3235842378115,-21.9799999676447,
-176.601941540627));
#138444=CARTESIAN_POINT('Ctrl Pts',(-58.3697659029187,-21.9799999836463,
-176.571657891927));
#138445=CARTESIAN_POINT('Ctrl Pts',(-58.4333419149396,-21.9800000056749,
-176.529967892024));
#138446=CARTESIAN_POINT('Ctrl Pts',(-58.4951281469291,-21.9800000132519,
-176.485368653424));
#138447=CARTESIAN_POINT('Ctrl Pts',(-58.554457957275,-21.9800000168151,
-176.438221543424));
#138448=CARTESIAN_POINT('Ctrl Pts',(-58.5638633718778,-21.98000001738,-176.430747423512));
#138449=CARTESIAN_POINT('Ctrl Pts',(-58.5732071081931,-21.9800000178323,
-176.423209364713));
#138450=CARTESIAN_POINT('Ctrl Pts',(-58.582486579001,-21.9800000181999,
-176.415608906189));
#138451=CARTESIAN_POINT('Ctrl Pts',(-58.6422321318881,-21.9800000205672,
-176.366673616007));
#138452=CARTESIAN_POINT('Ctrl Pts',(-58.6996264562076,-21.9800000199999,
-176.315076489292));
#138453=CARTESIAN_POINT('Ctrl Pts',(-58.754548274659,-21.9800000199988,
-176.260908374673));
#138454=CARTESIAN_POINT('Ctrl Pts',(-58.7869024533102,-21.9800000199981,
-176.228998199318));
#138455=CARTESIAN_POINT('Ctrl Pts',(-58.8184303801206,-21.9800000199976,
-176.196159475715));
#138456=CARTESIAN_POINT('Ctrl Pts',(-58.8491278703888,-21.9800000199976,
-176.162387482235));
#138457=CARTESIAN_POINT('Ctrl Pts',(-58.9319941632242,-21.9800000199974,
-176.071221726439));
#138458=CARTESIAN_POINT('Ctrl Pts',(-59.0089727564858,-21.9800000199996,
-175.972743969313));
#138459=CARTESIAN_POINT('Ctrl Pts',(-59.0773246245197,-21.9800000199999,
-175.870559516175));
#138460=CARTESIAN_POINT('Ctrl Pts',(-59.1060118933486,-21.98000002,-175.82767271642));
#138461=CARTESIAN_POINT('Ctrl Pts',(-59.1333062996812,-21.98000002,-175.784013939838));
#138462=CARTESIAN_POINT('Ctrl Pts',(-59.1592107352546,-21.98000002,-175.739584721266));
#138463=CARTESIAN_POINT('Ctrl Pts',(-59.1950270177852,-21.98000002,-175.678155494582));
#138464=CARTESIAN_POINT('Ctrl Pts',(-59.2281939400895,-21.9800000200315,
-175.615256612429));
#138465=CARTESIAN_POINT('Ctrl Pts',(-59.2587125449347,-21.9800000196412,
-175.550888840134));
#138466=CARTESIAN_POINT('Ctrl Pts',(-59.311304650302,-21.9800000189686,
-175.439965137037));
#138467=CARTESIAN_POINT('Ctrl Pts',(-59.356300154325,-21.98000001654,-175.323678961831));
#138468=CARTESIAN_POINT('Ctrl Pts',(-59.3921466355886,-21.9800000173947,
-175.205510135853));
#138469=CARTESIAN_POINT('Ctrl Pts',(-59.3996691193178,-21.9800000175741,
-175.180712079269));
#138470=CARTESIAN_POINT('Ctrl Pts',(-59.4067991608449,-21.9800000178929,
-175.15584684927));
#138471=CARTESIAN_POINT('Ctrl Pts',(-59.4135356395821,-21.9800000182925,
-175.130914599889));
#138472=CARTESIAN_POINT('Ctrl Pts',(-59.4621021364636,-21.9800000211732,
-174.95116609046));
#138473=CARTESIAN_POINT('Ctrl Pts',(-59.4903344201326,-21.9800000199997,
-174.767951128816));
#138474=CARTESIAN_POINT('Ctrl Pts',(-59.4979153635687,-21.98000002,-174.581221680408));
#138475=CARTESIAN_POINT('Ctrl Pts',(-59.4993044120658,-21.98000002,-174.547007434931));
#138476=CARTESIAN_POINT('Ctrl Pts',(-59.5,-21.98000002,-174.51267523574));
#138477=CARTESIAN_POINT('Ctrl Pts',(-59.5,-21.98000002,-174.47822483969));
#138478=CARTESIAN_POINT('',(-58.2281061322669,-21.98000002,-171.871644662643));
#138479=CARTESIAN_POINT('',(-58.2281061322669,-21.98000002,-176.848603273909));
#138480=CARTESIAN_POINT('',(-58.085700246061,-21.98000002,-171.237717270032));
#138481=CARTESIAN_POINT('Origin',(-56.8433387827296,-21.9799994107774,-171.841912580654));
#138482=CARTESIAN_POINT('',(-40.032098818041,-21.98000002,-133.252725050377));
#138483=CARTESIAN_POINT('Ctrl Pts',(-40.0320988180411,-21.98000002,-133.252725050377));
#138484=CARTESIAN_POINT('Ctrl Pts',(-46.0913111616059,-21.98000002,-145.894738473846));
#138485=CARTESIAN_POINT('Ctrl Pts',(-52.0964027110273,-21.98000002,-158.56247456275));
#138486=CARTESIAN_POINT('Ctrl Pts',(-58.085700246061,-21.98000002,-171.237717270032));
#138487=CARTESIAN_POINT('',(-39.5,-21.98000002,-130.903539806302));
#138488=CARTESIAN_POINT('Ctrl Pts',(-39.5,-21.98000002,-130.903539806302));
#138489=CARTESIAN_POINT('Ctrl Pts',(-39.5,-21.98000002,-131.168997483201));
#138490=CARTESIAN_POINT('Ctrl Pts',(-39.5196729008534,-21.98000002,-131.434381070373));
#138491=CARTESIAN_POINT('Ctrl Pts',(-39.5579798343684,-21.98000002,-131.695636340074));
#138492=CARTESIAN_POINT('Ctrl Pts',(-39.5785131750233,-21.98000002,-131.83567478634));
#138493=CARTESIAN_POINT('Ctrl Pts',(-39.6044013642058,-21.98000002,-131.974527214008));
#138494=CARTESIAN_POINT('Ctrl Pts',(-39.6354904757816,-21.98000002,-132.111568426422));
#138495=CARTESIAN_POINT('Ctrl Pts',(-39.7067779603525,-21.98000002,-132.425804595305));
#138496=CARTESIAN_POINT('Ctrl Pts',(-39.8050570910391,-21.98000002,-132.732328205563));
#138497=CARTESIAN_POINT('Ctrl Pts',(-39.9318010945657,-21.98000002,-133.030718310503));
#138498=CARTESIAN_POINT('Ctrl Pts',(-39.9634506501685,-21.98000002,-133.105230034567));
#138499=CARTESIAN_POINT('Ctrl Pts',(-39.9968754124349,-21.98000002,-133.179234513781));
#138500=CARTESIAN_POINT('Ctrl Pts',(-40.032098818041,-21.98000002,-133.252725050377));
#138501=CARTESIAN_POINT('',(-39.5,-21.98000002,-101.155103165204));
#138502=CARTESIAN_POINT('',(-39.5,-21.98000002,-55.24995));
#138503=CARTESIAN_POINT('',(-40.032098818038,-21.98000002,-98.8059179211358));
#138504=CARTESIAN_POINT('Ctrl Pts',(-40.032098818038,-21.98000002,-98.8059179211359));
#138505=CARTESIAN_POINT('Ctrl Pts',(-39.9030508971582,-21.98000002,-99.0751650535143));
#138506=CARTESIAN_POINT('Ctrl Pts',(-39.796952812407,-21.98000002,-99.355201219722));
#138507=CARTESIAN_POINT('Ctrl Pts',(-39.7146317074507,-21.98000002,-99.6400255235421));
#138508=CARTESIAN_POINT('Ctrl Pts',(-39.6845025786603,-21.98000002,-99.7442698499147));
#138509=CARTESIAN_POINT('Ctrl Pts',(-39.6575579700037,-21.98000002,-99.8491553321735));
#138510=CARTESIAN_POINT('Ctrl Pts',(-39.6338367806139,-21.98000002,-99.9543872911712));
#138511=CARTESIAN_POINT('Ctrl Pts',(-39.5613885485579,-21.98000002,-100.275782195106));
#138512=CARTESIAN_POINT('Ctrl Pts',(-39.5178914194315,-21.98000002,-100.602110104163));
#138513=CARTESIAN_POINT('Ctrl Pts',(-39.5044747449633,-21.98000002,-100.933563458968));
#138514=CARTESIAN_POINT('Ctrl Pts',(-39.5014958184563,-21.98000002,-101.007156597626));
#138515=CARTESIAN_POINT('Ctrl Pts',(-39.5,-21.98000002,-101.081002444678));
#138516=CARTESIAN_POINT('Ctrl Pts',(-39.5,-21.98000002,-101.155103165204));
#138517=CARTESIAN_POINT('Ctrl Pts',(-57.9716987024741,-21.98000002,-61.0621827299711));
#138518=CARTESIAN_POINT('Ctrl Pts',(-52.0201508381868,-21.98000002,-73.6568877040663));
#138519=CARTESIAN_POINT('Ctrl Pts',(-46.0528675815424,-21.98000002,-86.2441136451113));
#138520=CARTESIAN_POINT('Ctrl Pts',(-40.032098818038,-21.98000002,-98.8059179211357));
#138521=CARTESIAN_POINT('Ctrl Pts',(-59.5,-21.98000002,-58.1532962439713));
#138522=CARTESIAN_POINT('Ctrl Pts',(-60.,-21.98000002,-58.1532962439712));
#138523=CARTESIAN_POINT('Ctrl Pts',(-60.,-21.48000002,-58.1532962439713));
#138524=CARTESIAN_POINT('Ctrl Pts',(-59.4999999930587,-21.98000002,-57.8972567292831));
#138525=CARTESIAN_POINT('Ctrl Pts',(-59.9980388947882,-21.98000002,-57.846724408982));
#138526=CARTESIAN_POINT('Ctrl Pts',(-60.,-21.4819649551771,-57.8461243349599));
#138527=CARTESIAN_POINT('Ctrl Pts',(-59.4616086582853,-21.98000002,-57.6476410381502));
#138528=CARTESIAN_POINT('Ctrl Pts',(-59.9502437945621,-21.9800000199991,
-57.5478013960511));
#138529=CARTESIAN_POINT('Ctrl Pts',(-59.9539303867693,-21.4838860106857,
-57.5466594347187));
#138530=CARTESIAN_POINT('Ctrl Pts',(-59.34730526825,-21.98000002,-57.282960076491));
#138531=CARTESIAN_POINT('Ctrl Pts',(-59.8105866338858,-21.9800000200004,
-57.1115394631459));
#138532=CARTESIAN_POINT('Ctrl Pts',(-59.8167663234865,-21.4866995950233,
-57.1091506902012));
#138533=CARTESIAN_POINT('Ctrl Pts',(-59.29968672466,-21.98000002,-57.1639308209523));
#138534=CARTESIAN_POINT('Ctrl Pts',(-59.7527585815745,-21.9800000200004,
-56.9693956543515));
#138535=CARTESIAN_POINT('Ctrl Pts',(-59.7596240701279,-21.4876191423699,
-56.9663510387935));
#138536=CARTESIAN_POINT('Ctrl Pts',(-59.1883295347111,-21.98000002,-56.9370071244832));
#138537=CARTESIAN_POINT('Ctrl Pts',(-59.6179788443353,-21.9800000199995,
-56.6986593938776));
#138538=CARTESIAN_POINT('Ctrl Pts',(-59.6259954411174,-21.4893742131836,
-56.694110313108));
#138539=CARTESIAN_POINT('Ctrl Pts',(-59.1243146931145,-21.98000002,-56.8281652030541));
#138540=CARTESIAN_POINT('Ctrl Pts',(-59.5407153644089,-21.9800000200004,
-56.5688983662156));
#138541=CARTESIAN_POINT('Ctrl Pts',(-59.5491776307125,-21.4902170457339,
-56.5635325439996));
#138542=CARTESIAN_POINT('Ctrl Pts',(-58.9794096363452,-21.98000002,-56.6198336495764));
#138543=CARTESIAN_POINT('Ctrl Pts',(-59.3661855631985,-21.9800000199995,
-56.3207427939796));
#138544=CARTESIAN_POINT('Ctrl Pts',(-59.3752915646391,-21.4918319317587,
-56.3135970508604));
#138545=CARTESIAN_POINT('Ctrl Pts',(-58.897981763705,-21.98000002,-56.5200008958119));
#138546=CARTESIAN_POINT('Ctrl Pts',(-59.268291108539,-21.98000002,-56.2019010018047));
#138547=CARTESIAN_POINT('Ctrl Pts',(-59.2775781171727,-21.4926066631124,
-56.1938276864606));
#138548=CARTESIAN_POINT('Ctrl Pts',(-58.7233721306083,-21.98000002,-56.3364530063454));
#138549=CARTESIAN_POINT('Ctrl Pts',(-59.058685939558,-21.98000002,-55.9835815924875));
#138550=CARTESIAN_POINT('Ctrl Pts',(-59.0680465560033,-21.4940322909708,
-55.9736253396869));
#138551=CARTESIAN_POINT('Ctrl Pts',(-58.6296851267041,-21.98000002,-56.251851153689));
#138552=CARTESIAN_POINT('Ctrl Pts',(-58.9463663728276,-21.98000002,-55.8830032045419));
#138553=CARTESIAN_POINT('Ctrl Pts',(-58.9556221515304,-21.4946900550471,
-55.8721285607086));
#138554=CARTESIAN_POINT('Ctrl Pts',(-58.3295353039945,-21.98000002,-56.0194969731979));
#138555=CARTESIAN_POINT('Ctrl Pts',(-58.587136508474,-21.98000002,-55.607131606824));
#138556=CARTESIAN_POINT('Ctrl Pts',(-58.5954423658223,-21.4964978360334,
-55.5933734977247));
#138557=CARTESIAN_POINT('Ctrl Pts',(-58.1016300300823,-21.98000002,-55.8934667289665));
#138558=CARTESIAN_POINT('Ctrl Pts',(-58.3146314565664,-21.9800000200043,
-55.4574637281066));
#138559=CARTESIAN_POINT('Ctrl Pts',(-58.3219561351612,-21.4974802329133,
-55.4421752934307));
#138560=CARTESIAN_POINT('Ctrl Pts',(-57.866513770968,-21.98000002,-55.8065234638013));
#138561=CARTESIAN_POINT('Ctrl Pts',(-58.0337433152366,-21.98000002,-55.3542930871701));
#138562=CARTESIAN_POINT('Ctrl Pts',(-58.0398165251616,-21.4981583243581,
-55.3378696135325));
#138563=CARTESIAN_POINT('',(-60.,-21.48000002,-58.1532962439713));
#138564=CARTESIAN_POINT('Ctrl Pts',(-58.0831736437664,-21.4980516416407,
-55.3542805420642));
#138565=CARTESIAN_POINT('Ctrl Pts',(-58.3499299718387,-21.4973788455131,
-55.4577804898745));
#138566=CARTESIAN_POINT('Ctrl Pts',(-58.6077613800678,-21.4964360055793,
-55.6029075907754));
#138567=CARTESIAN_POINT('Ctrl Pts',(-58.9556221515304,-21.4946900550471,
-55.8721285607086));
#138568=CARTESIAN_POINT('Ctrl Pts',(-59.0680465560033,-21.4940322909708,
-55.9736253396869));
#138569=CARTESIAN_POINT('Ctrl Pts',(-59.2775781171727,-21.4926066631124,
-56.1938276864606));
#138570=CARTESIAN_POINT('Ctrl Pts',(-59.3752915646391,-21.4918319317587,
-56.3135970508604));
#138571=CARTESIAN_POINT('Ctrl Pts',(-59.5491776307125,-21.4902170457339,
-56.5635325439996));
#138572=CARTESIAN_POINT('Ctrl Pts',(-59.6259954411174,-21.4893742131836,
-56.694110313108));
#138573=CARTESIAN_POINT('Ctrl Pts',(-59.7596240701279,-21.4876191423699,
-56.9663510387935));
#138574=CARTESIAN_POINT('Ctrl Pts',(-59.8167663234865,-21.4866995950233,
-57.1091506902012));
#138575=CARTESIAN_POINT('Ctrl Pts',(-59.9539303867693,-21.4838860106857,
-57.5466594347187));
#138576=CARTESIAN_POINT('Ctrl Pts',(-60.,-21.4819649551771,-57.8461243349599));
#138577=CARTESIAN_POINT('Ctrl Pts',(-60.,-21.48000002,-58.1532962439713));
#138578=CARTESIAN_POINT('Origin',(-59.5,-21.48000002,-58.1532962439713));
#138579=CARTESIAN_POINT('Ctrl Pts',(-58.04813900635,-21.5914605167321,-55.3445609916381));
#138580=CARTESIAN_POINT('Ctrl Pts',(-59.9999999999999,-21.563522065113,
-56.0718305306275));
#138581=CARTESIAN_POINT('Ctrl Pts',(-60.,-21.4835561881163,-58.1534328789326));
#138582=CARTESIAN_POINT('Ctrl Pts',(-58.0747408021895,-21.3932704964989,
-55.3468739572293));
#138583=CARTESIAN_POINT('Ctrl Pts',(-60.,-21.3649831049967,-56.0851953591942));
#138584=CARTESIAN_POINT('Ctrl Pts',(-60.,-21.2836204844253,-58.1457522408661));
#138585=CARTESIAN_POINT('Ctrl Pts',(-58.1004355836544,-21.1945366814225,
-55.3490436413214));
#138586=CARTESIAN_POINT('Ctrl Pts',(-59.9999999999994,-21.1653697703472,
-56.0975649789358));
#138587=CARTESIAN_POINT('Ctrl Pts',(-60.,-21.0836896865644,-58.1378552621726));
#138588=CARTESIAN_POINT('Ctrl Pts',(-58.1252156299349,-20.9953105578148,
-55.3510803367174));
#138589=CARTESIAN_POINT('Ctrl Pts',(-60.,-20.9648839320844,-56.1090266406884));
#138590=CARTESIAN_POINT('Ctrl Pts',(-60.,-20.883761812232,-58.1298294552074));
#138591=CARTESIAN_POINT('',(-60.,-20.98000002,-58.1336824582564));
#138592=CARTESIAN_POINT('Ctrl Pts',(-60.,-20.98000002,-58.1336824582564));
#138593=CARTESIAN_POINT('Ctrl Pts',(-60.,-20.9819903749844,-57.8341710601268));
#138594=CARTESIAN_POINT('Ctrl Pts',(-59.9561544625383,-20.9839354847036,
-57.5420008057396));
#138595=CARTESIAN_POINT('Ctrl Pts',(-59.8258072839812,-20.986783840298,
-57.1148311652303));
#138596=CARTESIAN_POINT('Ctrl Pts',(-59.7713392035954,-20.9877182523804,
-56.9748142265907));
#138597=CARTESIAN_POINT('Ctrl Pts',(-59.6439928678614,-20.9895019296767,
-56.7077325083257));
#138598=CARTESIAN_POINT('Ctrl Pts',(-59.5707888728218,-20.9903591646404,
-56.5794722449985));
#138599=CARTESIAN_POINT('Ctrl Pts',(-59.4052064654638,-20.9920036864946,
-56.333575365965));
#138600=CARTESIAN_POINT('Ctrl Pts',(-59.3119800474081,-20.9927961294943,
-56.2151695770875));
#138601=CARTESIAN_POINT('Ctrl Pts',(-59.1114408594098,-20.9942622260151,
-55.9962288706011));
#138602=CARTESIAN_POINT('Ctrl Pts',(-59.0038498495005,-20.9949406197357,
-55.8949841496734));
#138603=CARTESIAN_POINT('Ctrl Pts',(-58.6648804276695,-20.9967833899732,
-55.6200886254342));
#138604=CARTESIAN_POINT('Ctrl Pts',(-58.4095966121519,-20.9978001101244,
-55.4685923770156));
#138605=CARTESIAN_POINT('Ctrl Pts',(-58.1440639002148,-20.9985364556097,
-55.3589167601806));
#138606=CARTESIAN_POINT('Ctrl Pts',(-60.,-20.98000002,-58.1336824582564));
#138607=CARTESIAN_POINT('Ctrl Pts',(-60.,-21.1466635001965,-58.1403364979909));
#138608=CARTESIAN_POINT('Ctrl Pts',(-60.,-21.3133297017902,-58.1468913732678));
#138609=CARTESIAN_POINT('Ctrl Pts',(-60.,-21.48000002,-58.1532962439713));
#138610=CARTESIAN_POINT('Ctrl Pts',(-60.,-20.98000002,-58.1336824582564));
#138611=CARTESIAN_POINT('Ctrl Pts',(-60.,-20.48000002,-58.1336824582564));
#138612=CARTESIAN_POINT('Ctrl Pts',(-59.5,-20.48000002,-58.1336824582564));
#138613=CARTESIAN_POINT('Ctrl Pts',(-60.,-20.9819903749844,-57.8341710601268));
#138614=CARTESIAN_POINT('Ctrl Pts',(-60.0019943000202,-20.4800000199965,
-57.8335762296713));
#138615=CARTESIAN_POINT('Ctrl Pts',(-59.4999999932334,-20.48000002,-57.8840234061944));
#138616=CARTESIAN_POINT('Ctrl Pts',(-59.9561544625383,-20.9839354847036,
-57.5420008057396));
#138617=CARTESIAN_POINT('Ctrl Pts',(-59.9599487537765,-20.48000002,-57.5408569976555));
#138618=CARTESIAN_POINT('Ctrl Pts',(-59.4634620545497,-20.48000002,-57.6404834185301));
#138619=CARTESIAN_POINT('Ctrl Pts',(-59.8258072839812,-20.986783840298,
-57.1148311652303));
#138620=CARTESIAN_POINT('Ctrl Pts',(-59.8322564407851,-20.48000002,-57.1124079291466));
#138621=CARTESIAN_POINT('Ctrl Pts',(-59.3548394021004,-20.48000002,-57.2844137892711));
#138622=CARTESIAN_POINT('Ctrl Pts',(-59.7713392035954,-20.9877182523804,
-56.9748142265907));
#138623=CARTESIAN_POINT('Ctrl Pts',(-59.7785418471728,-20.4800000199998,
-56.971709946724));
#138624=CARTESIAN_POINT('Ctrl Pts',(-59.3094493357903,-20.48000002,-57.1677018516063));
#138625=CARTESIAN_POINT('Ctrl Pts',(-59.6439928678614,-20.9895019296767,
-56.7077325083257));
#138626=CARTESIAN_POINT('Ctrl Pts',(-59.6524902953505,-20.4800000200002,
-56.7030545690594));
#138627=CARTESIAN_POINT('Ctrl Pts',(-59.2033273904236,-20.48000002,-56.945074258738));
#138628=CARTESIAN_POINT('Ctrl Pts',(-59.5707888728218,-20.9903591646404,
-56.5794722449985));
#138629=CARTESIAN_POINT('Ctrl Pts',(-59.5798070038494,-20.4800000200006,
-56.5739310816022));
#138630=CARTESIAN_POINT('Ctrl Pts',(-59.1423240613999,-20.48000002,-56.8381621017045));
#138631=CARTESIAN_POINT('Ctrl Pts',(-59.4052064654638,-20.9920036864946,
-56.333575365965));
#138632=CARTESIAN_POINT('Ctrl Pts',(-59.4150201769345,-20.4800000199993,
-56.3261371955428));
#138633=CARTESIAN_POINT('Ctrl Pts',(-59.0043387205048,-20.48000002,-56.6331931445326));
#138634=CARTESIAN_POINT('Ctrl Pts',(-59.3119800474081,-20.9927961294943,
-56.2151695770875));
#138635=CARTESIAN_POINT('Ctrl Pts',(-59.322050076116,-20.4800000199998,
-56.2067284595684));
#138636=CARTESIAN_POINT('Ctrl Pts',(-58.9266500387652,-20.48000002,-56.5344951934464));
#138637=CARTESIAN_POINT('Ctrl Pts',(-59.1114408594098,-20.9942622260151,
-55.9962288706011));
#138638=CARTESIAN_POINT('Ctrl Pts',(-59.1217230649246,-20.4800000200002,
-55.9857285998647));
#138639=CARTESIAN_POINT('Ctrl Pts',(-58.7595340502496,-20.48000002,-56.3519956346149));
#138640=CARTESIAN_POINT('Ctrl Pts',(-59.0038498495005,-20.9949406197357,
-55.8949841496734));
#138641=CARTESIAN_POINT('Ctrl Pts',(-59.0140876322601,-20.4800000199996,
-55.8834675579712));
#138642=CARTESIAN_POINT('Ctrl Pts',(-58.6698748748721,-20.48000002,-56.2676023678844));
#138643=CARTESIAN_POINT('Ctrl Pts',(-58.6593792112359,-20.9968132967355,
-55.6156272797255));
#138644=CARTESIAN_POINT('Ctrl Pts',(-58.6688057859238,-20.4800000200008,
-55.6008859078189));
#138645=CARTESIAN_POINT('Ctrl Pts',(-58.3828160087866,-20.48000002,-56.0347423933717));
#138646=CARTESIAN_POINT('Ctrl Pts',(-58.3970469849622,-20.9978498953169,
-55.4611742661273));
#138647=CARTESIAN_POINT('Ctrl Pts',(-58.4055356761976,-20.48000002,-55.4446537909846));
#138648=CARTESIAN_POINT('Ctrl Pts',(-58.1642057412792,-20.48000002,-55.9059968521648));
#138649=CARTESIAN_POINT('Ctrl Pts',(-58.124493706486,-20.9985901469525,
-55.3509197556537));
#138650=CARTESIAN_POINT('Ctrl Pts',(-58.1317309492636,-20.48000002,-55.333033840343));
#138651=CARTESIAN_POINT('Ctrl Pts',(-57.9370780887383,-20.48000002,-55.8140933660895));
#138652=CARTESIAN_POINT('',(-59.5,-20.48000002,-58.1336824582564));
#138653=CARTESIAN_POINT('Ctrl Pts',(-58.4684744114494,-20.4800000273303,
-56.1088024963514));
#138654=CARTESIAN_POINT('Ctrl Pts',(-58.5045026577924,-20.4800000196856,
-56.1349726812033));
#138655=CARTESIAN_POINT('Ctrl Pts',(-58.5397642385231,-20.48000002049,-56.1620276028478));
#138656=CARTESIAN_POINT('Ctrl Pts',(-58.5742078503022,-20.4800000209351,
-56.1899586284693));
#138657=CARTESIAN_POINT('Ctrl Pts',(-58.5777936723552,-20.4800000209814,
-56.1928664445334));
#138658=CARTESIAN_POINT('Ctrl Pts',(-58.5813717160946,-20.4800000210458,
-56.1957839761557));
#138659=CARTESIAN_POINT('Ctrl Pts',(-58.5849420358152,-20.480000021133,
-56.198711293078));
#138660=CARTESIAN_POINT('Ctrl Pts',(-58.6712575877011,-20.4800000232427,
-56.2694816989427));
#138661=CARTESIAN_POINT('Ctrl Pts',(-58.7525761505105,-20.4800000208245,
-56.3458655479582));
#138662=CARTESIAN_POINT('Ctrl Pts',(-58.8289004828144,-20.4800000205608,
-56.4278416205229));
#138663=CARTESIAN_POINT('Ctrl Pts',(-58.8336560351637,-20.4800000205444,
-56.4329493167544));
#138664=CARTESIAN_POINT('Ctrl Pts',(-58.8383922119778,-20.4800000205339,
-56.438078733635));
#138665=CARTESIAN_POINT('Ctrl Pts',(-58.8431090189103,-20.4800000205297,
-56.4432298704634));
#138666=CARTESIAN_POINT('Ctrl Pts',(-58.8623175352579,-20.480000020513,
-56.4642071327073));
#138667=CARTESIAN_POINT('Ctrl Pts',(-58.8812170617046,-20.4800000205714,
-56.4855758533909));
#138668=CARTESIAN_POINT('Ctrl Pts',(-58.8997746305286,-20.4800000209296,
-56.5072905946435));
#138669=CARTESIAN_POINT('Ctrl Pts',(-58.9619336923861,-20.4800000221292,
-56.580024688077));
#138670=CARTESIAN_POINT('Ctrl Pts',(-59.0202267572587,-20.4800000217717,
-56.6567158251598));
#138671=CARTESIAN_POINT('Ctrl Pts',(-59.0733581645971,-20.4800000210417,
-56.73565959907));
#138672=CARTESIAN_POINT('Ctrl Pts',(-59.1299234282924,-20.4800000202645,
-56.8197054697148));
#138673=CARTESIAN_POINT('Ctrl Pts',(-59.1811132500064,-20.480000019999,
-56.9067351897848));
#138674=CARTESIAN_POINT('Ctrl Pts',(-59.2269658512281,-20.4800000200342,
-56.9966989899188));
#138675=CARTESIAN_POINT('Ctrl Pts',(-59.2370332340863,-20.4800000200419,
-57.016451413886));
#138676=CARTESIAN_POINT('Ctrl Pts',(-59.2468434784441,-20.4800000200569,
-57.0363464697384));
#138677=CARTESIAN_POINT('Ctrl Pts',(-59.2563966865596,-20.480000020085,
-57.0563840875553));
#138678=CARTESIAN_POINT('Ctrl Pts',(-59.3094659573343,-20.4800000202415,
-57.167695570854));
#138679=CARTESIAN_POINT('Ctrl Pts',(-59.354874917347,-20.4800000213417,
-57.2844044844238));
#138680=CARTESIAN_POINT('Ctrl Pts',(-59.3910801060422,-20.4800000212014,
-57.4030935519939));
#138681=CARTESIAN_POINT('Ctrl Pts',(-59.4059237316432,-20.4800000211439,
-57.4517544247977));
#138682=CARTESIAN_POINT('Ctrl Pts',(-59.4192561241221,-20.4800000207682,
-57.5006743231195));
#138683=CARTESIAN_POINT('Ctrl Pts',(-59.4310694056707,-20.480000020378,
-57.5498521826326));
#138684=CARTESIAN_POINT('Ctrl Pts',(-59.453976422087,-20.4800000196214,
-57.6452124794769));
#138685=CARTESIAN_POINT('Ctrl Pts',(-59.4712138943901,-20.48000002,-57.7415452546604));
#138686=CARTESIAN_POINT('Ctrl Pts',(-59.4827195432934,-20.48000002,-57.8388478504797));
#138687=CARTESIAN_POINT('Ctrl Pts',(-59.4942251921967,-20.48000002,-57.936150446299));
#138688=CARTESIAN_POINT('Ctrl Pts',(-59.5,-20.48000002,-58.0344221425213));
#138689=CARTESIAN_POINT('Ctrl Pts',(-59.5,-20.48000002,-58.1336824582564));
#138690=CARTESIAN_POINT('Origin',(-59.5,-20.98000002,-58.1336824582564));
#138691=CARTESIAN_POINT('Ctrl Pts',(-57.8770125754992,-19.9259080025173,
-60.8508735991007));
#138692=CARTESIAN_POINT('Ctrl Pts',(-57.8224346115608,-20.48000002,-60.8252402001721));
#138693=CARTESIAN_POINT('Ctrl Pts',(-58.3269264615434,-20.48000002,-61.0621827299711));
#138694=CARTESIAN_POINT('Ctrl Pts',(-57.9394736727847,-19.9223173742648,
-60.7188022088811));
#138695=CARTESIAN_POINT('Ctrl Pts',(-57.8773360553627,-20.480000020003,
-60.6987815996246));
#138696=CARTESIAN_POINT('Ctrl Pts',(-58.4199720320461,-20.48000002,-60.8640724920291));
#138697=CARTESIAN_POINT('Ctrl Pts',(-57.9720322597472,-19.9204585218543,
-60.5756740647443));
#138698=CARTESIAN_POINT('Ctrl Pts',(-57.9049228489562,-20.4800000199977,
-60.5656525957412));
#138699=CARTESIAN_POINT('Ctrl Pts',(-58.4684744074159,-20.48000002,-60.6493857962184));
#138700=CARTESIAN_POINT('Ctrl Pts',(-57.9720322598041,-19.92045852138,-60.42825533736));
#138701=CARTESIAN_POINT('Ctrl Pts',(-57.9049228508695,-20.48000002,-60.42825533736));
#138702=CARTESIAN_POINT('Ctrl Pts',(-58.4684744114614,-20.48000002,-60.42825533736));
#138703=CARTESIAN_POINT('',(-58.3269264615434,-20.48000002,-61.0621827299711));
#138704=CARTESIAN_POINT('Origin',(-58.3269264615434,-19.98000002,-61.0621827299711));
#138705=CARTESIAN_POINT('Origin',(-56.2951177527026,-20.48000002,-60.2827926082911));
#138706=CARTESIAN_POINT('Origin',(83.2809572255632,-20.4800000199999,-55.24995));
#138707=CARTESIAN_POINT('',(-59.5,-20.48000002,-174.500886972636));
#138708=CARTESIAN_POINT('',(-58.5817791104913,-20.48000002,-176.438901946458));
#138709=CARTESIAN_POINT('Ctrl Pts',(-59.5,-20.48000002,-174.500886972636));
#138710=CARTESIAN_POINT('Ctrl Pts',(-59.5,-20.48000002,-174.594133457896));
#138711=CARTESIAN_POINT('Ctrl Pts',(-59.4948998873889,-20.48000002,-174.686506499847));
#138712=CARTESIAN_POINT('Ctrl Pts',(-59.484743418878,-20.48000002,-174.778024581704));
#138713=CARTESIAN_POINT('Ctrl Pts',(-59.4745869503671,-20.48000002,-174.869542663562));
#138714=CARTESIAN_POINT('Ctrl Pts',(-59.4593733052792,-20.4800000198432,
-174.96020535248));
#138715=CARTESIAN_POINT('Ctrl Pts',(-59.4391579117629,-20.4800000201565,
-175.050010672616));
#138716=CARTESIAN_POINT('Ctrl Pts',(-59.4270641008619,-20.4800000203439,
-175.103736490952));
#138717=CARTESIAN_POINT('Ctrl Pts',(-59.4131703468088,-20.4800000205099,
-175.157156500734));
#138718=CARTESIAN_POINT('Ctrl Pts',(-59.3974877716946,-20.4800000205022,
-175.210269911122));
#138719=CARTESIAN_POINT('Ctrl Pts',(-59.3634319732391,-20.4800000204854,
-175.325609361837));
#138720=CARTESIAN_POINT('Ctrl Pts',(-59.3206017517199,-20.4800000200584,
-175.43951508737));
#138721=CARTESIAN_POINT('Ctrl Pts',(-59.2705225473981,-20.480000020021,
-175.548294250575));
#138722=CARTESIAN_POINT('Ctrl Pts',(-59.2665668880551,-20.4800000200181,
-175.556886505965));
#138723=CARTESIAN_POINT('Ctrl Pts',(-59.2625645131408,-20.4800000200159,
-175.56545285612));
#138724=CARTESIAN_POINT('Ctrl Pts',(-59.2585154363462,-20.4800000200145,
-175.573993307709));
#138725=CARTESIAN_POINT('Ctrl Pts',(-59.223512146378,-20.4800000200017,
-175.647823446921));
#138726=CARTESIAN_POINT('Ctrl Pts',(-59.1850753506041,-20.4800000200467,
-175.719619366777));
#138727=CARTESIAN_POINT('Ctrl Pts',(-59.143147619382,-20.4800000203096,
-175.789501989862));
#138728=CARTESIAN_POINT('Ctrl Pts',(-59.1284714749915,-20.4800000204017,
-175.813963305486));
#138729=CARTESIAN_POINT('Ctrl Pts',(-59.1133672159704,-20.4800000205138,
-175.838189938605));
#138730=CARTESIAN_POINT('Ctrl Pts',(-59.0978311232235,-20.4800000206151,
-175.862186246726));
#138731=CARTESIAN_POINT('Ctrl Pts',(-59.057684395778,-20.4800000208766,
-175.924194967805));
#138732=CARTESIAN_POINT('Ctrl Pts',(-59.0143956166168,-20.4800000209379,
-175.984944386851));
#138733=CARTESIAN_POINT('Ctrl Pts',(-58.9683824813746,-20.4800000205207,
-176.043771514579));
#138734=CARTESIAN_POINT('Ctrl Pts',(-58.939956521226,-20.4800000202629,
-176.080113693386));
#138735=CARTESIAN_POINT('Ctrl Pts',(-58.9105390187326,-20.480000020158,
-176.115667750748));
#138736=CARTESIAN_POINT('Ctrl Pts',(-58.8802525752657,-20.4800000200989,
-176.150262230717));
#138737=CARTESIAN_POINT('Ctrl Pts',(-58.8008883718402,-20.4800000199439,
-176.240915441575));
#138738=CARTESIAN_POINT('Ctrl Pts',(-58.7158063838685,-20.4800000199516,
-176.324965650418));
#138739=CARTESIAN_POINT('Ctrl Pts',(-58.6252060810682,-20.4800000201162,
-176.402568149682));
#138740=CARTESIAN_POINT('Ctrl Pts',(-58.6108845926547,-20.4800000201422,
-176.414835032459));
#138741=CARTESIAN_POINT('Ctrl Pts',(-58.596406444494,-20.4800000201761,
-176.426947791328));
#138742=CARTESIAN_POINT('Ctrl Pts',(-58.5817791104913,-20.4800000202216,
-176.438901946458));
#138743=CARTESIAN_POINT('',(-59.5,-20.48000002,-174.524030413304));
#138744=CARTESIAN_POINT('',(-39.9829309662066,-20.48000002,-99.9929964369266));
#138745=CARTESIAN_POINT('Ctrl Pts',(-39.9829309662066,-20.48000002,-99.9929964369266));
#138746=CARTESIAN_POINT('Ctrl Pts',(-46.1212593572987,-20.48000002,-87.0272166609364));
#138747=CARTESIAN_POINT('Ctrl Pts',(-52.2285110086243,-20.48000002,-74.0467697366574));
#138748=CARTESIAN_POINT('Ctrl Pts',(-58.3269264615434,-20.48000002,-61.0621827299711));
#138749=CARTESIAN_POINT('',(-39.5,-20.48000002,-102.144196959718));
#138750=CARTESIAN_POINT('Ctrl Pts',(-39.5,-20.48000002,-102.144196959718));
#138751=CARTESIAN_POINT('Ctrl Pts',(-39.5,-20.48000002,-101.901224059727));
#138752=CARTESIAN_POINT('Ctrl Pts',(-39.5178405979396,-20.48000002,-101.658367298417));
#138753=CARTESIAN_POINT('Ctrl Pts',(-39.5526223904373,-20.48000002,-101.419269624472));
#138754=CARTESIAN_POINT('Ctrl Pts',(-39.5712680114436,-20.48000002,-101.291095534188));
#138755=CARTESIAN_POINT('Ctrl Pts',(-39.5947811831661,-20.48000002,-101.164001820978));
#138756=CARTESIAN_POINT('Ctrl Pts',(-39.6230172792885,-20.48000002,-101.038548856259));
#138757=CARTESIAN_POINT('Ctrl Pts',(-39.6919421332755,-20.48000002,-100.732315755265));
#138758=CARTESIAN_POINT('Ctrl Pts',(-39.7887207445114,-20.48000002,-100.433895586513));
#138759=CARTESIAN_POINT('Ctrl Pts',(-39.9146180003308,-20.48000002,-100.143643141333));
#138760=CARTESIAN_POINT('Ctrl Pts',(-39.9365064258825,-20.48000002,-100.093180015698));
#138761=CARTESIAN_POINT('Ctrl Pts',(-39.9592751462328,-20.48000002,-100.04296381121));
#138762=CARTESIAN_POINT('Ctrl Pts',(-39.9829309662065,-20.48000002,-99.9929964369266));
#138763=CARTESIAN_POINT('',(-39.5,-20.48000002,-129.914446011788));
#138764=CARTESIAN_POINT('',(-39.5,-20.48000002,-55.24995));
#138765=CARTESIAN_POINT('',(-39.9829309662066,-20.48000002,-132.065646534579));
#138766=CARTESIAN_POINT('Ctrl Pts',(-39.9829309662066,-20.48000002,-132.065646534579));
#138767=CARTESIAN_POINT('Ctrl Pts',(-39.8887941972359,-20.48000002,-131.866804677725));
#138768=CARTESIAN_POINT('Ctrl Pts',(-39.808012721684,-20.48000002,-131.661768384106));
#138769=CARTESIAN_POINT('Ctrl Pts',(-39.7410867352538,-20.48000002,-131.45329068418));
#138770=CARTESIAN_POINT('Ctrl Pts',(-39.6944643395886,-20.48000002,-131.308059656117));
#138771=CARTESIAN_POINT('Ctrl Pts',(-39.6545649019171,-20.48000002,-131.161159371035));
#138772=CARTESIAN_POINT('Ctrl Pts',(-39.6215434069806,-20.48000002,-131.013525238712));
#138773=CARTESIAN_POINT('Ctrl Pts',(-39.5522800663325,-20.48000002,-130.703859270587));
#138774=CARTESIAN_POINT('Ctrl Pts',(-39.5121705688285,-20.48000002,-130.389227115401));
#138775=CARTESIAN_POINT('Ctrl Pts',(-39.5023709529557,-20.48000002,-130.069431842175));
#138776=CARTESIAN_POINT('Ctrl Pts',(-39.5007919718943,-20.48000002,-130.017904242881));
#138777=CARTESIAN_POINT('Ctrl Pts',(-39.5,-20.48000002,-129.96624258113));
#138778=CARTESIAN_POINT('Ctrl Pts',(-39.5,-20.48000002,-129.914446011788));
#138779=CARTESIAN_POINT('',(-58.4402350532158,-20.48000002,-171.237717270032));
#138780=CARTESIAN_POINT('Ctrl Pts',(-58.4402350532158,-20.48000002,-171.237717270032));
#138781=CARTESIAN_POINT('Ctrl Pts',(-52.3041884424236,-20.48000002,-158.172646387016));
#138782=CARTESIAN_POINT('Ctrl Pts',(-46.1592765266851,-20.48000002,-145.111728668187));
#138783=CARTESIAN_POINT('Ctrl Pts',(-39.9829309662066,-20.48000002,-132.065646534579));
#138784=CARTESIAN_POINT('',(-58.5817791104913,-20.48000002,-171.871644662643));
#138785=CARTESIAN_POINT('Origin',(-56.4084014798071,-20.48000002,-172.018072886377));
#138786=CARTESIAN_POINT('',(-58.5817791104913,-20.48000002,-171.871644662643));
#138787=CARTESIAN_POINT('Origin',(0.,-12.9675000200281,-60.64995));
#138788=CARTESIAN_POINT('',(-39.5365899453791,-19.9017174926824,-99.7816873656535));
#138789=CARTESIAN_POINT('',(-39.4710976496823,-14.3145440753906,-101.167027481326));
#138790=CARTESIAN_POINT('Ctrl Pts',(-39.5365899624517,-19.9017174575869,
-99.7816873060563));
#138791=CARTESIAN_POINT('Ctrl Pts',(-39.5191359427996,-18.9900458934628,
-100.156305085366));
#138792=CARTESIAN_POINT('Ctrl Pts',(-39.5043113435924,-18.0551324974974,
-100.470115458113));
#138793=CARTESIAN_POINT('Ctrl Pts',(-39.4820945526735,-16.1678764290028,
-100.937768877564));
#138794=CARTESIAN_POINT('Ctrl Pts',(-39.474721832796,-15.2403172398251,
-101.091495325969));
#138795=CARTESIAN_POINT('Ctrl Pts',(-39.4710976496822,-14.3145440753934,
-101.167027481325));
#138796=CARTESIAN_POINT('Ctrl Pts',(-57.8770125754992,-19.9259080025173,
-60.8508735991007));
#138797=CARTESIAN_POINT('Ctrl Pts',(-51.7792721519529,-19.9203329617956,
-73.8354504791465));
#138798=CARTESIAN_POINT('Ctrl Pts',(-45.6728806072717,-19.9133770457548,
-86.8158923265289));
#138799=CARTESIAN_POINT('Ctrl Pts',(-39.5365899624517,-19.9017174575869,
-99.7816873060563));
#138800=CARTESIAN_POINT('Ctrl Pts',(-39.4710976496822,-14.3145440753934,
-101.167027481325));
#138801=CARTESIAN_POINT('Ctrl Pts',(-45.7410317152176,-14.3169685900793,
-87.7287563851229));
#138802=CARTESIAN_POINT('Ctrl Pts',(-52.0097486856907,-14.3183690440453,
-74.2898953083048));
#138803=CARTESIAN_POINT('Ctrl Pts',(-58.2781275348581,-14.3194901627709,
-60.8508735991007));
#138804=CARTESIAN_POINT('Ctrl Pts',(-58.3718694303385,-14.3184313509278,
-60.42825533736));
#138805=CARTESIAN_POINT('Ctrl Pts',(-58.383173457336,-13.83000002,-60.42825533736));
#138806=CARTESIAN_POINT('Ctrl Pts',(-58.871735578318,-13.83000002,-60.42825533736));
#138807=CARTESIAN_POINT('Ctrl Pts',(-58.3718694303297,-14.3184313513064,
-60.574130507918));
#138808=CARTESIAN_POINT('Ctrl Pts',(-58.3831734460811,-13.83000002,-60.57578605024));
#138809=CARTESIAN_POINT('Ctrl Pts',(-58.871735561804,-13.83000002,-60.6470682084222));
#138810=CARTESIAN_POINT('Ctrl Pts',(-58.3404329537672,-14.3187847426543,
-60.7173302229433));
#138811=CARTESIAN_POINT('Ctrl Pts',(-58.3509717578384,-13.8300000200006,
-60.7206801175402));
#138812=CARTESIAN_POINT('Ctrl Pts',(-58.8245931841484,-13.83000002,-60.8618675123431));
#138813=CARTESIAN_POINT('Ctrl Pts',(-58.2781275348581,-14.3194901627709,
-60.8508735991007));
#138814=CARTESIAN_POINT('Ctrl Pts',(-58.2874540965012,-13.83000002,-60.8552238163692));
#138815=CARTESIAN_POINT('Ctrl Pts',(-58.7311595360587,-13.83000002,-61.0621827299711));
#138816=CARTESIAN_POINT('',(-58.7311595360587,-13.83000002,-61.0621827299711));
#138817=CARTESIAN_POINT('Origin',(-58.7311595360587,-14.33000002,-61.0621827299711));
#138818=CARTESIAN_POINT('Origin',(-56.6451562406488,-13.83000002,-60.2668362080947));
#138819=CARTESIAN_POINT('Origin',(83.2809572255632,-13.8300000199999,-55.24995));
#138820=CARTESIAN_POINT('',(-59.5,-13.83000002,-57.9104088126279));
#138821=CARTESIAN_POINT('Ctrl Pts',(-59.5,-13.83000002,-57.9104088126279));
#138822=CARTESIAN_POINT('Ctrl Pts',(-59.5,-13.83000002,-57.7635265772534));
#138823=CARTESIAN_POINT('Ctrl Pts',(-59.4872752713112,-13.8300000201995,
-57.6187932998334));
#138824=CARTESIAN_POINT('Ctrl Pts',(-59.4620787130117,-13.8300000189704,
-57.4761129700909));
#138825=CARTESIAN_POINT('Ctrl Pts',(-59.4509269987809,-13.8300000184264,
-57.4129642557014));
#138826=CARTESIAN_POINT('Ctrl Pts',(-59.437331564423,-13.8300000175808,
-57.3502178600945));
#138827=CARTESIAN_POINT('Ctrl Pts',(-59.4213112185568,-13.8300000163283,
-57.287866292));
#138828=CARTESIAN_POINT('Ctrl Pts',(-59.3984317821363,-13.8300000145396,
-57.198818979923));
#138829=CARTESIAN_POINT('Ctrl Pts',(-59.370414675224,-13.8300000118888,
-57.1106006512125));
#138830=CARTESIAN_POINT('Ctrl Pts',(-59.3376309673359,-13.8300000085315,
-57.0241300655718));
#138831=CARTESIAN_POINT('Ctrl Pts',(-59.3184526052596,-13.8300000065676,
-56.9735450552971));
#138832=CARTESIAN_POINT('Ctrl Pts',(-59.2977312649336,-13.8300000075911,
-56.9238144825175));
#138833=CARTESIAN_POINT('Ctrl Pts',(-59.2754924251822,-13.8300000109221,
-56.8749259088891));
#138834=CARTESIAN_POINT('Ctrl Pts',(-59.2665370422079,-13.8300000122635,
-56.8552389151069));
#138835=CARTESIAN_POINT('Ctrl Pts',(-59.2573350139603,-13.8300000139055,
-56.8356886347887));
#138836=CARTESIAN_POINT('Ctrl Pts',(-59.2478858052507,-13.8300000154741,
-56.8162751713274));
#138837=CARTESIAN_POINT('Ctrl Pts',(-59.2292919233252,-13.8300000185606,
-56.778073914645));
#138838=CARTESIAN_POINT('Ctrl Pts',(-59.209718687562,-13.8300000193634,
-56.7403307398674));
#138839=CARTESIAN_POINT('Ctrl Pts',(-59.1892544368187,-13.8300000195901,
-56.7032294252422));
#138840=CARTESIAN_POINT('Ctrl Pts',(-59.1734934512784,-13.8300000197646,
-56.6746550449402));
#138841=CARTESIAN_POINT('Ctrl Pts',(-59.1571354382929,-13.8300000198488,
-56.6463349492494));
#138842=CARTESIAN_POINT('Ctrl Pts',(-59.140235511425,-13.8300000188361,
-56.6183428976771));
#138843=CARTESIAN_POINT('Ctrl Pts',(-59.0995076542868,-13.8300000163955,
-56.55088365443));
#138844=CARTESIAN_POINT('Ctrl Pts',(-59.0552769615241,-13.8300000132201,
-56.484916810245));
#138845=CARTESIAN_POINT('Ctrl Pts',(-59.0079404245038,-13.8300000140848,
-56.4210933496162));
#138846=CARTESIAN_POINT('Ctrl Pts',(-58.9649853093651,-13.8300000148695,
-56.3631773238055));
#138847=CARTESIAN_POINT('Ctrl Pts',(-58.9194738360321,-13.8300000183267,
-56.3070268147763));
#138848=CARTESIAN_POINT('Ctrl Pts',(-58.871735578318,-13.8300000195957,
-56.2531111209796));
#138849=CARTESIAN_POINT('',(-59.5,-13.83000002,-174.751208632418));
#138850=CARTESIAN_POINT('',(-59.5,-13.83000002,-57.9132014677655));
#138851=CARTESIAN_POINT('',(-58.9842656455866,-13.8300000191192,-176.271971760299));
#138852=CARTESIAN_POINT('Ctrl Pts',(-58.9842656455851,-13.8300000182384,
-176.271971760298));
#138853=CARTESIAN_POINT('Ctrl Pts',(-59.0284765648189,-13.8300000166394,
-176.214285352614));
#138854=CARTESIAN_POINT('Ctrl Pts',(-59.0700022374986,-13.8300000137057,
-176.154919321393));
#138855=CARTESIAN_POINT('Ctrl Pts',(-59.1087690495582,-13.8300000102313,
-176.094105263608));
#138856=CARTESIAN_POINT('Ctrl Pts',(-59.1458171677555,-13.830000006911,
-176.035987345698));
#138857=CARTESIAN_POINT('Ctrl Pts',(-59.1803457899704,-13.8300000031738,
-175.976545944297));
#138858=CARTESIAN_POINT('Ctrl Pts',(-59.2122555343191,-13.8300000007997,
-175.915955958697));
#138859=CARTESIAN_POINT('Ctrl Pts',(-59.2455714173138,-13.829999998321,
-175.852696007478));
#138860=CARTESIAN_POINT('Ctrl Pts',(-59.2762989800145,-13.8299999975166,
-175.787603392926));
#138861=CARTESIAN_POINT('Ctrl Pts',(-59.3042804787194,-13.8299999996639,
-175.721026919923));
#138862=CARTESIAN_POINT('Ctrl Pts',(-59.3272704921692,-13.8300000014281,
-175.666326704401));
#138863=CARTESIAN_POINT('Ctrl Pts',(-59.3484061154264,-13.8300000052622,
-175.610623961591));
#138864=CARTESIAN_POINT('Ctrl Pts',(-59.3675737697888,-13.8300000097259,
-175.554108016098));
#138865=CARTESIAN_POINT('Ctrl Pts',(-59.3904098382371,-13.830000015044,
-175.486775729355));
#138866=CARTESIAN_POINT('Ctrl Pts',(-59.4103356014117,-13.830000017107,
-175.418690311177));
#138867=CARTESIAN_POINT('Ctrl Pts',(-59.4272061992403,-13.8300000182966,
-175.350275598526));
#138868=CARTESIAN_POINT('Ctrl Pts',(-59.4492409439888,-13.8300000198503,
-175.260918911488));
#138869=CARTESIAN_POINT('Ctrl Pts',(-59.4663032629515,-13.8300000198819,
-175.170862100583));
#138870=CARTESIAN_POINT('Ctrl Pts',(-59.4783606526566,-13.8300000199558,
-175.079983307974));
#138871=CARTESIAN_POINT('Ctrl Pts',(-59.4903258960551,-13.8300000200293,
-174.989799039245));
#138872=CARTESIAN_POINT('Ctrl Pts',(-59.4973624498085,-13.83000002,-174.898805302285));
#138873=CARTESIAN_POINT('Ctrl Pts',(-59.4993876311078,-13.83000002,-174.80687604146));
#138874=CARTESIAN_POINT('Ctrl Pts',(-59.4997955668077,-13.83000002,-174.78835857472));
#138875=CARTESIAN_POINT('Ctrl Pts',(-59.5,-13.83000002,-174.769803126626));
#138876=CARTESIAN_POINT('Ctrl Pts',(-59.5,-13.83000002,-174.751208632418));
#138877=CARTESIAN_POINT('',(-58.9842656455947,-13.83000002,-171.871644662643));
#138878=CARTESIAN_POINT('',(-58.9842656455947,-13.83000002,-176.75597498356));
#138879=CARTESIAN_POINT('',(-58.8436897472855,-13.83000002,-171.237717270032));
#138880=CARTESIAN_POINT('Origin',(-56.7574781748151,-13.83000002,-172.032172120179));
#138881=CARTESIAN_POINT('',(-39.923987884714,-13.83000002,-130.68030635931));
#138882=CARTESIAN_POINT('Ctrl Pts',(-39.923987884714,-13.83000002,-130.68030635931));
#138883=CARTESIAN_POINT('Ctrl Pts',(-46.2315241188232,-13.83000002,-144.198991310165));
#138884=CARTESIAN_POINT('Ctrl Pts',(-52.5377799111353,-13.83000002,-157.718273616974));
#138885=CARTESIAN_POINT('Ctrl Pts',(-58.8436897472855,-13.83000002,-171.237717270032));
#138886=CARTESIAN_POINT('',(-39.5,-13.83000002,-128.768820397718));
#138887=CARTESIAN_POINT('Origin',(-46.1927888980657,-13.83000002,-128.28832565251));
#138888=CARTESIAN_POINT('',(-39.5,-13.83000002,-103.289822573788));
#138889=CARTESIAN_POINT('',(-39.5,-13.83000002,-55.24995));
#138890=CARTESIAN_POINT('',(-39.923987884714,-13.83000002,-101.378336612196));
#138891=CARTESIAN_POINT('Origin',(-46.1924380476731,-13.83000002,-103.773062785017));
#138892=CARTESIAN_POINT('Ctrl Pts',(-58.7311595360587,-13.83000002,-61.0621827299711));
#138893=CARTESIAN_POINT('Ctrl Pts',(-52.4627544636864,-13.83000002,-74.5012048985427));
#138894=CARTESIAN_POINT('Ctrl Pts',(-46.194004389791,-13.83000002,-87.9400661652057));
#138895=CARTESIAN_POINT('Ctrl Pts',(-39.923987884714,-13.83000002,-101.378336612196));
#138896=CARTESIAN_POINT('Ctrl Pts',(-59.5,-13.83000002,-57.9104088126279));
#138897=CARTESIAN_POINT('Ctrl Pts',(-60.,-13.83000002,-57.9104088126279));
#138898=CARTESIAN_POINT('Ctrl Pts',(-60.,-13.33000002,-57.9104088126279));
#138899=CARTESIAN_POINT('Ctrl Pts',(-59.4999999942362,-13.83000002,-57.6984561889535));
#138900=CARTESIAN_POINT('Ctrl Pts',(-59.9998595361682,-13.830000019997,
-57.6561017631169));
#138901=CARTESIAN_POINT('Ctrl Pts',(-60.,-13.3301404965737,-57.6560661294349));
#138902=CARTESIAN_POINT('Ctrl Pts',(-59.4734676164696,-13.83000002,-57.4909684574329));
#138903=CARTESIAN_POINT('Ctrl Pts',(-59.9678925924923,-13.8300000200007,
-57.4071493963694));
#138904=CARTESIAN_POINT('Ctrl Pts',(-59.9681611381428,-13.3302771999651,
-57.4070813040103));
#138905=CARTESIAN_POINT('Ctrl Pts',(-59.3690374493417,-13.83000002,-57.084794303535));
#138906=CARTESIAN_POINT('Ctrl Pts',(-59.8423361500656,-13.8300000199993,
-56.9198740502323));
#138907=CARTESIAN_POINT('Ctrl Pts',(-59.8428449408308,-13.3305433698035,
-56.9196731955795));
#138908=CARTESIAN_POINT('Ctrl Pts',(-59.2901412046916,-13.83000002,-56.8862343787282));
#138909=CARTESIAN_POINT('Ctrl Pts',(-59.7475635896442,-13.8300000199991,
-56.6816942845782));
#138910=CARTESIAN_POINT('Ctrl Pts',(-59.7481694456677,-13.3306727288355,
-56.6814017112205));
#138911=CARTESIAN_POINT('Ctrl Pts',(-59.0883322092721,-13.83000002,-56.5202440244056));
#138912=CARTESIAN_POINT('Ctrl Pts',(-59.5052494150047,-13.8300000200009,
-56.2427365274425));
#138913=CARTESIAN_POINT('Ctrl Pts',(-59.5059986510887,-13.3309100420639,
-56.2422140639419));
#138914=CARTESIAN_POINT('Ctrl Pts',(-58.9625961123716,-13.83000002,-56.3476402489859));
#138915=CARTESIAN_POINT('Ctrl Pts',(-59.3543264440767,-13.8300000199994,
-56.0357389914811));
#138916=CARTESIAN_POINT('Ctrl Pts',(-59.3551153361278,-13.3310213578394,
-56.0350898960933));
#138917=CARTESIAN_POINT('Ctrl Pts',(-58.6747340315543,-13.83000002,-56.0424403288692));
#138918=CARTESIAN_POINT('Ctrl Pts',(-59.0088785326184,-13.8300000200005,
-55.6697700183809));
#138919=CARTESIAN_POINT('Ctrl Pts',(-59.0096808365833,-13.3312174510841,
-55.6688506341933));
#138920=CARTESIAN_POINT('Ctrl Pts',(-58.5134387215907,-13.83000002,-55.9093078011895));
#138921=CARTESIAN_POINT('Ctrl Pts',(-58.8153502371001,-13.8300000200007,
-55.510138275251));
#138922=CARTESIAN_POINT('Ctrl Pts',(-58.8161264695431,-13.3313025928017,
-55.509091871258));
#138923=CARTESIAN_POINT('Ctrl Pts',(-58.3343300343787,-13.83000002,-55.796263236946));
#138924=CARTESIAN_POINT('Ctrl Pts',(-58.6004643384094,-13.83000002,-55.3745979500414));
#138925=CARTESIAN_POINT('Ctrl Pts',(-58.6011960412544,-13.3313747072047,
-55.3734386342923));
#138926=CARTESIAN_POINT('',(-60.,-13.33000002,-57.9104088126279));
#138927=CARTESIAN_POINT('Ctrl Pts',(-58.616886279706,-13.331369406142,-55.3834096347511));
#138928=CARTESIAN_POINT('Ctrl Pts',(-58.8255570887224,-13.3312984580582,
-55.5168999903146));
#138929=CARTESIAN_POINT('Ctrl Pts',(-59.0138940511391,-13.3312150861459,
-55.6733176015169));
#138930=CARTESIAN_POINT('Ctrl Pts',(-59.3551153360854,-13.3310213846274,
-56.0350898961282));
#138931=CARTESIAN_POINT('Ctrl Pts',(-59.5059986510485,-13.3309100688549,
-56.2422140639699));
#138932=CARTESIAN_POINT('Ctrl Pts',(-59.7481694456352,-13.3306727556329,
-56.6814017112362));
#138933=CARTESIAN_POINT('Ctrl Pts',(-59.8428449408035,-13.3305433966043,
-56.9196731955903));
#138934=CARTESIAN_POINT('Ctrl Pts',(-59.9681611381284,-13.3302772267731,
-57.4070813040139));
#138935=CARTESIAN_POINT('Ctrl Pts',(-59.9999999999925,-13.3301405233853,
-57.6560661294368));
#138936=CARTESIAN_POINT('Ctrl Pts',(-60.,-13.33000002,-57.9104088126279));
#138937=CARTESIAN_POINT('Origin',(-59.5,-13.33000002,-57.9104088126279));
#138938=CARTESIAN_POINT('Ctrl Pts',(-58.6015900410175,-13.341475878746,
-55.3737206461527));
#138939=CARTESIAN_POINT('Ctrl Pts',(-59.9999999999999,-13.3385258667613,
-56.2566220904403));
#138940=CARTESIAN_POINT('Ctrl Pts',(-60.,-13.3330000856764,-57.9104187956072));
#138941=CARTESIAN_POINT('Ctrl Pts',(-58.60257249872,-13.168900596776,-55.3737643179337));
#138942=CARTESIAN_POINT('Ctrl Pts',(-59.9999999999979,-13.1673253991122,
-56.2568074836807));
#138943=CARTESIAN_POINT('Ctrl Pts',(-60.,-13.1643269532066,-57.9098552131434));
#138944=CARTESIAN_POINT('Ctrl Pts',(-58.6028748593257,-12.996307708263,
-55.373777702491));
#138945=CARTESIAN_POINT('Ctrl Pts',(-60.0000000000015,-12.9960742306928,
-56.2568641234304));
#138946=CARTESIAN_POINT('Ctrl Pts',(-60.,-12.9956563413871,-57.9096813403539));
#138947=CARTESIAN_POINT('Ctrl Pts',(-58.6024972248876,-12.82373973381,-55.3737609414448));
#138948=CARTESIAN_POINT('Ctrl Pts',(-60.,-12.8248749582876,-56.2567930570856));
#138949=CARTESIAN_POINT('Ctrl Pts',(-60.,-12.827000187199,-57.9098981644024));
#138950=CARTESIAN_POINT('',(-60.,-12.83000002,-57.909894348981));
#138951=CARTESIAN_POINT('Ctrl Pts',(-60.,-12.83000002,-57.909894348981));
#138952=CARTESIAN_POINT('Ctrl Pts',(-59.9999999999994,-12.8299467047078,
-57.6556666887755));
#138953=CARTESIAN_POINT('Ctrl Pts',(-59.9681892936708,-12.8298948271699,
-57.4067922228919));
#138954=CARTESIAN_POINT('Ctrl Pts',(-59.8429857054854,-12.8297938186589,
-56.9195951650652));
#138955=CARTESIAN_POINT('Ctrl Pts',(-59.7483921213374,-12.8297447259539,
-56.6814121423212));
#138956=CARTESIAN_POINT('Ctrl Pts',(-59.5064293021062,-12.8296546610246,
-56.2423688578594));
#138957=CARTESIAN_POINT('Ctrl Pts',(-59.355679816355,-12.829612413403,-56.035304631569));
#138958=CARTESIAN_POINT('Ctrl Pts',(-59.0146398555283,-12.8295388666295,
-55.6734793535298));
#138959=CARTESIAN_POINT('Ctrl Pts',(-58.8263448628416,-12.8295072025013,
-55.5169944929564));
#138960=CARTESIAN_POINT('Ctrl Pts',(-58.6177174583935,-12.8294802501407,
-55.3834349955049));
#138961=CARTESIAN_POINT('Origin',(-60.,-12.9674754043409,-167.271246742335));
#138962=CARTESIAN_POINT('Ctrl Pts',(-60.,-12.83000002,-57.909894348981));
#138963=CARTESIAN_POINT('Ctrl Pts',(-60.,-12.33000002,-57.909894348981));
#138964=CARTESIAN_POINT('Ctrl Pts',(-59.5,-12.33000002,-57.909894348981));
#138965=CARTESIAN_POINT('Ctrl Pts',(-60.,-12.8299467103192,-57.6556666887753));
#138966=CARTESIAN_POINT('Ctrl Pts',(-59.9999466862306,-12.33000002,-57.6556802065741));
#138967=CARTESIAN_POINT('Ctrl Pts',(-59.4999999942389,-12.33000002,-57.6980379098391));
#138968=CARTESIAN_POINT('Ctrl Pts',(-59.9681892936719,-12.8298948327809,
-57.4067922228916));
#138969=CARTESIAN_POINT('Ctrl Pts',(-59.9680873501793,-12.33000002,-57.4068180594886));
#138970=CARTESIAN_POINT('Ctrl Pts',(-59.4734910794084,-12.33000002,-57.4906424667705));
#138971=CARTESIAN_POINT('Ctrl Pts',(-59.8429857054876,-12.8297938242694,
-56.9195951650643));
#138972=CARTESIAN_POINT('Ctrl Pts',(-59.8427924853442,-12.33000002,-56.9196714028451));
#138973=CARTESIAN_POINT('Ctrl Pts',(-59.3691547532245,-12.33000002,-57.0846448139696));
#138974=CARTESIAN_POINT('Ctrl Pts',(-59.74839212134,-12.8297447315641,-56.6814121423199));
#138975=CARTESIAN_POINT('Ctrl Pts',(-59.748161991806,-12.3300000200005,
-56.6815232165248));
#138976=CARTESIAN_POINT('Ctrl Pts',(-59.290326767749,-12.33000002,-56.8861589103251));
#138977=CARTESIAN_POINT('Ctrl Pts',(-59.5064293021094,-12.8296546666343,
-56.2423688578572));
#138978=CARTESIAN_POINT('Ctrl Pts',(-59.5061445952809,-12.3300000199994,
-56.2425672751971));
#138979=CARTESIAN_POINT('Ctrl Pts',(-59.0886910851255,-12.33000002,-56.5202894131685));
#138980=CARTESIAN_POINT('Ctrl Pts',(-59.3556798163584,-12.8296124190124,
-56.0353046315662));
#138981=CARTESIAN_POINT('Ctrl Pts',(-59.3553799746847,-12.3300000199993,
-56.035551183714));
#138982=CARTESIAN_POINT('Ctrl Pts',(-58.9630665125599,-12.33000002,-56.3477358485963));
#138983=CARTESIAN_POINT('Ctrl Pts',(-59.0105155640199,-12.8295379828168,
-55.6691036993668));
#138984=CARTESIAN_POINT('Ctrl Pts',(-59.010210485167,-12.3300000200007,
-55.6694530297022));
#138985=CARTESIAN_POINT('Ctrl Pts',(-58.6754296377554,-12.33000002,-56.0425683262376));
#138986=CARTESIAN_POINT('Ctrl Pts',(-58.8171130576816,-12.8295056604635,
-55.509345500426));
#138987=CARTESIAN_POINT('Ctrl Pts',(-58.8168178148591,-12.3300000200035,
-55.5097431582292));
#138988=CARTESIAN_POINT('Ctrl Pts',(-58.5142608782156,-12.33000002,-55.909436466106));
#138989=CARTESIAN_POINT('Ctrl Pts',(-58.6023581204233,-12.8294782784431,
-55.3736658212353));
#138990=CARTESIAN_POINT('Ctrl Pts',(-58.6020797386365,-12.33000002,-55.3741064461589));
#138991=CARTESIAN_POINT('Ctrl Pts',(-58.3352984336861,-12.33000002,-55.7963700340195));
#138992=CARTESIAN_POINT('',(-59.5,-12.33000002,-57.909894348981));
#138993=CARTESIAN_POINT('Ctrl Pts',(-58.8765127194368,-12.330000020523,
-56.2580153373943));
#138994=CARTESIAN_POINT('Ctrl Pts',(-58.9314422323999,-12.3300000222489,
-56.3204146345372));
#138995=CARTESIAN_POINT('Ctrl Pts',(-58.9833702988531,-12.3300000263278,
-56.3857545682232));
#138996=CARTESIAN_POINT('Ctrl Pts',(-59.03181875348,-12.3300000260899,-56.4533283814535));
#138997=CARTESIAN_POINT('Ctrl Pts',(-59.0712668703441,-12.3300000258961,
-56.5083489120731));
#138998=CARTESIAN_POINT('Ctrl Pts',(-59.1084086074742,-12.3300000229817,
-56.5648494607718));
#138999=CARTESIAN_POINT('Ctrl Pts',(-59.1430095719442,-12.3300000210667,
-56.6224388634737));
#139000=CARTESIAN_POINT('Ctrl Pts',(-59.159023041084,-12.3300000201805,
-56.6490914766905));
#139001=CARTESIAN_POINT('Ctrl Pts',(-59.1745444070377,-12.3300000202428,
-56.6760375771056));
#139002=CARTESIAN_POINT('Ctrl Pts',(-59.1895265613474,-12.3300000204054,
-56.7032144429067));
#139003=CARTESIAN_POINT('Ctrl Pts',(-59.2106099692481,-12.3300000206343,
-56.7414586723615));
#139004=CARTESIAN_POINT('Ctrl Pts',(-59.2307479204425,-12.3300000215029,
-56.7803865151708));
#139005=CARTESIAN_POINT('Ctrl Pts',(-59.2498439227782,-12.3300000247794,
-56.8197986433709));
#139006=CARTESIAN_POINT('Ctrl Pts',(-59.2732105276413,-12.3300000287887,
-56.868024843299));
#139007=CARTESIAN_POINT('Ctrl Pts',(-59.2950576358119,-12.3300000325183,
-56.9170923843778));
#139008=CARTESIAN_POINT('Ctrl Pts',(-59.3153788043346,-12.330000032611,
-56.9670066834514));
#139009=CARTESIAN_POINT('Ctrl Pts',(-59.3234660778806,-12.3300000326479,
-56.9868712197854));
#139010=CARTESIAN_POINT('Ctrl Pts',(-59.3313111418656,-12.3300000321978,
-57.0068701006058));
#139011=CARTESIAN_POINT('Ctrl Pts',(-59.3389114029545,-12.3300000313575,
-57.0270043936979));
#139012=CARTESIAN_POINT('Ctrl Pts',(-59.3711805702217,-12.3300000277898,
-57.1124905189758));
#139013=CARTESIAN_POINT('Ctrl Pts',(-59.398787967634,-12.3300000251841,
-57.1996595335916));
#139014=CARTESIAN_POINT('Ctrl Pts',(-59.4213798740153,-12.3300000234584,
-57.2876290029532));
#139015=CARTESIAN_POINT('Ctrl Pts',(-59.4552355589985,-12.3300000208724,
-57.4194579240094));
#139016=CARTESIAN_POINT('Ctrl Pts',(-59.4782525129323,-12.3300000202447,
-57.5530362590468));
#139017=CARTESIAN_POINT('Ctrl Pts',(-59.4902475546029,-12.3300000200727,
-57.6884558476609));
#139018=CARTESIAN_POINT('Ctrl Pts',(-59.4967374324384,-12.3300000199797,
-57.7617241705875));
#139019=CARTESIAN_POINT('Ctrl Pts',(-59.5,-12.33000002,-57.8355316833216));
#139020=CARTESIAN_POINT('Ctrl Pts',(-59.5,-12.33000002,-57.909894348981));
#139021=CARTESIAN_POINT('Origin',(-59.5,-12.83000002,-57.909894348981));
#139022=CARTESIAN_POINT('Ctrl Pts',(-58.2828791719688,-11.838774304476,
-60.8508735991007));
#139023=CARTESIAN_POINT('Ctrl Pts',(-58.2906927660831,-12.33000002,-60.8545178210735));
#139024=CARTESIAN_POINT('Ctrl Pts',(-58.7359481105893,-12.33000002,-61.0621827299711));
#139025=CARTESIAN_POINT('Ctrl Pts',(-58.3445491382077,-11.8393573204241,
-60.7186709323925));
#139026=CARTESIAN_POINT('Ctrl Pts',(-58.3533698277338,-12.3300000200013,
-60.7214865958624));
#139027=CARTESIAN_POINT('Ctrl Pts',(-58.8284361535292,-12.33000002,-60.863878626764));
#139028=CARTESIAN_POINT('Ctrl Pts',(-58.3766060098775,-11.8396582665817,
-60.575610749785));
#139029=CARTESIAN_POINT('Ctrl Pts',(-58.3860794582448,-12.330000020003,
-60.5770127531963));
#139030=CARTESIAN_POINT('Ctrl Pts',(-58.8765127155019,-12.33000002,-60.64928853347));
#139031=CARTESIAN_POINT('Ctrl Pts',(-58.376606009879,-11.839658266657,-60.42825533736));
#139032=CARTESIAN_POINT('Ctrl Pts',(-58.3860794606436,-12.33000002,-60.42825533736));
#139033=CARTESIAN_POINT('Ctrl Pts',(-58.8765127194474,-12.33000002,-60.42825533736));
#139034=CARTESIAN_POINT('',(-58.7359481105893,-12.33000002,-61.0621827299711));
#139035=CARTESIAN_POINT('Origin',(-58.7359481105893,-11.83000002,-61.0621827299711));
#139036=CARTESIAN_POINT('Origin',(-56.649087690066,-12.33000002,-60.2675479548571));
#139037=CARTESIAN_POINT('Origin',(83.2809572255632,-12.3300000199999,-55.24995));
#139038=CARTESIAN_POINT('',(-39.9232693735648,-12.33000002,-101.394976652855));
#139039=CARTESIAN_POINT('Ctrl Pts',(-39.9232693735648,-12.33000002,-101.394976652855));
#139040=CARTESIAN_POINT('Ctrl Pts',(-46.1948314689912,-12.33000002,-87.9510241496856));
#139041=CARTESIAN_POINT('Ctrl Pts',(-52.4655100689676,-12.33000002,-74.5066595330064));
#139042=CARTESIAN_POINT('Ctrl Pts',(-58.7359481105893,-12.33000002,-61.0621827299711));
#139043=CARTESIAN_POINT('',(-39.5,-12.33000002,-103.303524786513));
#139044=CARTESIAN_POINT('Origin',(-46.1908778693233,-12.33000002,-103.784865184756));
#139045=CARTESIAN_POINT('',(-39.5,-12.33000002,-128.755118184993));
#139046=CARTESIAN_POINT('',(-39.5,-12.33000002,-55.24995));
#139047=CARTESIAN_POINT('',(-39.9232693735648,-12.33000002,-130.663666318651));
#139048=CARTESIAN_POINT('Origin',(-46.1904260133999,-12.33000002,-128.271059668218));
#139049=CARTESIAN_POINT('',(-58.8484691650909,-12.33000002,-171.237717270032));
#139050=CARTESIAN_POINT('Ctrl Pts',(-58.8484691650909,-12.33000002,-171.237717270032));
#139051=CARTESIAN_POINT('Ctrl Pts',(-52.5405278046811,-12.33000002,-157.712819732223));
#139052=CARTESIAN_POINT('Ctrl Pts',(-46.2323452217992,-12.33000002,-144.188034690057));
#139053=CARTESIAN_POINT('Ctrl Pts',(-39.9232693735648,-12.33000002,-130.663666318651));
#139054=CARTESIAN_POINT('',(-58.9890336736409,-12.33000002,-171.871644662643));
#139055=CARTESIAN_POINT('Origin',(-56.7618024059963,-12.33000002,-172.033247591146));
#139056=CARTESIAN_POINT('',(-58.9890336736409,-12.3300000204739,-176.26629097911));
#139057=CARTESIAN_POINT('',(-58.9890336736409,-12.33000002,-171.871644662643));
#139058=CARTESIAN_POINT('',(-59.5,-12.33000002,-174.751778045594));
#139059=CARTESIAN_POINT('Ctrl Pts',(-59.5,-12.33000002,-174.751778045594));
#139060=CARTESIAN_POINT('Ctrl Pts',(-59.5,-12.33000002,-174.844927230273));
#139061=CARTESIAN_POINT('Ctrl Pts',(-59.4948737621761,-12.3300000199839,
-174.937101433735));
#139062=CARTESIAN_POINT('Ctrl Pts',(-59.4847164002782,-12.3300000200162,
-175.028427073489));
#139063=CARTESIAN_POINT('Ctrl Pts',(-59.474481566957,-12.3300000200487,
-175.120449264903));
#139064=CARTESIAN_POINT('Ctrl Pts',(-59.4591385334095,-12.3300000199961,
-175.211609900805));
#139065=CARTESIAN_POINT('Ctrl Pts',(-59.4387322722171,-12.3300000210573,
-175.302031274496));
#139066=CARTESIAN_POINT('Ctrl Pts',(-59.4350695133288,-12.3300000212478,
-175.318261179968));
#139067=CARTESIAN_POINT('Ctrl Pts',(-59.4312434964565,-12.3300000214808,
-175.334467250166));
#139068=CARTESIAN_POINT('Ctrl Pts',(-59.4272543062711,-12.330000021774,
-175.350650168439));
#139069=CARTESIAN_POINT('Ctrl Pts',(-59.4106840236565,-12.3300000229918,
-175.417870711165));
#139070=CARTESIAN_POINT('Ctrl Pts',(-59.3911649601375,-12.3300000250948,
-175.484771053152));
#139071=CARTESIAN_POINT('Ctrl Pts',(-59.3688362082559,-12.3300000304207,
-175.550947464116));
#139072=CARTESIAN_POINT('Ctrl Pts',(-59.3452983767326,-12.330000036035,
-175.620707261724));
#139073=CARTESIAN_POINT('Ctrl Pts',(-59.318757276387,-12.3300000404266,
-175.689252183756));
#139074=CARTESIAN_POINT('Ctrl Pts',(-59.2894219594715,-12.3300000414655,
-175.756217087946));
#139075=CARTESIAN_POINT('Ctrl Pts',(-59.265578831198,-12.3300000423099,
-175.810644752902));
#139076=CARTESIAN_POINT('Ctrl Pts',(-59.2398885853161,-12.3300000411891,
-175.864029149378));
#139077=CARTESIAN_POINT('Ctrl Pts',(-59.2124386122788,-12.330000039031,
-175.916169632722));
#139078=CARTESIAN_POINT('Ctrl Pts',(-59.1785809256147,-12.3300000363691,
-175.980481395257));
#139079=CARTESIAN_POINT('Ctrl Pts',(-59.1417731864694,-12.3300000322739,
-176.043500821863));
#139080=CARTESIAN_POINT('Ctrl Pts',(-59.1021371288072,-12.3300000288604,
-176.105011973128));
#139081=CARTESIAN_POINT('Ctrl Pts',(-59.0666804433847,-12.3300000258069,
-176.16003716153));
#139082=CARTESIAN_POINT('Ctrl Pts',(-59.0289595515132,-12.3300000233307,
-176.21385559589));
#139083=CARTESIAN_POINT('Ctrl Pts',(-58.9890336736408,-12.3300000218957,
-176.26629097911));
#139084=CARTESIAN_POINT('',(-59.5,-12.33000002,-174.749818876635));
#139085=CARTESIAN_POINT('Origin',(0.,-12.9675000200281,-60.64995));
#139086=CARTESIAN_POINT('',(-39.4702993039609,-11.842906113671,-101.183667521985));
#139087=CARTESIAN_POINT('',(-39.532390596215,-6.25584930029837,-99.8717339663452));
#139088=CARTESIAN_POINT('Ctrl Pts',(-39.4702993039609,-11.842906113671,
-101.183667521985));
#139089=CARTESIAN_POINT('Ctrl Pts',(-39.4717448060415,-11.4004606629204,
-101.15354495628));
#139090=CARTESIAN_POINT('Ctrl Pts',(-39.4740433475117,-10.9574131907765,
-101.105623514581));
#139091=CARTESIAN_POINT('Ctrl Pts',(-39.4806656803776,-10.023475093596,
-100.967196709792));
#139092=CARTESIAN_POINT('Ctrl Pts',(-39.4851934915317,-9.53196093055967,
-100.872391456905));
#139093=CARTESIAN_POINT('Ctrl Pts',(-39.5012939059505,-8.09530479773136,
-100.533838938409));
#139094=CARTESIAN_POINT('Ctrl Pts',(-39.5154754399064,-7.1657280964986,
-100.234102969279));
#139095=CARTESIAN_POINT('Ctrl Pts',(-39.532390596256,-6.25584930059377,
-99.8717339663646));
#139096=CARTESIAN_POINT('Ctrl Pts',(-58.2828791719688,-11.838774304476,
-60.8508735991007));
#139097=CARTESIAN_POINT('Ctrl Pts',(-52.0124594137882,-11.8397106642502,
-74.2953500811619));
#139098=CARTESIAN_POINT('Ctrl Pts',(-45.741803891981,-11.8408803347909,
-87.7397145657271));
#139099=CARTESIAN_POINT('Ctrl Pts',(-39.4702993039609,-11.842906113671,
-101.183667521985));
#139100=CARTESIAN_POINT('Ctrl Pts',(-39.532390596256,-6.25584930059377,
-99.8717339663646));
#139101=CARTESIAN_POINT('Ctrl Pts',(-45.6775416784359,-6.24451367567336,
-86.8752616232929));
#139102=CARTESIAN_POINT('Ctrl Pts',(-51.7945419641194,-6.23776491028108,
-73.8650082774501));
#139103=CARTESIAN_POINT('Ctrl Pts',(-57.9034184448965,-6.23235646472971,
-60.8508735991007));
#139104=CARTESIAN_POINT('Ctrl Pts',(-57.9983536018174,-6.23763109620483,
-60.42825533736));
#139105=CARTESIAN_POINT('Ctrl Pts',(-57.9336485918015,-5.68000002,-60.4282553373601));
#139106=CARTESIAN_POINT('Ctrl Pts',(-58.4950211556756,-5.68000001999999,
-60.42825533736));
#139107=CARTESIAN_POINT('Ctrl Pts',(-57.9983536015968,-6.23763109430342,
-60.5741740417057));
#139108=CARTESIAN_POINT('Ctrl Pts',(-57.9336485820782,-5.68000001999705,
-60.5646181976572));
#139109=CARTESIAN_POINT('Ctrl Pts',(-58.4950211389271,-5.68000001999999,
-60.6471359124214));
#139110=CARTESIAN_POINT('Ctrl Pts',(-57.9664686566087,-6.23586779901857,
-60.7174374956191));
#139111=CARTESIAN_POINT('Ctrl Pts',(-57.9064697980399,-5.68000002000461,
-60.6982006050192));
#139112=CARTESIAN_POINT('Ctrl Pts',(-58.4475018470026,-5.68000001999999,
-60.8620252214211));
#139113=CARTESIAN_POINT('Ctrl Pts',(-57.9034184448965,-6.23235646472971,
-60.8508735991007));
#139114=CARTESIAN_POINT('Ctrl Pts',(-57.8507724536939,-5.68000001999999,
-60.826158857425));
#139115=CARTESIAN_POINT('Ctrl Pts',(-58.3535376001277,-5.68000001999999,
-61.0621827299711));
#139116=CARTESIAN_POINT('',(-58.3535376001277,-5.68000001999999,-61.0621827299711));
#139117=CARTESIAN_POINT('Origin',(-58.3535376001277,-6.18000001999999,-61.0621827299711));
#139118=CARTESIAN_POINT('Origin',(-56.3184043809282,-5.68000001999999,-60.2809146158445));
#139119=CARTESIAN_POINT('Origin',(83.2809572255632,-5.68000001999993,-55.24995));
#139120=CARTESIAN_POINT('',(-59.5,-5.68000001999999,-58.1246434856214));
#139121=CARTESIAN_POINT('Ctrl Pts',(-59.5,-5.68000001999999,-58.1246434856214));
#139122=CARTESIAN_POINT('Ctrl Pts',(-59.5,-5.68000001999999,-58.0267693974302));
#139123=CARTESIAN_POINT('Ctrl Pts',(-59.4943836373774,-5.68000001999999,
-57.9298568609375));
#139124=CARTESIAN_POINT('Ctrl Pts',(-59.4831953566826,-5.68000001999999,
-57.8338865707097));
#139125=CARTESIAN_POINT('Ctrl Pts',(-59.4720070759879,-5.68000001999999,
-57.7379162804819));
#139126=CARTESIAN_POINT('Ctrl Pts',(-59.455245939737,-5.68000002032169,
-57.6428888905768));
#139127=CARTESIAN_POINT('Ctrl Pts',(-59.4329732446822,-5.68000001967878,
-57.548806713199));
#139128=CARTESIAN_POINT('Ctrl Pts',(-59.4211509304573,-5.68000001933753,
-57.4988680299284));
#139129=CARTESIAN_POINT('Ctrl Pts',(-59.4077647649328,-5.68000001901105,
-57.4491949286452));
#139130=CARTESIAN_POINT('Ctrl Pts',(-59.392823215944,-5.68000001896984,
-57.3997884127162));
#139131=CARTESIAN_POINT('Ctrl Pts',(-59.3572029910943,-5.68000001887159,
-57.2820046937892));
#139132=CARTESIAN_POINT('Ctrl Pts',(-59.3124912608683,-5.68000001980192,
-57.1660436798562));
#139133=CARTESIAN_POINT('Ctrl Pts',(-59.2602343180242,-5.68000001992935,
-57.0554150259142));
#139134=CARTESIAN_POINT('Ctrl Pts',(-59.2518183841936,-5.68000001994988,
-57.0375983803036));
#139135=CARTESIAN_POINT('Ctrl Pts',(-59.2431998624486,-5.68000001996158,
-57.0198940947568));
#139136=CARTESIAN_POINT('Ctrl Pts',(-59.2343787360437,-5.68000001996808,
-57.002302188435));
#139137=CARTESIAN_POINT('Ctrl Pts',(-59.1884199680699,-5.68000002000192,
-56.9106469616823));
#139138=CARTESIAN_POINT('Ctrl Pts',(-59.136987353068,-5.68000001969244,
-56.8220653476532));
#139139=CARTESIAN_POINT('Ctrl Pts',(-59.0800102832677,-5.68000001903091,
-56.7365294000527));
#139140=CARTESIAN_POINT('Ctrl Pts',(-59.0296633903434,-5.68000001844636,
-56.6609469032671));
#139141=CARTESIAN_POINT('Ctrl Pts',(-58.974589118716,-5.68000001849974,
-56.587361786818));
#139142=CARTESIAN_POINT('Ctrl Pts',(-58.9158341632416,-5.68000001947823,
-56.5172160817437));
#139143=CARTESIAN_POINT('Ctrl Pts',(-58.8953629897436,-5.68000001981915,
-56.4927761874893));
#139144=CARTESIAN_POINT('Ctrl Pts',(-58.8744667885101,-5.68000001977524,
-56.468763578303));
#139145=CARTESIAN_POINT('Ctrl Pts',(-58.8531845723455,-5.68000001964656,
-56.4452355795564));
#139146=CARTESIAN_POINT('Ctrl Pts',(-58.8093620434502,-5.68000001938158,
-56.396788726233));
#139147=CARTESIAN_POINT('Ctrl Pts',(-58.7638692855098,-5.6800000177515,
-56.3502656276834));
#139148=CARTESIAN_POINT('Ctrl Pts',(-58.7166522079594,-5.68000001767937,
-56.3056325667689));
#139149=CARTESIAN_POINT('Ctrl Pts',(-58.6815782873768,-5.68000001762579,
-56.2724781125951));
#139150=CARTESIAN_POINT('Ctrl Pts',(-58.6455688559318,-5.680000018255,-56.2403749966795));
#139151=CARTESIAN_POINT('Ctrl Pts',(-58.6086287388195,-5.68000001901365,
-56.2093177964104));
#139152=CARTESIAN_POINT('Ctrl Pts',(-58.6017994579946,-5.68000001915391,
-56.203576116122));
#139153=CARTESIAN_POINT('Ctrl Pts',(-58.5949404401232,-5.68000001924633,
-56.1978709269311));
#139154=CARTESIAN_POINT('Ctrl Pts',(-58.5880516973688,-5.68000001929971,
-56.1922018795935));
#139155=CARTESIAN_POINT('Ctrl Pts',(-58.5576786887571,-5.68000001953509,
-56.1672066040054));
#139156=CARTESIAN_POINT('Ctrl Pts',(-58.5266453103076,-5.68000002035884,
-56.1428933547174));
#139157=CARTESIAN_POINT('Ctrl Pts',(-58.4950211556753,-5.68000001545765,
-56.119278519931));
#139158=CARTESIAN_POINT('',(-59.5,-5.68000001999999,-174.511260182693));
#139159=CARTESIAN_POINT('',(-59.5,-5.68000001999999,-58.1042606444049));
#139160=CARTESIAN_POINT('',(-58.6082745331212,-5.68000001999999,-176.427328712824));
#139161=CARTESIAN_POINT('Ctrl Pts',(-58.6082745331212,-5.6800000199515,
-176.427328712824));
#139162=CARTESIAN_POINT('Ctrl Pts',(-58.6185667882716,-5.68000001995871,
-176.418676244678));
#139163=CARTESIAN_POINT('Ctrl Pts',(-58.628783204882,-5.68000001996413,
-176.409943629197));
#139164=CARTESIAN_POINT('Ctrl Pts',(-58.6389210444463,-5.68000001996836,
-176.401132572172));
#139165=CARTESIAN_POINT('Ctrl Pts',(-58.7108573560278,-5.68000001999836,
-176.338610874187));
#139166=CARTESIAN_POINT('Ctrl Pts',(-58.7792948136848,-5.68000001999946,
-176.271947442152));
#139167=CARTESIAN_POINT('Ctrl Pts',(-58.8440583693357,-5.68000001994282,
-176.201117847417));
#139168=CARTESIAN_POINT('Ctrl Pts',(-58.8596678064677,-5.68000001992916,
-176.184046361841));
#139169=CARTESIAN_POINT('Ctrl Pts',(-58.875063977428,-5.6800000199106,-176.166733035301));
#139170=CARTESIAN_POINT('Ctrl Pts',(-58.8902447330317,-5.68000001988414,
-176.149177868712));
#139171=CARTESIAN_POINT('Ctrl Pts',(-58.9227212058659,-5.68000001982754,
-176.111621774291));
#139172=CARTESIAN_POINT('Ctrl Pts',(-58.9541409398416,-5.68000001973543,
-176.072997877296));
#139173=CARTESIAN_POINT('Ctrl Pts',(-58.984359985497,-5.68000001956971,
-176.033520885199));
#139174=CARTESIAN_POINT('Ctrl Pts',(-59.0268866354123,-5.6800000193365,
-175.977965715067));
#139175=CARTESIAN_POINT('Ctrl Pts',(-59.0670052242284,-5.68000001940972,
-175.920749643185));
#139176=CARTESIAN_POINT('Ctrl Pts',(-59.1043833915299,-5.68000001957814,
-175.862401050087));
#139177=CARTESIAN_POINT('Ctrl Pts',(-59.1540049590066,-5.68000001980172,
-175.784940092029));
#139178=CARTESIAN_POINT('Ctrl Pts',(-59.199181192514,-5.68000001997512,
-175.70506448782));
#139179=CARTESIAN_POINT('Ctrl Pts',(-59.239965893642,-5.68000001998963,
-175.622670099363));
#139180=CARTESIAN_POINT('Ctrl Pts',(-59.2487993257315,-5.68000001999278,
-175.604824553978));
#139181=CARTESIAN_POINT('Ctrl Pts',(-59.2574265918444,-5.6800000199934,
-175.586860742585));
#139182=CARTESIAN_POINT('Ctrl Pts',(-59.2658479718429,-5.68000001999155,
-175.568777423473));
#139183=CARTESIAN_POINT('Ctrl Pts',(-59.2686911708562,-5.68000001999092,
-175.5626721919));
#139184=CARTESIAN_POINT('Ctrl Pts',(-59.2715106588893,-5.68000001999007,
-175.556553812533));
#139185=CARTESIAN_POINT('Ctrl Pts',(-59.2743064287832,-5.68000001998893,
-175.550422281673));
#139186=CARTESIAN_POINT('Ctrl Pts',(-59.3235845105522,-5.68000001996885,
-175.44234826609));
#139187=CARTESIAN_POINT('Ctrl Pts',(-59.3657187337311,-5.68000001965404,
-175.32923562655));
#139188=CARTESIAN_POINT('Ctrl Pts',(-59.3992004790972,-5.68000001961977,
-175.214817860028));
#139189=CARTESIAN_POINT('Ctrl Pts',(-59.4149912346775,-5.68000001960361,
-175.160855828914));
#139190=CARTESIAN_POINT('Ctrl Pts',(-59.4289384514506,-5.68000001972945,
-175.106577823109));
#139191=CARTESIAN_POINT('Ctrl Pts',(-59.441030144846,-5.68000001987896,
-175.051984501471));
#139192=CARTESIAN_POINT('Ctrl Pts',(-59.4606225263251,-5.68000002012122,
-174.963525991253));
#139193=CARTESIAN_POINT('Ctrl Pts',(-59.4753677357896,-5.68000001999999,
-174.874236789973));
#139194=CARTESIAN_POINT('Ctrl Pts',(-59.485211909548,-5.68000001999999,
-174.784118621956));
#139195=CARTESIAN_POINT('Ctrl Pts',(-59.4950560833064,-5.68000001999999,
-174.694000453939));
#139196=CARTESIAN_POINT('Ctrl Pts',(-59.5,-5.68000001999999,-174.603053692373));
#139197=CARTESIAN_POINT('Ctrl Pts',(-59.5,-5.68000001999999,-174.511260182694));
#139198=CARTESIAN_POINT('',(-58.6082745331205,-5.68000001999999,-171.871644662643));
#139199=CARTESIAN_POINT('',(-58.6082745331205,-5.68000001999999,-176.785131631246));
#139200=CARTESIAN_POINT('',(-58.4667946194619,-5.68000001999999,-171.237717270032));
#139201=CARTESIAN_POINT('Origin',(-56.431269633621,-5.68000001999999,-172.018134872838));
#139202=CARTESIAN_POINT('',(-39.9791515366304,-5.68000001999998,-131.975599874271));
#139203=CARTESIAN_POINT('Ctrl Pts',(-39.9791515366304,-5.68000001999998,
-131.975599874271));
#139204=CARTESIAN_POINT('Ctrl Pts',(-46.164205183661,-5.68000001999998,
-145.052367414711));
#139205=CARTESIAN_POINT('Ctrl Pts',(-52.3196619691199,-5.68000001999999,
-158.143093167052));
#139206=CARTESIAN_POINT('Ctrl Pts',(-58.4667946194619,-5.68000001999999,
-171.237717270032));
#139207=CARTESIAN_POINT('',(-39.5,-5.68000001999998,-129.839692850412));
#139208=CARTESIAN_POINT('Ctrl Pts',(-39.5,-5.68000001999998,-129.839692850412));
#139209=CARTESIAN_POINT('Ctrl Pts',(-39.5,-5.68000001999998,-130.0740119535));
#139210=CARTESIAN_POINT('Ctrl Pts',(-39.516697911888,-5.68000001999998,
-130.308218863705));
#139211=CARTESIAN_POINT('Ctrl Pts',(-39.5492808611242,-5.68000001999998,
-130.539004174614));
#139212=CARTESIAN_POINT('Ctrl Pts',(-39.568225357989,-5.68000001999998,
-130.673188209559));
#139213=CARTESIAN_POINT('Ctrl Pts',(-39.5925388156195,-5.68000001999998,
-130.806215404499));
#139214=CARTESIAN_POINT('Ctrl Pts',(-39.6220534778078,-5.68000001999998,
-130.937436349817));
#139215=CARTESIAN_POINT('Ctrl Pts',(-39.6907803864263,-5.68000001999998,
-131.242993291658));
#139216=CARTESIAN_POINT('Ctrl Pts',(-39.7874256609414,-5.68000001999998,
-131.540730203477));
#139217=CARTESIAN_POINT('Ctrl Pts',(-39.913239336921,-5.68000001999998,
-131.830296953197));
#139218=CARTESIAN_POINT('Ctrl Pts',(-39.9343840562227,-5.68000001999998,
-131.878962629596));
#139219=CARTESIAN_POINT('Ctrl Pts',(-39.9563527642831,-5.68000001999998,
-131.927397503975));
#139220=CARTESIAN_POINT('Ctrl Pts',(-39.9791515366304,-5.68000001999998,
-131.975599874271));
#139221=CARTESIAN_POINT('',(-39.5,-5.68000001999998,-102.218950121094));
#139222=CARTESIAN_POINT('',(-39.5,-5.68000001999998,-55.24995));
#139223=CARTESIAN_POINT('',(-39.9791515366304,-5.68000001999998,-100.083043097235));
#139224=CARTESIAN_POINT('Ctrl Pts',(-39.9791515366304,-5.68000001999998,
-100.083043097235));
#139225=CARTESIAN_POINT('Ctrl Pts',(-39.88674512358,-5.68000001999998,-100.278413622971));
#139226=CARTESIAN_POINT('Ctrl Pts',(-39.8073027352616,-5.68000001999998,
-100.479790373907));
#139227=CARTESIAN_POINT('Ctrl Pts',(-39.7413121766313,-5.68000001999998,
-100.684533556796));
#139228=CARTESIAN_POINT('Ctrl Pts',(-39.694147898587,-5.68000001999998,
-100.830866071718));
#139229=CARTESIAN_POINT('Ctrl Pts',(-39.6538540641004,-5.68000001999998,
-100.978917355179));
#139230=CARTESIAN_POINT('Ctrl Pts',(-39.620593360194,-5.68000001999998,
-101.127718496005));
#139231=CARTESIAN_POINT('Ctrl Pts',(-39.5515828956696,-5.68000001999998,
-101.436456274949));
#139232=CARTESIAN_POINT('Ctrl Pts',(-39.5117440272004,-5.68000001999998,
-101.750163184452));
#139233=CARTESIAN_POINT('Ctrl Pts',(-39.502232472568,-5.68000001999998,
-102.069036097455));
#139234=CARTESIAN_POINT('Ctrl Pts',(-39.5007456673965,-5.68000001999998,
-102.118880935069));
#139235=CARTESIAN_POINT('Ctrl Pts',(-39.5,-5.68000001999998,-102.16885201916));
#139236=CARTESIAN_POINT('Ctrl Pts',(-39.5,-5.68000001999998,-102.218950121094));
#139237=CARTESIAN_POINT('Ctrl Pts',(-58.3535376001277,-5.68000001999999,
-61.0621827299711));
#139238=CARTESIAN_POINT('Ctrl Pts',(-52.2440275184664,-5.68000001999999,
-74.0763270103718));
#139239=CARTESIAN_POINT('Ctrl Pts',(-46.1262203434603,-5.68000001999998,
-87.0865851147193));
#139240=CARTESIAN_POINT('Ctrl Pts',(-39.9791515366304,-5.68000001999998,
-100.083043097235));
#139241=CARTESIAN_POINT('Ctrl Pts',(-59.5,-5.68000001999999,-58.1246434856214));
#139242=CARTESIAN_POINT('Ctrl Pts',(-60.,-5.68000001999998,-58.1246434856214));
#139243=CARTESIAN_POINT('Ctrl Pts',(-60.,-5.18000001999999,-58.1246434856214));
#139244=CARTESIAN_POINT('Ctrl Pts',(-59.4999999932887,-5.68000001999999,
-57.8769929082306));
#139245=CARTESIAN_POINT('Ctrl Pts',(-60.0020017947382,-5.68000001999912,
-57.8269512006129));
#139246=CARTESIAN_POINT('Ctrl Pts',(-60.,-5.17800220042073,-57.8275435066813));
#139247=CARTESIAN_POINT('Ctrl Pts',(-59.4640366407682,-5.68000001999999,
-57.6353667913546));
#139248=CARTESIAN_POINT('Ctrl Pts',(-59.9606548869199,-5.68000002000021,
-57.5365322236183));
#139249=CARTESIAN_POINT('Ctrl Pts',(-59.9568439660775,-5.17605025203681,
-57.5376710843709));
#139250=CARTESIAN_POINT('Ctrl Pts',(-59.3571704209101,-5.68000001999999,
-57.2820131603569));
#139251=CARTESIAN_POINT('Ctrl Pts',(-59.8350835786331,-5.68000001999988,
-57.1113495469635));
#139252=CARTESIAN_POINT('Ctrl Pts',(-59.8286045065143,-5.17319230589712,
-57.1137623423983));
#139253=CARTESIAN_POINT('Ctrl Pts',(-59.3124762512969,-5.68000001999999,
-57.1660493315578));
#139254=CARTESIAN_POINT('Ctrl Pts',(-59.7822107642191,-5.68000001999999,
-56.971551755675));
#139255=CARTESIAN_POINT('Ctrl Pts',(-59.7749715022372,-5.17225378701852,
-56.9746437275083));
#139256=CARTESIAN_POINT('Ctrl Pts',(-59.2079771855437,-5.68000001999999,
-56.9447878986704));
#139257=CARTESIAN_POINT('Ctrl Pts',(-59.6581215271118,-5.68000001999999,
-56.7045411154571));
#139258=CARTESIAN_POINT('Ctrl Pts',(-59.6495726219715,-5.17046209438582,
-56.7092025345767));
#139259=CARTESIAN_POINT('Ctrl Pts',(-59.1479068869942,-5.68000001999999,
-56.8384914380986));
#139260=CARTESIAN_POINT('Ctrl Pts',(-59.5865663613646,-5.68000001999988,
-56.5761588403972));
#139261=CARTESIAN_POINT('Ctrl Pts',(-59.5774882635866,-5.16960084340769,
-56.5816816551612));
#139262=CARTESIAN_POINT('Ctrl Pts',(-59.0120618664304,-5.68000001999999,
-56.6346018834074));
#139263=CARTESIAN_POINT('Ctrl Pts',(-59.4243672282747,-5.6800000200001,
-56.3296643856923));
#139264=CARTESIAN_POINT('Ctrl Pts',(-59.4144742405229,-5.16794806289525,
-56.3370811282929));
#139265=CARTESIAN_POINT('Ctrl Pts',(-58.9355640571429,-5.68000001999999,
-56.5363163451986));
#139266=CARTESIAN_POINT('Ctrl Pts',(-59.332837232209,-5.68000002000004,
-56.210751177698));
#139267=CARTESIAN_POINT('Ctrl Pts',(-59.3226768695123,-5.16715091135939,
-56.219170776799));
#139268=CARTESIAN_POINT('Ctrl Pts',(-58.770777205737,-5.68000001999999,
-56.3541800398345));
#139269=CARTESIAN_POINT('Ctrl Pts',(-59.1353297626326,-5.68000001999993,
-55.9901841613723));
#139270=CARTESIAN_POINT('Ctrl Pts',(-59.1249326459437,-5.16567306852165,
-56.0006670964121));
#139271=CARTESIAN_POINT('Ctrl Pts',(-58.6823687426766,-5.68000001999999,
-56.2698716578318));
#139272=CARTESIAN_POINT('Ctrl Pts',(-59.0292080232237,-5.68000001999941,
-55.8880220414999));
#139273=CARTESIAN_POINT('Ctrl Pts',(-59.0188424909195,-5.16498867365063,
-55.8995247770565));
#139274=CARTESIAN_POINT('Ctrl Pts',(-58.3993671534221,-5.68000001999999,
-56.0369236173554));
#139275=CARTESIAN_POINT('Ctrl Pts',(-58.6888368836822,-5.68000002000116,
-55.6053191370779));
#139276=CARTESIAN_POINT('Ctrl Pts',(-58.6792405846915,-5.16309702763064,
-55.6200638122352));
#139277=CARTESIAN_POINT('Ctrl Pts',(-58.1837972805939,-5.68000001999999,
-55.907468794294));
#139278=CARTESIAN_POINT('Ctrl Pts',(-58.42924178916,-5.68000002000209,-55.448215858158));
#139279=CARTESIAN_POINT('Ctrl Pts',(-58.4205568275121,-5.16204487752377,
-55.4647607356853));
#139280=CARTESIAN_POINT('Ctrl Pts',(-57.9591100572707,-5.68000001999999,
-55.8140496618682));
#139281=CARTESIAN_POINT('Ctrl Pts',(-58.1583910096328,-5.68000001999999,
-55.3347486595489));
#139282=CARTESIAN_POINT('Ctrl Pts',(-58.1509320687249,-5.16128538415681,
-55.3526885469843));
#139283=CARTESIAN_POINT('',(-60.,-5.18000001999999,-58.1246434856214));
#139284=CARTESIAN_POINT('Ctrl Pts',(-58.1702690071152,-5.16134039100008,
-55.3608055405081));
#139285=CARTESIAN_POINT('Ctrl Pts',(-58.4329181295403,-5.16209542477378,
-55.4722107983731));
#139286=CARTESIAN_POINT('Ctrl Pts',(-58.6846580097054,-5.16312727866648,
-55.6245218487779));
#139287=CARTESIAN_POINT('Ctrl Pts',(-59.018842492426,-5.16498874849922,
-55.8995247753848));
#139288=CARTESIAN_POINT('Ctrl Pts',(-59.1249326474558,-5.1656731433235,
-56.0006670948875));
#139289=CARTESIAN_POINT('Ctrl Pts',(-59.3226768709922,-5.16715098605971,
-56.2191707755726));
#139290=CARTESIAN_POINT('Ctrl Pts',(-59.414474241965,-5.16794813754046,
-56.3370811272117));
#139291=CARTESIAN_POINT('Ctrl Pts',(-59.5774882649122,-5.16960091793786,
-56.5816816543548));
#139292=CARTESIAN_POINT('Ctrl Pts',(-59.6495726232209,-5.17046216885565,
-56.7092025338954));
#139293=CARTESIAN_POINT('Ctrl Pts',(-59.7749715032972,-5.17225386136191,
-56.9746437270556));
#139294=CARTESIAN_POINT('Ctrl Pts',(-59.8286045074639,-5.1731923801738,
-57.1137623420447));
#139295=CARTESIAN_POINT('Ctrl Pts',(-59.9568439666376,-5.17605032610843,
-57.5376710842035));
#139296=CARTESIAN_POINT('Ctrl Pts',(-60.0000000002948,-5.17800227435048,
-57.8275435065941));
#139297=CARTESIAN_POINT('Ctrl Pts',(-60.,-5.18000001999999,-58.1246434856214));
#139298=CARTESIAN_POINT('Origin',(-59.5,-5.18000001999999,-58.1246434856214));
#139299=CARTESIAN_POINT('Ctrl Pts',(-58.1516269266116,-5.16456703757977,
-55.3528444275805));
#139300=CARTESIAN_POINT('Ctrl Pts',(-60.,-5.19571559048276,-56.1206307397359));
#139301=CARTESIAN_POINT('Ctrl Pts',(-60.,-5.2768578914742,-58.1207219873789));
#139302=CARTESIAN_POINT('Ctrl Pts',(-58.1275061007746,-4.96483231244508,
-55.3509116092303));
#139303=CARTESIAN_POINT('Ctrl Pts',(-60.0000000000005,-4.99483472640263,
-56.1098379052425));
#139304=CARTESIAN_POINT('Ctrl Pts',(-60.,-5.07672217607537,-58.12884135333));
#139305=CARTESIAN_POINT('Ctrl Pts',(-58.1024667524284,-4.76557632116298,
-55.3488500157616));
#139306=CARTESIAN_POINT('Ctrl Pts',(-60.0000000000001,-4.79479350163006,
-56.0981738677439));
#139307=CARTESIAN_POINT('Ctrl Pts',(-60.,-4.87658373874773,-58.1368637570314));
#139308=CARTESIAN_POINT('Ctrl Pts',(-58.0765164643631,-4.56684999234778,
-55.3466493905885));
#139309=CARTESIAN_POINT('Ctrl Pts',(-60.,-4.59579029342123,-56.0855524411383));
#139310=CARTESIAN_POINT('Ctrl Pts',(-60.,-4.67644015442612,-58.1447026957153));
#139311=CARTESIAN_POINT('',(-60.,-4.68000002001403,-58.1445632485962));
#139312=CARTESIAN_POINT('Ctrl Pts',(-60.,-4.68000002001403,-58.1445632485962));
#139313=CARTESIAN_POINT('Ctrl Pts',(-60.,-4.67801447919764,-57.8400901274889));
#139314=CARTESIAN_POINT('Ctrl Pts',(-59.9547202743521,-4.67607375656258,
-57.5431941162335));
#139315=CARTESIAN_POINT('Ctrl Pts',(-59.819980312157,-4.67323178879642,
-57.1093239470213));
#139316=CARTESIAN_POINT('Ctrl Pts',(-59.7637842928231,-4.67230172637259,
-56.9674919122442));
#139317=CARTESIAN_POINT('Ctrl Pts',(-59.6323866477998,-4.67052667748359,
-56.6970587190125));
#139318=CARTESIAN_POINT('Ctrl Pts',(-59.5568525046157,-4.66967405412828,
-56.567291481448));
#139319=CARTESIAN_POINT('Ctrl Pts',(-59.385918342594,-4.66803974391678,
-56.318763868979));
#139320=CARTESIAN_POINT('Ctrl Pts',(-59.289776717509,-4.6672543224009,-56.1994379500303));
#139321=CARTESIAN_POINT('Ctrl Pts',(-59.0834337883813,-4.66580663221926,
-55.9796562580523));
#139322=CARTESIAN_POINT('Ctrl Pts',(-58.9727240508436,-4.66513801841297,
-55.8782346380825));
#139323=CARTESIAN_POINT('Ctrl Pts',(-58.6298042492702,-4.66335817424259,
-55.6084094028642));
#139324=CARTESIAN_POINT('Ctrl Pts',(-58.3750448694008,-4.66239047068315,
-55.4619202173471));
#139325=CARTESIAN_POINT('Ctrl Pts',(-58.1110275345658,-4.6616933513699,
-55.3564444847807));
#139326=CARTESIAN_POINT('Ctrl Pts',(-60.,-4.68000002001403,-58.1445632485962));
#139327=CARTESIAN_POINT('Ctrl Pts',(-60.,-4.84666977904325,-58.1380335512985));
#139328=CARTESIAN_POINT('Ctrl Pts',(-60.,-5.01333597711292,-58.1313769278999));
#139329=CARTESIAN_POINT('Ctrl Pts',(-60.,-5.18000001999999,-58.1246434856214));
#139330=CARTESIAN_POINT('Ctrl Pts',(-60.,-4.68000001999999,-58.1445632485961));
#139331=CARTESIAN_POINT('Ctrl Pts',(-59.9999999999999,-4.18000001999999,
-58.144563248596));
#139332=CARTESIAN_POINT('Ctrl Pts',(-59.5,-4.18000001999999,-58.1445632485962));
#139333=CARTESIAN_POINT('Ctrl Pts',(-60.,-4.67801447919764,-57.8400901274889));
#139334=CARTESIAN_POINT('Ctrl Pts',(-59.9980183704624,-4.18000001999736,
-57.8406912127677));
#139335=CARTESIAN_POINT('Ctrl Pts',(-59.4999999931196,-4.18000001999999,
-57.8907708245007));
#139336=CARTESIAN_POINT('Ctrl Pts',(-59.9547202743521,-4.67607375656258,
-57.5431941162335));
#139337=CARTESIAN_POINT('Ctrl Pts',(-59.9509926566885,-4.18000002000109,
-57.5443378186833));
#139338=CARTESIAN_POINT('Ctrl Pts',(-59.4622668978632,-4.18000001999999,
-57.6432940448109));
#139339=CARTESIAN_POINT('Ctrl Pts',(-59.819980312157,-4.67323178879642,
-57.1093239470213));
#139340=CARTESIAN_POINT('Ctrl Pts',(-59.8137304682065,-4.18000001999945,
-57.1117161950833));
#139341=CARTESIAN_POINT('Ctrl Pts',(-59.3499835921793,-4.18000001999999,
-57.2816425794726));
#139342=CARTESIAN_POINT('Ctrl Pts',(-59.7637842928231,-4.67230172637259,
-56.9674919122442));
#139343=CARTESIAN_POINT('Ctrl Pts',(-59.756837410337,-4.18000002,-56.9705421764153));
#139344=CARTESIAN_POINT('Ctrl Pts',(-59.3031535768727,-4.18000001999999,
-57.163418767372));
#139345=CARTESIAN_POINT('Ctrl Pts',(-59.6323866477998,-4.67052667748359,
-56.6970587190125));
#139346=CARTESIAN_POINT('Ctrl Pts',(-59.6242664035215,-4.18000001999999,
-56.7016181941089));
#139347=CARTESIAN_POINT('Ctrl Pts',(-59.1936555403131,-4.18000001999999,
-56.9379996304409));
#139348=CARTESIAN_POINT('Ctrl Pts',(-59.5568525046157,-4.66967405412828,
-56.567291481448));
#139349=CARTESIAN_POINT('Ctrl Pts',(-59.5482752170826,-4.18000001999972,
-56.5726707527956));
#139350=CARTESIAN_POINT('Ctrl Pts',(-59.130710421318,-4.18000001999999,
-56.8298323231333));
#139351=CARTESIAN_POINT('Ctrl Pts',(-59.385918342594,-4.66803974391678,
-56.318763868979));
#139352=CARTESIAN_POINT('Ctrl Pts',(-59.3766737402574,-4.18000002000027,
-56.3259306460082));
#139353=CARTESIAN_POINT('Ctrl Pts',(-58.9882652846901,-4.18000001999999,
-56.622672397275));
#139354=CARTESIAN_POINT('Ctrl Pts',(-59.289776717509,-4.6672543224009,-56.1994379500303));
#139355=CARTESIAN_POINT('Ctrl Pts',(-59.280338735327,-4.18000002000033,
-56.2075385111788));
#139356=CARTESIAN_POINT('Ctrl Pts',(-58.9081472639374,-4.18000001999999,
-56.5232083679403));
#139357=CARTESIAN_POINT('Ctrl Pts',(-59.0834337883813,-4.66580663221926,
-55.9796562580523));
#139358=CARTESIAN_POINT('Ctrl Pts',(-59.0738973083079,-4.18000001999967,
-55.9896554831564));
#139359=CARTESIAN_POINT('Ctrl Pts',(-58.7361948243045,-4.18000001999999,
-56.3400094513659));
#139360=CARTESIAN_POINT('Ctrl Pts',(-58.9727240508436,-4.66513801841297,
-55.8782346380825));
#139361=CARTESIAN_POINT('Ctrl Pts',(-58.9632803249174,-4.18000001999956,
-55.889161374227));
#139362=CARTESIAN_POINT('Ctrl Pts',(-58.6439367094154,-4.18000001999999,
-56.2554694851693));
#139363=CARTESIAN_POINT('Ctrl Pts',(-58.6181223301711,-4.66329754200289,
-55.5992175260631));
#139364=CARTESIAN_POINT('Ctrl Pts',(-58.6095926714098,-4.18000002000086,
-55.6130627249839));
#139365=CARTESIAN_POINT('Ctrl Pts',(-58.3484352743845,-4.18000001999999,
-56.0228947878735));
#139366=CARTESIAN_POINT('Ctrl Pts',(-58.3484766058291,-4.66229039631671,
-55.4467718445047));
#139367=CARTESIAN_POINT('Ctrl Pts',(-58.3409094947055,-4.18000001999966,
-55.4621795466313));
#139368=CARTESIAN_POINT('Ctrl Pts',(-58.1237304207495,-4.18000001999999,
-55.8958235878219));
#139369=CARTESIAN_POINT('Ctrl Pts',(-58.0697760887706,-4.66158691772347,
-55.3403413730918));
#139370=CARTESIAN_POINT('Ctrl Pts',(-58.0634433345606,-4.18000001999999,
-55.3569201007255));
#139371=CARTESIAN_POINT('Ctrl Pts',(-57.8914800739755,-4.18000001999999,
-55.8071084335971));
#139372=CARTESIAN_POINT('',(-59.5,-4.18000001999999,-58.1445632485962));
#139373=CARTESIAN_POINT('Ctrl Pts',(-58.1504944089168,-4.18000007585629,
-55.9233081330324));
#139374=CARTESIAN_POINT('Ctrl Pts',(-58.2011234110634,-4.1800000934009,
-55.9495719668715));
#139375=CARTESIAN_POINT('Ctrl Pts',(-58.2508802238442,-4.18000007907268,
-55.9776159745792));
#139376=CARTESIAN_POINT('Ctrl Pts',(-58.2996228616342,-4.18000005788132,
-56.007327702339));
#139377=CARTESIAN_POINT('Ctrl Pts',(-58.3611066386641,-4.18000003115063,
-56.0448059621867));
#139378=CARTESIAN_POINT('Ctrl Pts',(-58.4211714230485,-4.18000002563093,
-56.0849815311993));
#139379=CARTESIAN_POINT('Ctrl Pts',(-58.4791990630186,-4.18000002261545,
-56.1275622952346));
#139380=CARTESIAN_POINT('Ctrl Pts',(-58.5015978396008,-4.18000002145147,
-56.1439985490753));
#139381=CARTESIAN_POINT('Ctrl Pts',(-58.5236932870565,-4.18000002089499,
-56.1607926562338));
#139382=CARTESIAN_POINT('Ctrl Pts',(-58.5454508633043,-4.18000002055973,
-56.1779259948581));
#139383=CARTESIAN_POINT('Ctrl Pts',(-58.601384203271,-4.18000001969785,
-56.2219715651515));
#139384=CARTESIAN_POINT('Ctrl Pts',(-58.6553029072665,-4.18000001999999,
-56.2682684120419));
#139385=CARTESIAN_POINT('Ctrl Pts',(-58.7070968429494,-4.18000001999999,
-56.3167184080419));
#139386=CARTESIAN_POINT('Ctrl Pts',(-58.7466278917693,-4.18000001999999,
-56.3536972383227));
#139387=CARTESIAN_POINT('Ctrl Pts',(-58.7849870908598,-4.18000001999997,
-56.3919927767765));
#139388=CARTESIAN_POINT('Ctrl Pts',(-58.8221712586797,-4.18000002000008,
-56.4316087082659));
#139389=CARTESIAN_POINT('Ctrl Pts',(-58.9081478861484,-4.18000002000031,
-56.5232080201017));
#139390=CARTESIAN_POINT('Ctrl Pts',(-58.9882663096845,-4.18000002000183,
-56.6226714971191));
#139391=CARTESIAN_POINT('Ctrl Pts',(-59.059488987448,-4.18000002000189,
-56.7262515801497));
#139392=CARTESIAN_POINT('Ctrl Pts',(-59.0864350865984,-4.18000002000191,
-56.7654396488238));
#139393=CARTESIAN_POINT('Ctrl Pts',(-59.1121963184049,-4.18000002000164,
-56.8052844356691));
#139394=CARTESIAN_POINT('Ctrl Pts',(-59.1367770480425,-4.18000002000115,
-56.845783548759));
#139395=CARTESIAN_POINT('Ctrl Pts',(-59.1771662439534,-4.18000002000036,
-56.9123286284587));
#139396=CARTESIAN_POINT('Ctrl Pts',(-59.2143783070055,-4.1800000199807,
-56.9806361125577));
#139397=CARTESIAN_POINT('Ctrl Pts',(-59.2484246951019,-4.18000002050115,
-57.0506994175354));
#139398=CARTESIAN_POINT('Ctrl Pts',(-59.3031923634925,-4.18000002133835,
-57.1634045844535));
#139399=CARTESIAN_POINT('Ctrl Pts',(-59.3500454603234,-4.18000002397293,
-57.2816264448194));
#139400=CARTESIAN_POINT('Ctrl Pts',(-59.3874625053509,-4.18000002286791,
-57.4021771888577));
#139401=CARTESIAN_POINT('Ctrl Pts',(-59.3945407287637,-4.18000002265887,
-57.4249819052179));
#139402=CARTESIAN_POINT('Ctrl Pts',(-59.4012856253719,-4.18000002232778,
-57.4478436795316));
#139403=CARTESIAN_POINT('Ctrl Pts',(-59.4076964194497,-4.18000002192605,
-57.4707623700245));
#139404=CARTESIAN_POINT('Ctrl Pts',(-59.4578200392951,-4.18000001878511,
-57.6499551058506));
#139405=CARTESIAN_POINT('Ctrl Pts',(-59.4876405140701,-4.18000002000073,
-57.8326096057389));
#139406=CARTESIAN_POINT('Ctrl Pts',(-59.4968871656945,-4.18000002000007,
-58.0187658449342));
#139407=CARTESIAN_POINT('Ctrl Pts',(-59.4989612576684,-4.18000001999992,
-58.0605220586746));
#139408=CARTESIAN_POINT('Ctrl Pts',(-59.5,-4.18000001999999,-58.1024544069462));
#139409=CARTESIAN_POINT('Ctrl Pts',(-59.5,-4.18000001999999,-58.1445632485962));
#139410=CARTESIAN_POINT('Origin',(-59.5,-4.68000001999999,-58.1445632485962));
#139411=CARTESIAN_POINT('Ctrl Pts',(-57.5408897718184,-3.75014666797429,
-60.8901206419019));
#139412=CARTESIAN_POINT('Ctrl Pts',(-57.5947641336391,-4.18011275636206,
-60.9185429056887));
#139413=CARTESIAN_POINT('Ctrl Pts',(-57.9789048525842,-4.18000000314622,
-61.1211158812058));
#139414=CARTESIAN_POINT('Ctrl Pts',(-57.6237851397972,-3.75639532415342,
-60.7345335560658));
#139415=CARTESIAN_POINT('Ctrl Pts',(-57.68640755168,-4.1801105122733,-60.7564968901202));
#139416=CARTESIAN_POINT('Ctrl Pts',(-58.1017608867774,-4.18000000339119,
-60.8877040749259));
#139417=CARTESIAN_POINT('Ctrl Pts',(-57.6637036934156,-3.75937776709444,
-60.5618009361651));
#139418=CARTESIAN_POINT('Ctrl Pts',(-57.7319155584136,-4.18010945496984,
-60.5708624589659));
#139419=CARTESIAN_POINT('Ctrl Pts',(-58.1609260730227,-4.18000000350811,
-60.6285977191473));
#139420=CARTESIAN_POINT('Ctrl Pts',(-57.6557606890352,-3.75878386386294,
-60.3838931293299));
#139421=CARTESIAN_POINT('Ctrl Pts',(-57.7229085994607,-4.18010966305883,
-60.3808564105654));
#139422=CARTESIAN_POINT('Ctrl Pts',(-58.14915342597,-4.18000000348483,-60.3617046583731));
#139423=CARTESIAN_POINT('',(-58.0081705490647,-4.18000001999999,-61.0621827299711));
#139424=CARTESIAN_POINT('Origin',(-58.0081705490647,-3.68000001999999,-61.0621827299711));
#139425=CARTESIAN_POINT('Origin',(-56.7672600194274,-4.18000063577663,-60.4581517878592));
#139426=CARTESIAN_POINT('Origin',(83.2809572255632,-4.18000001999993,-55.24995));
#139427=CARTESIAN_POINT('',(-40.0271577790679,-4.18000001999998,-98.926539349744));
#139428=CARTESIAN_POINT('Ctrl Pts',(-40.0271577790679,-4.18000001999998,
-98.926539349744));
#139429=CARTESIAN_POINT('Ctrl Pts',(-46.0600710189762,-4.18000001999998,
-86.3237225210772));
#139430=CARTESIAN_POINT('Ctrl Pts',(-52.0416455898407,-4.18000001999999,
-73.6965260027483));
#139431=CARTESIAN_POINT('Ctrl Pts',(-58.0081705490647,-4.18000001999999,
-61.0621827299711));
#139432=CARTESIAN_POINT('',(-39.5,-4.18000001999998,-101.255910620448));
#139433=CARTESIAN_POINT('Ctrl Pts',(-39.5,-4.18000001999998,-101.255910620448));
#139434=CARTESIAN_POINT('Ctrl Pts',(-39.5,-4.18000001999998,-100.974485528874));
#139435=CARTESIAN_POINT('Ctrl Pts',(-39.5222808837211,-4.18000001999998,
-100.693150422383));
#139436=CARTESIAN_POINT('Ctrl Pts',(-39.5655905129044,-4.18000001999998,
-100.416810780316));
#139437=CARTESIAN_POINT('Ctrl Pts',(-39.5844991866037,-4.18000001999998,
-100.296162873128));
#139438=CARTESIAN_POINT('Ctrl Pts',(-39.6074169109197,-4.18000001999998,
-100.17646712623));
#139439=CARTESIAN_POINT('Ctrl Pts',(-39.6342425380314,-4.18000001999998,
-100.058132231812));
#139440=CARTESIAN_POINT('Ctrl Pts',(-39.705309269373,-4.18000001999998,
-99.7446381943797));
#139441=CARTESIAN_POINT('Ctrl Pts',(-39.8034555232829,-4.18000001999998,
-99.4388673313459));
#139442=CARTESIAN_POINT('Ctrl Pts',(-39.9301327648642,-4.18000001999998,
-99.1412335947868));
#139443=CARTESIAN_POINT('Ctrl Pts',(-39.9607955551634,-4.18000001999998,
-99.0691900237701));
#139444=CARTESIAN_POINT('Ctrl Pts',(-39.9931302150587,-4.18000001999999,
-98.997623275415));
#139445=CARTESIAN_POINT('Ctrl Pts',(-40.0271577790679,-4.18000001999999,
-98.926539349744));
#139446=CARTESIAN_POINT('',(-39.5,-4.18000001999998,-130.802732351058));
#139447=CARTESIAN_POINT('',(-39.5,-4.18000001999998,-55.24995));
#139448=CARTESIAN_POINT('',(-40.0271577790634,-4.18000001999998,-133.132103621752));
#139449=CARTESIAN_POINT('Ctrl Pts',(-40.0271577790634,-4.18000001999998,
-133.132103621752));
#139450=CARTESIAN_POINT('Ctrl Pts',(-39.9035045934269,-4.18000001999998,
-132.873790865235));
#139451=CARTESIAN_POINT('Ctrl Pts',(-39.8011022473414,-4.18000001999999,
-132.605500495508));
#139452=CARTESIAN_POINT('Ctrl Pts',(-39.7207150267769,-4.18000001999999,
-132.332596829933));
#139453=CARTESIAN_POINT('Ctrl Pts',(-39.6875913562998,-4.18000001999999,
-132.220146479902));
#139454=CARTESIAN_POINT('Ctrl Pts',(-39.658204991549,-4.18000001999999,
-132.106913147232));
#139455=CARTESIAN_POINT('Ctrl Pts',(-39.6326069664648,-4.18000001999999,
-131.993272849631));
#139456=CARTESIAN_POINT('Ctrl Pts',(-39.5604708508339,-4.18000001999999,
-131.673030580114));
#139457=CARTESIAN_POINT('Ctrl Pts',(-39.5173036683714,-4.18000001999998,
-131.347852435241));
#139458=CARTESIAN_POINT('Ctrl Pts',(-39.5042396692621,-4.18000001999998,
-131.017545146585));
#139459=CARTESIAN_POINT('Ctrl Pts',(-39.5014171427719,-4.18000001999998,
-130.946181005764));
#139460=CARTESIAN_POINT('Ctrl Pts',(-39.5,-4.18000001999998,-130.874577408243));
#139461=CARTESIAN_POINT('Ctrl Pts',(-39.5,-4.18000001999998,-130.802732351058));
#139462=CARTESIAN_POINT('',(-58.1221005562789,-4.18000001999999,-171.237717270032));
#139463=CARTESIAN_POINT('Ctrl Pts',(-58.1221005562789,-4.18000001999999,
-171.237717270032));
#139464=CARTESIAN_POINT('Ctrl Pts',(-52.1178384024439,-4.18000001999999,
-158.522841724749));
#139465=CARTESIAN_POINT('Ctrl Pts',(-46.0984712740486,-4.18000001999998,
-145.815138971718));
#139466=CARTESIAN_POINT('Ctrl Pts',(-40.0271577790634,-4.18000001999998,
-133.132103621752));
#139467=CARTESIAN_POINT('',(-58.2644174754153,-4.18000001999999,-171.871644662643));
#139468=CARTESIAN_POINT('Origin',(-56.1314697890424,-4.18000001999999,-172.0066931789));
#139469=CARTESIAN_POINT('',(-58.2644174754116,-4.18000003136422,-176.647241333317));
#139470=CARTESIAN_POINT('',(-58.2644174754153,-4.18000001999999,-171.871644662643));
#139471=CARTESIAN_POINT('',(-59.5,-4.18000001999999,-174.488343624884));
#139472=CARTESIAN_POINT('Ctrl Pts',(-59.5,-4.18000001999999,-174.488343624884));
#139473=CARTESIAN_POINT('Ctrl Pts',(-59.5,-4.18000001999999,-174.676432184924));
#139474=CARTESIAN_POINT('Ctrl Pts',(-59.4792627601893,-4.18000001935391,
-174.860994953506));
#139475=CARTESIAN_POINT('Ctrl Pts',(-59.4381337746335,-4.18000002064829,
-175.042081103098));
#139476=CARTESIAN_POINT('Ctrl Pts',(-59.431381263521,-4.18000002086079,
-175.071811625767));
#139477=CARTESIAN_POINT('Ctrl Pts',(-59.4240789892461,-4.18000002115769,
-175.101448468679));
#139478=CARTESIAN_POINT('Ctrl Pts',(-59.4162283471532,-4.18000002161129,
-175.130991885445));
#139479=CARTESIAN_POINT('Ctrl Pts',(-59.4092933860371,-4.18000002201199,
-175.157089425504));
#139480=CARTESIAN_POINT('Ctrl Pts',(-59.4019280344311,-4.18000002232545,
-175.183113688583));
#139481=CARTESIAN_POINT('Ctrl Pts',(-59.3941336392735,-4.18000002248887,
-175.209064512545));
#139482=CARTESIAN_POINT('Ctrl Pts',(-59.3589528015432,-4.18000002322649,
-175.326196337184));
#139483=CARTESIAN_POINT('Ctrl Pts',(-59.3147522563139,-4.18000002089879,
-175.441619139941));
#139484=CARTESIAN_POINT('Ctrl Pts',(-59.2630854722639,-4.18000002030225,
-175.551758766342));
#139485=CARTESIAN_POINT('Ctrl Pts',(-59.2343127518865,-4.18000001997004,
-175.613094433564));
#139486=CARTESIAN_POINT('Ctrl Pts',(-59.2031440665131,-4.18000001999999,
-175.673101168879));
#139487=CARTESIAN_POINT('Ctrl Pts',(-59.1695814056726,-4.18000001999999,
-175.731779921994));
#139488=CARTESIAN_POINT('Ctrl Pts',(-59.1428767576963,-4.18000001999999,
-175.778468575586));
#139489=CARTESIAN_POINT('Ctrl Pts',(-59.1146521957298,-4.18000001999991,
-175.824314777934));
#139490=CARTESIAN_POINT('Ctrl Pts',(-59.0849057084902,-4.18000002000059,
-175.869317498238));
#139491=CARTESIAN_POINT('Ctrl Pts',(-59.0177729179323,-4.18000002000213,
-175.970881026476));
#139492=CARTESIAN_POINT('Ctrl Pts',(-58.9421638152095,-4.18000002001086,
-176.068866658213));
#139493=CARTESIAN_POINT('Ctrl Pts',(-58.8606254499681,-4.18000002000853,
-176.15981892266));
#139494=CARTESIAN_POINT('Ctrl Pts',(-58.8332817762446,-4.18000002000775,
-176.190319522422));
#139495=CARTESIAN_POINT('Ctrl Pts',(-58.8052684934467,-4.18000002000547,
-176.220067577769));
#139496=CARTESIAN_POINT('Ctrl Pts',(-58.7765893403539,-4.18000002000312,
-176.2490672712));
#139497=CARTESIAN_POINT('Ctrl Pts',(-58.7334919025214,-4.18000001999957,
-176.292646399243));
#139498=CARTESIAN_POINT('Ctrl Pts',(-58.6887854216316,-4.1800000198565,
-176.334637716938));
#139499=CARTESIAN_POINT('Ctrl Pts',(-58.6426104314479,-4.18000002015176,
-176.374934331063));
#139500=CARTESIAN_POINT('Ctrl Pts',(-58.6279756118792,-4.18000002024535,
-176.387706043078));
#139501=CARTESIAN_POINT('Ctrl Pts',(-58.6131935185628,-4.18000002040339,
-176.400307828981));
#139502=CARTESIAN_POINT('Ctrl Pts',(-58.5982692931781,-4.18000002077447,
-176.412737145101));
#139503=CARTESIAN_POINT('Ctrl Pts',(-58.5771929061033,-4.18000002129852,
-176.430290155116));
#139504=CARTESIAN_POINT('Ctrl Pts',(-58.5557921166901,-4.18000002220248,
-176.447510765875));
#139505=CARTESIAN_POINT('Ctrl Pts',(-58.5341058949341,-4.18000002446768,
-176.464377473526));
#139506=CARTESIAN_POINT('Ctrl Pts',(-58.4881980669411,-4.18000002926289,
-176.500082813181));
#139507=CARTESIAN_POINT('Ctrl Pts',(-58.4409815652462,-4.18000004169373,
-176.534222750276));
#139508=CARTESIAN_POINT('Ctrl Pts',(-58.3925215548524,-4.18000005349381,
-176.566751049323));
#139509=CARTESIAN_POINT('Ctrl Pts',(-58.3507358574755,-4.18000006366869,
-176.59479928227));
#139510=CARTESIAN_POINT('Ctrl Pts',(-58.3080246526018,-4.18000007127262,
-176.621648795663));
#139511=CARTESIAN_POINT('Ctrl Pts',(-58.2644174754055,-4.18000006545692,
-176.647241333307));
#139512=CARTESIAN_POINT('',(-59.5,-4.18000001999999,-174.466077711105));
#139513=CARTESIAN_POINT('Origin',(0.,-12.9675000200281,-60.64995));
#139514=CARTESIAN_POINT('',(-39.585730865575,-3.78242429077387,-98.7152302188469));
#139515=CARTESIAN_POINT('',(-39.7525219239569,1.81208306810639,-94.9115092130908));
#139516=CARTESIAN_POINT('Ctrl Pts',(-39.585730865631,-3.78242429107081,
-98.7152302188737));
#139517=CARTESIAN_POINT('Ctrl Pts',(-39.5925554021339,-3.50286551329097,
-98.5654740436898));
#139518=CARTESIAN_POINT('Ctrl Pts',(-39.5995949827268,-3.22506435949984,
-98.4103062973797));
#139519=CARTESIAN_POINT('Ctrl Pts',(-39.6215565252267,-2.38668519024414,
-97.9237506811802));
#139520=CARTESIAN_POINT('Ctrl Pts',(-39.6371406048982,-1.82970860306462,
-97.5751506494424));
#139521=CARTESIAN_POINT('Ctrl Pts',(-39.6847862724127,-0.212218467036257,
-96.496949566391));
#139522=CARTESIAN_POINT('Ctrl Pts',(-39.7182100340316,0.816234902512257,
-95.7247235977679));
#139523=CARTESIAN_POINT('Ctrl Pts',(-39.7525219240432,1.8120830678168,-94.9115092131337));
#139524=CARTESIAN_POINT('Ctrl Pts',(-57.5607154366947,-3.75164060643487,
-60.8508735991007));
#139525=CARTESIAN_POINT('Ctrl Pts',(-51.5953561753878,-3.75882514278712,
-73.4851842515103));
#139526=CARTESIAN_POINT('Ctrl Pts',(-45.6152480050635,-3.76777552135149,
-86.1124074293824));
#139527=CARTESIAN_POINT('Ctrl Pts',(-39.585730865631,-3.78242429107081,
-98.7152302188737));
#139528=CARTESIAN_POINT('Ctrl Pts',(-39.7525219240432,1.8120830678168,-94.9115092131337));
#139529=CARTESIAN_POINT('Ctrl Pts',(-42.5630938966427,1.82180095215014,
-89.2547782578028));
#139530=CARTESIAN_POINT('Ctrl Pts',(-45.3466144966382,1.82978958392238,
-83.5843555039947));
#139531=CARTESIAN_POINT('Ctrl Pts',(-50.8828928487858,1.84368306852047,
-72.2280037103762));
#139532=CARTESIAN_POINT('Ctrl Pts',(-53.6353179962474,1.84957228639408,
-66.5419044818115));
#139533=CARTESIAN_POINT('Ctrl Pts',(-56.377904566775,1.85477723331148,-60.8508735991007));
#139534=CARTESIAN_POINT('Ctrl Pts',(-56.4768060379592,1.84328648456651,
-60.3843526253219));
#139535=CARTESIAN_POINT('Ctrl Pts',(-56.3127916612335,2.47013219497058,
-60.3918959659146));
#139536=CARTESIAN_POINT('Ctrl Pts',(-56.9600934028813,2.46999996959074,
-60.3623927486908));
#139537=CARTESIAN_POINT('Ctrl Pts',(-56.4849292473983,1.84234741764349,
-60.5602093497011));
#139538=CARTESIAN_POINT('Ctrl Pts',(-56.3176950849992,2.47013256123686,
-60.5376645429823));
#139539=CARTESIAN_POINT('Ctrl Pts',(-56.9719086646404,2.46999996957514,
-60.6262162467223));
#139540=CARTESIAN_POINT('Ctrl Pts',(-56.4442115172646,1.84705094373349,
-60.7334982606779));
#139541=CARTESIAN_POINT('Ctrl Pts',(-56.2937114156122,2.47013073129433,
-60.6793039133547));
#139542=CARTESIAN_POINT('Ctrl Pts',(-56.9126832861354,2.46999996965326,
-60.8861329835762));
#139543=CARTESIAN_POINT('Ctrl Pts',(-56.3570930423877,1.85720121361396,
-60.8904421107847));
#139544=CARTESIAN_POINT('Ctrl Pts',(-56.232192761867,2.4701269151012,-60.8230951160809));
#139545=CARTESIAN_POINT('Ctrl Pts',(-56.7859903733787,2.46999996982182,
-61.1215882796171));
#139546=CARTESIAN_POINT('',(-56.8161649572467,2.46999998000001,-61.0621827299711));
#139547=CARTESIAN_POINT('Origin',(-55.5227769329964,2.47000037335106,-60.4517448637277));
#139548=CARTESIAN_POINT('Origin',(-56.8161649572467,1.96999998000001,-61.0621827299711));
#139549=CARTESIAN_POINT('Origin',(83.2809572255632,2.46999998000007,-55.24995));
#139550=CARTESIAN_POINT('',(-57.,2.46999998000001,-55.74995));
#139551=CARTESIAN_POINT('',(83.2809572255632,2.46999998000007,-55.74995));
#139552=CARTESIAN_POINT('',(-59.5,2.46999998000001,-58.24995));
#139553=CARTESIAN_POINT('Origin',(-57.,2.46999998000001,-58.24995));
#139554=CARTESIAN_POINT('',(-59.5,2.46999998000001,-174.34995));
#139555=CARTESIAN_POINT('',(-59.5,2.46999998000001,-58.24995));
#139556=CARTESIAN_POINT('',(-57.077763566464,2.46999998000001,-176.848740272858));
#139557=CARTESIAN_POINT('Origin',(-57.,2.46999998000001,-174.34995));
#139558=CARTESIAN_POINT('',(-57.077763566464,2.46999998000001,-171.871644662643));
#139559=CARTESIAN_POINT('',(-57.077763566464,2.46999998000001,-176.84995));
#139560=CARTESIAN_POINT('',(-56.9324803875071,2.46999998000001,-171.237717270032));
#139561=CARTESIAN_POINT('Origin',(-55.639113972473,2.47000037313163,-171.847693895992));
#139562=CARTESIAN_POINT('',(-40.1772697316389,2.46999998000002,-136.935824627502));
#139563=CARTESIAN_POINT('Ctrl Pts',(-40.1772697316389,2.46999998000002,
-136.935824627502));
#139564=CARTESIAN_POINT('Ctrl Pts',(-43.0113367121144,2.46999998000002,
-142.632519945825));
#139565=CARTESIAN_POINT('Ctrl Pts',(-45.8169723643453,2.46999998000002,
-148.343102920405));
#139566=CARTESIAN_POINT('Ctrl Pts',(-48.6065865655743,2.46999998000001,
-154.061511783466));
#139567=CARTESIAN_POINT('Ctrl Pts',(-51.3962007668033,2.46999998000001,
-159.779920646528));
#139568=CARTESIAN_POINT('Ctrl Pts',(-54.1694328122146,2.46999998000001,
-165.506331589084));
#139569=CARTESIAN_POINT('Ctrl Pts',(-56.9324803874897,2.46999998000001,
-171.23771727004));
#139570=CARTESIAN_POINT('',(-39.5,2.46999998000002,-134.012863078852));
#139571=CARTESIAN_POINT('Ctrl Pts',(-39.5,2.46999998000002,-134.012863078852));
#139572=CARTESIAN_POINT('Ctrl Pts',(-39.5,2.46999998000002,-134.194202123598));
#139573=CARTESIAN_POINT('Ctrl Pts',(-39.5074991738613,2.46999998000002,
-134.375559257497));
#139574=CARTESIAN_POINT('Ctrl Pts',(-39.5222608830472,2.46999998000002,
-134.556078177935));
#139575=CARTESIAN_POINT('Ctrl Pts',(-39.5372803972933,2.46999998000002,
-134.739749761156));
#139576=CARTESIAN_POINT('Ctrl Pts',(-39.5598184209784,2.46999998000002,
-134.922554775989));
#139577=CARTESIAN_POINT('Ctrl Pts',(-39.5896791401062,2.46999998000002,
-135.103595442119));
#139578=CARTESIAN_POINT('Ctrl Pts',(-39.6126641240195,2.46999998000002,
-135.242949647918));
#139579=CARTESIAN_POINT('Ctrl Pts',(-39.6399889131325,2.46999998000002,
-135.381258722716));
#139580=CARTESIAN_POINT('Ctrl Pts',(-39.671584618531,2.46999998000002,-135.518108079287));
#139581=CARTESIAN_POINT('Ctrl Pts',(-39.7480265101501,2.46999998000002,
-135.849198129379));
#139582=CARTESIAN_POINT('Ctrl Pts',(-39.8488754308751,2.46999998000002,
-136.172910839316));
#139583=CARTESIAN_POINT('Ctrl Pts',(-39.976224515067,2.46999998000002,-136.488613556871));
#139584=CARTESIAN_POINT('Ctrl Pts',(-40.0371049338932,2.46999998000002,
-136.639538188887));
#139585=CARTESIAN_POINT('Ctrl Pts',(-40.1040424074824,2.46999998000002,
-136.788632003769));
#139586=CARTESIAN_POINT('Ctrl Pts',(-40.1772697316389,2.46999998000002,
-136.935824627502));
#139587=CARTESIAN_POINT('',(-39.5,2.46999998000002,-98.0457798926543));
#139588=CARTESIAN_POINT('',(-39.5,2.46999998000002,-55.24995));
#139589=CARTESIAN_POINT('',(-40.177269731639,2.46999998000002,-95.1228183440042));
#139590=CARTESIAN_POINT('Ctrl Pts',(-40.1772697316388,2.46999998000002,
-95.1228183440041));
#139591=CARTESIAN_POINT('Ctrl Pts',(-40.0557143101432,2.46999998000002,
-95.367154206676));
#139592=CARTESIAN_POINT('Ctrl Pts',(-39.9506490904769,2.46999998000002,
-95.6194942161999));
#139593=CARTESIAN_POINT('Ctrl Pts',(-39.862036785698,2.46999998000002,-95.876484568063));
#139594=CARTESIAN_POINT('Ctrl Pts',(-39.785571796048,2.46999998000002,-96.0982456953059));
#139595=CARTESIAN_POINT('Ctrl Pts',(-39.721358807228,2.46999998000002,-96.3234708895919));
#139596=CARTESIAN_POINT('Ctrl Pts',(-39.6694028678065,2.46999998000002,
-96.5500162443606));
#139597=CARTESIAN_POINT('Ctrl Pts',(-39.5883957972392,2.46999998000002,
-96.9032342930522));
#139598=CARTESIAN_POINT('Ctrl Pts',(-39.5360425809491,2.46999998000002,
-97.2613436845053));
#139599=CARTESIAN_POINT('Ctrl Pts',(-39.5132030141796,2.46999998000002,
-97.6244912071908));
#139600=CARTESIAN_POINT('Ctrl Pts',(-39.5044179952616,2.46999998000002,
-97.7641723968128));
#139601=CARTESIAN_POINT('Ctrl Pts',(-39.5,2.46999998000002,-97.9045990595778));
#139602=CARTESIAN_POINT('Ctrl Pts',(-39.5,2.46999998000002,-98.0457798926543));
#139603=CARTESIAN_POINT('Ctrl Pts',(-56.8161649572467,2.46999998000001,
-61.0621827299711));
#139604=CARTESIAN_POINT('Ctrl Pts',(-54.0722086604215,2.46999998000001,
-66.7532163030615));
#139605=CARTESIAN_POINT('Ctrl Pts',(-51.3181460106093,2.46999998000001,
-72.4393128412015));
#139606=CARTESIAN_POINT('Ctrl Pts',(-48.5478694191173,2.46999998000001,
-78.1174887380514));
#139607=CARTESIAN_POINT('Ctrl Pts',(-45.7775928276252,2.46999998000002,
-83.7956646349013));
#139608=CARTESIAN_POINT('Ctrl Pts',(-42.9914528488282,2.46999998000002,
-89.4660911391003));
#139609=CARTESIAN_POINT('Ctrl Pts',(-40.1772697316389,2.46999998000002,
-95.1228183440041));
#139610=CARTESIAN_POINT('Origin',(-60.,2.96999998000001,-55.74995));
#139611=CARTESIAN_POINT('',(-57.,2.96999998000001,-55.24995));
#139612=CARTESIAN_POINT('',(-60.,2.96999998000001,-55.24995));
#139613=CARTESIAN_POINT('Origin',(-57.,2.96999998000001,-55.74995));
#139614=CARTESIAN_POINT('Origin',(-60.,28.41999998,-55.24995));
#139615=CARTESIAN_POINT('',(-57.,3.46999998000001,-55.24995));
#139616=CARTESIAN_POINT('',(-60.,3.46999998000001,-55.24995));
#139617=CARTESIAN_POINT('',(-57.,28.41999998,-55.24995));
#139618=CARTESIAN_POINT('Origin',(83.2809572255632,3.46999998000007,-55.74995));
#139619=CARTESIAN_POINT('',(-57.,3.96999998000001,-55.74995));
#139620=CARTESIAN_POINT('',(83.2809572255632,3.96999998000007,-55.74995));
#139621=CARTESIAN_POINT('Origin',(-57.,3.46999998000001,-55.74995));
#139622=CARTESIAN_POINT('Ctrl Pts',(-55.6456300835169,4.33828227850038,
-60.8898982295148));
#139623=CARTESIAN_POINT('Ctrl Pts',(-55.7339281824781,3.96993431898625,
-60.9380383069126));
#139624=CARTESIAN_POINT('Ctrl Pts',(-56.0692321081993,3.96999998739438,
-61.1207654305588));
#139625=CARTESIAN_POINT('Ctrl Pts',(-55.7334016533014,4.32662458144452,
-60.7353258635364));
#139626=CARTESIAN_POINT('Ctrl Pts',(-55.8351750163154,3.96993697857447,
-60.7722679906112));
#139627=CARTESIAN_POINT('Ctrl Pts',(-56.1954681966718,3.96999998716033,
-60.8888693966731));
#139628=CARTESIAN_POINT('Ctrl Pts',(-55.7764277962604,4.32095586851412,
-60.5620589091497));
#139629=CARTESIAN_POINT('Ctrl Pts',(-55.8870156345094,3.96993824711686,
-60.5772788420628));
#139630=CARTESIAN_POINT('Ctrl Pts',(-56.2573698974905,3.96999998704652,
-60.6289874486285));
#139631=CARTESIAN_POINT('Ctrl Pts',(-55.7678794768586,4.32208288640323,
-60.3838032961762));
#139632=CARTESIAN_POINT('Ctrl Pts',(-55.8768003135833,3.96993799744087,
-60.3787010736661));
#139633=CARTESIAN_POINT('Ctrl Pts',(-56.2450717652166,3.96999998706915,
-60.3615697395426));
#139634=CARTESIAN_POINT('',(-56.0993680931338,3.96999998000001,-61.0621827299711));
#139635=CARTESIAN_POINT('Origin',(-56.0993680931338,4.46999998000001,-61.0621827299711));
#139636=CARTESIAN_POINT('Origin',(-54.7700863539085,3.96999970901095,-60.4480774066313));
#139637=CARTESIAN_POINT('Origin',(83.2809572255632,3.96999998000007,-55.24995));
#139638=CARTESIAN_POINT('',(-40.2576018765703,3.96999998000001,-92.9619213022396));
#139639=CARTESIAN_POINT('Ctrl Pts',(-40.2576018765703,3.96999998000001,
-92.9619213022396));
#139640=CARTESIAN_POINT('Ctrl Pts',(-42.9469753996782,3.96999998000001,
-87.669671462365));
#139641=CARTESIAN_POINT('Ctrl Pts',(-45.6032617662994,3.96999998000001,
-82.3609901712845));
#139642=CARTESIAN_POINT('Ctrl Pts',(-48.2402535232915,3.96999998000001,
-77.0427269617097));
#139643=CARTESIAN_POINT('Ctrl Pts',(-50.8772452802836,3.96999998000001,
-71.724463752135));
#139644=CARTESIAN_POINT('Ctrl Pts',(-53.4945730592583,3.96999998000001,
-66.3964351916018));
#139645=CARTESIAN_POINT('Ctrl Pts',(-56.0993680931338,3.96999998000001,
-61.0621827299711));
#139646=CARTESIAN_POINT('',(-39.5,3.96999998000002,-96.1952589849652));
#139647=CARTESIAN_POINT('Ctrl Pts',(-39.5,3.96999998000002,-96.1952589849652));
#139648=CARTESIAN_POINT('Ctrl Pts',(-39.5,3.96999998000001,-95.9142103380175));
#139649=CARTESIAN_POINT('Ctrl Pts',(-39.5161227273835,3.96999998000002,
-95.6343109988079));
#139650=CARTESIAN_POINT('Ctrl Pts',(-39.5801128567305,3.96999998000002,
-95.0767752377766));
#139651=CARTESIAN_POINT('Ctrl Pts',(-39.6280462441481,3.96999998000002,
-94.7999095964395));
#139652=CARTESIAN_POINT('Ctrl Pts',(-39.81711425019,3.96999998000002,-93.9870091546851));
#139653=CARTESIAN_POINT('Ctrl Pts',(-40.0026450649981,3.96999998000001,
-93.4636348550876));
#139654=CARTESIAN_POINT('Ctrl Pts',(-40.2576018765703,3.96999998000001,
-92.9619213022396));
#139655=CARTESIAN_POINT('',(-39.5,3.96999998000002,-135.863383986541));
#139656=CARTESIAN_POINT('',(-39.5,3.96999998000002,-55.24995));
#139657=CARTESIAN_POINT('',(-40.2576018765703,3.96999998000001,-139.096721669266));
#139658=CARTESIAN_POINT('Ctrl Pts',(-40.2576018765703,3.96999998000001,
-139.096721669266));
#139659=CARTESIAN_POINT('Ctrl Pts',(-40.1422232489776,3.96999998000001,
-138.869675289076));
#139660=CARTESIAN_POINT('Ctrl Pts',(-40.0403932052765,3.96999998000002,
-138.635953665709));
#139661=CARTESIAN_POINT('Ctrl Pts',(-39.9518763029248,3.96999998000002,
-138.39795690135));
#139662=CARTESIAN_POINT('Ctrl Pts',(-39.8589569884594,3.96999998000002,
-138.148123303454));
#139663=CARTESIAN_POINT('Ctrl Pts',(-39.7807077156224,3.96999998000002,
-137.893577344799));
#139664=CARTESIAN_POINT('Ctrl Pts',(-39.716907177829,3.96999998000002,-137.637072537678));
#139665=CARTESIAN_POINT('Ctrl Pts',(-39.7071356404147,3.96999998000002,
-137.597786876358));
#139666=CARTESIAN_POINT('Ctrl Pts',(-39.6977031285481,3.96999998000002,
-137.55845524907));
#139667=CARTESIAN_POINT('Ctrl Pts',(-39.6886089528968,3.96999998000002,
-137.519087538285));
#139668=CARTESIAN_POINT('Ctrl Pts',(-39.6032792176026,3.96999998000002,
-137.149704268237));
#139669=CARTESIAN_POINT('Ctrl Pts',(-39.5465796834614,3.96999998000002,
-136.775425176638));
#139670=CARTESIAN_POINT('Ctrl Pts',(-39.5191682987985,3.96999998000002,
-136.396137730949));
#139671=CARTESIAN_POINT('Ctrl Pts',(-39.5064128043265,3.96999998000002,
-136.219641761254));
#139672=CARTESIAN_POINT('Ctrl Pts',(-39.5000000000002,3.96999998000002,
-136.042061173864));
#139673=CARTESIAN_POINT('Ctrl Pts',(-39.5,3.96999998000002,-135.863383986541));
#139674=CARTESIAN_POINT('',(-56.217166622605,3.96999998000001,-171.237717270032));
#139675=CARTESIAN_POINT('Ctrl Pts',(-56.217166622605,3.96999998000001,-171.237717270032));
#139676=CARTESIAN_POINT('Ctrl Pts',(-53.5931275135095,3.96999998000001,
-165.863064362473));
#139677=CARTESIAN_POINT('Ctrl Pts',(-50.9564483006798,3.96999998000001,
-160.49468788009));
#139678=CARTESIAN_POINT('Ctrl Pts',(-48.2998833897147,3.96999998000001,
-155.136185612272));
#139679=CARTESIAN_POINT('Ctrl Pts',(-45.6433184787496,3.96999998000001,
-149.777683344454));
#139680=CARTESIAN_POINT('Ctrl Pts',(-42.9672487496428,3.96999998000001,
-144.428866165794));
#139681=CARTESIAN_POINT('Ctrl Pts',(-40.2576018765703,3.96999998000001,
-139.096721669266));
#139682=CARTESIAN_POINT('',(-56.3642936064049,3.96999998000001,-171.871644662643));
#139683=CARTESIAN_POINT('Origin',(-54.8887873789865,3.96999970486963,-171.85218621454));
#139684=CARTESIAN_POINT('',(-56.3642936064049,3.96999998000001,-176.84995));
#139685=CARTESIAN_POINT('',(-56.3642936064049,3.96999998000001,-171.871644662643));
#139686=CARTESIAN_POINT('',(-57.,3.96999998000001,-176.84995));
#139687=CARTESIAN_POINT('',(83.2809572255632,3.96999998000007,-176.84995));
#139688=CARTESIAN_POINT('',(-59.5,3.96999998000001,-174.34995));
#139689=CARTESIAN_POINT('Origin',(-57.,3.96999998000001,-174.34995));
#139690=CARTESIAN_POINT('',(-59.5,3.96999998000001,-58.24995));
#139691=CARTESIAN_POINT('',(-59.5,3.96999998000001,-174.34995));
#139692=CARTESIAN_POINT('Origin',(-57.,3.96999998000001,-58.24995));
#139693=CARTESIAN_POINT('Origin',(0.,-12.9675000200281,-60.64995));
#139694=CARTESIAN_POINT('',(-39.8417798628559,4.28988750369335,-92.7506121713693));
#139695=CARTESIAN_POINT('',(-40.0642139580843,9.89540189669765,-86.9391114694665));
#139696=CARTESIAN_POINT('Ctrl Pts',(-39.8417723428251,4.289984134881,-92.7507162230213));
#139697=CARTESIAN_POINT('Ctrl Pts',(-39.8692662103635,5.02430264837445,
-92.0707528204852));
#139698=CARTESIAN_POINT('Ctrl Pts',(-39.8971213137832,5.74554162158512,
-91.3685155609789));
#139699=CARTESIAN_POINT('Ctrl Pts',(-39.9251065221777,6.45615586467189,
-90.6478697442548));
#139700=CARTESIAN_POINT('Ctrl Pts',(-39.9717823825843,7.64137238140021,
-89.4459218055498));
#139701=CARTESIAN_POINT('Ctrl Pts',(-40.0183482409369,8.78465889880687,
-88.2051541708012));
#139702=CARTESIAN_POINT('Ctrl Pts',(-40.0642139729082,9.89540198625494,
-86.9391115876706));
#139703=CARTESIAN_POINT('Ctrl Pts',(-55.6666368275827,4.33549309160633,
-60.8508735991007));
#139704=CARTESIAN_POINT('Ctrl Pts',(-53.0636135602343,4.32979793687723,
-66.1851229317376));
#139705=CARTESIAN_POINT('Ctrl Pts',(-50.4483866480001,4.32340038871991,
-71.5131546215955));
#139706=CARTESIAN_POINT('Ctrl Pts',(-45.179787381339,4.30850505134695,-82.1496810408829));
#139707=CARTESIAN_POINT('Ctrl Pts',(-42.5267665530282,4.30001892806028,
-87.4583592350843));
#139708=CARTESIAN_POINT('Ctrl Pts',(-39.8417798628559,4.28988750369335,
-92.7506121713693));
#139709=CARTESIAN_POINT('Ctrl Pts',(-40.064213984323,9.89540181527278,-86.9391114268059));
#139710=CARTESIAN_POINT('Ctrl Pts',(-42.3769453355832,9.90511004939769,
-82.6211625585897));
#139711=CARTESIAN_POINT('Ctrl Pts',(-44.6533124708726,9.91361722903472,
-78.283718841389));
#139712=CARTESIAN_POINT('Ctrl Pts',(-49.1597584393762,9.92893028193935,
-69.5840753777615));
#139713=CARTESIAN_POINT('Ctrl Pts',(-51.3895604060249,9.93573233905146,
-65.2217230121251));
#139714=CARTESIAN_POINT('Ctrl Pts',(-53.6034226162473,9.94191093135268,
-60.8508735991007));
#139715=CARTESIAN_POINT('Ctrl Pts',(-53.7125918503832,9.92402752715881,
-60.40351858218));
#139716=CARTESIAN_POINT('Ctrl Pts',(-53.4161966316591,10.6200463510678,
-60.411613444258));
#139717=CARTESIAN_POINT('Ctrl Pts',(-54.1724511599881,10.6199999790608,
-60.3911473089805));
#139718=CARTESIAN_POINT('Ctrl Pts',(-53.7172936685689,9.92326040045936,
-60.5668141071178));
#139719=CARTESIAN_POINT('Ctrl Pts',(-53.4174513698505,10.620046463598,-60.5214955398562));
#139720=CARTESIAN_POINT('Ctrl Pts',(-54.1790134480646,10.6199999790597,
-60.6361119980643));
#139721=CARTESIAN_POINT('Ctrl Pts',(-53.6753724344268,9.93009784663695,
-60.7276561184828));
#139722=CARTESIAN_POINT('Ctrl Pts',(-53.4068684094031,10.6200454844905,
-60.6288932216019));
#139723=CARTESIAN_POINT('Ctrl Pts',(-54.1205022571196,10.6199999790689,
-60.8773492053566));
#139724=CARTESIAN_POINT('Ctrl Pts',(-53.5909494181271,9.94395845212128,
-60.8730306626157));
#139725=CARTESIAN_POINT('Ctrl Pts',(-53.3671997002977,10.6200436156875,
-60.752177389371));
#139726=CARTESIAN_POINT('Ctrl Pts',(-54.0027434996135,10.6199999790877,
-61.095435351044));
#139727=CARTESIAN_POINT('',(-54.0201152391274,10.61999998,-61.0621827299711));
#139728=CARTESIAN_POINT('Origin',(-52.5839997447372,10.6200000169309,-60.4356500018395));
#139729=CARTESIAN_POINT('Origin',(-54.0201152391274,10.11999998,-61.0621827299711));
#139730=CARTESIAN_POINT('Origin',(83.2809572255632,10.6199999800001,-55.24995));
#139731=CARTESIAN_POINT('',(-54.1424378198232,10.61999998,-171.237717270032));
#139732=CARTESIAN_POINT('',(-54.2951871140408,10.61999998,-171.871644662643));
#139733=CARTESIAN_POINT('Origin',(-52.7058336009045,10.6200000150414,-171.86389522969));
#139734=CARTESIAN_POINT('',(-40.4577925858907,10.61999998,-144.90822241383));
#139735=CARTESIAN_POINT('Ctrl Pts',(-40.4577925858907,10.61999998,-144.90822241383));
#139736=CARTESIAN_POINT('Ctrl Pts',(-42.7973924930771,10.61999998,-149.265897143292));
#139737=CARTESIAN_POINT('Ctrl Pts',(-45.0988060523871,10.61999998,-153.643419067936));
#139738=CARTESIAN_POINT('Ctrl Pts',(-47.3760737205893,10.61999998,-158.033490718866));
#139739=CARTESIAN_POINT('Ctrl Pts',(-49.6533413887914,10.61999998,-162.423562369795));
#139740=CARTESIAN_POINT('Ctrl Pts',(-51.9061626796858,10.61999998,-166.826339923461));
#139741=CARTESIAN_POINT('Ctrl Pts',(-54.1424378198232,10.61999998,-171.237717270032));
#139742=CARTESIAN_POINT('',(-39.5,10.61999998,-140.924467062102));
#139743=CARTESIAN_POINT('Ctrl Pts',(-39.5,10.61999998,-140.924467062102));
#139744=CARTESIAN_POINT('Ctrl Pts',(-39.5,10.61999998,-141.064641740712));
#139745=CARTESIAN_POINT('Ctrl Pts',(-39.503286113677,10.619999980029,-141.204536867587));
#139746=CARTESIAN_POINT('Ctrl Pts',(-39.5098002370266,10.6199999796907,
-141.344151254401));
#139747=CARTESIAN_POINT('Ctrl Pts',(-39.5163738758532,10.6199999793493,
-141.48504121068));
#139748=CARTESIAN_POINT('Ctrl Pts',(-39.5262347839855,10.6199999785395,
-141.625645980314));
#139749=CARTESIAN_POINT('Ctrl Pts',(-39.5393758471116,10.6199999780094,
-141.765968909085));
#139750=CARTESIAN_POINT('Ctrl Pts',(-39.5454296177965,10.6199999777652,
-141.830612296341));
#139751=CARTESIAN_POINT('Ctrl Pts',(-39.5521802385778,10.6199999776063,
-141.895195868192));
#139752=CARTESIAN_POINT('Ctrl Pts',(-39.5596307210412,10.6199999776383,
-141.959719632822));
#139753=CARTESIAN_POINT('Ctrl Pts',(-39.5766960195726,10.6199999777115,
-142.107511042464));
#139754=CARTESIAN_POINT('Ctrl Pts',(-39.5974615300863,10.6199999785835,
-142.255205307));
#139755=CARTESIAN_POINT('Ctrl Pts',(-39.6219007996117,10.6199999791661,
-142.402216894674));
#139756=CARTESIAN_POINT('Ctrl Pts',(-39.6461342711765,10.6199999797438,
-142.547990528615));
#139757=CARTESIAN_POINT('Ctrl Pts',(-39.6739797737404,10.6199999799661,
-142.693092202937));
#139758=CARTESIAN_POINT('Ctrl Pts',(-39.7053613936664,10.6199999799929,
-142.836960501119));
#139759=CARTESIAN_POINT('Ctrl Pts',(-39.7158636782078,10.6199999800019,
-142.885107977494));
#139760=CARTESIAN_POINT('Ctrl Pts',(-39.7267615964739,10.61999998,-142.933117442992));
#139761=CARTESIAN_POINT('Ctrl Pts',(-39.7380510717141,10.61999998,-142.980968310073));
#139762=CARTESIAN_POINT('Ctrl Pts',(-39.8192390703692,10.61999998,-143.32508670792));
#139763=CARTESIAN_POINT('Ctrl Pts',(-39.9201606061929,10.61999998,-143.66253928893));
#139764=CARTESIAN_POINT('Ctrl Pts',(-40.0436577688856,10.61999998,-143.992366080452));
#139765=CARTESIAN_POINT('Ctrl Pts',(-40.1606310196878,10.61999998,-144.304769306281));
#139766=CARTESIAN_POINT('Ctrl Pts',(-40.2978572937945,10.61999998,-144.61033131776));
#139767=CARTESIAN_POINT('Ctrl Pts',(-40.4577925858907,10.61999998,-144.90822241383));
#139768=CARTESIAN_POINT('',(-39.5,10.61999998,-91.1341759094044));
#139769=CARTESIAN_POINT('',(-39.5,10.61999998,-55.24995));
#139770=CARTESIAN_POINT('',(-40.4577925858907,10.61999998,-87.1504205576762));
#139771=CARTESIAN_POINT('Ctrl Pts',(-40.4577925858907,10.61999998,-87.1504205576762));
#139772=CARTESIAN_POINT('Ctrl Pts',(-40.3970580365439,10.61999998,-87.2635430663928));
#139773=CARTESIAN_POINT('Ctrl Pts',(-40.3395672151842,10.61999998,-87.3780682227962));
#139774=CARTESIAN_POINT('Ctrl Pts',(-40.2851314284313,10.61999998,-87.4939105062412));
#139775=CARTESIAN_POINT('Ctrl Pts',(-40.228662932352,10.61999998,-87.6140785045144));
#139776=CARTESIAN_POINT('Ctrl Pts',(-40.1754817433885,10.61999998,-87.7356644050421));
#139777=CARTESIAN_POINT('Ctrl Pts',(-40.1254267036636,10.61999998,-87.8586004744554));
#139778=CARTESIAN_POINT('Ctrl Pts',(-40.0931586145966,10.61999998,-87.9378514761361));
#139779=CARTESIAN_POINT('Ctrl Pts',(-40.0621906903527,10.61999998,-88.0176641176432));
#139780=CARTESIAN_POINT('Ctrl Pts',(-40.0324904304423,10.61999998,-88.0980242245577));
#139781=CARTESIAN_POINT('Ctrl Pts',(-39.9448659684135,10.61999998,-88.3351100668433));
#139782=CARTESIAN_POINT('Ctrl Pts',(-39.8685902579997,10.61999998,-88.5761404610461));
#139783=CARTESIAN_POINT('Ctrl Pts',(-39.8033297324296,10.61999998,-88.8189034289914));
#139784=CARTESIAN_POINT('Ctrl Pts',(-39.779079208429,10.61999998,-88.9091130791463));
#139785=CARTESIAN_POINT('Ctrl Pts',(-39.7563491787977,10.61999998,-88.9995618473627));
#139786=CARTESIAN_POINT('Ctrl Pts',(-39.735120734996,10.61999998,-89.090136059728));
#139787=CARTESIAN_POINT('Ctrl Pts',(-39.6384824206275,10.61999998,-89.5024573438502));
#139788=CARTESIAN_POINT('Ctrl Pts',(-39.5716278198207,10.61999998,-89.9196108763344));
#139789=CARTESIAN_POINT('Ctrl Pts',(-39.5345653063048,10.61999998,-90.3415980465025));
#139790=CARTESIAN_POINT('Ctrl Pts',(-39.5115257817286,10.61999998,-90.6039219650835));
#139791=CARTESIAN_POINT('Ctrl Pts',(-39.500000000001,10.61999998,-90.8681139415185));
#139792=CARTESIAN_POINT('Ctrl Pts',(-39.5,10.61999998,-91.1341759094044));
#139793=CARTESIAN_POINT('Ctrl Pts',(-54.0201152391274,10.61999998,-61.0621827299711));
#139794=CARTESIAN_POINT('Ctrl Pts',(-51.8036107556176,10.61999998,-65.4330353431782));
#139795=CARTESIAN_POINT('Ctrl Pts',(-49.570749196272,10.61999998,-69.7953845096745));
#139796=CARTESIAN_POINT('Ctrl Pts',(-47.313790090977,10.61999998,-74.1452062415669));
#139797=CARTESIAN_POINT('Ctrl Pts',(-45.056830985682,10.61999998,-78.4950279734592));
#139798=CARTESIAN_POINT('Ctrl Pts',(-42.7760635123042,10.61999998,-82.8324726037656));
#139799=CARTESIAN_POINT('Ctrl Pts',(-40.4577925858907,10.61999998,-87.1504205576762));
#139800=CARTESIAN_POINT('',(-59.5,10.61999998,-58.24995));
#139801=CARTESIAN_POINT('Origin',(-57.,10.61999998,-58.24995));
#139802=CARTESIAN_POINT('',(-59.5,10.61999998,-174.34995));
#139803=CARTESIAN_POINT('',(-59.5,10.61999998,-58.24995));
#139804=CARTESIAN_POINT('',(-57.,10.61999998,-176.84995));
#139805=CARTESIAN_POINT('Origin',(-57.,10.61999998,-174.34995));
#139806=CARTESIAN_POINT('',(-54.2951871140408,10.61999998,-176.84995));
#139807=CARTESIAN_POINT('',(83.2809572255632,10.6199999800001,-176.84995));
#139808=CARTESIAN_POINT('',(-54.2951871140408,10.61999998,-176.84995));
#139809=CARTESIAN_POINT('Origin',(0.,-12.9675000200281,-60.64995));
#139810=CARTESIAN_POINT('',(-39.4379155619868,-56.882767417621,-60.64995));
#139811=CARTESIAN_POINT('',(-39.4999994911539,-56.8280450701514,-60.6499500000002));
#139812=CARTESIAN_POINT('Ctrl Pts',(-39.4379155619868,-56.882767417621,
-60.64995));
#139813=CARTESIAN_POINT('Ctrl Pts',(-39.4584539679692,-56.8643229911399,
-60.64995));
#139814=CARTESIAN_POINT('Ctrl Pts',(-39.4791489724441,-56.8460828416128,
-60.64995));
#139815=CARTESIAN_POINT('Ctrl Pts',(-39.4999988314732,-56.8280445593217,
-60.64995));
#139816=CARTESIAN_POINT('',(-33.85,-61.3211699373828,-60.64995));
#139817=CARTESIAN_POINT('Origin',(0.,-12.9675000200281,-60.64995));
#139818=CARTESIAN_POINT('',(-33.85,-12.9675000200281,-60.64995));
#139819=CARTESIAN_POINT('',(-39.5,-12.9675000200281,-60.64995));
#139820=CARTESIAN_POINT('Ctrl Pts',(-39.4564221286262,-64.6472412200127,
-59.64995));
#139821=CARTESIAN_POINT('Ctrl Pts',(-39.9999999999999,-64.599684318524,
-59.64995));
#139822=CARTESIAN_POINT('Ctrl Pts',(-40.,-65.1453385690586,-59.64995));
#139823=CARTESIAN_POINT('Ctrl Pts',(-39.4564221286269,-64.6472412200127,
-59.7808732880376));
#139824=CARTESIAN_POINT('Ctrl Pts',(-39.9999999999999,-64.5996843185171,
-59.7746029379318));
#139825=CARTESIAN_POINT('Ctrl Pts',(-40.,-65.1453385690423,-59.8463349320561));
#139826=CARTESIAN_POINT('Ctrl Pts',(-39.4575563441365,-64.6210152418146,
-59.9116978933072));
#139827=CARTESIAN_POINT('Ctrl Pts',(-40.,-64.5762635801886,-59.898971233264));
#139828=CARTESIAN_POINT('Ctrl Pts',(-40.,-65.1061484482599,-60.0425718399612));
#139829=CARTESIAN_POINT('Ctrl Pts',(-39.4619222489981,-64.5200642984147,
-60.153568971423));
#139830=CARTESIAN_POINT('Ctrl Pts',(-39.9999999999999,-64.4844350369598,
-60.1322291512609));
#139831=CARTESIAN_POINT('Ctrl Pts',(-40.,-64.9552949839326,-60.4053784571341));
#139832=CARTESIAN_POINT('Ctrl Pts',(-39.4651522214972,-64.4453790312801,
-60.2644967268053));
#139833=CARTESIAN_POINT('Ctrl Pts',(-39.9999999999999,-64.4163683849594,
-60.2406767152616));
#139834=CARTESIAN_POINT('Ctrl Pts',(-40.,-64.8436909621967,-60.5717700902076));
#139835=CARTESIAN_POINT('Ctrl Pts',(-39.4732193617865,-64.2588460104538,
-60.4496168355678));
#139836=CARTESIAN_POINT('Ctrl Pts',(-39.9999999999999,-64.2423415370877,
-60.4261994932778));
#139837=CARTESIAN_POINT('Ctrl Pts',(-40.,-64.5649501059399,-60.8494502533521));
#139838=CARTESIAN_POINT('Ctrl Pts',(-39.4780533572402,-64.1470716093135,
-60.5237363920406));
#139839=CARTESIAN_POINT('Ctrl Pts',(-39.9999999999993,-64.1369109528056,
-60.5031527166045));
#139840=CARTESIAN_POINT('Ctrl Pts',(-40.,-64.3979228839314,-60.9606295880612));
#139841=CARTESIAN_POINT('Ctrl Pts',(-39.4885935839748,-63.9033544725257,
-60.623922672982));
#139842=CARTESIAN_POINT('Ctrl Pts',(-40.0000000000006,-63.9016439800941,
-60.6120353079401));
#139843=CARTESIAN_POINT('Ctrl Pts',(-40.,-64.0337304042775,-61.1109090094727));
#139844=CARTESIAN_POINT('Ctrl Pts',(-39.4942946417933,-63.771531360673,
-60.64995));
#139845=CARTESIAN_POINT('Ctrl Pts',(-39.9999999999999,-63.7723272342478,
-60.6442102195365));
#139846=CARTESIAN_POINT('Ctrl Pts',(-40.,-63.8367439033901,-61.149949999985));
#139847=CARTESIAN_POINT('Ctrl Pts',(-39.5,-63.6396088127436,-60.64995));
#139848=CARTESIAN_POINT('Ctrl Pts',(-39.9999999999999,-63.6396088127435,
-60.64995));
#139849=CARTESIAN_POINT('Ctrl Pts',(-40.,-63.6396088127436,-61.14995));
#139850=CARTESIAN_POINT('',(-40.,-63.6396088127436,-61.14995));
#139851=CARTESIAN_POINT('Origin',(-39.5,-63.6396088127436,-61.14995));
#139852=CARTESIAN_POINT('Ctrl Pts',(-40.,-65.1453385690586,-59.64995));
#139853=CARTESIAN_POINT('Ctrl Pts',(-40.,-65.1453385690423,-59.8463349320561));
#139854=CARTESIAN_POINT('Ctrl Pts',(-40.,-65.1061484482599,-60.0425718399612));
#139855=CARTESIAN_POINT('Ctrl Pts',(-40.,-64.9552949839326,-60.4053784571341));
#139856=CARTESIAN_POINT('Ctrl Pts',(-40.,-64.8436909621967,-60.5717700902076));
#139857=CARTESIAN_POINT('Ctrl Pts',(-40.,-64.5649501059399,-60.8494502533521));
#139858=CARTESIAN_POINT('Ctrl Pts',(-40.,-64.3979228839314,-60.9606295880612));
#139859=CARTESIAN_POINT('Ctrl Pts',(-40.,-64.0337304042775,-61.1109090094727));
#139860=CARTESIAN_POINT('Ctrl Pts',(-40.,-63.8367439033901,-61.149949999985));
#139861=CARTESIAN_POINT('Ctrl Pts',(-40.,-63.6396088127436,-61.14995));
#139862=CARTESIAN_POINT('Ctrl Pts',(-33.85,-64.133919761665,-60.64995));
#139863=CARTESIAN_POINT('Ctrl Pts',(-33.35,-64.1339197616649,-60.64995));
#139864=CARTESIAN_POINT('Ctrl Pts',(-33.35,-64.133919761665,-61.14995));
#139865=CARTESIAN_POINT('Ctrl Pts',(-33.8442946417933,-64.2658423095942,
-60.64995));
#139866=CARTESIAN_POINT('Ctrl Pts',(-33.35,-64.265066231498,-60.6556217969808));
#139867=CARTESIAN_POINT('Ctrl Pts',(-33.35,-64.3310548523114,-61.149949999985));
#139868=CARTESIAN_POINT('Ctrl Pts',(-33.8385935839748,-64.3976654214474,
-60.6239226729819));
#139869=CARTESIAN_POINT('Ctrl Pts',(-33.3499999999993,-64.399347719172,
-60.6353187454038));
#139870=CARTESIAN_POINT('Ctrl Pts',(-33.35,-64.5280413531989,-61.1109090094727));
#139871=CARTESIAN_POINT('Ctrl Pts',(-33.8280533572402,-64.6413825582346,
-60.5237363920407));
#139872=CARTESIAN_POINT('Ctrl Pts',(-33.3500000000007,-64.6507229380173,
-60.5426326522465));
#139873=CARTESIAN_POINT('Ctrl Pts',(-33.35,-64.8922338328527,-60.9606295880612));
#139874=CARTESIAN_POINT('Ctrl Pts',(-33.8232193617858,-64.7531569593752,
-60.4496168355678));
#139875=CARTESIAN_POINT('Ctrl Pts',(-33.35,-64.7680300213717,-60.4706504746468));
#139876=CARTESIAN_POINT('Ctrl Pts',(-33.35,-65.0592610548614,-60.849450253352));
#139877=CARTESIAN_POINT('Ctrl Pts',(-33.8151522214979,-64.9396899802014,
-60.2644967268053));
#139878=CARTESIAN_POINT('Ctrl Pts',(-33.35,-64.9649606354368,-60.2852157712117));
#139879=CARTESIAN_POINT('Ctrl Pts',(-33.35,-65.338001911118,-60.5717700902076));
#139880=CARTESIAN_POINT('Ctrl Pts',(-33.8119222489988,-65.0143752473362,
-60.1535689714224));
#139881=CARTESIAN_POINT('Ctrl Pts',(-33.35,-65.0449787669832,-60.1718710142623));
#139882=CARTESIAN_POINT('Ctrl Pts',(-33.35,-65.4496059328539,-60.4053784571335));
#139883=CARTESIAN_POINT('Ctrl Pts',(-33.8075563441358,-65.1153261907357,
-59.9116978933078));
#139884=CARTESIAN_POINT('Ctrl Pts',(-33.35,-65.1530905830856,-59.9224177216081));
#139885=CARTESIAN_POINT('Ctrl Pts',(-33.35,-65.6004593971813,-60.0425718399618));
#139886=CARTESIAN_POINT('Ctrl Pts',(-33.8064221286289,-65.1415521689339,
-59.7808732880372));
#139887=CARTESIAN_POINT('Ctrl Pts',(-33.35,-65.1814839309564,-59.7861314644984));
#139888=CARTESIAN_POINT('Ctrl Pts',(-33.35,-65.6396495179636,-59.8463349320557));
#139889=CARTESIAN_POINT('Ctrl Pts',(-33.8064221286261,-65.1415521689341,
-59.64995));
#139890=CARTESIAN_POINT('Ctrl Pts',(-33.3499999999999,-65.1814839309712,
-59.64995));
#139891=CARTESIAN_POINT('Ctrl Pts',(-33.35,-65.63964951798,-59.64995));
#139892=CARTESIAN_POINT('',(-33.35,-64.133919761665,-61.14995));
#139893=CARTESIAN_POINT('Origin',(-33.85,-64.133919761665,-61.14995));
#139894=CARTESIAN_POINT('Ctrl Pts',(-33.35,-64.133919761665,-61.14995));
#139895=CARTESIAN_POINT('Ctrl Pts',(-33.35,-64.3310548523114,-61.149949999985));
#139896=CARTESIAN_POINT('Ctrl Pts',(-33.35,-64.5280413531989,-61.1109090094727));
#139897=CARTESIAN_POINT('Ctrl Pts',(-33.35,-64.8922338328527,-60.9606295880612));
#139898=CARTESIAN_POINT('Ctrl Pts',(-33.35,-65.0592610548614,-60.849450253352));
#139899=CARTESIAN_POINT('Ctrl Pts',(-33.35,-65.338001911118,-60.5717700902076));
#139900=CARTESIAN_POINT('Ctrl Pts',(-33.35,-65.4496059328539,-60.4053784571335));
#139901=CARTESIAN_POINT('Ctrl Pts',(-33.35,-65.6004593971813,-60.0425718399618));
#139902=CARTESIAN_POINT('Ctrl Pts',(-33.35,-65.6396495179636,-59.8463349320557));
#139903=CARTESIAN_POINT('Ctrl Pts',(-33.35,-65.63964951798,-59.64995));
#139904=CARTESIAN_POINT('Origin',(-40.,67.7009572055632,-55.24995));
#139905=CARTESIAN_POINT('',(-40.,-62.6133861954129,-171.14995));
#139906=CARTESIAN_POINT('',(-40.,-64.1281275541908,-172.64995));
#139907=CARTESIAN_POINT('Ctrl Pts',(-40.,-62.6133861954129,-171.14995));
#139908=CARTESIAN_POINT('Ctrl Pts',(-40.,-62.8117011147884,-171.149950000016));
#139909=CARTESIAN_POINT('Ctrl Pts',(-40.,-63.0098665547682,-171.18899099047));
#139910=CARTESIAN_POINT('Ctrl Pts',(-40.,-63.3762386807026,-171.339270411997));
#139911=CARTESIAN_POINT('Ctrl Pts',(-40.,-63.5442655393439,-171.450449746589));
#139912=CARTESIAN_POINT('Ctrl Pts',(-40.,-63.8246746245531,-171.728129909852));
#139913=CARTESIAN_POINT('Ctrl Pts',(-40.,-63.9369465821947,-171.894521542842));
#139914=CARTESIAN_POINT('Ctrl Pts',(-40.,-64.0887028854776,-172.257328160063));
#139915=CARTESIAN_POINT('Ctrl Pts',(-40.,-64.1281275541786,-172.453565067926));
#139916=CARTESIAN_POINT('Ctrl Pts',(-40.,-64.1281275541908,-172.64995));
#139917=CARTESIAN_POINT('',(-40.,-56.978215522411,-171.14995));
#139918=CARTESIAN_POINT('',(-40.,-62.5431157780617,-171.14995));
#139919=CARTESIAN_POINT('',(-40.,-56.7758867300388,-171.126786878085));
#139920=CARTESIAN_POINT('Ctrl Pts',(-40.,-56.7758867300388,-171.126786878085));
#139921=CARTESIAN_POINT('Ctrl Pts',(-40.,-56.8424288281835,-171.142376649979));
#139922=CARTESIAN_POINT('Ctrl Pts',(-40.,-56.909888666977,-171.14995));
#139923=CARTESIAN_POINT('Ctrl Pts',(-40.,-56.978215522411,-171.14995));
#139924=CARTESIAN_POINT('',(-40.,-56.3715344108516,-170.85018387548));
#139925=CARTESIAN_POINT('Ctrl Pts',(-40.,-56.3715344108516,-170.85018387548));
#139926=CARTESIAN_POINT('Ctrl Pts',(-40.,-56.3837583326098,-170.871947332769));
#139927=CARTESIAN_POINT('Ctrl Pts',(-40.,-56.3977040563913,-170.892479579619));
#139928=CARTESIAN_POINT('Ctrl Pts',(-39.9999999999999,-56.4130583083895,
-170.911803741317));
#139929=CARTESIAN_POINT('Ctrl Pts',(-39.9999999999997,-56.4292409786976,
-170.93217051254));
#139930=CARTESIAN_POINT('Ctrl Pts',(-39.9999999999994,-56.4469891868559,
-170.951195798845));
#139931=CARTESIAN_POINT('Ctrl Pts',(-39.9999999999991,-56.4659895184401,
-170.968879578563));
#139932=CARTESIAN_POINT('Ctrl Pts',(-39.9999999999989,-56.4862759122404,
-170.987760307968));
#139933=CARTESIAN_POINT('Ctrl Pts',(-39.9999999999988,-56.5079910115924,
-171.00511257564));
#139934=CARTESIAN_POINT('Ctrl Pts',(-39.9999999999991,-56.5307948409902,
-171.020896071165));
#139935=CARTESIAN_POINT('Ctrl Pts',(-39.9999999999992,-56.5352406042463,
-171.023973172086));
#139936=CARTESIAN_POINT('Ctrl Pts',(-39.9999999999993,-56.5397278285604,
-171.026990509393));
#139937=CARTESIAN_POINT('Ctrl Pts',(-39.9999999999994,-56.5442540887154,
-171.029947579459));
#139938=CARTESIAN_POINT('Ctrl Pts',(-39.9999999999994,-56.5444049748233,
-171.030046155497));
#139939=CARTESIAN_POINT('Ctrl Pts',(-39.9999999999994,-56.5445558983641,
-171.030144660686));
#139940=CARTESIAN_POINT('Ctrl Pts',(-39.9999999999994,-56.5447068592425,
-171.030243095025));
#139941=CARTESIAN_POINT('Ctrl Pts',(-39.9999999999998,-56.5677583970532,
-171.045273895852));
#139942=CARTESIAN_POINT('Ctrl Pts',(-39.9999999999999,-56.5918056322567,
-171.058759052615));
#139943=CARTESIAN_POINT('Ctrl Pts',(-39.9999999999999,-56.6166148891246,
-171.070798762234));
#139944=CARTESIAN_POINT('Ctrl Pts',(-40.,-56.6425070267785,-171.083363984176));
#139945=CARTESIAN_POINT('Ctrl Pts',(-40.,-56.6692310020628,-171.094354961296));
#139946=CARTESIAN_POINT('Ctrl Pts',(-40.,-56.6965412231962,-171.103832593434));
#139947=CARTESIAN_POINT('Ctrl Pts',(-40.,-56.7225306079871,-171.112851847704));
#139948=CARTESIAN_POINT('Ctrl Pts',(-40.,-56.7490526547635,-171.120500083882));
#139949=CARTESIAN_POINT('Ctrl Pts',(-40.,-56.7758867300388,-171.126786878085));
#139950=CARTESIAN_POINT('',(-40.,-55.08000002,-165.390538702986));
#139951=CARTESIAN_POINT('Ctrl Pts',(-40.,-55.08000002,-165.390538702986));
#139952=CARTESIAN_POINT('Ctrl Pts',(-40.,-55.08000002,-165.865206657822));
#139953=CARTESIAN_POINT('Ctrl Pts',(-40.,-55.1054794225748,-166.33732512172));
#139954=CARTESIAN_POINT('Ctrl Pts',(-40.,-55.1564354838473,-166.806894369245));
#139955=CARTESIAN_POINT('Ctrl Pts',(-40.,-55.2073915451197,-167.27646361677));
#139956=CARTESIAN_POINT('Ctrl Pts',(-40.,-55.2841712278673,-167.745175405874));
#139957=CARTESIAN_POINT('Ctrl Pts',(-40.,-55.3883950832632,-168.207118124506));
#139958=CARTESIAN_POINT('Ctrl Pts',(-40.,-55.4926189386592,-168.669060843138));
#139959=CARTESIAN_POINT('Ctrl Pts',(-40.,-55.6233617621228,-169.121472747749));
#139960=CARTESIAN_POINT('Ctrl Pts',(-40.,-55.7848473238897,-169.562835831867));
#139961=CARTESIAN_POINT('Ctrl Pts',(-40.,-55.9143897222723,-169.916893692202));
#139962=CARTESIAN_POINT('Ctrl Pts',(-40.,-56.0634514911903,-170.263936360591));
#139963=CARTESIAN_POINT('Ctrl Pts',(-40.,-56.2378305482492,-170.601880104106));
#139964=CARTESIAN_POINT('Ctrl Pts',(-40.,-56.2808297421808,-170.685211834478));
#139965=CARTESIAN_POINT('Ctrl Pts',(-40.,-56.3253685536862,-170.767990232518));
#139966=CARTESIAN_POINT('Ctrl Pts',(-40.,-56.3715344108516,-170.85018387548));
#139967=CARTESIAN_POINT('',(-40.,-55.08000002,-66.6681042685293));
#139968=CARTESIAN_POINT('',(-40.,-55.08000002,-166.086292363451));
#139969=CARTESIAN_POINT('',(-40.,-56.2369767507657,-61.4585861992193));
#139970=CARTESIAN_POINT('Ctrl Pts',(-40.,-56.2369767507657,-61.4585861992193));
#139971=CARTESIAN_POINT('Ctrl Pts',(-40.,-56.0300621110256,-61.860218211459));
#139972=CARTESIAN_POINT('Ctrl Pts',(-40.,-55.8576823937473,-62.2755058381188));
#139973=CARTESIAN_POINT('Ctrl Pts',(-40.,-55.7121267698271,-62.7014001044593));
#139974=CARTESIAN_POINT('Ctrl Pts',(-40.,-55.566571145907,-63.1272943707998));
#139975=CARTESIAN_POINT('Ctrl Pts',(-40.,-55.4484096188021,-63.563870007102));
#139976=CARTESIAN_POINT('Ctrl Pts',(-40.,-55.355528959088,-64.0016972473019));
#139977=CARTESIAN_POINT('Ctrl Pts',(-40.,-55.2432744366403,-64.5308503337945));
#139978=CARTESIAN_POINT('Ctrl Pts',(-40.,-55.1660815895365,-65.0649117752177));
#139979=CARTESIAN_POINT('Ctrl Pts',(-40.,-55.1225595401112,-65.6036868919965));
#139980=CARTESIAN_POINT('Ctrl Pts',(-40.,-55.0940603190416,-65.9564890086839));
#139981=CARTESIAN_POINT('Ctrl Pts',(-40.,-55.0800000199998,-66.3113124768414));
#139982=CARTESIAN_POINT('Ctrl Pts',(-40.,-55.08000002,-66.6681042685293));
#139983=CARTESIAN_POINT('',(-40.,-56.8280459100727,-61.14995));
#139984=CARTESIAN_POINT('Ctrl Pts',(-40.,-56.8280459100727,-61.14995));
#139985=CARTESIAN_POINT('Ctrl Pts',(-40.,-56.777525746988,-61.1499499958728));
#139986=CARTESIAN_POINT('Ctrl Pts',(-40.,-56.7268325166736,-61.15437366761));
#139987=CARTESIAN_POINT('Ctrl Pts',(-40.,-56.6774814901222,-61.1633382145165));
#139988=CARTESIAN_POINT('Ctrl Pts',(-40.,-56.6695344165963,-61.1647817896226));
#139989=CARTESIAN_POINT('Ctrl Pts',(-40.,-56.6616221088453,-61.1663432172135));
#139990=CARTESIAN_POINT('Ctrl Pts',(-40.,-56.6537508667182,-61.1680231060305));
#139991=CARTESIAN_POINT('Ctrl Pts',(-40.,-56.6068413991694,-61.1780345741923));
#139992=CARTESIAN_POINT('Ctrl Pts',(-40.,-56.5611509800557,-61.1921536886353));
#139993=CARTESIAN_POINT('Ctrl Pts',(-40.,-56.5168370445324,-61.2111466189146));
#139994=CARTESIAN_POINT('Ctrl Pts',(-40.,-56.5074712817997,-61.2151607800694));
#139995=CARTESIAN_POINT('Ctrl Pts',(-40.,-56.4981670562375,-61.2193928254494));
#139996=CARTESIAN_POINT('Ctrl Pts',(-40.,-56.4889259423713,-61.2238502921498));
#139997=CARTESIAN_POINT('Ctrl Pts',(-40.,-56.4359851254178,-61.2493863835866));
#139998=CARTESIAN_POINT('Ctrl Pts',(-40.,-56.3871673636495,-61.2813158980448));
#139999=CARTESIAN_POINT('Ctrl Pts',(-40.,-56.3436555786936,-61.3209915546623));
#140000=CARTESIAN_POINT('Ctrl Pts',(-40.,-56.3001590827628,-61.3606532701805));
#140001=CARTESIAN_POINT('Ctrl Pts',(-40.,-56.2640024859216,-61.4061278501816));
#140002=CARTESIAN_POINT('Ctrl Pts',(-40.,-56.2369767507657,-61.4585861992193));
#140003=CARTESIAN_POINT('',(-40.,67.7009572055632,-61.14995));
#140004=CARTESIAN_POINT('',(-40.,-70.08000002,-55.74995));
#140005=CARTESIAN_POINT('',(-40.,67.7009572055632,-55.74995));
#140006=CARTESIAN_POINT('',(-40.,-72.58000002,-58.24995));
#140007=CARTESIAN_POINT('Origin',(-40.,-70.08000002,-58.24995));
#140008=CARTESIAN_POINT('',(-40.,-72.58000002,-174.34995));
#140009=CARTESIAN_POINT('',(-40.,-72.58000002,-58.24995));
#140010=CARTESIAN_POINT('',(-40.,-70.08000002,-176.84995));
#140011=CARTESIAN_POINT('Origin',(-40.,-70.08000002,-174.34995));
#140012=CARTESIAN_POINT('',(-40.,-64.1281275541909,-176.84995));
#140013=CARTESIAN_POINT('',(-40.,67.7009572055632,-176.84995));
#140014=CARTESIAN_POINT('',(-40.,-64.1281275541909,-55.24995));
#140015=CARTESIAN_POINT('Origin',(-40.5,-73.08000002,-55.74995));
#140016=CARTESIAN_POINT('',(-40.5,-70.08000002,-55.24995));
#140017=CARTESIAN_POINT('',(-40.5,-73.08000002,-55.24995));
#140018=CARTESIAN_POINT('Origin',(-40.5,-70.08000002,-55.74995));
#140019=CARTESIAN_POINT('Origin',(-41.5,-73.08000002,-55.24995));
#140020=CARTESIAN_POINT('',(-41.,-70.08000002,-55.24995));
#140021=CARTESIAN_POINT('',(-41.,-73.08000002,-55.24995));
#140022=CARTESIAN_POINT('',(-41.5,-70.08000002,-55.24995));
#140023=CARTESIAN_POINT('Origin',(-41.,-73.08000002,-55.74995));
#140024=CARTESIAN_POINT('',(-41.5,-70.08000002,-55.74995));
#140025=CARTESIAN_POINT('',(-41.5,-73.08000002,-55.74995));
#140026=CARTESIAN_POINT('Origin',(-41.,-70.08000002,-55.74995));
#140027=CARTESIAN_POINT('Origin',(-41.5,-73.08000002,-177.34995));
#140028=CARTESIAN_POINT('',(-41.5,-58.6035812240168,-171.14995));
#140029=CARTESIAN_POINT('',(-41.5,-56.3473237326807,-171.14995));
#140030=CARTESIAN_POINT('Ctrl Pts',(-41.5,-58.6035812240168,-171.14995));
#140031=CARTESIAN_POINT('Ctrl Pts',(-41.5,-58.4156574039305,-171.149950044596));
#140032=CARTESIAN_POINT('Ctrl Pts',(-41.4999999999992,-58.2278101348557,
-171.167358426711));
#140033=CARTESIAN_POINT('Ctrl Pts',(-41.5000000000009,-58.0399262281501,
-171.183208448531));
#140034=CARTESIAN_POINT('Ctrl Pts',(-41.5000000000009,-58.0397839854562,
-171.183220448228));
#140035=CARTESIAN_POINT('Ctrl Pts',(-41.5000000000009,-58.039641742701,
-171.183232446501));
#140036=CARTESIAN_POINT('Ctrl Pts',(-41.5000000000009,-58.0394994998845,
-171.183244443348));
#140037=CARTESIAN_POINT('Ctrl Pts',(-41.5000000000023,-57.8789705149886,
-171.196783556842));
#140038=CARTESIAN_POINT('Ctrl Pts',(-41.4999999999993,-57.7184422672608,
-171.208492413784));
#140039=CARTESIAN_POINT('Ctrl Pts',(-41.500000000002,-57.5579169091739,
-171.211623701818));
#140040=CARTESIAN_POINT('Ctrl Pts',(-41.5000000000025,-57.5306624002507,
-171.212155341919));
#140041=CARTESIAN_POINT('Ctrl Pts',(-41.5000000000032,-57.5034079726239,
-171.212439843791));
#140042=CARTESIAN_POINT('Ctrl Pts',(-41.5000000000045,-57.4761536342535,
-171.212444366369));
#140043=CARTESIAN_POINT('Ctrl Pts',(-41.5000000000045,-57.4759114394356,
-171.212444406558));
#140044=CARTESIAN_POINT('Ctrl Pts',(-41.5000000000045,-57.4756692446243,
-171.212444424596));
#140045=CARTESIAN_POINT('Ctrl Pts',(-41.5000000000045,-57.4754270498201,
-171.212444420506));
#140046=CARTESIAN_POINT('Ctrl Pts',(-41.5000000000123,-57.314176726691,
-171.21244169735));
#140047=CARTESIAN_POINT('Ctrl Pts',(-41.5000000000007,-57.1529297994809,
-171.202628065338));
#140048=CARTESIAN_POINT('Ctrl Pts',(-41.5000000000001,-56.9916840158814,
-171.189830777412));
#140049=CARTESIAN_POINT('Ctrl Pts',(-41.5,-56.9650429028844,-171.187716402784));
#140050=CARTESIAN_POINT('Ctrl Pts',(-41.5,-56.9384018138948,-171.185520466727));
#140051=CARTESIAN_POINT('Ctrl Pts',(-41.5,-56.9117607329796,-171.183273657174));
#140052=CARTESIAN_POINT('Ctrl Pts',(-41.5,-56.9116320467988,-171.18326280426));
#140053=CARTESIAN_POINT('Ctrl Pts',(-41.5,-56.9115033606235,-171.183251950612));
#140054=CARTESIAN_POINT('Ctrl Pts',(-41.5,-56.9113746744539,-171.183241096235));
#140055=CARTESIAN_POINT('Ctrl Pts',(-41.5000000000001,-56.7724125203318,
-171.171519963661));
#140056=CARTESIAN_POINT('Ctrl Pts',(-41.5,-56.6334506983164,-171.158942972401));
#140057=CARTESIAN_POINT('Ctrl Pts',(-41.5,-56.494486471775,-171.153174108112));
#140058=CARTESIAN_POINT('Ctrl Pts',(-41.5,-56.4454325541915,-171.151137717881));
#140059=CARTESIAN_POINT('Ctrl Pts',(-41.5,-56.3963783401894,-171.149950012104));
#140060=CARTESIAN_POINT('Ctrl Pts',(-41.5,-56.3473237326807,-171.14995));
#140061=CARTESIAN_POINT('',(-41.5,-62.2620341086569,-171.14995));
#140062=CARTESIAN_POINT('',(-41.5,-55.58000002,-171.14995));
#140063=CARTESIAN_POINT('',(-41.5,-63.7767754674349,-172.64995));
#140064=CARTESIAN_POINT('Ctrl Pts',(-41.5,-63.7767754674349,-172.64995));
#140065=CARTESIAN_POINT('Ctrl Pts',(-41.5,-63.7767754674226,-172.453565067926));
#140066=CARTESIAN_POINT('Ctrl Pts',(-41.5,-63.7373507987217,-172.257328160063));
#140067=CARTESIAN_POINT('Ctrl Pts',(-41.5,-63.5855944954388,-171.894521542842));
#140068=CARTESIAN_POINT('Ctrl Pts',(-41.5,-63.4733225377971,-171.728129909852));
#140069=CARTESIAN_POINT('Ctrl Pts',(-41.5,-63.192913452588,-171.450449746589));
#140070=CARTESIAN_POINT('Ctrl Pts',(-41.5,-63.0248865939453,-171.339270411997));
#140071=CARTESIAN_POINT('Ctrl Pts',(-41.5,-62.6585144680136,-171.18899099047));
#140072=CARTESIAN_POINT('Ctrl Pts',(-41.5,-62.4603490280314,-171.149950000016));
#140073=CARTESIAN_POINT('Ctrl Pts',(-41.5,-62.2620341086569,-171.14995));
#140074=CARTESIAN_POINT('',(-41.5,-63.7767754674349,-176.84995));
#140075=CARTESIAN_POINT('',(-41.5,-63.7767754674349,-177.34995));
#140076=CARTESIAN_POINT('',(-41.5,-70.08000002,-176.84995));
#140077=CARTESIAN_POINT('',(-41.5,-73.08000002,-176.84995));
#140078=CARTESIAN_POINT('',(-41.5,-72.58000002,-174.34995));
#140079=CARTESIAN_POINT('Origin',(-41.5,-70.08000002,-174.34995));
#140080=CARTESIAN_POINT('',(-41.5,-72.58000002,-58.24995));
#140081=CARTESIAN_POINT('',(-41.5,-72.58000002,-174.34995));
#140082=CARTESIAN_POINT('Origin',(-41.5,-70.08000002,-58.24995));
#140083=CARTESIAN_POINT('',(-41.5,-63.4208871539288,-61.14995));
#140084=CARTESIAN_POINT('Ctrl Pts',(-41.5,-63.4208871539288,-61.14995));
#140085=CARTESIAN_POINT('Ctrl Pts',(-41.5,-63.6180222445752,-61.149949999985));
#140086=CARTESIAN_POINT('Ctrl Pts',(-41.5,-63.8150087454628,-61.1109090094727));
#140087=CARTESIAN_POINT('Ctrl Pts',(-41.5,-64.1792012251166,-60.9606295880612));
#140088=CARTESIAN_POINT('Ctrl Pts',(-41.5,-64.3462284471252,-60.849450253352));
#140089=CARTESIAN_POINT('Ctrl Pts',(-41.5,-64.6249693033818,-60.5717700902076));
#140090=CARTESIAN_POINT('Ctrl Pts',(-41.5,-64.7365733251178,-60.4053784571342));
#140091=CARTESIAN_POINT('Ctrl Pts',(-41.5,-64.8874267894451,-60.0425718399611));
#140092=CARTESIAN_POINT('Ctrl Pts',(-41.5,-64.9266169102275,-59.8463349320562));
#140093=CARTESIAN_POINT('Ctrl Pts',(-41.5,-64.9266169102438,-59.64995));
#140094=CARTESIAN_POINT('',(-41.5,-58.6035812240174,-61.14995));
#140095=CARTESIAN_POINT('',(-41.5,-73.08000002,-61.14995));
#140096=CARTESIAN_POINT('',(-41.5,-56.3473237326805,-61.14995));
#140097=CARTESIAN_POINT('Ctrl Pts',(-41.5,-56.3473237326805,-61.14995));
#140098=CARTESIAN_POINT('Ctrl Pts',(-41.5,-56.4247882486865,-61.1499499808859));
#140099=CARTESIAN_POINT('Ctrl Pts',(-41.5,-56.5020743317105,-61.146992865599));
#140100=CARTESIAN_POINT('Ctrl Pts',(-41.5,-56.5792618257269,-61.1424262748502));
#140101=CARTESIAN_POINT('Ctrl Pts',(-41.5,-56.6823474618058,-61.1363274900916));
#140102=CARTESIAN_POINT('Ctrl Pts',(-41.5,-56.7852572696789,-61.1273561280416));
#140103=CARTESIAN_POINT('Ctrl Pts',(-41.5000000000002,-56.8881825068214,
-61.1186215077308));
#140104=CARTESIAN_POINT('Ctrl Pts',(-41.5000000000002,-56.8960417889417,
-61.1179545396757));
#140105=CARTESIAN_POINT('Ctrl Pts',(-41.5000000000002,-56.9039011612638,
-61.1172889307083));
#140106=CARTESIAN_POINT('Ctrl Pts',(-41.5000000000002,-56.9117607090172,
-61.1166260587005));
#140107=CARTESIAN_POINT('Ctrl Pts',(-41.5000000000002,-56.9118309970963,
-61.116620130624));
#140108=CARTESIAN_POINT('Ctrl Pts',(-41.5000000000002,-56.9119012851879,
-61.1166142029013));
#140109=CARTESIAN_POINT('Ctrl Pts',(-41.5000000000002,-56.9119715732919,
-61.1166082755328));
#140110=CARTESIAN_POINT('Ctrl Pts',(-41.5000000000007,-57.0997257526663,
-61.1007750386643));
#140111=CARTESIAN_POINT('Ctrl Pts',(-41.4999999999977,-57.2880101287523,
-61.0874286525006));
#140112=CARTESIAN_POINT('Ctrl Pts',(-41.5000000000023,-57.4761536341595,
-61.0874562423818));
#140113=CARTESIAN_POINT('Ctrl Pts',(-41.5000000000023,-57.476328431569,
-61.0874562680146));
#140114=CARTESIAN_POINT('Ctrl Pts',(-41.5000000000023,-57.4765032288573,
-61.087456305165));
#140115=CARTESIAN_POINT('Ctrl Pts',(-41.5000000000023,-57.4766780260241,
-61.0874563538243));
#140116=CARTESIAN_POINT('Ctrl Pts',(-41.500000000005,-57.5875579724858,
-61.0874872201067));
#140117=CARTESIAN_POINT('Ctrl Pts',(-41.5000000000027,-57.698214536846,
-61.0921466646789));
#140118=CARTESIAN_POINT('Ctrl Pts',(-41.5000000000012,-57.808755193549,
-61.099196348861));
#140119=CARTESIAN_POINT('Ctrl Pts',(-41.5000000000001,-57.8858564168486,
-61.1041134471534));
#140120=CARTESIAN_POINT('Ctrl Pts',(-41.5,-57.9629012529634,-61.1101948863673));
#140121=CARTESIAN_POINT('Ctrl Pts',(-41.5,-58.039926161923,-61.1166923365635));
#140122=CARTESIAN_POINT('Ctrl Pts',(-41.5,-58.0400259760022,-61.1167007563983));
#140123=CARTESIAN_POINT('Ctrl Pts',(-41.5,-58.0401257900677,-61.1167091766712));
#140124=CARTESIAN_POINT('Ctrl Pts',(-41.5,-58.0402256041196,-61.1167175973794));
#140125=CARTESIAN_POINT('Ctrl Pts',(-41.5000000000001,-58.1358345616333,
-61.1247835471793));
#140126=CARTESIAN_POINT('Ctrl Pts',(-41.5,-58.2314235934514,-61.1332503625508));
#140127=CARTESIAN_POINT('Ctrl Pts',(-41.5,-58.3271142909714,-61.1396237955236));
#140128=CARTESIAN_POINT('Ctrl Pts',(-41.5,-58.4115316341018,-61.145246372139));
#140129=CARTESIAN_POINT('Ctrl Pts',(-41.5,-58.4960281098014,-61.149241951551));
#140130=CARTESIAN_POINT('Ctrl Pts',(-41.5,-58.5806871719333,-61.1498651031254));
#140131=CARTESIAN_POINT('Ctrl Pts',(-41.5,-58.5883171817095,-61.149921265484));
#140132=CARTESIAN_POINT('Ctrl Pts',(-41.5,-58.5959485120575,-61.1499499981887));
#140133=CARTESIAN_POINT('Ctrl Pts',(-41.5,-58.6035812240174,-61.14995));
#140134=CARTESIAN_POINT('',(-41.5,-55.58000002,-61.14995));
#140135=CARTESIAN_POINT('',(-41.5,-73.08000002,-61.14995));
#140136=CARTESIAN_POINT('',(-41.5,-55.58000002,-171.14995));
#140137=CARTESIAN_POINT('',(-41.5,-55.58000002,-60.64995));
#140138=CARTESIAN_POINT('',(-41.5,-55.58000002,-171.14995));
#140139=CARTESIAN_POINT('Ctrl Pts',(-42.,-63.4208871539288,-60.64995));
#140140=CARTESIAN_POINT('Ctrl Pts',(-41.4999999999999,-63.4208871539288,
-60.64995));
#140141=CARTESIAN_POINT('Ctrl Pts',(-41.5,-63.4208871539288,-61.14995));
#140142=CARTESIAN_POINT('Ctrl Pts',(-41.9942946417934,-63.5528097018572,
-60.64995));
#140143=CARTESIAN_POINT('Ctrl Pts',(-41.5,-63.5520336237608,-60.6556217969809));
#140144=CARTESIAN_POINT('Ctrl Pts',(-41.5,-63.6180222445752,-61.149949999985));
#140145=CARTESIAN_POINT('Ctrl Pts',(-41.9885935839755,-63.6846328137124,
-60.6239226729814));
#140146=CARTESIAN_POINT('Ctrl Pts',(-41.4999999999993,-63.6863151114373,
-60.6353187454032));
#140147=CARTESIAN_POINT('Ctrl Pts',(-41.5,-63.8150087454628,-61.1109090094727));
#140148=CARTESIAN_POINT('Ctrl Pts',(-41.9780533572395,-63.9283499504973,
-60.5237363920413));
#140149=CARTESIAN_POINT('Ctrl Pts',(-41.5000000000007,-63.9376903302796,
-60.5426326522472));
#140150=CARTESIAN_POINT('Ctrl Pts',(-41.5,-64.1792012251166,-60.9606295880612));
#140151=CARTESIAN_POINT('Ctrl Pts',(-41.9732193617859,-64.0401243516391,
-60.4496168355678));
#140152=CARTESIAN_POINT('Ctrl Pts',(-41.5,-64.0549974136357,-60.4706504746468));
#140153=CARTESIAN_POINT('Ctrl Pts',(-41.5,-64.3462284471252,-60.849450253352));
#140154=CARTESIAN_POINT('Ctrl Pts',(-41.9651522214979,-64.2266573724653,
-60.2644967268053));
#140155=CARTESIAN_POINT('Ctrl Pts',(-41.4999999999999,-64.2519280277007,
-60.2852157712117));
#140156=CARTESIAN_POINT('Ctrl Pts',(-41.5,-64.6249693033818,-60.5717700902076));
#140157=CARTESIAN_POINT('Ctrl Pts',(-41.9619222489988,-64.3013426395998,
-60.153568971423));
#140158=CARTESIAN_POINT('Ctrl Pts',(-41.5,-64.3319461592471,-60.1718710142637));
#140159=CARTESIAN_POINT('Ctrl Pts',(-41.5,-64.7365733251178,-60.4053784571342));
#140160=CARTESIAN_POINT('Ctrl Pts',(-41.9575563441358,-64.4022935829999,
-59.9116978933072));
#140161=CARTESIAN_POINT('Ctrl Pts',(-41.5,-64.4400579753494,-59.9224177216068));
#140162=CARTESIAN_POINT('Ctrl Pts',(-41.5,-64.8874267894451,-60.0425718399611));
#140163=CARTESIAN_POINT('Ctrl Pts',(-41.9564221286289,-64.4285195611977,
-59.7808732880376));
#140164=CARTESIAN_POINT('Ctrl Pts',(-41.5,-64.4684513232201,-59.7861314644994));
#140165=CARTESIAN_POINT('Ctrl Pts',(-41.5,-64.9266169102275,-59.8463349320562));
#140166=CARTESIAN_POINT('Ctrl Pts',(-41.9564221286262,-64.428519561198,
-59.64995));
#140167=CARTESIAN_POINT('Ctrl Pts',(-41.5,-64.4684513232351,-59.64995));
#140168=CARTESIAN_POINT('Ctrl Pts',(-41.5,-64.9266169102438,-59.64995));
#140169=CARTESIAN_POINT('Origin',(-42.,-63.4208871539288,-61.14995));
#140170=CARTESIAN_POINT('Ctrl Pts',(-25.559825688233,-65.4594929016656,
-60.8818893816927));
#140171=CARTESIAN_POINT('Ctrl Pts',(-25.2,-65.5225267460509,-60.9659777046599));
#140172=CARTESIAN_POINT('Ctrl Pts',(-25.2,-65.7473676730038,-61.2659196908451));
#140173=CARTESIAN_POINT('Ctrl Pts',(-25.5689423412454,-65.58489046904,-60.7845618642934));
#140174=CARTESIAN_POINT('Ctrl Pts',(-25.2,-65.6598013792258,-60.8537298337023));
#140175=CARTESIAN_POINT('Ctrl Pts',(-25.2,-65.9366774304564,-61.1240102848084));
#140176=CARTESIAN_POINT('Ctrl Pts',(-25.5836282597575,-65.6869336598766,
-60.6533188274199));
#140177=CARTESIAN_POINT('Ctrl Pts',(-25.2,-65.7653321407853,-60.7026110037421));
#140178=CARTESIAN_POINT('Ctrl Pts',(-25.2,-66.0916524900825,-60.9336707597463));
#140179=CARTESIAN_POINT('Ctrl Pts',(-25.6175094928883,-65.8217787894205,
-60.3603674876955));
#140180=CARTESIAN_POINT('Ctrl Pts',(-25.2,-65.8913484330066,-60.3775874746364));
#140181=CARTESIAN_POINT('Ctrl Pts',(-25.2,-66.2983665260919,-60.5086792251106));
#140182=CARTESIAN_POINT('Ctrl Pts',(-25.6369719721911,-65.8562864448621,
-60.1960022731895));
#140183=CARTESIAN_POINT('Ctrl Pts',(-25.2,-65.9121534157352,-60.1989021139916));
#140184=CARTESIAN_POINT('Ctrl Pts',(-25.2,-66.3526821146748,-60.2701831868566));
#140185=CARTESIAN_POINT('Ctrl Pts',(-25.6564221286262,-65.8545847766702,
-60.0322609860583));
#140186=CARTESIAN_POINT('Ctrl Pts',(-25.2,-65.8945165387074,-60.0322609860583));
#140187=CARTESIAN_POINT('Ctrl Pts',(-25.2,-66.3526821257161,-60.0322609860583));
#140188=CARTESIAN_POINT('',(-25.2,-65.7473676730073,-61.2659196908498));
#140189=CARTESIAN_POINT('Origin',(-25.7,-65.7473676730073,-61.2659196908498));
#140190=CARTESIAN_POINT('Ctrl Pts',(-25.2,-65.7473676730038,-61.2659196908451));
#140191=CARTESIAN_POINT('Ctrl Pts',(-25.2,-65.7793674058565,-61.2419322158012));
#140192=CARTESIAN_POINT('Ctrl Pts',(-25.2,-65.8101247224078,-61.2167624788248));
#140193=CARTESIAN_POINT('Ctrl Pts',(-25.2,-65.8397093268158,-61.1904934725279));
#140194=CARTESIAN_POINT('Ctrl Pts',(-25.2,-65.8701731473597,-61.163443785378));
#140195=CARTESIAN_POINT('Ctrl Pts',(-25.2,-65.8993940496695,-61.1352280130908));
#140196=CARTESIAN_POINT('Ctrl Pts',(-25.2,-65.9274189899595,-61.105888948837));
#140197=CARTESIAN_POINT('Ctrl Pts',(-25.2,-65.953675127919,-61.0784016282334));
#140198=CARTESIAN_POINT('Ctrl Pts',(-25.2,-65.9788815373659,-61.0499274395304));
#140199=CARTESIAN_POINT('Ctrl Pts',(-25.2,-66.003048363658,-61.0204714365432));
#140200=CARTESIAN_POINT('Ctrl Pts',(-25.2,-66.0310884832222,-60.9862944272966));
#140201=CARTESIAN_POINT('Ctrl Pts',(-25.2,-66.0577887607432,-60.9507091443297));
#140202=CARTESIAN_POINT('Ctrl Pts',(-25.2,-66.0829136816528,-60.9139799086674));
#140203=CARTESIAN_POINT('Ctrl Pts',(-25.2,-66.1080535088014,-60.8772288821003));
#140204=CARTESIAN_POINT('Ctrl Pts',(-25.2,-66.1316155749469,-60.8393332860743));
#140205=CARTESIAN_POINT('Ctrl Pts',(-25.2,-66.1534043153279,-60.8005903814081));
#140206=CARTESIAN_POINT('Ctrl Pts',(-25.2,-66.1680937996861,-60.7744707764132));
#140207=CARTESIAN_POINT('Ctrl Pts',(-25.2,-66.1819781266407,-60.7479667213004));
#140208=CARTESIAN_POINT('Ctrl Pts',(-25.2,-66.1950095070847,-60.7211749919409));
#140209=CARTESIAN_POINT('Ctrl Pts',(-25.2,-66.2246788862505,-60.6601765443636));
#140210=CARTESIAN_POINT('Ctrl Pts',(-25.2,-66.2502610540319,-60.5971407841896));
#140211=CARTESIAN_POINT('Ctrl Pts',(-25.2,-66.2716923178953,-60.5326135007196));
#140212=CARTESIAN_POINT('Ctrl Pts',(-25.2,-66.2932651285445,-60.4676600347516));
#140213=CARTESIAN_POINT('Ctrl Pts',(-25.2,-66.3106323191261,-60.4011940591385));
#140214=CARTESIAN_POINT('Ctrl Pts',(-25.2,-66.3236799285786,-60.3337525435423));
#140215=CARTESIAN_POINT('Ctrl Pts',(-25.2,-66.3364083912035,-60.2679606593083));
#140216=CARTESIAN_POINT('Ctrl Pts',(-25.2,-66.345026048704,-60.2012392210405));
#140217=CARTESIAN_POINT('Ctrl Pts',(-25.2,-66.3493785138956,-60.1340856776664));
#140218=CARTESIAN_POINT('Ctrl Pts',(-25.2,-66.3515726828295,-60.1002321688644));
#140219=CARTESIAN_POINT('Ctrl Pts',(-25.2,-66.3526821241379,-60.0662689342246));
#140220=CARTESIAN_POINT('Ctrl Pts',(-25.2,-66.3526821257161,-60.0322609860583));
#140221=CARTESIAN_POINT('Origin',(-25.2,67.7009572055632,-55.24995));
#140222=CARTESIAN_POINT('',(-25.2,-70.08000002,-176.84995));
#140223=CARTESIAN_POINT('',(-25.2,-66.1031295107182,-176.84995));
#140224=CARTESIAN_POINT('',(-25.2,67.7009572055632,-176.84995));
#140225=CARTESIAN_POINT('',(-25.2,-72.58000002,-174.34995));
#140226=CARTESIAN_POINT('Origin',(-25.2,-70.08000002,-174.34995));
#140227=CARTESIAN_POINT('',(-25.2,-72.58000002,-58.24995));
#140228=CARTESIAN_POINT('',(-25.2,-72.58000002,-174.34995));
#140229=CARTESIAN_POINT('Origin',(-25.2,-70.08000002,-58.24995));
#140230=CARTESIAN_POINT('',(-25.2,-65.5994372375942,-61.4386408691297));
#140231=CARTESIAN_POINT('Origin',(-25.2,-66.2733246929871,-61.7660459272207));
#140232=CARTESIAN_POINT('',(-25.2,-56.0768896606488,-79.4153515046414));
#140233=CARTESIAN_POINT('Ctrl Pts',(-25.2,-56.0768896606488,-79.4153515046414));
#140234=CARTESIAN_POINT('Ctrl Pts',(-25.2,-59.3123551324919,-73.4555771707379));
#140235=CARTESIAN_POINT('Ctrl Pts',(-25.2,-62.4759494901776,-67.4577315724186));
#140236=CARTESIAN_POINT('Ctrl Pts',(-25.2,-65.5994372375941,-61.4386408691297));
#140237=CARTESIAN_POINT('',(-25.2,-55.08000002,-83.5456386250819));
#140238=CARTESIAN_POINT('Ctrl Pts',(-25.2,-55.08000002,-83.5456386250819));
#140239=CARTESIAN_POINT('Ctrl Pts',(-25.2,-55.08000002,-83.1859931739116));
#140240=CARTESIAN_POINT('Ctrl Pts',(-25.2,-55.1006621337637,-82.8281867002424));
#140241=CARTESIAN_POINT('Ctrl Pts',(-25.2,-55.1417030348395,-82.4721939873444));
#140242=CARTESIAN_POINT('Ctrl Pts',(-25.2,-55.1827439359154,-82.1162012744465));
#140243=CARTESIAN_POINT('Ctrl Pts',(-25.2,-55.2446154752335,-81.7605756924467));
#140244=CARTESIAN_POINT('Ctrl Pts',(-25.2,-55.3267103680732,-81.412917955686));
#140245=CARTESIAN_POINT('Ctrl Pts',(-25.2,-55.4088052609129,-81.0652602189252));
#140246=CARTESIAN_POINT('Ctrl Pts',(-25.2,-55.5103655940696,-80.7242806574902));
#140247=CARTESIAN_POINT('Ctrl Pts',(-25.2,-55.6343884585548,-80.3910074402699));
#140248=CARTESIAN_POINT('Ctrl Pts',(-25.2,-55.75841132304,-80.0577342230495));
#140249=CARTESIAN_POINT('Ctrl Pts',(-25.2,-55.9048956589413,-79.7321669507792));
#140250=CARTESIAN_POINT('Ctrl Pts',(-25.2,-56.0768896606488,-79.4153515046414));
#140251=CARTESIAN_POINT('',(-25.2,-55.08000002,-148.513004346424));
#140252=CARTESIAN_POINT('',(-25.2,-55.08000002,-84.0594740639255));
#140253=CARTESIAN_POINT('',(-25.2,-56.0768896606488,-152.643291466864));
#140254=CARTESIAN_POINT('Ctrl Pts',(-25.2,-56.0768896606487,-152.643291466864));
#140255=CARTESIAN_POINT('Ctrl Pts',(-25.2,-56.0149669290359,-152.529228896965));
#140256=CARTESIAN_POINT('Ctrl Pts',(-25.2,-55.9563289964362,-152.41374598058));
#140257=CARTESIAN_POINT('Ctrl Pts',(-25.2,-55.9007756544416,-152.296934067097));
#140258=CARTESIAN_POINT('Ctrl Pts',(-25.2,-55.8430042328458,-152.175458201578));
#140259=CARTESIAN_POINT('Ctrl Pts',(-25.2,-55.788568493397,-152.052544547971));
#140260=CARTESIAN_POINT('Ctrl Pts',(-25.2,-55.737292667624,-151.928266900594));
#140261=CARTESIAN_POINT('Ctrl Pts',(-25.2,-55.7009775154013,-151.840249562709));
#140262=CARTESIAN_POINT('Ctrl Pts',(-25.2,-55.6662483997962,-151.751547420779));
#140263=CARTESIAN_POINT('Ctrl Pts',(-25.2,-55.6330574644204,-151.662180878469));
#140264=CARTESIAN_POINT('Ctrl Pts',(-25.2,-55.5638026420096,-151.475712375937));
#140265=CARTESIAN_POINT('Ctrl Pts',(-25.2,-55.5013746560306,-151.2866750003));
#140266=CARTESIAN_POINT('Ctrl Pts',(-25.2,-55.445644045516,-151.096220906455));
#140267=CARTESIAN_POINT('Ctrl Pts',(-25.2,-55.400687777676,-150.942587110322));
#140268=CARTESIAN_POINT('Ctrl Pts',(-25.2,-55.3600885309565,-150.788032233726));
#140269=CARTESIAN_POINT('Ctrl Pts',(-25.2,-55.323754356376,-150.633166383806));
#140270=CARTESIAN_POINT('Ctrl Pts',(-25.2,-55.2248092846637,-150.21143635132));
#140271=CARTESIAN_POINT('Ctrl Pts',(-25.2,-55.1560866851002,-149.784875950083));
#140272=CARTESIAN_POINT('Ctrl Pts',(-25.2,-55.1174016248561,-149.353514705421));
#140273=CARTESIAN_POINT('Ctrl Pts',(-25.2,-55.0924544716303,-149.075339228934));
#140274=CARTESIAN_POINT('Ctrl Pts',(-25.2,-55.0800000200004,-148.795167064059));
#140275=CARTESIAN_POINT('Ctrl Pts',(-25.2,-55.08000002,-148.513004346424));
#140276=CARTESIAN_POINT('',(-25.2,-65.7246041881209,-170.861259130871));
#140277=CARTESIAN_POINT('Ctrl Pts',(-25.2,-65.7246041881209,-170.861259130871));
#140278=CARTESIAN_POINT('Ctrl Pts',(-25.2,-62.5605227754587,-164.761159036905));
#140279=CARTESIAN_POINT('Ctrl Pts',(-25.2,-59.3555847723563,-158.682695424483));
#140280=CARTESIAN_POINT('Ctrl Pts',(-25.2,-56.0768896606488,-152.643291466864));
#140281=CARTESIAN_POINT('',(-25.2,-65.7816577220592,-170.947457636992));
#140282=CARTESIAN_POINT('Ctrl Pts',(-25.2,-65.7816577220592,-170.947457636992));
#140283=CARTESIAN_POINT('Ctrl Pts',(-25.2,-65.759637326036,-170.920712146581));
#140284=CARTESIAN_POINT('Ctrl Pts',(-25.2,-65.7405592277015,-170.892019192244));
#140285=CARTESIAN_POINT('Ctrl Pts',(-25.2,-65.7246041881209,-170.861259130871));
#140286=CARTESIAN_POINT('',(-25.2,-66.1031295107175,-171.854014632589));
#140287=CARTESIAN_POINT('Ctrl Pts',(-25.2,-66.1031295107175,-171.854014632589));
#140288=CARTESIAN_POINT('Ctrl Pts',(-25.2,-66.1031295063964,-171.725572055906));
#140289=CARTESIAN_POINT('Ctrl Pts',(-25.2,-66.0871173562522,-171.599865253241));
#140290=CARTESIAN_POINT('Ctrl Pts',(-25.2,-66.0541497294316,-171.477055409759));
#140291=CARTESIAN_POINT('Ctrl Pts',(-25.2,-66.0447396524368,-171.442001322026));
#140292=CARTESIAN_POINT('Ctrl Pts',(-25.2,-66.0339478541515,-171.407183310008));
#140293=CARTESIAN_POINT('Ctrl Pts',(-25.2,-66.0217516132152,-171.372605255459));
#140294=CARTESIAN_POINT('Ctrl Pts',(-25.2,-65.9940406295851,-171.294040728194));
#140295=CARTESIAN_POINT('Ctrl Pts',(-25.2,-65.9598967243513,-171.219005811917));
#140296=CARTESIAN_POINT('Ctrl Pts',(-25.2,-65.9193893860812,-171.147550497268));
#140297=CARTESIAN_POINT('Ctrl Pts',(-25.2,-65.8796084720189,-171.077376601556));
#140298=CARTESIAN_POINT('Ctrl Pts',(-25.2,-65.8336900811277,-171.010655009755));
#140299=CARTESIAN_POINT('Ctrl Pts',(-25.2,-65.7816577220592,-170.947457636992));
#140300=CARTESIAN_POINT('',(-25.2,-66.1031295107182,-171.799329694116));
#140301=CARTESIAN_POINT('Origin',(0.,-12.9675000200281,-61.64995));
#140302=CARTESIAN_POINT('',(-31.1074520910898,-62.0598503138784,-61.2273317382593));
#140303=CARTESIAN_POINT('',(-25.5011648721215,-65.1922357602732,-61.2273317382593));
#140304=CARTESIAN_POINT('Origin',(0.,-12.9675000200281,-61.2273317382593));
#140305=CARTESIAN_POINT('Origin',(-25.767032515919,-66.4122774533306,-61.8843165123376));
#140306=CARTESIAN_POINT('',(-31.35,-62.9782728042642,-60.64995));
#140307=CARTESIAN_POINT('Origin',(0.,-12.9675000200281,-60.64995));
#140308=CARTESIAN_POINT('Ctrl Pts',(-31.1074520910898,-62.0598503138784,
-61.2273317382593));
#140309=CARTESIAN_POINT('Ctrl Pts',(-31.1192593280084,-62.1041984096607,
-61.1334442002736));
#140310=CARTESIAN_POINT('Ctrl Pts',(-31.1342845229578,-62.1606836378221,
-61.0509981549565));
#140311=CARTESIAN_POINT('Ctrl Pts',(-31.1697097530512,-62.2941363459118,
-60.9056817830676));
#140312=CARTESIAN_POINT('Ctrl Pts',(-31.1896892584046,-62.369523292851,
-60.8449704353912));
#140313=CARTESIAN_POINT('Ctrl Pts',(-31.2539016024624,-62.6123775685824,
-60.6987791235328));
#140314=CARTESIAN_POINT('Ctrl Pts',(-31.3019361194217,-62.7947963971694,
-60.64995));
#140315=CARTESIAN_POINT('Ctrl Pts',(-31.35,-62.9782728042642,-60.64995));
#140316=CARTESIAN_POINT('Origin',(0.,-12.9675000200281,-60.64995));
#140317=CARTESIAN_POINT('',(-31.35,-12.9675000200281,-60.64995));
#140318=CARTESIAN_POINT('Ctrl Pts',(-31.3064221286262,-65.3602738277489,
-59.64995));
#140319=CARTESIAN_POINT('Ctrl Pts',(-31.8499999999999,-65.3127169262601,
-59.64995));
#140320=CARTESIAN_POINT('Ctrl Pts',(-31.85,-65.8583711767947,-59.64995));
#140321=CARTESIAN_POINT('Ctrl Pts',(-31.3064221286269,-65.3602738277488,
-59.7808732880376));
#140322=CARTESIAN_POINT('Ctrl Pts',(-31.8499999999999,-65.3127169262533,
-59.7746029379323));
#140323=CARTESIAN_POINT('Ctrl Pts',(-31.85,-65.8583711767784,-59.8463349320561));
#140324=CARTESIAN_POINT('Ctrl Pts',(-31.3075563441358,-65.3340478495507,
-59.9116978933073));
#140325=CARTESIAN_POINT('Ctrl Pts',(-31.8499999999999,-65.2892961879233,
-59.8989712332632));
#140326=CARTESIAN_POINT('Ctrl Pts',(-31.85,-65.819181055996,-60.0425718399612));
#140327=CARTESIAN_POINT('Ctrl Pts',(-31.3119222489988,-65.2330969061508,
-60.1535689714229));
#140328=CARTESIAN_POINT('Ctrl Pts',(-31.8499999999999,-65.1974676446973,
-60.1322291512615));
#140329=CARTESIAN_POINT('Ctrl Pts',(-31.85,-65.6683275916687,-60.4053784571341));
#140330=CARTESIAN_POINT('Ctrl Pts',(-31.3151522214972,-65.1584116390162,
-60.2644967268053));
#140331=CARTESIAN_POINT('Ctrl Pts',(-31.8499999999999,-65.1294009926956,
-60.2406767152616));
#140332=CARTESIAN_POINT('Ctrl Pts',(-31.85,-65.5567235699328,-60.5717700902076));
#140333=CARTESIAN_POINT('Ctrl Pts',(-31.3232193617865,-64.9718786181899,
-60.4496168355678));
#140334=CARTESIAN_POINT('Ctrl Pts',(-31.8499999999999,-64.9553741448238,
-60.4261994932778));
#140335=CARTESIAN_POINT('Ctrl Pts',(-31.85,-65.2779827136761,-60.8494502533521));
#140336=CARTESIAN_POINT('Ctrl Pts',(-31.3280533572402,-64.8601042170482,
-60.5237363920412));
#140337=CARTESIAN_POINT('Ctrl Pts',(-31.8499999999993,-64.8499435605403,
-60.5031527166052));
#140338=CARTESIAN_POINT('Ctrl Pts',(-31.85,-65.1109554916676,-60.9606295880612));
#140339=CARTESIAN_POINT('Ctrl Pts',(-31.3385935839747,-64.6163870802633,
-60.6239226729814));
#140340=CARTESIAN_POINT('Ctrl Pts',(-31.8500000000006,-64.6146765878316,
-60.6120353079394));
#140341=CARTESIAN_POINT('Ctrl Pts',(-31.85,-64.7467630120136,-61.1109090094727));
#140342=CARTESIAN_POINT('Ctrl Pts',(-31.3442946417934,-64.4845639684081,
-60.64995));
#140343=CARTESIAN_POINT('Ctrl Pts',(-31.85,-64.4853598419829,-60.6442102195366));
#140344=CARTESIAN_POINT('Ctrl Pts',(-31.85,-64.5497765111262,-61.149949999985));
#140345=CARTESIAN_POINT('Ctrl Pts',(-31.35,-64.3526414204797,-60.64995));
#140346=CARTESIAN_POINT('Ctrl Pts',(-31.8499999999999,-64.3526414204797,
-60.64995));
#140347=CARTESIAN_POINT('Ctrl Pts',(-31.85,-64.3526414204797,-61.14995));
#140348=CARTESIAN_POINT('',(-31.85,-64.3526414204797,-61.14995));
#140349=CARTESIAN_POINT('Origin',(-31.35,-64.3526414204797,-61.14995));
#140350=CARTESIAN_POINT('Ctrl Pts',(-31.85,-65.8583711767947,-59.64995));
#140351=CARTESIAN_POINT('Ctrl Pts',(-31.85,-65.8583711767784,-59.8463349320561));
#140352=CARTESIAN_POINT('Ctrl Pts',(-31.85,-65.819181055996,-60.0425718399612));
#140353=CARTESIAN_POINT('Ctrl Pts',(-31.85,-65.6683275916687,-60.4053784571341));
#140354=CARTESIAN_POINT('Ctrl Pts',(-31.85,-65.5567235699328,-60.5717700902076));
#140355=CARTESIAN_POINT('Ctrl Pts',(-31.85,-65.2779827136761,-60.8494502533521));
#140356=CARTESIAN_POINT('Ctrl Pts',(-31.85,-65.1109554916676,-60.9606295880612));
#140357=CARTESIAN_POINT('Ctrl Pts',(-31.85,-64.7467630120136,-61.1109090094727));
#140358=CARTESIAN_POINT('Ctrl Pts',(-31.85,-64.5497765111262,-61.149949999985));
#140359=CARTESIAN_POINT('Ctrl Pts',(-31.85,-64.3526414204797,-61.14995));
#140360=CARTESIAN_POINT('Origin',(-31.85,67.7009572055632,-55.24995));
#140361=CARTESIAN_POINT('',(-31.85,-70.08000002,-55.74995));
#140362=CARTESIAN_POINT('',(-31.85,67.7009572055632,-55.74995));
#140363=CARTESIAN_POINT('',(-31.85,-72.58000002,-58.24995));
#140364=CARTESIAN_POINT('Origin',(-31.85,-70.08000002,-58.24995));
#140365=CARTESIAN_POINT('',(-31.85,-72.58000002,-174.34995));
#140366=CARTESIAN_POINT('',(-31.85,-72.58000002,-58.24995));
#140367=CARTESIAN_POINT('',(-31.85,-70.08000002,-176.84995));
#140368=CARTESIAN_POINT('Origin',(-31.85,-70.08000002,-174.34995));
#140369=CARTESIAN_POINT('',(-31.85,-65.2735353570153,-176.84995));
#140370=CARTESIAN_POINT('',(-31.85,67.7009572055632,-176.84995));
#140371=CARTESIAN_POINT('',(-31.85,-65.2735353570153,-172.64995));
#140372=CARTESIAN_POINT('',(-31.85,-65.2735353570153,-55.24995));
#140373=CARTESIAN_POINT('',(-31.85,-63.7587939982373,-171.14995));
#140374=CARTESIAN_POINT('Ctrl Pts',(-31.85,-63.7587939982373,-171.14995));
#140375=CARTESIAN_POINT('Ctrl Pts',(-31.85,-63.9571089176128,-171.149950000016));
#140376=CARTESIAN_POINT('Ctrl Pts',(-31.85,-64.1552743575927,-171.18899099047));
#140377=CARTESIAN_POINT('Ctrl Pts',(-31.85,-64.521646483527,-171.339270411997));
#140378=CARTESIAN_POINT('Ctrl Pts',(-31.85,-64.6896733421684,-171.450449746589));
#140379=CARTESIAN_POINT('Ctrl Pts',(-31.85,-64.9700824273775,-171.728129909852));
#140380=CARTESIAN_POINT('Ctrl Pts',(-31.85,-65.0823543850191,-171.894521542842));
#140381=CARTESIAN_POINT('Ctrl Pts',(-31.85,-65.2341106883021,-172.257328160063));
#140382=CARTESIAN_POINT('Ctrl Pts',(-31.85,-65.273535357003,-172.453565067926));
#140383=CARTESIAN_POINT('Ctrl Pts',(-31.85,-65.2735353570153,-172.64995));
#140384=CARTESIAN_POINT('',(-31.85,-63.1109998882233,-171.14995));
#140385=CARTESIAN_POINT('',(-31.85,-63.6885235808861,-171.14995));
#140386=CARTESIAN_POINT('',(-31.85,-62.5757608260974,-170.861259130871));
#140387=CARTESIAN_POINT('Ctrl Pts',(-31.85,-62.5757608260974,-170.861259130871));
#140388=CARTESIAN_POINT('Ctrl Pts',(-31.85,-62.5934214847795,-170.893275292324));
#140389=CARTESIAN_POINT('Ctrl Pts',(-31.85,-62.6145900881586,-170.922872024471));
#140390=CARTESIAN_POINT('Ctrl Pts',(-31.85,-62.6386464997607,-170.949982960699));
#140391=CARTESIAN_POINT('Ctrl Pts',(-31.85,-62.6499713199276,-170.962745731906));
#140392=CARTESIAN_POINT('Ctrl Pts',(-31.85,-62.6619368642693,-170.974957283073));
#140393=CARTESIAN_POINT('Ctrl Pts',(-31.85,-62.6744818503514,-170.986608828398));
#140394=CARTESIAN_POINT('Ctrl Pts',(-31.85,-62.703885288123,-171.013918184157));
#140395=CARTESIAN_POINT('Ctrl Pts',(-31.85,-62.7356294724133,-171.037482725823));
#140396=CARTESIAN_POINT('Ctrl Pts',(-31.85,-62.7694892975011,-171.057780531265));
#140397=CARTESIAN_POINT('Ctrl Pts',(-31.85,-62.7808526179145,-171.064592452659));
#140398=CARTESIAN_POINT('Ctrl Pts',(-31.85,-62.7924544589391,-171.071036069574));
#140399=CARTESIAN_POINT('Ctrl Pts',(-31.85,-62.8042869861286,-171.077128390385));
#140400=CARTESIAN_POINT('Ctrl Pts',(-31.85,-62.8513324723594,-171.10135112744));
#140401=CARTESIAN_POINT('Ctrl Pts',(-31.85,-62.9022833426441,-171.119790824143));
#140402=CARTESIAN_POINT('Ctrl Pts',(-31.85,-62.9536152465698,-171.131828583671));
#140403=CARTESIAN_POINT('Ctrl Pts',(-31.85,-63.0049433927144,-171.143865461968));
#140404=CARTESIAN_POINT('Ctrl Pts',(-31.85,-63.0574025248319,-171.14995));
#140405=CARTESIAN_POINT('Ctrl Pts',(-31.85,-63.1109998882233,-171.14995));
#140406=CARTESIAN_POINT('',(-31.85,-56.2763252281792,-159.66866755714));
#140407=CARTESIAN_POINT('Ctrl Pts',(-31.85,-56.2763252281792,-159.66866755714));
#140408=CARTESIAN_POINT('Ctrl Pts',(-31.85,-58.4123038607033,-163.37917596697));
#140409=CARTESIAN_POINT('Ctrl Pts',(-31.85,-60.5078491316876,-167.112441157955));
#140410=CARTESIAN_POINT('Ctrl Pts',(-31.85,-62.5757608260974,-170.86125913087));
#140411=CARTESIAN_POINT('',(-31.85,-55.08000002,-154.831379798159));
#140412=CARTESIAN_POINT('Ctrl Pts',(-31.85,-55.08000002,-154.831379798159));
#140413=CARTESIAN_POINT('Ctrl Pts',(-31.85,-55.08000002,-155.253410854053));
#140414=CARTESIAN_POINT('Ctrl Pts',(-31.85,-55.1042084466772,-155.6729366979));
#140415=CARTESIAN_POINT('Ctrl Pts',(-31.85,-55.1523697302198,-156.089983777379));
#140416=CARTESIAN_POINT('Ctrl Pts',(-31.85,-55.2005310137623,-156.507030856859));
#140417=CARTESIAN_POINT('Ctrl Pts',(-31.85,-55.2730856890926,-156.92345630647));
#140418=CARTESIAN_POINT('Ctrl Pts',(-31.85,-55.3707143450195,-157.332589580255));
#140419=CARTESIAN_POINT('Ctrl Pts',(-31.85,-55.4683430009464,-157.74172285404));
#140420=CARTESIAN_POINT('Ctrl Pts',(-31.85,-55.5903137943579,-158.141820520543));
#140421=CARTESIAN_POINT('Ctrl Pts',(-31.85,-55.7395613131142,-158.531793284255));
#140422=CARTESIAN_POINT('Ctrl Pts',(-31.85,-55.8729496111693,-158.880327073445));
#140423=CARTESIAN_POINT('Ctrl Pts',(-31.85,-56.0279262451313,-159.220847442033));
#140424=CARTESIAN_POINT('Ctrl Pts',(-31.85,-56.2101595915589,-159.551250340992));
#140425=CARTESIAN_POINT('Ctrl Pts',(-31.85,-56.2318262512452,-159.590533640737));
#140426=CARTESIAN_POINT('Ctrl Pts',(-31.85,-56.2538782710724,-159.629673897819));
#140427=CARTESIAN_POINT('Ctrl Pts',(-31.85,-56.2763252281792,-159.668667557141));
#140428=CARTESIAN_POINT('',(-31.85,-55.08000002,-77.227263173365));
#140429=CARTESIAN_POINT('',(-31.85,-55.08000002,-155.433057559267));
#140430=CARTESIAN_POINT('',(-31.85,-56.2763252281792,-72.3899754143654));
#140431=CARTESIAN_POINT('Ctrl Pts',(-31.85,-56.2763252281792,-72.3899754143654));
#140432=CARTESIAN_POINT('Ctrl Pts',(-31.85,-56.0652560607924,-72.7566335394409));
#140433=CARTESIAN_POINT('Ctrl Pts',(-31.85,-55.8881616822718,-73.1379857966025));
#140434=CARTESIAN_POINT('Ctrl Pts',(-31.85,-55.737982230652,-73.5309787881812));
#140435=CARTESIAN_POINT('Ctrl Pts',(-31.85,-55.5878027790321,-73.9239717797599));
#140436=CARTESIAN_POINT('Ctrl Pts',(-31.85,-55.4647382249676,-74.3299545387688));
#140437=CARTESIAN_POINT('Ctrl Pts',(-31.85,-55.367968034963,-74.7375921331689));
#140438=CARTESIAN_POINT('Ctrl Pts',(-31.85,-55.2585018339702,-75.1987107776474));
#140439=CARTESIAN_POINT('Ctrl Pts',(-31.85,-55.1807511519297,-75.6645810411795));
#140440=CARTESIAN_POINT('Ctrl Pts',(-31.85,-55.1338484059997,-76.1350729813869));
#140441=CARTESIAN_POINT('Ctrl Pts',(-31.85,-55.0978253247023,-76.4964285710389));
#140442=CARTESIAN_POINT('Ctrl Pts',(-31.85,-55.0800000199994,-76.8605105831145));
#140443=CARTESIAN_POINT('Ctrl Pts',(-31.85,-55.08000002,-77.227263173365));
#140444=CARTESIAN_POINT('',(-31.85,-62.4426282692182,-61.4386408691297));
#140445=CARTESIAN_POINT('Ctrl Pts',(-31.85,-62.4426282692182,-61.4386408691297));
#140446=CARTESIAN_POINT('Ctrl Pts',(-31.85,-60.41789121461,-65.1063702600533));
#140447=CARTESIAN_POINT('Ctrl Pts',(-31.85,-58.3664753860175,-68.7590777918155));
#140448=CARTESIAN_POINT('Ctrl Pts',(-31.85,-56.2763252281792,-72.3899754143654));
#140449=CARTESIAN_POINT('',(-31.85,-62.9782728042642,-61.14995));
#140450=CARTESIAN_POINT('Ctrl Pts',(-31.85,-62.9782728042642,-61.14995));
#140451=CARTESIAN_POINT('Ctrl Pts',(-31.85,-62.9222361461974,-61.14995));
#140452=CARTESIAN_POINT('Ctrl Pts',(-31.85,-62.8664016141262,-61.1566668506656));
#140453=CARTESIAN_POINT('Ctrl Pts',(-31.85,-62.8123519766725,-61.1700628877868));
#140454=CARTESIAN_POINT('Ctrl Pts',(-31.85,-62.763267528681,-61.1822283179052));
#140455=CARTESIAN_POINT('Ctrl Pts',(-31.85,-62.7156536890974,-61.1999027909623));
#140456=CARTESIAN_POINT('Ctrl Pts',(-31.85,-62.6707013203275,-61.2230949953743));
#140457=CARTESIAN_POINT('Ctrl Pts',(-31.85,-62.6234720220053,-61.2474619324434));
#140458=CARTESIAN_POINT('Ctrl Pts',(-31.85,-62.5794710795978,-61.2778158553603));
#140459=CARTESIAN_POINT('Ctrl Pts',(-31.85,-62.5405071542091,-61.3141449414402));
#140460=CARTESIAN_POINT('Ctrl Pts',(-31.85,-62.5015487187516,-61.350468908832));
#140461=CARTESIAN_POINT('Ctrl Pts',(-31.85,-62.4685524875291,-61.3916801947947));
#140462=CARTESIAN_POINT('Ctrl Pts',(-31.85,-62.4426282692182,-61.4386408691297));
#140463=CARTESIAN_POINT('',(-31.85,67.7009572055632,-61.14995));
#140464=CARTESIAN_POINT('Origin',(-32.35,-73.08000002,-55.74995));
#140465=CARTESIAN_POINT('',(-32.35,-70.08000002,-55.24995));
#140466=CARTESIAN_POINT('',(-32.35,-73.08000002,-55.24995));
#140467=CARTESIAN_POINT('Origin',(-32.35,-70.08000002,-55.74995));
#140468=CARTESIAN_POINT('Origin',(-41.5,-73.08000002,-55.24995));
#140469=CARTESIAN_POINT('',(-32.85,-70.08000002,-55.24995));
#140470=CARTESIAN_POINT('',(-32.85,-73.08000002,-55.24995));
#140471=CARTESIAN_POINT('',(-41.5,-70.08000002,-55.24995));
#140472=CARTESIAN_POINT('Origin',(-32.85,67.7009572055632,-55.74995));
#140473=CARTESIAN_POINT('',(-33.35,-70.08000002,-55.74995));
#140474=CARTESIAN_POINT('',(-33.35,67.7009572055632,-55.74995));
#140475=CARTESIAN_POINT('Origin',(-32.85,-70.08000002,-55.74995));
#140476=CARTESIAN_POINT('Origin',(-33.35,67.7009572055632,-55.24995));
#140477=CARTESIAN_POINT('',(-33.35,-70.08000002,-176.84995));
#140478=CARTESIAN_POINT('',(-33.35,-64.9221832702593,-176.84995));
#140479=CARTESIAN_POINT('',(-33.35,67.7009572055632,-176.84995));
#140480=CARTESIAN_POINT('',(-33.35,-72.58000002,-174.34995));
#140481=CARTESIAN_POINT('Origin',(-33.35,-70.08000002,-174.34995));
#140482=CARTESIAN_POINT('',(-33.35,-72.58000002,-58.24995));
#140483=CARTESIAN_POINT('',(-33.35,-72.58000002,-174.34995));
#140484=CARTESIAN_POINT('Origin',(-33.35,-70.08000002,-58.24995));
#140485=CARTESIAN_POINT('',(-33.35,-61.3211699373828,-61.14995));
#140486=CARTESIAN_POINT('',(-33.35,67.7009572055632,-61.14995));
#140487=CARTESIAN_POINT('',(-33.35,-60.7669593817595,-61.4386408691297));
#140488=CARTESIAN_POINT('Ctrl Pts',(-33.35,-60.7669593817595,-61.4386408691297));
#140489=CARTESIAN_POINT('Ctrl Pts',(-33.35,-60.7854255655573,-61.4063230635265));
#140490=CARTESIAN_POINT('Ctrl Pts',(-33.35,-60.8074669942764,-61.3766005831693));
#140491=CARTESIAN_POINT('Ctrl Pts',(-33.35,-60.8323159282117,-61.349574172408));
#140492=CARTESIAN_POINT('Ctrl Pts',(-33.35,-60.8598479301244,-61.3196295802292));
#140493=CARTESIAN_POINT('Ctrl Pts',(-33.35,-60.8908254879513,-61.2929954345222));
#140494=CARTESIAN_POINT('Ctrl Pts',(-33.35,-60.9241484264025,-61.2697698227383));
#140495=CARTESIAN_POINT('Ctrl Pts',(-33.35,-60.9500168068528,-61.2517399313259));
#140496=CARTESIAN_POINT('Ctrl Pts',(-33.35,-60.9772970763435,-61.2357633244769));
#140497=CARTESIAN_POINT('Ctrl Pts',(-33.35,-61.0054624679791,-61.2218683128494));
#140498=CARTESIAN_POINT('Ctrl Pts',(-33.35,-61.0316582964252,-61.2089449583455));
#140499=CARTESIAN_POINT('Ctrl Pts',(-33.35,-61.0586931044519,-61.1978139207404));
#140500=CARTESIAN_POINT('Ctrl Pts',(-33.35,-61.0863521110361,-61.1884108897488));
#140501=CARTESIAN_POINT('Ctrl Pts',(-33.35,-61.1146264284013,-61.1787986760331));
#140502=CARTESIAN_POINT('Ctrl Pts',(-33.35,-61.1435543947086,-61.1709920371076));
#140503=CARTESIAN_POINT('Ctrl Pts',(-33.35,-61.1729286914005,-61.1649732421567));
#140504=CARTESIAN_POINT('Ctrl Pts',(-33.35,-61.2017965294041,-61.1590582206179));
#140505=CARTESIAN_POINT('Ctrl Pts',(-33.35,-61.2310968493206,-61.1548700235783));
#140506=CARTESIAN_POINT('Ctrl Pts',(-33.35,-61.2606330881675,-61.1524405238988));
#140507=CARTESIAN_POINT('Ctrl Pts',(-33.35,-61.2807251508685,-61.1507878537622));
#140508=CARTESIAN_POINT('Ctrl Pts',(-33.35,-61.3009263849488,-61.14995));
#140509=CARTESIAN_POINT('Ctrl Pts',(-33.35,-61.3211699373828,-61.14995));
#140510=CARTESIAN_POINT('',(-33.35,-56.3642045114132,-69.0177323827589));
#140511=CARTESIAN_POINT('Ctrl Pts',(-33.35,-56.3642045114132,-69.0177323827589));
#140512=CARTESIAN_POINT('Ctrl Pts',(-33.35,-57.8514954063616,-66.5028158819518));
#140513=CARTESIAN_POINT('Ctrl Pts',(-33.35,-59.3174212852614,-63.975488272466));
#140514=CARTESIAN_POINT('Ctrl Pts',(-33.35,-60.7669593817595,-61.4386408691297));
#140515=CARTESIAN_POINT('',(-33.35,-55.08000002,-74.155095361993));
#140516=CARTESIAN_POINT('Ctrl Pts',(-33.35,-55.08000002,-74.155095361993));
#140517=CARTESIAN_POINT('Ctrl Pts',(-33.35,-55.0800000199996,-73.9307666441726));
#140518=CARTESIAN_POINT('Ctrl Pts',(-33.35,-55.0863156531016,-73.7071338026571));
#140519=CARTESIAN_POINT('Ctrl Pts',(-33.35,-55.099013419779,-73.4842001164092));
#140520=CARTESIAN_POINT('Ctrl Pts',(-33.35,-55.1117111864564,-73.2612664301613));
#140521=CARTESIAN_POINT('Ctrl Pts',(-33.35,-55.1307909278358,-73.0390315071252));
#140522=CARTESIAN_POINT('Ctrl Pts',(-33.35,-55.1563760274665,-72.8175000855932));
#140523=CARTESIAN_POINT('Ctrl Pts',(-33.35,-55.1806216024912,-72.6075670863636));
#140524=CARTESIAN_POINT('Ctrl Pts',(-33.35,-55.210750014218,-72.3979880684058));
#140525=CARTESIAN_POINT('Ctrl Pts',(-33.35,-55.2468600350687,-72.1892231805709));
#140526=CARTESIAN_POINT('Ctrl Pts',(-33.35,-55.2824608236509,-71.9834023457969));
#140527=CARTESIAN_POINT('Ctrl Pts',(-33.35,-55.3238757306228,-71.7783731405196));
#140528=CARTESIAN_POINT('Ctrl Pts',(-33.35,-55.3711489449082,-71.5745698720716));
#140529=CARTESIAN_POINT('Ctrl Pts',(-33.35,-55.3771233770109,-71.5488130284117));
#140530=CARTESIAN_POINT('Ctrl Pts',(-33.35,-55.3831913115131,-71.5230757533204));
#140531=CARTESIAN_POINT('Ctrl Pts',(-33.35,-55.3893527788883,-71.4973589120773));
#140532=CARTESIAN_POINT('Ctrl Pts',(-33.35,-55.49371790368,-71.061757912807));
#140533=CARTESIAN_POINT('Ctrl Pts',(-33.35,-55.62429768467,-70.6362303826932));
#140534=CARTESIAN_POINT('Ctrl Pts',(-33.35,-55.7846973533805,-70.2221616988514));
#140535=CARTESIAN_POINT('Ctrl Pts',(-33.35,-55.9170285274408,-69.8805512983134));
#140536=CARTESIAN_POINT('Ctrl Pts',(-33.35,-56.0694235888807,-69.5466508245293));
#140537=CARTESIAN_POINT('Ctrl Pts',(-33.35,-56.2474267877794,-69.2225907454076));
#140538=CARTESIAN_POINT('Ctrl Pts',(-33.35,-56.2851826821973,-69.1538550248807));
#140539=CARTESIAN_POINT('Ctrl Pts',(-33.35,-56.3240908525374,-69.0855620877321));
#140540=CARTESIAN_POINT('Ctrl Pts',(-33.35,-56.3642045114132,-69.0177323827589));
#140541=CARTESIAN_POINT('',(-33.35,-55.08000002,-157.903547609535));
#140542=CARTESIAN_POINT('',(-33.35,-55.08000002,-74.7820934264633));
#140543=CARTESIAN_POINT('',(-33.35,-56.3642045114216,-163.040910588762));
#140544=CARTESIAN_POINT('Ctrl Pts',(-33.35,-56.3642045114216,-163.040910588761));
#140545=CARTESIAN_POINT('Ctrl Pts',(-33.35,-56.15744649645,-162.69129563093));
#140546=CARTESIAN_POINT('Ctrl Pts',(-33.35,-55.9820013313226,-162.328090330091));
#140547=CARTESIAN_POINT('Ctrl Pts',(-33.35,-55.8312183864901,-161.954181181917));
#140548=CARTESIAN_POINT('Ctrl Pts',(-33.35,-55.8149691191711,-161.913886507288));
#140549=CARTESIAN_POINT('Ctrl Pts',(-33.35,-55.7990063112135,-161.873467504085));
#140550=CARTESIAN_POINT('Ctrl Pts',(-33.35,-55.7833216689026,-161.832927771927));
#140551=CARTESIAN_POINT('Ctrl Pts',(-33.35,-55.6220934454647,-161.4162049124));
#140552=CARTESIAN_POINT('Ctrl Pts',(-33.35,-55.4903395808871,-160.984647645305));
#140553=CARTESIAN_POINT('Ctrl Pts',(-33.35,-55.3869054679322,-160.551047169605));
#140554=CARTESIAN_POINT('Ctrl Pts',(-33.35,-55.2731785652171,-160.074298854097));
#140555=CARTESIAN_POINT('Ctrl Pts',(-33.35,-55.1917492545593,-159.592825164627));
#140556=CARTESIAN_POINT('Ctrl Pts',(-33.35,-55.1414674766992,-159.106794321394));
#140557=CARTESIAN_POINT('Ctrl Pts',(-33.35,-55.1002871472375,-158.708739377742));
#140558=CARTESIAN_POINT('Ctrl Pts',(-33.35,-55.08000002,-158.307627565795));
#140559=CARTESIAN_POINT('Ctrl Pts',(-33.35,-55.08000002,-157.903547609535));
#140560=CARTESIAN_POINT('',(-33.35,-60.9047458754482,-170.861259130871));
#140561=CARTESIAN_POINT('Ctrl Pts',(-33.35,-60.9047458754482,-170.861259130871));
#140562=CARTESIAN_POINT('Ctrl Pts',(-33.35,-59.4103419837617,-168.243380962845));
#140563=CARTESIAN_POINT('Ctrl Pts',(-33.35,-57.8986402212887,-165.635546042559));
#140564=CARTESIAN_POINT('Ctrl Pts',(-33.35,-56.3642045114219,-163.040910588762));
#140565=CARTESIAN_POINT('',(-33.35,-61.4584329769396,-171.14995));
#140566=CARTESIAN_POINT('Ctrl Pts',(-33.35,-61.4584329769396,-171.14995));
#140567=CARTESIAN_POINT('Ctrl Pts',(-33.35,-61.3933512658327,-171.14995));
#140568=CARTESIAN_POINT('Ctrl Pts',(-33.35,-61.3285261814765,-171.141518537402));
#140569=CARTESIAN_POINT('Ctrl Pts',(-33.35,-61.2661398376586,-171.124539608288));
#140570=CARTESIAN_POINT('Ctrl Pts',(-33.35,-61.2235444953616,-171.112946954301));
#140571=CARTESIAN_POINT('Ctrl Pts',(-33.35,-61.1820855819977,-171.09736868316));
#140572=CARTESIAN_POINT('Ctrl Pts',(-33.35,-61.1424600695407,-171.077754003862));
#140573=CARTESIAN_POINT('Ctrl Pts',(-33.35,-61.107639036433,-171.06051754798));
#140574=CARTESIAN_POINT('Ctrl Pts',(-33.35,-61.0743836755045,-171.040165282673));
#140575=CARTESIAN_POINT('Ctrl Pts',(-33.35,-61.0435144499431,-171.016803427716));
#140576=CARTESIAN_POINT('Ctrl Pts',(-33.35,-61.0154640589469,-170.995574869045));
#140577=CARTESIAN_POINT('Ctrl Pts',(-33.35,-60.9893827952823,-170.971860522156));
#140578=CARTESIAN_POINT('Ctrl Pts',(-33.35,-60.9659114268331,-170.945708806781));
#140579=CARTESIAN_POINT('Ctrl Pts',(-33.35,-60.9427675971716,-170.91992203396));
#140580=CARTESIAN_POINT('Ctrl Pts',(-33.35,-60.9221601342065,-170.891765212974));
#140581=CARTESIAN_POINT('Ctrl Pts',(-33.35,-60.9047458754482,-170.861259130871));
#140582=CARTESIAN_POINT('',(-33.35,-63.4074419114814,-171.14995));
#140583=CARTESIAN_POINT('',(-33.35,-61.8036605881122,-171.14995));
#140584=CARTESIAN_POINT('',(-33.35,-64.9221832702593,-172.64995));
#140585=CARTESIAN_POINT('Ctrl Pts',(-33.35,-64.9221832702593,-172.64995));
#140586=CARTESIAN_POINT('Ctrl Pts',(-33.35,-64.922183270247,-172.453565067926));
#140587=CARTESIAN_POINT('Ctrl Pts',(-33.35,-64.8827586015461,-172.257328160063));
#140588=CARTESIAN_POINT('Ctrl Pts',(-33.35,-64.7310022982632,-171.894521542842));
#140589=CARTESIAN_POINT('Ctrl Pts',(-33.35,-64.6187303406215,-171.728129909852));
#140590=CARTESIAN_POINT('Ctrl Pts',(-33.35,-64.3383212554124,-171.450449746589));
#140591=CARTESIAN_POINT('Ctrl Pts',(-33.35,-64.1702943967697,-171.339270411997));
#140592=CARTESIAN_POINT('Ctrl Pts',(-33.35,-63.8039222708381,-171.18899099047));
#140593=CARTESIAN_POINT('Ctrl Pts',(-33.35,-63.6057568308558,-171.149950000016));
#140594=CARTESIAN_POINT('Ctrl Pts',(-33.35,-63.4074419114814,-171.14995));
#140595=CARTESIAN_POINT('',(-33.35,-64.9221832702593,-55.24995));
#140596=CARTESIAN_POINT('Origin',(0.,-12.9675000200281,-60.64995));
#140597=CARTESIAN_POINT('',(-37.,33.02054075664,-60.64995));
#140598=CARTESIAN_POINT('',(-31.,37.2609769076718,-60.64995));
#140599=CARTESIAN_POINT('Origin',(0.,-12.9675000200281,-60.64995));
#140600=CARTESIAN_POINT('',(-37.,-12.9675000200281,-60.64995));
#140601=CARTESIAN_POINT('',(-31.,-12.9675000200281,-60.64995));
#140602=CARTESIAN_POINT('Ctrl Pts',(-30.9564221286262,39.4558948199267,
-59.64995));
#140603=CARTESIAN_POINT('Ctrl Pts',(-30.5,39.4958265819639,-59.64995));
#140604=CARTESIAN_POINT('Ctrl Pts',(-30.5,39.9539921689726,-59.64995));
#140605=CARTESIAN_POINT('Ctrl Pts',(-30.9564221286278,39.4558948199266,
-59.7808732880376));
#140606=CARTESIAN_POINT('Ctrl Pts',(-30.5,39.4958265819509,-59.7861314644993));
#140607=CARTESIAN_POINT('Ctrl Pts',(-30.5,39.9539921689583,-59.8463349320561));
#140608=CARTESIAN_POINT('Ctrl Pts',(-30.9575563441362,39.4296688417285,
-59.9116978933072));
#140609=CARTESIAN_POINT('Ctrl Pts',(-30.4999999999997,39.4674332340768,
-59.9224177216067));
#140610=CARTESIAN_POINT('Ctrl Pts',(-30.5,39.9148020481738,-60.0425718399611));
#140611=CARTESIAN_POINT('Ctrl Pts',(-30.9619222489984,39.3287178983286,
-60.153568971423));
#140612=CARTESIAN_POINT('Ctrl Pts',(-30.5000000000003,39.3593214179772,
-60.1718710142636));
#140613=CARTESIAN_POINT('Ctrl Pts',(-30.5,39.7639485838465,-60.4053784571342));
#140614=CARTESIAN_POINT('Ctrl Pts',(-30.9651522214976,39.2540326311941,
-60.2644967268053));
#140615=CARTESIAN_POINT('Ctrl Pts',(-30.5000000000001,39.2793032864295,
-60.2852157712117));
#140616=CARTESIAN_POINT('Ctrl Pts',(-30.5,39.65234456211,-60.5717700902076));
#140617=CARTESIAN_POINT('Ctrl Pts',(-30.9732193617862,39.0674996103677,
-60.4496168355678));
#140618=CARTESIAN_POINT('Ctrl Pts',(-30.5,39.0823726723643,-60.4706504746469));
#140619=CARTESIAN_POINT('Ctrl Pts',(-30.5,39.3736037058546,-60.8494502533521));
#140620=CARTESIAN_POINT('Ctrl Pts',(-30.9780533572398,38.9557252092273,
-60.5237363920407));
#140621=CARTESIAN_POINT('Ctrl Pts',(-30.5,38.9650655890091,-60.5426326522477));
#140622=CARTESIAN_POINT('Ctrl Pts',(-30.5,39.206576483846,-60.9606295880612));
#140623=CARTESIAN_POINT('Ctrl Pts',(-30.9885935839752,38.71200807244,-60.6239226729818));
#140624=CARTESIAN_POINT('Ctrl Pts',(-30.5,38.7136903701654,-60.6353187454024));
#140625=CARTESIAN_POINT('Ctrl Pts',(-30.5,38.8423840041908,-61.1109090094727));
#140626=CARTESIAN_POINT('Ctrl Pts',(-30.994294641792,38.5801849605867,-60.64995));
#140627=CARTESIAN_POINT('Ctrl Pts',(-30.4999999999973,38.5794088824901,
-60.655621796981));
#140628=CARTESIAN_POINT('Ctrl Pts',(-30.5,38.6453975033045,-61.149949999985));
#140629=CARTESIAN_POINT('Ctrl Pts',(-31.,38.4482624126576,-60.64995));
#140630=CARTESIAN_POINT('Ctrl Pts',(-30.5,38.4482624126575,-60.64995));
#140631=CARTESIAN_POINT('Ctrl Pts',(-30.5,38.4482624126576,-61.14995));
#140632=CARTESIAN_POINT('',(-30.5,38.4482624126576,-61.14995));
#140633=CARTESIAN_POINT('Ctrl Pts',(-30.5,39.9539921689726,-59.64995));
#140634=CARTESIAN_POINT('Ctrl Pts',(-30.5,39.9539921689583,-59.8463349320561));
#140635=CARTESIAN_POINT('Ctrl Pts',(-30.5,39.9148020481738,-60.0425718399611));
#140636=CARTESIAN_POINT('Ctrl Pts',(-30.5,39.7639485838465,-60.4053784571342));
#140637=CARTESIAN_POINT('Ctrl Pts',(-30.5,39.65234456211,-60.5717700902076));
#140638=CARTESIAN_POINT('Ctrl Pts',(-30.5,39.3736037058546,-60.8494502533521));
#140639=CARTESIAN_POINT('Ctrl Pts',(-30.5,39.206576483846,-60.9606295880612));
#140640=CARTESIAN_POINT('Ctrl Pts',(-30.5,38.8423840041908,-61.1109090094727));
#140641=CARTESIAN_POINT('Ctrl Pts',(-30.5,38.6453975033045,-61.149949999985));
#140642=CARTESIAN_POINT('Ctrl Pts',(-30.5,38.4482624126576,-61.14995));
#140643=CARTESIAN_POINT('Origin',(-31.,38.4482624126576,-61.14995));
#140644=CARTESIAN_POINT('Ctrl Pts',(-37.,37.923330431502,-60.64995));
#140645=CARTESIAN_POINT('Ctrl Pts',(-37.5,37.923330431502,-60.64995));
#140646=CARTESIAN_POINT('Ctrl Pts',(-37.5,37.923330431502,-61.14995));
#140647=CARTESIAN_POINT('Ctrl Pts',(-36.9942946417934,38.0552529794313,
-60.64995));
#140648=CARTESIAN_POINT('Ctrl Pts',(-37.5000000000028,38.0560488530063,
-60.6442102195364));
#140649=CARTESIAN_POINT('Ctrl Pts',(-37.5,38.1204655221491,-61.149949999985));
#140650=CARTESIAN_POINT('Ctrl Pts',(-36.9885935839748,38.1870760912844,
-60.6239226729819));
#140651=CARTESIAN_POINT('Ctrl Pts',(-37.5,38.1853655988526,-60.6120353079393));
#140652=CARTESIAN_POINT('Ctrl Pts',(-37.5,38.3174520230353,-61.1109090094727));
#140653=CARTESIAN_POINT('Ctrl Pts',(-36.9780533572402,38.4307932280718,
-60.5237363920407));
#140654=CARTESIAN_POINT('Ctrl Pts',(-37.5,38.4206325715641,-60.5031527166052));
#140655=CARTESIAN_POINT('Ctrl Pts',(-37.5,38.6816445026906,-60.9606295880611));
#140656=CARTESIAN_POINT('Ctrl Pts',(-36.9732193617859,38.5425676292119,
-60.4496168355682));
#140657=CARTESIAN_POINT('Ctrl Pts',(-37.4999999999993,38.5260631558441,
-60.4261994932771));
#140658=CARTESIAN_POINT('Ctrl Pts',(-37.5,38.8486717246983,-60.8494502533514));
#140659=CARTESIAN_POINT('Ctrl Pts',(-36.9651522214979,38.7291006500388,
-60.2644967268049));
#140660=CARTESIAN_POINT('Ctrl Pts',(-37.5000000000007,38.70009000372,-60.2406767152623));
#140661=CARTESIAN_POINT('Ctrl Pts',(-37.5,39.1274125809551,-60.5717700902082));
#140662=CARTESIAN_POINT('Ctrl Pts',(-36.9619222489981,38.8037859171731,
-60.153568971423));
#140663=CARTESIAN_POINT('Ctrl Pts',(-37.4999999999994,38.768156655719,-60.1322291512603));
#140664=CARTESIAN_POINT('Ctrl Pts',(-37.5,39.239016602691,-60.4053784571342));
#140665=CARTESIAN_POINT('Ctrl Pts',(-36.9575563441365,38.904736860573,-59.9116978933072));
#140666=CARTESIAN_POINT('Ctrl Pts',(-37.5000000000007,38.8599851989463,
-59.8989712332646));
#140667=CARTESIAN_POINT('Ctrl Pts',(-37.5,39.3898700670183,-60.0425718399611));
#140668=CARTESIAN_POINT('Ctrl Pts',(-36.9564221286271,38.9309628387711,
-59.7808732880376));
#140669=CARTESIAN_POINT('Ctrl Pts',(-37.5,38.8834059372763,-59.7746029379313));
#140670=CARTESIAN_POINT('Ctrl Pts',(-37.5,39.4290601878028,-59.8463349320561));
#140671=CARTESIAN_POINT('Ctrl Pts',(-36.9564221286262,38.9309628387712,
-59.64995));
#140672=CARTESIAN_POINT('Ctrl Pts',(-37.5,38.8834059372825,-59.64995));
#140673=CARTESIAN_POINT('Ctrl Pts',(-37.5,39.4290601878171,-59.64995));
#140674=CARTESIAN_POINT('',(-37.5,37.923330431502,-61.14995));
#140675=CARTESIAN_POINT('Origin',(-37.,37.923330431502,-61.14995));
#140676=CARTESIAN_POINT('Ctrl Pts',(-37.5,37.923330431502,-61.14995));
#140677=CARTESIAN_POINT('Ctrl Pts',(-37.5,38.1204655221491,-61.149949999985));
#140678=CARTESIAN_POINT('Ctrl Pts',(-37.5,38.3174520230353,-61.1109090094727));
#140679=CARTESIAN_POINT('Ctrl Pts',(-37.5,38.6816445026906,-60.9606295880611));
#140680=CARTESIAN_POINT('Ctrl Pts',(-37.5,38.8486717246983,-60.8494502533514));
#140681=CARTESIAN_POINT('Ctrl Pts',(-37.5,39.1274125809551,-60.5717700902082));
#140682=CARTESIAN_POINT('Ctrl Pts',(-37.5,39.239016602691,-60.4053784571342));
#140683=CARTESIAN_POINT('Ctrl Pts',(-37.5,39.3898700670183,-60.0425718399611));
#140684=CARTESIAN_POINT('Ctrl Pts',(-37.5,39.4290601878028,-59.8463349320561));
#140685=CARTESIAN_POINT('Ctrl Pts',(-37.5,39.4290601878171,-59.64995));
#140686=CARTESIAN_POINT('Origin',(-30.5,-9.33460238845303,-92.34995));
#140687=CARTESIAN_POINT('',(-30.5,43.91999998,-55.74995));
#140688=CARTESIAN_POINT('',(-30.5,39.4958265819638,-55.74995));
#140689=CARTESIAN_POINT('',(-30.5,46.41999998,-58.24995));
#140690=CARTESIAN_POINT('Origin',(-30.5,43.91999998,-58.24995));
#140691=CARTESIAN_POINT('',(-30.5,46.41999998,-58.24995));
#140692=CARTESIAN_POINT('',(-30.5,28.91999998,-91.34995));
#140693=CARTESIAN_POINT('Origin',(-30.5,29.41999998,-91.34995));
#140694=CARTESIAN_POINT('',(-30.5,28.91999998,-78.0460091084363));
#140695=CARTESIAN_POINT('',(-30.5,28.91999998,-91.34995));
#140696=CARTESIAN_POINT('',(-30.5,30.1096831288108,-73.2320455176344));
#140697=CARTESIAN_POINT('Ctrl Pts',(-30.5,30.1096831288108,-73.2320455176344));
#140698=CARTESIAN_POINT('Ctrl Pts',(-30.5,29.8999686314803,-73.5970828192481));
#140699=CARTESIAN_POINT('Ctrl Pts',(-30.5,29.7239010511178,-73.976669190304));
#140700=CARTESIAN_POINT('Ctrl Pts',(-30.5,29.5745597864535,-74.3678121335876));
#140701=CARTESIAN_POINT('Ctrl Pts',(-30.5,29.4252185217892,-74.7589550768711));
#140702=CARTESIAN_POINT('Ctrl Pts',(-30.5,29.3028136262495,-75.1629449137757));
#140703=CARTESIAN_POINT('Ctrl Pts',(-30.5,29.2065461283391,-75.5685697596184));
#140704=CARTESIAN_POINT('Ctrl Pts',(-30.5,29.0974180990884,-76.0283826871663));
#140705=CARTESIAN_POINT('Ctrl Pts',(-30.5,29.0199506911356,-76.4929481091058));
#140706=CARTESIAN_POINT('Ctrl Pts',(-30.5,28.9733024240056,-76.9621397516273));
#140707=CARTESIAN_POINT('Ctrl Pts',(-30.5,28.9376489765478,-77.3207447031833));
#140708=CARTESIAN_POINT('Ctrl Pts',(-30.5,28.91999998,-77.6820522875113));
#140709=CARTESIAN_POINT('Ctrl Pts',(-30.5,28.91999998,-78.0460091084363));
#140710=CARTESIAN_POINT('',(-30.5,36.7276789742547,-61.4386408691296));
#140711=CARTESIAN_POINT('Ctrl Pts',(-30.5,36.7276789742547,-61.4386408691296));
#140712=CARTESIAN_POINT('Ctrl Pts',(-30.5,34.5564250420216,-65.3892731044285));
#140713=CARTESIAN_POINT('Ctrl Pts',(-30.5,32.355340677558,-69.3231656718822));
#140714=CARTESIAN_POINT('Ctrl Pts',(-30.5,30.1096831288108,-73.2320455176344));
#140715=CARTESIAN_POINT('',(-30.5,37.2609769076718,-61.14995));
#140716=CARTESIAN_POINT('Ctrl Pts',(-30.5,37.2609769076718,-61.14995));
#140717=CARTESIAN_POINT('Ctrl Pts',(-30.5,37.2057964810295,-61.14995));
#140718=CARTESIAN_POINT('Ctrl Pts',(-30.5,37.1508139868679,-61.1565255904659));
#140719=CARTESIAN_POINT('Ctrl Pts',(-30.5,37.0975659565504,-61.1696247206415));
#140720=CARTESIAN_POINT('Ctrl Pts',(-30.5,37.0479567714751,-61.1818286870479));
#140721=CARTESIAN_POINT('Ctrl Pts',(-30.5,36.9998515275003,-61.199695577265));
#140722=CARTESIAN_POINT('Ctrl Pts',(-30.5,36.9544986327132,-61.223223625875));
#140723=CARTESIAN_POINT('Ctrl Pts',(-30.5,36.9220640062061,-61.2400499711985));
#140724=CARTESIAN_POINT('Ctrl Pts',(-30.5,36.8911731746044,-61.2597722334507));
#140725=CARTESIAN_POINT('Ctrl Pts',(-30.5,36.8624864317523,-61.2822151380555));
#140726=CARTESIAN_POINT('Ctrl Pts',(-30.5,36.8352464003271,-61.3035262164814));
#140727=CARTESIAN_POINT('Ctrl Pts',(-30.5,36.8099924249354,-61.3272911886642));
#140728=CARTESIAN_POINT('Ctrl Pts',(-30.5,36.7873187400316,-61.3533954059167));
#140729=CARTESIAN_POINT('Ctrl Pts',(-30.5,36.7660341218411,-61.3779003904282));
#140730=CARTESIAN_POINT('Ctrl Pts',(-30.5,36.7470225594144,-61.4044673363619));
#140731=CARTESIAN_POINT('Ctrl Pts',(-30.5,36.730815934666,-61.4330244036176));
#140732=CARTESIAN_POINT('Ctrl Pts',(-30.5,36.7297582655658,-61.4348880814715));
#140733=CARTESIAN_POINT('Ctrl Pts',(-30.5,36.728712560285,-61.4367602423504));
#140734=CARTESIAN_POINT('Ctrl Pts',(-30.5,36.7276789742547,-61.4386408691296));
#140735=CARTESIAN_POINT('',(-30.5,-9.33460238845303,-61.14995));
#140736=CARTESIAN_POINT('Origin',(-30.,0.,-55.74995));
#140737=CARTESIAN_POINT('',(-30.,43.91999998,-55.24995));
#140738=CARTESIAN_POINT('',(-30.,43.91999998,-55.24995));
#140739=CARTESIAN_POINT('Origin',(-30.,43.91999998,-55.74995));
#140740=CARTESIAN_POINT('Origin',(0.,0.,-55.24995));
#140741=CARTESIAN_POINT('',(-29.5,43.91999998,-55.24995));
#140742=CARTESIAN_POINT('',(-29.5,39.6270595772528,-55.24995));
#140743=CARTESIAN_POINT('',(0.,43.91999998,-55.24995));
#140744=CARTESIAN_POINT('Origin',(-29.5,-9.33460238845303,-55.74995));
#140745=CARTESIAN_POINT('',(-29.,43.91999998,-55.74995));
#140746=CARTESIAN_POINT('',(-29.,43.91999998,-55.74995));
#140747=CARTESIAN_POINT('Origin',(-29.5,43.91999998,-55.74995));
#140748=CARTESIAN_POINT('Origin',(-29.,-9.33460238845303,-92.34995));
#140749=CARTESIAN_POINT('',(-29.,38.7048160259599,-61.150138786574));
#140750=CARTESIAN_POINT('Ctrl Pts',(-29.,38.7048160259599,-61.150138786574));
#140751=CARTESIAN_POINT('Ctrl Pts',(-29.,38.7587438294333,-61.1488407776134));
#140752=CARTESIAN_POINT('Ctrl Pts',(-29.0000000000001,38.8125135208643,
-61.1445744929232));
#140753=CARTESIAN_POINT('Ctrl Pts',(-28.9999999999995,38.86581213546,-61.1374999313473));
#140754=CARTESIAN_POINT('Ctrl Pts',(-28.999999999999,38.9206199981767,-61.1302250405725));
#140755=CARTESIAN_POINT('Ctrl Pts',(-28.9999999999976,38.9749308760979,
-61.1199805166188));
#140756=CARTESIAN_POINT('Ctrl Pts',(-28.9999999999961,39.0284204191823,
-61.106886234665));
#140757=CARTESIAN_POINT('Ctrl Pts',(-28.9999999999946,39.0824266406301,
-61.0936654694441));
#140758=CARTESIAN_POINT('Ctrl Pts',(-28.9999999999932,39.135596867869,-61.0775394193));
#140759=CARTESIAN_POINT('Ctrl Pts',(-28.9999999999937,39.1875946577402,
-61.058579376025));
#140760=CARTESIAN_POINT('Ctrl Pts',(-28.999999999994,39.214574559218,-61.04874164829));
#140761=CARTESIAN_POINT('Ctrl Pts',(-28.9999999999949,39.2412386526437,
-61.0381401159529));
#140762=CARTESIAN_POINT('Ctrl Pts',(-28.999999999996,39.2675379042626,-61.0267795633669));
#140763=CARTESIAN_POINT('Ctrl Pts',(-28.999999999996,39.2679181300168,-61.02661531631));
#140764=CARTESIAN_POINT('Ctrl Pts',(-28.9999999999961,39.268298302465,-61.026450901664));
#140765=CARTESIAN_POINT('Ctrl Pts',(-28.9999999999961,39.268678421493,-61.0262863194886));
#140766=CARTESIAN_POINT('Ctrl Pts',(-29.0000000000039,39.4448840602191,
-60.9499936185261));
#140767=CARTESIAN_POINT('Ctrl Pts',(-29.,39.6087415856579,-60.8380654560188));
#140768=CARTESIAN_POINT('Ctrl Pts',(-29.,39.7446514854509,-60.6995134053984));
#140769=CARTESIAN_POINT('Ctrl Pts',(-29.,39.7447518137561,-60.6994111266649));
#140770=CARTESIAN_POINT('Ctrl Pts',(-29.,39.744852125437,-60.6993088358292));
#140771=CARTESIAN_POINT('Ctrl Pts',(-29.,39.7449524204946,-60.6992065328918));
#140772=CARTESIAN_POINT('Ctrl Pts',(-28.9999999999999,39.812931097784,-60.6298669408688));
#140773=CARTESIAN_POINT('Ctrl Pts',(-29.,39.8732750955302,-60.554966232983));
#140774=CARTESIAN_POINT('Ctrl Pts',(-29.,39.9261853767363,-60.4746513000797));
#140775=CARTESIAN_POINT('Ctrl Pts',(-29.,39.9261884127568,-60.4746466915656));
#140776=CARTESIAN_POINT('Ctrl Pts',(-29.,39.9261914487538,-60.4746420830303));
#140777=CARTESIAN_POINT('Ctrl Pts',(-29.,39.9261944847274,-60.4746374744739));
#140778=CARTESIAN_POINT('Ctrl Pts',(-29.,39.9791069872138,-60.3943171935884));
#140779=CARTESIAN_POINT('Ctrl Pts',(-29.0000000000001,40.0249202649622,
-60.3075521828599));
#140780=CARTESIAN_POINT('Ctrl Pts',(-28.9999999999999,40.0614666645048,
-60.2182183202257));
#140781=CARTESIAN_POINT('Ctrl Pts',(-28.9999999999999,40.0615163877946,
-60.218096776829));
#140782=CARTESIAN_POINT('Ctrl Pts',(-28.9999999999999,40.0615660940304,
-60.2179752284374));
#140783=CARTESIAN_POINT('Ctrl Pts',(-28.9999999999999,40.0616157832065,
-60.2178536750606));
#140784=CARTESIAN_POINT('Ctrl Pts',(-28.9999999999996,40.0995205469999,
-60.1251282086843));
#140785=CARTESIAN_POINT('Ctrl Pts',(-28.9999999999997,40.1280273344111,
-60.0287688634752));
#140786=CARTESIAN_POINT('Ctrl Pts',(-28.9999999999998,40.1466650082864,
-59.9302710126536));
#140787=CARTESIAN_POINT('Ctrl Pts',(-29.,40.1639177847726,-59.8390921769273));
#140788=CARTESIAN_POINT('Ctrl Pts',(-29.,40.1727138277874,-59.746082025009));
#140789=CARTESIAN_POINT('Ctrl Pts',(-29.,40.1727138277873,-59.6524466674074));
#140790=CARTESIAN_POINT('',(-29.,38.2024209812184,-61.4386408691297));
#140791=CARTESIAN_POINT('Ctrl Pts',(-29.,38.2024209812184,-61.4386408691297));
#140792=CARTESIAN_POINT('Ctrl Pts',(-29.,38.2265260808242,-61.3934796764616));
#140793=CARTESIAN_POINT('Ctrl Pts',(-29.,38.2570947542809,-61.3534209131338));
#140794=CARTESIAN_POINT('Ctrl Pts',(-29.,38.293280667393,-61.3178293882391));
#140795=CARTESIAN_POINT('Ctrl Pts',(-29.,38.3294709547425,-61.2822335609581));
#140796=CARTESIAN_POINT('Ctrl Pts',(-29.,38.3706505444737,-61.2520122466304));
#140797=CARTESIAN_POINT('Ctrl Pts',(-29.,38.4145916132166,-61.2276531730517));
#140798=CARTESIAN_POINT('Ctrl Pts',(-29.,38.4390337855644,-61.2141034645061));
#140799=CARTESIAN_POINT('Ctrl Pts',(-29.,38.4644512947928,-61.2023317240158));
#140800=CARTESIAN_POINT('Ctrl Pts',(-29.,38.490593259323,-61.1923093713145));
#140801=CARTESIAN_POINT('Ctrl Pts',(-29.,38.5172131854938,-61.1821037768321));
#140802=CARTESIAN_POINT('Ctrl Pts',(-29.,38.5445857496398,-61.1737118246007));
#140803=CARTESIAN_POINT('Ctrl Pts',(-29.,38.5724697430453,-61.1671525783509));
#140804=CARTESIAN_POINT('Ctrl Pts',(-29.,38.5996144829857,-61.1607672291985));
#140805=CARTESIAN_POINT('Ctrl Pts',(-29.,38.6272453201521,-61.1561187181941));
#140806=CARTESIAN_POINT('Ctrl Pts',(-29.,38.6551404973774,-61.1532723608215));
#140807=CARTESIAN_POINT('Ctrl Pts',(-29.,38.6716230181358,-61.1515905237032));
#140808=CARTESIAN_POINT('Ctrl Pts',(-29.,38.688197742811,-61.1505387782063));
#140809=CARTESIAN_POINT('Ctrl Pts',(-29.,38.7048160259599,-61.150138786574));
#140810=CARTESIAN_POINT('',(-29.,30.0207919771236,-76.4370443259982));
#140811=CARTESIAN_POINT('Ctrl Pts',(-29.,30.0207919771236,-76.4370443259982));
#140812=CARTESIAN_POINT('Ctrl Pts',(-29.,32.8015436034469,-71.4667836449984));
#140813=CARTESIAN_POINT('Ctrl Pts',(-29.,35.5206811754595,-66.4629124977081));
#140814=CARTESIAN_POINT('Ctrl Pts',(-29.,38.2024209812184,-61.4386408691297));
#140815=CARTESIAN_POINT('',(-29.,28.91999998,-80.9397703408579));
#140816=CARTESIAN_POINT('Ctrl Pts',(-29.,28.91999998,-80.9397703408579));
#140817=CARTESIAN_POINT('Ctrl Pts',(-29.,28.9199999800001,-80.5473141158908));
#140818=CARTESIAN_POINT('Ctrl Pts',(-29.,28.9425413961516,-80.1570353641503));
#140819=CARTESIAN_POINT('Ctrl Pts',(-29.,28.98734507234,-79.7689071194953));
#140820=CARTESIAN_POINT('Ctrl Pts',(-29.,29.0321487485283,-79.3807788748402));
#140821=CARTESIAN_POINT('Ctrl Pts',(-29.,29.0997153099482,-78.9928975232084));
#140822=CARTESIAN_POINT('Ctrl Pts',(-29.,29.1899491656343,-78.6129950217198));
#140823=CARTESIAN_POINT('Ctrl Pts',(-29.,29.2801830213205,-78.2330925202312));
#140824=CARTESIAN_POINT('Ctrl Pts',(-29.,29.3927364426023,-77.8611684636915));
#140825=CARTESIAN_POINT('Ctrl Pts',(-29.,29.5298914474149,-77.498038591685));
#140826=CARTESIAN_POINT('Ctrl Pts',(-29.,29.6670464522275,-77.1349087196785));
#140827=CARTESIAN_POINT('Ctrl Pts',(-29.,29.8286298518252,-76.7805111234986));
#140828=CARTESIAN_POINT('Ctrl Pts',(-29.,30.0207919771235,-76.4370443259982));
#140829=CARTESIAN_POINT('',(-29.,28.91999998,-91.34995));
#140830=CARTESIAN_POINT('',(-29.,28.91999998,-80.3749072158811));
#140831=CARTESIAN_POINT('Origin',(-29.,29.41999998,-91.34995));
#140832=CARTESIAN_POINT('',(-29.,46.41999998,-58.24995));
#140833=CARTESIAN_POINT('',(-29.,46.41999998,-92.34995));
#140834=CARTESIAN_POINT('Origin',(-29.,43.91999998,-58.24995));
#140835=CARTESIAN_POINT('Ctrl Pts',(-28.4933647440612,38.6927858841383,
-60.650327573148));
#140836=CARTESIAN_POINT('Ctrl Pts',(-29.,38.6926240909195,-60.6436056187277));
#140837=CARTESIAN_POINT('Ctrl Pts',(-29.,38.7048160259599,-61.150138786574));
#140838=CARTESIAN_POINT('Ctrl Pts',(-28.4870505338491,38.8213938162437,
-60.647315885492));
#140839=CARTESIAN_POINT('Ctrl Pts',(-29.0000000000007,38.8211017330502,
-60.6340675708554));
#140840=CARTESIAN_POINT('Ctrl Pts',(-29.,38.8968977730653,-61.1455154974199));
#140841=CARTESIAN_POINT('Ctrl Pts',(-28.4808526630789,38.9512642676271,
-60.6191174333591));
#140842=CARTESIAN_POINT('Ctrl Pts',(-28.9999999999993,38.9470356871939,
-60.5993042062512));
#140843=CARTESIAN_POINT('Ctrl Pts',(-29.,39.0908916037092,-61.103090199825));
#140844=CARTESIAN_POINT('Ctrl Pts',(-28.4702284641343,39.1877232210837,
-60.5175376561534));
#140845=CARTESIAN_POINT('Ctrl Pts',(-29.0000000000007,39.1728401027082,
-60.4895768580073));
#140846=CARTESIAN_POINT('Ctrl Pts',(-29.,39.4441857876827,-60.9504725910835));
#140847=CARTESIAN_POINT('Ctrl Pts',(-28.465656656414,39.2976315760154,-60.4428805969007));
#140848=CARTESIAN_POINT('Ctrl Pts',(-29.0000000000007,39.2753871003781,
-60.4130391624567));
#140849=CARTESIAN_POINT('Ctrl Pts',(-29.,39.6084483440092,-60.8383643971029));
#140850=CARTESIAN_POINT('Ctrl Pts',(-28.4606134496588,39.434276061177,-60.3041245704241));
#140851=CARTESIAN_POINT('Ctrl Pts',(-28.9999999999996,39.4020840949312,
-60.2760820218603));
#140852=CARTESIAN_POINT('Ctrl Pts',(-29.,39.8127532432739,-60.6300880930806));
#140853=CARTESIAN_POINT('Ctrl Pts',(-28.4592438293891,39.4746917169037,
-60.2541491598715));
#140854=CARTESIAN_POINT('Ctrl Pts',(-29.,39.439411822071,-60.2273142826608));
#140855=CARTESIAN_POINT('Ctrl Pts',(-29.,39.8731969861748,-60.5550848424531));
#140856=CARTESIAN_POINT('Ctrl Pts',(-28.4570887248156,39.5455314661108,
-60.1469471546371));
#140857=CARTESIAN_POINT('Ctrl Pts',(-29.,39.5049075987374,-60.1236050817051));
#140858=CARTESIAN_POINT('Ctrl Pts',(-29.,39.9791737873547,-60.3942177709194));
#140859=CARTESIAN_POINT('Ctrl Pts',(-28.4563005932054,39.5761796095201,
-60.0890325252997));
#140860=CARTESIAN_POINT('Ctrl Pts',(-29.0000000000002,39.5332188379146,
-60.0680634823705));
#140861=CARTESIAN_POINT('Ctrl Pts',(-29.,40.025042572592,-60.3073218018945));
#140862=CARTESIAN_POINT('Ctrl Pts',(-28.4548707416055,39.6494517959669,
-59.9101257001469));
#140863=CARTESIAN_POINT('Ctrl Pts',(-28.9999999999997,39.6014080499751,
-59.8970923098554));
#140864=CARTESIAN_POINT('Ctrl Pts',(-29.,40.1347632142717,-60.0389178342029));
#140865=CARTESIAN_POINT('Ctrl Pts',(-28.4551199545093,39.6747304042147,
-59.7821590925224));
#140866=CARTESIAN_POINT('Ctrl Pts',(-29.,39.6256255569264,-59.7761492712348));
#140867=CARTESIAN_POINT('Ctrl Pts',(-29.,40.1727138319509,-59.8469756744913));
#140868=CARTESIAN_POINT('Ctrl Pts',(-28.4564221286262,39.6746164787415,
-59.6524466674074));
#140869=CARTESIAN_POINT('Ctrl Pts',(-29.,39.6270595772528,-59.6524466674074));
#140870=CARTESIAN_POINT('Ctrl Pts',(-29.,40.1727138277874,-59.6524466674074));
#140871=CARTESIAN_POINT('Origin',(-28.5,38.7048160259599,-61.150138786574));
#140872=CARTESIAN_POINT('Ctrl Pts',(-39.,37.7046087726872,-61.14995));
#140873=CARTESIAN_POINT('Ctrl Pts',(-39.,37.7046087726872,-60.64995));
#140874=CARTESIAN_POINT('Ctrl Pts',(-39.5,37.7046087726872,-60.64995));
#140875=CARTESIAN_POINT('Ctrl Pts',(-39.,37.9017438633342,-61.149949999985));
#140876=CARTESIAN_POINT('Ctrl Pts',(-38.9999999999973,37.8357552425198,
-60.655621796981));
#140877=CARTESIAN_POINT('Ctrl Pts',(-39.4942946417934,37.8365313206165,
-60.64995));
#140878=CARTESIAN_POINT('Ctrl Pts',(-39.,38.0987303642205,-61.110909009472));
#140879=CARTESIAN_POINT('Ctrl Pts',(-39.,37.9700367301949,-60.6353187454024));
#140880=CARTESIAN_POINT('Ctrl Pts',(-39.4885935839755,37.9683544324696,
-60.6239226729818));
#140881=CARTESIAN_POINT('Ctrl Pts',(-39.,38.4629228438758,-60.9606295880618));
#140882=CARTESIAN_POINT('Ctrl Pts',(-39.,38.2214119490388,-60.5426326522478));
#140883=CARTESIAN_POINT('Ctrl Pts',(-39.4780533572395,38.2120715692569,
-60.5237363920407));
#140884=CARTESIAN_POINT('Ctrl Pts',(-39.,38.6299500658835,-60.8494502533514));
#140885=CARTESIAN_POINT('Ctrl Pts',(-39.,38.3387190323947,-60.4706504746467));
#140886=CARTESIAN_POINT('Ctrl Pts',(-39.4732193617859,38.3238459703974,
-60.4496168355678));
#140887=CARTESIAN_POINT('Ctrl Pts',(-39.,38.9086909221403,-60.5717700902082));
#140888=CARTESIAN_POINT('Ctrl Pts',(-39.,38.5356496464585,-60.2852157712116));
#140889=CARTESIAN_POINT('Ctrl Pts',(-39.4651522214979,38.5103789912237,
-60.2644967268053));
#140890=CARTESIAN_POINT('Ctrl Pts',(-39.,39.0202949438762,-60.4053784571342));
#140891=CARTESIAN_POINT('Ctrl Pts',(-39.,38.6156677780068,-60.1718710142637));
#140892=CARTESIAN_POINT('Ctrl Pts',(-39.4619222489988,38.5850642583582,
-60.153568971423));
#140893=CARTESIAN_POINT('Ctrl Pts',(-39.,39.1711484082035,-60.0425718399611));
#140894=CARTESIAN_POINT('Ctrl Pts',(-39.,38.7237795941064,-59.9224177216067));
#140895=CARTESIAN_POINT('Ctrl Pts',(-39.4575563441359,38.6860152017583,
-59.9116978933072));
#140896=CARTESIAN_POINT('Ctrl Pts',(-39.,39.2103385289879,-59.8463349320561));
#140897=CARTESIAN_POINT('Ctrl Pts',(-39.,38.7521729419779,-59.7861314644994));
#140898=CARTESIAN_POINT('Ctrl Pts',(-39.4564221286291,38.7122411799561,
-59.7808732880376));
#140899=CARTESIAN_POINT('Ctrl Pts',(-39.,39.2103385290023,-59.64995));
#140900=CARTESIAN_POINT('Ctrl Pts',(-39.,38.7521729419935,-59.64995));
#140901=CARTESIAN_POINT('Ctrl Pts',(-39.4564221286262,38.7122411799564,
-59.64995));
#140902=CARTESIAN_POINT('',(-39.,37.7046087726872,-61.14995));
#140903=CARTESIAN_POINT('Origin',(-39.5,37.7046087726872,-61.14995));
#140904=CARTESIAN_POINT('Ctrl Pts',(-39.,39.2103385290022,-59.64995));
#140905=CARTESIAN_POINT('Ctrl Pts',(-39.,39.2103385289878,-59.8463349320561));
#140906=CARTESIAN_POINT('Ctrl Pts',(-39.,39.1711484082035,-60.0425718399611));
#140907=CARTESIAN_POINT('Ctrl Pts',(-39.,39.0957216760398,-60.2239751485477));
#140908=CARTESIAN_POINT('Ctrl Pts',(-39.,39.0202949438762,-60.4053784571342));
#140909=CARTESIAN_POINT('Ctrl Pts',(-39.,38.9086909221403,-60.5717700902082));
#140910=CARTESIAN_POINT('Ctrl Pts',(-39.,38.7693204940119,-60.7106101717798));
#140911=CARTESIAN_POINT('Ctrl Pts',(-39.,38.6299500658835,-60.8494502533514));
#140912=CARTESIAN_POINT('Ctrl Pts',(-39.,38.4629228438757,-60.9606295880618));
#140913=CARTESIAN_POINT('Ctrl Pts',(-39.,38.2808266040481,-61.0357692987669));
#140914=CARTESIAN_POINT('Ctrl Pts',(-39.,38.0987303642205,-61.110909009472));
#140915=CARTESIAN_POINT('Ctrl Pts',(-39.,37.9017438633342,-61.149949999985));
#140916=CARTESIAN_POINT('Ctrl Pts',(-39.,37.7046087726872,-61.14995));
#140917=CARTESIAN_POINT('Origin',(-39.,46.91999998,-129.34995));
#140918=CARTESIAN_POINT('',(-39.,31.080768958446,-61.14995));
#140919=CARTESIAN_POINT('',(-39.,31.080768958446,-91.9958480337503));
#140920=CARTESIAN_POINT('',(-39.,31.080768958446,-129.34995));
#140921=CARTESIAN_POINT('',(-39.,31.080768958446,-61.14995));
#140922=CARTESIAN_POINT('',(-39.,43.91999998,-55.74995));
#140923=CARTESIAN_POINT('',(-39.,46.91999998,-55.74995));
#140924=CARTESIAN_POINT('',(-39.,46.41999998,-58.24995));
#140925=CARTESIAN_POINT('Origin',(-39.,43.91999998,-58.24995));
#140926=CARTESIAN_POINT('',(-39.,46.41999998,-91.9958480337503));
#140927=CARTESIAN_POINT('',(-39.,46.41999998,-129.34995));
#140928=CARTESIAN_POINT('',(-39.,46.41999998,-91.9958480337503));
#140929=CARTESIAN_POINT('Origin',(-38.5,-1.68631645800828E-14,-55.74995));
#140930=CARTESIAN_POINT('',(-38.5,43.91999998,-55.24995));
#140931=CARTESIAN_POINT('',(-38.5,-1.68631645800828E-14,-55.24995));
#140932=CARTESIAN_POINT('Origin',(-38.5,43.91999998,-55.74995));
#140933=CARTESIAN_POINT('Origin',(0.,0.,-55.24995));
#140934=CARTESIAN_POINT('',(-38.,43.91999998,-55.24995));
#140935=CARTESIAN_POINT('',(-38.,38.8834059372824,-55.24995));
#140936=CARTESIAN_POINT('',(0.,43.91999998,-55.24995));
#140937=CARTESIAN_POINT('Origin',(-38.,-9.33460238845303,-55.74995));
#140938=CARTESIAN_POINT('',(-37.5,43.91999998,-55.74995));
#140939=CARTESIAN_POINT('',(-37.5,43.91999998,-55.74995));
#140940=CARTESIAN_POINT('Origin',(-38.,43.91999998,-55.74995));
#140941=CARTESIAN_POINT('Origin',(-37.5,-9.33460238845303,-92.34995));
#140942=CARTESIAN_POINT('',(-37.5,46.41999998,-58.24995));
#140943=CARTESIAN_POINT('',(-37.5,46.41999998,-92.34995));
#140944=CARTESIAN_POINT('Origin',(-37.5,43.91999998,-58.24995));
#140945=CARTESIAN_POINT('',(-37.5,33.02054075664,-61.14995));
#140946=CARTESIAN_POINT('',(-37.5,-9.33460238845303,-61.14995));
#140947=CARTESIAN_POINT('',(-37.5,32.4374646344434,-61.4386408691296));
#140948=CARTESIAN_POINT('Ctrl Pts',(-37.5,32.4374646344434,-61.4386408691296));
#140949=CARTESIAN_POINT('Ctrl Pts',(-37.5,32.4670379954265,-61.3894770341505));
#140950=CARTESIAN_POINT('Ctrl Pts',(-37.5,32.5044515673201,-61.3474771045912));
#140951=CARTESIAN_POINT('Ctrl Pts',(-37.5,32.5478217582305,-61.3109844882787));
#140952=CARTESIAN_POINT('Ctrl Pts',(-37.5,32.5912010725173,-61.2744841953601));
#140953=CARTESIAN_POINT('Ctrl Pts',(-37.5,32.6399569706336,-61.2443658937749));
#140954=CARTESIAN_POINT('Ctrl Pts',(-37.5,32.6911307205588,-61.2206312870705));
#140955=CARTESIAN_POINT('Ctrl Pts',(-37.5,32.7200261312687,-61.2072294705187));
#140956=CARTESIAN_POINT('Ctrl Pts',(-37.5,32.7497820420349,-61.1958060470671));
#140957=CARTESIAN_POINT('Ctrl Pts',(-37.5,32.7801663767934,-61.1862777806123));
#140958=CARTESIAN_POINT('Ctrl Pts',(-37.5,32.8113193812834,-61.1765084659306));
#140959=CARTESIAN_POINT('Ctrl Pts',(-37.5,32.8431343593207,-61.168731309436));
#140960=CARTESIAN_POINT('Ctrl Pts',(-37.5,32.8753810744804,-61.1629086143648));
#140961=CARTESIAN_POINT('Ctrl Pts',(-37.5,32.9073189135581,-61.1571416921447));
#140962=CARTESIAN_POINT('Ctrl Pts',(-37.5,32.9396816981554,-61.1532921099755));
#140963=CARTESIAN_POINT('Ctrl Pts',(-37.5,32.9722439056897,-61.1513728702169));
#140964=CARTESIAN_POINT('Ctrl Pts',(-37.5,32.9883041294272,-61.1504262691642));
#140965=CARTESIAN_POINT('Ctrl Pts',(-37.5,33.0044127038511,-61.14995));
#140966=CARTESIAN_POINT('Ctrl Pts',(-37.5,33.02054075664,-61.14995));
#140967=CARTESIAN_POINT('',(-37.5,30.3198029183596,-64.9254179945056));
#140968=CARTESIAN_POINT('Ctrl Pts',(-37.5,30.3198029183591,-64.9254179945063));
#140969=CARTESIAN_POINT('Ctrl Pts',(-37.5,31.0308541172825,-63.7662953234662));
#140970=CARTESIAN_POINT('Ctrl Pts',(-37.5,31.7365266751429,-62.6039057229559));
#140971=CARTESIAN_POINT('Ctrl Pts',(-37.5,32.4374646344434,-61.4386408691296));
#140972=CARTESIAN_POINT('',(-37.5,28.91999998,-70.4461836365688));
#140973=CARTESIAN_POINT('Ctrl Pts',(-37.5,28.91999998,-70.4461836365688));
#140974=CARTESIAN_POINT('Ctrl Pts',(-37.5,28.91999998,-69.9121746574189));
#140975=CARTESIAN_POINT('Ctrl Pts',(-37.5,28.9527491161432,-69.3820227305135));
#140976=CARTESIAN_POINT('Ctrl Pts',(-37.5,29.0202545273688,-68.8559643077599));
#140977=CARTESIAN_POINT('Ctrl Pts',(-37.5,29.0748216912419,-68.4307314910118));
#140978=CARTESIAN_POINT('Ctrl Pts',(-37.5,29.1520996751857,-68.0081734812099));
#140979=CARTESIAN_POINT('Ctrl Pts',(-37.5,29.2531734731887,-67.5884180460506));
#140980=CARTESIAN_POINT('Ctrl Pts',(-37.5,29.3662299152087,-67.1188991701864));
#140981=CARTESIAN_POINT('Ctrl Pts',(-37.5,29.5081290337322,-66.6603034853492));
#140982=CARTESIAN_POINT('Ctrl Pts',(-37.5,29.6832395831696,-66.2153982561153));
#140983=CARTESIAN_POINT('Ctrl Pts',(-37.5,29.813724236086,-65.883874515234));
#140984=CARTESIAN_POINT('Ctrl Pts',(-37.5,29.9624113407314,-65.5596714884752));
#140985=CARTESIAN_POINT('Ctrl Pts',(-37.5,30.1346313217948,-65.2449329573506));
#140986=CARTESIAN_POINT('Ctrl Pts',(-37.5,30.1935307469916,-65.137292029416));
#140987=CARTESIAN_POINT('Ctrl Pts',(-37.5,30.2551830721499,-65.0307582682135));
#140988=CARTESIAN_POINT('Ctrl Pts',(-37.5,30.3198029183595,-64.9254179945056));
#140989=CARTESIAN_POINT('',(-37.5,28.91999998,-91.34995));
#140990=CARTESIAN_POINT('',(-37.5,28.91999998,-69.7748183683767));
#140991=CARTESIAN_POINT('Origin',(-37.5,29.41999998,-91.34995));
#140992=CARTESIAN_POINT('Origin',(0.,-12.9675000200281,-60.64995));
#140993=CARTESIAN_POINT('',(-48.4322308821779,20.76999998,-60.64995));
#140994=CARTESIAN_POINT('',(-43.9604906504041,26.41999998,-60.64995));
#140995=CARTESIAN_POINT('Origin',(0.,-12.9675000200281,-60.64995));
#140996=CARTESIAN_POINT('',(-1.41024658483895E-14,20.76999998,-60.64995));
#140997=CARTESIAN_POINT('',(-1.64641978096591E-14,26.4199999800001,-60.64995));
#140998=CARTESIAN_POINT('Ctrl Pts',(-51.6895836746289,26.3764221086262,
-59.64995));
#140999=CARTESIAN_POINT('Ctrl Pts',(-51.6420267731401,26.91999998,-59.64995));
#141000=CARTESIAN_POINT('Ctrl Pts',(-52.1876810236747,26.91999998,-59.64995));
#141001=CARTESIAN_POINT('Ctrl Pts',(-51.6895836746287,26.3764221086278,
-59.7808732880375));
#141002=CARTESIAN_POINT('Ctrl Pts',(-51.6420267731333,26.919999980002,-59.7746029379318));
#141003=CARTESIAN_POINT('Ctrl Pts',(-52.1876810236604,26.91999998,-59.8463349320561));
#141004=CARTESIAN_POINT('Ctrl Pts',(-51.6633576964307,26.3775563241358,
-59.9116978933072));
#141005=CARTESIAN_POINT('Ctrl Pts',(-51.6186060348034,26.9199999800004,
-59.8989712332639));
#141006=CARTESIAN_POINT('Ctrl Pts',(-52.148490902876,26.91999998,-60.0425718399612));
#141007=CARTESIAN_POINT('Ctrl Pts',(-51.5624067530308,26.3819222289988,
-60.1535689714229));
#141008=CARTESIAN_POINT('Ctrl Pts',(-51.5267774915774,26.9199999799997,
-60.1322291512607));
#141009=CARTESIAN_POINT('Ctrl Pts',(-51.9976374385487,26.91999998,-60.4053784571341));
#141010=CARTESIAN_POINT('Ctrl Pts',(-51.4877214858962,26.3851522014976,
-60.2644967268053));
#141011=CARTESIAN_POINT('Ctrl Pts',(-51.4587108395762,26.9199999799996,
-60.2406767152617));
#141012=CARTESIAN_POINT('Ctrl Pts',(-51.8860334168128,26.91999998,-60.5717700902076));
#141013=CARTESIAN_POINT('Ctrl Pts',(-51.3011884650699,26.3932193417862,
-60.4496168355678));
#141014=CARTESIAN_POINT('Ctrl Pts',(-51.2846839917031,26.9199999800004,
-60.4261994932779));
#141015=CARTESIAN_POINT('Ctrl Pts',(-51.6072925605561,26.91999998,-60.8494502533521));
#141016=CARTESIAN_POINT('Ctrl Pts',(-51.1894140639292,26.3980533372399,
-60.5237363920408));
#141017=CARTESIAN_POINT('Ctrl Pts',(-51.1792534074218,26.9199999799993,
-60.5031527166058));
#141018=CARTESIAN_POINT('Ctrl Pts',(-51.4402653385482,26.91999998,-60.9606295880611));
#141019=CARTESIAN_POINT('Ctrl Pts',(-50.9456969271423,26.4085935639752,
-60.6239226729817));
#141020=CARTESIAN_POINT('Ctrl Pts',(-50.9439864347103,26.9199999800007,
-60.6120353079387));
#141021=CARTESIAN_POINT('Ctrl Pts',(-51.0760728588929,26.91999998,-61.1109090094727));
#141022=CARTESIAN_POINT('Ctrl Pts',(-50.8138738152888,26.4142946217921,
-60.64995));
#141023=CARTESIAN_POINT('Ctrl Pts',(-50.8146696888639,26.9199999800028,
-60.6442102195338));
#141024=CARTESIAN_POINT('Ctrl Pts',(-50.8790863580067,26.91999998,-61.149949999985));
#141025=CARTESIAN_POINT('Ctrl Pts',(-50.6819512673597,26.41999998,-60.64995));
#141026=CARTESIAN_POINT('Ctrl Pts',(-50.6819512673597,26.91999998,-60.64995));
#141027=CARTESIAN_POINT('Ctrl Pts',(-50.6819512673597,26.91999998,-61.14995));
#141028=CARTESIAN_POINT('',(-50.6819512673597,26.91999998,-61.14995));
#141029=CARTESIAN_POINT('Ctrl Pts',(-52.1876810236747,26.91999998,-59.64995));
#141030=CARTESIAN_POINT('Ctrl Pts',(-52.1876810236604,26.91999998,-59.8463349320561));
#141031=CARTESIAN_POINT('Ctrl Pts',(-52.148490902876,26.91999998,-60.0425718399612));
#141032=CARTESIAN_POINT('Ctrl Pts',(-51.9976374385487,26.91999998,-60.4053784571341));
#141033=CARTESIAN_POINT('Ctrl Pts',(-51.8860334168128,26.91999998,-60.5717700902076));
#141034=CARTESIAN_POINT('Ctrl Pts',(-51.6072925605561,26.91999998,-60.8494502533521));
#141035=CARTESIAN_POINT('Ctrl Pts',(-51.4402653385482,26.91999998,-60.9606295880611));
#141036=CARTESIAN_POINT('Ctrl Pts',(-51.0760728588929,26.91999998,-61.1109090094727));
#141037=CARTESIAN_POINT('Ctrl Pts',(-50.8790863580067,26.91999998,-61.149949999985));
#141038=CARTESIAN_POINT('Ctrl Pts',(-50.6819512673597,26.91999998,-61.14995));
#141039=CARTESIAN_POINT('Origin',(-50.6819512673597,26.41999998,-61.14995));
#141040=CARTESIAN_POINT('Ctrl Pts',(-51.1762622162812,20.76999998,-60.64995));
#141041=CARTESIAN_POINT('Ctrl Pts',(-51.1762622162812,20.26999998,-60.64995));
#141042=CARTESIAN_POINT('Ctrl Pts',(-51.1762622162812,20.26999998,-61.14995));
#141043=CARTESIAN_POINT('Ctrl Pts',(-51.3081847642104,20.764294621792,-60.64995));
#141044=CARTESIAN_POINT('Ctrl Pts',(-51.3074086861135,20.2699999799973,
-60.6556217969837));
#141045=CARTESIAN_POINT('Ctrl Pts',(-51.3733973069281,20.26999998,-61.149949999985));
#141046=CARTESIAN_POINT('Ctrl Pts',(-51.4400078760636,20.7585935639752,
-60.6239226729818));
#141047=CARTESIAN_POINT('Ctrl Pts',(-51.4416901737888,20.2699999799993,
-60.6353187454032));
#141048=CARTESIAN_POINT('Ctrl Pts',(-51.5703838078145,20.26999998,-61.1109090094727));
#141049=CARTESIAN_POINT('Ctrl Pts',(-51.6837250128509,20.7480533372398,
-60.5237363920407));
#141050=CARTESIAN_POINT('Ctrl Pts',(-51.6930653926326,20.2699999800007,
-60.5426326522471));
#141051=CARTESIAN_POINT('Ctrl Pts',(-51.9345762874696,20.26999998,-60.9606295880612));
#141052=CARTESIAN_POINT('Ctrl Pts',(-51.7954994139911,20.7432193417859,
-60.4496168355681));
#141053=CARTESIAN_POINT('Ctrl Pts',(-51.810372475988,20.2699999799993,-60.4706504746462));
#141054=CARTESIAN_POINT('Ctrl Pts',(-52.1016035094776,20.26999998,-60.849450253352));
#141055=CARTESIAN_POINT('Ctrl Pts',(-51.9820324348179,20.7351522014979,
-60.264496726805));
#141056=CARTESIAN_POINT('Ctrl Pts',(-52.007303090053,20.2699999800007,-60.2852157712124));
#141057=CARTESIAN_POINT('Ctrl Pts',(-52.3803443657342,20.26999998,-60.5717700902076));
#141058=CARTESIAN_POINT('Ctrl Pts',(-52.0567177019522,20.7319222289985,
-60.153568971423));
#141059=CARTESIAN_POINT('Ctrl Pts',(-52.0873212216015,20.2699999800003,
-60.1718710142637));
#141060=CARTESIAN_POINT('Ctrl Pts',(-52.4919483874702,20.26999998,-60.4053784571342));
#141061=CARTESIAN_POINT('Ctrl Pts',(-52.1576686453522,20.7275563241362,
-59.9116978933072));
#141062=CARTESIAN_POINT('Ctrl Pts',(-52.1954330376997,20.2699999799997,
-59.9224177216067));
#141063=CARTESIAN_POINT('Ctrl Pts',(-52.6428018517975,20.26999998,-60.0425718399611));
#141064=CARTESIAN_POINT('Ctrl Pts',(-52.1838946235501,20.7264221086281,
-59.7808732880376));
#141065=CARTESIAN_POINT('Ctrl Pts',(-52.2238263855712,20.2699999800007,
-59.7861314644994));
#141066=CARTESIAN_POINT('Ctrl Pts',(-52.6819919725819,20.26999998,-59.8463349320562));
#141067=CARTESIAN_POINT('Ctrl Pts',(-52.1838946235503,20.7264221086262,
-59.64995));
#141068=CARTESIAN_POINT('Ctrl Pts',(-52.2238263855875,20.26999998,-59.6499499999999));
#141069=CARTESIAN_POINT('Ctrl Pts',(-52.6819919725962,20.26999998,-59.64995));
#141070=CARTESIAN_POINT('',(-51.1762622162812,20.26999998,-61.14995));
#141071=CARTESIAN_POINT('Origin',(-51.1762622162812,20.76999998,-61.14995));
#141072=CARTESIAN_POINT('Ctrl Pts',(-51.1762622162812,20.26999998,-61.14995));
#141073=CARTESIAN_POINT('Ctrl Pts',(-51.3733973069281,20.26999998,-61.149949999985));
#141074=CARTESIAN_POINT('Ctrl Pts',(-51.5703838078145,20.26999998,-61.1109090094727));
#141075=CARTESIAN_POINT('Ctrl Pts',(-51.9345762874696,20.26999998,-60.9606295880612));
#141076=CARTESIAN_POINT('Ctrl Pts',(-52.1016035094776,20.26999998,-60.849450253352));
#141077=CARTESIAN_POINT('Ctrl Pts',(-52.3803443657342,20.26999998,-60.5717700902076));
#141078=CARTESIAN_POINT('Ctrl Pts',(-52.4919483874702,20.26999998,-60.4053784571342));
#141079=CARTESIAN_POINT('Ctrl Pts',(-52.6428018517975,20.26999998,-60.0425718399611));
#141080=CARTESIAN_POINT('Ctrl Pts',(-52.6819919725819,20.26999998,-59.8463349320562));
#141081=CARTESIAN_POINT('Ctrl Pts',(-52.6819919725962,20.26999998,-59.64995));
#141082=CARTESIAN_POINT('Origin',(83.2809572255632,26.9199999800001,-55.24995));
#141083=CARTESIAN_POINT('',(-49.6616970192851,26.91999998,-171.14995));
#141084=CARTESIAN_POINT('',(-51.176438378063,26.91999998,-172.64995));
#141085=CARTESIAN_POINT('Ctrl Pts',(-49.6616970192851,26.91999998,-171.14995));
#141086=CARTESIAN_POINT('Ctrl Pts',(-49.8600119386601,26.91999998,-171.149950000016));
#141087=CARTESIAN_POINT('Ctrl Pts',(-50.058177378641,26.91999998,-171.18899099047));
#141088=CARTESIAN_POINT('Ctrl Pts',(-50.4245495045741,26.91999998,-171.339270411997));
#141089=CARTESIAN_POINT('Ctrl Pts',(-50.5925763632168,26.91999998,-171.450449746589));
#141090=CARTESIAN_POINT('Ctrl Pts',(-50.8729854484245,26.91999998,-171.728129909852));
#141091=CARTESIAN_POINT('Ctrl Pts',(-50.9852574060669,26.91999998,-171.894521542842));
#141092=CARTESIAN_POINT('Ctrl Pts',(-51.1370137093498,26.91999998,-172.257328160063));
#141093=CARTESIAN_POINT('Ctrl Pts',(-51.176438378046,26.91999998,-172.453565067926));
#141094=CARTESIAN_POINT('Ctrl Pts',(-51.176438378063,26.91999998,-172.64995));
#141095=CARTESIAN_POINT('',(-44.1114262156583,26.91999998,-171.14995));
#141096=CARTESIAN_POINT('',(-49.5914266019339,26.91999998,-171.14995));
#141097=CARTESIAN_POINT('',(-43.5020331013479,26.91999998,-170.861259130871));
#141098=CARTESIAN_POINT('Ctrl Pts',(-43.5020331013479,26.91999998,-170.861259130871));
#141099=CARTESIAN_POINT('Ctrl Pts',(-43.5336466193108,26.91999998,-170.911515457779));
#141100=CARTESIAN_POINT('Ctrl Pts',(-43.5734840835972,26.91999998,-170.953836204196));
#141101=CARTESIAN_POINT('Ctrl Pts',(-43.61923735557,26.91999998,-170.99036760152));
#141102=CARTESIAN_POINT('Ctrl Pts',(-43.6650022527906,26.91999998,-171.026908280947));
#141103=CARTESIAN_POINT('Ctrl Pts',(-43.7162207484477,26.91999998,-171.056845311872));
#141104=CARTESIAN_POINT('Ctrl Pts',(-43.7696000450754,26.91999998,-171.080313003677));
#141105=CARTESIAN_POINT('Ctrl Pts',(-43.8006630727512,26.91999998,-171.093969563544));
#141106=CARTESIAN_POINT('Ctrl Pts',(-43.8326179990562,26.91999998,-171.105532778688));
#141107=CARTESIAN_POINT('Ctrl Pts',(-43.8652115257657,26.91999998,-171.115097339925));
#141108=CARTESIAN_POINT('Ctrl Pts',(-43.8987093663282,26.91999998,-171.124927271807));
#141109=CARTESIAN_POINT('Ctrl Pts',(-43.9328831236168,26.91999998,-171.132646173148));
#141110=CARTESIAN_POINT('Ctrl Pts',(-43.9674767132984,26.91999998,-171.138304320373));
#141111=CARTESIAN_POINT('Ctrl Pts',(-44.0018197383425,26.91999998,-171.143921485104));
#141112=CARTESIAN_POINT('Ctrl Pts',(-44.0365780353935,26.91999998,-171.147507459409));
#141113=CARTESIAN_POINT('Ctrl Pts',(-44.0714975023722,26.91999998,-171.149061689887));
#141114=CARTESIAN_POINT('Ctrl Pts',(-44.0847888272127,26.91999998,-171.149653273435));
#141115=CARTESIAN_POINT('Ctrl Pts',(-44.0981033481738,26.91999998,-171.14995));
#141116=CARTESIAN_POINT('Ctrl Pts',(-44.1114262156583,26.91999998,-171.14995));
#141117=CARTESIAN_POINT('',(-41.0569324495328,26.91999998,-167.025025538602));
#141118=CARTESIAN_POINT('Ctrl Pts',(-41.0569324495328,26.91999998,-167.025025538602));
#141119=CARTESIAN_POINT('Ctrl Pts',(-41.879954591083,26.91999998,-168.29867810854));
#141120=CARTESIAN_POINT('Ctrl Pts',(-42.6945981803054,26.91999998,-169.577671730211));
#141121=CARTESIAN_POINT('Ctrl Pts',(-43.502033101348,26.91999998,-170.861259130871));
#141122=CARTESIAN_POINT('',(-39.5,26.91999998,-161.0070032805));
#141123=CARTESIAN_POINT('Ctrl Pts',(-39.5,26.91999998,-161.0070032805));
#141124=CARTESIAN_POINT('Ctrl Pts',(-39.5,26.91999998,-161.534495292789));
#141125=CARTESIAN_POINT('Ctrl Pts',(-39.5301402469972,26.91999998,-162.058113878039));
#141126=CARTESIAN_POINT('Ctrl Pts',(-39.5903041384792,26.91999998,-162.577874021264));
#141127=CARTESIAN_POINT('Ctrl Pts',(-39.6504680299611,26.91999998,-163.097634164489));
#141128=CARTESIAN_POINT('Ctrl Pts',(-39.7405665669947,26.91999998,-163.613547303305));
#141129=CARTESIAN_POINT('Ctrl Pts',(-39.864660766352,26.91999998,-164.12509154227));
#141130=CARTESIAN_POINT('Ctrl Pts',(-39.9267078660346,26.91999998,-164.380863661769));
#141131=CARTESIAN_POINT('Ctrl Pts',(-39.997456507107,26.91999998,-164.6357182099));
#141132=CARTESIAN_POINT('Ctrl Pts',(-40.0767145462179,26.91999998,-164.886071972517));
#141133=CARTESIAN_POINT('Ctrl Pts',(-40.1559725853186,26.91999998,-165.136425735101));
#141134=CARTESIAN_POINT('Ctrl Pts',(-40.2438971237555,26.91999998,-165.383070268404));
#141135=CARTESIAN_POINT('Ctrl Pts',(-40.3414754155803,26.91999998,-165.625583031388));
#141136=CARTESIAN_POINT('Ctrl Pts',(-40.4688793539746,26.91999998,-165.942221912202));
#141137=CARTESIAN_POINT('Ctrl Pts',(-40.6122052010756,26.91999998,-166.252046258618));
#141138=CARTESIAN_POINT('Ctrl Pts',(-40.7764339005815,26.91999998,-166.552924284045));
#141139=CARTESIAN_POINT('Ctrl Pts',(-40.8637697314878,26.91999998,-166.712929401488));
#141140=CARTESIAN_POINT('Ctrl Pts',(-40.9570176103092,26.91999998,-166.870404192079));
#141141=CARTESIAN_POINT('Ctrl Pts',(-41.0569324495327,26.91999998,-167.025025538601));
#141142=CARTESIAN_POINT('',(-39.5,26.91999998,-71.0516396909898));
#141143=CARTESIAN_POINT('',(-39.5,26.91999998,-55.24995));
#141144=CARTESIAN_POINT('',(-41.0569324495432,26.91999998,-65.0336174328882));
#141145=CARTESIAN_POINT('Ctrl Pts',(-41.0569324495432,26.91999998,-65.0336174328882));
#141146=CARTESIAN_POINT('Ctrl Pts',(-40.8648408575281,26.91999998,-65.3308851945513));
#141147=CARTESIAN_POINT('Ctrl Pts',(-40.6972294070533,26.91999998,-65.6389714709844));
#141148=CARTESIAN_POINT('Ctrl Pts',(-40.5488568184254,26.91999998,-65.9555599509487));
#141149=CARTESIAN_POINT('Ctrl Pts',(-40.4750173837546,26.91999998,-66.1131140827463));
#141150=CARTESIAN_POINT('Ctrl Pts',(-40.4059436807373,26.91999998,-66.2727743327574));
#141151=CARTESIAN_POINT('Ctrl Pts',(-40.3409938376608,26.91999998,-66.4342570423367));
#141152=CARTESIAN_POINT('Ctrl Pts',(-40.1455341065928,26.91999998,-66.9202222963147));
#141153=CARTESIAN_POINT('Ctrl Pts',(-39.9875645491708,26.91999998,-67.4263054005813));
#141154=CARTESIAN_POINT('Ctrl Pts',(-39.8638827946265,26.91999998,-67.936760324224));
#141155=CARTESIAN_POINT('Ctrl Pts',(-39.7402010400822,26.91999998,-68.4472152478667));
#141156=CARTESIAN_POINT('Ctrl Pts',(-39.6502847003092,26.91999998,-68.9623259739815));
#141157=CARTESIAN_POINT('Ctrl Pts',(-39.5902135268069,26.91999998,-69.4815519521983));
#141158=CARTESIAN_POINT('Ctrl Pts',(-39.5301423533046,26.91999998,-70.0007779304151));
#141159=CARTESIAN_POINT('Ctrl Pts',(-39.5000000000007,26.91999998,-70.5241306955437));
#141160=CARTESIAN_POINT('Ctrl Pts',(-39.5,26.91999998,-71.0516396909898));
#141161=CARTESIAN_POINT('',(-43.3501517762232,26.91999998,-61.4386408691297));
#141162=CARTESIAN_POINT('Ctrl Pts',(-43.3501517762232,26.91999998,-61.4386408691297));
#141163=CARTESIAN_POINT('Ctrl Pts',(-42.5924607769204,26.91999998,-62.641249943458));
#141164=CARTESIAN_POINT('Ctrl Pts',(-41.828377509759,26.91999998,-63.839782013441));
#141165=CARTESIAN_POINT('Ctrl Pts',(-41.0569324495432,26.91999998,-65.0336174328882));
#141166=CARTESIAN_POINT('',(-43.9604906504041,26.91999998,-61.14995));
#141167=CARTESIAN_POINT('Ctrl Pts',(-43.9604906504041,26.91999998,-61.14995));
#141168=CARTESIAN_POINT('Ctrl Pts',(-43.9014853731981,26.91999998,-61.14995));
#141169=CARTESIAN_POINT('Ctrl Pts',(-43.8433879790802,26.91999998,-61.1556451738328));
#141170=CARTESIAN_POINT('Ctrl Pts',(-43.7862158462631,26.91999998,-61.1670601882964));
#141171=CARTESIAN_POINT('Ctrl Pts',(-43.7290408237003,26.91999998,-61.178475779728));
#141172=CARTESIAN_POINT('Ctrl Pts',(-43.6721412316922,26.91999998,-61.1959228882129));
#141173=CARTESIAN_POINT('Ctrl Pts',(-43.6185804531072,26.91999998,-61.2193930049692));
#141174=CARTESIAN_POINT('Ctrl Pts',(-43.5650151406998,26.91999998,-61.2428651084281));
#141175=CARTESIAN_POINT('Ctrl Pts',(-43.5142347717189,26.91999998,-61.2723879193617));
#141176=CARTESIAN_POINT('Ctrl Pts',(-43.4680362753946,26.91999998,-61.3091376491944));
#141177=CARTESIAN_POINT('Ctrl Pts',(-43.4218479344169,26.91999998,-61.345879300707));
#141178=CARTESIAN_POINT('Ctrl Pts',(-43.3818141153598,26.91999998,-61.3883863242137));
#141179=CARTESIAN_POINT('Ctrl Pts',(-43.3501517762232,26.91999998,-61.4386408691297));
#141180=CARTESIAN_POINT('',(83.2809572255632,26.9199999800001,-61.14995));
#141181=CARTESIAN_POINT('',(-57.,26.91999998,-55.74995));
#141182=CARTESIAN_POINT('',(83.2809572255632,26.9199999800001,-55.74995));
#141183=CARTESIAN_POINT('',(-59.5,26.91999998,-58.24995));
#141184=CARTESIAN_POINT('Origin',(-57.,26.91999998,-58.24995));
#141185=CARTESIAN_POINT('',(-59.5,26.91999998,-174.34995));
#141186=CARTESIAN_POINT('',(-59.5,26.91999998,-58.24995));
#141187=CARTESIAN_POINT('',(-57.,26.91999998,-176.84995));
#141188=CARTESIAN_POINT('Origin',(-57.,26.91999998,-174.34995));
#141189=CARTESIAN_POINT('',(-51.176438378063,26.91999998,-176.84995));
#141190=CARTESIAN_POINT('',(83.2809572255632,26.9199999800001,-176.84995));
#141191=CARTESIAN_POINT('',(-51.176438378063,26.91999998,-55.24995));
#141192=CARTESIAN_POINT('Origin',(-60.,27.41999998,-55.74995));
#141193=CARTESIAN_POINT('',(-57.,27.41999998,-55.24995));
#141194=CARTESIAN_POINT('',(-60.,27.41999998,-55.24995));
#141195=CARTESIAN_POINT('Origin',(-57.,27.41999998,-55.74995));
#141196=CARTESIAN_POINT('Origin',(-60.,28.41999998,-55.24995));
#141197=CARTESIAN_POINT('',(-57.,27.91999998,-55.24995));
#141198=CARTESIAN_POINT('',(-60.,27.91999998,-55.24995));
#141199=CARTESIAN_POINT('',(-57.,28.41999998,-55.24995));
#141200=CARTESIAN_POINT('Origin',(-60.,27.91999998,-55.74995));
#141201=CARTESIAN_POINT('',(-57.,28.41999998,-55.74995));
#141202=CARTESIAN_POINT('',(-60.,28.41999998,-55.74995));
#141203=CARTESIAN_POINT('Origin',(-57.,27.91999998,-55.74995));
#141204=CARTESIAN_POINT('Ctrl Pts',(-50.4632296085449,28.91999998,-60.64995));
#141205=CARTESIAN_POINT('Ctrl Pts',(-50.4632296085449,28.41999998,-60.64995));
#141206=CARTESIAN_POINT('Ctrl Pts',(-50.4632296085449,28.41999998,-61.14995));
#141207=CARTESIAN_POINT('Ctrl Pts',(-50.5951521564739,28.9142946217921,
-60.64995));
#141208=CARTESIAN_POINT('Ctrl Pts',(-50.5943760783778,28.4199999799973,
-60.6556217969837));
#141209=CARTESIAN_POINT('Ctrl Pts',(-50.6603646991919,28.41999998,-61.149949999985));
#141210=CARTESIAN_POINT('Ctrl Pts',(-50.7269752683276,28.9085935639752,
-60.6239226729817));
#141211=CARTESIAN_POINT('Ctrl Pts',(-50.728657566052,28.4199999799997,-60.6353187454025));
#141212=CARTESIAN_POINT('Ctrl Pts',(-50.8573512000782,28.41999998,-61.1109090094727));
#141213=CARTESIAN_POINT('Ctrl Pts',(-50.9706924051143,28.8980533372399,
-60.5237363920408));
#141214=CARTESIAN_POINT('Ctrl Pts',(-50.9800327848971,28.4199999800004,
-60.5426326522478));
#141215=CARTESIAN_POINT('Ctrl Pts',(-51.2215436797334,28.41999998,-60.9606295880612));
#141216=CARTESIAN_POINT('Ctrl Pts',(-51.0824668062551,28.8932193417862,
-60.4496168355678));
#141217=CARTESIAN_POINT('Ctrl Pts',(-51.0973398682523,28.4199999799993,
-60.4706504746461));
#141218=CARTESIAN_POINT('Ctrl Pts',(-51.3885709017413,28.41999998,-60.849450253352));
#141219=CARTESIAN_POINT('Ctrl Pts',(-51.2689998270813,28.8851522014976,
-60.2644967268053));
#141220=CARTESIAN_POINT('Ctrl Pts',(-51.294270482316,28.4199999800007,-60.2852157712125));
#141221=CARTESIAN_POINT('Ctrl Pts',(-51.6673117579979,28.41999998,-60.5717700902076));
#141222=CARTESIAN_POINT('Ctrl Pts',(-51.343685094216,28.8819222289984,-60.153568971423));
#141223=CARTESIAN_POINT('Ctrl Pts',(-51.3742886138646,28.4199999800003,
-60.1718710142637));
#141224=CARTESIAN_POINT('Ctrl Pts',(-51.7789157797339,28.41999998,-60.4053784571342));
#141225=CARTESIAN_POINT('Ctrl Pts',(-51.4446360376159,28.8775563241362,
-59.9116978933072));
#141226=CARTESIAN_POINT('Ctrl Pts',(-51.4824004299641,28.4199999799996,
-59.9224177216067));
#141227=CARTESIAN_POINT('Ctrl Pts',(-51.9297692440612,28.41999998,-60.0425718399611));
#141228=CARTESIAN_POINT('Ctrl Pts',(-51.4708620158139,28.8764221086278,
-59.7808732880376));
#141229=CARTESIAN_POINT('Ctrl Pts',(-51.5107937778383,28.4199999799973,
-59.7861314644994));
#141230=CARTESIAN_POINT('Ctrl Pts',(-51.9689593648456,28.41999998,-59.8463349320562));
#141231=CARTESIAN_POINT('Ctrl Pts',(-51.4708620158141,28.8764221086262,
-59.64995));
#141232=CARTESIAN_POINT('Ctrl Pts',(-51.5107937778512,28.41999998,-59.6499499999999));
#141233=CARTESIAN_POINT('Ctrl Pts',(-51.9689593648599,28.41999998,-59.64995));
#141234=CARTESIAN_POINT('',(-50.4632296085449,28.41999998,-61.14995));
#141235=CARTESIAN_POINT('Origin',(-50.4632296085449,28.91999998,-61.14995));
#141236=CARTESIAN_POINT('Ctrl Pts',(-50.4632296085449,28.41999998,-61.14995));
#141237=CARTESIAN_POINT('Ctrl Pts',(-50.6603646991919,28.41999998,-61.149949999985));
#141238=CARTESIAN_POINT('Ctrl Pts',(-50.8573512000782,28.41999998,-61.1109090094727));
#141239=CARTESIAN_POINT('Ctrl Pts',(-51.2215436797334,28.41999998,-60.9606295880612));
#141240=CARTESIAN_POINT('Ctrl Pts',(-51.3885709017413,28.41999998,-60.849450253352));
#141241=CARTESIAN_POINT('Ctrl Pts',(-51.6673117579979,28.41999998,-60.5717700902076));
#141242=CARTESIAN_POINT('Ctrl Pts',(-51.7789157797339,28.41999998,-60.4053784571342));
#141243=CARTESIAN_POINT('Ctrl Pts',(-51.9297692440612,28.41999998,-60.0425718399611));
#141244=CARTESIAN_POINT('Ctrl Pts',(-51.9689593648456,28.41999998,-59.8463349320562));
#141245=CARTESIAN_POINT('Ctrl Pts',(-51.9689593648599,28.41999998,-59.64995));
#141246=CARTESIAN_POINT('Origin',(-60.,28.41999998,-55.24995));
#141247=CARTESIAN_POINT('',(-42.,28.41999998,-171.14995));
#141248=CARTESIAN_POINT('',(-42.,28.41999998,-95.34995));
#141249=CARTESIAN_POINT('',(-42.,28.41999998,-95.34995));
#141250=CARTESIAN_POINT('',(-43.6738487993976,28.41999998,-171.14995));
#141251=CARTESIAN_POINT('',(-41.7558360441701,28.41999998,-171.14995));
#141252=CARTESIAN_POINT('',(-45.342056117244,28.41999998,-171.14995));
#141253=CARTESIAN_POINT('Ctrl Pts',(-45.342056117244,28.41999998,-171.14995));
#141254=CARTESIAN_POINT('Ctrl Pts',(-45.2224947881419,28.41999998,-171.149950023642));
#141255=CARTESIAN_POINT('Ctrl Pts',(-45.1028907122947,28.41999998,-171.153734801587));
#141256=CARTESIAN_POINT('Ctrl Pts',(-44.9833706553313,28.41999998,-171.157527071728));
#141257=CARTESIAN_POINT('Ctrl Pts',(-44.9639944908913,28.41999998,-171.158141861008));
#141258=CARTESIAN_POINT('Ctrl Pts',(-44.9446205282351,28.41999998,-171.158756957286));
#141259=CARTESIAN_POINT('Ctrl Pts',(-44.9252493015934,28.41999998,-171.15935636922));
#141260=CARTESIAN_POINT('Ctrl Pts',(-44.7862513546676,28.41999998,-171.163657440581));
#141261=CARTESIAN_POINT('Ctrl Pts',(-44.6473090850418,28.41999998,-171.167020207454));
#141262=CARTESIAN_POINT('Ctrl Pts',(-44.5082302458003,28.41999998,-171.167024238765));
#141263=CARTESIAN_POINT('Ctrl Pts',(-44.5082032664897,28.41999998,-171.167024239547));
#141264=CARTESIAN_POINT('Ctrl Pts',(-44.5081762871737,28.41999998,-171.167024240203));
#141265=CARTESIAN_POINT('Ctrl Pts',(-44.5081493078523,28.41999998,-171.167024240732));
#141266=CARTESIAN_POINT('Ctrl Pts',(-44.3691292618367,28.41999998,-171.16702696589));
#141267=CARTESIAN_POINT('Ctrl Pts',(-44.2300667116137,28.41999998,-171.163669289098));
#141268=CARTESIAN_POINT('Ctrl Pts',(-44.0910473224682,28.41999998,-171.159368608161));
#141269=CARTESIAN_POINT('Ctrl Pts',(-43.9520204566156,28.41999998,-171.155067695926));
#141270=CARTESIAN_POINT('Ctrl Pts',(-43.8129841111527,28.41999998,-171.149950027538));
#141271=CARTESIAN_POINT('Ctrl Pts',(-43.6738487993976,28.41999998,-171.14995));
#141272=CARTESIAN_POINT('',(-49.3103449325291,28.41999998,-171.14995));
#141273=CARTESIAN_POINT('',(-41.7558360441701,28.41999998,-171.14995));
#141274=CARTESIAN_POINT('',(-50.825086291307,28.41999998,-172.64995));
#141275=CARTESIAN_POINT('Ctrl Pts',(-50.825086291307,28.41999998,-172.64995));
#141276=CARTESIAN_POINT('Ctrl Pts',(-50.82508629129,28.41999998,-172.453565067926));
#141277=CARTESIAN_POINT('Ctrl Pts',(-50.7856616225938,28.41999998,-172.257328160063));
#141278=CARTESIAN_POINT('Ctrl Pts',(-50.6339053193109,28.41999998,-171.894521542842));
#141279=CARTESIAN_POINT('Ctrl Pts',(-50.5216333616693,28.41999998,-171.728129909852));
#141280=CARTESIAN_POINT('Ctrl Pts',(-50.2412242764601,28.41999998,-171.450449746589));
#141281=CARTESIAN_POINT('Ctrl Pts',(-50.0731974178181,28.41999998,-171.339270411997));
#141282=CARTESIAN_POINT('Ctrl Pts',(-49.7068252918851,28.41999998,-171.18899099047));
#141283=CARTESIAN_POINT('Ctrl Pts',(-49.5086598519041,28.41999998,-171.149950000016));
#141284=CARTESIAN_POINT('Ctrl Pts',(-49.3103449325291,28.41999998,-171.14995));
#141285=CARTESIAN_POINT('',(-50.825086291307,28.41999998,-176.84995));
#141286=CARTESIAN_POINT('',(-50.825086291307,28.41999998,-55.24995));
#141287=CARTESIAN_POINT('',(-57.,28.41999998,-176.84995));
#141288=CARTESIAN_POINT('',(-60.,28.41999998,-176.84995));
#141289=CARTESIAN_POINT('',(-59.5,28.41999998,-174.34995));
#141290=CARTESIAN_POINT('Origin',(-57.,28.41999998,-174.34995));
#141291=CARTESIAN_POINT('',(-59.5,28.41999998,-58.24995));
#141292=CARTESIAN_POINT('',(-59.5,28.41999998,-174.34995));
#141293=CARTESIAN_POINT('Origin',(-57.,28.41999998,-58.24995));
#141294=CARTESIAN_POINT('',(-45.342056117244,28.41999998,-61.14995));
#141295=CARTESIAN_POINT('',(-60.,28.41999998,-61.14995));
#141296=CARTESIAN_POINT('',(-43.6738487993976,28.41999998,-61.14995));
#141297=CARTESIAN_POINT('Ctrl Pts',(-43.6738487993976,28.41999998,-61.14995));
#141298=CARTESIAN_POINT('Ctrl Pts',(-43.8129691638245,28.41999998,-61.1499499724651));
#141299=CARTESIAN_POINT('Ctrl Pts',(-43.9520102350777,28.41999998,-61.1448326154154));
#141300=CARTESIAN_POINT('Ctrl Pts',(-44.0910473222173,28.41999998,-61.1405313837273));
#141301=CARTESIAN_POINT('Ctrl Pts',(-44.2300643593017,28.41999998,-61.1362307723049));
#141302=CARTESIAN_POINT('Ctrl Pts',(-44.3691300592233,28.4199999800001,
-61.1328730966358));
#141303=CARTESIAN_POINT('Ctrl Pts',(-44.5081446038248,28.41999998,-61.1328757503144));
#141304=CARTESIAN_POINT('Ctrl Pts',(-44.5081731511562,28.41999998,-61.1328757508594));
#141305=CARTESIAN_POINT('Ctrl Pts',(-44.5082016984814,28.41999998,-61.132875751546));
#141306=CARTESIAN_POINT('Ctrl Pts',(-44.5082302458005,28.41999998,-61.1328757523744));
#141307=CARTESIAN_POINT('Ctrl Pts',(-44.6473090834153,28.41999998,-61.1328797881197));
#141308=CARTESIAN_POINT('Ctrl Pts',(-44.7862513535664,28.41999998,-61.1362425571023));
#141309=CARTESIAN_POINT('Ctrl Pts',(-44.9252493016292,28.41999998,-61.140543629625));
#141310=CARTESIAN_POINT('Ctrl Pts',(-45.0447391053953,28.41999998,-61.144241053356));
#141311=CARTESIAN_POINT('Ctrl Pts',(-45.1643332045556,28.41999998,-61.1485385900917));
#141312=CARTESIAN_POINT('Ctrl Pts',(-45.2839053205809,28.41999998,-61.1496673946892));
#141313=CARTESIAN_POINT('Ctrl Pts',(-45.3032896860482,28.41999998,-61.1498503902034));
#141314=CARTESIAN_POINT('Ctrl Pts',(-45.3226734672922,28.41999998,-61.1499499961673));
#141315=CARTESIAN_POINT('Ctrl Pts',(-45.342056117244,28.41999998,-61.14995));
#141316=CARTESIAN_POINT('',(-41.7558360441701,28.41999998,-61.14995));
#141317=CARTESIAN_POINT('',(-60.,28.41999998,-61.14995));
#141318=CARTESIAN_POINT('',(-41.7558360441701,28.41999998,-94.0656090587062));
#141319=CARTESIAN_POINT('',(-41.7558360441701,28.41999998,-60.64995));
#141320=CARTESIAN_POINT('Origin',(-38.5,28.41999998,-95.34995));
#141321=CARTESIAN_POINT('Origin',(83.2809572255632,12.1199999800001,-55.24995));
#141322=CARTESIAN_POINT('',(-57.,12.11999998,-176.84995));
#141323=CARTESIAN_POINT('',(-53.1963133798215,12.11999998,-176.84995));
#141324=CARTESIAN_POINT('',(83.2809572255632,12.1199999800001,-176.84995));
#141325=CARTESIAN_POINT('',(-59.5,12.11999998,-174.34995));
#141326=CARTESIAN_POINT('Origin',(-57.,12.11999998,-174.34995));
#141327=CARTESIAN_POINT('',(-59.5,12.11999998,-58.24995));
#141328=CARTESIAN_POINT('',(-59.5,12.11999998,-174.34995));
#141329=CARTESIAN_POINT('Origin',(-57.,12.11999998,-58.24995));
#141330=CARTESIAN_POINT('',(-53.2607580814926,12.11999998,-60.7033966151602));
#141331=CARTESIAN_POINT('Origin',(-50.5588767647388,12.11999998,-59.7245163413739));
#141332=CARTESIAN_POINT('',(-52.8224784153176,12.11999998,-61.275204160084));
#141333=CARTESIAN_POINT('Origin',(-52.0615368275148,12.11999998,-60.1416270042289));
#141334=CARTESIAN_POINT('',(-52.6867218473722,12.11999998,-61.4386408691297));
#141335=CARTESIAN_POINT('Origin',(-53.5608834560611,12.11999998,-61.8978040915907));
#141336=CARTESIAN_POINT('',(-40.5508657493525,12.11999998,-84.2187933558389));
#141337=CARTESIAN_POINT('Ctrl Pts',(-40.5508657493525,12.11999998,-84.2187933558389));
#141338=CARTESIAN_POINT('Ctrl Pts',(-42.6282147356021,12.11999998,-80.4512454090371));
#141339=CARTESIAN_POINT('Ctrl Pts',(-44.6709958246292,12.11999998,-76.6652818249174));
#141340=CARTESIAN_POINT('Ctrl Pts',(-46.6906839910419,12.11999998,-72.8670157601218));
#141341=CARTESIAN_POINT('Ctrl Pts',(-48.7103721574547,12.11999998,-69.0687496953263));
#141342=CARTESIAN_POINT('Ctrl Pts',(-50.7067642663818,12.11999998,-65.2580729321624));
#141343=CARTESIAN_POINT('Ctrl Pts',(-52.6867218473722,12.11999998,-61.4386408691297));
#141344=CARTESIAN_POINT('',(-39.5,12.11999998,-88.5398461374725));
#141345=CARTESIAN_POINT('Ctrl Pts',(-39.5,12.11999998,-88.5398461374725));
#141346=CARTESIAN_POINT('Ctrl Pts',(-39.5,12.11999998,-88.1633801721072));
#141347=CARTESIAN_POINT('Ctrl Pts',(-39.5216886477936,12.11999998,-87.7889298981599));
#141348=CARTESIAN_POINT('Ctrl Pts',(-39.5647508040475,12.11999998,-87.4164660273289));
#141349=CARTESIAN_POINT('Ctrl Pts',(-39.6078129603014,12.11999998,-87.0440021564979));
#141350=CARTESIAN_POINT('Ctrl Pts',(-39.672739619198,12.11999998,-86.6717926677294));
#141351=CARTESIAN_POINT('Ctrl Pts',(-39.7591103506482,12.11999998,-86.3076691214426));
#141352=CARTESIAN_POINT('Ctrl Pts',(-39.8454810820984,12.11999998,-85.9435455751558));
#141353=CARTESIAN_POINT('Ctrl Pts',(-39.9523131981843,12.11999998,-85.5865932598646));
#141354=CARTESIAN_POINT('Ctrl Pts',(-40.0830988504763,12.11999998,-85.2380360010512));
#141355=CARTESIAN_POINT('Ctrl Pts',(-40.2020523584857,12.11999998,-84.9210126276812));
#141356=CARTESIAN_POINT('Ctrl Pts',(-40.340821045384,12.11999998,-84.6109338990986));
#141357=CARTESIAN_POINT('Ctrl Pts',(-40.5020760733022,12.11999998,-84.3087360817072));
#141358=CARTESIAN_POINT('Ctrl Pts',(-40.5181158924597,12.11999998,-84.2786768742311));
#141359=CARTESIAN_POINT('Ctrl Pts',(-40.5343782322712,12.11999998,-84.2486956551327));
#141360=CARTESIAN_POINT('Ctrl Pts',(-40.5508657493525,12.11999998,-84.2187933558389));
#141361=CARTESIAN_POINT('',(-39.5,12.11999998,-143.518796834034));
#141362=CARTESIAN_POINT('',(-39.5,12.11999998,-55.24995));
#141363=CARTESIAN_POINT('',(-40.5508657493446,12.11999998,-147.839849615653));
#141364=CARTESIAN_POINT('Ctrl Pts',(-40.5508657493446,12.11999998,-147.839849615653));
#141365=CARTESIAN_POINT('Ctrl Pts',(-40.4872051775685,12.11999998,-147.72439272417));
#141366=CARTESIAN_POINT('Ctrl Pts',(-40.4268911487417,12.11999998,-147.607488691345));
#141367=CARTESIAN_POINT('Ctrl Pts',(-40.369709660312,12.11999998,-147.489235888513));
#141368=CARTESIAN_POINT('Ctrl Pts',(-40.3100900049245,12.11999998,-147.365940893103));
#141369=CARTESIAN_POINT('Ctrl Pts',(-40.2538755845828,12.11999998,-147.241179143609));
#141370=CARTESIAN_POINT('Ctrl Pts',(-40.2008730860127,12.11999998,-147.115031779943));
#141371=CARTESIAN_POINT('Ctrl Pts',(-40.1592698126768,12.11999998,-147.016014877103));
#141372=CARTESIAN_POINT('Ctrl Pts',(-40.119646471931,12.11999998,-146.916143544358));
#141373=CARTESIAN_POINT('Ctrl Pts',(-40.0819301037035,12.11999998,-146.815448147357));
#141374=CARTESIAN_POINT('Ctrl Pts',(-40.0215352750629,12.11999998,-146.654205654174));
#141375=CARTESIAN_POINT('Ctrl Pts',(-39.9660661346646,12.11999998,-146.490922340265));
#141376=CARTESIAN_POINT('Ctrl Pts',(-39.9154672964458,12.11999998,-146.32638803891));
#141377=CARTESIAN_POINT('Ctrl Pts',(-39.8629240743822,12.11999998,-146.15553110548));
#141378=CARTESIAN_POINT('Ctrl Pts',(-39.8156327203447,12.11999998,-145.983326186388));
#141379=CARTESIAN_POINT('Ctrl Pts',(-39.7734780737249,12.11999998,-145.81067296635));
#141380=CARTESIAN_POINT('Ctrl Pts',(-39.7676020779481,12.11999998,-145.786606589968));
#141381=CARTESIAN_POINT('Ctrl Pts',(-39.7618258061274,12.11999998,-145.762531511883));
#141382=CARTESIAN_POINT('Ctrl Pts',(-39.7561488675992,12.11999998,-145.738450173272));
#141383=CARTESIAN_POINT('Ctrl Pts',(-39.6543246883751,12.11999998,-145.306516213354));
#141384=CARTESIAN_POINT('Ctrl Pts',(-39.5830357134849,12.11999998,-144.869793515198));
#141385=CARTESIAN_POINT('Ctrl Pts',(-39.5419615359823,12.11999998,-144.428332293186));
#141386=CARTESIAN_POINT('Ctrl Pts',(-39.5139579007162,12.11999998,-144.127351974236));
#141387=CARTESIAN_POINT('Ctrl Pts',(-39.5,12.11999998,-143.824168887332));
#141388=CARTESIAN_POINT('Ctrl Pts',(-39.5,12.11999998,-143.518796834034));
#141389=CARTESIAN_POINT('',(-52.811758955289,12.11999998,-170.861259130871));
#141390=CARTESIAN_POINT('Ctrl Pts',(-52.811758955289,12.11999998,-170.861259130871));
#141391=CARTESIAN_POINT('Ctrl Pts',(-50.8116686437173,12.11999998,-167.001247608061));
#141392=CARTESIAN_POINT('Ctrl Pts',(-48.794913685955,12.11999998,-163.150111451771));
#141393=CARTESIAN_POINT('Ctrl Pts',(-46.7544651237368,12.11999998,-159.311594190676));
#141394=CARTESIAN_POINT('Ctrl Pts',(-44.7140165615186,12.11999998,-155.47307692958));
#141395=CARTESIAN_POINT('Ctrl Pts',(-42.6500867945137,12.11999998,-151.647065442471));
#141396=CARTESIAN_POINT('Ctrl Pts',(-40.5508657493446,12.11999998,-147.839849615653));
#141397=CARTESIAN_POINT('',(-52.8706140943225,12.11999998,-170.949706593448));
#141398=CARTESIAN_POINT('Ctrl Pts',(-52.8706140943225,12.11999998,-170.949706593448));
#141399=CARTESIAN_POINT('Ctrl Pts',(-52.8478318703964,12.11999998,-170.92232940649));
#141400=CARTESIAN_POINT('Ctrl Pts',(-52.8281487108054,12.11999998,-170.892890025127));
#141401=CARTESIAN_POINT('Ctrl Pts',(-52.811758955289,12.11999998,-170.861259130871));
#141402=CARTESIAN_POINT('',(-53.1963133798215,12.11999998,-171.855638188259));
#141403=CARTESIAN_POINT('Ctrl Pts',(-53.1963133798215,12.11999998,-171.855638188259));
#141404=CARTESIAN_POINT('Ctrl Pts',(-53.196313374732,12.11999998,-171.73372692869));
#141405=CARTESIAN_POINT('Ctrl Pts',(-53.1815021190177,12.11999998,-171.614382981042));
#141406=CARTESIAN_POINT('Ctrl Pts',(-53.1513539481864,12.11999998,-171.497697478252));
#141407=CARTESIAN_POINT('Ctrl Pts',(-53.1406117769373,12.11999998,-171.456120970666));
#141408=CARTESIAN_POINT('Ctrl Pts',(-53.1279219841079,12.11999998,-171.414882055034));
#141409=CARTESIAN_POINT('Ctrl Pts',(-53.1132591959952,12.11999998,-171.373985128688));
#141410=CARTESIAN_POINT('Ctrl Pts',(-53.0817091112288,12.11999998,-171.285986756006));
#141411=CARTESIAN_POINT('Ctrl Pts',(-53.0420949559112,12.11999998,-171.202535400955));
#141412=CARTESIAN_POINT('Ctrl Pts',(-52.9945125852814,12.11999998,-171.123638976918));
#141413=CARTESIAN_POINT('Ctrl Pts',(-52.9579184729698,12.11999998,-171.062962206006));
#141414=CARTESIAN_POINT('Ctrl Pts',(-52.9166104754484,12.11999998,-171.00498002573));
#141415=CARTESIAN_POINT('Ctrl Pts',(-52.8706140943225,12.11999998,-170.949706593449));
#141416=CARTESIAN_POINT('',(-53.1963133798215,12.11999998,-171.806096612245));
#141417=CARTESIAN_POINT('Ctrl Pts',(-52.81219032515,12.5218539749099,-60.5055220850798));
#141418=CARTESIAN_POINT('Ctrl Pts',(-52.8857929788877,12.11999998,-60.5379900686009));
#141419=CARTESIAN_POINT('Ctrl Pts',(-53.2607580814926,12.11999998,-60.7033966151602));
#141420=CARTESIAN_POINT('Ctrl Pts',(-52.8700875991767,12.5389561241882,
-60.3657903170377));
#141421=CARTESIAN_POINT('Ctrl Pts',(-52.9388615253298,12.1199999799981,
-60.3810288628603));
#141422=CARTESIAN_POINT('Ctrl Pts',(-53.3498368505456,12.11999998,-60.5014612122216));
#141423=CARTESIAN_POINT('Ctrl Pts',(-52.8985874779024,12.5574454029709,
-60.2163866339305));
#141424=CARTESIAN_POINT('Ctrl Pts',(-52.9540808994585,12.1199999800015,
-60.2191862528169));
#141425=CARTESIAN_POINT('Ctrl Pts',(-53.3950245780495,12.11999998,-60.2853240337268));
#141426=CARTESIAN_POINT('Ctrl Pts',(-52.8969272312866,12.5764221086261,
-60.0627241236309));
#141427=CARTESIAN_POINT('Ctrl Pts',(-52.9368589933238,12.11999998,-60.0627241236309));
#141428=CARTESIAN_POINT('Ctrl Pts',(-53.3950245803325,12.11999998,-60.0627241236311));
#141429=CARTESIAN_POINT('Origin',(-53.2607580814926,12.61999998,-60.7033966151602));
#141430=CARTESIAN_POINT('Ctrl Pts',(-52.4885489491165,12.6049688303995,
-60.8798615124595));
#141431=CARTESIAN_POINT('Ctrl Pts',(-52.7011006011713,12.5792267001133,
-60.7309116189004));
#141432=CARTESIAN_POINT('Ctrl Pts',(-52.8135194149171,12.5211707144541,
-60.5028360925954));
#141433=CARTESIAN_POINT('Ctrl Pts',(-52.5003487858574,12.5616578171005,
-60.8867883233088));
#141434=CARTESIAN_POINT('Ctrl Pts',(-52.7083699494148,12.5371106789483,
-60.7374192211268));
#141435=CARTESIAN_POINT('Ctrl Pts',(-52.8184252363688,12.4804454574502,
-60.5118893693287));
#141436=CARTESIAN_POINT('Ctrl Pts',(-52.5124335500125,12.5183120391401,
-60.8937038544239));
#141437=CARTESIAN_POINT('Ctrl Pts',(-52.7160214096145,12.4948853110753,
-60.7440415583411));
#141438=CARTESIAN_POINT('Ctrl Pts',(-52.823766550455,12.4396518133592,-60.5210243207318));
#141439=CARTESIAN_POINT('Ctrl Pts',(-52.5248032674767,12.4749209213966,
-60.9005813814078));
#141440=CARTESIAN_POINT('Ctrl Pts',(-52.7240626356492,12.4525613978151,
-60.750736804912));
#141441=CARTESIAN_POINT('Ctrl Pts',(-52.8295491865184,12.3987982841401,
-60.5301925771521));
#141442=CARTESIAN_POINT('',(-52.5245819708686,12.4756972986232,-60.9004583201709));
#141443=CARTESIAN_POINT('Ctrl Pts',(-52.4885489491165,12.6049688303995,
-60.8798615124595));
#141444=CARTESIAN_POINT('Ctrl Pts',(-52.5003074888079,12.5618093982546,
-60.8867640803813));
#141445=CARTESIAN_POINT('Ctrl Pts',(-52.5123202735365,12.518720787882,-60.8936385283445));
#141446=CARTESIAN_POINT('Ctrl Pts',(-52.5245819708709,12.4756972986243,
-60.9004583201737));
#141447=CARTESIAN_POINT('Ctrl Pts',(-52.81219032515,12.5218539749099,-60.5055220850798));
#141448=CARTESIAN_POINT('Ctrl Pts',(-52.7486445377005,12.4996864767879,
-60.660571058145));
#141449=CARTESIAN_POINT('Ctrl Pts',(-52.6505629615106,12.4839221309077,
-60.7971452199062));
#141450=CARTESIAN_POINT('Ctrl Pts',(-52.5245819708686,12.4756972986232,
-60.9004583201709));
#141451=CARTESIAN_POINT('Origin',(0.,-12.9675000200281,-61.64995));
#141452=CARTESIAN_POINT('',(-49.1629069712534,18.0283224583225,-61.2273317382593));
#141453=CARTESIAN_POINT('',(-52.2790965136749,12.4220352393542,-61.2273317382593));
#141454=CARTESIAN_POINT('Origin',(0.,-12.9675000200281,-61.2273317382593));
#141455=CARTESIAN_POINT('Origin',(-53.868230923887,12.7669411850502,-62.1522526801527));
#141456=CARTESIAN_POINT('',(-50.0811190791972,18.26999998,-60.64995));
#141457=CARTESIAN_POINT('Origin',(0.,-12.9675000200281,-60.64995));
#141458=CARTESIAN_POINT('Ctrl Pts',(-49.1629069712534,18.0283224583225,
-61.2273317382593));
#141459=CARTESIAN_POINT('Ctrl Pts',(-49.2072136788996,18.0400790290492,
-61.1335104039183));
#141460=CARTESIAN_POINT('Ctrl Pts',(-49.2636489250068,18.0550404895701,
-61.0510932718963));
#141461=CARTESIAN_POINT('Ctrl Pts',(-49.3970153298707,18.0903238932961,
-60.9057963508575));
#141462=CARTESIAN_POINT('Ctrl Pts',(-49.4723725947842,18.1102284712985,
-60.8450701877959));
#141463=CARTESIAN_POINT('Ctrl Pts',(-49.7151670266325,18.1742094267258,
-60.6988289354793));
#141464=CARTESIAN_POINT('Ctrl Pts',(-49.897617121419,18.2220908968247,-60.64995));
#141465=CARTESIAN_POINT('Ctrl Pts',(-50.0811190791972,18.26999998,-60.64995));
#141466=CARTESIAN_POINT('Origin',(0.,-12.9675000200281,-60.64995));
#141467=CARTESIAN_POINT('',(-1.30574517062348E-14,18.26999998,-60.64995));
#141468=CARTESIAN_POINT('Ctrl Pts',(-52.4026162823651,18.2264221086262,
-59.64995));
#141469=CARTESIAN_POINT('Ctrl Pts',(-52.3550593808763,18.76999998,-59.64995));
#141470=CARTESIAN_POINT('Ctrl Pts',(-52.900713631411,18.76999998,-59.64995));
#141471=CARTESIAN_POINT('Ctrl Pts',(-52.402616282365,18.2264221086281,-59.7808732880371));
#141472=CARTESIAN_POINT('Ctrl Pts',(-52.3550593808723,18.76999998,-59.7746029379313));
#141473=CARTESIAN_POINT('Ctrl Pts',(-52.9007136313967,18.76999998,-59.8463349320561));
#141474=CARTESIAN_POINT('Ctrl Pts',(-52.3763903041667,18.2275563241362,
-59.9116978933078));
#141475=CARTESIAN_POINT('Ctrl Pts',(-52.3316386425403,18.76999998,-59.8989712332646));
#141476=CARTESIAN_POINT('Ctrl Pts',(-52.8615235106123,18.76999998,-60.0425718399612));
#141477=CARTESIAN_POINT('Ctrl Pts',(-52.2754393607673,18.2319222289985,
-60.1535689714224));
#141478=CARTESIAN_POINT('Ctrl Pts',(-52.239810099313,18.76999998,-60.1322291512602));
#141479=CARTESIAN_POINT('Ctrl Pts',(-52.710670046285,18.76999998,-60.4053784571341));
#141480=CARTESIAN_POINT('Ctrl Pts',(-52.2007540936325,18.2351522014976,
-60.2644967268053));
#141481=CARTESIAN_POINT('Ctrl Pts',(-52.1717434473124,18.7699999799997,
-60.2406767152624));
#141482=CARTESIAN_POINT('Ctrl Pts',(-52.5990660245491,18.76999998,-60.5717700902076));
#141483=CARTESIAN_POINT('Ctrl Pts',(-52.0142210728062,18.2432193417862,
-60.4496168355678));
#141484=CARTESIAN_POINT('Ctrl Pts',(-51.9977165994394,18.7699999800003,
-60.4261994932772));
#141485=CARTESIAN_POINT('Ctrl Pts',(-52.3203251682923,18.76999998,-60.8494502533521));
#141486=CARTESIAN_POINT('Ctrl Pts',(-51.9024466716657,18.2480533372399,
-60.5237363920407));
#141487=CARTESIAN_POINT('Ctrl Pts',(-51.8922860151588,18.7699999800003,
-60.5031527166051));
#141488=CARTESIAN_POINT('Ctrl Pts',(-52.1532979462845,18.76999998,-60.9606295880612));
#141489=CARTESIAN_POINT('Ctrl Pts',(-51.6587295348784,18.2585935639752,
-60.6239226729819));
#141490=CARTESIAN_POINT('Ctrl Pts',(-51.657019042446,18.7699999799997,-60.6120353079393));
#141491=CARTESIAN_POINT('Ctrl Pts',(-51.7891054666292,18.76999998,-61.1109090094727));
#141492=CARTESIAN_POINT('Ctrl Pts',(-51.5269064230252,18.264294621793,-60.64995));
#141493=CARTESIAN_POINT('Ctrl Pts',(-51.5277022966008,18.7699999800007,
-60.6442102195358));
#141494=CARTESIAN_POINT('Ctrl Pts',(-51.592118965743,18.76999998,-61.149949999985));
#141495=CARTESIAN_POINT('Ctrl Pts',(-51.394983875096,18.26999998,-60.64995));
#141496=CARTESIAN_POINT('Ctrl Pts',(-51.394983875096,18.76999998,-60.64995));
#141497=CARTESIAN_POINT('Ctrl Pts',(-51.394983875096,18.76999998,-61.14995));
#141498=CARTESIAN_POINT('',(-51.394983875096,18.76999998,-61.14995));
#141499=CARTESIAN_POINT('Origin',(-51.394983875096,18.26999998,-61.14995));
#141500=CARTESIAN_POINT('Ctrl Pts',(-52.900713631411,18.76999998,-59.64995));
#141501=CARTESIAN_POINT('Ctrl Pts',(-52.9007136313967,18.76999998,-59.8463349320561));
#141502=CARTESIAN_POINT('Ctrl Pts',(-52.8615235106123,18.76999998,-60.0425718399612));
#141503=CARTESIAN_POINT('Ctrl Pts',(-52.710670046285,18.76999998,-60.4053784571341));
#141504=CARTESIAN_POINT('Ctrl Pts',(-52.5990660245491,18.76999998,-60.5717700902076));
#141505=CARTESIAN_POINT('Ctrl Pts',(-52.3203251682923,18.76999998,-60.8494502533521));
#141506=CARTESIAN_POINT('Ctrl Pts',(-52.1532979462845,18.76999998,-60.9606295880612));
#141507=CARTESIAN_POINT('Ctrl Pts',(-51.7891054666292,18.76999998,-61.1109090094727));
#141508=CARTESIAN_POINT('Ctrl Pts',(-51.592118965743,18.76999998,-61.149949999985));
#141509=CARTESIAN_POINT('Ctrl Pts',(-51.394983875096,18.76999998,-61.14995));
#141510=CARTESIAN_POINT('Origin',(83.2809572255632,18.7699999800001,-55.24995));
#141511=CARTESIAN_POINT('',(-57.,18.76999998,-55.74995));
#141512=CARTESIAN_POINT('',(83.2809572255632,18.7699999800001,-55.74995));
#141513=CARTESIAN_POINT('',(-59.5,18.76999998,-58.24995));
#141514=CARTESIAN_POINT('Origin',(-57.,18.76999998,-58.24995));
#141515=CARTESIAN_POINT('',(-59.5,18.76999998,-174.34995));
#141516=CARTESIAN_POINT('',(-59.5,18.76999998,-58.24995));
#141517=CARTESIAN_POINT('',(-57.,18.76999998,-176.84995));
#141518=CARTESIAN_POINT('Origin',(-57.,18.76999998,-174.34995));
#141519=CARTESIAN_POINT('',(-52.3218461808875,18.76999998,-176.84995));
#141520=CARTESIAN_POINT('',(83.2809572255632,18.7699999800001,-176.84995));
#141521=CARTESIAN_POINT('',(-52.3218461808875,18.76999998,-172.64995));
#141522=CARTESIAN_POINT('',(-52.3218461808875,18.76999998,-55.24995));
#141523=CARTESIAN_POINT('',(-50.8071048221096,18.76999998,-171.14995));
#141524=CARTESIAN_POINT('Ctrl Pts',(-50.8071048221096,18.76999998,-171.14995));
#141525=CARTESIAN_POINT('Ctrl Pts',(-51.0054197414846,18.76999998,-171.149950000016));
#141526=CARTESIAN_POINT('Ctrl Pts',(-51.2035851814656,18.76999998,-171.18899099047));
#141527=CARTESIAN_POINT('Ctrl Pts',(-51.5699573073986,18.76999998,-171.339270411997));
#141528=CARTESIAN_POINT('Ctrl Pts',(-51.7379841660413,18.76999998,-171.450449746589));
#141529=CARTESIAN_POINT('Ctrl Pts',(-52.0183932512491,18.76999998,-171.728129909852));
#141530=CARTESIAN_POINT('Ctrl Pts',(-52.1306652088914,18.76999998,-171.894521542842));
#141531=CARTESIAN_POINT('Ctrl Pts',(-52.2824215121743,18.76999998,-172.257328160063));
#141532=CARTESIAN_POINT('Ctrl Pts',(-52.3218461808705,18.76999998,-172.453565067926));
#141533=CARTESIAN_POINT('Ctrl Pts',(-52.3218461808875,18.76999998,-172.64995));
#141534=CARTESIAN_POINT('',(-50.2136602208993,18.76999998,-171.14995));
#141535=CARTESIAN_POINT('',(-50.7368344047584,18.76999998,-171.14995));
#141536=CARTESIAN_POINT('',(-49.6791770659623,18.76999998,-170.861259130871));
#141537=CARTESIAN_POINT('Ctrl Pts',(-49.6791770659623,18.76999998,-170.861259130871));
#141538=CARTESIAN_POINT('Ctrl Pts',(-49.6968576580123,18.76999998,-170.89335724814));
#141539=CARTESIAN_POINT('Ctrl Pts',(-49.7180606234586,18.76999998,-170.923027065572));
#141540=CARTESIAN_POINT('Ctrl Pts',(-49.742166968171,18.76999998,-170.95020183613));
#141541=CARTESIAN_POINT('Ctrl Pts',(-49.7534002577179,18.76999998,-170.962864978123));
#141542=CARTESIAN_POINT('Ctrl Pts',(-49.7652647303595,18.76999998,-170.974986007307));
#141543=CARTESIAN_POINT('Ctrl Pts',(-49.7777010515148,18.76999998,-170.986556367076));
#141544=CARTESIAN_POINT('Ctrl Pts',(-49.8071230954838,18.76999998,-171.013929705992));
#141545=CARTESIAN_POINT('Ctrl Pts',(-49.8388986066917,18.76999998,-171.037546210365));
#141546=CARTESIAN_POINT('Ctrl Pts',(-49.8728019101419,18.76999998,-171.057883544606));
#141547=CARTESIAN_POINT('Ctrl Pts',(-49.8840707206927,18.76999998,-171.064643286087));
#141548=CARTESIAN_POINT('Ctrl Pts',(-49.8955748425991,18.76999998,-171.071040378572));
#141549=CARTESIAN_POINT('Ctrl Pts',(-49.9073066431081,18.76999998,-171.07709133376));
#141550=CARTESIAN_POINT('Ctrl Pts',(-49.9542902216173,18.76999998,-171.101324232019));
#141551=CARTESIAN_POINT('Ctrl Pts',(-50.0051782135404,18.76999998,-171.119773228097));
#141552=CARTESIAN_POINT('Ctrl Pts',(-50.0564485939595,18.76999998,-171.131817408419));
#141553=CARTESIAN_POINT('Ctrl Pts',(-50.1077152012182,18.76999998,-171.143860702368));
#141554=CARTESIAN_POINT('Ctrl Pts',(-50.1601164670163,18.76999998,-171.14995));
#141555=CARTESIAN_POINT('Ctrl Pts',(-50.2136602208993,18.76999998,-171.14995));
#141556=CARTESIAN_POINT('',(-40.7628307834967,18.76999998,-155.145469613787));
#141557=CARTESIAN_POINT('Ctrl Pts',(-40.7628307834967,18.76999998,-155.145469613787));
#141558=CARTESIAN_POINT('Ctrl Pts',(-43.8140512781903,18.76999998,-160.339185894338));
#141559=CARTESIAN_POINT('Ctrl Pts',(-46.7729974319751,18.76999998,-165.585253981682));
#141560=CARTESIAN_POINT('Ctrl Pts',(-49.6791770659623,18.76999998,-170.861259130871));
#141561=CARTESIAN_POINT('',(-39.5,18.76999998,-150.084863924608));
#141562=CARTESIAN_POINT('Ctrl Pts',(-39.5,18.76999998,-150.084863924608));
#141563=CARTESIAN_POINT('Ctrl Pts',(-39.5,18.76999998,-150.526736484781));
#141564=CARTESIAN_POINT('Ctrl Pts',(-39.5253915082895,18.76999998,-150.965860868514));
#141565=CARTESIAN_POINT('Ctrl Pts',(-39.5759031870658,18.76999998,-151.402266443275));
#141566=CARTESIAN_POINT('Ctrl Pts',(-39.6264148658422,18.76999998,-151.838672018036));
#141567=CARTESIAN_POINT('Ctrl Pts',(-39.7023798052339,18.76999998,-152.273874561637));
#141568=CARTESIAN_POINT('Ctrl Pts',(-39.8051549665992,18.76999998,-152.702666397218));
#141569=CARTESIAN_POINT('Ctrl Pts',(-39.9079301279644,18.76999998,-153.131458232799));
#141570=CARTESIAN_POINT('Ctrl Pts',(-40.0364383090913,18.76999998,-153.550444480149));
#141571=CARTESIAN_POINT('Ctrl Pts',(-40.1940856267786,18.76999998,-153.958327235804));
#141572=CARTESIAN_POINT('Ctrl Pts',(-40.3268328904701,18.76999998,-154.301785789457));
#141573=CARTESIAN_POINT('Ctrl Pts',(-40.4800174576556,18.76999998,-154.637456687643));
#141574=CARTESIAN_POINT('Ctrl Pts',(-40.6592112617779,18.76999998,-154.963216752245));
#141575=CARTESIAN_POINT('Ctrl Pts',(-40.6928235206997,18.76999998,-155.024321162029));
#141576=CARTESIAN_POINT('Ctrl Pts',(-40.727351034357,18.76999998,-155.085076813253));
#141577=CARTESIAN_POINT('Ctrl Pts',(-40.7628307834967,18.76999998,-155.145469613787));
#141578=CARTESIAN_POINT('',(-39.5,18.76999998,-81.9737790469184));
#141579=CARTESIAN_POINT('',(-39.5,18.76999998,-55.24995));
#141580=CARTESIAN_POINT('',(-40.7628307834967,18.76999998,-76.9131733577189));
#141581=CARTESIAN_POINT('Ctrl Pts',(-40.7628307834967,18.76999998,-76.913173357719));
#141582=CARTESIAN_POINT('Ctrl Pts',(-40.5548564785642,18.76999998,-77.2671823633761));
#141583=CARTESIAN_POINT('Ctrl Pts',(-40.3788354530891,18.76999998,-77.6350438334276));
#141584=CARTESIAN_POINT('Ctrl Pts',(-40.2280138947791,18.76999998,-78.0138298371173));
#141585=CARTESIAN_POINT('Ctrl Pts',(-40.2160748553596,18.76999998,-78.0438145493842));
#141586=CARTESIAN_POINT('Ctrl Pts',(-40.2042937476386,18.76999998,-78.0738677286071));
#141587=CARTESIAN_POINT('Ctrl Pts',(-40.1926672329271,18.76999998,-78.1039879273901));
#141588=CARTESIAN_POINT('Ctrl Pts',(-40.0341671712826,18.76999998,-78.5146056819203));
#141589=CARTESIAN_POINT('Ctrl Pts',(-39.9044907334798,18.76999998,-78.9396134648084));
#141590=CARTESIAN_POINT('Ctrl Pts',(-39.802619647733,18.76999998,-79.366578420212));
#141591=CARTESIAN_POINT('Ctrl Pts',(-39.689990788524,18.76999998,-79.8386316578583));
#141592=CARTESIAN_POINT('Ctrl Pts',(-39.6094172115555,18.76999998,-80.315401745757));
#141593=CARTESIAN_POINT('Ctrl Pts',(-39.5598665237953,18.76999998,-80.7967368113115));
#141594=CARTESIAN_POINT('Ctrl Pts',(-39.5197815285328,18.76999998,-81.1861222001843));
#141595=CARTESIAN_POINT('Ctrl Pts',(-39.4999999999993,18.76999998,-81.57849522885));
#141596=CARTESIAN_POINT('Ctrl Pts',(-39.5,18.76999998,-81.9737790469184));
#141597=CARTESIAN_POINT('',(-49.5462350640495,18.76999998,-61.4386408691297));
#141598=CARTESIAN_POINT('Ctrl Pts',(-49.5462350640495,18.76999998,-61.4386408691297));
#141599=CARTESIAN_POINT('Ctrl Pts',(-46.6826907236407,18.76999998,-66.6332909352423));
#141600=CARTESIAN_POINT('Ctrl Pts',(-43.7675305143725,18.76999998,-71.7986436352564));
#141601=CARTESIAN_POINT('Ctrl Pts',(-40.7628307834967,18.76999998,-76.9131733577189));
#141602=CARTESIAN_POINT('',(-50.0811190791972,18.76999998,-61.14995));
#141603=CARTESIAN_POINT('Ctrl Pts',(-50.0811190791972,18.76999998,-61.14995));
#141604=CARTESIAN_POINT('Ctrl Pts',(-50.0253653304666,18.76999998,-61.14995));
#141605=CARTESIAN_POINT('Ctrl Pts',(-49.9698122997694,18.76999998,-61.156619759286));
#141606=CARTESIAN_POINT('Ctrl Pts',(-49.9160272892489,18.76999998,-61.1699168656485));
#141607=CARTESIAN_POINT('Ctrl Pts',(-49.8667673647605,18.76999998,-61.182095248603));
#141608=CARTESIAN_POINT('Ctrl Pts',(-49.8189890147707,18.76999998,-61.1998333372795));
#141609=CARTESIAN_POINT('Ctrl Pts',(-49.7739018815406,18.76999998,-61.2231365482226));
#141610=CARTESIAN_POINT('Ctrl Pts',(-49.7267405569306,18.76999998,-61.2475118015822));
#141611=CARTESIAN_POINT('Ctrl Pts',(-49.6828095888518,18.76999998,-61.2778731395778));
#141612=CARTESIAN_POINT('Ctrl Pts',(-49.6439176192587,18.76999998,-61.3141973629269));
#141613=CARTESIAN_POINT('Ctrl Pts',(-49.6050311049514,18.76999998,-61.3505164911619));
#141614=CARTESIAN_POINT('Ctrl Pts',(-49.572103750808,18.76999998,-61.391713439551));
#141615=CARTESIAN_POINT('Ctrl Pts',(-49.5462350640495,18.76999998,-61.4386408691297));
#141616=CARTESIAN_POINT('',(83.2809572255632,18.7699999800001,-61.14995));
#141617=CARTESIAN_POINT('Origin',(-60.,19.26999998,-55.74995));
#141618=CARTESIAN_POINT('',(-57.,19.26999998,-55.24995));
#141619=CARTESIAN_POINT('',(-60.,19.26999998,-55.24995));
#141620=CARTESIAN_POINT('Origin',(-57.,19.26999998,-55.74995));
#141621=CARTESIAN_POINT('Origin',(-60.,28.41999998,-55.24995));
#141622=CARTESIAN_POINT('',(-57.,19.76999998,-55.24995));
#141623=CARTESIAN_POINT('',(-60.,19.76999998,-55.24995));
#141624=CARTESIAN_POINT('',(-57.,28.41999998,-55.24995));
#141625=CARTESIAN_POINT('Origin',(83.2809572255632,19.7699999800001,-55.74995));
#141626=CARTESIAN_POINT('',(-57.,20.26999998,-55.74995));
#141627=CARTESIAN_POINT('',(83.2809572255632,20.2699999800001,-55.74995));
#141628=CARTESIAN_POINT('Origin',(-57.,19.76999998,-55.74995));
#141629=CARTESIAN_POINT('Origin',(83.2809572255632,20.2699999800001,-55.24995));
#141630=CARTESIAN_POINT('',(-57.,20.26999998,-176.84995));
#141631=CARTESIAN_POINT('',(-51.9704940941315,20.26999998,-176.84995));
#141632=CARTESIAN_POINT('',(83.2809572255632,20.2699999800001,-176.84995));
#141633=CARTESIAN_POINT('',(-59.5,20.26999998,-174.34995));
#141634=CARTESIAN_POINT('Origin',(-57.,20.26999998,-174.34995));
#141635=CARTESIAN_POINT('',(-59.5,20.26999998,-58.24995));
#141636=CARTESIAN_POINT('',(-59.5,20.26999998,-174.34995));
#141637=CARTESIAN_POINT('Origin',(-57.,20.26999998,-58.24995));
#141638=CARTESIAN_POINT('',(-48.4322308821779,20.26999998,-61.14995));
#141639=CARTESIAN_POINT('',(83.2809572255632,20.2699999800001,-61.14995));
#141640=CARTESIAN_POINT('',(-47.878929697957,20.26999998,-61.4386408691297));
#141641=CARTESIAN_POINT('Ctrl Pts',(-47.878929697957,20.26999998,-61.4386408691297));
#141642=CARTESIAN_POINT('Ctrl Pts',(-47.8974331987387,20.26999998,-61.4062039153375));
#141643=CARTESIAN_POINT('Ctrl Pts',(-47.9195379615588,20.26999998,-61.3763755387995));
#141644=CARTESIAN_POINT('Ctrl Pts',(-47.9444691614869,20.26999998,-61.3492604871258));
#141645=CARTESIAN_POINT('Ctrl Pts',(-47.9720805388406,20.26999998,-61.3192304875314));
#141646=CARTESIAN_POINT('Ctrl Pts',(-48.0031577468356,20.26999998,-61.2925292835123));
#141647=CARTESIAN_POINT('Ctrl Pts',(-48.0365924563163,20.26999998,-61.2692603439468));
#141648=CARTESIAN_POINT('Ctrl Pts',(-48.0621704908693,20.26999998,-61.2514592698696));
#141649=CARTESIAN_POINT('Ctrl Pts',(-48.089126771587,20.26999998,-61.2356661036976));
#141650=CARTESIAN_POINT('Ctrl Pts',(-48.1169536143029,20.26999998,-61.2219104511051));
#141651=CARTESIAN_POINT('Ctrl Pts',(-48.1430951909369,20.26999998,-61.2089878766662));
#141652=CARTESIAN_POINT('Ctrl Pts',(-48.1700747212765,20.26999998,-61.1978560977682));
#141653=CARTESIAN_POINT('Ctrl Pts',(-48.1976781569078,20.26999998,-61.1884510370574));
#141654=CARTESIAN_POINT('Ctrl Pts',(-48.2258927336205,20.26999998,-61.1788377479562));
#141655=CARTESIAN_POINT('Ctrl Pts',(-48.2547605141934,20.26999998,-61.171028311645));
#141656=CARTESIAN_POINT('Ctrl Pts',(-48.284075038586,20.26999998,-61.1650052516751));
#141657=CARTESIAN_POINT('Ctrl Pts',(-48.3128848180532,20.26999998,-61.1590858982813));
#141658=CARTESIAN_POINT('Ctrl Pts',(-48.3421274958272,20.26999998,-61.1548920321836));
#141659=CARTESIAN_POINT('Ctrl Pts',(-48.3716073656787,20.26999998,-61.1524557732793));
#141660=CARTESIAN_POINT('Ctrl Pts',(-48.3917271240067,20.26999998,-61.1507930474726));
#141661=CARTESIAN_POINT('Ctrl Pts',(-48.4119573716394,20.26999998,-61.14995));
#141662=CARTESIAN_POINT('Ctrl Pts',(-48.4322308821779,20.26999998,-61.14995));
#141663=CARTESIAN_POINT('',(-40.8552491802306,20.26999998,-73.4195575571114));
#141664=CARTESIAN_POINT('Ctrl Pts',(-40.8552491802306,20.26999998,-73.4195575571114));
#141665=CARTESIAN_POINT('Ctrl Pts',(-43.2510477030711,20.26999998,-69.4579107098797));
#141666=CARTESIAN_POINT('Ctrl Pts',(-45.5849708137067,20.26999998,-65.4599900833935));
#141667=CARTESIAN_POINT('Ctrl Pts',(-47.878929697957,20.26999998,-61.4386408691297));
#141668=CARTESIAN_POINT('',(-39.5,20.26999998,-78.7897987614789));
#141669=CARTESIAN_POINT('Ctrl Pts',(-39.5,20.26999998,-78.7897987614789));
#141670=CARTESIAN_POINT('Ctrl Pts',(-39.4999999999996,20.26999998,-78.4276754534817));
#141671=CARTESIAN_POINT('Ctrl Pts',(-39.5156108303728,20.26999998,-78.0671937952878));
#141672=CARTESIAN_POINT('Ctrl Pts',(-39.5473687221685,20.26999998,-77.7085899056884));
#141673=CARTESIAN_POINT('Ctrl Pts',(-39.5782679790921,20.26999998,-77.3596815527725));
#141674=CARTESIAN_POINT('Ctrl Pts',(-39.6244528955629,20.26999998,-77.0125506150128));
#141675=CARTESIAN_POINT('Ctrl Pts',(-39.686466172093,20.26999998,-76.6674187362246));
#141676=CARTESIAN_POINT('Ctrl Pts',(-39.7259630317165,20.26999998,-76.447600882196));
#141677=CARTESIAN_POINT('Ctrl Pts',(-39.7718817094826,20.26999998,-76.2285940465893));
#141678=CARTESIAN_POINT('Ctrl Pts',(-39.8243734219799,20.26999998,-76.0104569305838));
#141679=CARTESIAN_POINT('Ctrl Pts',(-39.9341806286948,20.26999998,-75.5541367564111));
#141680=CARTESIAN_POINT('Ctrl Pts',(-40.0717001000673,20.26999998,-75.1087680536983));
#141681=CARTESIAN_POINT('Ctrl Pts',(-40.2410990749131,20.26999998,-74.6759976525381));
#141682=CARTESIAN_POINT('Ctrl Pts',(-40.3724674808339,20.26999998,-74.3403854814384));
#141683=CARTESIAN_POINT('Ctrl Pts',(-40.5227478579483,20.26999998,-74.0122470450345));
#141684=CARTESIAN_POINT('Ctrl Pts',(-40.6973553853198,20.26999998,-73.6937223220025));
#141685=CARTESIAN_POINT('Ctrl Pts',(-40.747903487491,20.26999998,-73.6015108321186));
#141686=CARTESIAN_POINT('Ctrl Pts',(-40.8004906856034,20.26999998,-73.5101051618135));
#141687=CARTESIAN_POINT('Ctrl Pts',(-40.8552491802306,20.26999998,-73.4195575571114));
#141688=CARTESIAN_POINT('',(-39.5,20.26999998,-153.26884421004));
#141689=CARTESIAN_POINT('',(-39.5,20.26999998,-55.24995));
#141690=CARTESIAN_POINT('',(-40.8552491802207,20.26999998,-158.639085414378));
#141691=CARTESIAN_POINT('Ctrl Pts',(-40.8552491802207,20.26999998,-158.639085414378));
#141692=CARTESIAN_POINT('Ctrl Pts',(-40.6523563182981,20.26999998,-158.303585638801));
#141693=CARTESIAN_POINT('Ctrl Pts',(-40.4787269326741,20.26999998,-157.955339387341));
#141694=CARTESIAN_POINT('Ctrl Pts',(-40.3280973119502,20.26999998,-157.59707498981));
#141695=CARTESIAN_POINT('Ctrl Pts',(-40.2977909470182,20.26999998,-157.52499294166));
#141696=CARTESIAN_POINT('Ctrl Pts',(-40.2684157827682,20.26999998,-157.452505284515));
#141697=CARTESIAN_POINT('Ctrl Pts',(-40.2399210161217,20.26999998,-157.379634146926));
#141698=CARTESIAN_POINT('Ctrl Pts',(-40.0698006898873,20.26999998,-156.944576655372));
#141699=CARTESIAN_POINT('Ctrl Pts',(-39.9310881570986,20.26999998,-156.493265246319));
#141700=CARTESIAN_POINT('Ctrl Pts',(-39.8222693035353,20.26999998,-156.039426370008));
#141701=CARTESIAN_POINT('Ctrl Pts',(-39.7053251420368,20.26999998,-155.551700161656));
#141702=CARTESIAN_POINT('Ctrl Pts',(-39.6210196491341,20.26999998,-155.059280307642));
#141703=CARTESIAN_POINT('Ctrl Pts',(-39.5680311845015,20.26999998,-154.562356823708));
#141704=CARTESIAN_POINT('Ctrl Pts',(-39.5224060219208,20.26999998,-154.134486061611));
#141705=CARTESIAN_POINT('Ctrl Pts',(-39.5,20.26999998,-153.703276192992));
#141706=CARTESIAN_POINT('Ctrl Pts',(-39.5,20.26999998,-153.26884421004));
#141707=CARTESIAN_POINT('',(-48.0164881467928,20.26999998,-170.861259130871));
#141708=CARTESIAN_POINT('Ctrl Pts',(-48.0164881467928,20.26999998,-170.861259130871));
#141709=CARTESIAN_POINT('Ctrl Pts',(-45.678332174125,20.26999998,-166.758535769278));
#141710=CARTESIAN_POINT('Ctrl Pts',(-43.29896123138,20.26999998,-162.67996116032));
#141711=CARTESIAN_POINT('Ctrl Pts',(-40.8552491802207,20.26999998,-158.639085414378));
#141712=CARTESIAN_POINT('',(-48.5692718988023,20.26999998,-171.14995));
#141713=CARTESIAN_POINT('Ctrl Pts',(-48.5692718988023,20.26999998,-171.14995));
#141714=CARTESIAN_POINT('Ctrl Pts',(-48.5047948684865,20.26999998,-171.14995));
#141715=CARTESIAN_POINT('Ctrl Pts',(-48.4405703346684,20.26999998,-171.141645130581));
#141716=CARTESIAN_POINT('Ctrl Pts',(-48.3787338163772,20.26999998,-171.124930042695));
#141717=CARTESIAN_POINT('Ctrl Pts',(-48.3356628951272,20.26999998,-171.113287501137));
#141718=CARTESIAN_POINT('Ctrl Pts',(-48.2937500450322,20.26999998,-171.097563680328));
#141719=CARTESIAN_POINT('Ctrl Pts',(-48.2537194844918,20.26999998,-171.077708139862));
#141720=CARTESIAN_POINT('Ctrl Pts',(-48.2190067257619,20.26999998,-171.060490279898));
#141721=CARTESIAN_POINT('Ctrl Pts',(-48.1858587814808,20.26999998,-171.04016650214));
#141722=CARTESIAN_POINT('Ctrl Pts',(-48.1550885346334,20.26999998,-171.016846515546));
#141723=CARTESIAN_POINT('Ctrl Pts',(-48.1271078573602,20.26999998,-170.995640672703));
#141724=CARTESIAN_POINT('Ctrl Pts',(-48.1010921834767,20.26999998,-170.971956505702));
#141725=CARTESIAN_POINT('Ctrl Pts',(-48.0776779540561,20.26999998,-170.945845192498));
#141726=CARTESIAN_POINT('Ctrl Pts',(-48.0545175809105,20.26999998,-170.920016977258));
#141727=CARTESIAN_POINT('Ctrl Pts',(-48.033901319099,20.26999998,-170.891813734436));
#141728=CARTESIAN_POINT('Ctrl Pts',(-48.0164881467928,20.26999998,-170.861259130871));
#141729=CARTESIAN_POINT('',(-50.4557527353536,20.26999998,-171.14995));
#141730=CARTESIAN_POINT('',(-48.9127966158122,20.26999998,-171.14995));
#141731=CARTESIAN_POINT('',(-51.9704940941315,20.26999998,-172.64995));
#141732=CARTESIAN_POINT('Ctrl Pts',(-51.9704940941315,20.26999998,-172.64995));
#141733=CARTESIAN_POINT('Ctrl Pts',(-51.9704940941145,20.26999998,-172.453565067926));
#141734=CARTESIAN_POINT('Ctrl Pts',(-51.9310694254183,20.26999998,-172.257328160063));
#141735=CARTESIAN_POINT('Ctrl Pts',(-51.7793131221354,20.26999998,-171.894521542842));
#141736=CARTESIAN_POINT('Ctrl Pts',(-51.6670411644938,20.26999998,-171.728129909852));
#141737=CARTESIAN_POINT('Ctrl Pts',(-51.3866320792846,20.26999998,-171.450449746589));
#141738=CARTESIAN_POINT('Ctrl Pts',(-51.2186052206426,20.26999998,-171.339270411997));
#141739=CARTESIAN_POINT('Ctrl Pts',(-50.8522330947096,20.26999998,-171.18899099047));
#141740=CARTESIAN_POINT('Ctrl Pts',(-50.6540676547286,20.26999998,-171.149950000016));
#141741=CARTESIAN_POINT('Ctrl Pts',(-50.4557527353536,20.26999998,-171.14995));
#141742=CARTESIAN_POINT('',(-51.9704940941315,20.26999998,-55.24995));
#141743=CARTESIAN_POINT('Origin',(0.,-12.9675000200281,-61.64995));
#141744=CARTESIAN_POINT('',(-52.1700794675439,-38.5802945048887,-61.2273317382593));
#141745=CARTESIAN_POINT('',(-49.0214378669496,-44.1865817238571,-61.2273317382593));
#141746=CARTESIAN_POINT('Origin',(0.,-12.9675000200281,-61.2273317382593));
#141747=CARTESIAN_POINT('',(-49.940073970993,-44.43000002,-60.64995));
#141748=CARTESIAN_POINT('Ctrl Pts',(-49.940073970993,-44.43000002,-60.64995));
#141749=CARTESIAN_POINT('Ctrl Pts',(-49.847975325787,-44.405792727464,-60.64995));
#141750=CARTESIAN_POINT('Ctrl Pts',(-49.7578576522452,-44.382047471718,
-60.6621027778979));
#141751=CARTESIAN_POINT('Ctrl Pts',(-49.581571905815,-44.3354917333839,
-60.7102142267434));
#141752=CARTESIAN_POINT('Ctrl Pts',(-49.494126795535,-44.312341612126,-60.7470666030416));
#141753=CARTESIAN_POINT('Ctrl Pts',(-49.3327124735647,-44.2695203114938,
-60.8438912527599));
#141754=CARTESIAN_POINT('Ctrl Pts',(-49.2581152115204,-44.2496846870305,
-60.9035137960622));
#141755=CARTESIAN_POINT('Ctrl Pts',(-49.1234012768228,-44.2138057335947,
-61.0494267271759));
#141756=CARTESIAN_POINT('Ctrl Pts',(-49.0658454246046,-44.1984444719328,
-61.1333401037095));
#141757=CARTESIAN_POINT('Ctrl Pts',(-49.0214378669496,-44.1865817238571,
-61.2273317382593));
#141758=CARTESIAN_POINT('Origin',(0.,-12.9675000200281,-60.64995));
#141759=CARTESIAN_POINT('Origin',(-53.021204175293,-38.7665567539115,-61.6005868751704));
#141760=CARTESIAN_POINT('Ctrl Pts',(-52.877242281998,-38.7364221486262,
-60.0032396521562));
#141761=CARTESIAN_POINT('Ctrl Pts',(-52.9171740440352,-38.28000002,-60.0032396521562));
#141762=CARTESIAN_POINT('Ctrl Pts',(-53.3753396310439,-38.28000002,-60.0032396521563));
#141763=CARTESIAN_POINT('Ctrl Pts',(-52.8788986395818,-38.7174898948119,
-60.1690974501184));
#141764=CARTESIAN_POINT('Ctrl Pts',(-52.9343465054118,-38.28000002,-60.1721379135101));
#141765=CARTESIAN_POINT('Ctrl Pts',(-53.3753396328414,-38.28000002,-60.244893556147));
#141766=CARTESIAN_POINT('Ctrl Pts',(-52.8422535332614,-38.6982739394415,
-60.3389622441799));
#141767=CARTESIAN_POINT('Ctrl Pts',(-52.9111776732915,-38.28000002,-60.3567456822519));
#141768=CARTESIAN_POINT('Ctrl Pts',(-53.317850201657,-38.28000002,-60.4921247747839));
#141769=CARTESIAN_POINT('Ctrl Pts',(-52.6988044737759,-38.6656865171052,
-60.6372698562504));
#141770=CARTESIAN_POINT('Ctrl Pts',(-52.7751833670329,-38.28000002,-60.6874729542071));
#141771=CARTESIAN_POINT('Ctrl Pts',(-53.0984000724383,-38.28000002,-60.9263821015509));
#141772=CARTESIAN_POINT('Ctrl Pts',(-52.5917711956707,-38.6521075044106,
-60.7679496692827));
#141773=CARTESIAN_POINT('Ctrl Pts',(-52.6635868839933,-38.28000002,-60.8378349680257));
#141774=CARTESIAN_POINT('Ctrl Pts',(-52.9360725977236,-38.28000002,-61.1166772774171));
#141775=CARTESIAN_POINT('Ctrl Pts',(-52.4601060488526,-38.6442121687577,
-60.8635779995784));
#141776=CARTESIAN_POINT('Ctrl Pts',(-52.5193575501106,-38.28000002,-60.9475523661896));
#141777=CARTESIAN_POINT('Ctrl Pts',(-52.7375342894721,-38.28000002,-61.2567639997892));
#141778=CARTESIAN_POINT('',(-52.7375342894721,-38.28000002,-61.2567639997892));
#141779=CARTESIAN_POINT('Ctrl Pts',(-53.3753396310439,-38.28000002,-60.0032396521563));
#141780=CARTESIAN_POINT('Ctrl Pts',(-53.3753396310439,-38.28000002,-60.0589758767835));
#141781=CARTESIAN_POINT('Ctrl Pts',(-53.3722852139107,-38.28000002,-60.1146939077158));
#141782=CARTESIAN_POINT('Ctrl Pts',(-53.3663204826485,-38.28000002,-60.1700562792009));
#141783=CARTESIAN_POINT('Ctrl Pts',(-53.3600346473475,-38.28000002,-60.2283990164901));
#141784=CARTESIAN_POINT('Ctrl Pts',(-53.3505169273235,-38.28000002,-60.2863478004802));
#141785=CARTESIAN_POINT('Ctrl Pts',(-53.3378827651207,-38.28000002,-60.3435292248105));
#141786=CARTESIAN_POINT('Ctrl Pts',(-53.3251015247972,-38.28000002,-60.4013763154742));
#141787=CARTESIAN_POINT('Ctrl Pts',(-53.3091307297629,-38.28000002,-60.458439390228));
#141788=CARTESIAN_POINT('Ctrl Pts',(-53.2900367865638,-38.2800000200001,
-60.514335009952));
#141789=CARTESIAN_POINT('Ctrl Pts',(-53.2713085336432,-38.2800000200001,
-60.5691601077553));
#141790=CARTESIAN_POINT('Ctrl Pts',(-53.2495752764748,-38.2800000200002,
-60.6228632354968));
#141791=CARTESIAN_POINT('Ctrl Pts',(-53.2248527900284,-38.2800000200003,
-60.6750669890667));
#141792=CARTESIAN_POINT('Ctrl Pts',(-53.2194501346316,-38.2800000200003,
-60.6864751818296));
#141793=CARTESIAN_POINT('Ctrl Pts',(-53.2139045547126,-38.2800000200004,
-60.6978116715983));
#141794=CARTESIAN_POINT('Ctrl Pts',(-53.2082159323665,-38.2800000200004,
-60.7090723322489));
#141795=CARTESIAN_POINT('Ctrl Pts',(-53.2081854825349,-38.2800000200004,
-60.7091326078656));
#141796=CARTESIAN_POINT('Ctrl Pts',(-53.2081550286956,-38.2800000200004,
-60.7091928811299));
#141797=CARTESIAN_POINT('Ctrl Pts',(-53.2081245708486,-38.2800000200004,
-60.7092531520411));
#141798=CARTESIAN_POINT('Ctrl Pts',(-53.1761754390121,-38.2800000200006,
-60.7724750628699));
#141799=CARTESIAN_POINT('Ctrl Pts',(-53.1397892479681,-38.2800000200007,
-60.833387133241));
#141800=CARTESIAN_POINT('Ctrl Pts',(-53.0993211720575,-38.2800000200006,
-60.8914909948822));
#141801=CARTESIAN_POINT('Ctrl Pts',(-53.0593989894049,-38.2800000200005,
-60.948811065705));
#141802=CARTESIAN_POINT('Ctrl Pts',(-53.0155035526423,-38.2800000200003,
-61.003399073172));
#141803=CARTESIAN_POINT('Ctrl Pts',(-52.9679386190619,-38.2800000200002,
-61.0547432417688));
#141804=CARTESIAN_POINT('Ctrl Pts',(-52.9223553337123,-38.2800000200001,
-61.103948311807));
#141805=CARTESIAN_POINT('Ctrl Pts',(-52.8734012103222,-38.28000002,-61.1501747492911));
#141806=CARTESIAN_POINT('Ctrl Pts',(-52.8213200539946,-38.28000002,-61.1929312639283));
#141807=CARTESIAN_POINT('Ctrl Pts',(-52.7942271507162,-38.28000002,-61.2151734374372));
#141808=CARTESIAN_POINT('Ctrl Pts',(-52.7662877001538,-38.28000002,-61.2364758695292));
#141809=CARTESIAN_POINT('Ctrl Pts',(-52.7375342894721,-38.28000002,-61.2567639997892));
#141810=CARTESIAN_POINT('Origin',(-52.7375342894721,-38.78000002,-61.2567639997892));
#141811=CARTESIAN_POINT('Origin',(83.2809572255632,-38.28000002,-55.2499500000007));
#141812=CARTESIAN_POINT('',(-52.7704579175045,-38.28000002,-170.960578619515));
#141813=CARTESIAN_POINT('',(-53.1262583325313,-38.28000002,-171.916267709546));
#141814=CARTESIAN_POINT('Ctrl Pts',(-52.7704579175044,-38.28000002,-170.960578619515));
#141815=CARTESIAN_POINT('Ctrl Pts',(-52.8285971612714,-38.28000002,-171.026452630405));
#141816=CARTESIAN_POINT('Ctrl Pts',(-52.8797920295936,-38.28000002,-171.096554170654));
#141817=CARTESIAN_POINT('Ctrl Pts',(-52.9240704508372,-38.28000002,-171.170767761981));
#141818=CARTESIAN_POINT('Ctrl Pts',(-52.9683488720808,-38.28000002,-171.244981353309));
#141819=CARTESIAN_POINT('Ctrl Pts',(-53.0057109090821,-38.28000002,-171.323307205357));
#141820=CARTESIAN_POINT('Ctrl Pts',(-53.0361319037073,-38.28000002,-171.405662091087));
#141821=CARTESIAN_POINT('Ctrl Pts',(-53.0782642785414,-38.28000002,-171.519721705435));
#141822=CARTESIAN_POINT('Ctrl Pts',(-53.1052589026233,-38.28000002,-171.636480608475));
#141823=CARTESIAN_POINT('Ctrl Pts',(-53.1178820115772,-38.28000002,-171.755802197905));
#141824=CARTESIAN_POINT('Ctrl Pts',(-53.1234875228305,-38.28000002,-171.808789026646));
#141825=CARTESIAN_POINT('Ctrl Pts',(-53.126258330058,-38.28000002,-171.862281331533));
#141826=CARTESIAN_POINT('Ctrl Pts',(-53.1262583325313,-38.28000002,-171.916267709546));
#141827=CARTESIAN_POINT('',(-52.7021525552272,-38.28000002,-170.861259130871));
#141828=CARTESIAN_POINT('Ctrl Pts',(-52.7021525552272,-38.28000002,-170.861259130871));
#141829=CARTESIAN_POINT('Ctrl Pts',(-52.7208104423973,-38.28000002,-170.897192602603));
#141830=CARTESIAN_POINT('Ctrl Pts',(-52.7436752534113,-38.28000002,-170.930232830913));
#141831=CARTESIAN_POINT('Ctrl Pts',(-52.7704579175045,-38.28000002,-170.960578619515));
#141832=CARTESIAN_POINT('',(-40.5593018105246,-38.28000002,-148.113408860656));
#141833=CARTESIAN_POINT('Ctrl Pts',(-40.5593018105246,-38.28000002,-148.113408860656));
#141834=CARTESIAN_POINT('Ctrl Pts',(-42.6385266988695,-38.28000002,-151.875135830624));
#141835=CARTESIAN_POINT('Ctrl Pts',(-44.6827387638261,-38.28000002,-155.655552720007));
#141836=CARTESIAN_POINT('Ctrl Pts',(-46.7035558598462,-38.28000002,-159.448457893456));
#141837=CARTESIAN_POINT('Ctrl Pts',(-48.7243729558662,-38.28000002,-163.241363066904));
#141838=CARTESIAN_POINT('Ctrl Pts',(-50.7215893876843,-38.28000002,-167.046866324983));
#141839=CARTESIAN_POINT('Ctrl Pts',(-52.7021525552272,-38.28000002,-170.86125913087));
#141840=CARTESIAN_POINT('',(-39.5,-38.28000002,-143.762156710948));
#141841=CARTESIAN_POINT('Ctrl Pts',(-39.5,-38.28000002,-143.762156710948));
#141842=CARTESIAN_POINT('Ctrl Pts',(-39.5,-38.28000002,-144.141283590664));
#141843=CARTESIAN_POINT('Ctrl Pts',(-39.5218408888636,-38.28000002,-144.518367123251));
#141844=CARTESIAN_POINT('Ctrl Pts',(-39.5652079410422,-38.28000002,-144.893436753186));
#141845=CARTESIAN_POINT('Ctrl Pts',(-39.6085749932207,-38.28000002,-145.26850638312));
#141846=CARTESIAN_POINT('Ctrl Pts',(-39.6739630147302,-38.28000002,-145.643330762739));
#141847=CARTESIAN_POINT('Ctrl Pts',(-39.7609941006785,-38.28000002,-146.010070025021));
#141848=CARTESIAN_POINT('Ctrl Pts',(-39.8480251866268,-38.28000002,-146.376809287303));
#141849=CARTESIAN_POINT('Ctrl Pts',(-39.9556757536423,-38.28000002,-146.736297755287));
#141850=CARTESIAN_POINT('Ctrl Pts',(-40.0875243805731,-38.28000002,-147.087277124802));
#141851=CARTESIAN_POINT('Ctrl Pts',(-40.2065170359403,-38.28000002,-147.404034061373));
#141852=CARTESIAN_POINT('Ctrl Pts',(-40.3452186968574,-38.28000002,-147.713860479167));
#141853=CARTESIAN_POINT('Ctrl Pts',(-40.5063035885313,-38.28000002,-148.015815905667));
#141854=CARTESIAN_POINT('Ctrl Pts',(-40.5237072071016,-38.28000002,-148.048439182831));
#141855=CARTESIAN_POINT('Ctrl Pts',(-40.5413721449694,-38.28000002,-148.080970567495));
#141856=CARTESIAN_POINT('Ctrl Pts',(-40.5593018105246,-38.28000002,-148.113408860656));
#141857=CARTESIAN_POINT('',(-39.5,-38.28000002,-88.296486260558));
#141858=CARTESIAN_POINT('',(-39.5,-38.28000002,-55.2499500000007));
#141859=CARTESIAN_POINT('',(-40.5593018105246,-38.28000002,-83.9452341108497));
#141860=CARTESIAN_POINT('Ctrl Pts',(-40.5593018105246,-38.28000002,-83.9452341108497));
#141861=CARTESIAN_POINT('Ctrl Pts',(-40.495353484328,-38.28000002,-84.0609292165928));
#141862=CARTESIAN_POINT('Ctrl Pts',(-40.4347639681505,-38.28000002,-84.1780768945295));
#141863=CARTESIAN_POINT('Ctrl Pts',(-40.3773169004728,-38.28000002,-84.2965776208556));
#141864=CARTESIAN_POINT('Ctrl Pts',(-40.3173964789325,-38.28000002,-84.4201803348204));
#141865=CARTESIAN_POINT('Ctrl Pts',(-40.2608947873255,-38.28000002,-84.5452556205675));
#141866=CARTESIAN_POINT('Ctrl Pts',(-40.207615546208,-38.28000002,-84.6717210755968));
#141867=CARTESIAN_POINT('Ctrl Pts',(-40.1651845073098,-38.28000002,-84.7724368615028));
#141868=CARTESIAN_POINT('Ctrl Pts',(-40.1247982681521,-38.28000002,-84.8740350854922));
#141869=CARTESIAN_POINT('Ctrl Pts',(-40.086379235959,-38.28000002,-84.9764835369928));
#141870=CARTESIAN_POINT('Ctrl Pts',(-40.0265153547945,-38.28000002,-85.1361169680306));
#141871=CARTESIAN_POINT('Ctrl Pts',(-39.971455536752,-38.28000002,-85.2977643783894));
#141872=CARTESIAN_POINT('Ctrl Pts',(-39.9211479365401,-38.28000002,-85.4606561619592));
#141873=CARTESIAN_POINT('Ctrl Pts',(-39.8688810993164,-38.28000002,-85.6298917903944));
#141874=CARTESIAN_POINT('Ctrl Pts',(-39.821743908823,-38.28000002,-85.8004696290636));
#141875=CARTESIAN_POINT('Ctrl Pts',(-39.7796250224717,-38.28000002,-85.9715109372541));
#141876=CARTESIAN_POINT('Ctrl Pts',(-39.7722762919974,-38.28000002,-86.0013535229144));
#141877=CARTESIAN_POINT('Ctrl Pts',(-39.7650802005722,-38.28000002,-86.0312102022423));
#141878=CARTESIAN_POINT('Ctrl Pts',(-39.758035997616,-38.28000002,-86.0610762975502));
#141879=CARTESIAN_POINT('Ctrl Pts',(-39.6557558157212,-38.28000002,-86.4947250268103));
#141880=CARTESIAN_POINT('Ctrl Pts',(-39.5840763701735,-38.28000002,-86.933158987616));
#141881=CARTESIAN_POINT('Ctrl Pts',(-39.5426478307198,-38.28000002,-87.3763235090948));
#141882=CARTESIAN_POINT('Ctrl Pts',(-39.5141828100106,-38.28000002,-87.6808161957276));
#141883=CARTESIAN_POINT('Ctrl Pts',(-39.5,-38.28000002,-87.9875423033807));
#141884=CARTESIAN_POINT('Ctrl Pts',(-39.5,-38.28000002,-88.296486260558));
#141885=CARTESIAN_POINT('',(-52.5768547844511,-38.28000002,-61.4386408691297));
#141886=CARTESIAN_POINT('Ctrl Pts',(-52.5768547844511,-38.28000002,-61.4386408691297));
#141887=CARTESIAN_POINT('Ctrl Pts',(-50.6164600523975,-38.28000002,-65.2124493416261));
#141888=CARTESIAN_POINT('Ctrl Pts',(-48.6396458371541,-38.28000002,-68.9774905161615));
#141889=CARTESIAN_POINT('Ctrl Pts',(-46.6396326262455,-38.28000002,-72.7301444246032));
#141890=CARTESIAN_POINT('Ctrl Pts',(-44.6396194153369,-38.28000002,-76.4827983330448));
#141891=CARTESIAN_POINT('Ctrl Pts',(-42.6166038138442,-38.28000002,-80.2231699540513));
#141892=CARTESIAN_POINT('Ctrl Pts',(-40.5593018105246,-38.28000002,-83.9452341108497));
#141893=CARTESIAN_POINT('Origin',(-53.0468858550318,-38.28000002,-61.6241485284586));
#141894=CARTESIAN_POINT('',(-59.5,-38.28000002,-58.24995));
#141895=CARTESIAN_POINT('Origin',(-57.,-38.28000002,-58.24995));
#141896=CARTESIAN_POINT('',(-59.5,-38.28000002,-174.34995));
#141897=CARTESIAN_POINT('',(-59.5,-38.28000002,-58.24995));
#141898=CARTESIAN_POINT('',(-57.,-38.28000002,-176.84995));
#141899=CARTESIAN_POINT('Origin',(-57.,-38.28000002,-174.34995));
#141900=CARTESIAN_POINT('',(-53.1262583325313,-38.28000002,-176.84995));
#141901=CARTESIAN_POINT('',(83.2809572255632,-38.28000002,-176.84995));
#141902=CARTESIAN_POINT('',(-53.1262583325313,-38.28000002,-176.84995));
#141903=CARTESIAN_POINT('Ctrl Pts',(-51.4511770665258,-55.0364221486262,
-59.64995));
#141904=CARTESIAN_POINT('Ctrl Pts',(-51.491108828563,-54.58000002,-59.64995));
#141905=CARTESIAN_POINT('Ctrl Pts',(-51.9492744155716,-54.58000002,-59.64995));
#141906=CARTESIAN_POINT('Ctrl Pts',(-51.4511770665255,-55.0364221486294,
-59.7808732880376));
#141907=CARTESIAN_POINT('Ctrl Pts',(-51.4911088285445,-54.58000002,-59.7861314644994));
#141908=CARTESIAN_POINT('Ctrl Pts',(-51.9492744155546,-54.58000002,-59.8463349320562));
#141909=CARTESIAN_POINT('Ctrl Pts',(-51.4249510883276,-55.0375563641359,
-59.9116978933072));
#141910=CARTESIAN_POINT('Ctrl Pts',(-51.4627154806765,-54.58000002,-59.9224177216068));
#141911=CARTESIAN_POINT('Ctrl Pts',(-51.9100842947729,-54.58000002,-60.0425718399611));
#141912=CARTESIAN_POINT('Ctrl Pts',(-51.3240001449277,-55.0419222689988,
-60.153568971423));
#141913=CARTESIAN_POINT('Ctrl Pts',(-51.3546036645756,-54.58000002,-60.1718710142638));
#141914=CARTESIAN_POINT('Ctrl Pts',(-51.7592308304456,-54.58000002,-60.4053784571342));
#141915=CARTESIAN_POINT('Ctrl Pts',(-51.2493148777934,-55.0451522414979,
-60.2644967268049));
#141916=CARTESIAN_POINT('Ctrl Pts',(-51.2745855330292,-54.58000002,-60.2852157712116));
#141917=CARTESIAN_POINT('Ctrl Pts',(-51.6476268087097,-54.58000002,-60.5717700902076));
#141918=CARTESIAN_POINT('Ctrl Pts',(-51.0627818569665,-55.0532193817859,
-60.4496168355682));
#141919=CARTESIAN_POINT('Ctrl Pts',(-51.0776549189628,-54.58000002,-60.4706504746468));
#141920=CARTESIAN_POINT('Ctrl Pts',(-51.3688859524529,-54.58000002,-60.8494502533521));
#141921=CARTESIAN_POINT('Ctrl Pts',(-50.9510074558263,-55.0580533772402,
-60.5237363920407));
#141922=CARTESIAN_POINT('Ctrl Pts',(-50.9603478356083,-54.5800000199993,
-60.5426326522464));
#141923=CARTESIAN_POINT('Ctrl Pts',(-51.2018587304451,-54.58000002,-60.9606295880612));
#141924=CARTESIAN_POINT('Ctrl Pts',(-50.707290319039,-55.0685936039748,
-60.6239226729819));
#141925=CARTESIAN_POINT('Ctrl Pts',(-50.7089726167645,-54.5800000200007,
-60.6353187454038));
#141926=CARTESIAN_POINT('Ctrl Pts',(-50.8376662507899,-54.58000002,-61.1109090094727));
#141927=CARTESIAN_POINT('Ctrl Pts',(-50.5754672071858,-55.0742946617933,
-60.64995));
#141928=CARTESIAN_POINT('Ctrl Pts',(-50.5746911290892,-54.58000002,-60.6556217969812));
#141929=CARTESIAN_POINT('Ctrl Pts',(-50.6406797499036,-54.58000002,-61.149949999985));
#141930=CARTESIAN_POINT('Ctrl Pts',(-50.4435446592566,-55.08000002,-60.64995));
#141931=CARTESIAN_POINT('Ctrl Pts',(-50.4435446592566,-54.58000002,-60.64995));
#141932=CARTESIAN_POINT('Ctrl Pts',(-50.4435446592566,-54.58000002,-61.14995));
#141933=CARTESIAN_POINT('',(-50.4435446592566,-54.58000002,-61.14995));
#141934=CARTESIAN_POINT('Origin',(-50.4435446592566,-55.08000002,-61.14995));
#141935=CARTESIAN_POINT('Ctrl Pts',(-51.9492744155716,-54.58000002,-59.64995));
#141936=CARTESIAN_POINT('Ctrl Pts',(-51.9492744155546,-54.58000002,-59.8463349320562));
#141937=CARTESIAN_POINT('Ctrl Pts',(-51.9100842947729,-54.58000002,-60.0425718399611));
#141938=CARTESIAN_POINT('Ctrl Pts',(-51.7592308304456,-54.58000002,-60.4053784571342));
#141939=CARTESIAN_POINT('Ctrl Pts',(-51.6476268087097,-54.58000002,-60.5717700902076));
#141940=CARTESIAN_POINT('Ctrl Pts',(-51.3688859524529,-54.58000002,-60.8494502533521));
#141941=CARTESIAN_POINT('Ctrl Pts',(-51.2018587304451,-54.58000002,-60.9606295880612));
#141942=CARTESIAN_POINT('Ctrl Pts',(-50.8376662507899,-54.58000002,-61.1109090094727));
#141943=CARTESIAN_POINT('Ctrl Pts',(-50.6406797499036,-54.58000002,-61.149949999985));
#141944=CARTESIAN_POINT('Ctrl Pts',(-50.4435446592566,-54.58000002,-61.14995));
#141945=CARTESIAN_POINT('Origin',(-60.,-54.58000002,-55.24995));
#141946=CARTESIAN_POINT('',(-49.2787232447289,-54.58000002,-171.14995));
#141947=CARTESIAN_POINT('',(-50.7934646035069,-54.58000002,-172.64995));
#141948=CARTESIAN_POINT('Ctrl Pts',(-49.2787232447289,-54.58000002,-171.14995));
#141949=CARTESIAN_POINT('Ctrl Pts',(-49.477038164104,-54.58000002,-171.149950000016));
#141950=CARTESIAN_POINT('Ctrl Pts',(-49.6752036040849,-54.58000002,-171.18899099047));
#141951=CARTESIAN_POINT('Ctrl Pts',(-50.0415757300179,-54.58000002,-171.339270411997));
#141952=CARTESIAN_POINT('Ctrl Pts',(-50.2096025886599,-54.58000002,-171.450449746589));
#141953=CARTESIAN_POINT('Ctrl Pts',(-50.4900116738692,-54.58000002,-171.728129909852));
#141954=CARTESIAN_POINT('Ctrl Pts',(-50.6022836315107,-54.58000002,-171.894521542842));
#141955=CARTESIAN_POINT('Ctrl Pts',(-50.7540399347937,-54.58000002,-172.257328160063));
#141956=CARTESIAN_POINT('Ctrl Pts',(-50.7934646034919,-54.58000002,-172.453565067926));
#141957=CARTESIAN_POINT('Ctrl Pts',(-50.7934646035069,-54.58000002,-172.64995));
#141958=CARTESIAN_POINT('',(-45.8586217441902,-54.58000002,-171.14995));
#141959=CARTESIAN_POINT('',(-49.3489936620801,-54.58000002,-171.14995));
#141960=CARTESIAN_POINT('',(-43.1572831724514,-54.58000002,-171.14995));
#141961=CARTESIAN_POINT('Ctrl Pts',(-43.1572831724514,-54.58000002,-171.14995));
#141962=CARTESIAN_POINT('Ctrl Pts',(-43.279524411259,-54.58000002,-171.149950030568));
#141963=CARTESIAN_POINT('Ctrl Pts',(-43.4015975649118,-54.58000002,-171.160610139864));
#141964=CARTESIAN_POINT('Ctrl Pts',(-43.5235528170126,-54.58000002,-171.176313109177));
#141965=CARTESIAN_POINT('Ctrl Pts',(-43.6257700730144,-54.5800000200001,
-171.189474612323));
#141966=CARTESIAN_POINT('Ctrl Pts',(-43.7279044984664,-54.5800000200001,
-171.206180488419));
#141967=CARTESIAN_POINT('Ctrl Pts',(-43.829985527596,-54.5800000200001,
-171.223144870208));
#141968=CARTESIAN_POINT('Ctrl Pts',(-43.9984923413766,-54.5800000200002,
-171.251148250928));
#141969=CARTESIAN_POINT('Ctrl Pts',(-44.1669616089445,-54.5800000200002,
-171.278751491316));
#141970=CARTESIAN_POINT('Ctrl Pts',(-44.3358012503232,-54.5800000200001,
-171.290923113047));
#141971=CARTESIAN_POINT('Ctrl Pts',(-44.3914319971545,-54.5800000200001,
-171.294933524355));
#141972=CARTESIAN_POINT('Ctrl Pts',(-44.4471029574849,-54.5800000200001,
-171.297268373358));
#141973=CARTESIAN_POINT('Ctrl Pts',(-44.5028287572164,-54.58000002,-171.297388261734));
#141974=CARTESIAN_POINT('Ctrl Pts',(-44.5028370935956,-54.58000002,-171.297388279669));
#141975=CARTESIAN_POINT('Ctrl Pts',(-44.5028454299759,-54.58000002,-171.297388297554));
#141976=CARTESIAN_POINT('Ctrl Pts',(-44.5028537663573,-54.58000002,-171.29738831539));
#141977=CARTESIAN_POINT('Ctrl Pts',(-44.7276220562719,-54.58000002,-171.297869208197));
#141978=CARTESIAN_POINT('Ctrl Pts',(-44.9531763212381,-54.5800000200004,
-171.261837296445));
#141979=CARTESIAN_POINT('Ctrl Pts',(-45.1787623634369,-54.5800000200001,
-171.22433455003));
#141980=CARTESIAN_POINT('Ctrl Pts',(-45.1788060542272,-54.5800000200001,
-171.224327286617));
#141981=CARTESIAN_POINT('Ctrl Pts',(-45.178849745033,-54.5800000200001,
-171.224320023146));
#141982=CARTESIAN_POINT('Ctrl Pts',(-45.1788934358544,-54.5800000200001,
-171.224312759618));
#141983=CARTESIAN_POINT('Ctrl Pts',(-45.2946034848909,-54.58000002,-171.205076152327));
#141984=CARTESIAN_POINT('Ctrl Pts',(-45.4103612459202,-54.58000002,-171.185995253716));
#141985=CARTESIAN_POINT('Ctrl Pts',(-45.5265088418228,-54.58000002,-171.171982248345));
#141986=CARTESIAN_POINT('Ctrl Pts',(-45.6241378685024,-54.58000002,-171.160203476132));
#141987=CARTESIAN_POINT('Ctrl Pts',(-45.7220426205362,-54.58000002,-171.152008348194));
#141988=CARTESIAN_POINT('Ctrl Pts',(-45.8204240164945,-54.58000002,-171.150287040904));
#141989=CARTESIAN_POINT('Ctrl Pts',(-45.8331484827184,-54.58000002,-171.150064410231));
#141990=CARTESIAN_POINT('Ctrl Pts',(-45.8458809158945,-54.58000002,-171.149950003086));
#141991=CARTESIAN_POINT('Ctrl Pts',(-45.8586217441902,-54.58000002,-171.14995));
#141992=CARTESIAN_POINT('',(-42.5,-54.58000002,-171.14995));
#141993=CARTESIAN_POINT('',(-49.3489936620801,-54.58000002,-171.14995));
#141994=CARTESIAN_POINT('',(-42.5,-54.58000002,-61.14995));
#141995=CARTESIAN_POINT('',(-42.5,-54.58000002,-171.64995));
#141996=CARTESIAN_POINT('',(-43.1572831724516,-54.58000002,-61.14995));
#141997=CARTESIAN_POINT('',(-60.,-54.58000002,-61.14995));
#141998=CARTESIAN_POINT('',(-45.8586217441897,-54.58000002,-61.14995));
#141999=CARTESIAN_POINT('Ctrl Pts',(-45.8586217441897,-54.58000002,-61.14995));
#142000=CARTESIAN_POINT('Ctrl Pts',(-45.7594843223745,-54.58000002,-61.1499499759911));
#142001=CARTESIAN_POINT('Ctrl Pts',(-45.660855613418,-54.58000002,-61.1430183938606));
#142002=CARTESIAN_POINT('Ctrl Pts',(-45.5625314448157,-54.58000002,-61.1320945152429));
#142003=CARTESIAN_POINT('Ctrl Pts',(-45.4342876572931,-54.58000002,-61.1178465476446));
#142004=CARTESIAN_POINT('Ctrl Pts',(-45.3065614560445,-54.58000002,-61.0968118490375));
#142005=CARTESIAN_POINT('Ctrl Pts',(-45.1788934332666,-54.5800000200001,
-61.075587255946));
#142006=CARTESIAN_POINT('Ctrl Pts',(-45.1788516209101,-54.5800000200001,
-61.0755803047123));
#142007=CARTESIAN_POINT('Ctrl Pts',(-45.1788098085678,-54.5800000200001,
-61.0755733535312));
#142008=CARTESIAN_POINT('Ctrl Pts',(-45.1787679962398,-54.5800000200001,
-61.0755664024026));
#142009=CARTESIAN_POINT('Ctrl Pts',(-44.9531807615356,-54.5800000200004,
-61.0380634472604));
#142010=CARTESIAN_POINT('Ctrl Pts',(-44.7276252028241,-54.58000002,-61.0020307849363));
#142011=CARTESIAN_POINT('Ctrl Pts',(-44.5028537665277,-54.58000002,-61.0025117642945));
#142012=CARTESIAN_POINT('Ctrl Pts',(-44.502848607531,-54.58000002,-61.002511775334));
#142013=CARTESIAN_POINT('Ctrl Pts',(-44.5028434485348,-54.58000002,-61.0025117863925));
#142014=CARTESIAN_POINT('Ctrl Pts',(-44.502838289539,-54.58000002,-61.00251179747));
#142015=CARTESIAN_POINT('Ctrl Pts',(-44.3506760857117,-54.58000002,-61.0028385232137));
#142016=CARTESIAN_POINT('Ctrl Pts',(-44.1989241833619,-54.5800000200001,
-61.0196754576617));
#142017=CARTESIAN_POINT('Ctrl Pts',(-44.0472833113151,-54.5800000200001,
-61.0420612980709));
#142018=CARTESIAN_POINT('Ctrl Pts',(-43.9748362264978,-54.5800000200001,
-61.0527562304921));
#142019=CARTESIAN_POINT('Ctrl Pts',(-43.9024145037625,-54.58000002,-61.0647186315171));
#142020=CARTESIAN_POINT('Ctrl Pts',(-43.8299855489727,-54.58000002,-61.0767552584245));
#142021=CARTESIAN_POINT('Ctrl Pts',(-43.7015244308365,-54.58000002,-61.0981036066867));
#142022=CARTESIAN_POINT('Ctrl Pts',(-43.5729778197523,-54.58000002,-61.1190439724879));
#142023=CARTESIAN_POINT('Ctrl Pts',(-43.4442858805813,-54.58000002,-61.1330238652824));
#142024=CARTESIAN_POINT('Ctrl Pts',(-43.348706683562,-54.58000002,-61.1434066983979));
#142025=CARTESIAN_POINT('Ctrl Pts',(-43.2530473192986,-54.58000002,-61.1499499760532));
#142026=CARTESIAN_POINT('Ctrl Pts',(-43.1572831724516,-54.58000002,-61.14995));
#142027=CARTESIAN_POINT('',(-60.,-54.58000002,-61.14995));
#142028=CARTESIAN_POINT('',(-57.,-54.58000002,-55.74995));
#142029=CARTESIAN_POINT('',(-60.,-54.58000002,-55.74995));
#142030=CARTESIAN_POINT('',(-59.5,-54.58000002,-58.24995));
#142031=CARTESIAN_POINT('Origin',(-57.,-54.58000002,-58.24995));
#142032=CARTESIAN_POINT('',(-59.5,-54.58000002,-174.34995));
#142033=CARTESIAN_POINT('',(-59.5,-54.58000002,-58.24995));
#142034=CARTESIAN_POINT('',(-57.,-54.58000002,-176.84995));
#142035=CARTESIAN_POINT('Origin',(-57.,-54.58000002,-174.34995));
#142036=CARTESIAN_POINT('',(-50.7934646035069,-54.58000002,-176.84995));
#142037=CARTESIAN_POINT('',(-60.,-54.58000002,-176.84995));
#142038=CARTESIAN_POINT('',(-50.7934646035069,-54.58000002,-55.24995));
#142039=CARTESIAN_POINT('Origin',(-60.,-54.08000002,-55.74995));
#142040=CARTESIAN_POINT('',(-57.,-54.08000002,-55.24995));
#142041=CARTESIAN_POINT('',(-60.,-54.08000002,-55.24995));
#142042=CARTESIAN_POINT('Origin',(-57.,-54.08000002,-55.74995));
#142043=CARTESIAN_POINT('Origin',(-60.,28.41999998,-55.24995));
#142044=CARTESIAN_POINT('',(-57.,-53.58000002,-55.24995));
#142045=CARTESIAN_POINT('',(-60.,-53.58000002,-55.24995));
#142046=CARTESIAN_POINT('',(-57.,28.41999998,-55.24995));
#142047=CARTESIAN_POINT('Origin',(83.2809572255632,-53.5800000199999,-55.74995));
#142048=CARTESIAN_POINT('',(-57.,-53.08000002,-55.74995));
#142049=CARTESIAN_POINT('',(83.2809572255632,-53.0800000199999,-55.74995));
#142050=CARTESIAN_POINT('Origin',(-57.,-53.58000002,-55.74995));
#142051=CARTESIAN_POINT('Origin',(83.2809572255632,-53.0800000199999,-55.2499500000008));
#142052=CARTESIAN_POINT('',(-57.,-53.08000002,-176.84995));
#142053=CARTESIAN_POINT('',(-51.1448166902628,-53.08000002,-176.84995));
#142054=CARTESIAN_POINT('',(83.2809572255632,-53.0800000199999,-176.84995));
#142055=CARTESIAN_POINT('',(-59.5,-53.08000002,-174.34995));
#142056=CARTESIAN_POINT('Origin',(-57.,-53.08000002,-174.34995));
#142057=CARTESIAN_POINT('',(-59.5,-53.08000002,-58.24995));
#142058=CARTESIAN_POINT('',(-59.5,-53.08000002,-174.34995));
#142059=CARTESIAN_POINT('Origin',(-57.,-53.08000002,-58.24995));
#142060=CARTESIAN_POINT('',(-50.6622663180714,-53.08000002,-61.14995));
#142061=CARTESIAN_POINT('Ctrl Pts',(-50.6622663180714,-53.08000002,-61.14995));
#142062=CARTESIAN_POINT('Ctrl Pts',(-50.8594014087184,-53.08000002,-61.149949999985));
#142063=CARTESIAN_POINT('Ctrl Pts',(-51.0563879096046,-53.08000002,-61.1109090094727));
#142064=CARTESIAN_POINT('Ctrl Pts',(-51.4205803892599,-53.08000002,-60.9606295880612));
#142065=CARTESIAN_POINT('Ctrl Pts',(-51.5876076112677,-53.08000002,-60.8494502533514));
#142066=CARTESIAN_POINT('Ctrl Pts',(-51.8663484675245,-53.08000002,-60.5717700902082));
#142067=CARTESIAN_POINT('Ctrl Pts',(-51.9779524892604,-53.08000002,-60.4053784571342));
#142068=CARTESIAN_POINT('Ctrl Pts',(-52.1288059535877,-53.08000002,-60.0425718399611));
#142069=CARTESIAN_POINT('Ctrl Pts',(-52.1679960743694,-53.08000002,-59.8463349320561));
#142070=CARTESIAN_POINT('Ctrl Pts',(-52.1679960743864,-53.08000002,-59.64995));
#142071=CARTESIAN_POINT('',(-43.7578534463097,-53.08000002,-61.14995));
#142072=CARTESIAN_POINT('',(83.2809572255632,-53.0800000199999,-61.14995));
#142073=CARTESIAN_POINT('',(-43.1446480925044,-53.08000002,-61.4386408691297));
#142074=CARTESIAN_POINT('Ctrl Pts',(-43.1446480925044,-53.08000002,-61.4386408691297));
#142075=CARTESIAN_POINT('Ctrl Pts',(-43.1765609373872,-53.08000002,-61.3882288400421));
#142076=CARTESIAN_POINT('Ctrl Pts',(-43.2167516388878,-53.08000002,-61.3458652617053));
#142077=CARTESIAN_POINT('Ctrl Pts',(-43.2628503174202,-53.08000002,-61.3093295271296));
#142078=CARTESIAN_POINT('Ctrl Pts',(-43.3089610210815,-53.08000002,-61.2727842619789));
#142079=CARTESIAN_POINT('Ctrl Pts',(-43.3605330051288,-53.08000002,-61.2428744748388));
#142080=CARTESIAN_POINT('Ctrl Pts',(-43.414231413078,-53.08000002,-61.2194436041558));
#142081=CARTESIAN_POINT('Ctrl Pts',(-43.4456262415641,-53.08000002,-61.205744721927));
#142082=CARTESIAN_POINT('Ctrl Pts',(-43.477917759742,-53.08000002,-61.1941576093824));
#142083=CARTESIAN_POINT('Ctrl Pts',(-43.5108494925037,-53.08000002,-61.1845858141908));
#142084=CARTESIAN_POINT('Ctrl Pts',(-43.5447058226298,-53.08000002,-61.1747452795231));
#142085=CARTESIAN_POINT('Ctrl Pts',(-43.5792402145375,-53.08000002,-61.1670347524206));
#142086=CARTESIAN_POINT('Ctrl Pts',(-43.6141927055652,-53.08000002,-61.1614020099222));
#142087=CARTESIAN_POINT('Ctrl Pts',(-43.6489049458008,-53.08000002,-61.1558079848602));
#142088=CARTESIAN_POINT('Ctrl Pts',(-43.6840310643501,-53.08000002,-61.1522634649488));
#142089=CARTESIAN_POINT('Ctrl Pts',(-43.7193126347007,-53.08000002,-61.1507670586125));
#142090=CARTESIAN_POINT('Ctrl Pts',(-43.7321435462893,-53.08000002,-61.1502228578524));
#142091=CARTESIAN_POINT('Ctrl Pts',(-43.7449948697401,-53.08000002,-61.14995));
#142092=CARTESIAN_POINT('Ctrl Pts',(-43.7578534463097,-53.08000002,-61.14995));
#142093=CARTESIAN_POINT('',(-41.0647116264214,-53.08000002,-64.687079328241));
#142094=CARTESIAN_POINT('Ctrl Pts',(-41.0647116264215,-53.08000002,-64.6870793282409));
#142095=CARTESIAN_POINT('Ctrl Pts',(-41.7638515954828,-53.08000002,-63.6079981134234));
#142096=CARTESIAN_POINT('Ctrl Pts',(-42.4569204735311,-53.08000002,-62.5250292766735));
#142097=CARTESIAN_POINT('Ctrl Pts',(-43.1446480925044,-53.08000002,-61.4386408691297));
#142098=CARTESIAN_POINT('',(-39.5,-53.08000002,-70.7293062304687));
#142099=CARTESIAN_POINT('Ctrl Pts',(-39.5,-53.08000002,-70.7293062304687));
#142100=CARTESIAN_POINT('Ctrl Pts',(-39.5,-53.08000002,-70.1996325547074));
#142101=CARTESIAN_POINT('Ctrl Pts',(-39.5302602116353,-53.08000002,-69.6738635266889));
#142102=CARTESIAN_POINT('Ctrl Pts',(-39.5906692531643,-53.08000002,-69.1519847741694));
#142103=CARTESIAN_POINT('Ctrl Pts',(-39.6510782946932,-53.08000002,-68.6301060216499));
#142104=CARTESIAN_POINT('Ctrl Pts',(-39.7415458248093,-53.08000002,-68.1121058873189));
#142105=CARTESIAN_POINT('Ctrl Pts',(-39.8661752652165,-53.08000002,-67.5985138592656));
#142106=CARTESIAN_POINT('Ctrl Pts',(-39.9284899854243,-53.08000002,-67.3417178452216));
#142107=CARTESIAN_POINT('Ctrl Pts',(-39.9995673120589,-53.08000002,-67.0857801566515));
#142108=CARTESIAN_POINT('Ctrl Pts',(-40.0792084204325,-53.08000002,-66.8343727800802));
#142109=CARTESIAN_POINT('Ctrl Pts',(-40.1588495287955,-53.08000002,-66.5829654035428));
#142110=CARTESIAN_POINT('Ctrl Pts',(-40.2472081235396,-53.08000002,-66.3353006307905));
#142111=CARTESIAN_POINT('Ctrl Pts',(-40.3452847184366,-53.08000002,-66.0918080038346));
#142112=CARTESIAN_POINT('Ctrl Pts',(-40.4725149961156,-53.08000002,-65.7759361633318));
#142113=CARTESIAN_POINT('Ctrl Pts',(-40.6155606032241,-53.08000002,-65.4668542003385));
#142114=CARTESIAN_POINT('Ctrl Pts',(-40.7793840759704,-53.08000002,-65.1666925984838));
#142115=CARTESIAN_POINT('Ctrl Pts',(-40.8681301749544,-53.08000002,-65.0040897017021));
#142116=CARTESIAN_POINT('Ctrl Pts',(-40.9629743342391,-53.08000002,-64.8441048248421));
#142117=CARTESIAN_POINT('Ctrl Pts',(-41.0647116264214,-53.08000002,-64.687079328241));
#142118=CARTESIAN_POINT('',(-39.5,-53.08000002,-161.329336741015));
#142119=CARTESIAN_POINT('',(-39.5,-53.08000002,-55.2499500000008));
#142120=CARTESIAN_POINT('',(-41.0647116264263,-53.08000002,-167.371563643272));
#142121=CARTESIAN_POINT('Ctrl Pts',(-41.0647116264263,-53.08000002,-167.371563643272));
#142122=CARTESIAN_POINT('Ctrl Pts',(-40.8730279274754,-53.08000002,-167.075711184725));
#142123=CARTESIAN_POINT('Ctrl Pts',(-40.7056641754826,-53.08000002,-166.769103901981));
#142124=CARTESIAN_POINT('Ctrl Pts',(-40.5574162968198,-53.08000002,-166.454043185635));
#142125=CARTESIAN_POINT('Ctrl Pts',(-40.4818120706005,-53.08000002,-166.293366878586));
#142126=CARTESIAN_POINT('Ctrl Pts',(-40.4111805199785,-53.08000002,-166.130491546332));
#142127=CARTESIAN_POINT('Ctrl Pts',(-40.3448358791345,-53.08000002,-165.965720445509));
#142128=CARTESIAN_POINT('Ctrl Pts',(-40.1483999357586,-53.08000002,-165.477859388165));
#142129=CARTESIAN_POINT('Ctrl Pts',(-39.9897001835278,-53.08000002,-164.969734884954));
#142130=CARTESIAN_POINT('Ctrl Pts',(-39.8654535116526,-53.08000002,-164.457153153597));
#142131=CARTESIAN_POINT('Ctrl Pts',(-39.7412068397774,-53.08000002,-163.94457142224));
#142132=CARTESIAN_POINT('Ctrl Pts',(-39.6509082568844,-53.08000002,-163.427315362986));
#142133=CARTESIAN_POINT('Ctrl Pts',(-39.5905852088212,-53.08000002,-162.905931958774));
#142134=CARTESIAN_POINT('Ctrl Pts',(-39.530262160758,-53.08000002,-162.384548554563));
#142135=CARTESIAN_POINT('Ctrl Pts',(-39.4999999999991,-53.08000002,-161.85902605313));
#142136=CARTESIAN_POINT('Ctrl Pts',(-39.5,-53.08000002,-161.329336741015));
#142137=CARTESIAN_POINT('',(-43.2972503047852,-53.08000002,-170.861259130871));
#142138=CARTESIAN_POINT('Ctrl Pts',(-43.2972503047852,-53.08000002,-170.861259130871));
#142139=CARTESIAN_POINT('Ctrl Pts',(-42.5594745131554,-53.08000002,-169.693930655453));
#142140=CARTESIAN_POINT('Ctrl Pts',(-41.8155944388483,-53.08000002,-168.530506878352));
#142141=CARTESIAN_POINT('Ctrl Pts',(-41.0647116264263,-53.08000002,-167.371563643272));
#142142=CARTESIAN_POINT('',(-43.9094855672884,-53.08000002,-171.14995));
#142143=CARTESIAN_POINT('Ctrl Pts',(-43.9094855672884,-53.08000002,-171.14995));
#142144=CARTESIAN_POINT('Ctrl Pts',(-43.8503415173364,-53.08000002,-171.14995));
#142145=CARTESIAN_POINT('Ctrl Pts',(-43.7921001974326,-53.08000002,-171.144262868806));
#142146=CARTESIAN_POINT('Ctrl Pts',(-43.7347793831646,-53.08000002,-171.132860793684));
#142147=CARTESIAN_POINT('Ctrl Pts',(-43.6774556974662,-53.08000002,-171.121458147386));
#142148=CARTESIAN_POINT('Ctrl Pts',(-43.6204048981063,-53.08000002,-171.104031177905));
#142149=CARTESIAN_POINT('Ctrl Pts',(-43.5666850153843,-53.08000002,-171.080579637536));
#142150=CARTESIAN_POINT('Ctrl Pts',(-43.5129605101707,-53.08000002,-171.057126079209));
#142151=CARTESIAN_POINT('Ctrl Pts',(-43.4620141840633,-53.08000002,-171.02762282191));
#142152=CARTESIAN_POINT('Ctrl Pts',(-43.4156376346715,-53.08000002,-170.990867761886));
#142153=CARTESIAN_POINT('Ctrl Pts',(-43.3692713886891,-53.08000002,-170.95412086768));
#142154=CARTESIAN_POINT('Ctrl Pts',(-43.3290601923967,-53.08000002,-170.911589580894));
#142155=CARTESIAN_POINT('Ctrl Pts',(-43.2972503047852,-53.08000002,-170.861259130871));
#142156=CARTESIAN_POINT('',(-49.6300753314849,-53.08000002,-171.14995));
#142157=CARTESIAN_POINT('',(-43.4531980731446,-53.08000002,-171.14995));
#142158=CARTESIAN_POINT('',(-51.1448166902628,-53.08000002,-172.64995));
#142159=CARTESIAN_POINT('Ctrl Pts',(-51.1448166902628,-53.08000002,-172.64995));
#142160=CARTESIAN_POINT('Ctrl Pts',(-51.1448166902479,-53.08000002,-172.453565067926));
#142161=CARTESIAN_POINT('Ctrl Pts',(-51.1053920215496,-53.08000002,-172.257328160063));
#142162=CARTESIAN_POINT('Ctrl Pts',(-50.9536357182667,-53.08000002,-171.894521542842));
#142163=CARTESIAN_POINT('Ctrl Pts',(-50.8413637606251,-53.08000002,-171.728129909852));
#142164=CARTESIAN_POINT('Ctrl Pts',(-50.5609546754159,-53.08000002,-171.450449746589));
#142165=CARTESIAN_POINT('Ctrl Pts',(-50.3929278167739,-53.08000002,-171.339270411997));
#142166=CARTESIAN_POINT('Ctrl Pts',(-50.0265556908409,-53.08000002,-171.18899099047));
#142167=CARTESIAN_POINT('Ctrl Pts',(-49.8283902508599,-53.08000002,-171.149950000016));
#142168=CARTESIAN_POINT('Ctrl Pts',(-49.6300753314849,-53.08000002,-171.14995));
#142169=CARTESIAN_POINT('',(-51.1448166902628,-53.08000002,-55.2499500000008));
#142170=CARTESIAN_POINT('Ctrl Pts',(-50.6622663180714,-52.58000002,-60.64995));
#142171=CARTESIAN_POINT('Ctrl Pts',(-50.6622663180714,-53.0800000199999,
-60.64995));
#142172=CARTESIAN_POINT('Ctrl Pts',(-50.6622663180714,-53.08000002,-61.14995));
#142173=CARTESIAN_POINT('Ctrl Pts',(-50.7941888660007,-52.5742946617934,
-60.64995));
#142174=CARTESIAN_POINT('Ctrl Pts',(-50.7949847395758,-53.08000002,-60.6442102195366));
#142175=CARTESIAN_POINT('Ctrl Pts',(-50.8594014087184,-53.08000002,-61.149949999985));
#142176=CARTESIAN_POINT('Ctrl Pts',(-50.9260119778537,-52.5685936039755,
-60.6239226729819));
#142177=CARTESIAN_POINT('Ctrl Pts',(-50.9243014854221,-53.08000002,-60.61203530794));
#142178=CARTESIAN_POINT('Ctrl Pts',(-51.0563879096046,-53.08000002,-61.1109090094727));
#142179=CARTESIAN_POINT('Ctrl Pts',(-51.1697291146411,-52.5580533772395,
-60.5237363920407));
#142180=CARTESIAN_POINT('Ctrl Pts',(-51.1595684581335,-53.08000002,-60.5031527166044));
#142181=CARTESIAN_POINT('Ctrl Pts',(-51.4205803892599,-53.08000002,-60.9606295880612));
#142182=CARTESIAN_POINT('Ctrl Pts',(-51.2815035157812,-52.5532193817859,
-60.4496168355682));
#142183=CARTESIAN_POINT('Ctrl Pts',(-51.2649990424134,-53.0800000200007,
-60.4261994932773));
#142184=CARTESIAN_POINT('Ctrl Pts',(-51.5876076112677,-53.08000002,-60.8494502533514));
#142185=CARTESIAN_POINT('Ctrl Pts',(-51.4680365366082,-52.5451522414979,
-60.2644967268049));
#142186=CARTESIAN_POINT('Ctrl Pts',(-51.4390258902891,-53.0800000199993,
-60.2406767152623));
#142187=CARTESIAN_POINT('Ctrl Pts',(-51.8663484675245,-53.08000002,-60.5717700902082));
#142188=CARTESIAN_POINT('Ctrl Pts',(-51.5427218037424,-52.5419222689988,
-60.153568971423));
#142189=CARTESIAN_POINT('Ctrl Pts',(-51.507092542289,-53.08000002,-60.1322291512615));
#142190=CARTESIAN_POINT('Ctrl Pts',(-51.9779524892604,-53.08000002,-60.4053784571342));
#142191=CARTESIAN_POINT('Ctrl Pts',(-51.6436727471424,-52.5375563641358,
-59.9116978933072));
#142192=CARTESIAN_POINT('Ctrl Pts',(-51.598921085515,-53.08000002,-59.8989712332631));
#142193=CARTESIAN_POINT('Ctrl Pts',(-52.1288059535877,-53.08000002,-60.0425718399611));
#142194=CARTESIAN_POINT('Ctrl Pts',(-51.6698987253403,-52.5364221486294,
-59.7808732880376));
#142195=CARTESIAN_POINT('Ctrl Pts',(-51.6223418238443,-53.0800000200021,
-59.7746029379323));
#142196=CARTESIAN_POINT('Ctrl Pts',(-52.1679960743694,-53.08000002,-59.8463349320561));
#142197=CARTESIAN_POINT('Ctrl Pts',(-51.6698987253405,-52.5364221486262,
-59.64995));
#142198=CARTESIAN_POINT('Ctrl Pts',(-51.6223418238518,-53.08000002,-59.64995));
#142199=CARTESIAN_POINT('Ctrl Pts',(-52.1679960743864,-53.08000002,-59.64995));
#142200=CARTESIAN_POINT('Origin',(-50.6622663180714,-52.58000002,-61.14995));
#142201=CARTESIAN_POINT('Origin',(0.,-12.9675000200281,-60.64995));
#142202=CARTESIAN_POINT('',(-43.7578534463097,-52.58000002,-60.64995));
#142203=CARTESIAN_POINT('',(-48.2747189347426,-46.93000002,-60.64995));
#142204=CARTESIAN_POINT('Origin',(0.,-12.9675000200281,-60.64995));
#142205=CARTESIAN_POINT('',(1.65582490824295E-14,-52.58000002,-60.64995));
#142206=CARTESIAN_POINT('',(1.41965171211599E-14,-46.93000002,-60.64995));
#142207=CARTESIAN_POINT('Ctrl Pts',(-52.1642096742619,-46.8864221486262,
-59.64995));
#142208=CARTESIAN_POINT('Ctrl Pts',(-52.2041414362991,-46.43000002,-59.64995));
#142209=CARTESIAN_POINT('Ctrl Pts',(-52.6623070233078,-46.43000002,-59.64995));
#142210=CARTESIAN_POINT('Ctrl Pts',(-52.1642096742618,-46.8864221486274,
-59.7808732880376));
#142211=CARTESIAN_POINT('Ctrl Pts',(-52.2041414362827,-46.4300000200027,
-59.7861314645));
#142212=CARTESIAN_POINT('Ctrl Pts',(-52.6623070232907,-46.43000002,-59.8463349320562));
#142213=CARTESIAN_POINT('Ctrl Pts',(-52.1379836960638,-46.8875563641358,
-59.9116978933072));
#142214=CARTESIAN_POINT('Ctrl Pts',(-52.175748088412,-46.43000002,-59.9224177216061));
#142215=CARTESIAN_POINT('Ctrl Pts',(-52.6231169025091,-46.43000002,-60.0425718399611));
#142216=CARTESIAN_POINT('Ctrl Pts',(-52.0370327526638,-46.8919222689988,
-60.153568971423));
#142217=CARTESIAN_POINT('Ctrl Pts',(-52.0676362723124,-46.43000002,-60.1718710142644));
#142218=CARTESIAN_POINT('Ctrl Pts',(-52.4722634381817,-46.43000002,-60.4053784571342));
#142219=CARTESIAN_POINT('Ctrl Pts',(-51.9623474855296,-46.8951522414972,
-60.264496726805));
#142220=CARTESIAN_POINT('Ctrl Pts',(-51.9876181407653,-46.43000002,-60.2852157712123));
#142221=CARTESIAN_POINT('Ctrl Pts',(-52.3606594164458,-46.43000002,-60.5717700902076));
#142222=CARTESIAN_POINT('Ctrl Pts',(-51.7758144647026,-46.9032193817865,
-60.4496168355682));
#142223=CARTESIAN_POINT('Ctrl Pts',(-51.7906875266988,-46.43000002,-60.4706504746462));
#142224=CARTESIAN_POINT('Ctrl Pts',(-52.0819185601891,-46.43000002,-60.8494502533521));
#142225=CARTESIAN_POINT('Ctrl Pts',(-51.6640400635624,-46.9080533772402,
-60.5237363920407));
#142226=CARTESIAN_POINT('Ctrl Pts',(-51.6733804433437,-46.4300000200007,
-60.5426326522478));
#142227=CARTESIAN_POINT('Ctrl Pts',(-51.9148913381812,-46.43000002,-60.9606295880612));
#142228=CARTESIAN_POINT('Ctrl Pts',(-51.4203229267752,-46.9185936039748,
-60.6239226729819));
#142229=CARTESIAN_POINT('Ctrl Pts',(-51.4220052245013,-46.4300000199993,
-60.6353187454025));
#142230=CARTESIAN_POINT('Ctrl Pts',(-51.550698858526,-46.43000002,-61.1109090094727));
#142231=CARTESIAN_POINT('Ctrl Pts',(-51.288499814922,-46.9242946617933,
-60.64995));
#142232=CARTESIAN_POINT('Ctrl Pts',(-51.2877237368248,-46.4300000199999,
-60.6556217969811));
#142233=CARTESIAN_POINT('Ctrl Pts',(-51.3537123576397,-46.43000002,-61.149949999985));
#142234=CARTESIAN_POINT('Ctrl Pts',(-51.1565772669927,-46.93000002,-60.64995));
#142235=CARTESIAN_POINT('Ctrl Pts',(-51.1565772669928,-46.43000002,-60.64995));
#142236=CARTESIAN_POINT('Ctrl Pts',(-51.1565772669927,-46.43000002,-61.14995));
#142237=CARTESIAN_POINT('',(-51.1565772669927,-46.43000002,-61.14995));
#142238=CARTESIAN_POINT('Origin',(-51.1565772669927,-46.93000002,-61.14995));
#142239=CARTESIAN_POINT('Ctrl Pts',(-52.6623070233077,-46.43000002,-59.64995));
#142240=CARTESIAN_POINT('Ctrl Pts',(-52.6623070232906,-46.43000002,-59.8463349320562));
#142241=CARTESIAN_POINT('Ctrl Pts',(-52.623116902509,-46.43000002,-60.0425718399611));
#142242=CARTESIAN_POINT('Ctrl Pts',(-52.5476901703453,-46.43000002,-60.2239751485476));
#142243=CARTESIAN_POINT('Ctrl Pts',(-52.4722634381816,-46.43000002,-60.4053784571342));
#142244=CARTESIAN_POINT('Ctrl Pts',(-52.3606594164458,-46.43000002,-60.5717700902076));
#142245=CARTESIAN_POINT('Ctrl Pts',(-52.2212889883174,-46.43000002,-60.7106101717798));
#142246=CARTESIAN_POINT('Ctrl Pts',(-52.0819185601891,-46.43000002,-60.8494502533521));
#142247=CARTESIAN_POINT('Ctrl Pts',(-51.9148913381812,-46.43000002,-60.9606295880612));
#142248=CARTESIAN_POINT('Ctrl Pts',(-51.7327950983536,-46.43000002,-61.0357692987669));
#142249=CARTESIAN_POINT('Ctrl Pts',(-51.550698858526,-46.43000002,-61.1109090094727));
#142250=CARTESIAN_POINT('Ctrl Pts',(-51.3537123576397,-46.43000002,-61.149949999985));
#142251=CARTESIAN_POINT('Ctrl Pts',(-51.1565772669927,-46.43000002,-61.14995));
#142252=CARTESIAN_POINT('Origin',(83.2809572255632,-46.4300000199999,-55.2499500000008));
#142253=CARTESIAN_POINT('',(-57.,-46.43000002,-55.74995));
#142254=CARTESIAN_POINT('',(83.2809572255632,-46.4300000199999,-55.74995));
#142255=CARTESIAN_POINT('',(-59.5,-46.43000002,-58.24995));
#142256=CARTESIAN_POINT('Origin',(-57.,-46.43000002,-58.24995));
#142257=CARTESIAN_POINT('',(-59.5,-46.43000002,-174.34995));
#142258=CARTESIAN_POINT('',(-59.5,-46.43000002,-58.24995));
#142259=CARTESIAN_POINT('',(-57.,-46.43000002,-176.84995));
#142260=CARTESIAN_POINT('Origin',(-57.,-46.43000002,-174.34995));
#142261=CARTESIAN_POINT('',(-51.9388724063314,-46.43000002,-176.84995));
#142262=CARTESIAN_POINT('',(83.2809572255632,-46.4300000199999,-176.84995));
#142263=CARTESIAN_POINT('',(-51.9388724063314,-46.43000002,-172.64995));
#142264=CARTESIAN_POINT('',(-51.9388724063314,-46.43000002,-55.2499500000008));
#142265=CARTESIAN_POINT('',(-50.4241310475534,-46.43000002,-171.14995));
#142266=CARTESIAN_POINT('Ctrl Pts',(-50.4241310475534,-46.43000002,-171.14995));
#142267=CARTESIAN_POINT('Ctrl Pts',(-50.6224459669284,-46.43000002,-171.149950000016));
#142268=CARTESIAN_POINT('Ctrl Pts',(-50.8206114069094,-46.43000002,-171.18899099047));
#142269=CARTESIAN_POINT('Ctrl Pts',(-51.1869835328424,-46.43000002,-171.339270411997));
#142270=CARTESIAN_POINT('Ctrl Pts',(-51.3550103914843,-46.43000002,-171.450449746589));
#142271=CARTESIAN_POINT('Ctrl Pts',(-51.6354194766937,-46.43000002,-171.728129909852));
#142272=CARTESIAN_POINT('Ctrl Pts',(-51.7476914343352,-46.43000002,-171.894521542842));
#142273=CARTESIAN_POINT('Ctrl Pts',(-51.8994477376182,-46.43000002,-172.257328160063));
#142274=CARTESIAN_POINT('Ctrl Pts',(-51.9388724063164,-46.43000002,-172.453565067926));
#142275=CARTESIAN_POINT('Ctrl Pts',(-51.9388724063314,-46.43000002,-172.64995));
#142276=CARTESIAN_POINT('',(-48.4122058243951,-46.43000002,-171.14995));
#142277=CARTESIAN_POINT('',(-50.4944014649046,-46.43000002,-171.14995));
#142278=CARTESIAN_POINT('',(-47.8576079004676,-46.43000002,-170.861259130871));
#142279=CARTESIAN_POINT('Ctrl Pts',(-47.8576079004676,-46.43000002,-170.861259130871));
#142280=CARTESIAN_POINT('Ctrl Pts',(-47.8760580377295,-46.43000002,-170.89352615778));
#142281=CARTESIAN_POINT('Ctrl Pts',(-47.8980723549741,-46.43000002,-170.923203523829));
#142282=CARTESIAN_POINT('Ctrl Pts',(-47.9228861329636,-46.43000002,-170.950192158739));
#142283=CARTESIAN_POINT('Ctrl Pts',(-47.9503841163788,-46.43000002,-170.98010026203));
#142284=CARTESIAN_POINT('Ctrl Pts',(-47.981319017648,-46.43000002,-171.00670574507));
#142285=CARTESIAN_POINT('Ctrl Pts',(-48.0145941519157,-46.43000002,-171.02991277546));
#142286=CARTESIAN_POINT('Ctrl Pts',(-48.0405863852474,-46.43000002,-171.048040502428));
#142287=CARTESIAN_POINT('Ctrl Pts',(-48.0680050205668,-46.43000002,-171.06409541242));
#142288=CARTESIAN_POINT('Ctrl Pts',(-48.0963149978629,-46.43000002,-171.078049783599));
#142289=CARTESIAN_POINT('Ctrl Pts',(-48.1225339813698,-46.43000002,-171.090973475624));
#142290=CARTESIAN_POINT('Ctrl Pts',(-48.1495923840829,-46.43000002,-171.102104191555));
#142291=CARTESIAN_POINT('Ctrl Pts',(-48.177275111639,-46.43000002,-171.111506345608));
#142292=CARTESIAN_POINT('Ctrl Pts',(-48.2055749629089,-46.43000002,-171.121118099391));
#142293=CARTESIAN_POINT('Ctrl Pts',(-48.234528655658,-46.43000002,-171.128923533851));
#142294=CARTESIAN_POINT('Ctrl Pts',(-48.2639285033285,-46.43000002,-171.134940493274));
#142295=CARTESIAN_POINT('Ctrl Pts',(-48.2928212065521,-46.43000002,-171.140853660745));
#142296=CARTESIAN_POINT('Ctrl Pts',(-48.3221462163591,-46.43000002,-171.145039422868));
#142297=CARTESIAN_POINT('Ctrl Pts',(-48.3517066016403,-46.43000002,-171.147466016794));
#142298=CARTESIAN_POINT('Ctrl Pts',(-48.3717866301037,-46.43000002,-171.149114374034));
#142299=CARTESIAN_POINT('Ctrl Pts',(-48.3919752683816,-46.43000002,-171.14995));
#142300=CARTESIAN_POINT('Ctrl Pts',(-48.4122058243951,-46.43000002,-171.14995));
#142301=CARTESIAN_POINT('',(-40.8634877666247,-46.43000002,-158.96051646616));
#142302=CARTESIAN_POINT('Ctrl Pts',(-40.8634877666247,-46.43000002,-158.96051646616));
#142303=CARTESIAN_POINT('Ctrl Pts',(-43.2493545263947,-46.43000002,-162.895404681481));
#142304=CARTESIAN_POINT('Ctrl Pts',(-45.5734709768386,-46.43000002,-166.866583832071));
#142305=CARTESIAN_POINT('Ctrl Pts',(-47.8576079004676,-46.43000002,-170.861259130871));
#142306=CARTESIAN_POINT('',(-39.5,-46.43000002,-153.563058845195));
#142307=CARTESIAN_POINT('Ctrl Pts',(-39.5,-46.43000002,-153.563058845195));
#142308=CARTESIAN_POINT('Ctrl Pts',(-39.4999999999995,-46.43000002,-153.949465551028));
#142309=CARTESIAN_POINT('Ctrl Pts',(-39.5176594219082,-46.43000002,-154.333958533364));
#142310=CARTESIAN_POINT('Ctrl Pts',(-39.5536573145523,-46.43000002,-154.716308049412));
#142311=CARTESIAN_POINT('Ctrl Pts',(-39.5886363261013,-46.43000002,-155.087835579366));
#142312=CARTESIAN_POINT('Ctrl Pts',(-39.6409303087516,-46.43000002,-155.457339415589));
#142313=CARTESIAN_POINT('Ctrl Pts',(-39.711211141592,-46.43000002,-155.824604113663));
#142314=CARTESIAN_POINT('Ctrl Pts',(-39.7452479661607,-46.43000002,-156.002469451813));
#142315=CARTESIAN_POINT('Ctrl Pts',(-39.7835042486637,-46.43000002,-156.179809528778));
#142316=CARTESIAN_POINT('Ctrl Pts',(-39.8260607087683,-46.43000002,-156.356599303471));
#142317=CARTESIAN_POINT('Ctrl Pts',(-39.9364913068056,-46.43000002,-156.815354578187));
#142318=CARTESIAN_POINT('Ctrl Pts',(-40.0748112905465,-46.43000002,-157.263052526106));
#142319=CARTESIAN_POINT('Ctrl Pts',(-40.2452594329879,-46.43000002,-157.698012597756));
#142320=CARTESIAN_POINT('Ctrl Pts',(-40.3764895639192,-46.43000002,-158.032893731307));
#142321=CARTESIAN_POINT('Ctrl Pts',(-40.5265005956173,-46.43000002,-158.360328778722));
#142322=CARTESIAN_POINT('Ctrl Pts',(-40.7006921181746,-46.43000002,-158.678176979839));
#142323=CARTESIAN_POINT('Ctrl Pts',(-40.7527491045398,-46.43000002,-158.773165640762));
#142324=CARTESIAN_POINT('Ctrl Pts',(-40.8069659798529,-46.43000002,-158.867297969463));
#142325=CARTESIAN_POINT('Ctrl Pts',(-40.8634877666247,-46.43000002,-158.960516466159));
#142326=CARTESIAN_POINT('',(-39.5,-46.43000002,-78.4955841262963));
#142327=CARTESIAN_POINT('',(-39.5,-46.43000002,-55.2499500000008));
#142328=CARTESIAN_POINT('',(-40.8634877666247,-46.43000002,-73.0981265053466));
#142329=CARTESIAN_POINT('Ctrl Pts',(-40.8634877666247,-46.43000002,-73.0981265053466));
#142330=CARTESIAN_POINT('Ctrl Pts',(-40.661044199348,-46.43000002,-73.4320063432862));
#142331=CARTESIAN_POINT('Ctrl Pts',(-40.4876415800298,-46.43000002,-73.7785418551243));
#142332=CARTESIAN_POINT('Ctrl Pts',(-40.3370596438449,-46.43000002,-74.1350223226556));
#142333=CARTESIAN_POINT('Ctrl Pts',(-40.305064047112,-46.43000002,-74.210767166767));
#142334=CARTESIAN_POINT('Ctrl Pts',(-40.2740989238678,-46.43000002,-74.2869610781288));
#142335=CARTESIAN_POINT('Ctrl Pts',(-40.2441048562922,-46.43000002,-74.3635781632946));
#142336=CARTESIAN_POINT('Ctrl Pts',(-40.0729487154701,-46.43000002,-74.8007807729435));
#142337=CARTESIAN_POINT('Ctrl Pts',(-39.9334371777348,-46.43000002,-75.2543998579721));
#142338=CARTESIAN_POINT('Ctrl Pts',(-39.8240030986842,-46.43000002,-75.7106064091747));
#142339=CARTESIAN_POINT('Ctrl Pts',(-39.7066850117819,-46.43000002,-76.1996796511091));
#142340=CARTESIAN_POINT('Ctrl Pts',(-39.6220553949032,-46.43000002,-76.6934446581353));
#142341=CARTESIAN_POINT('Ctrl Pts',(-39.5687675179992,-46.43000002,-77.1917081792648));
#142342=CARTESIAN_POINT('Ctrl Pts',(-39.5226417428819,-46.43000002,-77.6230031089943));
#142343=CARTESIAN_POINT('Ctrl Pts',(-39.5,-46.43000002,-78.0576687430938));
#142344=CARTESIAN_POINT('Ctrl Pts',(-39.5,-46.43000002,-78.4955841262963));
#142345=CARTESIAN_POINT('',(-47.7195914591242,-46.43000002,-61.4386408691297));
#142346=CARTESIAN_POINT('Ctrl Pts',(-47.7195914591242,-46.43000002,-61.4386408691297));
#142347=CARTESIAN_POINT('Ctrl Pts',(-45.4798130845491,-46.43000002,-65.351943995909));
#142348=CARTESIAN_POINT('Ctrl Pts',(-43.2013098945494,-46.43000002,-69.2424758480089));
#142349=CARTESIAN_POINT('Ctrl Pts',(-40.8634877666247,-46.43000002,-73.0981265053466));
#142350=CARTESIAN_POINT('',(-48.2747189347426,-46.43000002,-61.14995));
#142351=CARTESIAN_POINT('Ctrl Pts',(-48.2747189347426,-46.43000002,-61.14995));
#142352=CARTESIAN_POINT('Ctrl Pts',(-48.2086234136051,-46.43000002,-61.14995));
#142353=CARTESIAN_POINT('Ctrl Pts',(-48.1427915915172,-46.43000002,-61.1585974051143));
#142354=CARTESIAN_POINT('Ctrl Pts',(-48.0794858636046,-46.43000002,-61.1760262255644));
#142355=CARTESIAN_POINT('Ctrl Pts',(-48.0376978539717,-46.43000002,-61.1875309620373));
#142356=CARTESIAN_POINT('Ctrl Pts',(-47.9970101587091,-46.43000002,-61.2028630486499));
#142357=CARTESIAN_POINT('Ctrl Pts',(-47.9580757097656,-46.43000002,-61.2220733995985));
#142358=CARTESIAN_POINT('Ctrl Pts',(-47.9230818282115,-46.43000002,-61.2393394650997));
#142359=CARTESIAN_POINT('Ctrl Pts',(-47.8896549296879,-46.43000002,-61.2597370764849));
#142360=CARTESIAN_POINT('Ctrl Pts',(-47.8586276391547,-46.43000002,-61.2831656716456));
#142361=CARTESIAN_POINT('Ctrl Pts',(-47.8304660966181,-46.43000002,-61.3044303508313));
#142362=CARTESIAN_POINT('Ctrl Pts',(-47.8042802405272,-46.43000002,-61.3281927143748));
#142363=CARTESIAN_POINT('Ctrl Pts',(-47.7807177502455,-46.43000002,-61.3544087872413));
#142364=CARTESIAN_POINT('Ctrl Pts',(-47.7576005025357,-46.43000002,-61.3801294747912));
#142365=CARTESIAN_POINT('Ctrl Pts',(-47.7370072711932,-46.43000002,-61.4082122550317));
#142366=CARTESIAN_POINT('Ctrl Pts',(-47.7195914591242,-46.43000002,-61.4386408691297));
#142367=CARTESIAN_POINT('',(83.2809572255632,-46.4300000199999,-61.14995));
#142368=CARTESIAN_POINT('Origin',(-60.,-45.93000002,-55.74995));
#142369=CARTESIAN_POINT('',(-57.,-45.93000002,-55.24995));
#142370=CARTESIAN_POINT('',(-60.,-45.93000002,-55.24995));
#142371=CARTESIAN_POINT('Origin',(-57.,-45.93000002,-55.74995));
#142372=CARTESIAN_POINT('Origin',(-60.,28.41999998,-55.24995));
#142373=CARTESIAN_POINT('',(-57.,-45.43000002,-55.24995));
#142374=CARTESIAN_POINT('',(-60.,-45.43000002,-55.24995));
#142375=CARTESIAN_POINT('',(-57.,28.41999998,-55.24995));
#142376=CARTESIAN_POINT('Origin',(83.2809572255632,-45.4300000199999,-55.74995));
#142377=CARTESIAN_POINT('',(-57.,-44.93000002,-55.74995));
#142378=CARTESIAN_POINT('',(83.2809572255632,-44.93000002,-55.74995));
#142379=CARTESIAN_POINT('Origin',(-57.,-45.43000002,-55.74995));
#142380=CARTESIAN_POINT('Ctrl Pts',(-51.3752989258075,-44.43000002,-60.64995));
#142381=CARTESIAN_POINT('Ctrl Pts',(-51.3752989258075,-44.93000002,-60.64995));
#142382=CARTESIAN_POINT('Ctrl Pts',(-51.3752989258075,-44.93000002,-61.14995));
#142383=CARTESIAN_POINT('Ctrl Pts',(-51.5072214737368,-44.4242946617934,
-60.64995));
#142384=CARTESIAN_POINT('Ctrl Pts',(-51.5080173473124,-44.9300000200007,
-60.6442102195364));
#142385=CARTESIAN_POINT('Ctrl Pts',(-51.5724340164545,-44.93000002,-61.149949999985));
#142386=CARTESIAN_POINT('Ctrl Pts',(-51.6390445855899,-44.4185936039755,
-60.6239226729819));
#142387=CARTESIAN_POINT('Ctrl Pts',(-51.6373340931575,-44.9300000200007,
-60.61203530794));
#142388=CARTESIAN_POINT('Ctrl Pts',(-51.7694205173407,-44.93000002,-61.1109090094727));
#142389=CARTESIAN_POINT('Ctrl Pts',(-51.8827617223772,-44.4080533772395,
-60.5237363920407));
#142390=CARTESIAN_POINT('Ctrl Pts',(-51.8726010658704,-44.9300000199993,
-60.5031527166044));
#142391=CARTESIAN_POINT('Ctrl Pts',(-52.1336129969961,-44.93000002,-60.9606295880612));
#142392=CARTESIAN_POINT('Ctrl Pts',(-51.9945361235173,-44.4032193817859,
-60.4496168355682));
#142393=CARTESIAN_POINT('Ctrl Pts',(-51.9780316501496,-44.93000002,-60.4261994932779));
#142394=CARTESIAN_POINT('Ctrl Pts',(-52.3006402190038,-44.93000002,-60.8494502533521));
#142395=CARTESIAN_POINT('Ctrl Pts',(-52.1810691443443,-44.3951522414979,
-60.2644967268049));
#142396=CARTESIAN_POINT('Ctrl Pts',(-52.1520584980253,-44.93000002,-60.2406767152616));
#142397=CARTESIAN_POINT('Ctrl Pts',(-52.5793810752606,-44.93000002,-60.5717700902076));
#142398=CARTESIAN_POINT('Ctrl Pts',(-52.2557544114786,-44.3919222689988,
-60.153568971423));
#142399=CARTESIAN_POINT('Ctrl Pts',(-52.2201251500251,-44.93000002,-60.1322291512615));
#142400=CARTESIAN_POINT('Ctrl Pts',(-52.6909850969965,-44.93000002,-60.4053784571342));
#142401=CARTESIAN_POINT('Ctrl Pts',(-52.3567053548786,-44.3875563641358,
-59.9116978933072));
#142402=CARTESIAN_POINT('Ctrl Pts',(-52.3119536932511,-44.93000002,-59.8989712332631));
#142403=CARTESIAN_POINT('Ctrl Pts',(-52.8418385613238,-44.93000002,-60.0425718399611));
#142404=CARTESIAN_POINT('Ctrl Pts',(-52.3829313330764,-44.3864221486294,
-59.7808732880376));
#142405=CARTESIAN_POINT('Ctrl Pts',(-52.3353744315805,-44.9300000200007,
-59.7746029379323));
#142406=CARTESIAN_POINT('Ctrl Pts',(-52.8810286821055,-44.93000002,-59.8463349320562));
#142407=CARTESIAN_POINT('Ctrl Pts',(-52.3829313330767,-44.3864221486262,
-59.64995));
#142408=CARTESIAN_POINT('Ctrl Pts',(-52.3353744315879,-44.93000002,-59.64995));
#142409=CARTESIAN_POINT('Ctrl Pts',(-52.8810286821225,-44.93000002,-59.64995));
#142410=CARTESIAN_POINT('',(-51.3752989258075,-44.93000002,-61.14995));
#142411=CARTESIAN_POINT('Origin',(-51.3752989258075,-44.43000002,-61.14995));
#142412=CARTESIAN_POINT('Ctrl Pts',(-51.3752989258075,-44.93000002,-61.14995));
#142413=CARTESIAN_POINT('Ctrl Pts',(-51.5724340164545,-44.93000002,-61.149949999985));
#142414=CARTESIAN_POINT('Ctrl Pts',(-51.7694205173407,-44.93000002,-61.1109090094727));
#142415=CARTESIAN_POINT('Ctrl Pts',(-52.1336129969961,-44.93000002,-60.9606295880612));
#142416=CARTESIAN_POINT('Ctrl Pts',(-52.3006402190038,-44.93000002,-60.8494502533521));
#142417=CARTESIAN_POINT('Ctrl Pts',(-52.5793810752606,-44.93000002,-60.5717700902076));
#142418=CARTESIAN_POINT('Ctrl Pts',(-52.6909850969965,-44.93000002,-60.4053784571342));
#142419=CARTESIAN_POINT('Ctrl Pts',(-52.8418385613238,-44.93000002,-60.0425718399611));
#142420=CARTESIAN_POINT('Ctrl Pts',(-52.8810286821055,-44.93000002,-59.8463349320562));
#142421=CARTESIAN_POINT('Ctrl Pts',(-52.8810286821225,-44.93000002,-59.64995));
#142422=CARTESIAN_POINT('Origin',(83.2809572255632,-44.93000002,-55.2499500000007));
#142423=CARTESIAN_POINT('',(-57.,-44.93000002,-176.84995));
#142424=CARTESIAN_POINT('',(-52.2902244930873,-44.93000002,-176.84995));
#142425=CARTESIAN_POINT('',(83.2809572255632,-44.93000002,-176.84995));
#142426=CARTESIAN_POINT('',(-59.5,-44.93000002,-174.34995));
#142427=CARTESIAN_POINT('Origin',(-57.,-44.93000002,-174.34995));
#142428=CARTESIAN_POINT('',(-59.5,-44.93000002,-58.24995));
#142429=CARTESIAN_POINT('',(-59.5,-44.93000002,-174.34995));
#142430=CARTESIAN_POINT('Origin',(-57.,-44.93000002,-58.24995));
#142431=CARTESIAN_POINT('',(-49.940073970993,-44.93000002,-61.14995));
#142432=CARTESIAN_POINT('',(83.2809572255632,-44.93000002,-61.14995));
#142433=CARTESIAN_POINT('',(-49.4036629110189,-44.93000002,-61.4386408691297));
#142434=CARTESIAN_POINT('Ctrl Pts',(-49.4036629110189,-44.93000002,-61.4386408691297));
#142435=CARTESIAN_POINT('Ctrl Pts',(-49.421292954971,-44.93000002,-61.4067508873822));
#142436=CARTESIAN_POINT('Ctrl Pts',(-49.4424088019262,-44.93000002,-61.3772666862022));
#142437=CARTESIAN_POINT('Ctrl Pts',(-49.4663885772136,-44.93000002,-61.3502540659087));
#142438=CARTESIAN_POINT('Ctrl Pts',(-49.4778548596159,-44.93000002,-61.33733758404));
#142439=CARTESIAN_POINT('Ctrl Pts',(-49.4899767151878,-44.93000002,-61.3249865422104));
#142440=CARTESIAN_POINT('Ctrl Pts',(-49.5026897554816,-44.93000002,-61.3132100906898));
#142441=CARTESIAN_POINT('Ctrl Pts',(-49.5320647115447,-44.93000002,-61.2859992317605));
#142442=CARTESIAN_POINT('Ctrl Pts',(-49.5637608854771,-44.93000002,-61.2625146831493));
#142443=CARTESIAN_POINT('Ctrl Pts',(-49.597554081752,-44.93000002,-61.2422777750133));
#142444=CARTESIAN_POINT('Ctrl Pts',(-49.6090633503044,-44.93000002,-61.2353854997602));
#142445=CARTESIAN_POINT('Ctrl Pts',(-49.6208161109919,-44.93000002,-61.2288703265774));
#142446=CARTESIAN_POINT('Ctrl Pts',(-49.6328042123455,-44.93000002,-61.2227144603287));
#142447=CARTESIAN_POINT('Ctrl Pts',(-49.679945666351,-44.93000002,-61.1985074172725));
#142448=CARTESIAN_POINT('Ctrl Pts',(-49.7309938530465,-44.93000002,-61.1800821085049));
#142449=CARTESIAN_POINT('Ctrl Pts',(-49.7824210964939,-44.93000002,-61.1680542343897));
#142450=CARTESIAN_POINT('Ctrl Pts',(-49.833844605741,-44.93000002,-61.1560272336343));
#142451=CARTESIAN_POINT('Ctrl Pts',(-49.8863934436428,-44.93000002,-61.14995));
#142452=CARTESIAN_POINT('Ctrl Pts',(-49.940073970993,-44.93000002,-61.14995));
#142453=CARTESIAN_POINT('',(-40.7712064624936,-44.93000002,-76.6047958451324));
#142454=CARTESIAN_POINT('Ctrl Pts',(-40.7712064624935,-44.93000002,-76.6047958451324));
#142455=CARTESIAN_POINT('Ctrl Pts',(-43.723712605206,-44.93000002,-71.5921120242627));
#142456=CARTESIAN_POINT('Ctrl Pts',(-46.5890589653218,-44.93000002,-66.5298175388285));
#142457=CARTESIAN_POINT('Ctrl Pts',(-49.4036629110189,-44.93000002,-61.4386408691297));
#142458=CARTESIAN_POINT('',(-39.5,-44.93000002,-81.6937887068282));
#142459=CARTESIAN_POINT('Ctrl Pts',(-39.5,-44.93000002,-81.6937887068282));
#142460=CARTESIAN_POINT('Ctrl Pts',(-39.5,-44.93000002,-81.4715915443627));
#142461=CARTESIAN_POINT('Ctrl Pts',(-39.5062851881924,-44.93000002,-81.2500804744028));
#142462=CARTESIAN_POINT('Ctrl Pts',(-39.5189031887286,-44.93000002,-81.0292580402078));
#142463=CARTESIAN_POINT('Ctrl Pts',(-39.5308326200065,-44.93000002,-80.820485973209));
#142464=CARTESIAN_POINT('Ctrl Pts',(-39.5484229321411,-44.93000002,-80.6123290364163));
#142465=CARTESIAN_POINT('Ctrl Pts',(-39.5717668549559,-44.93000002,-80.4047900585203));
#142466=CARTESIAN_POINT('Ctrl Pts',(-39.5731142710435,-44.93000002,-80.392810865484));
#142467=CARTESIAN_POINT('Ctrl Pts',(-39.5744808704139,-44.93000002,-80.3808337323845));
#142468=CARTESIAN_POINT('Ctrl Pts',(-39.5758666762242,-44.93000002,-80.3688586602483));
#142469=CARTESIAN_POINT('Ctrl Pts',(-39.5992261762147,-44.93000002,-80.167003757221));
#142470=CARTESIAN_POINT('Ctrl Pts',(-39.6280811656786,-44.93000002,-79.9654411052776));
#142471=CARTESIAN_POINT('Ctrl Pts',(-39.6625124125991,-44.93000002,-79.7646415180465));
#142472=CARTESIAN_POINT('Ctrl Pts',(-39.6964841131887,-44.93000002,-79.5665219590392));
#142473=CARTESIAN_POINT('Ctrl Pts',(-39.735884231964,-44.93000002,-79.3691455608356));
#142474=CARTESIAN_POINT('Ctrl Pts',(-39.7807398869814,-44.93000002,-79.1729578992683));
#142475=CARTESIAN_POINT('Ctrl Pts',(-39.7892690083245,-44.93000002,-79.1356536090762));
#142476=CARTESIAN_POINT('Ctrl Pts',(-39.7979952284868,-44.93000002,-79.0983922704894));
#142477=CARTESIAN_POINT('Ctrl Pts',(-39.8069185231454,-44.93000002,-79.0611769040833));
#142478=CARTESIAN_POINT('Ctrl Pts',(-39.9103339550991,-44.93000002,-78.6298739672843));
#142479=CARTESIAN_POINT('Ctrl Pts',(-40.0396611959927,-44.93000002,-78.2084773864585));
#142480=CARTESIAN_POINT('Ctrl Pts',(-40.1983721980467,-44.93000002,-77.7983145251762));
#142481=CARTESIAN_POINT('Ctrl Pts',(-40.3310078543919,-44.93000002,-77.455539168644));
#142482=CARTESIAN_POINT('Ctrl Pts',(-40.4839381620924,-44.93000002,-77.1205226744026));
#142483=CARTESIAN_POINT('Ctrl Pts',(-40.6627223002475,-44.93000002,-76.7953903625546));
#142484=CARTESIAN_POINT('Ctrl Pts',(-40.6978701506679,-44.93000002,-76.7314713707381));
#142485=CARTESIAN_POINT('Ctrl Pts',(-40.7340173780027,-44.93000002,-76.6679344511564));
#142486=CARTESIAN_POINT('Ctrl Pts',(-40.7712064624936,-44.93000002,-76.6047958451324));
#142487=CARTESIAN_POINT('',(-39.5,-44.93000002,-150.364854264666));
#142488=CARTESIAN_POINT('',(-39.5,-44.93000002,-55.2499500000007));
#142489=CARTESIAN_POINT('',(-40.7712064624936,-44.93000002,-155.453847126373));
#142490=CARTESIAN_POINT('Ctrl Pts',(-40.7712064624936,-44.93000002,-155.453847126373));
#142491=CARTESIAN_POINT('Ctrl Pts',(-40.5636969173457,-44.93000002,-155.101543121134));
#142492=CARTESIAN_POINT('Ctrl Pts',(-40.3878808277004,-44.93000002,-154.735494168741));
#142493=CARTESIAN_POINT('Ctrl Pts',(-40.2370488760485,-44.93000002,-154.358609995095));
#142494=CARTESIAN_POINT('Ctrl Pts',(-40.2234902738441,-44.93000002,-154.324731081963));
#142495=CARTESIAN_POINT('Ctrl Pts',(-40.2101335892538,-44.93000002,-154.290764600354));
#142496=CARTESIAN_POINT('Ctrl Pts',(-40.1969739657515,-44.93000002,-154.256712656464));
#142497=CARTESIAN_POINT('Ctrl Pts',(-40.0374208080236,-44.93000002,-153.843851667435));
#142498=CARTESIAN_POINT('Ctrl Pts',(-39.9069198944888,-44.93000002,-153.416428338648));
#142499=CARTESIAN_POINT('Ctrl Pts',(-39.8044156663649,-44.93000002,-152.987004278786));
#142500=CARTESIAN_POINT('Ctrl Pts',(-39.6913863431124,-44.93000002,-152.513487119906));
#142501=CARTESIAN_POINT('Ctrl Pts',(-39.6104670975055,-44.93000002,-152.035255380817));
#142502=CARTESIAN_POINT('Ctrl Pts',(-39.560598744179,-44.93000002,-151.552464535407));
#142503=CARTESIAN_POINT('Ctrl Pts',(-39.5200177005092,-44.93000002,-151.159586987341));
#142504=CARTESIAN_POINT('Ctrl Pts',(-39.4999999999997,-44.93000002,-150.763690175803));
#142505=CARTESIAN_POINT('Ctrl Pts',(-39.5,-44.93000002,-150.364854264666));
#142506=CARTESIAN_POINT('',(-49.5369875341119,-44.93000002,-170.861259130871));
#142507=CARTESIAN_POINT('Ctrl Pts',(-49.5369875341119,-44.93000002,-170.861259130871));
#142508=CARTESIAN_POINT('Ctrl Pts',(-46.6796235355215,-44.93000002,-165.688723110732));
#142509=CARTESIAN_POINT('Ctrl Pts',(-43.770354187064,-44.93000002,-160.545717743323));
#142510=CARTESIAN_POINT('Ctrl Pts',(-40.7712064624936,-44.93000002,-155.453847126373));
#142511=CARTESIAN_POINT('',(-50.0729884546894,-44.93000002,-171.14995));
#142512=CARTESIAN_POINT('Ctrl Pts',(-50.0729884546894,-44.93000002,-171.14995));
#142513=CARTESIAN_POINT('Ctrl Pts',(-50.0168171487332,-44.93000002,-171.14995));
#142514=CARTESIAN_POINT('Ctrl Pts',(-49.9608486377765,-44.93000002,-171.143210614633));
#142515=CARTESIAN_POINT('Ctrl Pts',(-49.9066731284723,-44.93000002,-171.129767219263));
#142516=CARTESIAN_POINT('Ctrl Pts',(-49.8576729639807,-44.93000002,-171.117608061131));
#142517=CARTESIAN_POINT('Ctrl Pts',(-49.8101382025066,-44.93000002,-171.099963916562));
#142518=CARTESIAN_POINT('Ctrl Pts',(-49.7652508518366,-44.93000002,-171.076824577701));
#142519=CARTESIAN_POINT('Ctrl Pts',(-49.7179896877752,-44.93000002,-171.052461542819));
#142520=CARTESIAN_POINT('Ctrl Pts',(-49.6739559670876,-44.93000002,-171.022111093102));
#142521=CARTESIAN_POINT('Ctrl Pts',(-49.6349583346168,-44.93000002,-170.985779705428));
#142522=CARTESIAN_POINT('Ctrl Pts',(-49.5959662083459,-44.93000002,-170.949453447498));
#142523=CARTESIAN_POINT('Ctrl Pts',(-49.5629377334322,-44.93000002,-170.908235414179));
#142524=CARTESIAN_POINT('Ctrl Pts',(-49.5369875341119,-44.93000002,-170.861259130871));
#142525=CARTESIAN_POINT('',(-50.7754831343094,-44.93000002,-171.14995));
#142526=CARTESIAN_POINT('',(-49.7553180351958,-44.93000002,-171.14995));
#142527=CARTESIAN_POINT('',(-52.2902244930873,-44.93000002,-172.64995));
#142528=CARTESIAN_POINT('Ctrl Pts',(-52.2902244930873,-44.93000002,-172.64995));
#142529=CARTESIAN_POINT('Ctrl Pts',(-52.2902244930723,-44.93000002,-172.453565067926));
#142530=CARTESIAN_POINT('Ctrl Pts',(-52.2507998243741,-44.93000002,-172.257328160063));
#142531=CARTESIAN_POINT('Ctrl Pts',(-52.0990435210912,-44.93000002,-171.894521542842));
#142532=CARTESIAN_POINT('Ctrl Pts',(-51.9867715634496,-44.93000002,-171.728129909852));
#142533=CARTESIAN_POINT('Ctrl Pts',(-51.7063624782404,-44.93000002,-171.450449746589));
#142534=CARTESIAN_POINT('Ctrl Pts',(-51.5383356195984,-44.93000002,-171.339270411997));
#142535=CARTESIAN_POINT('Ctrl Pts',(-51.1719634936654,-44.93000002,-171.18899099047));
#142536=CARTESIAN_POINT('Ctrl Pts',(-50.9737980536844,-44.93000002,-171.149950000016));
#142537=CARTESIAN_POINT('Ctrl Pts',(-50.7754831343094,-44.93000002,-171.14995));
#142538=CARTESIAN_POINT('',(-52.2902244930873,-44.93000002,-55.2499500000007));
#142539=CARTESIAN_POINT('Origin',(0.,-12.9675000200281,-60.64995));
#142540=CARTESIAN_POINT('',(1.31515029790052E-14,-44.43000002,-60.64995));
#142541=CARTESIAN_POINT('Origin',(-1.8346904061005E-14,28.9199999800001,
-61.14995));
#142542=CARTESIAN_POINT('Origin',(-45.342056117244,28.91999998,-61.14995));
#142543=CARTESIAN_POINT('Origin',(-44.5079524583208,31.5404524382925,235.35105));
#142544=CARTESIAN_POINT('',(-44.5079524583208,29.5404524382925,-52.64995));
#142545=CARTESIAN_POINT('Origin',(-44.5079524583208,31.5404524382925,-52.64995));
#142546=CARTESIAN_POINT('',(-44.5079524583208,29.5404524382925,-55.24995));
#142547=CARTESIAN_POINT('',(-44.5079524583208,29.5404524382925,235.35105));
#142548=CARTESIAN_POINT('Origin',(-44.5079524583208,31.5404524382925,-55.24995));
#142549=CARTESIAN_POINT('Origin',(0.,45.41999998,-55.24995));
#142550=CARTESIAN_POINT('',(-44.5079524583208,28.7904524382925,-55.24995));
#142551=CARTESIAN_POINT('Origin',(-44.5079524583208,31.5404524382925,-55.24995));
#142552=CARTESIAN_POINT('Origin',(-44.5079524583208,31.5404524382925,-52.64995));
#142553=CARTESIAN_POINT('',(-44.5079524583208,28.7904524382925,-60.649950000076));
#142554=CARTESIAN_POINT('',(-44.5079524583208,28.7904524382925,-52.64995));
#142555=CARTESIAN_POINT('Ctrl Pts',(-44.5079556015694,28.7904524382943,
-60.6499500000744));
#142556=CARTESIAN_POINT('Ctrl Pts',(-44.5807764535743,28.7904525215285,
-60.6499499625289));
#142557=CARTESIAN_POINT('Ctrl Pts',(-44.6535686798933,28.7933450738462,
-60.6499600881128));
#142558=CARTESIAN_POINT('Ctrl Pts',(-44.8330889160976,28.807634767527,-60.6499589648009));
#142559=CARTESIAN_POINT('Ctrl Pts',(-44.9394280112978,28.8223952301239,
-60.6499497576228));
#142560=CARTESIAN_POINT('Ctrl Pts',(-45.1451244228601,28.8633251672665,
-60.6499554517945));
#142561=CARTESIAN_POINT('Ctrl Pts',(-45.2444206001228,28.8889220866332,
-60.64995));
#142562=CARTESIAN_POINT('Ctrl Pts',(-45.342056117244,28.91999998,-60.64995));
#142563=CARTESIAN_POINT('Ctrl Pts',(-43.6738487993976,28.91999998,-60.64995));
#142564=CARTESIAN_POINT('Ctrl Pts',(-43.7715308492441,28.8889072750245,
-60.64995));
#142565=CARTESIAN_POINT('Ctrl Pts',(-43.8708751019496,28.8633007826373,
-60.6499548134291));
#142566=CARTESIAN_POINT('Ctrl Pts',(-44.0766026663055,28.8223760301817,
-60.6499497945332));
#142567=CARTESIAN_POINT('Ctrl Pts',(-44.1829231968646,28.8076227744794,
-60.6499592870445));
#142568=CARTESIAN_POINT('Ctrl Pts',(-44.3623973025031,28.7933425641166,
-60.6499605225574));
#142569=CARTESIAN_POINT('Ctrl Pts',(-44.4351590053701,28.7904524382924,
-60.6499500380157));
#142570=CARTESIAN_POINT('Ctrl Pts',(-44.5079524583208,28.7904524382924,
-60.6499500000761));
#142571=CARTESIAN_POINT('Origin',(-1.8346904061005E-14,28.9199999800001,
-61.14995));
#142572=CARTESIAN_POINT('Origin',(-43.6738487993998,28.91999998,-61.1499500000012));
#142573=CARTESIAN_POINT('Origin',(-41.7558360441701,28.91999998,-61.14995));
#142574=CARTESIAN_POINT('Ctrl Pts',(-41.4049466656477,29.0638025010082,
-60.64995));
#142575=CARTESIAN_POINT('Ctrl Pts',(-41.5509245680609,28.91999998,-60.64995));
#142576=CARTESIAN_POINT('Ctrl Pts',(-41.7558360441701,28.91999998,-60.64995));
#142577=CARTESIAN_POINT('Ctrl Pts',(-41.0540572871252,28.7076050220163,
-60.64995));
#142578=CARTESIAN_POINT('Ctrl Pts',(-41.3460130919516,28.41999998,-60.64995));
#142579=CARTESIAN_POINT('Ctrl Pts',(-41.7558360441701,28.41999998,-60.64995));
#142580=CARTESIAN_POINT('Ctrl Pts',(-41.0540572871252,28.7076050220163,
-61.14995));
#142581=CARTESIAN_POINT('Ctrl Pts',(-41.3460130919516,28.41999998,-61.14995));
#142582=CARTESIAN_POINT('Ctrl Pts',(-41.7558360441701,28.41999998,-61.14995));
#142583=CARTESIAN_POINT('',(-41.0540572871253,28.7076050220164,-61.14995));
#142584=CARTESIAN_POINT('Origin',(-41.4049466656476,29.0638025010082,-61.14995));
#142585=CARTESIAN_POINT('Origin',(-41.7558360441701,29.41999998,-61.14995));
#142586=CARTESIAN_POINT('Origin',(0.,-12.9675000200281,-61.14995));
#142587=CARTESIAN_POINT('',(-39.3277310924369,30.3404619167909,-61.14995));
#142588=CARTESIAN_POINT('Origin',(-39.6638655462185,30.7106154376184,-61.14995));
#142589=CARTESIAN_POINT('Origin',(0.,-12.9675000200281,-61.14995));
#142590=CARTESIAN_POINT('Ctrl Pts',(-39.5,31.080768958446,-60.64995));
#142591=CARTESIAN_POINT('Ctrl Pts',(-39.5,30.859420873127,-60.64995));
#142592=CARTESIAN_POINT('Ctrl Pts',(-39.6638655462185,30.7106154376184,
-60.64995));
#142593=CARTESIAN_POINT('Ctrl Pts',(-39.,31.080768958446,-60.64995));
#142594=CARTESIAN_POINT('Ctrl Pts',(-39.,30.638072787808,-60.64995));
#142595=CARTESIAN_POINT('Ctrl Pts',(-39.327731092437,30.3404619167909,-60.64995));
#142596=CARTESIAN_POINT('Ctrl Pts',(-39.,31.080768958446,-61.14995));
#142597=CARTESIAN_POINT('Ctrl Pts',(-39.,30.638072787808,-61.14995));
#142598=CARTESIAN_POINT('Ctrl Pts',(-39.327731092437,30.3404619167909,-61.14995));
#142599=CARTESIAN_POINT('Origin',(-39.5,31.080768958446,-61.14995));
#142600=CARTESIAN_POINT('Origin',(-40.,31.080768958446,-61.14995));
#142601=CARTESIAN_POINT('Origin',(-39.5,46.91999998,-61.14995));
#142602=CARTESIAN_POINT('Origin',(-42.,-12.9675000200281,-61.14995));
#142603=CARTESIAN_POINT('Origin',(-42.,-58.6035812240174,-61.14995));
#142604=CARTESIAN_POINT('Origin',(-44.5079524583206,-57.475452478349,235.35105));
#142605=CARTESIAN_POINT('',(-44.5079524583206,-59.475452478349,-52.64995));
#142606=CARTESIAN_POINT('Origin',(-44.5079524583206,-57.4754524783489,-52.64995));
#142607=CARTESIAN_POINT('',(-44.5079524583206,-59.475452478349,-55.24995));
#142608=CARTESIAN_POINT('',(-44.5079524583206,-59.475452478349,235.35105));
#142609=CARTESIAN_POINT('Origin',(-44.5079524583206,-57.4754524783489,-55.24995));
#142610=CARTESIAN_POINT('Origin',(0.,45.41999998,-55.24995));
#142611=CARTESIAN_POINT('',(-44.5079524583206,-60.2254524783489,-55.24995));
#142612=CARTESIAN_POINT('Origin',(-44.5079524583206,-57.4754524783489,-55.24995));
#142613=CARTESIAN_POINT('Origin',(-44.5079524583206,-57.4754524783489,-52.64995));
#142614=CARTESIAN_POINT('',(-44.5079524583206,-60.2254524783489,-52.64995));
#142615=CARTESIAN_POINT('',(-43.1572831724516,-55.08000002,-60.64995));
#142616=CARTESIAN_POINT('Ctrl Pts',(-43.1572831724516,-55.08000002,-60.64995));
#142617=CARTESIAN_POINT('Ctrl Pts',(-43.2591939625004,-55.0225379010846,
-60.64995));
#142618=CARTESIAN_POINT('Ctrl Pts',(-43.3646678477756,-54.9716377963979,
-60.6499762002035));
#142619=CARTESIAN_POINT('Ctrl Pts',(-43.5936897926153,-54.8786129298137,
-60.6499834450286));
#142620=CARTESIAN_POINT('Ctrl Pts',(-43.7176454367697,-54.8382440852848,
-60.6498840207772));
#142621=CARTESIAN_POINT('Ctrl Pts',(-43.9338902925228,-54.7844427443954,
-60.6500640176676));
#142622=CARTESIAN_POINT('Ctrl Pts',(-44.0248533307545,-54.7666339585926,
-60.6502067882311));
#142623=CARTESIAN_POINT('Ctrl Pts',(-44.1415243890079,-54.7498576856671,
-60.6502317877326));
#142624=CARTESIAN_POINT('Ctrl Pts',(-44.1665445877625,-54.7466107515332,
-60.6502292561755));
#142625=CARTESIAN_POINT('Ctrl Pts',(-44.2185163631109,-54.74059222261,-60.6502076153997));
#142626=CARTESIAN_POINT('Ctrl Pts',(-44.2454709099202,-54.7378737484825,
-60.6501872468532));
#142627=CARTESIAN_POINT('Ctrl Pts',(-44.3345799963878,-54.7302149256925,
-60.6500997974043));
#142628=CARTESIAN_POINT('Ctrl Pts',(-44.3968571027281,-54.7269903094689,
-60.6500013450001));
#142629=CARTESIAN_POINT('Ctrl Pts',(-44.4753229318579,-54.7255987179309,
-60.6499540212932));
#142630=CARTESIAN_POINT('Ctrl Pts',(-44.4914595252895,-54.7254545924531,
-60.6499486298046));
#142631=CARTESIAN_POINT('Ctrl Pts',(-44.5716245853561,-54.7254442044781,
-60.6499568462188));
#142632=CARTESIAN_POINT('Ctrl Pts',(-44.635636337937,-54.7276720035774,
-60.6500693941759));
#142633=CARTESIAN_POINT('Ctrl Pts',(-44.8100535271152,-54.7398514986511,
-60.6502928314114));
#142634=CARTESIAN_POINT('Ctrl Pts',(-44.9200103914693,-54.7542422074975,
-60.6502860595425));
#142635=CARTESIAN_POINT('Ctrl Pts',(-45.1075048885113,-54.7904085846981,
-60.650061577148));
#142636=CARTESIAN_POINT('Ctrl Pts',(-45.1854986877238,-54.8090210757263,
-60.6499482199387));
#142637=CARTESIAN_POINT('Ctrl Pts',(-45.3711482014312,-54.8619988092867,
-60.6499529098674));
#142638=CARTESIAN_POINT('Ctrl Pts',(-45.4777060174319,-54.8996370242669,
-60.6499736151979));
#142639=CARTESIAN_POINT('Ctrl Pts',(-45.6764516340763,-54.9839240727125,
-60.6499624365077));
#142640=CARTESIAN_POINT('Ctrl Pts',(-45.7689217186581,-55.0294229071022,
-60.64995));
#142641=CARTESIAN_POINT('Ctrl Pts',(-45.8586217441897,-55.08000002,-60.64995));
#142642=CARTESIAN_POINT('',(-42.,-56.3473237326805,-60.64995));
#142643=CARTESIAN_POINT('Origin',(-44.5079524583206,-57.4754524783489,-60.64995));
#142644=CARTESIAN_POINT('Ctrl Pts',(-42.,-58.6035812240174,-60.64995));
#142645=CARTESIAN_POINT('Ctrl Pts',(-41.9586127577213,-58.5115728992456,
-60.64995));
#142646=CARTESIAN_POINT('Ctrl Pts',(-41.9223200866006,-58.4173567491329,
-60.6499639595534));
#142647=CARTESIAN_POINT('Ctrl Pts',(-41.8579031946497,-58.2180944893023,
-60.6499671932779));
#142648=CARTESIAN_POINT('Ctrl Pts',(-41.8306620008004,-58.1129431414189,
-60.6499312309338));
#142649=CARTESIAN_POINT('Ctrl Pts',(-41.7951274186657,-57.9323775711289,
-60.6499828894708));
#142650=CARTESIAN_POINT('Ctrl Pts',(-41.7836058362703,-57.8577298063975,
-60.6500200799918));
#142651=CARTESIAN_POINT('Ctrl Pts',(-41.763699988371,-57.6806798505207,
-60.6500271654877));
#142652=CARTESIAN_POINT('Ctrl Pts',(-41.7579524619679,-57.5781054625679,
-60.6499494618776));
#142653=CARTESIAN_POINT('Ctrl Pts',(-41.7579524619679,-57.3728595819394,
-60.6499505378071));
#142654=CARTESIAN_POINT('Ctrl Pts',(-41.7636932451375,-57.2703453579396,
-60.6500300767565));
#142655=CARTESIAN_POINT('Ctrl Pts',(-41.7835828980496,-57.0933348984399,
-60.6500220919564));
#142656=CARTESIAN_POINT('Ctrl Pts',(-41.795103251114,-57.0186677636544,
-60.6499835586185));
#142657=CARTESIAN_POINT('Ctrl Pts',(-41.8306429216694,-56.8380335332052,
-60.6499306306421));
#142658=CARTESIAN_POINT('Ctrl Pts',(-41.8578946341288,-56.732833798761,
-60.6499676698703));
#142659=CARTESIAN_POINT('Ctrl Pts',(-41.9223259722371,-56.5335329279262,
-60.6499642647307));
#142660=CARTESIAN_POINT('Ctrl Pts',(-41.9586161144824,-56.4393245950086,
-60.64995));
#142661=CARTESIAN_POINT('Ctrl Pts',(-42.,-56.3473237326805,-60.64995));
#142662=CARTESIAN_POINT('Origin',(1.8445455022812E-14,-55.08000002,-61.14995));
#142663=CARTESIAN_POINT('Origin',(-45.8586217441897,-55.08000002,-61.14995));
#142664=CARTESIAN_POINT('Origin',(3.3975957231091E-14,-70.08000002,-58.24995));
#142665=CARTESIAN_POINT('',(-24.7,-73.08000002,-58.24995));
#142666=CARTESIAN_POINT('Origin',(-24.7,-70.08000002,-58.24995));
#142667=CARTESIAN_POINT('',(-24.2,-73.08000002,-58.24995));
#142668=CARTESIAN_POINT('',(41.5,-73.0800000199999,-58.24995));
#142669=CARTESIAN_POINT('Origin',(-24.2,-70.08000002,-58.24995));
#142670=CARTESIAN_POINT('Origin',(-24.7,-70.08000002,-58.24995));
#142671=CARTESIAN_POINT('Origin',(-24.7,-72.58000002,-58.24995));
#142672=CARTESIAN_POINT('Origin',(-38.,46.41999998,-92.34995));
#142673=CARTESIAN_POINT('',(-38.,46.91999998,-58.24995));
#142674=CARTESIAN_POINT('',(-38.,46.91999998,-58.24995));
#142675=CARTESIAN_POINT('Origin',(-38.,46.41999998,-58.24995));
#142676=CARTESIAN_POINT('Origin',(39.,46.91999998,-129.34995));
#142677=CARTESIAN_POINT('',(-38.5,46.91999998,-58.24995));
#142678=CARTESIAN_POINT('',(-38.5,46.91999998,-129.34995));
#142679=CARTESIAN_POINT('',(39.,46.91999998,-58.24995));
#142680=CARTESIAN_POINT('Ctrl Pts',(-39.3571428571429,46.41999998,-92.4750054575003));
#142681=CARTESIAN_POINT('Ctrl Pts',(-39.,46.41999998,-92.3685260300003));
#142682=CARTESIAN_POINT('Ctrl Pts',(-39.,46.41999998,-91.9958480337503));
#142683=CARTESIAN_POINT('Ctrl Pts',(-39.3571428368889,46.5515558031783,
-92.4750054514617));
#142684=CARTESIAN_POINT('Ctrl Pts',(-38.9999999828818,46.5004721093605,
-92.3685260276219));
#142685=CARTESIAN_POINT('Ctrl Pts',(-39.,46.4857778904494,-91.9958480266757));
#142686=CARTESIAN_POINT('Ctrl Pts',(-39.3344873999803,46.6833015096169,
-92.4680006788624));
#142687=CARTESIAN_POINT('Ctrl Pts',(-38.9800988943412,46.5814616819635,
-92.3656111964877));
#142688=CARTESIAN_POINT('Ctrl Pts',(-38.9867843211749,46.5516507463266,
-91.9876757856315));
#142689=CARTESIAN_POINT('Ctrl Pts',(-39.2481885236226,46.925205464765,-92.444400991043));
#142690=CARTESIAN_POINT('Ctrl Pts',(-38.9110717002523,46.7195168934596,
-92.3578064732695));
#142691=CARTESIAN_POINT('Ctrl Pts',(-38.9364433009268,46.6726027208644,
-91.9601428292582));
#142692=CARTESIAN_POINT('Ctrl Pts',(-39.1845108402481,47.0356954006484,
-92.4279818041452));
#142693=CARTESIAN_POINT('Ctrl Pts',(-38.8613908761224,46.7770047607051,
-92.3532077914066));
#142694=CARTESIAN_POINT('Ctrl Pts',(-38.8992979918264,46.7278476911263,
-91.9409870962964));
#142695=CARTESIAN_POINT('Ctrl Pts',(-39.0271570378558,47.2191189043121,
-92.3955365750638));
#142696=CARTESIAN_POINT('Ctrl Pts',(-38.7552585438029,46.8601105768582,
-92.347890765886));
#142697=CARTESIAN_POINT('Ctrl Pts',(-38.8075082704007,46.819559441354,-91.903134346114));
#142698=CARTESIAN_POINT('Ctrl Pts',(-38.9319509445986,47.2935007246494,
-92.3793987064332));
#142699=CARTESIAN_POINT('Ctrl Pts',(-38.6983937732817,46.8857748070212,
-92.3473559512381));
#142700=CARTESIAN_POINT('Ctrl Pts',(-38.7519713842669,46.8567503512399,
-91.884306817494));
#142701=CARTESIAN_POINT('Ctrl Pts',(-38.7257728904125,47.3934379073013,
-92.3566603033275));
#142702=CARTESIAN_POINT('Ctrl Pts',(-38.5942499321354,46.9153405921297,
-92.3486011659899));
#142703=CARTESIAN_POINT('Ctrl Pts',(-38.631700852823,46.9067189447356,-91.8577786938935));
#142704=CARTESIAN_POINT('Ctrl Pts',(-38.6117163199788,47.4199999701223,
-92.34995));
#142705=CARTESIAN_POINT('Ctrl Pts',(-38.5461650349159,46.9199999780196,
-92.3499499995552));
#142706=CARTESIAN_POINT('Ctrl Pts',(-38.5651678532719,46.91999998,-91.849950002847));
#142707=CARTESIAN_POINT('Ctrl Pts',(-38.5,47.41999998,-92.34995));
#142708=CARTESIAN_POINT('Ctrl Pts',(-38.5,46.91999998,-92.34995));
#142709=CARTESIAN_POINT('Ctrl Pts',(-38.5,46.91999998,-91.84995));
#142710=CARTESIAN_POINT('Origin',(-39.5,46.41999998,-91.9958480337503));
#142711=CARTESIAN_POINT('Ctrl Pts',(-39.,46.41999998,-91.9958480337503));
#142712=CARTESIAN_POINT('Ctrl Pts',(-39.,46.4857778904494,-91.9958480266757));
#142713=CARTESIAN_POINT('Ctrl Pts',(-38.9867843211749,46.5516507463266,
-91.9876757856315));
#142714=CARTESIAN_POINT('Ctrl Pts',(-38.9364433009268,46.6726027208644,
-91.9601428292582));
#142715=CARTESIAN_POINT('Ctrl Pts',(-38.8992979918264,46.7278476911263,
-91.9409870962964));
#142716=CARTESIAN_POINT('Ctrl Pts',(-38.8075082704007,46.819559441354,-91.903134346114));
#142717=CARTESIAN_POINT('Ctrl Pts',(-38.7519713842669,46.8567503512399,
-91.884306817494));
#142718=CARTESIAN_POINT('Ctrl Pts',(-38.631700852823,46.9067189447356,-91.8577786938935));
#142719=CARTESIAN_POINT('Ctrl Pts',(-38.5651678532719,46.91999998,-91.849950002847));
#142720=CARTESIAN_POINT('Ctrl Pts',(-38.5,46.91999998,-91.84995));
#142721=CARTESIAN_POINT('Ctrl Pts',(-41.0540572871253,28.7076050220164,
-93.3976987687948));
#142722=CARTESIAN_POINT('Ctrl Pts',(-40.9209666515892,28.8387123238495,
-93.5739383154377));
#142723=CARTESIAN_POINT('Ctrl Pts',(-40.9899542848408,29.0638025010082,
-93.6765918018241));
#142724=CARTESIAN_POINT('Ctrl Pts',(-41.181465342889,28.5820956174237,-93.4924903917862));
#142725=CARTESIAN_POINT('Ctrl Pts',(-40.9927653037546,28.7197223139655,
-93.6733291751567));
#142726=CARTESIAN_POINT('Ctrl Pts',(-41.0445777715999,29.0010249744694,
-93.7578714615268));
#142727=CARTESIAN_POINT('Ctrl Pts',(-41.3136336664734,28.5141965951637,
-93.601569918277));
#142728=CARTESIAN_POINT('Ctrl Pts',(-41.064373682842,28.640994986895,-93.7860557549848));
#142729=CARTESIAN_POINT('Ctrl Pts',(-41.1012013116007,28.9670983124193,
-93.8513385014916));
#142730=CARTESIAN_POINT('Ctrl Pts',(-41.5532792074141,28.4325824175145,
-93.828366995811));
#142731=CARTESIAN_POINT('Ctrl Pts',(-41.1909352247283,28.5106646509549,
-94.0164009875504));
#142732=CARTESIAN_POINT('Ctrl Pts',(-41.203906529354,28.9262911739198,-94.0457359962981));
#142733=CARTESIAN_POINT('Ctrl Pts',(-41.6609761593771,28.4199999800001,
-93.9453729847263));
#142734=CARTESIAN_POINT('Ctrl Pts',(-41.245616944193,28.4623003387481,-94.1347575623882));
#142735=CARTESIAN_POINT('Ctrl Pts',(-41.2500626594833,28.9199999557335,
-94.1460275680244));
#142736=CARTESIAN_POINT('Ctrl Pts',(-41.7558360441699,28.41999998,-94.0656090587062));
#142737=CARTESIAN_POINT('Ctrl Pts',(-41.2907166092886,28.4199999800001,
-94.2490863360339));
#142738=CARTESIAN_POINT('Ctrl Pts',(-41.2907166092886,28.91999998,-94.2490863360339));
#142739=CARTESIAN_POINT('',(-41.0540572871253,28.7076050220164,-93.3976987687948));
#142740=CARTESIAN_POINT('Origin',(-41.4049466656476,29.0638025010082,-93.3976987687947));
#142741=CARTESIAN_POINT('Origin',(-41.75583604417,28.91999998,-94.0656090587062));
#142742=CARTESIAN_POINT('Ctrl Pts',(-41.7558360441701,28.41999998,-94.0656090587062));
#142743=CARTESIAN_POINT('Ctrl Pts',(-41.6609761593771,28.4199999800001,
-93.9453729847263));
#142744=CARTESIAN_POINT('Ctrl Pts',(-41.5532792074141,28.4325824175145,
-93.828366995811));
#142745=CARTESIAN_POINT('Ctrl Pts',(-41.3136336664734,28.5141965951637,
-93.601569918277));
#142746=CARTESIAN_POINT('Ctrl Pts',(-41.181465342889,28.5820956174237,-93.4924903917862));
#142747=CARTESIAN_POINT('Ctrl Pts',(-41.0540572871253,28.7076050220164,
-93.3976987687948));
#142748=CARTESIAN_POINT('Origin',(-38.5,28.91999998,-95.34995));
#142749=CARTESIAN_POINT('Origin',(-42.,28.91999998,-95.34995));
#142750=CARTESIAN_POINT('Origin',(-39.5,58.91999998,-91.9958480337503));
#142751=CARTESIAN_POINT('Origin',(-39.5,31.080768958446,-91.9958480337503));
#142752=CARTESIAN_POINT('Ctrl Pts',(-39.,31.080768958446,-91.9958480337503));
#142753=CARTESIAN_POINT('Ctrl Pts',(-39.,31.080768958446,-92.3685260300003));
#142754=CARTESIAN_POINT('Ctrl Pts',(-39.3571428571429,31.080768958446,-92.4750054575003));
#142755=CARTESIAN_POINT('Ctrl Pts',(-39.,30.7973529986378,-91.9958480635187));
#142756=CARTESIAN_POINT('Ctrl Pts',(-39.0000001561187,30.8288322275033,
-92.3685260646169));
#142757=CARTESIAN_POINT('Ctrl Pts',(-39.3571429430277,30.9391538899445,
-92.4750054831062));
#142758=CARTESIAN_POINT('Ctrl Pts',(-39.1237015311635,30.5257400818631,
-92.0131591004063));
#142759=CARTESIAN_POINT('Ctrl Pts',(-39.0995023767794,30.5843250255347,
-92.3886066067861));
#142760=CARTESIAN_POINT('Ctrl Pts',(-39.410274588038,30.8031308123719,-92.4898846529936));
#142761=CARTESIAN_POINT('Ctrl Pts',(-39.3277310924369,30.3404619167909,
-92.0491293459315));
#142762=CARTESIAN_POINT('Ctrl Pts',(-39.2532568247562,30.4080916052285,
-92.4345203712043));
#142763=CARTESIAN_POINT('Ctrl Pts',(-39.4975990396159,30.7106154376184,
-92.5206751536556));
#142764=CARTESIAN_POINT('',(-39.3277310924369,30.3404619167909,-92.0491293459315));
#142765=CARTESIAN_POINT('Origin',(-39.6638655462185,30.7106154376184,-92.0491293459315));
#142766=CARTESIAN_POINT('Ctrl Pts',(-39.3277310924369,30.3404619167909,
-92.0491293459315));
#142767=CARTESIAN_POINT('Ctrl Pts',(-39.1237015311635,30.5257400818631,
-92.0131591004063));
#142768=CARTESIAN_POINT('Ctrl Pts',(-39.,30.7973529986378,-91.9958480635187));
#142769=CARTESIAN_POINT('Ctrl Pts',(-39.,31.080768958446,-91.9958480337503));
#142770=CARTESIAN_POINT('Ctrl Pts',(-40.9899542848408,29.0638025010082,
-93.6765918018241));
#142771=CARTESIAN_POINT('Ctrl Pts',(-40.9209666515892,28.8387123238495,
-93.5739383154377));
#142772=CARTESIAN_POINT('Ctrl Pts',(-41.0540572871253,28.7076050220164,
-93.3976987687948));
#142773=CARTESIAN_POINT('Ctrl Pts',(-40.7930602005308,29.2900891143653,
-93.3836137237161));
#142774=CARTESIAN_POINT('Ctrl Pts',(-40.6946394065552,29.0602110175707,
-93.2636650794047));
#142775=CARTESIAN_POINT('Ctrl Pts',(-40.8263518506557,28.931917162897,-93.0559775318146));
#142776=CARTESIAN_POINT('Ctrl Pts',(-40.5646325235533,29.548843193136,-93.1505624120075));
#142777=CARTESIAN_POINT('Ctrl Pts',(-40.4345448959912,29.3109818121476,
-93.0268336432776));
#142778=CARTESIAN_POINT('Ctrl Pts',(-40.5620537232219,29.1885351995273,
-92.7839978150636));
#142779=CARTESIAN_POINT('Ctrl Pts',(-40.0606440851126,30.1068692044787,
-92.7683994467215));
#142780=CARTESIAN_POINT('Ctrl Pts',(-39.8699190705461,29.8439046252157,
-92.6499647524336));
#142781=CARTESIAN_POINT('Ctrl Pts',(-39.979050150362,29.7418321774292,-92.3381410201203));
#142782=CARTESIAN_POINT('Ctrl Pts',(-39.7830757934441,30.4081688522969,
-92.6213339269874));
#142783=CARTESIAN_POINT('Ctrl Pts',(-39.5589873293178,30.1314683688792,
-92.5153277294035));
#142784=CARTESIAN_POINT('Ctrl Pts',(-39.6579655806366,30.0405777253273,
-92.1665648604216));
#142785=CARTESIAN_POINT('Ctrl Pts',(-39.4975990396159,30.7106154376184,
-92.5206751536556));
#142786=CARTESIAN_POINT('Ctrl Pts',(-39.2532568247562,30.4080916052286,
-92.4345203712043));
#142787=CARTESIAN_POINT('Ctrl Pts',(-39.3277310924369,30.3404619167909,
-92.0491293459315));
#142788=CARTESIAN_POINT('Ctrl Pts',(-41.0540572871253,28.7076050220164,
-93.3976987687948));
#142789=CARTESIAN_POINT('Ctrl Pts',(-40.8263518506557,28.931917162897,-93.0559775318146));
#142790=CARTESIAN_POINT('Ctrl Pts',(-40.5620537232219,29.1885351995273,
-92.7839978150636));
#142791=CARTESIAN_POINT('Ctrl Pts',(-39.979050150362,29.7418321774292,-92.3381410201203));
#142792=CARTESIAN_POINT('Ctrl Pts',(-39.6579655806366,30.0405777253273,
-92.1665648604216));
#142793=CARTESIAN_POINT('Ctrl Pts',(-39.3277310924369,30.3404619167909,
-92.0491293459315));
#142794=CARTESIAN_POINT('Origin',(-4.,46.41999998,-92.34995));
#142795=CARTESIAN_POINT('',(-4.,46.91999998,-57.9072287192657));
#142796=CARTESIAN_POINT('Origin',(39.,46.91999998,-129.34995));
#142797=CARTESIAN_POINT('',(-4.5,46.91999998,-92.34995));
#142798=CARTESIAN_POINT('Origin',(-4.5,46.41999998,-92.34995));
#142799=CARTESIAN_POINT('Ctrl Pts',(-5.00000098575356,31.8716754827171,
-91.8489571492625));
#142800=CARTESIAN_POINT('Ctrl Pts',(-4.99900616154964,31.8716754827171,
-92.34995));
#142801=CARTESIAN_POINT('Ctrl Pts',(-5.5,31.8716754827171,-92.34995));
#142802=CARTESIAN_POINT('Ctrl Pts',(-5.00000096584847,31.7882063435841,
-91.8489671288812));
#142803=CARTESIAN_POINT('Ctrl Pts',(-4.99903601393703,31.7072113826353,
-92.3399186475543));
#142804=CARTESIAN_POINT('Ctrl Pts',(-5.48989377680063,31.7056523166615,
-92.34995));
#142805=CARTESIAN_POINT('Ctrl Pts',(-5.0000009456393,31.7039607739183,-91.8276307576481));
#142806=CARTESIAN_POINT('Ctrl Pts',(-4.99906555653788,31.5446619586649,
-92.2883582792096));
#142807=CARTESIAN_POINT('Ctrl Pts',(-5.47963373781052,31.538103809625,-92.3071746231476));
#142808=CARTESIAN_POINT('Ctrl Pts',(-5.00000091915851,31.5940866659345,
-91.7681041344864));
#142809=CARTESIAN_POINT('Ctrl Pts',(-4.99910325428599,31.3370094182925,
-92.161272810455));
#142810=CARTESIAN_POINT('Ctrl Pts',(-5.46619042199875,31.3196047327668,
-92.1878686007335));
#142811=CARTESIAN_POINT('Ctrl Pts',(-5.00000091080218,31.559505537537,-91.7433851154801));
#142812=CARTESIAN_POINT('Ctrl Pts',(-4.99911492812357,31.2726858878274,
-92.1103972204605));
#142813=CARTESIAN_POINT('Ctrl Pts',(-5.46194839019336,31.2508398250121,
-92.1383294170381));
#142814=CARTESIAN_POINT('Ctrl Pts',(-5.00000089592572,31.4980571027819,
-91.6865378587354));
#142815=CARTESIAN_POINT('Ctrl Pts',(-4.99913545432373,31.1595480268538,
-91.9961676804234));
#142816=CARTESIAN_POINT('Ctrl Pts',(-5.45439667136824,31.1286541135227,
-92.0244078521253));
#142817=CARTESIAN_POINT('Ctrl Pts',(-5.00000088941156,31.4712115049486,
-91.6546739801726));
#142818=CARTESIAN_POINT('Ctrl Pts',(-4.99914433728297,31.1105664451877,
-91.9333048742068));
#142819=CARTESIAN_POINT('Ctrl Pts',(-5.45108997919633,31.0752759499814,
-91.9605552262364));
#142820=CARTESIAN_POINT('Ctrl Pts',(-5.00000087274503,31.4026135113337,
-91.5484928091743));
#142821=CARTESIAN_POINT('Ctrl Pts',(-4.99916680129901,30.9866628751625,
-91.7272955383522));
#142822=CARTESIAN_POINT('Ctrl Pts',(-5.44262999595016,30.938884482232,-91.7477840212027));
#142823=CARTESIAN_POINT('Ctrl Pts',(-5.00000086614597,31.3755689941199,
-91.4665221319677));
#142824=CARTESIAN_POINT('Ctrl Pts',(-4.99917557417014,30.9382275273277,
-91.5708670061703));
#142825=CARTESIAN_POINT('Ctrl Pts',(-5.43928039898085,30.8851161679224,
-91.5835323055617));
#142826=CARTESIAN_POINT('Ctrl Pts',(-5.00000086340344,31.3643200540024,
-91.3002194649783));
#142827=CARTESIAN_POINT('Ctrl Pts',(-4.99917920690221,30.9181743619019,
-91.2558237036598));
#142828=CARTESIAN_POINT('Ctrl Pts',(-5.43788833142316,30.8627516985332,
-91.2503023235849));
#142829=CARTESIAN_POINT('Ctrl Pts',(-5.00000086731321,31.3803302826731,
-91.214808683899));
#142830=CARTESIAN_POINT('Ctrl Pts',(-4.99917405374185,30.946764229838,-91.0936720204704));
#142831=CARTESIAN_POINT('Ctrl Pts',(-5.4398728408893,30.894582824155,-91.0791566847487));
#142832=CARTESIAN_POINT('Ctrl Pts',(-5.0000008759766,31.4159376038031,-91.1390388927801));
#142833=CARTESIAN_POINT('Ctrl Pts',(-4.99916246706242,31.0105597677355,
-90.9485621815415));
#142834=CARTESIAN_POINT('Ctrl Pts',(-5.44427033638568,30.9653765476951,
-90.9273317382594));
#142835=CARTESIAN_POINT('Origin',(-5.5,31.415090518797,-91.1386408691297));
#142836=CARTESIAN_POINT('Ctrl Pts',(-12.,30.2507177004773,-91.1386408691297));
#142837=CARTESIAN_POINT('Ctrl Pts',(-12.,29.679733250215,-90.8631216114042));
#142838=CARTESIAN_POINT('Ctrl Pts',(-11.3834743397155,29.812801930373,-90.9273317382593));
#142839=CARTESIAN_POINT('Ctrl Pts',(-12.,30.2139234693476,-91.2148931255634));
#142840=CARTESIAN_POINT('Ctrl Pts',(-11.9999999999987,29.5832417343753,
-91.0342442171839));
#142841=CARTESIAN_POINT('Ctrl Pts',(-11.3742392183232,29.741677094381,-91.0798230944648));
#142842=CARTESIAN_POINT('Ctrl Pts',(-12.,30.1973151560885,-91.3015254072135));
#142843=CARTESIAN_POINT('Ctrl Pts',(-11.9999999999999,29.5383067623994,
-91.2361587739122));
#142844=CARTESIAN_POINT('Ctrl Pts',(-11.3700547859617,29.7095698537212,
-91.2531008141058));
#142845=CARTESIAN_POINT('Ctrl Pts',(-12.,30.2066913195442,-91.427825927492));
#142846=CARTESIAN_POINT('Ctrl Pts',(-12.0000000000001,29.5635939180596,
-91.5323968928992));
#142847=CARTESIAN_POINT('Ctrl Pts',(-11.3724129716406,29.7276939951996,
-91.5057018551446));
#142848=CARTESIAN_POINT('Ctrl Pts',(-12.,30.2155293203062,-91.4701692696895));
#142849=CARTESIAN_POINT('Ctrl Pts',(-11.9999999999998,29.5872932859939,
-91.6306703852657));
#142850=CARTESIAN_POINT('Ctrl Pts',(-11.374636075473,29.7447777509884,-91.5903885436157));
#142851=CARTESIAN_POINT('Ctrl Pts',(-12.,30.2434629903521,-91.5500105484349));
#142852=CARTESIAN_POINT('Ctrl Pts',(-12.0000000000001,29.6609253730622,
-91.812155424579));
#142853=CARTESIAN_POINT('Ctrl Pts',(-11.3816540502047,29.7987767762788,
-91.7500710926331));
#142854=CARTESIAN_POINT('Ctrl Pts',(-12.,30.2626690028682,-91.5881956385046));
#142855=CARTESIAN_POINT('Ctrl Pts',(-11.9999999999999,29.7106471563183,
-91.8964616250679));
#142856=CARTESIAN_POINT('Ctrl Pts',(-11.3864765114273,29.8359053318054,
-91.8264412916623));
#142857=CARTESIAN_POINT('Ctrl Pts',(-12.,30.3342288077533,-91.6940226905849));
#142858=CARTESIAN_POINT('Ctrl Pts',(-12.0000000000001,29.8895113426933,
-92.1195167159054));
#142859=CARTESIAN_POINT('Ctrl Pts',(-11.4044123087811,29.9742563988052,
-92.0380953518635));
#142860=CARTESIAN_POINT('Ctrl Pts',(-12.,30.3998197343385,-91.7515247512526));
#142861=CARTESIAN_POINT('Ctrl Pts',(-11.9999999999989,30.0452979686933,
-92.2283418495211));
#142862=CARTESIAN_POINT('Ctrl Pts',(-11.4208142717207,30.101082992511,-92.1530994985312));
#142863=CARTESIAN_POINT('Ctrl Pts',(-12.,30.5498659135928,-91.8294071489743));
#142864=CARTESIAN_POINT('Ctrl Pts',(-12.0000000000011,30.3770555999401,
-92.3523349137576));
#142865=CARTESIAN_POINT('Ctrl Pts',(-11.458128525139,30.3912975665021,-92.3088643019226));
#142866=CARTESIAN_POINT('Ctrl Pts',(-12.,30.635088667613,-91.8499499468525));
#142867=CARTESIAN_POINT('Ctrl Pts',(-12.,30.5530678891822,-92.3711185577562));
#142868=CARTESIAN_POINT('Ctrl Pts',(-11.4792261802719,30.5561711606282,
-92.34995));
#142869=CARTESIAN_POINT('Ctrl Pts',(-12.,30.7194735506599,-91.84995));
#142870=CARTESIAN_POINT('Ctrl Pts',(-12.,30.7194735506598,-92.34995));
#142871=CARTESIAN_POINT('Ctrl Pts',(-11.5,30.7194735506599,-92.34995));
#142872=CARTESIAN_POINT('Origin',(-11.5,30.2507177004773,-91.1386408691297));
#142873=CARTESIAN_POINT('Origin',(-12.5,46.41999998,-92.34995));
#142874=CARTESIAN_POINT('',(-12.5,46.91999998,-58.2396719107252));
#142875=CARTESIAN_POINT('Origin',(39.,46.91999998,-129.34995));
#142876=CARTESIAN_POINT('',(-13.,46.91999998,-92.34995));
#142877=CARTESIAN_POINT('Origin',(-13.,46.41999998,-92.34995));
#142878=CARTESIAN_POINT('Ctrl Pts',(-13.5,29.9836543272765,-91.84995));
#142879=CARTESIAN_POINT('Ctrl Pts',(-13.5,29.9836543272765,-92.34995));
#142880=CARTESIAN_POINT('Ctrl Pts',(-14.,29.9836543272765,-92.34995));
#142881=CARTESIAN_POINT('Ctrl Pts',(-13.5,29.9498130224307,-91.8499499813658));
#142882=CARTESIAN_POINT('Ctrl Pts',(-13.5,29.9198591164476,-92.340077310875));
#142883=CARTESIAN_POINT('Ctrl Pts',(-13.9900288285115,29.9192223045234,
-92.34995));
#142884=CARTESIAN_POINT('Ctrl Pts',(-13.5,29.9164799575816,-91.8468718299503));
#142885=CARTESIAN_POINT('Ctrl Pts',(-13.4999999999992,29.8581345500688,
-92.3247747757233));
#142886=CARTESIAN_POINT('Ctrl Pts',(-13.9801870069313,29.8557668849998,
-92.3437935523175));
#142887=CARTESIAN_POINT('Ctrl Pts',(-13.5,29.8836583509375,-91.8408299848543));
#142888=CARTESIAN_POINT('Ctrl Pts',(-13.5,29.7983343836869,-92.3043420473086));
#142889=CARTESIAN_POINT('Ctrl Pts',(-13.9704776589253,29.7932964571608,
-92.3317099697086));
#142890=CARTESIAN_POINT('Origin',(-14.,29.8836583509375,-91.8408299848543));
#142891=CARTESIAN_POINT('Ctrl Pts',(-13.5,29.8836583509376,-91.8408299848543));
#142892=CARTESIAN_POINT('Ctrl Pts',(-13.5,29.798334383687,-92.3043420473087));
#142893=CARTESIAN_POINT('Ctrl Pts',(-13.9704776589254,29.793296457161,-92.3317099697086));
#142894=CARTESIAN_POINT('Ctrl Pts',(-13.5,29.8088158028921,-91.8270528245268));
#142895=CARTESIAN_POINT('Ctrl Pts',(-13.5,29.6658016093476,-92.2593052595342));
#142896=CARTESIAN_POINT('Ctrl Pts',(-13.9485824763266,29.6507732526529,
-92.3041572803908));
#142897=CARTESIAN_POINT('Ctrl Pts',(-13.5,29.7360856593875,-91.7971835648529));
#142898=CARTESIAN_POINT('Ctrl Pts',(-13.5,29.5406281722262,-92.1878683704653));
#142899=CARTESIAN_POINT('Ctrl Pts',(-13.9277414892694,29.5120300570818,
-92.2444171371624));
#142900=CARTESIAN_POINT('Ctrl Pts',(-13.5,29.6110266364568,-91.7101609842055));
#142901=CARTESIAN_POINT('Ctrl Pts',(-13.5,29.3333704157687,-92.0065554596633));
#142902=CARTESIAN_POINT('Ctrl Pts',(-13.8924131672203,29.2732201982241,
-92.0703719609639));
#142903=CARTESIAN_POINT('Ctrl Pts',(-13.5,29.5578590401594,-91.6523482016898));
#142904=CARTESIAN_POINT('Ctrl Pts',(-13.4999999999999,29.2476129207544,
-91.895386283959));
#142905=CARTESIAN_POINT('Ctrl Pts',(-13.8776710606793,29.1715523493698,
-91.9547463954628));
#142906=CARTESIAN_POINT('Ctrl Pts',(-13.5,29.4834479217461,-91.5199437062307));
#142907=CARTESIAN_POINT('Ctrl Pts',(-13.5000000000001,29.1302566914018,
-91.6522607622863));
#142908=CARTESIAN_POINT('Ctrl Pts',(-13.8571693529918,29.0291974882966,
-91.6899374203782));
#142909=CARTESIAN_POINT('Ctrl Pts',(-13.5,29.4617011701904,-91.4445487431295));
#142910=CARTESIAN_POINT('Ctrl Pts',(-13.5000000000001,29.0962692564556,
-91.5174684103174));
#142911=CARTESIAN_POINT('Ctrl Pts',(-13.851254772454,28.9875557647693,-91.5391474846049));
#142912=CARTESIAN_POINT('Ctrl Pts',(-13.5,29.4559384360516,-91.2911813034188));
#142913=CARTESIAN_POINT('Ctrl Pts',(-13.4999999999999,29.0873381907095,
-91.2460073456115));
#142914=CARTESIAN_POINT('Ctrl Pts',(-13.8496827900737,28.9765232161018,
-91.2324126084916));
#142915=CARTESIAN_POINT('Ctrl Pts',(-13.5,29.4717444256829,-91.2146593048585));
#142916=CARTESIAN_POINT('Ctrl Pts',(-13.4999999999996,29.1119956223332,
-91.1098405101534));
#142917=CARTESIAN_POINT('Ctrl Pts',(-13.8539744318671,29.0067940350096,
-91.0793665022882));
#142918=CARTESIAN_POINT('Ctrl Pts',(-13.5,29.5044693674792,-91.1451435916293));
#142919=CARTESIAN_POINT('Ctrl Pts',(-13.5,29.162996502681,-90.984393353347));
#142920=CARTESIAN_POINT('Ctrl Pts',(-13.8629670146647,29.0694104105324,
-90.9403371832566));
#142921=CARTESIAN_POINT('Origin',(-14.,29.5044693674792,-91.1451435916293));
#142922=CARTESIAN_POINT('Ctrl Pts',(-21.7666112105514,28.41999998,-87.8078183592076));
#142923=CARTESIAN_POINT('Ctrl Pts',(-20.7092106783515,28.41999998,-86.6470800003654));
#142924=CARTESIAN_POINT('Ctrl Pts',(-19.8416434885933,29.3176415862829,
-85.6947270505041));
#142925=CARTESIAN_POINT('Ctrl Pts',(-20.7402388551495,28.41999998,-88.7428151801658));
#142926=CARTESIAN_POINT('Ctrl Pts',(-19.7296405475835,28.4199999799976,
-87.5847244149266));
#142927=CARTESIAN_POINT('Ctrl Pts',(-18.8896716409139,29.2827357288726,
-86.6297133466452));
#142928=CARTESIAN_POINT('Ctrl Pts',(-19.6830654074503,28.4199999800001,
-89.6522445020127));
#142929=CARTESIAN_POINT('Ctrl Pts',(-18.7197222668567,28.41999998,-88.4987039616193));
#142930=CARTESIAN_POINT('Ctrl Pts',(-17.9119477871191,29.2478866829953,
-87.5391531932496));
#142931=CARTESIAN_POINT('Ctrl Pts',(-17.4871574021565,28.4199999800001,
-91.4036210595759));
#142932=CARTESIAN_POINT('Ctrl Pts',(-16.6238286994528,28.41999998,-90.2586559409325));
#142933=CARTESIAN_POINT('Ctrl Pts',(-15.8876250911483,29.1791411788287,
-89.290529750932));
#142934=CARTESIAN_POINT('Ctrl Pts',(-16.353131902533,28.4199999800001,-92.2410073071712));
#142935=CARTESIAN_POINT('Ctrl Pts',(-15.5423832476573,28.4199999800097,
-91.1005048403699));
#142936=CARTESIAN_POINT('Ctrl Pts',(-14.8453850851454,29.1454134093176,
-90.1279271408305));
#142937=CARTESIAN_POINT('Ctrl Pts',(-15.1919283151595,28.4199999800001,
-93.0160464292372));
#142938=CARTESIAN_POINT('Ctrl Pts',(-14.4341913591531,28.41999998,-91.8807658383619));
#142939=CARTESIAN_POINT('Ctrl Pts',(-13.781556827362,29.1135284095041,-90.9029551205337));
#142940=CARTESIAN_POINT('',(-20.,28.4199999800001,-89.3628471840451));
#142941=CARTESIAN_POINT('Origin',(-20.0888710624269,28.4200000295341,-83.1773333845304));
#142942=CARTESIAN_POINT('Ctrl Pts',(-19.8077681778583,29.3163999071086,
-85.7279764688716));
#142943=CARTESIAN_POINT('Ctrl Pts',(-19.8136574212126,29.2576540355216,
-85.8367033527245));
#142944=CARTESIAN_POINT('Ctrl Pts',(-19.8196451473997,29.202108371412,-85.946486159213));
#142945=CARTESIAN_POINT('Ctrl Pts',(-19.8256705338347,29.1496220282844,
-86.0572294761739));
#142946=CARTESIAN_POINT('Ctrl Pts',(-19.831938355614,29.0950238629849,-86.1724286225603));
#142947=CARTESIAN_POINT('Ctrl Pts',(-19.8382471186921,29.0437352856753,
-86.288667271822));
#142948=CARTESIAN_POINT('Ctrl Pts',(-19.8445663866126,28.9956132814831,
-86.4058785872911));
#142949=CARTESIAN_POINT('Ctrl Pts',(-19.8509287374279,28.9471631957372,
-86.5238890147492));
#142950=CARTESIAN_POINT('Ctrl Pts',(-19.8573022294804,28.9019223155722,
-86.6428858945738));
#142951=CARTESIAN_POINT('Ctrl Pts',(-19.863688044158,28.8597720721441,-86.7628362248108));
#142952=CARTESIAN_POINT('Ctrl Pts',(-19.870186584175,28.8168777732216,-86.884903973478));
#142953=CARTESIAN_POINT('Ctrl Pts',(-19.8766984153534,28.7771835491368,
-87.0079596644619));
#142954=CARTESIAN_POINT('Ctrl Pts',(-19.8832503422814,28.7406029640851,
-87.1319972358868));
#142955=CARTESIAN_POINT('Ctrl Pts',(-19.8894441753394,28.7060216814381,
-87.2492555659603));
#142956=CARTESIAN_POINT('Ctrl Pts',(-19.8956744956213,28.6742230445864,
-87.3673920903953));
#142957=CARTESIAN_POINT('Ctrl Pts',(-19.9019775505939,28.6451714612775,
-87.486417589477));
#142958=CARTESIAN_POINT('Ctrl Pts',(-19.9110636635093,28.6032924093798,
-87.6579977405552));
#142959=CARTESIAN_POINT('Ctrl Pts',(-19.9202391291903,28.5671050608127,
-87.8316012622964));
#142960=CARTESIAN_POINT('Ctrl Pts',(-19.9294481187907,28.5367577809419,
-88.0065835848011));
#142961=CARTESIAN_POINT('Ctrl Pts',(-19.9386272558149,28.5065088771713,
-88.180998671014));
#142962=CARTESIAN_POINT('Ctrl Pts',(-19.9478394433303,28.4820622096005,
-88.3567835651411));
#142963=CARTESIAN_POINT('Ctrl Pts',(-19.9570427327963,28.463517168047,-88.5332849397664));
#142964=CARTESIAN_POINT('Ctrl Pts',(-19.9661625657539,28.4451402951058,
-88.708185779221));
#142965=CARTESIAN_POINT('Ctrl Pts',(-19.9752734569136,28.4325584744372,
-88.883790083378));
#142966=CARTESIAN_POINT('Ctrl Pts',(-19.9843510994179,28.4258221481163,
-89.0594484841297));
#142967=CARTESIAN_POINT('Ctrl Pts',(-19.989578681727,28.4219428699572,-89.1606056675928));
#142968=CARTESIAN_POINT('Ctrl Pts',(-19.9947955600196,28.420001288699,-89.2617805437457));
#142969=CARTESIAN_POINT('Ctrl Pts',(-20.,28.4199999806615,-89.3628471840451));
#142970=CARTESIAN_POINT('Origin',(-13.9259921622961,31.8088924073546,-92.6508709683574));
#142971=CARTESIAN_POINT('Origin',(-60.,28.41999998,-55.24995));
#142972=CARTESIAN_POINT('',(-20.,28.4199999800001,-91.34995));
#142973=CARTESIAN_POINT('Ctrl Pts',(-20.,29.41999998,-92.34995));
#142974=CARTESIAN_POINT('Ctrl Pts',(-20.,28.41999998,-92.34995));
#142975=CARTESIAN_POINT('Ctrl Pts',(-20.,28.41999998,-91.34995));
#142976=CARTESIAN_POINT('Ctrl Pts',(-20.5,29.41999998,-92.34995));
#142977=CARTESIAN_POINT('Ctrl Pts',(-20.5,28.41999998,-92.34995));
#142978=CARTESIAN_POINT('Ctrl Pts',(-20.5,28.41999998,-91.34995));
#142979=CARTESIAN_POINT('Ctrl Pts',(-20.5,29.41999998,-91.84995));
#142980=CARTESIAN_POINT('Ctrl Pts',(-20.5,28.91999998,-91.84995));
#142981=CARTESIAN_POINT('Ctrl Pts',(-20.5,28.91999998,-91.34995));
#142982=CARTESIAN_POINT('Origin',(-20.,28.9199999800001,-91.34995));
#142983=CARTESIAN_POINT('Origin',(-21.,46.41999998,-92.34995));
#142984=CARTESIAN_POINT('',(-21.,46.91999998,-58.24995));
#142985=CARTESIAN_POINT('',(-21.,46.91999998,-58.24995));
#142986=CARTESIAN_POINT('Origin',(-21.,46.41999998,-58.24995));
#142987=CARTESIAN_POINT('Origin',(39.,46.91999998,-129.34995));
#142988=CARTESIAN_POINT('',(-21.5,46.91999998,-58.24995));
#142989=CARTESIAN_POINT('',(-21.5,46.91999998,-92.34995));
#142990=CARTESIAN_POINT('',(39.,46.91999998,-58.24995));
#142991=CARTESIAN_POINT('Origin',(-21.5,46.41999998,-92.34995));
#142992=CARTESIAN_POINT('Origin',(-21.5,46.41999998,-58.24995));
#142993=CARTESIAN_POINT('Ctrl Pts',(-22.5,28.41999998,-91.34995));
#142994=CARTESIAN_POINT('Ctrl Pts',(-22.5,28.41999998,-92.34995));
#142995=CARTESIAN_POINT('Ctrl Pts',(-22.5,29.41999998,-92.34995));
#142996=CARTESIAN_POINT('Ctrl Pts',(-22.,28.41999998,-91.34995));
#142997=CARTESIAN_POINT('Ctrl Pts',(-22.,28.41999998,-92.34995));
#142998=CARTESIAN_POINT('Ctrl Pts',(-22.,29.41999998,-92.34995));
#142999=CARTESIAN_POINT('Ctrl Pts',(-22.,28.91999998,-91.34995));
#143000=CARTESIAN_POINT('Ctrl Pts',(-22.,28.91999998,-91.84995));
#143001=CARTESIAN_POINT('Ctrl Pts',(-22.,29.41999998,-91.84995));
#143002=CARTESIAN_POINT('Origin',(-22.5,28.9199999800001,-91.34995));
#143003=CARTESIAN_POINT('Origin',(-60.,28.41999998,-55.24995));
#143004=CARTESIAN_POINT('',(-28.5,28.41999998,-80.9397703408579));
#143005=CARTESIAN_POINT('',(-28.5,28.41999998,-91.34995));
#143006=CARTESIAN_POINT('',(-22.5,28.41999998,-87.1305533863517));
#143007=CARTESIAN_POINT('Ctrl Pts',(-22.5,28.41999998,-87.1305533863517));
#143008=CARTESIAN_POINT('Ctrl Pts',(-22.9996306884463,28.4199999800004,
-86.6629501694543));
#143009=CARTESIAN_POINT('Ctrl Pts',(-23.4925641465851,28.4199999800118,
-86.1891300413705));
#143010=CARTESIAN_POINT('Ctrl Pts',(-23.9796464830031,28.4199999800316,
-85.7094996089126));
#143011=CARTESIAN_POINT('Ctrl Pts',(-24.4984981224756,28.4199999800526,
-85.1985859140088));
#143012=CARTESIAN_POINT('Ctrl Pts',(-25.0107103809229,28.4199999800828,
-84.6810791338099));
#143013=CARTESIAN_POINT('Ctrl Pts',(-25.5172665601457,28.4199999801285,
-84.15742328956));
#143014=CARTESIAN_POINT('Ctrl Pts',(-25.9324040800905,28.419999980166,-83.7282720968532));
#143015=CARTESIAN_POINT('Ctrl Pts',(-26.3437419377233,28.4199999802138,
-83.2949899596838));
#143016=CARTESIAN_POINT('Ctrl Pts',(-26.7518048403012,28.4199999802818,
-82.85780136844));
#143017=CARTESIAN_POINT('Ctrl Pts',(-27.3023421757726,28.4199999803735,
-82.2679691621764));
#143018=CARTESIAN_POINT('Ctrl Pts',(-27.8456527104533,28.4199999804996,
-81.6723376117165));
#143019=CARTESIAN_POINT('Ctrl Pts',(-28.3826963466553,28.4199999807123,
-81.0712589143804));
#143020=CARTESIAN_POINT('Ctrl Pts',(-28.4218307391328,28.4199999807278,
-81.0274582842905));
#143021=CARTESIAN_POINT('Ctrl Pts',(-28.460931835895,28.4199999807438,-80.9836287163303));
#143022=CARTESIAN_POINT('Ctrl Pts',(-28.5,28.4199999807603,-80.9397703408579));
#143023=CARTESIAN_POINT('',(-22.5,28.4199999800001,-87.5942752792638));
#143024=CARTESIAN_POINT('Ctrl Pts',(-28.5,29.41999998,-92.34995));
#143025=CARTESIAN_POINT('Ctrl Pts',(-28.5,28.41999998,-92.34995));
#143026=CARTESIAN_POINT('Ctrl Pts',(-28.5,28.41999998,-91.34995));
#143027=CARTESIAN_POINT('Ctrl Pts',(-29.,29.41999998,-92.34995));
#143028=CARTESIAN_POINT('Ctrl Pts',(-29.,28.41999998,-92.34995));
#143029=CARTESIAN_POINT('Ctrl Pts',(-29.,28.41999998,-91.34995));
#143030=CARTESIAN_POINT('Ctrl Pts',(-29.,29.41999998,-91.84995));
#143031=CARTESIAN_POINT('Ctrl Pts',(-29.,28.91999998,-91.84995));
#143032=CARTESIAN_POINT('Ctrl Pts',(-29.,28.91999998,-91.34995));
#143033=CARTESIAN_POINT('Origin',(-28.5,28.91999998,-91.34995));
#143034=CARTESIAN_POINT('Origin',(-29.5,46.41999998,-92.34995));
#143035=CARTESIAN_POINT('',(-29.5,46.91999998,-58.24995));
#143036=CARTESIAN_POINT('',(-29.5,46.91999998,-58.24995));
#143037=CARTESIAN_POINT('Origin',(-29.5,46.41999998,-58.24995));
#143038=CARTESIAN_POINT('Origin',(39.,46.91999998,-129.34995));
#143039=CARTESIAN_POINT('',(-30.,46.91999998,-58.24995));
#143040=CARTESIAN_POINT('',(-30.,46.91999998,-92.34995));
#143041=CARTESIAN_POINT('',(39.,46.91999998,-58.24995));
#143042=CARTESIAN_POINT('Origin',(-30.,46.41999998,-92.34995));
#143043=CARTESIAN_POINT('Origin',(-30.,46.41999998,-58.24995));
#143044=CARTESIAN_POINT('Ctrl Pts',(-31.,28.41999998,-91.34995));
#143045=CARTESIAN_POINT('Ctrl Pts',(-31.,28.41999998,-92.34995));
#143046=CARTESIAN_POINT('Ctrl Pts',(-31.,29.41999998,-92.34995));
#143047=CARTESIAN_POINT('Ctrl Pts',(-30.5,28.41999998,-91.34995));
#143048=CARTESIAN_POINT('Ctrl Pts',(-30.5,28.41999998,-92.34995));
#143049=CARTESIAN_POINT('Ctrl Pts',(-30.5,29.41999998,-92.34995));
#143050=CARTESIAN_POINT('Ctrl Pts',(-30.5,28.91999998,-91.34995));
#143051=CARTESIAN_POINT('Ctrl Pts',(-30.5,28.91999998,-91.84995));
#143052=CARTESIAN_POINT('Ctrl Pts',(-30.5,29.41999998,-91.84995));
#143053=CARTESIAN_POINT('Origin',(-31.,28.91999998,-91.34995));
#143054=CARTESIAN_POINT('Origin',(-60.,28.41999998,-55.24995));
#143055=CARTESIAN_POINT('',(-37.,28.41999998,-70.4461836365688));
#143056=CARTESIAN_POINT('',(-37.,28.41999998,-91.34995));
#143057=CARTESIAN_POINT('',(-31.,28.41999998,-78.0460091084363));
#143058=CARTESIAN_POINT('Ctrl Pts',(-31.,28.41999998,-78.0460091084363));
#143059=CARTESIAN_POINT('Ctrl Pts',(-31.6054626504327,28.4199999800001,
-77.3245680023291));
#143060=CARTESIAN_POINT('Ctrl Pts',(-32.2037002325589,28.4199999800031,
-76.5972335154354));
#143061=CARTESIAN_POINT('Ctrl Pts',(-32.7954596657072,28.4199999800058,
-75.8646586780361));
#143062=CARTESIAN_POINT('Ctrl Pts',(-33.4345463106021,28.4199999800088,
-75.0734946192274));
#143063=CARTESIAN_POINT('Ctrl Pts',(-34.0660773010423,28.4199999800106,
-74.2762178948229));
#143064=CARTESIAN_POINT('Ctrl Pts',(-34.6909510193196,28.4199999800288,
-73.4736062556181));
#143065=CARTESIAN_POINT('Ctrl Pts',(-34.9391029883029,28.4199999800361,
-73.1548704010415));
#143066=CARTESIAN_POINT('Ctrl Pts',(-35.1862046047006,28.4199999800463,
-72.8352927773724));
#143067=CARTESIAN_POINT('Ctrl Pts',(-35.4323104279066,28.4199999800634,
-72.5149207187905));
#143068=CARTESIAN_POINT('Ctrl Pts',(-35.9594751118247,28.4199999801002,
-71.8286759449022));
#143069=CARTESIAN_POINT('Ctrl Pts',(-36.4818085017622,28.4199999801598,
-71.1391285306312));
#143070=CARTESIAN_POINT('Ctrl Pts',(-37.,28.4199999803545,-70.4461836365688));
#143071=CARTESIAN_POINT('',(-31.,28.41999998,-78.6384479219785));
#143072=CARTESIAN_POINT('Ctrl Pts',(-37.,29.41999998,-92.34995));
#143073=CARTESIAN_POINT('Ctrl Pts',(-37.,28.41999998,-92.34995));
#143074=CARTESIAN_POINT('Ctrl Pts',(-37.,28.41999998,-91.34995));
#143075=CARTESIAN_POINT('Ctrl Pts',(-37.5,29.41999998,-92.34995));
#143076=CARTESIAN_POINT('Ctrl Pts',(-37.5,28.41999998,-92.34995));
#143077=CARTESIAN_POINT('Ctrl Pts',(-37.5,28.41999998,-91.34995));
#143078=CARTESIAN_POINT('Ctrl Pts',(-37.5,29.41999998,-91.84995));
#143079=CARTESIAN_POINT('Ctrl Pts',(-37.5,28.91999998,-91.84995));
#143080=CARTESIAN_POINT('Ctrl Pts',(-37.5,28.91999998,-91.34995));
#143081=CARTESIAN_POINT('Origin',(-37.,28.91999998,-91.34995));
#143082=CARTESIAN_POINT('Origin',(-42.,28.91999998,-92.34995));
#143083=CARTESIAN_POINT('Origin',(-42.,28.91999998,-171.14995));
#143084=CARTESIAN_POINT('Origin',(-42.,58.91999998,-171.14995));
#143085=CARTESIAN_POINT('',(-42.,28.91999998,-171.64995));
#143086=CARTESIAN_POINT('Origin',(-42.,28.91999998,-171.14995));
#143087=CARTESIAN_POINT('Origin',(-42.,30.4123236926243,-171.14995));
#143088=CARTESIAN_POINT('',(-42.,28.91999998,-171.64995));
#143089=CARTESIAN_POINT('Ctrl Pts',(-42.0000617764046,30.4123236926243,
-171.649949996184));
#143090=CARTESIAN_POINT('Ctrl Pts',(-41.5,30.4123236926243,-171.650011780222));
#143091=CARTESIAN_POINT('Ctrl Pts',(-41.5,30.4123236926243,-171.14995));
#143092=CARTESIAN_POINT('Ctrl Pts',(-41.929864311704,30.5683704599569,-171.649958724212));
#143093=CARTESIAN_POINT('Ctrl Pts',(-41.5000000000006,30.5590517401679,
-171.583996757915));
#143094=CARTESIAN_POINT('Ctrl Pts',(-41.5,30.6002163674433,-171.149950044589));
#143095=CARTESIAN_POINT('Ctrl Pts',(-41.8681695534321,30.7453325953812,
-171.649964230513));
#143096=CARTESIAN_POINT('Ctrl Pts',(-41.5,30.7482244616852,-171.547558090571));
#143097=CARTESIAN_POINT('Ctrl Pts',(-41.5,30.7881194136978,-171.167360442076));
#143098=CARTESIAN_POINT('Ctrl Pts',(-41.782059127798,31.1278785851814,-171.649970496006));
#143099=CARTESIAN_POINT('Ctrl Pts',(-41.5,31.1331148272644,-171.511616746684));
#143100=CARTESIAN_POINT('Ctrl Pts',(-41.5,31.1638381213445,-171.199054581264));
#143101=CARTESIAN_POINT('Ctrl Pts',(-41.7580490411456,31.3335084853296,
-171.649971475853));
#143102=CARTESIAN_POINT('Ctrl Pts',(-41.5000000000007,31.3394417200798,
-171.507283264433));
#143103=CARTESIAN_POINT('Ctrl Pts',(-41.5,31.3517239082014,-171.212413163406));
#143104=CARTESIAN_POINT('Ctrl Pts',(-41.7579337455091,31.7458587360553,
-171.649971481651));
#143105=CARTESIAN_POINT('Ctrl Pts',(-41.4999999999994,31.739954085554,-171.507256427626));
#143106=CARTESIAN_POINT('Ctrl Pts',(-41.5,31.72777865723,-171.212471328128));
#143107=CARTESIAN_POINT('Ctrl Pts',(-41.7818539242555,31.9518486363857,
-171.649970508384));
#143108=CARTESIAN_POINT('Ctrl Pts',(-41.5000000000001,31.9466344699074,
-171.511552982749));
#143109=CARTESIAN_POINT('Ctrl Pts',(-41.5,31.9159478899749,-171.199145438258));
#143110=CARTESIAN_POINT('Ctrl Pts',(-41.8680165447745,32.3351574715402,
-171.649964244171));
#143111=CARTESIAN_POINT('Ctrl Pts',(-41.5,32.3322632068598,-171.547472271891));
#143112=CARTESIAN_POINT('Ctrl Pts',(-41.5,32.2923404450921,-171.167401493624));
#143113=CARTESIAN_POINT('Ctrl Pts',(-41.9298158029953,32.5124265790917,
-171.649958730482));
#143114=CARTESIAN_POINT('Ctrl Pts',(-41.5,32.5217552106974,-171.583952704406));
#143115=CARTESIAN_POINT('Ctrl Pts',(-41.5,32.4805522169437,-171.149950046396));
#143116=CARTESIAN_POINT('Ctrl Pts',(-42.0000617764046,32.6685811839606,
-171.649949996184));
#143117=CARTESIAN_POINT('Ctrl Pts',(-41.5,32.6685811839606,-171.650011780222));
#143118=CARTESIAN_POINT('Ctrl Pts',(-41.5,32.6685811839606,-171.14995));
#143119=CARTESIAN_POINT('Origin',(-42.,32.6685811839606,-171.14995));
#143120=CARTESIAN_POINT('Origin',(-42.,58.91999998,-171.14995));
#143121=CARTESIAN_POINT('',(-42.,36.3270340686007,-171.64995));
#143122=CARTESIAN_POINT('Origin',(-42.,36.3270340686007,-171.14995));
#143123=CARTESIAN_POINT('',(-42.,28.91999998,-171.64995));
#143124=CARTESIAN_POINT('Ctrl Pts',(-42.,36.3270340686007,-171.64995));
#143125=CARTESIAN_POINT('Ctrl Pts',(-41.5,36.3270340686007,-171.64995));
#143126=CARTESIAN_POINT('Ctrl Pts',(-41.5,36.3270340686007,-171.14995));
#143127=CARTESIAN_POINT('Ctrl Pts',(-41.9908895000013,36.460524412126,-171.64995));
#143128=CARTESIAN_POINT('Ctrl Pts',(-41.5,36.4592824973649,-171.640924254979));
#143129=CARTESIAN_POINT('Ctrl Pts',(-41.5,36.5253489879757,-171.149950000016));
#143130=CARTESIAN_POINT('Ctrl Pts',(-41.9817858670191,36.5939141376228,
-171.675977326981));
#143131=CARTESIAN_POINT('Ctrl Pts',(-41.5,36.5965520755147,-171.658003579003));
#143132=CARTESIAN_POINT('Ctrl Pts',(-41.5,36.7235144279567,-171.18899099047));
#143133=CARTESIAN_POINT('Ctrl Pts',(-41.9649548930127,36.840527660716,-171.776163607997));
#143134=CARTESIAN_POINT('Ctrl Pts',(-41.5,36.8549873364184,-171.746711574348));
#143135=CARTESIAN_POINT('Ctrl Pts',(-41.5,37.0898865538897,-171.339270411997));
#143136=CARTESIAN_POINT('Ctrl Pts',(-41.9572358131754,36.9536304124011,
-171.850283164392));
#143137=CARTESIAN_POINT('Ctrl Pts',(-41.4999999999986,36.9765510525756,
-171.817687494207));
#143138=CARTESIAN_POINT('Ctrl Pts',(-41.5,37.2579134125323,-171.450449746589));
#143139=CARTESIAN_POINT('Ctrl Pts',(-41.9443539433771,37.1423802312719,
-172.035403273234));
#143140=CARTESIAN_POINT('Ctrl Pts',(-41.5000000000014,37.1809962719461,
-172.003556970024));
#143141=CARTESIAN_POINT('Ctrl Pts',(-41.5,37.5383224977403,-171.728129909852));
#143142=CARTESIAN_POINT('Ctrl Pts',(-41.9391962191204,37.2179530739059,
-172.146331028561));
#143143=CARTESIAN_POINT('Ctrl Pts',(-41.5,37.2645653642152,-172.118296873734));
#143144=CARTESIAN_POINT('Ctrl Pts',(-41.5,37.6505944553831,-171.894521542842));
#143145=CARTESIAN_POINT('Ctrl Pts',(-41.9322246014265,37.3201037397322,
-172.388202106709));
#143146=CARTESIAN_POINT('Ctrl Pts',(-41.5,37.3773763733446,-172.371853931892));
#143147=CARTESIAN_POINT('Ctrl Pts',(-41.5,37.8023507586648,-172.257328160063));
#143148=CARTESIAN_POINT('Ctrl Pts',(-41.9304134495219,37.3466413930076,
-172.51902671195));
#143149=CARTESIAN_POINT('Ctrl Pts',(-41.5,37.4071320584576,-172.511015867074));
#143150=CARTESIAN_POINT('Ctrl Pts',(-41.5,37.8417754273637,-172.453565067926));
#143151=CARTESIAN_POINT('Ctrl Pts',(-41.93041344952,37.3466413930079,-172.64995));
#143152=CARTESIAN_POINT('Ctrl Pts',(-41.5,37.4071320584705,-172.64995));
#143153=CARTESIAN_POINT('Ctrl Pts',(-41.5,37.8417754273786,-172.64995));
#143154=CARTESIAN_POINT('',(-41.93041344952,37.3466413930079,-172.64995));
#143155=CARTESIAN_POINT('Origin',(-42.,37.8417754273786,-172.64995));
#143156=CARTESIAN_POINT('Ctrl Pts',(-41.93041344952,37.3466413930079,-172.64995));
#143157=CARTESIAN_POINT('Ctrl Pts',(-41.9304134495219,37.3466413930076,
-172.51902671195));
#143158=CARTESIAN_POINT('Ctrl Pts',(-41.9322246014265,37.3201037397322,
-172.388202106709));
#143159=CARTESIAN_POINT('Ctrl Pts',(-41.9391962191204,37.2179530739059,
-172.146331028561));
#143160=CARTESIAN_POINT('Ctrl Pts',(-41.9443539433771,37.1423802312719,
-172.035403273234));
#143161=CARTESIAN_POINT('Ctrl Pts',(-41.9572358131754,36.9536304124011,
-171.850283164392));
#143162=CARTESIAN_POINT('Ctrl Pts',(-41.9649548930127,36.840527660716,-171.776163607997));
#143163=CARTESIAN_POINT('Ctrl Pts',(-41.9817858670191,36.5939141376228,
-171.675977326981));
#143164=CARTESIAN_POINT('Ctrl Pts',(-41.9908895000013,36.460524412126,-171.64995));
#143165=CARTESIAN_POINT('Ctrl Pts',(-42.,36.3270340686007,-171.64995));
#143166=CARTESIAN_POINT('Origin',(-42.,37.8417754273786,-171.64995));
#143167=CARTESIAN_POINT('',(-41.93041344952,37.3466413930079,-174.34995));
#143168=CARTESIAN_POINT('Origin',(-42.,37.8417754273786,-174.34995));
#143169=CARTESIAN_POINT('',(-41.93041344952,37.3466413930079,-171.64995));
#143170=CARTESIAN_POINT('Ctrl Pts',(-41.93041344952,37.3466413930079,-174.34995));
#143171=CARTESIAN_POINT('Ctrl Pts',(-41.5,37.4071320584705,-174.34995));
#143172=CARTESIAN_POINT('Ctrl Pts',(-41.5,37.8417754273786,-174.34995));
#143173=CARTESIAN_POINT('Ctrl Pts',(-41.9304134495165,37.3466413930083,
-174.808181527339));
#143174=CARTESIAN_POINT('Ctrl Pts',(-41.4999999999921,37.4071320584705,
-174.750729116851));
#143175=CARTESIAN_POINT('Ctrl Pts',(-41.5,37.8417754273818,-174.742719880575));
#143176=CARTESIAN_POINT('Ctrl Pts',(-41.8393178154807,37.3594440494534,
-175.266067601));
#143177=CARTESIAN_POINT('Ctrl Pts',(-41.418170761701,37.4186324079233,-175.152286591264));
#143178=CARTESIAN_POINT('Ctrl Pts',(-41.4219180279654,37.8545780838243,
-175.135193658002));
#143179=CARTESIAN_POINT('Ctrl Pts',(-41.4886658111382,37.4087249748338,
-176.112616425556));
#143180=CARTESIAN_POINT('Ctrl Pts',(-41.1060831277358,37.4624934645027,
-175.889590467068));
#143181=CARTESIAN_POINT('Ctrl Pts',(-41.1213591671024,37.9038590092046,
-175.860806936189));
#143182=CARTESIAN_POINT('Ctrl Pts',(-41.2292473935486,37.445183855779,-176.500863524274));
#143183=CARTESIAN_POINT('Ctrl Pts',(-40.8743194488686,37.4950657253844,
-176.226515658809));
#143184=CARTESIAN_POINT('Ctrl Pts',(-40.8990005234543,37.9403178901501,
-176.193590163665));
#143185=CARTESIAN_POINT('Ctrl Pts',(-40.5813269737971,37.5362431323916,
-177.148783944032));
#143186=CARTESIAN_POINT('Ctrl Pts',(-40.3016108905592,37.5755546642088,
-176.782638117262));
#143187=CARTESIAN_POINT('Ctrl Pts',(-40.343640163665,38.0313771667621,-176.748950523454));
#143188=CARTESIAN_POINT('Ctrl Pts',(-40.193079875155,37.5908077037056,-177.408202361589));
#143189=CARTESIAN_POINT('Ctrl Pts',(-39.9585494594759,37.6237688040866,
-177.001555340038));
#143190=CARTESIAN_POINT('Ctrl Pts',(-40.0108569362568,38.0859417380754,
-176.971309167074));
#143191=CARTESIAN_POINT('Ctrl Pts',(-39.3465310504406,37.7097823821472,
-177.758854365991));
#143192=CARTESIAN_POINT('Ctrl Pts',(-39.218856185771,37.7277259142,-177.290648705564));
#143193=CARTESIAN_POINT('Ctrl Pts',(-39.2852436579338,38.204916416519,-177.271868027993));
#143194=CARTESIAN_POINT('Ctrl Pts',(-38.8886449769195,37.7741340731185,
-177.849949999987));
#143195=CARTESIAN_POINT('Ctrl Pts',(-38.8208550398785,37.7836613274466,
-177.358977353131));
#143196=CARTESIAN_POINT('Ctrl Pts',(-38.8927698806272,38.2692681074913,
-177.34995));
#143197=CARTESIAN_POINT('Ctrl Pts',(-38.43041344952,37.8385343144662,-177.84995));
#143198=CARTESIAN_POINT('Ctrl Pts',(-38.43041344952,37.8385343144661,-177.34995));
#143199=CARTESIAN_POINT('Ctrl Pts',(-38.5,38.333668348837,-177.34995));
#143200=CARTESIAN_POINT('Ctrl Pts',(-38.43041344952,37.8385343144662,-177.84995));
#143201=CARTESIAN_POINT('Ctrl Pts',(-38.8886449769195,37.7741340731185,
-177.849949999987));
#143202=CARTESIAN_POINT('Ctrl Pts',(-39.3465310504406,37.7097823821472,
-177.758854365991));
#143203=CARTESIAN_POINT('Ctrl Pts',(-39.7698054627978,37.6502950429264,
-177.58352836379));
#143204=CARTESIAN_POINT('Ctrl Pts',(-40.193079875155,37.5908077037056,-177.408202361589));
#143205=CARTESIAN_POINT('Ctrl Pts',(-40.5813269737971,37.5362431323916,
-177.148783944032));
#143206=CARTESIAN_POINT('Ctrl Pts',(-40.9052871836729,37.4907134940853,
-176.824823734153));
#143207=CARTESIAN_POINT('Ctrl Pts',(-41.2292473935486,37.445183855779,-176.500863524274));
#143208=CARTESIAN_POINT('Ctrl Pts',(-41.4886658111382,37.4087249748338,
-176.112616425556));
#143209=CARTESIAN_POINT('Ctrl Pts',(-41.6639918133095,37.3840845121436,
-175.689342013278));
#143210=CARTESIAN_POINT('Ctrl Pts',(-41.8393178154807,37.3594440494534,
-175.266067601));
#143211=CARTESIAN_POINT('Ctrl Pts',(-41.9304134495165,37.3466413930083,
-174.808181527339));
#143212=CARTESIAN_POINT('Ctrl Pts',(-41.93041344952,37.3466413930079,-174.34995));
#143213=CARTESIAN_POINT('Origin',(-45.5612236321975,36.8363642992885,-171.64995));
#143214=CARTESIAN_POINT('',(-44.628608857647,36.9674347581595,-172.64995));
#143215=CARTESIAN_POINT('',(-44.628608857647,36.9674347581595,-171.64995));
#143216=CARTESIAN_POINT('',(-44.628608857647,36.9674347581595,-172.64995));
#143217=CARTESIAN_POINT('Origin',(-44.2110895547669,33.9966305519348,-171.64995));
#143218=CARTESIAN_POINT('',(-46.2674193015002,36.1810087180727,-172.64995));
#143219=CARTESIAN_POINT('',(-46.2674193015002,36.1810087180727,-171.64995));
#143220=CARTESIAN_POINT('Origin',(-44.2110895547669,33.9966305519348,-172.64995));
#143221=CARTESIAN_POINT('Origin',(0.,-12.9675000200281,-171.64995));
#143222=CARTESIAN_POINT('',(-49.1485087381009,33.2999192814719,-172.64995));
#143223=CARTESIAN_POINT('',(-49.1485087381009,33.2999192814719,-171.64995));
#143224=CARTESIAN_POINT('Origin',(0.,-12.9675000200281,-172.64995));
#143225=CARTESIAN_POINT('Origin',(-46.9641305719631,31.2435895347386,-171.64995));
#143226=CARTESIAN_POINT('',(-49.9349347781878,31.6611088376188,-172.64995));
#143227=CARTESIAN_POINT('',(-49.9349347781878,31.6611088376188,-171.64995));
#143228=CARTESIAN_POINT('Origin',(-46.9641305719631,31.2435895347386,-172.64995));
#143229=CARTESIAN_POINT('Origin',(-52.6124803109502,12.6093824234965,-171.64995));
#143230=CARTESIAN_POINT('',(-50.3299522569362,28.85041342952,-172.64995));
#143231=CARTESIAN_POINT('',(-50.3904429223989,28.41999998,-172.64995));
#143232=CARTESIAN_POINT('',(-52.5050296388285,13.3739336825608,-172.133326251627));
#143233=CARTESIAN_POINT('',(-52.5050296388285,13.3739336825608,-171.64995));
#143234=CARTESIAN_POINT('',(-51.9770573602378,17.1306516479033,-172.64995));
#143235=CARTESIAN_POINT('Ctrl Pts',(-51.9770573602378,17.1306516479033,
-172.64995));
#143236=CARTESIAN_POINT('Ctrl Pts',(-52.0505828082768,16.6074909011023,
-172.64994999816));
#143237=CARTESIAN_POINT('Ctrl Pts',(-52.1235483667,16.0883139759212,-172.620408747532));
#143238=CARTESIAN_POINT('Ctrl Pts',(-52.1959928599554,15.5728446220577,
-172.563374785654));
#143239=CARTESIAN_POINT('Ctrl Pts',(-52.2118579788214,15.4599584356367,
-172.550884525264));
#143240=CARTESIAN_POINT('Ctrl Pts',(-52.2276981039084,15.3472500891943,
-172.537075526609));
#143241=CARTESIAN_POINT('Ctrl Pts',(-52.2435136369168,15.2347167244825,
-172.521968983896));
#143242=CARTESIAN_POINT('Ctrl Pts',(-52.2955483171873,14.8644707359723,
-172.472266952379));
#143243=CARTESIAN_POINT('Ctrl Pts',(-52.347327733492,14.4960410449546,-172.409096799907));
#143244=CARTESIAN_POINT('Ctrl Pts',(-52.3987708154505,14.1300044971607,
-172.328180486668));
#143245=CARTESIAN_POINT('Ctrl Pts',(-52.4343604559392,13.8767710467971,
-172.272200510581));
#143246=CARTESIAN_POINT('Ctrl Pts',(-52.4697891103107,13.6246830721773,
-172.207726272012));
#143247=CARTESIAN_POINT('Ctrl Pts',(-52.5050296388285,13.3739336825608,
-172.133326251627));
#143248=CARTESIAN_POINT('',(-51.8267121465167,18.20041342952,-172.64995));
#143249=CARTESIAN_POINT('',(-52.3378926620474,14.5631750666398,-172.64995));
#143250=CARTESIAN_POINT('',(-51.8267121465167,18.20041342952,-176.84995));
#143251=CARTESIAN_POINT('',(-51.8267121465167,18.20041342952,-171.64995));
#143252=CARTESIAN_POINT('',(-51.6861713118143,19.20041342952,-177.84995));
#143253=CARTESIAN_POINT('Ctrl Pts',(-51.6861713118143,19.20041342952,-177.84995));
#143254=CARTESIAN_POINT('Ctrl Pts',(-51.7230681564996,18.9378787379949,
-177.849949999941));
#143255=CARTESIAN_POINT('Ctrl Pts',(-51.7595317568342,18.6784267402051,
-177.742176873059));
#143256=CARTESIAN_POINT('Ctrl Pts',(-51.7855486890661,18.4933066483335,
-177.557056781187));
#143257=CARTESIAN_POINT('Ctrl Pts',(-51.8115656212979,18.3081865564618,
-177.371936689315));
#143258=CARTESIAN_POINT('Ctrl Pts',(-51.8267121465076,18.2004134295853,
-177.112484691526));
#143259=CARTESIAN_POINT('Ctrl Pts',(-51.8267121465167,18.20041342952,-176.84995));
#143260=CARTESIAN_POINT('',(-51.6159008944631,19.70041342952,-177.84995));
#143261=CARTESIAN_POINT('',(-52.6124803109502,12.6093824234965,-177.84995));
#143262=CARTESIAN_POINT('',(-51.4753600597607,20.70041342952,-176.84995));
#143263=CARTESIAN_POINT('Ctrl Pts',(-51.4753600597607,20.70041342952,-176.84995));
#143264=CARTESIAN_POINT('Ctrl Pts',(-51.4753600597699,20.7004134294547,
-177.112484691526));
#143265=CARTESIAN_POINT('Ctrl Pts',(-51.4905065849796,20.5926403025782,
-177.371936689315));
#143266=CARTESIAN_POINT('Ctrl Pts',(-51.5165235172115,20.4075202107065,
-177.557056781187));
#143267=CARTESIAN_POINT('Ctrl Pts',(-51.5425404494433,20.2224001188348,
-177.742176873059));
#143268=CARTESIAN_POINT('Ctrl Pts',(-51.5790040497779,19.9629481210451,
-177.849949999941));
#143269=CARTESIAN_POINT('Ctrl Pts',(-51.6159008944631,19.70041342952,-177.84995));
#143270=CARTESIAN_POINT('',(-51.4753600597607,20.70041342952,-172.64995));
#143271=CARTESIAN_POINT('',(-51.4753600597607,20.70041342952,-171.64995));
#143272=CARTESIAN_POINT('',(-50.6813043436922,26.35041342952,-172.64995));
#143273=CARTESIAN_POINT('',(-51.5358507252234,20.26999998,-172.64995));
#143274=CARTESIAN_POINT('',(-50.6813043436922,26.35041342952,-176.84995));
#143275=CARTESIAN_POINT('',(-50.6813043436922,26.35041342952,-171.64995));
#143276=CARTESIAN_POINT('',(-50.5407635089898,27.3504134295199,-177.84995));
#143277=CARTESIAN_POINT('Ctrl Pts',(-50.5407635089898,27.3504134295199,
-177.84995));
#143278=CARTESIAN_POINT('Ctrl Pts',(-50.5776603536751,27.0878787379949,
-177.849949999941));
#143279=CARTESIAN_POINT('Ctrl Pts',(-50.6141239540097,26.8284267402052,
-177.742176873059));
#143280=CARTESIAN_POINT('Ctrl Pts',(-50.6401408862415,26.6433066483335,
-177.557056781187));
#143281=CARTESIAN_POINT('Ctrl Pts',(-50.6661578184733,26.4581865564618,
-177.371936689315));
#143282=CARTESIAN_POINT('Ctrl Pts',(-50.681304343683,26.3504134295853,-177.112484691526));
#143283=CARTESIAN_POINT('Ctrl Pts',(-50.6813043436922,26.35041342952,-176.84995));
#143284=CARTESIAN_POINT('',(-50.4704930916386,27.85041342952,-177.84995));
#143285=CARTESIAN_POINT('',(-52.6124803109502,12.6093824234965,-177.84995));
#143286=CARTESIAN_POINT('',(-50.3299522569362,28.85041342952,-176.84995));
#143287=CARTESIAN_POINT('Ctrl Pts',(-50.3299522569362,28.85041342952,-176.84995));
#143288=CARTESIAN_POINT('Ctrl Pts',(-50.3299522569454,28.8504134294547,
-177.112484691526));
#143289=CARTESIAN_POINT('Ctrl Pts',(-50.3450987821552,28.7426403025778,
-177.371936689315));
#143290=CARTESIAN_POINT('Ctrl Pts',(-50.3711157143869,28.5575202107065,
-177.557056781187));
#143291=CARTESIAN_POINT('Ctrl Pts',(-50.3971326466187,28.3724001188352,
-177.742176873059));
#143292=CARTESIAN_POINT('Ctrl Pts',(-50.4335962469534,28.1129481210447,
-177.849949999941));
#143293=CARTESIAN_POINT('Ctrl Pts',(-50.4704930916386,27.85041342952,-177.84995));
#143294=CARTESIAN_POINT('',(-50.3299522569362,28.85041342952,-171.64995));
#143295=CARTESIAN_POINT('Origin',(-57.4563699825364,14.0697991873612,-179.64995));
#143296=CARTESIAN_POINT('',(-52.7229737572976,12.4589111791821,-171.855631767295));
#143297=CARTESIAN_POINT('',(-52.7229737572976,12.4589111791821,-176.84995));
#143298=CARTESIAN_POINT('',(-52.7229737572976,12.4589111791821,-179.64995));
#143299=CARTESIAN_POINT('Ctrl Pts',(-52.5050296388285,13.3739336825608,
-172.133326251627));
#143300=CARTESIAN_POINT('Ctrl Pts',(-52.5484527228769,13.0649623850707,
-172.023316132141));
#143301=CARTESIAN_POINT('Ctrl Pts',(-52.6198951421523,12.7615490364788,
-171.918010656511));
#143302=CARTESIAN_POINT('Ctrl Pts',(-52.7229737572976,12.4589111791821,
-171.855638188259));
#143303=CARTESIAN_POINT('',(-52.9322463618642,11.9408779899289,-177.695579616717));
#143304=CARTESIAN_POINT('',(-52.9322463618642,11.9408779899289,-179.64995));
#143305=CARTESIAN_POINT('Ctrl Pts',(-52.7229737572976,12.4589111791821,
-176.84995));
#143306=CARTESIAN_POINT('Ctrl Pts',(-52.7229737689762,12.4589111448658,
-177.021627393075));
#143307=CARTESIAN_POINT('Ctrl Pts',(-52.7396382131267,12.4078638336875,
-177.193608615338));
#143308=CARTESIAN_POINT('Ctrl Pts',(-52.8083222549725,12.2244699412272,
-177.486975267512));
#143309=CARTESIAN_POINT('Ctrl Pts',(-52.8614762873877,12.0912699189313,
-177.610143591528));
#143310=CARTESIAN_POINT('Ctrl Pts',(-52.9322463618642,11.9408779899289,
-177.695579616717));
#143311=CARTESIAN_POINT('Origin',(0.,-12.9675000200281,-179.64995));
#143312=CARTESIAN_POINT('',(-52.9322463618642,-37.8758780299853,-177.801086692062));
#143313=CARTESIAN_POINT('',(-52.9322463618642,-37.8758780299853,-179.64995));
#143314=CARTESIAN_POINT('',(-53.0752347700893,-37.5697245962714,-177.84995));
#143315=CARTESIAN_POINT('Origin',(-53.46537255433,-36.3098838506748,-168.829790838513));
#143316=CARTESIAN_POINT('',(-53.3022372549338,-37.073961884407,-177.84995));
#143317=CARTESIAN_POINT('Origin',(0.,-12.9675000200281,-177.84995));
#143318=CARTESIAN_POINT('',(-53.7396474992599,-36.0824364606782,-176.84995));
#143319=CARTESIAN_POINT('Ctrl Pts',(-53.7396474992599,-36.0824364606782,
-176.84995));
#143320=CARTESIAN_POINT('Ctrl Pts',(-53.7396474962954,-36.0824364675704,
-176.886929243848));
#143321=CARTESIAN_POINT('Ctrl Pts',(-53.7387474700292,-36.084532659728,
-176.923734373979));
#143322=CARTESIAN_POINT('Ctrl Pts',(-53.7370043459075,-36.0885863209691,
-176.960178957691));
#143323=CARTESIAN_POINT('Ctrl Pts',(-53.7352184275947,-36.0927395007421,
-176.997518266259));
#143324=CARTESIAN_POINT('Ctrl Pts',(-53.7325474396826,-36.0989476220765,
-177.034480202452));
#143325=CARTESIAN_POINT('Ctrl Pts',(-53.7290307937802,-36.1071124473775,
-177.070872685112));
#143326=CARTESIAN_POINT('Ctrl Pts',(-53.7254987744608,-36.1153129661398,
-177.107424261644));
#143327=CARTESIAN_POINT('Ctrl Pts',(-53.7211135624651,-36.1254876499985,
-177.143402563608));
#143328=CARTESIAN_POINT('Ctrl Pts',(-53.7158949175065,-36.1375837241684,
-177.178604159826));
#143329=CARTESIAN_POINT('Ctrl Pts',(-53.7124883567771,-36.145479645729,
-177.201582610407));
#143330=CARTESIAN_POINT('Ctrl Pts',(-53.7087262603452,-36.1541952209921,
-177.224229886336));
#143331=CARTESIAN_POINT('Ctrl Pts',(-53.7046098856868,-36.1637255131277,
-177.246483747673));
#143332=CARTESIAN_POINT('Ctrl Pts',(-53.7045192628111,-36.1639353245641,
-177.246973671229));
#143333=CARTESIAN_POINT('Ctrl Pts',(-53.7044284725267,-36.1641455209115,
-177.247463380496));
#143334=CARTESIAN_POINT('Ctrl Pts',(-53.7043375149313,-36.1643561019227,
-177.247952874551));
#143335=CARTESIAN_POINT('Ctrl Pts',(-53.6892733519036,-36.1992319874256,
-177.329021620969));
#143336=CARTESIAN_POINT('Ctrl Pts',(-53.6695548792039,-36.2447904442786,
-177.404845363428));
#143337=CARTESIAN_POINT('Ctrl Pts',(-53.6462229783026,-36.2984391069735,
-177.472877385954));
#143338=CARTESIAN_POINT('Ctrl Pts',(-53.63420658674,-36.3260692319461,-177.507915226417));
#143339=CARTESIAN_POINT('Ctrl Pts',(-53.621231984313,-36.3558446669857,
-177.540885760614));
#143340=CARTESIAN_POINT('Ctrl Pts',(-53.6074429005481,-36.3874074842064,
-177.571437587764));
#143341=CARTESIAN_POINT('Ctrl Pts',(-53.6072249340652,-36.3879064032337,
-177.571920525892));
#143342=CARTESIAN_POINT('Ctrl Pts',(-53.6070067635404,-36.3884057700779,
-177.572402861668));
#143343=CARTESIAN_POINT('Ctrl Pts',(-53.6067883895477,-36.3889055833105,
-177.572884593669));
#143344=CARTESIAN_POINT('Ctrl Pts',(-53.5821747509554,-36.4452411483472,
-177.627182164609));
#143345=CARTESIAN_POINT('Ctrl Pts',(-53.5548118941679,-36.5076136010266,
-177.674313675415));
#143346=CARTESIAN_POINT('Ctrl Pts',(-53.525557578149,-36.573947440761,-177.713411209491));
#143347=CARTESIAN_POINT('Ctrl Pts',(-53.5065780536932,-36.6169833036631,
-177.738776786443));
#143348=CARTESIAN_POINT('Ctrl Pts',(-53.4868028977425,-36.6616853915001,
-177.760761117544));
#143349=CARTESIAN_POINT('Ctrl Pts',(-53.4664703600909,-36.7074778455205,
-177.779132991661));
#143350=CARTESIAN_POINT('Ctrl Pts',(-53.4662816165212,-36.7079029292647,
-177.779303534716));
#143351=CARTESIAN_POINT('Ctrl Pts',(-53.4660928305315,-36.7083280943329,
-177.779473761639));
#143352=CARTESIAN_POINT('Ctrl Pts',(-53.4659040022552,-36.7087533403953,
-177.77964367236));
#143353=CARTESIAN_POINT('Ctrl Pts',(-53.449183813925,-36.7464076281519,
-177.794688766856));
#143354=CARTESIAN_POINT('Ctrl Pts',(-53.4320805422693,-36.7848119006861,
-177.807311664152));
#143355=CARTESIAN_POINT('Ctrl Pts',(-53.414687406387,-36.8237527438975,
-177.817537516946));
#143356=CARTESIAN_POINT('Ctrl Pts',(-53.3964494296165,-36.8645850698633,
-177.828260072498));
#143357=CARTESIAN_POINT('Ctrl Pts',(-53.3778922436238,-36.9060085268256,
-177.836347616446));
#143358=CARTESIAN_POINT('Ctrl Pts',(-53.3591168326372,-36.9477888085125,
-177.841770056554));
#143359=CARTESIAN_POINT('Ctrl Pts',(-53.3414627191038,-36.9870739052215,
-177.846868659901));
#143360=CARTESIAN_POINT('Ctrl Pts',(-53.32361520173,-37.0266755174969,-177.84961057998));
#143361=CARTESIAN_POINT('Ctrl Pts',(-53.3056598276501,-37.0663926738602,
-177.849920463284));
#143362=CARTESIAN_POINT('Ctrl Pts',(-53.3045193956941,-37.0689153010198,
-177.84994014546));
#143363=CARTESIAN_POINT('Ctrl Pts',(-53.3033785305218,-37.0714383891504,
-177.84994999975));
#143364=CARTESIAN_POINT('Ctrl Pts',(-53.3022372549337,-37.073961884407,
-177.84995));
#143365=CARTESIAN_POINT('',(-53.7396474992599,-36.0824364606782,-171.871644662643));
#143366=CARTESIAN_POINT('',(-53.7396474992599,-36.0824364606782,-179.64995));
#143367=CARTESIAN_POINT('',(-55.8171229357418,-30.4803178166104,-171.871644662643));
#143368=CARTESIAN_POINT('Origin',(0.,-12.9675000200281,-171.871644662643));
#143369=CARTESIAN_POINT('',(-55.8171229357418,-30.4803178166104,-176.84995));
#143370=CARTESIAN_POINT('',(-55.8171229357418,-30.4803178166104,-179.64995));
#143371=CARTESIAN_POINT('',(-56.1185967245324,-29.4887923928816,-177.84995));
#143372=CARTESIAN_POINT('Ctrl Pts',(-56.1185967245324,-29.4887923928816,
-177.84995));
#143373=CARTESIAN_POINT('Ctrl Pts',(-56.0810569766533,-29.6163052971279,
-177.849949980253));
#143374=CARTESIAN_POINT('Ctrl Pts',(-56.04332441336,-29.7428150883777,-177.825190994024));
#143375=CARTESIAN_POINT('Ctrl Pts',(-55.9716327345056,-29.9804872937887,
-177.727911302019));
#143376=CARTESIAN_POINT('Ctrl Pts',(-55.9382985315747,-30.0895950523083,
-177.656111307255));
#143377=CARTESIAN_POINT('Ctrl Pts',(-55.8527945813582,-30.367294876883,
-177.382125514336));
#143378=CARTESIAN_POINT('Ctrl Pts',(-55.8171229439391,-30.4803177904842,
-177.121808892945));
#143379=CARTESIAN_POINT('Ctrl Pts',(-55.8171229357418,-30.4803178166104,
-176.84995));
#143380=CARTESIAN_POINT('',(-56.262175563026,-28.9930296810172,-177.84995));
#143381=CARTESIAN_POINT('Origin',(0.,-12.9675000200281,-177.84995));
#143382=CARTESIAN_POINT('',(-56.5169491525423,-28.0699653316567,-177.215087021068));
#143383=CARTESIAN_POINT('Ctrl Pts',(-56.5169491525423,-28.0699653316567,
-177.215087021068));
#143384=CARTESIAN_POINT('Ctrl Pts',(-56.4972682976465,-28.1436156829388,
-177.404470992826));
#143385=CARTESIAN_POINT('Ctrl Pts',(-56.4617523202342,-28.2759697513382,
-177.568612620023));
#143386=CARTESIAN_POINT('Ctrl Pts',(-56.3721096851181,-28.6028436438479,
-177.790491903933));
#143387=CARTESIAN_POINT('Ctrl Pts',(-56.3176963010821,-28.7981083537361,
-177.849949971516));
#143388=CARTESIAN_POINT('Ctrl Pts',(-56.262175563026,-28.9930296810172,
-177.84995));
#143389=CARTESIAN_POINT('',(-56.5351989170821,-28.0015042572884,-176.849882244789));
#143390=CARTESIAN_POINT('Origin',(-55.1126545812022,-33.3251112519863,-176.014041861122));
#143391=CARTESIAN_POINT('',(-56.5351989170821,-28.0015042572884,-171.871644662643));
#143392=CARTESIAN_POINT('',(-56.5351989170821,-28.0015042572884,-179.64995));
#143393=CARTESIAN_POINT('',(-57.7346476057222,-22.3993856132206,-171.871644662643));
#143394=CARTESIAN_POINT('Origin',(0.,-12.9675000200281,-171.871644662643));
#143395=CARTESIAN_POINT('',(-57.7346476057222,-22.3993856132206,-176.657965001855));
#143396=CARTESIAN_POINT('',(-57.7346476057223,-22.3993856132206,-179.64995));
#143397=CARTESIAN_POINT('',(-57.8819282087167,-21.4487963148736,-177.697497252237));
#143398=CARTESIAN_POINT('Ctrl Pts',(-57.8819282087167,-21.4487963148736,
-177.697497252237));
#143399=CARTESIAN_POINT('Ctrl Pts',(-57.8765896421257,-21.4852301944858,
-177.698151252249));
#143400=CARTESIAN_POINT('Ctrl Pts',(-57.8712308062151,-21.5215461998529,
-177.696528688191));
#143401=CARTESIAN_POINT('Ctrl Pts',(-57.8658871784514,-21.5575327106499,
-177.692745867402));
#143402=CARTESIAN_POINT('Ctrl Pts',(-57.8604287549616,-21.5942923100333,
-177.688881781285));
#143403=CARTESIAN_POINT('Ctrl Pts',(-57.8549860188209,-21.630709268616,
-177.682763561799));
#143404=CARTESIAN_POINT('Ctrl Pts',(-57.849594035819,-21.6665701891049,
-177.674461317079));
#143405=CARTESIAN_POINT('Ctrl Pts',(-57.8442188129476,-21.7023196415672,
-177.66618487858));
#143406=CARTESIAN_POINT('Ctrl Pts',(-57.8388938392211,-21.7375177024571,
-177.655737740554));
#143407=CARTESIAN_POINT('Ctrl Pts',(-57.8336539589831,-21.7719470718028,
-177.643138949619));
#143408=CARTESIAN_POINT('Ctrl Pts',(-57.8307658910941,-21.7909235276623,
-177.63619486657));
#143409=CARTESIAN_POINT('Ctrl Pts',(-57.8279036918339,-21.8096662565538,
-177.62859626689));
#143410=CARTESIAN_POINT('Ctrl Pts',(-57.8250735265724,-21.8281360946975,
-177.620340114691));
#143411=CARTESIAN_POINT('Ctrl Pts',(-57.825000507433,-21.8286126222366,
-177.62012710341));
#143412=CARTESIAN_POINT('Ctrl Pts',(-57.8249275065196,-21.8290889901148,
-177.619913645942));
#143413=CARTESIAN_POINT('Ctrl Pts',(-57.8248545239147,-21.8295651979082,
-177.619699742645));
#143414=CARTESIAN_POINT('Ctrl Pts',(-57.8134041423527,-21.9042783566095,
-177.586140042007));
#143415=CARTESIAN_POINT('Ctrl Pts',(-57.8024908179666,-21.9744875656957,
-177.5418492558));
#143416=CARTESIAN_POINT('Ctrl Pts',(-57.7925715206908,-22.0376966071899,
-177.489169880456));
#143417=CARTESIAN_POINT('Ctrl Pts',(-57.7867917707696,-22.074527084434,
-177.458474801256));
#143418=CARTESIAN_POINT('Ctrl Pts',(-57.7813493744914,-22.1089817246166,
-177.424931754286));
#143419=CARTESIAN_POINT('Ctrl Pts',(-57.776333363324,-22.1405749184086,
-177.389003065334));
#143420=CARTESIAN_POINT('Ctrl Pts',(-57.7762581999322,-22.1410483327462,
-177.388464684929));
#143421=CARTESIAN_POINT('Ctrl Pts',(-57.7761831269835,-22.141521141353,
-177.387925738145));
#143422=CARTESIAN_POINT('Ctrl Pts',(-57.7761081445995,-22.1419933437069,
-177.387386226876));
#143423=CARTESIAN_POINT('Ctrl Pts',(-57.7675362470183,-22.1959749590623,
-177.325709935863));
#143424=CARTESIAN_POINT('Ctrl Pts',(-57.7601479409379,-22.2420339156224,
-177.256653403117));
#143425=CARTESIAN_POINT('Ctrl Pts',(-57.7541200519868,-22.2794160573285,
-177.182965839539));
#143426=CARTESIAN_POINT('Ctrl Pts',(-57.7505729125353,-22.3014137534883,
-177.139604048044));
#143427=CARTESIAN_POINT('Ctrl Pts',(-57.7474968850876,-22.3204065587794,
-177.094637483863));
#143428=CARTESIAN_POINT('Ctrl Pts',(-57.7449284196372,-22.3362374915981,
-177.048618868861));
#143429=CARTESIAN_POINT('Ctrl Pts',(-57.7449026192307,-22.3363965143727,
-177.048156608808));
#143430=CARTESIAN_POINT('Ctrl Pts',(-57.7448768691533,-22.3365552239542,
-177.047694236815));
#143431=CARTESIAN_POINT('Ctrl Pts',(-57.7448511693847,-22.3367136204909,
-177.04723175335));
#143432=CARTESIAN_POINT('Ctrl Pts',(-57.7426315058001,-22.3503941726404,
-177.007287514071));
#143433=CARTESIAN_POINT('Ctrl Pts',(-57.740792620676,-22.3617057222206,
-176.966623027288));
#143434=CARTESIAN_POINT('Ctrl Pts',(-57.7393137106679,-22.3707907309251,
-176.925440939058));
#143435=CARTESIAN_POINT('Ctrl Pts',(-57.7377438892451,-22.3804342124164,
-176.881727309435));
#143436=CARTESIAN_POINT('Ctrl Pts',(-57.7365796223128,-22.3875691725098,
-176.837429305389));
#143437=CARTESIAN_POINT('Ctrl Pts',(-57.7358055387825,-22.3923071177908,
-176.792774052489));
#143438=CARTESIAN_POINT('Ctrl Pts',(-57.7350314552522,-22.3970450630717,
-176.748118799589));
#143439=CARTESIAN_POINT('Ctrl Pts',(-57.7346476057222,-22.3993856132206,
-176.703104836952));
#143440=CARTESIAN_POINT('Ctrl Pts',(-57.7346476057222,-22.3993856132206,
-176.657965001855));
#143441=CARTESIAN_POINT('',(-57.9523179894071,-20.9536655363849,-177.688917160843));
#143442=CARTESIAN_POINT('Origin',(-1.12335876835565,-12.9875583193149,-185.751570786959));
#143443=CARTESIAN_POINT('',(-58.0853233553176,-19.9205720538986,-176.438901946458));
#143444=CARTESIAN_POINT('Ctrl Pts',(-58.0853233553176,-19.9205720538986,
-176.438901946458));
#143445=CARTESIAN_POINT('Ctrl Pts',(-58.0853233563387,-19.9205720453688,
-176.739635437133));
#143446=CARTESIAN_POINT('Ctrl Pts',(-58.0755566427899,-20.0041330036795,
-177.044575565272));
#143447=CARTESIAN_POINT('Ctrl Pts',(-58.0411746905458,-20.2805473548039,
-177.404658872083));
#143448=CARTESIAN_POINT('Ctrl Pts',(-58.0268899075637,-20.3936565135702,
-177.503861519498));
#143449=CARTESIAN_POINT('Ctrl Pts',(-57.9924606110737,-20.6579008473032,
-177.646467205152));
#143450=CARTESIAN_POINT('Ctrl Pts',(-57.9732407850675,-20.8018374150098,
-177.686379114698));
#143451=CARTESIAN_POINT('Ctrl Pts',(-57.9523179894071,-20.9536655363849,
-177.688917160843));
#143452=CARTESIAN_POINT('',(-58.0853233553176,-19.9205720538986,-171.871644662643));
#143453=CARTESIAN_POINT('',(-58.0853233553177,-19.9205720538986,-179.64995));
#143454=CARTESIAN_POINT('',(-58.4843989875811,-14.3184534098307,-171.871644662643));
#143455=CARTESIAN_POINT('Origin',(0.,-12.9675000200281,-171.871644662643));
#143456=CARTESIAN_POINT('',(-58.4843989875811,-14.3184534098307,-176.2719717603));
#143457=CARTESIAN_POINT('',(-58.4843989875811,-14.3184534098307,-179.64995));
#143458=CARTESIAN_POINT('',(-58.4988777713114,-13.3298527448197,-177.624285947696));
#143459=CARTESIAN_POINT('Ctrl Pts',(-58.4988777713114,-13.3298527448197,
-177.624285947696));
#143460=CARTESIAN_POINT('Ctrl Pts',(-58.4979165468949,-13.4850345491919,
-177.624397973596));
#143461=CARTESIAN_POINT('Ctrl Pts',(-58.4962883484962,-13.6395668470119,
-177.578389493351));
#143462=CARTESIAN_POINT('Ctrl Pts',(-58.4926597506031,-13.9035447147552,
-177.415964369801));
#143463=CARTESIAN_POINT('Ctrl Pts',(-58.4906864354198,-14.0146226773921,
-177.299459860577));
#143464=CARTESIAN_POINT('Ctrl Pts',(-58.4858850316409,-14.2631520760781,
-176.90254004861));
#143465=CARTESIAN_POINT('Ctrl Pts',(-58.4843989865928,-14.3184534526179,
-176.580946374937));
#143466=CARTESIAN_POINT('Ctrl Pts',(-58.4843989875811,-14.3184534098307,
-176.2719717603));
#143467=CARTESIAN_POINT('',(-58.4998385375645,-12.8300551987823,-177.624173936067));
#143468=CARTESIAN_POINT('Origin',(-0.784469541075961,-12.9675000162872,
-184.352939511374));
#143469=CARTESIAN_POINT('',(-58.48912660861,-11.8396398505087,-176.26629097911));
#143470=CARTESIAN_POINT('Ctrl Pts',(-58.48912660861,-11.8396398505087,-176.26629097911));
#143471=CARTESIAN_POINT('Ctrl Pts',(-58.48912660861,-11.8396398505087,-176.409811534267));
#143472=CARTESIAN_POINT('Ctrl Pts',(-58.4893483896326,-11.8507761032368,
-176.551488494009));
#143473=CARTESIAN_POINT('Ctrl Pts',(-58.4898674690037,-11.8787272918338,
-176.69038150372));
#143474=CARTESIAN_POINT('Ctrl Pts',(-58.4899146582257,-11.8812683191139,
-176.703008191328));
#143475=CARTESIAN_POINT('Ctrl Pts',(-58.4899643050979,-11.8839483504645,
-176.715611866643));
#143476=CARTESIAN_POINT('Ctrl Pts',(-58.4900164667572,-11.8867716762097,
-176.728191820333));
#143477=CARTESIAN_POINT('Ctrl Pts',(-58.4900183886416,-11.8868757010012,
-176.72865532585));
#143478=CARTESIAN_POINT('Ctrl Pts',(-58.4900203139396,-11.886979920305,
-176.72911879896));
#143479=CARTESIAN_POINT('Ctrl Pts',(-58.4900222426542,-11.8870843343361,
-176.729582239632));
#143480=CARTESIAN_POINT('Ctrl Pts',(-58.4904143757935,-11.9083130858161,
-176.82380584864));
#143481=CARTESIAN_POINT('Ctrl Pts',(-58.4909611779826,-11.9381550632,-176.917576442102));
#143482=CARTESIAN_POINT('Ctrl Pts',(-58.491628008076,-11.977637278452,-177.007000513354));
#143483=CARTESIAN_POINT('Ctrl Pts',(-58.4920261001825,-12.0012078377274,
-177.060385951801));
#143484=CARTESIAN_POINT('Ctrl Pts',(-58.4924669768134,-12.0282147910085,
-177.11222193254));
#143485=CARTESIAN_POINT('Ctrl Pts',(-58.4929432955759,-12.0588830464209,
-177.16167335862));
#143486=CARTESIAN_POINT('Ctrl Pts',(-58.4929498715258,-12.0593064454722,
-177.162356073909));
#143487=CARTESIAN_POINT('Ctrl Pts',(-58.4929564542504,-12.0597305436947,
-177.163038337516));
#143488=CARTESIAN_POINT('Ctrl Pts',(-58.4929630437302,-12.0601553416844,
-177.163720147168));
#143489=CARTESIAN_POINT('Ctrl Pts',(-58.4935968230333,-12.1010126145907,
-177.229296924179));
#143490=CARTESIAN_POINT('Ctrl Pts',(-58.4943004033954,-12.1491458631888,
-177.291840545738));
#143491=CARTESIAN_POINT('Ctrl Pts',(-58.4950024041184,-12.2028473374637,
-177.347256942163));
#143492=CARTESIAN_POINT('Ctrl Pts',(-58.4950097920195,-12.203412495261,
-177.347840147912));
#143493=CARTESIAN_POINT('Ctrl Pts',(-58.4950171797681,-12.2039782717463,
-177.348422567924));
#143494=CARTESIAN_POINT('Ctrl Pts',(-58.4950245672806,-12.2045446649403,
-177.349004197405));
#143495=CARTESIAN_POINT('Ctrl Pts',(-58.4957264419677,-12.2583566950054,
-177.404263800622));
#143496=CARTESIAN_POINT('Ctrl Pts',(-58.4964292592559,-12.3178002283294,
-177.452938198818));
#143497=CARTESIAN_POINT('Ctrl Pts',(-58.4970868450185,-12.3836929510146,
-177.494029767074));
#143498=CARTESIAN_POINT('Ctrl Pts',(-58.497092582954,-12.3842679150954,
-177.494388322234));
#143499=CARTESIAN_POINT('Ctrl Pts',(-58.4970983175096,-12.3848433769923,
-177.494746304328));
#143500=CARTESIAN_POINT('Ctrl Pts',(-58.4971040486531,-12.3854193371859,
-177.495103712595));
#143501=CARTESIAN_POINT('Ctrl Pts',(-58.4975789393164,-12.4331442135926,
-177.524719067176));
#143502=CARTESIAN_POINT('Ctrl Pts',(-58.4980179792098,-12.4835732801599,
-177.549749276793));
#143503=CARTESIAN_POINT('Ctrl Pts',(-58.4984026087067,-12.5359391559795,
-177.569640300895));
#143504=CARTESIAN_POINT('Ctrl Pts',(-58.4987756724468,-12.586730397031,
-177.588933204606));
#143505=CARTESIAN_POINT('Ctrl Pts',(-58.4990975247219,-12.6393425576089,
-177.603390836224));
#143506=CARTESIAN_POINT('Ctrl Pts',(-58.4993516232983,-12.6930550657785,
-177.612550490896));
#143507=CARTESIAN_POINT('Ctrl Pts',(-58.4995646774467,-12.7380914168376,
-177.620230590698));
#143508=CARTESIAN_POINT('Ctrl Pts',(-58.4997300980035,-12.7839007001903,
-177.624186575413));
#143509=CARTESIAN_POINT('Ctrl Pts',(-58.4998385375645,-12.8300551987823,
-177.624173936067));
#143510=CARTESIAN_POINT('',(-58.48912660861,-11.8396398505087,-171.871644662643));
#143511=CARTESIAN_POINT('',(-58.48912660861,-11.8396398505087,-179.64995));
#143512=CARTESIAN_POINT('',(-58.1115942404669,-6.23752120644091,-171.871644662643));
#143513=CARTESIAN_POINT('Origin',(0.,-12.9675000200281,-171.871644662643));
#143514=CARTESIAN_POINT('',(-58.1115942404669,-6.2375212064409,-176.427328712824));
#143515=CARTESIAN_POINT('',(-58.1115942404669,-6.2375212064409,-179.64995));
#143516=CARTESIAN_POINT('',(-57.9826110754301,-5.20432973493148,-177.68524973918));
#143517=CARTESIAN_POINT('Ctrl Pts',(-57.9826110754301,-5.20432973493148,
-177.68524973918));
#143518=CARTESIAN_POINT('Ctrl Pts',(-57.9864133803307,-5.2327289015275,
-177.684790303892));
#143519=CARTESIAN_POINT('Ctrl Pts',(-57.9901585317882,-5.26087114190315,
-177.682937908873));
#143520=CARTESIAN_POINT('Ctrl Pts',(-57.9938499513602,-5.28876235919762,
-177.679797008529));
#143521=CARTESIAN_POINT('Ctrl Pts',(-57.9976152499095,-5.31721178304887,
-177.676593247137));
#143522=CARTESIAN_POINT('Ctrl Pts',(-58.0013246616446,-5.34540021247655,
-177.672048874718));
#143523=CARTESIAN_POINT('Ctrl Pts',(-58.0049820412409,-5.37334248086361,
-177.666219172833));
#143524=CARTESIAN_POINT('Ctrl Pts',(-58.007100919411,-5.38953064535377,
-177.662841774415));
#143525=CARTESIAN_POINT('Ctrl Pts',(-58.0092023028963,-5.40563608053654,
-177.659031970271));
#143526=CARTESIAN_POINT('Ctrl Pts',(-58.0112866328471,-5.42166024630091,
-177.654792733909));
#143527=CARTESIAN_POINT('Ctrl Pts',(-58.0127082279004,-5.43258935796885,
-177.651901407879));
#143528=CARTESIAN_POINT('Ctrl Pts',(-58.0141227858996,-5.44348757569482,
-177.648808284626));
#143529=CARTESIAN_POINT('Ctrl Pts',(-58.0155294925106,-5.45434822190654,
-177.64551435811));
#143530=CARTESIAN_POINT('Ctrl Pts',(-58.0189462259725,-5.48072752022011,
-177.637513777987));
#143531=CARTESIAN_POINT('Ctrl Pts',(-58.0223147701654,-5.50687103546867,
-177.628330087141));
#143532=CARTESIAN_POINT('Ctrl Pts',(-58.0256102732283,-5.5325791664003,
-177.618027059099));
#143533=CARTESIAN_POINT('Ctrl Pts',(-58.0292381208968,-5.5608799086786,
-177.606684992183));
#143534=CARTESIAN_POINT('Ctrl Pts',(-58.0327774052011,-5.58865274716566,
-177.593984257917));
#143535=CARTESIAN_POINT('Ctrl Pts',(-58.0361953413916,-5.61562914495262,
-177.580061370298));
#143536=CARTESIAN_POINT('Ctrl Pts',(-58.0369297082255,-5.62142520746788,
-177.577069943211));
#143537=CARTESIAN_POINT('Ctrl Pts',(-58.0376584880584,-5.62718459987921,
-177.574022261851));
#143538=CARTESIAN_POINT('Ctrl Pts',(-58.0383813818279,-5.63290483163266,
-177.570919942798));
#143539=CARTESIAN_POINT('Ctrl Pts',(-58.0384493306635,-5.63344250826457,
-177.570628338449));
#143540=CARTESIAN_POINT('Ctrl Pts',(-58.0385172322329,-5.63397987194777,
-177.570336244847));
#143541=CARTESIAN_POINT('Ctrl Pts',(-58.0385850863885,-5.63451692127423,
-177.570043663697));
#143542=CARTESIAN_POINT('Ctrl Pts',(-58.0490694432021,-5.71749808455882,
-177.524836039379));
#143543=CARTESIAN_POINT('Ctrl Pts',(-58.0585606908555,-5.79407235500368,
-177.467381876561));
#143544=CARTESIAN_POINT('Ctrl Pts',(-58.0668921625487,-5.86215495271816,
-177.400951487675));
#143545=CARTESIAN_POINT('Ctrl Pts',(-58.0716810779971,-5.90128871155089,
-177.362767415605));
#143546=CARTESIAN_POINT('Ctrl Pts',(-58.0760868293938,-5.93761722714578,
-177.321616651462));
#143547=CARTESIAN_POINT('Ctrl Pts',(-58.0800778613687,-5.97074680033053,
-177.278112939551));
#143548=CARTESIAN_POINT('Ctrl Pts',(-58.0801358840197,-5.97122844660027,
-177.27748047138));
#143549=CARTESIAN_POINT('Ctrl Pts',(-58.0801938210413,-5.97170942905892,
-177.276847523818));
#143550=CARTESIAN_POINT('Ctrl Pts',(-58.0802516724784,-5.97218974777175,
-177.276214098177));
#143551=CARTESIAN_POINT('Ctrl Pts',(-58.086346247512,-6.0227907108724,-177.209483515685));
#143552=CARTESIAN_POINT('Ctrl Pts',(-58.0914882451368,-6.06600199005215,
-177.137485615197));
#143553=CARTESIAN_POINT('Ctrl Pts',(-58.0957336562472,-6.10193041985869,
-177.061710183546));
#143554=CARTESIAN_POINT('Ctrl Pts',(-58.0990967930801,-6.1303922631263,
-177.001682276099));
#143555=CARTESIAN_POINT('Ctrl Pts',(-58.1018971540568,-6.15428295037259,
-176.939282520675));
#143556=CARTESIAN_POINT('Ctrl Pts',(-58.1041602520257,-6.17363798086331,
-176.875236987128));
#143557=CARTESIAN_POINT('Ctrl Pts',(-58.1041777800786,-6.17378788864586,
-176.874740944307));
#143558=CARTESIAN_POINT('Ctrl Pts',(-58.1041952749008,-6.1739375157485,
-176.874244853752));
#143559=CARTESIAN_POINT('Ctrl Pts',(-58.104212736516,-6.1740868623495,-176.873748715522));
#143560=CARTESIAN_POINT('Ctrl Pts',(-58.1067717090136,-6.19597337403407,
-176.801040431038));
#143561=CARTESIAN_POINT('Ctrl Pts',(-58.1086155525892,-6.2118188643998,
-176.72738700765));
#143562=CARTESIAN_POINT('Ctrl Pts',(-58.1098212142835,-6.22220604020927,
-176.652935850911));
#143563=CARTESIAN_POINT('Ctrl Pts',(-58.1110268759779,-6.23259321601874,
-176.578484694172));
#143564=CARTESIAN_POINT('Ctrl Pts',(-58.1115942404669,-6.23752120644093,
-176.50323543809));
#143565=CARTESIAN_POINT('Ctrl Pts',(-58.1115942404669,-6.2375212064409,
-176.427328712824));
#143566=CARTESIAN_POINT('',(-57.914127722791,-4.70894021166827,-177.693561815623));
#143567=CARTESIAN_POINT('Origin',(-1.08549480256543,-12.950394379074,-185.613342531869));
#143568=CARTESIAN_POINT('',(-57.7706512256236,-3.75870764711888,-176.647241333324));
#143569=CARTESIAN_POINT('Ctrl Pts',(-57.7706512256236,-3.75870764711888,
-176.647241333324));
#143570=CARTESIAN_POINT('Ctrl Pts',(-57.7706512234859,-3.7587076337082,
-176.91349018761));
#143571=CARTESIAN_POINT('Ctrl Pts',(-57.7839302828914,-3.84070116554495,
-177.179630564281));
#143572=CARTESIAN_POINT('Ctrl Pts',(-57.8378689508709,-4.18900518947036,
-177.581280960616));
#143573=CARTESIAN_POINT('Ctrl Pts',(-57.8761547096863,-4.44264996470081,
-177.698192218067));
#143574=CARTESIAN_POINT('Ctrl Pts',(-57.914127722791,-4.70894021166827,
-177.693561815623));
#143575=CARTESIAN_POINT('',(-57.7706512256236,-3.75870764711888,-171.871644662643));
#143576=CARTESIAN_POINT('',(-57.7706512256236,-3.75870764711888,-179.64995));
#143577=CARTESIAN_POINT('',(-56.5940537057312,1.84341099694893,-171.871644662643));
#143578=CARTESIAN_POINT('Origin',(0.,-12.9675000200281,-171.871644662643));
#143579=CARTESIAN_POINT('',(-56.5940537057312,1.84341099694892,-176.848740272858));
#143580=CARTESIAN_POINT('',(-56.5940537057312,1.84341099694893,-179.64995));
#143581=CARTESIAN_POINT('',(-56.5169491525423,2.13496529160038,-177.558207897086));
#143582=CARTESIAN_POINT('Ctrl Pts',(-56.5169491525423,2.13496529160038,
-177.558207897086));
#143583=CARTESIAN_POINT('Ctrl Pts',(-56.5659347005564,1.95164994081541,
-177.37392715461));
#143584=CARTESIAN_POINT('Ctrl Pts',(-56.5940537017931,1.84341101199667,
-177.116606872607));
#143585=CARTESIAN_POINT('Ctrl Pts',(-56.5940537057312,1.84341099694892,
-176.848740272858));
#143586=CARTESIAN_POINT('',(-56.3252430313217,2.83493642067774,-177.84995));
#143587=CARTESIAN_POINT('Ctrl Pts',(-56.3252430313217,2.83493642067774,
-177.84995));
#143588=CARTESIAN_POINT('Ctrl Pts',(-56.3976379760506,2.57689628418379,
-177.849949962148));
#143589=CARTESIAN_POINT('Ctrl Pts',(-56.4669147992933,2.32220551629932,
-177.746434148089));
#143590=CARTESIAN_POINT('Ctrl Pts',(-56.5169491525423,2.13496529160038,
-177.558207897086));
#143591=CARTESIAN_POINT('',(-56.1837939657261,3.33069913254215,-177.84995));
#143592=CARTESIAN_POINT('Origin',(0.,-12.9675000200281,-177.84995));
#143593=CARTESIAN_POINT('',(-55.8866301012659,4.32222455627096,-176.84995));
#143594=CARTESIAN_POINT('Ctrl Pts',(-55.8866301012659,4.32222455627096,
-176.84995));
#143595=CARTESIAN_POINT('Ctrl Pts',(-55.8866301033422,4.3222245495596,-176.887711783017));
#143596=CARTESIAN_POINT('Ctrl Pts',(-55.8873019941254,4.32005750494367,
-176.925285001291));
#143597=CARTESIAN_POINT('Ctrl Pts',(-55.8886053322676,4.31584578460431,
-176.962497615251));
#143598=CARTESIAN_POINT('Ctrl Pts',(-55.8899346297675,4.31155017693619,
-177.000451414885));
#143599=CARTESIAN_POINT('Ctrl Pts',(-55.8919208352951,4.30512748218138,
-177.038031169975));
#143600=CARTESIAN_POINT('Ctrl Pts',(-55.8945372498695,4.2966554166734,-177.075061157623));
#143601=CARTESIAN_POINT('Ctrl Pts',(-55.8971529093906,4.28818579606139,
-177.112080459038));
#143602=CARTESIAN_POINT('Ctrl Pts',(-55.9003985106906,4.27766770883152,
-177.148551411106));
#143603=CARTESIAN_POINT('Ctrl Pts',(-55.9042621819464,4.26513074059418,
-177.184288779349));
#143604=CARTESIAN_POINT('Ctrl Pts',(-55.9062291959159,4.25874810862931,
-177.202482848646));
#143605=CARTESIAN_POINT('Ctrl Pts',(-55.9083566338582,4.25184146461301,
-177.22048652526));
#143606=CARTESIAN_POINT('Ctrl Pts',(-55.9106442880651,4.24441025685161,
-177.238272995257));
#143607=CARTESIAN_POINT('Ctrl Pts',(-55.9107052688196,4.24421216718633,
-177.238747119518));
#143608=CARTESIAN_POINT('Ctrl Pts',(-55.9107663607186,4.2440137135512,-177.239221068301));
#143609=CARTESIAN_POINT('Ctrl Pts',(-55.9108275637053,4.24381489610749,
-177.239694840879));
#143610=CARTESIAN_POINT('Ctrl Pts',(-55.921455868223,4.20928892853543,-177.321968590922));
#143611=CARTESIAN_POINT('Ctrl Pts',(-55.9354579988732,4.16369334127097,
-177.399293819938));
#143612=CARTESIAN_POINT('Ctrl Pts',(-55.9520401750182,4.10936168614069,
-177.468909678496));
#143613=CARTESIAN_POINT('Ctrl Pts',(-55.9599200188453,4.08354330418918,
-177.50199110813));
#143614=CARTESIAN_POINT('Ctrl Pts',(-55.9683824151876,4.05575233687861,
-177.533330971158));
#143615=CARTESIAN_POINT('Ctrl Pts',(-55.977341715845,4.02624042822255,-177.562628970791));
#143616=CARTESIAN_POINT('Ctrl Pts',(-55.9774917411594,4.02574624530113,
-177.563119571762));
#143617=CARTESIAN_POINT('Ctrl Pts',(-55.9776419059241,4.025251579432,-177.563609601226));
#143618=CARTESIAN_POINT('Ctrl Pts',(-55.9777922097306,4.02475643181778,
-177.564099057738));
#143619=CARTESIAN_POINT('Ctrl Pts',(-55.9952457911948,3.96725889117992,
-177.620935736128));
#143620=CARTESIAN_POINT('Ctrl Pts',(-56.0147502621915,3.90266672703055,
-177.670629519414));
#143621=CARTESIAN_POINT('Ctrl Pts',(-56.035495980374,3.83347839358597,-177.711737746819));
#143622=CARTESIAN_POINT('Ctrl Pts',(-56.0478214929272,3.79237199924909,
-177.73616109859));
#143623=CARTESIAN_POINT('Ctrl Pts',(-56.0605847921298,3.74964437876968,
-177.757554032043));
#143624=CARTESIAN_POINT('Ctrl Pts',(-56.0736137591996,3.70582717944109,
-177.775616713981));
#143625=CARTESIAN_POINT('Ctrl Pts',(-56.0737452759341,3.7053848807584,-177.775799041938));
#143626=CARTESIAN_POINT('Ctrl Pts',(-56.0738768160358,3.70494248350759,
-177.775981025699));
#143627=CARTESIAN_POINT('Ctrl Pts',(-56.0740083793673,3.70449998810519,
-177.776162665075));
#143628=CARTESIAN_POINT('Ctrl Pts',(-56.0854652800848,3.6659662581182,-177.791980326975));
#143629=CARTESIAN_POINT('Ctrl Pts',(-56.0971863579254,3.62638912180277,
-177.805308764985));
#143630=CARTESIAN_POINT('Ctrl Pts',(-56.1090759206044,3.58608423515432,
-177.816113161796));
#143631=CARTESIAN_POINT('Ctrl Pts',(-56.1213067753348,3.54462238943047,
-177.827227700776));
#143632=CARTESIAN_POINT('Ctrl Pts',(-56.1337163559748,3.50238900930299,
-177.835671763787));
#143633=CARTESIAN_POINT('Ctrl Pts',(-56.1462034955942,3.45971409454013,
-177.841352247251));
#143634=CARTESIAN_POINT('Ctrl Pts',(-56.1579134207247,3.41969531745779,
-177.846679170638));
#143635=CARTESIAN_POINT('Ctrl Pts',(-56.1696918925471,3.37928709608612,
-177.849575574952));
#143636=CARTESIAN_POINT('Ctrl Pts',(-56.181452499676,3.33876843673331,-177.849916077404));
#143637=CARTESIAN_POINT('Ctrl Pts',(-56.1822330780449,3.33607912072425,
-177.84993867733));
#143638=CARTESIAN_POINT('Ctrl Pts',(-56.1830135754984,3.33338932446783,
-177.849949999684));
#143639=CARTESIAN_POINT('Ctrl Pts',(-56.1837939657261,3.33069913254215,
-177.84995));
#143640=CARTESIAN_POINT('',(-55.8866301012659,4.32222455627096,-171.871644662643));
#143641=CARTESIAN_POINT('',(-55.8866301012659,4.32222455627096,-179.64995));
#143642=CARTESIAN_POINT('',(-53.8350584096845,9.92434320033876,-171.871644662643));
#143643=CARTESIAN_POINT('Origin',(0.,-12.9675000200281,-171.871644662643));
#143644=CARTESIAN_POINT('',(-53.8350584096845,9.92434320033876,-176.84995));
#143645=CARTESIAN_POINT('',(-53.8350584096845,9.92434320033876,-179.64995));
#143646=CARTESIAN_POINT('',(-53.4025720561307,10.9158686240676,-177.84995));
#143647=CARTESIAN_POINT('Ctrl Pts',(-53.4025720561307,10.9158686240675,
-177.84995));
#143648=CARTESIAN_POINT('Ctrl Pts',(-53.4256992941538,10.8641567398107,
-177.849949993739));
#143649=CARTESIAN_POINT('Ctrl Pts',(-53.4485179803107,10.8129304526923,
-177.845955353724));
#143650=CARTESIAN_POINT('Ctrl Pts',(-53.4709798749292,10.7623159210355,
-177.837971298851));
#143651=CARTESIAN_POINT('Ctrl Pts',(-53.4932283385007,10.7121823244318,
-177.8300631078));
#143652=CARTESIAN_POINT('Ctrl Pts',(-53.5151269426185,10.6626484619086,
-177.818240932981));
#143653=CARTESIAN_POINT('Ctrl Pts',(-53.5366259143442,10.6138407725573,
-177.80245915115));
#143654=CARTESIAN_POINT('Ctrl Pts',(-53.5459258227763,10.5927278073634,
-177.795632353673));
#143655=CARTESIAN_POINT('Ctrl Pts',(-53.5551508985509,10.5717508130022,
-177.788063986787));
#143656=CARTESIAN_POINT('Ctrl Pts',(-53.5642968110718,10.5509205718341,
-177.77974738364));
#143657=CARTESIAN_POINT('Ctrl Pts',(-53.5644850520156,10.5504918443291,
-177.779576211522));
#143658=CARTESIAN_POINT('Ctrl Pts',(-53.5646732319863,10.5500632415521,
-177.779404746864));
#143659=CARTESIAN_POINT('Ctrl Pts',(-53.5648613509312,10.5496347636521,
-177.779232989633));
#143660=CARTESIAN_POINT('Ctrl Pts',(-53.5997722939231,10.4701182239962,
-177.747358438588));
#143661=CARTESIAN_POINT('Ctrl Pts',(-53.6324973478398,10.3950941639657,
-177.70548367066));
#143662=CARTESIAN_POINT('Ctrl Pts',(-53.6625657515364,10.3258245179381,
-177.65369711681));
#143663=CARTESIAN_POINT('Ctrl Pts',(-53.6768635990427,10.2928860604893,
-177.629072056654));
#143664=CARTESIAN_POINT('Ctrl Pts',(-53.6905609342834,10.2612483121633,
-177.602206386714));
#143665=CARTESIAN_POINT('Ctrl Pts',(-53.7036082895117,10.2310442594454,
-177.573112646646));
#143666=CARTESIAN_POINT('Ctrl Pts',(-53.7038266840866,10.2305386856232,
-177.572625657913));
#143667=CARTESIAN_POINT('Ctrl Pts',(-53.7040448535835,10.2300336133805,
-177.572138119876));
#143668=CARTESIAN_POINT('Ctrl Pts',(-53.7042627976345,10.2295290436849,
-177.571650033405));
#143669=CARTESIAN_POINT('Ctrl Pts',(-53.7326736221947,10.1637541760739,
-177.508023891499));
#143670=CARTESIAN_POINT('Ctrl Pts',(-53.757265528039,10.106491327388,-177.435049789273));
#143671=CARTESIAN_POINT('Ctrl Pts',(-53.777230163758,10.059865738004,-177.354607724318));
#143672=CARTESIAN_POINT('Ctrl Pts',(-53.7856960958566,10.0400943242234,
-177.320496555482));
#143673=CARTESIAN_POINT('Ctrl Pts',(-53.7933301997471,10.0222350963628,
-177.28504246554));
#143674=CARTESIAN_POINT('Ctrl Pts',(-53.8000719149495,10.0064474410941,
-177.248388344963));
#143675=CARTESIAN_POINT('Ctrl Pts',(-53.8001626051629,10.0062350640087,
-177.247895270142));
#143676=CARTESIAN_POINT('Ctrl Pts',(-53.8002531267728,10.0060230790139,
-177.247402027608));
#143677=CARTESIAN_POINT('Ctrl Pts',(-53.800343479687,10.0058114863479,-177.246908617746));
#143678=CARTESIAN_POINT('Ctrl Pts',(-53.8073717082883,9.989352453007,-177.208528037134));
#143679=CARTESIAN_POINT('Ctrl Pts',(-53.8133972227366,9.97522506645285,
-177.169027476767));
#143680=CARTESIAN_POINT('Ctrl Pts',(-53.8183528652338,9.96359686430567,
-177.128668162154));
#143681=CARTESIAN_POINT('Ctrl Pts',(-53.8232487909443,9.95210878503223,
-177.088795187826));
#143682=CARTESIAN_POINT('Ctrl Pts',(-53.8271003741327,9.9430602856234,-177.048084581928));
#143683=CARTESIAN_POINT('Ctrl Pts',(-53.829861825915,9.93656859429005,-177.006803377711));
#143684=CARTESIAN_POINT('Ctrl Pts',(-53.8325710248907,9.93019974018784,
-176.966303305646));
#143685=CARTESIAN_POINT('Ctrl Pts',(-53.8342309082794,9.92629199069107,
-176.925254528035));
#143686=CARTESIAN_POINT('Ctrl Pts',(-53.8348176649726,9.92491022336673,
-176.883916088102));
#143687=CARTESIAN_POINT('Ctrl Pts',(-53.8349780875801,9.9245324403442,-176.872613924192));
#143688=CARTESIAN_POINT('Ctrl Pts',(-53.8350584093113,9.92434320121651,
-176.861290124361));
#143689=CARTESIAN_POINT('Ctrl Pts',(-53.8350584096845,9.92434320033876,
-176.84995));
#143690=CARTESIAN_POINT('',(-53.1780777607544,11.411631335932,-177.84995));
#143691=CARTESIAN_POINT('Origin',(0.,-12.9675000200281,-177.84995));
#143692=CARTESIAN_POINT('Ctrl Pts',(-52.9322463618642,11.9408779899289,
-177.695579616717));
#143693=CARTESIAN_POINT('Ctrl Pts',(-53.0073952368163,11.7811807683279,
-177.797243661242));
#143694=CARTESIAN_POINT('Ctrl Pts',(-53.092575147757,11.598137759657,-177.849949986084));
#143695=CARTESIAN_POINT('Ctrl Pts',(-53.1780777607544,11.411631335932,-177.84995));
#143696=CARTESIAN_POINT('Origin',(-57.4563699825363,-40.0047992274175,-179.64995));
#143697=CARTESIAN_POINT('',(-52.5050296388285,-39.3089337226171,-172.133326251627));
#143698=CARTESIAN_POINT('',(-52.5050296388285,-39.3089337226171,-171.64995));
#143699=CARTESIAN_POINT('',(-52.6451348158797,-38.6439112191206,-171.916267709118));
#143700=CARTESIAN_POINT('Ctrl Pts',(-52.6451348158641,-38.6439112191758,
-171.916267709546));
#143701=CARTESIAN_POINT('Ctrl Pts',(-52.5828776664721,-38.8638072188231,
-171.976552511458));
#143702=CARTESIAN_POINT('Ctrl Pts',(-52.5365289707088,-39.0848043302806,
-172.053524336593));
#143703=CARTESIAN_POINT('Ctrl Pts',(-52.5050296388285,-39.3089337226171,
-172.133326251627));
#143704=CARTESIAN_POINT('',(-52.6451348158641,-38.6439112191758,-176.84995));
#143705=CARTESIAN_POINT('',(-52.6451348158641,-38.6439112191758,-179.64995));
#143706=CARTESIAN_POINT('Ctrl Pts',(-52.9322463618642,-37.8758780299853,
-177.801086692062));
#143707=CARTESIAN_POINT('Ctrl Pts',(-52.8342434317084,-38.0841419017282,
-177.740238340822));
#143708=CARTESIAN_POINT('Ctrl Pts',(-52.7606534316743,-38.2807615372527,
-177.619039957031));
#143709=CARTESIAN_POINT('Ctrl Pts',(-52.6665978216312,-38.5625293047724,
-177.280964618108));
#143710=CARTESIAN_POINT('Ctrl Pts',(-52.6451348250506,-38.6439111866979,
-177.06710203648));
#143711=CARTESIAN_POINT('Ctrl Pts',(-52.6451348158641,-38.6439112191758,
-176.84995));
#143712=CARTESIAN_POINT('Origin',(-52.6124803109501,-38.5443824635529,-171.64995));
#143713=CARTESIAN_POINT('',(-51.4437383719606,-46.86041346952,-172.64995));
#143714=CARTESIAN_POINT('',(-50.6496826558921,-52.51041346952,-172.64995));
#143715=CARTESIAN_POINT('',(-50.5696324866523,-53.08000002,-172.64995));
#143716=CARTESIAN_POINT('',(-51.4437383719606,-46.86041346952,-176.84995));
#143717=CARTESIAN_POINT('',(-51.4437383719606,-46.86041346952,-171.64995));
#143718=CARTESIAN_POINT('',(-51.584279206663,-45.86041346952,-177.84995));
#143719=CARTESIAN_POINT('Ctrl Pts',(-51.584279206663,-45.86041346952,-177.84995));
#143720=CARTESIAN_POINT('Ctrl Pts',(-51.5473823619777,-46.1229481610447,
-177.849949999941));
#143721=CARTESIAN_POINT('Ctrl Pts',(-51.5109187616431,-46.3824001588352,
-177.742176873059));
#143722=CARTESIAN_POINT('Ctrl Pts',(-51.4849018294113,-46.5675202507065,
-177.557056781187));
#143723=CARTESIAN_POINT('Ctrl Pts',(-51.4588848971795,-46.7526403425778,
-177.371936689315));
#143724=CARTESIAN_POINT('Ctrl Pts',(-51.4437383719698,-46.8604134694541,
-177.112484691526));
#143725=CARTESIAN_POINT('Ctrl Pts',(-51.4437383719606,-46.86041346952,-176.84995));
#143726=CARTESIAN_POINT('',(-51.6545496240141,-45.3604134695199,-177.84995));
#143727=CARTESIAN_POINT('',(-52.6124803109501,-38.5443824635529,-177.84995));
#143728=CARTESIAN_POINT('',(-51.7950904587165,-44.36041346952,-176.84995));
#143729=CARTESIAN_POINT('Ctrl Pts',(-51.7950904587165,-44.36041346952,-176.84995));
#143730=CARTESIAN_POINT('Ctrl Pts',(-51.7950904587073,-44.3604134695857,
-177.112484691526));
#143731=CARTESIAN_POINT('Ctrl Pts',(-51.7799439334977,-44.4681865964612,
-177.371936689315));
#143732=CARTESIAN_POINT('Ctrl Pts',(-51.7539270012658,-44.6533066883334,
-177.557056781187));
#143733=CARTESIAN_POINT('Ctrl Pts',(-51.7279100690339,-44.8384267802056,
-177.742176873059));
#143734=CARTESIAN_POINT('Ctrl Pts',(-51.6914464686995,-45.0978787779945,
-177.849949999941));
#143735=CARTESIAN_POINT('Ctrl Pts',(-51.6545496240141,-45.3604134695199,
-177.84995));
#143736=CARTESIAN_POINT('',(-51.7950904587165,-44.36041346952,-172.64995));
#143737=CARTESIAN_POINT('',(-51.7950904587165,-44.36041346952,-171.64995));
#143738=CARTESIAN_POINT('',(-51.9770573602378,-43.0656516879596,-172.64995));
#143739=CARTESIAN_POINT('',(-51.7150402894768,-44.93000002,-172.64995));
#143740=CARTESIAN_POINT('Ctrl Pts',(-52.5050296388285,-39.3089337226171,
-172.133326251627));
#143741=CARTESIAN_POINT('Ctrl Pts',(-52.4540911811657,-39.671379681976,
-172.240867836498));
#143742=CARTESIAN_POINT('Ctrl Pts',(-52.4027597205576,-40.0366220025921,
-172.327673864957));
#143743=CARTESIAN_POINT('Ctrl Pts',(-52.3511170282707,-40.4040788516728,
-172.398058085082));
#143744=CARTESIAN_POINT('Ctrl Pts',(-52.3153892921749,-40.6582949033385,
-172.446751689745));
#143745=CARTESIAN_POINT('Ctrl Pts',(-52.2795125603002,-40.913571115058,
-172.487583846607));
#143746=CARTESIAN_POINT('Ctrl Pts',(-52.2435136369167,-41.1697167645394,
-172.521968983892));
#143747=CARTESIAN_POINT('Ctrl Pts',(-52.1712955694628,-41.6835750151102,
-172.590949606935));
#143748=CARTESIAN_POINT('Ctrl Pts',(-52.0985648108884,-42.2010812525561,
-172.632879273597));
#143749=CARTESIAN_POINT('Ctrl Pts',(-52.0252827479205,-42.7225102245918,
-172.645720761145));
#143750=CARTESIAN_POINT('Ctrl Pts',(-52.0092341999975,-42.8367015765715,
-172.648533007688));
#143751=CARTESIAN_POINT('Ctrl Pts',(-51.9931592080461,-42.9510810875898,
-172.649949999597));
#143752=CARTESIAN_POINT('Ctrl Pts',(-51.9770573602378,-43.0656516879596,
-172.64995));
#143753=CARTESIAN_POINT('',(-49.9349347781878,-57.596108877675,-172.64995));
#143754=CARTESIAN_POINT('',(-49.9349347781878,-57.596108877675,-171.64995));
#143755=CARTESIAN_POINT('',(-50.2983305691361,-55.0104134695199,-172.64995));
#143756=CARTESIAN_POINT('',(-49.9349347781878,-57.596108877675,-172.64995));
#143757=CARTESIAN_POINT('',(-50.2983305691361,-55.0104134695199,-176.84995));
#143758=CARTESIAN_POINT('',(-50.2983305691361,-55.0104134695199,-171.64995));
#143759=CARTESIAN_POINT('',(-50.4388714038385,-54.0104134695199,-177.84995));
#143760=CARTESIAN_POINT('Ctrl Pts',(-50.4388714038385,-54.0104134695199,
-177.84995));
#143761=CARTESIAN_POINT('Ctrl Pts',(-50.4019745591532,-54.2729481610447,
-177.849949999941));
#143762=CARTESIAN_POINT('Ctrl Pts',(-50.3655109588186,-54.5324001588352,
-177.742176873059));
#143763=CARTESIAN_POINT('Ctrl Pts',(-50.3394940265868,-54.7175202507064,
-177.557056781187));
#143764=CARTESIAN_POINT('Ctrl Pts',(-50.313477094355,-54.9026403425777,
-177.371936689315));
#143765=CARTESIAN_POINT('Ctrl Pts',(-50.2983305691453,-55.0104134694541,
-177.112484691526));
#143766=CARTESIAN_POINT('Ctrl Pts',(-50.2983305691361,-55.0104134695199,
-176.84995));
#143767=CARTESIAN_POINT('',(-50.5091418211897,-53.5104134695199,-177.84995));
#143768=CARTESIAN_POINT('',(-52.6124803109501,-38.5443824635529,-177.84995));
#143769=CARTESIAN_POINT('',(-50.6496826558921,-52.51041346952,-176.84995));
#143770=CARTESIAN_POINT('Ctrl Pts',(-50.6496826558921,-52.51041346952,-176.84995));
#143771=CARTESIAN_POINT('Ctrl Pts',(-50.6496826558828,-52.5104134695858,
-177.112484691526));
#143772=CARTESIAN_POINT('Ctrl Pts',(-50.6345361306733,-52.6181865964613,
-177.371936689314));
#143773=CARTESIAN_POINT('Ctrl Pts',(-50.6085191984413,-52.8033066883334,
-177.557056781187));
#143774=CARTESIAN_POINT('Ctrl Pts',(-50.5825022662094,-52.9884267802056,
-177.742176873059));
#143775=CARTESIAN_POINT('Ctrl Pts',(-50.546038665875,-53.2478787779945,
-177.849949999941));
#143776=CARTESIAN_POINT('Ctrl Pts',(-50.5091418211897,-53.5104134695199,
-177.84995));
#143777=CARTESIAN_POINT('',(-50.6496826558921,-52.51041346952,-171.64995));
#143778=CARTESIAN_POINT('Origin',(-46.9641305719631,-57.1785895747948,-171.64995));
#143779=CARTESIAN_POINT('',(-49.148508738101,-59.2349193215281,-172.64995));
#143780=CARTESIAN_POINT('',(-49.148508738101,-59.2349193215281,-171.64995));
#143781=CARTESIAN_POINT('Origin',(-46.9641305719631,-57.1785895747948,-172.64995));
#143782=CARTESIAN_POINT('Origin',(0.,-12.9675000200281,-171.64995));
#143783=CARTESIAN_POINT('',(-46.2674193015002,-62.1160087581289,-172.64995));
#143784=CARTESIAN_POINT('',(-46.2674193015002,-62.1160087581289,-171.64995));
#143785=CARTESIAN_POINT('Origin',(0.,-12.9675000200281,-172.64995));
#143786=CARTESIAN_POINT('Origin',(-44.2110895547669,-59.9316305919911,-171.64995));
#143787=CARTESIAN_POINT('',(-44.628608857647,-62.9024347982158,-172.64995));
#143788=CARTESIAN_POINT('',(-44.628608857647,-62.9024347982158,-171.64995));
#143789=CARTESIAN_POINT('Origin',(-44.2110895547669,-59.9316305919911,-172.64995));
#143790=CARTESIAN_POINT('Origin',(-45.5612236321975,-62.7713643393447,-171.64995));
#143791=CARTESIAN_POINT('',(-41.9304134495199,-63.2816414330641,-172.64995));
#143792=CARTESIAN_POINT('',(-41.5,-63.3421320985267,-172.64995));
#143793=CARTESIAN_POINT('',(-30.098151667932,-64.9445573802656,-172.64995));
#143794=CARTESIAN_POINT('Ctrl Pts',(-30.098151667932,-64.9445573802656,
-172.64995));
#143795=CARTESIAN_POINT('Ctrl Pts',(-29.5972390118835,-65.0149560630596,
-172.649949998196));
#143796=CARTESIAN_POINT('Ctrl Pts',(-29.1003075629514,-65.0847952236824,
-172.623020954979));
#143797=CARTESIAN_POINT('Ctrl Pts',(-28.6071269714123,-65.1541072356763,
-172.570721117616));
#143798=CARTESIAN_POINT('Ctrl Pts',(-28.4194541760847,-65.1804829269826,
-172.550819165184));
#143799=CARTESIAN_POINT('Ctrl Pts',(-28.2323246108402,-65.2067822722795,
-172.527242787946));
#143800=CARTESIAN_POINT('Ctrl Pts',(-28.0457258647366,-65.2330070158113,
-172.500075926044));
#143801=CARTESIAN_POINT('Ctrl Pts',(-27.7072474293089,-65.2805770576551,
-172.450796940499));
#143802=CARTESIAN_POINT('Ctrl Pts',(-27.3705571686055,-65.3278957879305,
-172.389422697018));
#143803=CARTESIAN_POINT('Ctrl Pts',(-27.0359780488069,-65.3749178167011,
-172.313768645042));
#143804=CARTESIAN_POINT('Ctrl Pts',(-26.7013989290084,-65.4219398454716,
-172.238114593065));
#143805=CARTESIAN_POINT('Ctrl Pts',(-26.3688785032062,-65.4686725436693,
-172.14853549193));
#143806=CARTESIAN_POINT('Ctrl Pts',(-26.0394480946395,-65.5149709682656,
-172.038055421481));
#143807=CARTESIAN_POINT('',(-31.28041344952,-64.7784013226445,-172.64995));
#143808=CARTESIAN_POINT('',(-27.530675086669,-65.3053926820751,-172.64995));
#143809=CARTESIAN_POINT('',(-31.28041344952,-64.7784013226445,-176.84995));
#143810=CARTESIAN_POINT('',(-31.28041344952,-64.7784013226445,-171.64995));
#143811=CARTESIAN_POINT('',(-32.28041344952,-64.6378604879421,-177.84995));
#143812=CARTESIAN_POINT('Ctrl Pts',(-32.28041344952,-64.6378604879421,-177.84995));
#143813=CARTESIAN_POINT('Ctrl Pts',(-32.0178787579952,-64.6747573326273,
-177.849949999941));
#143814=CARTESIAN_POINT('Ctrl Pts',(-31.7584267602047,-64.711220932962,
-177.742176873059));
#143815=CARTESIAN_POINT('Ctrl Pts',(-31.5733066683334,-64.7372378651937,
-177.557056781187));
#143816=CARTESIAN_POINT('Ctrl Pts',(-31.3881865764622,-64.7632547974255,
-177.371936689315));
#143817=CARTESIAN_POINT('Ctrl Pts',(-31.2804134495858,-64.7784013226352,
-177.112484691526));
#143818=CARTESIAN_POINT('Ctrl Pts',(-31.28041344952,-64.7784013226445,-176.84995));
#143819=CARTESIAN_POINT('',(-32.7804134495199,-64.5675900705909,-177.84995));
#143820=CARTESIAN_POINT('',(-45.5612236321975,-62.7713643393447,-177.84995));
#143821=CARTESIAN_POINT('',(-33.7804134495199,-64.4270492358885,-176.84995));
#143822=CARTESIAN_POINT('Ctrl Pts',(-33.7804134495199,-64.4270492358885,
-176.84995));
#143823=CARTESIAN_POINT('Ctrl Pts',(-33.7804134494542,-64.4270492358978,
-177.112484691526));
#143824=CARTESIAN_POINT('Ctrl Pts',(-33.6726403225778,-64.4421957611075,
-177.371936689315));
#143825=CARTESIAN_POINT('Ctrl Pts',(-33.4875202307065,-64.4682126933392,
-177.557056781187));
#143826=CARTESIAN_POINT('Ctrl Pts',(-33.3024001388352,-64.494229625571,
-177.742176873059));
#143827=CARTESIAN_POINT('Ctrl Pts',(-33.0429481410447,-64.5306932259057,
-177.849949999941));
#143828=CARTESIAN_POINT('Ctrl Pts',(-32.7804134495199,-64.5675900705909,
-177.84995));
#143829=CARTESIAN_POINT('',(-33.7804134495199,-64.4270492358885,-172.64995));
#143830=CARTESIAN_POINT('',(-33.7804134495199,-64.4270492358885,-171.64995));
#143831=CARTESIAN_POINT('',(-39.43041344952,-63.6329935198201,-172.64995));
#143832=CARTESIAN_POINT('',(-33.35,-64.4875399013512,-172.64995));
#143833=CARTESIAN_POINT('',(-39.43041344952,-63.63299351982,-176.84995));
#143834=CARTESIAN_POINT('',(-39.43041344952,-63.63299351982,-171.64995));
#143835=CARTESIAN_POINT('',(-40.4304134495199,-63.4924526851176,-177.84995));
#143836=CARTESIAN_POINT('Ctrl Pts',(-40.4304134495199,-63.4924526851176,
-177.84995));
#143837=CARTESIAN_POINT('Ctrl Pts',(-40.1678787579952,-63.5293495298029,
-177.849949999941));
#143838=CARTESIAN_POINT('Ctrl Pts',(-39.9084267602046,-63.5658131301376,
-177.742176873059));
#143839=CARTESIAN_POINT('Ctrl Pts',(-39.7233066683334,-63.5918300623693,
-177.557056781187));
#143840=CARTESIAN_POINT('Ctrl Pts',(-39.5381865764622,-63.6178469946011,
-177.371936689315));
#143841=CARTESIAN_POINT('Ctrl Pts',(-39.4304134495858,-63.6329935198108,
-177.112484691526));
#143842=CARTESIAN_POINT('Ctrl Pts',(-39.43041344952,-63.63299351982,-176.84995));
#143843=CARTESIAN_POINT('',(-40.9304134495199,-63.4221822677665,-177.84995));
#143844=CARTESIAN_POINT('',(-45.5612236321975,-62.7713643393447,-177.84995));
#143845=CARTESIAN_POINT('',(-41.9304134495199,-63.2816414330641,-176.84995));
#143846=CARTESIAN_POINT('Ctrl Pts',(-41.9304134495199,-63.2816414330641,
-176.84995));
#143847=CARTESIAN_POINT('Ctrl Pts',(-41.9304134494542,-63.2816414330733,
-177.112484691526));
#143848=CARTESIAN_POINT('Ctrl Pts',(-41.8226403225787,-63.2967879582829,
-177.371936689315));
#143849=CARTESIAN_POINT('Ctrl Pts',(-41.6375202307065,-63.3228048905148,
-177.557056781187));
#143850=CARTESIAN_POINT('Ctrl Pts',(-41.4524001388343,-63.3488218227467,
-177.742176873059));
#143851=CARTESIAN_POINT('Ctrl Pts',(-41.1929481410454,-63.3852854230811,
-177.849949999941));
#143852=CARTESIAN_POINT('Ctrl Pts',(-40.9304134495199,-63.4221822677665,
-177.84995));
#143853=CARTESIAN_POINT('',(-41.9304134495199,-63.2816414330641,-171.64995));
#143854=CARTESIAN_POINT('Ctrl Pts',(-42.0000617764046,-58.6035812240168,
-171.649949996184));
#143855=CARTESIAN_POINT('Ctrl Pts',(-41.5,-58.6035812240167,-171.650011780221));
#143856=CARTESIAN_POINT('Ctrl Pts',(-41.5,-58.6035812240168,-171.14995));
#143857=CARTESIAN_POINT('Ctrl Pts',(-41.9298643117037,-58.4475344566842,
-171.649958724212));
#143858=CARTESIAN_POINT('Ctrl Pts',(-41.5,-58.4568531764746,-171.583996757909));
#143859=CARTESIAN_POINT('Ctrl Pts',(-41.5,-58.415688549198,-171.149950044589));
#143860=CARTESIAN_POINT('Ctrl Pts',(-41.8681695534326,-58.2705723212599,
-171.649964230513));
#143861=CARTESIAN_POINT('Ctrl Pts',(-41.5,-58.2676804549564,-171.547558090573));
#143862=CARTESIAN_POINT('Ctrl Pts',(-41.5,-58.227785502943,-171.167360442076));
#143863=CARTESIAN_POINT('Ctrl Pts',(-41.7820591277973,-57.8880263314597,
-171.649970496006));
#143864=CARTESIAN_POINT('Ctrl Pts',(-41.5,-57.8827900893765,-171.511616746682));
#143865=CARTESIAN_POINT('Ctrl Pts',(-41.5,-57.8520667952971,-171.199054581264));
#143866=CARTESIAN_POINT('Ctrl Pts',(-41.7580490411456,-57.6823964313123,
-171.649971475853));
#143867=CARTESIAN_POINT('Ctrl Pts',(-41.4999999999974,-57.6764631965623,
-171.507283264427));
#143868=CARTESIAN_POINT('Ctrl Pts',(-41.5,-57.6641810084405,-171.212413163406));
#143869=CARTESIAN_POINT('Ctrl Pts',(-41.7579337455091,-57.2700461805852,
-171.649971481651));
#143870=CARTESIAN_POINT('Ctrl Pts',(-41.5000000000026,-57.275950831087,
-171.507256427632));
#143871=CARTESIAN_POINT('Ctrl Pts',(-41.5,-57.2881262594105,-171.212471328128));
#143872=CARTESIAN_POINT('Ctrl Pts',(-41.7818539242554,-57.0640562802561,
-171.649970508384));
#143873=CARTESIAN_POINT('Ctrl Pts',(-41.5,-57.0692704467351,-171.511552982749));
#143874=CARTESIAN_POINT('Ctrl Pts',(-41.5,-57.0999570266663,-171.199145438258));
#143875=CARTESIAN_POINT('Ctrl Pts',(-41.8680165447745,-56.6807474451005,
-171.649964244171));
#143876=CARTESIAN_POINT('Ctrl Pts',(-41.5,-56.6836417097802,-171.547472271891));
#143877=CARTESIAN_POINT('Ctrl Pts',(-41.5,-56.7235644715492,-171.167401493624));
#143878=CARTESIAN_POINT('Ctrl Pts',(-41.929815802996,-56.5034783375505,
-171.649958730482));
#143879=CARTESIAN_POINT('Ctrl Pts',(-41.4999999999999,-56.494149705945,
-171.583952704407));
#143880=CARTESIAN_POINT('Ctrl Pts',(-41.5,-56.5353526996975,-171.149950046396));
#143881=CARTESIAN_POINT('Ctrl Pts',(-42.0000617764046,-56.3473237326807,
-171.649949996184));
#143882=CARTESIAN_POINT('Ctrl Pts',(-41.5,-56.3473237326807,-171.650011780221));
#143883=CARTESIAN_POINT('Ctrl Pts',(-41.5,-56.3473237326807,-171.14995));
#143884=CARTESIAN_POINT('Origin',(-42.,-58.6035812240168,-171.14995));
#143885=CARTESIAN_POINT('Origin',(-42.,-56.3473237326807,-171.14995));
#143886=CARTESIAN_POINT('Origin',(0.,-12.9675000200281,-171.64995));
#143887=CARTESIAN_POINT('',(-48.9446667094463,-57.4569357767149,-171.64995));
#143888=CARTESIAN_POINT('',(-49.2787232447289,-55.08000002,-171.64995));
#143889=CARTESIAN_POINT('',(-49.3685531658572,-54.4408269190399,-171.64995));
#143890=CARTESIAN_POINT('',(-48.4203826827217,-58.549476072617,-171.64995));
#143891=CARTESIAN_POINT('Origin',(-46.9641305719631,-57.1785895747948,-171.64995));
#143892=CARTESIAN_POINT('',(-45.5819760525891,-61.3878827027496,-171.64995));
#143893=CARTESIAN_POINT('Origin',(0.,-12.9675000200281,-171.64995));
#143894=CARTESIAN_POINT('',(-44.489435756687,-61.9121667294742,-171.64995));
#143895=CARTESIAN_POINT('Origin',(-44.2110895547669,-59.9316305919911,-171.64995));
#143896=CARTESIAN_POINT('',(-42.,-62.2620341086569,-171.64995));
#143897=CARTESIAN_POINT('',(-44.489435756687,-61.9121667294742,-171.64995));
#143898=CARTESIAN_POINT('',(-42.,-62.3323045260081,-171.64995));
#143899=CARTESIAN_POINT('',(-42.5,-55.08000002,-171.64995));
#143900=CARTESIAN_POINT('Ctrl Pts',(-43.1572831724514,-55.0801481215059,
-171.649949978066));
#143901=CARTESIAN_POINT('Ctrl Pts',(-43.1572831724515,-54.58000002,-171.650098123446));
#143902=CARTESIAN_POINT('Ctrl Pts',(-43.1572831724514,-54.58000002,-171.14995));
#143903=CARTESIAN_POINT('Ctrl Pts',(-43.3271185292342,-54.9843723315205,
-171.649978738968));
#143904=CARTESIAN_POINT('Ctrl Pts',(-43.3143913613982,-54.5800000199971,
-171.56146605948));
#143905=CARTESIAN_POINT('Ctrl Pts',(-43.3817682803707,-54.58000002,-171.149950056136));
#143906=CARTESIAN_POINT('Ctrl Pts',(-43.529947173783,-54.8943395876967,
-171.649995064611));
#143907=CARTESIAN_POINT('Ctrl Pts',(-43.5407821982002,-54.5800000200016,
-171.520211742113));
#143908=CARTESIAN_POINT('Ctrl Pts',(-43.6059648750607,-54.58000002,-171.185915645006));
#143909=CARTESIAN_POINT('Ctrl Pts',(-43.9881565230544,-54.7646161135083,
-171.65000835312));
#143910=CARTESIAN_POINT('Ctrl Pts',(-44.0046317151095,-54.5800000199985,
-171.495876387334));
#143911=CARTESIAN_POINT('Ctrl Pts',(-44.0540062919344,-54.58000002,-171.260373422648));
#143912=CARTESIAN_POINT('Ctrl Pts',(-44.2440095987557,-54.7260645641701,
-171.650006647719));
#143913=CARTESIAN_POINT('Ctrl Pts',(-44.2580491347888,-54.58000002,-171.503655116484));
#143914=CARTESIAN_POINT('Ctrl Pts',(-44.2780419706102,-54.58000002,-171.296906912307));
#143915=CARTESIAN_POINT('Ctrl Pts',(-44.7601884828714,-54.7249655177493,
-171.65000663285));
#143916=CARTESIAN_POINT('Ctrl Pts',(-44.7466180387422,-54.58000002,-171.503788967852));
#143917=CARTESIAN_POINT('Ctrl Pts',(-44.7276655629966,-54.58000002,-171.297869301671));
#143918=CARTESIAN_POINT('Ctrl Pts',(-45.0183788445838,-54.7626525929476,
-171.650008425802));
#143919=CARTESIAN_POINT('Ctrl Pts',(-45.00211408603,-54.58000002,-171.49586884709));
#143920=CARTESIAN_POINT('Ctrl Pts',(-44.9532637149971,-54.58000002,-171.261822611311));
#143921=CARTESIAN_POINT('Ctrl Pts',(-45.4809398893321,-54.8922510295823,
-171.649995402787));
#143922=CARTESIAN_POINT('Ctrl Pts',(-45.4698465063652,-54.58000002,-171.519435241711));
#143923=CARTESIAN_POINT('Ctrl Pts',(-45.4045230317323,-54.58000002,-171.186802156157));
#143924=CARTESIAN_POINT('Ctrl Pts',(-45.6855420836464,-54.9825427397827,
-171.649979290157));
#143925=CARTESIAN_POINT('Ctrl Pts',(-45.6987517183234,-54.5800000199883,
-171.559908009068));
#143926=CARTESIAN_POINT('Ctrl Pts',(-45.6299507757146,-54.58000002,-171.149950055386));
#143927=CARTESIAN_POINT('Ctrl Pts',(-45.8586217441902,-55.0801481215059,
-171.649949978066));
#143928=CARTESIAN_POINT('Ctrl Pts',(-45.8586217441902,-54.58000002,-171.650098123446));
#143929=CARTESIAN_POINT('Ctrl Pts',(-45.8586217441902,-54.58000002,-171.14995));
#143930=CARTESIAN_POINT('Origin',(-43.1572831724514,-55.08000002,-171.14995));
#143931=CARTESIAN_POINT('Origin',(-45.8586217441902,-55.08000002,-171.14995));
#143932=CARTESIAN_POINT('Origin',(0.,-12.9675000200281,-171.64995));
#143933=CARTESIAN_POINT('',(-42.,-55.58000002,-171.64995));
#143934=CARTESIAN_POINT('',(-42.,-62.3323045260081,-171.64995));
#143935=CARTESIAN_POINT('',(-42.5,-55.08000002,-171.64995));
#143936=CARTESIAN_POINT('Origin',(-42.5,-55.58000002,-171.64995));
#143937=CARTESIAN_POINT('',(-42.5,-55.08000002,-171.64995));
#143938=CARTESIAN_POINT('Ctrl Pts',(-45.342056117244,28.9200050678815,-171.649949999974));
#143939=CARTESIAN_POINT('Ctrl Pts',(-45.342056117244,28.41999998,-171.649955087908));
#143940=CARTESIAN_POINT('Ctrl Pts',(-45.342056117244,28.41999998,-171.14995));
#143941=CARTESIAN_POINT('Ctrl Pts',(-45.2161093325492,28.8799153348106,
-171.649950408626));
#143942=CARTESIAN_POINT('Ctrl Pts',(-45.2207546457863,28.4199999799926,
-171.611343620546));
#143943=CARTESIAN_POINT('Ctrl Pts',(-45.2032855852167,28.41999998,-171.149950027441));
#143944=CARTESIAN_POINT('Ctrl Pts',(-45.0809055449373,28.8470468727513,
-171.649950690988));
#143945=CARTESIAN_POINT('Ctrl Pts',(-45.0814092233328,28.4199999800032,
-171.586474354512));
#143946=CARTESIAN_POINT('Ctrl Pts',(-45.0642313709306,28.41999998,-171.155055788632));
#143947=CARTESIAN_POINT('Ctrl Pts',(-44.7999542633241,28.8023061531436,
-171.649951053492));
#143948=CARTESIAN_POINT('Ctrl Pts',(-44.7998786663722,28.4199999799969,
-171.556875075933));
#143949=CARTESIAN_POINT('Ctrl Pts',(-44.7862672310248,28.41999998,-171.163656910012));
#143950=CARTESIAN_POINT('Ctrl Pts',(-44.6541596767004,28.7904721518725,
-171.64995113455));
#143951=CARTESIAN_POINT('Ctrl Pts',(-44.6527441767021,28.4199999799986,
-171.550586180072));
#143952=CARTESIAN_POINT('Ctrl Pts',(-44.6472721153249,28.41999998,-171.16702013224));
#143953=CARTESIAN_POINT('Ctrl Pts',(-44.36232828092,28.7904412154044,-171.649951134795));
#143954=CARTESIAN_POINT('Ctrl Pts',(-44.3637416796286,28.4199999800014,
-171.550568959217));
#143955=CARTESIAN_POINT('Ctrl Pts',(-44.3691883762669,28.41999998,-171.167028040093));
#143956=CARTESIAN_POINT('Ctrl Pts',(-44.2164190292983,28.802252604719,-171.649951053893));
#143957=CARTESIAN_POINT('Ctrl Pts',(-44.2164931090597,28.4199999799986,
-171.556843793952));
#143958=CARTESIAN_POINT('Ctrl Pts',(-44.2300913879779,28.41999998,-171.163669856825));
#143959=CARTESIAN_POINT('Ctrl Pts',(-43.9353228646307,28.846974377406,-171.649950691605));
#143960=CARTESIAN_POINT('Ctrl Pts',(-43.9348222136901,28.4199999800015,
-171.586421593668));
#143961=CARTESIAN_POINT('Ctrl Pts',(-43.9520032655911,28.41999998,-171.15506708045));
#143962=CARTESIAN_POINT('Ctrl Pts',(-43.8001087095933,28.8798156647999,
-171.649950409642));
#143963=CARTESIAN_POINT('Ctrl Pts',(-43.7954409326623,28.41999998,-171.611251100138));
#143964=CARTESIAN_POINT('Ctrl Pts',(-43.8129594627921,28.41999998,-171.149950027533));
#143965=CARTESIAN_POINT('Ctrl Pts',(-43.6738487993976,28.9200050678815,
-171.649949999974));
#143966=CARTESIAN_POINT('Ctrl Pts',(-43.6738487993976,28.41999998,-171.649955087908));
#143967=CARTESIAN_POINT('Ctrl Pts',(-43.6738487993976,28.41999998,-171.14995));
#143968=CARTESIAN_POINT('Origin',(-45.342056117244,28.91999998,-171.14995));
#143969=CARTESIAN_POINT('Origin',(-43.6738487993976,28.91999998,-171.14995));
#143970=CARTESIAN_POINT('Origin',(0.,-12.9675000200281,-171.64995));
#143971=CARTESIAN_POINT('',(-44.489435756687,35.9771666894179,-171.64995));
#143972=CARTESIAN_POINT('',(-41.3608268990399,36.416863989729,-171.64995));
#143973=CARTESIAN_POINT('',(-45.5819760525891,35.4528826626933,-171.64995));
#143974=CARTESIAN_POINT('Origin',(-44.2110895547669,33.9966305519348,-171.64995));
#143975=CARTESIAN_POINT('',(-48.4203826827217,32.6144760325608,-171.64995));
#143976=CARTESIAN_POINT('Origin',(0.,-12.9675000200281,-171.64995));
#143977=CARTESIAN_POINT('',(-48.9446667094463,31.5219357366587,-171.64995));
#143978=CARTESIAN_POINT('Origin',(-46.9641305719631,31.2435895347386,-171.64995));
#143979=CARTESIAN_POINT('',(-49.3103449325291,28.91999998,-171.64995));
#143980=CARTESIAN_POINT('',(-48.9446667094463,31.5219357366587,-171.64995));
#143981=CARTESIAN_POINT('',(-49.3806153498803,28.91999998,-171.64995));
#143982=CARTESIAN_POINT('Origin',(0.,-12.9675000200281,-171.64995));
#143983=CARTESIAN_POINT('',(-49.3806153498803,28.91999998,-171.64995));
#143984=CARTESIAN_POINT('Origin',(-24.2,67.7009572055632,-176.84995));
#143985=CARTESIAN_POINT('',(-24.2,-70.08000002,-177.34995));
#143986=CARTESIAN_POINT('Origin',(-24.2,-70.08000002,-176.84995));
#143987=CARTESIAN_POINT('',(-24.2,-73.08000002,-177.34995));
#143988=CARTESIAN_POINT('Ctrl Pts',(-23.0233258551573,-66.6335614680093,
-171.428053802042));
#143989=CARTESIAN_POINT('Ctrl Pts',(-23.7000418723672,-66.4085345904138,
-171.549239609537));
#143990=CARTESIAN_POINT('Ctrl Pts',(-23.6999999991623,-67.045403335443,
-171.20624326695));
#143991=CARTESIAN_POINT('Ctrl Pts',(-23.0096928629965,-66.7164302706428,
-171.571078901801));
#143992=CARTESIAN_POINT('Ctrl Pts',(-23.7000436385783,-66.4472919682874,
-171.670421709922));
#143993=CARTESIAN_POINT('Ctrl Pts',(-23.6999999991454,-67.1609416565799,
-171.420795636143));
#143994=CARTESIAN_POINT('Ctrl Pts',(-23.0026938228076,-66.7592463230786,
-171.731032985107));
#143995=CARTESIAN_POINT('Ctrl Pts',(-23.7000445959748,-66.4581897882961,
-171.777275420463));
#143996=CARTESIAN_POINT('Ctrl Pts',(-23.6999999991368,-67.220679933255,
-171.660715193487));
#143997=CARTESIAN_POINT('Ctrl Pts',(-23.0034444927493,-66.754655532928,
-171.89560645919));
#143998=CARTESIAN_POINT('Ctrl Pts',(-23.700044492639,-66.4569597257248,
-171.887725483309));
#143999=CARTESIAN_POINT('Ctrl Pts',(-23.6999999991377,-67.2142749444987,
-171.907589194352));
#144000=CARTESIAN_POINT('Origin',(-23.2,-67.0618271655313,-171.237717270032));
#144001=CARTESIAN_POINT('Origin',(0.,-12.9675000200281,-171.64995));
#144002=CARTESIAN_POINT('',(-17.3782102443554,-55.386710964082,-144.502505142985));
#144003=CARTESIAN_POINT('Ctrl Pts',(-17.3782102443554,-55.386710964082,
-144.502505142985));
#144004=CARTESIAN_POINT('Ctrl Pts',(-17.393698976901,-59.8910064811234,
-153.453571806853));
#144005=CARTESIAN_POINT('Ctrl Pts',(-17.4052435876731,-64.3204354194662,
-162.443049524475));
#144006=CARTESIAN_POINT('Ctrl Pts',(-17.4148840712405,-68.7171063154928,
-171.449026400902));
#144007=CARTESIAN_POINT('',(-22.9849163979996,-55.5914230987146,-150.046801024052));
#144008=CARTESIAN_POINT('Ctrl Pts',(-22.9849164538399,-55.5914231005407,
-150.046800950003));
#144009=CARTESIAN_POINT('Ctrl Pts',(-21.8819096287209,-55.5491926957159,
-148.844364427775));
#144010=CARTESIAN_POINT('Ctrl Pts',(-20.7471390543143,-55.506534730412,
-147.668247996036));
#144011=CARTESIAN_POINT('Ctrl Pts',(-19.5724972232793,-55.4640266335675,
-146.531662497644));
#144012=CARTESIAN_POINT('Ctrl Pts',(-18.8525414070574,-55.4379727754883,
-145.835031985619));
#144013=CARTESIAN_POINT('Ctrl Pts',(-18.1219084936406,-55.4121270272551,
-145.157368487698));
#144014=CARTESIAN_POINT('Ctrl Pts',(-17.3782871132615,-55.3867051178771,
-144.502418094041));
#144015=CARTESIAN_POINT('Ctrl Pts',(-23.0213852109847,-66.6453596297547,
-171.449026400902));
#144016=CARTESIAN_POINT('Ctrl Pts',(-23.0112491123844,-63.0152939322715,
-164.285990110815));
#144017=CARTESIAN_POINT('Ctrl Pts',(-22.9994804181366,-59.343937645489,
-157.144704426787));
#144018=CARTESIAN_POINT('Ctrl Pts',(-22.9849163103246,-55.591423110293,
-150.046801090999));
#144019=CARTESIAN_POINT('Ctrl Pts',(-17.4014093021639,-68.8184551193695,
-171.915576738158));
#144020=CARTESIAN_POINT('Ctrl Pts',(-17.0499387022882,-68.9277121722468,
-171.920632758432));
#144021=CARTESIAN_POINT('Ctrl Pts',(-17.0500000069342,-69.2954487057978,
-171.937551171933));
#144022=CARTESIAN_POINT('Ctrl Pts',(-17.4003036470898,-68.8268112548536,
-171.739609324912));
#144023=CARTESIAN_POINT('Ctrl Pts',(-17.0499389461697,-68.9377102872281,
-171.724562885898));
#144024=CARTESIAN_POINT('Ctrl Pts',(-17.0500000069124,-69.3074655181351,
-171.673561286109));
#144025=CARTESIAN_POINT('Ctrl Pts',(-17.4058449755969,-68.7849016359872,
-171.566109516219));
#144026=CARTESIAN_POINT('Ctrl Pts',(-17.0499377162343,-68.887140708855,
-171.529148195035));
#144027=CARTESIAN_POINT('Ctrl Pts',(-17.0500000070217,-69.2471945003534,
-171.413338787174));
#144028=CARTESIAN_POINT('Ctrl Pts',(-17.4177209010562,-68.6958205805999,
-171.409539580699));
#144029=CARTESIAN_POINT('Ctrl Pts',(-17.049935034885,-68.784349448281,-171.361182926232));
#144030=CARTESIAN_POINT('Ctrl Pts',(-17.050000007256,-69.1191208280442,
-171.178440426026));
#144031=CARTESIAN_POINT('Origin',(-17.55,-69.1496478013716,-171.237717270032));
#144032=CARTESIAN_POINT('Origin',(-16.55,-73.08000002,-176.84995));
#144033=CARTESIAN_POINT('',(-16.55,-70.08000002,-177.34995));
#144034=CARTESIAN_POINT('',(-16.55,-73.08000002,-177.34995));
#144035=CARTESIAN_POINT('Origin',(-16.55,-70.08000002,-176.84995));
#144036=CARTESIAN_POINT('Origin',(-41.5,-73.08000002,-177.34995));
#144037=CARTESIAN_POINT('',(-16.05,-70.08000002,-177.34995));
#144038=CARTESIAN_POINT('',(-16.05,-73.08000002,-177.34995));
#144039=CARTESIAN_POINT('',(41.5,-70.08000002,-177.34995));
#144040=CARTESIAN_POINT('Origin',(-16.05,67.7009572055632,-176.84995));
#144041=CARTESIAN_POINT('Origin',(-16.05,-70.08000002,-176.84995));
#144042=CARTESIAN_POINT('Ctrl Pts',(-14.9365391746094,-69.4116829512029,
-171.409919376296));
#144043=CARTESIAN_POINT('Ctrl Pts',(-15.5501264775731,-69.2858420378444,
-171.477695372047));
#144044=CARTESIAN_POINT('Ctrl Pts',(-15.5499999899231,-69.8405291599117,
-171.179005018994));
#144045=CARTESIAN_POINT('Ctrl Pts',(-14.9264726997877,-69.4976592258842,
-171.564867666237));
#144046=CARTESIAN_POINT('Ctrl Pts',(-15.5501302527645,-69.3463988305637,
-171.619616090566));
#144047=CARTESIAN_POINT('Ctrl Pts',(-15.5499999897578,-69.9655161046422,
-171.411462758814));
#144048=CARTESIAN_POINT('Ctrl Pts',(-14.9216112388798,-69.5395284795157,
-171.737936502975));
#144049=CARTESIAN_POINT('Ctrl Pts',(-15.5501321305785,-69.3710444733645,
-171.760987815194));
#144050=CARTESIAN_POINT('Ctrl Pts',(-15.5499999896779,-70.0263968022397,
-171.67105498688));
#144051=CARTESIAN_POINT('Ctrl Pts',(-14.9225783333433,-69.5312053406244,
-171.916063466645));
#144052=CARTESIAN_POINT('Ctrl Pts',(-15.550131758936,-69.3660274114058,
-171.908368448016));
#144053=CARTESIAN_POINT('Ctrl Pts',(-15.5499999896938,-70.0142946511941,
-171.938280796929));
#144054=CARTESIAN_POINT('Origin',(-15.05,-69.870344670579,-171.237717270032));
#144055=CARTESIAN_POINT('Origin',(0.,-12.9675000200281,-171.64995));
#144056=CARTESIAN_POINT('',(-9.30242220787652,-55.1547652726017,-138.840493482365));
#144057=CARTESIAN_POINT('Ctrl Pts',(-9.30242220787652,-55.1547652726017,
-138.840493482365));
#144058=CARTESIAN_POINT('Ctrl Pts',(-9.31373871873353,-60.3366136239018,
-149.697543382477));
#144059=CARTESIAN_POINT('Ctrl Pts',(-9.32139301854133,-65.4864258912612,
-160.57036601249));
#144060=CARTESIAN_POINT('Ctrl Pts',(-9.3276302147955,-70.6241744288951,
-171.449026400902));
#144061=CARTESIAN_POINT('',(-14.8995695352622,-55.3054345022359,-142.448537940653));
#144062=CARTESIAN_POINT('Ctrl Pts',(-14.8995694550282,-55.3054345175152,
-142.448537985759));
#144063=CARTESIAN_POINT('Ctrl Pts',(-13.8974507820956,-55.2740998389091,
-141.671728947382));
#144064=CARTESIAN_POINT('Ctrl Pts',(-12.8656304705197,-55.2438017962785,
-140.937883847407));
#144065=CARTESIAN_POINT('Ctrl Pts',(-10.9773541322587,-55.1936555815648,
-139.745510662921));
#144066=CARTESIAN_POINT('Ctrl Pts',(-10.1477730317694,-55.1733155860424,
-139.269609716656));
#144067=CARTESIAN_POINT('Ctrl Pts',(-9.30242220787652,-55.1547652726017,
-138.840493482365));
#144068=CARTESIAN_POINT('Ctrl Pts',(-14.9341313545396,-69.4322546019744,
-171.449026400902));
#144069=CARTESIAN_POINT('Ctrl Pts',(-14.9252396269456,-64.7624344426112,
-161.762591659591));
#144070=CARTESIAN_POINT('Ctrl Pts',(-14.9144862578123,-60.0660270491051,
-152.089344301479));
#144071=CARTESIAN_POINT('Ctrl Pts',(-14.8995694550282,-55.3054345175152,
-142.448537985759));
#144072=CARTESIAN_POINT('Ctrl Pts',(-9.32033898305081,-70.7202599648223,
-171.871644662643));
#144073=CARTESIAN_POINT('Ctrl Pts',(-8.89999999999996,-70.7880957152448,
-171.871644662643));
#144074=CARTESIAN_POINT('Ctrl Pts',(-8.9,-71.2138732976838,-171.871644662643));
#144075=CARTESIAN_POINT('Ctrl Pts',(-9.32033898569755,-70.7202599643952,
-171.725683074261));
#144076=CARTESIAN_POINT('Ctrl Pts',(-8.89999999999997,-70.7880957023883,
-171.715624308049));
#144077=CARTESIAN_POINT('Ctrl Pts',(-8.9,-71.2138732807092,-171.652697712588));
#144078=CARTESIAN_POINT('Ctrl Pts',(-9.32278024510803,-70.6879410017649,
-171.582358093922));
#144079=CARTESIAN_POINT('Ctrl Pts',(-8.90000000000455,-70.7514100828351,
-171.561941332422));
#144080=CARTESIAN_POINT('Ctrl Pts',(-8.9,-71.16598797688,-171.437720890984));
#144081=CARTESIAN_POINT('Ctrl Pts',(-9.3276302147955,-70.6241744288951,
-171.449026400902));
#144082=CARTESIAN_POINT('Ctrl Pts',(-8.89999999999997,-70.680735306053,
-171.422308714525));
#144083=CARTESIAN_POINT('Ctrl Pts',(-8.9,-71.0715121820529,-171.237717270032));
#144084=CARTESIAN_POINT('Origin',(-9.4,-71.0715121820529,-171.237717270032));
#144085=CARTESIAN_POINT('Ctrl Pts',(-8.9,-72.58000002,-174.451268889151));
#144086=CARTESIAN_POINT('Ctrl Pts',(-8.89999999999996,-73.0800000199999,
-174.45126888915));
#144087=CARTESIAN_POINT('Ctrl Pts',(-8.4,-73.08000002,-174.451268889151));
#144088=CARTESIAN_POINT('Ctrl Pts',(-8.9,-72.58000001309,-174.70608894667));
#144089=CARTESIAN_POINT('Ctrl Pts',(-8.89999999999997,-73.0780290434905,
-174.756376067791));
#144090=CARTESIAN_POINT('Ctrl Pts',(-8.40197484549326,-73.08000002,-174.75697631869));
#144091=CARTESIAN_POINT('Ctrl Pts',(-8.9,-72.5419664714886,-174.954543971783));
#144092=CARTESIAN_POINT('Ctrl Pts',(-8.89999999999997,-73.0306532835766,
-175.053905133681));
#144093=CARTESIAN_POINT('Ctrl Pts',(-8.40390532350201,-73.0343597586633,
-175.055047332367));
#144094=CARTESIAN_POINT('Ctrl Pts',(-8.9,-72.4287614956301,-175.317581230789));
#144095=CARTESIAN_POINT('Ctrl Pts',(-8.89999999999997,-72.892300013639,
-175.488192872161));
#144096=CARTESIAN_POINT('Ctrl Pts',(-8.40673247093662,-72.8985137923177,
-175.490582060873));
#144097=CARTESIAN_POINT('Ctrl Pts',(-8.9,-72.3815711902508,-175.436174718935));
#144098=CARTESIAN_POINT('Ctrl Pts',(-8.89999999999996,-72.8349801887897,
-175.629812439872));
#144099=CARTESIAN_POINT('Ctrl Pts',(-8.40765712457444,-72.8418854248583,
-175.632858253021));
#144100=CARTESIAN_POINT('Ctrl Pts',(-8.9,-72.2712246146549,-175.662282844729));
#144101=CARTESIAN_POINT('Ctrl Pts',(-8.89999999999995,-72.7014018648635,
-175.899567338683));
#144102=CARTESIAN_POINT('Ctrl Pts',(-8.40942187655549,-72.7094695330285,
-175.904119271778));
#144103=CARTESIAN_POINT('Ctrl Pts',(-8.9,-72.2077913051056,-175.770759223));
#144104=CARTESIAN_POINT('Ctrl Pts',(-8.90000000000094,-72.6248303464193,
-176.028888062411));
#144105=CARTESIAN_POINT('Ctrl Pts',(-8.41026946333178,-72.6333495611344,
-176.034257895752));
#144106=CARTESIAN_POINT('Ctrl Pts',(-8.9,-72.0642238201576,-175.978456398961));
#144107=CARTESIAN_POINT('Ctrl Pts',(-8.89999999999898,-72.4518932717193,
-176.276278393733));
#144108=CARTESIAN_POINT('Ctrl Pts',(-8.41189381664575,-72.4610685811814,
-176.283431179031));
#144109=CARTESIAN_POINT('Ctrl Pts',(-8.9,-71.9835055577593,-176.078093003191));
#144110=CARTESIAN_POINT('Ctrl Pts',(-8.89999999999997,-72.354843766023,
-176.394881486481));
#144111=CARTESIAN_POINT('Ctrl Pts',(-8.41267385193151,-72.3642066660697,
-176.402964676645));
#144112=CARTESIAN_POINT('Ctrl Pts',(-8.9,-71.8103399713904,-176.261453778625));
#144113=CARTESIAN_POINT('Ctrl Pts',(-8.89999999999996,-72.1469580486365,
-176.612968031678));
#144114=CARTESIAN_POINT('Ctrl Pts',(-8.41411048564612,-72.15640796091,-176.622941542856));
#144115=CARTESIAN_POINT('Ctrl Pts',(-8.9,-71.7174295924368,-176.34602338026));
#144116=CARTESIAN_POINT('Ctrl Pts',(-8.89999999999996,-72.0355638390553,
-176.713502881279));
#144117=CARTESIAN_POINT('Ctrl Pts',(-8.41477368991416,-72.0449155064423,
-176.724399172119));
#144118=CARTESIAN_POINT('Ctrl Pts',(-8.9,-71.4198068682475,-176.578502281526));
#144119=CARTESIAN_POINT('Ctrl Pts',(-8.89999999999996,-71.6793465425378,
-176.989505620533));
#144120=CARTESIAN_POINT('Ctrl Pts',(-8.4165979801388,-71.6877682388606,
-177.003302608065));
#144121=CARTESIAN_POINT('Ctrl Pts',(-8.9,-71.1936270830052,-176.705108386635));
#144122=CARTESIAN_POINT('Ctrl Pts',(-8.90000000001297,-71.4089014982389,
-177.139847092069));
#144123=CARTESIAN_POINT('Ctrl Pts',(-8.41759316850175,-71.4163525958445,
-177.155190995531));
#144124=CARTESIAN_POINT('Ctrl Pts',(-8.9,-70.9600741080247,-176.793015835821));
#144125=CARTESIAN_POINT('Ctrl Pts',(-8.89999999999996,-71.1298793121603,
-177.244155204947));
#144126=CARTESIAN_POINT('Ctrl Pts',(-8.41828452049191,-71.1360889256296,
-177.260652939026));
#144127=CARTESIAN_POINT('',(-8.4,-73.08000002,-174.451268889151));
#144128=CARTESIAN_POINT('Ctrl Pts',(-8.4181782717274,-71.1781985203566,
-177.244444626904));
#144129=CARTESIAN_POINT('Ctrl Pts',(-8.41749277252308,-71.4434978899076,
-177.139867487715));
#144130=CARTESIAN_POINT('Ctrl Pts',(-8.41653697428584,-71.6997115543464,
-176.993975834412));
#144131=CARTESIAN_POINT('Ctrl Pts',(-8.41477368991416,-72.0449155064423,
-176.724399172119));
#144132=CARTESIAN_POINT('Ctrl Pts',(-8.41411048564612,-72.15640796091,-176.622941542856));
#144133=CARTESIAN_POINT('Ctrl Pts',(-8.41267385193151,-72.3642066660697,
-176.402964676645));
#144134=CARTESIAN_POINT('Ctrl Pts',(-8.41189381664575,-72.4610685811814,
-176.283431179031));
#144135=CARTESIAN_POINT('Ctrl Pts',(-8.41026946333178,-72.6333495611344,
-176.034257895752));
#144136=CARTESIAN_POINT('Ctrl Pts',(-8.40942187655549,-72.7094695330285,
-175.904119271778));
#144137=CARTESIAN_POINT('Ctrl Pts',(-8.40765712457444,-72.8418854248583,
-175.632858253021));
#144138=CARTESIAN_POINT('Ctrl Pts',(-8.40673247093662,-72.8985137923177,
-175.490582060873));
#144139=CARTESIAN_POINT('Ctrl Pts',(-8.40390532350201,-73.0343597586633,
-175.055047332367));
#144140=CARTESIAN_POINT('Ctrl Pts',(-8.40197484549326,-73.08000002,-174.75697631869));
#144141=CARTESIAN_POINT('Ctrl Pts',(-8.4,-73.08000002,-174.451268889151));
#144142=CARTESIAN_POINT('Origin',(-8.4,-72.58000002,-174.451268889151));
#144143=CARTESIAN_POINT('Ctrl Pts',(-8.51230691249381,-71.1434663357063,
-177.254202907715));
#144144=CARTESIAN_POINT('Ctrl Pts',(-8.48384574056985,-73.08000002,-176.520599502442));
#144145=CARTESIAN_POINT('Ctrl Pts',(-8.40355780430818,-73.08000002,-174.451130838212));
#144146=CARTESIAN_POINT('Ctrl Pts',(-8.31384446654331,-71.169690780161,
-177.251953160255));
#144147=CARTESIAN_POINT('Ctrl Pts',(-8.285073768204,-73.0800000200061,-176.507651386999));
#144148=CARTESIAN_POINT('Ctrl Pts',(-8.20353011255175,-73.08000002,-174.458891192924));
#144149=CARTESIAN_POINT('Ctrl Pts',(-8.11484675268687,-71.1950080123697,
-177.249844108498));
#144150=CARTESIAN_POINT('Ctrl Pts',(-8.08524840860191,-73.0800000200063,
-176.495676023668));
#144151=CARTESIAN_POINT('Ctrl Pts',(-8.00350691066062,-73.08000002,-174.46684979476));
#144152=CARTESIAN_POINT('Ctrl Pts',(-7.91536503462484,-71.2194103886422,
-177.247865511992));
#144153=CARTESIAN_POINT('Ctrl Pts',(-7.88456937757999,-73.0800000199998,
-176.484587012089));
#144154=CARTESIAN_POINT('Ctrl Pts',(-7.80348623696872,-73.08000002,-174.474919939778));
#144155=CARTESIAN_POINT('',(-7.9,-73.08000002,-174.471034982976));
#144156=CARTESIAN_POINT('Ctrl Pts',(-7.9,-73.08000002,-174.471034982976));
#144157=CARTESIAN_POINT('Ctrl Pts',(-7.90199316078775,-73.08000002,-174.769251346187));
#144158=CARTESIAN_POINT('Ctrl Pts',(-7.90394076068631,-73.0365253516511,
-175.060187649793));
#144159=CARTESIAN_POINT('Ctrl Pts',(-7.90679252703161,-72.9073122055494,
-175.485606387024));
#144160=CARTESIAN_POINT('Ctrl Pts',(-7.90772857701081,-72.8532929465542,
-175.625142180141));
#144161=CARTESIAN_POINT('Ctrl Pts',(-7.90951546143904,-72.7269941355612,
-175.891343758978));
#144162=CARTESIAN_POINT('Ctrl Pts',(-7.9103743244834,-72.6543924247951,
-176.019207476496));
#144163=CARTESIAN_POINT('Ctrl Pts',(-7.9120222658245,-72.4901918790006,
-176.264409528534));
#144164=CARTESIAN_POINT('Ctrl Pts',(-7.91281676658892,-72.3977319011293,
-176.382553154925));
#144165=CARTESIAN_POINT('Ctrl Pts',(-7.91428825612723,-72.198695730848,
-176.6012613201));
#144166=CARTESIAN_POINT('Ctrl Pts',(-7.91496944868021,-72.0919119068452,
-176.702452310058));
#144167=CARTESIAN_POINT('Ctrl Pts',(-7.91682110979193,-71.7555164883556,
-176.977410112178));
#144168=CARTESIAN_POINT('Ctrl Pts',(-7.91784535584628,-71.5021289246249,
-177.129353672878));
#144169=CARTESIAN_POINT('Ctrl Pts',(-7.91859121655449,-71.2381488509313,
-177.239961484006));
#144170=CARTESIAN_POINT('Ctrl Pts',(-7.9,-73.08000002,-174.471034982976));
#144171=CARTESIAN_POINT('Ctrl Pts',(-8.06666381945983,-73.08000002,-174.464342510025));
#144172=CARTESIAN_POINT('Ctrl Pts',(-8.23333002609749,-73.08000002,-174.457737044943));
#144173=CARTESIAN_POINT('Ctrl Pts',(-8.4,-73.08000002,-174.451268889151));
#144174=CARTESIAN_POINT('Ctrl Pts',(-7.9,-73.08000002,-174.471034982976));
#144175=CARTESIAN_POINT('Ctrl Pts',(-7.39999999999995,-73.0800000199999,
-174.471034982977));
#144176=CARTESIAN_POINT('Ctrl Pts',(-7.4,-72.58000002,-174.471034982976));
#144177=CARTESIAN_POINT('Ctrl Pts',(-7.90199316078775,-73.08000002,-174.769251346187));
#144178=CARTESIAN_POINT('Ctrl Pts',(-7.39999999999996,-73.081997137201,
-174.769844466953));
#144179=CARTESIAN_POINT('Ctrl Pts',(-7.4,-72.5800000132661,-174.719615315523));
#144180=CARTESIAN_POINT('Ctrl Pts',(-7.90394076068631,-73.0365253516511,
-175.060187649793));
#144181=CARTESIAN_POINT('Ctrl Pts',(-7.39999999999996,-73.040326257465,
-175.061328113453));
#144182=CARTESIAN_POINT('Ctrl Pts',(-7.4,-72.5437711321103,-174.962127460747));
#144183=CARTESIAN_POINT('Ctrl Pts',(-7.90679252703161,-72.9073122055494,
-175.485606387024));
#144184=CARTESIAN_POINT('Ctrl Pts',(-7.39999999999996,-72.9137734508192,
-175.488022550208));
#144185=CARTESIAN_POINT('Ctrl Pts',(-7.4,-72.4360935067573,-175.316738645421));
#144186=CARTESIAN_POINT('Ctrl Pts',(-7.90772857701081,-72.8532929465542,
-175.625142180141));
#144187=CARTESIAN_POINT('Ctrl Pts',(-7.40000000000002,-72.8605108035235,
-175.628237972001));
#144188=CARTESIAN_POINT('Ctrl Pts',(-7.4,-72.3910774582401,-175.433049854657));
#144189=CARTESIAN_POINT('Ctrl Pts',(-7.90951546143904,-72.7269941355612,
-175.891343758978));
#144190=CARTESIAN_POINT('Ctrl Pts',(-7.39999999999993,-72.7355139213092,
-175.896009980972));
#144191=CARTESIAN_POINT('Ctrl Pts',(-7.4,-72.2858284501893,-175.654944429739));
#144192=CARTESIAN_POINT('Ctrl Pts',(-7.9103743244834,-72.6543924247951,
-176.019207476496));
#144193=CARTESIAN_POINT('Ctrl Pts',(-7.39999999999901,-72.6634371311262,
-176.024735407069));
#144194=CARTESIAN_POINT('Ctrl Pts',(-7.4,-72.2253270246874,-175.761526340889));
#144195=CARTESIAN_POINT('Ctrl Pts',(-7.9120222658245,-72.4901918790006,
-176.264409528534));
#144196=CARTESIAN_POINT('Ctrl Pts',(-7.40000000000093,-72.5000420015558,
-176.271831635453));
#144197=CARTESIAN_POINT('Ctrl Pts',(-7.4,-72.0884932351423,-175.96591668417));
#144198=CARTESIAN_POINT('Ctrl Pts',(-7.91281676658892,-72.3977319011293,
-176.382553154925));
#144199=CARTESIAN_POINT('Ctrl Pts',(-7.39999999999761,-72.4078441030974,
-176.390977561524));
#144200=CARTESIAN_POINT('Ctrl Pts',(-7.4,-72.0114432535103,-176.064396375895));
#144201=CARTESIAN_POINT('Ctrl Pts',(-7.91428825612723,-72.198695730848,
-176.6012613201));
#144202=CARTESIAN_POINT('Ctrl Pts',(-7.40000000000231,-72.2090331198025,
-176.611745838634));
#144203=CARTESIAN_POINT('Ctrl Pts',(-7.4,-71.8455797798041,-176.246702589259));
#144204=CARTESIAN_POINT('Ctrl Pts',(-7.91496944868021,-72.0919119068452,
-176.702452310058));
#144205=CARTESIAN_POINT('Ctrl Pts',(-7.40000000000137,-72.1022117673413,
-176.713954380549));
#144206=CARTESIAN_POINT('Ctrl Pts',(-7.4,-71.7565932593015,-176.331051292497));
#144207=CARTESIAN_POINT('Ctrl Pts',(-7.91685114292327,-71.7500603021656,
-176.981869807169));
#144208=CARTESIAN_POINT('Ctrl Pts',(-7.39999999999722,-71.7595719221786,
-176.996603847265));
#144209=CARTESIAN_POINT('Ctrl Pts',(-7.4,-71.4717169212771,-176.56396241752));
#144210=CARTESIAN_POINT('Ctrl Pts',(-7.91789548135802,-71.4896799957509,
-177.136789521634));
#144211=CARTESIAN_POINT('Ctrl Pts',(-7.39999999999657,-71.4982684775377,
-177.153312936568));
#144212=CARTESIAN_POINT('Ctrl Pts',(-7.4,-71.2547332556153,-176.693097313134));
#144213=CARTESIAN_POINT('Ctrl Pts',(-7.91864558019502,-71.2187040784628,
-177.248023282853));
#144214=CARTESIAN_POINT('Ctrl Pts',(-7.39999999999996,-71.2260554869631,
-177.265927135801));
#144215=CARTESIAN_POINT('Ctrl Pts',(-7.4,-71.028920068719,-176.785817298486));
#144216=CARTESIAN_POINT('Origin',(-7.9,-72.58000002,-174.471034982976));
#144217=CARTESIAN_POINT('Ctrl Pts',(-6.84687749809456,-70.9710952348089,
-171.449026400902));
#144218=CARTESIAN_POINT('Ctrl Pts',(-7.39999999999995,-70.9175980522952,
-171.474145745141));
#144219=CARTESIAN_POINT('Ctrl Pts',(-7.4,-71.4211246238516,-171.237717270032));
#144220=CARTESIAN_POINT('Ctrl Pts',(-6.84335093752903,-71.0335272731666,
-171.581102626116));
#144221=CARTESIAN_POINT('Ctrl Pts',(-7.40000000000424,-70.9726288200743,
-171.600718024433));
#144222=CARTESIAN_POINT('Ctrl Pts',(-7.4,-71.5141496698322,-171.435834655863));
#144223=CARTESIAN_POINT('Ctrl Pts',(-6.84152542419482,-71.0660673850682,
-171.724228262147));
#144224=CARTESIAN_POINT('Ctrl Pts',(-7.39999999999997,-71.0003029730699,
-171.734045906264));
#144225=CARTESIAN_POINT('Ctrl Pts',(-7.4,-71.5626363329153,-171.650517772678));
#144226=CARTESIAN_POINT('Ctrl Pts',(-6.84152542372878,-71.066067385123,
-171.871644662643));
#144227=CARTESIAN_POINT('Ctrl Pts',(-7.39999999999996,-71.0003029749948,
-171.871644662643));
#144228=CARTESIAN_POINT('Ctrl Pts',(-7.4,-71.5626363369615,-171.871644662643));
#144229=CARTESIAN_POINT('Origin',(-6.9,-71.4211246238516,-171.237717270032));
#144230=CARTESIAN_POINT('Origin',(0.,-12.9675000200281,-171.64995));
#144231=CARTESIAN_POINT('',(-1.23668893165473,-55.0504165218146,-136.482360813851));
#144232=CARTESIAN_POINT('Ctrl Pts',(-1.23668893165476,-55.0504165218146,
-136.482360813851));
#144233=CARTESIAN_POINT('Ctrl Pts',(-1.23673299366641,-55.1913381585796,
-136.784440607054));
#144234=CARTESIAN_POINT('Ctrl Pts',(-1.23677661819369,-55.3322593149882,
-137.08652062441));
#144235=CARTESIAN_POINT('Ctrl Pts',(-1.23699261729668,-56.0368627647092,
-138.596921799561));
#144236=CARTESIAN_POINT('Ctrl Pts',(-1.23715863033152,-56.6005380707885,
-139.805246217854));
#144237=CARTESIAN_POINT('Ctrl Pts',(-1.23731859936897,-57.1642067307399,
-141.01357373723));
#144238=CARTESIAN_POINT('Ctrl Pts',(-1.23795847551899,-59.4188813711729,
-145.84688381608));
#144239=CARTESIAN_POINT('Ctrl Pts',(-1.23850317159002,-61.6734513223852,
-150.68024274455));
#144240=CARTESIAN_POINT('Ctrl Pts',(-1.23898586311735,-63.927952799307,
-155.513633616344));
#144241=CARTESIAN_POINT('Ctrl Pts',(-1.23951632777425,-66.4055876545563,
-160.825396689281));
#144242=CARTESIAN_POINT('Ctrl Pts',(-1.23997137264739,-68.8831392394364,
-166.137198611174));
#144243=CARTESIAN_POINT('Ctrl Pts',(-1.24037635835043,-71.360635368318,
-171.449026400902));
#144244=CARTESIAN_POINT('',(-6.82752390438728,-55.1067946098355,-137.742762001241));
#144245=CARTESIAN_POINT('Ctrl Pts',(-6.82752390105444,-55.106794611208,
-137.742762010959));
#144246=CARTESIAN_POINT('Ctrl Pts',(-6.37447262318503,-55.0992223452637,
-137.571341088341));
#144247=CARTESIAN_POINT('Ctrl Pts',(-5.91551255237738,-55.0922385931689,
-137.414112752179));
#144248=CARTESIAN_POINT('Ctrl Pts',(-4.97306841018422,-55.0794633322322,
-137.127585972214));
#144249=CARTESIAN_POINT('Ctrl Pts',(-4.48820368733454,-55.0737025194561,
-136.999007240366));
#144250=CARTESIAN_POINT('Ctrl Pts',(-3.08479586460781,-55.0595407739023,
-136.68378809349));
#144251=CARTESIAN_POINT('Ctrl Pts',(-2.16238887065941,-55.0533427639956,
-136.546951183472));
#144252=CARTESIAN_POINT('Ctrl Pts',(-1.23668893165476,-55.0504165218146,
-136.482360813851));
#144253=CARTESIAN_POINT('Ctrl Pts',(-6.84687749809456,-70.9710952348089,
-171.449026400902));
#144254=CARTESIAN_POINT('Ctrl Pts',(-6.84214680864307,-65.6936814169362,
-160.208420694676));
#144255=CARTESIAN_POINT('Ctrl Pts',(-6.83631983013148,-60.409494445995,
-148.971070239119));
#144256=CARTESIAN_POINT('Ctrl Pts',(-6.82752390105444,-55.106794611208,
-137.742762010959));
#144257=CARTESIAN_POINT('Ctrl Pts',(-1.23940677966098,-71.4543692372681,
-171.871644662643));
#144258=CARTESIAN_POINT('Ctrl Pts',(-0.749999999999965,-71.4647403528508,
-171.871644662643));
#144259=CARTESIAN_POINT('Ctrl Pts',(-0.749999999999965,-71.9542570083556,
-171.871644662643));
#144260=CARTESIAN_POINT('Ctrl Pts',(-1.23940678000784,-71.4543692372607,
-171.725769781663));
#144261=CARTESIAN_POINT('Ctrl Pts',(-0.749999999999918,-71.4647403416089,
-171.724250912112));
#144262=CARTESIAN_POINT('Ctrl Pts',(-0.749999999999965,-71.9542569918424,
-171.652832243085));
#144263=CARTESIAN_POINT('Ctrl Pts',(-1.23973038817724,-71.4229357713421,
-171.582570495172));
#144264=CARTESIAN_POINT('Ctrl Pts',(-0.749999999994911,-71.432604194084,
-171.579497326419));
#144265=CARTESIAN_POINT('Ctrl Pts',(-0.749999999999965,-71.9071171402653,
-171.43803354201));
#144266=CARTESIAN_POINT('Ctrl Pts',(-1.24037635835043,-71.360635368318,
-171.449026400902));
#144267=CARTESIAN_POINT('Ctrl Pts',(-0.749999999999965,-71.3691907154173,
-171.445036077089));
#144268=CARTESIAN_POINT('Ctrl Pts',(-0.749999999999965,-71.813687061541,
-171.237717270032));
#144269=CARTESIAN_POINT('Origin',(-1.24999999999996,-71.813687061541,-171.237717270032));
#144270=CARTESIAN_POINT('Origin',(-25.7,-66.1031295107182,-179.64995));
#144271=CARTESIAN_POINT('Origin',(-25.7,-66.1031295107182,-176.84995));
#144272=CARTESIAN_POINT('Origin',(-25.7,-66.1031295107182,-171.854014632589));
#144273=CARTESIAN_POINT('Ctrl Pts',(-25.2,-66.1031295107182,-176.84995));
#144274=CARTESIAN_POINT('Ctrl Pts',(-25.2,-65.7373527968361,-176.84995));
#144275=CARTESIAN_POINT('Ctrl Pts',(-25.548606520496,-65.6266003779638,
-176.84995));
#144276=CARTESIAN_POINT('Ctrl Pts',(-25.2,-66.103129518477,-176.919185448026));
#144277=CARTESIAN_POINT('Ctrl Pts',(-25.1999999820547,-65.7373528064706,
-176.935176476617));
#144278=CARTESIAN_POINT('Ctrl Pts',(-25.5486064910184,-65.6266003873288,
-176.988420898571));
#144279=CARTESIAN_POINT('Ctrl Pts',(-25.1851215566574,-66.1120606092764,
-176.989079172076));
#144280=CARTESIAN_POINT('Ctrl Pts',(-25.1785584539962,-65.7486947399145,
-177.021615691098));
#144281=CARTESIAN_POINT('Ctrl Pts',(-25.5128982512925,-65.6373177084965,
-177.128208340634));
#144282=CARTESIAN_POINT('Ctrl Pts',(-25.1297698837022,-66.151663029906,
-177.114520781302));
#144283=CARTESIAN_POINT('Ctrl Pts',(-25.0944218125655,-65.7952388640609,
-177.17698788051));
#144284=CARTESIAN_POINT('Ctrl Pts',(-25.3800542465628,-65.6848405887261,
-177.37909156612));
#144285=CARTESIAN_POINT('Ctrl Pts',(-25.0892600555381,-66.1826911909829,
-177.170686801435));
#144286=CARTESIAN_POINT('Ctrl Pts',(-25.0308899200954,-65.8308593817032,
-177.246991922054));
#144287=CARTESIAN_POINT('Ctrl Pts',(-25.2828559308331,-65.7220623109706,
-177.491403988801));
#144288=CARTESIAN_POINT('Ctrl Pts',(-25.0407404589729,-66.228934721057,
-177.2158679411));
#144289=CARTESIAN_POINT('Ctrl Pts',(-24.9516549782085,-65.8798945343464,
-177.298823774072));
#144290=CARTESIAN_POINT('Ctrl Pts',(-25.166383622031,-65.7775666303703,
-177.581785882201));
#144291=CARTESIAN_POINT('Ctrl Pts',(-25.0407404589729,-66.228934721057,
-177.2158679411));
#144292=CARTESIAN_POINT('Ctrl Pts',(-25.0892600555381,-66.1826911909829,
-177.170686801435));
#144293=CARTESIAN_POINT('Ctrl Pts',(-25.1297698837022,-66.151663029906,
-177.114520781302));
#144294=CARTESIAN_POINT('Ctrl Pts',(-25.1851215566574,-66.1120606092764,
-176.989079172076));
#144295=CARTESIAN_POINT('Ctrl Pts',(-25.2,-66.103129518477,-176.919185448026));
#144296=CARTESIAN_POINT('Ctrl Pts',(-25.2,-66.1031295107182,-176.84995));
#144297=CARTESIAN_POINT('Ctrl Pts',(-26.0394480946395,-65.5149709682657,
-172.038055421481));
#144298=CARTESIAN_POINT('Ctrl Pts',(-26.1751497442534,-65.4958993451585,
-171.625426858395));
#144299=CARTESIAN_POINT('Ctrl Pts',(-26.2234488624093,-65.1680142434972,
-171.34400271074));
#144300=CARTESIAN_POINT('Ctrl Pts',(-25.8509081007284,-65.5414685363847,
-171.953748619745));
#144301=CARTESIAN_POINT('Ctrl Pts',(-25.9647846003821,-65.5168153550888,
-171.580148440091));
#144302=CARTESIAN_POINT('Ctrl Pts',(-25.9874436760592,-65.2410608891827,
-171.301817192477));
#144303=CARTESIAN_POINT('Ctrl Pts',(-25.6648820617275,-65.585552959265,
-171.879293448435));
#144304=CARTESIAN_POINT('Ctrl Pts',(-25.7473133163572,-65.5608787626348,
-171.533711217624));
#144305=CARTESIAN_POINT('Ctrl Pts',(-25.7492812072149,-65.3269811309762,
-171.264627955552));
#144306=CARTESIAN_POINT('Ctrl Pts',(-25.4789353138755,-65.6496769315936,
-171.836539704699));
#144307=CARTESIAN_POINT('Ctrl Pts',(-25.5297569849445,-65.6321510137328,
-171.506776385146));
#144308=CARTESIAN_POINT('Ctrl Pts',(-25.5048932192108,-65.4282717079069,
-171.24324485235));
#144309=CARTESIAN_POINT('',(-25.5241645957023,-65.4203114663316,-171.244965273982));
#144310=CARTESIAN_POINT('',(-26.2234488624093,-65.1680142434972,-171.34400271074));
#144311=CARTESIAN_POINT('Ctrl Pts',(-25.5241645957028,-65.4203114663335,
-171.244965273985));
#144312=CARTESIAN_POINT('Ctrl Pts',(-25.7618083043786,-65.3224706961895,
-171.266588348947));
#144313=CARTESIAN_POINT('Ctrl Pts',(-25.9936511816685,-65.2391401680605,
-171.302927382557));
#144314=CARTESIAN_POINT('Ctrl Pts',(-26.2234488624093,-65.1680142434972,
-171.34400271074));
#144315=CARTESIAN_POINT('Origin',(-25.9002749936795,-64.5247028995241,-172.038055421481));
#144316=CARTESIAN_POINT('Ctrl Pts',(-25.5241645957028,-65.4203114663335,
-171.244965273984));
#144317=CARTESIAN_POINT('Ctrl Pts',(-25.5204167023824,-65.4915081760158,
-171.329224126564));
#144318=CARTESIAN_POINT('Ctrl Pts',(-25.5190396326646,-65.5455021430107,
-171.42367336987));
#144319=CARTESIAN_POINT('Ctrl Pts',(-25.5254918386358,-65.6165368852731,
-171.632443841085));
#144320=CARTESIAN_POINT('Ctrl Pts',(-25.5332781069629,-65.6314702205409,
-171.740892625582));
#144321=CARTESIAN_POINT('Ctrl Pts',(-25.5486065204936,-65.6266003779646,
-171.854014632593));
#144322=CARTESIAN_POINT('Origin',(-24.7,-73.08000002,-176.84995));
#144323=CARTESIAN_POINT('',(-24.7,-70.08000002,-177.34995));
#144324=CARTESIAN_POINT('',(-24.7,-73.08000002,-177.34995));
#144325=CARTESIAN_POINT('Origin',(-24.7,-70.08000002,-176.84995));
#144326=CARTESIAN_POINT('Origin',(-41.5,-73.08000002,-177.34995));
#144327=CARTESIAN_POINT('',(41.5,-70.08000002,-177.34995));
#144328=CARTESIAN_POINT('Ctrl Pts',(-1.23668893165476,-55.0504165218147,
-95.5762821576554));
#144329=CARTESIAN_POINT('Ctrl Pts',(-0.749999999999964,-55.0621625368994,
-95.581761778993));
#144330=CARTESIAN_POINT('Ctrl Pts',(-0.749999999999971,-55.5033748716332,
-95.7875912885257));
#144331=CARTESIAN_POINT('Ctrl Pts',(-1.23837727019305,-60.4501569855996,
-84.0013918846235));
#144332=CARTESIAN_POINT('Ctrl Pts',(-0.750000000108156,-60.4692939396047,
-83.9872370540609));
#144333=CARTESIAN_POINT('Ctrl Pts',(-0.749999999999969,-60.9031648374056,
-84.2127012585751));
#144334=CARTESIAN_POINT('Ctrl Pts',(-1.23947201783252,-65.8492492116834,
-72.4261878753526));
#144335=CARTESIAN_POINT('Ctrl Pts',(-0.749999999981978,-65.8633206076967,
-72.4204079747872));
#144336=CARTESIAN_POINT('Ctrl Pts',(-0.749999999999967,-66.3022815738571,
-72.6374971882577));
#144337=CARTESIAN_POINT('Ctrl Pts',(-1.24035792914739,-71.2481103336038,
-60.8508735991007));
#144338=CARTESIAN_POINT('Ctrl Pts',(-0.749999999999965,-71.2566817467536,
-60.8548714197835));
#144339=CARTESIAN_POINT('Ctrl Pts',(-0.749999999999965,-71.701161634982,
-61.062182729971));
#144340=CARTESIAN_POINT('Origin',(-1.24999999999997,-55.5033748716332,-95.7875912885257));
#144341=CARTESIAN_POINT('Ctrl Pts',(-1.24037635835043,-71.360635368318,
-171.449026400902));
#144342=CARTESIAN_POINT('Ctrl Pts',(-0.749999999999976,-71.3691907154172,
-171.445036077089));
#144343=CARTESIAN_POINT('Ctrl Pts',(-0.749999999999965,-71.813687061541,
-171.237717270032));
#144344=CARTESIAN_POINT('Ctrl Pts',(-1.23948769887611,-65.9242696435089,
-159.793291324051));
#144345=CARTESIAN_POINT('Ctrl Pts',(-0.74999999977637,-65.9383759687714,
-159.799181671811));
#144346=CARTESIAN_POINT('Ctrl Pts',(-0.749999999999967,-66.3773023734559,
-159.58198200727));
#144347=CARTESIAN_POINT('Ctrl Pts',(-1.23838899982829,-60.4876714538986,
-148.137667147083));
#144348=CARTESIAN_POINT('Ctrl Pts',(-0.749999999843541,-60.5069208340151,
-148.152089356292));
#144349=CARTESIAN_POINT('Ctrl Pts',(-0.74999999999997,-60.9406796476674,
-147.926357767621));
#144350=CARTESIAN_POINT('Ctrl Pts',(-1.23668893165476,-55.0504165218146,
-136.482360813851));
#144351=CARTESIAN_POINT('Ctrl Pts',(-0.749999999999973,-55.0621625368995,
-136.476881192513));
#144352=CARTESIAN_POINT('Ctrl Pts',(-0.749999999999973,-55.5033748716332,
-136.27105168298));
#144353=CARTESIAN_POINT('Origin',(-1.24999999999997,-55.5033748716332,-136.27105168298));
#144354=CARTESIAN_POINT('Ctrl Pts',(-0.749999999999973,-55.08000002,-134.362052670054));
#144355=CARTESIAN_POINT('Ctrl Pts',(-0.749999999999966,-54.5800000199999,
-134.362052670054));
#144356=CARTESIAN_POINT('Ctrl Pts',(-1.24999999999997,-54.58000002,-134.362052670054));
#144357=CARTESIAN_POINT('Ctrl Pts',(-0.749999999999973,-55.0800000255278,
-135.020977206459));
#144358=CARTESIAN_POINT('Ctrl Pts',(-0.750000000006689,-54.5841777042435,
-135.09091556402));
#144359=CARTESIAN_POINT('Ctrl Pts',(-1.24580493030994,-54.58000002,-135.093949837831));
#144360=CARTESIAN_POINT('Ctrl Pts',(-0.749999999999973,-55.2219738253108,
-135.667845593964));
#144361=CARTESIAN_POINT('Ctrl Pts',(-0.74999999999389,-54.744924951658,
-135.807520949259));
#144362=CARTESIAN_POINT('Ctrl Pts',(-1.24129514745974,-54.7377489917927,
-135.812422632741));
#144363=CARTESIAN_POINT('Ctrl Pts',(-0.749999999999973,-55.5033748716332,
-136.27105168298));
#144364=CARTESIAN_POINT('Ctrl Pts',(-0.749999999999978,-55.0621625368994,
-136.476881192513));
#144365=CARTESIAN_POINT('Ctrl Pts',(-1.23668893165479,-55.0504165218146,
-136.482360813851));
#144366=CARTESIAN_POINT('',(-1.2499999994373,-54.58000002,-134.362052687297));
#144367=CARTESIAN_POINT('Origin',(-1.24999999999997,-55.08000002,-134.362052670054));
#144368=CARTESIAN_POINT('Origin',(-1.23487154781912,-62.0135240636403,-133.822664549727));
#144369=CARTESIAN_POINT('Origin',(-1.24999999999997,-55.08000002,-55.24995));
#144370=CARTESIAN_POINT('',(-1.24999998181205,-54.5800000199982,-97.6965897229033));
#144371=CARTESIAN_POINT('Origin',(-1.24999999999997,-55.08000002,-97.6965903014517));
#144372=CARTESIAN_POINT('',(-1.24999999999997,-54.58000002,-134.339054731985));
#144373=CARTESIAN_POINT('Ctrl Pts',(-0.749999999999973,-55.5033748716332,
-95.7875912885257));
#144374=CARTESIAN_POINT('Ctrl Pts',(-0.749999999999967,-55.0621625368995,
-95.5817617789931));
#144375=CARTESIAN_POINT('Ctrl Pts',(-1.23668893165476,-55.0504165218147,
-95.5762821576554));
#144376=CARTESIAN_POINT('Ctrl Pts',(-0.749999999999973,-55.2248025687359,
-96.3847337445855));
#144377=CARTESIAN_POINT('Ctrl Pts',(-0.750000000004237,-54.7481304442385,
-96.2443585547261));
#144378=CARTESIAN_POINT('Ctrl Pts',(-1.24124884403065,-54.7408920390033,
-96.2394858776278));
#144379=CARTESIAN_POINT('Ctrl Pts',(-0.749999999999973,-55.0800000216326,
-97.0309759697293));
#144380=CARTESIAN_POINT('Ctrl Pts',(-0.75000000000672,-54.5842199033567,
-96.9603643458105));
#144381=CARTESIAN_POINT('Ctrl Pts',(-1.24576233955167,-54.58000002,-96.9572624945429));
#144382=CARTESIAN_POINT('Ctrl Pts',(-0.749999999999973,-55.08000002,-97.6965903014517));
#144383=CARTESIAN_POINT('Ctrl Pts',(-0.749999999999965,-54.5800000199999,
-97.6965903014516));
#144384=CARTESIAN_POINT('Ctrl Pts',(-1.25,-54.58000002,-97.6965903014517));
#144385=CARTESIAN_POINT('Origin',(-1.23485323729605,-62.0131682900771,-98.2327688037691));
#144386=CARTESIAN_POINT('Ctrl Pts',(-6.8604212943599,-55.1073456615429,
-94.3034047511324));
#144387=CARTESIAN_POINT('Ctrl Pts',(-7.2042299691157,-54.58000002,-95.3011321772634));
#144388=CARTESIAN_POINT('Ctrl Pts',(-7.58857520038279,-54.58000002,-96.4164960598359));
#144389=CARTESIAN_POINT('Ctrl Pts',(-5.93585888223459,-55.0918247516195,
-94.6548535475511));
#144390=CARTESIAN_POINT('Ctrl Pts',(-6.23607825680947,-54.580000019985,
-95.6541184528592));
#144391=CARTESIAN_POINT('Ctrl Pts',(-6.56867789944001,-54.58000002,-96.7679442920248));
#144392=CARTESIAN_POINT('Ctrl Pts',(-4.99263467931988,-55.0788453329258,
-94.9451426129372));
#144393=CARTESIAN_POINT('Ctrl Pts',(-5.24614565799262,-54.58000002,-95.9461039187036));
#144394=CARTESIAN_POINT('Ctrl Pts',(-5.52653095835546,-54.58000002,-97.0582339217052));
#144395=CARTESIAN_POINT('Ctrl Pts',(-3.06075099962147,-55.0592467101081,
-95.3814216329573));
#144396=CARTESIAN_POINT('Ctrl Pts',(-3.21753929952213,-54.58000002,-96.3846721597723));
#144397=CARTESIAN_POINT('Ctrl Pts',(-3.38973164031852,-54.58000002,-97.4945129415963));
#144398=CARTESIAN_POINT('Ctrl Pts',(-2.0669285329079,-55.052711592208,-95.5256220795631));
#144399=CARTESIAN_POINT('Ctrl Pts',(-2.17279343333145,-54.5800000200112,
-96.5297363078781));
#144400=CARTESIAN_POINT('Ctrl Pts',(-2.28937244057036,-54.58000002,-97.638711952094));
#144401=CARTESIAN_POINT('Ctrl Pts',(-1.09375770007614,-55.0499908864773,
-95.5856784364438));
#144402=CARTESIAN_POINT('Ctrl Pts',(-1.14972373305894,-54.5800000199999,
-96.5901184946094));
#144403=CARTESIAN_POINT('Ctrl Pts',(-1.21149627184771,-54.58000002,-97.6987697451473));
#144404=CARTESIAN_POINT('',(-6.9,-54.58000002,-96.6432622057672));
#144405=CARTESIAN_POINT('Ctrl Pts',(-6.9,-54.5800000200288,-96.6432622057672));
#144406=CARTESIAN_POINT('Ctrl Pts',(-6.49061970139217,-54.5800000200775,
-96.7718187571058));
#144407=CARTESIAN_POINT('Ctrl Pts',(-6.07861873660027,-54.5800000205753,
-96.8899526380548));
#144408=CARTESIAN_POINT('Ctrl Pts',(-5.66396816650188,-54.5800000217474,
-96.9971605311361));
#144409=CARTESIAN_POINT('Ctrl Pts',(-5.26447645459909,-54.5800000228767,
-97.100449101863));
#144410=CARTESIAN_POINT('Ctrl Pts',(-4.86252531660949,-54.5800000241933,
-97.1935960044572));
#144411=CARTESIAN_POINT('Ctrl Pts',(-4.45809517257588,-54.5800000232613,
-97.2761964906685));
#144412=CARTESIAN_POINT('Ctrl Pts',(-4.34240961804981,-54.5800000229947,
-97.2998240149577));
#144413=CARTESIAN_POINT('Ctrl Pts',(-4.22645442245894,-54.5800000225654,
-97.3225679069059));
#144414=CARTESIAN_POINT('Ctrl Pts',(-4.1103033922506,-54.5800000220553,
-97.3444205163838));
#144415=CARTESIAN_POINT('Ctrl Pts',(-3.87438492650358,-54.5800000210192,
-97.3888061244265));
#144416=CARTESIAN_POINT('Ctrl Pts',(-3.63765702198839,-54.580000020604,
-97.4294862943975));
#144417=CARTESIAN_POINT('Ctrl Pts',(-3.4002729301617,-54.5800000203617,
-97.466451043988));
#144418=CARTESIAN_POINT('Ctrl Pts',(-3.16793216733923,-54.5800000201245,
-97.502630461283));
#144419=CARTESIAN_POINT('Ctrl Pts',(-2.93496148468305,-54.5800000200661,
-97.5352507112809));
#144420=CARTESIAN_POINT('Ctrl Pts',(-2.70149448625264,-54.5800000200335,
-97.5642527645727));
#144421=CARTESIAN_POINT('Ctrl Pts',(-2.47413670468755,-54.5800000200018,
-97.5924959104631));
#144422=CARTESIAN_POINT('Ctrl Pts',(-2.24630713852154,-54.580000020002,
-97.617307762456));
#144423=CARTESIAN_POINT('Ctrl Pts',(-2.01813705515799,-54.5800000200007,
-97.6385856637395));
#144424=CARTESIAN_POINT('Ctrl Pts',(-1.80087152563782,-54.5800000199995,
-97.6588466656259));
#144425=CARTESIAN_POINT('Ctrl Pts',(-1.5832964702307,-54.58000002,-97.6759032884734));
#144426=CARTESIAN_POINT('Ctrl Pts',(-1.36554569823268,-54.58000002,-97.6896238013577));
#144427=CARTESIAN_POINT('Ctrl Pts',(-1.32703559408406,-54.58000002,-97.6920503295178));
#144428=CARTESIAN_POINT('Ctrl Pts',(-1.28852006462875,-54.58000002,-97.6943724020827));
#144429=CARTESIAN_POINT('Ctrl Pts',(-1.24999994858807,-54.58000002,-97.6965891455738));
#144430=CARTESIAN_POINT('Ctrl Pts',(-6.9,-54.58000002,-96.6432622057672));
#144431=CARTESIAN_POINT('Ctrl Pts',(-6.8883412776675,-54.58000002,-96.2390470799649));
#144432=CARTESIAN_POINT('Ctrl Pts',(-6.87644795534686,-54.6248256750472,
-95.842546745885));
#144433=CARTESIAN_POINT('Ctrl Pts',(-6.86432673276943,-54.7125511587359,
-95.4535552447955));
#144434=CARTESIAN_POINT('Ctrl Pts',(-6.85220551051008,-54.8002766401224,
-95.0645637539141));
#144435=CARTESIAN_POINT('Ctrl Pts',(-6.83977061823003,-54.9324757175662,
-94.6806963775948));
#144436=CARTESIAN_POINT('Ctrl Pts',(-6.82752390201859,-55.1067945974843,
-94.3158809892684));
#144437=CARTESIAN_POINT('Ctrl Pts',(-6.84677576889373,-70.8578246683297,
-60.8508735991007));
#144438=CARTESIAN_POINT('Ctrl Pts',(-7.39999999999997,-70.8042142666047,
-60.8257004209668));
#144439=CARTESIAN_POINT('Ctrl Pts',(-7.4,-71.3078420373655,-61.0621827299711));
#144440=CARTESIAN_POINT('Ctrl Pts',(-6.84206094040904,-65.61805576689,-72.0110063808198));
#144441=CARTESIAN_POINT('Ctrl Pts',(-7.39999999999996,-65.5311408351844,
-72.0430210271706));
#144442=CARTESIAN_POINT('Ctrl Pts',(-7.4,-66.0675133276181,-72.2223201517098));
#144443=CARTESIAN_POINT('Ctrl Pts',(-6.83625690025051,-60.3715570323219,
-83.1679040708394));
#144444=CARTESIAN_POINT('Ctrl Pts',(-7.39999999995234,-60.2531402990131,
-83.2491486934777));
#144445=CARTESIAN_POINT('Ctrl Pts',(-7.4,-60.8202894597531,-83.3792196747323));
#144446=CARTESIAN_POINT('Ctrl Pts',(-6.82752390105444,-55.106794611208,
-94.3158809605474));
#144447=CARTESIAN_POINT('Ctrl Pts',(-7.39999999999997,-55.0309624818203,
-94.2800587259558));
#144448=CARTESIAN_POINT('Ctrl Pts',(-7.4,-55.5541151520872,-94.5271900914177));
#144449=CARTESIAN_POINT('Origin',(-6.9,-55.5541151520872,-94.5271900914178));
#144450=CARTESIAN_POINT('Ctrl Pts',(-7.4,-55.08000002,-96.6432622057672));
#144451=CARTESIAN_POINT('Ctrl Pts',(-7.39999999999996,-54.58000002,-96.6432622057672));
#144452=CARTESIAN_POINT('Ctrl Pts',(-6.9,-54.58000002,-96.6432622057672));
#144453=CARTESIAN_POINT('Ctrl Pts',(-7.4,-55.0800000228223,-96.276173584436));
#144454=CARTESIAN_POINT('Ctrl Pts',(-7.39999999999997,-54.5682037738145,
-96.2342789461818));
#144455=CARTESIAN_POINT('Ctrl Pts',(-6.8883412776675,-54.58000002,-96.2390470799649));
#144456=CARTESIAN_POINT('Ctrl Pts',(-7.4,-55.1203431091477,-95.9158883524807));
#144457=CARTESIAN_POINT('Ctrl Pts',(-7.39999999999997,-54.6014014206736,
-95.8348803330818));
#144458=CARTESIAN_POINT('Ctrl Pts',(-6.87644795534686,-54.6248256750472,
-95.842546745885));
#144459=CARTESIAN_POINT('Ctrl Pts',(-7.4,-55.2782489805768,-95.2085406483778));
#144460=CARTESIAN_POINT('Ctrl Pts',(-7.39999999999995,-54.7508604913788,
-95.0452270964761));
#144461=CARTESIAN_POINT('Ctrl Pts',(-6.85220551019199,-54.8002766424245,
-95.064563743706));
#144462=CARTESIAN_POINT('Ctrl Pts',(-7.4,-55.3972278356279,-94.8593050327909));
#144463=CARTESIAN_POINT('Ctrl Pts',(-7.39999999999369,-54.8709621105524,
-94.6521767160421));
#144464=CARTESIAN_POINT('Ctrl Pts',(-6.83977061757738,-54.9324757245047,
-94.6806963574476));
#144465=CARTESIAN_POINT('Ctrl Pts',(-7.4,-55.5541151520872,-94.5271900914177));
#144466=CARTESIAN_POINT('Ctrl Pts',(-7.39999999999997,-55.0309624818203,
-94.2800587259558));
#144467=CARTESIAN_POINT('Ctrl Pts',(-6.82752390105444,-55.106794611208,
-94.3158809605474));
#144468=CARTESIAN_POINT('Origin',(-6.9,-55.08000002,-96.6432622057672));
#144469=CARTESIAN_POINT('Origin',(-6.9,-55.08000002,-55.24995));
#144470=CARTESIAN_POINT('',(-6.9,-54.58000002,-135.415380765739));
#144471=CARTESIAN_POINT('Origin',(-6.9,-55.08000002,-135.415380765739));
#144472=CARTESIAN_POINT('',(-6.9,-54.58000002,-96.4806904787158));
#144473=CARTESIAN_POINT('Ctrl Pts',(-7.4,-55.569842315739,-137.564432008667));
#144474=CARTESIAN_POINT('Ctrl Pts',(-7.40000000000011,-55.0472163216404,
-137.816090401511));
#144475=CARTESIAN_POINT('Ctrl Pts',(-6.82627940990429,-55.1242727612674,
-137.778985645859));
#144476=CARTESIAN_POINT('Ctrl Pts',(-7.4,-55.4051297298433,-137.222270602494));
#144477=CARTESIAN_POINT('Ctrl Pts',(-7.39999999999862,-54.8790351803965,
-137.432659902946));
#144478=CARTESIAN_POINT('Ctrl Pts',(-6.8389262967378,-54.941259203202,-137.403152734529));
#144479=CARTESIAN_POINT('Ctrl Pts',(-7.4,-55.2827981883505,-136.868178474904));
#144480=CARTESIAN_POINT('Ctrl Pts',(-7.39999999999997,-54.7552910012621,
-137.033997183801));
#144481=CARTESIAN_POINT('Ctrl Pts',(-6.85155371766594,-54.805333739172,
-137.013956482872));
#144482=CARTESIAN_POINT('Ctrl Pts',(-7.4,-55.1186770997702,-136.137553696396));
#144483=CARTESIAN_POINT('Ctrl Pts',(-7.39999999999997,-54.5997930545306,
-136.218266932015));
#144484=CARTESIAN_POINT('Ctrl Pts',(-6.87660583005939,-54.6229757043942,
-136.210378498132));
#144485=CARTESIAN_POINT('Ctrl Pts',(-7.4,-55.0773024992163,-135.758275388548));
#144486=CARTESIAN_POINT('Ctrl Pts',(-7.40000000000133,-54.5659876123841,
-135.797876258651));
#144487=CARTESIAN_POINT('Ctrl Pts',(-6.88911403108312,-54.5770033281604,
-135.792971583838));
#144488=CARTESIAN_POINT('Ctrl Pts',(-7.4,-55.0801363807228,-135.378851871089));
#144489=CARTESIAN_POINT('Ctrl Pts',(-7.39999999999985,-54.581282028365,
-135.375165330398));
#144490=CARTESIAN_POINT('Ctrl Pts',(-6.90113321290139,-54.5801514737049,
-135.375156474088));
#144491=CARTESIAN_POINT('Origin',(-6.9,-55.5541151520872,-137.531452880088));
#144492=CARTESIAN_POINT('Ctrl Pts',(-6.82752391167578,-55.1067946098897,
-137.742761979991));
#144493=CARTESIAN_POINT('Ctrl Pts',(-6.83099153048951,-55.0574368043954,
-137.639465676912));
#144494=CARTESIAN_POINT('Ctrl Pts',(-6.83446840923335,-55.0116501943323,
-137.535137214437));
#144495=CARTESIAN_POINT('Ctrl Pts',(-6.83793753742844,-54.9693403128155,
-137.429833297904));
#144496=CARTESIAN_POINT('Ctrl Pts',(-6.84144322128202,-54.9265845943354,
-137.323419749845));
#144497=CARTESIAN_POINT('Ctrl Pts',(-6.84494129126791,-54.887378543277,
-137.216009330928));
#144498=CARTESIAN_POINT('Ctrl Pts',(-6.84842852672726,-54.851659632403,
-137.10762244633));
#144499=CARTESIAN_POINT('Ctrl Pts',(-6.85194224941648,-54.8156694192284,
-136.998412311235));
#144500=CARTESIAN_POINT('Ctrl Pts',(-6.85544530921929,-54.7832189819739,
-136.888209905991));
#144501=CARTESIAN_POINT('Ctrl Pts',(-6.85894403334902,-54.7542891926763,
-136.777010277306));
#144502=CARTESIAN_POINT('Ctrl Pts',(-6.86066524620696,-54.7400570544824,
-136.72230512663));
#144503=CARTESIAN_POINT('Ctrl Pts',(-6.86238552435822,-54.7266777157171,
-136.667358321512));
#144504=CARTESIAN_POINT('Ctrl Pts',(-6.86410608128596,-54.7141533541175,
-136.612168082043));
#144505=CARTESIAN_POINT('Ctrl Pts',(-6.86788574855968,-54.686640216424,
-136.490927837918));
#144506=CARTESIAN_POINT('Ctrl Pts',(-6.8716696820525,-54.6632062886195,
-136.368281734253));
#144507=CARTESIAN_POINT('Ctrl Pts',(-6.87543688800749,-54.6440113887563,
-136.244623751257));
#144508=CARTESIAN_POINT('Ctrl Pts',(-6.87918616660092,-54.6249078334902,
-136.121554231276));
#144509=CARTESIAN_POINT('Ctrl Pts',(-6.88291869407914,-54.6100032909578,
-135.997482854682));
#144510=CARTESIAN_POINT('Ctrl Pts',(-6.88662022495319,-54.5994096525472,
-135.872820988136));
#144511=CARTESIAN_POINT('Ctrl Pts',(-6.89030244377386,-54.5888712844875,
-135.748809521845));
#144512=CARTESIAN_POINT('Ctrl Pts',(-6.8939538237197,-54.5825991054037,
-135.624214165788));
#144513=CARTESIAN_POINT('Ctrl Pts',(-6.89756933233812,-54.5806551119451,
-135.499456180952));
#144514=CARTESIAN_POINT('Ctrl Pts',(-6.89838131639757,-54.5802185228322,
-135.471437579514));
#144515=CARTESIAN_POINT('Ctrl Pts',(-6.89919153278588,-54.580000040183,
-135.443410824955));
#144516=CARTESIAN_POINT('Ctrl Pts',(-6.9,-54.5800000200014,-135.415380765739));
#144517=CARTESIAN_POINT('Ctrl Pts',(-6.82752390105444,-55.106794611208,
-137.742762010959));
#144518=CARTESIAN_POINT('Ctrl Pts',(-7.39999999999997,-55.0309624818203,
-137.77858424555));
#144519=CARTESIAN_POINT('Ctrl Pts',(-7.4,-55.5541151520872,-137.531452880088));
#144520=CARTESIAN_POINT('Ctrl Pts',(-6.83631982946675,-60.4094944461354,
-148.971070239217));
#144521=CARTESIAN_POINT('Ctrl Pts',(-7.39999999999996,-60.2903951615484,
-148.888188464867));
#144522=CARTESIAN_POINT('Ctrl Pts',(-7.4,-60.858236996045,-148.759754479668));
#144523=CARTESIAN_POINT('Ctrl Pts',(-6.84214680798085,-65.6936814170396,
-160.208420694715));
#144524=CARTESIAN_POINT('Ctrl Pts',(-7.40000000024359,-65.6065688428949,
-160.175729571892));
#144525=CARTESIAN_POINT('Ctrl Pts',(-7.4,-66.1431501582269,-159.997106821727));
#144526=CARTESIAN_POINT('Ctrl Pts',(-6.84687749809456,-70.9710952348089,
-171.449026400902));
#144527=CARTESIAN_POINT('Ctrl Pts',(-7.39999999999995,-70.9175980522951,
-171.474145745141));
#144528=CARTESIAN_POINT('Ctrl Pts',(-7.4,-71.4211246238516,-171.237717270032));
#144529=CARTESIAN_POINT('Origin',(-7.9,-72.58000002,-55.24995));
#144530=CARTESIAN_POINT('',(-7.9,-73.08000002,-174.491325336599));
#144531=CARTESIAN_POINT('Origin',(3.54807775957937E-14,-73.08000002,3.11172719585489E-30));
#144532=CARTESIAN_POINT('',(-8.4,-73.08000002,-58.1922197332626));
#144533=CARTESIAN_POINT('Origin',(-8.4,-72.58000002,-55.24995));
#144534=CARTESIAN_POINT('Ctrl Pts',(-9.30242220787995,-55.1547652726018,
-93.2181494891395));
#144535=CARTESIAN_POINT('Ctrl Pts',(-8.89999999999997,-55.2270244231188,
-93.2526539147005));
#144536=CARTESIAN_POINT('Ctrl Pts',(-8.9,-55.5972887473416,-93.4294586200098));
#144537=CARTESIAN_POINT('Ctrl Pts',(-9.31365506854171,-60.298307210959,
-82.4413594877101));
#144538=CARTESIAN_POINT('Ctrl Pts',(-8.89999999981176,-60.4125449242165,
-82.3706902717217));
#144539=CARTESIAN_POINT('Ctrl Pts',(-8.9,-60.7433024895534,-82.6526792495127));
#144540=CARTESIAN_POINT('Ctrl Pts',(-9.32127686740287,-65.4102595335587,
-71.6490160146723));
#144541=CARTESIAN_POINT('Ctrl Pts',(-8.89999999999997,-65.4986935712713,
-71.6191417519029));
#144542=CARTESIAN_POINT('Ctrl Pts',(-8.9,-65.8565639782118,-71.8603324984455));
#144543=CARTESIAN_POINT('Ctrl Pts',(-9.32749162718857,-70.5102313269446,
-60.8508735991008));
#144544=CARTESIAN_POINT('Ctrl Pts',(-8.89999999999996,-70.5668839574465,
-60.8776359696917));
#144545=CARTESIAN_POINT('Ctrl Pts',(-8.9,-70.9575466375288,-61.0621827299711));
#144546=CARTESIAN_POINT('Origin',(-9.4,-55.5972887473416,-93.4294586200098));
#144547=CARTESIAN_POINT('Ctrl Pts',(-9.3276302147955,-70.6241744288951,
-171.449026400902));
#144548=CARTESIAN_POINT('Ctrl Pts',(-8.89999999999996,-70.6807353060531,
-171.422308714525));
#144549=CARTESIAN_POINT('Ctrl Pts',(-8.9,-71.0715121820529,-171.237717270032));
#144550=CARTESIAN_POINT('Ctrl Pts',(-9.32139302491482,-65.48642588992,-160.570366012028));
#144551=CARTESIAN_POINT('Ctrl Pts',(-8.89999999999997,-65.5751008964372,
-160.600947379136));
#144552=CARTESIAN_POINT('Ctrl Pts',(-8.9,-65.932751045448,-160.359049360718));
#144553=CARTESIAN_POINT('Ctrl Pts',(-9.31373872503275,-60.3366136221522,
-149.697543381378));
#144554=CARTESIAN_POINT('Ctrl Pts',(-8.89999999996837,-60.4515277778623,
-149.769759336176));
#144555=CARTESIAN_POINT('Ctrl Pts',(-8.9,-60.7816272203214,-149.486223352848));
#144556=CARTESIAN_POINT('Ctrl Pts',(-9.30242220787994,-55.1547652725975,
-138.840493482357));
#144557=CARTESIAN_POINT('Ctrl Pts',(-8.89999999999998,-55.2270244231145,
-138.805989056796));
#144558=CARTESIAN_POINT('Ctrl Pts',(-8.9,-55.5972887473373,-138.629184351487));
#144559=CARTESIAN_POINT('Origin',(-9.4,-55.5972887473373,-138.629184351487));
#144560=CARTESIAN_POINT('Ctrl Pts',(-8.9,-55.0800615856017,-136.31269455866));
#144561=CARTESIAN_POINT('Ctrl Pts',(-8.89999999999949,-54.5790205502306,
-136.310262631249));
#144562=CARTESIAN_POINT('Ctrl Pts',(-9.40104578491443,-54.580068463696,
-136.310267776416));
#144563=CARTESIAN_POINT('Ctrl Pts',(-8.9,-55.0781191191466,-136.719181715364));
#144564=CARTESIAN_POINT('Ctrl Pts',(-8.90000000000701,-54.5929085780248,
-136.748100743102));
#144565=CARTESIAN_POINT('Ctrl Pts',(-9.38483903200563,-54.5779095798998,
-136.755056625822));
#144566=CARTESIAN_POINT('Ctrl Pts',(-8.9,-55.1221566249649,-137.117922857594));
#144567=CARTESIAN_POINT('Ctrl Pts',(-8.90000000000104,-54.6552983120157,
-137.181065343466));
#144568=CARTESIAN_POINT('Ctrl Pts',(-9.36838029157539,-54.6268396387186,
-137.190977807678));
#144569=CARTESIAN_POINT('Ctrl Pts',(-8.9,-55.2980260549037,-137.900349863317));
#144570=CARTESIAN_POINT('Ctrl Pts',(-8.89999999999895,-54.8759793513846,
-138.023440966196));
#144571=CARTESIAN_POINT('Ctrl Pts',(-9.33501744196278,-54.8222491183721,
-138.045571332617));
#144572=CARTESIAN_POINT('Ctrl Pts',(-8.9,-55.4315173683664,-138.286573753949));
#144573=CARTESIAN_POINT('Ctrl Pts',(-8.89999999999893,-55.0334227401566,
-138.436762949154));
#144574=CARTESIAN_POINT('Ctrl Pts',(-9.31799140452363,-54.9705730458312,
-138.46700628841));
#144575=CARTESIAN_POINT('Ctrl Pts',(-8.9,-55.6084336906355,-138.652375441382));
#144576=CARTESIAN_POINT('Ctrl Pts',(-8.90000000000005,-55.2398419057005,
-138.830621016037));
#144577=CARTESIAN_POINT('Ctrl Pts',(-9.30138592606904,-55.1671456462707,
-138.865776623046));
#144578=CARTESIAN_POINT('',(-9.4,-54.58000002,-136.338455187671));
#144579=CARTESIAN_POINT('Origin',(-9.4,-55.08000002,-136.338455187671));
#144580=CARTESIAN_POINT('Ctrl Pts',(-9.4,-54.58000002,-136.338455187671));
#144581=CARTESIAN_POINT('Ctrl Pts',(-9.39568379879652,-54.5800000235886,
-136.456736569618));
#144582=CARTESIAN_POINT('Ctrl Pts',(-9.39134381256866,-54.5836651351887,
-136.574405163223));
#144583=CARTESIAN_POINT('Ctrl Pts',(-9.3869894402585,-54.5908887409915,
-136.691443516044));
#144584=CARTESIAN_POINT('Ctrl Pts',(-9.38259558962493,-54.5981778386323,
-136.809542981149));
#144585=CARTESIAN_POINT('Ctrl Pts',(-9.37818673013582,-54.6090898788391,
-136.927001658915));
#144586=CARTESIAN_POINT('Ctrl Pts',(-9.37376332616986,-54.6235628810459,
-137.043824528223));
#144587=CARTESIAN_POINT('Ctrl Pts',(-9.36931395071144,-54.6381208597708,
-137.161333309172));
#144588=CARTESIAN_POINT('Ctrl Pts',(-9.36484943919976,-54.6562815979561,
-137.278199798939));
#144589=CARTESIAN_POINT('Ctrl Pts',(-9.3603669253627,-54.6780337583374,
-137.394437436029));
#144590=CARTESIAN_POINT('Ctrl Pts',(-9.35747954189939,-54.6920452774223,
-137.469311188425));
#144591=CARTESIAN_POINT('Ctrl Pts',(-9.35458463586583,-54.7075480263028,
-137.543924144405));
#144592=CARTESIAN_POINT('Ctrl Pts',(-9.35168199702453,-54.7245503765222,
-137.618278743991));
#144593=CARTESIAN_POINT('Ctrl Pts',(-9.346722739198,-54.7535994739144,-137.745316122767));
#144594=CARTESIAN_POINT('Ctrl Pts',(-9.34174931509111,-54.7870830771536,
-137.871831855925));
#144595=CARTESIAN_POINT('Ctrl Pts',(-9.33675902757907,-54.8249939643255,
-137.997389579686));
#144596=CARTESIAN_POINT('Ctrl Pts',(-9.33180868381611,-54.8626014014535,
-138.121942301993));
#144597=CARTESIAN_POINT('Ctrl Pts',(-9.32684197484257,-54.9045657752775,
-138.245551915827));
#144598=CARTESIAN_POINT('Ctrl Pts',(-9.32187694789394,-54.9508338578952,
-138.36778554022));
#144599=CARTESIAN_POINT('Ctrl Pts',(-9.31696142496181,-54.9966406225888,
-138.48880042896));
#144600=CARTESIAN_POINT('Ctrl Pts',(-9.31204783361034,-55.0466658539161,
-138.608466213002));
#144601=CARTESIAN_POINT('Ctrl Pts',(-9.30717021919832,-55.1008095430556,
-138.726361914857));
#144602=CARTESIAN_POINT('Ctrl Pts',(-9.30558887632612,-55.1183631521896,
-138.764584191577));
#144603=CARTESIAN_POINT('Ctrl Pts',(-9.30401142729987,-55.1363492545961,
-138.802620437397));
#144604=CARTESIAN_POINT('Ctrl Pts',(-9.30243932966332,-55.1547633023018,
-138.840456402819));
#144605=CARTESIAN_POINT('Origin',(-9.4,-55.08000002,-55.24995));
#144606=CARTESIAN_POINT('',(-9.4,-54.58000002,-95.7201877838351));
#144607=CARTESIAN_POINT('Origin',(-9.4,-55.08000002,-95.7201877838351));
#144608=CARTESIAN_POINT('',(-9.4,-54.58000002,-136.131917111522));
#144609=CARTESIAN_POINT('Ctrl Pts',(-8.9,-55.5972887473416,-93.4294586200098));
#144610=CARTESIAN_POINT('Ctrl Pts',(-8.89999999999997,-55.2270244231188,
-93.2526539147005));
#144611=CARTESIAN_POINT('Ctrl Pts',(-9.30242220787995,-55.1547652726018,
-93.2181494891395));
#144612=CARTESIAN_POINT('Ctrl Pts',(-8.9,-55.4259676862915,-93.7882391070165));
#144613=CARTESIAN_POINT('Ctrl Pts',(-8.90000000000102,-55.0269773455407,
-93.6389456903403));
#144614=CARTESIAN_POINT('Ctrl Pts',(-9.31868748160984,-54.9644104418147,
-93.609279542603));
#144615=CARTESIAN_POINT('Ctrl Pts',(-8.9,-55.2983039792949,-94.15951472994));
#144616=CARTESIAN_POINT('Ctrl Pts',(-8.90000000000064,-54.8762991189121,
-94.036294307786));
#144617=CARTESIAN_POINT('Ctrl Pts',(-9.33504644279423,-54.8225599750811,
-94.0144115846847));
#144618=CARTESIAN_POINT('Ctrl Pts',(-8.9,-55.1250790215096,-94.9253056568412));
#144619=CARTESIAN_POINT('Ctrl Pts',(-8.89999999999928,-54.6591463230926,
-94.8606734038326));
#144620=CARTESIAN_POINT('Ctrl Pts',(-9.36771205478627,-54.6300877991462,
-94.8508246266895));
#144621=CARTESIAN_POINT('Ctrl Pts',(-8.9,-55.0800000205144,-95.3226944715878));
#144622=CARTESIAN_POINT('Ctrl Pts',(-8.89999999999998,-54.5956237519515,
-95.2920343273126));
#144623=CARTESIAN_POINT('Ctrl Pts',(-9.38412882836456,-54.58000002,-95.28525344501));
#144624=CARTESIAN_POINT('Ctrl Pts',(-8.9,-55.08000002,-95.7201877838351));
#144625=CARTESIAN_POINT('Ctrl Pts',(-8.89999999999996,-54.58000002,-95.720187783835));
#144626=CARTESIAN_POINT('Ctrl Pts',(-9.4,-54.58000002,-95.7201877838351));
#144627=CARTESIAN_POINT('Ctrl Pts',(-9.30242220787995,-55.1547652726018,
-93.2181494891395));
#144628=CARTESIAN_POINT('Ctrl Pts',(-9.31868748160984,-54.9644104418147,
-93.609279542603));
#144629=CARTESIAN_POINT('Ctrl Pts',(-9.33504644279423,-54.8225599750811,
-94.0144115846847));
#144630=CARTESIAN_POINT('Ctrl Pts',(-9.36771205478627,-54.6300877991462,
-94.8508246266895));
#144631=CARTESIAN_POINT('Ctrl Pts',(-9.38412882836456,-54.58000002,-95.28525344501));
#144632=CARTESIAN_POINT('Ctrl Pts',(-9.4,-54.58000002,-95.7201877838351));
#144633=CARTESIAN_POINT('Ctrl Pts',(-14.9356335973474,-55.3065630170304,
-89.5821211232313));
#144634=CARTESIAN_POINT('Ctrl Pts',(-15.6303319911964,-54.58000002,-90.5558876551412));
#144635=CARTESIAN_POINT('Ctrl Pts',(-16.4431419066885,-54.58000002,-91.6952124319348));
#144636=CARTESIAN_POINT('Ctrl Pts',(-13.9221964884044,-55.2748268726715,
-90.3693030445756));
#144637=CARTESIAN_POINT('Ctrl Pts',(-14.580009345269,-54.5800000199812,
-91.3456221401381));
#144638=CARTESIAN_POINT('Ctrl Pts',(-15.339723951503,-54.58000002,-92.4824059293848));
#144639=CARTESIAN_POINT('Ctrl Pts',(-12.878461314285,-55.2441424314898,
-91.1126600131971));
#144640=CARTESIAN_POINT('Ctrl Pts',(-13.4941774039103,-54.58000002,-92.0929943757894));
#144641=CARTESIAN_POINT('Ctrl Pts',(-14.2000751633255,-54.58000002,-93.2257513219804));
#144642=CARTESIAN_POINT('Ctrl Pts',(-10.7089431339248,-55.1865276043544,
-92.4826203625704));
#144643=CARTESIAN_POINT('Ctrl Pts',(-11.232462400793,-54.58000002,-93.4698992380895));
#144644=CARTESIAN_POINT('Ctrl Pts',(-11.824167023199,-54.58000002,-94.5957116711942));
#144645=CARTESIAN_POINT('Ctrl Pts',(-9.60108129664725,-55.1600911541447,
-93.0975581705506));
#144646=CARTESIAN_POINT('Ctrl Pts',(-10.0749231938442,-54.5800000200141,
-94.0883976981553));
#144647=CARTESIAN_POINT('Ctrl Pts',(-10.607529289827,-54.58000002,-95.2106503240539));
#144648=CARTESIAN_POINT('Ctrl Pts',(-8.4637455188182,-55.1370659786207,
-93.6259289312743));
#144649=CARTESIAN_POINT('Ctrl Pts',(-8.88330761013172,-54.58000002,-94.6201459052405));
#144650=CARTESIAN_POINT('Ctrl Pts',(-9.35547542469517,-54.58000002,-95.7390202399778));
#144651=CARTESIAN_POINT('',(-15.05,-54.5800000203361,-92.6513075005872));
#144652=CARTESIAN_POINT('Ctrl Pts',(-15.05,-54.5800000213444,-92.6513075005872));
#144653=CARTESIAN_POINT('Ctrl Pts',(-14.7116749748798,-54.5800000217462,
-92.8742343330668));
#144654=CARTESIAN_POINT('Ctrl Pts',(-14.3706840440903,-54.5800000214065,
-93.0921200800074));
#144655=CARTESIAN_POINT('Ctrl Pts',(-14.0263093380871,-54.580000021009,
-93.3049061919424));
#144656=CARTESIAN_POINT('Ctrl Pts',(-13.6916633339156,-54.5800000206227,
-93.5116810243007));
#144657=CARTESIAN_POINT('Ctrl Pts',(-13.3538223587274,-54.5800000202949,
-93.7136406704415));
#144658=CARTESIAN_POINT('Ctrl Pts',(-13.0120992871415,-54.5800000201906,
-93.9106936784565));
#144659=CARTESIAN_POINT('Ctrl Pts',(-12.7734325857321,-54.5800000201177,
-94.0483197135013));
#144660=CARTESIAN_POINT('Ctrl Pts',(-12.5336633488411,-54.5800000201,-94.1830804413658));
#144661=CARTESIAN_POINT('Ctrl Pts',(-12.2925916871682,-54.5800000202013,
-94.3149150255473));
#144662=CARTESIAN_POINT('Ctrl Pts',(-11.7801234903736,-54.5800000204166,
-94.5951679228056));
#144663=CARTESIAN_POINT('Ctrl Pts',(-11.2613422805828,-54.5800000202694,
-94.8625400042015));
#144664=CARTESIAN_POINT('Ctrl Pts',(-10.7355463256442,-54.580000020136,
-95.115608977548));
#144665=CARTESIAN_POINT('Ctrl Pts',(-10.2954190750505,-54.5800000200243,
-95.3274450527468));
#144666=CARTESIAN_POINT('Ctrl Pts',(-9.85037652345821,-54.5800000200001,
-95.529258479393));
#144667=CARTESIAN_POINT('Ctrl Pts',(-9.4,-54.58000002,-95.7201877838351));
#144668=CARTESIAN_POINT('Ctrl Pts',(-15.05,-54.58000002,-92.6513075005872));
#144669=CARTESIAN_POINT('Ctrl Pts',(-15.024892260307,-54.5800000199942,
-92.1213653817233));
#144670=CARTESIAN_POINT('Ctrl Pts',(-14.9996997962388,-54.6413287797313,
-91.6021394176372));
#144671=CARTESIAN_POINT('Ctrl Pts',(-14.9493011641311,-54.8817452975028,
-90.5846126994908));
#144672=CARTESIAN_POINT('Ctrl Pts',(-14.9239041921259,-55.0632253928883,
-90.0827451820339));
#144673=CARTESIAN_POINT('Ctrl Pts',(-14.8995694550283,-55.3054345175152,
-89.6101049857472));
#144674=CARTESIAN_POINT('Ctrl Pts',(-14.9339094669349,-69.3159372152924,
-60.8508735991008));
#144675=CARTESIAN_POINT('Ctrl Pts',(-15.55,-69.1834807533182,-60.7869757488078));
#144676=CARTESIAN_POINT('Ctrl Pts',(-15.55,-69.753968537624,-61.0621827299711));
#144677=CARTESIAN_POINT('Ctrl Pts',(-14.9250579803326,-64.6843968356381,
-70.4566455899725));
#144678=CARTESIAN_POINT('Ctrl Pts',(-15.5499999999812,-64.4850428243905,
-70.4989618700373));
#144679=CARTESIAN_POINT('Ctrl Pts',(-15.55,-65.1200769667078,-70.6679657074144));
#144680=CARTESIAN_POINT('Ctrl Pts',(-14.9143624117001,-60.0265024281888,
-80.0493410623047));
#144681=CARTESIAN_POINT('Ctrl Pts',(-15.5500000002265,-59.7682625842489,
-80.1682572157014));
#144682=CARTESIAN_POINT('Ctrl Pts',(-15.55,-60.4591562379615,-80.2606677496439));
#144683=CARTESIAN_POINT('Ctrl Pts',(-14.8995694550282,-55.3054345175152,
-89.6101049857472));
#144684=CARTESIAN_POINT('Ctrl Pts',(-15.55,-55.1214867472491,-89.519172133185));
#144685=CARTESIAN_POINT('Ctrl Pts',(-15.55,-55.7328910677637,-89.8214141166175));
#144686=CARTESIAN_POINT('Origin',(-15.05,-55.7328910677637,-89.8214141166176));
#144687=CARTESIAN_POINT('Ctrl Pts',(-15.55,-55.08000002,-92.6513075005872));
#144688=CARTESIAN_POINT('Ctrl Pts',(-15.55,-54.5800000199999,-92.6513075005872));
#144689=CARTESIAN_POINT('Ctrl Pts',(-15.05,-54.58000002,-92.6513075005872));
#144690=CARTESIAN_POINT('Ctrl Pts',(-15.55,-55.0800000226551,-92.1594703795246));
#144691=CARTESIAN_POINT('Ctrl Pts',(-15.5499999999999,-54.5542439251598,
-92.1076806752376));
#144692=CARTESIAN_POINT('Ctrl Pts',(-15.024892260188,-54.58000002,-92.1213653817264));
#144693=CARTESIAN_POINT('Ctrl Pts',(-15.55,-55.1351959031758,-91.676922782688));
#144694=CARTESIAN_POINT('Ctrl Pts',(-15.5499999999983,-54.5897383680245,
-91.5814692358521));
#144695=CARTESIAN_POINT('Ctrl Pts',(-14.9996997961174,-54.6413287797427,
-91.6021394176417));
#144696=CARTESIAN_POINT('Ctrl Pts',(-15.55,-55.3515707703666,-90.7300471126767));
#144697=CARTESIAN_POINT('Ctrl Pts',(-15.5500000000017,-54.7672056222625,
-90.5350573580561));
#144698=CARTESIAN_POINT('Ctrl Pts',(-14.9493011640063,-54.8817452975266,
-90.5846126995011));
#144699=CARTESIAN_POINT('Ctrl Pts',(-15.55,-55.5149014993407,-90.2623845064693));
#144700=CARTESIAN_POINT('Ctrl Pts',(-15.5499999999938,-54.9184989239094,
-90.0093785901182));
#144701=CARTESIAN_POINT('Ctrl Pts',(-14.923904192,-55.0632253929174,-90.0827451820487));
#144702=CARTESIAN_POINT('Ctrl Pts',(-15.55,-55.7328910677637,-89.8214141166176));
#144703=CARTESIAN_POINT('Ctrl Pts',(-15.55,-55.121486747249,-89.5191721331851));
#144704=CARTESIAN_POINT('Ctrl Pts',(-14.8995694550282,-55.3054345175152,
-89.6101049857472));
#144705=CARTESIAN_POINT('Origin',(-15.05,-55.08000002,-92.6513075005872));
#144706=CARTESIAN_POINT('Origin',(-15.05,-55.08000002,-55.24995));
#144707=CARTESIAN_POINT('',(-15.05,-54.580000020672,-139.407335470919));
#144708=CARTESIAN_POINT('Origin',(-15.05,-55.08000002,-139.407335470919));
#144709=CARTESIAN_POINT('',(-15.05,-54.58000002,-92.3169104578858));
#144710=CARTESIAN_POINT('Ctrl Pts',(-15.55,-55.784673861554,-142.339558479678));
#144711=CARTESIAN_POINT('Ctrl Pts',(-15.5500000000003,-55.1714603843291,
-142.657475116176));
#144712=CARTESIAN_POINT('Ctrl Pts',(-14.8938285640752,-55.3629945164905,
-142.558190130607));
#144713=CARTESIAN_POINT('Ctrl Pts',(-15.55,-55.5401271863377,-141.867316731602));
#144714=CARTESIAN_POINT('Ctrl Pts',(-15.5499999999988,-54.9426861434529,
-142.132025071305));
#144715=CARTESIAN_POINT('Ctrl Pts',(-14.9199544375999,-55.0912805253495,
-142.052148874024));
#144716=CARTESIAN_POINT('Ctrl Pts',(-15.55,-55.362894042524,-141.374710914757));
#144717=CARTESIAN_POINT('Ctrl Pts',(-15.5499999999981,-54.7770460479369,
-141.577324726442));
#144718=CARTESIAN_POINT('Ctrl Pts',(-14.946753914001,-54.8943433954032,
-141.523569141345));
#144719=CARTESIAN_POINT('Ctrl Pts',(-15.55,-55.1280599014707,-140.353868077711));
#144720=CARTESIAN_POINT('Ctrl Pts',(-15.5500000000017,-54.5840535900085,
-140.448758797019));
#144721=CARTESIAN_POINT('Ctrl Pts',(-15.001105737931,-54.6334073692214,
-140.426579139991));
#144722=CARTESIAN_POINT('Ctrl Pts',(-15.55,-55.0715453714938,-139.821424819443));
#144723=CARTESIAN_POINT('Ctrl Pts',(-15.5499999999997,-54.5490322450014,
-139.868468877722));
#144724=CARTESIAN_POINT('Ctrl Pts',(-15.0288653188588,-54.5706093318628,
-139.853620894103));
#144725=CARTESIAN_POINT('Ctrl Pts',(-15.55,-55.0810227214706,-139.29316520423));
#144726=CARTESIAN_POINT('Ctrl Pts',(-15.55,-54.5868072552659,-139.284387084));
#144727=CARTESIAN_POINT('Ctrl Pts',(-15.0557386144632,-54.5811354380133,
-139.284304796475));
#144728=CARTESIAN_POINT('Origin',(-15.05,-55.7328910677637,-142.237228854888));
#144729=CARTESIAN_POINT('Ctrl Pts',(-14.8995696008973,-55.3054345059085,
-142.448537780858));
#144730=CARTESIAN_POINT('Ctrl Pts',(-14.9050869560101,-55.2505199530171,
-142.341378389044));
#144731=CARTESIAN_POINT('Ctrl Pts',(-14.9106657820154,-55.1989345061021,
-142.233184634051));
#144732=CARTESIAN_POINT('Ctrl Pts',(-14.916264781587,-55.1505541483133,
-142.124033611185));
#144733=CARTESIAN_POINT('Ctrl Pts',(-14.9220196156331,-55.1008272414598,
-142.011844636256));
#144734=CARTESIAN_POINT('Ctrl Pts',(-14.9277960872094,-55.0544854940107,
-141.898643995188));
#144735=CARTESIAN_POINT('Ctrl Pts',(-14.933578643377,-55.0114188364469,
-141.784475897057));
#144736=CARTESIAN_POINT('Ctrl Pts',(-14.9394267629822,-54.9678638830437,
-141.669013344923));
#144737=CARTESIAN_POINT('Ctrl Pts',(-14.94528159598,-54.9276580556282,-141.552560655841));
#144738=CARTESIAN_POINT('Ctrl Pts',(-14.9511502353055,-54.8907235501576,
-141.435131421174));
#144739=CARTESIAN_POINT('Ctrl Pts',(-14.9570741056195,-54.8534414463534,
-141.31659703549));
#144740=CARTESIAN_POINT('Ctrl Pts',(-14.9630125985182,-54.8194920355816,
-141.19706689485));
#144741=CARTESIAN_POINT('Ctrl Pts',(-14.9689885366562,-54.7888405203331,
-141.076532755565));
#144742=CARTESIAN_POINT('Ctrl Pts',(-14.9706613173099,-54.7802605684443,
-141.042792918966));
#144743=CARTESIAN_POINT('Ctrl Pts',(-14.9723370964144,-54.7719393157975,
-141.0089743197));
#144744=CARTESIAN_POINT('Ctrl Pts',(-14.974016496481,-54.7638766966098,
-140.975076596103));
#144745=CARTESIAN_POINT('Ctrl Pts',(-14.9812183326244,-54.7293014554678,
-140.829711679284));
#144746=CARTESIAN_POINT('Ctrl Pts',(-14.9884710425149,-54.6994331689373,
-140.68264626882));
#144747=CARTESIAN_POINT('Ctrl Pts',(-14.9957348293262,-54.6744372616794,
-140.534379348079));
#144748=CARTESIAN_POINT('Ctrl Pts',(-15.0029606082856,-54.6495721458076,
-140.386888235788));
#144749=CARTESIAN_POINT('Ctrl Pts',(-15.0101970249367,-54.6295286679905,
-140.238208426256));
#144750=CARTESIAN_POINT('Ctrl Pts',(-15.0174130265094,-54.6144231957733,
-140.088851404552));
#144751=CARTESIAN_POINT('Ctrl Pts',(-15.0245747584206,-54.5994313278638,
-139.940617657963));
#144752=CARTESIAN_POINT('Ctrl Pts',(-15.0317160929112,-54.5893035220428,
-139.791717139304));
#144753=CARTESIAN_POINT('Ctrl Pts',(-15.0388192449019,-54.5841064305008,
-139.642665710458));
#144754=CARTESIAN_POINT('Ctrl Pts',(-15.0425567571479,-54.5813718426295,
-139.564238338876));
#144755=CARTESIAN_POINT('Ctrl Pts',(-15.0462839352885,-54.5800015872439,
-139.485769424767));
#144756=CARTESIAN_POINT('Ctrl Pts',(-15.05,-54.5800000213439,-139.407335470919));
#144757=CARTESIAN_POINT('Ctrl Pts',(-14.8995694550282,-55.3054345175152,
-142.448537985759));
#144758=CARTESIAN_POINT('Ctrl Pts',(-15.55,-55.1214867472491,-142.539470838321));
#144759=CARTESIAN_POINT('Ctrl Pts',(-15.55,-55.7328910677637,-142.237228854888));
#144760=CARTESIAN_POINT('Ctrl Pts',(-14.9144862578123,-60.0660270491051,
-152.089344301479));
#144761=CARTESIAN_POINT('Ctrl Pts',(-15.5500000000456,-59.8063638088322,
-151.967058554268));
#144762=CARTESIAN_POINT('Ctrl Pts',(-15.55,-60.4987241912205,-151.878017105041));
#144763=CARTESIAN_POINT('Ctrl Pts',(-14.9252396269456,-64.7624344426112,
-161.762591659591));
#144764=CARTESIAN_POINT('Ctrl Pts',(-15.549999999915,-64.5626692295554,
-161.718722395353));
#144765=CARTESIAN_POINT('Ctrl Pts',(-15.55,-65.1981673386922,-161.551271258869));
#144766=CARTESIAN_POINT('Ctrl Pts',(-14.9341313545396,-69.4322546019743,
-171.449026400902));
#144767=CARTESIAN_POINT('Ctrl Pts',(-15.5499999999999,-69.3001099534342,
-171.51276528209));
#144768=CARTESIAN_POINT('Ctrl Pts',(-15.55,-69.870344670579,-171.237717270032));
#144769=CARTESIAN_POINT('Origin',(-16.05,-70.08000002,-174.34995));
#144770=CARTESIAN_POINT('',(-16.05,-73.08000002,-174.34995));
#144771=CARTESIAN_POINT('Origin',(-16.05,-72.58000002,-174.34995));
#144772=CARTESIAN_POINT('Origin',(-16.05,-70.08000002,-174.34995));
#144773=CARTESIAN_POINT('Origin',(-16.05,-72.58000002,-55.24995));
#144774=CARTESIAN_POINT('',(-16.05,-73.08000002,-58.24995));
#144775=CARTESIAN_POINT('Origin',(-16.05,-72.58000002,-58.24995));
#144776=CARTESIAN_POINT('',(-16.05,-73.08000002,-174.34995));
#144777=CARTESIAN_POINT('Origin',(-16.05,-70.08000002,-58.24995));
#144778=CARTESIAN_POINT('Origin',(-16.05,-70.08000002,-58.24995));
#144779=CARTESIAN_POINT('Origin',(3.3975957231091E-14,-70.08000002,-58.24995));
#144780=CARTESIAN_POINT('',(-16.55,-73.08000002,-58.24995));
#144781=CARTESIAN_POINT('Origin',(-16.55,-70.08000002,-58.24995));
#144782=CARTESIAN_POINT('',(41.5,-73.0800000199999,-58.24995));
#144783=CARTESIAN_POINT('Origin',(-16.55,-70.08000002,-58.24995));
#144784=CARTESIAN_POINT('Origin',(-16.55,-72.58000002,-58.24995));
#144785=CARTESIAN_POINT('Ctrl Pts',(-17.3782102443508,-55.3867109640818,
-87.5561378285247));
#144786=CARTESIAN_POINT('Ctrl Pts',(-17.0499999999999,-55.4939415516614,
-87.6101736986065));
#144787=CARTESIAN_POINT('Ctrl Pts',(-17.05,-55.8060398696737,-87.7674469593951));
#144788=CARTESIAN_POINT('Ctrl Pts',(-17.3935607753682,-59.8507835488919,
-78.6850032603101));
#144789=CARTESIAN_POINT('Ctrl Pts',(-17.0499999998605,-60.0039146247672,
-78.6330864204663));
#144790=CARTESIAN_POINT('Ctrl Pts',(-17.05,-60.2763921316847,-78.8963304394585));
#144791=CARTESIAN_POINT('Ctrl Pts',(-17.4050347595683,-64.2412639062053,
-69.7761086016325));
#144792=CARTESIAN_POINT('Ctrl Pts',(-17.0499999999316,-64.3705933782976,
-69.756601957739));
#144793=CARTESIAN_POINT('Ctrl Pts',(-17.05,-64.6707170319981,-69.9874285386638));
#144794=CARTESIAN_POINT('Ctrl Pts',(-17.4146253252297,-68.5993151180197,
-60.8508735991007));
#144795=CARTESIAN_POINT('Ctrl Pts',(-17.05,-68.6914563568371,-60.8958957033858));
#144796=CARTESIAN_POINT('Ctrl Pts',(-17.05,-69.0317756926871,-61.0621827299711));
#144797=CARTESIAN_POINT('Origin',(-17.55,-55.8060398696737,-87.7674469593951));
#144798=CARTESIAN_POINT('Ctrl Pts',(-17.4148840712406,-68.7171063154928,
-171.449026400902));
#144799=CARTESIAN_POINT('Ctrl Pts',(-17.0499999999999,-68.809126121555,
-171.404072041895));
#144800=CARTESIAN_POINT('Ctrl Pts',(-17.05,-69.1496478013716,-171.237717270032));
#144801=CARTESIAN_POINT('Ctrl Pts',(-17.4052437025222,-64.32043537753,-162.443049517833));
#144802=CARTESIAN_POINT('Ctrl Pts',(-17.05,-64.4501495263083,-162.463595694273));
#144803=CARTESIAN_POINT('Ctrl Pts',(-17.05,-64.7499600097223,-162.23172927942));
#144804=CARTESIAN_POINT('Ctrl Pts',(-17.393699089013,-59.8910064308848,
-153.453571789302));
#144805=CARTESIAN_POINT('Ctrl Pts',(-17.0500000000351,-60.0450216003852,
-153.507379856851));
#144806=CARTESIAN_POINT('Ctrl Pts',(-17.05,-60.3166713897233,-153.242244037967));
#144807=CARTESIAN_POINT('Ctrl Pts',(-17.3782102443508,-55.3867109640869,
-144.502505142991));
#144808=CARTESIAN_POINT('Ctrl Pts',(-17.05,-55.4939415516665,-144.448469272909));
#144809=CARTESIAN_POINT('Ctrl Pts',(-17.05,-55.8060398696787,-144.291196012121));
#144810=CARTESIAN_POINT('Origin',(-17.55,-55.8060398696787,-144.291196012121));
#144811=CARTESIAN_POINT('Ctrl Pts',(-17.05,-55.0805074616842,-141.090900894366));
#144812=CARTESIAN_POINT('Ctrl Pts',(-17.0499999999999,-54.575891747757,
-141.084786328764));
#144813=CARTESIAN_POINT('Ctrl Pts',(-17.5546323543766,-54.5805643956983,
-141.084837323443));
#144814=CARTESIAN_POINT('Ctrl Pts',(-17.05,-55.0737407427313,-141.662277194932));
#144815=CARTESIAN_POINT('Ctrl Pts',(-17.05,-54.5986790821796,-141.679101787038));
#144816=CARTESIAN_POINT('Ctrl Pts',(-17.5241509980515,-54.5730421239016,
-141.696718195611));
#144817=CARTESIAN_POINT('Ctrl Pts',(-17.05,-55.1346896361868,-142.222271907188));
#144818=CARTESIAN_POINT('Ctrl Pts',(-17.05,-54.6883224645955,-142.274289971467));
#144819=CARTESIAN_POINT('Ctrl Pts',(-17.493703373038,-54.6407602724392,
-142.295501749987));
#144820=CARTESIAN_POINT('Ctrl Pts',(-17.05,-55.3871982275049,-143.319730865885));
#144821=CARTESIAN_POINT('Ctrl Pts',(-17.05,-55.007218915137,-143.426193042337));
#144822=CARTESIAN_POINT('Ctrl Pts',(-17.4330935790494,-54.9213199751476,
-143.467340431406));
#144823=CARTESIAN_POINT('Ctrl Pts',(-17.05,-55.5814626759696,-143.861508336615));
#144824=CARTESIAN_POINT('Ctrl Pts',(-17.05,-55.2333139511105,-143.992542009422));
#144825=CARTESIAN_POINT('Ctrl Pts',(-17.4026795826987,-55.1371704105482,
-144.044980325084));
#144826=CARTESIAN_POINT('Ctrl Pts',(-17.05,-55.8450287809867,-144.367275073454));
#144827=CARTESIAN_POINT('Ctrl Pts',(-17.05,-55.5380988270127,-144.527216600776));
#144828=CARTESIAN_POINT('Ctrl Pts',(-17.3739345303265,-55.4300165573977,
-144.583528621283));
#144829=CARTESIAN_POINT('',(-17.55,-54.58000002,-141.176536909659));
#144830=CARTESIAN_POINT('Origin',(-17.55,-55.08000002,-141.176536909659));
#144831=CARTESIAN_POINT('Ctrl Pts',(-17.55,-54.58000002,-141.176536909659));
#144832=CARTESIAN_POINT('Ctrl Pts',(-17.5434039653577,-54.5800000265972,
-141.308685646377));
#144833=CARTESIAN_POINT('Ctrl Pts',(-17.5367960353516,-54.5835879338551,
-141.440239551843));
#144834=CARTESIAN_POINT('Ctrl Pts',(-17.5301956955585,-54.5906604912783,
-141.571176756649));
#144835=CARTESIAN_POINT('Ctrl Pts',(-17.5234840454982,-54.5978523225997,
-141.70432212887));
#144836=CARTESIAN_POINT('Ctrl Pts',(-17.5167797303469,-54.6086468223138,
-141.836830569671));
#144837=CARTESIAN_POINT('Ctrl Pts',(-17.5100862770427,-54.622980971367,
-141.968701840416));
#144838=CARTESIAN_POINT('Ctrl Pts',(-17.503372066993,-54.6373595713593,
-142.100982050807));
#144839=CARTESIAN_POINT('Ctrl Pts',(-17.4966681563516,-54.6552995984296,
-142.232621988595));
#144840=CARTESIAN_POINT('Ctrl Pts',(-17.4899699068517,-54.6767881709156,
-142.363631902612));
#144841=CARTESIAN_POINT('Ctrl Pts',(-17.4832987536179,-54.6981898162009,
-142.494111845403));
#144842=CARTESIAN_POINT('Ctrl Pts',(-17.4766325502404,-54.7231114151653,
-142.623967706529));
#144843=CARTESIAN_POINT('Ctrl Pts',(-17.4699683223166,-54.7515915027105,
-142.753207159389));
#144844=CARTESIAN_POINT('Ctrl Pts',(-17.4677609485311,-54.7610248833477,
-142.796014785954));
#144845=CARTESIAN_POINT('Ctrl Pts',(-17.465553848176,-54.7708490838071,
-142.838754709885));
#144846=CARTESIAN_POINT('Ctrl Pts',(-17.4633471473699,-54.7810667130108,
-142.881426904301));
#144847=CARTESIAN_POINT('Ctrl Pts',(-17.4557628915023,-54.8161838951985,
-143.02808785625));
#144848=CARTESIAN_POINT('Ctrl Pts',(-17.4482142625559,-54.8560016932433,
-143.174199894099));
#144849=CARTESIAN_POINT('Ctrl Pts',(-17.440677260134,-54.9005823896015,
-143.31931656486));
#144850=CARTESIAN_POINT('Ctrl Pts',(-17.4333152627617,-54.9441279467171,
-143.461063706365));
#144851=CARTESIAN_POINT('Ctrl Pts',(-17.4259644460376,-54.9922184111824,
-143.601861162394));
#144852=CARTESIAN_POINT('Ctrl Pts',(-17.4186373285509,-55.0448895417837,
-143.741267924584));
#144853=CARTESIAN_POINT('Ctrl Pts',(-17.4115478748488,-55.0958522215165,
-143.876152862365));
#144854=CARTESIAN_POINT('Ctrl Pts',(-17.4044808446839,-55.1511037543352,
-144.009735693423));
#144855=CARTESIAN_POINT('Ctrl Pts',(-17.3974781607216,-55.2106471239,-144.141594677413));
#144856=CARTESIAN_POINT('Ctrl Pts',(-17.3910063762535,-55.2656762893459,
-144.263456941818));
#144857=CARTESIAN_POINT('Ctrl Pts',(-17.3845899846665,-55.3243713219084,
-144.383846491428));
#144858=CARTESIAN_POINT('Ctrl Pts',(-17.3782835568631,-55.3867049962959,
-144.502414961715));
#144859=CARTESIAN_POINT('Origin',(-17.55,-55.08000002,-55.24995));
#144860=CARTESIAN_POINT('',(-17.55,-54.58000002,-90.8821060618472));
#144861=CARTESIAN_POINT('Origin',(-17.55,-55.08000002,-90.8821060618472));
#144862=CARTESIAN_POINT('',(-17.55,-54.58000002,-140.803447286915));
#144863=CARTESIAN_POINT('Ctrl Pts',(-17.05,-55.8060398696737,-87.7674469593951));
#144864=CARTESIAN_POINT('Ctrl Pts',(-17.0499999999999,-55.4939415516614,
-87.6101736986065));
#144865=CARTESIAN_POINT('Ctrl Pts',(-17.3782102443508,-55.3867109640818,
-87.5561378285247));
#144866=CARTESIAN_POINT('Ctrl Pts',(-17.05,-55.5622216475024,-88.2512880043934));
#144867=CARTESIAN_POINT('Ctrl Pts',(-17.05,-55.2114257865401,-88.1214372575005));
#144868=CARTESIAN_POINT('Ctrl Pts',(-17.4056693808345,-55.1158123847072,
-88.0713943440392));
#144869=CARTESIAN_POINT('Ctrl Pts',(-17.05,-55.3841798573999,-88.7556128927223));
#144870=CARTESIAN_POINT('Ctrl Pts',(-17.05,-55.0036171481024,-88.6486574682591));
#144871=CARTESIAN_POINT('Ctrl Pts',(-17.4339593787444,-54.9179776170691,
-88.6091505606876));
#144872=CARTESIAN_POINT('Ctrl Pts',(-17.05,-55.1424163647715,-89.7992759203947));
#144873=CARTESIAN_POINT('Ctrl Pts',(-17.0499999999999,-54.6987064687868,
-89.7439019899564));
#144874=CARTESIAN_POINT('Ctrl Pts',(-17.4916046269366,-54.6493515142325,
-89.7235249939138));
#144875=CARTESIAN_POINT('Ctrl Pts',(-17.05,-55.0800000196891,-90.3423386098486));
#144876=CARTESIAN_POINT('Ctrl Pts',(-17.0500000000018,-54.6080382399387,
-90.3203722819605));
#144877=CARTESIAN_POINT('Ctrl Pts',(-17.5211522384036,-54.58000002,-90.3041534556916));
#144878=CARTESIAN_POINT('Ctrl Pts',(-17.05,-55.08000002,-90.8821060618472));
#144879=CARTESIAN_POINT('Ctrl Pts',(-17.0499999999999,-54.58000002,-90.8821060618472));
#144880=CARTESIAN_POINT('Ctrl Pts',(-17.55,-54.58000002,-90.8821060618472));
#144881=CARTESIAN_POINT('Ctrl Pts',(-17.3782123830793,-55.3866898645837,
-87.5561779606742));
#144882=CARTESIAN_POINT('Ctrl Pts',(-17.4056708497953,-55.1158021121638,
-88.0714222670871));
#144883=CARTESIAN_POINT('Ctrl Pts',(-17.4339601270529,-54.9179741299611,
-88.6091650266831));
#144884=CARTESIAN_POINT('Ctrl Pts',(-17.4916046269366,-54.6493515142325,
-89.7235249939138));
#144885=CARTESIAN_POINT('Ctrl Pts',(-17.5211522384036,-54.58000002,-90.3041534556916));
#144886=CARTESIAN_POINT('Ctrl Pts',(-17.55,-54.58000002,-90.8821060618472));
#144887=CARTESIAN_POINT('Origin',(-16.55,-72.58000002,-55.24995));
#144888=CARTESIAN_POINT('',(-16.55,-73.08000002,-174.34995));
#144889=CARTESIAN_POINT('Origin',(-16.55,-72.58000002,-174.34995));
#144890=CARTESIAN_POINT('',(-16.55,-73.08000002,-58.24995));
#144891=CARTESIAN_POINT('Origin',(-16.55,-70.08000002,-174.34995));
#144892=CARTESIAN_POINT('Origin',(-16.55,-70.08000002,-174.34995));
#144893=CARTESIAN_POINT('Ctrl Pts',(-23.0246352694011,-55.592944139339,
-81.9685164608053));
#144894=CARTESIAN_POINT('Ctrl Pts',(-23.9800920467566,-54.58000002,-82.9059773201362));
#144895=CARTESIAN_POINT('Ctrl Pts',(-25.1782904241482,-54.58000002,-84.0816077695088));
#144896=CARTESIAN_POINT('Ctrl Pts',(-21.9095359072908,-55.5502317234241,
-83.1856130754768));
#144897=CARTESIAN_POINT('Ctrl Pts',(-22.8383173576717,-54.5800000199764,
-84.1257656115259));
#144898=CARTESIAN_POINT('Ctrl Pts',(-23.9841110090257,-54.58000002,-85.2987111873827));
#144899=CARTESIAN_POINT('Ctrl Pts',(-20.7596485158525,-55.5069863868931,
-84.3783409260868));
#144900=CARTESIAN_POINT('Ctrl Pts',(-21.6556870958812,-54.5800000200059,
-85.3242347169187));
#144901=CARTESIAN_POINT('Ctrl Pts',(-22.7486109694941,-54.58000002,-86.4914322348344));
#144902=CARTESIAN_POINT('Ctrl Pts',(-18.3831304802005,-55.4209867081881,
-86.677763648685));
#144903=CARTESIAN_POINT('Ctrl Pts',(-19.2046498564005,-54.580000019994,
-87.6346041928195));
#144904=CARTESIAN_POINT('Ctrl Pts',(-20.1853568720873,-54.58000002,-88.7908549573443));
#144905=CARTESIAN_POINT('Ctrl Pts',(-17.1656615705366,-55.378552771758,
-87.7759223265742));
#144906=CARTESIAN_POINT('Ctrl Pts',(-17.9458952665752,-54.5800000199822,
-88.7385064703248));
#144907=CARTESIAN_POINT('Ctrl Pts',(-18.8674767865624,-54.58000002,-89.8890267533221));
#144908=CARTESIAN_POINT('Ctrl Pts',(-15.908562035693,-55.3376387148139,
-88.8056746987062));
#144909=CARTESIAN_POINT('Ctrl Pts',(-16.6397068497462,-54.58000002,-89.7756104658071));
#144910=CARTESIAN_POINT('Ctrl Pts',(-17.501426021519,-54.58000002,-90.9187660074097));
#144911=CARTESIAN_POINT('',(-23.2,-54.58000002,-86.035464915697));
#144912=CARTESIAN_POINT('Ctrl Pts',(-23.2,-54.5800000205323,-86.035464915697));
#144913=CARTESIAN_POINT('Ctrl Pts',(-22.7416005579447,-54.5800000204569,
-86.47348855531));
#144914=CARTESIAN_POINT('Ctrl Pts',(-22.2778852067935,-54.580000020382,
-86.9061566639853));
#144915=CARTESIAN_POINT('Ctrl Pts',(-21.8082168238936,-54.5800000203146,
-87.3329667341744));
#144916=CARTESIAN_POINT('Ctrl Pts',(-21.6948114072064,-54.5800000202983,
-87.4360236475592));
#144917=CARTESIAN_POINT('Ctrl Pts',(-21.5810587192231,-54.5800000202825,
-87.5387388947569));
#144918=CARTESIAN_POINT('Ctrl Pts',(-21.4669494079306,-54.5800000202671,
-87.6411051232897));
#144919=CARTESIAN_POINT('Ctrl Pts',(-21.0322856597371,-54.5800000202087,
-88.0310372688657));
#144920=CARTESIAN_POINT('Ctrl Pts',(-20.593585201871,-54.5800000201577,
-88.4149271477262));
#144921=CARTESIAN_POINT('Ctrl Pts',(-20.1500339722446,-54.580000020117,
-88.7924150855441));
#144922=CARTESIAN_POINT('Ctrl Pts',(-19.7265254012931,-54.5800000200782,
-89.1528455531393));
#144923=CARTESIAN_POINT('Ctrl Pts',(-19.2985947426906,-54.5800000200487,
-89.507439867046));
#144924=CARTESIAN_POINT('Ctrl Pts',(-18.86550622925,-54.5800000200292,-89.8558463488877));
#144925=CARTESIAN_POINT('Ctrl Pts',(-18.4324177158093,-54.5800000200098,
-90.2042528307294));
#144926=CARTESIAN_POINT('Ctrl Pts',(-17.9941717501709,-54.5800000200003,
-90.5464720515007));
#144927=CARTESIAN_POINT('Ctrl Pts',(-17.55,-54.58000002,-90.8821060618472));
#144928=CARTESIAN_POINT('Ctrl Pts',(-23.2,-54.58000002,-86.035464915697));
#144929=CARTESIAN_POINT('Ctrl Pts',(-23.1631558847544,-54.5800000199942,
-85.3330272043352));
#144930=CARTESIAN_POINT('Ctrl Pts',(-23.1266268845704,-54.6631759768875,
-84.6443771511168));
#144931=CARTESIAN_POINT('Ctrl Pts',(-23.0544213837377,-54.9946392601494,
-83.2949364329151));
#144932=CARTESIAN_POINT('Ctrl Pts',(-23.0184485783994,-55.2464820492743,
-82.6288060065001));
#144933=CARTESIAN_POINT('Ctrl Pts',(-22.9849163124812,-55.5914230881085,
-82.0118419201864));
#144934=CARTESIAN_POINT('Ctrl Pts',(-23.0210431649761,-66.5230748737403,
-60.8508735991007));
#144935=CARTESIAN_POINT('Ctrl Pts',(-23.6999999999999,-66.2910081673095,
-60.7330850354506));
#144936=CARTESIAN_POINT('Ctrl Pts',(-23.7,-66.9393955463102,-61.0621827299711));
#144937=CARTESIAN_POINT('Ctrl Pts',(-23.0109831737233,-62.9327835325611,
-67.9329755599233));
#144938=CARTESIAN_POINT('Ctrl Pts',(-23.7000000000839,-62.6252669058498,
-67.9176543808627));
#144939=CARTESIAN_POINT('Ctrl Pts',(-23.7,-63.3447762129971,-68.1442919238122));
#144940=CARTESIAN_POINT('Ctrl Pts',(-22.9993168926453,-59.3018045077389,
-74.9936336228867));
#144941=CARTESIAN_POINT('Ctrl Pts',(-23.7000000000403,-58.9382045046749,
-75.0250759674623));
#144942=CARTESIAN_POINT('Ctrl Pts',(-23.7,-59.7084208561779,-75.2049556739983));
#144943=CARTESIAN_POINT('Ctrl Pts',(-22.9849163103247,-55.591423110293,
-82.011841880507));
#144944=CARTESIAN_POINT('Ctrl Pts',(-23.7,-55.290324925596,-81.8523243454179));
#144945=CARTESIAN_POINT('Ctrl Pts',(-23.7,-55.9902808012637,-82.2231510113773));
#144946=CARTESIAN_POINT('Origin',(-23.2,-55.9902808012638,-82.2231510113773));
#144947=CARTESIAN_POINT('Ctrl Pts',(-23.7,-55.08000002,-86.035464915697));
#144948=CARTESIAN_POINT('Ctrl Pts',(-23.7,-54.58000002,-86.0354649156969));
#144949=CARTESIAN_POINT('Ctrl Pts',(-23.2,-54.58000002,-86.035464915697));
#144950=CARTESIAN_POINT('Ctrl Pts',(-23.7,-55.0800000221098,-85.3715851430748));
#144951=CARTESIAN_POINT('Ctrl Pts',(-23.7,-54.5417374496194,-85.3059841364058));
#144952=CARTESIAN_POINT('Ctrl Pts',(-23.163155884673,-54.58000002,-85.3330272043393));
#144953=CARTESIAN_POINT('Ctrl Pts',(-23.7,-55.1548583802702,-84.7198400663338));
#144954=CARTESIAN_POINT('Ctrl Pts',(-23.6999999999999,-54.5866204760292,
-84.6055144627376));
#144955=CARTESIAN_POINT('Ctrl Pts',(-23.1266268844869,-54.6631759768986,
-84.6443771511225));
#144956=CARTESIAN_POINT('Ctrl Pts',(-23.7,-55.4531753402921,-83.4411601721359));
#144957=CARTESIAN_POINT('Ctrl Pts',(-23.7,-54.8153941542428,-83.2070098309739));
#144958=CARTESIAN_POINT('Ctrl Pts',(-23.054421382878,-54.9946392637262,
-83.2949364184621));
#144959=CARTESIAN_POINT('Ctrl Pts',(-23.7,-55.6798282904624,-82.8091473369244));
#144960=CARTESIAN_POINT('Ctrl Pts',(-23.7000000000021,-55.01791265188,-82.4979478032362));
#144961=CARTESIAN_POINT('Ctrl Pts',(-23.0184485767712,-55.2464820601011,
-82.6288059779555));
#144962=CARTESIAN_POINT('Ctrl Pts',(-23.7,-55.9902808012637,-82.2231510113773));
#144963=CARTESIAN_POINT('Ctrl Pts',(-23.7,-55.290324925596,-81.8523243454179));
#144964=CARTESIAN_POINT('Ctrl Pts',(-22.9849163103247,-55.591423110293,
-82.011841880507));
#144965=CARTESIAN_POINT('Origin',(-23.2,-55.08000002,-86.035464915697));
#144966=CARTESIAN_POINT('Origin',(-23.2,-55.08000002,-55.24995));
#144967=CARTESIAN_POINT('',(-23.2,-54.5800000202568,-146.023178055809));
#144968=CARTESIAN_POINT('Origin',(-23.2,-55.08000002,-146.023178055809));
#144969=CARTESIAN_POINT('',(-23.2,-54.58000002,-85.5535812563546));
#144970=CARTESIAN_POINT('Ctrl Pts',(-23.7,-56.1877984637886,-150.184170074209));
#144971=CARTESIAN_POINT('Ctrl Pts',(-23.7000000000058,-55.4758653944209,
-150.617415324691));
#144972=CARTESIAN_POINT('Ctrl Pts',(-22.9645964648804,-55.8110221483383,
-150.413695161775));
#144973=CARTESIAN_POINT('Ctrl Pts',(-23.7,-55.770760534689,-149.494224653333));
#144974=CARTESIAN_POINT('Ctrl Pts',(-23.6999999999915,-55.104992262177,
-149.853316450234));
#144975=CARTESIAN_POINT('Ctrl Pts',(-23.0041504913057,-55.3476739653898,
-149.687711142526));
#144976=CARTESIAN_POINT('Ctrl Pts',(-23.7,-55.4874608362993,-148.759183505398));
#144977=CARTESIAN_POINT('Ctrl Pts',(-23.6999999999971,-54.84406999352,-149.022400495565));
#144978=CARTESIAN_POINT('Ctrl Pts',(-23.0460611054753,-55.0328364107862,
-148.913176733992));
#144979=CARTESIAN_POINT('Ctrl Pts',(-23.7,-55.126303632832,-147.221582957655));
#144980=CARTESIAN_POINT('Ctrl Pts',(-23.7000000000026,-54.5663401762214,
-147.338490969714));
#144981=CARTESIAN_POINT('Ctrl Pts',(-23.132906798941,-54.6314878274362,
-147.290542781339));
#144982=CARTESIAN_POINT('Ctrl Pts',(-23.7,-55.0524032880678,-146.416006958094));
#144983=CARTESIAN_POINT('Ctrl Pts',(-23.699999999999,-54.5265437589966,
-146.473947688457));
#144984=CARTESIAN_POINT('Ctrl Pts',(-23.1780014932925,-54.5493513836785,
-146.439171475211));
#144985=CARTESIAN_POINT('Ctrl Pts',(-23.7,-55.0891865678663,-145.627934484655));
#144986=CARTESIAN_POINT('Ctrl Pts',(-23.7000000000002,-54.6108701043512,
-145.605394331135));
#144987=CARTESIAN_POINT('Ctrl Pts',(-23.2215734466188,-54.5901934669506,
-145.604851313073));
#144988=CARTESIAN_POINT('Origin',(-23.2,-55.9902808012637,-149.835491960129));
#144989=CARTESIAN_POINT('Ctrl Pts',(-22.9849164538399,-55.5914231005407,
-150.046800950003));
#144990=CARTESIAN_POINT('Ctrl Pts',(-22.9908372008831,-55.5305186315594,
-149.937866229653));
#144991=CARTESIAN_POINT('Ctrl Pts',(-22.9968799288713,-55.472742437367,
-149.827854316054));
#144992=CARTESIAN_POINT('Ctrl Pts',(-23.0029707306892,-55.4179474788907,
-149.716871524626));
#144993=CARTESIAN_POINT('Ctrl Pts',(-23.0091875113402,-55.3620191712851,
-149.603593225481));
#144994=CARTESIAN_POINT('Ctrl Pts',(-23.0154546055321,-55.3091959345735,
-149.489303295622));
#144995=CARTESIAN_POINT('Ctrl Pts',(-23.0217323073057,-55.2593300727596,
-149.374077739874));
#144996=CARTESIAN_POINT('Ctrl Pts',(-23.0281927026225,-55.2080130156976,
-149.255498892459));
#144997=CARTESIAN_POINT('Ctrl Pts',(-23.0346646369944,-55.1598271938812,
-149.135928921938));
#144998=CARTESIAN_POINT('Ctrl Pts',(-23.0411415414134,-55.1146326815648,
-149.015415012526));
#144999=CARTESIAN_POINT('Ctrl Pts',(-23.0477026343699,-55.0688507188787,
-148.893334631057));
#145000=CARTESIAN_POINT('Ctrl Pts',(-23.0542693270987,-55.0261376966006,
-148.770285167514));
#145001=CARTESIAN_POINT('Ctrl Pts',(-23.0608656006907,-54.98638023854,-148.646285053031));
#145002=CARTESIAN_POINT('Ctrl Pts',(-23.0675533958685,-54.9460711560571,
-148.520564469111));
#145003=CARTESIAN_POINT('Ctrl Pts',(-23.074272175774,-54.9087996853551,
-148.393866137308));
#145004=CARTESIAN_POINT('Ctrl Pts',(-23.0810701888432,-54.8744894117583,
-148.266185449915));
#145005=CARTESIAN_POINT('Ctrl Pts',(-23.0839762476771,-54.8598222328834,
-148.211603679368));
#145006=CARTESIAN_POINT('Ctrl Pts',(-23.0868970210003,-54.8456967589052,
-148.156842142755));
#145007=CARTESIAN_POINT('Ctrl Pts',(-23.089837136435,-54.8321096326547,
-148.101899565739));
#145008=CARTESIAN_POINT('Ctrl Pts',(-23.1005386667511,-54.7826547569155,
-147.901917739631));
#145009=CARTESIAN_POINT('Ctrl Pts',(-23.1113627267195,-54.7403626997578,
-147.699512147701));
#145010=CARTESIAN_POINT('Ctrl Pts',(-23.1222318129805,-54.7053520485838,
-147.495526029615));
#145011=CARTESIAN_POINT('Ctrl Pts',(-23.1332194694889,-54.6699594681963,
-147.289314638505));
#145012=CARTESIAN_POINT('Ctrl Pts',(-23.1442532408192,-54.642007812508,
-147.081487627851));
#145013=CARTESIAN_POINT('Ctrl Pts',(-23.155279897433,-54.6215740728526,
-146.872924136455));
#145014=CARTESIAN_POINT('Ctrl Pts',(-23.1661946839301,-54.6013476421687,
-146.666476610302));
#145015=CARTESIAN_POINT('Ctrl Pts',(-23.1771027123396,-54.588487337632,
-146.459307075042));
#145016=CARTESIAN_POINT('Ctrl Pts',(-23.1879759364348,-54.5830254173653,
-146.25228214336));
#145017=CARTESIAN_POINT('Ctrl Pts',(-23.1919887037201,-54.5810096937153,
-146.175879517442));
#145018=CARTESIAN_POINT('Ctrl Pts',(-23.1959969478324,-54.5800011956741,
-146.099496753778));
#145019=CARTESIAN_POINT('Ctrl Pts',(-23.2,-54.5800000210274,-146.023178055809));
#145020=CARTESIAN_POINT('Ctrl Pts',(-22.9849163103247,-55.591423110293,
-150.046801090999));
#145021=CARTESIAN_POINT('Ctrl Pts',(-23.6999999999999,-55.2903249255959,
-150.206318626088));
#145022=CARTESIAN_POINT('Ctrl Pts',(-23.7,-55.9902808012637,-149.835491960129));
#145023=CARTESIAN_POINT('Ctrl Pts',(-22.9994804181366,-59.343937645489,
-157.144704426787));
#145024=CARTESIAN_POINT('Ctrl Pts',(-23.7,-58.9786022357095,-157.10917403496));
#145025=CARTESIAN_POINT('Ctrl Pts',(-23.7,-59.7506418899787,-156.933381838169));
#145026=CARTESIAN_POINT('Ctrl Pts',(-23.0112491123844,-63.0152939322715,
-164.285990110815));
#145027=CARTESIAN_POINT('Ctrl Pts',(-23.7000000003822,-62.707250125371,
-164.298966961939));
#145028=CARTESIAN_POINT('Ctrl Pts',(-23.7,-63.4274104915032,-164.074673486974));
#145029=CARTESIAN_POINT('Ctrl Pts',(-23.0213852109847,-66.6453596297547,
-171.449026400902));
#145030=CARTESIAN_POINT('Ctrl Pts',(-23.7,-66.413901371901,-171.56646471025));
#145031=CARTESIAN_POINT('Ctrl Pts',(-23.7,-67.0618271655313,-171.237717270032));
#145032=CARTESIAN_POINT('Origin',(-24.2,-70.08000002,-174.34995));
#145033=CARTESIAN_POINT('',(-24.2,-73.08000002,-174.34995));
#145034=CARTESIAN_POINT('Origin',(-24.2,-72.58000002,-174.34995));
#145035=CARTESIAN_POINT('Origin',(-24.2,-70.08000002,-174.34995));
#145036=CARTESIAN_POINT('Origin',(-24.2,-72.58000002,-55.24995));
#145037=CARTESIAN_POINT('Origin',(-24.2,-72.58000002,-58.24995));
#145038=CARTESIAN_POINT('',(-24.2,-73.08000002,-174.34995));
#145039=CARTESIAN_POINT('Origin',(-24.2,-70.08000002,-58.24995));
#145040=CARTESIAN_POINT('Origin',(0.,-12.9675000200281,-60.64995));
#145041=CARTESIAN_POINT('',(-28.2496026309167,29.643102187894,-76.2257352477989));
#145042=CARTESIAN_POINT('',(-22.2890532034791,29.4093902975657,-83.1809305852948));
#145043=CARTESIAN_POINT('Ctrl Pts',(-28.2496026843433,29.6431021904052,
-76.2257353081032));
#145044=CARTESIAN_POINT('Ctrl Pts',(-27.0281878838229,29.5945550182985,
-77.7598757997112));
#145045=CARTESIAN_POINT('Ctrl Pts',(-25.7765799171754,29.5448662110019,
-79.270584144585));
#145046=CARTESIAN_POINT('Ctrl Pts',(-24.4879779898396,29.4944735933695,
-80.7447462809204));
#145047=CARTESIAN_POINT('Ctrl Pts',(-23.7649962843928,29.4662003618423,
-81.5718382111928));
#145048=CARTESIAN_POINT('Ctrl Pts',(-23.0327081268011,29.4377909731413,
-82.3848464598177));
#145049=CARTESIAN_POINT('Ctrl Pts',(-22.2891503921926,29.4093838642151,
-83.1810211215431));
#145050=CARTESIAN_POINT('Ctrl Pts',(-28.2795019009908,37.8065307949999,
-61.2273317382593));
#145051=CARTESIAN_POINT('Ctrl Pts',(-28.2706820191605,35.1297158291743,
-66.2515800426151));
#145052=CARTESIAN_POINT('Ctrl Pts',(-28.2608542879989,32.4163856120597,
-71.2554899486297));
#145053=CARTESIAN_POINT('Ctrl Pts',(-28.2496025504691,29.6431021990262,
-76.2257351951279));
#145054=CARTESIAN_POINT('Ctrl Pts',(-22.2890532034791,29.4093902975657,
-83.1809305852948));
#145055=CARTESIAN_POINT('Ctrl Pts',(-22.3038722896351,33.2381690976656,
-75.8991829023387));
#145056=CARTESIAN_POINT('Ctrl Pts',(-22.3157407792727,36.9852293035361,
-68.5739513473019));
#145057=CARTESIAN_POINT('Ctrl Pts',(-22.3259225534137,40.6914751389564,
-61.2273317382593));
#145058=CARTESIAN_POINT('Ctrl Pts',(-22.,41.1098595241823,-61.4386408691297));
#145059=CARTESIAN_POINT('Ctrl Pts',(-22.,40.7995210108967,-61.2819013639433));
#145060=CARTESIAN_POINT('Ctrl Pts',(-22.3259225534138,40.6914751389564,
-61.2273317382593));
#145061=CARTESIAN_POINT('Ctrl Pts',(-22.,41.1233751604146,-61.4118804447591));
#145062=CARTESIAN_POINT('Ctrl Pts',(-22.,40.8194184511061,-61.2339961299344));
#145063=CARTESIAN_POINT('Ctrl Pts',(-22.3307532272019,40.7164963923335,
-61.1738110360374));
#145064=CARTESIAN_POINT('Ctrl Pts',(-22.,41.1392509618672,-61.3865876948747));
#145065=CARTESIAN_POINT('Ctrl Pts',(-22.,40.8429002807173,-61.1881281443964));
#145066=CARTESIAN_POINT('Ctrl Pts',(-22.3364246839863,40.745888690896,-61.1232259520736));
#145067=CARTESIAN_POINT('Ctrl Pts',(-22.,41.1573899115079,-61.3627217630986));
#145068=CARTESIAN_POINT('Ctrl Pts',(-22.,40.8698280768405,-61.1441646043172));
#145069=CARTESIAN_POINT('Ctrl Pts',(-22.3428990418276,40.7794755973204,
-61.0754935261973));
#145070=CARTESIAN_POINT('Origin',(-22.5,41.1098595241823,-61.4386408691296));
#145071=CARTESIAN_POINT('Ctrl Pts',(-29.,38.7048160259599,-61.150138786574));
#145072=CARTESIAN_POINT('Ctrl Pts',(-29.,38.6926240909195,-60.6436056187277));
#145073=CARTESIAN_POINT('Ctrl Pts',(-28.4933647440612,38.6927858841382,
-60.650327573148));
#145074=CARTESIAN_POINT('Ctrl Pts',(-29.,38.6042425482601,-61.1525595652015));
#145075=CARTESIAN_POINT('Ctrl Pts',(-29.,38.5056874437974,-60.6032547660267));
#145076=CARTESIAN_POINT('Ctrl Pts',(-28.4508217728044,38.5151017970219,
-60.6551690977179));
#145077=CARTESIAN_POINT('Ctrl Pts',(-29.,38.5024684382473,-61.1789379706814));
#145078=CARTESIAN_POINT('Ctrl Pts',(-29.,38.2987442898004,-60.603134659432));
#145079=CARTESIAN_POINT('Ctrl Pts',(-28.4075947879363,38.335472514688,-60.707925961796));
#145080=CARTESIAN_POINT('Ctrl Pts',(-29.,38.3706532052714,-61.2520107824808));
#145081=CARTESIAN_POINT('Ctrl Pts',(-29.0000000000001,37.990375163389,-60.6863576421133));
#145082=CARTESIAN_POINT('Ctrl Pts',(-28.3514280416523,38.1029959208976,
-60.8540715547449));
#145083=CARTESIAN_POINT('Ctrl Pts',(-29.,38.3294709783247,-61.2822335925436));
#145084=CARTESIAN_POINT('Ctrl Pts',(-29.,37.8822359354345,-60.7316627868476));
#145085=CARTESIAN_POINT('Ctrl Pts',(-28.3338483525148,38.0303960306507,
-60.9145171861254));
#145086=CARTESIAN_POINT('Ctrl Pts',(-29.,38.2570904307121,-61.3534252594253));
#145087=CARTESIAN_POINT('Ctrl Pts',(-29.,37.6732261500514,-60.8640556435108));
#145088=CARTESIAN_POINT('Ctrl Pts',(-28.302912455342,37.9028346914031,-61.0569005178125));
#145089=CARTESIAN_POINT('Ctrl Pts',(-29.,38.2265217687548,-61.3934878926125));
#145090=CARTESIAN_POINT('Ctrl Pts',(-29.,37.5759010011862,-60.9505556565881));
#145091=CARTESIAN_POINT('Ctrl Pts',(-28.28982523324,37.8489775515987,-61.1370349799883));
#145092=CARTESIAN_POINT('Ctrl Pts',(-29.,38.2024209812184,-61.4386408691297));
#145093=CARTESIAN_POINT('Ctrl Pts',(-29.,37.4942143736512,-61.0606306836509));
#145094=CARTESIAN_POINT('Ctrl Pts',(-28.2795019009908,37.8065307949999,
-61.2273317382593));
#145095=CARTESIAN_POINT('Origin',(-28.5,38.2024209812184,-61.4386408691297));
#145096=CARTESIAN_POINT('Ctrl Pts',(-22.3259225534138,40.6914751389564,
-61.2273317382593));
#145097=CARTESIAN_POINT('Ctrl Pts',(-22.,40.7995210108967,-61.2819013639433));
#145098=CARTESIAN_POINT('Ctrl Pts',(-22.,41.1098595241823,-61.4386408691296));
#145099=CARTESIAN_POINT('Ctrl Pts',(-22.3157409333924,36.9852292354808,
-68.5739513464269));
#145100=CARTESIAN_POINT('Ctrl Pts',(-22.,37.1246521940256,-68.5757439011997));
#145101=CARTESIAN_POINT('Ctrl Pts',(-22.,37.3993732891074,-68.7852685139811));
#145102=CARTESIAN_POINT('Ctrl Pts',(-22.3038724392466,33.2381690210168,
-75.8991829107314));
#145103=CARTESIAN_POINT('Ctrl Pts',(-22.,33.3938486289533,-75.8821367178777));
#145104=CARTESIAN_POINT('Ctrl Pts',(-22.,33.6470169072337,-76.1105064350252));
#145105=CARTESIAN_POINT('Ctrl Pts',(-22.2890532034791,29.4093902975657,
-83.1809305852948));
#145106=CARTESIAN_POINT('Ctrl Pts',(-22.,29.5283900973743,-83.243628644349));
#145107=CARTESIAN_POINT('Ctrl Pts',(-22.,29.8104512658091,-83.3922397161652));
#145108=CARTESIAN_POINT('Origin',(-22.5,29.8104512658091,-83.3922397161652));
#145109=CARTESIAN_POINT('Ctrl Pts',(-22.,28.9209370328038,-87.2580513882026));
#145110=CARTESIAN_POINT('Ctrl Pts',(-21.999999999999,28.4137949053905,-87.2657118253129));
#145111=CARTESIAN_POINT('Ctrl Pts',(-22.5071523107133,28.4210424206146,
-87.2656152652095));
#145112=CARTESIAN_POINT('Ctrl Pts',(-22.,28.9107311888036,-86.5629863693187));
#145113=CARTESIAN_POINT('Ctrl Pts',(-22.000000000005,28.4408939884557,-86.5559074723074));
#145114=CARTESIAN_POINT('Ctrl Pts',(-22.468671524864,28.4096955954818,-86.5292441588387));
#145115=CARTESIAN_POINT('Ctrl Pts',(-22.,28.9839131874059,-85.8815326469363));
#145116=CARTESIAN_POINT('Ctrl Pts',(-22.,28.5474819289643,-85.8378355431043));
#145117=CARTESIAN_POINT('Ctrl Pts',(-22.4305087782965,28.4910039358137,
-85.8083788789715));
#145118=CARTESIAN_POINT('Ctrl Pts',(-22.,29.295020387663,-84.5463837617919));
#145119=CARTESIAN_POINT('Ctrl Pts',(-22.,28.9360692653603,-84.4506314222478));
#145120=CARTESIAN_POINT('Ctrl Pts',(-22.355087560244,28.8366692516703,-84.3978739445244));
#145121=CARTESIAN_POINT('Ctrl Pts',(-22.,29.5364895794699,-83.8869642769993));
#145122=CARTESIAN_POINT('Ctrl Pts',(-22.,29.2130027933481,-83.7664986820836));
#145123=CARTESIAN_POINT('Ctrl Pts',(-22.3174945400501,29.1049725391609,
-83.7022104338494));
#145124=CARTESIAN_POINT('Ctrl Pts',(-22.,29.8707648402079,-83.2803097208969));
#145125=CARTESIAN_POINT('Ctrl Pts',(-22.,29.5958623314302,-83.1287896750421));
#145126=CARTESIAN_POINT('Ctrl Pts',(-22.2826967104608,29.4763786725123,
-83.0629642223148));
#145127=CARTESIAN_POINT('Origin',(-22.5,28.91999998,-87.1305533863517));
#145128=CARTESIAN_POINT('Ctrl Pts',(-22.5,28.41999998,-87.1305533863517));
#145129=CARTESIAN_POINT('Ctrl Pts',(-22.4925022607297,28.4199999873068,
-86.9872865310408));
#145130=CARTESIAN_POINT('Ctrl Pts',(-22.4850006342183,28.4236086928051,
-86.8445929131946));
#145131=CARTESIAN_POINT('Ctrl Pts',(-22.4775177354222,28.4307308473477,
-86.7024958507061));
#145132=CARTESIAN_POINT('Ctrl Pts',(-22.4699230794522,28.4379593713449,
-86.5582765670637));
#145133=CARTESIAN_POINT('Ctrl Pts',(-22.4623471167486,28.4488065524411,
-86.4146711023061));
#145134=CARTESIAN_POINT('Ctrl Pts',(-22.4547938831896,28.4632181376622,
-86.2716829402881));
#145135=CARTESIAN_POINT('Ctrl Pts',(-22.4472338797339,28.4776426398602,
-86.1285666192395));
#145136=CARTESIAN_POINT('Ctrl Pts',(-22.4396959238395,28.4956377181282,
-85.9860679209476));
#145137=CARTESIAN_POINT('Ctrl Pts',(-22.4321746206815,28.5171995170665,
-85.8441807994112));
#145138=CARTESIAN_POINT('Ctrl Pts',(-22.4247161392233,28.5385812210358,
-85.703478790342));
#145139=CARTESIAN_POINT('Ctrl Pts',(-22.4172732887684,28.5634703812369,
-85.563377409009));
#145140=CARTESIAN_POINT('Ctrl Pts',(-22.4098425012551,28.5919139122317,
-85.4238730636314));
#145141=CARTESIAN_POINT('Ctrl Pts',(-22.4041287008053,28.613785168798,-85.3166031423822));
#145142=CARTESIAN_POINT('Ctrl Pts',(-22.3984219659058,28.637759060564,-85.2096861754146));
#145143=CARTESIAN_POINT('Ctrl Pts',(-22.3927255817788,28.6638766966531,
-85.1031257785058));
#145144=CARTESIAN_POINT('Ctrl Pts',(-22.3845799691,28.7012239230554,-84.9507484632194));
#145145=CARTESIAN_POINT('Ctrl Pts',(-22.3765086248503,28.7429980834321,
-84.7988713990416));
#145146=CARTESIAN_POINT('Ctrl Pts',(-22.3684633632018,28.7893041990692,
-84.6479093361407));
#145147=CARTESIAN_POINT('Ctrl Pts',(-22.3607674226928,28.8335997268858,
-84.5035019686805));
#145148=CARTESIAN_POINT('Ctrl Pts',(-22.3530953888868,28.8820428891203,
-84.3599318427346));
#145149=CARTESIAN_POINT('Ctrl Pts',(-22.3454424670516,28.9347184012903,
-84.2175904338271));
#145150=CARTESIAN_POINT('Ctrl Pts',(-22.3379638731583,28.9861940039585,
-84.0784914577315));
#145151=CARTESIAN_POINT('Ctrl Pts',(-22.3305035664366,29.0417120299716,
-83.9405658640323));
#145152=CARTESIAN_POINT('Ctrl Pts',(-22.3230932050103,29.1013344342888,
-83.8042070196682));
#145153=CARTESIAN_POINT('Ctrl Pts',(-22.3159094320307,29.1591337496624,
-83.6720176532777));
#145154=CARTESIAN_POINT('Ctrl Pts',(-22.3087727947964,29.2207908881213,
-83.5413008445181));
#145155=CARTESIAN_POINT('Ctrl Pts',(-22.3017446842256,29.2863365897173,
-83.4124403467295));
#145156=CARTESIAN_POINT('Ctrl Pts',(-22.2974989203793,29.3259335151363,
-83.3345942119541));
#145157=CARTESIAN_POINT('Ctrl Pts',(-22.2932933884543,29.3669490393746,
-83.2574260278765));
#145158=CARTESIAN_POINT('Ctrl Pts',(-22.289147100448,29.4093837384563,-83.1810246462237));
#145159=CARTESIAN_POINT('Origin',(-22.5,28.9199999800001,-55.24995));
#145160=CARTESIAN_POINT('Origin',(-21.5,43.91999998,-58.24995));
#145161=CARTESIAN_POINT('Origin',(-21.5,43.91999998,-58.24995));
#145162=CARTESIAN_POINT('Origin',(0.,43.91999998,-58.24995));
#145163=CARTESIAN_POINT('Origin',(-21.,43.91999998,-58.24995));
#145164=CARTESIAN_POINT('Origin',(-21.,43.91999998,-58.24995));
#145165=CARTESIAN_POINT('Origin',(-20.,28.9199999800001,-55.24995));
#145166=CARTESIAN_POINT('Origin',(-20.,28.9199999800001,-89.3628471840452));
#145167=CARTESIAN_POINT('Ctrl Pts',(-20.5,29.8613644840354,-85.690726129678));
#145168=CARTESIAN_POINT('Ctrl Pts',(-20.4999999999939,29.1873928364402,
-85.3058817835744));
#145169=CARTESIAN_POINT('Ctrl Pts',(-19.7932806530567,29.4660338803574,
-85.4648851598992));
#145170=CARTESIAN_POINT('Ctrl Pts',(-20.5,29.5176010887559,-86.2951263081817));
#145171=CARTESIAN_POINT('Ctrl Pts',(-20.500000000012,28.8766555508427,-85.9756966173608));
#145172=CARTESIAN_POINT('Ctrl Pts',(-19.8280358121594,29.0840893038539,
-86.104597627145));
#145173=CARTESIAN_POINT('Ctrl Pts',(-20.5,29.2776631432131,-86.9330351311447));
#145174=CARTESIAN_POINT('Ctrl Pts',(-20.5,28.6555724448382,-86.6950722871695));
#145175=CARTESIAN_POINT('Ctrl Pts',(-19.8643899928891,28.8174577851778,
-86.7807486916538));
#145176=CARTESIAN_POINT('Ctrl Pts',(-20.5,28.9676187538565,-88.2625011309141));
#145177=CARTESIAN_POINT('Ctrl Pts',(-20.5,28.4126392368736,-88.1554121614486));
#145178=CARTESIAN_POINT('Ctrl Pts',(-19.9391390454861,28.4729318977163,
-88.1921218543361));
#145179=CARTESIAN_POINT('Ctrl Pts',(-20.5,28.8999739472064,-88.958655057919));
#145180=CARTESIAN_POINT('Ctrl Pts',(-20.5,28.3749512792384,-88.9062582006903));
#145181=CARTESIAN_POINT('Ctrl Pts',(-19.9777772185812,28.3977575511637,
-88.9322835714639));
#145182=CARTESIAN_POINT('Ctrl Pts',(-20.5,28.9251268357589,-89.6426008613895));
#145183=CARTESIAN_POINT('Ctrl Pts',(-20.5,28.4403470064429,-89.6603905900511));
#145184=CARTESIAN_POINT('Ctrl Pts',(-20.0151084810686,28.4256906082963,
-89.6607392320332));
#145185=CARTESIAN_POINT('Origin',(-20.,29.726759920701,-85.9392854774869));
#145186=CARTESIAN_POINT('Ctrl Pts',(-19.8077680666402,29.3163999141123,
-85.7279763466165));
#145187=CARTESIAN_POINT('Ctrl Pts',(-20.5,29.0600890554149,-85.5959926642051));
#145188=CARTESIAN_POINT('Ctrl Pts',(-20.5,29.726759920701,-85.9392854774869));
#145189=CARTESIAN_POINT('Ctrl Pts',(-19.8234665452012,33.5607487699413,
-77.4712163753771));
#145190=CARTESIAN_POINT('Ctrl Pts',(-20.5000000001728,33.2278557603418,
-77.5610859264982));
#145191=CARTESIAN_POINT('Ctrl Pts',(-20.5,33.9784532599698,-77.6825438045949));
#145192=CARTESIAN_POINT('Ctrl Pts',(-19.8355385600285,37.7216554195719,
-69.1708971047811));
#145193=CARTESIAN_POINT('Ctrl Pts',(-20.5000000002289,37.4529027206824,
-69.1923113693162));
#145194=CARTESIAN_POINT('Ctrl Pts',(-20.5,38.1440461521965,-69.3822166533219));
#145195=CARTESIAN_POINT('Ctrl Pts',(-19.8457268663587,41.8441333387867,
-60.8508735991007));
#145196=CARTESIAN_POINT('Ctrl Pts',(-20.5,41.6540022187559,-60.7565814715328));
#145197=CARTESIAN_POINT('Ctrl Pts',(-20.5,42.270218132516,-61.0621827299711));
#145198=CARTESIAN_POINT('Ctrl Pts',(-13.8920088064511,43.6468101642065,
-60.8508735991007));
#145199=CARTESIAN_POINT('Ctrl Pts',(-13.5,43.724980245498,-60.8884062566336));
#145200=CARTESIAN_POINT('Ctrl Pts',(-13.5,44.086908282047,-61.0621827299711));
#145201=CARTESIAN_POINT('Ctrl Pts',(-13.883422492558,38.8394158858892,-70.8677262129548));
#145202=CARTESIAN_POINT('Ctrl Pts',(-13.5,38.9561333124887,-70.8371780085667));
#145203=CARTESIAN_POINT('Ctrl Pts',(-13.5,39.2774015744131,-71.0790468430123));
#145204=CARTESIAN_POINT('Ctrl Pts',(-13.8729900235566,34.0078012896411,
-80.8725774805421));
#145205=CARTESIAN_POINT('Ctrl Pts',(-13.5000000000877,34.1527775267561,
-80.7999951426717));
#145206=CARTESIAN_POINT('Ctrl Pts',(-13.5,34.4430593692808,-81.0839048048873));
#145207=CARTESIAN_POINT('Ctrl Pts',(-13.8582614853459,29.115831713372,-90.8469388041467));
#145208=CARTESIAN_POINT('Ctrl Pts',(-13.5,29.2108963546553,-90.8936099040706));
#145209=CARTESIAN_POINT('Ctrl Pts',(-13.5,29.5462485400348,-91.058247935017));
#145210=CARTESIAN_POINT('Origin',(-14.,29.5462485400348,-91.058247935017));
#145211=CARTESIAN_POINT('Ctrl Pts',(-13.8582614853459,29.115831713372,-90.8469388041467));
#145212=CARTESIAN_POINT('Ctrl Pts',(-13.5,29.2108963546553,-90.8936099040706));
#145213=CARTESIAN_POINT('Ctrl Pts',(-13.5,29.5462485400348,-91.058247935017));
#145214=CARTESIAN_POINT('Ctrl Pts',(-13.8598257678503,29.1000938294036,
-90.8779461296248));
#145215=CARTESIAN_POINT('Ctrl Pts',(-13.5,29.1946688455411,-90.923776404174));
#145216=CARTESIAN_POINT('Ctrl Pts',(-13.5,29.5320844445084,-91.0870988658315));
#145217=CARTESIAN_POINT('Ctrl Pts',(-13.8613943096149,29.0846206527093,
-90.9090791787867));
#145218=CARTESIAN_POINT('Ctrl Pts',(-13.4999999999997,29.1787031940904,
-90.9540383533105));
#145219=CARTESIAN_POINT('Ctrl Pts',(-13.5,29.518158585283,-91.1160643410222));
#145220=CARTESIAN_POINT('Ctrl Pts',(-13.8629670146618,29.0694104105324,
-90.9403371832586));
#145221=CARTESIAN_POINT('Ctrl Pts',(-13.5,29.1629965026825,-90.9843933533492));
#145222=CARTESIAN_POINT('Ctrl Pts',(-13.5,29.5044693674792,-91.1451435916293));
#145223=CARTESIAN_POINT('Ctrl Pts',(-11.3834743397155,29.812801930373,-90.9273317382593));
#145224=CARTESIAN_POINT('Ctrl Pts',(-12.,29.679733250215,-90.8631216114043));
#145225=CARTESIAN_POINT('Ctrl Pts',(-12.,30.2507177004773,-91.1386408691297));
#145226=CARTESIAN_POINT('Ctrl Pts',(-11.3956361798112,34.6396513996494,
-80.9174913671817));
#145227=CARTESIAN_POINT('Ctrl Pts',(-11.9999999998861,34.4484178829812,
-81.0174669870403));
#145228=CARTESIAN_POINT('Ctrl Pts',(-12.,35.0807977947169,-81.1288119730547));
#145229=CARTESIAN_POINT('Ctrl Pts',(-11.4042255504145,39.4271199662976,
-70.8881122426161));
#145230=CARTESIAN_POINT('Ctrl Pts',(-11.999999999893,39.2806183751482,-70.92559601425));
#145231=CARTESIAN_POINT('Ctrl Pts',(-12.,39.8700921493796,-71.0994291820815));
#145232=CARTESIAN_POINT('Ctrl Pts',(-11.4112929481563,44.1984900402045,
-60.8508735991007));
#145233=CARTESIAN_POINT('Ctrl Pts',(-12.,44.102645384174,-60.8052987597771));
#145234=CARTESIAN_POINT('Ctrl Pts',(-12.,44.6428767076058,-61.062182729971));
#145235=CARTESIAN_POINT('Ctrl Pts',(-5.45757488824865,45.0702713246265,
-60.8508735991007));
#145236=CARTESIAN_POINT('Ctrl Pts',(-5.,45.1055585268383,-60.8674008824013));
#145237=CARTESIAN_POINT('Ctrl Pts',(-5.,45.5214348882082,-61.0621827299711));
#145238=CARTESIAN_POINT('Ctrl Pts',(-5.45419794131935,40.3738290579191,
-70.8788685457756));
#145239=CARTESIAN_POINT('Ctrl Pts',(-5.00000000013405,40.4263150647969,
-70.8653394730463));
#145240=CARTESIAN_POINT('Ctrl Pts',(-5.,40.8246742459034,-71.0901794372786));
#145241=CARTESIAN_POINT('Ctrl Pts',(-5.4500940393161,35.6738220550387,-80.9051511012611));
#145242=CARTESIAN_POINT('Ctrl Pts',(-5.00000000002896,35.7394456595583,
-80.8717315350143));
#145243=CARTESIAN_POINT('Ctrl Pts',(-5.,36.1242566254946,-81.1164625478583));
#145244=CARTESIAN_POINT('Ctrl Pts',(-5.44427033638569,30.9653765476951,
-90.9273317382593));
#145245=CARTESIAN_POINT('Ctrl Pts',(-4.99999999999999,31.0104747491644,
-90.9485222334823));
#145246=CARTESIAN_POINT('Ctrl Pts',(-5.,31.4150905187971,-91.1386408691297));
#145247=CARTESIAN_POINT('Origin',(-57.,11.11999998,-58.24995));
#145248=CARTESIAN_POINT('',(-60.,11.11999998,-58.24995));
#145249=CARTESIAN_POINT('Origin',(-57.,11.11999998,-58.24995));
#145250=CARTESIAN_POINT('Origin',(-59.5,11.11999998,-58.24995));
#145251=CARTESIAN_POINT('Origin',(-57.,-2.42462934179819E-14,-58.24995));
#145252=CARTESIAN_POINT('',(-60.,11.61999998,-58.24995));
#145253=CARTESIAN_POINT('Origin',(-57.,11.61999998,-58.24995));
#145254=CARTESIAN_POINT('',(-60.,-54.58000002,-58.24995));
#145255=CARTESIAN_POINT('Origin',(-57.,11.61999998,-58.24995));
#145256=CARTESIAN_POINT('Origin',(-59.5,11.61999998,-58.24995));
#145257=CARTESIAN_POINT('Origin',(-57.,-37.78000002,-58.24995));
#145258=CARTESIAN_POINT('',(-60.,-37.78000002,-58.24995));
#145259=CARTESIAN_POINT('Origin',(-57.,-37.78000002,-58.24995));
#145260=CARTESIAN_POINT('Origin',(-59.5,-37.78000002,-58.24995));
#145261=CARTESIAN_POINT('Origin',(-57.,-2.42462934179819E-14,-58.24995));
#145262=CARTESIAN_POINT('',(-60.,-37.28000002,-58.24995));
#145263=CARTESIAN_POINT('Origin',(-57.,-37.28000002,-58.24995));
#145264=CARTESIAN_POINT('',(-60.,-54.58000002,-58.24995));
#145265=CARTESIAN_POINT('Origin',(-57.,-37.28000002,-58.24995));
#145266=CARTESIAN_POINT('Origin',(-59.5,-37.28000002,-58.24995));
#145267=CARTESIAN_POINT('Origin',(-60.,-37.28000002,-176.84995));
#145268=CARTESIAN_POINT('',(-53.7578119323263,-37.28000002,-177.34995));
#145269=CARTESIAN_POINT('',(-57.,-37.28000002,-177.34995));
#145270=CARTESIAN_POINT('',(-60.,-37.28000002,-177.34995));
#145271=CARTESIAN_POINT('Origin',(-57.,-37.28000002,-176.84995));
#145272=CARTESIAN_POINT('Ctrl Pts',(-53.7578119323263,-37.28000002,-177.34995));
#145273=CARTESIAN_POINT('Ctrl Pts',(-53.8142255012181,-37.2176314844153,
-177.34995));
#145274=CARTESIAN_POINT('Ctrl Pts',(-53.8706043508049,-37.1546953024018,
-177.33811707005));
#145275=CARTESIAN_POINT('Ctrl Pts',(-53.9751511105352,-37.0369743252984,
-177.291477883886));
#145276=CARTESIAN_POINT('Ctrl Pts',(-54.0238234872226,-36.9816277442484,
-177.25641751247));
#145277=CARTESIAN_POINT('Ctrl Pts',(-54.1061105508192,-36.8874586360784,
-177.16641977034));
#145278=CARTESIAN_POINT('Ctrl Pts',(-54.1401753140075,-36.8481352183371,
-177.110787176626));
#145279=CARTESIAN_POINT('Ctrl Pts',(-54.1865253922149,-36.7944813746413,
-176.987117359946));
#145280=CARTESIAN_POINT('Ctrl Pts',(-54.1989607146972,-36.78000002,-176.918317891383));
#145281=CARTESIAN_POINT('Ctrl Pts',(-54.1989607257493,-36.78000002,-176.84995));
#145282=CARTESIAN_POINT('Origin',(-54.1989607257493,-36.28000002,-179.64995));
#145283=CARTESIAN_POINT('Origin',(-54.1989607257493,-36.28000002,-171.871644662643));
#145284=CARTESIAN_POINT('Origin',(-54.1989607257493,-36.28000002,-176.84995));
#145285=CARTESIAN_POINT('Ctrl Pts',(-53.7393383808294,-36.0824871697421,
-171.894658379227));
#145286=CARTESIAN_POINT('Ctrl Pts',(-53.4395062235889,-36.7800433691512,
-171.887030357483));
#145287=CARTESIAN_POINT('Ctrl Pts',(-54.198558315946,-36.7800000191852,
-171.906167818573));
#145288=CARTESIAN_POINT('Ctrl Pts',(-53.7436938429485,-36.0817727411102,
-171.73251549148));
#145289=CARTESIAN_POINT('Ctrl Pts',(-53.4406325939148,-36.7800434674344,
-171.778613128972));
#145290=CARTESIAN_POINT('Ctrl Pts',(-54.2046305452577,-36.7800000191843,
-171.662933242578));
#145291=CARTESIAN_POINT('Ctrl Pts',(-53.7019584052344,-36.0886165914289,
-171.572834421444));
#145292=CARTESIAN_POINT('Ctrl Pts',(-53.4304080193297,-36.7800425499783,
-171.672542976741));
#145293=CARTESIAN_POINT('Ctrl Pts',(-54.1464425180027,-36.7800000191923,
-171.423436673449));
#145294=CARTESIAN_POINT('Ctrl Pts',(-53.6182347475042,-36.1024349685042,
-171.42841039455));
#145295=CARTESIAN_POINT('Ctrl Pts',(-53.391611466063,-36.7800408062075,
-171.55046073112));
#145296=CARTESIAN_POINT('Ctrl Pts',(-54.0297882222689,-36.7800000192084,
-171.20677750911));
#145297=CARTESIAN_POINT('',(-53.6298444656516,-36.1005191032365,-171.449026400902));
#145298=CARTESIAN_POINT('Origin',(-54.0459394689003,-36.28000002,-171.237717270032));
#145299=CARTESIAN_POINT('Origin',(-52.5055674318865,-36.2860379741571,-171.88552542821));
#145300=CARTESIAN_POINT('Ctrl Pts',(-53.6298444656516,-36.1005191032365,
-171.449026400902));
#145301=CARTESIAN_POINT('Ctrl Pts',(-53.3968439469627,-36.78000002,-171.567353073206));
#145302=CARTESIAN_POINT('Ctrl Pts',(-54.0459394689003,-36.78000002,-171.237717270032));
#145303=CARTESIAN_POINT('Ctrl Pts',(-51.4138274897758,-36.0943068851322,
-167.080125911017));
#145304=CARTESIAN_POINT('Ctrl Pts',(-51.1479384960996,-36.78000002,-167.162122528925));
#145305=CARTESIAN_POINT('Ctrl Pts',(-51.827241891131,-36.78000002,-166.868814837648));
#145306=CARTESIAN_POINT('Ctrl Pts',(-49.181606116838,-36.0874694888798,
-162.719878659059));
#145307=CARTESIAN_POINT('Ctrl Pts',(-48.8961865333283,-36.7800000199664,
-162.797005637805));
#145308=CARTESIAN_POINT('Ctrl Pts',(-49.5919157423408,-36.78000002,-162.508569528187));
#145309=CARTESIAN_POINT('Ctrl Pts',(-44.6695423554902,-36.0720830782198,
-154.02490615155));
#145310=CARTESIAN_POINT('Ctrl Pts',(-44.3536351698063,-36.7800000200344,
-154.11869394055));
#145311=CARTESIAN_POINT('Ctrl Pts',(-45.0722737045335,-36.78000002,-153.813597020681));
#145312=CARTESIAN_POINT('Ctrl Pts',(-42.3899819460371,-36.0635378106947,
-149.6900251133));
#145313=CARTESIAN_POINT('Ctrl Pts',(-42.0456232774016,-36.78000002,-149.775736877395));
#145314=CARTESIAN_POINT('Ctrl Pts',(-42.7882496386931,-36.78000002,-149.478711493085));
#145315=CARTESIAN_POINT('Ctrl Pts',(-40.0734472163172,-36.0537915241817,
-145.374999642302));
#145316=CARTESIAN_POINT('Ctrl Pts',(-39.7490326214954,-36.78000002,-145.549584755123));
#145317=CARTESIAN_POINT('Ctrl Pts',(-40.4661024946855,-36.78000002,-145.163690511432));
#145318=CARTESIAN_POINT('',(-40.0734471921219,-36.0537915982708,-145.374999599156));
#145319=CARTESIAN_POINT('Origin',(-40.4661024946856,-36.28000002,-145.163690511432));
#145320=CARTESIAN_POINT('Ctrl Pts',(-40.0734472163172,-36.0537915241817,
-145.374999642303));
#145321=CARTESIAN_POINT('Ctrl Pts',(-42.3899819460361,-36.0635378106967,
-149.6900251133));
#145322=CARTESIAN_POINT('Ctrl Pts',(-44.6695423554893,-36.0720830782218,
-154.02490615155));
#145323=CARTESIAN_POINT('Ctrl Pts',(-49.1816061168372,-36.0874694888818,
-162.719878659059));
#145324=CARTESIAN_POINT('Ctrl Pts',(-51.413827489775,-36.0943068851342,
-167.080125911017));
#145325=CARTESIAN_POINT('Ctrl Pts',(-53.6298444656516,-36.1005191032365,
-171.449026400902));
#145326=CARTESIAN_POINT('Ctrl Pts',(-39.5,-36.78000002,-141.149515588739));
#145327=CARTESIAN_POINT('Ctrl Pts',(-38.9999999999999,-36.78000002,-141.149515588739));
#145328=CARTESIAN_POINT('Ctrl Pts',(-39.,-36.28000002,-141.149515588739));
#145329=CARTESIAN_POINT('Ctrl Pts',(-39.5000000020403,-36.78000002,-141.848776286889));
#145330=CARTESIAN_POINT('Ctrl Pts',(-38.9595709612524,-36.78000002,-141.917511819575));
#145331=CARTESIAN_POINT('Ctrl Pts',(-39.,-36.2411525212205,-141.887468602714));
#145332=CARTESIAN_POINT('Ctrl Pts',(-39.5789972525929,-36.78000002,-142.535527260215));
#145333=CARTESIAN_POINT('Ctrl Pts',(-39.0069624314851,-36.78000002,-142.654181226843));
#145334=CARTESIAN_POINT('Ctrl Pts',(-39.0877747262142,-36.202664552653,
-142.611197003283));
#145335=CARTESIAN_POINT('Ctrl Pts',(-39.8950301507098,-36.78000002,-143.883204247708));
#145336=CARTESIAN_POINT('Ctrl Pts',(-39.2475606867303,-36.78000002,-144.126025522057));
#145337=CARTESIAN_POINT('Ctrl Pts',(-39.4389223885666,-36.1266531472167,
-144.029685314679));
#145338=CARTESIAN_POINT('Ctrl Pts',(-40.1353628336737,-36.78000002,-144.549109040068));
#145339=CARTESIAN_POINT('Ctrl Pts',(-39.4615987310595,-36.78000002,-144.873235586497));
#145340=CARTESIAN_POINT('Ctrl Pts',(-39.7059668714196,-36.0888399354841,
-144.729666200452));
#145341=CARTESIAN_POINT('Ctrl Pts',(-40.4661024946855,-36.78000002,-145.163690511432));
#145342=CARTESIAN_POINT('Ctrl Pts',(-39.7490326214954,-36.78000002,-145.549584755123));
#145343=CARTESIAN_POINT('Ctrl Pts',(-40.0734472163172,-36.0537915241817,
-145.374999642303));
#145344=CARTESIAN_POINT('',(-39.000000000323,-36.28000002,-141.149515588739));
#145345=CARTESIAN_POINT('Origin',(-39.5,-36.28000002,-141.149515588739));
#145346=CARTESIAN_POINT('Ctrl Pts',(-39.,-36.28000002,-141.149515588739));
#145347=CARTESIAN_POINT('Ctrl Pts',(-39.,-36.2411525212205,-141.887468602714));
#145348=CARTESIAN_POINT('Ctrl Pts',(-39.0877747262142,-36.202664552653,
-142.611197003283));
#145349=CARTESIAN_POINT('Ctrl Pts',(-39.438922384402,-36.1266531481182,
-144.029685297855));
#145350=CARTESIAN_POINT('Ctrl Pts',(-39.705966858751,-36.088839937278,-144.729666167245));
#145351=CARTESIAN_POINT('Ctrl Pts',(-40.0734471901673,-36.0537915266758,
-145.374999596381));
#145352=CARTESIAN_POINT('Origin',(-39.5,-36.28000002,-55.24995));
#145353=CARTESIAN_POINT('',(-39.0000000003234,-36.28000002,-90.9091273827666));
#145354=CARTESIAN_POINT('Origin',(-39.5,-36.28000002,-90.9091273827666));
#145355=CARTESIAN_POINT('',(-39.,-36.28000002,-129.34995));
#145356=CARTESIAN_POINT('Ctrl Pts',(-40.6770017977572,-36.78000002,-86.5290501999886));
#145357=CARTESIAN_POINT('Ctrl Pts',(-39.9462151352518,-36.7800000199977,
-86.0754691928917));
#145358=CARTESIAN_POINT('Ctrl Pts',(-40.3079584328326,-36.0324776431912,
-86.2996877651884));
#145359=CARTESIAN_POINT('Ctrl Pts',(-40.2312592357455,-36.78000002,-87.252600640522));
#145360=CARTESIAN_POINT('Ctrl Pts',(-39.5535852275517,-36.7800000200034,
-86.8763713735618));
#145361=CARTESIAN_POINT('Ctrl Pts',(-39.8127216435129,-36.07379497991,-87.0589794447612));
#145362=CARTESIAN_POINT('Ctrl Pts',(-39.9312338876434,-36.78000002,-88.0264426730864));
#145363=CARTESIAN_POINT('Ctrl Pts',(-39.2777008559782,-36.78000002,-87.752028167821));
#145364=CARTESIAN_POINT('Ctrl Pts',(-39.4792833821553,-36.1178028681844,
-87.8722265567825));
#145365=CARTESIAN_POINT('Ctrl Pts',(-39.5486697096471,-36.78000002,-89.6471359721043));
#145366=CARTESIAN_POINT('Ctrl Pts',(-38.9856597630179,-36.78000002,-89.5246670643281));
#145367=CARTESIAN_POINT('Ctrl Pts',(-39.0541288673858,-36.2092330444632,
-89.5780096393087));
#145368=CARTESIAN_POINT('Ctrl Pts',(-39.470934045995,-36.78000002,-90.4953146912642));
#145369=CARTESIAN_POINT('Ctrl Pts',(-38.9434898522956,-36.7800000199999,
-90.4333580855596));
#145370=CARTESIAN_POINT('Ctrl Pts',(-38.967723555261,-36.2567217271198,
-90.4720476855702));
#145371=CARTESIAN_POINT('Ctrl Pts',(-39.5096795928158,-36.78000002,-91.3254326715997));
#145372=CARTESIAN_POINT('Ctrl Pts',(-39.0324507754533,-36.78000002,-91.348061068846));
#145373=CARTESIAN_POINT('Ctrl Pts',(-39.0107369205707,-36.302690307335,
-91.3486055792047));
#145374=CARTESIAN_POINT('Origin',(-40.4661024946855,-36.28000002,-86.8949524600738));
#145375=CARTESIAN_POINT('Ctrl Pts',(-40.0734472049734,-36.0537916894494,
-86.683643483585));
#145376=CARTESIAN_POINT('Ctrl Pts',(-40.0114299049165,-36.0597067375102,
-86.7925528685563));
#145377=CARTESIAN_POINT('Ctrl Pts',(-39.9525082269032,-36.0657556651474,
-86.9025541827257));
#145378=CARTESIAN_POINT('Ctrl Pts',(-39.8965331132721,-36.071857980972,
-87.0135362800466));
#145379=CARTESIAN_POINT('Ctrl Pts',(-39.8393965078108,-36.0780869207464,
-87.1268212721892));
#145380=CARTESIAN_POINT('Ctrl Pts',(-39.7853292584481,-36.0843716935665,
-87.2411283173954));
#145381=CARTESIAN_POINT('Ctrl Pts',(-39.7341789370736,-36.0906669132536,
-87.3563756163275));
#145382=CARTESIAN_POINT('Ctrl Pts',(-39.6814728827467,-36.0971536015463,
-87.4751281526814));
#145383=CARTESIAN_POINT('Ctrl Pts',(-39.6318631125474,-36.1036516536209,
-87.5948792120369));
#145384=CARTESIAN_POINT('Ctrl Pts',(-39.585201243061,-36.1101500863352,
-87.7155749645938));
#145385=CARTESIAN_POINT('Ctrl Pts',(-39.5379048483671,-36.1167368871198,
-87.8379119822408));
#145386=CARTESIAN_POINT('Ctrl Pts',(-39.4936364182298,-36.1233245580757,
-87.9612199614972));
#145387=CARTESIAN_POINT('Ctrl Pts',(-39.4522709948862,-36.1299348761892,
-88.0854741526894));
#145388=CARTESIAN_POINT('Ctrl Pts',(-39.410242901257,-36.1366510909922,
-88.2117188846207));
#145389=CARTESIAN_POINT('Ctrl Pts',(-39.3712109975668,-36.1433912403681,
-88.3389408708692));
#145390=CARTESIAN_POINT('Ctrl Pts',(-39.3350839554796,-36.1502043283924,
-88.4671395179936));
#145391=CARTESIAN_POINT('Ctrl Pts',(-39.3109789632385,-36.1547502149216,
-88.5526773095123));
#145392=CARTESIAN_POINT('Ctrl Pts',(-39.2881680479569,-36.1593291055865,
-88.6386504236153));
#145393=CARTESIAN_POINT('Ctrl Pts',(-39.2666353702995,-36.1639599373599,
-88.7250630960682));
#145394=CARTESIAN_POINT('Ctrl Pts',(-39.2122577419081,-36.1756544257708,
-88.9432856629837));
#145395=CARTESIAN_POINT('Ctrl Pts',(-39.1661135646958,-36.1874916418147,
-89.1641945089367));
#145396=CARTESIAN_POINT('Ctrl Pts',(-39.1282921823357,-36.1993765320403,
-89.3868152665253));
#145397=CARTESIAN_POINT('Ctrl Pts',(-39.088819852784,-36.2117802115041,
-89.6191536782976));
#145398=CARTESIAN_POINT('Ctrl Pts',(-39.0584124114518,-36.2242363436397,
-89.8533578805103));
#145399=CARTESIAN_POINT('Ctrl Pts',(-39.0371354777509,-36.2366815663543,
-90.0883178712863));
#145400=CARTESIAN_POINT('Ctrl Pts',(-39.016148797974,-36.2489570148533,
-90.320072604186));
#145401=CARTESIAN_POINT('Ctrl Pts',(-39.0040453665294,-36.2612227588303,
-90.5525637896143));
#145402=CARTESIAN_POINT('Ctrl Pts',(-39.0008560407261,-36.2734488399052,
-90.7847063396569));
#145403=CARTESIAN_POINT('Ctrl Pts',(-39.0002860653393,-36.2756338049164,
-90.826193333433));
#145404=CARTESIAN_POINT('Ctrl Pts',(-39.0000007020242,-36.2778175640703,
-90.8676691154279));
#145405=CARTESIAN_POINT('Ctrl Pts',(-39.0000000012937,-36.28000002,-90.9091273827666));
#145406=CARTESIAN_POINT('Ctrl Pts',(-40.0734472163172,-36.0537915241817,
-86.6836433292035));
#145407=CARTESIAN_POINT('Ctrl Pts',(-39.7490326214953,-36.78000002,-86.5090582163831));
#145408=CARTESIAN_POINT('Ctrl Pts',(-40.4661024946855,-36.78000002,-86.8949524600738));
#145409=CARTESIAN_POINT('Ctrl Pts',(-42.3689613408276,-36.0634493712886,
-82.407773086856));
#145410=CARTESIAN_POINT('Ctrl Pts',(-42.0251435460116,-36.78000002,-82.3205925927599));
#145411=CARTESIAN_POINT('Ctrl Pts',(-42.7671781583824,-36.78000002,-82.6190865682492));
#145412=CARTESIAN_POINT('Ctrl Pts',(-44.6279666698635,-36.0719269202766,
-78.1127593269182));
#145413=CARTESIAN_POINT('Ctrl Pts',(-44.3122026972581,-36.7800000199999,
-78.0178858717772));
#145414=CARTESIAN_POINT('Ctrl Pts',(-45.0306161020287,-36.78000002,-78.3240684577782));
#145415=CARTESIAN_POINT('Ctrl Pts',(-49.0993449617391,-36.0872029629615,
-69.4983516685814));
#145416=CARTESIAN_POINT('Ctrl Pts',(-48.8138634148613,-36.78000002,-69.420066134471));
#145417=CARTESIAN_POINT('Ctrl Pts',(-49.5095281828678,-36.78000002,-69.7096607994621));
#145418=CARTESIAN_POINT('Ctrl Pts',(-51.3114450013405,-36.0939978375791,
-65.1788088209436));
#145419=CARTESIAN_POINT('Ctrl Pts',(-51.0452850559209,-36.7800000200001,
-65.0958859597511));
#145420=CARTESIAN_POINT('Ctrl Pts',(-51.7247198970815,-36.78000002,-65.3901198450985));
#145421=CARTESIAN_POINT('Ctrl Pts',(-53.5074514076768,-36.1001753985996,
-60.8508735991007));
#145422=CARTESIAN_POINT('Ctrl Pts',(-53.2738374538033,-36.7800000199999,
-60.7321930665019));
#145423=CARTESIAN_POINT('Ctrl Pts',(-53.9233979868778,-36.78000002,-61.0621827299711));
#145424=CARTESIAN_POINT('Origin',(-59.5,-37.28000002,-55.24995));
#145425=CARTESIAN_POINT('',(-60.,-37.28000002,-174.34995));
#145426=CARTESIAN_POINT('Origin',(-59.5,-37.28000002,-174.34995));
#145427=CARTESIAN_POINT('',(-60.,-37.28000002,-58.24995));
#145428=CARTESIAN_POINT('Origin',(-57.,-37.28000002,-174.34995));
#145429=CARTESIAN_POINT('Origin',(-57.,-37.28000002,-174.34995));
#145430=CARTESIAN_POINT('Ctrl Pts',(-39.,-38.3588510099497,-88.7507007177297));
#145431=CARTESIAN_POINT('Ctrl Pts',(-39.,-37.0899493132599,-87.566881951549));
#145432=CARTESIAN_POINT('Ctrl Pts',(-40.0751063884513,-36.0938884806558,
-86.6376094090262));
#145433=CARTESIAN_POINT('Ctrl Pts',(-39.,-37.1517824539261,-90.044523203833));
#145434=CARTESIAN_POINT('Ctrl Pts',(-38.9999999999755,-35.9377762186181,
-88.8634929468774));
#145435=CARTESIAN_POINT('Ctrl Pts',(-40.0284942066422,-34.9676073874133,
-87.9314164096932));
#145436=CARTESIAN_POINT('Ctrl Pts',(-39.,-35.9043080884012,-91.3133047711639));
#145437=CARTESIAN_POINT('Ctrl Pts',(-39.0000000000062,-34.7456425298457,
-90.138609363953));
#145438=CARTESIAN_POINT('Ctrl Pts',(-39.9811083568879,-33.8078923846355,
-89.2002134624161));
#145439=CARTESIAN_POINT('Ctrl Pts',(-39.,-33.3065376953223,-93.7717385435459));
#145440=CARTESIAN_POINT('Ctrl Pts',(-38.9999999999938,-32.2660375633753,
-92.6092802152048));
#145441=CARTESIAN_POINT('Ctrl Pts',(-39.8860349814824,-31.4034505542693,
-91.6586472348866));
#145442=CARTESIAN_POINT('Ctrl Pts',(-39.,-31.9694828580011,-94.9490286570666));
#145443=CARTESIAN_POINT('Ctrl Pts',(-39.,-30.9915371636578,-93.792984660173));
#145444=CARTESIAN_POINT('Ctrl Pts',(-39.8388209456929,-30.1709967638591,
-92.8359193626927));
#145445=CARTESIAN_POINT('Ctrl Pts',(-39.,-30.5806160716777,-96.0559019707015));
#145446=CARTESIAN_POINT('Ctrl Pts',(-39.,-29.6660656545474,-94.9083553778138));
#145447=CARTESIAN_POINT('Ctrl Pts',(-39.7930043023957,-28.8965637205256,
-93.942810661998));
#145448=CARTESIAN_POINT('',(-39.,-30.63000002,-96.0164973302555));
#145449=CARTESIAN_POINT('Ctrl Pts',(-39.,-30.63000002,-96.0164973302555));
#145450=CARTESIAN_POINT('Ctrl Pts',(-39.0000000000004,-31.0448154973603,
-95.6851069386961));
#145451=CARTESIAN_POINT('Ctrl Pts',(-39.0000000000118,-31.4542117376853,
-95.3480909235783));
#145452=CARTESIAN_POINT('Ctrl Pts',(-39.0000000000377,-31.8588908811782,
-95.0057530542713));
#145453=CARTESIAN_POINT('Ctrl Pts',(-39.0000000000646,-32.2780518714119,
-94.651164282894));
#145454=CARTESIAN_POINT('Ctrl Pts',(-39.0000000001072,-32.692151896703,
-94.2908656551339));
#145455=CARTESIAN_POINT('Ctrl Pts',(-39.0000000001713,-33.101937367171,
-93.925148764688));
#145456=CARTESIAN_POINT('Ctrl Pts',(-39.0000000002394,-33.5373888365781,
-93.5365260125201));
#145457=CARTESIAN_POINT('Ctrl Pts',(-39.0000000003318,-33.9679681800119,
-93.1417847772573));
#145458=CARTESIAN_POINT('Ctrl Pts',(-39.0000000004578,-34.3945363851635,
-92.7412278682546));
#145459=CARTESIAN_POINT('Ctrl Pts',(-39.0000000004786,-34.4649233357429,
-92.6751329764701));
#145460=CARTESIAN_POINT('Ctrl Pts',(-39.0000000005003,-34.5352010050805,
-92.6088796460175));
#145461=CARTESIAN_POINT('Ctrl Pts',(-39.000000000523,-34.605373184231,-92.5424691324455));
#145462=CARTESIAN_POINT('Ctrl Pts',(-39.0000000006715,-35.0646606142765,
-92.1078023674154));
#145463=CARTESIAN_POINT('Ctrl Pts',(-39.0000000008613,-35.5177770524177,
-91.6679502774283));
#145464=CARTESIAN_POINT('Ctrl Pts',(-39.0000000011092,-35.9656372187857,
-91.2230746457426));
#145465=CARTESIAN_POINT('Ctrl Pts',(-39.0000000011674,-36.0707105046109,
-91.1187015670117));
#145466=CARTESIAN_POINT('Ctrl Pts',(-39.0000000012288,-36.1754942796843,
-91.0140518531514));
#145467=CARTESIAN_POINT('Ctrl Pts',(-39.0000000012937,-36.28000002,-90.9091273827666));
#145468=CARTESIAN_POINT('Ctrl Pts',(-39.,-30.63000002,-96.0164973302555));
#145469=CARTESIAN_POINT('Ctrl Pts',(-39.0000000079586,-30.6231766417215,
-95.8820262726144));
#145470=CARTESIAN_POINT('Ctrl Pts',(-39.0035821145827,-30.6163413437257,
-95.7481485193516));
#145471=CARTESIAN_POINT('Ctrl Pts',(-39.0106426175382,-30.6095153827799,
-95.6148868536627));
#145472=CARTESIAN_POINT('Ctrl Pts',(-39.0178214769745,-30.6025749970231,
-95.4793912987054));
#145473=CARTESIAN_POINT('Ctrl Pts',(-39.0285958092194,-30.5956437403606,
-95.3445319365772));
#145474=CARTESIAN_POINT('Ctrl Pts',(-39.0429017264386,-30.5887258812893,
-95.2103098405928));
#145475=CARTESIAN_POINT('Ctrl Pts',(-39.0572494516417,-30.5817878052871,
-95.0756954904708));
#145476=CARTESIAN_POINT('Ctrl Pts',(-39.0751492079689,-30.5748625588069,
-94.9417213032506));
#145477=CARTESIAN_POINT('Ctrl Pts',(-39.0965870557023,-30.5679453488797,
-94.808377425016));
#145478=CARTESIAN_POINT('Ctrl Pts',(-39.1179306962842,-30.5610585361571,
-94.6756195173088));
#145479=CARTESIAN_POINT('Ctrl Pts',(-39.1427814447475,-30.5541790046426,
-94.5434855565985));
#145480=CARTESIAN_POINT('Ctrl Pts',(-39.1711767973116,-30.5473030129425,
-94.4119675106066));
#145481=CARTESIAN_POINT('Ctrl Pts',(-39.1839235911889,-30.5442163511831,
-94.3529285034445));
#145482=CARTESIAN_POINT('Ctrl Pts',(-39.1973853608932,-30.5411304784574,
-94.2940137110658));
#145483=CARTESIAN_POINT('Ctrl Pts',(-39.2115687799563,-30.5380456903908,
-94.2352231979354));
#145484=CARTESIAN_POINT('Ctrl Pts',(-39.2472280937484,-30.5302900550844,
-94.0874147360689));
#145485=CARTESIAN_POINT('Ctrl Pts',(-39.2874998404854,-30.522578402994,
-93.9401454048209));
#145486=CARTESIAN_POINT('Ctrl Pts',(-39.332455133363,-30.5148808266874,
-93.793846273556));
#145487=CARTESIAN_POINT('Ctrl Pts',(-39.3763272094434,-30.507368726738,
-93.6510722817411));
#145488=CARTESIAN_POINT('Ctrl Pts',(-39.4246605045649,-30.4998700742262,
-93.5092222546581));
#145489=CARTESIAN_POINT('Ctrl Pts',(-39.4775038131332,-30.4923933804749,
-93.3687230037208));
#145490=CARTESIAN_POINT('Ctrl Pts',(-39.530512762818,-30.4848932504942,
-93.227783347869));
#145491=CARTESIAN_POINT('Ctrl Pts',(-39.5880608773232,-30.4774152181983,
-93.0882029261299));
#145492=CARTESIAN_POINT('Ctrl Pts',(-39.6501685426812,-30.4700048105513,
-92.9504399167027));
#145493=CARTESIAN_POINT('Ctrl Pts',(-39.7091203015329,-30.4629709514925,
-92.8196771249667));
#145494=CARTESIAN_POINT('Ctrl Pts',(-39.7721804412542,-30.4559984296717,
-92.6905520637433));
#145495=CARTESIAN_POINT('Ctrl Pts',(-39.8393317526662,-30.4491558380067,
-92.5634785170804));
#145496=CARTESIAN_POINT('Ctrl Pts',(-39.8429266116615,-30.4487895286722,
-92.5566757983741));
#145497=CARTESIAN_POINT('Ctrl Pts',(-39.8465331858288,-30.4484235982178,
-92.5498789637867));
#145498=CARTESIAN_POINT('Ctrl Pts',(-39.8501514691891,-30.4480580593471,
-92.543088078389));
#145499=CARTESIAN_POINT('Ctrl Pts',(-55.5967474138374,-30.4937575588533,
-60.8508735991007));
#145500=CARTESIAN_POINT('Ctrl Pts',(-55.6892944482707,-30.13000002,-60.8961225062558));
#145501=CARTESIAN_POINT('Ctrl Pts',(-56.0289353856639,-30.13000002,-61.0621827299711));
#145502=CARTESIAN_POINT('Ctrl Pts',(-53.0072677069205,-30.4880260434848,
-66.1508000801069));
#145503=CARTESIAN_POINT('Ctrl Pts',(-53.1140955473737,-30.1300000200305,
-66.1737552088486));
#145504=CARTESIAN_POINT('Ctrl Pts',(-53.4376477846732,-30.13000002,-66.3621114555649));
#145505=CARTESIAN_POINT('Ctrl Pts',(-50.405384759569,-30.4815921581836,
-71.4443972343972));
#145506=CARTESIAN_POINT('Ctrl Pts',(-50.518482898395,-30.13000002,-71.4624685012804));
#145507=CARTESIAN_POINT('Ctrl Pts',(-50.8336218773704,-30.13000002,-71.655706365272));
#145508=CARTESIAN_POINT('Ctrl Pts',(-45.1629315870884,-30.4666308723541,
-82.01174695052));
#145509=CARTESIAN_POINT('Ctrl Pts',(-45.2819556815256,-30.13000002,-82.0338364947541));
#145510=CARTESIAN_POINT('Ctrl Pts',(-45.5856873606873,-30.13000002,-82.223056081386));
#145511=CARTESIAN_POINT('Ctrl Pts',(-42.5227129344255,-30.4581147715466,
-87.2856833539494));
#145512=CARTESIAN_POINT('Ctrl Pts',(-42.650123001142,-30.13000002,-87.3003867975457));
#145513=CARTESIAN_POINT('Ctrl Pts',(-42.94214612644,-30.13000002,-87.4969984415611));
#145514=CARTESIAN_POINT('Ctrl Pts',(-39.850159149164,-30.447965242174,-92.5429803300057));
#145515=CARTESIAN_POINT('Ctrl Pts',(-39.9609182162754,-30.13000002,-92.5993786427328));
#145516=CARTESIAN_POINT('Ctrl Pts',(-40.2651432342477,-30.13000002,-92.7542894608761));
#145517=CARTESIAN_POINT('Origin',(-40.2651432342477,-30.63000002,-92.754289460876));
#145518=CARTESIAN_POINT('Ctrl Pts',(-39.5006706228584,-30.13000002,-96.1170957262314));
#145519=CARTESIAN_POINT('Ctrl Pts',(-38.9951731461558,-30.13000002,-96.1239966937518));
#145520=CARTESIAN_POINT('Ctrl Pts',(-39.0007459084378,-30.6355158392231,
-96.123928310321));
#145521=CARTESIAN_POINT('Ctrl Pts',(-39.4926444736916,-30.13000002,-95.5146217937464));
#145522=CARTESIAN_POINT('Ctrl Pts',(-39.018727596565,-30.1300000199999,
-95.5002240857988));
#145523=CARTESIAN_POINT('Ctrl Pts',(-38.9918233137184,-30.6029340469193,
-95.4804746285911));
#145524=CARTESIAN_POINT('Ctrl Pts',(-39.5567080597613,-30.13000002,-94.9242583718701));
#145525=CARTESIAN_POINT('Ctrl Pts',(-39.1128426389465,-30.13000002,-94.8742326636326));
#145526=CARTESIAN_POINT('Ctrl Pts',(-39.0630015628091,-30.5704212349622,
-94.8509849588091));
#145527=CARTESIAN_POINT('Ctrl Pts',(-39.824074198694,-30.13000002,-93.7675786356602));
#145528=CARTESIAN_POINT('Ctrl Pts',(-39.4497207067778,-30.13000002,-93.6636460107682));
#145529=CARTESIAN_POINT('Ctrl Pts',(-39.3600684015271,-30.5057885431007,
-93.6194738625269));
#145530=CARTESIAN_POINT('Ctrl Pts',(-40.0302908384928,-30.13000002,-93.1965579604184));
#145531=CARTESIAN_POINT('Ctrl Pts',(-39.6888362216248,-30.13000002,-93.0681539889851));
#145532=CARTESIAN_POINT('Ctrl Pts',(-39.5891998109869,-30.4733919576177,
-93.0124665383103));
#145533=CARTESIAN_POINT('Ctrl Pts',(-40.3113967419659,-30.13000002,-92.6651768309653));
#145534=CARTESIAN_POINT('Ctrl Pts',(-40.0131400269601,-30.13000002,-92.5073906291708));
#145535=CARTESIAN_POINT('Ctrl Pts',(-39.9015329389956,-30.4429085637657,
-92.4483628961121));
#145536=CARTESIAN_POINT('Origin',(-39.5,-30.63000002,-96.0164973302555));
#145537=CARTESIAN_POINT('Origin',(-39.5,-30.63000002,-55.24995));
#145538=CARTESIAN_POINT('',(-39.,-30.63000002,-136.04214564125));
#145539=CARTESIAN_POINT('Origin',(-39.5,-30.63000002,-136.04214564125));
#145540=CARTESIAN_POINT('',(-39.,-30.63000002,-129.34995));
#145541=CARTESIAN_POINT('Ctrl Pts',(-40.2651432342477,-30.13000002,-139.30435351063));
#145542=CARTESIAN_POINT('Ctrl Pts',(-39.9609182162754,-30.13000002,-139.459264328773));
#145543=CARTESIAN_POINT('Ctrl Pts',(-39.850159149164,-30.447965242174,-139.5156626415));
#145544=CARTESIAN_POINT('Ctrl Pts',(-40.0075294671789,-30.13000002,-138.798433034953));
#145545=CARTESIAN_POINT('Ctrl Pts',(-39.6630612728547,-30.13000002,-138.925676053694));
#145546=CARTESIAN_POINT('Ctrl Pts',(-39.5639348330521,-30.4769451657213,
-138.978519823589));
#145547=CARTESIAN_POINT('Ctrl Pts',(-39.8201451200256,-30.13000002,-138.270288236581));
#145548=CARTESIAN_POINT('Ctrl Pts',(-39.4450625268456,-30.13000002,-138.37488926852));
#145549=CARTESIAN_POINT('Ctrl Pts',(-39.3557167999464,-30.5068849023477,
-138.41703103581));
#145550=CARTESIAN_POINT('Ctrl Pts',(-39.5656143592083,-30.13000002,-137.176619865119));
#145551=CARTESIAN_POINT('Ctrl Pts',(-39.1248051359359,-30.13000002,-137.23047141255));
#145552=CARTESIAN_POINT('Ctrl Pts',(-39.0729048436467,-30.5680016657979,
-137.252632910085));
#145553=CARTESIAN_POINT('Ctrl Pts',(-39.5000000014551,-30.13000002,-136.607413315277));
#145554=CARTESIAN_POINT('Ctrl Pts',(-39.0297176446585,-30.13000002,-136.627803193949));
#145555=CARTESIAN_POINT('Ctrl Pts',(-39.,-30.5993710675033,-136.645762741564));
#145556=CARTESIAN_POINT('Ctrl Pts',(-39.5,-30.13000002,-136.04214564125));
#145557=CARTESIAN_POINT('Ctrl Pts',(-39.,-30.13000002,-136.04214564125));
#145558=CARTESIAN_POINT('Ctrl Pts',(-39.,-30.63000002,-136.04214564125));
#145559=CARTESIAN_POINT('',(-39.850159149164,-30.447965242174,-139.5156626415));
#145560=CARTESIAN_POINT('Origin',(-40.2651432342477,-30.63000002,-139.30435351063));
#145561=CARTESIAN_POINT('Ctrl Pts',(-39.8501336361171,-30.4479678253678,
-139.515614761992));
#145562=CARTESIAN_POINT('Ctrl Pts',(-39.5639224597867,-30.4769469448861,
-138.978486457187));
#145563=CARTESIAN_POINT('Ctrl Pts',(-39.3557125984323,-30.5068858103113,
-138.417013737266));
#145564=CARTESIAN_POINT('Ctrl Pts',(-39.0729048436467,-30.5680016657979,
-137.252632910085));
#145565=CARTESIAN_POINT('Ctrl Pts',(-39.,-30.5993710675033,-136.645762741564));
#145566=CARTESIAN_POINT('Ctrl Pts',(-39.,-30.63000002,-136.04214564125));
#145567=CARTESIAN_POINT('Ctrl Pts',(-39.850159149164,-30.447965242174,-139.5156626415));
#145568=CARTESIAN_POINT('Ctrl Pts',(-39.9609182162754,-30.1300000199999,
-139.459264328773));
#145569=CARTESIAN_POINT('Ctrl Pts',(-40.2651432342477,-30.13000002,-139.30435351063));
#145570=CARTESIAN_POINT('Ctrl Pts',(-42.5429900246349,-30.4581917776324,
-144.812847565038));
#145571=CARTESIAN_POINT('Ctrl Pts',(-42.6706800009636,-30.13000002,-144.798763083095));
#145572=CARTESIAN_POINT('Ctrl Pts',(-42.9624569131523,-30.13000002,-144.601532315192));
#145573=CARTESIAN_POINT('Ctrl Pts',(-45.2030035072277,-30.4667604203174,
-150.126917764117));
#145574=CARTESIAN_POINT('Ctrl Pts',(-45.3221739986871,-30.1300000200307,
-150.105257848785));
#145575=CARTESIAN_POINT('Ctrl Pts',(-45.6258101137111,-30.13000002,-149.91560863326));
#145576=CARTESIAN_POINT('Ctrl Pts',(-50.484627394531,-30.4818027714,-160.774746655264));
#145577=CARTESIAN_POINT('Ctrl Pts',(-50.5978344679358,-30.1300000199689,
-160.757133407541));
#145578=CARTESIAN_POINT('Ctrl Pts',(-50.9129382266982,-30.13000002,-160.563437524381));
#145579=CARTESIAN_POINT('Ctrl Pts',(-53.105875183067,-30.4882648083968,
-166.108694936931));
#145580=CARTESIAN_POINT('Ctrl Pts',(-53.2127313470812,-30.1300000198871,
-166.08608254617));
#145581=CARTESIAN_POINT('Ctrl Pts',(-53.53633422979,-30.13000002,-165.897383514726));
#145582=CARTESIAN_POINT('Ctrl Pts',(-55.7146117108563,-30.4940179634924,
-171.449026400902));
#145583=CARTESIAN_POINT('Ctrl Pts',(-55.8070372118623,-30.13000002,-171.403845487572));
#145584=CARTESIAN_POINT('Ctrl Pts',(-56.1468816861249,-30.13000002,-171.237717270032));
#145585=CARTESIAN_POINT('',(-55.7146117108563,-30.4940179634924,-171.449026400902));
#145586=CARTESIAN_POINT('Origin',(-56.146881686125,-30.63000002,-171.237717270032));
#145587=CARTESIAN_POINT('Ctrl Pts',(-55.7146117108563,-30.4940179634924,
-171.449026400902));
#145588=CARTESIAN_POINT('Ctrl Pts',(-53.105875183067,-30.4882648083968,
-166.108694936931));
#145589=CARTESIAN_POINT('Ctrl Pts',(-50.484627394531,-30.4818027714,-160.774746655264));
#145590=CARTESIAN_POINT('Ctrl Pts',(-45.2030035072277,-30.4667604203174,
-150.126917764117));
#145591=CARTESIAN_POINT('Ctrl Pts',(-42.5429900246349,-30.4581917776324,
-144.812847565038));
#145592=CARTESIAN_POINT('Ctrl Pts',(-39.850159149164,-30.447965242174,-139.5156626415));
#145593=CARTESIAN_POINT('Ctrl Pts',(-55.6935671754689,-30.4968373543262,
-171.410008924778));
#145594=CARTESIAN_POINT('Ctrl Pts',(-55.7825352402592,-30.1299356988045,
-171.361452749053));
#145595=CARTESIAN_POINT('Ctrl Pts',(-56.1167176003611,-30.1300000271399,
-171.179145966886));
#145596=CARTESIAN_POINT('Ctrl Pts',(-55.7814946229066,-30.4850537049709,
-171.564548662911));
#145597=CARTESIAN_POINT('Ctrl Pts',(-55.8840206261747,-30.1299383387469,
-171.527291609574));
#145598=CARTESIAN_POINT('Ctrl Pts',(-56.2430624746474,-30.1300000269106,
-171.410992898787));
#145599=CARTESIAN_POINT('Ctrl Pts',(-55.8246219322658,-30.4793202225602,
-171.737832654878));
#145600=CARTESIAN_POINT('Ctrl Pts',(-55.9360241189749,-30.1299395985436,
-171.722483207042));
#145601=CARTESIAN_POINT('Ctrl Pts',(-56.3050537145652,-30.130000026799,
-171.670900042786));
#145602=CARTESIAN_POINT('Ctrl Pts',(-55.8160539307423,-30.4804600576221,
-171.916099630748));
#145603=CARTESIAN_POINT('Ctrl Pts',(-55.925777764091,-30.1299393505852,
-171.921245295793));
#145604=CARTESIAN_POINT('Ctrl Pts',(-56.2927384034373,-30.1300000268212,
-171.938334598151));
#145605=CARTESIAN_POINT('Origin',(-56.294192362543,-30.63000002,-171.871644662643));
#145606=CARTESIAN_POINT('Origin',(-54.6808724388942,-30.6336549073814,-171.881456078396));
#145607=CARTESIAN_POINT('Origin',(-56.294192362543,-30.63000002,-179.64995));
#145608=CARTESIAN_POINT('Origin',(-56.294192362543,-30.63000002,-176.84995));
#145609=CARTESIAN_POINT('Origin',(83.2809572255632,-29.6300000199999,-176.84995));
#145610=CARTESIAN_POINT('',(-57.,-29.63000002,-177.34995));
#145611=CARTESIAN_POINT('Origin',(-57.,-29.63000002,-176.84995));
#145612=CARTESIAN_POINT('',(-56.5982428503831,-29.63000002,-177.34995));
#145613=CARTESIAN_POINT('',(-60.,-29.63000002,-177.34995));
#145614=CARTESIAN_POINT('Ctrl Pts',(-56.294192362543,-30.13000002,-176.84995));
#145615=CARTESIAN_POINT('Ctrl Pts',(-56.2941923707649,-30.1300000200003,
-176.98587944854));
#145616=CARTESIAN_POINT('Ctrl Pts',(-56.3301688951883,-30.0730055436657,
-177.116037754475));
#145617=CARTESIAN_POINT('Ctrl Pts',(-56.4164036466448,-29.9329688836733,
-177.253030654974));
#145618=CARTESIAN_POINT('Ctrl Pts',(-56.4500227583409,-29.8779487295679,
-177.288930648015));
#145619=CARTESIAN_POINT('Ctrl Pts',(-56.5223271856603,-29.7580969359688,
-177.337570500007));
#145620=CARTESIAN_POINT('Ctrl Pts',(-56.5603834356575,-29.6942993846806,
-177.34995));
#145621=CARTESIAN_POINT('Ctrl Pts',(-56.5982428503831,-29.63000002,-177.34995));
#145622=CARTESIAN_POINT('Origin',(-57.,-29.63000002,-174.34995));
#145623=CARTESIAN_POINT('',(-60.,-29.63000002,-174.34995));
#145624=CARTESIAN_POINT('Origin',(-59.5,-29.63000002,-174.34995));
#145625=CARTESIAN_POINT('Origin',(-57.,-29.63000002,-174.34995));
#145626=CARTESIAN_POINT('Origin',(-59.5,-29.63000002,-55.24995));
#145627=CARTESIAN_POINT('',(-60.,-29.63000002,-58.24995));
#145628=CARTESIAN_POINT('Origin',(-59.5,-29.63000002,-58.24995));
#145629=CARTESIAN_POINT('',(-60.,-29.63000002,-174.34995));
#145630=CARTESIAN_POINT('Origin',(-57.,-29.63000002,-58.24995));
#145631=CARTESIAN_POINT('Origin',(-57.,-29.63000002,-58.24995));
#145632=CARTESIAN_POINT('Origin',(-57.,-2.42462934179819E-14,-58.24995));
#145633=CARTESIAN_POINT('',(-60.,-29.13000002,-58.24995));
#145634=CARTESIAN_POINT('Origin',(-57.,-29.13000002,-58.24995));
#145635=CARTESIAN_POINT('',(-60.,-54.58000002,-58.24995));
#145636=CARTESIAN_POINT('Origin',(-57.,-29.13000002,-58.24995));
#145637=CARTESIAN_POINT('Origin',(-59.5,-29.13000002,-58.24995));
#145638=CARTESIAN_POINT('Ctrl Pts',(-39.7602371906926,-27.9700232578782,
-94.7283182364936));
#145639=CARTESIAN_POINT('Ctrl Pts',(-39.5607615517246,-28.6300000199999,
-94.628899882694));
#145640=CARTESIAN_POINT('Ctrl Pts',(-40.1842134716234,-28.63000002,-94.9396273673639));
#145641=CARTESIAN_POINT('Ctrl Pts',(-42.5604321400969,-27.9797945689722,
-89.1025347299149));
#145642=CARTESIAN_POINT('Ctrl Pts',(-42.3373257946448,-28.63000002,-89.0914456452771));
#145643=CARTESIAN_POINT('Ctrl Pts',(-42.9880924510224,-28.63000002,-89.3138497353063));
#145644=CARTESIAN_POINT('Ctrl Pts',(-45.3330806261701,-27.9878402480233,
-83.4627911786917));
#145645=CARTESIAN_POINT('Ctrl Pts',(-45.1354691768678,-28.630000020022,
-83.4336169877673));
#145646=CARTESIAN_POINT('Ctrl Pts',(-45.7634210292322,-28.63000002,-83.6741003095587));
#145647=CARTESIAN_POINT('Ctrl Pts',(-50.8469740031289,-28.0018438144725,
-72.1674540521641));
#145648=CARTESIAN_POINT('Ctrl Pts',(-50.6710028559025,-28.6300000199784,
-72.148355955617));
#145649=CARTESIAN_POINT('Ctrl Pts',(-51.2816902902029,-28.63000002,-72.3787631830378));
#145650=CARTESIAN_POINT('Ctrl Pts',(-53.5878832423525,-28.0077864042225,
-66.5116884426403));
#145651=CARTESIAN_POINT('Ctrl Pts',(-53.4278489247074,-28.6300000200659,
-66.4825194498726));
#145652=CARTESIAN_POINT('Ctrl Pts',(-54.0242786911866,-28.63000002,-66.7229996739341));
#145653=CARTESIAN_POINT('Ctrl Pts',(-56.3187331343194,-28.0130417005584,
-60.8508735991007));
#145654=CARTESIAN_POINT('Ctrl Pts',(-56.1850547298497,-28.63000002,-60.7863522634768));
#145655=CARTESIAN_POINT('Ctrl Pts',(-56.7565335485771,-28.63000002,-61.0621827299711));
#145656=CARTESIAN_POINT('Origin',(-40.1842134716234,-28.13000002,-94.9396273673639));
#145657=CARTESIAN_POINT('Origin',(-59.5,-29.13000002,-55.24995));
#145658=CARTESIAN_POINT('',(-60.,-29.13000002,-174.34995));
#145659=CARTESIAN_POINT('Origin',(-59.5,-29.13000002,-174.34995));
#145660=CARTESIAN_POINT('',(-60.,-29.13000002,-58.24995));
#145661=CARTESIAN_POINT('Origin',(-57.,-29.13000002,-174.34995));
#145662=CARTESIAN_POINT('',(-57.,-29.13000002,-177.34995));
#145663=CARTESIAN_POINT('',(-57.,-28.664523125878,-177.032518510534));
#145664=CARTESIAN_POINT('Origin',(-57.,-29.13000002,-176.84995));
#145665=CARTESIAN_POINT('Origin',(-57.,-29.13000002,-174.34995));
#145666=CARTESIAN_POINT('Ctrl Pts',(-57.,-28.664523125878,-177.032518510534));
#145667=CARTESIAN_POINT('Ctrl Pts',(-57.0114676733044,-28.6416054347749,
-176.974087537723));
#145668=CARTESIAN_POINT('Ctrl Pts',(-57.0179413444383,-28.63000002,-176.912963832989));
#145669=CARTESIAN_POINT('Ctrl Pts',(-57.0184057454332,-28.63000002,-176.849882244789));
#145670=CARTESIAN_POINT('Origin',(-57.0184057454332,-28.13000002,-179.64995));
#145671=CARTESIAN_POINT('Origin',(-57.0184057454332,-28.13000002,-171.871644662643));
#145672=CARTESIAN_POINT('Origin',(-57.0184057454332,-28.13000002,-176.849882244789));
#145673=CARTESIAN_POINT('Ctrl Pts',(-56.5341822214496,-28.0016231613287,
-171.915549358366));
#145674=CARTESIAN_POINT('Ctrl Pts',(-56.3674234002834,-28.6301310958619,
-171.907871533399));
#145675=CARTESIAN_POINT('Ctrl Pts',(-57.0170289507251,-28.6300000098419,
-171.937510237498));
#145676=CARTESIAN_POINT('Ctrl Pts',(-56.5423215389878,-28.0006714526254,
-171.739685194435));
#145677=CARTESIAN_POINT('Ctrl Pts',(-56.3722793953445,-28.6301314641988,
-171.762633256233));
#145678=CARTESIAN_POINT('Ctrl Pts',(-57.0288581213359,-28.6300000098265,
-171.673675468004));
#145679=CARTESIAN_POINT('Ctrl Pts',(-56.5015214234675,-28.0054385079109,
-171.56638157453));
#145680=CARTESIAN_POINT('Ctrl Pts',(-56.3485431365434,-28.6301296243107,
-171.621528645646));
#145681=CARTESIAN_POINT('Ctrl Pts',(-56.9695606031425,-28.6300000099035,
-171.413737441436));
#145682=CARTESIAN_POINT('Ctrl Pts',(-56.4142663415167,-28.0157208016423,
-171.409463522487));
#145683=CARTESIAN_POINT('Ctrl Pts',(-56.287357164279,-28.6301257916421,
-171.477955081175));
#145684=CARTESIAN_POINT('Ctrl Pts',(-56.8427717751314,-28.6300000100697,
-171.178320644756));
#145685=CARTESIAN_POINT('',(-56.4351108624337,-28.0132652467914,-171.449026400902));
#145686=CARTESIAN_POINT('Origin',(-56.8729709358987,-28.13000002,-171.237717270032));
#145687=CARTESIAN_POINT('Origin',(-55.1751592863144,-28.1616555077833,-171.933533580786));
#145688=CARTESIAN_POINT('Ctrl Pts',(-56.4351108624337,-28.0132652467914,
-171.449026400902));
#145689=CARTESIAN_POINT('Ctrl Pts',(-56.3017476121307,-28.63000002,-171.51338685352));
#145690=CARTESIAN_POINT('Ctrl Pts',(-56.8729709358987,-28.63000002,-171.237717270032));
#145691=CARTESIAN_POINT('Ctrl Pts',(-53.6851592779725,-28.007992698407,
-165.747855383941));
#145692=CARTESIAN_POINT('Ctrl Pts',(-53.5252373050999,-28.6300000202211,
-165.776484176476));
#145693=CARTESIAN_POINT('Ctrl Pts',(-54.1216126416942,-28.63000002,-165.536544112802));
#145694=CARTESIAN_POINT('Ctrl Pts',(-50.9250693333912,-28.0020271923581,
-160.051772415584));
#145695=CARTESIAN_POINT('Ctrl Pts',(-50.7490667135706,-28.63000002,-160.070107012222));
#145696=CARTESIAN_POINT('Ctrl Pts',(-51.3598402340296,-28.63000002,-159.840463284713));
#145697=CARTESIAN_POINT('Ctrl Pts',(-45.3724783922449,-27.9879549525026,
-148.675968242465));
#145698=CARTESIAN_POINT('Ctrl Pts',(-45.1747354310855,-28.63000002,-148.704407489125));
#145699=CARTESIAN_POINT('Ctrl Pts',(-45.8028572712098,-28.63000002,-148.464659111595));
#145700=CARTESIAN_POINT('Ctrl Pts',(-42.5803228338128,-27.9798639777307,
-142.996070008035));
#145701=CARTESIAN_POINT('Ctrl Pts',(-42.3567693699165,-28.6300000199999,
-143.005974713683));
#145702=CARTESIAN_POINT('Ctrl Pts',(-43.0080092605004,-28.63000002,-142.784754854138));
#145703=CARTESIAN_POINT('Ctrl Pts',(-39.7602371906926,-27.9700232578782,
-137.330324735012));
#145704=CARTESIAN_POINT('Ctrl Pts',(-39.5607615517247,-28.63000002,-137.429743088812));
#145705=CARTESIAN_POINT('Ctrl Pts',(-40.1842134716234,-28.63000002,-137.119015604142));
#145706=CARTESIAN_POINT('',(-39.7602371906121,-27.9700232581448,-137.330324735053));
#145707=CARTESIAN_POINT('Origin',(-40.1842134716235,-28.13000002,-137.119015604142));
#145708=CARTESIAN_POINT('Ctrl Pts',(-39.7602371906927,-27.9700232578782,
-137.330324735012));
#145709=CARTESIAN_POINT('Ctrl Pts',(-42.5803228332686,-27.9798639793132,
-142.996070008059));
#145710=CARTESIAN_POINT('Ctrl Pts',(-45.3724783917581,-27.9879549540833,
-148.675968242535));
#145711=CARTESIAN_POINT('Ctrl Pts',(-50.9250693329494,-28.0020271939342,
-160.051772415631));
#145712=CARTESIAN_POINT('Ctrl Pts',(-53.6851592775679,-28.0079926999806,
-165.747855384014));
#145713=CARTESIAN_POINT('Ctrl Pts',(-56.4351108624337,-28.0132652467914,
-171.449026400902));
#145714=CARTESIAN_POINT('Ctrl Pts',(-39.5,-28.63000002,-134.169022080262));
#145715=CARTESIAN_POINT('Ctrl Pts',(-39.,-28.63000002,-134.169022080263));
#145716=CARTESIAN_POINT('Ctrl Pts',(-39.,-28.13000002,-134.169022080262));
#145717=CARTESIAN_POINT('Ctrl Pts',(-39.500000002646,-28.63000002,-134.681913680777));
#145718=CARTESIAN_POINT('Ctrl Pts',(-38.9725065924499,-28.63000002,-134.735408648257));
#145719=CARTESIAN_POINT('Ctrl Pts',(-39.,-28.1032444606982,-134.720208320017));
#145720=CARTESIAN_POINT('Ctrl Pts',(-39.5577923442835,-28.63000002,-135.185082649765));
#145721=CARTESIAN_POINT('Ctrl Pts',(-39.0091060618314,-28.6300000199999,
-135.282961361938));
#145722=CARTESIAN_POINT('Ctrl Pts',(-39.0642137165569,-28.076417661445,
-135.260142317137));
#145723=CARTESIAN_POINT('Ctrl Pts',(-39.7843604313674,-28.63000002,-136.172328627912));
#145724=CARTESIAN_POINT('Ctrl Pts',(-39.1926311399543,-28.63000002,-136.37231025087));
#145725=CARTESIAN_POINT('Ctrl Pts',(-39.3159560341664,-28.0228058044255,
-136.318039323049));
#145726=CARTESIAN_POINT('Ctrl Pts',(-39.9554204749436,-28.63000002,-136.659959223536));
#145727=CARTESIAN_POINT('Ctrl Pts',(-39.3499007457719,-28.63000002,-136.920217264961));
#145728=CARTESIAN_POINT('Ctrl Pts',(-39.5060247583741,-27.995814073424,
-136.839791694484));
#145729=CARTESIAN_POINT('Ctrl Pts',(-40.1842134716234,-28.63000002,-137.119015604142));
#145730=CARTESIAN_POINT('Ctrl Pts',(-39.5607615517247,-28.63000002,-137.429743088812));
#145731=CARTESIAN_POINT('Ctrl Pts',(-39.7602371906926,-27.9700232578782,
-137.330324735012));
#145732=CARTESIAN_POINT('',(-39.0000000005543,-28.13000002,-134.169022080262));
#145733=CARTESIAN_POINT('Origin',(-39.5,-28.13000002,-134.169022080262));
#145734=CARTESIAN_POINT('Ctrl Pts',(-39.,-28.13000002,-134.169022080262));
#145735=CARTESIAN_POINT('Ctrl Pts',(-38.9999999999924,-28.1032444608434,
-134.720208320021));
#145736=CARTESIAN_POINT('Ctrl Pts',(-39.0642137165422,-28.0764176615931,
-135.260142317143));
#145737=CARTESIAN_POINT('Ctrl Pts',(-39.3159560341354,-28.0228058045779,
-136.318039323063));
#145738=CARTESIAN_POINT('Ctrl Pts',(-39.5060247583362,-27.9958140735776,
-136.839791694503));
#145739=CARTESIAN_POINT('Ctrl Pts',(-39.7602371906927,-27.9700232578782,
-137.330324735012));
#145740=CARTESIAN_POINT('Origin',(-39.5,-28.13000002,-55.24995));
#145741=CARTESIAN_POINT('',(-39.,-28.13000002,-97.8896208912436));
#145742=CARTESIAN_POINT('Origin',(-39.5,-28.13000002,-97.8896208912436));
#145743=CARTESIAN_POINT('',(-39.,-28.13000002,-129.34995));
#145744=CARTESIAN_POINT('Ctrl Pts',(-40.2462900890831,-28.63000002,-94.8183794182931));
#145745=CARTESIAN_POINT('Ctrl Pts',(-39.6202740741427,-28.6300000199999,
-94.4888005385705));
#145746=CARTESIAN_POINT('Ctrl Pts',(-39.829240962964,-27.9630991838752,
-94.598792800159));
#145747=CARTESIAN_POINT('Ctrl Pts',(-39.9855126261077,-28.63000002,-95.3144293640507));
#145748=CARTESIAN_POINT('Ctrl Pts',(-39.3786468753042,-28.6300000200001,
-95.0400168527107));
#145749=CARTESIAN_POINT('Ctrl Pts',(-39.5394940969938,-27.9910419130939,
-95.1287084620502));
#145750=CARTESIAN_POINT('Ctrl Pts',(-39.7974846477126,-28.63000002,-95.8327740427122));
#145751=CARTESIAN_POINT('Ctrl Pts',(-39.2039361117733,-28.63000002,-95.6237032606678));
#145752=CARTESIAN_POINT('Ctrl Pts',(-39.3305596959349,-28.0197890414477,
-95.6832525232954));
#145753=CARTESIAN_POINT('Ctrl Pts',(-39.5490809018585,-28.63000002,-96.907936854151));
#145754=CARTESIAN_POINT('Ctrl Pts',(-39.0023017017761,-28.63000002,-96.8105692004775));
#145755=CARTESIAN_POINT('Ctrl Pts',(-39.054543707667,-28.078192313553,-96.8353311856082));
#145756=CARTESIAN_POINT('Ctrl Pts',(-39.4899744060911,-28.63000002,-97.4691620834926));
#145757=CARTESIAN_POINT('Ctrl Pts',(-38.9664569591492,-28.630000020001,
-97.4208997464886));
#145758=CARTESIAN_POINT('Ctrl Pts',(-38.9888645974602,-28.1080699462563,
-97.4376221179531));
#145759=CARTESIAN_POINT('Ctrl Pts',(-39.501388445999,-28.63000002,-98.0251051604236));
#145760=CARTESIAN_POINT('Ctrl Pts',(-39.0084033239769,-28.6300000199997,
-98.0351337801891));
#145761=CARTESIAN_POINT('Ctrl Pts',(-39.0015413990503,-28.1369597759577,
-98.0352430155923));
#145762=CARTESIAN_POINT('Ctrl Pts',(-39.760237187334,-27.9700232996177,
-94.7283182916262));
#145763=CARTESIAN_POINT('Ctrl Pts',(-39.7044170752792,-27.9756864894409,
-94.8360299998448));
#145764=CARTESIAN_POINT('Ctrl Pts',(-39.6518994857077,-27.9814177835746,
-94.9447812612047));
#145765=CARTESIAN_POINT('Ctrl Pts',(-39.6025567448821,-27.9871721516943,
-95.0544919306715));
#145766=CARTESIAN_POINT('Ctrl Pts',(-39.5517891646793,-27.9930926850929,
-95.167370646326));
#145767=CARTESIAN_POINT('Ctrl Pts',(-39.5043816087621,-27.9990379606581,
-95.2812653110876));
#145768=CARTESIAN_POINT('Ctrl Pts',(-39.4602180947879,-28.0049899521968,
-95.3961280885268));
#145769=CARTESIAN_POINT('Ctrl Pts',(-39.4155272969176,-28.0110130066788,
-95.5123622535062));
#145770=CARTESIAN_POINT('Ctrl Pts',(-39.3741578024,-28.0170434313907,-95.6295883656512));
#145771=CARTESIAN_POINT('Ctrl Pts',(-39.3360241014405,-28.0230875256045,
-95.7477895402997));
#145772=CARTESIAN_POINT('Ctrl Pts',(-39.2974753811385,-28.0291973993243,
-95.8672771301809));
#145773=CARTESIAN_POINT('Ctrl Pts',(-39.2622327498326,-28.0353218042364,
-95.9877618235928));
#145774=CARTESIAN_POINT('Ctrl Pts',(-39.2302521220656,-28.041484578967,
-96.1092496303843));
#145775=CARTESIAN_POINT('Ctrl Pts',(-39.2171315325446,-28.044012960778,
-96.1590920429952));
#145776=CARTESIAN_POINT('Ctrl Pts',(-39.2045605552519,-28.0465479531573,
-96.2091035093114));
#145777=CARTESIAN_POINT('Ctrl Pts',(-39.1925385381225,-28.0490916877327,
-96.2592851281618));
#145778=CARTESIAN_POINT('Ctrl Pts',(-39.1566966697309,-28.0566754566536,
-96.4088942128223));
#145779=CARTESIAN_POINT('Ctrl Pts',(-39.1256874125126,-28.0643165321069,
-96.5602560280547));
#145780=CARTESIAN_POINT('Ctrl Pts',(-39.0996770774813,-28.0719711520587,
-96.7128532814895));
#145781=CARTESIAN_POINT('Ctrl Pts',(-39.0738134555235,-28.0795825956031,
-96.8645897996801));
#145782=CARTESIAN_POINT('Ctrl Pts',(-39.052892611788,-28.0872070957307,
-97.0175476213926));
#145783=CARTESIAN_POINT('Ctrl Pts',(-39.0370318360345,-28.0948111078542,
-97.1711980730793));
#145784=CARTESIAN_POINT('Ctrl Pts',(-39.0213056660934,-28.1023505869281,
-97.3235445378627));
#145785=CARTESIAN_POINT('Ctrl Pts',(-39.010554075202,-28.1098696306334,
-97.4765716712978));
#145786=CARTESIAN_POINT('Ctrl Pts',(-39.004844939737,-28.1173495596137,
-97.6297480128119));
#145787=CARTESIAN_POINT('Ctrl Pts',(-39.0016168605909,-28.1215788869617,
-97.7163575102999));
#145788=CARTESIAN_POINT('Ctrl Pts',(-39.0000000254363,-28.1257959890489,
-97.803014437355));
#145789=CARTESIAN_POINT('Ctrl Pts',(-39.0000000000003,-28.13000002,-97.8896208912436));
#145790=CARTESIAN_POINT('Ctrl Pts',(-39.,-29.6093496431988,-96.8114293882212));
#145791=CARTESIAN_POINT('Ctrl Pts',(-39.,-28.741729147553,-95.6677964063875));
#145792=CARTESIAN_POINT('Ctrl Pts',(-39.7614971661825,-28.0062467616585,
-94.6983380795177));
#145793=CARTESIAN_POINT('Ctrl Pts',(-39.,-29.0535677480794,-97.2330749436175));
#145794=CARTESIAN_POINT('Ctrl Pts',(-39.,-28.2134674407351,-96.0912283932403));
#145795=CARTESIAN_POINT('Ctrl Pts',(-39.7437819827477,-27.4973039569491,
-95.1199826758911));
#145796=CARTESIAN_POINT('Ctrl Pts',(-39.,-28.4877143439141,-97.6439384126816));
#145797=CARTESIAN_POINT('Ctrl Pts',(-39.,-27.6753857963049,-96.504280291422));
#145798=CARTESIAN_POINT('Ctrl Pts',(-39.7262969548998,-26.9800167700376,
-95.5308471039398));
#145799=CARTESIAN_POINT('Ctrl Pts',(-39.,-27.3325353334211,-98.4405542704251));
#145800=CARTESIAN_POINT('Ctrl Pts',(-39.,-26.5774575077333,-97.3050952674327));
#145801=CARTESIAN_POINT('Ctrl Pts',(-39.6919956601185,-25.9258412309992,
-96.3274629617598));
#145802=CARTESIAN_POINT('Ctrl Pts',(-39.,-26.741479037393,-98.8273374953048));
#145803=CARTESIAN_POINT('Ctrl Pts',(-39.,-26.0159584590169,-97.6939770973016));
#145804=CARTESIAN_POINT('Ctrl Pts',(-39.6751334260609,-25.3873798477126,
-96.7142461865699));
#145805=CARTESIAN_POINT('Ctrl Pts',(-39.,-24.9430461321624,-99.9336024831245));
#145806=CARTESIAN_POINT('Ctrl Pts',(-39.,-24.3098005849941,-98.8051808316371));
#145807=CARTESIAN_POINT('Ctrl Pts',(-39.6263764589698,-23.7517847228855,
-97.8205111744839));
#145808=CARTESIAN_POINT('Ctrl Pts',(-39.,-23.7104174150638,-100.600117065969));
#145809=CARTESIAN_POINT('Ctrl Pts',(-38.9999999999805,-23.1402109105079,
-99.4757726121153));
#145810=CARTESIAN_POINT('Ctrl Pts',(-39.5962627317006,-22.634454054442,
-98.4870223585708));
#145811=CARTESIAN_POINT('Ctrl Pts',(-39.,-22.4346346021703,-101.175614049055));
#145812=CARTESIAN_POINT('Ctrl Pts',(-39.,-21.9292338920902,-100.055223222194));
#145813=CARTESIAN_POINT('Ctrl Pts',(-39.5698473334291,-21.4814334314007,
-99.0625227403511));
#145814=CARTESIAN_POINT('',(-39.,-22.48000002,-101.155103165204));
#145815=CARTESIAN_POINT('Ctrl Pts',(-39.,-22.48000002,-101.155103165204));
#145816=CARTESIAN_POINT('Ctrl Pts',(-39.0000000000003,-23.0421399014201,
-100.900364693921));
#145817=CARTESIAN_POINT('Ctrl Pts',(-39.0000000001808,-23.5949958654236,
-100.62835315127));
#145818=CARTESIAN_POINT('Ctrl Pts',(-39.0000000005377,-24.1395638864485,
-100.340934396651));
#145819=CARTESIAN_POINT('Ctrl Pts',(-39.0000000008113,-24.556943999504,
-100.120644427968));
#145820=CARTESIAN_POINT('Ctrl Pts',(-39.0000000009101,-24.9694552602955,
-99.8913025435703));
#145821=CARTESIAN_POINT('Ctrl Pts',(-39.0000000004916,-25.3775420853185,
-99.6537285981461));
#145822=CARTESIAN_POINT('Ctrl Pts',(-39.0000000002285,-25.6341396980635,
-99.5043463992897));
#145823=CARTESIAN_POINT('Ctrl Pts',(-39.0000000001306,-25.8888446969123,
-99.35177201821));
#145824=CARTESIAN_POINT('Ctrl Pts',(-39.0000000000752,-26.1419870362595,
-99.1960691366333));
#145825=CARTESIAN_POINT('Ctrl Pts',(-39.0000000000073,-26.4522179455434,
-99.005252196827));
#145826=CARTESIAN_POINT('Ctrl Pts',(-39.0000000000056,-26.7601021070991,
-98.8096624723068));
#145827=CARTESIAN_POINT('Ctrl Pts',(-39.0000000000023,-27.0653588164938,
-98.6099244013003));
#145828=CARTESIAN_POINT('Ctrl Pts',(-38.9999999999992,-27.3493059604975,
-98.424129779706));
#145829=CARTESIAN_POINT('Ctrl Pts',(-39.0000000000001,-27.6309803020601,
-98.2347441815219));
#145830=CARTESIAN_POINT('Ctrl Pts',(-39.0000000000002,-27.9101240577928,
-98.0422452092007));
#145831=CARTESIAN_POINT('Ctrl Pts',(-39.0000000000002,-27.9835605023139,
-97.9916030586567));
#145832=CARTESIAN_POINT('Ctrl Pts',(-39.0000000000002,-28.0568495646841,
-97.9407287002963));
#145833=CARTESIAN_POINT('Ctrl Pts',(-39.0000000000003,-28.13000002,-97.8896208912436));
#145834=CARTESIAN_POINT('Ctrl Pts',(-39.,-22.48000002,-101.155103165204));
#145835=CARTESIAN_POINT('Ctrl Pts',(-39.0000000057918,-22.4754395071655,
-101.035865090646));
#145836=CARTESIAN_POINT('Ctrl Pts',(-39.0036588655062,-22.4708531165579,
-100.917240445859));
#145837=CARTESIAN_POINT('Ctrl Pts',(-39.0108683903437,-22.4662513204906,
-100.799247589009));
#145838=CARTESIAN_POINT('Ctrl Pts',(-39.0181431578016,-22.4616078804535,
-100.680186955385));
#145839=CARTESIAN_POINT('Ctrl Pts',(-39.029032762941,-22.4569483804398,
-100.561768681035));
#145840=CARTESIAN_POINT('Ctrl Pts',(-39.0434732513881,-22.4522736097561,
-100.443988180248));
#145841=CARTESIAN_POINT('Ctrl Pts',(-39.0580014482079,-22.4475704455364,
-100.325492306425));
#145842=CARTESIAN_POINT('Ctrl Pts',(-39.076123635818,-22.4428513856762,
-100.2076409891));
#145843=CARTESIAN_POINT('Ctrl Pts',(-39.0978263127888,-22.4381133533492,
-100.09042036964));
#145844=CARTESIAN_POINT('Ctrl Pts',(-39.1130274182268,-22.4347947153274,
-100.008316074474));
#145845=CARTESIAN_POINT('Ctrl Pts',(-39.1299862043444,-22.4314666759937,
-99.9265209885234));
#145846=CARTESIAN_POINT('Ctrl Pts',(-39.1487132156732,-22.4281288757921,
-99.8450316540307));
#145847=CARTESIAN_POINT('Ctrl Pts',(-39.1782377095244,-22.4228665912877,
-99.7165577981164));
#145848=CARTESIAN_POINT('Ctrl Pts',(-39.2122145373374,-22.4175906493126,
-99.5886109020029));
#145849=CARTESIAN_POINT('Ctrl Pts',(-39.2506379380908,-22.41229684322,-99.4616289686943));
#145850=CARTESIAN_POINT('Ctrl Pts',(-39.2887401124853,-22.4070472942733,
-99.3357086265846));
#145851=CARTESIAN_POINT('Ctrl Pts',(-39.3312150950707,-22.4017804193251,
-99.2107375266136));
#145852=CARTESIAN_POINT('Ctrl Pts',(-39.3780123572035,-22.3965150583138,
-99.0871503677225));
#145853=CARTESIAN_POINT('Ctrl Pts',(-39.4243143618565,-22.3913054208491,
-98.96487113716));
#145854=CARTESIAN_POINT('Ctrl Pts',(-39.474847826133,-22.3860975663706,
-98.8439471061793));
#145855=CARTESIAN_POINT('Ctrl Pts',(-39.529516301983,-22.3809282592383,
-98.7248012575205));
#145856=CARTESIAN_POINT('Ctrl Pts',(-39.5495316353077,-22.3790356620202,
-98.6811793376099));
#145857=CARTESIAN_POINT('Ctrl Pts',(-39.5701007714082,-22.3771483895887,
-98.6377957636978));
#145858=CARTESIAN_POINT('Ctrl Pts',(-39.5912172963669,-22.3752687460488,
-98.5946711914791));
#145859=CARTESIAN_POINT('Ctrl Pts',(-57.5245249214072,-22.4066238608121,
-60.8508735991008));
#145860=CARTESIAN_POINT('Ctrl Pts',(-57.5817506954796,-21.98000002,-60.8779152752782));
#145861=CARTESIAN_POINT('Ctrl Pts',(-57.9716987024741,-21.98000002,-61.0621827299711));
#145862=CARTESIAN_POINT('Ctrl Pts',(-51.5741970743562,-22.3992883743679,
-73.4455439799432));
#145863=CARTESIAN_POINT('Ctrl Pts',(-51.6744341991619,-21.980000020072,
-73.3940563428121));
#145864=CARTESIAN_POINT('Ctrl Pts',(-52.0201596782203,-21.98000002,-73.6568689967289));
#145865=CARTESIAN_POINT('Ctrl Pts',(-45.6084483216386,-22.3901517945239,
-86.0327992211263));
#145866=CARTESIAN_POINT('Ctrl Pts',(-45.7509404552383,-21.98000002,-85.9093076925101));
#145867=CARTESIAN_POINT('Ctrl Pts',(-46.0528581107812,-21.98000002,-86.2441334050211));
#145868=CARTESIAN_POINT('Ctrl Pts',(-39.5912209089315,-22.3752378108182,
-98.5946087902654));
#145869=CARTESIAN_POINT('Ctrl Pts',(-39.6675936435968,-21.98000002,-98.6312136095384));
#145870=CARTESIAN_POINT('Ctrl Pts',(-40.032098818038,-21.98000002,-98.8059179211357));
#145871=CARTESIAN_POINT('Origin',(-40.032098818038,-22.4800000199998,-98.8059179211357));
#145872=CARTESIAN_POINT('Ctrl Pts',(-39.5000802079448,-21.98000002,-101.18483134797));
#145873=CARTESIAN_POINT('Ctrl Pts',(-38.9988245498377,-21.98000002,-101.187579451807));
#145874=CARTESIAN_POINT('Ctrl Pts',(-39.0000891720766,-22.4812615520007,
-101.187572533131));
#145875=CARTESIAN_POINT('Ctrl Pts',(-39.4978248085922,-21.98000002,-100.766749896626));
#145876=CARTESIAN_POINT('Ctrl Pts',(-39.0135806132542,-21.98000002,-100.738591066592));
#145877=CARTESIAN_POINT('Ctrl Pts',(-38.9975824433844,-22.4638259428356,
-100.730929118733));
#145878=CARTESIAN_POINT('Ctrl Pts',(-39.5431523621162,-21.98000002,-100.356681579714));
#145879=CARTESIAN_POINT('Ctrl Pts',(-39.0782818391802,-21.9800000199993,
-100.29429926997));
#145880=CARTESIAN_POINT('Ctrl Pts',(-39.047945770245,-22.4461087815554,
-100.283504254757));
#145881=CARTESIAN_POINT('Ctrl Pts',(-39.7245173679265,-21.98000002,-99.5521100005686));
#145882=CARTESIAN_POINT('Ctrl Pts',(-39.3065757091719,-21.9800000200007,
-99.4303875276426));
#145883=CARTESIAN_POINT('Ctrl Pts',(-39.2494612149797,-22.4101874992009,
-99.4065735026009));
#145884=CARTESIAN_POINT('Ctrl Pts',(-39.862287275171,-21.98000002,-99.1549631973435));
#145885=CARTESIAN_POINT('Ctrl Pts',(-39.4691358483957,-21.9800000199999,
-99.0065780221483));
#145886=CARTESIAN_POINT('Ctrl Pts',(-39.402539249954,-22.3918503540147,
-98.9741976287182));
#145887=CARTESIAN_POINT('Ctrl Pts',(-40.0449984320234,-21.98000002,-98.7791972647193));
#145888=CARTESIAN_POINT('Ctrl Pts',(-39.6824251849823,-21.9800000199999,
-98.6029227401544));
#145889=CARTESIAN_POINT('Ctrl Pts',(-39.6055502466993,-22.3739864322111,
-98.5655472422949));
#145890=CARTESIAN_POINT('Origin',(-39.5,-22.48000002,-101.155103165204));
#145891=CARTESIAN_POINT('Origin',(-39.5,-22.48000002,-55.24995));
#145892=CARTESIAN_POINT('',(-39.,-22.48000002,-130.903539806302));
#145893=CARTESIAN_POINT('Origin',(-39.5,-22.48000002,-130.903539806302));
#145894=CARTESIAN_POINT('',(-39.,-22.48000002,-129.34995));
#145895=CARTESIAN_POINT('Ctrl Pts',(-40.0320988180411,-21.98000002,-133.252725050377));
#145896=CARTESIAN_POINT('Ctrl Pts',(-39.6675936435998,-21.98000002,-133.427429361974));
#145897=CARTESIAN_POINT('Ctrl Pts',(-39.5912209089345,-22.3752378108182,
-133.464034181247));
#145898=CARTESIAN_POINT('Ctrl Pts',(-39.8558398148562,-21.98000002,-132.884976140755));
#145899=CARTESIAN_POINT('Ctrl Pts',(-39.4616506489997,-21.98000002,-133.032398833922));
#145900=CARTESIAN_POINT('Ctrl Pts',(-39.3953798878174,-22.3926947961315,
-133.064083894138));
#145901=CARTESIAN_POINT('Ctrl Pts',(-39.7245793327553,-21.98000002,-132.504273278823));
#145902=CARTESIAN_POINT('Ctrl Pts',(-39.306634221246,-21.98000002,-132.626108677501));
#145903=CARTESIAN_POINT('Ctrl Pts',(-39.2495325922488,-22.4102623065174,
-132.649599803771));
#145904=CARTESIAN_POINT('Ctrl Pts',(-39.5464016190797,-21.98000002,-131.71886357396));
#145905=CARTESIAN_POINT('Ctrl Pts',(-39.0825794362701,-21.9800000199999,
-131.782866385322));
#145906=CARTESIAN_POINT('Ctrl Pts',(-39.0515573542344,-22.4453411404847,
-131.793566113248));
#145907=CARTESIAN_POINT('Ctrl Pts',(-39.5000000005303,-21.98000002,-131.311180490184));
#145908=CARTESIAN_POINT('Ctrl Pts',(-39.0167438766121,-21.98000002,-131.341321155374));
#145909=CARTESIAN_POINT('Ctrl Pts',(-39.,-22.4629715740863,-131.348761468896));
#145910=CARTESIAN_POINT('Ctrl Pts',(-39.5,-21.98000002,-130.903539806302));
#145911=CARTESIAN_POINT('Ctrl Pts',(-39.,-21.98000002,-130.903539806302));
#145912=CARTESIAN_POINT('Ctrl Pts',(-39.,-22.48000002,-130.903539806302));
#145913=CARTESIAN_POINT('',(-39.5912209088598,-22.3752378112049,-133.464034181283));
#145914=CARTESIAN_POINT('Origin',(-40.0320988180411,-22.48000002,-133.252725050377));
#145915=CARTESIAN_POINT('Ctrl Pts',(-39.5912209089345,-22.3752378108182,
-133.464034181247));
#145916=CARTESIAN_POINT('Ctrl Pts',(-39.3953798878174,-22.3926947961315,
-133.064083894138));
#145917=CARTESIAN_POINT('Ctrl Pts',(-39.2495325922488,-22.4102623065174,
-132.649599803771));
#145918=CARTESIAN_POINT('Ctrl Pts',(-39.0515573542344,-22.4453411404847,
-131.793566113248));
#145919=CARTESIAN_POINT('Ctrl Pts',(-39.,-22.4629715740863,-131.348761468896));
#145920=CARTESIAN_POINT('Ctrl Pts',(-39.,-22.48000002,-130.903539806302));
#145921=CARTESIAN_POINT('Ctrl Pts',(-39.5912209089345,-22.3752378108182,
-133.464034181247));
#145922=CARTESIAN_POINT('Ctrl Pts',(-39.6675936435998,-21.98000002,-133.427429361974));
#145923=CARTESIAN_POINT('Ctrl Pts',(-40.0320988180411,-21.98000002,-133.252725050377));
#145924=CARTESIAN_POINT('Ctrl Pts',(-45.6468692907591,-22.3902470227078,
-146.106052933848));
#145925=CARTESIAN_POINT('Ctrl Pts',(-45.790260298639,-21.98000002,-146.231563592216));
#145926=CARTESIAN_POINT('Ctrl Pts',(-46.0913014593244,-21.98000002,-145.894718230889));
#145927=CARTESIAN_POINT('Ctrl Pts',(-51.6504270099243,-22.3994099070849,
-158.773819030963));
#145928=CARTESIAN_POINT('Ctrl Pts',(-51.7509431131532,-21.9800000203624,
-158.826102375503));
#145929=CARTESIAN_POINT('Ctrl Pts',(-52.0964117641256,-21.98000002,-158.56249372189));
#145930=CARTESIAN_POINT('Ctrl Pts',(-57.638503474757,-22.4067641070473,
-171.449026400902));
#145931=CARTESIAN_POINT('Ctrl Pts',(-57.6956367824858,-21.98000002,-171.422029807066));
#145932=CARTESIAN_POINT('Ctrl Pts',(-58.085700246061,-21.98000002,-171.237717270032));
#145933=CARTESIAN_POINT('',(-57.638503474757,-22.4067641070473,-171.449026400902));
#145934=CARTESIAN_POINT('Origin',(-58.085700246061,-22.48000002,-171.237717270032));
#145935=CARTESIAN_POINT('Ctrl Pts',(-57.638503474757,-22.4067641070473,
-171.449026400902));
#145936=CARTESIAN_POINT('Ctrl Pts',(-51.650427014377,-22.3994098885056,
-158.773819033279));
#145937=CARTESIAN_POINT('Ctrl Pts',(-45.6468692971616,-22.39024700439,-146.106052939452));
#145938=CARTESIAN_POINT('Ctrl Pts',(-39.5912209089345,-22.3752378108181,
-133.464034181247));
#145939=CARTESIAN_POINT('Ctrl Pts',(-57.6186574596683,-22.4082912353334,
-171.40978315061));
#145940=CARTESIAN_POINT('Ctrl Pts',(-57.6735493970763,-21.9798882430102,
-171.380807602766));
#145941=CARTESIAN_POINT('Ctrl Pts',(-58.0564197191617,-21.9800000366742,
-171.178790026127));
#145942=CARTESIAN_POINT('Ctrl Pts',(-57.7016369198821,-22.4019038408433,
-171.565352937794));
#145943=CARTESIAN_POINT('Ctrl Pts',(-57.7654281245283,-21.9798905214978,
-171.542966774725));
#145944=CARTESIAN_POINT('Ctrl Pts',(-58.1793335836445,-21.9800000364255,
-171.412176181737));
#145945=CARTESIAN_POINT('Ctrl Pts',(-57.7416081447113,-22.3988541543228,
-171.738094620076));
#145946=CARTESIAN_POINT('Ctrl Pts',(-57.811087281066,-21.9798915951361,
-171.728859197825));
#145947=CARTESIAN_POINT('Ctrl Pts',(-58.2385448347245,-21.9800000363068,
-171.671295447806));
#145948=CARTESIAN_POINT('Ctrl Pts',(-57.7336548687769,-22.399461430235,
-171.916008414622));
#145949=CARTESIAN_POINT('Ctrl Pts',(-57.8020514502591,-21.9798913838386,
-171.91910344938));
#145950=CARTESIAN_POINT('Ctrl Pts',(-58.2267633341816,-21.9800000363304,
-171.938197690258));
#145951=CARTESIAN_POINT('Origin',(-58.2281061322669,-22.48000002,-171.871644662643));
#145952=CARTESIAN_POINT('Origin',(-56.6903638456505,-22.4806382361538,-171.875913019551));
#145953=CARTESIAN_POINT('Origin',(-58.2281061322669,-22.48000002,-179.64995));
#145954=CARTESIAN_POINT('Origin',(-58.2281061322669,-22.48000002,-176.657965001855));
#145955=CARTESIAN_POINT('Ctrl Pts',(-60.,-21.48000002,-174.47822483969));
#145956=CARTESIAN_POINT('Ctrl Pts',(-60.,-21.98000002,-174.47822483969));
#145957=CARTESIAN_POINT('Ctrl Pts',(-59.5,-21.98000002,-174.47822483969));
#145958=CARTESIAN_POINT('Ctrl Pts',(-60.,-21.4822140856788,-174.77632287275));
#145959=CARTESIAN_POINT('Ctrl Pts',(-59.9977907999382,-21.9800000199965,
-174.775666642734));
#145960=CARTESIAN_POINT('Ctrl Pts',(-59.4999999932692,-21.98000002,-174.72672222605));
#145961=CARTESIAN_POINT('Ctrl Pts',(-59.9565698697824,-21.4843793273514,
-175.067148740399));
#145962=CARTESIAN_POINT('Ctrl Pts',(-59.9524075929633,-21.98000002,-175.065899995449));
#145963=CARTESIAN_POINT('Ctrl Pts',(-59.4638082272143,-21.98000002,-174.969157756816));
#145964=CARTESIAN_POINT('Ctrl Pts',(-59.8274910918555,-21.4875521339025,
-175.492414399022));
#145965=CARTESIAN_POINT('Ctrl Pts',(-59.8205081565721,-21.98000002,-175.489804158754));
#145966=CARTESIAN_POINT('Ctrl Pts',(-59.3562425753485,-21.98000002,-175.323664095203));
#145967=CARTESIAN_POINT('Ctrl Pts',(-59.7735239255666,-21.4885940652802,
-175.631914079949));
#145968=CARTESIAN_POINT('Ctrl Pts',(-59.7657533403762,-21.9800000200007,
-175.628582862653));
#145969=CARTESIAN_POINT('Ctrl Pts',(-59.3112699374162,-21.98000002,-175.439952697294));
#145970=CARTESIAN_POINT('Ctrl Pts',(-59.6473451018805,-21.4905837846614,
-175.89805223939));
#145971=CARTESIAN_POINT('Ctrl Pts',(-59.6382394618755,-21.9800000199994,
-175.893067776338));
#145972=CARTESIAN_POINT('Ctrl Pts',(-59.2061209187896,-21.98000002,-175.661808757878));
#145973=CARTESIAN_POINT('Ctrl Pts',(-59.5748118056443,-21.4915405113197,
-176.025889197601));
#145974=CARTESIAN_POINT('Ctrl Pts',(-59.5651790529315,-21.9800000199994,
-176.020005430174));
#145975=CARTESIAN_POINT('Ctrl Pts',(-59.1456765053938,-21.98000002,-175.768375282423));
#145976=CARTESIAN_POINT('Ctrl Pts',(-59.4107666107714,-21.493376849955,
-176.271048580335));
#145977=CARTESIAN_POINT('Ctrl Pts',(-59.4003458450454,-21.9800000200006,
-176.263201660659));
#145978=CARTESIAN_POINT('Ctrl Pts',(-59.0089721749525,-21.98000002,-175.972743369523));
#145979=CARTESIAN_POINT('Ctrl Pts',(-59.3183914660909,-21.4942625520954,
-176.389181693558));
#145980=CARTESIAN_POINT('Ctrl Pts',(-59.3077278616495,-21.9800000199987,
-176.380304393309));
#145981=CARTESIAN_POINT('Ctrl Pts',(-58.9319928876421,-21.98000002,-176.071220734744));
#145982=CARTESIAN_POINT('Ctrl Pts',(-59.1195126442718,-21.495903657329,
-176.607905725284));
#145983=CARTESIAN_POINT('Ctrl Pts',(-59.1086757415209,-21.9800000200013,
-176.59692321781));
#145984=CARTESIAN_POINT('Ctrl Pts',(-58.7662605376602,-21.98000002,-176.253552125047));
#145985=CARTESIAN_POINT('Ctrl Pts',(-59.012812502338,-21.4966636432885,
-176.7091099968));
#145986=CARTESIAN_POINT('Ctrl Pts',(-59.0020443621077,-21.9800000199996,
-176.697095400112));
#145987=CARTESIAN_POINT('Ctrl Pts',(-58.6773437522104,-21.98000002,-176.337917446619));
#145988=CARTESIAN_POINT('Ctrl Pts',(-58.6712299408253,-21.4987636190772,
-176.988586760981));
#145989=CARTESIAN_POINT('Ctrl Pts',(-58.6613611188049,-21.9800000200008,
-176.973308002926));
#145990=CARTESIAN_POINT('Ctrl Pts',(-58.3926916168304,-21.98000002,-176.570893328242));
#145991=CARTESIAN_POINT('Ctrl Pts',(-58.4110432062101,-21.4999301516852,
-177.143590179504));
#145992=CARTESIAN_POINT('Ctrl Pts',(-58.4021689190209,-21.9800000199881,
-177.126531916838));
#145993=CARTESIAN_POINT('Ctrl Pts',(-58.1758692424685,-21.98000002,-176.700106570217));
#145994=CARTESIAN_POINT('Ctrl Pts',(-58.140200132617,-21.5007687140674,
-177.254954590203));
#145995=CARTESIAN_POINT('Ctrl Pts',(-58.132621442372,-21.98000002,-177.23652912386));
#145996=CARTESIAN_POINT('Ctrl Pts',(-57.9501667771809,-21.98000002,-176.792941619423));
#145997=CARTESIAN_POINT('',(-60.,-21.48000002,-174.47822483969));
#145998=CARTESIAN_POINT('Origin',(-59.5,-21.48000002,-174.47822483969));
#145999=CARTESIAN_POINT('',(-58.1799818946227,-21.5006430239517,-177.238261718428));
#146000=CARTESIAN_POINT('Ctrl Pts',(-60.,-21.48000002,-174.47822483969));
#146001=CARTESIAN_POINT('Ctrl Pts',(-60.,-21.4822140856788,-174.77632287275));
#146002=CARTESIAN_POINT('Ctrl Pts',(-59.9565698697824,-21.4843793273514,
-175.067148740399));
#146003=CARTESIAN_POINT('Ctrl Pts',(-59.8274910918555,-21.4875521339025,
-175.492414399022));
#146004=CARTESIAN_POINT('Ctrl Pts',(-59.7735239255666,-21.4885940652802,
-175.631914079949));
#146005=CARTESIAN_POINT('Ctrl Pts',(-59.6473451018805,-21.4905837846614,
-175.89805223939));
#146006=CARTESIAN_POINT('Ctrl Pts',(-59.5748118056443,-21.4915405113197,
-176.025889197601));
#146007=CARTESIAN_POINT('Ctrl Pts',(-59.4107666107714,-21.493376849955,
-176.271048580335));
#146008=CARTESIAN_POINT('Ctrl Pts',(-59.3183914660909,-21.4942625520954,
-176.389181693558));
#146009=CARTESIAN_POINT('Ctrl Pts',(-59.1195126442718,-21.495903657329,
-176.607905725284));
#146010=CARTESIAN_POINT('Ctrl Pts',(-59.012812502338,-21.4966636432885,
-176.7091099968));
#146011=CARTESIAN_POINT('Ctrl Pts',(-58.6824004740714,-21.4986949450522,
-176.979447229759));
#146012=CARTESIAN_POINT('Ctrl Pts',(-58.4364911965918,-21.4998151450696,
-177.128307927537));
#146013=CARTESIAN_POINT('Ctrl Pts',(-58.1799818947148,-21.5006430233981,
-177.238261718413));
#146014=CARTESIAN_POINT('Ctrl Pts',(-58.2281061322669,-21.98000002,-176.657965001855));
#146015=CARTESIAN_POINT('Ctrl Pts',(-58.1997838724148,-21.98000002,-176.740111438881));
#146016=CARTESIAN_POINT('Ctrl Pts',(-58.1775901524469,-21.9698497118448,
-176.818815489061));
#146017=CARTESIAN_POINT('Ctrl Pts',(-58.1467121091855,-21.9264637442851,
-176.962169933093));
#146018=CARTESIAN_POINT('Ctrl Pts',(-58.1379476084663,-21.8930112710375,
-177.027055273752));
#146019=CARTESIAN_POINT('Ctrl Pts',(-58.1325374345936,-21.8059684297317,
-177.133613057603));
#146020=CARTESIAN_POINT('Ctrl Pts',(-58.135834617463,-21.751763745641,-177.175847704912));
#146021=CARTESIAN_POINT('Ctrl Pts',(-58.1516959167317,-21.6321056009482,
-177.229926261063));
#146022=CARTESIAN_POINT('Ctrl Pts',(-58.1643305096628,-21.5659716479372,
-177.242027715059));
#146023=CARTESIAN_POINT('Ctrl Pts',(-58.1799818947148,-21.5006430233981,
-177.238261718413));
#146024=CARTESIAN_POINT('Origin',(-59.5,-21.48000002,-55.24995));
#146025=CARTESIAN_POINT('',(-60.,-21.48000002,-174.45635375974));
#146026=CARTESIAN_POINT('Origin',(-60.,-2.55003103885676E-14,0.));
#146027=CARTESIAN_POINT('',(-60.,-20.98000002,-174.500886972636));
#146028=CARTESIAN_POINT('',(-60.,-20.98000002,-58.1134713856835));
#146029=CARTESIAN_POINT('Ctrl Pts',(-60.,-21.48000002,-174.47822483969));
#146030=CARTESIAN_POINT('Ctrl Pts',(-60.,-21.3133292808184,-174.485664661366));
#146031=CARTESIAN_POINT('Ctrl Pts',(-60.,-21.1466632268706,-174.493235890728));
#146032=CARTESIAN_POINT('Ctrl Pts',(-60.,-20.98000002,-174.500886972636));
#146033=CARTESIAN_POINT('Origin',(-59.5,-20.98000002,-55.24995));
#146034=CARTESIAN_POINT('Origin',(-59.5,-20.98000002,-174.500886972636));
#146035=CARTESIAN_POINT('Ctrl Pts',(-39.5365899624517,-19.9017174575869,
-99.7816873060563));
#146036=CARTESIAN_POINT('Ctrl Pts',(-39.4537365768202,-20.48000002,-99.742462415759));
#146037=CARTESIAN_POINT('Ctrl Pts',(-39.9829309662066,-20.48000002,-99.9929964369266));
#146038=CARTESIAN_POINT('Ctrl Pts',(-45.6728806075319,-19.9133770447829,
-86.815892326284));
#146039=CARTESIAN_POINT('Ctrl Pts',(-45.5211976544485,-20.48000002,-86.9586415917399));
#146040=CARTESIAN_POINT('Ctrl Pts',(-46.1212593572987,-20.48000002,-87.0272166609364));
#146041=CARTESIAN_POINT('Ctrl Pts',(-51.7792721521254,-19.9203329608279,
-73.8354504790526));
#146042=CARTESIAN_POINT('Ctrl Pts',(-51.6794916123544,-20.4800000199249,
-73.8897477208158));
#146043=CARTESIAN_POINT('Ctrl Pts',(-52.2285110086243,-20.48000002,-74.0467697366574));
#146044=CARTESIAN_POINT('Ctrl Pts',(-57.8770125754992,-19.9259080025173,
-60.8508735991007));
#146045=CARTESIAN_POINT('Ctrl Pts',(-57.8224346115608,-20.48000002,-60.8252402001721));
#146046=CARTESIAN_POINT('Ctrl Pts',(-58.3269264615434,-20.48000002,-61.0621827299711));
#146047=CARTESIAN_POINT('Origin',(-39.9829309662066,-19.98000002,-99.9929964369266));
#146048=CARTESIAN_POINT('Ctrl Pts',(-59.5,-20.48000002,-174.500886972636));
#146049=CARTESIAN_POINT('Ctrl Pts',(-60.,-20.48000002,-174.500886972636));
#146050=CARTESIAN_POINT('Ctrl Pts',(-60.,-20.98000002,-174.500886972636));
#146051=CARTESIAN_POINT('Ctrl Pts',(-59.4999999934397,-20.48000002,-174.74311983516));
#146052=CARTESIAN_POINT('Ctrl Pts',(-60.0022242907223,-20.48000002,-174.792108323791));
#146053=CARTESIAN_POINT('Ctrl Pts',(-60.,-20.9822194010082,-174.791464522024));
#146054=CARTESIAN_POINT('Ctrl Pts',(-59.4655777479701,-20.48000002,-174.979582459221));
#146055=CARTESIAN_POINT('Ctrl Pts',(-59.9629392387446,-20.4800000199999,
-175.076359449429));
#146056=CARTESIAN_POINT('Ctrl Pts',(-59.9586932949262,-20.9843889926879,
-175.075119998302));
#146057=CARTESIAN_POINT('Ctrl Pts',(-59.3634105452706,-20.48000002,-175.325604118318));
#146058=CARTESIAN_POINT('Ctrl Pts',(-59.8433264812564,-20.48000002,-175.492827860986));
#146059=CARTESIAN_POINT('Ctrl Pts',(-59.8360926556437,-20.9875676565265,
-175.49019987132));
#146060=CARTESIAN_POINT('Ctrl Pts',(-59.3205935345334,-20.48000002,-175.43951222267));
#146061=CARTESIAN_POINT('Ctrl Pts',(-59.7928073162253,-20.4800000200006,
-175.630213503224));
#146062=CARTESIAN_POINT('Ctrl Pts',(-59.7847122422101,-20.9886147234176,
-175.626841448369));
#146063=CARTESIAN_POINT('Ctrl Pts',(-59.2204432327122,-20.48000002,-175.657072445029));
#146064=CARTESIAN_POINT('Ctrl Pts',(-59.674123349008,-20.4800000199994,
-175.892915048025));
#146065=CARTESIAN_POINT('Ctrl Pts',(-59.6645318784846,-20.9906156905346,
-175.887821675912));
#146066=CARTESIAN_POINT('Ctrl Pts',(-59.162871562207,-20.48000002,-175.761697975082));
#146067=CARTESIAN_POINT('Ctrl Pts',(-59.605650654114,-20.4800000200002,
-176.019368430779));
#146068=CARTESIAN_POINT('Ctrl Pts',(-59.5954458739788,-20.9915785299556,
-176.013328010605));
#146069=CARTESIAN_POINT('Ctrl Pts',(-59.032749049719,-20.48000002,-175.962647558431));
#146070=CARTESIAN_POINT('Ctrl Pts',(-59.4504692034509,-20.4800000199998,
-176.262509186853));
#146071=CARTESIAN_POINT('Ctrl Pts',(-59.4392988603324,-20.9934287142977,
-176.254382360717));
#146072=CARTESIAN_POINT('Ctrl Pts',(-58.9595157418279,-20.48000002,-176.059697515632));
#146073=CARTESIAN_POINT('Ctrl Pts',(-59.3629214966957,-20.48000002,-176.380037040048));
#146074=CARTESIAN_POINT('Ctrl Pts',(-59.3514188912717,-20.9943227517297,
-176.370801152158));
#146075=CARTESIAN_POINT('Ctrl Pts',(-58.800974443077,-20.48000002,-176.240813845549));
#146076=CARTESIAN_POINT('Ctrl Pts',(-59.1730156260874,-20.48000002,-176.599598651605));
#146077=CARTESIAN_POINT('Ctrl Pts',(-59.1611693306144,-20.9959919273243,
-176.588063887092));
#146078=CARTESIAN_POINT('Ctrl Pts',(-58.7159164062094,-20.48000002,-176.324867284949));
#146079=CARTESIAN_POINT('Ctrl Pts',(-59.0709534896778,-20.4800000200012,
-176.701568343258));
#146080=CARTESIAN_POINT('Ctrl Pts',(-59.0590996873029,-20.9967669365736,
-176.688892319953));
#146081=CARTESIAN_POINT('Ctrl Pts',(-58.4437643988224,-20.48000002,-176.557945321316));
#146082=CARTESIAN_POINT('Ctrl Pts',(-58.7436561080181,-20.4800000199975,
-176.984811315106));
#146083=CARTESIAN_POINT('Ctrl Pts',(-58.7325172788836,-20.9989167502369,
-176.968486930424));
#146084=CARTESIAN_POINT('Ctrl Pts',(-58.2366741051621,-20.48000002,-176.68900326854));
#146085=CARTESIAN_POINT('Ctrl Pts',(-58.4942266187642,-20.4800000200099,
-177.144085084891));
#146086=CARTESIAN_POINT('Ctrl Pts',(-58.484009011739,-21.0001266369645,
-177.125700665905));
#146087=CARTESIAN_POINT('Ctrl Pts',(-58.0184329245781,-20.48000002,-176.786456163744));
#146088=CARTESIAN_POINT('Ctrl Pts',(-58.2310611931749,-20.4800000199999,
-177.262627176116));
#146089=CARTESIAN_POINT('Ctrl Pts',(-58.2221195094937,-21.0010265837306,
-177.24260269584));
#146090=CARTESIAN_POINT('',(-58.2408314794356,-21.0009616714991,-177.234172657581));
#146091=CARTESIAN_POINT('Ctrl Pts',(-58.2408316684982,-21.000961690655,
-177.234173073119));
#146092=CARTESIAN_POINT('Ctrl Pts',(-58.4958429921241,-21.0000687461186,
-177.118186472847));
#146093=CARTESIAN_POINT('Ctrl Pts',(-58.7377089067135,-20.998882511313,
-176.964042263202));
#146094=CARTESIAN_POINT('Ctrl Pts',(-59.0590996887611,-20.9967668730019,
-176.688892321512));
#146095=CARTESIAN_POINT('Ctrl Pts',(-59.1611693320729,-20.995991863797,
-176.588063888513));
#146096=CARTESIAN_POINT('Ctrl Pts',(-59.3514188926903,-20.9943226882988,
-176.370801153298));
#146097=CARTESIAN_POINT('Ctrl Pts',(-59.4392988617113,-20.9934286509189,
-176.25438236172));
#146098=CARTESIAN_POINT('Ctrl Pts',(-59.5954458752409,-20.9915784666852,
-176.013328011352));
#146099=CARTESIAN_POINT('Ctrl Pts',(-59.664531879672,-20.990615627321,-175.887821676543));
#146100=CARTESIAN_POINT('Ctrl Pts',(-59.7847122432143,-20.9886146603231,
-175.626841448787));
#146101=CARTESIAN_POINT('Ctrl Pts',(-59.836092656542,-20.9875675934948,
-175.490199871646));
#146102=CARTESIAN_POINT('Ctrl Pts',(-59.9586932954552,-20.984388929849,
-175.075119998456));
#146103=CARTESIAN_POINT('Ctrl Pts',(-60.0000000002777,-20.9822193383029,
-174.791464522104));
#146104=CARTESIAN_POINT('Ctrl Pts',(-60.,-20.98000002,-174.500886972636));
#146105=CARTESIAN_POINT('Ctrl Pts',(-58.2408309122627,-21.0009616140329,
-177.234171411));
#146106=CARTESIAN_POINT('Ctrl Pts',(-58.2451692158037,-20.9815789540505,
-177.233091079908));
#146107=CARTESIAN_POINT('Ctrl Pts',(-58.2497081333482,-20.962409235832,
-177.230657978534));
#146108=CARTESIAN_POINT('Ctrl Pts',(-58.2544730703504,-20.943543143678,
-177.226940751589));
#146109=CARTESIAN_POINT('Ctrl Pts',(-58.259312250581,-20.9243830959921,
-177.22316560595));
#146110=CARTESIAN_POINT('Ctrl Pts',(-58.2643851390725,-20.9055354515583,
-177.218067292576));
#146111=CARTESIAN_POINT('Ctrl Pts',(-58.269703032832,-20.8870439871654,
-177.211703850792));
#146112=CARTESIAN_POINT('Ctrl Pts',(-58.2751367003253,-20.8681499525119,
-177.205201873067));
#146113=CARTESIAN_POINT('Ctrl Pts',(-58.28082669489,-20.8496264838163,-177.197380013113));
#146114=CARTESIAN_POINT('Ctrl Pts',(-58.2867604599995,-20.8314829595576,
-177.18826855295));
#146115=CARTESIAN_POINT('Ctrl Pts',(-58.2918979870607,-20.8157740723432,
-177.180379738296));
#146116=CARTESIAN_POINT('Ctrl Pts',(-58.2972179599825,-20.8003487350648,
-177.171523735368));
#146117=CARTESIAN_POINT('Ctrl Pts',(-58.3026938424719,-20.7852040043215,
-177.161696010758));
#146118=CARTESIAN_POINT('Ctrl Pts',(-58.309742257017,-20.7657100979675,
-177.149046017406));
#146119=CARTESIAN_POINT('Ctrl Pts',(-58.3169594019401,-20.7470208494275,
-177.134987393464));
#146120=CARTESIAN_POINT('Ctrl Pts',(-58.3243946994305,-20.729187882357,
-177.119617493859));
#146121=CARTESIAN_POINT('Ctrl Pts',(-58.3320743703935,-20.710768805034,
-177.10374243683));
#146122=CARTESIAN_POINT('Ctrl Pts',(-58.3399872192437,-20.6932616945543,
-177.086468930266));
#146123=CARTESIAN_POINT('Ctrl Pts',(-58.3481588912673,-20.6766903075191,
-177.06786817926));
#146124=CARTESIAN_POINT('Ctrl Pts',(-58.3567372752991,-20.659294146548,
-177.048341650914));
#146125=CARTESIAN_POINT('Ctrl Pts',(-58.3656012090582,-20.6429273606653,
-177.027352254574));
#146126=CARTESIAN_POINT('Ctrl Pts',(-58.3747427271629,-20.6276079654216,
-177.004940996223));
#146127=CARTESIAN_POINT('Ctrl Pts',(-58.377271631966,-20.6233700159071,
-176.998741157395));
#146128=CARTESIAN_POINT('Ctrl Pts',(-58.3798215549078,-20.6192122591398,
-176.992432289584));
#146129=CARTESIAN_POINT('Ctrl Pts',(-58.3823918217751,-20.6151352360893,
-176.986014819637));
#146130=CARTESIAN_POINT('Ctrl Pts',(-58.3921799248114,-20.5996090966801,
-176.961575778744));
#146131=CARTESIAN_POINT('Ctrl Pts',(-58.402161806076,-20.5854344582556,
-176.935836605802));
#146132=CARTESIAN_POINT('Ctrl Pts',(-58.4123668786042,-20.5726356287647,
-176.908971720649));
#146133=CARTESIAN_POINT('Ctrl Pts',(-58.4230115467541,-20.5592854744898,
-176.880949598656));
#146134=CARTESIAN_POINT('Ctrl Pts',(-58.4338992850076,-20.5474313492243,
-176.851703114916));
#146135=CARTESIAN_POINT('Ctrl Pts',(-58.4450457241721,-20.5370573305028,
-176.821397121147));
#146136=CARTESIAN_POINT('Ctrl Pts',(-58.4570445066189,-20.5258900337632,
-176.788773695792));
#146137=CARTESIAN_POINT('Ctrl Pts',(-58.469343309893,-20.5164370754064,
-176.754922805974));
#146138=CARTESIAN_POINT('Ctrl Pts',(-58.4819374094809,-20.5086424875326,
-176.720006455305));
#146139=CARTESIAN_POINT('Ctrl Pts',(-58.4951021738506,-20.5004947107105,
-176.683507972345));
#146140=CARTESIAN_POINT('Ctrl Pts',(-58.5085896080475,-20.49415825095,-176.645845027844));
#146141=CARTESIAN_POINT('Ctrl Pts',(-58.5223669924781,-20.4895440418049,
-176.607156904439));
#146142=CARTESIAN_POINT('Ctrl Pts',(-58.5368459438342,-20.4846948695911,
-176.566498718578));
#146143=CARTESIAN_POINT('Ctrl Pts',(-58.5516451680495,-20.4817475506061,
-176.524707986652));
#146144=CARTESIAN_POINT('Ctrl Pts',(-58.5666969888986,-20.4805798588946,
-176.481901643726));
#146145=CARTESIAN_POINT('Ctrl Pts',(-58.5716977806305,-20.4801919069574,
-176.467679736096));
#146146=CARTESIAN_POINT('Ctrl Pts',(-58.5767262175753,-20.4800002580357,
-176.453345390789));
#146147=CARTESIAN_POINT('Ctrl Pts',(-58.5817791104913,-20.4800000202216,
-176.438901946458));
#146148=CARTESIAN_POINT('Origin',(-58.5817791104913,-19.98000002,-179.64995));
#146149=CARTESIAN_POINT('Origin',(-58.5817791104913,-19.98000002,-176.438901946458));
#146150=CARTESIAN_POINT('Origin',(-58.5817791104913,-19.98000002,-171.871644662643));
#146151=CARTESIAN_POINT('Ctrl Pts',(-58.0853233553177,-19.9205720538986,
-171.871644662643));
#146152=CARTESIAN_POINT('Ctrl Pts',(-58.0183573349639,-20.48000002,-171.871644662643));
#146153=CARTESIAN_POINT('Ctrl Pts',(-58.5817791104913,-20.48000002,-171.871644662643));
#146154=CARTESIAN_POINT('Ctrl Pts',(-58.0853233550829,-19.9205720558596,
-171.725723025901));
#146155=CARTESIAN_POINT('Ctrl Pts',(-58.018357325283,-20.48000002,-171.735617762033));
#146156=CARTESIAN_POINT('Ctrl Pts',(-58.5817790937258,-20.48000002,-171.652759539508));
#146157=CARTESIAN_POINT('Ctrl Pts',(-58.0534084851269,-19.9223906228206,
-171.582455328445));
#146158=CARTESIAN_POINT('Ctrl Pts',(-57.9913238325147,-20.4800000200031,
-171.602371122267));
#146159=CARTESIAN_POINT('Ctrl Pts',(-58.5342346140381,-20.48000002,-171.437864213701));
#146160=CARTESIAN_POINT('Ctrl Pts',(-57.9903087491627,-19.9260113903464,
-171.449026400902));
#146161=CARTESIAN_POINT('Ctrl Pts',(-57.9358462259716,-20.48000002,-171.474604875281));
#146162=CARTESIAN_POINT('Ctrl Pts',(-58.4402350532158,-20.48000002,-171.237717270032));
#146163=CARTESIAN_POINT('',(-57.9903087491627,-19.9260113903464,-171.449026400902));
#146164=CARTESIAN_POINT('Origin',(-58.4402350532158,-19.98000002,-171.237717270032));
#146165=CARTESIAN_POINT('Origin',(-56.628753050575,-20.0041469075947,-171.968943421328));
#146166=CARTESIAN_POINT('Ctrl Pts',(-57.9903087491627,-19.9260113903464,
-171.449026400902));
#146167=CARTESIAN_POINT('Ctrl Pts',(-57.9358462259716,-20.48000002,-171.474604875281));
#146168=CARTESIAN_POINT('Ctrl Pts',(-58.4402350532158,-20.48000002,-171.237717270032));
#146169=CARTESIAN_POINT('Ctrl Pts',(-51.8549375290089,-19.9204232153646,
-158.383965825354));
#146170=CARTESIAN_POINT('Ctrl Pts',(-51.754926284906,-20.4800000196472,
-158.328906441527));
#146171=CARTESIAN_POINT('Ctrl Pts',(-52.3041884424236,-20.48000002,-158.172646387016));
#146172=CARTESIAN_POINT('Ctrl Pts',(-45.7108852546953,-19.9134492574988,
-145.323053305542));
#146173=CARTESIAN_POINT('Ctrl Pts',(-45.5582765746385,-20.48000002,-145.178124710387));
#146174=CARTESIAN_POINT('Ctrl Pts',(-46.1592765266851,-20.48000002,-145.111728668187));
#146175=CARTESIAN_POINT('Ctrl Pts',(-39.5365899624517,-19.9017174575869,
-132.27695566545));
#146176=CARTESIAN_POINT('Ctrl Pts',(-39.4537365768201,-20.48000002,-132.316180555747));
#146177=CARTESIAN_POINT('Ctrl Pts',(-39.9829309662066,-20.48000002,-132.065646534579));
#146178=CARTESIAN_POINT('',(-39.5365899624061,-19.9017174579054,-132.276955665471));
#146179=CARTESIAN_POINT('Origin',(-39.9829309662066,-19.98000002,-132.065646534579));
#146180=CARTESIAN_POINT('Ctrl Pts',(-39.5365899624517,-19.9017174575869,
-132.27695566545));
#146181=CARTESIAN_POINT('Ctrl Pts',(-45.7108852544235,-19.9134492585078,
-145.323053305284));
#146182=CARTESIAN_POINT('Ctrl Pts',(-51.8549375288294,-19.9204232163692,
-158.383965825256));
#146183=CARTESIAN_POINT('Ctrl Pts',(-57.9903087491627,-19.9260113903464,
-171.449026400902));
#146184=CARTESIAN_POINT('Ctrl Pts',(-39.5,-20.48000002,-129.914446011788));
#146185=CARTESIAN_POINT('Ctrl Pts',(-39.,-20.48000002,-129.914446011788));
#146186=CARTESIAN_POINT('Ctrl Pts',(-39.,-19.98000002,-129.914446011788));
#146187=CARTESIAN_POINT('Ctrl Pts',(-39.5000000028435,-20.48000002,-130.287671434236));
#146188=CARTESIAN_POINT('Ctrl Pts',(-38.9872746975485,-20.48000002,-130.330124066848));
#146189=CARTESIAN_POINT('Ctrl Pts',(-39.,-19.9674346440713,-130.324899900514));
#146190=CARTESIAN_POINT('Ctrl Pts',(-39.5411198836701,-20.48000002,-130.653963774132));
#146191=CARTESIAN_POINT('Ctrl Pts',(-39.0203709824336,-20.48000002,-130.73585622864));
#146192=CARTESIAN_POINT('Ctrl Pts',(-39.0456887600695,-19.9546004036482,
-130.727459443406));
#146193=CARTESIAN_POINT('Ctrl Pts',(-39.7019669306849,-20.48000002,-131.373086703203));
#146194=CARTESIAN_POINT('Ctrl Pts',(-39.1707024462744,-20.48000002,-131.538360679722));
#146195=CARTESIAN_POINT('Ctrl Pts',(-39.2244077003248,-19.9284125341257,
-131.517220896748));
#146196=CARTESIAN_POINT('Ctrl Pts',(-39.8231470367065,-20.48000002,-131.72814043837));
#146197=CARTESIAN_POINT('Ctrl Pts',(-39.2920635693995,-20.48000002,-131.938092167695));
#146198=CARTESIAN_POINT('Ctrl Pts',(-39.3590527322559,-19.9149653023259,
-131.906857743156));
#146199=CARTESIAN_POINT('Ctrl Pts',(-39.9829309662066,-20.48000002,-132.065646534579));
#146200=CARTESIAN_POINT('Ctrl Pts',(-39.4537365768201,-20.48000002,-132.316180555747));
#146201=CARTESIAN_POINT('Ctrl Pts',(-39.5365899624517,-19.9017174575869,
-132.27695566545));
#146202=CARTESIAN_POINT('',(-39.,-19.98000002,-129.914446011788));
#146203=CARTESIAN_POINT('Origin',(-39.5,-19.98000002,-129.914446011788));
#146204=CARTESIAN_POINT('Ctrl Pts',(-39.,-19.98000002,-129.914446011788));
#146205=CARTESIAN_POINT('Ctrl Pts',(-39.,-19.9674346440713,-130.324899900514));
#146206=CARTESIAN_POINT('Ctrl Pts',(-39.0456887600695,-19.9546004036482,
-130.727459443406));
#146207=CARTESIAN_POINT('Ctrl Pts',(-39.1350482301972,-19.9415064688869,
-131.122340170077));
#146208=CARTESIAN_POINT('Ctrl Pts',(-39.2244077003248,-19.9284125341257,
-131.517220896748));
#146209=CARTESIAN_POINT('Ctrl Pts',(-39.3590527322559,-19.9149653023259,
-131.906857743156));
#146210=CARTESIAN_POINT('Ctrl Pts',(-39.5365899624517,-19.9017174575869,
-132.27695566545));
#146211=CARTESIAN_POINT('Origin',(-39.5,-19.98000002,-55.24995));
#146212=CARTESIAN_POINT('',(-39.,-19.9800000199999,-102.144196959718));
#146213=CARTESIAN_POINT('Origin',(-39.5,-19.98000002,-102.144196959718));
#146214=CARTESIAN_POINT('',(-39.,-19.98000002,-129.34995));
#146215=CARTESIAN_POINT('Ctrl Pts',(-40.0012502563217,-20.48000002,-99.954717797516));
#146216=CARTESIAN_POINT('Ctrl Pts',(-39.4725489992773,-20.48000002,-99.6988739218247));
#146217=CARTESIAN_POINT('Ctrl Pts',(-39.5569491658928,-19.9001814680542,
-99.7397158520094));
#146218=CARTESIAN_POINT('Ctrl Pts',(-39.8323199385717,-20.48000002,-100.303930668773));
#146219=CARTESIAN_POINT('Ctrl Pts',(-39.301375019511,-20.48000002,-100.090148174869));
#146220=CARTESIAN_POINT('Ctrl Pts',(-39.3692493188849,-19.9139264408504,
-100.122626239893));
#146221=CARTESIAN_POINT('Ctrl Pts',(-39.7069896112656,-20.48000002,-100.665459816052));
#146222=CARTESIAN_POINT('Ctrl Pts',(-39.1755409765978,-20.48000002,-100.497354008517));
#146223=CARTESIAN_POINT('Ctrl Pts',(-39.2299915028605,-19.9276433576926,
-100.519356460951));
#146224=CARTESIAN_POINT('Ctrl Pts',(-39.5390449391743,-20.48000002,-101.411637934188));
#146225=CARTESIAN_POINT('Ctrl Pts',(-39.018406306162,-20.48000002,-101.330154470495));
#146226=CARTESIAN_POINT('Ctrl Pts',(-39.0433847037664,-19.9548298743016,
-101.338822719377));
#146227=CARTESIAN_POINT('Ctrl Pts',(-39.4968660312411,-20.48000002,-101.799124124856));
#146228=CARTESIAN_POINT('Ctrl Pts',(-38.9847617214833,-20.48000002,-101.759282695456));
#146229=CARTESIAN_POINT('Ctrl Pts',(-38.9965184980456,-19.9683907683482,
-101.764681199409));
#146230=CARTESIAN_POINT('Ctrl Pts',(-39.5001813816655,-20.48000002,-102.186616395301));
#146231=CARTESIAN_POINT('Ctrl Pts',(-39.001593844989,-20.48000002,-102.190836991961));
#146232=CARTESIAN_POINT('Ctrl Pts',(-39.0002014519442,-19.9813964268796,
-102.190849108877));
#146233=CARTESIAN_POINT('Ctrl Pts',(-39.5365899564018,-19.9017175093585,
-99.7816874458032));
#146234=CARTESIAN_POINT('Ctrl Pts',(-39.4868412510969,-19.9054297760661,
-99.8853949251705));
#146235=CARTESIAN_POINT('Ctrl Pts',(-39.4406574931192,-19.9091517930361,
-99.990138214928));
#146236=CARTESIAN_POINT('Ctrl Pts',(-39.3979429037,-19.9128649009136,-100.095860132891));
#146237=CARTESIAN_POINT('Ctrl Pts',(-39.3547717131843,-19.9166177003614,
-100.202712173941));
#146238=CARTESIAN_POINT('Ctrl Pts',(-39.3151435367721,-19.9203617208069,
-100.310564614436));
#146239=CARTESIAN_POINT('Ctrl Pts',(-39.2789942567738,-19.924093206991,
-100.419396332393));
#146240=CARTESIAN_POINT('Ctrl Pts',(-39.2425575305557,-19.9278543646264,
-100.529093441471));
#146241=CARTESIAN_POINT('Ctrl Pts',(-39.2096547048051,-19.931603147313,
-100.639786363507));
#146242=CARTESIAN_POINT('Ctrl Pts',(-39.1802648150382,-19.9353461978555,
-100.751479335446));
#146243=CARTESIAN_POINT('Ctrl Pts',(-39.1647600945192,-19.9373208548893,
-100.81040328268));
#146244=CARTESIAN_POINT('Ctrl Pts',(-39.1502338657269,-19.9392940583882,
-100.869605905783));
#146245=CARTESIAN_POINT('Ctrl Pts',(-39.1366886677995,-19.9412674210986,
-100.929089335053));
#146246=CARTESIAN_POINT('Ctrl Pts',(-39.1088256225296,-19.945326711692,
-101.051449265963));
#146247=CARTESIAN_POINT('Ctrl Pts',(-39.0850665637736,-19.9493899507519,
-101.175230562368));
#146248=CARTESIAN_POINT('Ctrl Pts',(-39.0655733708748,-19.9534338869003,
-101.300036499352));
#146249=CARTESIAN_POINT('Ctrl Pts',(-39.0461769195927,-19.9574577536366,
-101.424223044317));
#146250=CARTESIAN_POINT('Ctrl Pts',(-39.0310043253741,-19.9614623125903,
-101.549423682696));
#146251=CARTESIAN_POINT('Ctrl Pts',(-39.0201697390594,-19.9654321073935,
-101.675224312219));
#146252=CARTESIAN_POINT('Ctrl Pts',(-39.0093951990674,-19.9693799012109,
-101.800327742515));
#146253=CARTESIAN_POINT('Ctrl Pts',(-39.0029108630928,-19.9732931398505,
-101.926024090876));
#146254=CARTESIAN_POINT('Ctrl Pts',(-39.0007812701477,-19.9771667798669,
-102.05188934728));
#146255=CARTESIAN_POINT('Ctrl Pts',(-39.0002608009155,-19.978113491514,
-102.082650621869));
#146256=CARTESIAN_POINT('Ctrl Pts',(-39.0000002133804,-19.9790578925252,
-102.113421924474));
#146257=CARTESIAN_POINT('Ctrl Pts',(-39.000000000131,-19.9800000199999,
-102.144196959718));
#146258=CARTESIAN_POINT('Ctrl Pts',(-39.4705101402401,-14.154883972851,
-101.179273599517));
#146259=CARTESIAN_POINT('Ctrl Pts',(-39.,-14.2196500163134,-102.183653245897));
#146260=CARTESIAN_POINT('Ctrl Pts',(-39.,-14.2911437666779,-103.292364908221));
#146261=CARTESIAN_POINT('Ctrl Pts',(-39.473885603051,-15.1336440339978,
-101.108924169704));
#146262=CARTESIAN_POINT('Ctrl Pts',(-38.9999999999962,-15.2519052464411,
-102.112898232639));
#146263=CARTESIAN_POINT('Ctrl Pts',(-39.,-15.3821188871317,-103.222014874282));
#146264=CARTESIAN_POINT('Ctrl Pts',(-39.4814699289176,-16.1148163368312,
-100.950916925651));
#146265=CARTESIAN_POINT('Ctrl Pts',(-39.,-16.2866475513133,-101.953874758818));
#146266=CARTESIAN_POINT('Ctrl Pts',(-39.,-16.4753328054123,-103.064008234267));
#146267=CARTESIAN_POINT('Ctrl Pts',(-39.5044475737172,-18.0667048767241,
-100.467247875485));
#146268=CARTESIAN_POINT('Ctrl Pts',(-39.,-18.3422738396393,-101.467519549647));
#146269=CARTESIAN_POINT('Ctrl Pts',(-39.,-18.6473032869024,-102.580339184276));
#146270=CARTESIAN_POINT('Ctrl Pts',(-39.5194922305763,-19.012479411179,
-100.148762913439));
#146271=CARTESIAN_POINT('Ctrl Pts',(-39.,-19.3376015901503,-101.147059506123));
#146272=CARTESIAN_POINT('Ctrl Pts',(-39.,-19.6982839688054,-102.261854767811));
#146273=CARTESIAN_POINT('Ctrl Pts',(-39.5372194307944,-19.9345274212658,
-99.7681750639369));
#146274=CARTESIAN_POINT('Ctrl Pts',(-39.,-20.3054076594241,-100.764738681203));
#146275=CARTESIAN_POINT('Ctrl Pts',(-39.,-20.7209336217775,-101.88126637264));
#146276=CARTESIAN_POINT('',(-39.0000000000002,-14.330000015482,-103.28982244638));
#146277=CARTESIAN_POINT('Ctrl Pts',(-39.,-14.3300000071455,-103.289822320808));
#146278=CARTESIAN_POINT('Ctrl Pts',(-39.,-14.6503224302959,-103.268556852662));
#146279=CARTESIAN_POINT('Ctrl Pts',(-38.9999999999999,-14.9696787697432,
-103.239819970848));
#146280=CARTESIAN_POINT('Ctrl Pts',(-39.0000000000001,-15.2880843675558,
-103.203826801699));
#146281=CARTESIAN_POINT('Ctrl Pts',(-39.0000000000004,-15.6115732353053,
-103.167259010131));
#146282=CARTESIAN_POINT('Ctrl Pts',(-38.9999999999999,-15.9340810135531,
-103.123201376372));
#146283=CARTESIAN_POINT('Ctrl Pts',(-39.0000000000089,-16.2556315657684,
-103.071825704719));
#146284=CARTESIAN_POINT('Ctrl Pts',(-39.0000000000177,-16.568088880393,
-103.021902903184));
#146285=CARTESIAN_POINT('Ctrl Pts',(-39.0000000000333,-16.8796426042166,
-102.965069752024));
#146286=CARTESIAN_POINT('Ctrl Pts',(-39.000000000099,-17.1903180517835,
-102.90143687879));
#146287=CARTESIAN_POINT('Ctrl Pts',(-39.0000000001251,-17.3140185734884,
-102.87610040731));
#146288=CARTESIAN_POINT('Ctrl Pts',(-39.0000000001567,-17.4376802476524,
-102.849665441423));
#146289=CARTESIAN_POINT('Ctrl Pts',(-39.0000000001917,-17.5613085289994,
-102.822130971399));
#146290=CARTESIAN_POINT('Ctrl Pts',(-39.000000000283,-17.8840119032273,
-102.750258530179));
#146291=CARTESIAN_POINT('Ctrl Pts',(-39.0000000004,-18.2040368478248,-102.671531783398));
#146292=CARTESIAN_POINT('Ctrl Pts',(-39.0000000004561,-18.5218724866246,
-102.586181685713));
#146293=CARTESIAN_POINT('Ctrl Pts',(-39.0000000005153,-18.8564962428641,
-102.496323385396));
#146294=CARTESIAN_POINT('Ctrl Pts',(-39.0000000004874,-19.1886932216437,
-102.399123389359));
#146295=CARTESIAN_POINT('Ctrl Pts',(-39.0000000003521,-19.519010542234,
-102.294797669286));
#146296=CARTESIAN_POINT('Ctrl Pts',(-39.000000000289,-19.6730648764625,
-102.246141942363));
#146297=CARTESIAN_POINT('Ctrl Pts',(-39.0000000002054,-19.8267100435457,
-102.195935559143));
#146298=CARTESIAN_POINT('Ctrl Pts',(-39.000000000131,-19.98000002,-102.144196959718));
#146299=CARTESIAN_POINT('Origin',(-46.4345084630437,-14.3111647034258,-103.828563644064));
#146300=CARTESIAN_POINT('Ctrl Pts',(-58.2781275348581,-14.3194901627709,
-60.8508735991007));
#146301=CARTESIAN_POINT('Ctrl Pts',(-58.2874540965012,-13.83000002,-60.8552238163692));
#146302=CARTESIAN_POINT('Ctrl Pts',(-58.7311595360587,-13.83000002,-61.0621827299711));
#146303=CARTESIAN_POINT('Ctrl Pts',(-52.0097486856907,-14.3183690440453,
-74.2898953083048));
#146304=CARTESIAN_POINT('Ctrl Pts',(-52.0270272593534,-13.8300000198715,
-74.2797364934824));
#146305=CARTESIAN_POINT('Ctrl Pts',(-52.4627544636864,-13.83000002,-74.5012048985427));
#146306=CARTESIAN_POINT('Ctrl Pts',(-45.7410317152176,-14.3169685900793,
-87.7287563851229));
#146307=CARTESIAN_POINT('Ctrl Pts',(-45.7671827316852,-13.8300000198453,
-87.7027488289555));
#146308=CARTESIAN_POINT('Ctrl Pts',(-46.194004389791,-13.83000002,-87.9400661652057));
#146309=CARTESIAN_POINT('Ctrl Pts',(-39.4710976496822,-14.3145440753934,
-101.167027481326));
#146310=CARTESIAN_POINT('Ctrl Pts',(-39.4846775617168,-13.83000002,-101.173363584839));
#146311=CARTESIAN_POINT('Ctrl Pts',(-39.923987884714,-13.83000002,-101.378336612196));
#146312=CARTESIAN_POINT('Origin',(-39.923987884714,-14.33000002,-101.378336612196));
#146313=CARTESIAN_POINT('Ctrl Pts',(-39.5,-13.83000002,-103.289822573788));
#146314=CARTESIAN_POINT('Ctrl Pts',(-39.,-13.83000002,-103.289822573788));
#146315=CARTESIAN_POINT('Ctrl Pts',(-39.,-14.33000002,-103.289822573788));
#146316=CARTESIAN_POINT('Ctrl Pts',(-39.5000000055327,-13.83000002,-102.630037977128));
#146317=CARTESIAN_POINT('Ctrl Pts',(-39.0048213824044,-13.83000002,-102.560555788171));
#146318=CARTESIAN_POINT('Ctrl Pts',(-39.,-14.3251554673834,-102.557050168938));
#146319=CARTESIAN_POINT('Ctrl Pts',(-39.6421844024665,-13.83000002,-101.982314517002));
#146320=CARTESIAN_POINT('Ctrl Pts',(-39.1662598483009,-13.830000019993,
-101.843408229318));
#146321=CARTESIAN_POINT('Ctrl Pts',(-39.1579830770898,-14.319921441001,
-101.837719843386));
#146322=CARTESIAN_POINT('Ctrl Pts',(-39.923987884714,-13.83000002,-101.378336612196));
#146323=CARTESIAN_POINT('Ctrl Pts',(-39.4846775617168,-13.83000002,-101.173363584839));
#146324=CARTESIAN_POINT('Ctrl Pts',(-39.4710976496822,-14.3145440753935,
-101.167027481325));
#146325=CARTESIAN_POINT('Origin',(-39.5,-14.33000002,-103.289822573788));
#146326=CARTESIAN_POINT('Origin',(-39.5,-14.33000002,-55.24995));
#146327=CARTESIAN_POINT('',(-39.,-14.3300000196436,-128.768820403088));
#146328=CARTESIAN_POINT('Origin',(-39.5,-14.33000002,-128.768820397718));
#146329=CARTESIAN_POINT('',(-39.,-14.33000002,-129.34995));
#146330=CARTESIAN_POINT('Ctrl Pts',(-39.923987884714,-13.83000002,-130.68030635931));
#146331=CARTESIAN_POINT('Ctrl Pts',(-39.4846775617168,-13.83000002,-130.885279386667));
#146332=CARTESIAN_POINT('Ctrl Pts',(-39.4710976496822,-14.3145440753934,
-130.89161549018));
#146333=CARTESIAN_POINT('Ctrl Pts',(-39.6450175280278,-13.83000002,-130.082400567686));
#146334=CARTESIAN_POINT('Ctrl Pts',(-39.1694803296317,-13.83000002,-130.222011573448));
#146335=CARTESIAN_POINT('Ctrl Pts',(-39.1611309974652,-14.3198673792142,
-130.227665983087));
#146336=CARTESIAN_POINT('Ctrl Pts',(-39.5000000016417,-13.83000002,-129.435305216167));
#146337=CARTESIAN_POINT('Ctrl Pts',(-39.0048700588287,-13.83000002,-129.505450476954));
#146338=CARTESIAN_POINT('Ctrl Pts',(-39.,-14.325106270286,-129.50903420183));
#146339=CARTESIAN_POINT('Ctrl Pts',(-39.5,-13.83000002,-128.768820397718));
#146340=CARTESIAN_POINT('Ctrl Pts',(-38.9999999999999,-13.83000002,-128.768820397718));
#146341=CARTESIAN_POINT('Ctrl Pts',(-39.,-14.33000002,-128.768820397718));
#146342=CARTESIAN_POINT('',(-39.4710976496822,-14.3145440753934,-130.89161549018));
#146343=CARTESIAN_POINT('Origin',(-39.923987884714,-14.33000002,-130.68030635931));
#146344=CARTESIAN_POINT('Origin',(-46.4348610974772,-14.3111430565211,-128.233135964139));
#146345=CARTESIAN_POINT('Ctrl Pts',(-39.4710976496822,-14.3145440753934,
-130.89161549018));
#146346=CARTESIAN_POINT('Ctrl Pts',(-39.4846775617168,-13.83000002,-130.885279386667));
#146347=CARTESIAN_POINT('Ctrl Pts',(-39.923987884714,-13.83000002,-130.68030635931));
#146348=CARTESIAN_POINT('Ctrl Pts',(-45.7785509549148,-14.3169830983588,
-144.410301102566));
#146349=CARTESIAN_POINT('Ctrl Pts',(-45.8048635488014,-13.83000002,-144.43668735532));
#146350=CARTESIAN_POINT('Ctrl Pts',(-46.2315241188232,-13.83000002,-144.198991310165));
#146351=CARTESIAN_POINT('Ctrl Pts',(-52.0847736772191,-14.3183867301138,
-157.929583215096));
#146352=CARTESIAN_POINT('Ctrl Pts',(-52.1020957034304,-13.8300000201034,
-157.939875120093));
#146353=CARTESIAN_POINT('Ctrl Pts',(-52.5377799111353,-13.83000002,-157.718273616974));
#146354=CARTESIAN_POINT('Ctrl Pts',(-58.3906572805143,-14.3195102506022,
-171.449026400902));
#146355=CARTESIAN_POINT('Ctrl Pts',(-58.3999663918639,-13.83000002,-171.444684327491));
#146356=CARTESIAN_POINT('Ctrl Pts',(-58.8436897472855,-13.83000002,-171.237717270032));
#146357=CARTESIAN_POINT('',(-58.3906572805143,-14.3195102506022,-171.449026400902));
#146358=CARTESIAN_POINT('Origin',(-58.8436897472855,-14.33000002,-171.237717270032));
#146359=CARTESIAN_POINT('Ctrl Pts',(-58.3906572805143,-14.3195102506022,
-171.449026400902));
#146360=CARTESIAN_POINT('Ctrl Pts',(-52.0847736772191,-14.3183867301138,
-157.929583215096));
#146361=CARTESIAN_POINT('Ctrl Pts',(-45.7785509549148,-14.3169830983588,
-144.410301102566));
#146362=CARTESIAN_POINT('Ctrl Pts',(-39.4710976496822,-14.3145440753934,
-130.89161549018));
#146363=CARTESIAN_POINT('Ctrl Pts',(-58.3906572805143,-14.3195102506022,
-171.449026400902));
#146364=CARTESIAN_POINT('Ctrl Pts',(-58.3999663918639,-13.83000002,-171.444684327491));
#146365=CARTESIAN_POINT('Ctrl Pts',(-58.8436897472855,-13.83000002,-171.237717270032));
#146366=CARTESIAN_POINT('Ctrl Pts',(-58.452336355597,-14.3188132239679,
-171.581227559315));
#146367=CARTESIAN_POINT('Ctrl Pts',(-58.4628431558437,-13.8300000200007,
-171.577873523862));
#146368=CARTESIAN_POINT('Ctrl Pts',(-58.9361841983689,-13.83000002,-171.436019148456));
#146369=CARTESIAN_POINT('Ctrl Pts',(-58.484398987579,-14.3184534099214,
-171.72428852145));
#146370=CARTESIAN_POINT('Ctrl Pts',(-58.4956819559116,-13.83000002,-171.722618633075));
#146371=CARTESIAN_POINT('Ctrl Pts',(-58.9842656416468,-13.83000002,-171.650610345097));
#146372=CARTESIAN_POINT('Ctrl Pts',(-58.4843989875811,-14.3184534098307,
-171.871644662643));
#146373=CARTESIAN_POINT('Ctrl Pts',(-58.4956819583251,-13.83000002,-171.871644662643));
#146374=CARTESIAN_POINT('Ctrl Pts',(-58.9842656455947,-13.83000002,-171.871644662643));
#146375=CARTESIAN_POINT('Origin',(-58.9842656455946,-14.33000002,-171.871644662643));
#146376=CARTESIAN_POINT('Origin',(-57.4849665102709,-14.329895034911,-171.871652207609));
#146377=CARTESIAN_POINT('Origin',(-58.9842656455947,-14.33000002,-179.64995));
#146378=CARTESIAN_POINT('Origin',(-58.9842656455946,-14.33000002,-176.2719717603));
#146379=CARTESIAN_POINT('Ctrl Pts',(-60.,-13.33000002,-174.751208632418));
#146380=CARTESIAN_POINT('Ctrl Pts',(-60.,-13.83000002,-174.751208632417));
#146381=CARTESIAN_POINT('Ctrl Pts',(-59.5,-13.83000002,-174.751208632418));
#146382=CARTESIAN_POINT('Ctrl Pts',(-60.,-13.3301495200469,-174.995764866376));
#146383=CARTESIAN_POINT('Ctrl Pts',(-59.9998505155736,-13.83000002,-174.995728395116));
#146384=CARTESIAN_POINT('Ctrl Pts',(-59.499999994458,-13.83000002,-174.955005950799));
#146385=CARTESIAN_POINT('Ctrl Pts',(-59.9705302647519,-13.3302950638363,
-175.235357479373));
#146386=CARTESIAN_POINT('Ctrl Pts',(-59.9702437452671,-13.8300000199993,
-175.235287718005));
#146387=CARTESIAN_POINT('Ctrl Pts',(-59.4754418884424,-13.83000002,-175.154666905584));
#146388=CARTESIAN_POINT('Ctrl Pts',(-59.8546684450659,-13.3305785951146,
-175.704793574078));
#146389=CARTESIAN_POINT('Ctrl Pts',(-59.8541239849711,-13.8300000200007,
-175.704587709371));
#146390=CARTESIAN_POINT('Ctrl Pts',(-59.3788903697392,-13.83000002,-175.545864512034));
#146391=CARTESIAN_POINT('Ctrl Pts',(-59.7669119843163,-13.3307170303008,
-175.935426552567));
#146392=CARTESIAN_POINT('Ctrl Pts',(-59.7662611489698,-13.8300000199988,
-175.935125812779));
#146393=CARTESIAN_POINT('Ctrl Pts',(-59.3057599866248,-13.83000002,-175.738059080183));
#146394=CARTESIAN_POINT('Ctrl Pts',(-59.5422070340633,-13.3309719059141,
-176.362223209373));
#146395=CARTESIAN_POINT('Ctrl Pts',(-59.5413945721013,-13.8300000200012,
-176.361684206804));
#146396=CARTESIAN_POINT('Ctrl Pts',(-59.1185058620249,-13.83000002,-176.093723731171));
#146397=CARTESIAN_POINT('Ctrl Pts',(-59.4027363887007,-13.331091646732,
-176.563890694693));
#146398=CARTESIAN_POINT('Ctrl Pts',(-59.4018755020326,-13.8300000199995,
-176.563219594419));
#146399=CARTESIAN_POINT('Ctrl Pts',(-59.0022803225031,-13.83000002,-176.261780328219));
#146400=CARTESIAN_POINT('Ctrl Pts',(-59.0800292616587,-13.3313061338651,
-176.92662799811));
#146401=CARTESIAN_POINT('Ctrl Pts',(-59.0791375439908,-13.8300000200005,
-176.925670411677));
#146402=CARTESIAN_POINT('Ctrl Pts',(-58.7333577194631,-13.83000002,-176.564062061699));
#146403=CARTESIAN_POINT('Ctrl Pts',(-58.8992210551541,-13.3313999972609,
-177.086172425279));
#146404=CARTESIAN_POINT('Ctrl Pts',(-58.8983479608961,-13.830000020003,
-177.085078467603));
#146405=CARTESIAN_POINT('Ctrl Pts',(-58.5826842101506,-13.83000002,-176.697016027753));
#146406=CARTESIAN_POINT('Ctrl Pts',(-58.6989442326066,-13.3314807280565,
-177.223786737086));
#146407=CARTESIAN_POINT('Ctrl Pts',(-58.698108161756,-13.83000002,-177.222569964948));
#146408=CARTESIAN_POINT('Ctrl Pts',(-58.4157868605055,-13.83000002,-176.811694866106));
#146409=CARTESIAN_POINT('',(-60.,-13.33000002,-174.751208632418));
#146410=CARTESIAN_POINT('Origin',(-59.5,-13.33000002,-174.751208632418));
#146411=CARTESIAN_POINT('',(-58.7133156820334,-13.3314748988427,-177.213850299147));
#146412=CARTESIAN_POINT('Ctrl Pts',(-60.,-13.33000002,-174.751208632418));
#146413=CARTESIAN_POINT('Ctrl Pts',(-59.9999999999956,-13.3301495346025,
-174.995764866375));
#146414=CARTESIAN_POINT('Ctrl Pts',(-59.9705302647436,-13.3302950783898,
-175.235357479371));
#146415=CARTESIAN_POINT('Ctrl Pts',(-59.8546684450501,-13.330578609664,
-175.704793574072));
#146416=CARTESIAN_POINT('Ctrl Pts',(-59.7669119842973,-13.3307170448482,
-175.935426552558));
#146417=CARTESIAN_POINT('Ctrl Pts',(-59.5422070340396,-13.3309719204577,
-176.362223209358));
#146418=CARTESIAN_POINT('Ctrl Pts',(-59.4027363886756,-13.3310916612739,
-176.563890694673));
#146419=CARTESIAN_POINT('Ctrl Pts',(-59.0838978236773,-13.3313035771661,
-176.922279560609));
#146420=CARTESIAN_POINT('Ctrl Pts',(-58.9078798727822,-13.3313955032287,
-177.078509506427));
#146421=CARTESIAN_POINT('Ctrl Pts',(-58.7133155825256,-13.3314748983292,
-177.213850156091));
#146422=CARTESIAN_POINT('Ctrl Pts',(-58.9842656455839,-13.8300000182384,
-176.2719717603));
#146423=CARTESIAN_POINT('Ctrl Pts',(-58.9705475680472,-13.8299985684035,
-176.318283990653));
#146424=CARTESIAN_POINT('Ctrl Pts',(-58.9568482086768,-13.8291036195285,
-176.363544967324));
#146425=CARTESIAN_POINT('Ctrl Pts',(-58.9433630154086,-13.8271227458294,
-176.407719581748));
#146426=CARTESIAN_POINT('Ctrl Pts',(-58.9375094778774,-13.8262629050906,
-176.426894521128));
#146427=CARTESIAN_POINT('Ctrl Pts',(-58.9316958151412,-13.8251982285538,
-176.445864414423));
#146428=CARTESIAN_POINT('Ctrl Pts',(-58.9259357951406,-13.8239121842354,
-176.464624333952));
#146429=CARTESIAN_POINT('Ctrl Pts',(-58.9141476212573,-13.8212802291303,
-176.503017463389));
#146430=CARTESIAN_POINT('Ctrl Pts',(-58.9026487920717,-13.8177209175776,
-176.540494484498));
#146431=CARTESIAN_POINT('Ctrl Pts',(-58.8915082859054,-13.8130914358196,
-176.577029027276));
#146432=CARTESIAN_POINT('Ctrl Pts',(-58.8808983823344,-13.8086824480856,
-176.61182349443));
#146433=CARTESIAN_POINT('Ctrl Pts',(-58.8706133980374,-13.8033020833572,
-176.645763126895));
#146434=CARTESIAN_POINT('Ctrl Pts',(-58.8607007260993,-13.7968342336531,
-176.678780444292));
#146435=CARTESIAN_POINT('Ctrl Pts',(-58.8510239250903,-13.7905202857153,
-176.711012118285));
#146436=CARTESIAN_POINT('Ctrl Pts',(-58.8417018329604,-13.7831691988171,
-176.742364795295));
#146437=CARTESIAN_POINT('Ctrl Pts',(-58.8327678658211,-13.7746910572516,
-176.77273210973));
#146438=CARTESIAN_POINT('Ctrl Pts',(-58.8241038159165,-13.7664690613032,
-176.802181952519));
#146439=CARTESIAN_POINT('Ctrl Pts',(-58.8158046324015,-13.7571863673228,
-176.830704717276));
#146440=CARTESIAN_POINT('Ctrl Pts',(-58.8078925277743,-13.7467891715621,
-176.858164968786));
#146441=CARTESIAN_POINT('Ctrl Pts',(-58.8013265549649,-13.7381609104514,
-176.880953249939));
#146442=CARTESIAN_POINT('Ctrl Pts',(-58.7950269503204,-13.7287653913972,
-176.903008963654));
#146443=CARTESIAN_POINT('Ctrl Pts',(-58.7890032485162,-13.7185926712373,
-176.924237158836));
#146444=CARTESIAN_POINT('Ctrl Pts',(-58.7821559295512,-13.7070290411075,
-176.948367872505));
#146445=CARTESIAN_POINT('Ctrl Pts',(-58.7757052330373,-13.6944274034058,
-176.971448103492));
#146446=CARTESIAN_POINT('Ctrl Pts',(-58.7696820480974,-13.6807980296988,
-176.993291172281));
#146447=CARTESIAN_POINT('Ctrl Pts',(-58.7637361328157,-13.6673435031963,
-177.014854022801));
#146448=CARTESIAN_POINT('Ctrl Pts',(-58.7582066537988,-13.652887074821,
-177.035210397418));
#146449=CARTESIAN_POINT('Ctrl Pts',(-58.7531241153642,-13.6374870520949,
-177.054167379287));
#146450=CARTESIAN_POINT('Ctrl Pts',(-58.748098500889,-13.622259508196,-177.072912044716));
#146451=CARTESIAN_POINT('Ctrl Pts',(-58.7435097100686,-13.6061093469723,
-177.09028749886));
#146452=CARTESIAN_POINT('Ctrl Pts',(-58.7393905432394,-13.5891436743187,
-177.106107850033));
#146453=CARTESIAN_POINT('Ctrl Pts',(-58.7366479699053,-13.5778477974228,
-177.116641162973));
#146454=CARTESIAN_POINT('Ctrl Pts',(-58.734113656591,-13.566191488644,-177.126485125293));
#146455=CARTESIAN_POINT('Ctrl Pts',(-58.731798600167,-13.5542186631085,
-177.135588421566));
#146456=CARTESIAN_POINT('Ctrl Pts',(-58.7283814629564,-13.5365461834111,
-177.149025334857));
#146457=CARTESIAN_POINT('Ctrl Pts',(-58.7254282875152,-13.5181135256879,
-177.160900208221));
#146458=CARTESIAN_POINT('Ctrl Pts',(-58.7229449134023,-13.4990734099497,
-177.171064863308));
#146459=CARTESIAN_POINT('Ctrl Pts',(-58.720478237815,-13.4801613223885,
-177.181161169952));
#146460=CARTESIAN_POINT('Ctrl Pts',(-58.718474856036,-13.4606504791436,
-177.189569223433));
#146461=CARTESIAN_POINT('Ctrl Pts',(-58.7169426300318,-13.4407334079337,
-177.196171639718));
#146462=CARTESIAN_POINT('Ctrl Pts',(-58.7154162187833,-13.4208919214619,
-177.202749000014));
#146463=CARTESIAN_POINT('Ctrl Pts',(-58.7143572377876,-13.4006482027158,
-177.207533658972));
#146464=CARTESIAN_POINT('Ctrl Pts',(-58.7137783664067,-13.3802242025167,
-177.210450127637));
#146465=CARTESIAN_POINT('Ctrl Pts',(-58.7133198720031,-13.3640473969248,
-177.21276011325));
#146466=CARTESIAN_POINT('Ctrl Pts',(-58.7131626636372,-13.3477583510132,
-177.213898867151));
#146467=CARTESIAN_POINT('Ctrl Pts',(-58.7133159805679,-13.3314749003853,
-177.213850728308));
#146468=CARTESIAN_POINT('Origin',(-59.5,-13.33000002,-55.24995));
#146469=CARTESIAN_POINT('',(-60.,-13.33000002,-174.748117418411));
#146470=CARTESIAN_POINT('Origin',(-60.,-2.55003103885676E-14,0.));
#146471=CARTESIAN_POINT('',(-60.,-12.83000002,-174.751778045593));
#146472=CARTESIAN_POINT('',(-60.,-12.83000002,-57.911664394164));
#146473=CARTESIAN_POINT('Origin',(-60.,-12.9674774176428,-75.9457339865586));
#146474=CARTESIAN_POINT('Origin',(-59.5,-12.83000002,-55.24995));
#146475=CARTESIAN_POINT('Origin',(-59.5,-12.83000002,-174.751778045594));
#146476=CARTESIAN_POINT('Ctrl Pts',(-39.4702993039609,-11.842906113671,
-101.183667521985));
#146477=CARTESIAN_POINT('Ctrl Pts',(-39.4816972464314,-12.33000002,-101.188984626754));
#146478=CARTESIAN_POINT('Ctrl Pts',(-39.9232693735648,-12.33000002,-101.394976652855));
#146479=CARTESIAN_POINT('Ctrl Pts',(-45.741803891981,-11.8408803347909,
-87.7397145657271));
#146480=CARTESIAN_POINT('Ctrl Pts',(-45.7637467547491,-12.3300000200387,
-87.7178689736084));
#146481=CARTESIAN_POINT('Ctrl Pts',(-46.1948314689912,-12.33000002,-87.9510241496856));
#146482=CARTESIAN_POINT('Ctrl Pts',(-52.0124594137882,-11.8397106642502,
-74.2953500811619));
#146483=CARTESIAN_POINT('Ctrl Pts',(-52.0269437270063,-12.3300000197686,
-74.2868280745294));
#146484=CARTESIAN_POINT('Ctrl Pts',(-52.4655100689676,-12.33000002,-74.5066595330064));
#146485=CARTESIAN_POINT('Ctrl Pts',(-58.2828791719688,-11.838774304476,
-60.8508735991007));
#146486=CARTESIAN_POINT('Ctrl Pts',(-58.2906927660831,-12.33000002,-60.8545178210735));
#146487=CARTESIAN_POINT('Ctrl Pts',(-58.7359481105893,-12.33000002,-61.0621827299711));
#146488=CARTESIAN_POINT('Origin',(-39.9232693735648,-11.83000002,-101.394976652855));
#146489=CARTESIAN_POINT('Ctrl Pts',(-59.5,-12.33000002,-174.751778045593));
#146490=CARTESIAN_POINT('Ctrl Pts',(-60.,-12.33000002,-174.751778045593));
#146491=CARTESIAN_POINT('Ctrl Pts',(-60.,-12.83000002,-174.751778045593));
#146492=CARTESIAN_POINT('Ctrl Pts',(-59.4999999944591,-12.33000002,-174.955507700223));
#146493=CARTESIAN_POINT('Ctrl Pts',(-59.9999432570754,-12.33000002,-174.996239713811));
#146494=CARTESIAN_POINT('Ctrl Pts',(-60.,-12.8299432805227,-174.99625355239));
#146495=CARTESIAN_POINT('Ctrl Pts',(-59.4754576845908,-12.33000002,-175.155103617038));
#146496=CARTESIAN_POINT('Ctrl Pts',(-59.970440441932,-12.33000002,-175.235742099222));
#146497=CARTESIAN_POINT('Ctrl Pts',(-59.9705492201332,-12.8298880430416,
-175.2357685753));
#146498=CARTESIAN_POINT('Ctrl Pts',(-59.3789691429701,-12.33000002,-175.546176541216));
#146499=CARTESIAN_POINT('Ctrl Pts',(-59.8545561835904,-12.33000002,-175.704977777008));
#146500=CARTESIAN_POINT('Ctrl Pts',(-59.8547629729398,-12.8297804365705,
-175.705055936053));
#146501=CARTESIAN_POINT('Ctrl Pts',(-59.3058851982286,-12.33000002,-175.738316981093));
#146502=CARTESIAN_POINT('Ctrl Pts',(-59.7668149966741,-12.3300000199993,
-175.935510188038));
#146503=CARTESIAN_POINT('Ctrl Pts',(-59.7670622382429,-12.8297278961218,
-175.935624391263));
#146504=CARTESIAN_POINT('Ctrl Pts',(-59.1187478700854,-12.33000002,-176.093893786804));
#146505=CARTESIAN_POINT('Ctrl Pts',(-59.5421886833106,-12.3300000200007,
-176.362111673427));
#146506=CARTESIAN_POINT('Ctrl Pts',(-59.5424974437338,-12.829631160742,
-176.362316424594));
#146507=CARTESIAN_POINT('Ctrl Pts',(-59.0025998517383,-12.33000002,-176.261909367341));
#146508=CARTESIAN_POINT('Ctrl Pts',(-59.4027925942033,-12.3300000200005,
-176.563680085108));
#146509=CARTESIAN_POINT('Ctrl Pts',(-59.4031198237833,-12.8295857148276,
-176.563935060575));
#146510=CARTESIAN_POINT('Ctrl Pts',(-58.73383039456,-12.33000002,-176.564162347066));
#146511=CARTESIAN_POINT('Ctrl Pts',(-59.0802573870172,-12.3300000199995,
-176.926274585031));
#146512=CARTESIAN_POINT('Ctrl Pts',(-59.0805964717746,-12.8295042980195,
-176.926638521725));
#146513=CARTESIAN_POINT('Ctrl Pts',(-58.5832426931945,-12.33000002,-176.697112268189));
#146514=CARTESIAN_POINT('Ctrl Pts',(-58.8995591592806,-12.3300000199849,
-177.085762552869));
#146515=CARTESIAN_POINT('Ctrl Pts',(-58.8998912349101,-12.8294686666967,
-177.086178383746));
#146516=CARTESIAN_POINT('Ctrl Pts',(-58.4164435759292,-12.33000002,-176.811801263203));
#146517=CARTESIAN_POINT('Ctrl Pts',(-58.699414230519,-12.33000002,-177.223342557405));
#146518=CARTESIAN_POINT('Ctrl Pts',(-58.699732291115,-12.8294380172077,
-177.223805132118));
#146519=CARTESIAN_POINT('',(-58.7141461350347,-12.8294402383603,-177.213832217127));
#146520=CARTESIAN_POINT('Ctrl Pts',(-58.7141461350374,-12.8294402383603,
-177.213832217125));
#146521=CARTESIAN_POINT('Ctrl Pts',(-58.9085758506643,-12.8294703748154,
-177.078488401254));
#146522=CARTESIAN_POINT('Ctrl Pts',(-59.0844765777018,-12.8295052680351,
-176.922275030383));
#146523=CARTESIAN_POINT('Ctrl Pts',(-59.4031198237771,-12.8295857053604,
-176.56393506057));
#146524=CARTESIAN_POINT('Ctrl Pts',(-59.542497443728,-12.8296311512744,
-176.36231642459));
#146525=CARTESIAN_POINT('Ctrl Pts',(-59.7670622382382,-12.8297278866533,
-175.93562439126));
#146526=CARTESIAN_POINT('Ctrl Pts',(-59.8547629729359,-12.8297804271015,
-175.705055936052));
#146527=CARTESIAN_POINT('Ctrl Pts',(-59.9705492201311,-12.8298880335715,
-175.235768575299));
#146528=CARTESIAN_POINT('Ctrl Pts',(-59.9999999999989,-12.8299432710521,
-174.996253552389));
#146529=CARTESIAN_POINT('Ctrl Pts',(-60.,-12.83000002,-174.751778045593));
#146530=CARTESIAN_POINT('Ctrl Pts',(-58.7141461350374,-12.8294402383603,
-177.213832217125));
#146531=CARTESIAN_POINT('Ctrl Pts',(-58.71386124121,-12.7496539972645,-177.213921724807));
#146532=CARTESIAN_POINT('Ctrl Pts',(-58.7207402303504,-12.6723026604245,
-177.185595547246));
#146533=CARTESIAN_POINT('Ctrl Pts',(-58.7409598721377,-12.5716812769085,
-177.108237839695));
#146534=CARTESIAN_POINT('Ctrl Pts',(-58.7491768361659,-12.5414135007217,
-177.077379300711));
#146535=CARTESIAN_POINT('Ctrl Pts',(-58.7686983660461,-12.486608549538,
-177.006030037118));
#146536=CARTESIAN_POINT('Ctrl Pts',(-58.7801197877863,-12.4620381958002,
-176.965157505607));
#146537=CARTESIAN_POINT('Ctrl Pts',(-58.817725908538,-12.3995214017445,
-176.833790628028));
#146538=CARTESIAN_POINT('Ctrl Pts',(-58.8482938287677,-12.3711206280572,
-176.731313674606));
#146539=CARTESIAN_POINT('Ctrl Pts',(-58.9148079297158,-12.3367286443605,
-176.512401023853));
#146540=CARTESIAN_POINT('Ctrl Pts',(-58.9511729872876,-12.33000002,-176.394565470062));
#146541=CARTESIAN_POINT('Ctrl Pts',(-58.9890336736409,-12.33000002,-176.26629097911));
#146542=CARTESIAN_POINT('Origin',(-58.9890336736409,-11.83000002,-179.64995));
#146543=CARTESIAN_POINT('Origin',(-58.9890336736409,-11.83000002,-176.26629097911));
#146544=CARTESIAN_POINT('Origin',(-58.9890336736409,-11.83000002,-171.871644662643));
#146545=CARTESIAN_POINT('Ctrl Pts',(-58.48912660861,-11.8396398505087,-171.871644662643));
#146546=CARTESIAN_POINT('Ctrl Pts',(-58.4985823439911,-12.33000002,-171.871644662643));
#146547=CARTESIAN_POINT('Ctrl Pts',(-58.9890336736409,-12.33000002,-171.871644662643));
#146548=CARTESIAN_POINT('Ctrl Pts',(-58.4891266086039,-11.8396398501934,
-171.725770040011));
#146549=CARTESIAN_POINT('Ctrl Pts',(-58.4985823327705,-12.33000002,-171.724385262387));
#146550=CARTESIAN_POINT('Ctrl Pts',(-58.9890336571231,-12.33000002,-171.652832645897));
#146551=CARTESIAN_POINT('Ctrl Pts',(-58.4576958292209,-11.8393453695788,
-171.582571135794));
#146552=CARTESIAN_POINT('Ctrl Pts',(-58.46651035226,-12.3300000200013,-171.579769437466));
#146553=CARTESIAN_POINT('Ctrl Pts',(-58.9418960593107,-12.33000002,-171.438034482585));
#146554=CARTESIAN_POINT('Ctrl Pts',(-58.3953999019963,-11.8387575339013,
-171.449026400902));
#146555=CARTESIAN_POINT('Ctrl Pts',(-58.4031988243933,-12.33000002,-171.445389024352));
#146556=CARTESIAN_POINT('Ctrl Pts',(-58.8484691650909,-12.33000002,-171.237717270032));
#146557=CARTESIAN_POINT('',(-58.3953999019963,-11.8387575339013,-171.449026400902));
#146558=CARTESIAN_POINT('Origin',(-58.8484691650909,-11.83000002,-171.237717270032));
#146559=CARTESIAN_POINT('Origin',(-57.4895222060999,-11.8300902499738,-171.871649915017));
#146560=CARTESIAN_POINT('Ctrl Pts',(-58.3953999019963,-11.8387575339013,
-171.449026400902));
#146561=CARTESIAN_POINT('Ctrl Pts',(-58.4031988243933,-12.33000002,-171.445389024352));
#146562=CARTESIAN_POINT('Ctrl Pts',(-58.8484691650909,-12.33000002,-171.237717270032));
#146563=CARTESIAN_POINT('Ctrl Pts',(-52.0874768317228,-11.839695897332,
-157.924129189572));
#146564=CARTESIAN_POINT('Ctrl Pts',(-52.1019974789428,-12.3300000202716,
-157.93276270106));
#146565=CARTESIAN_POINT('Ctrl Pts',(-52.5405278046811,-12.33000002,-157.712819732222));
#146566=CARTESIAN_POINT('Ctrl Pts',(-45.7793173035632,-11.8408682174628,
-144.399344282617));
#146567=CARTESIAN_POINT('Ctrl Pts',(-45.801395679434,-12.33000002,-144.421507685211));
#146568=CARTESIAN_POINT('Ctrl Pts',(-46.2323452217992,-12.33000002,-144.188034690057));
#146569=CARTESIAN_POINT('Ctrl Pts',(-39.4702993039609,-11.842906113671,
-130.874975449521));
#146570=CARTESIAN_POINT('Ctrl Pts',(-39.4816972464314,-12.33000002,-130.869658344752));
#146571=CARTESIAN_POINT('Ctrl Pts',(-39.9232693735648,-12.33000002,-130.663666318651));
#146572=CARTESIAN_POINT('',(-39.4702993039609,-11.842906113671,-130.874975449521));
#146573=CARTESIAN_POINT('Origin',(-39.9232693735648,-11.83000002,-130.663666318651));
#146574=CARTESIAN_POINT('Ctrl Pts',(-39.4702993039609,-11.842906113671,
-130.874975449521));
#146575=CARTESIAN_POINT('Ctrl Pts',(-45.7793173035632,-11.8408682174628,
-144.399344282617));
#146576=CARTESIAN_POINT('Ctrl Pts',(-52.0874768317228,-11.839695897332,
-157.924129189572));
#146577=CARTESIAN_POINT('Ctrl Pts',(-58.3953999019963,-11.8387575339013,
-171.449026400902));
#146578=CARTESIAN_POINT('Ctrl Pts',(-39.5,-12.33000002,-128.755118184993));
#146579=CARTESIAN_POINT('Ctrl Pts',(-39.,-12.33000002,-128.755118184993));
#146580=CARTESIAN_POINT('Ctrl Pts',(-39.,-11.83000002,-128.755118184993));
#146581=CARTESIAN_POINT('Ctrl Pts',(-39.5000000055219,-12.33000002,-129.413887248834));
#146582=CARTESIAN_POINT('Ctrl Pts',(-39.0040281122736,-12.33000002,-129.483935534574));
#146583=CARTESIAN_POINT('Ctrl Pts',(-39.,-11.8340442872404,-129.486859645108));
#146584=CARTESIAN_POINT('Ctrl Pts',(-39.6419410176262,-12.33000002,-130.060600444225));
#146585=CARTESIAN_POINT('Ctrl Pts',(-39.1646430478985,-12.33000002,-130.200415506093));
#146586=CARTESIAN_POINT('Ctrl Pts',(-39.1577125252496,-11.8384144493887,
-130.205177204234));
#146587=CARTESIAN_POINT('Ctrl Pts',(-39.9232693735648,-12.33000002,-130.663666318651));
#146588=CARTESIAN_POINT('Ctrl Pts',(-39.4816972464314,-12.33000002,-130.869658344752));
#146589=CARTESIAN_POINT('Ctrl Pts',(-39.4702993039609,-11.8429061136709,
-130.874975449521));
#146590=CARTESIAN_POINT('',(-39.,-11.8300000206964,-128.75511820843));
#146591=CARTESIAN_POINT('Origin',(-39.5,-11.83000002,-128.755118184993));
#146592=CARTESIAN_POINT('Origin',(-46.4327247058357,-11.8457999179355,-128.216011994814));
#146593=CARTESIAN_POINT('Origin',(-39.5,-11.83000002,-55.24995));
#146594=CARTESIAN_POINT('',(-39.,-11.8300000202903,-103.303524781275));
#146595=CARTESIAN_POINT('Origin',(-39.5,-11.83000002,-103.303524786513));
#146596=CARTESIAN_POINT('',(-39.,-11.83000002,-129.34995));
#146597=CARTESIAN_POINT('Ctrl Pts',(-39.9232693735648,-12.33000002,-101.394976652855));
#146598=CARTESIAN_POINT('Ctrl Pts',(-39.4816972464314,-12.33000002,-101.188984626754));
#146599=CARTESIAN_POINT('Ctrl Pts',(-39.4702993039609,-11.842906113671,
-101.183667521985));
#146600=CARTESIAN_POINT('Ctrl Pts',(-39.6447687306727,-12.33000002,-101.991980946201));
#146601=CARTESIAN_POINT('Ctrl Pts',(-39.1678459389433,-12.3300000200023,
-101.851466764233));
#146602=CARTESIAN_POINT('Ctrl Pts',(-39.1608544296035,-11.8384595965422,
-101.84673342232));
#146603=CARTESIAN_POINT('Ctrl Pts',(-39.5000000016323,-12.33000002,-102.638067201068));
#146604=CARTESIAN_POINT('Ctrl Pts',(-39.0040688095373,-12.3300000199977,
-102.567343181294));
#146605=CARTESIAN_POINT('Ctrl Pts',(-39.,-11.834085348836,-102.564353929887));
#146606=CARTESIAN_POINT('Ctrl Pts',(-39.5,-12.33000002,-103.303524786513));
#146607=CARTESIAN_POINT('Ctrl Pts',(-39.,-12.33000002,-103.303524786513));
#146608=CARTESIAN_POINT('Ctrl Pts',(-39.,-11.83000002,-103.303524786513));
#146609=CARTESIAN_POINT('Origin',(-46.4332003469387,-11.8458180863447,-103.839606692281));
#146610=CARTESIAN_POINT('Ctrl Pts',(-39.5330007135517,-6.22310220971892,
-99.8586617838914));
#146611=CARTESIAN_POINT('Ctrl Pts',(-39.,-5.86351617202512,-100.855722952121));
#146612=CARTESIAN_POINT('Ctrl Pts',(-39.,-5.46102446043621,-101.971753092595));
#146613=CARTESIAN_POINT('Ctrl Pts',(-39.5158163721933,-7.1434218710037,
-100.226898392254));
#146614=CARTESIAN_POINT('Ctrl Pts',(-39.0000000000075,-6.82975403393395,
-101.225648609944));
#146615=CARTESIAN_POINT('Ctrl Pts',(-39.,-6.48207062104881,-102.33998922066));
#146616=CARTESIAN_POINT('Ctrl Pts',(-39.50142226749,-8.08385740698738,-100.53114117287));
#146617=CARTESIAN_POINT('Ctrl Pts',(-39.,-7.81966925102655,-101.531783862877));
#146618=CARTESIAN_POINT('Ctrl Pts',(-39.,-7.52739464652098,-102.644232481647));
#146619=CARTESIAN_POINT('Ctrl Pts',(-39.485193560998,-9.53196095727464,
-100.872391313355));
#146620=CARTESIAN_POINT('Ctrl Pts',(-39.,-9.34536808184436,-101.875027810475));
#146621=CARTESIAN_POINT('Ctrl Pts',(-39.,-9.13906178103241,-102.985482622022));
#146622=CARTESIAN_POINT('Ctrl Pts',(-39.4806657492121,-10.0234751165263,
-100.967196566129));
#146623=CARTESIAN_POINT('Ctrl Pts',(-39.,-9.86335482772211,-101.970380205613));
#146624=CARTESIAN_POINT('Ctrl Pts',(-39.,-9.68642581410213,-103.080287874832));
#146625=CARTESIAN_POINT('Ctrl Pts',(-39.4737139394979,-11.0038787161503,
-101.11251041402));
#146626=CARTESIAN_POINT('Ctrl Pts',(-39.,-10.8967689955421,-102.116504004052));
#146627=CARTESIAN_POINT('Ctrl Pts',(-39.,-10.7786703656218,-103.225601722724));
#146628=CARTESIAN_POINT('Ctrl Pts',(-39.4712727906473,-11.493239882702,
-101.16338521793));
#146629=CARTESIAN_POINT('Ctrl Pts',(-39.0000000000038,-11.4127969575427,
-102.167673995048));
#146630=CARTESIAN_POINT('Ctrl Pts',(-39.,-11.32407160958,-103.276476522877));
#146631=CARTESIAN_POINT('Ctrl Pts',(-39.4698732852484,-11.9818774403001,
-101.192544694569));
#146632=CARTESIAN_POINT('Ctrl Pts',(-39.,-11.9281041096302,-102.196998431102));
#146633=CARTESIAN_POINT('Ctrl Pts',(-39.,-11.8687533077036,-103.305636003273));
#146634=CARTESIAN_POINT('',(-39.,-6.18000001999998,-102.218950121094));
#146635=CARTESIAN_POINT('Ctrl Pts',(-39.0000000000558,-6.18000001999998,
-102.218950121094));
#146636=CARTESIAN_POINT('Ctrl Pts',(-39.0000000001314,-6.5292524637215,
-102.333137272009));
#146637=CARTESIAN_POINT('Ctrl Pts',(-39.0000000002528,-6.88066423664115,
-102.43942079016));
#146638=CARTESIAN_POINT('Ctrl Pts',(-39.0000000003133,-7.23418430799942,
-102.53736711789));
#146639=CARTESIAN_POINT('Ctrl Pts',(-39.0000000003723,-7.57920291835826,
-102.632958029471));
#146640=CARTESIAN_POINT('Ctrl Pts',(-39.0000000003716,-7.92622968243009,
-102.720607819346));
#146641=CARTESIAN_POINT('Ctrl Pts',(-39.0000000003073,-8.2751996248623,
-102.799960112763));
#146642=CARTESIAN_POINT('Ctrl Pts',(-39.0000000002873,-8.38389527497889,
-102.824676422314));
#146643=CARTESIAN_POINT('Ctrl Pts',(-39.0000000002619,-8.49277931386626,
-102.848588085813));
#146644=CARTESIAN_POINT('Ctrl Pts',(-39.0000000002334,-8.60184941027751,
-102.871685311886));
#146645=CARTESIAN_POINT('Ctrl Pts',(-39.0000000002017,-8.72319901066901,
-102.897382906795));
#146646=CARTESIAN_POINT('Ctrl Pts',(-39.0000000001662,-8.84492476936504,
-102.922084618583));
#146647=CARTESIAN_POINT('Ctrl Pts',(-39.0000000001318,-8.96688496783026,
-102.945759157014));
#146648=CARTESIAN_POINT('Ctrl Pts',(-39.0000000000546,-9.2409571131078,
-102.998961198483));
#146649=CARTESIAN_POINT('Ctrl Pts',(-39.0000000000303,-9.5168957930922,
-103.04710594614));
#146650=CARTESIAN_POINT('Ctrl Pts',(-39.0000000000166,-9.79353842563631,
-103.08982360864));
#146651=CARTESIAN_POINT('Ctrl Pts',(-39.0000000000094,-9.93973590489248,
-103.112398634476));
#146652=CARTESIAN_POINT('Ctrl Pts',(-39.0000000000059,-10.0861301614979,
-103.133457170461));
#146653=CARTESIAN_POINT('Ctrl Pts',(-39.0000000000038,-10.2325489057379,
-103.152938666286));
#146654=CARTESIAN_POINT('Ctrl Pts',(-38.9999999999998,-10.5104673644924,
-103.189916631927));
#146655=CARTESIAN_POINT('Ctrl Pts',(-39.0000000000001,-10.7886085240243,
-103.221310636521));
#146656=CARTESIAN_POINT('Ctrl Pts',(-39.,-11.0672887212858,-103.24709706551));
#146657=CARTESIAN_POINT('Ctrl Pts',(-39.,-11.3209998818248,-103.270573096062));
#146658=CARTESIAN_POINT('Ctrl Pts',(-39.,-11.5751577965224,-103.289400790235));
#146659=CARTESIAN_POINT('Ctrl Pts',(-39.,-11.8300000206635,-103.303524774541));
#146660=CARTESIAN_POINT('Ctrl Pts',(-39.,-6.18000001999998,-102.218950121094));
#146661=CARTESIAN_POINT('Ctrl Pts',(-39.,-6.19216140385576,-101.811197248376));
#146662=CARTESIAN_POINT('Ctrl Pts',(-39.0453283089643,-6.20458878978192,
-101.411268531309));
#146663=CARTESIAN_POINT('Ctrl Pts',(-39.133992622656,-6.21727492932601,
-101.018951298921));
#146664=CARTESIAN_POINT('Ctrl Pts',(-39.2226569363477,-6.22996106887011,
-100.626634066533));
#146665=CARTESIAN_POINT('Ctrl Pts',(-39.3562549507175,-6.2429965854182,
-100.239515789679));
#146666=CARTESIAN_POINT('Ctrl Pts',(-39.5323905962559,-6.25584930059377,
-99.8717339663646));
#146667=CARTESIAN_POINT('Ctrl Pts',(-57.9034184448965,-6.23235646472971,
-60.8508735991007));
#146668=CARTESIAN_POINT('Ctrl Pts',(-57.8507724536939,-5.68000001999999,
-60.826158857425));
#146669=CARTESIAN_POINT('Ctrl Pts',(-58.3535376001277,-5.68000001999999,
-61.0621827299711));
#146670=CARTESIAN_POINT('Ctrl Pts',(-51.794541964381,-6.23776491179514,
-73.865008277307));
#146671=CARTESIAN_POINT('Ctrl Pts',(-51.698167660392,-5.68000001999999,
-73.9177186732266));
#146672=CARTESIAN_POINT('Ctrl Pts',(-52.2440275184664,-5.68000001999999,
-74.0763270103718));
#146673=CARTESIAN_POINT('Ctrl Pts',(-45.6775416788308,-6.24451367719405,
-86.8752616229197));
#146674=CARTESIAN_POINT('Ctrl Pts',(-45.5309288684318,-5.68000001999999,
-87.0138122441779));
#146675=CARTESIAN_POINT('Ctrl Pts',(-46.1262203434603,-5.68000001999998,
-87.0865851147193));
#146676=CARTESIAN_POINT('Ctrl Pts',(-39.532390596256,-6.25584930059378,
-99.8717339663645));
#146677=CARTESIAN_POINT('Ctrl Pts',(-39.4524980147409,-5.68000001999998,
-99.8339463478929));
#146678=CARTESIAN_POINT('Ctrl Pts',(-39.9791515366304,-5.68000001999998,
-100.083043097235));
#146679=CARTESIAN_POINT('Origin',(-39.9791515366304,-6.18000001999998,-100.083043097235));
#146680=CARTESIAN_POINT('Ctrl Pts',(-39.5,-5.68000001999998,-102.218950121094));
#146681=CARTESIAN_POINT('Ctrl Pts',(-39.,-5.68000001999997,-102.218950121094));
#146682=CARTESIAN_POINT('Ctrl Pts',(-39.,-6.18000001999998,-102.218950121094));
#146683=CARTESIAN_POINT('Ctrl Pts',(-39.5000000028438,-5.68000001999998,
-101.848394057804));
#146684=CARTESIAN_POINT('Ctrl Pts',(-38.9876888787772,-5.68000001999998,
-101.806176686079));
#146685=CARTESIAN_POINT('Ctrl Pts',(-39.,-6.19216140385576,-101.811197248376));
#146686=CARTESIAN_POINT('Ctrl Pts',(-39.5407954776771,-5.68000001999998,
-101.484716832152));
#146687=CARTESIAN_POINT('Ctrl Pts',(-39.0208449410789,-5.68000001999935,
-101.403186844504));
#146688=CARTESIAN_POINT('Ctrl Pts',(-39.0453283089643,-6.20458878978192,
-101.411268531309));
#146689=CARTESIAN_POINT('Ctrl Pts',(-39.7003912431037,-5.68000001999998,
-100.770720159946));
#146690=CARTESIAN_POINT('Ctrl Pts',(-39.1707994584459,-5.68000002000062,
-100.606268005686));
#146691=CARTESIAN_POINT('Ctrl Pts',(-39.2226569363477,-6.22996106887011,
-100.626634066533));
#146692=CARTESIAN_POINT('Ctrl Pts',(-39.8206290570768,-5.68000001999998,
-100.418199709297));
#146693=CARTESIAN_POINT('Ctrl Pts',(-39.2916053087195,-5.68000001999999,
-100.209430566875));
#146694=CARTESIAN_POINT('Ctrl Pts',(-39.3562549507175,-6.24299658541821,
-100.239515789679));
#146695=CARTESIAN_POINT('Ctrl Pts',(-39.9791515366304,-5.68000001999998,
-100.083043097235));
#146696=CARTESIAN_POINT('Ctrl Pts',(-39.4524980147409,-5.68000001999997,
-99.8339463478928));
#146697=CARTESIAN_POINT('Ctrl Pts',(-39.532390596256,-6.25584930059378,
-99.8717339663646));
#146698=CARTESIAN_POINT('Origin',(-39.5,-6.18000001999998,-102.218950121094));
#146699=CARTESIAN_POINT('Origin',(-39.5,-6.18000001999998,-55.24995));
#146700=CARTESIAN_POINT('',(-39.,-6.180000128392,-129.839693182379));
#146701=CARTESIAN_POINT('Origin',(-39.5,-6.18000001999998,-129.839692850412));
#146702=CARTESIAN_POINT('',(-39.,-6.18000001999998,-129.34995));
#146703=CARTESIAN_POINT('Ctrl Pts',(-39.9969223514525,-5.68000001999998,
-132.012776560392));
#146704=CARTESIAN_POINT('Ctrl Pts',(-39.470792948266,-5.68000002000005,
-132.267009143905));
#146705=CARTESIAN_POINT('Ctrl Pts',(-39.5521401151701,-6.25730737076538,
-132.227701231429));
#146706=CARTESIAN_POINT('Ctrl Pts',(-39.8295349406256,-5.68000001999998,
-131.666258024272));
#146707=CARTESIAN_POINT('Ctrl Pts',(-39.3006695783278,-5.68000001999948,
-131.878729031704));
#146708=CARTESIAN_POINT('Ctrl Pts',(-39.3661545598248,-6.24398265079956,
-131.8474745135));
#146709=CARTESIAN_POINT('Ctrl Pts',(-39.7053043876582,-5.68000001999998,
-131.307566389594));
#146710=CARTESIAN_POINT('Ctrl Pts',(-39.1755529568228,-5.68000001999998,
-131.474771483057));
#146711=CARTESIAN_POINT('Ctrl Pts',(-39.2281188468193,-6.23069539389422,
-131.453591269587));
#146712=CARTESIAN_POINT('Ctrl Pts',(-39.5388026007107,-5.68000001999998,
-130.56730645407));
#146713=CARTESIAN_POINT('Ctrl Pts',(-39.0189458914379,-5.68000001999998,
-130.64844019392));
#146714=CARTESIAN_POINT('Ctrl Pts',(-39.0431153529893,-6.20437672316564,
-130.640102780831));
#146715=CARTESIAN_POINT('Ctrl Pts',(-39.4969580610254,-5.68000001999998,
-130.182934036597));
#146716=CARTESIAN_POINT('Ctrl Pts',(-38.9852239260594,-5.68000001999999,
-130.222593346134));
#146717=CARTESIAN_POINT('Ctrl Pts',(-38.9966207132988,-6.19125736973878,
-130.217409891789));
#146718=CARTESIAN_POINT('Ctrl Pts',(-39.5001721107769,-5.68000001999998,
-129.798501466855));
#146719=CARTESIAN_POINT('Ctrl Pts',(-39.0015087008599,-5.68000001999997,
-129.794376582926));
#146720=CARTESIAN_POINT('Ctrl Pts',(-39.0001911577035,-6.17867888247173,
-129.794365306846));
#146721=CARTESIAN_POINT('',(-39.5323905961839,-6.25584930016544,-132.186909003948));
#146722=CARTESIAN_POINT('Origin',(-39.9791515366304,-6.18000001999998,-131.975599874271));
#146723=CARTESIAN_POINT('Ctrl Pts',(-39.5323905963862,-6.25584929916185,
-132.186909001152));
#146724=CARTESIAN_POINT('Ctrl Pts',(-39.4827974250407,-6.25223045792151,
-132.083355469824));
#146725=CARTESIAN_POINT('Ctrl Pts',(-39.4367726852657,-6.24860303206125,
-131.978767031507));
#146726=CARTESIAN_POINT('Ctrl Pts',(-39.3942214051111,-6.24498502939129,
-131.873200439616));
#146727=CARTESIAN_POINT('Ctrl Pts',(-39.3512191473345,-6.24132868150033,
-131.766515005461));
#146728=CARTESIAN_POINT('Ctrl Pts',(-39.3117636484726,-6.23768164276984,
-131.658829829889));
#146729=CARTESIAN_POINT('Ctrl Pts',(-39.2757918197085,-6.23404744051803,
-131.550165596048));
#146730=CARTESIAN_POINT('Ctrl Pts',(-39.2395417371362,-6.23038512652847,
-131.440660808978));
#146731=CARTESIAN_POINT('Ctrl Pts',(-39.2068288893847,-6.22673549716918,
-131.330160851267));
#146732=CARTESIAN_POINT('Ctrl Pts',(-39.1776335251109,-6.22309201957265,
-131.218661164678));
#146733=CARTESIAN_POINT('Ctrl Pts',(-39.1627061939244,-6.22122914174575,
-131.161652362414));
#146734=CARTESIAN_POINT('Ctrl Pts',(-39.1486991701159,-6.21936774251756,
-131.104381884175));
#146735=CARTESIAN_POINT('Ctrl Pts',(-39.1356148793413,-6.21750639488709,
-131.046847777288));
#146736=CARTESIAN_POINT('Ctrl Pts',(-39.1079099645233,-6.21356514362349,
-130.925024014895));
#146737=CARTESIAN_POINT('Ctrl Pts',(-39.0842950823765,-6.20962076305806,
-130.801786127621));
#146738=CARTESIAN_POINT('Ctrl Pts',(-39.0649315130416,-6.20569589299001,
-130.677528828003));
#146739=CARTESIAN_POINT('Ctrl Pts',(-39.0456626856946,-6.20179022650919,
-130.553879493961));
#146740=CARTESIAN_POINT('Ctrl Pts',(-39.0306039018712,-6.19790406888684,
-130.42922110532));
#146741=CARTESIAN_POINT('Ctrl Pts',(-39.0198687243699,-6.19405235733965,
-130.303965852542));
#146742=CARTESIAN_POINT('Ctrl Pts',(-39.0091916684706,-6.19022149944355,
-130.179388747469));
#146743=CARTESIAN_POINT('Ctrl Pts',(-39.002791676982,-6.18642488444214,
-130.054221669759));
#146744=CARTESIAN_POINT('Ctrl Pts',(-39.0007326738071,-6.18266722871172,
-129.928886829007));
#146745=CARTESIAN_POINT('Ctrl Pts',(-39.0002443724431,-6.1817760846664,
-129.899163138222));
#146746=CARTESIAN_POINT('Ctrl Pts',(-39.0000000000001,-6.18088708117259,
-129.869430069098));
#146747=CARTESIAN_POINT('Ctrl Pts',(-39.,-6.18000018270164,-129.839693348042));
#146748=CARTESIAN_POINT('Ctrl Pts',(-39.532390596256,-6.25584930059378,
-132.186909005141));
#146749=CARTESIAN_POINT('Ctrl Pts',(-39.452498014741,-5.68000001999998,
-132.224696623613));
#146750=CARTESIAN_POINT('Ctrl Pts',(-39.9791515366304,-5.68000001999998,
-131.975599874271));
#146751=CARTESIAN_POINT('Ctrl Pts',(-45.7155147614494,-6.24444363034862,
-145.263691191481));
#146752=CARTESIAN_POINT('Ctrl Pts',(-45.5680069655751,-5.68000001999999,
-145.12303284731));
#146753=CARTESIAN_POINT('Ctrl Pts',(-46.164205183661,-5.68000001999998,
-145.052367414711));
#146754=CARTESIAN_POINT('Ctrl Pts',(-51.870165118292,-6.23767750446664,
-158.354412070984));
#146755=CARTESIAN_POINT('Ctrl Pts',(-51.7735675289641,-5.68000001999999,
-158.300965634462));
#146756=CARTESIAN_POINT('Ctrl Pts',(-52.3196619691199,-5.68000001999999,
-158.143093167052));
#146757=CARTESIAN_POINT('Ctrl Pts',(-58.0166638356104,-6.23225639415715,
-171.449026400902));
#146758=CARTESIAN_POINT('Ctrl Pts',(-57.9641288550927,-5.68000001999999,
-171.47368839131));
#146759=CARTESIAN_POINT('Ctrl Pts',(-58.4667946194619,-5.68000001999999,
-171.237717270032));
#146760=CARTESIAN_POINT('',(-58.0166638356104,-6.23225639415715,-171.449026400902));
#146761=CARTESIAN_POINT('Origin',(-58.4667946194619,-6.18000001999999,-171.237717270032));
#146762=CARTESIAN_POINT('Ctrl Pts',(-58.0166638356104,-6.23225639415715,
-171.449026400902));
#146763=CARTESIAN_POINT('Ctrl Pts',(-51.8701651180199,-6.23767750289604,
-158.354412070834));
#146764=CARTESIAN_POINT('Ctrl Pts',(-45.7155147610371,-6.24444362877111,
-145.263691191088));
#146765=CARTESIAN_POINT('Ctrl Pts',(-39.532390596256,-6.25584930059378,
-132.186909005141));
#146766=CARTESIAN_POINT('Ctrl Pts',(-58.0166638356104,-6.23225639415715,
-171.449026400902));
#146767=CARTESIAN_POINT('Ctrl Pts',(-57.9641288550927,-5.68000002000002,
-171.47368839131));
#146768=CARTESIAN_POINT('Ctrl Pts',(-58.4667946194619,-5.68000001999999,
-171.237717270032));
#146769=CARTESIAN_POINT('Ctrl Pts',(-58.0790703543615,-6.23572556787351,
-171.581106868264));
#146770=CARTESIAN_POINT('Ctrl Pts',(-58.0192749608379,-5.68000001999239,
-171.600361788065));
#146771=CARTESIAN_POINT('Ctrl Pts',(-58.559801654985,-5.68000001999999,
-171.435840927268));
#146772=CARTESIAN_POINT('Ctrl Pts',(-58.1115942404139,-6.23752120598293,
-171.724230304954));
#146773=CARTESIAN_POINT('Ctrl Pts',(-58.0470269895722,-5.68000001999999,
-171.733866658521));
#146774=CARTESIAN_POINT('Ctrl Pts',(-58.608274529079,-5.68000001999999,
-171.650520905847));
#146775=CARTESIAN_POINT('Ctrl Pts',(-58.1115942404669,-6.2375212064409,
-171.871644662643));
#146776=CARTESIAN_POINT('Ctrl Pts',(-58.0470269915054,-5.68000001999999,
-171.871644662643));
#146777=CARTESIAN_POINT('Ctrl Pts',(-58.6082745331205,-5.68000001999999,
-171.871644662643));
#146778=CARTESIAN_POINT('Origin',(-58.6082745331205,-6.18000001999999,-171.871644662643));
#146779=CARTESIAN_POINT('Origin',(-56.6529025639176,-6.15643989082879,-171.969043985007));
#146780=CARTESIAN_POINT('Origin',(-58.6082745331205,-6.18000001999999,-179.64995));
#146781=CARTESIAN_POINT('Origin',(-58.6082745331205,-6.18000001999999,-176.427328712824));
#146782=CARTESIAN_POINT('Ctrl Pts',(-60.,-5.18000001999999,-174.511260182693));
#146783=CARTESIAN_POINT('Ctrl Pts',(-60.,-5.68000001999998,-174.511260182694));
#146784=CARTESIAN_POINT('Ctrl Pts',(-59.5,-5.68000001999999,-174.511260182693));
#146785=CARTESIAN_POINT('Ctrl Pts',(-60.,-5.17778160006748,-174.799392136338));
#146786=CARTESIAN_POINT('Ctrl Pts',(-60.0022233258349,-5.68000002000248,
-174.800030292485));
#146787=CARTESIAN_POINT('Ctrl Pts',(-59.4999999934949,-5.68000001999999,
-174.751455697725));
#146788=CARTESIAN_POINT('Ctrl Pts',(-59.9593729581191,-5.1756134281897,
-175.080714219829));
#146789=CARTESIAN_POINT('Ctrl Pts',(-59.9636195754477,-5.68000001999999,
-175.081942695907));
#146790=CARTESIAN_POINT('Ctrl Pts',(-59.4661441339012,-5.68000001999999,
-174.985974426754));
#146791=CARTESIAN_POINT('Ctrl Pts',(-59.8388406974375,-5.17243729299778,
-175.492475419334));
#146792=CARTESIAN_POINT('Ctrl Pts',(-59.8460772881358,-5.68000001999999,
-175.49508011951));
#146793=CARTESIAN_POINT('Ctrl Pts',(-59.3657005801303,-5.68000001999999,
-175.329231362388));
#146794=CARTESIAN_POINT('Ctrl Pts',(-59.7882941049042,-5.17139018325129,
-175.628164866621));
#146795=CARTESIAN_POINT('Ctrl Pts',(-59.7963955952484,-5.68000002000071,
-175.631508024916));
#146796=CARTESIAN_POINT('Ctrl Pts',(-59.3235784200839,-5.68000001999999,
-175.4423463311));
#146797=CARTESIAN_POINT('Ctrl Pts',(-59.6700340607039,-5.16938852396119,
-175.887451075324));
#146798=CARTESIAN_POINT('Ctrl Pts',(-59.6796421793893,-5.68000001999927,
-175.892503005072));
#146799=CARTESIAN_POINT('Ctrl Pts',(-59.2250283845896,-5.68000001999999,
-175.658495472519));
#146800=CARTESIAN_POINT('Ctrl Pts',(-59.6020511144931,-5.16842516963192,
-176.012189602522));
#146801=CARTESIAN_POINT('Ctrl Pts',(-59.6122794132826,-5.6800000200009,
-176.018182187565));
#146802=CARTESIAN_POINT('Ctrl Pts',(-59.1683759292615,-5.68000001999999,
-175.762481455964));
#146803=CARTESIAN_POINT('Ctrl Pts',(-59.4484275192731,-5.16657340194589,
-176.251884189743));
#146804=CARTESIAN_POINT('Ctrl Pts',(-59.4596388112852,-5.68000001999906,
-176.259950074275));
#146805=CARTESIAN_POINT('Ctrl Pts',(-59.0403562655437,-5.68000001999999,
-175.962298484052));
#146806=CARTESIAN_POINT('Ctrl Pts',(-59.3620233301153,-5.16567852041965,
-176.367676771746));
#146807=CARTESIAN_POINT('Ctrl Pts',(-59.3735776050024,-5.68000001999968,
-176.376845479805));
#146808=CARTESIAN_POINT('Ctrl Pts',(-58.9683527741555,-5.68000001999999,
-176.058826880554));
#146809=CARTESIAN_POINT('Ctrl Pts',(-59.1745444884326,-5.16400295101772,
-176.584424539694));
#146810=CARTESIAN_POINT('Ctrl Pts',(-59.1864690073094,-5.6800000200003,
-176.595885870473));
#146811=CARTESIAN_POINT('Ctrl Pts',(-58.8121204079676,-5.68000001999999,
-176.239514776908));
#146812=CARTESIAN_POINT('Ctrl Pts',(-59.0739603306682,-5.16322437006847,
-176.685107962755));
#146813=CARTESIAN_POINT('Ctrl Pts',(-59.0859070073554,-5.68000001999999,
-176.697708952909));
#146814=CARTESIAN_POINT('Ctrl Pts',(-58.7283002756348,-5.68000001999999,
-176.3234477233));
#146815=CARTESIAN_POINT('Ctrl Pts',(-58.7521818176688,-5.16106213487567,
-176.9646578323));
#146816=CARTESIAN_POINT('Ctrl Pts',(-58.7634647581383,-5.68000001999999,
-176.980908577071));
#146817=CARTESIAN_POINT('Ctrl Pts',(-58.460151514568,-5.68000001999999,
-176.556489535136));
#146818=CARTESIAN_POINT('Ctrl Pts',(-58.5075501754184,-5.15984115636875,
-177.122423932479));
#146819=CARTESIAN_POINT('Ctrl Pts',(-58.5179479000405,-5.68000002000922,
-177.140745767071));
#146820=CARTESIAN_POINT('Ctrl Pts',(-58.2562917522372,-5.68000001999999,
-176.688008530437));
#146821=CARTESIAN_POINT('Ctrl Pts',(-58.2485390147982,-5.15892282666644,
-177.241058641939));
#146822=CARTESIAN_POINT('Ctrl Pts',(-58.2576969618386,-5.68000001999996,
-177.261045698521));
#146823=CARTESIAN_POINT('Ctrl Pts',(-58.0404491789985,-5.68000001999999,
-176.786906275262));
#146824=CARTESIAN_POINT('',(-60.,-5.18000001999999,-174.511260182693));
#146825=CARTESIAN_POINT('Origin',(-59.5,-5.18000001999999,-174.511260182693));
#146826=CARTESIAN_POINT('',(-58.2670189319755,-5.15898895260712,-177.232517863302));
#146827=CARTESIAN_POINT('Ctrl Pts',(-60.,-5.18000001999999,-174.511260182693));
#146828=CARTESIAN_POINT('Ctrl Pts',(-60.,-5.17778160006748,-174.799392136338));
#146829=CARTESIAN_POINT('Ctrl Pts',(-59.9593729581191,-5.1756134281897,
-175.080714219829));
#146830=CARTESIAN_POINT('Ctrl Pts',(-59.8388406974375,-5.17243729299778,
-175.492475419334));
#146831=CARTESIAN_POINT('Ctrl Pts',(-59.7882941049042,-5.17139018325129,
-175.628164866621));
#146832=CARTESIAN_POINT('Ctrl Pts',(-59.6700340607039,-5.16938852396119,
-175.887451075324));
#146833=CARTESIAN_POINT('Ctrl Pts',(-59.6020511144931,-5.16842516963192,
-176.012189602522));
#146834=CARTESIAN_POINT('Ctrl Pts',(-59.4484275192731,-5.16657340194589,
-176.251884189743));
#146835=CARTESIAN_POINT('Ctrl Pts',(-59.3620233301153,-5.16567852041965,
-176.367676771746));
#146836=CARTESIAN_POINT('Ctrl Pts',(-59.1745444884326,-5.16400295101772,
-176.584424539694));
#146837=CARTESIAN_POINT('Ctrl Pts',(-59.0739603306682,-5.16322437006847,
-176.685107962755));
#146838=CARTESIAN_POINT('Ctrl Pts',(-58.757290323262,-5.16109646218508,
-176.960219742078));
#146839=CARTESIAN_POINT('Ctrl Pts',(-58.5191843003194,-5.15989943361415,
-177.114893703118));
#146840=CARTESIAN_POINT('Ctrl Pts',(-58.267019098174,-5.15898893607586,
-177.232518219478));
#146841=CARTESIAN_POINT('Ctrl Pts',(-58.6082745331212,-5.6800000199515,
-176.427328712824));
#146842=CARTESIAN_POINT('Ctrl Pts',(-58.5950348472832,-5.67999973335255,
-176.465341940165));
#146843=CARTESIAN_POINT('Ctrl Pts',(-58.5820378685848,-5.67873096779289,
-176.502404330564));
#146844=CARTESIAN_POINT('Ctrl Pts',(-58.5692957758333,-5.6761247427438,
-176.538599126011));
#146845=CARTESIAN_POINT('Ctrl Pts',(-58.5575251017621,-5.67371720842369,
-176.572034539534));
#146846=CARTESIAN_POINT('Ctrl Pts',(-58.5459718188596,-5.67016847694687,
-176.604730379523));
#146847=CARTESIAN_POINT('Ctrl Pts',(-58.5346113579762,-5.66540164772652,
-176.636740993982));
#146848=CARTESIAN_POINT('Ctrl Pts',(-58.5234535848567,-5.66071986593212,
-176.668180490779));
#146849=CARTESIAN_POINT('Ctrl Pts',(-58.5124820659697,-5.65486292007998,
-176.698960019499));
#146850=CARTESIAN_POINT('Ctrl Pts',(-58.5016375963336,-5.64773536444049,
-176.729106516791));
#146851=CARTESIAN_POINT('Ctrl Pts',(-58.4887024183243,-5.63923368533013,
-176.765064965835));
#146852=CARTESIAN_POINT('Ctrl Pts',(-58.4761091181577,-5.62901675142965,
-176.799703323515));
#146853=CARTESIAN_POINT('Ctrl Pts',(-58.4638764455671,-5.61705712797886,
-176.832892052454));
#146854=CARTESIAN_POINT('Ctrl Pts',(-58.4526854472824,-5.60611592731065,
-176.863254592272));
#146855=CARTESIAN_POINT('Ctrl Pts',(-58.4417961169189,-5.5937155379102,
-176.892404008976));
#146856=CARTESIAN_POINT('Ctrl Pts',(-58.4311972672537,-5.57985231740509,
-176.920211869705));
#146857=CARTESIAN_POINT('Ctrl Pts',(-58.4230739091552,-5.56922702238551,
-176.941524862887));
#146858=CARTESIAN_POINT('Ctrl Pts',(-58.4151206678837,-5.55774254710736,
-176.962049198181));
#146859=CARTESIAN_POINT('Ctrl Pts',(-58.4073220826608,-5.54540973774009,
-176.981713767982));
#146860=CARTESIAN_POINT('Ctrl Pts',(-58.3980439115344,-5.53073708718778,
-177.005109196579));
#146861=CARTESIAN_POINT('Ctrl Pts',(-58.3890004170057,-5.51486733758817,
-177.027269841537));
#146862=CARTESIAN_POINT('Ctrl Pts',(-58.380218810449,-5.49787963522563,
-177.048004584116));
#146863=CARTESIAN_POINT('Ctrl Pts',(-58.3716510587059,-5.48130562731634,
-177.06823438213));
#146864=CARTESIAN_POINT('Ctrl Pts',(-58.3633324493104,-5.46366723978173,
-177.08710603058));
#146865=CARTESIAN_POINT('Ctrl Pts',(-58.3552874425923,-5.44508712768701,
-177.104443177883));
#146866=CARTESIAN_POINT('Ctrl Pts',(-58.3474557388646,-5.42699964333175,
-177.121320653057));
#146867=CARTESIAN_POINT('Ctrl Pts',(-58.3398831703244,-5.40801984922685,
-177.136743017005));
#146868=CARTESIAN_POINT('Ctrl Pts',(-58.3325937137739,-5.38830856612735,
-177.150561531819));
#146869=CARTESIAN_POINT('Ctrl Pts',(-58.3309779449681,-5.38393939592455,
-177.153624520812));
#146870=CARTESIAN_POINT('Ctrl Pts',(-58.3293760968208,-5.37953446911859,
-177.156608794961));
#146871=CARTESIAN_POINT('Ctrl Pts',(-58.3277884517205,-5.37509584628772,
-177.159512900979));
#146872=CARTESIAN_POINT('Ctrl Pts',(-58.3210194032167,-5.35617143224425,
-177.171894783105));
#146873=CARTESIAN_POINT('Ctrl Pts',(-58.3144830662044,-5.33655034723311,
-177.182868588345));
#146874=CARTESIAN_POINT('Ctrl Pts',(-58.3082161502908,-5.31639591374794,
-177.192297826593));
#146875=CARTESIAN_POINT('Ctrl Pts',(-58.30204887787,-5.29656193424289,-177.201577140661));
#146876=CARTESIAN_POINT('Ctrl Pts',(-58.2961423730487,-5.27621189722801,
-177.209359719377));
#146877=CARTESIAN_POINT('Ctrl Pts',(-58.2905359191037,-5.25554184478381,
-177.215544429679));
#146878=CARTESIAN_POINT('Ctrl Pts',(-58.2850147109265,-5.23518607914303,
-177.221635101863));
#146879=CARTESIAN_POINT('Ctrl Pts',(-58.279784399567,-5.21452076912564,
-177.226175439045));
#146880=CARTESIAN_POINT('Ctrl Pts',(-58.2748885905143,-5.19376312460734,
-177.229108942955));
#146881=CARTESIAN_POINT('Ctrl Pts',(-58.2721582012751,-5.18218660097016,
-177.230744956007));
#146882=CARTESIAN_POINT('Ctrl Pts',(-58.2695319717949,-5.17058183724987,
-177.231881985786));
#146883=CARTESIAN_POINT('Ctrl Pts',(-58.2670184333942,-5.15898900219905,
-177.232516794804));
#146884=CARTESIAN_POINT('Origin',(-59.5,-5.18000001999999,-55.24995));
#146885=CARTESIAN_POINT('',(-60.,-5.18000001999999,-174.534521368494));
#146886=CARTESIAN_POINT('Origin',(-60.,-2.55003103885676E-14,0.));
#146887=CARTESIAN_POINT('',(-60.,-4.68000001999999,-174.488343624884));
#146888=CARTESIAN_POINT('',(-60.,-4.68000001999999,-58.1637190207452));
#146889=CARTESIAN_POINT('Ctrl Pts',(-60.,-5.18000001999999,-174.511260182694));
#146890=CARTESIAN_POINT('Ctrl Pts',(-60.,-5.01333573888012,-174.503547232447));
#146891=CARTESIAN_POINT('Ctrl Pts',(-60.,-4.84666961885575,-174.495891400547));
#146892=CARTESIAN_POINT('Ctrl Pts',(-60.,-4.68000001999999,-174.488343624884));
#146893=CARTESIAN_POINT('Origin',(-59.5,-4.68000001999999,-55.24995));
#146894=CARTESIAN_POINT('Origin',(-59.5,-4.68000001999999,-174.488343624884));
#146895=CARTESIAN_POINT('Ctrl Pts',(-39.585730865631,-3.7824242910708,-98.7152302188737));
#146896=CARTESIAN_POINT('Ctrl Pts',(-39.6607823401664,-4.18000001999998,
-98.7511570311542));
#146897=CARTESIAN_POINT('Ctrl Pts',(-40.0271577790679,-4.18000001999998,
-98.926539349744));
#146898=CARTESIAN_POINT('Ctrl Pts',(-45.6152479999264,-3.76777550625849,
-86.1124074338642));
#146899=CARTESIAN_POINT('Ctrl Pts',(-45.7555532717617,-4.18000001999998,
-85.989998533184));
#146900=CARTESIAN_POINT('Ctrl Pts',(-46.0600623067188,-4.18000001999998,
-86.3237407210712));
#146901=CARTESIAN_POINT('Ctrl Pts',(-51.5953561718106,-3.75882512748543,
-73.4851842533606));
#146902=CARTESIAN_POINT('Ctrl Pts',(-51.6938180895878,-4.18000002,-73.4342549076826));
#146903=CARTESIAN_POINT('Ctrl Pts',(-52.0416537250564,-4.18000001999999,
-73.6965087765536));
#146904=CARTESIAN_POINT('Ctrl Pts',(-57.5607154366947,-3.75164060643487,
-60.8508735991007));
#146905=CARTESIAN_POINT('Ctrl Pts',(-57.6167925372613,-4.18000001999999,
-60.8773558160983));
#146906=CARTESIAN_POINT('Ctrl Pts',(-58.0081705490647,-4.18000001999999,
-61.0621827299711));
#146907=CARTESIAN_POINT('Origin',(-40.0271577790679,-3.68000001999999,-98.926539349744));
#146908=CARTESIAN_POINT('Ctrl Pts',(-59.5,-4.18000001999999,-174.488343624884));
#146909=CARTESIAN_POINT('Ctrl Pts',(-60.,-4.18000002,-174.488343624884));
#146910=CARTESIAN_POINT('Ctrl Pts',(-60.,-4.68000001999999,-174.488343624884));
#146911=CARTESIAN_POINT('Ctrl Pts',(-59.499999993334,-4.18000001999999,
-174.734541991424));
#146912=CARTESIAN_POINT('Ctrl Pts',(-59.9977796185047,-4.18000001999829,
-174.78302738694));
#146913=CARTESIAN_POINT('Ctrl Pts',(-60.,-4.67777472283721,-174.78368089075));
#146914=CARTESIAN_POINT('Ctrl Pts',(-59.4644630183961,-4.18000001999999,
-174.974786360247));
#146915=CARTESIAN_POINT('Ctrl Pts',(-59.9531694408477,-4.18000002000085,
-175.070632089297));
#146916=CARTESIAN_POINT('Ctrl Pts',(-59.9573556192874,-4.67559899657361,
-175.071875505894));
#146917=CARTESIAN_POINT('Ctrl Pts',(-59.3588972809293,-4.18000001999999,
-175.326182058073));
#146918=CARTESIAN_POINT('Ctrl Pts',(-59.8236519200077,-4.18000001999958,
-175.490806712526));
#146919=CARTESIAN_POINT('Ctrl Pts',(-59.8306767385091,-4.67241126250759,
-175.493405719049));
#146920=CARTESIAN_POINT('Ctrl Pts',(-59.3147195516479,-4.18000001999999,
-175.441607525732));
#146921=CARTESIAN_POINT('Ctrl Pts',(-59.7698424718428,-4.18000001999956,
-175.628550598836));
#146922=CARTESIAN_POINT('Ctrl Pts',(-59.7776634626824,-4.67136322522169,
-175.631868709625));
#146923=CARTESIAN_POINT('Ctrl Pts',(-59.2114199113778,-4.18000001999999,
-175.661895244315));
#146924=CARTESIAN_POINT('Ctrl Pts',(-59.6445293525488,-4.18000002000041,
-175.891155901683));
#146925=CARTESIAN_POINT('Ctrl Pts',(-59.6537038929485,-4.66936150715186,
-175.896123076728));
#146926=CARTESIAN_POINT('Ctrl Pts',(-59.1520385607459,-4.18000001999999,
-175.767754281813));
#146927=CARTESIAN_POINT('Ctrl Pts',(-59.5727342923808,-4.18000002000089,
-176.017245435328));
#146928=CARTESIAN_POINT('Ctrl Pts',(-59.5824462721252,-4.66839878682381,
-176.023110187492));
#146929=CARTESIAN_POINT('Ctrl Pts',(-59.0177715691528,-4.18000001999999,
-175.970879863896));
#146930=CARTESIAN_POINT('Ctrl Pts',(-59.4108028292072,-4.1800000199991,
-176.258951716569));
#146931=CARTESIAN_POINT('Ctrl Pts',(-59.4213258837533,-4.66655021592386,
-176.266776880891));
#146932=CARTESIAN_POINT('Ctrl Pts',(-58.9421612688066,-4.18000001999999,
-176.06886452411));
#146933=CARTESIAN_POINT('Ctrl Pts',(-59.3198146755637,-4.18000001999915,
-176.37546218739));
#146934=CARTESIAN_POINT('Ctrl Pts',(-59.3305935235461,-4.66565781609966,
-176.3843179035));
#146935=CARTESIAN_POINT('Ctrl Pts',(-58.7790852805764,-4.18000001999999,
-176.250769420981));
#146936=CARTESIAN_POINT('Ctrl Pts',(-59.1239216856836,-4.18000002000084,
-176.591561815318));
#146937=CARTESIAN_POINT('Ctrl Pts',(-59.1349023357136,-4.66400011582949,
-176.602528392516));
#146938=CARTESIAN_POINT('Ctrl Pts',(-58.6915944853457,-4.18000001999999,
-176.33503132506));
#146939=CARTESIAN_POINT('Ctrl Pts',(-59.0189867750955,-4.18000001999871,
-176.691604703902));
#146940=CARTESIAN_POINT('Ctrl Pts',(-59.0299133821615,-4.66323171680632,
-176.703607721972));
#146941=CARTESIAN_POINT('Ctrl Pts',(-58.4115655020993,-4.18000001999999,
-176.56808461344));
#146942=CARTESIAN_POINT('Ctrl Pts',(-58.6838036746477,-4.18000002000249,
-176.967887143763));
#146943=CARTESIAN_POINT('Ctrl Pts',(-58.6938786030259,-4.66110543474911,
-176.983174915482));
#146944=CARTESIAN_POINT('Ctrl Pts',(-58.1982641486948,-4.18000001999999,
-176.698056997615));
#146945=CARTESIAN_POINT('Ctrl Pts',(-58.4288067817606,-4.18000002000125,
-177.121996578829));
#146946=CARTESIAN_POINT('Ctrl Pts',(-58.437917085704,-4.65991812350376,
-177.139087667033));
#146947=CARTESIAN_POINT('Ctrl Pts',(-57.9753315069797,-4.18000001999999,
-176.792613205276));
#146948=CARTESIAN_POINT('Ctrl Pts',(-58.1625546348518,-4.18000002,-177.234024164027));
#146949=CARTESIAN_POINT('Ctrl Pts',(-58.1703978083756,-4.65905396057624,
-177.252515804372));
#146950=CARTESIAN_POINT('',(-58.2078173720072,-4.65917712473139,-177.236349008097));
#146951=CARTESIAN_POINT('Ctrl Pts',(-58.2078173720829,-4.65917712520045,
-177.236349008084));
#146952=CARTESIAN_POINT('Ctrl Pts',(-58.4617634457135,-4.66002956379037,
-177.124453281026));
#146953=CARTESIAN_POINT('Ctrl Pts',(-58.7043445390845,-4.66117165864448,
-176.974467684704));
#146954=CARTESIAN_POINT('Ctrl Pts',(-59.0299133821615,-4.66323171680632,
-176.703607721972));
#146955=CARTESIAN_POINT('Ctrl Pts',(-59.1349023357136,-4.66400011582949,
-176.602528392516));
#146956=CARTESIAN_POINT('Ctrl Pts',(-59.3305935235461,-4.66565781609966,
-176.3843179035));
#146957=CARTESIAN_POINT('Ctrl Pts',(-59.4213258837533,-4.66655021592386,
-176.266776880891));
#146958=CARTESIAN_POINT('Ctrl Pts',(-59.5824462721252,-4.66839878682381,
-176.023110187492));
#146959=CARTESIAN_POINT('Ctrl Pts',(-59.6537038929485,-4.66936150715186,
-175.896123076728));
#146960=CARTESIAN_POINT('Ctrl Pts',(-59.7776634626824,-4.67136322522169,
-175.631868709625));
#146961=CARTESIAN_POINT('Ctrl Pts',(-59.8306767385091,-4.67241126250759,
-175.493405719049));
#146962=CARTESIAN_POINT('Ctrl Pts',(-59.9573556192874,-4.67559899657361,
-175.071875505894));
#146963=CARTESIAN_POINT('Ctrl Pts',(-60.,-4.67777472283721,-174.78368089075));
#146964=CARTESIAN_POINT('Ctrl Pts',(-60.,-4.68000001999999,-174.488343624884));
#146965=CARTESIAN_POINT('Ctrl Pts',(-58.2078173720829,-4.65917712520045,
-177.236349008084));
#146966=CARTESIAN_POINT('Ctrl Pts',(-58.1766173277935,-4.52496538336098,
-177.243973427637));
#146967=CARTESIAN_POINT('Ctrl Pts',(-58.1596733704946,-4.39698767568444,
-177.184652644663));
#146968=CARTESIAN_POINT('Ctrl Pts',(-58.1740867503666,-4.22134717274183,
-176.965019674666));
#146969=CARTESIAN_POINT('Ctrl Pts',(-58.2063099446428,-4.18000001999999,
-176.814456128226));
#146970=CARTESIAN_POINT('Ctrl Pts',(-58.2644174754153,-4.18000001999999,
-176.647241333324));
#146971=CARTESIAN_POINT('Origin',(-58.2644174754153,-3.68000001999999,-179.64995));
#146972=CARTESIAN_POINT('Origin',(-58.2644174754153,-3.68000001999999,-176.647241333324));
#146973=CARTESIAN_POINT('Origin',(-58.2644174754153,-3.68000001999999,-171.871644662643));
#146974=CARTESIAN_POINT('Ctrl Pts',(-57.7706512256236,-3.75870764711888,
-171.871644662643));
#146975=CARTESIAN_POINT('Ctrl Pts',(-57.8378063278745,-4.18000001999999,
-171.871644662643));
#146976=CARTESIAN_POINT('Ctrl Pts',(-58.2644174754153,-4.18000001999999,
-171.871644662643));
#146977=CARTESIAN_POINT('Ctrl Pts',(-57.7706512252069,-3.75870764450445,
-171.725685252419));
#146978=CARTESIAN_POINT('Ctrl Pts',(-57.8378063150439,-4.18000001999999,
-171.715730578987));
#146979=CARTESIAN_POINT('Ctrl Pts',(-58.2644174584531,-4.18000001999999,
-171.652701076652));
#146980=CARTESIAN_POINT('Ctrl Pts',(-57.7383541282856,-3.7562957918519,
-171.582363368286));
#146981=CARTESIAN_POINT('Ctrl Pts',(-57.801183875227,-4.18000002000114,
-171.562158552623));
#146982=CARTESIAN_POINT('Ctrl Pts',(-58.2165506240601,-4.18000001999999,
-171.437728673605));
#146983=CARTESIAN_POINT('Ctrl Pts',(-57.6746235421417,-3.75150367745622,
-171.449026400902));
#146984=CARTESIAN_POINT('Ctrl Pts',(-57.7306096110337,-4.18000001999999,
-171.422588467367));
#146985=CARTESIAN_POINT('Ctrl Pts',(-58.1221005562789,-4.18000001999999,
-171.237717270032));
#146986=CARTESIAN_POINT('',(-57.6746235421417,-3.75150367745622,-171.449026400902));
#146987=CARTESIAN_POINT('Origin',(-58.1221005562789,-3.68000001999999,-171.237717270032));
#146988=CARTESIAN_POINT('Origin',(-56.7293330762435,-3.67954981718445,-171.875507808352));
#146989=CARTESIAN_POINT('Ctrl Pts',(-57.6746235421417,-3.75150367745622,
-171.449026400902));
#146990=CARTESIAN_POINT('Ctrl Pts',(-57.7306096110337,-4.18000001999999,
-171.422588467367));
#146991=CARTESIAN_POINT('Ctrl Pts',(-58.1221005562789,-4.18000001999999,
-171.237717270032));
#146992=CARTESIAN_POINT('Ctrl Pts',(-51.6715280616305,-3.75870638021677,
-158.734184170827));
#146993=CARTESIAN_POINT('Ctrl Pts',(-51.7702631771107,-4.18000001999999,
-158.785894332693));
#146994=CARTESIAN_POINT('Ctrl Pts',(-52.1178467328245,-4.18000001999999,
-158.52285936551));
#146995=CARTESIAN_POINT('Ctrl Pts',(-45.6536266465224,-3.76768226491552,
-146.026454114168));
#146996=CARTESIAN_POINT('Ctrl Pts',(-45.7948164697718,-4.18000001999998,
-146.15085325192));
#146997=CARTESIAN_POINT('Ctrl Pts',(-46.0984623496487,-4.18000001999998,
-145.815120328436));
#146998=CARTESIAN_POINT('Ctrl Pts',(-39.5857308656265,-3.78242429107081,
-133.343412752623));
#146999=CARTESIAN_POINT('Ctrl Pts',(-39.660782340162,-4.18000001999998,
-133.307485940342));
#147000=CARTESIAN_POINT('Ctrl Pts',(-40.0271577790634,-4.18000001999998,
-133.132103621752));
#147001=CARTESIAN_POINT('',(-39.5857307322485,-3.78242358451346,-133.343412816471));
#147002=CARTESIAN_POINT('Origin',(-40.0271577790634,-3.68000001999999,-133.132103621752));
#147003=CARTESIAN_POINT('Ctrl Pts',(-39.5857308656309,-3.78242429107441,
-133.34341275263));
#147004=CARTESIAN_POINT('Ctrl Pts',(-45.6536266516538,-3.7676822799009,
-146.026454118689));
#147005=CARTESIAN_POINT('Ctrl Pts',(-51.6715280651912,-3.75870639540982,
-158.734184172691));
#147006=CARTESIAN_POINT('Ctrl Pts',(-57.6746235421417,-3.75150367745622,
-171.449026400902));
#147007=CARTESIAN_POINT('Ctrl Pts',(-39.5000746910952,-4.18000001999998,
-130.774156597103));
#147008=CARTESIAN_POINT('Ctrl Pts',(-38.9988856571825,-4.18000001999998,
-130.771495097562));
#147009=CARTESIAN_POINT('Ctrl Pts',(-39.0000830375701,-3.67880541495414,
-130.771501481495));
#147010=CARTESIAN_POINT('Ctrl Pts',(-39.4979098764889,-4.18000001999998,
-131.188377903755));
#147011=CARTESIAN_POINT('Ctrl Pts',(-39.0133259194552,-4.18000001999998,
-131.216802997827));
#147012=CARTESIAN_POINT('Ctrl Pts',(-38.9976770037577,-3.69581922809734,
-131.224220780693));
#147013=CARTESIAN_POINT('Ctrl Pts',(-39.5428199578347,-4.18000001999998,
-131.594670912653));
#147014=CARTESIAN_POINT('Ctrl Pts',(-39.0772732138211,-4.18000001999999,
-131.657324358274));
#147015=CARTESIAN_POINT('Ctrl Pts',(-39.0475765097186,-3.71311681177937,
-131.667826133903));
#147016=CARTESIAN_POINT('Ctrl Pts',(-39.7223936198539,-4.18000001999998,
-132.391873207535));
#147017=CARTESIAN_POINT('Ctrl Pts',(-39.3031001496673,-4.18000001999998,
-132.514074181288));
#147018=CARTESIAN_POINT('Ctrl Pts',(-39.247101643641,-3.74820970445091,
-132.537336227375));
#147019=CARTESIAN_POINT('Ctrl Pts',(-39.8587693570671,-4.18000001999998,
-132.785389893012));
#147020=CARTESIAN_POINT('Ctrl Pts',(-39.4640070783496,-4.18000001999999,
-132.934381121693));
#147021=CARTESIAN_POINT('Ctrl Pts',(-39.3986305924887,-3.76613472203319,
-132.966073941729));
#147022=CARTESIAN_POINT('Ctrl Pts',(-40.0395629979198,-4.18000001999998,
-133.157837806796));
#147023=CARTESIAN_POINT('Ctrl Pts',(-39.6750481329511,-4.18000001999998,
-133.334759037945));
#147024=CARTESIAN_POINT('Ctrl Pts',(-39.5995110806651,-3.78361375906165,
-133.371422516669));
#147025=CARTESIAN_POINT('',(-39.,-3.68000001999998,-130.802732351058));
#147026=CARTESIAN_POINT('Origin',(-39.5,-3.68000001999999,-130.802732351058));
#147027=CARTESIAN_POINT('Ctrl Pts',(-39.,-3.68000001999998,-130.802732351058));
#147028=CARTESIAN_POINT('Ctrl Pts',(-39.0000000012333,-3.68447440683702,
-130.921592018194));
#147029=CARTESIAN_POINT('Ctrl Pts',(-39.0036588240764,-3.68897484526234,
-131.039838409487));
#147030=CARTESIAN_POINT('Ctrl Pts',(-39.0108684419194,-3.69349116787911,
-131.157453391765));
#147031=CARTESIAN_POINT('Ctrl Pts',(-39.018143549427,-3.698048515202,-131.276136747693));
#147032=CARTESIAN_POINT('Ctrl Pts',(-39.0290338743149,-3.70262240489881,
-131.394178091007));
#147033=CARTESIAN_POINT('Ctrl Pts',(-39.0434756876213,-3.70721214335521,
-131.51158216155));
#147034=CARTESIAN_POINT('Ctrl Pts',(-39.0580054854929,-3.71182984409958,
-131.629701498652));
#147035=CARTESIAN_POINT('Ctrl Pts',(-39.0761300225471,-3.71646401900972,
-131.747176766763));
#147036=CARTESIAN_POINT('Ctrl Pts',(-39.0978360495535,-3.72111772532618,
-131.864021839488));
#147037=CARTESIAN_POINT('Ctrl Pts',(-39.1126626346933,-3.72429650018426,
-131.943834391939));
#147038=CARTESIAN_POINT('Ctrl Pts',(-39.1291613559977,-3.72748446873514,
-132.023353094883));
#147039=CARTESIAN_POINT('Ctrl Pts',(-39.1473419267964,-3.73068197101817,
-132.102581139799));
#147040=CARTESIAN_POINT('Ctrl Pts',(-39.1767331515572,-3.73585114360985,
-132.230663437175));
#147041=CARTESIAN_POINT('Ctrl Pts',(-39.2105770847552,-3.74103515521041,
-132.358219146246));
#147042=CARTESIAN_POINT('Ctrl Pts',(-39.2488673046334,-3.74623841689841,
-132.484810818648));
#147043=CARTESIAN_POINT('Ctrl Pts',(-39.2868385612724,-3.75139833464094,
-132.610347963549));
#147044=CARTESIAN_POINT('Ctrl Pts',(-39.3291826030354,-3.75657694721291,
-132.734936713211));
#147045=CARTESIAN_POINT('Ctrl Pts',(-39.3758480040126,-3.76175604867458,
-132.858142986391));
#147046=CARTESIAN_POINT('Ctrl Pts',(-39.4220236042586,-3.76688079021157,
-132.980056084726));
#147047=CARTESIAN_POINT('Ctrl Pts',(-39.4724305009679,-3.77200571552313,
-133.100615173967));
#147048=CARTESIAN_POINT('Ctrl Pts',(-39.5269712029935,-3.77709501234611,
-133.219397957436));
#147049=CARTESIAN_POINT('Ctrl Pts',(-39.5460539232582,-3.77887565733251,
-133.260957720053));
#147050=CARTESIAN_POINT('Ctrl Pts',(-39.565642246535,-3.78065179793913,
-133.302300046887));
#147051=CARTESIAN_POINT('Ctrl Pts',(-39.5857305461208,-3.78242147649458,
-133.343406945925));
#147052=CARTESIAN_POINT('Origin',(-39.5,-3.68000001999999,-55.24995));
#147053=CARTESIAN_POINT('',(-39.,-3.68000001999999,-101.255910620448));
#147054=CARTESIAN_POINT('Origin',(-39.5,-3.68000001999999,-101.255910620448));
#147055=CARTESIAN_POINT('',(-39.,-3.68000001999999,-129.34995));
#147056=CARTESIAN_POINT('Ctrl Pts',(-40.0271577790679,-4.18000001999998,
-98.926539349744));
#147057=CARTESIAN_POINT('Ctrl Pts',(-39.6607823401664,-4.18000001999998,
-98.7511570311542));
#147058=CARTESIAN_POINT('Ctrl Pts',(-39.585730865631,-3.7824242910708,-98.7152302188737));
#147059=CARTESIAN_POINT('Ctrl Pts',(-39.8525718691684,-4.18000001999998,
-99.2912510907428));
#147060=CARTESIAN_POINT('Ctrl Pts',(-39.4568105653931,-4.18000001999998,
-99.1432082613171));
#147061=CARTESIAN_POINT('Ctrl Pts',(-39.3917487041449,-3.76533335821317,
-99.1121767214752));
#147062=CARTESIAN_POINT('Ctrl Pts',(-39.7225112880865,-4.18000001999998,
-99.6687555669174));
#147063=CARTESIAN_POINT('Ctrl Pts',(-39.3032261512475,-4.18000001999998,
-99.546440425348));
#147064=CARTESIAN_POINT('Ctrl Pts',(-39.247234764848,-3.74814762956703,
-99.5234791492765));
#147065=CARTESIAN_POINT('Ctrl Pts',(-39.5459737882558,-4.18000001999998,
-100.447508896771));
#147066=CARTESIAN_POINT('Ctrl Pts',(-39.0814385609748,-4.18000001999998,
-100.383271856169));
#147067=CARTESIAN_POINT('Ctrl Pts',(-39.0510819866434,-3.71385382853417,
-100.372855479779));
#147068=CARTESIAN_POINT('Ctrl Pts',(-39.5000000005413,-4.18000001999998,
-100.851700064103));
#147069=CARTESIAN_POINT('Ctrl Pts',(-39.0163583103527,-4.18000001999998,
-100.821360983603));
#147070=CARTESIAN_POINT('Ctrl Pts',(-39.,-3.69662981211624,-100.814149183564));
#147071=CARTESIAN_POINT('Ctrl Pts',(-39.5,-4.18000001999998,-101.255910620448));
#147072=CARTESIAN_POINT('Ctrl Pts',(-39.,-4.18000001999998,-101.255910620448));
#147073=CARTESIAN_POINT('Ctrl Pts',(-39.,-3.68000001999999,-101.255910620448));
#147074=CARTESIAN_POINT('Ctrl Pts',(-39.585730865631,-3.78242429107081,
-98.7152302188737));
#147075=CARTESIAN_POINT('Ctrl Pts',(-39.3917487041449,-3.76533335821317,
-99.1121767214752));
#147076=CARTESIAN_POINT('Ctrl Pts',(-39.247234764848,-3.74814762956703,
-99.5234791492765));
#147077=CARTESIAN_POINT('Ctrl Pts',(-39.0510819866434,-3.71385382853417,
-100.372855479779));
#147078=CARTESIAN_POINT('Ctrl Pts',(-39.,-3.69662981211624,-100.814149183564));
#147079=CARTESIAN_POINT('Ctrl Pts',(-39.,-3.68000001999999,-101.255910620448));
#147080=CARTESIAN_POINT('Ctrl Pts',(-39.7537575098556,1.84791950156463,
-94.88221628274));
#147081=CARTESIAN_POINT('Ctrl Pts',(-39.,2.57466119081605,-95.8526318986117));
#147082=CARTESIAN_POINT('Ctrl Pts',(-39.,3.43040799630139,-96.9953075914435));
#147083=CARTESIAN_POINT('Ctrl Pts',(-39.7190124561908,0.840911054897691,
-95.7061821932407));
#147084=CARTESIAN_POINT('Ctrl Pts',(-38.999999999981,1.53000629023279,-96.6793461871002));
#147085=CARTESIAN_POINT('Ctrl Pts',(-39.,2.33014533501219,-97.8192913905431));
#147086=CARTESIAN_POINT('Ctrl Pts',(-39.6851659166312,-0.199330185460902,
-96.4883583800562));
#147087=CARTESIAN_POINT('Ctrl Pts',(-39.,0.446335000557117,-97.4659519416263));
#147088=CARTESIAN_POINT('Ctrl Pts',(-39.,1.18987438490308,-98.6014496888564));
#147089=CARTESIAN_POINT('Ctrl Pts',(-39.6371406048982,-1.82970860306462,
-97.5751506494424));
#147090=CARTESIAN_POINT('Ctrl Pts',(-39.,-1.25780287903679,-98.559490287645));
#147091=CARTESIAN_POINT('Ctrl Pts',(-39.,-0.603530653465397,-99.6882419580977));
#147092=CARTESIAN_POINT('Ctrl Pts',(-39.6215565252267,-2.38668519024414,
-97.9237506811802));
#147093=CARTESIAN_POINT('Ctrl Pts',(-39.0000000000024,-1.8401867654384,
-98.9100191480635));
#147094=CARTESIAN_POINT('Ctrl Pts',(-39.,-1.21720470538169,-100.036841989918));
#147095=CARTESIAN_POINT('Ctrl Pts',(-39.5921016697827,-3.5111206545489,
-98.5763198411428));
#147096=CARTESIAN_POINT('Ctrl Pts',(-38.9999999999976,-3.01722910704029,
-99.5661158351118));
#147097=CARTESIAN_POINT('Ctrl Pts',(-39.,-2.45808495944723,-100.689411149812));
#147098=CARTESIAN_POINT('Ctrl Pts',(-39.5781805091624,-4.08013436254483,
-98.8814533069127));
#147099=CARTESIAN_POINT('Ctrl Pts',(-38.9999999999927,-3.61357659227868,
-99.872970636237));
#147100=CARTESIAN_POINT('Ctrl Pts',(-39.,-3.08699664896505,-100.99454469153));
#147101=CARTESIAN_POINT('Ctrl Pts',(-39.5652360655961,-4.65691592725724,
-99.1628818945567));
#147102=CARTESIAN_POINT('Ctrl Pts',(-39.,-4.21906349874734,-100.156129970618));
#147103=CARTESIAN_POINT('Ctrl Pts',(-39.,-3.72540427022208,-101.27597320326));
#147104=CARTESIAN_POINT('',(-39.0000000006157,1.96999998000003,-98.0457798926543));
#147105=CARTESIAN_POINT('Ctrl Pts',(-39.0000000024628,1.96999998000006,
-98.0457798926544));
#147106=CARTESIAN_POINT('Ctrl Pts',(-39.0000000032442,1.50691588072647,
-98.365026252185));
#147107=CARTESIAN_POINT('Ctrl Pts',(-39.0000000016551,1.03814546726177,
-98.6748799793953));
#147108=CARTESIAN_POINT('Ctrl Pts',(-39.0000000008071,0.562698589434805,
-98.9745405549415));
#147109=CARTESIAN_POINT('Ctrl Pts',(-39.0000000004711,0.374284444265228,
-99.0932926044673));
#147110=CARTESIAN_POINT('Ctrl Pts',(-39.0000000002453,0.184822272632785,
-99.2104442275566));
#147111=CARTESIAN_POINT('Ctrl Pts',(-39.0000000001311,-0.00574774121677549,
-99.3259468990427));
#147112=CARTESIAN_POINT('Ctrl Pts',(-38.9999999999777,-0.26189475793881,
-99.4811951677863));
#147113=CARTESIAN_POINT('Ctrl Pts',(-39.,-0.520415976845914,-99.6335997492721));
#147114=CARTESIAN_POINT('Ctrl Pts',(-39.,-0.780592906922155,-99.7825242060483));
#147115=CARTESIAN_POINT('Ctrl Pts',(-39.,-1.12946683952906,-99.9822185482085));
#147116=CARTESIAN_POINT('Ctrl Pts',(-39.,-1.48228932648713,-100.176247523887));
#147117=CARTESIAN_POINT('Ctrl Pts',(-39.,-1.83764512720227,-100.363126009317));
#147118=CARTESIAN_POINT('Ctrl Pts',(-39.0000000000001,-2.17904755464651,
-100.542666538653));
#147119=CARTESIAN_POINT('Ctrl Pts',(-39.0000000000001,-2.52330369642182,
-100.715959269877));
#147120=CARTESIAN_POINT('Ctrl Pts',(-39.0000000000001,-2.87085998622629,
-100.882657599431));
#147121=CARTESIAN_POINT('Ctrl Pts',(-39.0000000000001,-3.13854475842017,
-101.011047174533));
#147122=CARTESIAN_POINT('Ctrl Pts',(-39.,-3.40818747901881,-101.135524193408));
#147123=CARTESIAN_POINT('Ctrl Pts',(-39.,-3.68000001999998,-101.255910620448));
#147124=CARTESIAN_POINT('Ctrl Pts',(-39.,1.96999998000002,-98.0457798926543));
#147125=CARTESIAN_POINT('Ctrl Pts',(-38.9999999999933,1.94361525900156,
-97.4993505936098));
#147126=CARTESIAN_POINT('Ctrl Pts',(-39.0635968999836,1.91714776127833,
-96.9640681661433));
#147127=CARTESIAN_POINT('Ctrl Pts',(-39.3128539180174,1.86422808137617,
-95.9152577284781));
#147128=CARTESIAN_POINT('Ctrl Pts',(-39.5010226635731,1.83757264806834,
-95.3979932721565));
#147129=CARTESIAN_POINT('Ctrl Pts',(-39.7525219240432,1.8120830678168,-94.9115092131337));
#147130=CARTESIAN_POINT('Ctrl Pts',(-56.377904566775,1.85477723331148,-60.8508735991007));
#147131=CARTESIAN_POINT('Ctrl Pts',(-56.246666128119,2.46999998000001,-60.7875964218516));
#147132=CARTESIAN_POINT('Ctrl Pts',(-56.8161649572467,2.46999998000001,
-61.0621827299711));
#147133=CARTESIAN_POINT('Ctrl Pts',(-53.635317996248,1.84957228639176,-66.5419044818116));
#147134=CARTESIAN_POINT('Ctrl Pts',(-53.4780298924679,2.46999998009932,
-66.5137036410044));
#147135=CARTESIAN_POINT('Ctrl Pts',(-54.072208955501,2.46999998000001,-66.753215691109));
#147136=CARTESIAN_POINT('Ctrl Pts',(-50.8828928487864,1.84368306851814,
-72.2280037103763));
#147137=CARTESIAN_POINT('Ctrl Pts',(-50.7098482191461,2.46999998,-72.2098982919583));
#147138=CARTESIAN_POINT('Ctrl Pts',(-51.318146010607,2.46999998000001,-72.4393128412535));
#147139=CARTESIAN_POINT('Ctrl Pts',(-45.3466144966389,1.82978958392005,
-83.5843555039948));
#147140=CARTESIAN_POINT('Ctrl Pts',(-45.1522541442582,2.46999998,-83.5563536764924));
#147141=CARTESIAN_POINT('Ctrl Pts',(-45.7775928276463,2.46999998000002,
-83.7956646348582));
#147142=CARTESIAN_POINT('Ctrl Pts',(-42.5630938966436,1.8218009521478,-89.2547782578028));
#147143=CARTESIAN_POINT('Ctrl Pts',(-42.3434811549778,2.46999997991896,
-89.2449404232873));
#147144=CARTESIAN_POINT('Ctrl Pts',(-42.9914518100362,2.46999998000002,
-89.4660932271532));
#147145=CARTESIAN_POINT('Ctrl Pts',(-39.7525219240432,1.81208306781681,
-94.9115092131337));
#147146=CARTESIAN_POINT('Ctrl Pts',(-39.5564442323333,2.46999998000002,
-94.8139619018177));
#147147=CARTESIAN_POINT('Ctrl Pts',(-40.1772697316389,2.46999998000002,
-95.1228183440041));
#147148=CARTESIAN_POINT('Origin',(-40.1772697316389,1.96999998000002,-95.1228183440041));
#147149=CARTESIAN_POINT('Ctrl Pts',(-39.5,2.46999998000002,-98.0457798926543));
#147150=CARTESIAN_POINT('Ctrl Pts',(-39.,2.46999998000002,-98.0457798926543));
#147151=CARTESIAN_POINT('Ctrl Pts',(-39.,1.96999998000002,-98.0457798926543));
#147152=CARTESIAN_POINT('Ctrl Pts',(-39.5000000026568,2.46999998000002,
-97.5376233160284));
#147153=CARTESIAN_POINT('Ctrl Pts',(-38.9728980858888,2.46999998000002,
-97.4844974242186));
#147154=CARTESIAN_POINT('Ctrl Pts',(-39.,1.9436152588707,-97.4993505936135));
#147155=CARTESIAN_POINT('Ctrl Pts',(-39.5572372093883,2.46999998000002,
-97.0390962063516));
#147156=CARTESIAN_POINT('Ctrl Pts',(-39.0092761144151,2.46999998000002,
-96.9417291681898));
#147157=CARTESIAN_POINT('Ctrl Pts',(-39.0635968999967,1.91714776114478,
-96.9640681661487));
#147158=CARTESIAN_POINT('Ctrl Pts',(-39.7815685268491,2.46999998000002,
-96.0609362825129));
#147159=CARTESIAN_POINT('Ctrl Pts',(-39.1914722350304,2.46999998000002,
-95.8620324116114));
#147160=CARTESIAN_POINT('Ctrl Pts',(-39.312853918045,1.86422808123875,-95.9152577284902));
#147161=CARTESIAN_POINT('Ctrl Pts',(-39.9509186646822,2.46999998000002,
-95.5778016189611));
#147162=CARTESIAN_POINT('Ctrl Pts',(-39.3474064560568,2.46999997999991,
-95.3191244694837));
#147163=CARTESIAN_POINT('Ctrl Pts',(-39.5010226636067,1.83757264792979,
-95.3979932721737));
#147164=CARTESIAN_POINT('Ctrl Pts',(-40.1772697316389,2.46999998000002,
-95.1228183440041));
#147165=CARTESIAN_POINT('Ctrl Pts',(-39.5564442323333,2.46999998000002,
-94.8139619018179));
#147166=CARTESIAN_POINT('Ctrl Pts',(-39.7525219240431,1.81208306781681,
-94.9115092131337));
#147167=CARTESIAN_POINT('Origin',(-39.5,1.96999998000002,-98.0457798926543));
#147168=CARTESIAN_POINT('Origin',(-39.5,1.96999998000002,-55.24995));
#147169=CARTESIAN_POINT('',(-39.0000000009311,1.96999998000004,-134.012863078852));
#147170=CARTESIAN_POINT('Origin',(-39.5,1.96999998000002,-134.012863078852));
#147171=CARTESIAN_POINT('',(-39.,1.96999998000002,-129.34995));
#147172=CARTESIAN_POINT('Ctrl Pts',(-40.2368360569361,2.46999998000002,
-137.052481127874));
#147173=CARTESIAN_POINT('Ctrl Pts',(-39.6136204540295,2.46999998000002,
-137.379413138382));
#147174=CARTESIAN_POINT('Ctrl Pts',(-39.8187349738493,1.80543983340093,
-137.271832963441));
#147175=CARTESIAN_POINT('Ctrl Pts',(-39.9798259099587,2.46999998000002,
-136.561879380276));
#147176=CARTESIAN_POINT('Ctrl Pts',(-39.3750396288604,2.46999997999999,
-136.834113716861));
#147177=CARTESIAN_POINT('Ctrl Pts',(-39.533173705558,1.83299741787672,-136.747405829844));
#147178=CARTESIAN_POINT('Ctrl Pts',(-39.7942596598039,2.46999998000002,
-136.049446128364));
#147179=CARTESIAN_POINT('Ctrl Pts',(-39.2024243343545,2.46999998000014,
-136.257081974912));
#147180=CARTESIAN_POINT('Ctrl Pts',(-39.3269752687565,1.86132354549721,
-136.198841734389));
#147181=CARTESIAN_POINT('Ctrl Pts',(-39.548909562734,2.46999998000002,-134.986769967065));
#147182=CARTESIAN_POINT('Ctrl Pts',(-39.002744048575,2.4699999799999,-135.08361190439));
#147183=CARTESIAN_POINT('Ctrl Pts',(-39.0543528686939,1.91883278031583,
-135.059436829036));
#147184=CARTESIAN_POINT('Ctrl Pts',(-39.4903493414456,2.46999998000002,
-134.432158073852));
#147185=CARTESIAN_POINT('Ctrl Pts',(-38.9670451935713,2.46999998000003,
-134.480163550531));
#147186=CARTESIAN_POINT('Ctrl Pts',(-38.9892810036075,1.94823440239765,
-134.463878808121));
#147187=CARTESIAN_POINT('Ctrl Pts',(-39.5012955382995,2.46999998000002,
-133.88255272146));
#147188=CARTESIAN_POINT('Ctrl Pts',(-39.0080109328159,2.46999998000002,
-133.872820118988));
#147189=CARTESIAN_POINT('Ctrl Pts',(-39.0014382726235,1.9766623627072,-133.872717663268));
#147190=CARTESIAN_POINT('',(-39.7525219025349,1.81208317107913,-137.147133709894));
#147191=CARTESIAN_POINT('Origin',(-40.1772697316389,1.96999998000002,-136.935824627502));
#147192=CARTESIAN_POINT('Ctrl Pts',(-39.7525219099498,1.81208323948034,
-137.14713352867));
#147193=CARTESIAN_POINT('Ctrl Pts',(-39.6968925343529,1.81772142131488,
-137.039526872226));
#147194=CARTESIAN_POINT('Ctrl Pts',(-39.6445718142832,1.8234260406068,-136.930881467314));
#147195=CARTESIAN_POINT('Ctrl Pts',(-39.5954328440081,1.82915287678578,
-136.821276650554));
#147196=CARTESIAN_POINT('Ctrl Pts',(-39.5448884088858,1.83504351100306,
-136.708536934625));
#147197=CARTESIAN_POINT('Ctrl Pts',(-39.4977095071828,1.84095797203305,
-136.594781798714));
#147198=CARTESIAN_POINT('Ctrl Pts',(-39.4537815356419,1.8468787701165,-136.48005817389));
#147199=CARTESIAN_POINT('Ctrl Pts',(-39.409336899226,1.8528692064804,-136.363985211385));
#147200=CARTESIAN_POINT('Ctrl Pts',(-39.3682194543804,1.85886662434155,
-136.246920256174));
#147201=CARTESIAN_POINT('Ctrl Pts',(-39.3303455734763,1.86487745082245,
-136.128879413488));
#147202=CARTESIAN_POINT('Ctrl Pts',(-39.2920753921181,1.87095117271324,
-136.009603428312));
#147203=CARTESIAN_POINT('Ctrl Pts',(-39.2571164969226,1.87703914799669,
-135.889330315293));
#147204=CARTESIAN_POINT('Ctrl Pts',(-39.2254271316397,1.88316486453392,
-135.768053582341));
#147205=CARTESIAN_POINT('Ctrl Pts',(-39.2133661623124,1.88549631164886,
-135.72189566964));
#147206=CARTESIAN_POINT('Ctrl Pts',(-39.2017792998293,1.88783335377127,
-135.675592196414));
#147207=CARTESIAN_POINT('Ctrl Pts',(-39.1906661181429,1.89017765116493,
-135.629142282584));
#147208=CARTESIAN_POINT('Ctrl Pts',(-39.1550653416186,1.89768754436866,
-135.480341241757));
#147209=CARTESIAN_POINT('Ctrl Pts',(-39.1242778288881,1.90525270160959,
-135.329794467711));
#147210=CARTESIAN_POINT('Ctrl Pts',(-39.0984708604229,1.91283024764293,
-135.178016532208));
#147211=CARTESIAN_POINT('Ctrl Pts',(-39.0728066063579,1.92036588929918,
-135.027077939654));
#147212=CARTESIAN_POINT('Ctrl Pts',(-39.0520680596019,1.92791344971714,
-134.87492201065));
#147213=CARTESIAN_POINT('Ctrl Pts',(-39.0363734628629,1.93543991782654,
-134.7220749885));
#147214=CARTESIAN_POINT('Ctrl Pts',(-39.0208096281387,1.94290367797656,
-134.570501435488));
#147215=CARTESIAN_POINT('Ctrl Pts',(-39.0102060825658,1.95034640301488,
-134.418248521206));
#147216=CARTESIAN_POINT('Ctrl Pts',(-39.0046315415482,1.95774958009969,
-134.265845522775));
#147217=CARTESIAN_POINT('Ctrl Pts',(-39.0015475992384,1.96184515872506,
-134.181533280117));
#147218=CARTESIAN_POINT('Ctrl Pts',(-39.000001959376,1.96592890236697,-134.097175367266));
#147219=CARTESIAN_POINT('Ctrl Pts',(-39.0000000018622,1.96999998000005,
-134.012863078852));
#147220=CARTESIAN_POINT('Ctrl Pts',(-39.7525219240432,1.81208306781681,
-137.147133758372));
#147221=CARTESIAN_POINT('Ctrl Pts',(-39.5564442323333,2.46999998000002,
-137.244681069688));
#147222=CARTESIAN_POINT('Ctrl Pts',(-40.1772697316389,2.46999998000002,
-136.935824627502));
#147223=CARTESIAN_POINT('Ctrl Pts',(-42.5829522730059,1.82186961480941,
-142.84383290998));
#147224=CARTESIAN_POINT('Ctrl Pts',(-42.3628976020159,2.46999998000001,
-142.852500243629));
#147225=CARTESIAN_POINT('Ctrl Pts',(-43.0113356415696,2.46999998000002,
-142.632517793947));
#147226=CARTESIAN_POINT('Ctrl Pts',(-45.385956606115,1.82990288117652,-148.554412051289));
#147227=CARTESIAN_POINT('Ctrl Pts',(-45.1914659347836,2.46999998002648,
-148.581690034117));
#147228=CARTESIAN_POINT('Ctrl Pts',(-45.8169723643538,2.46999998000002,
-148.343102920422));
#147229=CARTESIAN_POINT('Ctrl Pts',(-50.9608945753704,1.84386393970469,
-159.991229777381));
#147230=CARTESIAN_POINT('Ctrl Pts',(-50.7878173967191,2.46999997997405,
-160.008583439984));
#147231=CARTESIAN_POINT('Ctrl Pts',(-51.3962007668006,2.46999998000001,
-159.779920646508));
#147232=CARTESIAN_POINT('Ctrl Pts',(-53.7324859673961,1.84977562860519,
-165.717643463624));
#147233=CARTESIAN_POINT('Ctrl Pts',(-53.5753070147928,2.46999998000001,
-165.745313705806));
#147234=CARTESIAN_POINT('Ctrl Pts',(-54.1694331140562,2.46999998000001,
-165.506332215193));
#147235=CARTESIAN_POINT('Ctrl Pts',(-56.4941621559325,1.85499746228791,
-171.449026400902));
#147236=CARTESIAN_POINT('Ctrl Pts',(-56.3632322083114,2.46999998,-171.512146507354));
#147237=CARTESIAN_POINT('Ctrl Pts',(-56.9324803875071,2.46999998000001,
-171.237717270032));
#147238=CARTESIAN_POINT('',(-56.4941621559325,1.85499746228791,-171.449026400902));
#147239=CARTESIAN_POINT('Origin',(-56.9324803875071,1.96999998000001,-171.237717270032));
#147240=CARTESIAN_POINT('Ctrl Pts',(-56.4941621559325,1.85499746228791,
-171.449026400902));
#147241=CARTESIAN_POINT('Ctrl Pts',(-53.7324859673955,1.8497756286075,-165.717643463624));
#147242=CARTESIAN_POINT('Ctrl Pts',(-50.9608945753698,1.84386393970701,
-159.991229777381));
#147243=CARTESIAN_POINT('Ctrl Pts',(-45.3859566061143,1.82990288117884,
-148.554412051289));
#147244=CARTESIAN_POINT('Ctrl Pts',(-42.5829522730051,1.82186961481174,
-142.84383290998));
#147245=CARTESIAN_POINT('Ctrl Pts',(-39.7525219240432,1.81208306781682,
-137.147133758372));
#147246=CARTESIAN_POINT('Ctrl Pts',(-56.4736088945599,1.8573874935658,-171.409915902424));
#147247=CARTESIAN_POINT('Ctrl Pts',(-56.3489175136905,2.47012711531616,
-171.477038599322));
#147248=CARTESIAN_POINT('Ctrl Pts',(-56.9026784671178,2.46999996978156,
-171.178999526256));
#147249=CARTESIAN_POINT('Ctrl Pts',(-56.5595092645592,1.84739527439962,
-171.564880044108));
#147250=CARTESIAN_POINT('Ctrl Pts',(-56.4096617452282,2.47013088089768,
-171.619083147105));
#147251=CARTESIAN_POINT('Ctrl Pts',(-57.0276127026275,2.4699999696149,-171.411480993498));
#147252=CARTESIAN_POINT('Ctrl Pts',(-56.6013299245167,1.84257107601692,
-171.737940501487));
#147253=CARTESIAN_POINT('Ctrl Pts',(-56.4344504334064,2.4701327527474,-171.760758212924));
#147254=CARTESIAN_POINT('Ctrl Pts',(-57.0884505381249,2.46999996953445,
-171.671060999849));
#147255=CARTESIAN_POINT('Ctrl Pts',(-56.5930162481435,1.8435307818068,-171.916062071863));
#147256=CARTESIAN_POINT('Ctrl Pts',(-56.4294059961933,2.47013238231052,
-171.908444781729));
#147257=CARTESIAN_POINT('Ctrl Pts',(-57.0763566157493,2.46999996955046,
-171.938278709053));
#147258=CARTESIAN_POINT('Origin',(-57.077763566464,1.96999998000001,-171.871644662643));
#147259=CARTESIAN_POINT('Origin',(-55.230246199376,2.00193147732671,-171.934196687458));
#147260=CARTESIAN_POINT('Origin',(-57.077763566464,1.96999998000001,-179.64995));
#147261=CARTESIAN_POINT('Origin',(-57.077763566464,1.96999998000001,-176.848740272858));
#147262=CARTESIAN_POINT('Origin',(-57.,2.96999998000001,-174.34995));
#147263=CARTESIAN_POINT('',(-60.,2.96999998000001,-174.34995));
#147264=CARTESIAN_POINT('Origin',(-59.5,2.96999998000001,-174.34995));
#147265=CARTESIAN_POINT('',(-57.,2.96999998000001,-177.34995));
#147266=CARTESIAN_POINT('Origin',(-57.,2.96999998000001,-174.34995));
#147267=CARTESIAN_POINT('',(-57.,2.61702308584989,-177.204078948543));
#147268=CARTESIAN_POINT('Origin',(-57.,2.96999998000001,-176.84995));
#147269=CARTESIAN_POINT('Ctrl Pts',(-57.077763566464,2.46999998000001,-176.848740272858));
#147270=CARTESIAN_POINT('Ctrl Pts',(-57.0736014896981,2.46999998000001,
-176.982739539051));
#147271=CARTESIAN_POINT('Ctrl Pts',(-57.043897408659,2.52469464001198,-177.112050866152));
#147272=CARTESIAN_POINT('Ctrl Pts',(-57.,2.61702308584989,-177.204078948543));
#147273=CARTESIAN_POINT('Origin',(-59.5,2.96999998000001,-55.24995));
#147274=CARTESIAN_POINT('',(-60.,2.96999998000001,-58.24995));
#147275=CARTESIAN_POINT('Origin',(-59.5,2.96999998000001,-58.24995));
#147276=CARTESIAN_POINT('',(-60.,2.96999998000001,-174.34995));
#147277=CARTESIAN_POINT('Origin',(-57.,2.96999998000001,-58.24995));
#147278=CARTESIAN_POINT('Origin',(-57.,2.96999998000001,-58.24995));
#147279=CARTESIAN_POINT('Origin',(-57.,-2.42462934179819E-14,-58.24995));
#147280=CARTESIAN_POINT('',(-60.,3.46999998000001,-58.24995));
#147281=CARTESIAN_POINT('Origin',(-57.,3.46999998000001,-58.24995));
#147282=CARTESIAN_POINT('',(-60.,-54.58000002,-58.24995));
#147283=CARTESIAN_POINT('Origin',(-57.,3.46999998000001,-58.24995));
#147284=CARTESIAN_POINT('Origin',(-59.5,3.46999998000001,-58.24995));
#147285=CARTESIAN_POINT('Ctrl Pts',(-39.8417798628559,4.28988750369336,
-92.7506121713693));
#147286=CARTESIAN_POINT('Ctrl Pts',(-39.9519009607656,3.96999998000002,
-92.8065726369586));
#147287=CARTESIAN_POINT('Ctrl Pts',(-40.2576018765703,3.96999998000001,
-92.9619213022396));
#147288=CARTESIAN_POINT('Ctrl Pts',(-42.5267665504115,4.30001893486917,
-87.4583592347964));
#147289=CARTESIAN_POINT('Ctrl Pts',(-42.6535990616308,3.96999998005189,
-87.4723136103566));
#147290=CARTESIAN_POINT('Ctrl Pts',(-42.9469739380577,3.96999998000001,
-87.6696743385966));
#147291=CARTESIAN_POINT('Ctrl Pts',(-45.1797873789129,4.30850505828642,
-82.1496810404423));
#147292=CARTESIAN_POINT('Ctrl Pts',(-45.2981339154354,3.96999997998722,
-82.1711713234106));
#147293=CARTESIAN_POINT('Ctrl Pts',(-45.6032617662856,3.96999998000001,
-82.3609901713122));
#147294=CARTESIAN_POINT('Ctrl Pts',(-50.4483866457226,4.32340039588272,
-71.5131546212415));
#147295=CARTESIAN_POINT('Ctrl Pts',(-50.5607523082128,3.96999998001296,
-71.5306210575042));
#147296=CARTESIAN_POINT('Ctrl Pts',(-50.8772452803079,3.96999998000001,
-71.7244637521124));
#147297=CARTESIAN_POINT('Ctrl Pts',(-53.0636135580956,4.32979794413352,
-66.1851229312852));
#147298=CARTESIAN_POINT('Ctrl Pts',(-53.1696590969437,3.96999998001539,
-66.20755441643));
#147299=CARTESIAN_POINT('Ctrl Pts',(-53.4945734938964,3.96999998000001,
-66.3964343016074));
#147300=CARTESIAN_POINT('Ctrl Pts',(-55.6666368275827,4.33549309160632,
-60.8508735991007));
#147301=CARTESIAN_POINT('Ctrl Pts',(-55.7583700098454,3.96999998000001,
-60.8956682801396));
#147302=CARTESIAN_POINT('Ctrl Pts',(-56.0993680931338,3.96999998000001,
-61.0621827299711));
#147303=CARTESIAN_POINT('Origin',(-40.2576018765703,4.46999998000001,-92.9619213022396));
#147304=CARTESIAN_POINT('Origin',(-59.5,3.46999998000001,-55.24995));
#147305=CARTESIAN_POINT('',(-60.,3.46999998000001,-174.34995));
#147306=CARTESIAN_POINT('Origin',(-59.5,3.46999998000001,-174.34995));
#147307=CARTESIAN_POINT('',(-60.,3.46999998000001,-58.24995));
#147308=CARTESIAN_POINT('Origin',(-57.,3.46999998000001,-174.34995));
#147309=CARTESIAN_POINT('',(-57.,3.46999998000002,-177.34995));
#147310=CARTESIAN_POINT('Origin',(-57.,3.46999998000001,-176.84995));
#147311=CARTESIAN_POINT('Origin',(-57.,3.46999998000001,-174.34995));
#147312=CARTESIAN_POINT('Origin',(-60.,3.46999998000001,-176.84995));
#147313=CARTESIAN_POINT('',(-56.6639973329545,3.46999998000001,-177.34995));
#147314=CARTESIAN_POINT('',(-60.,3.46999998000001,-177.34995));
#147315=CARTESIAN_POINT('Ctrl Pts',(-56.6639973329545,3.46999998000001,
-177.34995));
#147316=CARTESIAN_POINT('Ctrl Pts',(-56.6512525237428,3.49196718394931,
-177.34995));
#147317=CARTESIAN_POINT('Ctrl Pts',(-56.638409424179,3.51400749072922,-177.348497985071));
#147318=CARTESIAN_POINT('Ctrl Pts',(-56.6256111772538,3.53587766712532,
-177.345591130597));
#147319=CARTESIAN_POINT('Ctrl Pts',(-56.6128072828548,3.55775749415936,
-177.342682993417));
#147320=CARTESIAN_POINT('Ctrl Pts',(-56.6000482806874,3.57946622894872,
-177.338318792525));
#147321=CARTESIAN_POINT('Ctrl Pts',(-56.5874775033198,3.60076486111489,
-177.332547706032));
#147322=CARTESIAN_POINT('Ctrl Pts',(-56.5758782741082,3.62041740201721,
-177.327222645132));
#147323=CARTESIAN_POINT('Ctrl Pts',(-56.5644392996185,3.63972036831063,
-177.320700481022));
#147324=CARTESIAN_POINT('Ctrl Pts',(-56.55327318179,3.65849822816206,-177.313057342243));
#147325=CARTESIAN_POINT('Ctrl Pts',(-56.5409041295215,3.6792990412609,-177.304590802261));
#147326=CARTESIAN_POINT('Ctrl Pts',(-56.528767320844,3.69963447340031,-177.294675450318));
#147327=CARTESIAN_POINT('Ctrl Pts',(-56.5170063855842,3.71926351161968,
-177.283387067871));
#147328=CARTESIAN_POINT('Ctrl Pts',(-56.505259388952,3.73886928622555,-177.272112063999));
#147329=CARTESIAN_POINT('Ctrl Pts',(-56.4938873753229,3.75776959928665,
-177.259467555873));
#147330=CARTESIAN_POINT('Ctrl Pts',(-56.4830334644546,3.77574315014845,
-177.245577493872));
#147331=CARTESIAN_POINT('Ctrl Pts',(-56.4736856290318,3.79122271299519,
-177.233614799948));
#147332=CARTESIAN_POINT('Ctrl Pts',(-56.4647220893045,3.80601492740013,
-177.220729185059));
#147333=CARTESIAN_POINT('Ctrl Pts',(-56.4562342721766,3.81999568465454,
-177.207025631657));
#147334=CARTESIAN_POINT('Ctrl Pts',(-56.4462721306327,3.8364048839292,-177.190941786237));
#147335=CARTESIAN_POINT('Ctrl Pts',(-56.4369089397934,3.85179681888003,
-177.173631278226));
#147336=CARTESIAN_POINT('Ctrl Pts',(-56.428262942834,3.86596506309141,-177.155255835143));
#147337=CARTESIAN_POINT('Ctrl Pts',(-56.4196371964386,3.88010012258878,
-177.136923430832));
#147338=CARTESIAN_POINT('Ctrl Pts',(-56.4117252882495,3.89301662424524,
-177.117531554289));
#147339=CARTESIAN_POINT('Ctrl Pts',(-56.4046446325427,3.90454306311565,
-177.097280363919));
#147340=CARTESIAN_POINT('Ctrl Pts',(-56.3987249342272,3.91417960577361,
-177.080349596136));
#147341=CARTESIAN_POINT('Ctrl Pts',(-56.3933862479742,3.92284500927668,
-177.06281908411));
#147342=CARTESIAN_POINT('Ctrl Pts',(-56.3886971856441,3.93046120142969,
-177.044822942092));
#147343=CARTESIAN_POINT('Ctrl Pts',(-56.3832835309579,3.9392543100379,-177.024045888662));
#147344=CARTESIAN_POINT('Ctrl Pts',(-56.3787297459052,3.94667107841779,
-177.002591890815));
#147345=CARTESIAN_POINT('Ctrl Pts',(-56.3750770606607,3.95260434330808,
-176.980690309454));
#147346=CARTESIAN_POINT('Ctrl Pts',(-56.3714253659076,3.95853599928657,
-176.958794667101));
#147347=CARTESIAN_POINT('Ctrl Pts',(-56.3686742823299,3.96298466796628,
-176.936452422772));
#147348=CARTESIAN_POINT('Ctrl Pts',(-56.3668650065705,3.96589210375174,
-176.913910938087));
#147349=CARTESIAN_POINT('Ctrl Pts',(-56.3651621901663,3.96862846349338,
-176.892695813916));
#147350=CARTESIAN_POINT('Ctrl Pts',(-56.3642936087743,3.96999998000001,
-176.871304903324));
#147351=CARTESIAN_POINT('Ctrl Pts',(-56.3642936064049,3.96999998000001,
-176.84995));
#147352=CARTESIAN_POINT('Origin',(-56.3642936064049,4.46999998000001,-179.64995));
#147353=CARTESIAN_POINT('Origin',(-56.3642936064049,4.46999998000001,-171.871644662643));
#147354=CARTESIAN_POINT('Origin',(-56.3642936064049,4.46999998000001,-176.84995));
#147355=CARTESIAN_POINT('Ctrl Pts',(-55.8855878616368,4.32236176169507,
-171.915575297858));
#147356=CARTESIAN_POINT('Ctrl Pts',(-55.9943718457987,3.96993791925994,
-171.920606124721));
#147357=CARTESIAN_POINT('Ctrl Pts',(-56.362878117604,3.96999998707827,-171.9375490258));
#147358=CARTESIAN_POINT('Ctrl Pts',(-55.8939328694509,4.32126340276226,
-171.739613349113));
#147359=CARTESIAN_POINT('Ctrl Pts',(-56.0043522879837,3.96993816409125,
-171.724641829017));
#147360=CARTESIAN_POINT('Ctrl Pts',(-56.3748852598388,3.96999998705621,
-171.673567304561));
#147361=CARTESIAN_POINT('Ctrl Pts',(-55.8520802190683,4.32676800360642,
-171.566123460328));
#147362=CARTESIAN_POINT('Ctrl Pts',(-55.9538751380083,3.96993692936931,
-171.529346602164));
#147363=CARTESIAN_POINT('Ctrl Pts',(-56.3146644389369,3.96999998716678,
-171.413359333373));
#147364=CARTESIAN_POINT('Ctrl Pts',(-55.7630923089791,4.33856909837021,
-171.409535679069));
#147365=CARTESIAN_POINT('Ctrl Pts',(-55.8512265932963,3.96993423686637,
-171.361424046831));
#147366=CARTESIAN_POINT('Ctrl Pts',(-56.1866565229903,3.96999998740383,
-171.178434208374));
#147367=CARTESIAN_POINT('',(-55.7843555297028,4.33575017898885,-171.449026400902));
#147368=CARTESIAN_POINT('Origin',(-56.2171666226051,4.46999998000001,-171.237717270032));
#147369=CARTESIAN_POINT('Origin',(-54.7568819751872,4.47301625251356,-171.880572980261));
#147370=CARTESIAN_POINT('Ctrl Pts',(-55.7843555297028,4.33575017898885,
-171.449026400902));
#147371=CARTESIAN_POINT('Ctrl Pts',(-55.8759673883189,3.96999998,-171.404299214979));
#147372=CARTESIAN_POINT('Ctrl Pts',(-56.2171666226051,3.96999998000001,
-171.237717270032));
#147373=CARTESIAN_POINT('Ctrl Pts',(-53.1620910906406,4.33003381235646,
-166.074376691472));
#147374=CARTESIAN_POINT('Ctrl Pts',(-53.2681640678716,3.96999998006972,
-166.052285867785));
#147375=CARTESIAN_POINT('Ctrl Pts',(-53.5931279590331,3.96999998000001,
-165.863065274939));
#147376=CARTESIAN_POINT('Ctrl Pts',(-50.5275177831741,4.32360860554286,
-160.70599701099));
#147377=CARTESIAN_POINT('Ctrl Pts',(-50.6399914208629,3.96999998001567,
-160.688987094682));
#147378=CARTESIAN_POINT('Ctrl Pts',(-50.9564483006955,3.96999998000001,
-160.494687880121));
#147379=CARTESIAN_POINT('Ctrl Pts',(-45.2197944205701,4.30863333062082,
-149.988992475295));
#147380=CARTESIAN_POINT('Ctrl Pts',(-45.3382862796144,3.96999997998453,
-149.967930534599));
#147381=CARTESIAN_POINT('Ctrl Pts',(-45.6433184787346,3.96999998000001,
-149.777683344423));
#147382=CARTESIAN_POINT('Ctrl Pts',(-42.547006853164,4.30009530891334,-144.640178460294));
#147383=CARTESIAN_POINT('Ctrl Pts',(-42.6741187750921,3.96999998000002,
-144.626843683376));
#147384=CARTESIAN_POINT('Ctrl Pts',(-42.9672472399765,3.96999998000001,
-144.428863195016));
#147385=CARTESIAN_POINT('Ctrl Pts',(-39.8417798628559,4.28988750369336,
-139.308030800137));
#147386=CARTESIAN_POINT('Ctrl Pts',(-39.9519009607656,3.96999998000002,
-139.252070334547));
#147387=CARTESIAN_POINT('Ctrl Pts',(-40.2576018765703,3.96999998000001,
-139.096721669266));
#147388=CARTESIAN_POINT('',(-39.8417798628559,4.28988750369336,-139.308030800137));
#147389=CARTESIAN_POINT('Origin',(-40.2576018765703,4.46999998000001,-139.096721669266));
#147390=CARTESIAN_POINT('Ctrl Pts',(-39.8417798628559,4.28988750369336,
-139.308030800137));
#147391=CARTESIAN_POINT('Ctrl Pts',(-42.547006853164,4.30009530891334,-144.640178460294));
#147392=CARTESIAN_POINT('Ctrl Pts',(-45.2197944205701,4.30863333062082,
-149.988992475295));
#147393=CARTESIAN_POINT('Ctrl Pts',(-50.5275177831741,4.32360860554286,
-160.70599701099));
#147394=CARTESIAN_POINT('Ctrl Pts',(-53.1620910906406,4.33003381235646,
-166.074376691472));
#147395=CARTESIAN_POINT('Ctrl Pts',(-55.7843555297028,4.33575017898885,
-171.449026400902));
#147396=CARTESIAN_POINT('Ctrl Pts',(-39.5006452494647,3.96999998000002,
-135.765140647295));
#147397=CARTESIAN_POINT('Ctrl Pts',(-38.9952902504278,3.96999998000001,
-135.758345202901));
#147398=CARTESIAN_POINT('Ctrl Pts',(-39.0007176781796,4.47537333373487,
-135.758410867476));
#147399=CARTESIAN_POINT('Ctrl Pts',(-39.4928147031327,3.96999998000002,
-136.361732614249));
#147400=CARTESIAN_POINT('Ctrl Pts',(-39.0186539030837,3.96999997999999,
-136.376595312284));
#147401=CARTESIAN_POINT('Ctrl Pts',(-38.9920125861994,4.44319084885118,
-136.395928609904));
#147402=CARTESIAN_POINT('Ctrl Pts',(-39.5563016945132,3.96999998000002,
-136.946343610491));
#147403=CARTESIAN_POINT('Ctrl Pts',(-39.1119466604377,3.96999998000028,
-136.996763230774));
#147404=CARTESIAN_POINT('Ctrl Pts',(-39.0625502874059,4.41106266091723,
-137.019624934458));
#147405=CARTESIAN_POINT('Ctrl Pts',(-39.8209093071024,3.96999998000002,
-138.091801575276));
#147406=CARTESIAN_POINT('Ctrl Pts',(-39.4455065674113,3.96999997999977,
-138.196241930898));
#147407=CARTESIAN_POINT('Ctrl Pts',(-39.3565523056356,4.34716680534984,
-138.239852049834));
#147408=CARTESIAN_POINT('Ctrl Pts',(-40.0249067020314,3.96999998000001,
-138.657274953305));
#147409=CARTESIAN_POINT('Ctrl Pts',(-39.6822172442077,3.96999997999977,
-138.786193354514));
#147410=CARTESIAN_POINT('Ctrl Pts',(-39.5832177453656,4.31512711082335,
-138.841288520716));
#147411=CARTESIAN_POINT('Ctrl Pts',(-40.3026878259433,3.96999998000001,
-139.183790066217));
#147412=CARTESIAN_POINT('Ctrl Pts',(-40.0028354069033,3.96999998000006,
-139.341990301777));
#147413=CARTESIAN_POINT('Ctrl Pts',(-39.8918569639406,4.28495188925998,
-139.400527284681));
#147414=CARTESIAN_POINT('',(-39.,4.46999998000001,-135.863383986541));
#147415=CARTESIAN_POINT('Origin',(-39.5,4.46999998000001,-135.863383986541));
#147416=CARTESIAN_POINT('Ctrl Pts',(-39.,4.46999998000001,-135.863383986541));
#147417=CARTESIAN_POINT('Ctrl Pts',(-39.0000000079857,4.46322313781914,
-135.997345455347));
#147418=CARTESIAN_POINT('Ctrl Pts',(-39.0035816630906,4.45643395135115,
-136.13071326381));
#147419=CARTESIAN_POINT('Ctrl Pts',(-39.0106410212532,4.44965345252242,
-136.263464717827));
#147420=CARTESIAN_POINT('Ctrl Pts',(-39.0178191132844,4.4427589100598,-136.398448966009));
#147421=CARTESIAN_POINT('Ctrl Pts',(-39.0285923600607,4.43587283021838,
-136.532796678209));
#147422=CARTESIAN_POINT('Ctrl Pts',(-39.0428966292102,4.42899941624294,
-136.66650693885));
#147423=CARTESIAN_POINT('Ctrl Pts',(-39.0572438241962,4.42210537576492,
-136.800618452064));
#147424=CARTESIAN_POINT('Ctrl Pts',(-39.0751430414656,4.4152234353718,-136.934089519031));
#147425=CARTESIAN_POINT('Ctrl Pts',(-39.0965800947071,4.40834883766489,
-137.066930171756));
#147426=CARTESIAN_POINT('Ctrl Pts',(-39.1179262242621,4.40150339805911,
-137.199207390612));
#147427=CARTESIAN_POINT('Ctrl Pts',(-39.1427802868893,4.39466455837632,
-137.330860369876));
#147428=CARTESIAN_POINT('Ctrl Pts',(-39.1711795471352,4.38782864206007,
-137.461897287268));
#147429=CARTESIAN_POINT('Ctrl Pts',(-39.1833297324556,4.38490400073638,
-137.517959410589));
#147430=CARTESIAN_POINT('Ctrl Pts',(-39.1961294752992,4.38197996731975,
-137.573908673113));
#147431=CARTESIAN_POINT('Ctrl Pts',(-39.2095844945887,4.37905678995323,
-137.629745040165));
#147432=CARTESIAN_POINT('Ctrl Pts',(-39.2451525049022,4.37132944296962,
-137.777347093828));
#147433=CARTESIAN_POINT('Ctrl Pts',(-39.2853508698145,4.36364419626997,
-137.924407380269));
#147434=CARTESIAN_POINT('Ctrl Pts',(-39.3302483641922,4.35597229663866,
-138.070491499552));
#147435=CARTESIAN_POINT('Ctrl Pts',(-39.3740760812887,4.34848319616003,
-138.213094857289));
#147436=CARTESIAN_POINT('Ctrl Pts',(-39.4223823137413,4.34100686721553,
-138.354768046511));
#147437=CARTESIAN_POINT('Ctrl Pts',(-39.4752127095435,4.3335527104114,-138.49508114583));
#147438=CARTESIAN_POINT('Ctrl Pts',(-39.527445058374,4.32618293563461,-138.633805882562));
#147439=CARTESIAN_POINT('Ctrl Pts',(-39.5841004388002,4.31883493157336,
-138.771201096999));
#147440=CARTESIAN_POINT('Ctrl Pts',(-39.6451946704874,4.31155255374419,
-138.906825786004));
#147441=CARTESIAN_POINT('Ctrl Pts',(-39.7062889021745,4.30427017591502,
-139.04245047501));
#147442=CARTESIAN_POINT('Ctrl Pts',(-39.771822798885,4.29705359933063,-139.176304484137));
#147443=CARTESIAN_POINT('Ctrl Pts',(-39.8417721751959,4.28997973064454,
-139.307922594137));
#147444=CARTESIAN_POINT('Origin',(-39.5,4.46999998000002,-55.24995));
#147445=CARTESIAN_POINT('',(-39.,4.46999998000002,-96.1952589849652));
#147446=CARTESIAN_POINT('Origin',(-39.5,4.46999998000001,-96.1952589849652));
#147447=CARTESIAN_POINT('',(-39.,4.46999998000002,-129.34995));
#147448=CARTESIAN_POINT('Ctrl Pts',(-40.2576018765703,3.96999998000001,
-92.9619213022396));
#147449=CARTESIAN_POINT('Ctrl Pts',(-39.9519009607655,3.96999998000001,
-92.8065726369586));
#147450=CARTESIAN_POINT('Ctrl Pts',(-39.8417798628559,4.28988750369336,
-92.7506121713693));
#147451=CARTESIAN_POINT('Ctrl Pts',(-40.0026978626623,3.96999998000001,
-93.4635309699092));
#147452=CARTESIAN_POINT('Ctrl Pts',(-39.6570458949425,3.9699999800025,-93.3357860473751));
#147453=CARTESIAN_POINT('Ctrl Pts',(-39.558565846057,4.31859237238363,-93.2834642887004));
#147454=CARTESIAN_POINT('Ctrl Pts',(-39.817114250256,3.96999998000002,-93.9870091547076));
#147455=CARTESIAN_POINT('Ctrl Pts',(-39.4410018196003,3.96999998000002,
-93.8819356839734));
#147456=CARTESIAN_POINT('Ctrl Pts',(-39.3523491668799,4.34822838553358,
-93.8402926529419));
#147457=CARTESIAN_POINT('Ctrl Pts',(-39.5650235754014,3.96999998000002,
-95.0708764103351));
#147458=CARTESIAN_POINT('Ctrl Pts',(-39.1236627362708,3.96999998000002,
-95.0167026881129));
#147459=CARTESIAN_POINT('Ctrl Pts',(-39.0722484171839,4.40869400027786,
-94.9948839370727));
#147460=CARTESIAN_POINT('Ctrl Pts',(-39.500000001452,3.96999998000002,-95.6349699403799));
#147461=CARTESIAN_POINT('Ctrl Pts',(-39.0293922558424,3.96999998000002,
-95.61424653503));
#147462=CARTESIAN_POINT('Ctrl Pts',(-39.,4.43971662334272,-95.5966316298752));
#147463=CARTESIAN_POINT('Ctrl Pts',(-39.5,3.96999998000002,-96.1952589849652));
#147464=CARTESIAN_POINT('Ctrl Pts',(-39.,3.96999998000001,-96.1952589849652));
#147465=CARTESIAN_POINT('Ctrl Pts',(-39.,4.46999998000002,-96.1952589849652));
#147466=CARTESIAN_POINT('Ctrl Pts',(-39.8417543268295,4.28989009189502,
-92.7506602165031));
#147467=CARTESIAN_POINT('Ctrl Pts',(-39.5585534503141,4.31859415382189,
-93.2834977599907));
#147468=CARTESIAN_POINT('Ctrl Pts',(-39.3523449576258,4.34822929418925,
-93.8403100037277));
#147469=CARTESIAN_POINT('Ctrl Pts',(-39.2122987920319,4.3784611929057,-94.4175882950073));
#147470=CARTESIAN_POINT('Ctrl Pts',(-39.072248417184,4.40869400027783,-94.9948839370727));
#147471=CARTESIAN_POINT('Ctrl Pts',(-39.,4.43971662334269,-95.5966316298752));
#147472=CARTESIAN_POINT('Ctrl Pts',(-39.,4.46999997999998,-96.1952589849652));
#147473=CARTESIAN_POINT('Ctrl Pts',(-40.0658654432757,9.93538940172282,
-86.8935063764011));
#147474=CARTESIAN_POINT('Ctrl Pts',(-39.,10.9256777712437,-87.8240033916746));
#147475=CARTESIAN_POINT('Ctrl Pts',(-39.,12.1842625441365,-89.0065976851046));
#147476=CARTESIAN_POINT('Ctrl Pts',(-40.0194662171323,8.81210183467955,
-88.1753591901201));
#147477=CARTESIAN_POINT('Ctrl Pts',(-39.,9.77616182941803,-89.1086695731953));
#147478=CARTESIAN_POINT('Ctrl Pts',(-39.,10.9797897629302,-90.28846680179));
#147479=CARTESIAN_POINT('Ctrl Pts',(-39.9723426990601,7.65560021428954,
-89.4314931216999));
#147480=CARTESIAN_POINT('Ctrl Pts',(-39.,8.58691729751272,-90.3710832422126));
#147481=CARTESIAN_POINT('Ctrl Pts',(-39.,9.73513866768107,-91.5445844304498));
#147482=CARTESIAN_POINT('Ctrl Pts',(-39.8778703452952,5.25671151505436,
-91.8642463668096));
#147483=CARTESIAN_POINT('Ctrl Pts',(-39.,6.11218708321155,-92.8159732515183));
#147484=CARTESIAN_POINT('Ctrl Pts',(-39.,7.14206310577898,-93.9773376754667));
#147485=CARTESIAN_POINT('Ctrl Pts',(-39.8310091356278,4.02698776925249,
-93.0281766935241));
#147486=CARTESIAN_POINT('Ctrl Pts',(-38.9999999999877,4.84006269065046,
-93.9862863085864));
#147487=CARTESIAN_POINT('Ctrl Pts',(-39.,5.80730703259943,-95.141285808143));
#147488=CARTESIAN_POINT('Ctrl Pts',(-39.7856125955649,2.75522821384069,
-94.1210748292835));
#147489=CARTESIAN_POINT('Ctrl Pts',(-39.,3.51696389869249,-95.0875400976674));
#147490=CARTESIAN_POINT('Ctrl Pts',(-39.,4.4206962941175,-96.234166137987));
#147491=CARTESIAN_POINT('',(-39.0000000003509,10.11999998,-91.1341759094044));
#147492=CARTESIAN_POINT('Ctrl Pts',(-39.0000000014036,10.11999998,-91.1341759094044));
#147493=CARTESIAN_POINT('Ctrl Pts',(-39.0000000011199,9.67730365003607,
-91.5752858705177));
#147494=CARTESIAN_POINT('Ctrl Pts',(-39.0000000008905,9.22960685182023,
-92.0113795712675));
#147495=CARTESIAN_POINT('Ctrl Pts',(-39.0000000007062,8.77598048479483,
-92.4423316323824));
#147496=CARTESIAN_POINT('Ctrl Pts',(-39.0000000006606,8.66387047827009,
-92.5488378716476));
#147497=CARTESIAN_POINT('Ctrl Pts',(-39.0000000006178,8.55139809473461,
-92.655029929952));
#147498=CARTESIAN_POINT('Ctrl Pts',(-39.0000000005776,8.43854888592042,
-92.7609056252126));
#147499=CARTESIAN_POINT('Ctrl Pts',(-39.0000000004289,8.02088208267292,
-93.1527627205862));
#147500=CARTESIAN_POINT('Ctrl Pts',(-39.000000000316,7.59947404052636,-93.538972567434));
#147501=CARTESIAN_POINT('Ctrl Pts',(-39.0000000002313,7.17350510091871,
-93.9192513866139));
#147502=CARTESIAN_POINT('Ctrl Pts',(-39.0000000001502,6.76608030666306,
-94.2829751355963));
#147503=CARTESIAN_POINT('Ctrl Pts',(-39.000000000095,6.35448332404243,-94.6412733528635));
#147504=CARTESIAN_POINT('Ctrl Pts',(-39.0000000000588,5.93796915879824,
-94.9938596180162));
#147505=CARTESIAN_POINT('Ctrl Pts',(-39.0000000000244,5.54178994091724,
-95.3292320072887));
#147506=CARTESIAN_POINT('Ctrl Pts',(-39.0000000000072,5.14116207582966,
-95.6594367346931));
#147507=CARTESIAN_POINT('Ctrl Pts',(-39.0000000000019,4.7354162137309,-95.9841886223937));
#147508=CARTESIAN_POINT('Ctrl Pts',(-39.0000000000007,4.64718860219477,
-96.0548044587339));
#147509=CARTESIAN_POINT('Ctrl Pts',(-39.0000000000001,4.55871888403425,
-96.1251623137627));
#147510=CARTESIAN_POINT('Ctrl Pts',(-39.,4.46999998000004,-96.1952589849652));
#147511=CARTESIAN_POINT('Ctrl Pts',(-39.,10.11999998,-91.1341759094044));
#147512=CARTESIAN_POINT('Ctrl Pts',(-39.,10.0814485101051,-90.4015548889157));
#147513=CARTESIAN_POINT('Ctrl Pts',(-39.0871202471367,10.0432464379346,
-89.6831085829417));
#147514=CARTESIAN_POINT('Ctrl Pts',(-39.4353702716187,9.96778569194113,
-88.2750332463665));
#147515=CARTESIAN_POINT('Ctrl Pts',(-39.7001620921283,9.93023578423926,
-87.5801598805708));
#147516=CARTESIAN_POINT('Ctrl Pts',(-40.0642139577648,9.89540181781398,
-86.9391114735715));
#147517=CARTESIAN_POINT('Ctrl Pts',(-53.6034226162473,9.94191093135267,
-60.8508735991007));
#147518=CARTESIAN_POINT('Ctrl Pts',(-53.3728980178288,10.61999998,-60.7339721953768));
#147519=CARTESIAN_POINT('Ctrl Pts',(-54.0201152391274,10.61999998,-61.0621827299711));
#147520=CARTESIAN_POINT('Ctrl Pts',(-51.389560409622,9.93573232969473,-65.2217230132311));
#147521=CARTESIAN_POINT('Ctrl Pts',(-51.1265017070351,10.6199999801373,
-65.1408421794535));
#147522=CARTESIAN_POINT('Ctrl Pts',(-51.803611404114,10.61999998,-65.4330340644));
#147523=CARTESIAN_POINT('Ctrl Pts',(-49.1597584431958,9.92893027259159,
-69.5840753787896));
#147524=CARTESIAN_POINT('Ctrl Pts',(-48.8773807075708,10.619999979979,-69.5080715791473));
#147525=CARTESIAN_POINT('Ctrl Pts',(-49.5707491962873,10.61999998,-69.7953845096657));
#147526=CARTESIAN_POINT('Ctrl Pts',(-44.653312474994,9.91361721971961,-78.2837188426078));
#147527=CARTESIAN_POINT('Ctrl Pts',(-44.3407772417843,10.6199999800215,
-78.1912921743765));
#147528=CARTESIAN_POINT('Ctrl Pts',(-45.0568309856751,10.61999998,-78.4950279734725));
#147529=CARTESIAN_POINT('Ctrl Pts',(-42.3769453400103,9.90511004010749,
-82.6211625596856));
#147530=CARTESIAN_POINT('Ctrl Pts',(-42.0362703406502,10.6199999800752,
-82.5368298570061));
#147531=CARTESIAN_POINT('Ctrl Pts',(-42.7760616201669,10.61999998,-82.8324761280086));
#147532=CARTESIAN_POINT('Ctrl Pts',(-40.064213984323,9.8954018152728,-86.9391114268059));
#147533=CARTESIAN_POINT('Ctrl Pts',(-39.7432392475337,10.61999998,-86.7667827168808));
#147534=CARTESIAN_POINT('Ctrl Pts',(-40.4577925858907,10.61999998,-87.1504205576762));
#147535=CARTESIAN_POINT('Origin',(-40.4577925858907,10.11999998,-87.1504205576762));
#147536=CARTESIAN_POINT('Ctrl Pts',(-53.7132658667155,9.94427345760885,
-171.427096642113));
#147537=CARTESIAN_POINT('Ctrl Pts',(-53.4900212150555,10.6200436404067,
-171.547539040488));
#147538=CARTESIAN_POINT('Ctrl Pts',(-54.1252562655568,10.6199999790853,
-171.204806771057));
#147539=CARTESIAN_POINT('Ctrl Pts',(-53.7965641368282,9.93061460392252,
-171.570704923163));
#147540=CARTESIAN_POINT('Ctrl Pts',(-53.5293152990567,10.6200454840217,
-171.669460818784));
#147541=CARTESIAN_POINT('Ctrl Pts',(-54.2414728015497,10.6199999790668,
-171.420234627167));
#147542=CARTESIAN_POINT('Ctrl Pts',(-53.8395077234189,9.92361807935438,
-171.731386846755));
#147543=CARTESIAN_POINT('Ctrl Pts',(-53.5404438804703,10.6200464809797,
-171.777144153382));
#147544=CARTESIAN_POINT('Ctrl Pts',(-54.3014296083321,10.6199999790573,
-171.661245462915));
#147545=CARTESIAN_POINT('Ctrl Pts',(-53.8346934801606,9.92440268025274,
-171.896703002604));
#147546=CARTESIAN_POINT('Ctrl Pts',(-53.5391294683121,10.6200463684923,
-171.888526671099));
#147547=CARTESIAN_POINT('Ctrl Pts',(-54.2947083191068,10.6199999790584,
-171.909234173462));
#147548=CARTESIAN_POINT('',(-53.7255998841352,9.94225131873297,-171.449026400902));
#147549=CARTESIAN_POINT('Origin',(-54.1424378198232,10.11999998,-171.237717270032));
#147550=CARTESIAN_POINT('Origin',(-54.2951871140408,10.11999998,-171.871644662643));
#147551=CARTESIAN_POINT('Origin',(-52.5986019878193,10.1270016580449,-171.886013583419));
#147552=CARTESIAN_POINT('Origin',(-54.2951871140408,10.11999998,-179.64995));
#147553=CARTESIAN_POINT('Origin',(-54.2951871140408,10.11999998,-176.84995));
#147554=CARTESIAN_POINT('Origin',(83.2809572255632,11.1199999800001,-176.84995));
#147555=CARTESIAN_POINT('',(-57.,11.11999998,-177.34995));
#147556=CARTESIAN_POINT('Origin',(-57.,11.11999998,-176.84995));
#147557=CARTESIAN_POINT('',(-53.8590042959267,11.11999998,-177.34995));
#147558=CARTESIAN_POINT('',(-60.,11.11999998,-177.34995));
#147559=CARTESIAN_POINT('Ctrl Pts',(-54.2951871140408,10.61999998,-176.84995));
#147560=CARTESIAN_POINT('Ctrl Pts',(-54.2951871094022,10.61999998,-176.919796282647));
#147561=CARTESIAN_POINT('Ctrl Pts',(-54.282897054019,10.6344777440414,-176.987189324297));
#147562=CARTESIAN_POINT('Ctrl Pts',(-54.2369068974943,10.6883272976786,
-177.111149481396));
#147563=CARTESIAN_POINT('Ctrl Pts',(-54.2036611796727,10.7271494012897,
-177.166153898004));
#147564=CARTESIAN_POINT('Ctrl Pts',(-54.1215658763003,10.8221729031368,
-177.256908861057));
#147565=CARTESIAN_POINT('Ctrl Pts',(-54.0742219292009,10.8766241714759,
-177.291358543608));
#147566=CARTESIAN_POINT('Ctrl Pts',(-53.9700011606116,10.9953079956486,
-177.338340413074));
#147567=CARTESIAN_POINT('Ctrl Pts',(-53.9152095126149,11.0571633006792,
-177.34995));
#147568=CARTESIAN_POINT('Ctrl Pts',(-53.8590042959267,11.11999998,-177.34995));
#147569=CARTESIAN_POINT('Origin',(-57.,11.11999998,-174.34995));
#147570=CARTESIAN_POINT('',(-60.,11.11999998,-174.34995));
#147571=CARTESIAN_POINT('Origin',(-59.5,11.11999998,-174.34995));
#147572=CARTESIAN_POINT('Origin',(-57.,11.11999998,-174.34995));
#147573=CARTESIAN_POINT('Origin',(-59.5,11.11999998,-55.24995));
#147574=CARTESIAN_POINT('',(-60.,11.11999998,-174.34995));
#147575=CARTESIAN_POINT('Ctrl Pts',(-39.5,10.61999998,-91.1341759094044));
#147576=CARTESIAN_POINT('Ctrl Pts',(-39.,10.61999998,-91.1341759094044));
#147577=CARTESIAN_POINT('Ctrl Pts',(-39.,10.11999998,-91.1341759094044));
#147578=CARTESIAN_POINT('Ctrl Pts',(-39.5000000020536,10.61999998,-90.4402448608912));
#147579=CARTESIAN_POINT('Ctrl Pts',(-38.9598916786063,10.61999998,-90.3719688890004));
#147580=CARTESIAN_POINT('Ctrl Pts',(-39.,10.0814485101051,-90.4015548889157));
#147581=CARTESIAN_POINT('Ctrl Pts',(-39.5784082214306,10.61999998,-89.7587725653299));
#147582=CARTESIAN_POINT('Ctrl Pts',(-39.0069350308393,10.61999998,-89.6407441936901));
#147583=CARTESIAN_POINT('Ctrl Pts',(-39.0871202471367,10.0432464379346,
-89.6831085829417));
#147584=CARTESIAN_POINT('Ctrl Pts',(-39.89183324926,10.61999998,-88.4214995542899));
#147585=CARTESIAN_POINT('Ctrl Pts',(-39.245797474144,10.61999998,-88.1799493597601));
#147586=CARTESIAN_POINT('Ctrl Pts',(-39.4353702758529,9.96778569102363,
-88.2750332292462));
#147587=CARTESIAN_POINT('Ctrl Pts',(-40.1301388343916,10.61999998,-87.7606994776464));
#147588=CARTESIAN_POINT('Ctrl Pts',(-39.4581171327344,10.61999998,-87.4384896017421));
#147589=CARTESIAN_POINT('Ctrl Pts',(-39.7001621050063,9.93023578241304,
-87.580159846776));
#147590=CARTESIAN_POINT('Ctrl Pts',(-40.4577925858907,10.61999998,-87.1504205576762));
#147591=CARTESIAN_POINT('Ctrl Pts',(-39.7432392475336,10.61999998,-86.7667827168808));
#147592=CARTESIAN_POINT('Ctrl Pts',(-40.064213984323,9.8954018152728,-86.9391114268059));
#147593=CARTESIAN_POINT('Origin',(-39.5,10.11999998,-91.1341759094044));
#147594=CARTESIAN_POINT('Origin',(-39.5,10.11999998,-55.24995));
#147595=CARTESIAN_POINT('',(-39.0000000003307,10.11999998,-140.924467062102));
#147596=CARTESIAN_POINT('Origin',(-39.5,10.11999998,-140.924467062102));
#147597=CARTESIAN_POINT('',(-39.,10.11999998,-129.34995));
#147598=CARTESIAN_POINT('Ctrl Pts',(-40.6666545727859,10.61999998,-145.271541906631));
#147599=CARTESIAN_POINT('Ctrl Pts',(-39.9386298681517,10.61999998,-145.722049280659));
#147600=CARTESIAN_POINT('Ctrl Pts',(-40.2964538775261,9.87423053204576,
-145.500920636949));
#147601=CARTESIAN_POINT('Ctrl Pts',(-40.2252930694247,10.61999998,-144.553023210506));
#147602=CARTESIAN_POINT('Ctrl Pts',(-39.5493658636703,10.61999998,-144.926690587367));
#147603=CARTESIAN_POINT('Ctrl Pts',(-39.8060841900594,9.91530069853091,
-144.746634756903));
#147604=CARTESIAN_POINT('Ctrl Pts',(-39.9277556139221,10.61999998,-143.785038173526));
#147605=CARTESIAN_POINT('Ctrl Pts',(-39.275725873409,10.61999998,-144.057794964171));
#147606=CARTESIAN_POINT('Ctrl Pts',(-39.4754129960987,9.95900873040137,
-143.939244770734));
#147607=CARTESIAN_POINT('Ctrl Pts',(-39.5483465195115,10.61999998,-142.176898403278));
#147608=CARTESIAN_POINT('Ctrl Pts',(-38.9857875579427,10.61999998,-142.298553027766));
#147609=CARTESIAN_POINT('Ctrl Pts',(-39.053767673473,10.0497742339444,-142.246026638163));
#147610=CARTESIAN_POINT('Ctrl Pts',(-39.471139351319,10.61999998,-141.33510811083));
#147611=CARTESIAN_POINT('Ctrl Pts',(-38.9439335251668,10.61999998,-141.396464936279));
#147612=CARTESIAN_POINT('Ctrl Pts',(-38.9679508580438,10.0969150082091,
-141.358373831859));
#147613=CARTESIAN_POINT('Ctrl Pts',(-39.5096103982927,10.61999998,-140.51133866194));
#147614=CARTESIAN_POINT('Ctrl Pts',(-39.0322223955025,10.61999998,-140.488711952169));
#147615=CARTESIAN_POINT('Ctrl Pts',(-39.0106607951198,10.1425265025536,
-140.488167507581));
#147616=CARTESIAN_POINT('',(-40.0642139705729,9.89540191650284,-145.11953147077));
#147617=CARTESIAN_POINT('Origin',(-40.4577925858907,10.11999998,-144.90822241383));
#147618=CARTESIAN_POINT('Ctrl Pts',(-40.0642139728404,9.89540198157303,
-145.11953138824));
#147619=CARTESIAN_POINT('Ctrl Pts',(-40.002351458265,9.90132139175144,-145.010598868768));
#147620=CARTESIAN_POINT('Ctrl Pts',(-39.94358948579,9.90737279989773,-144.900576570422));
#147621=CARTESIAN_POINT('Ctrl Pts',(-39.8877792387549,9.91347673417978,
-144.789574845718));
#147622=CARTESIAN_POINT('Ctrl Pts',(-39.8308107857465,9.919707340776,-144.676269550121));
#147623=CARTESIAN_POINT('Ctrl Pts',(-39.7769170800584,9.92599288696455,
-144.561943605637));
#147624=CARTESIAN_POINT('Ctrl Pts',(-39.7259463774167,9.93228888280149,
-144.446677879912));
#147625=CARTESIAN_POINT('Ctrl Pts',(-39.6734351827218,9.93877516307736,
-144.327928467966));
#147626=CARTESIAN_POINT('Ctrl Pts',(-39.6240255672203,9.94527281200331,
-144.208181399467));
#147627=CARTESIAN_POINT('Ctrl Pts',(-39.5775704396244,9.95177155785657,
-144.087489445839));
#147628=CARTESIAN_POINT('Ctrl Pts',(-39.5304878255662,9.95835808465577,
-143.965167261688));
#147629=CARTESIAN_POINT('Ctrl Pts',(-39.4864394012381,9.96494622145986,
-143.841874086364));
#147630=CARTESIAN_POINT('Ctrl Pts',(-39.4453020254186,9.97155811034743,
-143.717633667422));
#147631=CARTESIAN_POINT('Ctrl Pts',(-39.4035199172632,9.97827362515868,
-143.591446069937));
#147632=CARTESIAN_POINT('Ctrl Pts',(-39.3647402527405,9.98501420275193,
-143.464280813464));
#147633=CARTESIAN_POINT('Ctrl Pts',(-39.3288740919353,9.99182873162542,
-143.336137664792));
#147634=CARTESIAN_POINT('Ctrl Pts',(-39.3062701153551,9.99612346090792,
-143.255377843655));
#147635=CARTESIAN_POINT('Ctrl Pts',(-39.2848241991159,10.0004480486441,
-143.174229132943));
#147636=CARTESIAN_POINT('Ctrl Pts',(-39.2645234280954,10.0048182625419,
-143.092687886665));
#147637=CARTESIAN_POINT('Ctrl Pts',(-39.2108307463155,10.0163768631431,
-142.877022768137));
#147638=CARTESIAN_POINT('Ctrl Pts',(-39.1652210086604,10.0280753656729,
-142.65870232555));
#147639=CARTESIAN_POINT('Ctrl Pts',(-39.1277908815641,10.0398210480943,
-142.438684630891));
#147640=CARTESIAN_POINT('Ctrl Pts',(-39.089043042221,10.0519802324398,-142.210921303682));
#147641=CARTESIAN_POINT('Ctrl Pts',(-39.0590605395586,10.0641904270523,
-141.981338102442));
#147642=CARTESIAN_POINT('Ctrl Pts',(-39.037912413284,10.0763900147051,-141.751001744749));
#147643=CARTESIAN_POINT('Ctrl Pts',(-39.0170605976466,10.0884186714896,
-141.523892675944));
#147644=CARTESIAN_POINT('Ctrl Pts',(-39.0047974378935,10.1004377695582,
-141.296050430499));
#147645=CARTESIAN_POINT('Ctrl Pts',(-39.0011547572432,10.11241789425,-141.068516354615));
#147646=CARTESIAN_POINT('Ctrl Pts',(-39.0003857691051,10.1149469586025,
-141.020482771066));
#147647=CARTESIAN_POINT('Ctrl Pts',(-39.0000008244016,10.11747437054,-140.972463017993));
#147648=CARTESIAN_POINT('Ctrl Pts',(-39.0000000013228,10.1199999800001,
-140.924467062102));
#147649=CARTESIAN_POINT('Ctrl Pts',(-40.064213984323,9.8954018152728,-145.1195315447));
#147650=CARTESIAN_POINT('Ctrl Pts',(-39.7432392475336,10.61999998,-145.291860254625));
#147651=CARTESIAN_POINT('Ctrl Pts',(-40.4577925858907,10.61999998,-144.90822241383));
#147652=CARTESIAN_POINT('Ctrl Pts',(-42.3982233528881,9.90519935947367,
-149.477207192598));
#147653=CARTESIAN_POINT('Ctrl Pts',(-42.0569998298599,10.61999998,-149.560052788611));
#147654=CARTESIAN_POINT('Ctrl Pts',(-42.7973905232547,10.61999998,-149.265893474329));
#147655=CARTESIAN_POINT('Ctrl Pts',(-44.6952062210366,9.91377387366803,
-153.854728198786));
#147656=CARTESIAN_POINT('Ctrl Pts',(-44.3825306854435,10.6199999800261,
-153.946076900384));
#147657=CARTESIAN_POINT('Ctrl Pts',(-45.0988060523808,10.61999998,-153.643419067924));
#147658=CARTESIAN_POINT('Ctrl Pts',(-49.2422260788803,9.92919580612355,
-162.634871500674));
#147659=CARTESIAN_POINT('Ctrl Pts',(-48.9599089008669,10.6199999799746,
-162.709726895544));
#147660=CARTESIAN_POINT('Ctrl Pts',(-49.6533413888222,10.61999998,-162.423562369795));
#147661=CARTESIAN_POINT('Ctrl Pts',(-51.491975374397,9.936039246645,-167.037652347168));
#147662=CARTESIAN_POINT('Ctrl Pts',(-51.2291869847762,10.6199999797401,
-167.117625919029));
#147663=CARTESIAN_POINT('Ctrl Pts',(-51.9061633492443,10.61999998,-166.826341244199));
#147664=CARTESIAN_POINT('Ctrl Pts',(-53.7255998841352,9.94225131873298,
-171.449026400902));
#147665=CARTESIAN_POINT('Ctrl Pts',(-53.4956787755832,10.61999998,-171.565581122671));
#147666=CARTESIAN_POINT('Ctrl Pts',(-54.1424378198232,10.61999998,-171.237717270032));
#147667=CARTESIAN_POINT('Ctrl Pts',(-53.7255998841352,9.94225131873297,
-171.449026400902));
#147668=CARTESIAN_POINT('Ctrl Pts',(-51.4919753743962,9.93603924664709,
-167.037652347168));
#147669=CARTESIAN_POINT('Ctrl Pts',(-49.2422260788795,9.92919580612563,
-162.634871500674));
#147670=CARTESIAN_POINT('Ctrl Pts',(-44.6952062210357,9.91377387367011,
-153.854728198786));
#147671=CARTESIAN_POINT('Ctrl Pts',(-42.3982233528871,9.90519935947574,
-149.477207192598));
#147672=CARTESIAN_POINT('Ctrl Pts',(-40.064213984323,9.8954018152728,-145.1195315447));
#147673=CARTESIAN_POINT('Ctrl Pts',(-38.8323560497301,-56.2084592670262,
-61.2273317382593));
#147674=CARTESIAN_POINT('Ctrl Pts',(-39.0122500629964,-56.4087764892537,
-60.6499500000001));
#147675=CARTESIAN_POINT('Ctrl Pts',(-39.4379155619868,-56.882767417621,
-60.64995));
#147676=CARTESIAN_POINT('Ctrl Pts',(-38.9597499727218,-56.0859430057577,
-61.2402727589806));
#147677=CARTESIAN_POINT('Ctrl Pts',(-39.1308890120013,-56.2886813392436,
-60.64995));
#147678=CARTESIAN_POINT('Ctrl Pts',(-39.5470561894999,-56.7847541538272,
-60.64995));
#147679=CARTESIAN_POINT('Ctrl Pts',(-39.0917129041016,-55.9712198429402,
-61.2536666704059));
#147680=CARTESIAN_POINT('Ctrl Pts',(-39.2535572856597,-56.1757390223779,
-60.64995));
#147681=CARTESIAN_POINT('Ctrl Pts',(-39.6600993514669,-56.6929757051825,
-60.64995));
#147682=CARTESIAN_POINT('Ctrl Pts',(-39.2278317447683,-55.8636034060938,
-61.2674693219905));
#147683=CARTESIAN_POINT('Ctrl Pts',(-39.3796800351166,-56.0692409848678,
-60.64995));
#147684=CARTESIAN_POINT('Ctrl Pts',(-39.7766890844069,-56.606882728875,
-60.64995));
#147685=CARTESIAN_POINT('',(-39.2253966502056,-55.8655297208509,-61.2672223984388));
#147686=CARTESIAN_POINT('',(-38.8323576630952,-56.2084583512428,-61.2273323469212));
#147687=CARTESIAN_POINT('Ctrl Pts',(-39.2253966502054,-55.865529720851,
-61.2672223984388));
#147688=CARTESIAN_POINT('Ctrl Pts',(-39.0894849099381,-55.973106721351,
-61.2534405956196));
#147689=CARTESIAN_POINT('Ctrl Pts',(-38.9583675005087,-56.087272628509,
-61.2401323247394));
#147690=CARTESIAN_POINT('Ctrl Pts',(-38.8323573704738,-56.2084579968516,
-61.227331872424));
#147691=CARTESIAN_POINT('Origin',(-39.4379155619868,-56.882767417621,-61.64995));
#147692=CARTESIAN_POINT('Ctrl Pts',(-39.2253966502054,-55.865529720851,
-61.2672223984388));
#147693=CARTESIAN_POINT('Ctrl Pts',(-39.2371501417372,-55.9108514932488,
-61.1623844624743));
#147694=CARTESIAN_POINT('Ctrl Pts',(-39.2529884923231,-55.9713882406491,
-61.071384516352));
#147695=CARTESIAN_POINT('Ctrl Pts',(-39.2917636103596,-56.1160106335832,
-60.9126819775317));
#147696=CARTESIAN_POINT('Ctrl Pts',(-39.3137989788887,-56.1967066207402,
-60.8488138257101));
#147697=CARTESIAN_POINT('Ctrl Pts',(-39.3624939333409,-56.3700857302443,
-60.7466874393643));
#147698=CARTESIAN_POINT('Ctrl Pts',(-39.388248240317,-56.4595484948523,
-60.710350981156));
#147699=CARTESIAN_POINT('Ctrl Pts',(-39.4424275296133,-56.6422462965493,
-60.6618415351963));
#147700=CARTESIAN_POINT('Ctrl Pts',(-39.4710350160438,-56.736024652106,
-60.6499500783916));
#147701=CARTESIAN_POINT('Ctrl Pts',(-39.4999997135852,-56.828045000138,
-60.6499500000004));
#147702=CARTESIAN_POINT('Origin',(-39.5,-12.9675000200281,-61.14995));
#147703=CARTESIAN_POINT('Origin',(-39.5,-56.8280459100727,-61.14995));
#147704=CARTESIAN_POINT('Origin',(-33.85,67.7009572055632,-61.14995));
#147705=CARTESIAN_POINT('Origin',(-33.85,-61.3211699373828,-61.14995));
#147706=CARTESIAN_POINT('Origin',(0.,-12.9675000200281,-61.64995));
#147707=CARTESIAN_POINT('',(-33.5881101525803,-60.3971457002532,-61.2273317382593));
#147708=CARTESIAN_POINT('Origin',(0.,-12.9675000200281,-61.2273317382593));
#147709=CARTESIAN_POINT('Ctrl Pts',(-33.85,-61.3211699373828,-60.64995));
#147710=CARTESIAN_POINT('Ctrl Pts',(-33.7991562663074,-61.1403193911197,
-60.64995));
#147711=CARTESIAN_POINT('Ctrl Pts',(-33.7471512515707,-60.9562715767294,
-60.6978885776012));
#147712=CARTESIAN_POINT('Ctrl Pts',(-33.6552207448938,-60.6322769136983,
-60.8896846949796));
#147713=CARTESIAN_POINT('Ctrl Pts',(-33.6142503615382,-60.4886315879339,
-61.034824258355));
#147714=CARTESIAN_POINT('Ctrl Pts',(-33.5881101525803,-60.3971457002532,
-61.2273317382593));
#147715=CARTESIAN_POINT('Ctrl Pts',(-39.5,-62.6133861954129,-171.64995));
#147716=CARTESIAN_POINT('Ctrl Pts',(-40.,-62.6133861954129,-171.64995));
#147717=CARTESIAN_POINT('Ctrl Pts',(-40.,-62.6133861954129,-171.14995));
#147718=CARTESIAN_POINT('Ctrl Pts',(-39.4908895000012,-62.7468765389391,
-171.64995));
#147719=CARTESIAN_POINT('Ctrl Pts',(-39.9999999999999,-62.7481681417254,
-171.659148653594));
#147720=CARTESIAN_POINT('Ctrl Pts',(-40.,-62.8117011147884,-171.149950000016));
#147721=CARTESIAN_POINT('Ctrl Pts',(-39.4817858670191,-62.8802662644338,
-171.67597732698));
#147722=CARTESIAN_POINT('Ctrl Pts',(-40.,-62.8775589599766,-171.69520402023));
#147723=CARTESIAN_POINT('Ctrl Pts',(-40.,-63.0098665547682,-171.18899099047));
#147724=CARTESIAN_POINT('Ctrl Pts',(-39.4649548930126,-63.1268797875294,
-171.776163607997));
#147725=CARTESIAN_POINT('Ctrl Pts',(-40.0000000000001,-63.1103377557996,
-171.809929875206));
#147726=CARTESIAN_POINT('Ctrl Pts',(-40.,-63.3762386807026,-171.339270411997));
#147727=CARTESIAN_POINT('Ctrl Pts',(-39.4572358131761,-63.2399825392123,
-171.850283164391));
#147728=CARTESIAN_POINT('Ctrl Pts',(-40.000000000002,-63.2129124685353,
-171.888983273332));
#147729=CARTESIAN_POINT('Ctrl Pts',(-40.,-63.5442655393439,-171.450449746589));
#147730=CARTESIAN_POINT('Ctrl Pts',(-39.4443539433762,-63.4287323580851,
-172.035403273235));
#147731=CARTESIAN_POINT('Ctrl Pts',(-39.9999999999979,-63.3805692396919,
-172.075215659168));
#147732=CARTESIAN_POINT('Ctrl Pts',(-40.,-63.8246746245531,-171.728129909852));
#147733=CARTESIAN_POINT('Ctrl Pts',(-39.4391962191206,-63.5043052007179,
-172.14633102856));
#147734=CARTESIAN_POINT('Ctrl Pts',(-40.,-63.4448403055015,-172.182182441317));
#147735=CARTESIAN_POINT('Ctrl Pts',(-40.,-63.9369465821947,-171.894521542842));
#147736=CARTESIAN_POINT('Ctrl Pts',(-39.4322246014262,-63.6064558665446,
-172.38820210671));
#147737=CARTESIAN_POINT('Ctrl Pts',(-40.,-63.5312736349196,-172.409726298163));
#147738=CARTESIAN_POINT('Ctrl Pts',(-40.,-64.0887028854776,-172.257328160063));
#147739=CARTESIAN_POINT('Ctrl Pts',(-39.4304134495212,-63.6329935198199,
-172.51902671195));
#147740=CARTESIAN_POINT('Ctrl Pts',(-40.,-63.5529433505843,-172.529650273728));
#147741=CARTESIAN_POINT('Ctrl Pts',(-40.,-64.1281275541786,-172.453565067926));
#147742=CARTESIAN_POINT('Ctrl Pts',(-39.43041344952,-63.63299351982,-172.64995));
#147743=CARTESIAN_POINT('Ctrl Pts',(-40.,-63.5529433505803,-172.64995));
#147744=CARTESIAN_POINT('Ctrl Pts',(-40.,-64.1281275541908,-172.64995));
#147745=CARTESIAN_POINT('',(-39.5,-62.6133861954129,-171.64995));
#147746=CARTESIAN_POINT('Origin',(-39.5,-62.6133861954129,-171.14995));
#147747=CARTESIAN_POINT('',(-39.5,-63.6281275541908,-172.64995));
#147748=CARTESIAN_POINT('Origin',(-39.5,-64.1281275541908,-172.64995));
#147749=CARTESIAN_POINT('Origin',(-39.5,-64.1281275541908,-172.64995));
#147750=CARTESIAN_POINT('Ctrl Pts',(-39.43041344952,-63.6329935198201,-172.64995));
#147751=CARTESIAN_POINT('Ctrl Pts',(-39.4304134495212,-63.6329935198199,
-172.51902671195));
#147752=CARTESIAN_POINT('Ctrl Pts',(-39.4322246014262,-63.6064558665446,
-172.38820210671));
#147753=CARTESIAN_POINT('Ctrl Pts',(-39.4391962191206,-63.5043052007179,
-172.14633102856));
#147754=CARTESIAN_POINT('Ctrl Pts',(-39.4443539433762,-63.4287323580851,
-172.035403273235));
#147755=CARTESIAN_POINT('Ctrl Pts',(-39.4572358131761,-63.2399825392123,
-171.850283164391));
#147756=CARTESIAN_POINT('Ctrl Pts',(-39.4649548930126,-63.1268797875294,
-171.776163607997));
#147757=CARTESIAN_POINT('Ctrl Pts',(-39.4817858670191,-62.8802662644338,
-171.67597732698));
#147758=CARTESIAN_POINT('Ctrl Pts',(-39.4908895000012,-62.7468765389391,
-171.64995));
#147759=CARTESIAN_POINT('Ctrl Pts',(-39.5,-62.6133861954129,-171.64995));
#147760=CARTESIAN_POINT('Origin',(-39.5,-64.1281275541909,-55.24995));
#147761=CARTESIAN_POINT('Origin',(-39.5,-64.1281275541909,-176.84995));
#147762=CARTESIAN_POINT('Origin',(-40.5,67.7009572055632,-176.84995));
#147763=CARTESIAN_POINT('',(-40.5,-70.08000002,-177.34995));
#147764=CARTESIAN_POINT('Origin',(-40.5,-70.08000002,-176.84995));
#147765=CARTESIAN_POINT('',(-40.5,-63.9875867194884,-177.34995));
#147766=CARTESIAN_POINT('',(-40.5,-73.08000002,-177.34995));
#147767=CARTESIAN_POINT('Ctrl Pts',(-40.,-64.1281275541909,-176.84995));
#147768=CARTESIAN_POINT('Ctrl Pts',(-40.,-64.1281275541799,-176.981217345763));
#147769=CARTESIAN_POINT('Ctrl Pts',(-40.0538865634702,-64.1129810289718,
-177.110943344657));
#147770=CARTESIAN_POINT('Ctrl Pts',(-40.2390066553433,-64.0609471645084,
-177.29606343653));
#147771=CARTESIAN_POINT('Ctrl Pts',(-40.3687326542369,-64.0244835641743,
-177.34995));
#147772=CARTESIAN_POINT('Ctrl Pts',(-40.5,-63.9875867194884,-177.34995));
#147773=CARTESIAN_POINT('Origin',(-40.5,-70.08000002,-174.34995));
#147774=CARTESIAN_POINT('',(-40.5,-73.08000002,-174.34995));
#147775=CARTESIAN_POINT('Origin',(-40.5,-72.58000002,-174.34995));
#147776=CARTESIAN_POINT('Origin',(-40.5,-70.08000002,-174.34995));
#147777=CARTESIAN_POINT('Origin',(-40.5,-72.58000002,-55.24995));
#147778=CARTESIAN_POINT('',(-40.5,-73.08000002,-58.24995));
#147779=CARTESIAN_POINT('Origin',(-40.5,-72.58000002,-58.24995));
#147780=CARTESIAN_POINT('',(-40.5,-73.08000002,-174.34995));
#147781=CARTESIAN_POINT('Origin',(-40.5,-70.08000002,-58.24995));
#147782=CARTESIAN_POINT('Origin',(-40.5,-70.08000002,-58.24995));
#147783=CARTESIAN_POINT('Ctrl Pts',(-40.,-56.2369767507698,-61.4585861992214));
#147784=CARTESIAN_POINT('Ctrl Pts',(-40.,-55.4129915017071,-61.0340816633164));
#147785=CARTESIAN_POINT('Ctrl Pts',(-39.2253966502054,-55.8655297208549,
-61.2672223984414));
#147786=CARTESIAN_POINT('Ctrl Pts',(-40.,-56.2639883391117,-61.4061555156247));
#147787=CARTESIAN_POINT('Ctrl Pts',(-39.9999999999999,-55.5211143346859,
-60.8908068027146));
#147788=CARTESIAN_POINT('Ctrl Pts',(-39.2371501417372,-55.9108514932488,
-61.1623844624743));
#147789=CARTESIAN_POINT('Ctrl Pts',(-40.,-56.3001438773882,-61.3606672793622));
#147790=CARTESIAN_POINT('Ctrl Pts',(-40.0000000000002,-55.6524517483454,
-60.789214714877));
#147791=CARTESIAN_POINT('Ctrl Pts',(-39.2529884923231,-55.9713882406491,
-61.071384516352));
#147792=CARTESIAN_POINT('Ctrl Pts',(-40.,-56.3871674054812,-61.2813159675772));
#147793=CARTESIAN_POINT('Ctrl Pts',(-39.9999999999997,-55.9239397495629,
-60.6499875251594));
#147794=CARTESIAN_POINT('Ctrl Pts',(-39.2917636103596,-56.1160106335832,
-60.9126819775317));
#147795=CARTESIAN_POINT('Ctrl Pts',(-40.,-56.4359944422203,-61.2493819347541));
#147796=CARTESIAN_POINT('Ctrl Pts',(-40.0000000000002,-56.0556314220498,
-60.6123860933136));
#147797=CARTESIAN_POINT('Ctrl Pts',(-39.3137989788887,-56.1967066207402,
-60.8488138257101));
#147798=CARTESIAN_POINT('Ctrl Pts',(-40.,-56.5418574657904,-61.1983186977834));
#147799=CARTESIAN_POINT('Ctrl Pts',(-39.9999999999998,-56.3054150365844,
-60.5765024526906));
#147800=CARTESIAN_POINT('Ctrl Pts',(-39.3624939333409,-56.3700857302443,
-60.7466874393643));
#147801=CARTESIAN_POINT('Ctrl Pts',(-40.,-56.5969271200065,-61.1801504966336));
#147802=CARTESIAN_POINT('Ctrl Pts',(-40.0000000000002,-56.4198805079413,
-60.5763728571923));
#147803=CARTESIAN_POINT('Ctrl Pts',(-39.388248240317,-56.4595484948523,
-60.710350981156));
#147804=CARTESIAN_POINT('Ctrl Pts',(-40.,-56.7105746147406,-61.1558957215692));
#147805=CARTESIAN_POINT('Ctrl Pts',(-39.9999999999997,-56.6330323209014,
-60.5986229708875));
#147806=CARTESIAN_POINT('Ctrl Pts',(-39.4424276189043,-56.6422465976472,
-60.6618414552496));
#147807=CARTESIAN_POINT('Ctrl Pts',(-40.,-56.769502228095,-61.1499499952173));
#147808=CARTESIAN_POINT('Ctrl Pts',(-40.,-56.733312609114,-60.6201312992477));
#147809=CARTESIAN_POINT('Ctrl Pts',(-39.4710352046322,-56.7360252703185,
-60.64995));
#147810=CARTESIAN_POINT('Ctrl Pts',(-40.,-56.8280459100727,-61.14995));
#147811=CARTESIAN_POINT('Ctrl Pts',(-40.,-56.8280459100727,-60.64995));
#147812=CARTESIAN_POINT('Ctrl Pts',(-39.5,-56.8280459100727,-60.64995));
#147813=CARTESIAN_POINT('Origin',(-39.5,-56.2369767507657,-61.4585861992193));
#147814=CARTESIAN_POINT('Ctrl Pts',(-40.,-55.08000002,-66.6681042685293));
#147815=CARTESIAN_POINT('Ctrl Pts',(-39.9999999999999,-54.5800000200005,
-66.6681042685296));
#147816=CARTESIAN_POINT('Ctrl Pts',(-39.5,-54.58000002,-66.6681042685296));
#147817=CARTESIAN_POINT('Ctrl Pts',(-40.,-55.0800000210321,-65.7666038778627));
#147818=CARTESIAN_POINT('Ctrl Pts',(-40.000000000023,-54.5300790303385,
-65.6851286065597));
#147819=CARTESIAN_POINT('Ctrl Pts',(-39.4524759569592,-54.5800000199993,
-65.7323260169345));
#147820=CARTESIAN_POINT('Ctrl Pts',(-40.,-55.1697676396346,-64.8773517277477));
#147821=CARTESIAN_POINT('Ctrl Pts',(-40.,-54.5798306201335,-64.744699921287));
#147822=CARTESIAN_POINT('Ctrl Pts',(-39.4055862633018,-54.6797418208431,
-64.8099001089231));
#147823=CARTESIAN_POINT('Ctrl Pts',(-40.,-55.4484096194251,-63.5638700072085));
#147824=CARTESIAN_POINT('Ctrl Pts',(-40.,-54.7700293023446,-63.3785482937886));
#147825=CARTESIAN_POINT('Ctrl Pts',(-39.336341776171,-54.9893440187367,
-63.4482326198876));
#147826=CARTESIAN_POINT('Ctrl Pts',(-40.,-55.5665711459207,-63.1272943707367));
#147827=CARTESIAN_POINT('Ctrl Pts',(-40.,-54.8613740727702,-62.9031901152049));
#147828=CARTESIAN_POINT('Ctrl Pts',(-39.3133286552319,-55.1206346051679,
-62.9957806797004));
#147829=CARTESIAN_POINT('Ctrl Pts',(-40.,-55.8576823946199,-62.2755058384848));
#147830=CARTESIAN_POINT('Ctrl Pts',(-40.,-55.0944248813133,-61.958211698159));
#147831=CARTESIAN_POINT('Ctrl Pts',(-39.2684369452391,-55.4440915465439,
-62.113263414855));
#147832=CARTESIAN_POINT('Ctrl Pts',(-40.,-56.0300729172808,-61.8601972461309));
#147833=CARTESIAN_POINT('Ctrl Pts',(-39.9999999999954,-55.2406041652953,
-61.4857700511268));
#147834=CARTESIAN_POINT('Ctrl Pts',(-39.2465526403215,-55.635643675915,
-61.6830846593873));
#147835=CARTESIAN_POINT('Ctrl Pts',(-40.,-56.2369767507657,-61.4585861992193));
#147836=CARTESIAN_POINT('Ctrl Pts',(-39.9999999999999,-55.4129915017042,
-61.0340816633138));
#147837=CARTESIAN_POINT('Ctrl Pts',(-39.2253966502057,-55.8655297208508,
-61.2672223984388));
#147838=CARTESIAN_POINT('',(-39.4999999999985,-54.58000002,-66.6681042685273));
#147839=CARTESIAN_POINT('Origin',(-39.5,-55.08000002,-66.6681042685293));
#147840=CARTESIAN_POINT('Ctrl Pts',(-39.4999999999998,-54.58000002,-66.6681042685264));
#147841=CARTESIAN_POINT('Ctrl Pts',(-39.4524759569591,-54.5800000199995,
-65.7323260169324));
#147842=CARTESIAN_POINT('Ctrl Pts',(-39.4055862633018,-54.6797418208433,
-64.8099001089221));
#147843=CARTESIAN_POINT('Ctrl Pts',(-39.3594232718812,-54.8861432861055,
-63.9021217828994));
#147844=CARTESIAN_POINT('Ctrl Pts',(-39.336341776171,-54.9893440187367,
-63.4482326198876));
#147845=CARTESIAN_POINT('Ctrl Pts',(-39.3133286552319,-55.1206346051679,
-62.9957806797004));
#147846=CARTESIAN_POINT('Ctrl Pts',(-39.2908828002355,-55.2823630758559,
-62.5545220472777));
#147847=CARTESIAN_POINT('Ctrl Pts',(-39.2684369452391,-55.4440915465439,
-62.113263414855));
#147848=CARTESIAN_POINT('Ctrl Pts',(-39.2465526403215,-55.635643675915,
-61.6830846593873));
#147849=CARTESIAN_POINT('Ctrl Pts',(-39.2253966502057,-55.8655297208508,
-61.2672223984388));
#147850=CARTESIAN_POINT('Origin',(-39.5,-55.08000002,-55.24995));
#147851=CARTESIAN_POINT('',(-39.500000000001,-54.5800000272407,-165.390538702985));
#147852=CARTESIAN_POINT('Origin',(-39.5,-55.08000002,-165.390538702986));
#147853=CARTESIAN_POINT('',(-39.5,-54.58000002,-65.9723506080548));
#147854=CARTESIAN_POINT('Ctrl Pts',(-40.,-56.6722032836053,-171.341255501002));
#147855=CARTESIAN_POINT('Ctrl Pts',(-40.0000000001137,-55.8041715439994,
-171.924697687766));
#147856=CARTESIAN_POINT('Ctrl Pts',(-39.1858850120268,-56.3494037900291,
-171.558563918009));
#147857=CARTESIAN_POINT('Ctrl Pts',(-40.,-56.2965099144784,-170.777391973768));
#147858=CARTESIAN_POINT('Ctrl Pts',(-39.9999999999143,-55.4797123312201,
-171.269409810123));
#147859=CARTESIAN_POINT('Ctrl Pts',(-39.2155551754103,-55.9319856785339,
-170.974971030089));
#147860=CARTESIAN_POINT('Ctrl Pts',(-40.,-56.0109271117334,-170.180744149099));
#147861=CARTESIAN_POINT('Ctrl Pts',(-39.9999999999952,-55.2256104869306,
-170.571031243329));
#147862=CARTESIAN_POINT('Ctrl Pts',(-39.2469773767058,-55.6146249695499,
-170.357118875318));
#147863=CARTESIAN_POINT('Ctrl Pts',(-40.,-55.6233617621208,-169.121472747772));
#147864=CARTESIAN_POINT('Ctrl Pts',(-40.0000000000031,-54.9053220020434,
-169.365642604229));
#147865=CARTESIAN_POINT('Ctrl Pts',(-39.3027883964039,-55.1839423830242,
-169.259798402231));
#147866=CARTESIAN_POINT('Ctrl Pts',(-40.,-55.4926189390281,-168.669060842998));
#147867=CARTESIAN_POINT('Ctrl Pts',(-39.9999999999966,-54.8025817540441,
-168.87099339974));
#147868=CARTESIAN_POINT('Ctrl Pts',(-39.3266337428489,-55.0386476654379,
-168.790991740383));
#147869=CARTESIAN_POINT('Ctrl Pts',(-40.,-55.2841712278759,-167.745175405929));
#147870=CARTESIAN_POINT('Ctrl Pts',(-40.0000000000032,-54.652921563694,
-167.876994762206));
#147871=CARTESIAN_POINT('Ctrl Pts',(-39.3753411897441,-54.8069842833506,
-167.833305054064));
#147872=CARTESIAN_POINT('Ctrl Pts',(-40.,-55.2073915453443,-167.276463616742));
#147873=CARTESIAN_POINT('Ctrl Pts',(-39.9999999999983,-54.6026909074407,
-167.378313758009));
#147874=CARTESIAN_POINT('Ctrl Pts',(-39.4000576364837,-54.7216476273791,
-167.347287707124));
#147875=CARTESIAN_POINT('Ctrl Pts',(-40.,-55.0850969980186,-166.149497422722));
#147876=CARTESIAN_POINT('Ctrl Pts',(-40.0000000000022,-54.5458436605536,
-166.205385693978));
#147877=CARTESIAN_POINT('Ctrl Pts',(-39.4594926871994,-54.5856996258501,
-166.178289848186));
#147878=CARTESIAN_POINT('Ctrl Pts',(-40.,-55.0636927642167,-165.48708770397));
#147879=CARTESIAN_POINT('Ctrl Pts',(-39.9999999999982,-54.5563796453996,
-165.512919816513));
#147880=CARTESIAN_POINT('Ctrl Pts',(-39.4944321648363,-54.5618858497227,
-165.490853406471));
#147881=CARTESIAN_POINT('Ctrl Pts',(-40.,-55.0922303077977,-164.819732953691));
#147882=CARTESIAN_POINT('Ctrl Pts',(-40.000000000001,-54.6215232574257,
-164.799179282796));
#147883=CARTESIAN_POINT('Ctrl Pts',(-39.5296265256636,-54.5935615132292,
-164.79794189457));
#147884=CARTESIAN_POINT('',(-39.2122208635193,-56.0150383143298,-171.050417704751));
#147885=CARTESIAN_POINT('Origin',(-39.5,-56.3715344108516,-170.85018387548));
#147886=CARTESIAN_POINT('Ctrl Pts',(-39.2122209299349,-56.0150383965967,
-171.050417658543));
#147887=CARTESIAN_POINT('Ctrl Pts',(-39.2176920240228,-55.9502202919629,
-170.942877531713));
#147888=CARTESIAN_POINT('Ctrl Pts',(-39.223270534427,-55.8882949524817,
-170.834314512742));
#147889=CARTESIAN_POINT('Ctrl Pts',(-39.2288829748732,-55.8290588250374,
-170.724845259101));
#147890=CARTESIAN_POINT('Ctrl Pts',(-39.2343962193041,-55.7708696553047,
-170.617310799043));
#147891=CARTESIAN_POINT('Ctrl Pts',(-39.2399426498585,-55.7152747925546,
-170.508901566233));
#147892=CARTESIAN_POINT('Ctrl Pts',(-39.2454989375751,-55.6620831693815,
-170.399696352995));
#147893=CARTESIAN_POINT('Ctrl Pts',(-39.2512051809869,-55.6074559857685,
-170.287543858313));
#147894=CARTESIAN_POINT('Ctrl Pts',(-39.2569220065517,-55.5553628501384,
-170.174551727666));
#147895=CARTESIAN_POINT('Ctrl Pts',(-39.2626691268043,-55.5056090682723,
-170.060774196067));
#147896=CARTESIAN_POINT('Ctrl Pts',(-39.2684162470568,-55.4558552864062,
-169.946996664467));
#147897=CARTESIAN_POINT('Ctrl Pts',(-39.2741940917426,-55.4084403442429,
-169.832433450238));
#147898=CARTESIAN_POINT('Ctrl Pts',(-39.2800617718131,-55.3631904849041,
-169.717111289443));
#147899=CARTESIAN_POINT('Ctrl Pts',(-39.2871522937894,-55.3085104208571,
-169.577755648775));
#147900=CARTESIAN_POINT('Ctrl Pts',(-39.294325000306,-55.2570245901798,
-169.437305122195));
#147901=CARTESIAN_POINT('Ctrl Pts',(-39.3015373451061,-55.2085712742073,
-169.295831576444));
#147902=CARTESIAN_POINT('Ctrl Pts',(-39.3088735883845,-55.1592855947966,
-169.151927703592));
#147903=CARTESIAN_POINT('Ctrl Pts',(-39.3162513066387,-55.1131368408751,
-169.006965058834));
#147904=CARTESIAN_POINT('Ctrl Pts',(-39.3236655900776,-55.0699792255175,
-168.860991534233));
#147905=CARTESIAN_POINT('Ctrl Pts',(-39.3312378630505,-55.0259019728685,
-168.711907487985));
#147906=CARTESIAN_POINT('Ctrl Pts',(-39.338848831729,-54.9849440780085,
-168.561768651607));
#147907=CARTESIAN_POINT('Ctrl Pts',(-39.3465267116663,-54.9469854226183,
-168.410602488952));
#147908=CARTESIAN_POINT('Ctrl Pts',(-39.3481905542304,-54.9387595546668,
-168.377843876194));
#147909=CARTESIAN_POINT('Ctrl Pts',(-39.3498576428533,-54.9306746831772,
-168.345036944899));
#147910=CARTESIAN_POINT('Ctrl Pts',(-39.3515284245708,-54.9227298376717,
-168.312181860565));
#147911=CARTESIAN_POINT('Ctrl Pts',(-39.3614981829113,-54.8753219752868,
-168.116131564091));
#147912=CARTESIAN_POINT('Ctrl Pts',(-39.3715435135549,-54.8330294768335,
-167.918870234154));
#147913=CARTESIAN_POINT('Ctrl Pts',(-39.3816147897886,-54.7957193986694,
-167.72083429289));
#147914=CARTESIAN_POINT('Ctrl Pts',(-39.3923369317758,-54.755998121411,
-167.510000091592));
#147915=CARTESIAN_POINT('Ctrl Pts',(-39.4030889139488,-54.7219231119699,
-167.298287584114));
#147916=CARTESIAN_POINT('Ctrl Pts',(-39.4138599647255,-54.6933495306438,
-167.086193912557));
#147917=CARTESIAN_POINT('Ctrl Pts',(-39.4176831357619,-54.6832073735972,
-167.010911528422));
#147918=CARTESIAN_POINT('Ctrl Pts',(-39.4215091024699,-54.6737585376848,
-166.935580892192));
#147919=CARTESIAN_POINT('Ctrl Pts',(-39.4253385442059,-54.6649972877646,
-166.860223572993));
#147920=CARTESIAN_POINT('Ctrl Pts',(-39.4341538597949,-54.6448290260898,
-166.686752190876));
#147921=CARTESIAN_POINT('Ctrl Pts',(-39.4429806358386,-54.6282782237945,
-166.51292724887));
#147922=CARTESIAN_POINT('Ctrl Pts',(-39.4518268440872,-54.6152997906991,
-166.338743654899));
#147923=CARTESIAN_POINT('Ctrl Pts',(-39.4606992732954,-54.6022828883569,
-166.164043765037));
#147924=CARTESIAN_POINT('Ctrl Pts',(-39.4695921259226,-54.5928597871802,
-165.98898246163));
#147925=CARTESIAN_POINT('Ctrl Pts',(-39.4785063203304,-54.5870365021765,
-165.813559429325));
#147926=CARTESIAN_POINT('Ctrl Pts',(-39.485659909963,-54.5823633495253,
-165.672783457004));
#147927=CARTESIAN_POINT('Ctrl Pts',(-39.4928272584983,-54.5800095666538,
-165.531774511173));
#147928=CARTESIAN_POINT('Ctrl Pts',(-39.5000000000025,-54.5800000489627,
-165.390538702984));
#147929=CARTESIAN_POINT('Ctrl Pts',(-39.2122207971108,-56.0150382320575,
-171.05041775096));
#147930=CARTESIAN_POINT('Ctrl Pts',(-39.9999999999999,-55.5316163075193,
-171.321942247435));
#147931=CARTESIAN_POINT('Ctrl Pts',(-40.,-56.3715344108516,-170.85018387548));
#147932=CARTESIAN_POINT('Ctrl Pts',(-39.2305303132587,-56.0826793050571,
-171.197160563313));
#147933=CARTESIAN_POINT('Ctrl Pts',(-40.0000000000016,-55.7019737694774,
-171.520946951432));
#147934=CARTESIAN_POINT('Ctrl Pts',(-40.,-56.4127345596313,-170.923536275602));
#147935=CARTESIAN_POINT('Ctrl Pts',(-39.2581734308863,-56.1834313742016,
-171.318842218969));
#147936=CARTESIAN_POINT('Ctrl Pts',(-40.0000000000015,-55.9148019306841,
-171.629811017638));
#147937=CARTESIAN_POINT('Ctrl Pts',(-40.,-56.4743979142815,-170.984396086855));
#147938=CARTESIAN_POINT('Ctrl Pts',(-39.3228477027581,-56.4100322256565,
-171.502227500722));
#147939=CARTESIAN_POINT('Ctrl Pts',(-39.9999999999985,-56.2996107654989,
-171.733927689933));
#147940=CARTESIAN_POINT('Ctrl Pts',(-40.,-56.6150166715838,-171.07608877299));
#147941=CARTESIAN_POINT('Ctrl Pts',(-39.3604560080182,-56.5377771955238,
-171.565812105304));
#147942=CARTESIAN_POINT('Ctrl Pts',(-39.9999999999952,-56.4773256662664,
-171.740119136472));
#147943=CARTESIAN_POINT('Ctrl Pts',(-40.,-56.6951614830789,-171.107874245193));
#147944=CARTESIAN_POINT('Ctrl Pts',(-39.399271366643,-56.6641713142699,
-171.60362375617));
#147945=CARTESIAN_POINT('Ctrl Pts',(-40.,-56.6359876224367,-171.723920704753));
#147946=CARTESIAN_POINT('Ctrl Pts',(-40.,-56.7758867300388,-171.126786878085));
#147947=CARTESIAN_POINT('',(-39.3992713666431,-56.66417131427,-171.60362375617));
#147948=CARTESIAN_POINT('Origin',(-39.5,-56.7758867300388,-171.126786878085));
#147949=CARTESIAN_POINT('Ctrl Pts',(-39.3992713666431,-56.66417131427,-171.60362375617));
#147950=CARTESIAN_POINT('Ctrl Pts',(-39.3604560080182,-56.5377771955238,
-171.565812105304));
#147951=CARTESIAN_POINT('Ctrl Pts',(-39.3228477027581,-56.4100322256565,
-171.502227500722));
#147952=CARTESIAN_POINT('Ctrl Pts',(-39.2581734308863,-56.1834313742016,
-171.318842218969));
#147953=CARTESIAN_POINT('Ctrl Pts',(-39.2305303132587,-56.0826793050571,
-171.197160563313));
#147954=CARTESIAN_POINT('Ctrl Pts',(-39.2122207971107,-56.0150382320571,
-171.050417750959));
#147955=CARTESIAN_POINT('Ctrl Pts',(-40.,-56.978215522411,-171.14995));
#147956=CARTESIAN_POINT('Ctrl Pts',(-40.,-56.9782155224109,-171.64995));
#147957=CARTESIAN_POINT('Ctrl Pts',(-39.5,-56.978215522411,-171.64995));
#147958=CARTESIAN_POINT('Ctrl Pts',(-40.,-56.9099188320733,-171.149949989769));
#147959=CARTESIAN_POINT('Ctrl Pts',(-40.000000000001,-56.8683451300554,
-171.685098426659));
#147960=CARTESIAN_POINT('Ctrl Pts',(-39.4660557514084,-56.8721092179034,
-171.64995));
#147961=CARTESIAN_POINT('Ctrl Pts',(-40.,-56.8423993478631,-171.142369716128));
#147962=CARTESIAN_POINT('Ctrl Pts',(-40.0000000000047,-56.7549311731639,
-171.710009011284));
#147963=CARTESIAN_POINT('Ctrl Pts',(-39.4324273161011,-56.7672721138937,
-171.634782634301));
#147964=CARTESIAN_POINT('Ctrl Pts',(-40.,-56.7758867300387,-171.126786878085));
#147965=CARTESIAN_POINT('Ctrl Pts',(-40.,-56.6359876224365,-171.723920704752));
#147966=CARTESIAN_POINT('Ctrl Pts',(-39.399271366643,-56.6641713142698,
-171.60362375617));
#147967=CARTESIAN_POINT('',(-39.5,-56.978215522411,-171.64995));
#147968=CARTESIAN_POINT('Origin',(-39.5,-56.978215522411,-171.14995));
#147969=CARTESIAN_POINT('Origin',(-39.9792151682723,-58.6764055302657,-160.124501606025));
#147970=CARTESIAN_POINT('Origin',(-39.5,67.7009572055632,-171.14995));
#147971=CARTESIAN_POINT('',(-39.5,-56.5665827677457,-171.64995));
#147972=CARTESIAN_POINT('Origin',(3.3975957231091E-14,-70.08000002,-58.24995));
#147973=CARTESIAN_POINT('',(-41.,-73.08000002,-58.24995));
#147974=CARTESIAN_POINT('',(41.5,-73.0800000199999,-58.24995));
#147975=CARTESIAN_POINT('Origin',(-41.,-70.08000002,-58.24995));
#147976=CARTESIAN_POINT('Origin',(-41.,-70.08000002,-58.24995));
#147977=CARTESIAN_POINT('Origin',(-41.,-72.58000002,-58.24995));
#147978=CARTESIAN_POINT('Origin',(-42.,-73.08000002,-171.14995));
#147979=CARTESIAN_POINT('Origin',(-42.,-55.58000002,-171.14995));
#147980=CARTESIAN_POINT('Origin',(-42.5,-55.58000002,-177.34995));
#147981=CARTESIAN_POINT('Origin',(-42.5,-55.58000002,-61.14995));
#147982=CARTESIAN_POINT('Origin',(-42.5,-55.58000002,-171.14995));
#147983=CARTESIAN_POINT('Origin',(-42.,-12.9675000200281,-61.14995));
#147984=CARTESIAN_POINT('Origin',(-42.,-56.3473237326805,-61.14995));
#147985=CARTESIAN_POINT('',(-42.,-55.58000002,-60.64995));
#147986=CARTESIAN_POINT('',(-42.,-12.9675000200281,-60.64995));
#147987=CARTESIAN_POINT('Origin',(-42.,-55.58000002,-61.14995));
#147988=CARTESIAN_POINT('Ctrl Pts',(-41.5,-58.6035812240174,-61.14995));
#147989=CARTESIAN_POINT('Ctrl Pts',(-41.5,-58.6035812240174,-60.6498882197787));
#147990=CARTESIAN_POINT('Ctrl Pts',(-42.0000617764046,-58.6035812240174,
-60.6499500038163));
#147991=CARTESIAN_POINT('Ctrl Pts',(-41.5,-58.4156885491981,-61.1499499554112));
#147992=CARTESIAN_POINT('Ctrl Pts',(-41.4999999999964,-58.4568531764755,
-60.7159032420905));
#147993=CARTESIAN_POINT('Ctrl Pts',(-41.9298643117028,-58.4475344566847,
-60.6499412757882));
#147994=CARTESIAN_POINT('Ctrl Pts',(-41.5,-58.2277855029442,-61.1325395579243));
#147995=CARTESIAN_POINT('Ctrl Pts',(-41.5000000000007,-58.2676804549562,
-60.7523419094271));
#147996=CARTESIAN_POINT('Ctrl Pts',(-41.8681695534325,-58.2705723212611,
-60.6499357694868));
#147997=CARTESIAN_POINT('Ctrl Pts',(-41.5,-57.8520667952968,-61.1008454187365));
#147998=CARTESIAN_POINT('Ctrl Pts',(-41.4999999999994,-57.8827900893775,
-60.7882832533183));
#147999=CARTESIAN_POINT('Ctrl Pts',(-41.7820591277972,-57.8880263314595,
-60.6499295039941));
#148000=CARTESIAN_POINT('Ctrl Pts',(-41.5,-57.6641810084401,-61.0874868365943));
#148001=CARTESIAN_POINT('Ctrl Pts',(-41.5000000000007,-57.6764631965609,
-60.7926167355675));
#148002=CARTESIAN_POINT('Ctrl Pts',(-41.7580490411453,-57.6823964313119,
-60.6499285241464));
#148003=CARTESIAN_POINT('Ctrl Pts',(-41.5,-57.2881262594113,-61.0874286718719));
#148004=CARTESIAN_POINT('Ctrl Pts',(-41.4999999999994,-57.2759508310879,
-60.7926435723737));
#148005=CARTESIAN_POINT('Ctrl Pts',(-41.7579337455089,-57.270046180586,
-60.6499285183491));
#148006=CARTESIAN_POINT('Ctrl Pts',(-41.5,-57.0999570266671,-61.1007545617424));
#148007=CARTESIAN_POINT('Ctrl Pts',(-41.5,-57.0692704467339,-60.7883470172518));
#148008=CARTESIAN_POINT('Ctrl Pts',(-41.7818539242553,-57.0640562802561,
-60.6499294916166));
#148009=CARTESIAN_POINT('Ctrl Pts',(-41.5,-56.7235644715484,-61.1324985063765));
#148010=CARTESIAN_POINT('Ctrl Pts',(-41.5,-56.6836417097814,-60.7524277281085));
#148011=CARTESIAN_POINT('Ctrl Pts',(-41.8680165447744,-56.6807474451004,
-60.6499357558287));
#148012=CARTESIAN_POINT('Ctrl Pts',(-41.5,-56.5353526996978,-61.1499499536044));
#148013=CARTESIAN_POINT('Ctrl Pts',(-41.5000000000006,-56.4941497059427,
-60.7159472955962));
#148014=CARTESIAN_POINT('Ctrl Pts',(-41.9298158029953,-56.5034783375499,
-60.6499412695178));
#148015=CARTESIAN_POINT('Ctrl Pts',(-41.5,-56.3473237326805,-61.14995));
#148016=CARTESIAN_POINT('Ctrl Pts',(-41.5,-56.3473237326805,-60.6498882197787));
#148017=CARTESIAN_POINT('Ctrl Pts',(-42.0000617764046,-56.3473237326805,
-60.6499500038163));
#148018=CARTESIAN_POINT('Origin',(-41.,-72.58000002,-4.66002702801304E-15));
#148019=CARTESIAN_POINT('',(-41.,-73.08000002,-174.34995));
#148020=CARTESIAN_POINT('Origin',(-41.,-72.58000002,-174.34995));
#148021=CARTESIAN_POINT('',(-41.,-73.08000002,-58.24995));
#148022=CARTESIAN_POINT('Origin',(-41.,-70.08000002,-174.34995));
#148023=CARTESIAN_POINT('',(-41.,-70.08000002,-177.34995));
#148024=CARTESIAN_POINT('Origin',(-41.,-70.08000002,-176.84995));
#148025=CARTESIAN_POINT('Origin',(-41.,-70.08000002,-174.34995));
#148026=CARTESIAN_POINT('Origin',(-41.,-73.08000002,-176.84995));
#148027=CARTESIAN_POINT('',(-41.,-63.9173163021373,-177.34995));
#148028=CARTESIAN_POINT('',(-41.,-73.08000002,-177.34995));
#148029=CARTESIAN_POINT('Ctrl Pts',(-41.,-63.9173163021373,-177.34995));
#148030=CARTESIAN_POINT('Ctrl Pts',(-41.1312673457634,-63.8804194574513,
-177.34995));
#148031=CARTESIAN_POINT('Ctrl Pts',(-41.2609933446562,-63.8439558571173,
-177.296063436531));
#148032=CARTESIAN_POINT('Ctrl Pts',(-41.4461134365302,-63.7919219926539,
-177.110943344657));
#148033=CARTESIAN_POINT('Ctrl Pts',(-41.5,-63.7767754674458,-176.981217345763));
#148034=CARTESIAN_POINT('Ctrl Pts',(-41.5,-63.7767754674349,-176.84995));
#148035=CARTESIAN_POINT('Origin',(-42.,-63.7767754674349,-171.64995));
#148036=CARTESIAN_POINT('Origin',(-42.,-63.7767754674349,-176.84995));
#148037=CARTESIAN_POINT('Origin',(-42.,-63.7767754674349,-172.64995));
#148038=CARTESIAN_POINT('Ctrl Pts',(-41.9304134495199,-63.2816414330641,
-172.64995));
#148039=CARTESIAN_POINT('Ctrl Pts',(-41.5,-63.3421320985268,-172.64995));
#148040=CARTESIAN_POINT('Ctrl Pts',(-41.5,-63.7767754674349,-172.64995));
#148041=CARTESIAN_POINT('Ctrl Pts',(-41.9304134495211,-63.2816414330639,
-172.51902671195));
#148042=CARTESIAN_POINT('Ctrl Pts',(-41.5,-63.3421320985213,-172.511015867074));
#148043=CARTESIAN_POINT('Ctrl Pts',(-41.5,-63.7767754674226,-172.453565067926));
#148044=CARTESIAN_POINT('Ctrl Pts',(-41.9322246014262,-63.2551037797886,
-172.38820210671));
#148045=CARTESIAN_POINT('Ctrl Pts',(-41.4999999999999,-63.3123764134035,
-172.371853931892));
#148046=CARTESIAN_POINT('Ctrl Pts',(-41.5,-63.7373507987217,-172.257328160063));
#148047=CARTESIAN_POINT('Ctrl Pts',(-41.9391962191206,-63.152953113962,
-172.14633102856));
#148048=CARTESIAN_POINT('Ctrl Pts',(-41.5,-63.1995654042688,-172.118296873734));
#148049=CARTESIAN_POINT('Ctrl Pts',(-41.5,-63.5855944954388,-171.894521542842));
#148050=CARTESIAN_POINT('Ctrl Pts',(-41.9443539433762,-63.0773802713291,
-172.035403273235));
#148051=CARTESIAN_POINT('Ctrl Pts',(-41.500000000002,-63.1159963120049,
-172.003556970023));
#148052=CARTESIAN_POINT('Ctrl Pts',(-41.5,-63.4733225377971,-171.728129909852));
#148053=CARTESIAN_POINT('Ctrl Pts',(-41.9572358131761,-62.8886304524563,
-171.850283164391));
#148054=CARTESIAN_POINT('Ctrl Pts',(-41.499999999998,-62.9115510926292,
-171.817687494207));
#148055=CARTESIAN_POINT('Ctrl Pts',(-41.5,-63.192913452588,-171.450449746589));
#148056=CARTESIAN_POINT('Ctrl Pts',(-41.9649548930126,-62.7755277007723,
-171.776163607997));
#148057=CARTESIAN_POINT('Ctrl Pts',(-41.4999999999999,-62.7899873764732,
-171.746711574348));
#148058=CARTESIAN_POINT('Ctrl Pts',(-41.5,-63.0248865939453,-171.339270411997));
#148059=CARTESIAN_POINT('Ctrl Pts',(-41.981785867019,-62.528914177679,-171.675977326981));
#148060=CARTESIAN_POINT('Ctrl Pts',(-41.5,-62.5315521155723,-171.658003579003));
#148061=CARTESIAN_POINT('Ctrl Pts',(-41.5,-62.6585144680136,-171.18899099047));
#148062=CARTESIAN_POINT('Ctrl Pts',(-41.9908895000012,-62.3955244521823,
-171.64995));
#148063=CARTESIAN_POINT('Ctrl Pts',(-41.4999999999999,-62.3942825374201,
-171.640924254979));
#148064=CARTESIAN_POINT('Ctrl Pts',(-41.5,-62.4603490280314,-171.149950000016));
#148065=CARTESIAN_POINT('Ctrl Pts',(-42.,-62.2620341086569,-171.64995));
#148066=CARTESIAN_POINT('Ctrl Pts',(-41.4999999999999,-62.2620341086569,
-171.64995));
#148067=CARTESIAN_POINT('Ctrl Pts',(-41.5,-62.2620341086569,-171.14995));
#148068=CARTESIAN_POINT('Origin',(-42.,-62.2620341086569,-171.14995));
#148069=CARTESIAN_POINT('Ctrl Pts',(-42.,-62.2620341086569,-171.64995));
#148070=CARTESIAN_POINT('Ctrl Pts',(-41.9908895000012,-62.3955244521823,
-171.64995));
#148071=CARTESIAN_POINT('Ctrl Pts',(-41.981785867019,-62.528914177679,-171.675977326981));
#148072=CARTESIAN_POINT('Ctrl Pts',(-41.9649548930126,-62.7755277007723,
-171.776163607997));
#148073=CARTESIAN_POINT('Ctrl Pts',(-41.9572358131761,-62.8886304524563,
-171.850283164391));
#148074=CARTESIAN_POINT('Ctrl Pts',(-41.9443539433762,-63.0773802713291,
-172.035403273235));
#148075=CARTESIAN_POINT('Ctrl Pts',(-41.9391962191206,-63.152953113962,
-172.14633102856));
#148076=CARTESIAN_POINT('Ctrl Pts',(-41.9322246014262,-63.2551037797886,
-172.38820210671));
#148077=CARTESIAN_POINT('Ctrl Pts',(-41.9304134495211,-63.2816414330639,
-172.51902671195));
#148078=CARTESIAN_POINT('Ctrl Pts',(-41.9304134495199,-63.2816414330641,
-172.64995));
#148079=CARTESIAN_POINT('Origin',(-42.,-73.08000002,-171.14995));
#148080=CARTESIAN_POINT('Ctrl Pts',(-25.2,-65.7473676730093,-61.2659196908482));
#148081=CARTESIAN_POINT('Ctrl Pts',(-25.2,-65.5225267460558,-60.9659777046635));
#148082=CARTESIAN_POINT('Ctrl Pts',(-25.5598256882329,-65.4594929016704,
-60.8818893816965));
#148083=CARTESIAN_POINT('Ctrl Pts',(-25.2,-65.68613088204,-61.3118237091767));
#148084=CARTESIAN_POINT('Ctrl Pts',(-25.1999999999999,-65.4328856316129,
-61.057360567634));
#148085=CARTESIAN_POINT('Ctrl Pts',(-25.5355900377414,-65.3488148482479,
-60.9737014968053));
#148086=CARTESIAN_POINT('Ctrl Pts',(-25.2,-65.635123981304,-61.3698711298632));
#148087=CARTESIAN_POINT('Ctrl Pts',(-25.2,-65.3589455123936,-61.1652193216821));
#148088=CARTESIAN_POINT('Ctrl Pts',(-25.5153438106255,-65.2566822918862,
-61.0897986661581));
#148089=CARTESIAN_POINT('Ctrl Pts',(-25.2,-65.5994372375941,-61.4386408691297));
#148090=CARTESIAN_POINT('Ctrl Pts',(-25.2,-65.3080942147004,-61.2874541854323));
#148091=CARTESIAN_POINT('Ctrl Pts',(-25.5011648721215,-65.1922357602732,
-61.2273317382593));
#148092=CARTESIAN_POINT('Origin',(-25.7,-65.5994372375942,-61.4386408691297));
#148093=CARTESIAN_POINT('Ctrl Pts',(-25.5486065204957,-65.6266003779639,
-171.854014632591));
#148094=CARTESIAN_POINT('Ctrl Pts',(-25.1999999999999,-65.7373527968364,
-171.85401463259));
#148095=CARTESIAN_POINT('Ctrl Pts',(-25.2,-66.1031295107182,-171.854014632589));
#148096=CARTESIAN_POINT('Ctrl Pts',(-25.5332781069629,-65.6314702205409,
-171.740892625582));
#148097=CARTESIAN_POINT('Ctrl Pts',(-25.2,-65.7495636563843,-171.730197187823));
#148098=CARTESIAN_POINT('Ctrl Pts',(-25.2,-66.1031295051642,-171.688945996574));
#148099=CARTESIAN_POINT('Ctrl Pts',(-25.5254918386358,-65.6165368852731,
-171.632443841085));
#148100=CARTESIAN_POINT('Ctrl Pts',(-25.2,-65.7357529125625,-171.605967390697));
#148101=CARTESIAN_POINT('Ctrl Pts',(-25.2,-66.0766766441701,-171.528325399449));
#148102=CARTESIAN_POINT('Ctrl Pts',(-25.5190396326646,-65.5455021430107,
-171.42367336987));
#148103=CARTESIAN_POINT('Ctrl Pts',(-25.1999999999999,-65.6576340206492,
-171.369178819378));
#148104=CARTESIAN_POINT('Ctrl Pts',(-25.2,-65.9668265905144,-171.216885108557));
#148105=CARTESIAN_POINT('Ctrl Pts',(-25.5204167023824,-65.4915081760158,
-171.329224126564));
#148106=CARTESIAN_POINT('Ctrl Pts',(-25.2,-65.5955175213768,-171.261530708485));
#148107=CARTESIAN_POINT('Ctrl Pts',(-25.2,-65.8865499901975,-171.074857506769));
#148108=CARTESIAN_POINT('Ctrl Pts',(-25.5241645957028,-65.4203114663335,
-171.244965273984));
#148109=CARTESIAN_POINT('Ctrl Pts',(-25.1999999999999,-65.5143246899125,
-171.167561256232));
#148110=CARTESIAN_POINT('Ctrl Pts',(-25.2,-65.7816577220592,-170.947457636992));
#148111=CARTESIAN_POINT('Origin',(-25.7,-65.7816577220592,-170.947457636992));
#148112=CARTESIAN_POINT('Ctrl Pts',(-25.2,-65.7246041881209,-170.861259130871));
#148113=CARTESIAN_POINT('Ctrl Pts',(-25.2,-65.4329690822618,-171.012528323755));
#148114=CARTESIAN_POINT('Ctrl Pts',(-25.5015460489969,-65.3172168042439,
-171.07256826174));
#148115=CARTESIAN_POINT('Ctrl Pts',(-25.2,-65.7405566104338,-170.892014084856));
#148116=CARTESIAN_POINT('Ctrl Pts',(-25.2,-65.4555942264487,-171.066917428723));
#148117=CARTESIAN_POINT('Ctrl Pts',(-25.5078751098564,-65.3460382794916,
-171.13407782586));
#148118=CARTESIAN_POINT('Ctrl Pts',(-25.2,-65.7596409576893,-170.920716557309));
#148119=CARTESIAN_POINT('Ctrl Pts',(-25.1999999999994,-65.4828113676634,
-171.118510663779));
#148120=CARTESIAN_POINT('Ctrl Pts',(-25.5154426820321,-65.380521047679,
-171.191481806562));
#148121=CARTESIAN_POINT('Ctrl Pts',(-25.2,-65.7816577220592,-170.947457636992));
#148122=CARTESIAN_POINT('Ctrl Pts',(-25.2,-65.5143246899125,-171.167561256232));
#148123=CARTESIAN_POINT('Ctrl Pts',(-25.5241645957028,-65.4203114663335,
-171.244965273984));
#148124=CARTESIAN_POINT('',(-25.5015460489969,-65.317216804244,-171.07256826174));
#148125=CARTESIAN_POINT('Origin',(-25.7,-65.7246041881209,-170.861259130871));
#148126=CARTESIAN_POINT('Origin',(-25.6922800193975,-66.1910492956378,-170.643493704359));
#148127=CARTESIAN_POINT('Ctrl Pts',(-25.5015460489969,-65.317216804244,
-171.07256826174));
#148128=CARTESIAN_POINT('Ctrl Pts',(-25.2,-65.4329690822618,-171.012528323755));
#148129=CARTESIAN_POINT('Ctrl Pts',(-25.2,-65.7246041881209,-170.861259130871));
#148130=CARTESIAN_POINT('Ctrl Pts',(-25.4919266567716,-62.1578398412392,
-164.972503788787));
#148131=CARTESIAN_POINT('Ctrl Pts',(-25.1999999998579,-62.297876586317,
-164.952133926682));
#148132=CARTESIAN_POINT('Ctrl Pts',(-25.2,-62.5605386715726,-164.761189683274));
#148133=CARTESIAN_POINT('Ctrl Pts',(-25.4809754250192,-58.9585757861229,
-158.893982149016));
#148134=CARTESIAN_POINT('Ctrl Pts',(-25.2,-59.109002613422,-158.883754709366));
#148135=CARTESIAN_POINT('Ctrl Pts',(-25.2,-59.3555677916457,-158.682664145768));
#148136=CARTESIAN_POINT('Ctrl Pts',(-25.4679548160676,-55.6876551762764,
-152.854600597735));
#148137=CARTESIAN_POINT('Ctrl Pts',(-25.2,-55.8110355215084,-152.787619396006));
#148138=CARTESIAN_POINT('Ctrl Pts',(-25.2,-56.0768896606488,-152.643291466864));
#148139=CARTESIAN_POINT('',(-25.4679548160676,-55.6876551762764,-152.854600597735));
#148140=CARTESIAN_POINT('Origin',(-25.7,-56.0768896606488,-152.643291466864));
#148141=CARTESIAN_POINT('Ctrl Pts',(-25.4679548160676,-55.6876551762764,
-152.854600597735));
#148142=CARTESIAN_POINT('Ctrl Pts',(-25.4809753053448,-58.9585758501934,
-158.89398214466));
#148143=CARTESIAN_POINT('Ctrl Pts',(-25.4919265333855,-62.1578399004274,
-164.972503780177));
#148144=CARTESIAN_POINT('Ctrl Pts',(-25.5015460489969,-65.317216804244,
-171.07256826174));
#148145=CARTESIAN_POINT('Ctrl Pts',(-25.2,-55.0810255612707,-148.372593301835));
#148146=CARTESIAN_POINT('Ctrl Pts',(-25.1999999999977,-54.5731343323654,
-148.364947473313));
#148147=CARTESIAN_POINT('Ctrl Pts',(-25.7078909275495,-54.5811410568989,
-148.365051987889));
#148148=CARTESIAN_POINT('Ctrl Pts',(-25.2,-55.0698197461487,-149.14066186414));
#148149=CARTESIAN_POINT('Ctrl Pts',(-25.2000000000109,-54.6032311838736,
-149.141970394971));
#148150=CARTESIAN_POINT('Ctrl Pts',(-25.6652819751675,-54.5686815890185,
-149.174446315097));
#148151=CARTESIAN_POINT('Ctrl Pts',(-25.2,-55.1504277383396,-149.894402552637));
#148152=CARTESIAN_POINT('Ctrl Pts',(-25.1999999999999,-54.719333665426,
-149.93311152841));
#148153=CARTESIAN_POINT('Ctrl Pts',(-25.6231363511229,-54.6582401725082,
-149.967634915182));
#148154=CARTESIAN_POINT('Ctrl Pts',(-25.2,-55.4970587519645,-151.371835493675));
#148155=CARTESIAN_POINT('Ctrl Pts',(-25.2,-55.1489528075744,-151.46123340427));
#148156=CARTESIAN_POINT('Ctrl Pts',(-25.5400582915436,-55.0433748333577,
-151.520527347314));
#148157=CARTESIAN_POINT('Ctrl Pts',(-25.2,-55.7668139911694,-152.10111968119));
#148158=CARTESIAN_POINT('Ctrl Pts',(-25.2,-55.4558433261223,-152.21575400765));
#148159=CARTESIAN_POINT('Ctrl Pts',(-25.4988024926329,-55.3431110792067,
-152.286087899488));
#148160=CARTESIAN_POINT('Ctrl Pts',(-25.2,-56.1447163878713,-152.765324933197));
#148161=CARTESIAN_POINT('Ctrl Pts',(-25.2,-55.886418136883,-152.912368886688));
#148162=CARTESIAN_POINT('Ctrl Pts',(-25.4610913766845,-55.7629867532576,
-152.982594400152));
#148163=CARTESIAN_POINT('',(-25.7,-54.58000002,-148.513004346424));
#148164=CARTESIAN_POINT('Origin',(-25.7,-55.08000002,-148.513004346424));
#148165=CARTESIAN_POINT('Ctrl Pts',(-25.7,-54.58000002,-148.513004346424));
#148166=CARTESIAN_POINT('Ctrl Pts',(-25.6920855143309,-54.5800000317253,
-148.663195106218));
#148167=CARTESIAN_POINT('Ctrl Pts',(-25.6841718538579,-54.5836287914609,
-148.812839156877));
#148168=CARTESIAN_POINT('Ctrl Pts',(-25.6762813054516,-54.5907991607014,
-148.961912671116));
#148169=CARTESIAN_POINT('Ctrl Pts',(-25.6682875469831,-54.5980633199066,
-149.112936098834));
#148170=CARTESIAN_POINT('Ctrl Pts',(-25.660316862259,-54.6089618260389,
-149.263374635832));
#148171=CARTESIAN_POINT('Ctrl Pts',(-25.6523724200598,-54.6234496539193,
-149.413223047264));
#148172=CARTESIAN_POINT('Ctrl Pts',(-25.6444353407179,-54.6379240545753,
-149.562932580165));
#148173=CARTESIAN_POINT('Ctrl Pts',(-25.6365236874188,-54.65598091595,-149.712053836966));
#148174=CARTESIAN_POINT('Ctrl Pts',(-25.6286315318916,-54.6776258877763,
-149.860590148905));
#148175=CARTESIAN_POINT('Ctrl Pts',(-25.6207455186128,-54.6992540139137,
-150.009010859101));
#148176=CARTESIAN_POINT('Ctrl Pts',(-25.6128781619883,-54.7244646682897,
-150.156848301768));
#148177=CARTESIAN_POINT('Ctrl Pts',(-25.6050263127155,-54.7533155629583,
-150.304102915368));
#148178=CARTESIAN_POINT('Ctrl Pts',(-25.5971744634426,-54.7821664576269,
-150.451357528967));
#148179=CARTESIAN_POINT('Ctrl Pts',(-25.5893372800479,-54.814657808455,
-150.598030081328));
#148180=CARTESIAN_POINT('Ctrl Pts',(-25.5815267843809,-54.8508978232776,
-150.744106601026));
#148181=CARTESIAN_POINT('Ctrl Pts',(-25.5733098976718,-54.8890234568904,
-150.897783686886));
#148182=CARTESIAN_POINT('Ctrl Pts',(-25.5651918395491,-54.9313235556008,
-151.050969095924));
#148183=CARTESIAN_POINT('Ctrl Pts',(-25.5571115988274,-54.9779166473137,
-151.203276624969));
#148184=CARTESIAN_POINT('Ctrl Pts',(-25.5493889213721,-55.02244792198,-151.348844308081));
#148185=CARTESIAN_POINT('Ctrl Pts',(-25.5417007566369,-55.0709013570447,
-151.49361015005));
#148186=CARTESIAN_POINT('Ctrl Pts',(-25.534031385493,-55.1233796653412,
-151.637208739292));
#148187=CARTESIAN_POINT('Ctrl Pts',(-25.5265369085761,-55.1746612453797,
-151.777532670965));
#148188=CARTESIAN_POINT('Ctrl Pts',(-25.5190603419181,-55.2297869278435,
-151.916742020613));
#148189=CARTESIAN_POINT('Ctrl Pts',(-25.5116243691151,-55.2888416006855,
-152.054467340709));
#148190=CARTESIAN_POINT('Ctrl Pts',(-25.5042409693129,-55.3474787516445,
-152.191218930323));
#148191=CARTESIAN_POINT('Ctrl Pts',(-25.496897587104,-55.4099903172709,
-152.326507400918));
#148192=CARTESIAN_POINT('Ctrl Pts',(-25.4896541364441,-55.4764373972532,
-152.459942269866));
#148193=CARTESIAN_POINT('Ctrl Pts',(-25.4824106857843,-55.5428844772355,
-152.593377138814));
#148194=CARTESIAN_POINT('Ctrl Pts',(-25.4752672708635,-55.613267946895,
-152.724958308978));
#148195=CARTESIAN_POINT('Ctrl Pts',(-25.468320993909,-55.6876143391068,
-152.85426703406));
#148196=CARTESIAN_POINT('Origin',(-25.7,-55.08000002,-55.24995));
#148197=CARTESIAN_POINT('',(-25.7,-54.58000002,-83.5456386250818));
#148198=CARTESIAN_POINT('Origin',(-25.7,-55.08000002,-83.5456386250819));
#148199=CARTESIAN_POINT('',(-25.7,-54.58000002,-147.999168907581));
#148200=CARTESIAN_POINT('Ctrl Pts',(-25.2,-56.0768896606488,-79.4153515046414));
#148201=CARTESIAN_POINT('Ctrl Pts',(-25.2,-55.8110355215084,-79.2710235754997));
#148202=CARTESIAN_POINT('Ctrl Pts',(-25.4679548160676,-55.6876551762764,
-79.2040423737711));
#148203=CARTESIAN_POINT('Ctrl Pts',(-25.2,-55.7330239637487,-80.0487571235243));
#148204=CARTESIAN_POINT('Ctrl Pts',(-25.2,-55.4183788566373,-79.9347575264689));
#148205=CARTESIAN_POINT('Ctrl Pts',(-25.5038900524126,-55.3056215869824,
-79.8682921770632));
#148206=CARTESIAN_POINT('Ctrl Pts',(-25.2,-55.4909001541243,-80.7176024822967));
#148207=CARTESIAN_POINT('Ctrl Pts',(-25.2000000000012,-55.1418983306402,
-80.6264944503603));
#148208=CARTESIAN_POINT('Ctrl Pts',(-25.541710547536,-55.0365557241775,
-80.5705069627783));
#148209=CARTESIAN_POINT('Ctrl Pts',(-25.2,-55.2446154752418,-81.7605756924265));
#148210=CARTESIAN_POINT('Ctrl Pts',(-25.1999999999993,-54.8419593173495,
-81.6877104640905));
#148211=CARTESIAN_POINT('Ctrl Pts',(-25.6003533292375,-54.7629060815823,
-81.666730198729));
#148212=CARTESIAN_POINT('Ctrl Pts',(-25.2,-55.1827439360829,-82.1162012744658));
#148213=CARTESIAN_POINT('Ctrl Pts',(-25.2,-54.7609521776091,-82.0570705103581));
#148214=CARTESIAN_POINT('Ctrl Pts',(-25.6202954530102,-54.6941599265733,
-82.0407267561828));
#148215=CARTESIAN_POINT('Ctrl Pts',(-25.2,-55.1006621337656,-82.8281867002427));
#148216=CARTESIAN_POINT('Ctrl Pts',(-25.2,-54.6393723317538,-82.7989454077316));
#148217=CARTESIAN_POINT('Ctrl Pts',(-25.6600938511042,-54.6029579243694,
-82.7899562024642));
#148218=CARTESIAN_POINT('Ctrl Pts',(-25.2,-55.0800000206675,-83.1859979964978));
#148219=CARTESIAN_POINT('Ctrl Pts',(-25.2,-54.5995766430915,-83.1741390671131));
#148220=CARTESIAN_POINT('Ctrl Pts',(-25.6800320694526,-54.58000002,-83.1667133317899));
#148221=CARTESIAN_POINT('Ctrl Pts',(-25.2,-55.08000002,-83.5456386250819));
#148222=CARTESIAN_POINT('Ctrl Pts',(-25.2,-54.58000002,-83.5456386250818));
#148223=CARTESIAN_POINT('Ctrl Pts',(-25.7,-54.58000002,-83.5456386250819));
#148224=CARTESIAN_POINT('',(-25.4679548160676,-55.6876551762764,-79.2040423737711));
#148225=CARTESIAN_POINT('Origin',(-25.7,-56.0768896606488,-79.4153515046414));
#148226=CARTESIAN_POINT('Ctrl Pts',(-25.4679630512114,-55.687567629395,
-79.2041945974705));
#148227=CARTESIAN_POINT('Ctrl Pts',(-25.5038958305178,-55.3055804804405,
-79.8683994594255));
#148228=CARTESIAN_POINT('Ctrl Pts',(-25.5417135339568,-55.0365417883965,
-80.5705627886394));
#148229=CARTESIAN_POINT('Ctrl Pts',(-25.6003533292375,-54.7629060815823,
-81.666730198729));
#148230=CARTESIAN_POINT('Ctrl Pts',(-25.6202954530102,-54.6941599265733,
-82.0407267561828));
#148231=CARTESIAN_POINT('Ctrl Pts',(-25.6600938511042,-54.6029579243694,
-82.7899562024642));
#148232=CARTESIAN_POINT('Ctrl Pts',(-25.6800320694526,-54.58000002,-83.1667133317899));
#148233=CARTESIAN_POINT('Ctrl Pts',(-25.7,-54.58000002,-83.5456386250818));
#148234=CARTESIAN_POINT('Ctrl Pts',(-25.4679548160676,-55.6876551762764,
-79.2040423737711));
#148235=CARTESIAN_POINT('Ctrl Pts',(-25.2,-55.8110355215084,-79.2710235754996));
#148236=CARTESIAN_POINT('Ctrl Pts',(-25.2,-56.0768896606488,-79.4153515046414));
#148237=CARTESIAN_POINT('Ctrl Pts',(-25.4808037502955,-58.9154492031739,
-73.2442891352868));
#148238=CARTESIAN_POINT('Ctrl Pts',(-25.2000000000118,-59.0651351497249,
-73.255975182323));
#148239=CARTESIAN_POINT('Ctrl Pts',(-25.2,-59.3123390931711,-73.4556067153995));
#148240=CARTESIAN_POINT('Ctrl Pts',(-25.4916367264251,-62.0734180747052,
-67.2463887183684));
#148241=CARTESIAN_POINT('Ctrl Pts',(-25.200000000035,-62.2130344026582,
-67.2677845851136));
#148242=CARTESIAN_POINT('Ctrl Pts',(-25.2,-62.4759645157842,-67.4577026174502));
#148243=CARTESIAN_POINT('Ctrl Pts',(-25.5011648721215,-65.1922357602732,
-61.2273317382594));
#148244=CARTESIAN_POINT('Ctrl Pts',(-25.1999999999999,-65.3080942147003,
-61.2874541854323));
#148245=CARTESIAN_POINT('Ctrl Pts',(-25.2,-65.5994372375941,-61.4386408691297));
#148246=CARTESIAN_POINT('Ctrl Pts',(-25.5011648721215,-65.1922357602732,
-61.2273317382593));
#148247=CARTESIAN_POINT('Ctrl Pts',(-25.4916365654323,-62.0734181517779,
-67.2463887301796));
#148248=CARTESIAN_POINT('Ctrl Pts',(-25.4808035940994,-58.9154492864362,
-73.2442891417871));
#148249=CARTESIAN_POINT('Ctrl Pts',(-25.4679548160676,-55.6876551762764,
-79.2040423737711));
#148250=CARTESIAN_POINT('Origin',(-24.7,-72.58000002,-55.24995));
#148251=CARTESIAN_POINT('',(-24.7,-73.08000002,-174.34995));
#148252=CARTESIAN_POINT('Origin',(-24.7,-72.58000002,-174.34995));
#148253=CARTESIAN_POINT('',(-24.7,-73.08000002,-58.24995));
#148254=CARTESIAN_POINT('Origin',(-24.7,-70.08000002,-174.34995));
#148255=CARTESIAN_POINT('Origin',(-24.7,-70.08000002,-174.34995));
#148256=CARTESIAN_POINT('Origin',(0.,-12.9675000200281,-60.64995));
#148257=CARTESIAN_POINT('',(-31.0842852491212,-55.9092501930852,-72.1786663403248));
#148258=CARTESIAN_POINT('Ctrl Pts',(-25.4683317116696,-55.6876147551788,
-79.2043632317979));
#148259=CARTESIAN_POINT('Ctrl Pts',(-27.4082623732412,-55.7634597160082,
-76.9351801749559));
#148260=CARTESIAN_POINT('Ctrl Pts',(-29.2789232576535,-55.8380366706268,
-74.5726148012184));
#148261=CARTESIAN_POINT('Ctrl Pts',(-31.0842854210862,-55.9092502160976,
-72.1786665455479));
#148262=CARTESIAN_POINT('Ctrl Pts',(-31.0842850915596,-55.9092502513102,
-72.178666283495));
#148263=CARTESIAN_POINT('Ctrl Pts',(-31.0926997270338,-57.9933062771889,
-68.5477739115119));
#148264=CARTESIAN_POINT('Ctrl Pts',(-31.1003697028526,-60.0396054894506,
-64.8950530444828));
#148265=CARTESIAN_POINT('Ctrl Pts',(-31.1074520910898,-62.0598503138784,
-61.2273317382593));
#148266=CARTESIAN_POINT('Ctrl Pts',(-31.85,-62.4426282692183,-61.4386408691297));
#148267=CARTESIAN_POINT('Ctrl Pts',(-31.8499999999999,-61.6992317916067,
-61.028255523305));
#148268=CARTESIAN_POINT('Ctrl Pts',(-31.1074520910898,-62.0598503138784,
-61.2273317382593));
#148269=CARTESIAN_POINT('Ctrl Pts',(-31.85,-62.4685470764636,-61.3916901534439));
#148270=CARTESIAN_POINT('Ctrl Pts',(-31.8500000000001,-61.7930681218295,
-60.9114185604269));
#148271=CARTESIAN_POINT('Ctrl Pts',(-31.1192593280084,-62.1041984096607,
-61.1334442002736));
#148272=CARTESIAN_POINT('Ctrl Pts',(-31.85,-62.5015432853809,-61.3504740791978));
#148273=CARTESIAN_POINT('Ctrl Pts',(-31.8499999999998,-61.9033127772783,
-60.8239692453656));
#148274=CARTESIAN_POINT('Ctrl Pts',(-31.1342845229578,-62.1606836378221,
-61.0509981549565));
#148275=CARTESIAN_POINT('Ctrl Pts',(-31.85,-62.5794711033445,-61.2778158898142));
#148276=CARTESIAN_POINT('Ctrl Pts',(-31.8500000000002,-62.1341758421231,
-60.6961222616711));
#148277=CARTESIAN_POINT('Ctrl Pts',(-31.1697097530512,-62.2941363459118,
-60.9056817830676));
#148278=CARTESIAN_POINT('Ctrl Pts',(-31.85,-62.6234753527752,-61.2474602210686));
#148279=CARTESIAN_POINT('Ctrl Pts',(-31.8500000000001,-62.2503354665,-60.6558084251244));
#148280=CARTESIAN_POINT('Ctrl Pts',(-31.1896892584046,-62.369523292851,
-60.8449704353912));
#148281=CARTESIAN_POINT('Ctrl Pts',(-31.85,-62.765153261125,-61.1743645550205));
#148282=CARTESIAN_POINT('Ctrl Pts',(-31.8499999999996,-62.5772240699999,
-60.5884818802849));
#148283=CARTESIAN_POINT('Ctrl Pts',(-31.2539016024624,-62.6123775685824,
-60.6987791235328));
#148284=CARTESIAN_POINT('Ctrl Pts',(-31.85,-62.8714721065165,-61.1499500118284));
#148285=CARTESIAN_POINT('Ctrl Pts',(-31.85,-62.7861985042763,-60.599633723582));
#148286=CARTESIAN_POINT('Ctrl Pts',(-31.3019361194217,-62.7947963971694,
-60.64995));
#148287=CARTESIAN_POINT('Ctrl Pts',(-31.85,-62.9782728042642,-61.14995));
#148288=CARTESIAN_POINT('Ctrl Pts',(-31.8499999999999,-62.9782728042642,
-60.64995));
#148289=CARTESIAN_POINT('Ctrl Pts',(-31.35,-62.9782728042642,-60.64995));
#148290=CARTESIAN_POINT('Origin',(-31.35,-62.4426282692182,-61.4386408691297));
#148291=CARTESIAN_POINT('Origin',(-31.35,-62.9782728042642,-61.14995));
#148292=CARTESIAN_POINT('Origin',(-31.35,67.7009572055632,-61.14995));
#148293=CARTESIAN_POINT('Ctrl Pts',(-31.1074520910898,-62.0598503138784,
-61.2273317382593));
#148294=CARTESIAN_POINT('Ctrl Pts',(-31.85,-61.6992317916068,-61.0282555233051));
#148295=CARTESIAN_POINT('Ctrl Pts',(-31.85,-62.4426282692182,-61.4386408691297));
#148296=CARTESIAN_POINT('Ctrl Pts',(-31.1003696873064,-60.0396054978548,
-64.8950530477878));
#148297=CARTESIAN_POINT('Ctrl Pts',(-31.8500000000147,-59.6343590655212,
-64.7356884621635));
#148298=CARTESIAN_POINT('Ctrl Pts',(-31.85,-60.4178950612392,-65.1063632921145));
#148299=CARTESIAN_POINT('Ctrl Pts',(-31.0926997115701,-57.9933062860146,
-68.5477739147732));
#148300=CARTESIAN_POINT('Ctrl Pts',(-31.85,-57.56108933629,-68.3880588333245));
#148301=CARTESIAN_POINT('Ctrl Pts',(-31.85,-58.3664713365843,-68.7590848262753));
#148302=CARTESIAN_POINT('Ctrl Pts',(-31.0842850915597,-55.9092502513102,
-72.178666283495));
#148303=CARTESIAN_POINT('Ctrl Pts',(-31.85,-55.4929314270087,-71.9390096071439));
#148304=CARTESIAN_POINT('Ctrl Pts',(-31.85,-56.2763252281792,-72.3899754143654));
#148305=CARTESIAN_POINT('Origin',(-31.35,-56.2763252281792,-72.3899754143654));
#148306=CARTESIAN_POINT('Ctrl Pts',(-31.85,-55.08000002,-77.227263173365));
#148307=CARTESIAN_POINT('Ctrl Pts',(-31.85,-54.5800000200009,-77.2272631733658));
#148308=CARTESIAN_POINT('Ctrl Pts',(-31.3500000000009,-54.58000002,-77.2272631733658));
#148309=CARTESIAN_POINT('Ctrl Pts',(-31.85,-55.0800000215433,-76.3831770294161));
#148310=CARTESIAN_POINT('Ctrl Pts',(-31.85,-54.5315963664815,-76.3014537863538));
#148311=CARTESIAN_POINT('Ctrl Pts',(-31.3038531467957,-54.5800000199985,
-76.3446192991014));
#148312=CARTESIAN_POINT('Ctrl Pts',(-31.85,-55.1744276549191,-75.5528673220433));
#148313=CARTESIAN_POINT('Ctrl Pts',(-31.85,-54.5888070575115,-75.4165208091089));
#148314=CARTESIAN_POINT('Ctrl Pts',(-31.258313471615,-54.6849196157793,
-75.4773117729577));
#148315=CARTESIAN_POINT('Ctrl Pts',(-31.85,-55.4647382256782,-74.3299545388963));
#148316=CARTESIAN_POINT('Ctrl Pts',(-31.85,-54.7984161464127,-74.129239130374));
#148317=CARTESIAN_POINT('Ctrl Pts',(-31.1911093410829,-55.0074869144856,
-74.2010813719198));
#148318=CARTESIAN_POINT('Ctrl Pts',(-31.85,-55.5878027790484,-73.9239717796963));
#148319=CARTESIAN_POINT('Ctrl Pts',(-31.85,-54.8981200391591,-73.6821630179211));
#148320=CARTESIAN_POINT('Ctrl Pts',(-31.1687759778426,-55.1442253086702,
-73.7776011027959));
#148321=CARTESIAN_POINT('Ctrl Pts',(-31.85,-55.8881616831611,-73.1379857970122));
#148322=CARTESIAN_POINT('Ctrl Pts',(-31.85,-55.1503671712329,-72.798619733739));
#148323=CARTESIAN_POINT('Ctrl Pts',(-31.1255062785665,-55.4779574226737,
-72.9580899132975));
#148324=CARTESIAN_POINT('Ctrl Pts',(-31.85,-56.0652689851553,-72.7566110978467));
#148325=CARTESIAN_POINT('Ctrl Pts',(-31.8500000000028,-55.3074747056296,
-72.358974665281));
#148326=CARTESIAN_POINT('Ctrl Pts',(-31.1044941422599,-55.6747504070549,
-72.5606146570313));
#148327=CARTESIAN_POINT('Ctrl Pts',(-31.85,-56.2763252281792,-72.3899754143654));
#148328=CARTESIAN_POINT('Ctrl Pts',(-31.85,-55.4929314270087,-71.9390096071439));
#148329=CARTESIAN_POINT('Ctrl Pts',(-31.0842850915597,-55.9092502513102,
-72.178666283495));
#148330=CARTESIAN_POINT('',(-31.3499999999941,-54.58000002,-77.227263173365));
#148331=CARTESIAN_POINT('Origin',(-31.35,-55.08000002,-77.2272631733642));
#148332=CARTESIAN_POINT('Ctrl Pts',(-31.3500000000009,-54.58000002,-77.227263173365));
#148333=CARTESIAN_POINT('Ctrl Pts',(-31.3038531467958,-54.5800000199986,
-76.3446192991009));
#148334=CARTESIAN_POINT('Ctrl Pts',(-31.2583134716152,-54.6849196157794,
-75.4773117729574));
#148335=CARTESIAN_POINT('Ctrl Pts',(-31.2135107179272,-54.8999644815834,
-74.6264915055991));
#148336=CARTESIAN_POINT('Ctrl Pts',(-31.1911093410832,-55.0074869144855,
-74.2010813719198));
#148337=CARTESIAN_POINT('Ctrl Pts',(-31.1687759778429,-55.1442253086701,
-73.7776011027959));
#148338=CARTESIAN_POINT('Ctrl Pts',(-31.147141128205,-55.3110913656718,
-73.3678455080466));
#148339=CARTESIAN_POINT('Ctrl Pts',(-31.125506279948,-55.4779574120224,
-72.9580899394523));
#148340=CARTESIAN_POINT('Ctrl Pts',(-31.1044941449429,-55.6747503819319,
-72.5606147077732));
#148341=CARTESIAN_POINT('Ctrl Pts',(-31.0842850954301,-55.9092502064053,
-72.1786663566345));
#148342=CARTESIAN_POINT('Origin',(-31.35,-55.08000002,-55.24995));
#148343=CARTESIAN_POINT('',(-31.3500000000014,-54.5800000295902,-154.831379798157));
#148344=CARTESIAN_POINT('Origin',(-31.35,-55.08000002,-154.831379798159));
#148345=CARTESIAN_POINT('',(-31.35,-54.58000002,-76.6255854122387));
#148346=CARTESIAN_POINT('Ctrl Pts',(-31.85,-56.5198937114388,-160.061984623621));
#148347=CARTESIAN_POINT('Ctrl Pts',(-31.8500000000001,-55.7195063092811,
-160.597458213624));
#148348=CARTESIAN_POINT('Ctrl Pts',(-31.0622729759187,-56.1800587903026,
-160.289522595203));
#148349=CARTESIAN_POINT('Ctrl Pts',(-31.85,-56.196322380357,-159.575614753933));
#148350=CARTESIAN_POINT('Ctrl Pts',(-31.8499999999999,-55.4302476503449,
-160.032901980985));
#148351=CARTESIAN_POINT('Ctrl Pts',(-31.0890805685714,-55.8205456059185,
-159.783030537725));
#148352=CARTESIAN_POINT('Ctrl Pts',(-31.85,-55.9428521111973,-159.062977148996));
#148353=CARTESIAN_POINT('Ctrl Pts',(-31.85,-55.1997164518874,-159.434441959105));
#148354=CARTESIAN_POINT('Ctrl Pts',(-31.1173271740076,-55.5388836657292,
-159.248854752969));
#148355=CARTESIAN_POINT('Ctrl Pts',(-31.85,-55.5903137943537,-158.141820520556));
#148356=CARTESIAN_POINT('Ctrl Pts',(-31.8499999999999,-54.8995758370652,
-158.384410590095));
#148357=CARTESIAN_POINT('Ctrl Pts',(-31.1680335221376,-55.1471418726124,
-158.288448312723));
#148358=CARTESIAN_POINT('Ctrl Pts',(-31.85,-55.4683430012288,-157.741722853926));
#148359=CARTESIAN_POINT('Ctrl Pts',(-31.8499999999999,-54.8007327275664,
-157.943927818991));
#148360=CARTESIAN_POINT('Ctrl Pts',(-31.1900434374137,-55.0116036525937,
-157.87112199741));
#148361=CARTESIAN_POINT('Ctrl Pts',(-31.85,-55.2730856891008,-156.923456306516));
#148362=CARTESIAN_POINT('Ctrl Pts',(-31.8499999999999,-54.6553685473472,
-157.056547547799));
#148363=CARTESIAN_POINT('Ctrl Pts',(-31.2350144161398,-54.7946179131854,
-157.017203864823));
#148364=CARTESIAN_POINT('Ctrl Pts',(-31.85,-55.2005310139637,-156.507030856831));
#148365=CARTESIAN_POINT('Ctrl Pts',(-31.8500000000015,-54.6061056306454,
-156.61011452235));
#148366=CARTESIAN_POINT('Ctrl Pts',(-31.2578793589119,-54.7139857241292,
-156.582429725824));
#148367=CARTESIAN_POINT('Ctrl Pts',(-31.85,-55.0867689945819,-155.521921774446));
#148368=CARTESIAN_POINT('Ctrl Pts',(-31.8499999999981,-54.5497265489757,
-155.574697108694));
#148369=CARTESIAN_POINT('Ctrl Pts',(-31.3119027856115,-54.5875443127981,
-155.553382086724));
#148370=CARTESIAN_POINT('Ctrl Pts',(-31.85,-55.0656087290325,-154.94924650253));
#148371=CARTESIAN_POINT('Ctrl Pts',(-31.8500000000013,-54.5573584552804,
-154.971890850079));
#148372=CARTESIAN_POINT('Ctrl Pts',(-31.3432560810077,-54.5640138310673,
-154.954760169123));
#148373=CARTESIAN_POINT('Ctrl Pts',(-31.85,-55.0895347934625,-154.371949728242));
#148374=CARTESIAN_POINT('Ctrl Pts',(-31.8499999999992,-54.6141856226549,
-154.351866222665));
#148375=CARTESIAN_POINT('Ctrl Pts',(-31.3747904412016,-54.590578610047,
-154.350869818715));
#148376=CARTESIAN_POINT('',(-31.084285288415,-55.9092502162754,-159.879976566996));
#148377=CARTESIAN_POINT('Origin',(-31.35,-56.2763252281792,-159.66866755714));
#148378=CARTESIAN_POINT('Ctrl Pts',(-31.0842854211463,-55.9092502161047,
-159.87997642591));
#148379=CARTESIAN_POINT('Ctrl Pts',(-31.0896514277362,-55.8469879056698,
-159.77856394342));
#148380=CARTESIAN_POINT('Ctrl Pts',(-31.095109779591,-55.7874666718174,
-159.676149018302));
#148381=CARTESIAN_POINT('Ctrl Pts',(-31.1006032503633,-55.7305129240826,
-159.572833254483));
#148382=CARTESIAN_POINT('Ctrl Pts',(-31.1061823346791,-55.672671574981,
-159.46790735583));
#148383=CARTESIAN_POINT('Ctrl Pts',(-31.1117978298489,-55.6174776776756,
-159.362052199246));
#148384=CARTESIAN_POINT('Ctrl Pts',(-31.1174329116102,-55.5647534325291,
-159.255340693208));
#148385=CARTESIAN_POINT('Ctrl Pts',(-31.1231991622453,-55.5108019150638,
-159.146145243073));
#148386=CARTESIAN_POINT('Ctrl Pts',(-31.1289861521601,-55.4594356856543,
-159.036052959027));
#148387=CARTESIAN_POINT('Ctrl Pts',(-31.1348175145198,-55.4104789077723,
-158.925109188129));
#148388=CARTESIAN_POINT('Ctrl Pts',(-31.1388264610931,-55.3768220888628,
-158.848837534484));
#148389=CARTESIAN_POINT('Ctrl Pts',(-31.1428572605651,-55.3443043684264,
-158.772162749669));
#148390=CARTESIAN_POINT('Ctrl Pts',(-31.1469275973672,-55.3128748584107,
-158.695091598692));
#148391=CARTESIAN_POINT('Ctrl Pts',(-31.1539498174176,-55.2586520886162,
-158.562127028925));
#148392=CARTESIAN_POINT('Ctrl Pts',(-31.1610514741968,-55.2076908016112,
-158.427997684076));
#148393=CARTESIAN_POINT('Ctrl Pts',(-31.1681970280243,-55.159847533947,
-158.292768518215));
#148394=CARTESIAN_POINT('Ctrl Pts',(-31.1755499129171,-55.1106160749836,
-158.153615624719));
#148395=CARTESIAN_POINT('Ctrl Pts',(-31.1829497326462,-55.0646854243966,
-158.013297832529));
#148396=CARTESIAN_POINT('Ctrl Pts',(-31.1903953483088,-55.0219287506999,
-157.871856051504));
#148397=CARTESIAN_POINT('Ctrl Pts',(-31.1978409639714,-54.9791720770031,
-157.73041427048));
#148398=CARTESIAN_POINT('Ctrl Pts',(-31.205333071078,-54.9395888987774,
-157.587847970466));
#148399=CARTESIAN_POINT('Ctrl Pts',(-31.2128985676693,-54.9030908083614,
-157.4441753669));
#148400=CARTESIAN_POINT('Ctrl Pts',(-31.222941383244,-54.854641432111,-157.253457223902));
#148401=CARTESIAN_POINT('Ctrl Pts',(-31.233071348161,-54.8117414293067,
-157.061174547668));
#148402=CARTESIAN_POINT('Ctrl Pts',(-31.2432320500935,-54.7743373143562,
-156.867957719114));
#148403=CARTESIAN_POINT('Ctrl Pts',(-31.2539055300877,-54.7350455336035,
-156.664989856478));
#148404=CARTESIAN_POINT('Ctrl Pts',(-31.2646128592783,-54.7018177706184,
-156.460991131094));
#148405=CARTESIAN_POINT('Ctrl Pts',(-31.2753335192659,-54.6745648754831,
-156.25666969964));
#148406=CARTESIAN_POINT('Ctrl Pts',(-31.2772548724241,-54.6696806205773,
-156.220051279873));
#148407=CARTESIAN_POINT('Ctrl Pts',(-31.2791767652949,-54.6649882224971,
-156.183422440874));
#148408=CARTESIAN_POINT('Ctrl Pts',(-31.2810992223836,-54.6604871030235,
-156.146787191114));
#148409=CARTESIAN_POINT('Ctrl Pts',(-31.2894544615779,-54.6409246742618,
-155.987565809011));
#148410=CARTESIAN_POINT('Ctrl Pts',(-31.2978181349023,-54.6249422843353,
-155.827972968174));
#148411=CARTESIAN_POINT('Ctrl Pts',(-31.3061986924678,-54.6125104976354,
-155.668000735124));
#148412=CARTESIAN_POINT('Ctrl Pts',(-31.3145757427008,-54.6000839137411,
-155.508095451776));
#148413=CARTESIAN_POINT('Ctrl Pts',(-31.3229704705527,-54.5912052112514,
-155.347810416513));
#148414=CARTESIAN_POINT('Ctrl Pts',(-31.3313828706828,-54.5858956626337,
-155.187144207599));
#148415=CARTESIAN_POINT('Ctrl Pts',(-31.337581338876,-54.5819834535472,
-155.068761300189));
#148416=CARTESIAN_POINT('Ctrl Pts',(-31.3437892685361,-54.5800100820981,
-154.950171544755));
#148417=CARTESIAN_POINT('Ctrl Pts',(-31.3500000000037,-54.5800000583607,
-154.831379798155));
#148418=CARTESIAN_POINT('Ctrl Pts',(-31.0842850915597,-55.9092502513102,
-159.879976688011));
#148419=CARTESIAN_POINT('Ctrl Pts',(-31.8499999999999,-55.4929314270088,
-160.119633364362));
#148420=CARTESIAN_POINT('Ctrl Pts',(-31.85,-56.2763252281792,-159.66866755714));
#148421=CARTESIAN_POINT('Ctrl Pts',(-31.0928842088245,-58.0390008802754,
-163.590479273921));
#148422=CARTESIAN_POINT('Ctrl Pts',(-31.8500000000438,-57.6056192097127,
-163.747040286917));
#148423=CARTESIAN_POINT('Ctrl Pts',(-31.85,-58.4122993941661,-163.37916820794));
#148424=CARTESIAN_POINT('Ctrl Pts',(-31.1007058108654,-60.129339000976,
-167.323759171684));
#148425=CARTESIAN_POINT('Ctrl Pts',(-31.8499999999999,-59.7238064590067,
-167.480553670321));
#148426=CARTESIAN_POINT('Ctrl Pts',(-31.85,-60.5078533703316,-167.112448841938));
#148427=CARTESIAN_POINT('Ctrl Pts',(-31.1079170675507,-62.1926886331265,
-171.07256826174));
#148428=CARTESIAN_POINT('Ctrl Pts',(-31.8499999999999,-61.8331341426276,
-171.27090462831));
#148429=CARTESIAN_POINT('Ctrl Pts',(-31.85,-62.5757608260975,-170.861259130871));
#148430=CARTESIAN_POINT('',(-31.1079170675507,-62.1926886331265,-171.07256826174));
#148431=CARTESIAN_POINT('Origin',(-31.35,-62.5757608260974,-170.861259130871));
#148432=CARTESIAN_POINT('Ctrl Pts',(-31.1079170675507,-62.1926886331265,
-171.07256826174));
#148433=CARTESIAN_POINT('Ctrl Pts',(-31.1007058117848,-60.1293390004784,
-167.323759171876));
#148434=CARTESIAN_POINT('Ctrl Pts',(-31.092884209739,-58.0390008797519,
-163.59047927411));
#148435=CARTESIAN_POINT('Ctrl Pts',(-31.0842850915597,-55.9092502513102,
-159.879976688011));
#148436=CARTESIAN_POINT('Ctrl Pts',(-31.85,-63.1109998882233,-171.14995));
#148437=CARTESIAN_POINT('Ctrl Pts',(-31.8499999999999,-63.1109998882232,
-171.64995));
#148438=CARTESIAN_POINT('Ctrl Pts',(-31.35,-63.1109998882233,-171.64995));
#148439=CARTESIAN_POINT('Ctrl Pts',(-31.85,-63.0574084096236,-171.149949978884));
#148440=CARTESIAN_POINT('Ctrl Pts',(-31.8499999999969,-63.0165988837716,
-171.67463547811));
#148441=CARTESIAN_POINT('Ctrl Pts',(-31.3259104704307,-63.0188778416583,
-171.64995));
#148442=CARTESIAN_POINT('Ctrl Pts',(-31.85,-63.0049471542817,-171.14386632127));
#148443=CARTESIAN_POINT('Ctrl Pts',(-31.8500000000009,-62.9206095930479,
-171.689168561081));
#148444=CARTESIAN_POINT('Ctrl Pts',(-31.3022843203587,-62.9287506782315,
-171.637782628619));
#148445=CARTESIAN_POINT('Ctrl Pts',(-31.85,-62.9022833467989,-171.11979081221));
#148446=CARTESIAN_POINT('Ctrl Pts',(-31.8499999999991,-62.7178130579107,
-171.697646145438));
#148447=CARTESIAN_POINT('Ctrl Pts',(-31.2559687677351,-62.752470972064,
-171.58963163834));
#148448=CARTESIAN_POINT('Ctrl Pts',(-31.85,-62.8513307506207,-171.101350238814));
#148449=CARTESIAN_POINT('Ctrl Pts',(-31.8499999999999,-62.6084779204031,
-171.690011580914));
#148450=CARTESIAN_POINT('Ctrl Pts',(-31.2329391869239,-62.6650327081311,
-171.552750471208));
#148451=CARTESIAN_POINT('Ctrl Pts',(-31.85,-62.7572432252394,-171.052906534958));
#148452=CARTESIAN_POINT('Ctrl Pts',(-31.85,-62.3853423742397,-171.644110259622));
#148453=CARTESIAN_POINT('Ctrl Pts',(-31.1903462652202,-62.5036508698849,
-171.455863076335));
#148454=CARTESIAN_POINT('Ctrl Pts',(-31.85,-62.7137529944933,-171.02308307076));
#148455=CARTESIAN_POINT('Ctrl Pts',(-31.8499999999993,-62.2707897308557,
-171.604668782303));
#148456=CARTESIAN_POINT('Ctrl Pts',(-31.1706237499557,-62.4290960074683,
-171.396216101863));
#148457=CARTESIAN_POINT('Ctrl Pts',(-31.85,-62.6352107798375,-170.950134506763));
#148458=CARTESIAN_POINT('Ctrl Pts',(-31.8500000000008,-62.0386786747199,
-171.476624739535));
#148459=CARTESIAN_POINT('Ctrl Pts',(-31.1349614654849,-62.2945035389765,
-171.250319053184));
#148460=CARTESIAN_POINT('Ctrl Pts',(-31.85,-62.6016585634489,-170.908207754234));
#148461=CARTESIAN_POINT('Ctrl Pts',(-31.8499999999999,-61.9268239314477,
-171.387766739956));
#148462=CARTESIAN_POINT('Ctrl Pts',(-31.1197024222507,-62.2370348840453,
-171.166463157496));
#148463=CARTESIAN_POINT('Ctrl Pts',(-31.85,-62.5757608260974,-170.861259130871));
#148464=CARTESIAN_POINT('Ctrl Pts',(-31.85,-61.8331341426276,-171.270904628311));
#148465=CARTESIAN_POINT('Ctrl Pts',(-31.1079170675507,-62.1926886331265,
-171.07256826174));
#148466=CARTESIAN_POINT('',(-31.35,-63.1109998882233,-171.64995));
#148467=CARTESIAN_POINT('Origin',(-31.35,-63.1109998882233,-171.14995));
#148468=CARTESIAN_POINT('Ctrl Pts',(-31.35,-63.1109998882233,-171.64995));
#148469=CARTESIAN_POINT('Ctrl Pts',(-31.3259104704307,-63.0188778416583,
-171.64995));
#148470=CARTESIAN_POINT('Ctrl Pts',(-31.3022843203587,-62.9287506782315,
-171.637782628619));
#148471=CARTESIAN_POINT('Ctrl Pts',(-31.2559687677351,-62.752470972064,
-171.58963163834));
#148472=CARTESIAN_POINT('Ctrl Pts',(-31.2329391869239,-62.6650327081311,
-171.552750471208));
#148473=CARTESIAN_POINT('Ctrl Pts',(-31.1903462652202,-62.5036508698849,
-171.455863076335));
#148474=CARTESIAN_POINT('Ctrl Pts',(-31.1706237499557,-62.4290960074683,
-171.396216101863));
#148475=CARTESIAN_POINT('Ctrl Pts',(-31.1349614654849,-62.2945035389765,
-171.250319053184));
#148476=CARTESIAN_POINT('Ctrl Pts',(-31.1197024222507,-62.2370348840453,
-171.166463157496));
#148477=CARTESIAN_POINT('Ctrl Pts',(-31.1079170675507,-62.1926886331265,
-171.07256826174));
#148478=CARTESIAN_POINT('Origin',(-31.35,-12.9675000200281,-171.14995));
#148479=CARTESIAN_POINT('',(-31.35,-63.7587939982373,-171.64995));
#148480=CARTESIAN_POINT('Origin',(-31.35,-63.7587939982373,-171.14995));
#148481=CARTESIAN_POINT('',(-31.35,-62.7949079300497,-171.64995));
#148482=CARTESIAN_POINT('Ctrl Pts',(-31.35,-63.7587939982373,-171.64995));
#148483=CARTESIAN_POINT('Ctrl Pts',(-31.8499999999999,-63.7587939982373,
-171.64995));
#148484=CARTESIAN_POINT('Ctrl Pts',(-31.85,-63.7587939982373,-171.14995));
#148485=CARTESIAN_POINT('Ctrl Pts',(-31.3408895000012,-63.8922843417627,
-171.64995));
#148486=CARTESIAN_POINT('Ctrl Pts',(-31.85,-63.8935759445488,-171.659148653594));
#148487=CARTESIAN_POINT('Ctrl Pts',(-31.85,-63.9571089176128,-171.149950000016));
#148488=CARTESIAN_POINT('Ctrl Pts',(-31.331785867019,-64.0256740672594,
-171.675977326981));
#148489=CARTESIAN_POINT('Ctrl Pts',(-31.85,-64.0229667628024,-171.69520402023));
#148490=CARTESIAN_POINT('Ctrl Pts',(-31.85,-64.1552743575927,-171.18899099047));
#148491=CARTESIAN_POINT('Ctrl Pts',(-31.3149548930126,-64.2722875903527,
-171.776163607997));
#148492=CARTESIAN_POINT('Ctrl Pts',(-31.85,-64.2557455586227,-171.809929875206));
#148493=CARTESIAN_POINT('Ctrl Pts',(-31.85,-64.521646483527,-171.339270411997));
#148494=CARTESIAN_POINT('Ctrl Pts',(-31.3072358131761,-64.3853903420367,
-171.850283164391));
#148495=CARTESIAN_POINT('Ctrl Pts',(-31.850000000002,-64.3583202713598,
-171.888983273332));
#148496=CARTESIAN_POINT('Ctrl Pts',(-31.85,-64.6896733421684,-171.450449746589));
#148497=CARTESIAN_POINT('Ctrl Pts',(-31.2943539433762,-64.5741401609095,
-172.035403273235));
#148498=CARTESIAN_POINT('Ctrl Pts',(-31.8499999999979,-64.5259770425163,
-172.075215659168));
#148499=CARTESIAN_POINT('Ctrl Pts',(-31.85,-64.9700824273775,-171.728129909852));
#148500=CARTESIAN_POINT('Ctrl Pts',(-31.2891962191206,-64.6497130035424,
-172.14633102856));
#148501=CARTESIAN_POINT('Ctrl Pts',(-31.85,-64.590248108326,-172.182182441317));
#148502=CARTESIAN_POINT('Ctrl Pts',(-31.85,-65.0823543850191,-171.894521542842));
#148503=CARTESIAN_POINT('Ctrl Pts',(-31.2822246014263,-64.751863669369,
-172.38820210671));
#148504=CARTESIAN_POINT('Ctrl Pts',(-31.8499999999999,-64.676681437744,
-172.409726298163));
#148505=CARTESIAN_POINT('Ctrl Pts',(-31.85,-65.2341106883021,-172.257328160063));
#148506=CARTESIAN_POINT('Ctrl Pts',(-31.2804134495219,-64.7784013226442,
-172.51902671195));
#148507=CARTESIAN_POINT('Ctrl Pts',(-31.85,-64.6983511534103,-172.529650273729));
#148508=CARTESIAN_POINT('Ctrl Pts',(-31.85,-65.273535357003,-172.453565067926));
#148509=CARTESIAN_POINT('Ctrl Pts',(-31.28041344952,-64.7784013226445,-172.64995));
#148510=CARTESIAN_POINT('Ctrl Pts',(-31.85,-64.6983511534048,-172.64995));
#148511=CARTESIAN_POINT('Ctrl Pts',(-31.85,-65.2735353570153,-172.64995));
#148512=CARTESIAN_POINT('Origin',(-31.35,-65.2735353570153,-172.64995));
#148513=CARTESIAN_POINT('Ctrl Pts',(-31.28041344952,-64.7784013226445,-172.64995));
#148514=CARTESIAN_POINT('Ctrl Pts',(-31.2804134495219,-64.7784013226442,
-172.51902671195));
#148515=CARTESIAN_POINT('Ctrl Pts',(-31.2822246014263,-64.751863669369,
-172.38820210671));
#148516=CARTESIAN_POINT('Ctrl Pts',(-31.2891962191206,-64.6497130035424,
-172.14633102856));
#148517=CARTESIAN_POINT('Ctrl Pts',(-31.2943539433762,-64.5741401609095,
-172.035403273235));
#148518=CARTESIAN_POINT('Ctrl Pts',(-31.3072358131761,-64.3853903420367,
-171.850283164391));
#148519=CARTESIAN_POINT('Ctrl Pts',(-31.3149548930126,-64.2722875903527,
-171.776163607997));
#148520=CARTESIAN_POINT('Ctrl Pts',(-31.331785867019,-64.0256740672594,
-171.675977326981));
#148521=CARTESIAN_POINT('Ctrl Pts',(-31.3408895000012,-63.8922843417627,
-171.64995));
#148522=CARTESIAN_POINT('Ctrl Pts',(-31.35,-63.7587939982373,-171.64995));
#148523=CARTESIAN_POINT('Origin',(-31.35,-65.2735353570153,-171.64995));
#148524=CARTESIAN_POINT('Origin',(-31.35,-65.2735353570153,-176.84995));
#148525=CARTESIAN_POINT('Origin',(-32.35,67.7009572055632,-176.84995));
#148526=CARTESIAN_POINT('',(-32.35,-70.08000002,-177.34995));
#148527=CARTESIAN_POINT('Origin',(-32.35,-70.08000002,-176.84995));
#148528=CARTESIAN_POINT('',(-32.35,-65.1329945223129,-177.34995));
#148529=CARTESIAN_POINT('',(-32.35,-73.08000002,-177.34995));
#148530=CARTESIAN_POINT('Ctrl Pts',(-31.85,-65.2735353570153,-176.84995));
#148531=CARTESIAN_POINT('Ctrl Pts',(-31.85,-65.2735353570043,-176.981217345763));
#148532=CARTESIAN_POINT('Ctrl Pts',(-31.9038865634697,-65.2583888317962,
-177.110943344657));
#148533=CARTESIAN_POINT('Ctrl Pts',(-32.0890066553437,-65.2063549673329,
-177.296063436531));
#148534=CARTESIAN_POINT('Ctrl Pts',(-32.2187326542366,-65.1698913669989,
-177.34995));
#148535=CARTESIAN_POINT('Ctrl Pts',(-32.35,-65.1329945223129,-177.34995));
#148536=CARTESIAN_POINT('Origin',(-32.35,-70.08000002,-174.34995));
#148537=CARTESIAN_POINT('',(-32.35,-73.08000002,-174.34995));
#148538=CARTESIAN_POINT('Origin',(-32.35,-72.58000002,-174.34995));
#148539=CARTESIAN_POINT('Origin',(-32.35,-70.08000002,-174.34995));
#148540=CARTESIAN_POINT('Origin',(-32.35,-72.58000002,-55.24995));
#148541=CARTESIAN_POINT('',(-32.35,-73.08000002,-58.24995));
#148542=CARTESIAN_POINT('Origin',(-32.35,-72.58000002,-58.24995));
#148543=CARTESIAN_POINT('',(-32.35,-73.08000002,-174.34995));
#148544=CARTESIAN_POINT('Origin',(-32.35,-70.08000002,-58.24995));
#148545=CARTESIAN_POINT('Origin',(-32.35,-70.08000002,-58.24995));
#148546=CARTESIAN_POINT('Origin',(3.3975957231091E-14,-70.08000002,-58.24995));
#148547=CARTESIAN_POINT('',(-32.85,-73.08000002,-58.24995));
#148548=CARTESIAN_POINT('Origin',(-32.85,-70.08000002,-58.24995));
#148549=CARTESIAN_POINT('',(41.5,-73.0800000199999,-58.24995));
#148550=CARTESIAN_POINT('Origin',(-32.85,-70.08000002,-58.24995));
#148551=CARTESIAN_POINT('Origin',(-32.85,-72.58000002,-58.24995));
#148552=CARTESIAN_POINT('Origin',(-32.85,-73.08000002,-176.84995));
#148553=CARTESIAN_POINT('',(-32.85,-65.0627241049617,-177.34995));
#148554=CARTESIAN_POINT('',(-32.85,-70.08000002,-177.34995));
#148555=CARTESIAN_POINT('',(-32.85,-73.08000002,-177.34995));
#148556=CARTESIAN_POINT('Origin',(-32.85,-70.08000002,-176.84995));
#148557=CARTESIAN_POINT('Ctrl Pts',(-32.85,-65.0627241049617,-177.34995));
#148558=CARTESIAN_POINT('Ctrl Pts',(-32.9812673457631,-65.0258272602758,
-177.34995));
#148559=CARTESIAN_POINT('Ctrl Pts',(-33.1109933446567,-64.9893636599417,
-177.29606343653));
#148560=CARTESIAN_POINT('Ctrl Pts',(-33.2961134365298,-64.9373297954784,
-177.110943344657));
#148561=CARTESIAN_POINT('Ctrl Pts',(-33.35,-64.9221832702703,-176.981217345763));
#148562=CARTESIAN_POINT('Ctrl Pts',(-33.35,-64.9221832702593,-176.84995));
#148563=CARTESIAN_POINT('Origin',(-33.85,-64.9221832702593,-171.64995));
#148564=CARTESIAN_POINT('Origin',(-33.85,-64.9221832702593,-176.84995));
#148565=CARTESIAN_POINT('Origin',(-33.85,-64.9221832702593,-172.64995));
#148566=CARTESIAN_POINT('Ctrl Pts',(-33.7804134495199,-64.4270492358885,
-172.64995));
#148567=CARTESIAN_POINT('Ctrl Pts',(-33.3499999999999,-64.4875399013512,
-172.64995));
#148568=CARTESIAN_POINT('Ctrl Pts',(-33.35,-64.9221832702593,-172.64995));
#148569=CARTESIAN_POINT('Ctrl Pts',(-33.7804134495211,-64.4270492358883,
-172.51902671195));
#148570=CARTESIAN_POINT('Ctrl Pts',(-33.35,-64.4875399013443,-172.511015867074));
#148571=CARTESIAN_POINT('Ctrl Pts',(-33.35,-64.922183270247,-172.453565067926));
#148572=CARTESIAN_POINT('Ctrl Pts',(-33.7822246014263,-64.4005115826131,
-172.38820210671));
#148573=CARTESIAN_POINT('Ctrl Pts',(-33.35,-64.4577842162266,-172.371853931892));
#148574=CARTESIAN_POINT('Ctrl Pts',(-33.35,-64.8827586015461,-172.257328160063));
#148575=CARTESIAN_POINT('Ctrl Pts',(-33.7891962191206,-64.2983609167864,
-172.14633102856));
#148576=CARTESIAN_POINT('Ctrl Pts',(-33.35,-64.3449732070946,-172.118296873734));
#148577=CARTESIAN_POINT('Ctrl Pts',(-33.35,-64.7310022982632,-171.894521542842));
#148578=CARTESIAN_POINT('Ctrl Pts',(-33.7943539433762,-64.2227880741536,
-172.035403273235));
#148579=CARTESIAN_POINT('Ctrl Pts',(-33.3500000000013,-64.2614041148292,
-172.003556970023));
#148580=CARTESIAN_POINT('Ctrl Pts',(-33.35,-64.6187303406215,-171.728129909852));
#148581=CARTESIAN_POINT('Ctrl Pts',(-33.8072358131761,-64.0340382552807,
-171.850283164391));
#148582=CARTESIAN_POINT('Ctrl Pts',(-33.3499999999986,-64.0569588954535,
-171.817687494207));
#148583=CARTESIAN_POINT('Ctrl Pts',(-33.35,-64.3383212554124,-171.450449746589));
#148584=CARTESIAN_POINT('Ctrl Pts',(-33.8149548930127,-63.9209355035967,
-171.776163607997));
#148585=CARTESIAN_POINT('Ctrl Pts',(-33.3499999999999,-63.9353951792977,
-171.746711574348));
#148586=CARTESIAN_POINT('Ctrl Pts',(-33.35,-64.1702943967697,-171.339270411997));
#148587=CARTESIAN_POINT('Ctrl Pts',(-33.831785867019,-63.6743219805034,
-171.675977326981));
#148588=CARTESIAN_POINT('Ctrl Pts',(-33.3499999999999,-63.6769599183967,
-171.658003579003));
#148589=CARTESIAN_POINT('Ctrl Pts',(-33.35,-63.8039222708381,-171.18899099047));
#148590=CARTESIAN_POINT('Ctrl Pts',(-33.8408895000012,-63.5409322550068,
-171.64995));
#148591=CARTESIAN_POINT('Ctrl Pts',(-33.35,-63.5396903402446,-171.640924254979));
#148592=CARTESIAN_POINT('Ctrl Pts',(-33.35,-63.6057568308558,-171.149950000016));
#148593=CARTESIAN_POINT('Ctrl Pts',(-33.85,-63.4074419114814,-171.64995));
#148594=CARTESIAN_POINT('Ctrl Pts',(-33.35,-63.4074419114814,-171.64995));
#148595=CARTESIAN_POINT('Ctrl Pts',(-33.35,-63.4074419114814,-171.14995));
#148596=CARTESIAN_POINT('',(-33.85,-63.4074419114814,-171.64995));
#148597=CARTESIAN_POINT('Origin',(-33.85,-63.4074419114814,-171.14995));
#148598=CARTESIAN_POINT('Ctrl Pts',(-33.85,-63.4074419114814,-171.64995));
#148599=CARTESIAN_POINT('Ctrl Pts',(-33.8408895000012,-63.5409322550068,
-171.64995));
#148600=CARTESIAN_POINT('Ctrl Pts',(-33.831785867019,-63.6743219805034,
-171.675977326981));
#148601=CARTESIAN_POINT('Ctrl Pts',(-33.8149548930127,-63.9209355035967,
-171.776163607997));
#148602=CARTESIAN_POINT('Ctrl Pts',(-33.8072358131761,-64.0340382552807,
-171.850283164391));
#148603=CARTESIAN_POINT('Ctrl Pts',(-33.7943539433762,-64.2227880741536,
-172.035403273235));
#148604=CARTESIAN_POINT('Ctrl Pts',(-33.7891962191206,-64.2983609167864,
-172.14633102856));
#148605=CARTESIAN_POINT('Ctrl Pts',(-33.7822246014263,-64.4005115826131,
-172.38820210671));
#148606=CARTESIAN_POINT('Ctrl Pts',(-33.7804134495211,-64.4270492358883,
-172.51902671195));
#148607=CARTESIAN_POINT('Ctrl Pts',(-33.7804134495199,-64.4270492358885,
-172.64995));
#148608=CARTESIAN_POINT('Origin',(-33.85,-12.9675000200281,-171.14995));
#148609=CARTESIAN_POINT('',(-33.85,-61.4584329769396,-171.64995));
#148610=CARTESIAN_POINT('Origin',(-33.85,-61.4584329769396,-171.14995));
#148611=CARTESIAN_POINT('',(-33.85,-63.4777123288326,-171.64995));
#148612=CARTESIAN_POINT('Ctrl Pts',(-33.35,-60.9047458754482,-170.861259130871));
#148613=CARTESIAN_POINT('Ctrl Pts',(-33.35,-60.6616577186179,-171.000024903864));
#148614=CARTESIAN_POINT('Ctrl Pts',(-33.5886122085038,-60.5345771657123,
-171.07256826174));
#148615=CARTESIAN_POINT('Ctrl Pts',(-33.35,-60.9589985837086,-170.956298004649));
#148616=CARTESIAN_POINT('Ctrl Pts',(-33.35,-60.7324577567303,-171.164705534849));
#148617=CARTESIAN_POINT('Ctrl Pts',(-33.6143702523473,-60.6248836296038,
-171.262628507825));
#148618=CARTESIAN_POINT('Ctrl Pts',(-33.35,-61.0447979165095,-171.029411101528));
#148619=CARTESIAN_POINT('Ctrl Pts',(-33.35,-60.8476105616749,-171.30214317251));
#148620=CARTESIAN_POINT('Ctrl Pts',(-33.6550624512799,-60.7677941641835,
-171.408872220814));
#148621=CARTESIAN_POINT('Ctrl Pts',(-33.35,-61.2401222274203,-171.126096896401));
#148622=CARTESIAN_POINT('Ctrl Pts',(-33.35,-61.1206228774013,-171.52051244062));
#148623=CARTESIAN_POINT('Ctrl Pts',(-33.7473474982865,-61.0935989844289,
-171.602243775044));
#148624=CARTESIAN_POINT('Ctrl Pts',(-33.35,-61.3489942654266,-171.149949989359));
#148625=CARTESIAN_POINT('Ctrl Pts',(-33.35,-61.28441455953,-171.601111075884));
#148626=CARTESIAN_POINT('Ctrl Pts',(-33.7986334045837,-61.2754078195329,
-171.64995));
#148627=CARTESIAN_POINT('Ctrl Pts',(-33.35,-61.4584329769396,-171.14995));
#148628=CARTESIAN_POINT('Ctrl Pts',(-33.35,-61.4584329769396,-171.64995));
#148629=CARTESIAN_POINT('Ctrl Pts',(-33.85,-61.4584329769396,-171.64995));
#148630=CARTESIAN_POINT('',(-33.5886122085038,-60.5345771657123,-171.07256826174));
#148631=CARTESIAN_POINT('Origin',(-33.85,-60.9047458754482,-170.861259130871));
#148632=CARTESIAN_POINT('Ctrl Pts',(-33.5886122085038,-60.5345771657123,
-171.07256826174));
#148633=CARTESIAN_POINT('Ctrl Pts',(-33.6143702523473,-60.6248836296038,
-171.262628507825));
#148634=CARTESIAN_POINT('Ctrl Pts',(-33.6550624512799,-60.7677941641835,
-171.408872220814));
#148635=CARTESIAN_POINT('Ctrl Pts',(-33.7473474982865,-61.0935989844289,
-171.602243775044));
#148636=CARTESIAN_POINT('Ctrl Pts',(-33.7986334045837,-61.2754078195329,
-171.64995));
#148637=CARTESIAN_POINT('Ctrl Pts',(-33.85,-61.4584329769396,-171.64995));
#148638=CARTESIAN_POINT('Ctrl Pts',(-33.5886122085038,-60.5345771657124,
-171.07256826174));
#148639=CARTESIAN_POINT('Ctrl Pts',(-33.35,-60.6616577186179,-171.000024903864));
#148640=CARTESIAN_POINT('Ctrl Pts',(-33.35,-60.9047458754482,-170.861259130871));
#148641=CARTESIAN_POINT('Ctrl Pts',(-33.5831748521597,-59.0440141159766,
-168.454692464379));
#148642=CARTESIAN_POINT('Ctrl Pts',(-33.3499999999583,-59.1768144406969,
-168.390475993822));
#148643=CARTESIAN_POINT('Ctrl Pts',(-33.35,-59.4103431251365,-168.243382962268));
#148644=CARTESIAN_POINT('Ctrl Pts',(-33.5774199132796,-57.5365496870091,
-165.846853703856));
#148645=CARTESIAN_POINT('Ctrl Pts',(-33.3500000000315,-57.6703808898087,
-165.782543034447));
#148646=CARTESIAN_POINT('Ctrl Pts',(-33.35,-57.8986390322929,-165.635544032027));
#148647=CARTESIAN_POINT('Ctrl Pts',(-33.5712930253539,-56.0068938993568,
-163.252219719633));
#148648=CARTESIAN_POINT('Ctrl Pts',(-33.35,-56.1347789227867,-163.176590079091));
#148649=CARTESIAN_POINT('Ctrl Pts',(-33.35,-56.364204511422,-163.040910588762));
#148650=CARTESIAN_POINT('',(-33.5716736357884,-56.0068703689372,-163.251931093946));
#148651=CARTESIAN_POINT('Origin',(-33.85,-56.3642045114216,-163.040910588762));
#148652=CARTESIAN_POINT('Ctrl Pts',(-33.5712930253608,-56.0068938993483,
-163.252219719627));
#148653=CARTESIAN_POINT('Ctrl Pts',(-33.5774199132796,-57.5365496870091,
-165.846853703856));
#148654=CARTESIAN_POINT('Ctrl Pts',(-33.5831748521597,-59.0440141159766,
-168.454692464379));
#148655=CARTESIAN_POINT('Ctrl Pts',(-33.5886122085038,-60.5345771657123,
-171.07256826174));
#148656=CARTESIAN_POINT('Ctrl Pts',(-33.35,-55.0808765597097,-157.757860472338));
#148657=CARTESIAN_POINT('Ctrl Pts',(-33.35,-54.572872815689,-157.751515483814));
#148658=CARTESIAN_POINT('Ctrl Pts',(-33.8579839047711,-54.5809755801308,
-157.751597589538));
#148659=CARTESIAN_POINT('Ctrl Pts',(-33.35,-55.0694930553304,-158.705257460135));
#148660=CARTESIAN_POINT('Ctrl Pts',(-33.3499999999996,-54.6110102505827,
-158.691991727223));
#148661=CARTESIAN_POINT('Ctrl Pts',(-33.80673251536,-54.5683165271959,-158.739783519818));
#148662=CARTESIAN_POINT('Ctrl Pts',(-33.35,-55.1688504851514,-159.636950827836));
#148663=CARTESIAN_POINT('Ctrl Pts',(-33.3500000000034,-54.7494053948693,
-159.663263893567));
#148664=CARTESIAN_POINT('Ctrl Pts',(-33.7562189642388,-54.6787070453326,
-159.710574965063));
#148665=CARTESIAN_POINT('Ctrl Pts',(-33.35,-55.4903395816263,-160.984647645179));
#148666=CARTESIAN_POINT('Ctrl Pts',(-33.3499999999985,-55.1481757182452,
-161.073717268302));
#148667=CARTESIAN_POINT('Ctrl Pts',(-33.6830697051085,-55.0359064417903,
-161.113596033539));
#148668=CARTESIAN_POINT('Ctrl Pts',(-33.35,-55.6220934455112,-161.416204912461));
#148669=CARTESIAN_POINT('Ctrl Pts',(-33.3499999999999,-55.3013349864854,
-161.515699606681));
#148670=CARTESIAN_POINT('Ctrl Pts',(-33.659632768152,-55.1822975465829,
-161.56267650153));
#148671=CARTESIAN_POINT('Ctrl Pts',(-33.35,-55.9619578801892,-162.294644651832));
#148672=CARTESIAN_POINT('Ctrl Pts',(-33.35,-55.6869269417485,-162.409962964754));
#148673=CARTESIAN_POINT('Ctrl Pts',(-33.6119102026057,-55.5599217541785,
-162.476435800135));
#148674=CARTESIAN_POINT('Ctrl Pts',(-33.35,-56.176692790625,-162.740743620178));
#148675=CARTESIAN_POINT('Ctrl Pts',(-33.3500000000058,-55.9251276981362,
-162.865361276924));
#148676=CARTESIAN_POINT('Ctrl Pts',(-33.5876645600733,-55.7985279932288,
-162.94028227478));
#148677=CARTESIAN_POINT('Ctrl Pts',(-33.35,-56.4397410822123,-163.165758499336));
#148678=CARTESIAN_POINT('Ctrl Pts',(-33.3499999999981,-56.217599796636,
-163.303416706069));
#148679=CARTESIAN_POINT('Ctrl Pts',(-33.5645633535224,-56.0907870577493,
-163.381999868627));
#148680=CARTESIAN_POINT('',(-33.85,-54.58000002,-157.903547609535));
#148681=CARTESIAN_POINT('Origin',(-33.85,-55.08000002,-157.903547609535));
#148682=CARTESIAN_POINT('Ctrl Pts',(-33.85,-54.58000002,-157.903547609535));
#148683=CARTESIAN_POINT('Ctrl Pts',(-33.8413583508933,-54.5800000297389,
-158.070131241816));
#148684=CARTESIAN_POINT('Ctrl Pts',(-33.8327288620928,-54.5836479443981,
-158.236223407547));
#148685=CARTESIAN_POINT('Ctrl Pts',(-33.8241299270602,-54.5908750783497,
-158.401801779095));
#148686=CARTESIAN_POINT('Ctrl Pts',(-33.8154839223325,-54.5981417728969,
-158.568286509794));
#148687=CARTESIAN_POINT('Ctrl Pts',(-33.8068680592598,-54.6090265097566,
-158.734252422455));
#148688=CARTESIAN_POINT('Ctrl Pts',(-33.7982810557359,-54.6235053947455,
-158.899692634749));
#148689=CARTESIAN_POINT('Ctrl Pts',(-33.789726461072,-54.6379296338786,
-159.064508446613));
#148690=CARTESIAN_POINT('Ctrl Pts',(-33.7811996706316,-54.6559207511339,
-159.228803188151));
#148691=CARTESIAN_POINT('Ctrl Pts',(-33.7726915920417,-54.6775054187261,
-159.392576016311));
#148692=CARTESIAN_POINT('Ctrl Pts',(-33.7642741433225,-54.6988601618283,
-159.55460430132));
#148693=CARTESIAN_POINT('Ctrl Pts',(-33.7558741693399,-54.7237323809422,
-159.716122386248));
#148694=CARTESIAN_POINT('Ctrl Pts',(-33.7474876838614,-54.7521979722951,
-159.877125459224));
#148695=CARTESIAN_POINT('Ctrl Pts',(-33.7393031126239,-54.7799782219408,
-160.034252198857));
#148696=CARTESIAN_POINT('Ctrl Pts',(-33.7311306553308,-54.8111812601365,
-160.190888981756));
#148697=CARTESIAN_POINT('Ctrl Pts',(-33.7229827232003,-54.8459221337957,
-160.347018683881));
#148698=CARTESIAN_POINT('Ctrl Pts',(-33.7174882513588,-54.8693492744507,
-160.452303096932));
#148699=CARTESIAN_POINT('Ctrl Pts',(-33.7120052711149,-54.8943861173903,
-160.55735665573));
#148700=CARTESIAN_POINT('Ctrl Pts',(-33.7065443988847,-54.9210783233629,
-160.662168853243));
#148701=CARTESIAN_POINT('Ctrl Pts',(-33.6983891423225,-54.9609404147537,
-160.818695196566));
#148702=CARTESIAN_POINT('Ctrl Pts',(-33.6902654326991,-55.0045623826382,
-160.974930621019));
#148703=CARTESIAN_POINT('Ctrl Pts',(-33.6821730230048,-55.0520345142193,
-161.130338629735));
#148704=CARTESIAN_POINT('Ctrl Pts',(-33.6742415228735,-55.0985627094162,
-161.282656503904));
#148705=CARTESIAN_POINT('Ctrl Pts',(-33.6663403863785,-55.1487899099227,
-161.434179332344));
#148706=CARTESIAN_POINT('Ctrl Pts',(-33.658499112823,-55.2027656519471,
-161.584384445067));
#148707=CARTESIAN_POINT('Ctrl Pts',(-33.6512693155289,-55.252532270962,
-161.722876299715));
#148708=CARTESIAN_POINT('Ctrl Pts',(-33.64409090952,-55.3054855287205,-161.860247619697));
#148709=CARTESIAN_POINT('Ctrl Pts',(-33.6370064807475,-55.3616319074669,
-161.996077647676));
#148710=CARTESIAN_POINT('Ctrl Pts',(-33.6310339771099,-55.4089659215521,
-162.110588691862));
#148711=CARTESIAN_POINT('Ctrl Pts',(-33.6251574486299,-55.4585971099375,
-162.224128770533));
#148712=CARTESIAN_POINT('Ctrl Pts',(-33.6193265052801,-55.5106817363739,
-162.336662125923));
#148713=CARTESIAN_POINT('Ctrl Pts',(-33.6135805978345,-55.5620067836071,
-162.447554344527));
#148714=CARTESIAN_POINT('Ctrl Pts',(-33.6078786491602,-55.6157148224026,
-162.557469198455));
#148715=CARTESIAN_POINT('Ctrl Pts',(-33.6022090581942,-55.6719741097404,
-162.66634452554));
#148716=CARTESIAN_POINT('Ctrl Pts',(-33.5966802445508,-55.7268364652903,
-162.772516451774));
#148717=CARTESIAN_POINT('Ctrl Pts',(-33.5911820484159,-55.7841255741681,
-162.877699928124));
#148718=CARTESIAN_POINT('Ctrl Pts',(-33.5857420390386,-55.844006448796,
-162.981808400476));
#148719=CARTESIAN_POINT('Ctrl Pts',(-33.5809929344731,-55.8962821923382,
-163.072694644792));
#148720=CARTESIAN_POINT('Ctrl Pts',(-33.5762886530756,-55.9505335934556,
-163.162761236236));
#148721=CARTESIAN_POINT('Ctrl Pts',(-33.5716736357884,-56.0068703689372,
-163.251931093946));
#148722=CARTESIAN_POINT('Origin',(-33.85,-55.08000002,-55.24995));
#148723=CARTESIAN_POINT('',(-33.8499999999899,-54.58000002,-74.1550953619836));
#148724=CARTESIAN_POINT('Origin',(-33.85,-55.08000002,-74.155095361993));
#148725=CARTESIAN_POINT('',(-33.85,-54.58000002,-157.276549545042));
#148726=CARTESIAN_POINT('Ctrl Pts',(-33.35,-56.3642045114132,-69.0177323827589));
#148727=CARTESIAN_POINT('Ctrl Pts',(-33.35,-56.134778922778,-68.8820528924306));
#148728=CARTESIAN_POINT('Ctrl Pts',(-33.5712930253538,-56.006893899348,
-68.8064232518886));
#148729=CARTESIAN_POINT('Ctrl Pts',(-33.35,-56.1349989919057,-69.4053046881168));
#148730=CARTESIAN_POINT('Ctrl Pts',(-33.35,-55.8795696344188,-69.2811581349632));
#148731=CARTESIAN_POINT('Ctrl Pts',(-33.5923541472839,-55.7522317441443,
-69.2092624885051));
#148732=CARTESIAN_POINT('Ctrl Pts',(-33.35,-55.9450970231818,-69.808093015459));
#148733=CARTESIAN_POINT('Ctrl Pts',(-33.35,-55.6684723180091,-69.6920753057542));
#148734=CARTESIAN_POINT('Ctrl Pts',(-33.6142403739361,-55.5412189114063,
-69.628091942105));
#148735=CARTESIAN_POINT('Ctrl Pts',(-33.35,-55.6242976847011,-70.6362303826783));
#148736=CARTESIAN_POINT('Ctrl Pts',(-33.35,-55.3039535321835,-70.5365374259244));
#148737=CARTESIAN_POINT('Ctrl Pts',(-33.659221513549,-55.1847752040192,
-70.4895195351988));
#148738=CARTESIAN_POINT('Ctrl Pts',(-33.35,-55.4937179039915,-71.0617579129361));
#148739=CARTESIAN_POINT('Ctrl Pts',(-33.35,-55.152213923386,-70.9724898647665));
#148740=CARTESIAN_POINT('Ctrl Pts',(-33.682327027756,-55.0396865574335,
-70.9323196038346));
#148741=CARTESIAN_POINT('Ctrl Pts',(-33.35,-55.1806225291757,-72.3685609104781));
#148742=CARTESIAN_POINT('Ctrl Pts',(-33.35,-54.7649354301353,-72.3373662781827));
#148743=CARTESIAN_POINT('Ctrl Pts',(-33.7532457656832,-54.6918028086424,
-72.2927601348896));
#148744=CARTESIAN_POINT('Ctrl Pts',(-33.35,-55.0800000211738,-73.2600087408747));
#148745=CARTESIAN_POINT('Ctrl Pts',(-33.3499999999911,-54.6261840530745,
-73.2648134588722));
#148746=CARTESIAN_POINT('Ctrl Pts',(-33.801572917506,-54.5800000199981,
-73.221574548752));
#148747=CARTESIAN_POINT('Ctrl Pts',(-33.35,-55.08000002,-74.155095361993));
#148748=CARTESIAN_POINT('Ctrl Pts',(-33.35,-54.5800000199987,-74.155095361994));
#148749=CARTESIAN_POINT('Ctrl Pts',(-33.8500000000012,-54.58000002,-74.155095361994));
#148750=CARTESIAN_POINT('',(-33.5713955981573,-56.0068423841382,-68.80655523181));
#148751=CARTESIAN_POINT('Origin',(-33.85,-56.3642045114132,-69.0177323827589));
#148752=CARTESIAN_POINT('Ctrl Pts',(-33.5712993597704,-56.0068173078863,
-68.8065444112298));
#148753=CARTESIAN_POINT('Ctrl Pts',(-33.592358535658,-55.7521894346693,
-69.2093464673669));
#148754=CARTESIAN_POINT('Ctrl Pts',(-33.614242628708,-55.5412010439342,
-69.6281351229303));
#148755=CARTESIAN_POINT('Ctrl Pts',(-33.659221513549,-55.1847752040192,
-70.4895195351988));
#148756=CARTESIAN_POINT('Ctrl Pts',(-33.682327027756,-55.0396865574335,
-70.9323196038346));
#148757=CARTESIAN_POINT('Ctrl Pts',(-33.7532457656832,-54.6918028086424,
-72.2927601348896));
#148758=CARTESIAN_POINT('Ctrl Pts',(-33.801572917506,-54.5800000199981,
-73.221574548752));
#148759=CARTESIAN_POINT('Ctrl Pts',(-33.8499999999899,-54.58000002,-74.1550953619836));
#148760=CARTESIAN_POINT('Ctrl Pts',(-33.5712930253538,-56.006893899348,
-68.8064232518886));
#148761=CARTESIAN_POINT('Ctrl Pts',(-33.35,-56.134778922778,-68.8820528924306));
#148762=CARTESIAN_POINT('Ctrl Pts',(-33.35,-56.3642045114132,-69.0177323827589));
#148763=CARTESIAN_POINT('Ctrl Pts',(-33.5772316679252,-57.489551829777,
-66.2915080112617));
#148764=CARTESIAN_POINT('Ctrl Pts',(-33.35,-57.623019767821,-66.3564728841549));
#148765=CARTESIAN_POINT('Ctrl Pts',(-33.35,-57.8514943778664,-66.5028176210733));
#148766=CARTESIAN_POINT('Ctrl Pts',(-33.5828208370019,-58.9513545007691,
-63.7641770795492));
#148767=CARTESIAN_POINT('Ctrl Pts',(-33.35,-59.0838703919199,-63.828995910853));
#148768=CARTESIAN_POINT('Ctrl Pts',(-33.35,-59.3174222737568,-63.975486542669));
#148769=CARTESIAN_POINT('Ctrl Pts',(-33.5881101525803,-60.3971457002532,
-61.2273317382593));
#148770=CARTESIAN_POINT('Ctrl Pts',(-33.35,-60.5242644024533,-61.2999665374096));
#148771=CARTESIAN_POINT('Ctrl Pts',(-33.35,-60.7669593817595,-61.4386408691297));
#148772=CARTESIAN_POINT('Origin',(-33.85,-60.7669593817595,-61.4386408691297));
#148773=CARTESIAN_POINT('Ctrl Pts',(-33.5881101525803,-60.3971457002532,
-61.2273317382593));
#148774=CARTESIAN_POINT('Ctrl Pts',(-33.5828208370019,-58.9513545007691,
-63.7641770795492));
#148775=CARTESIAN_POINT('Ctrl Pts',(-33.5772316679252,-57.489551829777,
-66.2915080112617));
#148776=CARTESIAN_POINT('Ctrl Pts',(-33.5712930253538,-56.006893899348,
-68.8064232518886));
#148777=CARTESIAN_POINT('Ctrl Pts',(-33.35,-61.3211699373828,-61.14995));
#148778=CARTESIAN_POINT('Ctrl Pts',(-33.35,-61.3211699373828,-60.64995));
#148779=CARTESIAN_POINT('Ctrl Pts',(-33.85,-61.3211699373828,-60.64995));
#148780=CARTESIAN_POINT('Ctrl Pts',(-33.35,-61.2129519920939,-61.1499500348135));
#148781=CARTESIAN_POINT('Ctrl Pts',(-33.3499999999981,-61.1490609397226,
-60.6983362970117));
#148782=CARTESIAN_POINT('Ctrl Pts',(-33.7991562663074,-61.1403193911197,
-60.64995));
#148783=CARTESIAN_POINT('Ctrl Pts',(-33.35,-61.1026558608156,-61.1739192791944));
#148784=CARTESIAN_POINT('Ctrl Pts',(-33.35,-60.9832965997767,-60.7797248720816));
#148785=CARTESIAN_POINT('Ctrl Pts',(-33.7471512515707,-60.9562715767294,
-60.6978885776012));
#148786=CARTESIAN_POINT('Ctrl Pts',(-33.35,-60.9082690803677,-61.269817357096));
#148787=CARTESIAN_POINT('Ctrl Pts',(-33.35,-60.7117483921024,-60.9965405405777));
#148788=CARTESIAN_POINT('Ctrl Pts',(-33.6552207448938,-60.6322769136983,
-60.8896846949796));
#148789=CARTESIAN_POINT('Ctrl Pts',(-33.35,-60.8219736344732,-61.3423603399148));
#148790=CARTESIAN_POINT('Ctrl Pts',(-33.3499999999996,-60.5960155996905,
-61.1331508909766));
#148791=CARTESIAN_POINT('Ctrl Pts',(-33.6142503615382,-60.4886315879339,
-61.034824258355));
#148792=CARTESIAN_POINT('Ctrl Pts',(-33.35,-60.7669593817595,-61.4386408691297));
#148793=CARTESIAN_POINT('Ctrl Pts',(-33.35,-60.5242644024533,-61.2999665374096));
#148794=CARTESIAN_POINT('Ctrl Pts',(-33.5881101525803,-60.3971457002532,
-61.2273317382593));
#148795=CARTESIAN_POINT('Origin',(-32.85,-72.58000002,-55.24995));
#148796=CARTESIAN_POINT('',(-32.85,-73.08000002,-174.34995));
#148797=CARTESIAN_POINT('Origin',(-32.85,-72.58000002,-174.34995));
#148798=CARTESIAN_POINT('',(-32.85,-73.08000002,-58.24995));
#148799=CARTESIAN_POINT('Origin',(-32.85,-70.08000002,-174.34995));
#148800=CARTESIAN_POINT('Origin',(-32.85,-70.08000002,-174.34995));
#148801=CARTESIAN_POINT('Origin',(0.,-12.9675000200281,-61.64995));
#148802=CARTESIAN_POINT('',(-30.7601599624812,36.3431985357226,-61.2273317382593));
#148803=CARTESIAN_POINT('',(-36.7137393100582,32.0861766206928,-61.2273317382593));
#148804=CARTESIAN_POINT('Origin',(0.,-12.9675000200281,-61.2273317382593));
#148805=CARTESIAN_POINT('Ctrl Pts',(-37.,33.02054075664,-60.64995));
#148806=CARTESIAN_POINT('Ctrl Pts',(-36.9450144953722,32.8396166159335,
-60.64995));
#148807=CARTESIAN_POINT('Ctrl Pts',(-36.8889168804295,32.6559426968113,
-60.6963841656953));
#148808=CARTESIAN_POINT('Ctrl Pts',(-36.8135029743542,32.4100449984504,
-60.8387768064376));
#148809=CARTESIAN_POINT('Ctrl Pts',(-36.7895122380439,32.3319990572285,
-60.8990185151424));
#148810=CARTESIAN_POINT('Ctrl Pts',(-36.7467810375704,32.1932186054134,
-61.0450197081848));
#148811=CARTESIAN_POINT('Ctrl Pts',(-36.7283245477951,32.1334017245463,
-61.1290643654114));
#148812=CARTESIAN_POINT('Ctrl Pts',(-36.7137393100582,32.0861766206928,
-61.2273317382593));
#148813=CARTESIAN_POINT('Ctrl Pts',(-30.7601599624812,36.3431985357226,
-61.2273317382593));
#148814=CARTESIAN_POINT('Ctrl Pts',(-30.7833440352389,36.4311997587239,
-61.0408976853214));
#148815=CARTESIAN_POINT('Ctrl Pts',(-30.820204224048,36.5713423922847,-60.8940610213177));
#148816=CARTESIAN_POINT('Ctrl Pts',(-30.9048607560821,36.8949030802612,
-60.6989334962026));
#148817=CARTESIAN_POINT('Ctrl Pts',(-30.9524183405754,37.0774198714491,
-60.64995));
#148818=CARTESIAN_POINT('Ctrl Pts',(-31.,37.2609769076718,-60.64995));
#148819=CARTESIAN_POINT('Origin',(-31.,-9.33460238845303,-61.14995));
#148820=CARTESIAN_POINT('Origin',(-31.,37.2609769076718,-61.14995));
#148821=CARTESIAN_POINT('Origin',(-37.,-12.9675000200281,-61.14995));
#148822=CARTESIAN_POINT('Origin',(-37.,33.02054075664,-61.14995));
#148823=CARTESIAN_POINT('Ctrl Pts',(-30.5,36.7276789742547,-61.4386408691297));
#148824=CARTESIAN_POINT('Ctrl Pts',(-30.5,36.4678387256643,-61.2958335593366));
#148825=CARTESIAN_POINT('Ctrl Pts',(-30.7601599624812,36.3431985357226,
-61.2273317382593));
#148826=CARTESIAN_POINT('Ctrl Pts',(-30.5,36.7789093803379,-61.3454266101228));
#148827=CARTESIAN_POINT('Ctrl Pts',(-30.5,36.536757012545,-61.1328271281761));
#148828=CARTESIAN_POINT('Ctrl Pts',(-30.7833440352389,36.4311997587239,
-61.0408976853214));
#148829=CARTESIAN_POINT('Ctrl Pts',(-30.5,36.8604662025248,-61.2720055170969));
#148830=CARTESIAN_POINT('Ctrl Pts',(-30.5000000000002,36.6495790716841,
-60.9942767827739));
#148831=CARTESIAN_POINT('Ctrl Pts',(-30.820204224048,36.5713423922847,-60.8940610213177));
#148832=CARTESIAN_POINT('Ctrl Pts',(-30.5,37.0485310665384,-61.1744417416632));
#148833=CARTESIAN_POINT('Ctrl Pts',(-30.4999999999998,36.921160791843,-60.7754981362285));
#148834=CARTESIAN_POINT('Ctrl Pts',(-30.9048607560821,36.8949030802612,
-60.6989334962026));
#148835=CARTESIAN_POINT('Ctrl Pts',(-30.5,37.1545174137893,-61.1499500119967));
#148836=CARTESIAN_POINT('Ctrl Pts',(-30.5,37.0857740751484,-60.6953661941756));
#148837=CARTESIAN_POINT('Ctrl Pts',(-30.9524183405754,37.0774198714491,
-60.64995));
#148838=CARTESIAN_POINT('Ctrl Pts',(-30.5,37.2609769076718,-61.14995));
#148839=CARTESIAN_POINT('Ctrl Pts',(-30.5,37.2609769076718,-60.64995));
#148840=CARTESIAN_POINT('Ctrl Pts',(-31.,37.2609769076718,-60.64995));
#148841=CARTESIAN_POINT('Origin',(-31.,36.7276789742547,-61.4386408691296));
#148842=CARTESIAN_POINT('Ctrl Pts',(-30.7601599624812,36.3431985357226,
-61.2273317382593));
#148843=CARTESIAN_POINT('Ctrl Pts',(-30.5,36.4678387256643,-61.2958335593366));
#148844=CARTESIAN_POINT('Ctrl Pts',(-30.5,36.7276789742547,-61.4386408691296));
#148845=CARTESIAN_POINT('Ctrl Pts',(-30.7526164452201,34.1766563796975,
-65.1779528603621));
#148846=CARTESIAN_POINT('Ctrl Pts',(-30.5,34.3134045700868,-65.2278638132481));
#148847=CARTESIAN_POINT('Ctrl Pts',(-30.5,34.5564303542403,-65.3892634389964));
#148848=CARTESIAN_POINT('Ctrl Pts',(-30.7443983582191,31.9809814038522,
-69.1118639196982));
#148849=CARTESIAN_POINT('Ctrl Pts',(-30.5,32.1210861733241,-69.1599841087648));
#148850=CARTESIAN_POINT('Ctrl Pts',(-30.5,32.3553350664733,-69.3231754387568));
#148851=CARTESIAN_POINT('Ctrl Pts',(-30.7353076117347,29.741870145346,-73.0207363867641));
#148852=CARTESIAN_POINT('Ctrl Pts',(-30.5,29.8691857803939,-73.0938794170475));
#148853=CARTESIAN_POINT('Ctrl Pts',(-30.5,30.1096831288108,-73.2320455176344));
#148854=CARTESIAN_POINT('',(-30.735362854857,29.74186581737,-73.0207804888355));
#148855=CARTESIAN_POINT('Origin',(-31.,30.1096831288108,-73.2320455176344));
#148856=CARTESIAN_POINT('Ctrl Pts',(-30.7353076117299,29.7418701453522,
-73.0207363867594));
#148857=CARTESIAN_POINT('Ctrl Pts',(-30.7443983582191,31.9809814038522,
-69.1118639196982));
#148858=CARTESIAN_POINT('Ctrl Pts',(-30.7526164452201,34.1766563796975,
-65.1779528603621));
#148859=CARTESIAN_POINT('Ctrl Pts',(-30.7601599624812,36.3431985357226,
-61.2273317382593));
#148860=CARTESIAN_POINT('Ctrl Pts',(-30.5,28.920951499305,-78.1925828079988));
#148861=CARTESIAN_POINT('Ctrl Pts',(-30.5000000000003,28.4128149071901,
-78.1994146967941));
#148862=CARTESIAN_POINT('Ctrl Pts',(-31.0081211823014,28.4210588880653,
-78.1993225690759));
#148863=CARTESIAN_POINT('Ctrl Pts',(-30.5,28.9094064694558,-77.302118472504));
#148864=CARTESIAN_POINT('Ctrl Pts',(-30.4999999999984,28.4483980825612,
-77.3106418208197));
#148865=CARTESIAN_POINT('Ctrl Pts',(-30.9594146236477,28.4082208355605,
-77.2678456234727));
#148866=CARTESIAN_POINT('Ctrl Pts',(-30.5,29.002822674508,-76.426962221765));
#148867=CARTESIAN_POINT('Ctrl Pts',(-30.5,28.579933321534,-76.3966655405999));
#148868=CARTESIAN_POINT('Ctrl Pts',(-30.9113712398487,28.5120100836853,
-76.353449058608));
#148869=CARTESIAN_POINT('Ctrl Pts',(-30.5,29.3028136269337,-75.1629449138939));
#148870=CARTESIAN_POINT('Ctrl Pts',(-30.5,28.9539620571574,-75.0718448818203));
#148871=CARTESIAN_POINT('Ctrl Pts',(-30.8418282567564,28.8453229371035,
-75.0340563370096));
#148872=CARTESIAN_POINT('Ctrl Pts',(-30.5,29.4252185218281,-74.758955076818));
#148873=CARTESIAN_POINT('Ctrl Pts',(-30.5000000000007,29.0970410698504,
-74.6573521788374));
#148874=CARTESIAN_POINT('Ctrl Pts',(-30.8195774733883,28.9813262599642,
-74.6125704712075));
#148875=CARTESIAN_POINT('Ctrl Pts',(-30.5,29.7412533702373,-73.9312213579753));
#148876=CARTESIAN_POINT('Ctrl Pts',(-30.4999999999992,29.4573184808354,
-73.8131874683998));
#148877=CARTESIAN_POINT('Ctrl Pts',(-30.7739516476249,29.3324729246049,
-73.7493614137364));
#148878=CARTESIAN_POINT('Ctrl Pts',(-30.5,29.9412605039864,-73.5090015627542));
#148879=CARTESIAN_POINT('Ctrl Pts',(-30.5000000000002,29.6801451335267,
-73.3815386187724));
#148880=CARTESIAN_POINT('Ctrl Pts',(-30.7506559835889,29.5547110389812,
-73.3092557539648));
#148881=CARTESIAN_POINT('Ctrl Pts',(-30.5,30.1841529915896,-73.1054052864862));
#148882=CARTESIAN_POINT('Ctrl Pts',(-30.5,29.9511540345493,-72.9650282514353));
#148883=CARTESIAN_POINT('Ctrl Pts',(-30.7283768517831,29.8245792311644,
-72.888770763772));
#148884=CARTESIAN_POINT('Origin',(-31.,28.91999998,-78.0460091084363));
#148885=CARTESIAN_POINT('Ctrl Pts',(-31.,28.41999998,-78.0460091084363));
#148886=CARTESIAN_POINT('Ctrl Pts',(-30.9915553765912,28.4199999839581,
-77.8845784212935));
#148887=CARTESIAN_POINT('Ctrl Pts',(-30.9831189817359,28.4236427988899,
-77.7236551810799));
#148888=CARTESIAN_POINT('Ctrl Pts',(-30.974710992956,28.4308536388649,-77.5632621201644));
#148889=CARTESIAN_POINT('Ctrl Pts',(-30.9662475726578,28.4381120178909,
-77.4018116326618));
#148890=CARTESIAN_POINT('Ctrl Pts',(-30.9578122144729,28.4489851481422,
-77.240897706449));
#148891=CARTESIAN_POINT('Ctrl Pts',(-30.9494053624499,28.4634423631753,
-77.0805267505334));
#148892=CARTESIAN_POINT('Ctrl Pts',(-30.9410119089526,28.477876536841,-76.9204113878366));
#148893=CARTESIAN_POINT('Ctrl Pts',(-30.9326460542808,28.4958831701324,
-76.7608365749435));
#148894=CARTESIAN_POINT('Ctrl Pts',(-30.9242998354382,28.5174821139553,
-76.6018020101865));
#148895=CARTESIAN_POINT('Ctrl Pts',(-30.9160313168687,28.5388799794379,
-76.4442479995983));
#148896=CARTESIAN_POINT('Ctrl Pts',(-30.9077812401549,28.5638036464743,
-76.287223543863));
#148897=CARTESIAN_POINT('Ctrl Pts',(-30.8995458905796,28.5923228488236,
-76.1307320214001));
#148898=CARTESIAN_POINT('Ctrl Pts',(-30.8914871613302,28.620230410979,-75.9775967114978));
#148899=CARTESIAN_POINT('Ctrl Pts',(-30.8834417951,28.6515812866277,-75.8249711322362));
#148900=CARTESIAN_POINT('Ctrl Pts',(-30.8754216976956,28.6864860901755,
-75.6728712878223));
#148901=CARTESIAN_POINT('Ctrl Pts',(-30.8716293533375,28.7029910062798,
-75.6009500931339));
#148902=CARTESIAN_POINT('Ctrl Pts',(-30.8678429521625,28.7202911839302,
-75.5291466906985));
#148903=CARTESIAN_POINT('Ctrl Pts',(-30.8640657072001,28.7384015524274,
-75.4574643697372));
#148904=CARTESIAN_POINT('Ctrl Pts',(-30.8560438465024,28.7768631440684,
-75.3052302416943));
#148905=CARTESIAN_POINT('Ctrl Pts',(-30.8480465637921,28.8190554047428,
-75.1532523926285));
#148906=CARTESIAN_POINT('Ctrl Pts',(-30.8400772928907,28.86505678019,-75.0020584970304));
#148907=CARTESIAN_POINT('Ctrl Pts',(-30.8322415679512,28.9102872823649,
-74.8533982503052));
#148908=CARTESIAN_POINT('Ctrl Pts',(-30.8244332481999,28.9592007097099,
-74.7054961433376));
#148909=CARTESIAN_POINT('Ctrl Pts',(-30.816683261254,29.0118331998908,-74.5588697982428));
#148910=CARTESIAN_POINT('Ctrl Pts',(-30.8103937252398,29.0545473289367,
-74.4398745425673));
#148911=CARTESIAN_POINT('Ctrl Pts',(-30.804143211839,29.0997102947523,-74.3217198951437));
#148912=CARTESIAN_POINT('Ctrl Pts',(-30.7979595444717,29.1473196130014,
-74.2046886808605));
#148913=CARTESIAN_POINT('Ctrl Pts',(-30.7918740622196,29.1941729839906,
-74.0895157041872));
#148914=CARTESIAN_POINT('Ctrl Pts',(-30.7858770793326,29.243410990576,-73.975346469923));
#148915=CARTESIAN_POINT('Ctrl Pts',(-30.7799226196483,29.2951820844478,
-73.862212594861));
#148916=CARTESIAN_POINT('Ctrl Pts',(-30.7740541865778,29.3462052192879,
-73.7507132130523));
#148917=CARTESIAN_POINT('Ctrl Pts',(-30.7682267315409,29.3996893836541,
-73.64021925808));
#148918=CARTESIAN_POINT('Ctrl Pts',(-30.7624318804288,29.4557967629243,
-73.5307896724718));
#148919=CARTESIAN_POINT('Ctrl Pts',(-30.7567739030089,29.5105788925869,
-73.4239448006263));
#148920=CARTESIAN_POINT('Ctrl Pts',(-30.751146830599,29.5678624292832,-73.3181144970074));
#148921=CARTESIAN_POINT('Ctrl Pts',(-30.7455806691336,29.6278083791469,
-73.2133836177019));
#148922=CARTESIAN_POINT('Ctrl Pts',(-30.7421458129149,29.6648007876413,
-73.1487546064333));
#148923=CARTESIAN_POINT('Ctrl Pts',(-30.7387349098385,29.7028072292658,
-73.0845448640455));
#148924=CARTESIAN_POINT('Ctrl Pts',(-30.735362854857,29.74186581737,-73.0207804888355));
#148925=CARTESIAN_POINT('Origin',(-31.,28.91999998,-55.24995));
#148926=CARTESIAN_POINT('Origin',(-30.,43.91999998,-58.24995));
#148927=CARTESIAN_POINT('Origin',(-30.,43.91999998,-58.24995));
#148928=CARTESIAN_POINT('Origin',(0.,43.91999998,-58.24995));
#148929=CARTESIAN_POINT('Origin',(-29.5,43.91999998,-58.24995));
#148930=CARTESIAN_POINT('Origin',(-29.5,43.91999998,-58.24995));
#148931=CARTESIAN_POINT('Origin',(-28.5,28.91999998,-55.24995));
#148932=CARTESIAN_POINT('Origin',(-28.5,28.91999998,-80.9397703408579));
#148933=CARTESIAN_POINT('Ctrl Pts',(-29.,30.190901134448,-76.1489606194832));
#148934=CARTESIAN_POINT('Ctrl Pts',(-29.,29.4220372877054,-75.6687700201129));
#148935=CARTESIAN_POINT('Ctrl Pts',(-28.2332370915911,29.8322352061969,
-75.9248722755917));
#148936=CARTESIAN_POINT('Ctrl Pts',(-29.,29.9217980586497,-76.5811393756123));
#148937=CARTESIAN_POINT('Ctrl Pts',(-29.,29.1809262360145,-76.1656388830817));
#148938=CARTESIAN_POINT('Ctrl Pts',(-28.2574251716161,29.5332350272111,
-76.376269388315));
#148939=CARTESIAN_POINT('Ctrl Pts',(-29.,29.7057519229925,-77.032432603564));
#148940=CARTESIAN_POINT('Ctrl Pts',(-28.9999999999999,28.9849557677507,
-76.6882938526006));
#148941=CARTESIAN_POINT('Ctrl Pts',(-28.2826568860398,29.2931653796995,
-76.8479190563244));
#148942=CARTESIAN_POINT('Ctrl Pts',(-29.,29.392736442598,-77.861168463682));
#148943=CARTESIAN_POINT('Ctrl Pts',(-29.,28.7176256604522,-77.6280825227319));
#148944=CARTESIAN_POINT('Ctrl Pts',(-28.3289101078372,28.945348491788,-77.7145676490796));
#148945=CARTESIAN_POINT('Ctrl Pts',(-29.,29.2801830215621,-78.2330925203216));
#148946=CARTESIAN_POINT('Ctrl Pts',(-29.,28.6258554431304,-78.0379074931216));
#148947=CARTESIAN_POINT('Ctrl Pts',(-28.3496415967673,28.8202788507468,
-78.1036928430455));
#148948=CARTESIAN_POINT('Ctrl Pts',(-29.,29.0997153099535,-78.9928975231766));
#148949=CARTESIAN_POINT('Ctrl Pts',(-29.,28.4904715640779,-78.8635127668171));
#148950=CARTESIAN_POINT('Ctrl Pts',(-28.391922778916,28.6197368000676,-78.8990673308349));
#148951=CARTESIAN_POINT('Ctrl Pts',(-29.,29.0321487487139,-79.3807788748604));
#148952=CARTESIAN_POINT('Ctrl Pts',(-29.,28.4443634216833,-79.2803384248115));
#148953=CARTESIAN_POINT('Ctrl Pts',(-28.4134719614193,28.5446520387322,
-79.3053196265795));
#148954=CARTESIAN_POINT('Ctrl Pts',(-29.,28.9298976880956,-80.2665661129666));
#148955=CARTESIAN_POINT('Ctrl Pts',(-29.,28.3932524579211,-80.2165321508882));
#148956=CARTESIAN_POINT('Ctrl Pts',(-28.4625827973001,28.4310142561314,
-80.23358931143));
#148957=CARTESIAN_POINT('Ctrl Pts',(-29.,28.9090504215435,-80.7677709009127));
#148958=CARTESIAN_POINT('Ctrl Pts',(-29.,28.3982322973888,-80.7457941266633));
#148959=CARTESIAN_POINT('Ctrl Pts',(-28.4902997525053,28.4078381678252,
-80.7592040367449));
#148960=CARTESIAN_POINT('Ctrl Pts',(-29.,28.9253917285729,-81.2725388309494));
#148961=CARTESIAN_POINT('Ctrl Pts',(-29.,28.4434678656906,-81.2883860649699));
#148962=CARTESIAN_POINT('Ctrl Pts',(-28.5181235174212,28.4259824926159,
-81.288955297043));
#148963=CARTESIAN_POINT('Origin',(-28.5,30.0207919771236,-76.4370443259982));
#148964=CARTESIAN_POINT('Ctrl Pts',(-28.2496026843433,29.6431021904052,
-76.2257353081032));
#148965=CARTESIAN_POINT('Ctrl Pts',(-28.2550962738409,29.5820653332084,
-76.3283221218245));
#148966=CARTESIAN_POINT('Ctrl Pts',(-28.2606732058844,29.5238127198801,
-76.4318902828666));
#148967=CARTESIAN_POINT('Ctrl Pts',(-28.2662832665929,29.4681738066383,
-76.5363451683756));
#148968=CARTESIAN_POINT('Ctrl Pts',(-28.2719809006041,29.4116663674314,
-76.6424305993962));
#148969=CARTESIAN_POINT('Ctrl Pts',(-28.2777129255254,29.3578541761501,
-76.749430806199));
#148970=CARTESIAN_POINT('Ctrl Pts',(-28.283468252918,29.3065658506586,-76.8572811154413));
#148971=CARTESIAN_POINT('Ctrl Pts',(-28.2893486242973,29.2541632016442,
-76.9674746506592));
#148972=CARTESIAN_POINT('Ctrl Pts',(-28.2952535950716,29.2043946076021,
-77.0785558251055));
#148973=CARTESIAN_POINT('Ctrl Pts',(-28.3012106132358,29.1570952891048,
-77.1904887281123));
#148974=CARTESIAN_POINT('Ctrl Pts',(-28.3037621110354,29.1368361420388,
-77.2384315995022));
#148975=CARTESIAN_POINT('Ctrl Pts',(-28.3063236154331,29.1170302805272,
-77.2865311147115));
#148976=CARTESIAN_POINT('Ctrl Pts',(-28.3088992066467,29.0976661808502,
-77.3347860946956));
#148977=CARTESIAN_POINT('Ctrl Pts',(-28.3159268080949,29.0448304768712,
-77.4664516965293));
#148978=CARTESIAN_POINT('Ctrl Pts',(-28.3230277381525,28.9952999216831,
-77.599259998328));
#148979=CARTESIAN_POINT('Ctrl Pts',(-28.330171515793,28.9489397170328,-77.7331526861724));
#148980=CARTESIAN_POINT('Ctrl Pts',(-28.3374902152524,28.9014443410868,
-77.8703238568681));
#148981=CARTESIAN_POINT('Ctrl Pts',(-28.3448543969108,28.8572757382811,
-78.008633563989));
#148982=CARTESIAN_POINT('Ctrl Pts',(-28.3522654021615,28.816321248413,-78.148048277229));
#148983=CARTESIAN_POINT('Ctrl Pts',(-28.3584846660916,28.7819525260875,
-78.2650441324539));
#148984=CARTESIAN_POINT('Ctrl Pts',(-28.3647377201567,28.7498477794226,
-78.3828188721135));
#148985=CARTESIAN_POINT('Ctrl Pts',(-28.3710388306812,28.7199623512604,
-78.5013644791918));
#148986=CARTESIAN_POINT('Ctrl Pts',(-28.3798275485611,28.6782784931823,
-78.6667105546906));
#148987=CARTESIAN_POINT('Ctrl Pts',(-28.3886940030905,28.6409287992575,
-78.8335385750663));
#148988=CARTESIAN_POINT('Ctrl Pts',(-28.3975938613373,28.6079545239895,
-79.001265263691));
#148989=CARTESIAN_POINT('Ctrl Pts',(-28.4065760881628,28.5746750703563,
-79.1705442701821));
#148990=CARTESIAN_POINT('Ctrl Pts',(-28.4155919241668,28.5458521783277,
-79.3407383620272));
#148991=CARTESIAN_POINT('Ctrl Pts',(-28.4246146635513,28.5214788033205,
-79.5112521906048));
#148992=CARTESIAN_POINT('Ctrl Pts',(-28.4281545108594,28.5119165160557,
-79.5781490487952));
#148993=CARTESIAN_POINT('Ctrl Pts',(-28.4316956575249,28.5030385796938,
-79.6450951903288));
#148994=CARTESIAN_POINT('Ctrl Pts',(-28.4352374739099,28.494842646572,-79.7120549851513));
#148995=CARTESIAN_POINT('Ctrl Pts',(-28.4433977632336,28.4759593453834,
-79.8663293007611));
#148996=CARTESIAN_POINT('Ctrl Pts',(-28.4515635189675,28.4606589509008,
-80.0209567625393));
#148997=CARTESIAN_POINT('Ctrl Pts',(-28.4597425456804,28.4489176045266,
-80.1759457293561));
#148998=CARTESIAN_POINT('Ctrl Pts',(-28.4679114902169,28.4371907315526,
-80.3307436433532));
#148999=CARTESIAN_POINT('Ctrl Pts',(-28.4760944511414,28.4290144033317,
-80.4859028728578));
#149000=CARTESIAN_POINT('Ctrl Pts',(-28.4842901842144,28.4244151626594,
-80.641424208971));
#149001=CARTESIAN_POINT('Ctrl Pts',(-28.4895232658188,28.4214784879847,
-80.7407265942301));
#149002=CARTESIAN_POINT('Ctrl Pts',(-28.4947613318242,28.4200012042165,
-80.8401764231172));
#149003=CARTESIAN_POINT('Ctrl Pts',(-28.5,28.4199999807603,-80.9397703408579));
#149004=CARTESIAN_POINT('Ctrl Pts',(-28.2496025504691,29.6431021990262,
-76.2257351951278));
#149005=CARTESIAN_POINT('Ctrl Pts',(-29.,29.2642096076976,-76.0137531166873));
#149006=CARTESIAN_POINT('Ctrl Pts',(-29.,30.0207919771236,-76.4370443259982));
#149007=CARTESIAN_POINT('Ctrl Pts',(-28.2608542879989,32.4163856120597,
-71.2554899486297));
#149008=CARTESIAN_POINT('Ctrl Pts',(-29.,32.0024463153694,-71.1716406391234));
#149009=CARTESIAN_POINT('Ctrl Pts',(-29.,32.8015320477175,-71.4668042994815));
#149010=CARTESIAN_POINT('Ctrl Pts',(-28.2706820191605,35.1297158291743,
-66.2515800426151));
#149011=CARTESIAN_POINT('Ctrl Pts',(-28.9999999999899,34.7556963975018,
-66.1533445021367));
#149012=CARTESIAN_POINT('Ctrl Pts',(-29.,35.5206920342409,-66.4628921538691));
#149013=CARTESIAN_POINT('Ctrl Pts',(-28.2795019009908,37.8065307949999,
-61.2273317382593));
#149014=CARTESIAN_POINT('Ctrl Pts',(-29.,37.4942143736512,-61.0606306836509));
#149015=CARTESIAN_POINT('Ctrl Pts',(-29.,38.2024209812184,-61.4386408691297));
#149016=CARTESIAN_POINT('Origin',(-40.,31.080768958446,-179.64995));
#149017=CARTESIAN_POINT('',(-39.3277310924369,30.340461916791,-179.64995));
#149018=CARTESIAN_POINT('Origin',(-38.5,46.41999998,-129.34995));
#149019=CARTESIAN_POINT('Origin',(-38.5,46.41999998,-58.24995));
#149020=CARTESIAN_POINT('Origin',(-38.5,43.91999998,-58.24995));
#149021=CARTESIAN_POINT('Origin',(-38.5,43.91999998,-58.24995));
#149022=CARTESIAN_POINT('Origin',(0.,43.91999998,-58.24995));
#149023=CARTESIAN_POINT('Origin',(-38.,43.91999998,-58.24995));
#149024=CARTESIAN_POINT('Origin',(-38.,43.91999998,-58.24995));
#149025=CARTESIAN_POINT('Origin',(-37.,28.91999998,-55.24995));
#149026=CARTESIAN_POINT('Origin',(-37.,28.91999998,-70.4461836365688));
#149027=CARTESIAN_POINT('Ctrl Pts',(-37.5,30.3198029183707,-64.9254179945125));
#149028=CARTESIAN_POINT('Ctrl Pts',(-37.5,29.4819543139285,-64.4114488783659));
#149029=CARTESIAN_POINT('Ctrl Pts',(-36.7055659807485,29.9753365781889,
-64.7141088636423));
#149030=CARTESIAN_POINT('Ctrl Pts',(-37.5,30.066275812609,-65.3387061138468));
#149031=CARTESIAN_POINT('Ctrl Pts',(-37.5,29.2617307842025,-64.8907595368038));
#149032=CARTESIAN_POINT('Ctrl Pts',(-36.7276066422259,29.6936558584646,
-65.1425806750807));
#149033=CARTESIAN_POINT('Ctrl Pts',(-37.5,29.8583501338385,-65.770493027413));
#149034=CARTESIAN_POINT('Ctrl Pts',(-37.4999999999999,29.0782932545581,
-65.3939122854256));
#149035=CARTESIAN_POINT('Ctrl Pts',(-36.7506399492972,29.4626112609503,
-65.5904100084171));
#149036=CARTESIAN_POINT('Ctrl Pts',(-37.5,29.5081290337376,-66.6603034853058));
#149037=CARTESIAN_POINT('Ctrl Pts',(-37.5,28.7875108426025,-66.3978618624443));
#149038=CARTESIAN_POINT('Ctrl Pts',(-36.7981064172734,29.0734767074675,
-66.5135522731121));
#149039=CARTESIAN_POINT('Ctrl Pts',(-37.5,29.3662299161008,-67.1188991703195));
#149040=CARTESIAN_POINT('Ctrl Pts',(-37.5,28.6734901542511,-66.902255679337));
#149041=CARTESIAN_POINT('Ctrl Pts',(-36.8225713421442,28.9158110192433,
-66.9894827414662));
#149042=CARTESIAN_POINT('Ctrl Pts',(-37.5,29.0270605890893,-68.5274557979285));
#149043=CARTESIAN_POINT('Ctrl Pts',(-37.5,28.43212483966,-68.3736721849867));
#149044=CARTESIAN_POINT('Ctrl Pts',(-36.8977082013987,28.5389562140588,
-68.4518423383231));
#149045=CARTESIAN_POINT('Ctrl Pts',(-37.5,28.9199999811121,-69.4807175010263));
#149046=CARTESIAN_POINT('Ctrl Pts',(-37.5,28.3657190858733,-69.3869874906105));
#149047=CARTESIAN_POINT('Ctrl Pts',(-36.9485508209842,28.41999998,-69.4422434553462));
#149048=CARTESIAN_POINT('Ctrl Pts',(-37.5,28.91999998,-70.4461836365688));
#149049=CARTESIAN_POINT('Ctrl Pts',(-37.5,28.41999998,-70.4461836365687));
#149050=CARTESIAN_POINT('Ctrl Pts',(-37.,28.41999998,-70.4461836365688));
#149051=CARTESIAN_POINT('',(-36.7055660333102,29.9753365541058,-64.7141088836342));
#149052=CARTESIAN_POINT('Origin',(-37.,30.3198029183592,-64.9254179945062));
#149053=CARTESIAN_POINT('Ctrl Pts',(-36.7055659821207,29.9753365605306,
-64.714108890491));
#149054=CARTESIAN_POINT('Ctrl Pts',(-36.7276066431882,29.6936558488113,
-65.1425806937914));
#149055=CARTESIAN_POINT('Ctrl Pts',(-36.750639949793,29.4626112568857,-65.5904100180595));
#149056=CARTESIAN_POINT('Ctrl Pts',(-36.7981064172734,29.0734767074675,
-66.5135522731121));
#149057=CARTESIAN_POINT('Ctrl Pts',(-36.8225713421442,28.9158110192433,
-66.9894827414662));
#149058=CARTESIAN_POINT('Ctrl Pts',(-36.8977082013987,28.5389562140588,
-68.4518423383231));
#149059=CARTESIAN_POINT('Ctrl Pts',(-36.9485508209842,28.41999998,-69.4422434553462));
#149060=CARTESIAN_POINT('Ctrl Pts',(-37.,28.41999998,-70.4461836365688));
#149061=CARTESIAN_POINT('Ctrl Pts',(-36.7055659807482,29.9753365781776,
-64.714108863636));
#149062=CARTESIAN_POINT('Ctrl Pts',(-37.5,29.4819543139165,-64.4114488783587));
#149063=CARTESIAN_POINT('Ctrl Pts',(-37.5,30.3198029183591,-64.9254179945063));
#149064=CARTESIAN_POINT('Ctrl Pts',(-36.7083606505135,30.6839990376866,
-63.5549861665061));
#149065=CARTESIAN_POINT('Ctrl Pts',(-37.5,30.1937476367692,-63.2670920970213));
#149066=CARTESIAN_POINT('Ctrl Pts',(-37.5,31.0308541172825,-63.7662953234662));
#149067=CARTESIAN_POINT('Ctrl Pts',(-36.7110836457466,31.3874027455588,
-62.3925965705953));
#149068=CARTESIAN_POINT('Ctrl Pts',(-37.5,30.9051975556495,-62.1106946535587));
#149069=CARTESIAN_POINT('Ctrl Pts',(-37.5,31.7365266751429,-62.6039057229559));
#149070=CARTESIAN_POINT('Ctrl Pts',(-36.7137393100582,32.0861766206928,
-61.2273317382593));
#149071=CARTESIAN_POINT('Ctrl Pts',(-37.5,31.6156971887288,-60.9443257831195));
#149072=CARTESIAN_POINT('Ctrl Pts',(-37.5,32.4374646344434,-61.4386408691296));
#149073=CARTESIAN_POINT('Origin',(-37.,32.4374646344434,-61.4386408691297));
#149074=CARTESIAN_POINT('Ctrl Pts',(-36.7137393100582,32.0861766206928,
-61.2273317382593));
#149075=CARTESIAN_POINT('Ctrl Pts',(-36.7110837808245,31.3874382843756,
-62.3925373065787));
#149076=CARTESIAN_POINT('Ctrl Pts',(-36.7083607806502,30.6840320430885,
-63.5549321813014));
#149077=CARTESIAN_POINT('Ctrl Pts',(-36.7055659807394,29.9753365781839,
-64.7141088636381));
#149078=CARTESIAN_POINT('Ctrl Pts',(-37.5,33.02054075664,-61.14995));
#149079=CARTESIAN_POINT('Ctrl Pts',(-37.5,33.0205407566399,-60.64995));
#149080=CARTESIAN_POINT('Ctrl Pts',(-37.,33.02054075664,-60.64995));
#149081=CARTESIAN_POINT('Ctrl Pts',(-37.5,32.9079637588407,-61.149950027061));
#149082=CARTESIAN_POINT('Ctrl Pts',(-37.4999999999984,32.829451263505,-60.5918750690658));
#149083=CARTESIAN_POINT('Ctrl Pts',(-36.9450144953722,32.8396166159335,
-60.64995));
#149084=CARTESIAN_POINT('Ctrl Pts',(-37.5,32.7934674553098,-61.173167066129));
#149085=CARTESIAN_POINT('Ctrl Pts',(-37.5,32.6176893530803,-60.5649300622629));
#149086=CARTESIAN_POINT('Ctrl Pts',(-36.8889168804295,32.6559426968113,
-60.6963841656953));
#149087=CARTESIAN_POINT('Ctrl Pts',(-37.5,32.6399623596936,-61.2443634115781));
#149088=CARTESIAN_POINT('Ctrl Pts',(-37.5,32.2741011266166,-60.5989161145872));
#149089=CARTESIAN_POINT('Ctrl Pts',(-36.8135029743542,32.4100449984504,
-60.8387768064376));
#149090=CARTESIAN_POINT('Ctrl Pts',(-37.5,32.5912011068259,-61.27448425119));
#149091=CARTESIAN_POINT('Ctrl Pts',(-37.5,32.1451108386466,-60.6268090630372));
#149092=CARTESIAN_POINT('Ctrl Pts',(-36.7895122380439,32.3319990572285,
-60.8990185151424));
#149093=CARTESIAN_POINT('Ctrl Pts',(-37.5,32.5044425233165,-61.3474848604736));
#149094=CARTESIAN_POINT('Ctrl Pts',(-37.4999999999999,31.876172903305,-60.7353807030111));
#149095=CARTESIAN_POINT('Ctrl Pts',(-36.7467810375704,32.1932186054134,
-61.0450197081848));
#149096=CARTESIAN_POINT('Ctrl Pts',(-37.5,32.4670287634048,-61.3894925929396));
#149097=CARTESIAN_POINT('Ctrl Pts',(-37.5,31.7388049050588,-60.8179479783099));
#149098=CARTESIAN_POINT('Ctrl Pts',(-36.7283245477951,32.1334017245463,
-61.1290643654114));
#149099=CARTESIAN_POINT('Ctrl Pts',(-37.5,32.4374646344434,-61.4386408691296));
#149100=CARTESIAN_POINT('Ctrl Pts',(-37.5,31.6156971887288,-60.9443257831194));
#149101=CARTESIAN_POINT('Ctrl Pts',(-36.7137393100582,32.0861766206928,
-61.2273317382593));
#149102=CARTESIAN_POINT('Origin',(0.,-12.9675000200281,-61.64995));
#149103=CARTESIAN_POINT('',(-43.0147613882085,26.1152677387813,-61.2273317382593));
#149104=CARTESIAN_POINT('',(-47.508501172308,20.508980519813,-61.2273317382593));
#149105=CARTESIAN_POINT('Origin',(0.,-12.9675000200281,-61.2273317382593));
#149106=CARTESIAN_POINT('Ctrl Pts',(-48.4322308821779,20.76999998,-60.64995));
#149107=CARTESIAN_POINT('Ctrl Pts',(-48.2513645254321,20.7193046642187,
-60.64995));
#149108=CARTESIAN_POINT('Ctrl Pts',(-48.0673245582317,20.6674580465872,
-60.6979267287055));
#149109=CARTESIAN_POINT('Ctrl Pts',(-47.7433968711081,20.5758225659973,
-60.8898150965897));
#149110=CARTESIAN_POINT('Ctrl Pts',(-47.5998785057972,20.5350112502637,
-61.0349912654872));
#149111=CARTESIAN_POINT('Ctrl Pts',(-47.508501172308,20.508980519813,-61.2273317382593));
#149112=CARTESIAN_POINT('Ctrl Pts',(-43.0147613882085,26.1152677387813,
-61.2273317382593));
#149113=CARTESIAN_POINT('Ctrl Pts',(-43.0636216624014,26.1311367864154,
-61.1268955825468));
#149114=CARTESIAN_POINT('Ctrl Pts',(-43.1254911751643,26.1512115744493,
-61.0418249229491));
#149115=CARTESIAN_POINT('Ctrl Pts',(-43.2683662178942,26.1974732479793,
-60.8948259755643));
#149116=CARTESIAN_POINT('Ctrl Pts',(-43.3469540657763,26.2228767030678,
-60.8357750676355));
#149117=CARTESIAN_POINT('Ctrl Pts',(-43.512870268579,26.2763890014657,-60.7418969884463));
#149118=CARTESIAN_POINT('Ctrl Pts',(-43.6010803778225,26.3047810522968,
-60.7070015638854));
#149119=CARTESIAN_POINT('Ctrl Pts',(-43.7785234711652,26.3617623367046,
-60.6613392327119));
#149120=CARTESIAN_POINT('Ctrl Pts',(-43.8687620016371,26.3906766531834,
-60.64995));
#149121=CARTESIAN_POINT('Ctrl Pts',(-43.9604906504041,26.41999998,-60.64995));
#149122=CARTESIAN_POINT('Origin',(-1.64641978096591E-14,26.4199999800001,
-61.14995));
#149123=CARTESIAN_POINT('Origin',(-43.9604906504041,26.41999998,-61.14995));
#149124=CARTESIAN_POINT('Origin',(83.2809572255632,20.76999998,-61.14995));
#149125=CARTESIAN_POINT('Origin',(-48.4322308821779,20.76999998,-61.14995));
#149126=CARTESIAN_POINT('Ctrl Pts',(-49.6616970192851,26.41999998,-171.64995));
#149127=CARTESIAN_POINT('Ctrl Pts',(-49.6616970192851,26.91999998,-171.64995));
#149128=CARTESIAN_POINT('Ctrl Pts',(-49.6616970192851,26.91999998,-171.14995));
#149129=CARTESIAN_POINT('Ctrl Pts',(-49.7951873628098,26.4108894799999,
-171.64995));
#149130=CARTESIAN_POINT('Ctrl Pts',(-49.7964789655964,26.91999998,-171.659148653595));
#149131=CARTESIAN_POINT('Ctrl Pts',(-49.8600119386601,26.91999998,-171.149950000016));
#149132=CARTESIAN_POINT('Ctrl Pts',(-49.9285770883077,26.4017858470187,
-171.675977326981));
#149133=CARTESIAN_POINT('Ctrl Pts',(-49.9258697838501,26.91999998,-171.69520402023));
#149134=CARTESIAN_POINT('Ctrl Pts',(-50.058177378641,26.91999998,-171.18899099047));
#149135=CARTESIAN_POINT('Ctrl Pts',(-50.1751906113998,26.3849548730131,
-171.776163607997));
#149136=CARTESIAN_POINT('Ctrl Pts',(-50.1586485796703,26.91999998,-171.809929875206));
#149137=CARTESIAN_POINT('Ctrl Pts',(-50.4245495045741,26.91999998,-171.339270411997));
#149138=CARTESIAN_POINT('Ctrl Pts',(-50.2882933630855,26.3772357931757,
-171.850283164393));
#149139=CARTESIAN_POINT('Ctrl Pts',(-50.2612232924101,26.9199999800027,
-171.888983273332));
#149140=CARTESIAN_POINT('Ctrl Pts',(-50.5925763632168,26.91999998,-171.450449746589));
#149141=CARTESIAN_POINT('Ctrl Pts',(-50.4770431819562,26.3643539233768,
-172.035403273234));
#149142=CARTESIAN_POINT('Ctrl Pts',(-50.4288800635612,26.9199999799973,
-172.075215659168));
#149143=CARTESIAN_POINT('Ctrl Pts',(-50.8729854484245,26.91999998,-171.728129909852));
#149144=CARTESIAN_POINT('Ctrl Pts',(-50.5526160245901,26.3591961991206,
-172.14633102856));
#149145=CARTESIAN_POINT('Ctrl Pts',(-50.493151129373,26.91999998,-172.18218244132));
#149146=CARTESIAN_POINT('Ctrl Pts',(-50.9852574060669,26.91999998,-171.894521542842));
#149147=CARTESIAN_POINT('Ctrl Pts',(-50.6547666904167,26.3522245814263,
-172.38820210671));
#149148=CARTESIAN_POINT('Ctrl Pts',(-50.5795844587924,26.91999998,-172.40972629816));
#149149=CARTESIAN_POINT('Ctrl Pts',(-51.1370137093498,26.91999998,-172.257328160063));
#149150=CARTESIAN_POINT('Ctrl Pts',(-50.6813043436918,26.3504134295228,
-172.51902671195));
#149151=CARTESIAN_POINT('Ctrl Pts',(-50.6012541744511,26.91999998,-172.529650273731));
#149152=CARTESIAN_POINT('Ctrl Pts',(-51.176438378046,26.91999998,-172.453565067926));
#149153=CARTESIAN_POINT('Ctrl Pts',(-50.6813043436922,26.35041342952,-172.64995));
#149154=CARTESIAN_POINT('Ctrl Pts',(-50.6012541744525,26.9199999800001,
-172.64995));
#149155=CARTESIAN_POINT('Ctrl Pts',(-51.176438378063,26.91999998,-172.64995));
#149156=CARTESIAN_POINT('',(-49.6616970192851,26.41999998,-171.64995));
#149157=CARTESIAN_POINT('Origin',(-49.6616970192851,26.41999998,-171.14995));
#149158=CARTESIAN_POINT('',(-50.676438378063,26.41999998,-172.64995));
#149159=CARTESIAN_POINT('Origin',(-51.176438378063,26.41999998,-172.64995));
#149160=CARTESIAN_POINT('Origin',(-51.176438378063,26.41999998,-172.64995));
#149161=CARTESIAN_POINT('Ctrl Pts',(-50.6813043436922,26.35041342952,-172.64995));
#149162=CARTESIAN_POINT('Ctrl Pts',(-50.6813043436918,26.3504134295228,
-172.51902671195));
#149163=CARTESIAN_POINT('Ctrl Pts',(-50.6547666904167,26.3522245814263,
-172.38820210671));
#149164=CARTESIAN_POINT('Ctrl Pts',(-50.5526160245901,26.3591961991206,
-172.14633102856));
#149165=CARTESIAN_POINT('Ctrl Pts',(-50.4770431819562,26.3643539233768,
-172.035403273234));
#149166=CARTESIAN_POINT('Ctrl Pts',(-50.2882933630855,26.3772357931757,
-171.850283164393));
#149167=CARTESIAN_POINT('Ctrl Pts',(-50.1751906113998,26.3849548730131,
-171.776163607997));
#149168=CARTESIAN_POINT('Ctrl Pts',(-49.9285770883077,26.4017858470187,
-171.675977326981));
#149169=CARTESIAN_POINT('Ctrl Pts',(-49.7951873628098,26.4108894799999,
-171.64995));
#149170=CARTESIAN_POINT('Ctrl Pts',(-49.6616970192851,26.41999998,-171.64995));
#149171=CARTESIAN_POINT('Origin',(-51.176438378063,26.41999998,-55.24995));
#149172=CARTESIAN_POINT('Origin',(-51.176438378063,26.41999998,-176.84995));
#149173=CARTESIAN_POINT('Origin',(83.2809572255632,27.41999998,-176.84995));
#149174=CARTESIAN_POINT('',(-57.,27.41999998,-177.34995));
#149175=CARTESIAN_POINT('Origin',(-57.,27.41999998,-176.84995));
#149176=CARTESIAN_POINT('',(-51.0358975433606,27.41999998,-177.34995));
#149177=CARTESIAN_POINT('',(-60.,27.41999998,-177.34995));
#149178=CARTESIAN_POINT('Ctrl Pts',(-51.176438378063,26.91999998,-176.84995));
#149179=CARTESIAN_POINT('Ctrl Pts',(-51.1764383780557,26.91999998,-176.981217345763));
#149180=CARTESIAN_POINT('Ctrl Pts',(-51.161291852844,26.9738865434699,-177.110943344657));
#149181=CARTESIAN_POINT('Ctrl Pts',(-51.1092579883806,27.1590066353435,
-177.29606343653));
#149182=CARTESIAN_POINT('Ctrl Pts',(-51.0727943880466,27.2887326342368,
-177.34995));
#149183=CARTESIAN_POINT('Ctrl Pts',(-51.0358975433606,27.41999998,-177.34995));
#149184=CARTESIAN_POINT('Origin',(-57.,27.41999998,-174.34995));
#149185=CARTESIAN_POINT('',(-60.,27.41999998,-174.34995));
#149186=CARTESIAN_POINT('Origin',(-59.5,27.41999998,-174.34995));
#149187=CARTESIAN_POINT('Origin',(-57.,27.41999998,-174.34995));
#149188=CARTESIAN_POINT('Origin',(-59.5,27.41999998,-55.24995));
#149189=CARTESIAN_POINT('',(-60.,27.41999998,-58.24995));
#149190=CARTESIAN_POINT('Origin',(-59.5,27.41999998,-58.24995));
#149191=CARTESIAN_POINT('',(-60.,27.41999998,-174.34995));
#149192=CARTESIAN_POINT('Origin',(-57.,27.41999998,-58.24995));
#149193=CARTESIAN_POINT('Origin',(-57.,27.41999998,-58.24995));
#149194=CARTESIAN_POINT('Ctrl Pts',(-43.3501517762232,26.91999998,-61.4386408691297));
#149195=CARTESIAN_POINT('Ctrl Pts',(-42.4913556541499,26.91999998,-60.8975655472507));
#149196=CARTESIAN_POINT('Ctrl Pts',(-43.0147613882086,26.1152677387813,
-61.2273317382593));
#149197=CARTESIAN_POINT('Ctrl Pts',(-43.3818037825525,26.91999998,-61.3884029511195));
#149198=CARTESIAN_POINT('Ctrl Pts',(-42.6316122966568,26.9199999800009,
-60.7676176413114));
#149199=CARTESIAN_POINT('Ctrl Pts',(-43.0636216624014,26.1311367864154,
-61.1268955825468));
#149200=CARTESIAN_POINT('Ctrl Pts',(-43.4218378639138,26.91999998,-61.3458874687825));
#149201=CARTESIAN_POINT('Ctrl Pts',(-42.7839211391678,26.91999998,-60.6895038034116));
#149202=CARTESIAN_POINT('Ctrl Pts',(-43.1254911751643,26.1512115744493,
-61.0418249229491));
#149203=CARTESIAN_POINT('Ctrl Pts',(-43.5142348068871,26.91999998,-61.2723879804742));
#149204=CARTESIAN_POINT('Ctrl Pts',(-43.0730867590013,26.91999998,-60.5931776502515));
#149205=CARTESIAN_POINT('Ctrl Pts',(-43.2683662178942,26.1974732479793,
-60.8948259755643));
#149206=CARTESIAN_POINT('Ctrl Pts',(-43.5650210354047,26.91999998,-61.2428625417913));
#149207=CARTESIAN_POINT('Ctrl Pts',(-43.2058848140176,26.9199999800003,
-60.57262210769));
#149208=CARTESIAN_POINT('Ctrl Pts',(-43.3469540657763,26.2228767030678,
-60.8357750676355));
#149209=CARTESIAN_POINT('Ctrl Pts',(-43.6721398787422,26.91999998,-61.1959234862494));
#149210=CARTESIAN_POINT('Ctrl Pts',(-43.4490485146957,26.9199999799997,
-60.5604852270767));
#149211=CARTESIAN_POINT('Ctrl Pts',(-43.512870268579,26.2763890014657,-60.7418969884463));
#149212=CARTESIAN_POINT('Ctrl Pts',(-43.7290408259741,26.91999998,-61.1784757886431));
#149213=CARTESIAN_POINT('Ctrl Pts',(-43.5624944559174,26.9199999800001,
-60.5672455602404));
#149214=CARTESIAN_POINT('Ctrl Pts',(-43.6010803778225,26.3047810522968,
-60.7070015638854));
#149215=CARTESIAN_POINT('Ctrl Pts',(-43.8433908708859,26.91999998,-61.1556446096555));
#149216=CARTESIAN_POINT('Ctrl Pts',(-43.7695073126827,26.9199999799999,
-60.5973801431191));
#149217=CARTESIAN_POINT('Ctrl Pts',(-43.7785234711652,26.3617623367046,
-60.6613392327119));
#149218=CARTESIAN_POINT('Ctrl Pts',(-43.901489846726,26.91999998,-61.1499500121981));
#149219=CARTESIAN_POINT('Ctrl Pts',(-43.8659505814334,26.91999998,-60.6197279239548));
#149220=CARTESIAN_POINT('Ctrl Pts',(-43.8687620016371,26.3906766531834,
-60.64995));
#149221=CARTESIAN_POINT('Ctrl Pts',(-43.9604906504041,26.91999998,-61.14995));
#149222=CARTESIAN_POINT('Ctrl Pts',(-43.9604906504041,26.91999998,-60.64995));
#149223=CARTESIAN_POINT('Ctrl Pts',(-43.9604906504041,26.41999998,-60.64995));
#149224=CARTESIAN_POINT('Origin',(-43.3501517762232,26.41999998,-61.4386408691297));
#149225=CARTESIAN_POINT('Ctrl Pts',(-43.0147613882085,26.1152677387813,
-61.2273317382593));
#149226=CARTESIAN_POINT('Ctrl Pts',(-42.4913556541499,26.91999998,-60.8975655472507));
#149227=CARTESIAN_POINT('Ctrl Pts',(-43.3501517762232,26.91999998,-61.4386408691297));
#149228=CARTESIAN_POINT('Ctrl Pts',(-42.2597213352523,26.1123501122717,
-62.4299407790815));
#149229=CARTESIAN_POINT('Ctrl Pts',(-41.7218722762073,26.9199999800149,
-62.1010809579055));
#149230=CARTESIAN_POINT('Ctrl Pts',(-42.5924607769204,26.91999998,-62.641249943458));
#149231=CARTESIAN_POINT('Ctrl Pts',(-41.4984253110313,26.1093585902154,
-63.6284728402189));
#149232=CARTESIAN_POINT('Ctrl Pts',(-40.950890457431,26.91999998,-63.291651632712));
#149233=CARTESIAN_POINT('Ctrl Pts',(-41.828377509759,26.91999998,-63.839782013441));
#149234=CARTESIAN_POINT('Ctrl Pts',(-40.7299249439368,26.1062890581501,
-64.8223083020179));
#149235=CARTESIAN_POINT('Ctrl Pts',(-40.1792441039523,26.91999998,-64.466463596043));
#149236=CARTESIAN_POINT('Ctrl Pts',(-41.0569324495432,26.91999998,-65.0336174328882));
#149237=CARTESIAN_POINT('',(-40.7299249193735,26.1062892385305,-64.8223083970342));
#149238=CARTESIAN_POINT('Origin',(-41.0569324495432,26.41999998,-65.0336174328882));
#149239=CARTESIAN_POINT('Ctrl Pts',(-40.7299249439368,26.1062890581501,
-64.8223083020179));
#149240=CARTESIAN_POINT('Ctrl Pts',(-41.4984715481572,26.1093587748547,
-63.6284010127));
#149241=CARTESIAN_POINT('Ctrl Pts',(-42.2597732523974,26.1123503129199,
-62.4298580866994));
#149242=CARTESIAN_POINT('Ctrl Pts',(-43.0147613882085,26.1152677387813,
-61.2273317382593));
#149243=CARTESIAN_POINT('Ctrl Pts',(-39.5144819943711,26.91999998,-71.6866097071051));
#149244=CARTESIAN_POINT('Ctrl Pts',(-39.0463811742787,26.9199999800001,
-71.7084369835555));
#149245=CARTESIAN_POINT('Ctrl Pts',(-39.0160373395819,26.4523138460616,
-71.7098742332801));
#149246=CARTESIAN_POINT('Ctrl Pts',(-39.4806747297125,26.91999998,-70.9435045713511));
#149247=CARTESIAN_POINT('Ctrl Pts',(-38.9720076653828,26.91999998,-70.912377553647));
#149248=CARTESIAN_POINT('Ctrl Pts',(-38.978537754162,26.4135029236992,-70.9394725339304));
#149249=CARTESIAN_POINT('Ctrl Pts',(-39.5061138838564,26.91999998,-70.2084683216835));
#149250=CARTESIAN_POINT('Ctrl Pts',(-38.9629719358347,26.91999998,-70.1446290088561));
#149251=CARTESIAN_POINT('Ctrl Pts',(-39.0068635113108,26.3751216436924,
-70.177811990567));
#149252=CARTESIAN_POINT('Ctrl Pts',(-39.6502847005361,26.91999998,-68.962325974017));
#149253=CARTESIAN_POINT('Ctrl Pts',(-39.0341587958529,26.91999998,-68.8494630385759));
#149254=CARTESIAN_POINT('Ctrl Pts',(-39.167181524895,26.3100882014274,-68.8871399937697));
#149255=CARTESIAN_POINT('Ctrl Pts',(-39.7402010400563,26.91999998,-68.4472152479348));
#149256=CARTESIAN_POINT('Ctrl Pts',(-39.0948775434837,26.91999998,-68.3006173151149));
#149257=CARTESIAN_POINT('Ctrl Pts',(-39.2671383510483,26.2832177198684,
-68.3538279338855));
#149258=CARTESIAN_POINT('Ctrl Pts',(-39.9875645500817,26.91999998,-67.4263054007275));
#149259=CARTESIAN_POINT('Ctrl Pts',(-39.2756374048449,26.9199999800001,
-67.1987893176786));
#149260=CARTESIAN_POINT('Ctrl Pts',(-39.5420936115266,26.229992717107,-67.2971964534767));
#149261=CARTESIAN_POINT('Ctrl Pts',(-40.1455341066151,26.91999998,-66.9202222962256));
#149262=CARTESIAN_POINT('Ctrl Pts',(-39.4018640899458,26.91999998,-66.6416836709376));
#149263=CARTESIAN_POINT('Ctrl Pts',(-39.7176630408463,26.2036238867825,
-66.7735892994237));
#149264=CARTESIAN_POINT('Ctrl Pts',(-40.61463744109,26.91999998,-65.7539057414421));
#149265=CARTESIAN_POINT('Ctrl Pts',(-39.796333686452,26.91999998,-65.2926622581118));
#149266=CARTESIAN_POINT('Ctrl Pts',(-40.2389877944043,26.1428985608433,
-65.5672893219614));
#149267=CARTESIAN_POINT('Ctrl Pts',(-40.9615610612356,26.91999998,-65.1057170341448));
#149268=CARTESIAN_POINT('Ctrl Pts',(-40.11277553943,26.91999998,-64.5135594045473));
#149269=CARTESIAN_POINT('Ctrl Pts',(-40.6245440189136,26.1091814001426,
-64.8971044625718));
#149270=CARTESIAN_POINT('Ctrl Pts',(-41.4294996031359,26.91999998,-64.5117188784924));
#149271=CARTESIAN_POINT('Ctrl Pts',(-40.529229952824,26.9199999800001,-63.7929022611462));
#149272=CARTESIAN_POINT('Ctrl Pts',(-41.1444123040958,26.0783301967522,
-64.2833612530845));
#149273=CARTESIAN_POINT('',(-39.000000010887,26.4199999800102,-71.0516396909909));
#149274=CARTESIAN_POINT('Origin',(-39.5,26.41999998,-71.0516396909898));
#149275=CARTESIAN_POINT('Ctrl Pts',(-39.0000000435479,26.4199999800162,
-71.0516396909931));
#149276=CARTESIAN_POINT('Ctrl Pts',(-39.0000145113878,26.4110146624994,
-70.873151997142));
#149277=CARTESIAN_POINT('Ctrl Pts',(-39.0036304228359,26.4020422627355,
-70.695134532768));
#149278=CARTESIAN_POINT('Ctrl Pts',(-39.0107908237139,26.3931003506741,
-70.5175991632096));
#149279=CARTESIAN_POINT('Ctrl Pts',(-39.0181773354903,26.383876071214,-70.3344575877166));
#149280=CARTESIAN_POINT('Ctrl Pts',(-39.0293349875578,26.3746834666836,
-70.1518284820121));
#149281=CARTESIAN_POINT('Ctrl Pts',(-39.0442524846789,26.3655198198259,
-69.9697097783002));
#149282=CARTESIAN_POINT('Ctrl Pts',(-39.0591699818001,26.3563561729682,
-69.7875910745883));
#149283=CARTESIAN_POINT('Ctrl Pts',(-39.0778470554579,26.3472204702714,
-69.6059820644029));
#149284=CARTESIAN_POINT('Ctrl Pts',(-39.1003301500804,26.3381020579365,
-69.4248755353872));
#149285=CARTESIAN_POINT('Ctrl Pts',(-39.1213238524142,26.3295876946992,
-69.2557664058523));
#149286=CARTESIAN_POINT('Ctrl Pts',(-39.1456304742869,26.3211123234295,
-69.0871090856946));
#149287=CARTESIAN_POINT('Ctrl Pts',(-39.1733342259095,26.3126536217979,
-68.9189042123943));
#149288=CARTESIAN_POINT('Ctrl Pts',(-39.2006004315504,26.3043285147409,
-68.7533559239289));
#149289=CARTESIAN_POINT('Ctrl Pts',(-39.2311575812492,26.2960187931794,
-68.588245391205));
#149290=CARTESIAN_POINT('Ctrl Pts',(-39.2651315757516,26.2877200435148,
-68.4235850326121));
#149291=CARTESIAN_POINT('Ctrl Pts',(-39.2982115270493,26.2796396797319,
-68.2632577963625));
#149292=CARTESIAN_POINT('Ctrl Pts',(-39.3345313341293,26.271569099348,-68.103356945394));
#149293=CARTESIAN_POINT('Ctrl Pts',(-39.374245173882,26.2635303553443,-67.9439118935694));
#149294=CARTESIAN_POINT('Ctrl Pts',(-39.3840891720875,26.2615377658078,
-67.9043897316779));
#149295=CARTESIAN_POINT('Ctrl Pts',(-39.3941418699496,26.2595472856189,
-67.8648956791587));
#149296=CARTESIAN_POINT('Ctrl Pts',(-39.4044059318906,26.257559574683,-67.8254304044373));
#149297=CARTESIAN_POINT('Ctrl Pts',(-39.4477904535049,26.2491578436181,
-67.658617102451));
#149298=CARTESIAN_POINT('Ctrl Pts',(-39.4949549804392,26.2408118245717,
-67.4922912802412));
#149299=CARTESIAN_POINT('Ctrl Pts',(-39.5460345952973,26.2325004784911,
-67.3269367477042));
#149300=CARTESIAN_POINT('Ctrl Pts',(-39.5960590796543,26.2243608164527,
-67.1649978754315));
#149301=CARTESIAN_POINT('Ctrl Pts',(-39.6498392227994,26.2162544279808,
-67.0039905928097));
#149302=CARTESIAN_POINT('Ctrl Pts',(-39.7074854141219,26.2082016737779,
-66.8443933108068));
#149303=CARTESIAN_POINT('Ctrl Pts',(-39.7636025178171,26.2003625220096,
-66.6890294087318));
#149304=CARTESIAN_POINT('Ctrl Pts',(-39.8233838830514,26.1925743712279,
-66.535001809439));
#149305=CARTESIAN_POINT('Ctrl Pts',(-39.886906568172,26.1848929410533,-66.3827738490702));
#149306=CARTESIAN_POINT('Ctrl Pts',(-39.9025350537342,26.183003078867,-66.3453212055576));
#149307=CARTESIAN_POINT('Ctrl Pts',(-39.9183898602438,26.1811198480103,
-66.3079775972808));
#149308=CARTESIAN_POINT('Ctrl Pts',(-39.9344718328247,26.1792444109355,
-66.2707501214404));
#149309=CARTESIAN_POINT('Ctrl Pts',(-39.9822660966514,26.1736707703951,
-66.1601132084024));
#149310=CARTESIAN_POINT('Ctrl Pts',(-40.0320921744015,26.1682149601011,
-66.0503548440615));
#149311=CARTESIAN_POINT('Ctrl Pts',(-40.0841320620358,26.1628014935,-65.9415105087306));
#149312=CARTESIAN_POINT('Ctrl Pts',(-40.1349313000628,26.1575170858865,
-65.8352610614368));
#149313=CARTESIAN_POINT('Ctrl Pts',(-40.1878406174558,26.152272806562,-65.7298824473367));
#149314=CARTESIAN_POINT('Ctrl Pts',(-40.2430471767249,26.1470364906056,
-65.6254334149233));
#149315=CARTESIAN_POINT('Ctrl Pts',(-40.2974041735934,26.1418807552399,
-65.5225917272148));
#149316=CARTESIAN_POINT('Ctrl Pts',(-40.353988821302,26.1367325300632,-65.4206511037866));
#149317=CARTESIAN_POINT('Ctrl Pts',(-40.4129890297332,26.1316016887989,
-65.3196948551107));
#149318=CARTESIAN_POINT('Ctrl Pts',(-40.4705491871184,26.1265960788436,
-65.2212027019928));
#149319=CARTESIAN_POINT('Ctrl Pts',(-40.5304090124457,26.1216069449867,
-65.1236474232294));
#149320=CARTESIAN_POINT('Ctrl Pts',(-40.5927434226748,26.1166843178501,
-65.0271336117946));
#149321=CARTESIAN_POINT('Ctrl Pts',(-40.637191990793,26.1131741582642,-64.9583128640543));
#149322=CARTESIAN_POINT('Ctrl Pts',(-40.6828988377376,26.1096986589903,
-64.8900222275229));
#149323=CARTESIAN_POINT('Ctrl Pts',(-40.7299249270772,26.1062893712319,
-64.8223085129012));
#149324=CARTESIAN_POINT('Origin',(-39.5,26.41999998,-55.24995));
#149325=CARTESIAN_POINT('',(-39.0000000108873,26.4199999800017,-161.007003280499));
#149326=CARTESIAN_POINT('Origin',(-39.5,26.41999998,-161.0070032805));
#149327=CARTESIAN_POINT('',(-39.,26.41999998,-129.34995));
#149328=CARTESIAN_POINT('Ctrl Pts',(-41.4298327884615,26.91999998,-167.547398188302));
#149329=CARTESIAN_POINT('Ctrl Pts',(-40.5295342387659,26.9199999800211,
-168.266393711463));
#149330=CARTESIAN_POINT('Ctrl Pts',(-41.1447896171409,26.078294457151,-167.775763627336));
#149331=CARTESIAN_POINT('Ctrl Pts',(-40.9612348539621,26.91999998,-166.952514419193));
#149332=CARTESIAN_POINT('Ctrl Pts',(-40.1124742201721,26.919999979984,-167.544709932801));
#149333=CARTESIAN_POINT('Ctrl Pts',(-40.6241898364545,26.109190890174,-167.161108892939));
#149334=CARTESIAN_POINT('Ctrl Pts',(-40.6146946127263,26.91999998,-166.304618713242));
#149335=CARTESIAN_POINT('Ctrl Pts',(-39.796315247074,26.91999998,-166.765696010883));
#149336=CARTESIAN_POINT('Ctrl Pts',(-40.239058378987,26.1428924785697,-166.491226580831));
#149337=CARTESIAN_POINT('Ctrl Pts',(-40.2438971241064,26.91999998,-165.383070268286));
#149338=CARTESIAN_POINT('Ctrl Pts',(-39.4770684823812,26.91999998,-165.674348404122));
#149339=CARTESIAN_POINT('Ctrl Pts',(-39.826994448169,26.1908718557831,-165.538116630435));
#149340=CARTESIAN_POINT('Ctrl Pts',(-40.1559725857258,26.91999998,-165.136425734968));
#149341=CARTESIAN_POINT('Ctrl Pts',(-39.4061926872737,26.91999998,-165.399736081576));
#149342=CARTESIAN_POINT('Ctrl Pts',(-39.7292761024087,26.2037183818383,
-165.282971165658));
#149343=CARTESIAN_POINT('Ctrl Pts',(-39.9974565076864,26.91999998,-164.635718209756));
#149344=CARTESIAN_POINT('Ctrl Pts',(-39.2823615806739,26.91999998,-164.849118133022));
#149345=CARTESIAN_POINT('Ctrl Pts',(-39.5530950653548,26.2298065015692,
-164.764919225151));
#149346=CARTESIAN_POINT('Ctrl Pts',(-39.9267078667251,26.91999998,-164.380863661625));
#149347=CARTESIAN_POINT('Ctrl Pts',(-39.2284349479001,26.91999998,-164.571842280085));
#149348=CARTESIAN_POINT('Ctrl Pts',(-39.4744590694183,26.2430893614396,
-164.501193577802));
#149349=CARTESIAN_POINT('Ctrl Pts',(-39.7405665669667,26.91999998,-163.613547303229));
#149350=CARTESIAN_POINT('Ctrl Pts',(-39.0951163240011,26.91999998,-163.76037459309));
#149351=CARTESIAN_POINT('Ctrl Pts',(-39.2675481437431,26.2830943322452,
-163.707008328011));
#149352=CARTESIAN_POINT('Ctrl Pts',(-39.6504680302044,26.91999998,-163.097634164455));
#149353=CARTESIAN_POINT('Ctrl Pts',(-39.034250805552,26.919999979999,-163.210613020243));
#149354=CARTESIAN_POINT('Ctrl Pts',(-39.1673881282116,26.3100067475891,
-163.172866145833));
#149355=CARTESIAN_POINT('Ctrl Pts',(-39.5060746903532,26.91999998,-161.850209820763));
#149356=CARTESIAN_POINT('Ctrl Pts',(-38.9629253593384,26.9199999800013,
-161.914115824651));
#149357=CARTESIAN_POINT('Ctrl Pts',(-39.0068209359397,26.3751075091203,
-161.880866818163));
#149358=CARTESIAN_POINT('Ctrl Pts',(-39.4806915865888,26.91999998,-161.114953773424));
#149359=CARTESIAN_POINT('Ctrl Pts',(-38.9720162576935,26.9199999800008,
-161.146047041293));
#149360=CARTESIAN_POINT('Ctrl Pts',(-38.9785566343046,26.4135006774998,
-161.118978397722));
#149361=CARTESIAN_POINT('Ctrl Pts',(-39.5144747798535,26.91999998,-160.372187822257));
#149362=CARTESIAN_POINT('Ctrl Pts',(-39.0463593412646,26.9199999799985,
-160.350365998772));
#149363=CARTESIAN_POINT('Ctrl Pts',(-39.0160285899416,26.45229437412,-160.348928929189));
#149364=CARTESIAN_POINT('',(-40.7299249193732,26.1062892385183,-167.236334574448));
#149365=CARTESIAN_POINT('Origin',(-41.0569324495328,26.41999998,-167.025025538602));
#149366=CARTESIAN_POINT('Ctrl Pts',(-40.7299249270775,26.1062893712214,
-167.236334458579));
#149367=CARTESIAN_POINT('Ctrl Pts',(-40.6645853304908,26.1110263480999,
-167.142250794741));
#149368=CARTESIAN_POINT('Ctrl Pts',(-40.6018092312385,26.1158892443008,
-167.047079458829));
#149369=CARTESIAN_POINT('Ctrl Pts',(-40.5414282215195,26.1207982581812,
-166.950942290991));
#149370=CARTESIAN_POINT('Ctrl Pts',(-40.4792943195239,26.1258497833008,
-166.852014210915));
#149371=CARTESIAN_POINT('Ctrl Pts',(-40.4196959436351,26.1309501291377,
-166.752063428848));
#149372=CARTESIAN_POINT('Ctrl Pts',(-40.3624432000981,26.1360584358626,
-166.651192119132));
#149373=CARTESIAN_POINT('Ctrl Pts',(-40.3043231046772,26.1412441310092,
-166.548792656962));
#149374=CARTESIAN_POINT('Ctrl Pts',(-40.248619615909,26.1464382085178,-166.445444459256));
#149375=CARTESIAN_POINT('Ctrl Pts',(-40.1951374467669,26.1516433268258,
-166.341224092504));
#149376=CARTESIAN_POINT('Ctrl Pts',(-40.1404552306636,26.1569652389458,
-166.234665201784));
#149377=CARTESIAN_POINT('Ctrl Pts',(-40.0880945140287,26.1622988986898,
-166.127194440059));
#149378=CARTESIAN_POINT('Ctrl Pts',(-40.0378597432825,26.1676913791697,
-166.018863887683));
#149379=CARTESIAN_POINT('Ctrl Pts',(-40.0025451368701,26.1714822459918,
-165.942708452658));
#149380=CARTESIAN_POINT('Ctrl Pts',(-39.968281445585,26.1753031256121,-165.866127477038));
#149381=CARTESIAN_POINT('Ctrl Pts',(-39.9350068722586,26.1791820283199,
-165.789131151273));
#149382=CARTESIAN_POINT('Ctrl Pts',(-39.8781104841659,26.1858145868105,
-165.657474682251));
#149383=CARTESIAN_POINT('Ctrl Pts',(-39.824173358347,26.1925157729063,-165.524625114876));
#149384=CARTESIAN_POINT('Ctrl Pts',(-39.7730275511278,26.1992640596196,
-165.39065734938));
#149385=CARTESIAN_POINT('Ctrl Pts',(-39.726719856284,26.2053739954839,-165.2693621985));
#149386=CARTESIAN_POINT('Ctrl Pts',(-39.6827002133185,26.2115233790131,
-165.147149841886));
#149387=CARTESIAN_POINT('Ctrl Pts',(-39.6408588199536,26.2177241633614,
-165.024056999754));
#149388=CARTESIAN_POINT('Ctrl Pts',(-39.593547601588,26.2247355613755,-164.8848725256));
#149389=CARTESIAN_POINT('Ctrl Pts',(-39.5489550215303,26.2318160157631,
-164.744332341484));
#149390=CARTESIAN_POINT('Ctrl Pts',(-39.5071363085111,26.238934446759,-164.60301081883));
#149391=CARTESIAN_POINT('Ctrl Pts',(-39.4711232425277,26.2450646336215,
-164.481308811457));
#149392=CARTESIAN_POINT('Ctrl Pts',(-39.4371664077637,26.25122276278,-164.359027557099));
#149393=CARTESIAN_POINT('Ctrl Pts',(-39.4052702587627,26.2573922922468,
-164.236533904511));
#149394=CARTESIAN_POINT('Ctrl Pts',(-39.3636932871594,26.2654343399386,
-164.076862117327));
#149395=CARTESIAN_POINT('Ctrl Pts',(-39.325582511077,26.2735180911288,-163.916749616534));
#149396=CARTESIAN_POINT('Ctrl Pts',(-39.2907701194594,26.2816124879209,
-163.756231489263));
#149397=CARTESIAN_POINT('Ctrl Pts',(-39.2553129100334,26.2898568144063,
-163.592740140613));
#149398=CARTESIAN_POINT('Ctrl Pts',(-39.2232769169584,26.2981128611817,
-163.428827555342));
#149399=CARTESIAN_POINT('Ctrl Pts',(-39.1945240576485,26.3063791197979,
-163.264509373524));
#149400=CARTESIAN_POINT('Ctrl Pts',(-39.1651338062026,26.3148286244759,
-163.096548593391));
#149401=CARTESIAN_POINT('Ctrl Pts',(-39.1391734849508,26.3232895602475,
-162.928163525903));
#149402=CARTESIAN_POINT('Ctrl Pts',(-39.1165429759402,26.3317816876087,
-162.759356000773));
#149403=CARTESIAN_POINT('Ctrl Pts',(-39.1109704816533,26.333872773195,-162.717789150953));
#149404=CARTESIAN_POINT('Ctrl Pts',(-39.105600118859,26.3359658181642,-162.67619663796));
#149405=CARTESIAN_POINT('Ctrl Pts',(-39.1004308539458,26.3380612268828,
-162.634578411071));
#149406=CARTESIAN_POINT('Ctrl Pts',(-39.0785784610887,26.3469192938001,
-162.458642787875));
#149407=CARTESIAN_POINT('Ctrl Pts',(-39.0603220000318,26.3557925737031,
-162.282263412771));
#149408=CARTESIAN_POINT('Ctrl Pts',(-39.0456144734669,26.3646901587427,
-162.105434547007));
#149409=CARTESIAN_POINT('Ctrl Pts',(-39.0304671535062,26.3738538047763,
-161.923318037057));
#149410=CARTESIAN_POINT('Ctrl Pts',(-39.0190841572563,26.3830442343986,
-161.740724053985));
#149411=CARTESIAN_POINT('Ctrl Pts',(-39.0114709868334,26.3922645834336,
-161.557650702015));
#149412=CARTESIAN_POINT('Ctrl Pts',(-39.0038578164105,26.4014849324685,
-161.374577350044));
#149413=CARTESIAN_POINT('Ctrl Pts',(-39.0000149601043,26.4107361238319,
-161.191023970058));
#149414=CARTESIAN_POINT('Ctrl Pts',(-39.0000000435492,26.4199999800048,
-161.007003280497));
#149415=CARTESIAN_POINT('Ctrl Pts',(-40.7299249439265,26.10628905815,-167.236334669472));
#149416=CARTESIAN_POINT('Ctrl Pts',(-40.1792441039419,26.91999998,-167.592179375447));
#149417=CARTESIAN_POINT('Ctrl Pts',(-41.0569324495328,26.91999998,-167.025025538602));
#149418=CARTESIAN_POINT('Ctrl Pts',(-41.5498055229506,26.1095638122232,
-168.509987294195));
#149419=CARTESIAN_POINT('Ctrl Pts',(-41.0020315723371,26.9199999800235,
-168.844852386549));
#149420=CARTESIAN_POINT('Ctrl Pts',(-41.879954591083,26.91999998,-168.29867810854));
#149421=CARTESIAN_POINT('Ctrl Pts',(-42.361486708359,26.1127497675934,-169.788980903725));
#149422=CARTESIAN_POINT('Ctrl Pts',(-41.8241014260219,26.9199999799921,
-170.115499778852));
#149423=CARTESIAN_POINT('Ctrl Pts',(-42.6945981803054,26.91999998,-169.577671730211));
#149424=CARTESIAN_POINT('Ctrl Pts',(-43.1661128544364,26.1158519257145,
-171.07256826174));
#149425=CARTESIAN_POINT('Ctrl Pts',(-42.6444458925864,26.91999998,-171.400720533971));
#149426=CARTESIAN_POINT('Ctrl Pts',(-43.502033101348,26.91999998,-170.861259130871));
#149427=CARTESIAN_POINT('',(-43.1661128544364,26.1158519257145,-171.07256826174));
#149428=CARTESIAN_POINT('Origin',(-43.5020331013479,26.41999998,-170.861259130871));
#149429=CARTESIAN_POINT('Ctrl Pts',(-43.1661128544364,26.1158519257145,
-171.07256826174));
#149430=CARTESIAN_POINT('Ctrl Pts',(-42.3615449736022,26.1127499922191,
-169.789073851883));
#149431=CARTESIAN_POINT('Ctrl Pts',(-41.5498582787394,26.1095640229222,
-168.510069248237));
#149432=CARTESIAN_POINT('Ctrl Pts',(-40.7299249439363,26.1062890581356,
-167.236334669465));
#149433=CARTESIAN_POINT('Ctrl Pts',(-44.1114262156583,26.91999998,-171.14995));
#149434=CARTESIAN_POINT('Ctrl Pts',(-44.1114262156583,26.91999998,-171.64995));
#149435=CARTESIAN_POINT('Ctrl Pts',(-44.1114262156583,26.41999998,-171.64995));
#149436=CARTESIAN_POINT('Ctrl Pts',(-43.9948946430299,26.91999998,-171.149949978158));
#149437=CARTESIAN_POINT('Ctrl Pts',(-43.9189401667911,26.91999998,-171.71139261988));
#149438=CARTESIAN_POINT('Ctrl Pts',(-43.9300489743418,26.362103375035,-171.64995));
#149439=CARTESIAN_POINT('Ctrl Pts',(-43.8763450763459,26.91999998,-171.127242425404));
#149440=CARTESIAN_POINT('Ctrl Pts',(-43.7068322349107,26.91999998,-171.744547621103));
#149441=CARTESIAN_POINT('Ctrl Pts',(-43.7459157865524,26.3030441696697,
-171.604534812847));
#149442=CARTESIAN_POINT('Ctrl Pts',(-43.7162275365378,26.91999998,-171.05684827667));
#149443=CARTESIAN_POINT('Ctrl Pts',(-43.3564708632233,26.91999998,-171.726334995184));
#149444=CARTESIAN_POINT('Ctrl Pts',(-43.4976348610037,26.2230846254426,
-171.46374657232));
#149445=CARTESIAN_POINT('Ctrl Pts',(-43.665002290469,26.91999998,-171.026908215035));
#149446=CARTESIAN_POINT('Ctrl Pts',(-43.2222824786043,26.91999998,-171.705069685313));
#149447=CARTESIAN_POINT('Ctrl Pts',(-43.4182794830488,26.1974705898599,
-171.403866413424));
#149448=CARTESIAN_POINT('Ctrl Pts',(-43.5734725485514,26.91999998,-170.953826827844));
#149449=CARTESIAN_POINT('Ctrl Pts',(-42.9355727403744,26.91999998,-171.608576267085));
#149450=CARTESIAN_POINT('Ctrl Pts',(-43.2765868661323,26.1516592710682,
-171.257703672334));
#149451=CARTESIAN_POINT('Ctrl Pts',(-43.5336346878404,26.91999998,-170.91149625204));
#149452=CARTESIAN_POINT('Ctrl Pts',(-42.7841822677167,26.9199999800011,
-171.530641542159));
#149453=CARTESIAN_POINT('Ctrl Pts',(-43.2149501334587,26.1316898999239,
-171.173001781957));
#149454=CARTESIAN_POINT('Ctrl Pts',(-43.5020331013479,26.91999998,-170.861259130871));
#149455=CARTESIAN_POINT('Ctrl Pts',(-42.6444458925863,26.91999998,-171.400720533971));
#149456=CARTESIAN_POINT('Ctrl Pts',(-43.1661128544364,26.1158519257145,
-171.07256826174));
#149457=CARTESIAN_POINT('',(-44.1114262156583,26.41999998,-171.64995));
#149458=CARTESIAN_POINT('Origin',(-44.1114262156583,26.41999998,-171.14995));
#149459=CARTESIAN_POINT('Ctrl Pts',(-44.1114262156583,26.41999998,-171.64995));
#149460=CARTESIAN_POINT('Ctrl Pts',(-43.9300489743418,26.362103375035,-171.64995));
#149461=CARTESIAN_POINT('Ctrl Pts',(-43.7459157865524,26.3030441696697,
-171.604534812847));
#149462=CARTESIAN_POINT('Ctrl Pts',(-43.4976348610037,26.2230846254426,
-171.46374657232));
#149463=CARTESIAN_POINT('Ctrl Pts',(-43.4182794830488,26.1974705898599,
-171.403866413424));
#149464=CARTESIAN_POINT('Ctrl Pts',(-43.2765868661323,26.1516592710682,
-171.257703672334));
#149465=CARTESIAN_POINT('Ctrl Pts',(-43.2149501334587,26.1316898999239,
-171.173001781957));
#149466=CARTESIAN_POINT('Ctrl Pts',(-43.1661128544364,26.1158519257145,
-171.07256826174));
#149467=CARTESIAN_POINT('Origin',(83.2809572255632,26.4199999800001,-171.14995));
#149468=CARTESIAN_POINT('',(-43.6598261881496,26.41999998,-171.64995));
#149469=CARTESIAN_POINT('Origin',(-57.,-2.42462934179819E-14,-58.24995));
#149470=CARTESIAN_POINT('',(-60.,27.91999998,-58.24995));
#149471=CARTESIAN_POINT('',(-60.,-54.58000002,-58.24995));
#149472=CARTESIAN_POINT('Origin',(-57.,27.91999998,-58.24995));
#149473=CARTESIAN_POINT('Origin',(-57.,27.91999998,-58.24995));
#149474=CARTESIAN_POINT('Origin',(-59.5,27.91999998,-58.24995));
#149475=CARTESIAN_POINT('Origin',(-41.7558360441701,29.41999998,-179.64995));
#149476=CARTESIAN_POINT('',(-41.0540572871253,28.7076050220164,-179.64995));
#149477=CARTESIAN_POINT('Ctrl Pts',(-45.342056117244,28.41999998,-61.14995));
#149478=CARTESIAN_POINT('Ctrl Pts',(-45.342056117244,28.41999998,-60.6499449120928));
#149479=CARTESIAN_POINT('Ctrl Pts',(-45.342056117244,28.9200050678813,-60.6499500000259));
#149480=CARTESIAN_POINT('Ctrl Pts',(-45.2032855852163,28.41999998,-61.1499499725599));
#149481=CARTESIAN_POINT('Ctrl Pts',(-45.2207546457868,28.41999998,-60.688556379456));
#149482=CARTESIAN_POINT('Ctrl Pts',(-45.2161093325487,28.8799153348109,
-60.6499495913736));
#149483=CARTESIAN_POINT('Ctrl Pts',(-45.0642313709311,28.41999998,-61.1448442113686));
#149484=CARTESIAN_POINT('Ctrl Pts',(-45.0814092233342,28.4199999800005,
-60.7134256454893));
#149485=CARTESIAN_POINT('Ctrl Pts',(-45.0809055449378,28.8470468727513,
-60.6499493090119));
#149486=CARTESIAN_POINT('Ctrl Pts',(-44.7862672310244,28.41999998,-61.1362430899869));
#149487=CARTESIAN_POINT('Ctrl Pts',(-44.7998786663716,28.4199999799995,
-60.7430249240652));
#149488=CARTESIAN_POINT('Ctrl Pts',(-44.7999542633237,28.8023061531432,
-60.6499489465081));
#149489=CARTESIAN_POINT('Ctrl Pts',(-44.647272115325,28.41999998,-61.1328798677618));
#149490=CARTESIAN_POINT('Ctrl Pts',(-44.652744176702,28.41999998,-60.7493138199263));
#149491=CARTESIAN_POINT('Ctrl Pts',(-44.6541596767004,28.7904721518728,
-60.6499488654503));
#149492=CARTESIAN_POINT('Ctrl Pts',(-44.3691883762669,28.41999998,-61.1328719599062));
#149493=CARTESIAN_POINT('Ctrl Pts',(-44.3637416796284,28.41999998,-60.7493310407855));
#149494=CARTESIAN_POINT('Ctrl Pts',(-44.36232828092,28.7904412154038,-60.6499488652048));
#149495=CARTESIAN_POINT('Ctrl Pts',(-44.2300913879779,28.41999998,-61.1362301431742));
#149496=CARTESIAN_POINT('Ctrl Pts',(-44.2164931090599,28.41999998,-60.7430562060495));
#149497=CARTESIAN_POINT('Ctrl Pts',(-44.2164190292987,28.8022526047183,
-60.6499489461074));
#149498=CARTESIAN_POINT('Ctrl Pts',(-43.952003265591,28.41999998,-61.1448329195507));
#149499=CARTESIAN_POINT('Ctrl Pts',(-43.9348222136893,28.41999998,-60.7134784063315));
#149500=CARTESIAN_POINT('Ctrl Pts',(-43.9353228646302,28.8469743774063,
-60.6499493083947));
#149501=CARTESIAN_POINT('Ctrl Pts',(-43.812959462792,28.41999998,-61.149949972467));
#149502=CARTESIAN_POINT('Ctrl Pts',(-43.7954409326635,28.4199999800005,
-60.6886488998596));
#149503=CARTESIAN_POINT('Ctrl Pts',(-43.8001087095939,28.8798156648002,
-60.6499495903585));
#149504=CARTESIAN_POINT('Ctrl Pts',(-43.6738487993976,28.41999998,-61.14995));
#149505=CARTESIAN_POINT('Ctrl Pts',(-43.6738487993976,28.41999998,-60.6499449120928));
#149506=CARTESIAN_POINT('Ctrl Pts',(-43.6738487993976,28.9200050678813,
-60.6499500000259));
#149507=CARTESIAN_POINT('Origin',(-59.5,27.91999998,0.));
#149508=CARTESIAN_POINT('',(-60.,27.91999998,-174.34995));
#149509=CARTESIAN_POINT('Origin',(-59.5,27.91999998,-174.34995));
#149510=CARTESIAN_POINT('',(-60.,27.91999998,-58.24995));
#149511=CARTESIAN_POINT('Origin',(-57.,27.91999998,-174.34995));
#149512=CARTESIAN_POINT('',(-57.,27.91999998,-177.34995));
#149513=CARTESIAN_POINT('Origin',(-57.,27.91999998,-176.84995));
#149514=CARTESIAN_POINT('Origin',(-57.,27.91999998,-174.34995));
#149515=CARTESIAN_POINT('Origin',(-60.,27.91999998,-176.84995));
#149516=CARTESIAN_POINT('',(-50.9656271260094,27.91999998,-177.34995));
#149517=CARTESIAN_POINT('',(-60.,27.91999998,-177.34995));
#149518=CARTESIAN_POINT('Ctrl Pts',(-50.9656271260094,27.91999998,-177.34995));
#149519=CARTESIAN_POINT('Ctrl Pts',(-50.9287302813235,28.0512673257631,
-177.34995));
#149520=CARTESIAN_POINT('Ctrl Pts',(-50.8922666809894,28.1809933246567,
-177.29606343653));
#149521=CARTESIAN_POINT('Ctrl Pts',(-50.840232816526,28.3661134165298,-177.110943344657));
#149522=CARTESIAN_POINT('Ctrl Pts',(-50.8250862913143,28.41999998,-176.981217345763));
#149523=CARTESIAN_POINT('Ctrl Pts',(-50.825086291307,28.41999998,-176.84995));
#149524=CARTESIAN_POINT('Origin',(-50.825086291307,28.91999998,-171.64995));
#149525=CARTESIAN_POINT('Origin',(-50.825086291307,28.91999998,-176.84995));
#149526=CARTESIAN_POINT('Origin',(-50.825086291307,28.91999998,-172.64995));
#149527=CARTESIAN_POINT('Ctrl Pts',(-50.3299522569362,28.85041342952,-172.64995));
#149528=CARTESIAN_POINT('Ctrl Pts',(-50.3904429223989,28.41999998,-172.64995));
#149529=CARTESIAN_POINT('Ctrl Pts',(-50.825086291307,28.41999998,-172.64995));
#149530=CARTESIAN_POINT('Ctrl Pts',(-50.3299522569358,28.8504134295228,
-172.51902671195));
#149531=CARTESIAN_POINT('Ctrl Pts',(-50.3904429223853,28.4199999800017,
-172.511015867074));
#149532=CARTESIAN_POINT('Ctrl Pts',(-50.82508629129,28.41999998,-172.453565067926));
#149533=CARTESIAN_POINT('Ctrl Pts',(-50.3034146036607,28.8522245814264,
-172.38820210671));
#149534=CARTESIAN_POINT('Ctrl Pts',(-50.3606872372737,28.41999998,-172.371853931892));
#149535=CARTESIAN_POINT('Ctrl Pts',(-50.7856616225938,28.41999998,-172.257328160063));
#149536=CARTESIAN_POINT('Ctrl Pts',(-50.2012639378342,28.8591961991206,
-172.14633102856));
#149537=CARTESIAN_POINT('Ctrl Pts',(-50.247876228143,28.41999998,-172.118296873734));
#149538=CARTESIAN_POINT('Ctrl Pts',(-50.6339053193109,28.41999998,-171.894521542842));
#149539=CARTESIAN_POINT('Ctrl Pts',(-50.1256910952006,28.8643539233763,
-172.035403273235));
#149540=CARTESIAN_POINT('Ctrl Pts',(-50.1643071358756,28.4199999800017,
-172.003556970023));
#149541=CARTESIAN_POINT('Ctrl Pts',(-50.5216333616693,28.41999998,-171.728129909852));
#149542=CARTESIAN_POINT('Ctrl Pts',(-49.9369412763291,28.8772357931761,
-171.850283164392));
#149543=CARTESIAN_POINT('Ctrl Pts',(-49.9598619165025,28.4199999799983,
-171.817687494207));
#149544=CARTESIAN_POINT('Ctrl Pts',(-50.2412242764601,28.41999998,-171.450449746589));
#149545=CARTESIAN_POINT('Ctrl Pts',(-49.8238385246439,28.8849548730131,
-171.776163607997));
#149546=CARTESIAN_POINT('Ctrl Pts',(-49.8382982003454,28.4199999800004,
-171.746711574348));
#149547=CARTESIAN_POINT('Ctrl Pts',(-50.0731974178181,28.41999998,-171.339270411997));
#149548=CARTESIAN_POINT('Ctrl Pts',(-49.5772250015517,28.9017858470187,
-171.675977326981));
#149549=CARTESIAN_POINT('Ctrl Pts',(-49.5798629394444,28.4199999799996,
-171.658003579003));
#149550=CARTESIAN_POINT('Ctrl Pts',(-49.7068252918851,28.41999998,-171.18899099047));
#149551=CARTESIAN_POINT('Ctrl Pts',(-49.443835276054,28.9108894800008,-171.64995));
#149552=CARTESIAN_POINT('Ctrl Pts',(-49.4425933612922,28.41999998,-171.640924254978));
#149553=CARTESIAN_POINT('Ctrl Pts',(-49.5086598519041,28.41999998,-171.149950000016));
#149554=CARTESIAN_POINT('Ctrl Pts',(-49.3103449325291,28.91999998,-171.64995));
#149555=CARTESIAN_POINT('Ctrl Pts',(-49.3103449325291,28.41999998,-171.64995));
#149556=CARTESIAN_POINT('Ctrl Pts',(-49.3103449325291,28.41999998,-171.14995));
#149557=CARTESIAN_POINT('Origin',(-49.3103449325291,28.91999998,-171.14995));
#149558=CARTESIAN_POINT('Ctrl Pts',(-49.3103449325291,28.91999998,-171.64995));
#149559=CARTESIAN_POINT('Ctrl Pts',(-49.443835276054,28.9108894800008,-171.64995));
#149560=CARTESIAN_POINT('Ctrl Pts',(-49.5772250015517,28.9017858470187,
-171.675977326981));
#149561=CARTESIAN_POINT('Ctrl Pts',(-49.8238385246439,28.8849548730131,
-171.776163607997));
#149562=CARTESIAN_POINT('Ctrl Pts',(-49.9369412763291,28.8772357931761,
-171.850283164392));
#149563=CARTESIAN_POINT('Ctrl Pts',(-50.1256910952006,28.8643539233763,
-172.035403273235));
#149564=CARTESIAN_POINT('Ctrl Pts',(-50.2012639378342,28.8591961991206,
-172.14633102856));
#149565=CARTESIAN_POINT('Ctrl Pts',(-50.3034146036607,28.8522245814264,
-172.38820210671));
#149566=CARTESIAN_POINT('Ctrl Pts',(-50.3299522569358,28.8504134295228,
-172.51902671195));
#149567=CARTESIAN_POINT('Ctrl Pts',(-50.3299522569362,28.85041342952,-172.64995));
#149568=CARTESIAN_POINT('Origin',(-60.,28.91999998,-171.14995));
#149569=CARTESIAN_POINT('Origin',(-60.,28.91999998,-171.14995));
#149570=CARTESIAN_POINT('Origin',(-42.,28.91999998,-171.14995));
#149571=CARTESIAN_POINT('Origin',(-60.,11.61999998,-176.84995));
#149572=CARTESIAN_POINT('',(-53.6325912458891,11.61999998,-177.34995));
#149573=CARTESIAN_POINT('',(-53.3846587239314,11.8868850448361,-177.272764808359));
#149574=CARTESIAN_POINT('Ctrl Pts',(-53.6325912458891,11.61999998,-177.34995));
#149575=CARTESIAN_POINT('Ctrl Pts',(-53.6010140858531,11.6544395308136,
-177.34995));
#149576=CARTESIAN_POINT('Ctrl Pts',(-53.5694844728451,11.6886293911647,
-177.346396020703));
#149577=CARTESIAN_POINT('Ctrl Pts',(-53.5384795926869,11.7220946388468,
-177.339415709356));
#149578=CARTESIAN_POINT('Ctrl Pts',(-53.5095770053376,11.7532907679517,
-177.332908699574));
#149579=CARTESIAN_POINT('Ctrl Pts',(-53.4811304040669,11.7838607674282,
-177.323423109353));
#149580=CARTESIAN_POINT('Ctrl Pts',(-53.4535263405212,11.8134148549189,
-177.311025575324));
#149581=CARTESIAN_POINT('Ctrl Pts',(-53.4298706264844,11.8387416710648,
-177.300401323598));
#149582=CARTESIAN_POINT('Ctrl Pts',(-53.4068336627752,11.8633233108441,
-177.287637217697));
#149583=CARTESIAN_POINT('Ctrl Pts',(-53.3846587239314,11.886885044836,-177.272764808359));
#149584=CARTESIAN_POINT('',(-57.,11.61999998,-177.34995));
#149585=CARTESIAN_POINT('',(-60.,11.61999998,-177.34995));
#149586=CARTESIAN_POINT('Origin',(-57.,11.61999998,-176.84995));
#149587=CARTESIAN_POINT('Ctrl Pts',(-53.3846587239314,11.8868850448361,
-177.272764808359));
#149588=CARTESIAN_POINT('Ctrl Pts',(-53.3209180569567,11.9546120038032,
-177.230014853822));
#149589=CARTESIAN_POINT('Ctrl Pts',(-53.2731270360347,12.0145014233151,
-177.168462633103));
#149590=CARTESIAN_POINT('Ctrl Pts',(-53.2113113817619,12.0970286741326,
-177.021779308321));
#149591=CARTESIAN_POINT('Ctrl Pts',(-53.1963133903003,12.11999998,-176.935788696125));
#149592=CARTESIAN_POINT('Ctrl Pts',(-53.1963133798215,12.11999998,-176.84995));
#149593=CARTESIAN_POINT('Origin',(-53.1963133798215,12.61999998,-179.64995));
#149594=CARTESIAN_POINT('Origin',(-53.1963133798215,12.61999998,-171.855638188259));
#149595=CARTESIAN_POINT('Origin',(-53.1963133798215,12.61999998,-176.84995));
#149596=CARTESIAN_POINT('Ctrl Pts',(-52.7217372011832,12.4615824973952,
-171.881858542095));
#149597=CARTESIAN_POINT('Ctrl Pts',(-52.8357962988228,12.1199999800004,
-171.884866486815));
#149598=CARTESIAN_POINT('Ctrl Pts',(-53.1958197283118,12.11999998,-171.894290758533));
#149599=CARTESIAN_POINT('Ctrl Pts',(-52.7290806418237,12.4488888857452,
-171.760397092706));
#149600=CARTESIAN_POINT('Ctrl Pts',(-52.8493435053801,12.1199999799985,
-171.750925740441));
#149601=CARTESIAN_POINT('Ctrl Pts',(-53.2003775471301,12.11999998,-171.715353582304));
#149602=CARTESIAN_POINT('Ctrl Pts',(-52.7133768168196,12.4424829119345,
-171.643651148372));
#149603=CARTESIAN_POINT('Ctrl Pts',(-52.8340183717379,12.11999998,-171.617247566893));
#149604=CARTESIAN_POINT('Ctrl Pts',(-53.1734142621322,12.11999998,-171.541767472582));
#149605=CARTESIAN_POINT('Ctrl Pts',(-52.6344997605979,12.4386942197548,
-171.419334545233));
#149606=CARTESIAN_POINT('Ctrl Pts',(-52.7460023418722,12.11999998,-171.362905444502));
#149607=CARTESIAN_POINT('Ctrl Pts',(-53.0531021129573,12.11999998,-171.206197136279));
#149608=CARTESIAN_POINT('Ctrl Pts',(-52.5738654759387,12.4413473579302,
-171.318822511501));
#149609=CARTESIAN_POINT('Ctrl Pts',(-52.6758688342237,12.1199999799997,
-171.248558765417));
#149610=CARTESIAN_POINT('Ctrl Pts',(-52.9635655392073,12.11999998,-171.054813778703));
#149611=CARTESIAN_POINT('Ctrl Pts',(-52.4932465322732,12.4468321277953,
-171.230060927849));
#149612=CARTESIAN_POINT('Ctrl Pts',(-52.5838617435422,12.1199999800001,
-171.150392701598));
#149613=CARTESIAN_POINT('Ctrl Pts',(-52.8454881851277,12.11999998,-170.920313606715));
#149614=CARTESIAN_POINT('',(-52.5103993912278,12.4456688534686,-171.249463176904));
#149615=CARTESIAN_POINT('Origin',(-52.8706140943225,12.61999998,-170.949706593448));
#149616=CARTESIAN_POINT('Ctrl Pts',(-52.5103994272594,12.4456688709067,
-171.249463146917));
#149617=CARTESIAN_POINT('Ctrl Pts',(-52.5325366961564,12.4442258341098,
-171.275226079363));
#149618=CARTESIAN_POINT('Ctrl Pts',(-52.5530277603095,12.4430004743987,
-171.301970103452));
#149619=CARTESIAN_POINT('Ctrl Pts',(-52.5718680671356,12.4420632072567,
-171.329650850542));
#149620=CARTESIAN_POINT('Ctrl Pts',(-52.5908098491538,12.4411208919293,
-171.357480688046));
#149621=CARTESIAN_POINT('Ctrl Pts',(-52.6080841933948,12.4404700110404,
-171.386258116276));
#149622=CARTESIAN_POINT('Ctrl Pts',(-52.623669495073,12.4401548684418,-171.415979764924));
#149623=CARTESIAN_POINT('Ctrl Pts',(-52.6392009898804,12.4398408138451,
-171.445598802217));
#149624=CARTESIAN_POINT('Ctrl Pts',(-52.6530559575077,12.439860219518,-171.476156593959));
#149625=CARTESIAN_POINT('Ctrl Pts',(-52.665181108264,12.4402279645502,-171.507677529715));
#149626=CARTESIAN_POINT('Ctrl Pts',(-52.6682114522294,12.4403198721859,
-171.515555310319));
#149627=CARTESIAN_POINT('Ctrl Pts',(-52.6711335593541,12.4404333955636,
-171.523493340927));
#149628=CARTESIAN_POINT('Ctrl Pts',(-52.6739461945108,12.4405684861021,
-171.531492148308));
#149629=CARTESIAN_POINT('Ctrl Pts',(-52.6852405434796,12.4411109523655,
-171.563611963663));
#149630=CARTESIAN_POINT('Ctrl Pts',(-52.6945617501349,12.4420117639115,
-171.596133997172));
#149631=CARTESIAN_POINT('Ctrl Pts',(-52.7019620487256,12.4433297091624,
-171.629022442916));
#149632=CARTESIAN_POINT('Ctrl Pts',(-52.7094702315576,12.444666867898,-171.66239034837));
#149633=CARTESIAN_POINT('Ctrl Pts',(-52.7150019789283,12.4464332409464,
-171.696136308534));
#149634=CARTESIAN_POINT('Ctrl Pts',(-52.7185804246579,12.4486728316355,
-171.730263044942));
#149635=CARTESIAN_POINT('Ctrl Pts',(-52.7221795352094,12.4509253555213,
-171.764586856555));
#149636=CARTESIAN_POINT('Ctrl Pts',(-52.723803419686,12.4536561359556,-171.799296939246));
#149637=CARTESIAN_POINT('Ctrl Pts',(-52.7234321145001,12.4568970612263,
-171.834421393416));
#149638=CARTESIAN_POINT('Ctrl Pts',(-52.723357573706,12.4575476881298,-171.841472748491));
#149639=CARTESIAN_POINT('Ctrl Pts',(-52.7232024646285,12.458218847644,-171.84854085354));
#149640=CARTESIAN_POINT('Ctrl Pts',(-52.7229663801057,12.4589107657309,
-171.855625995355));
#149641=CARTESIAN_POINT('Ctrl Pts',(-52.811758955289,12.11999998,-170.861259130871));
#149642=CARTESIAN_POINT('Ctrl Pts',(-52.5194581681217,12.11999998,-171.0127167027));
#149643=CARTESIAN_POINT('Ctrl Pts',(-52.4039495302269,12.4224147476539,
-171.07256826174));
#149644=CARTESIAN_POINT('Ctrl Pts',(-52.8281457246307,12.11999998,-170.892884198111));
#149645=CARTESIAN_POINT('Ctrl Pts',(-52.5427333133061,12.11999998,-171.068676662146));
#149646=CARTESIAN_POINT('Ctrl Pts',(-52.4335834030071,12.4288943780099,
-171.135818022105));
#149647=CARTESIAN_POINT('Ctrl Pts',(-52.8478360402188,12.11999998,-170.922334416373));
#149648=CARTESIAN_POINT('Ctrl Pts',(-52.5708615508922,12.11999998,-171.121670121752));
#149649=CARTESIAN_POINT('Ctrl Pts',(-52.4691942899059,12.4366759982665,
-171.194717391534));
#149650=CARTESIAN_POINT('Ctrl Pts',(-52.8706140943225,12.11999998,-170.949706593448));
#149651=CARTESIAN_POINT('Ctrl Pts',(-52.6035237155536,12.11999998,-171.171968757444));
#149652=CARTESIAN_POINT('Ctrl Pts',(-52.5103993792154,12.4456688476555,
-171.249463186897));
#149653=CARTESIAN_POINT('',(-52.4039495302269,12.4224147476539,-171.07256826174));
#149654=CARTESIAN_POINT('Origin',(-52.811758955289,12.61999998,-170.861259130871));
#149655=CARTESIAN_POINT('Origin',(-53.2781268802541,12.612394155154,-170.643546468484));
#149656=CARTESIAN_POINT('Ctrl Pts',(-52.4039495302269,12.4224147476539,
-171.07256826174));
#149657=CARTESIAN_POINT('Ctrl Pts',(-52.5194581681217,12.11999998,-171.0127167027));
#149658=CARTESIAN_POINT('Ctrl Pts',(-52.811758955289,12.11999998,-170.861259130871));
#149659=CARTESIAN_POINT('Ctrl Pts',(-50.4067968770089,12.4163544181458,
-167.212559451309));
#149660=CARTESIAN_POINT('Ctrl Pts',(-50.5326451268968,12.11999998,-167.168095406566));
#149661=CARTESIAN_POINT('Ctrl Pts',(-50.8116692616976,12.11999998,-167.001248800573));
#149662=CARTESIAN_POINT('Ctrl Pts',(-48.3933978906048,12.4097551621214,
-163.361420582663));
#149663=CARTESIAN_POINT('Ctrl Pts',(-48.5227235736013,12.1199999799924,
-163.318503470872));
#149664=CARTESIAN_POINT('Ctrl Pts',(-48.7949136859973,12.11999998,-163.150111451781));
#149665=CARTESIAN_POINT('Ctrl Pts',(-44.3204976166945,12.3951430089669,
-155.684386060413));
#149666=CARTESIAN_POINT('Ctrl Pts',(-44.4529340155615,12.1199999800075,
-155.63827143996));
#149667=CARTESIAN_POINT('Ctrl Pts',(-44.7140165615046,12.11999998,-155.473076929555));
#149668=CARTESIAN_POINT('Ctrl Pts',(-42.2612000992887,12.3871318438137,
-151.858374821466));
#149669=CARTESIAN_POINT('Ctrl Pts',(-42.3975527923274,12.11999998,-151.814329756678));
#149670=CARTESIAN_POINT('Ctrl Pts',(-42.6500851427248,12.11999998,-151.647062446733));
#149671=CARTESIAN_POINT('Ctrl Pts',(-40.1676286103837,12.3781782553102,
-148.051158746523));
#149672=CARTESIAN_POINT('Ctrl Pts',(-40.2925576368927,12.11999998,-147.98227543296));
#149673=CARTESIAN_POINT('Ctrl Pts',(-40.5508657493446,12.11999998,-147.839849615653));
#149674=CARTESIAN_POINT('',(-40.1676233686655,12.3782630082023,-148.051084687213));
#149675=CARTESIAN_POINT('Origin',(-40.5508657493455,12.6199999799991,-147.839849615653));
#149676=CARTESIAN_POINT('Ctrl Pts',(-40.1676286103913,12.3781782553039,
-148.05115874653));
#149677=CARTESIAN_POINT('Ctrl Pts',(-42.2612000992887,12.3871318438137,
-151.858374821466));
#149678=CARTESIAN_POINT('Ctrl Pts',(-44.3204976166945,12.3951430089669,
-155.684386060413));
#149679=CARTESIAN_POINT('Ctrl Pts',(-48.3933978906048,12.4097551621214,
-163.361420582663));
#149680=CARTESIAN_POINT('Ctrl Pts',(-50.4067968770089,12.4163544181458,
-167.212559451309));
#149681=CARTESIAN_POINT('Ctrl Pts',(-52.4039495302269,12.4224147476539,
-171.07256826174));
#149682=CARTESIAN_POINT('Ctrl Pts',(-39.5011854382618,12.11999998,-143.364449166524));
#149683=CARTESIAN_POINT('Ctrl Pts',(-38.9925241823799,12.11999998,-143.356382176468));
#149684=CARTESIAN_POINT('Ctrl Pts',(-39.0013190202884,12.6286555741689,
-143.356503342193));
#149685=CARTESIAN_POINT('Ctrl Pts',(-39.4888154687586,12.11999998,-144.170854505439));
#149686=CARTESIAN_POINT('Ctrl Pts',(-39.0234415001674,12.11999998,-144.168885424266));
#149687=CARTESIAN_POINT('Ctrl Pts',(-38.9875647212365,12.5840154882559,
-144.20450574525));
#149688=CARTESIAN_POINT('Ctrl Pts',(-39.5732179658618,12.11999998,-144.962464848579));
#149689=CARTESIAN_POINT('Ctrl Pts',(-39.144316819298,12.11999998,-144.998554248167));
#149690=CARTESIAN_POINT('Ctrl Pts',(-39.0813386654269,12.5398855005079,
-145.035762056675));
#149691=CARTESIAN_POINT('Ctrl Pts',(-39.9390749458245,12.11999998,-146.514415033293));
#149692=CARTESIAN_POINT('Ctrl Pts',(-39.5960174049575,12.11999998,-146.600763849103));
#149693=CARTESIAN_POINT('Ctrl Pts',(-39.4878341117614,12.4529560363788,
-146.663462436008));
#149694=CARTESIAN_POINT('Ctrl Pts',(-40.2242048982474,12.11999998,-147.279924873294));
#149695=CARTESIAN_POINT('Ctrl Pts',(-39.9191166230722,12.11999998,-147.391920922171));
#149696=CARTESIAN_POINT('Ctrl Pts',(-39.8046575553952,12.4098586926345,
-147.465310993273));
#149697=CARTESIAN_POINT('Ctrl Pts',(-40.6264968255545,12.11999998,-147.973584999442));
#149698=CARTESIAN_POINT('Ctrl Pts',(-40.3763612390272,12.11999998,-148.118773982031));
#149699=CARTESIAN_POINT('Ctrl Pts',(-40.2516272065149,12.3706972604334,
-148.191122309056));
#149700=CARTESIAN_POINT('',(-39.,12.61999998,-143.518796834034));
#149701=CARTESIAN_POINT('Origin',(-39.5,12.61999998,-143.518796834034));
#149702=CARTESIAN_POINT('Ctrl Pts',(-39.,12.61999998,-143.518796834034));
#149703=CARTESIAN_POINT('Ctrl Pts',(-39.0000000062752,12.6119352885895,
-143.671852275596));
#149704=CARTESIAN_POINT('Ctrl Pts',(-39.0036267878565,12.6038716318385,
-143.824372346437));
#149705=CARTESIAN_POINT('Ctrl Pts',(-39.0107948009928,12.5958320293859,
-143.976333330001));
#149706=CARTESIAN_POINT('Ctrl Pts',(-39.018273628606,12.5874438191974,-144.134883541672));
#149707=CARTESIAN_POINT('Ctrl Pts',(-39.0296066235717,12.5790811718621,
-144.292825751123));
#149708=CARTESIAN_POINT('Ctrl Pts',(-39.0447472042233,12.5707473406039,
-144.450154052002));
#149709=CARTESIAN_POINT('Ctrl Pts',(-39.0594100046057,12.562676493985,-144.602517658352));
#149710=CARTESIAN_POINT('Ctrl Pts',(-39.0776439179631,12.5546318065498,
-144.754306301496));
#149711=CARTESIAN_POINT('Ctrl Pts',(-39.0994578733345,12.5466067917887,
-144.905522814717));
#149712=CARTESIAN_POINT('Ctrl Pts',(-39.1211182504263,12.538638276087,-145.055674707993));
#149713=CARTESIAN_POINT('Ctrl Pts',(-39.1463084852436,12.53068835278,-145.205263225827));
#149714=CARTESIAN_POINT('Ctrl Pts',(-39.175088270677,12.5227534543617,-145.354288091831));
#149715=CARTESIAN_POINT('Ctrl Pts',(-39.2033745208226,12.5149546289654,
-145.500757378319));
#149716=CARTESIAN_POINT('Ctrl Pts',(-39.2351285884225,12.5071695759667,
-145.64668282469));
#149717=CARTESIAN_POINT('Ctrl Pts',(-39.2704536342457,12.4994090078912,
-145.792051096222));
#149718=CARTESIAN_POINT('Ctrl Pts',(-39.2751179610196,12.4983843007857,
-145.811245554577));
#149719=CARTESIAN_POINT('Ctrl Pts',(-39.2798446093254,12.4973600503235,
-145.830430271798));
#149720=CARTESIAN_POINT('Ctrl Pts',(-39.2846338730941,12.4963363105606,
-145.84960519063));
#149721=CARTESIAN_POINT('Ctrl Pts',(-39.3228940288552,12.4881579255985,
-146.002788522491));
#149722=CARTESIAN_POINT('Ctrl Pts',(-39.3651577699322,12.4800894902938,
-146.155474174756));
#149723=CARTESIAN_POINT('Ctrl Pts',(-39.4115476402542,12.4720604749179,
-146.307305745164));
#149724=CARTESIAN_POINT('Ctrl Pts',(-39.4576308395821,12.4640845372098,
-146.458133597771));
#149725=CARTESIAN_POINT('Ctrl Pts',(-39.5077865778487,12.4561471247028,
-146.608118946099));
#149726=CARTESIAN_POINT('Ctrl Pts',(-39.5621399172821,12.4482218744652,
-146.756880619399));
#149727=CARTESIAN_POINT('Ctrl Pts',(-39.6132477630658,12.4407698490485,
-146.896759580596));
#149728=CARTESIAN_POINT('Ctrl Pts',(-39.6680675972591,12.4333287413512,
-147.035556528922));
#149729=CARTESIAN_POINT('Ctrl Pts',(-39.7266970656795,12.4259153625784,
-147.172925407409));
#149730=CARTESIAN_POINT('Ctrl Pts',(-39.7840967394881,12.4186574846744,
-147.307412876408));
#149731=CARTESIAN_POINT('Ctrl Pts',(-39.8451486132704,12.4114262190347,
-147.440531530225));
#149732=CARTESIAN_POINT('Ctrl Pts',(-39.9099278090628,12.4042745591491,
-147.571928505937));
#149733=CARTESIAN_POINT('Ctrl Pts',(-39.9729591449271,12.397315863989,-147.699780153467));
#149734=CARTESIAN_POINT('Ctrl Pts',(-40.0395200099146,12.3904327283686,
-147.826001622394));
#149735=CARTESIAN_POINT('Ctrl Pts',(-40.1096540546844,12.3837078549757,
-147.950242323608));
#149736=CARTESIAN_POINT('Ctrl Pts',(-40.1287133093867,12.3818803391771,
-147.984005315271));
#149737=CARTESIAN_POINT('Ctrl Pts',(-40.1480362664377,12.3800646988528,
-148.017621885214));
#149738=CARTESIAN_POINT('Ctrl Pts',(-40.1676233686655,12.3782630082023,
-148.051084687213));
#149739=CARTESIAN_POINT('Origin',(-39.5,12.61999998,-55.24995));
#149740=CARTESIAN_POINT('',(-39.,12.61999998,-88.5398461374725));
#149741=CARTESIAN_POINT('Origin',(-39.5,12.61999998,-88.5398461374725));
#149742=CARTESIAN_POINT('',(-39.,12.61999998,-129.34995));
#149743=CARTESIAN_POINT('Ctrl Pts',(-40.5508657493525,12.11999998,-84.2187933558389));
#149744=CARTESIAN_POINT('Ctrl Pts',(-40.2925576369006,12.11999998,-84.0763675385317));
#149745=CARTESIAN_POINT('Ctrl Pts',(-40.1676286103916,12.3781782553103,
-84.0074842249685));
#149746=CARTESIAN_POINT('Ctrl Pts',(-40.1865238705097,12.11999998,-84.8795757011402));
#149747=CARTESIAN_POINT('Ctrl Pts',(-39.8775141197021,12.1199999800054,
-84.7681083762916));
#149748=CARTESIAN_POINT('Ctrl Pts',(-39.7628532325843,12.4154575211986,
-84.6989357525887));
#149749=CARTESIAN_POINT('Ctrl Pts',(-39.9318518139617,12.11999998,-85.5794220290239));
#149750=CARTESIAN_POINT('Ctrl Pts',(-39.5877950605282,12.11999998,-85.491056146558));
#149751=CARTESIAN_POINT('Ctrl Pts',(-39.4798353483971,12.4548420036467,
-85.4321181873043));
#149752=CARTESIAN_POINT('Ctrl Pts',(-39.6727396192083,12.11999998,-86.6717926677035));
#149753=CARTESIAN_POINT('Ctrl Pts',(-39.2736158380134,12.11999998,-86.5998217220713));
#149754=CARTESIAN_POINT('Ctrl Pts',(-39.1919329104561,12.5160219327601,
-86.5777868689076));
#149755=CARTESIAN_POINT('Ctrl Pts',(-39.6078129604692,12.11999998,-87.0440021565177));
#149756=CARTESIAN_POINT('Ctrl Pts',(-39.1889752494415,12.11999998,-86.9856596406021));
#149757=CARTESIAN_POINT('Ctrl Pts',(-39.1197921781136,12.5368211423774,
-86.9683825953982));
#149758=CARTESIAN_POINT('Ctrl Pts',(-39.5216886477957,12.11999998,-87.7889298981597));
#149759=CARTESIAN_POINT('Ctrl Pts',(-39.0619634825428,12.11999998,-87.7602623143372));
#149760=CARTESIAN_POINT('Ctrl Pts',(-39.0240984977364,12.5783336340252,
-87.7505987241496));
#149761=CARTESIAN_POINT('Ctrl Pts',(-39.5000000006739,12.11999998,-88.163385731595));
#149762=CARTESIAN_POINT('Ctrl Pts',(-39.0204289960451,12.11999998,-88.152135192235));
#149763=CARTESIAN_POINT('Ctrl Pts',(-39.,12.5991444608023,-88.1440404246245));
#149764=CARTESIAN_POINT('Ctrl Pts',(-39.5,12.11999998,-88.5398461374725));
#149765=CARTESIAN_POINT('Ctrl Pts',(-39.,12.11999998,-88.5398461374725));
#149766=CARTESIAN_POINT('Ctrl Pts',(-39.,12.61999998,-88.5398461374725));
#149767=CARTESIAN_POINT('',(-40.1676094221395,12.3781800225324,-84.0075170032023));
#149768=CARTESIAN_POINT('Origin',(-40.5508657493525,12.61999998,-84.2187933558389));
#149769=CARTESIAN_POINT('Ctrl Pts',(-40.1676094221395,12.3781800225324,
-84.0075170032023));
#149770=CARTESIAN_POINT('Ctrl Pts',(-39.7628442883141,12.4154587658777,
-84.6989589235648));
#149771=CARTESIAN_POINT('Ctrl Pts',(-39.4798323155101,12.4548426481422,
-85.4321302562663));
#149772=CARTESIAN_POINT('Ctrl Pts',(-39.2879003897697,12.4956286230557,
-86.1958973083732));
#149773=CARTESIAN_POINT('Ctrl Pts',(-39.1919329104561,12.5160219327601,
-86.5777868689076));
#149774=CARTESIAN_POINT('Ctrl Pts',(-39.1197921781136,12.5368211423774,
-86.9683825953982));
#149775=CARTESIAN_POINT('Ctrl Pts',(-39.071945337925,12.5575773882013,-87.3594906597739));
#149776=CARTESIAN_POINT('Ctrl Pts',(-39.0240984977364,12.5783336340252,
-87.7505987241496));
#149777=CARTESIAN_POINT('Ctrl Pts',(-39.,12.5991444608023,-88.1440404246245));
#149778=CARTESIAN_POINT('Ctrl Pts',(-39.,12.61999998,-88.5398461374725));
#149779=CARTESIAN_POINT('Ctrl Pts',(-40.1676286103916,12.3781782553103,
-84.0074842249685));
#149780=CARTESIAN_POINT('Ctrl Pts',(-40.2925576369006,12.11999998,-84.0763675385317));
#149781=CARTESIAN_POINT('Ctrl Pts',(-40.5508657493525,12.11999998,-84.2187933558389));
#149782=CARTESIAN_POINT('Ctrl Pts',(-42.2393869130494,12.3870385552721,
-80.2399360160109));
#149783=CARTESIAN_POINT('Ctrl Pts',(-42.3754889509591,12.11999998,-80.2844795011615));
#149784=CARTESIAN_POINT('Ctrl Pts',(-42.6282131590433,12.11999998,-80.4512482683356));
#149785=CARTESIAN_POINT('Ctrl Pts',(-44.2775738677864,12.39497584134,-76.4539726940548));
#149786=CARTESIAN_POINT('Ctrl Pts',(-44.4098483480378,12.11999998,-76.5004916194052));
#149787=CARTESIAN_POINT('Ctrl Pts',(-44.6709958246245,12.11999998,-76.6652818249261));
#149788=CARTESIAN_POINT('Ctrl Pts',(-48.3090097368786,12.4094651694423,
-68.8574405644517));
#149789=CARTESIAN_POINT('Ctrl Pts',(-48.4382080167511,12.11999998,-68.9007945866128));
#149790=CARTESIAN_POINT('Ctrl Pts',(-48.710372157466,12.11999998,-69.0687496953211));
#149791=CARTESIAN_POINT('Ctrl Pts',(-50.3020637690764,12.4160155627679,
-65.046761180979));
#149792=CARTESIAN_POINT('Ctrl Pts',(-50.4278516292118,12.1199999799963,
-65.0915922935902));
#149793=CARTESIAN_POINT('Ctrl Pts',(-50.7067648613536,12.11999998,-65.2580717844373));
#149794=CARTESIAN_POINT('Ctrl Pts',(-52.2790965136749,12.4220352393542,
-61.2273317382593));
#149795=CARTESIAN_POINT('Ctrl Pts',(-52.3947118718251,12.11999998,-61.287265650179));
#149796=CARTESIAN_POINT('Ctrl Pts',(-52.6867218473722,12.11999998,-61.4386408691297));
#149797=CARTESIAN_POINT('Origin',(-52.6867218473722,12.61999998,-61.4386408691297));
#149798=CARTESIAN_POINT('Ctrl Pts',(-52.2790965136749,12.4220352393542,
-61.2273317382593));
#149799=CARTESIAN_POINT('Ctrl Pts',(-50.3020637710939,12.4160155580201,
-65.0467611816981));
#149800=CARTESIAN_POINT('Ctrl Pts',(-48.3090097389604,12.409465164778,-68.8574405651503));
#149801=CARTESIAN_POINT('Ctrl Pts',(-44.2775738699394,12.3949758368643,
-76.453972694812));
#149802=CARTESIAN_POINT('Ctrl Pts',(-42.2393869152768,12.3870385509018,
-80.2399360167399));
#149803=CARTESIAN_POINT('Ctrl Pts',(-40.1676286103916,12.3781782553103,
-84.0074842249685));
#149804=CARTESIAN_POINT('Ctrl Pts',(-52.8224784153177,12.11999998,-61.275204160084));
#149805=CARTESIAN_POINT('Ctrl Pts',(-52.5913010098401,12.11999998,-60.9843891047162));
#149806=CARTESIAN_POINT('Ctrl Pts',(-52.5245819708721,12.475697298624,-60.9004583201679));
#149807=CARTESIAN_POINT('Ctrl Pts',(-52.7664652938449,12.11999998,-61.3197306493527));
#149808=CARTESIAN_POINT('Ctrl Pts',(-52.5094515064391,12.1199999800004,
-61.0719533871486));
#149809=CARTESIAN_POINT('Ctrl Pts',(-52.4232534240833,12.4535953097813,
-60.9895181215267));
#149810=CARTESIAN_POINT('Ctrl Pts',(-52.7200145740509,12.11999998,-61.3744177048719));
#149811=CARTESIAN_POINT('Ctrl Pts',(-52.4421916143175,12.11999998,-61.1731178858937));
#149812=CARTESIAN_POINT('Ctrl Pts',(-52.339276259362,12.4352188308071,-61.0988911211005));
#149813=CARTESIAN_POINT('Ctrl Pts',(-52.6867218473722,12.11999998,-61.4386408691297));
#149814=CARTESIAN_POINT('Ctrl Pts',(-52.3947118718252,12.11999998,-61.287265650179));
#149815=CARTESIAN_POINT('Ctrl Pts',(-52.2790965136749,12.4220352393542,
-61.2273317382593));
#149816=CARTESIAN_POINT('Origin',(-52.8224784153158,12.6199999800056,-61.2752041600831));
#149817=CARTESIAN_POINT('Ctrl Pts',(-52.5245819708698,12.4756972986233,
-60.9004583201698));
#149818=CARTESIAN_POINT('Ctrl Pts',(-52.5913010098385,12.11999998,-60.9843891047178));
#149819=CARTESIAN_POINT('Ctrl Pts',(-52.8224784153175,12.11999998,-61.2752041600839));
#149820=CARTESIAN_POINT('Ctrl Pts',(-52.6505629615106,12.4839221309077,
-60.7971452199062));
#149821=CARTESIAN_POINT('Ctrl Pts',(-52.7297264322295,12.1199999799996,
-60.865773772671));
#149822=CARTESIAN_POINT('Ctrl Pts',(-53.0127900201976,12.11999998,-61.1239198608288));
#149823=CARTESIAN_POINT('Ctrl Pts',(-52.7486445377005,12.4996864767879,
-60.660571058145));
#149824=CARTESIAN_POINT('Ctrl Pts',(-52.8314129775774,12.1199999800002,
-60.7072763762979));
#149825=CARTESIAN_POINT('Ctrl Pts',(-53.1625689933938,12.11999998,-60.9259844495965));
#149826=CARTESIAN_POINT('Ctrl Pts',(-52.81219032515,12.5218539749099,-60.5055220850798));
#149827=CARTESIAN_POINT('Ctrl Pts',(-52.8857929788878,12.11999998,-60.5379900686008));
#149828=CARTESIAN_POINT('Ctrl Pts',(-53.2607580814926,12.11999998,-60.7033966151602));
#149829=CARTESIAN_POINT('Origin',(-59.5,11.61999998,-55.24995));
#149830=CARTESIAN_POINT('',(-60.,11.61999998,-174.34995));
#149831=CARTESIAN_POINT('Origin',(-59.5,11.61999998,-174.34995));
#149832=CARTESIAN_POINT('',(-60.,11.61999998,-58.24995));
#149833=CARTESIAN_POINT('Origin',(-57.,11.61999998,-174.34995));
#149834=CARTESIAN_POINT('Origin',(-57.,11.61999998,-174.34995));
#149835=CARTESIAN_POINT('Origin',(0.,-12.9675000200281,-60.64995));
#149836=CARTESIAN_POINT('',(-40.4031452851323,17.9943647515726,-76.7018642453134));
#149837=CARTESIAN_POINT('Ctrl Pts',(-40.1676234671477,12.3782653664715,
-84.0075554250447));
#149838=CARTESIAN_POINT('Ctrl Pts',(-40.1941985853479,13.012226003964,-83.2338432608986));
#149839=CARTESIAN_POINT('Ctrl Pts',(-40.2205526779777,13.6386751861752,
-82.4505770135348));
#149840=CARTESIAN_POINT('Ctrl Pts',(-40.2466278643551,14.2587699734049,
-81.6591515576613));
#149841=CARTESIAN_POINT('Ctrl Pts',(-40.3002576413502,15.5341413043586,
-80.0313982564001));
#149842=CARTESIAN_POINT('Ctrl Pts',(-40.352516590638,16.777641980889,-78.3751691578809));
#149843=CARTESIAN_POINT('Ctrl Pts',(-40.4031453084497,17.9943647931319,
-76.7018643085084));
#149844=CARTESIAN_POINT('Ctrl Pts',(-40.4031453149964,17.9943646866131,
-76.7018642268486));
#149845=CARTESIAN_POINT('Ctrl Pts',(-43.3980120961201,18.0071650557604,
-71.5873748987318));
#149846=CARTESIAN_POINT('Ctrl Pts',(-46.3056933853622,18.0183276393305,
-66.4219286454218));
#149847=CARTESIAN_POINT('Ctrl Pts',(-49.1629069712534,18.0283224583225,
-61.2273317382593));
#149848=CARTESIAN_POINT('Ctrl Pts',(-49.5462350640495,18.76999998,-61.4386408691297));
#149849=CARTESIAN_POINT('Ctrl Pts',(-48.8042785465888,18.76999998,-61.0296382684994));
#149850=CARTESIAN_POINT('Ctrl Pts',(-49.1629069712534,18.0283224583225,
-61.2273317382593));
#149851=CARTESIAN_POINT('Ctrl Pts',(-49.5720983755525,18.76999998,-61.3917233465932));
#149852=CARTESIAN_POINT('Ctrl Pts',(-48.8976639972856,18.7699999800003,
-60.912976735742));
#149853=CARTESIAN_POINT('Ctrl Pts',(-49.2072136788996,18.0400790290492,
-61.1335104039183));
#149854=CARTESIAN_POINT('Ctrl Pts',(-49.6050257059303,18.76999998,-61.3505216375984));
#149855=CARTESIAN_POINT('Ctrl Pts',(-49.0074625403989,18.7699999800005,
-60.8254916046238));
#149856=CARTESIAN_POINT('Ctrl Pts',(-49.2636489250068,18.0550404895701,
-61.0510932718963));
#149857=CARTESIAN_POINT('Ctrl Pts',(-49.6828096124638,18.76999998,-61.2778731737785));
#149858=CARTESIAN_POINT('Ctrl Pts',(-49.2376424762765,18.7699999799996,
-60.6973789326117));
#149859=CARTESIAN_POINT('Ctrl Pts',(-49.3970153298707,18.0903238932961,
-60.9057963508575));
#149860=CARTESIAN_POINT('Ctrl Pts',(-49.7267438680042,18.76999998,-61.2475100972213));
#149861=CARTESIAN_POINT('Ctrl Pts',(-49.3535760550633,18.7699999800002,
-60.656860805429));
#149862=CARTESIAN_POINT('Ctrl Pts',(-49.4723725947842,18.1102284712985,
-60.8450701877959));
#149863=CARTESIAN_POINT('Ctrl Pts',(-49.8682179142305,18.76999998,-61.1743894610928));
#149864=CARTESIAN_POINT('Ctrl Pts',(-49.6800903574717,18.7699999799997,
-60.5889551600382));
#149865=CARTESIAN_POINT('Ctrl Pts',(-49.7151670266325,18.1742094267258,
-60.6988289354793));
#149866=CARTESIAN_POINT('Ctrl Pts',(-49.9744290136678,18.76999998,-61.1499500118827));
#149867=CARTESIAN_POINT('Ctrl Pts',(-49.8890563478339,18.76999998,-60.5998057785282));
#149868=CARTESIAN_POINT('Ctrl Pts',(-49.897617121419,18.2220908968247,-60.64995));
#149869=CARTESIAN_POINT('Ctrl Pts',(-50.0811190791972,18.76999998,-61.14995));
#149870=CARTESIAN_POINT('Ctrl Pts',(-50.0811190791972,18.76999998,-60.64995));
#149871=CARTESIAN_POINT('Ctrl Pts',(-50.0811190791972,18.26999998,-60.64995));
#149872=CARTESIAN_POINT('Origin',(-49.5462350640495,18.26999998,-61.4386408691297));
#149873=CARTESIAN_POINT('Origin',(-50.0811190791972,18.26999998,-61.14995));
#149874=CARTESIAN_POINT('Origin',(83.2809572255632,18.26999998,-61.14995));
#149875=CARTESIAN_POINT('Ctrl Pts',(-49.1629069712534,18.0283224583225,
-61.2273317382593));
#149876=CARTESIAN_POINT('Ctrl Pts',(-48.8042785465888,18.76999998,-61.0296382684995));
#149877=CARTESIAN_POINT('Ctrl Pts',(-49.5462350640495,18.76999998,-61.4386408691297));
#149878=CARTESIAN_POINT('Ctrl Pts',(-46.3056933853622,18.0183276393305,
-66.4219286454218));
#149879=CARTESIAN_POINT('Ctrl Pts',(-45.867410270929,18.769999980105,-66.3106234612426));
#149880=CARTESIAN_POINT('Ctrl Pts',(-46.6827176097033,18.76999998,-66.6332421622494));
#149881=CARTESIAN_POINT('Ctrl Pts',(-43.3980120961201,18.0071650557604,
-71.5873748987318));
#149882=CARTESIAN_POINT('Ctrl Pts',(-42.9058979134104,18.76999997996,-71.4956126488948));
#149883=CARTESIAN_POINT('Ctrl Pts',(-43.7675014857899,18.76999998,-71.7986930470318));
#149884=CARTESIAN_POINT('Ctrl Pts',(-40.4031453149964,17.9943646866131,
-76.7018642268486));
#149885=CARTESIAN_POINT('Ctrl Pts',(-39.9612665046713,18.76999998,-76.4422678974524));
#149886=CARTESIAN_POINT('Ctrl Pts',(-40.7628307834967,18.76999998,-76.913173357719));
#149887=CARTESIAN_POINT('Origin',(-40.7628307834967,18.26999998,-76.9131733577189));
#149888=CARTESIAN_POINT('Ctrl Pts',(-39.5,18.76999998,-81.9737790469184));
#149889=CARTESIAN_POINT('Ctrl Pts',(-39.0000000000011,18.76999998,-81.9737790469193));
#149890=CARTESIAN_POINT('Ctrl Pts',(-39.,18.2699999800011,-81.9737790469193));
#149891=CARTESIAN_POINT('Ctrl Pts',(-39.5000000014778,18.76999998,-81.0900715307985));
#149892=CARTESIAN_POINT('Ctrl Pts',(-38.9495856510588,18.76999998,-81.0044062795137));
#149893=CARTESIAN_POINT('Ctrl Pts',(-38.9999999999983,18.2220313158448,
-81.0514322138321));
#149894=CARTESIAN_POINT('Ctrl Pts',(-39.5988774762002,18.76999998,-80.2205083311056));
#149895=CARTESIAN_POINT('Ctrl Pts',(-39.0100135050444,18.76999998,-80.0786830893324));
#149896=CARTESIAN_POINT('Ctrl Pts',(-39.1098638639319,18.1747125385734,
-80.1448153615248));
#149897=CARTESIAN_POINT('Ctrl Pts',(-39.9044907342272,18.76999998,-78.9396134649389));
#149898=CARTESIAN_POINT('Ctrl Pts',(-39.229508253648,18.7699999800001,-78.7338553009239));
#149899=CARTESIAN_POINT('Ctrl Pts',(-39.4494341483978,18.1049192927842,
-78.810548635267));
#149900=CARTESIAN_POINT('Ctrl Pts',(-40.0341671712988,18.76999998,-78.514605681855));
#149901=CARTESIAN_POINT('Ctrl Pts',(-39.3342349384753,18.76999998,-78.2659886991342));
#149902=CARTESIAN_POINT('Ctrl Pts',(-39.5935190801229,18.0817455339462,
-78.3680408652321));
#149903=CARTESIAN_POINT('Ctrl Pts',(-40.3511672955439,18.76999998,-77.6933701733068));
#149904=CARTESIAN_POINT('Ctrl Pts',(-39.5993180096537,18.76999998,-77.3418642254583));
#149905=CARTESIAN_POINT('Ctrl Pts',(-39.9457414385913,18.036947832209,-77.5133471330197));
#149906=CARTESIAN_POINT('Ctrl Pts',(-40.5384105179099,18.76999998,-77.2951763044633));
#149907=CARTESIAN_POINT('Ctrl Pts',(-39.7649903796933,18.76999998,-76.8813885224012));
#149908=CARTESIAN_POINT('Ctrl Pts',(-40.1537986734602,18.0152160834001,
-77.0990973343972));
#149909=CARTESIAN_POINT('Ctrl Pts',(-40.7628307834967,18.76999998,-76.913173357719));
#149910=CARTESIAN_POINT('Ctrl Pts',(-39.9612665046713,18.76999998,-76.4422678974524));
#149911=CARTESIAN_POINT('Ctrl Pts',(-40.4031453149964,17.9943646866131,
-76.7018642268486));
#149912=CARTESIAN_POINT('',(-39.,18.2699999799838,-81.9737790469184));
#149913=CARTESIAN_POINT('Origin',(-39.5,18.26999998,-81.9737790469175));
#149914=CARTESIAN_POINT('Ctrl Pts',(-39.,18.2699999800011,-81.9737790469184));
#149915=CARTESIAN_POINT('Ctrl Pts',(-38.9999999999983,18.2220313158448,
-81.0514322138315));
#149916=CARTESIAN_POINT('Ctrl Pts',(-39.109863863932,18.1747125385734,-80.1448153615245));
#149917=CARTESIAN_POINT('Ctrl Pts',(-39.3362440535758,18.1281837080473,
-79.2553042106863));
#149918=CARTESIAN_POINT('Ctrl Pts',(-39.4494341483978,18.1049192927842,
-78.810548635267));
#149919=CARTESIAN_POINT('Ctrl Pts',(-39.5935190801229,18.0817455339463,
-78.3680408652321));
#149920=CARTESIAN_POINT('Ctrl Pts',(-39.7696302593571,18.0593466830776,
-77.9406939991259));
#149921=CARTESIAN_POINT('Ctrl Pts',(-39.9457414342936,18.0369478327556,
-77.5133471434485));
#149922=CARTESIAN_POINT('Ctrl Pts',(-40.1537986633056,18.0152160844608,
-77.0990973546155));
#149923=CARTESIAN_POINT('Ctrl Pts',(-40.4031452967415,17.9943646881397,
-76.7018642559303));
#149924=CARTESIAN_POINT('Origin',(-39.5,18.26999998,-55.24995));
#149925=CARTESIAN_POINT('',(-39.,18.26999998,-150.084863924608));
#149926=CARTESIAN_POINT('Origin',(-39.5,18.26999998,-150.084863924608));
#149927=CARTESIAN_POINT('',(-39.,18.26999998,-129.34995));
#149928=CARTESIAN_POINT('Ctrl Pts',(-40.7628307834967,18.76999998,-155.145469613787));
#149929=CARTESIAN_POINT('Ctrl Pts',(-39.9612665046713,18.76999998,-155.616375074053));
#149930=CARTESIAN_POINT('Ctrl Pts',(-40.4031453149963,17.9943646866131,
-155.356778744658));
#149931=CARTESIAN_POINT('Ctrl Pts',(-40.5382265796732,18.76999998,-154.763153570891));
#149932=CARTESIAN_POINT('Ctrl Pts',(-39.7648410678857,18.76999998,-155.176920406762));
#149933=CARTESIAN_POINT('Ctrl Pts',(-40.1535949024652,18.0152331222464,
-154.959221008645));
#149934=CARTESIAN_POINT('Ctrl Pts',(-40.3517329455581,18.76999998,-154.366209991013));
#149935=CARTESIAN_POINT('Ctrl Pts',(-39.5997667004894,18.76999998,-154.717664579548));
#149936=CARTESIAN_POINT('Ctrl Pts',(-39.9463699385113,18.0368966498548,
-154.546270136328));
#149937=CARTESIAN_POINT('Ctrl Pts',(-40.0364383090907,18.76999998,-153.550444480173));
#149938=CARTESIAN_POINT('Ctrl Pts',(-39.3360417060011,18.76999998,-153.799575452297));
#149939=CARTESIAN_POINT('Ctrl Pts',(-39.5960425666541,18.0813960858844,
-153.697271402021));
#149940=CARTESIAN_POINT('Ctrl Pts',(-39.9079301282699,18.76999998,-153.131458232674));
#149941=CARTESIAN_POINT('Ctrl Pts',(-39.23220455254,18.76999998,-153.338508255374));
#149942=CARTESIAN_POINT('Ctrl Pts',(-39.4532556977585,18.1042418116532,
-153.261037480867));
#149943=CARTESIAN_POINT('Ctrl Pts',(-39.7023798052426,18.76999998,-152.273874561686));
#149944=CARTESIAN_POINT('Ctrl Pts',(-39.0797143668984,18.76999998,-152.409570079113));
#149945=CARTESIAN_POINT('Ctrl Pts',(-39.2248664505887,18.1509702537189,
-152.367727156036));
#149946=CARTESIAN_POINT('Ctrl Pts',(-39.6264148660465,18.76999998,-151.83867201801));
#149947=CARTESIAN_POINT('Ctrl Pts',(-39.0281802867267,18.76999998,-151.943644934638));
#149948=CARTESIAN_POINT('Ctrl Pts',(-39.1404609620539,18.1746678021094,
-151.914185519153));
#149949=CARTESIAN_POINT('Ctrl Pts',(-39.5253915082876,18.76999998,-150.965860868517));
#149950=CARTESIAN_POINT('Ctrl Pts',(-38.9776025606259,18.76999998,-151.019307709025));
#149951=CARTESIAN_POINT('Ctrl Pts',(-39.0282127872062,18.2221486757409,
-151.004139862532));
#149952=CARTESIAN_POINT('Ctrl Pts',(-39.5000000006086,18.76999998,-150.526727576342));
#149953=CARTESIAN_POINT('Ctrl Pts',(-38.9754245522527,18.76999998,-150.557403393481));
#149954=CARTESIAN_POINT('Ctrl Pts',(-39.,18.2460151034934,-150.546047809514));
#149955=CARTESIAN_POINT('Ctrl Pts',(-39.5,18.76999998,-150.084863924608));
#149956=CARTESIAN_POINT('Ctrl Pts',(-39.,18.76999998,-150.084863924608));
#149957=CARTESIAN_POINT('Ctrl Pts',(-39.,18.26999998,-150.084863924608));
#149958=CARTESIAN_POINT('',(-40.4031452850214,17.9943647518538,-155.356778726108));
#149959=CARTESIAN_POINT('Origin',(-40.7628307834967,18.26999998,-155.145469613787));
#149960=CARTESIAN_POINT('Ctrl Pts',(-40.4031452966654,17.994364688146,-155.356778715455));
#149961=CARTESIAN_POINT('Ctrl Pts',(-40.1535948923173,18.0152331233072,
-154.959220988423));
#149962=CARTESIAN_POINT('Ctrl Pts',(-39.9463699342223,18.0368966503995,
-154.546270125934));
#149963=CARTESIAN_POINT('Ctrl Pts',(-39.5960425666541,18.0813960858844,
-153.697271402021));
#149964=CARTESIAN_POINT('Ctrl Pts',(-39.4532556977585,18.1042418116532,
-153.261037480867));
#149965=CARTESIAN_POINT('Ctrl Pts',(-39.2248664505887,18.1509702537189,
-152.367727156036));
#149966=CARTESIAN_POINT('Ctrl Pts',(-39.1404609620539,18.1746678021094,
-151.914185519153));
#149967=CARTESIAN_POINT('Ctrl Pts',(-39.0282127872062,18.2221486757409,
-151.004139862532));
#149968=CARTESIAN_POINT('Ctrl Pts',(-39.,18.2460151034934,-150.546047809514));
#149969=CARTESIAN_POINT('Ctrl Pts',(-39.,18.26999998,-150.084863924608));
#149970=CARTESIAN_POINT('Ctrl Pts',(-40.4031453149964,17.9943646866131,
-155.356778744658));
#149971=CARTESIAN_POINT('Ctrl Pts',(-39.9612665046713,18.76999998,-155.616375074053));
#149972=CARTESIAN_POINT('Ctrl Pts',(-40.7628307834967,18.76999998,-155.145469613787));
#149973=CARTESIAN_POINT('Ctrl Pts',(-43.4443793123589,18.0073632340302,
-160.550451772752));
#149974=CARTESIAN_POINT('Ctrl Pts',(-42.9502082118644,18.76999998,-160.637466725898));
#149975=CARTESIAN_POINT('Ctrl Pts',(-43.8140202568649,18.76999998,-160.339133090562));
#149976=CARTESIAN_POINT('Ctrl Pts',(-46.3957674250336,18.0186733043079,
-165.796619822254));
#149977=CARTESIAN_POINT('Ctrl Pts',(-45.9568836537051,18.7699999799361,
-165.904661000913));
#149978=CARTESIAN_POINT('Ctrl Pts',(-46.773026135633,18.76999998,-165.585306091383));
#149979=CARTESIAN_POINT('Ctrl Pts',(-49.2955572616308,18.0287857662076,
-171.07256826174));
#149980=CARTESIAN_POINT('Ctrl Pts',(-48.9379852680023,18.76999998,-171.26952948831));
#149981=CARTESIAN_POINT('Ctrl Pts',(-49.6791770659623,18.76999998,-170.861259130871));
#149982=CARTESIAN_POINT('',(-49.2955572616308,18.0287857662077,-171.07256826174));
#149983=CARTESIAN_POINT('Origin',(-49.6791770659623,18.26999998,-170.861259130871));
#149984=CARTESIAN_POINT('Ctrl Pts',(-49.2955572616308,18.0287857662077,
-171.07256826174));
#149985=CARTESIAN_POINT('Ctrl Pts',(-46.3957674250336,18.0186733043079,
-165.796619822254));
#149986=CARTESIAN_POINT('Ctrl Pts',(-43.4443793123589,18.0073632340302,
-160.550451772752));
#149987=CARTESIAN_POINT('Ctrl Pts',(-40.4031453149964,17.9943646866131,
-155.356778744658));
#149988=CARTESIAN_POINT('Ctrl Pts',(-50.2136602208993,18.76999998,-171.14995));
#149989=CARTESIAN_POINT('Ctrl Pts',(-50.2136602208993,18.76999998,-171.64995));
#149990=CARTESIAN_POINT('Ctrl Pts',(-50.2136602208993,18.26999998,-171.64995));
#149991=CARTESIAN_POINT('Ctrl Pts',(-50.1601223770514,18.76999998,-171.149949978729));
#149992=CARTESIAN_POINT('Ctrl Pts',(-50.1192510514274,18.769999979997,-171.674554621579));
#149993=CARTESIAN_POINT('Ctrl Pts',(-50.1215225801538,18.2459873673078,
-171.64995));
#149994=CARTESIAN_POINT('Ctrl Pts',(-50.1077189781947,18.76999998,-171.143861566653));
#149995=CARTESIAN_POINT('Ctrl Pts',(-50.0232655392308,18.76999998,-171.688977816336));
#149996=CARTESIAN_POINT('Ctrl Pts',(-50.0313889586563,18.2224389306129,
-171.637773119416));
#149997=CARTESIAN_POINT('Ctrl Pts',(-50.005178217729,18.76999998,-171.11977321611));
#149998=CARTESIAN_POINT('Ctrl Pts',(-49.820539749869,18.76999998,-171.697170816346));
#149999=CARTESIAN_POINT('Ctrl Pts',(-49.8551127360827,18.1762799424075,
-171.589596446108));
#150000=CARTESIAN_POINT('Ctrl Pts',(-49.9542884930289,18.76999998,-171.101323338366));
#150001=CARTESIAN_POINT('Ctrl Pts',(-49.711275177471,18.7699999800001,-171.68935836961));
#150002=CARTESIAN_POINT('Ctrl Pts',(-49.7676788911518,18.1533289077801,
-171.552696670458));
#150003=CARTESIAN_POINT('Ctrl Pts',(-49.8603247967136,18.76999998,-171.052859322317));
#150004=CARTESIAN_POINT('Ctrl Pts',(-49.4884000599828,18.7699999799999,
-171.64306834795));
#150005=CARTESIAN_POINT('Ctrl Pts',(-49.6063178327574,18.1108845812496,
-171.455768650908));
#150006=CARTESIAN_POINT('Ctrl Pts',(-49.8169023670873,18.76999998,-171.023027979234));
#150007=CARTESIAN_POINT('Ctrl Pts',(-49.3740663050079,18.76999998,-171.603425591907));
#150008=CARTESIAN_POINT('Ctrl Pts',(-49.531790370394,18.0912355578117,-171.396105918926));
#150009=CARTESIAN_POINT('Ctrl Pts',(-49.7384998091177,18.76999998,-170.950084676266));
#150010=CARTESIAN_POINT('Ctrl Pts',(-49.1426233976849,18.76999998,-171.475106253347));
#150011=CARTESIAN_POINT('Ctrl Pts',(-49.3972764264867,18.0557138798866,
-171.250219392074));
#150012=CARTESIAN_POINT('Ctrl Pts',(-49.7050206304183,18.76999998,-170.908176521547));
#150013=CARTESIAN_POINT('Ctrl Pts',(-49.0312290116693,18.7699999799994,
-171.386219492649));
#150014=CARTESIAN_POINT('Ctrl Pts',(-49.3398639704239,18.040521010502,-171.166400641829));
#150015=CARTESIAN_POINT('Ctrl Pts',(-49.6791770659623,18.76999998,-170.861259130871));
#150016=CARTESIAN_POINT('Ctrl Pts',(-48.9379852680023,18.76999998,-171.26952948831));
#150017=CARTESIAN_POINT('Ctrl Pts',(-49.2955572616308,18.0287857662076,
-171.07256826174));
#150018=CARTESIAN_POINT('',(-50.2136602208993,18.26999998,-171.64995));
#150019=CARTESIAN_POINT('Origin',(-50.2136602208993,18.26999998,-171.14995));
#150020=CARTESIAN_POINT('Ctrl Pts',(-50.2136602208993,18.26999998,-171.64995));
#150021=CARTESIAN_POINT('Ctrl Pts',(-50.1215225801538,18.2459873673078,
-171.64995));
#150022=CARTESIAN_POINT('Ctrl Pts',(-50.0313889586563,18.2224389306129,
-171.637773119416));
#150023=CARTESIAN_POINT('Ctrl Pts',(-49.8551127360827,18.1762799424075,
-171.589596446108));
#150024=CARTESIAN_POINT('Ctrl Pts',(-49.7676788911518,18.1533289077801,
-171.552696670458));
#150025=CARTESIAN_POINT('Ctrl Pts',(-49.6063178327574,18.1108845812496,
-171.455768650908));
#150026=CARTESIAN_POINT('Ctrl Pts',(-49.531790370394,18.0912355578117,-171.396105918926));
#150027=CARTESIAN_POINT('Ctrl Pts',(-49.3972764264867,18.0557138798866,
-171.250219392074));
#150028=CARTESIAN_POINT('Ctrl Pts',(-49.3398639704239,18.040521010502,-171.166400641829));
#150029=CARTESIAN_POINT('Ctrl Pts',(-49.2955572616308,18.0287857662077,
-171.07256826174));
#150030=CARTESIAN_POINT('Origin',(-1.30574517062348E-14,18.26999998,-171.14995));
#150031=CARTESIAN_POINT('',(-50.8071048221096,18.26999998,-171.64995));
#150032=CARTESIAN_POINT('Origin',(-50.8071048221096,18.26999998,-171.14995));
#150033=CARTESIAN_POINT('',(-49.8991400004038,18.26999998,-171.64995));
#150034=CARTESIAN_POINT('Ctrl Pts',(-50.8071048221096,18.26999998,-171.64995));
#150035=CARTESIAN_POINT('Ctrl Pts',(-50.8071048221095,18.76999998,-171.64995));
#150036=CARTESIAN_POINT('Ctrl Pts',(-50.8071048221096,18.76999998,-171.14995));
#150037=CARTESIAN_POINT('Ctrl Pts',(-50.9405951656344,18.2608894800009,
-171.64995));
#150038=CARTESIAN_POINT('Ctrl Pts',(-50.9418867684204,18.76999998,-171.659148653595));
#150039=CARTESIAN_POINT('Ctrl Pts',(-51.0054197414846,18.76999998,-171.149950000016));
#150040=CARTESIAN_POINT('Ctrl Pts',(-51.0739848911322,18.2517858470187,
-171.675977326981));
#150041=CARTESIAN_POINT('Ctrl Pts',(-51.0712775866753,18.7699999800004,
-171.69520402023));
#150042=CARTESIAN_POINT('Ctrl Pts',(-51.2035851814656,18.76999998,-171.18899099047));
#150043=CARTESIAN_POINT('Ctrl Pts',(-51.3205984142243,18.2349548730131,
-171.776163607997));
#150044=CARTESIAN_POINT('Ctrl Pts',(-51.3040563824941,18.7699999799997,
-171.809929875206));
#150045=CARTESIAN_POINT('Ctrl Pts',(-51.5699573073986,18.76999998,-171.339270411997));
#150046=CARTESIAN_POINT('Ctrl Pts',(-51.43370116591,18.227235793176,-171.850283164393));
#150047=CARTESIAN_POINT('Ctrl Pts',(-51.406631095234,18.7699999800021,-171.888983273332));
#150048=CARTESIAN_POINT('Ctrl Pts',(-51.7379841660413,18.76999998,-171.450449746589));
#150049=CARTESIAN_POINT('Ctrl Pts',(-51.6224509847807,18.2143539233764,
-172.035403273234));
#150050=CARTESIAN_POINT('Ctrl Pts',(-51.5742878663865,18.769999979998,-172.075215659168));
#150051=CARTESIAN_POINT('Ctrl Pts',(-52.0183932512491,18.76999998,-171.728129909852));
#150052=CARTESIAN_POINT('Ctrl Pts',(-51.6980238274146,18.2091961991206,
-172.14633102856));
#150053=CARTESIAN_POINT('Ctrl Pts',(-51.6385589321982,18.76999998,-172.182182441318));
#150054=CARTESIAN_POINT('Ctrl Pts',(-52.1306652088914,18.76999998,-171.894521542842));
#150055=CARTESIAN_POINT('Ctrl Pts',(-51.8001744932412,18.2022245814263,
-172.38820210671));
#150056=CARTESIAN_POINT('Ctrl Pts',(-51.7249922616163,18.76999998,-172.409726298163));
#150057=CARTESIAN_POINT('Ctrl Pts',(-52.2824215121743,18.76999998,-172.257328160063));
#150058=CARTESIAN_POINT('Ctrl Pts',(-51.8267121465163,18.2004134295229,
-172.51902671195));
#150059=CARTESIAN_POINT('Ctrl Pts',(-51.746661977275,18.769999979999,-172.529650273729));
#150060=CARTESIAN_POINT('Ctrl Pts',(-52.3218461808705,18.76999998,-172.453565067926));
#150061=CARTESIAN_POINT('Ctrl Pts',(-51.8267121465167,18.20041342952,-172.64995));
#150062=CARTESIAN_POINT('Ctrl Pts',(-51.746661977277,18.76999998,-172.64995));
#150063=CARTESIAN_POINT('Ctrl Pts',(-52.3218461808875,18.76999998,-172.64995));
#150064=CARTESIAN_POINT('Origin',(-52.3218461808875,18.26999998,-172.64995));
#150065=CARTESIAN_POINT('Ctrl Pts',(-51.8267121465167,18.20041342952,-172.64995));
#150066=CARTESIAN_POINT('Ctrl Pts',(-51.8267121465163,18.2004134295229,
-172.51902671195));
#150067=CARTESIAN_POINT('Ctrl Pts',(-51.8001744932412,18.2022245814263,
-172.38820210671));
#150068=CARTESIAN_POINT('Ctrl Pts',(-51.6980238274146,18.2091961991206,
-172.14633102856));
#150069=CARTESIAN_POINT('Ctrl Pts',(-51.6224509847807,18.2143539233764,
-172.035403273234));
#150070=CARTESIAN_POINT('Ctrl Pts',(-51.43370116591,18.227235793176,-171.850283164393));
#150071=CARTESIAN_POINT('Ctrl Pts',(-51.3205984142243,18.2349548730131,
-171.776163607997));
#150072=CARTESIAN_POINT('Ctrl Pts',(-51.0739848911322,18.2517858470187,
-171.675977326981));
#150073=CARTESIAN_POINT('Ctrl Pts',(-50.9405951656344,18.2608894800009,
-171.64995));
#150074=CARTESIAN_POINT('Ctrl Pts',(-50.8071048221096,18.26999998,-171.64995));
#150075=CARTESIAN_POINT('Origin',(-52.3218461808875,18.26999998,-171.64995));
#150076=CARTESIAN_POINT('Origin',(-52.3218461808875,18.26999998,-176.84995));
#150077=CARTESIAN_POINT('Origin',(83.2809572255632,19.26999998,-176.84995));
#150078=CARTESIAN_POINT('',(-57.,19.26999998,-177.34995));
#150079=CARTESIAN_POINT('Origin',(-57.,19.26999998,-176.84995));
#150080=CARTESIAN_POINT('',(-52.1813053461851,19.26999998,-177.34995));
#150081=CARTESIAN_POINT('',(-60.,19.26999998,-177.34995));
#150082=CARTESIAN_POINT('Ctrl Pts',(-52.3218461808875,18.76999998,-176.84995));
#150083=CARTESIAN_POINT('Ctrl Pts',(-52.3218461808802,18.76999998,-176.981217345763));
#150084=CARTESIAN_POINT('Ctrl Pts',(-52.3066996556685,18.8238865434699,
-177.110943344657));
#150085=CARTESIAN_POINT('Ctrl Pts',(-52.2546657912052,19.0090066353435,
-177.29606343653));
#150086=CARTESIAN_POINT('Ctrl Pts',(-52.2182021908711,19.1387326342368,
-177.34995));
#150087=CARTESIAN_POINT('Ctrl Pts',(-52.1813053461851,19.26999998,-177.34995));
#150088=CARTESIAN_POINT('Origin',(-57.,19.26999998,-174.34995));
#150089=CARTESIAN_POINT('',(-60.,19.26999998,-174.34995));
#150090=CARTESIAN_POINT('Origin',(-59.5,19.26999998,-174.34995));
#150091=CARTESIAN_POINT('Origin',(-57.,19.26999998,-174.34995));
#150092=CARTESIAN_POINT('Origin',(-59.5,19.26999998,-55.24995));
#150093=CARTESIAN_POINT('',(-60.,19.26999998,-58.24995));
#150094=CARTESIAN_POINT('Origin',(-59.5,19.26999998,-58.24995));
#150095=CARTESIAN_POINT('',(-60.,19.26999998,-174.34995));
#150096=CARTESIAN_POINT('Origin',(-57.,19.26999998,-58.24995));
#150097=CARTESIAN_POINT('Origin',(-57.,19.26999998,-58.24995));
#150098=CARTESIAN_POINT('Origin',(-57.,-2.42462934179819E-14,-58.24995));
#150099=CARTESIAN_POINT('',(-60.,19.76999998,-58.24995));
#150100=CARTESIAN_POINT('Origin',(-57.,19.76999998,-58.24995));
#150101=CARTESIAN_POINT('',(-60.,-54.58000002,-58.24995));
#150102=CARTESIAN_POINT('Origin',(-57.,19.76999998,-58.24995));
#150103=CARTESIAN_POINT('Origin',(-59.5,19.76999998,-58.24995));
#150104=CARTESIAN_POINT('Origin',(-60.,19.76999998,-176.84995));
#150105=CARTESIAN_POINT('',(-52.1110349288339,19.76999998,-177.34995));
#150106=CARTESIAN_POINT('',(-57.,19.76999998,-177.34995));
#150107=CARTESIAN_POINT('',(-60.,19.76999998,-177.34995));
#150108=CARTESIAN_POINT('Origin',(-57.,19.76999998,-176.84995));
#150109=CARTESIAN_POINT('Ctrl Pts',(-52.1110349288339,19.76999998,-177.34995));
#150110=CARTESIAN_POINT('Ctrl Pts',(-52.0741380841476,19.9012673257632,
-177.34995));
#150111=CARTESIAN_POINT('Ctrl Pts',(-52.0376744838139,20.0309933246565,
-177.29606343653));
#150112=CARTESIAN_POINT('Ctrl Pts',(-51.9856406193506,20.2161134165301,
-177.110943344657));
#150113=CARTESIAN_POINT('Ctrl Pts',(-51.9704940941388,20.26999998,-176.981217345763));
#150114=CARTESIAN_POINT('Ctrl Pts',(-51.9704940941315,20.26999998,-176.84995));
#150115=CARTESIAN_POINT('Origin',(-51.9704940941315,20.76999998,-171.64995));
#150116=CARTESIAN_POINT('Origin',(-51.9704940941315,20.76999998,-176.84995));
#150117=CARTESIAN_POINT('Origin',(-51.9704940941315,20.76999998,-172.64995));
#150118=CARTESIAN_POINT('Ctrl Pts',(-51.4753600597607,20.70041342952,-172.64995));
#150119=CARTESIAN_POINT('Ctrl Pts',(-51.5358507252234,20.26999998,-172.64995));
#150120=CARTESIAN_POINT('Ctrl Pts',(-51.9704940941315,20.26999998,-172.64995));
#150121=CARTESIAN_POINT('Ctrl Pts',(-51.4753600597603,20.7004134295229,
-172.51902671195));
#150122=CARTESIAN_POINT('Ctrl Pts',(-51.5358507252071,20.26999998,-172.511015867074));
#150123=CARTESIAN_POINT('Ctrl Pts',(-51.9704940941145,20.26999998,-172.453565067926));
#150124=CARTESIAN_POINT('Ctrl Pts',(-51.4488224064852,20.7022245814263,
-172.38820210671));
#150125=CARTESIAN_POINT('Ctrl Pts',(-51.5060950400989,20.26999998,-172.371853931892));
#150126=CARTESIAN_POINT('Ctrl Pts',(-51.9310694254183,20.26999998,-172.257328160063));
#150127=CARTESIAN_POINT('Ctrl Pts',(-51.3466717406587,20.7091961991206,
-172.14633102856));
#150128=CARTESIAN_POINT('Ctrl Pts',(-51.3932840309667,20.26999998,-172.118296873734));
#150129=CARTESIAN_POINT('Ctrl Pts',(-51.7793131221354,20.26999998,-171.894521542842));
#150130=CARTESIAN_POINT('Ctrl Pts',(-51.2710988980251,20.7143539233764,
-172.035403273235));
#150131=CARTESIAN_POINT('Ctrl Pts',(-51.3097149387001,20.2699999800017,
-172.003556970023));
#150132=CARTESIAN_POINT('Ctrl Pts',(-51.6670411644938,20.26999998,-171.728129909852));
#150133=CARTESIAN_POINT('Ctrl Pts',(-51.0823490791536,20.727235793176,-171.850283164392));
#150134=CARTESIAN_POINT('Ctrl Pts',(-51.105269719327,20.2699999799983,-171.817687494207));
#150135=CARTESIAN_POINT('Ctrl Pts',(-51.3866320792846,20.26999998,-171.450449746589));
#150136=CARTESIAN_POINT('Ctrl Pts',(-50.9692463274684,20.7349548730131,
-171.776163607997));
#150137=CARTESIAN_POINT('Ctrl Pts',(-50.9837060031699,20.26999998,-171.746711574348));
#150138=CARTESIAN_POINT('Ctrl Pts',(-51.2186052206426,20.26999998,-171.339270411997));
#150139=CARTESIAN_POINT('Ctrl Pts',(-50.7226328043762,20.7517858470187,
-171.675977326981));
#150140=CARTESIAN_POINT('Ctrl Pts',(-50.725270742269,20.26999998,-171.658003579003));
#150141=CARTESIAN_POINT('Ctrl Pts',(-50.8522330947096,20.26999998,-171.18899099047));
#150142=CARTESIAN_POINT('Ctrl Pts',(-50.5892430788785,20.760889480001,-171.64995));
#150143=CARTESIAN_POINT('Ctrl Pts',(-50.5880011641168,20.26999998,-171.640924254979));
#150144=CARTESIAN_POINT('Ctrl Pts',(-50.6540676547286,20.26999998,-171.149950000016));
#150145=CARTESIAN_POINT('Ctrl Pts',(-50.4557527353536,20.76999998,-171.64995));
#150146=CARTESIAN_POINT('Ctrl Pts',(-50.4557527353535,20.26999998,-171.64995));
#150147=CARTESIAN_POINT('Ctrl Pts',(-50.4557527353536,20.26999998,-171.14995));
#150148=CARTESIAN_POINT('',(-50.4557527353536,20.76999998,-171.64995));
#150149=CARTESIAN_POINT('Origin',(-50.4557527353536,20.76999998,-171.14995));
#150150=CARTESIAN_POINT('Ctrl Pts',(-50.4557527353536,20.76999998,-171.64995));
#150151=CARTESIAN_POINT('Ctrl Pts',(-50.5892430788785,20.760889480001,-171.64995));
#150152=CARTESIAN_POINT('Ctrl Pts',(-50.7226328043762,20.7517858470187,
-171.675977326981));
#150153=CARTESIAN_POINT('Ctrl Pts',(-50.9692463274684,20.7349548730131,
-171.776163607997));
#150154=CARTESIAN_POINT('Ctrl Pts',(-51.0823490791536,20.727235793176,-171.850283164392));
#150155=CARTESIAN_POINT('Ctrl Pts',(-51.2710988980251,20.7143539233764,
-172.035403273235));
#150156=CARTESIAN_POINT('Ctrl Pts',(-51.3466717406587,20.7091961991206,
-172.14633102856));
#150157=CARTESIAN_POINT('Ctrl Pts',(-51.4488224064852,20.7022245814263,
-172.38820210671));
#150158=CARTESIAN_POINT('Ctrl Pts',(-51.4753600597603,20.7004134295229,
-172.51902671195));
#150159=CARTESIAN_POINT('Ctrl Pts',(-51.4753600597607,20.70041342952,-172.64995));
#150160=CARTESIAN_POINT('Origin',(-1.41024658483895E-14,20.76999998,-171.14995));
#150161=CARTESIAN_POINT('',(-48.5692718988023,20.76999998,-171.64995));
#150162=CARTESIAN_POINT('Origin',(-48.5692718988023,20.76999998,-171.14995));
#150163=CARTESIAN_POINT('',(-50.5260231527048,20.76999998,-171.64995));
#150164=CARTESIAN_POINT('Ctrl Pts',(-48.0164881467928,20.26999998,-170.861259130871));
#150165=CARTESIAN_POINT('Ctrl Pts',(-47.7727200234913,20.26999998,-171.000183411942));
#150166=CARTESIAN_POINT('Ctrl Pts',(-47.6457075325507,20.5094809071607,
-171.07256826174));
#150167=CARTESIAN_POINT('Ctrl Pts',(-48.0706057955098,20.26999998,-170.956218123485));
#150168=CARTESIAN_POINT('Ctrl Pts',(-47.8434294594086,20.2699999800004,
-171.164785257117));
#150169=CARTESIAN_POINT('Ctrl Pts',(-47.7359101824116,20.5351319377708,
-171.262470025419));
#150170=CARTESIAN_POINT('Ctrl Pts',(-48.1562174294056,20.26999998,-171.029346177368));
#150171=CARTESIAN_POINT('Ctrl Pts',(-47.9584699210001,20.26999998,-171.302270428196));
#150172=CARTESIAN_POINT('Ctrl Pts',(-47.8786973574541,20.5756668312168,
-171.408742372302));
#150173=CARTESIAN_POINT('Ctrl Pts',(-48.3512215443805,20.26999998,-171.126070092674));
#150174=CARTESIAN_POINT('Ctrl Pts',(-48.2313965321131,20.26999998,-171.520661616426));
#150175=CARTESIAN_POINT('Ctrl Pts',(-48.2043974294738,20.6676448702122,
-171.602190167782));
#150176=CARTESIAN_POINT('Ctrl Pts',(-48.4599658479004,20.26999998,-171.149949989306));
#150177=CARTESIAN_POINT('Ctrl Pts',(-48.3952116684766,20.26999998,-171.601246355348));
#150178=CARTESIAN_POINT('Ctrl Pts',(-48.3862309601951,20.7187835557883,
-171.64995));
#150179=CARTESIAN_POINT('Ctrl Pts',(-48.5692718988023,20.26999998,-171.14995));
#150180=CARTESIAN_POINT('Ctrl Pts',(-48.5692718988023,20.26999998,-171.64995));
#150181=CARTESIAN_POINT('Ctrl Pts',(-48.5692718988023,20.76999998,-171.64995));
#150182=CARTESIAN_POINT('',(-47.6457075325507,20.5094809071607,-171.07256826174));
#150183=CARTESIAN_POINT('Origin',(-48.0164881467928,20.76999998,-170.861259130871));
#150184=CARTESIAN_POINT('Ctrl Pts',(-47.6457075325507,20.5094809071607,
-171.07256826174));
#150185=CARTESIAN_POINT('Ctrl Pts',(-47.7359101824116,20.5351319377708,
-171.262470025419));
#150186=CARTESIAN_POINT('Ctrl Pts',(-47.8786973574541,20.5756668312168,
-171.408742372302));
#150187=CARTESIAN_POINT('Ctrl Pts',(-48.2043974294738,20.6676448702122,
-171.602190167782));
#150188=CARTESIAN_POINT('Ctrl Pts',(-48.3862309601951,20.7187835557883,
-171.64995));
#150189=CARTESIAN_POINT('Ctrl Pts',(-48.5692718988023,20.76999998,-171.64995));
#150190=CARTESIAN_POINT('Ctrl Pts',(-47.6457075325507,20.5094809071607,
-171.07256826174));
#150191=CARTESIAN_POINT('Ctrl Pts',(-47.7727200234913,20.26999998,-171.000183411942));
#150192=CARTESIAN_POINT('Ctrl Pts',(-48.0164881467928,20.26999998,-170.861259130871));
#150193=CARTESIAN_POINT('Ctrl Pts',(-45.3135333962397,20.5009878795767,
-166.96987023406));
#150194=CARTESIAN_POINT('Ctrl Pts',(-45.4541703457615,20.2699999799837,
-166.918724083766));
#150195=CARTESIAN_POINT('Ctrl Pts',(-45.6783453674058,20.26999998,-166.758558919217));
#150196=CARTESIAN_POINT('Ctrl Pts',(-42.941059217223,20.4917195215043,-162.891251079751));
#150197=CARTESIAN_POINT('Ctrl Pts',(-43.0850828436089,20.26999998,-162.842145218595));
#150198=CARTESIAN_POINT('Ctrl Pts',(-43.2989471172158,20.26999998,-162.679937821406));
#150199=CARTESIAN_POINT('Ctrl Pts',(-40.5058324224685,20.4814581622113,
-158.850394545248));
#150200=CARTESIAN_POINT('Ctrl Pts',(-40.6336903802499,20.26999998,-158.773072684364));
#150201=CARTESIAN_POINT('Ctrl Pts',(-40.8552491802207,20.26999998,-158.639085414378));
#150202=CARTESIAN_POINT('',(-40.5058112296754,20.4818276543828,-158.850123897688));
#150203=CARTESIAN_POINT('Origin',(-40.8552491802207,20.76999998,-158.639085414378));
#150204=CARTESIAN_POINT('Ctrl Pts',(-40.5058324224782,20.4814581622043,
-158.850394545254));
#150205=CARTESIAN_POINT('Ctrl Pts',(-42.941059217223,20.4917195215043,-162.891251079751));
#150206=CARTESIAN_POINT('Ctrl Pts',(-45.3135333962397,20.5009878795767,
-166.96987023406));
#150207=CARTESIAN_POINT('Ctrl Pts',(-47.6457075325507,20.5094809071607,
-171.07256826174));
#150208=CARTESIAN_POINT('Ctrl Pts',(-39.5009242507648,20.26999998,-153.115786956963));
#150209=CARTESIAN_POINT('Ctrl Pts',(-38.9925815845935,20.2699999799997,
-153.109400650742));
#150210=CARTESIAN_POINT('Ctrl Pts',(-39.0010287272926,20.7783180048152,
-153.109486542985));
#150211=CARTESIAN_POINT('Ctrl Pts',(-39.4889697665367,20.26999998,-154.10717684131));
#150212=CARTESIAN_POINT('Ctrl Pts',(-39.0319940367927,20.2699999800017,
-154.089975297154));
#150213=CARTESIAN_POINT('Ctrl Pts',(-38.9877342686064,20.7251370715181,
-154.141750666168));
#150214=CARTESIAN_POINT('Ctrl Pts',(-39.5928133816968,20.26999998,-155.082459683401));
#150215=CARTESIAN_POINT('Ctrl Pts',(-39.1755337328108,20.26999998,-155.105670642999));
#150216=CARTESIAN_POINT('Ctrl Pts',(-39.1031090110774,20.6727392618587,
-155.156196882157));
#150217=CARTESIAN_POINT('Ctrl Pts',(-39.9310881578732,20.26999998,-156.493265246185));
#150218=CARTESIAN_POINT('Ctrl Pts',(-39.5936268082786,20.26999998,-156.580999082022));
#150219=CARTESIAN_POINT('Ctrl Pts',(-39.4789583459802,20.5969029691765,
-156.622397172782));
#150220=CARTESIAN_POINT('Ctrl Pts',(-40.0698006899404,20.26999998,-156.944576655439));
#150221=CARTESIAN_POINT('Ctrl Pts',(-39.7542561576979,20.26999998,-157.042684697946));
#150222=CARTESIAN_POINT('Ctrl Pts',(-39.6330812307821,20.5726365813876,
-157.091232676227));
#150223=CARTESIAN_POINT('Ctrl Pts',(-40.4284839815743,20.26999998,-157.861855948356));
#150224=CARTESIAN_POINT('Ctrl Pts',(-40.1598249794629,20.26999998,-157.975302673127));
#150225=CARTESIAN_POINT('Ctrl Pts',(-40.0316153142837,20.5233115816645,
-158.043776827648));
#150226=CARTESIAN_POINT('Ctrl Pts',(-40.6556223798764,20.26999998,-158.327340856604));
#150227=CARTESIAN_POINT('Ctrl Pts',(-40.4110126646261,20.26999998,-158.450056605571));
#150228=CARTESIAN_POINT('Ctrl Pts',(-40.2840071293548,20.4982773543068,
-158.526971120527));
#150229=CARTESIAN_POINT('Ctrl Pts',(-40.9360042062312,20.26999998,-158.769481550799));
#150230=CARTESIAN_POINT('Ctrl Pts',(-40.7219957046872,20.26999998,-158.905394499841));
#150231=CARTESIAN_POINT('Ctrl Pts',(-40.5955208521275,20.4745034644437,
-158.985715203387));
#150232=CARTESIAN_POINT('',(-39.,20.76999998,-153.26884421004));
#150233=CARTESIAN_POINT('Origin',(-39.5,20.76999998,-153.26884421004));
#150234=CARTESIAN_POINT('Ctrl Pts',(-39.,20.76999998,-153.26884421004));
#150235=CARTESIAN_POINT('Ctrl Pts',(-39.0000000113268,20.7612499005546,
-153.438661222045));
#150236=CARTESIAN_POINT('Ctrl Pts',(-39.0036425975434,20.7525133314444,
-153.607997478032));
#150237=CARTESIAN_POINT('Ctrl Pts',(-39.0108614735808,20.7438083498483,
-153.776830647326));
#150238=CARTESIAN_POINT('Ctrl Pts',(-39.0181154374938,20.7350610570518,
-153.946484442602));
#150239=CARTESIAN_POINT('Ctrl Pts',(-39.0289800693621,20.7263449029416,
-154.115630850492));
#150240=CARTESIAN_POINT('Ctrl Pts',(-39.0434339731224,20.7176579343566,
-154.284262690438));
#150241=CARTESIAN_POINT('Ctrl Pts',(-39.0578177633858,20.7090131048196,
-154.452076525214));
#150242=CARTESIAN_POINT('Ctrl Pts',(-39.0757558973881,20.7003963326059,
-154.619381424156));
#150243=CARTESIAN_POINT('Ctrl Pts',(-39.0972774424432,20.6917977102686,
-154.786176160187));
#150244=CARTESIAN_POINT('Ctrl Pts',(-39.118556656787,20.6832959076654,-154.951092802107));
#150245=CARTESIAN_POINT('Ctrl Pts',(-39.1433391102861,20.6748110028389,
-155.115511340156));
#150246=CARTESIAN_POINT('Ctrl Pts',(-39.1717028274331,20.6663381714659,
-155.279426755488));
#150247=CARTESIAN_POINT('Ctrl Pts',(-39.1993404733963,20.6580822326346,
-155.439146167206));
#150248=CARTESIAN_POINT('Ctrl Pts',(-39.2303787405759,20.6498370259114,
-155.598388419814));
#150249=CARTESIAN_POINT('Ctrl Pts',(-39.2649340810352,20.6416141318001,
-155.757136681022));
#150250=CARTESIAN_POINT('Ctrl Pts',(-39.2935660208686,20.6348007881512,
-155.888672663684));
#150251=CARTESIAN_POINT('Ctrl Pts',(-39.3246135032229,20.6280028352214,
-156.019869432432));
#150252=CARTESIAN_POINT('Ctrl Pts',(-39.3581636245473,20.621240911696,-156.150706929915));
#150253=CARTESIAN_POINT('Ctrl Pts',(-39.3991815569979,20.6129738738596,
-156.31066711551));
#150254=CARTESIAN_POINT('Ctrl Pts',(-39.4439970735942,20.6047446721664,
-156.470288588488));
#150255=CARTESIAN_POINT('Ctrl Pts',(-39.4927105570457,20.5965487965378,
-156.629036157844));
#150256=CARTESIAN_POINT('Ctrl Pts',(-39.5402989256382,20.5885422176049,
-156.784117201293));
#150257=CARTESIAN_POINT('Ctrl Pts',(-39.5916077486878,20.5805677027968,
-156.938364068926));
#150258=CARTESIAN_POINT('Ctrl Pts',(-39.6466989484637,20.572653205052,-157.091258703666));
#150259=CARTESIAN_POINT('Ctrl Pts',(-39.7014925828694,20.5647814560667,
-157.243327505083));
#150260=CARTESIAN_POINT('Ctrl Pts',(-39.760028377299,20.5569693454962,-157.394058454827));
#150261=CARTESIAN_POINT('Ctrl Pts',(-39.8223280030638,20.5492728001288,
-157.542925319488));
#150262=CARTESIAN_POINT('Ctrl Pts',(-39.8698220890173,20.5434053429372,
-157.656413893121));
#150263=CARTESIAN_POINT('Ctrl Pts',(-39.9195353179802,20.5376387400302,
-157.768959999866));
#150264=CARTESIAN_POINT('Ctrl Pts',(-39.9716295140578,20.531917355076,-157.880527437696));
#150265=CARTESIAN_POINT('Ctrl Pts',(-40.0229635294114,20.5262794590109,
-157.990466835897));
#150266=CARTESIAN_POINT('Ctrl Pts',(-40.0766101067617,20.52068517217,-158.099456116636));
#150267=CARTESIAN_POINT('Ctrl Pts',(-40.1327424435931,20.515118298375,-158.207433310574));
#150268=CARTESIAN_POINT('Ctrl Pts',(-40.189569989177,20.5094824778801,-158.316747820836));
#150269=CARTESIAN_POINT('Ctrl Pts',(-40.2489458840389,20.5038743074662,
-158.42502532234));
#150270=CARTESIAN_POINT('Ctrl Pts',(-40.3110598226681,20.4983210960923,
-158.532169335452));
#150271=CARTESIAN_POINT('Ctrl Pts',(-40.3731737612972,20.4927678847185,
-158.639313348565));
#150272=CARTESIAN_POINT('Ctrl Pts',(-40.4380265406518,20.48726933986,-158.745324062406));
#150273=CARTESIAN_POINT('Ctrl Pts',(-40.5058069606272,20.4819020842353,
-158.850069378908));
#150274=CARTESIAN_POINT('Origin',(-39.5,20.76999998,-55.24995));
#150275=CARTESIAN_POINT('',(-39.,20.769999979994,-78.7897987614735));
#150276=CARTESIAN_POINT('Origin',(-39.5,20.76999998,-78.7897987614789));
#150277=CARTESIAN_POINT('',(-39.,20.76999998,-129.34995));
#150278=CARTESIAN_POINT('Ctrl Pts',(-40.9018414229103,20.26999998,-73.3435694268454));
#150279=CARTESIAN_POINT('Ctrl Pts',(-40.684666116315,20.26999998,-73.2084555874168));
#150280=CARTESIAN_POINT('Ctrl Pts',(-40.5575787214805,20.4774056435493,
-73.1293894159588));
#150281=CARTESIAN_POINT('Ctrl Pts',(-40.6368001443165,20.26999998,-73.7699218893582));
#150282=CARTESIAN_POINT('Ctrl Pts',(-40.390530128252,20.26999998,-73.6473693843928));
#150283=CARTESIAN_POINT('Ctrl Pts',(-40.2631070795345,20.5003287096446,
-73.5717684720406));
#150284=CARTESIAN_POINT('Ctrl Pts',(-40.4211667416632,20.26999998,-74.2159715169244));
#150285=CARTESIAN_POINT('Ctrl Pts',(-40.151872039737,20.26999998,-74.1021113025596));
#150286=CARTESIAN_POINT('Ctrl Pts',(-40.0234990701502,20.5243153760975,
-74.0347965829616));
#150287=CARTESIAN_POINT('Ctrl Pts',(-40.0717001001047,20.26999998,-75.1087680536759));
#150288=CARTESIAN_POINT('Ctrl Pts',(-39.7564818699868,20.26999998,-75.0104879262006));
#150289=CARTESIAN_POINT('Ctrl Pts',(-39.6352044867726,20.5723197033564,
-74.9619127222182));
#150290=CARTESIAN_POINT('Ctrl Pts',(-39.9341806290214,20.26999998,-75.5541367565536));
#150291=CARTESIAN_POINT('Ctrl Pts',(-39.5972778875,20.26999998,-75.4662534410499));
#150292=CARTESIAN_POINT('Ctrl Pts',(-39.4824063073862,20.5962647124333,
-75.4245702559575));
#150293=CARTESIAN_POINT('Ctrl Pts',(-39.5978219804271,20.26999998,-76.9519251307675));
#150294=CARTESIAN_POINT('Ctrl Pts',(-39.1821433177468,20.26999998,-76.9267633860652));
#150295=CARTESIAN_POINT('Ctrl Pts',(-39.1086810672092,20.6713961121791,
-76.8772353049354));
#150296=CARTESIAN_POINT('Ctrl Pts',(-39.4934964889571,20.26999998,-77.9105369836536));
#150297=CARTESIAN_POINT('Ctrl Pts',(-39.0385195691145,20.26999998,-77.9239546370935));
#150298=CARTESIAN_POINT('Ctrl Pts',(-38.9927679036048,20.7228955117014,
-77.8743245155055));
#150299=CARTESIAN_POINT('Ctrl Pts',(-39.500313254109,20.26999998,-78.8787081544503));
#150300=CARTESIAN_POINT('Ctrl Pts',(-38.9954730195525,20.26999998,-78.8823876098162));
#150301=CARTESIAN_POINT('Ctrl Pts',(-39.0003486606699,20.7748318783165,
-78.8823661670891));
#150302=CARTESIAN_POINT('',(-40.5058117853578,20.4818179386473,-73.2085119571815));
#150303=CARTESIAN_POINT('Origin',(-40.8552491802306,20.76999998,-73.4195575571114));
#150304=CARTESIAN_POINT('Ctrl Pts',(-40.505806959117,20.4819020767265,-73.2085735870852));
#150305=CARTESIAN_POINT('Ctrl Pts',(-40.4421126804931,20.4869458048838,
-73.3070042835559));
#150306=CARTESIAN_POINT('Ctrl Pts',(-40.3810512373412,20.4921043295325,
-73.4064758506061));
#150307=CARTESIAN_POINT('Ctrl Pts',(-40.3224551183704,20.497309951475,-73.5068769259294));
#150308=CARTESIAN_POINT('Ctrl Pts',(-40.2622487774598,20.502658623961,-73.6100370238146));
#150309=CARTESIAN_POINT('Ctrl Pts',(-40.2046444490715,20.5080570688536,
-73.7141784357249));
#150310=CARTESIAN_POINT('Ctrl Pts',(-40.1494592619306,20.5134764228891,
-73.819212537194));
#150311=CARTESIAN_POINT('Ctrl Pts',(-40.0934408446496,20.518977602671,-73.9258325276237));
#150312=CARTESIAN_POINT('Ctrl Pts',(-40.0399145313078,20.5245005572052,
-74.0333725142232));
#150313=CARTESIAN_POINT('Ctrl Pts',(-39.9886979257668,20.5300581159715,
-74.1417711463612));
#150314=CARTESIAN_POINT('Ctrl Pts',(-39.9364977330605,20.5357224046435,
-74.2522515155093));
#150315=CARTESIAN_POINT('Ctrl Pts',(-39.8866961963328,20.5414229208258,
-74.3636240099572));
#150316=CARTESIAN_POINT('Ctrl Pts',(-39.8391190270575,20.5472137255442,
-74.4758535022212));
#150317=CARTESIAN_POINT('Ctrl Pts',(-39.8339320212271,20.5478450564598,
-74.4880890984027));
#150318=CARTESIAN_POINT('Ctrl Pts',(-39.8287714776101,20.5484774968517,
-74.5003349078318));
#150319=CARTESIAN_POINT('Ctrl Pts',(-39.823637188238,20.5491111427775,-74.5125909043337));
#150320=CARTESIAN_POINT('Ctrl Pts',(-39.7672426362845,20.5560710500776,
-74.6472096181163));
#150321=CARTESIAN_POINT('Ctrl Pts',(-39.714047999184,20.5631207512728,-74.7830391075794));
#150322=CARTESIAN_POINT('Ctrl Pts',(-39.663900248601,20.5702172270692,-74.9200044351338));
#150323=CARTESIAN_POINT('Ctrl Pts',(-39.6129146480068,20.5774322681504,
-75.0592581285652));
#150324=CARTESIAN_POINT('Ctrl Pts',(-39.5650778944283,20.5846961163451,
-75.1996862413939));
#150325=CARTESIAN_POINT('Ctrl Pts',(-39.5202529103467,20.592002925974,-75.341239035909));
#150326=CARTESIAN_POINT('Ctrl Pts',(-39.4745072702815,20.5994598094544,
-75.485699169488));
#150327=CARTESIAN_POINT('Ctrl Pts',(-39.4318977457585,20.6069619918687,
-75.6313310442599));
#150328=CARTESIAN_POINT('Ctrl Pts',(-39.3923135370132,20.6145361975083,
-75.7781064604276));
#150329=CARTESIAN_POINT('Ctrl Pts',(-39.3814836461544,20.6166084334584,
-75.818262921507));
#150330=CARTESIAN_POINT('Ctrl Pts',(-39.3708804344681,20.618686219437,-75.8585050995266));
#150331=CARTESIAN_POINT('Ctrl Pts',(-39.3605021656695,20.6207704310745,
-75.8988326670837));
#150332=CARTESIAN_POINT('Ctrl Pts',(-39.3193535035498,20.6290340945156,
-76.0587269118477));
#150333=CARTESIAN_POINT('Ctrl Pts',(-39.2819485474107,20.6373550060547,
-76.219143860454));
#150334=CARTESIAN_POINT('Ctrl Pts',(-39.2481348789061,20.6456934458296,
-76.3800221605525));
#150335=CARTESIAN_POINT('Ctrl Pts',(-39.2135346702094,20.6542258461628,
-76.5446426529261));
#150336=CARTESIAN_POINT('Ctrl Pts',(-39.1826942310796,20.662777321259,-76.7097467270594));
#150337=CARTESIAN_POINT('Ctrl Pts',(-39.1554910444983,20.6713348080893,
-76.8752903404046));
#150338=CARTESIAN_POINT('Ctrl Pts',(-39.1275435484723,20.6801264372784,
-77.0453634111553));
#150339=CARTESIAN_POINT('Ctrl Pts',(-39.1034346619081,20.6889252566924,
-77.2159010245324));
#150340=CARTESIAN_POINT('Ctrl Pts',(-39.0830814703597,20.6977357804694,
-77.3868692663841));
#150341=CARTESIAN_POINT('Ctrl Pts',(-39.0625908672524,20.706605787193,-77.5589917750047));
#150342=CARTESIAN_POINT('Ctrl Pts',(-39.0459068328891,20.7154885933009,
-77.7315514531776));
#150343=CARTESIAN_POINT('Ctrl Pts',(-39.0329976347586,20.7243937714343,
-77.9045173161638));
#150344=CARTESIAN_POINT('Ctrl Pts',(-39.0200859150497,20.7333006890332,
-78.0775169649027));
#150345=CARTESIAN_POINT('Ctrl Pts',(-39.0109507853562,20.7422308710463,
-78.2509236424966));
#150346=CARTESIAN_POINT('Ctrl Pts',(-39.0056110895819,20.7511851236737,
-78.4246994601558));
#150347=CARTESIAN_POINT('Ctrl Pts',(-39.0018769231076,20.7574470291037,
-78.5462247042482));
#150348=CARTESIAN_POINT('Ctrl Pts',(-39.0000000081285,20.76372052433,-78.6679303367742));
#150349=CARTESIAN_POINT('Ctrl Pts',(-39.,20.769999979994,-78.7897987614735));
#150350=CARTESIAN_POINT('Ctrl Pts',(-40.5058324224785,20.4814581622114,
-73.2082484262411));
#150351=CARTESIAN_POINT('Ctrl Pts',(-40.6336903802598,20.26999998,-73.2855702871256));
#150352=CARTESIAN_POINT('Ctrl Pts',(-40.8552491802306,20.26999998,-73.4195575571114));
#150353=CARTESIAN_POINT('Ctrl Pts',(-42.8933128344149,20.4915183317059,
-69.2466191256953));
#150354=CARTESIAN_POINT('Ctrl Pts',(-43.0367110660153,20.26999998,-69.2967901887638));
#150355=CARTESIAN_POINT('Ctrl Pts',(-43.2510347775237,20.26999998,-69.4579320833189));
#150356=CARTESIAN_POINT('Ctrl Pts',(-45.2204439541918,20.5006239318743,
-65.2486577002759));
#150357=CARTESIAN_POINT('Ctrl Pts',(-45.3606391668745,20.269999980008,-65.3006916020456));
#150358=CARTESIAN_POINT('Ctrl Pts',(-45.5849829096511,20.26999998,-65.4599688790667));
#150359=CARTESIAN_POINT('Ctrl Pts',(-47.508501172308,20.508980519813,-61.2273317382593));
#150360=CARTESIAN_POINT('Ctrl Pts',(-47.6355531845903,20.26999998,-61.2998079338862));
#150361=CARTESIAN_POINT('Ctrl Pts',(-47.878929697957,20.26999998,-61.4386408691297));
#150362=CARTESIAN_POINT('Origin',(-47.878929697957,20.76999998,-61.4386408691297));
#150363=CARTESIAN_POINT('Ctrl Pts',(-47.508501172308,20.508980519813,-61.2273317382593));
#150364=CARTESIAN_POINT('Ctrl Pts',(-45.2204439541918,20.5006239318743,
-65.2486577002759));
#150365=CARTESIAN_POINT('Ctrl Pts',(-42.8933128344149,20.4915183317059,
-69.2466191256953));
#150366=CARTESIAN_POINT('Ctrl Pts',(-40.5058324224785,20.4814581622114,
-73.2082484262411));
#150367=CARTESIAN_POINT('Ctrl Pts',(-48.4322308821779,20.26999998,-61.14995));
#150368=CARTESIAN_POINT('Ctrl Pts',(-48.4322308821778,20.26999998,-60.64995));
#150369=CARTESIAN_POINT('Ctrl Pts',(-48.4322308821779,20.76999998,-60.64995));
#150370=CARTESIAN_POINT('Ctrl Pts',(-48.3241446058921,20.26999998,-61.1499500351048));
#150371=CARTESIAN_POINT('Ctrl Pts',(-48.2600808089264,20.2699999799996,
-60.6982023497825));
#150372=CARTESIAN_POINT('Ctrl Pts',(-48.2513645254321,20.7193046642187,
-60.64995));
#150373=CARTESIAN_POINT('Ctrl Pts',(-48.2139982277207,20.26999998,-61.1739383548812));
#150374=CARTESIAN_POINT('Ctrl Pts',(-48.0943216716052,20.2699999800004,
-60.7795557753816));
#150375=CARTESIAN_POINT('Ctrl Pts',(-48.0673245582317,20.6674580465872,
-60.6979267287055));
#150376=CARTESIAN_POINT('Ctrl Pts',(-48.0199090060446,20.26999998,-61.2698825577664));
#150377=CARTESIAN_POINT('Ctrl Pts',(-47.822827316261,20.2699999799996,-60.9964143345891));
#150378=CARTESIAN_POINT('Ctrl Pts',(-47.7433968711081,20.5758225659973,
-60.8898150965897));
#150379=CARTESIAN_POINT('Ctrl Pts',(-47.9338045255937,20.26999998,-61.3424446783372));
#150380=CARTESIAN_POINT('Ctrl Pts',(-47.7072095971588,20.2699999800002,
-61.1330776360543));
#150381=CARTESIAN_POINT('Ctrl Pts',(-47.5998785057972,20.5350112502637,
-61.0349912654872));
#150382=CARTESIAN_POINT('Ctrl Pts',(-47.878929697957,20.26999998,-61.4386408691297));
#150383=CARTESIAN_POINT('Ctrl Pts',(-47.6355531845903,20.26999998,-61.2998079338861));
#150384=CARTESIAN_POINT('Ctrl Pts',(-47.508501172308,20.508980519813,-61.2273317382593));
#150385=CARTESIAN_POINT('Origin',(-59.5,19.76999998,-55.24995));
#150386=CARTESIAN_POINT('',(-60.,19.76999998,-174.34995));
#150387=CARTESIAN_POINT('Origin',(-59.5,19.76999998,-174.34995));
#150388=CARTESIAN_POINT('',(-60.,19.76999998,-58.24995));
#150389=CARTESIAN_POINT('Origin',(-57.,19.76999998,-174.34995));
#150390=CARTESIAN_POINT('Origin',(-57.,19.76999998,-174.34995));
#150391=CARTESIAN_POINT('Origin',(0.,-12.9675000200281,-60.64995));
#150392=CARTESIAN_POINT('',(-40.4124516162212,-44.1531546065107,-76.3934867515094));
#150393=CARTESIAN_POINT('',(-40.1769968691274,-38.5367831471222,-83.7339979355897));
#150394=CARTESIAN_POINT('Ctrl Pts',(-40.4124516186295,-44.153154649867,
-76.3934867953418));
#150395=CARTESIAN_POINT('Ctrl Pts',(-40.3617744129706,-42.9337786094335,
-78.0770953638969));
#150396=CARTESIAN_POINT('Ctrl Pts',(-40.3094531768732,-41.687877666225,
-79.7436883163613));
#150397=CARTESIAN_POINT('Ctrl Pts',(-40.2557312547753,-40.4102611753384,
-81.3821766826868));
#150398=CARTESIAN_POINT('Ctrl Pts',(-40.2297515899839,-39.7924119460272,
-82.174541826367));
#150399=CARTESIAN_POINT('Ctrl Pts',(-40.2034884202245,-39.1682975463451,
-82.9589328525541));
#150400=CARTESIAN_POINT('Ctrl Pts',(-40.1769969653749,-38.5367854415027,
-83.7339951196695));
#150401=CARTESIAN_POINT('Ctrl Pts',(-49.0214378669496,-44.1865817238571,
-61.2273317382593));
#150402=CARTESIAN_POINT('Ctrl Pts',(-46.2131449010667,-44.1767154324357,
-66.3184583453296));
#150403=CARTESIAN_POINT('Ctrl Pts',(-43.3552388512871,-44.1657199195518,
-71.3808409460202));
#150404=CARTESIAN_POINT('Ctrl Pts',(-40.4124516249929,-44.1531545436406,
-76.3934867142621));
#150405=CARTESIAN_POINT('Ctrl Pts',(-40.1770020116941,-38.5366991465431,
-83.7339249799794));
#150406=CARTESIAN_POINT('Ctrl Pts',(-42.228714191533,-38.5454826541321,
-80.0118606023558));
#150407=CARTESIAN_POINT('Ctrl Pts',(-44.247123664849,-38.5533652514423,
-76.2714892021909));
#150408=CARTESIAN_POINT('Ctrl Pts',(-48.239176789686,-38.5677719010369,
-68.7661813852757));
#150409=CARTESIAN_POINT('Ctrl Pts',(-50.2126317933694,-38.5742944332221,
-65.0011376410615));
#150410=CARTESIAN_POINT('Ctrl Pts',(-52.1700794675439,-38.5802945048887,
-61.2273317382593));
#150411=CARTESIAN_POINT('Ctrl Pts',(-52.5768547844511,-38.28000002,-61.4386408691297));
#150412=CARTESIAN_POINT('Ctrl Pts',(-52.2861787013546,-38.28000002,-61.287642251635));
#150413=CARTESIAN_POINT('Ctrl Pts',(-52.1700794675439,-38.5802945048887,
-61.2273317382593));
#150414=CARTESIAN_POINT('Ctrl Pts',(-52.6146146074011,-38.28000002,-61.3659524750795));
#150415=CARTESIAN_POINT('Ctrl Pts',(-52.3399181230539,-38.28000002,-61.1584857199633));
#150416=CARTESIAN_POINT('Ctrl Pts',(-52.238210979969,-38.595348210897,-61.0819498253042));
#150417=CARTESIAN_POINT('Ctrl Pts',(-52.6705520955624,-38.28000002,-61.3040259447327));
#150418=CARTESIAN_POINT('Ctrl Pts',(-52.4211494089633,-38.28000002,-61.0428817134857));
#150419=CARTESIAN_POINT('Ctrl Pts',(-52.3391546482515,-38.6176244716287,
-60.958102271836));
#150420=CARTESIAN_POINT('Ctrl Pts',(-52.7375342894722,-38.28000002,-61.2567639997891));
#150421=CARTESIAN_POINT('Ctrl Pts',(-52.5193575501107,-38.28000002,-60.9475523661893));
#150422=CARTESIAN_POINT('Ctrl Pts',(-52.4601060488528,-38.6442121687577,
-60.8635779995782));
#150423=CARTESIAN_POINT('Origin',(-52.5768547844511,-38.78000002,-61.4386408691297));
#150424=CARTESIAN_POINT('Ctrl Pts',(-49.940073970993,-44.93000002,-61.14995));
#150425=CARTESIAN_POINT('Ctrl Pts',(-49.940073970993,-44.9300000199999,
-60.64995));
#150426=CARTESIAN_POINT('Ctrl Pts',(-49.940073970993,-44.43000002,-60.64995));
#150427=CARTESIAN_POINT('Ctrl Pts',(-49.8863992897437,-44.93000002,-61.1499500208808));
#150428=CARTESIAN_POINT('Ctrl Pts',(-49.8456849729423,-44.93000002,-60.6251406982113));
#150429=CARTESIAN_POINT('Ctrl Pts',(-49.847975325787,-44.405792727464,-60.64995));
#150430=CARTESIAN_POINT('Ctrl Pts',(-49.8338483436824,-44.93000002,-61.1560263819637));
#150431=CARTESIAN_POINT('Ctrl Pts',(-49.7496896969128,-44.93000002,-60.6104390400057));
#150432=CARTESIAN_POINT('Ctrl Pts',(-49.7578576522452,-44.382047471718,
-60.6621027778979));
#150433=CARTESIAN_POINT('Ctrl Pts',(-49.7309938571501,-44.93000002,-61.1800821203567));
#150434=CARTESIAN_POINT('Ctrl Pts',(-49.5467847765664,-44.93000002,-60.601523688823));
#150435=CARTESIAN_POINT('Ctrl Pts',(-49.581571905815,-44.3354917333839,
-60.7102142267434));
#150436=CARTESIAN_POINT('Ctrl Pts',(-49.6799439551145,-44.93000002,-61.1985082982007));
#150437=CARTESIAN_POINT('Ctrl Pts',(-49.4373419157212,-44.9300000199997,
-60.6088839981636));
#150438=CARTESIAN_POINT('Ctrl Pts',(-49.494126795535,-44.312341612126,-60.7470666030416));
#150439=CARTESIAN_POINT('Ctrl Pts',(-49.5856644732959,-44.93000002,-61.2469206297));
#150440=CARTESIAN_POINT('Ctrl Pts',(-49.2138065931458,-44.9300000200003,
-60.6541841685405));
#150441=CARTESIAN_POINT('Ctrl Pts',(-49.3327124735647,-44.2695203114938,
-60.8438912527599));
#150442=CARTESIAN_POINT('Ctrl Pts',(-49.5420691606389,-44.93000002,-61.2767318781126));
#150443=CARTESIAN_POINT('Ctrl Pts',(-49.0989170947817,-44.9300000200002,
-60.6933131425846));
#150444=CARTESIAN_POINT('Ctrl Pts',(-49.2581152115204,-44.2496846870305,
-60.9035137960622));
#150445=CARTESIAN_POINT('Ctrl Pts',(-49.4633104246523,-44.93000002,-61.3496883835064));
#150446=CARTESIAN_POINT('Ctrl Pts',(-48.8657738933764,-44.9300000199998,
-60.8209262952069));
#150447=CARTESIAN_POINT('Ctrl Pts',(-49.1234012768228,-44.2138057335947,
-61.0494267271759));
#150448=CARTESIAN_POINT('Ctrl Pts',(-49.4296447656355,-44.93000002,-61.3916439172571));
#150449=CARTESIAN_POINT('Ctrl Pts',(-48.7532051342216,-44.93000002,-60.9097365191184));
#150450=CARTESIAN_POINT('Ctrl Pts',(-49.0658454246046,-44.1984444719328,
-61.1333401037095));
#150451=CARTESIAN_POINT('Ctrl Pts',(-49.4036629110189,-44.93000002,-61.4386408691297));
#150452=CARTESIAN_POINT('Ctrl Pts',(-48.6588221091937,-44.93000002,-61.026863396898));
#150453=CARTESIAN_POINT('Ctrl Pts',(-49.0214378669497,-44.1865817238571,
-61.2273317382593));
#150454=CARTESIAN_POINT('Origin',(-49.4036629110189,-44.43000002,-61.4386408691297));
#150455=CARTESIAN_POINT('Origin',(-49.940073970993,-44.43000002,-61.14995));
#150456=CARTESIAN_POINT('Ctrl Pts',(-52.418503743379,-38.6078427661477,
-171.27120723903));
#150457=CARTESIAN_POINT('Ctrl Pts',(-52.508648517912,-38.28000002,-171.191647032252));
#150458=CARTESIAN_POINT('Ctrl Pts',(-52.7704579175044,-38.28000002,-170.960578619515));
#150459=CARTESIAN_POINT('Ctrl Pts',(-52.4966135335128,-38.6055762491043,
-171.358452481822));
#150460=CARTESIAN_POINT('Ctrl Pts',(-52.5972087752045,-38.2800000200018,
-171.289280606396));
#150461=CARTESIAN_POINT('Ctrl Pts',(-52.8865885798003,-38.28000002,-171.092159149585));
#150462=CARTESIAN_POINT('Ctrl Pts',(-52.5554277399439,-38.6065951776351,
-171.457851777602));
#150463=CARTESIAN_POINT('Ctrl Pts',(-52.6638881026927,-38.2800000200005,
-171.402873892562));
#150464=CARTESIAN_POINT('Ctrl Pts',(-52.9752899136351,-38.28000002,-171.24095231752));
#150465=CARTESIAN_POINT('Ctrl Pts',(-52.6330841414732,-38.6181228329597,
-171.679920679702));
#150466=CARTESIAN_POINT('Ctrl Pts',(-52.7468873373812,-38.2800000199994,
-171.654013242837));
#150467=CARTESIAN_POINT('Ctrl Pts',(-53.0969739026007,-38.28000002,-171.570371861396));
#150468=CARTESIAN_POINT('Ctrl Pts',(-52.6495272179227,-38.6283824768232,
-171.795722243821));
#150469=CARTESIAN_POINT('Ctrl Pts',(-52.7606056378773,-38.28000002,-171.785522775662));
#150470=CARTESIAN_POINT('Ctrl Pts',(-53.1262583244907,-38.28000002,-171.740763530748));
#150471=CARTESIAN_POINT('Ctrl Pts',(-52.6451348158641,-38.6439112191758,
-171.916267709546));
#150472=CARTESIAN_POINT('Ctrl Pts',(-52.748069378376,-38.28000002,-171.916267709546));
#150473=CARTESIAN_POINT('Ctrl Pts',(-53.1262583325313,-38.28000002,-171.916267709546));
#150474=CARTESIAN_POINT('',(-52.418503743379,-38.607842766148,-171.271207239029));
#150475=CARTESIAN_POINT('Origin',(-52.7704579175045,-38.78000002,-170.960578619515));
#150476=CARTESIAN_POINT('Origin',(-53.1262583325313,-38.78000002,-171.916267709546));
#150477=CARTESIAN_POINT('Ctrl Pts',(-52.6451348158641,-38.6439112191758,
-171.916267709546));
#150478=CARTESIAN_POINT('Ctrl Pts',(-52.6495272179227,-38.6283824768232,
-171.795722243821));
#150479=CARTESIAN_POINT('Ctrl Pts',(-52.6330841414732,-38.6181228329597,
-171.679920679702));
#150480=CARTESIAN_POINT('Ctrl Pts',(-52.5554277399439,-38.6065951776351,
-171.457851777602));
#150481=CARTESIAN_POINT('Ctrl Pts',(-52.4966135335128,-38.6055762491043,
-171.358452481822));
#150482=CARTESIAN_POINT('Ctrl Pts',(-52.418503743379,-38.6078427661481,
-171.27120723903));
#150483=CARTESIAN_POINT('Origin',(-53.1262583325313,-38.78000002,-179.64995));
#150484=CARTESIAN_POINT('Origin',(-53.1262583325313,-38.78000002,-176.84995));
#150485=CARTESIAN_POINT('Origin',(83.2809572255632,-37.78000002,-176.84995));
#150486=CARTESIAN_POINT('',(-53.3846587239314,-37.9343850848642,-177.325518346031));
#150487=CARTESIAN_POINT('Ctrl Pts',(-53.1262583325313,-38.28000002,-176.84995));
#150488=CARTESIAN_POINT('Ctrl Pts',(-53.1262583407606,-38.28000002,-176.958526013972));
#150489=CARTESIAN_POINT('Ctrl Pts',(-53.1455750275301,-38.2433781645652,
-177.065457314865));
#150490=CARTESIAN_POINT('Ctrl Pts',(-53.2302250969522,-38.1165826570878,
-177.234494972704));
#150491=CARTESIAN_POINT('Ctrl Pts',(-53.2963306348783,-38.0282371456548,
-177.295050892481));
#150492=CARTESIAN_POINT('Ctrl Pts',(-53.3846587239314,-37.9343850848642,
-177.325518346031));
#150493=CARTESIAN_POINT('',(-57.,-37.78000002,-177.34995));
#150494=CARTESIAN_POINT('Origin',(-57.,-37.78000002,-176.84995));
#150495=CARTESIAN_POINT('',(-53.5288692553037,-37.78000002,-177.34995));
#150496=CARTESIAN_POINT('',(-60.,-37.78000002,-177.34995));
#150497=CARTESIAN_POINT('Origin',(-53.5072457281298,-37.7806204038353,-176.855120810331));
#150498=CARTESIAN_POINT('Origin',(-57.,-37.78000002,-174.34995));
#150499=CARTESIAN_POINT('',(-60.,-37.78000002,-174.34995));
#150500=CARTESIAN_POINT('Origin',(-59.5,-37.78000002,-174.34995));
#150501=CARTESIAN_POINT('Origin',(-57.,-37.78000002,-174.34995));
#150502=CARTESIAN_POINT('Origin',(-59.5,-37.78000002,-55.2499500000007));
#150503=CARTESIAN_POINT('',(-60.,-37.78000002,-174.34995));
#150504=CARTESIAN_POINT('Ctrl Pts',(-52.1700794675439,-38.5802945048887,
-61.2273317382593));
#150505=CARTESIAN_POINT('Ctrl Pts',(-52.2861787013546,-38.28000002,-61.287642251635));
#150506=CARTESIAN_POINT('Ctrl Pts',(-52.5768547844511,-38.28000002,-61.4386408691297));
#150507=CARTESIAN_POINT('Ctrl Pts',(-50.2126317933694,-38.5742944332221,
-65.0011376410615));
#150508=CARTESIAN_POINT('Ctrl Pts',(-50.3387340734665,-38.2800000200587,
-65.0466233854387));
#150509=CARTESIAN_POINT('Ctrl Pts',(-50.6164606414324,-38.28000002,-65.2124482077584));
#150510=CARTESIAN_POINT('Ctrl Pts',(-48.239176789686,-38.5677719010369,
-68.7661813852757));
#150511=CARTESIAN_POINT('Ctrl Pts',(-48.3685987197966,-38.28000002,-68.8102729799503));
#150512=CARTESIAN_POINT('Ctrl Pts',(-48.6396458371624,-38.28000002,-68.9774905161504));
#150513=CARTESIAN_POINT('Ctrl Pts',(-44.247123664849,-38.5533652514423,
-76.2714892021909));
#150514=CARTESIAN_POINT('Ctrl Pts',(-44.3795316629781,-38.28000002,-76.3187098252974));
#150515=CARTESIAN_POINT('Ctrl Pts',(-44.6396194153305,-38.28000002,-76.4827983330569));
#150516=CARTESIAN_POINT('Ctrl Pts',(-42.228714191533,-38.5454826541321,
-80.0118606023558));
#150517=CARTESIAN_POINT('Ctrl Pts',(-42.3648252555903,-38.2800000199999,
-80.0572213824928));
#150518=CARTESIAN_POINT('Ctrl Pts',(-42.6166022657662,-38.28000002,-80.2231727548289));
#150519=CARTESIAN_POINT('Ctrl Pts',(-40.177002011694,-38.5366991465431,
-83.7339249799794));
#150520=CARTESIAN_POINT('Ctrl Pts',(-40.3021382496555,-38.28000002,-83.8030917170923));
#150521=CARTESIAN_POINT('Ctrl Pts',(-40.5593018105246,-38.28000002,-83.9452341108497));
#150522=CARTESIAN_POINT('Origin',(-40.5593018105246,-38.78000002,-83.9452341108497));
#150523=CARTESIAN_POINT('Ctrl Pts',(-39.501185810989,-38.28000002,-88.4514222001374));
#150524=CARTESIAN_POINT('Ctrl Pts',(-38.9924949303698,-38.2800000199999,
-88.4594633229731));
#150525=CARTESIAN_POINT('Ctrl Pts',(-39.0013194479405,-38.78868436226,-88.4593423056752));
#150526=CARTESIAN_POINT('Ctrl Pts',(-39.4887748891021,-38.28000002,-87.6395099780675));
#150527=CARTESIAN_POINT('Ctrl Pts',(-39.0236444192854,-38.2800000199999,
-87.6419250197084));
#150528=CARTESIAN_POINT('Ctrl Pts',(-38.9875195439244,-38.7437610060684,
-87.6058431711693));
#150529=CARTESIAN_POINT('Ctrl Pts',(-39.573744011109,-38.28000002,-86.8424396494651));
#150530=CARTESIAN_POINT('Ctrl Pts',(-39.1452121684012,-38.2800000199999,
-86.8067306385414));
#150531=CARTESIAN_POINT('Ctrl Pts',(-39.0819230239498,-38.6993578205918,
-86.7691329026017));
#150532=CARTESIAN_POINT('Ctrl Pts',(-39.9423232315955,-38.28000002,-85.2797330990276));
#150533=CARTESIAN_POINT('Ctrl Pts',(-39.6000058575066,-38.28000002,-85.1938582132543));
#150534=CARTESIAN_POINT('Ctrl Pts',(-39.4914430970225,-38.6119029144712,
-85.1306812313982));
#150535=CARTESIAN_POINT('Ctrl Pts',(-40.2295799875885,-38.28000002,-84.5090080181066));
#150536=CARTESIAN_POINT('Ctrl Pts',(-39.9253332832201,-38.28000002,-84.3974254090272));
#150537=CARTESIAN_POINT('Ctrl Pts',(-39.8106304317714,-38.5685582950589,
-84.3236210863548));
#150538=CARTESIAN_POINT('Ctrl Pts',(-40.6353602321306,-38.28000002,-83.8110748193107));
#150539=CARTESIAN_POINT('Ctrl Pts',(-40.3863780761056,-38.2800000199999,
-83.6661897145683));
#150540=CARTESIAN_POINT('Ctrl Pts',(-40.2614750853509,-38.5292032377738,
-83.5935603822576));
#150541=CARTESIAN_POINT('',(-39.,-38.78000002,-88.296486260558));
#150542=CARTESIAN_POINT('Origin',(-39.5,-38.78000002,-88.296486260558));
#150543=CARTESIAN_POINT('Ctrl Pts',(-39.,-38.7800000199999,-88.296486260558));
#150544=CARTESIAN_POINT('Ctrl Pts',(-39.0000000062169,-38.7719099009273,
-88.1429224351612));
#150545=CARTESIAN_POINT('Ctrl Pts',(-39.0036277971858,-38.7638211626808,
-87.9898921853818));
#150546=CARTESIAN_POINT('Ctrl Pts',(-39.0107984053575,-38.7557567490772,
-87.8374192038769));
#150547=CARTESIAN_POINT('Ctrl Pts',(-39.0183112214607,-38.7473074718426,
-87.677669648007));
#150548=CARTESIAN_POINT('Ctrl Pts',(-39.0297122017381,-38.7388842761647,
-87.5185312036824));
#150549=CARTESIAN_POINT('Ctrl Pts',(-39.0449550120729,-38.7304903061357,
-87.3600099107693));
#150550=CARTESIAN_POINT('Ctrl Pts',(-39.0596505316727,-38.7223977202955,
-87.207180300231));
#150551=CARTESIAN_POINT('Ctrl Pts',(-39.077917034903,-38.7143314169322,
-87.0549234998415));
#150552=CARTESIAN_POINT('Ctrl Pts',(-39.0997643567929,-38.7062848243322,
-86.9032368258097));
#150553=CARTESIAN_POINT('Ctrl Pts',(-39.1214542928114,-38.698296198562,
-86.7526428870573));
#150554=CARTESIAN_POINT('Ctrl Pts',(-39.1466736915941,-38.6903261944346,
-86.6026101662608));
#150555=CARTESIAN_POINT('Ctrl Pts',(-39.1754830928313,-38.6823712868514,
-86.4531391760827));
#150556=CARTESIAN_POINT('Ctrl Pts',(-39.2037909907832,-38.6745548553252,
-86.3062701210167));
#150557=CARTESIAN_POINT('Ctrl Pts',(-39.235565317799,-38.6667522576286,
-86.1599427682393));
#150558=CARTESIAN_POINT('Ctrl Pts',(-39.270909903876,-38.6589743777485,
-86.0141707055388));
#150559=CARTESIAN_POINT('Ctrl Pts',(-39.2761061202792,-38.6578309056783,
-85.9927398934287));
#150560=CARTESIAN_POINT('Ctrl Pts',(-39.2813795805843,-38.6566880047769,
-85.9713211164729));
#150561=CARTESIAN_POINT('Ctrl Pts',(-39.2867306934393,-38.6555457510815,
-85.9499144550484));
#150562=CARTESIAN_POINT('Ctrl Pts',(-39.3250047995163,-38.6473757235958,
-85.7968022235706));
#150563=CARTESIAN_POINT('Ctrl Pts',(-39.3672569048895,-38.6393176867488,
-85.6441886491297));
#150564=CARTESIAN_POINT('Ctrl Pts',(-39.4136102954607,-38.6312998630796,
-85.4924257215471));
#150565=CARTESIAN_POINT('Ctrl Pts',(-39.4600767763118,-38.6232624779951,
-85.340292531687));
#150566=CARTESIAN_POINT('Ctrl Pts',(-39.5106653738111,-38.6152650402226,
-85.18901375742));
#150567=CARTESIAN_POINT('Ctrl Pts',(-39.5655061564177,-38.6072793248838,
-85.038976709348));
#150568=CARTESIAN_POINT('Ctrl Pts',(-39.6166005030304,-38.5998391519308,
-84.8991894091933));
#150569=CARTESIAN_POINT('Ctrl Pts',(-39.6713866171152,-38.5924093742851,
-84.7604801244748));
#150570=CARTESIAN_POINT('Ctrl Pts',(-39.7299639667939,-38.5850061155278,
-84.623191394671));
#150571=CARTESIAN_POINT('Ctrl Pts',(-39.787313465737,-38.5777580378559,
-84.4887803995003));
#150572=CARTESIAN_POINT('Ctrl Pts',(-39.8482976383897,-38.5705354069193,
-84.3557310522515));
#150573=CARTESIAN_POINT('Ctrl Pts',(-39.9129938870569,-38.5633907141695,
-84.2243930007107));
#150574=CARTESIAN_POINT('Ctrl Pts',(-39.975932931367,-38.5564400772652,
-84.0966222007675));
#150575=CARTESIAN_POINT('Ctrl Pts',(-40.0423857789552,-38.5495633891073,
-83.9704711495694));
#150576=CARTESIAN_POINT('Ctrl Pts',(-40.1123986724843,-38.5428430665576,
-83.8462874167416));
#150577=CARTESIAN_POINT('Ctrl Pts',(-40.1336047881332,-38.5408075566678,
-83.8086735649592));
#150578=CARTESIAN_POINT('Ctrl Pts',(-40.1551372943644,-38.5387866226394,
-83.7712403709099));
#150579=CARTESIAN_POINT('Ctrl Pts',(-40.1769968691274,-38.5367831471222,
-83.7339979355897));
#150580=CARTESIAN_POINT('Origin',(-39.5,-38.78000002,-55.2499500000007));
#150581=CARTESIAN_POINT('',(-39.,-38.78000002,-143.762156710948));
#150582=CARTESIAN_POINT('Origin',(-39.5,-38.78000002,-143.762156710948));
#150583=CARTESIAN_POINT('',(-39.,-38.78000002,-129.34995));
#150584=CARTESIAN_POINT('Ctrl Pts',(-40.5593018105246,-38.28000002,-148.113408860656));
#150585=CARTESIAN_POINT('Ctrl Pts',(-40.3021382496555,-38.28000002,-148.255551254414));
#150586=CARTESIAN_POINT('Ctrl Pts',(-40.177002011694,-38.5366991465431,
-148.324717991527));
#150587=CARTESIAN_POINT('Ctrl Pts',(-40.1916835970713,-38.28000002,-147.4483151549));
#150588=CARTESIAN_POINT('Ctrl Pts',(-39.8835176458245,-38.2800000199999,
-147.559388080201));
#150589=CARTESIAN_POINT('Ctrl Pts',(-39.7685879100996,-38.5741769664791,
-147.628968394962));
#150590=CARTESIAN_POINT('Ctrl Pts',(-39.9350562729928,-38.28000002,-146.743548549419));
#150591=CARTESIAN_POINT('Ctrl Pts',(-39.5917422326584,-38.28000002,-146.831469990429));
#150592=CARTESIAN_POINT('Ctrl Pts',(-39.4833958584245,-38.6137964624649,
-146.890860603676));
#150593=CARTESIAN_POINT('Ctrl Pts',(-39.6739630147418,-38.28000002,-145.64333076277));
#150594=CARTESIAN_POINT('Ctrl Pts',(-39.2753714947002,-38.28000002,-145.715141322844));
#150595=CARTESIAN_POINT('Ctrl Pts',(-39.1932922388301,-38.6753614306792,
-145.737334852943));
#150596=CARTESIAN_POINT('Ctrl Pts',(-39.6085749933904,-38.28000002,-145.268506383101));
#150597=CARTESIAN_POINT('Ctrl Pts',(-39.1901844457866,-38.28000002,-145.326704913328));
#150598=CARTESIAN_POINT('Ctrl Pts',(-39.1206388813576,-38.6962900137231,
-145.344124086281));
#150599=CARTESIAN_POINT('Ctrl Pts',(-39.5218408888656,-38.28000002,-144.51836712325));
#150600=CARTESIAN_POINT('Ctrl Pts',(-39.0623543759033,-38.28000002,-144.546929015961));
#150601=CARTESIAN_POINT('Ctrl Pts',(-39.0242676544824,-38.7380634612154,
-144.556697955888));
#150602=CARTESIAN_POINT('Ctrl Pts',(-39.5000000006721,-38.28000002,-144.14127791415));
#150603=CARTESIAN_POINT('Ctrl Pts',(-39.0205601185727,-38.28000002,-144.152421745394));
#150604=CARTESIAN_POINT('Ctrl Pts',(-39.,-38.7590078240271,-144.160623302193));
#150605=CARTESIAN_POINT('Ctrl Pts',(-39.5,-38.28000002,-143.762156710948));
#150606=CARTESIAN_POINT('Ctrl Pts',(-38.9999999999999,-38.2800000199999,
-143.762156710948));
#150607=CARTESIAN_POINT('Ctrl Pts',(-39.,-38.78000002,-143.762156710948));
#150608=CARTESIAN_POINT('',(-40.1769830688311,-38.5367008848306,-148.324685721429));
#150609=CARTESIAN_POINT('Origin',(-40.5593018105246,-38.78000002,-148.113408860656));
#150610=CARTESIAN_POINT('Ctrl Pts',(-40.1769830688311,-38.5367008848306,
-148.324685721429));
#150611=CARTESIAN_POINT('Ctrl Pts',(-39.768579091655,-38.5741781915598,
-147.628945571812));
#150612=CARTESIAN_POINT('Ctrl Pts',(-39.4833928683118,-38.6137970970181,
-146.890848714228));
#150613=CARTESIAN_POINT('Ctrl Pts',(-39.2899934453616,-38.6548397746078,
-146.121843436521));
#150614=CARTESIAN_POINT('Ctrl Pts',(-39.1932922388302,-38.6753614306792,
-145.737334852943));
#150615=CARTESIAN_POINT('Ctrl Pts',(-39.1206388813576,-38.6962900137231,
-145.344124086281));
#150616=CARTESIAN_POINT('Ctrl Pts',(-39.07245326792,-38.7171767374692,-144.950411021085));
#150617=CARTESIAN_POINT('Ctrl Pts',(-39.0242676544824,-38.7380634612153,
-144.556697955888));
#150618=CARTESIAN_POINT('Ctrl Pts',(-39.,-38.759007824027,-144.160623302193));
#150619=CARTESIAN_POINT('Ctrl Pts',(-39.,-38.7800000199999,-143.762156710948));
#150620=CARTESIAN_POINT('Ctrl Pts',(-40.1770020116941,-38.5366991465431,
-148.324717991527));
#150621=CARTESIAN_POINT('Ctrl Pts',(-40.3021382496555,-38.28000002,-148.255551254414));
#150622=CARTESIAN_POINT('Ctrl Pts',(-40.5593018105247,-38.28000002,-148.113408860656));
#150623=CARTESIAN_POINT('Ctrl Pts',(-42.2505775009144,-38.5455762523402,
-152.086445166823));
#150624=CARTESIAN_POINT('Ctrl Pts',(-42.3869374257262,-38.280000019955,
-152.041577619703));
#150625=CARTESIAN_POINT('Ctrl Pts',(-42.6385250759047,-38.28000002,-151.875132894361));
#150626=CARTESIAN_POINT('Ctrl Pts',(-44.2901446089557,-38.5535332680681,
-155.866861850893));
#150627=CARTESIAN_POINT('Ctrl Pts',(-44.4227143745257,-38.2800000199852,
-155.82004311619));
#150628=CARTESIAN_POINT('Ctrl Pts',(-44.6827387638399,-38.28000002,-155.655552720034));
#150629=CARTESIAN_POINT('Ctrl Pts',(-48.3237478755738,-38.5680639323333,
-163.452672197745));
#150630=CARTESIAN_POINT('Ctrl Pts',(-48.4532973709855,-38.280000020015,
-163.409015135176));
#150631=CARTESIAN_POINT('Ctrl Pts',(-48.7243729558795,-38.28000002,-163.241363066864));
#150632=CARTESIAN_POINT('Ctrl Pts',(-50.3175866645898,-38.5746359826999,
-167.258178117331));
#150633=CARTESIAN_POINT('Ctrl Pts',(-50.4437502527583,-38.2800000199406,
-167.213058728775));
#150634=CARTESIAN_POINT('Ctrl Pts',(-50.7215899998133,-38.28000002,-167.046867503852));
#150635=CARTESIAN_POINT('Ctrl Pts',(-52.2951895046066,-38.58067735034,-171.07256826174));
#150636=CARTESIAN_POINT('Ctrl Pts',(-52.4111831155989,-38.28000002,-171.012340412829));
#150637=CARTESIAN_POINT('Ctrl Pts',(-52.7021525552272,-38.28000002,-170.861259130871));
#150638=CARTESIAN_POINT('',(-52.2951895046066,-38.58067735034,-171.07256826174));
#150639=CARTESIAN_POINT('Origin',(-52.7021525552272,-38.78000002,-170.861259130871));
#150640=CARTESIAN_POINT('Ctrl Pts',(-52.2951895046066,-38.58067735034,-171.07256826174));
#150641=CARTESIAN_POINT('Ctrl Pts',(-50.3175866666889,-38.5746359777978,
-167.25817811658));
#150642=CARTESIAN_POINT('Ctrl Pts',(-48.3237478777393,-38.5680639275182,
-163.452672197015));
#150643=CARTESIAN_POINT('Ctrl Pts',(-44.2901446111941,-38.5535332634494,
-155.866861850102));
#150644=CARTESIAN_POINT('Ctrl Pts',(-42.2505775032295,-38.5455762478314,
-152.086445166061));
#150645=CARTESIAN_POINT('Ctrl Pts',(-40.1770020116941,-38.5366991465431,
-148.324717991527));
#150646=CARTESIAN_POINT('Ctrl Pts',(-52.7704579175044,-38.28000002,-170.960578619515));
#150647=CARTESIAN_POINT('Ctrl Pts',(-52.5086485179119,-38.28000002,-171.191647032251));
#150648=CARTESIAN_POINT('Ctrl Pts',(-52.4185037433787,-38.6078427661476,
-171.271207239029));
#150649=CARTESIAN_POINT('Ctrl Pts',(-52.7436831755344,-38.28000002,-170.930241803514));
#150650=CARTESIAN_POINT('Ctrl Pts',(-52.4702729319568,-38.2800000200013,
-171.135526834247));
#150651=CARTESIAN_POINT('Ctrl Pts',(-52.370156234462,-38.5972036761564,
-171.210531232685));
#150652=CARTESIAN_POINT('Ctrl Pts',(-52.7208049303309,-38.28000002,-170.897181907961));
#150653=CARTESIAN_POINT('Ctrl Pts',(-52.4376229301059,-38.2800000199995,
-171.075889787111));
#150654=CARTESIAN_POINT('Ctrl Pts',(-52.3288572922619,-38.5881022353565,
-171.144413209532));
#150655=CARTESIAN_POINT('Ctrl Pts',(-52.7021525552272,-38.28000002,-170.861259130871));
#150656=CARTESIAN_POINT('Ctrl Pts',(-52.4111831155989,-38.28000002,-171.012340412829));
#150657=CARTESIAN_POINT('Ctrl Pts',(-52.2951895046066,-38.58067735034,-171.072568261741));
#150658=CARTESIAN_POINT('Origin',(-81.3222999502966,-44.9387978456672,-153.374633169906));
#150659=CARTESIAN_POINT('Ctrl Pts',(-49.2787232447289,-55.08000002,-171.64995));
#150660=CARTESIAN_POINT('Ctrl Pts',(-49.2787232447289,-54.58000002,-171.64995));
#150661=CARTESIAN_POINT('Ctrl Pts',(-49.2787232447289,-54.58000002,-171.14995));
#150662=CARTESIAN_POINT('Ctrl Pts',(-49.4122135882539,-55.0708895200012,
-171.64995));
#150663=CARTESIAN_POINT('Ctrl Pts',(-49.4109716734917,-54.58000002,-171.640924254979));
#150664=CARTESIAN_POINT('Ctrl Pts',(-49.477038164104,-54.58000002,-171.149950000016));
#150665=CARTESIAN_POINT('Ctrl Pts',(-49.5456033137516,-55.061785887019,
-171.675977326981));
#150666=CARTESIAN_POINT('Ctrl Pts',(-49.548241251645,-54.58000002,-171.658003579003));
#150667=CARTESIAN_POINT('Ctrl Pts',(-49.6752036040849,-54.58000002,-171.18899099047));
#150668=CARTESIAN_POINT('Ctrl Pts',(-49.7922168368437,-55.0449549130127,
-171.776163607997));
#150669=CARTESIAN_POINT('Ctrl Pts',(-49.8066765125445,-54.5800000199999,
-171.746711574348));
#150670=CARTESIAN_POINT('Ctrl Pts',(-50.0415757300179,-54.58000002,-171.339270411997));
#150671=CARTESIAN_POINT('Ctrl Pts',(-49.9053195885289,-55.037235833176,
-171.850283164392));
#150672=CARTESIAN_POINT('Ctrl Pts',(-49.9282402287017,-54.5800000199992,
-171.817687494207));
#150673=CARTESIAN_POINT('Ctrl Pts',(-50.2096025886599,-54.58000002,-171.450449746589));
#150674=CARTESIAN_POINT('Ctrl Pts',(-50.0940694074005,-55.0243539633763,
-172.035403273235));
#150675=CARTESIAN_POINT('Ctrl Pts',(-50.1326854480763,-54.5800000200006,
-172.003556970024));
#150676=CARTESIAN_POINT('Ctrl Pts',(-50.4900116738692,-54.58000002,-171.728129909852));
#150677=CARTESIAN_POINT('Ctrl Pts',(-50.1696422500339,-55.0191962391206,
-172.14633102856));
#150678=CARTESIAN_POINT('Ctrl Pts',(-50.2162545403414,-54.58000002,-172.118296873734));
#150679=CARTESIAN_POINT('Ctrl Pts',(-50.6022836315107,-54.58000002,-171.894521542842));
#150680=CARTESIAN_POINT('Ctrl Pts',(-50.2717929158607,-55.0122246214262,
-172.38820210671));
#150681=CARTESIAN_POINT('Ctrl Pts',(-50.3290655494749,-54.58000002,-172.371853931892));
#150682=CARTESIAN_POINT('Ctrl Pts',(-50.7540399347937,-54.58000002,-172.257328160063));
#150683=CARTESIAN_POINT('Ctrl Pts',(-50.2983305691357,-55.0104134695225,
-172.51902671195));
#150684=CARTESIAN_POINT('Ctrl Pts',(-50.3588212345858,-54.5800000199993,
-172.511015867073));
#150685=CARTESIAN_POINT('Ctrl Pts',(-50.7934646034919,-54.58000002,-172.453565067926));
#150686=CARTESIAN_POINT('Ctrl Pts',(-50.2983305691361,-55.0104134695199,
-172.64995));
#150687=CARTESIAN_POINT('Ctrl Pts',(-50.3588212345988,-54.5800000199999,
-172.64995));
#150688=CARTESIAN_POINT('Ctrl Pts',(-50.7934646035069,-54.58000002,-172.64995));
#150689=CARTESIAN_POINT('Origin',(-49.2787232447289,-55.08000002,-171.14995));
#150690=CARTESIAN_POINT('Origin',(-50.7934646035069,-55.08000002,-172.64995));
#150691=CARTESIAN_POINT('Ctrl Pts',(-50.2983305691361,-55.0104134695199,
-172.64995));
#150692=CARTESIAN_POINT('Ctrl Pts',(-50.2983305691357,-55.0104134695225,
-172.51902671195));
#150693=CARTESIAN_POINT('Ctrl Pts',(-50.2717929158607,-55.0122246214262,
-172.38820210671));
#150694=CARTESIAN_POINT('Ctrl Pts',(-50.1696422500339,-55.0191962391206,
-172.14633102856));
#150695=CARTESIAN_POINT('Ctrl Pts',(-50.0940694074005,-55.0243539633763,
-172.035403273235));
#150696=CARTESIAN_POINT('Ctrl Pts',(-49.9053195885289,-55.037235833176,
-171.850283164392));
#150697=CARTESIAN_POINT('Ctrl Pts',(-49.7922168368437,-55.0449549130127,
-171.776163607997));
#150698=CARTESIAN_POINT('Ctrl Pts',(-49.5456033137516,-55.061785887019,
-171.675977326981));
#150699=CARTESIAN_POINT('Ctrl Pts',(-49.4122135882539,-55.0708895200012,
-171.64995));
#150700=CARTESIAN_POINT('Ctrl Pts',(-49.2787232447289,-55.08000002,-171.64995));
#150701=CARTESIAN_POINT('Origin',(-50.7934646035069,-55.08000002,-171.64995));
#150702=CARTESIAN_POINT('Origin',(-50.7934646035069,-55.08000002,-176.84995));
#150703=CARTESIAN_POINT('Origin',(-60.,-54.08000002,-176.84995));
#150704=CARTESIAN_POINT('',(-57.,-54.08000002,-177.34995));
#150705=CARTESIAN_POINT('Origin',(-57.,-54.08000002,-176.84995));
#150706=CARTESIAN_POINT('',(-50.9340054382093,-54.08000002,-177.34995));
#150707=CARTESIAN_POINT('',(-60.,-54.08000002,-177.34995));
#150708=CARTESIAN_POINT('Ctrl Pts',(-50.7934646035069,-54.58000002,-176.84995));
#150709=CARTESIAN_POINT('Ctrl Pts',(-50.7934646035178,-54.58000002,-176.981217345763));
#150710=CARTESIAN_POINT('Ctrl Pts',(-50.8086111287259,-54.5261134565302,
-177.110943344657));
#150711=CARTESIAN_POINT('Ctrl Pts',(-50.8606449931892,-54.3409933646562,
-177.296063436531));
#150712=CARTESIAN_POINT('Ctrl Pts',(-50.8971085935234,-54.2112673657634,
-177.34995));
#150713=CARTESIAN_POINT('Ctrl Pts',(-50.9340054382093,-54.08000002,-177.34995));
#150714=CARTESIAN_POINT('Origin',(-57.,-54.08000002,-174.34995));
#150715=CARTESIAN_POINT('',(-60.,-54.08000002,-174.34995));
#150716=CARTESIAN_POINT('Origin',(-59.5,-54.08000002,-174.34995));
#150717=CARTESIAN_POINT('Origin',(-57.,-54.08000002,-174.34995));
#150718=CARTESIAN_POINT('Origin',(-59.5,-54.08000002,0.));
#150719=CARTESIAN_POINT('',(-60.,-54.08000002,-58.24995));
#150720=CARTESIAN_POINT('Origin',(-59.5,-54.08000002,-58.24995));
#150721=CARTESIAN_POINT('',(-60.,-54.08000002,-174.34995));
#150722=CARTESIAN_POINT('Origin',(-57.,-54.08000002,-58.24995));
#150723=CARTESIAN_POINT('Origin',(-57.,-54.08000002,-58.24995));
#150724=CARTESIAN_POINT('Ctrl Pts',(-43.1572831724516,-54.58000002,-61.14995));
#150725=CARTESIAN_POINT('Ctrl Pts',(-43.1572831724515,-54.58000002,-60.6498018765538));
#150726=CARTESIAN_POINT('Ctrl Pts',(-43.1572831724516,-55.0801481215056,
-60.6499500219341));
#150727=CARTESIAN_POINT('Ctrl Pts',(-43.3817682803708,-54.58000002,-61.1499499438652));
#150728=CARTESIAN_POINT('Ctrl Pts',(-43.3143913613969,-54.58000002,-60.738433940519));
#150729=CARTESIAN_POINT('Ctrl Pts',(-43.3271185292341,-54.9843723315204,
-60.6499212610322));
#150730=CARTESIAN_POINT('Ctrl Pts',(-43.6059648750607,-54.58000002,-61.1139843549936));
#150731=CARTESIAN_POINT('Ctrl Pts',(-43.5407821982001,-54.58000002,-60.7796882578929));
#150732=CARTESIAN_POINT('Ctrl Pts',(-43.5299471737832,-54.894339587696,
-60.6499049353895));
#150733=CARTESIAN_POINT('Ctrl Pts',(-44.0540062919343,-54.58000002,-61.0395265773532));
#150734=CARTESIAN_POINT('Ctrl Pts',(-44.0046317151094,-54.58000002,-60.8040236126606));
#150735=CARTESIAN_POINT('Ctrl Pts',(-43.9881565230544,-54.7646161135089,
-60.6498916468798));
#150736=CARTESIAN_POINT('Ctrl Pts',(-44.2780419706101,-54.58000002,-61.0029930876918));
#150737=CARTESIAN_POINT('Ctrl Pts',(-44.2580491347896,-54.58000002,-60.7962448835177));
#150738=CARTESIAN_POINT('Ctrl Pts',(-44.2440095987556,-54.7260645641702,
-60.6498933522813));
#150739=CARTESIAN_POINT('Ctrl Pts',(-44.7276655629963,-54.58000002,-61.0020306983307));
#150740=CARTESIAN_POINT('Ctrl Pts',(-44.7466180387412,-54.58000002,-60.7961110321463));
#150741=CARTESIAN_POINT('Ctrl Pts',(-44.7601884828711,-54.7249655177494,
-60.6498933671499));
#150742=CARTESIAN_POINT('Ctrl Pts',(-44.9532637149968,-54.58000002,-61.0380773886891));
#150743=CARTESIAN_POINT('Ctrl Pts',(-45.0021140860287,-54.58000002,-60.8040311529121));
#150744=CARTESIAN_POINT('Ctrl Pts',(-45.0183788445834,-54.7626525929485,
-60.6498915741974));
#150745=CARTESIAN_POINT('Ctrl Pts',(-45.4045230317319,-54.58000002,-61.1130978438444));
#150746=CARTESIAN_POINT('Ctrl Pts',(-45.4698465063654,-54.58000002,-60.7804647582876));
#150747=CARTESIAN_POINT('Ctrl Pts',(-45.4809398893316,-54.8922510295813,
-60.6499045972132));
#150748=CARTESIAN_POINT('Ctrl Pts',(-45.6299507757142,-54.58000002,-61.149949944621));
#150749=CARTESIAN_POINT('Ctrl Pts',(-45.6987517183195,-54.58000002,-60.7399919909285));
#150750=CARTESIAN_POINT('Ctrl Pts',(-45.6855420836464,-54.9825427397823,
-60.6499207098429));
#150751=CARTESIAN_POINT('Ctrl Pts',(-45.8586217441897,-54.58000002,-61.14995));
#150752=CARTESIAN_POINT('Ctrl Pts',(-45.8586217441896,-54.58000002,-60.6498018765538));
#150753=CARTESIAN_POINT('Ctrl Pts',(-45.8586217441897,-55.0801481215056,
-60.6499500219341));
#150754=CARTESIAN_POINT('Origin',(-43.1572831724516,-55.08000002,-61.14995));
#150755=CARTESIAN_POINT('Origin',(1.8445455022812E-14,-55.08000002,-61.14995));
#150756=CARTESIAN_POINT('',(-42.5,-55.08000002,-60.64995));
#150757=CARTESIAN_POINT('Origin',(-42.5,-55.08000002,-61.14995));
#150758=CARTESIAN_POINT('',(1.8445455022812E-14,-55.08000002,-60.64995));
#150759=CARTESIAN_POINT('Origin',(-60.,-55.08000002,-171.14995));
#150760=CARTESIAN_POINT('Origin',(-42.5,-55.08000002,-171.14995));
#150761=CARTESIAN_POINT('Origin',(-60.,-55.08000002,-171.14995));
#150762=CARTESIAN_POINT('Origin',(-57.,-2.42462934179819E-14,-58.24995));
#150763=CARTESIAN_POINT('',(-60.,-53.58000002,-58.24995));
#150764=CARTESIAN_POINT('Origin',(-57.,-53.58000002,-58.24995));
#150765=CARTESIAN_POINT('',(-60.,-54.58000002,-58.24995));
#150766=CARTESIAN_POINT('Origin',(-57.,-53.58000002,-58.24995));
#150767=CARTESIAN_POINT('Origin',(-59.5,-53.58000002,-58.24995));
#150768=CARTESIAN_POINT('Origin',(-60.,-53.58000002,-176.84995));
#150769=CARTESIAN_POINT('',(-51.0042758555605,-53.58000002,-177.34995));
#150770=CARTESIAN_POINT('',(-57.,-53.58000002,-177.34995));
#150771=CARTESIAN_POINT('',(-60.,-53.58000002,-177.34995));
#150772=CARTESIAN_POINT('Origin',(-57.,-53.58000002,-176.84995));
#150773=CARTESIAN_POINT('Ctrl Pts',(-51.0042758555605,-53.58000002,-177.34995));
#150774=CARTESIAN_POINT('Ctrl Pts',(-51.0411727002473,-53.4487326742368,
-177.34995));
#150775=CARTESIAN_POINT('Ctrl Pts',(-51.0776363005805,-53.3190066753437,
-177.296063436531));
#150776=CARTESIAN_POINT('Ctrl Pts',(-51.1296701650438,-53.1338865834697,
-177.110943344657));
#150777=CARTESIAN_POINT('Ctrl Pts',(-51.1448166902519,-53.08000002,-176.981217345763));
#150778=CARTESIAN_POINT('Ctrl Pts',(-51.1448166902628,-53.08000002,-176.84995));
#150779=CARTESIAN_POINT('Origin',(-51.1448166902628,-52.58000002,-171.64995));
#150780=CARTESIAN_POINT('',(-50.6448166902628,-52.58000002,-172.64995));
#150781=CARTESIAN_POINT('Origin',(-51.1448166902628,-52.58000002,-172.64995));
#150782=CARTESIAN_POINT('Origin',(-51.1448166902628,-52.58000002,-176.84995));
#150783=CARTESIAN_POINT('Origin',(-51.1448166902628,-52.58000002,-172.64995));
#150784=CARTESIAN_POINT('Ctrl Pts',(-50.6496826558921,-52.51041346952,-172.64995));
#150785=CARTESIAN_POINT('Ctrl Pts',(-50.5696324866524,-53.08000002,-172.64995));
#150786=CARTESIAN_POINT('Ctrl Pts',(-51.1448166902628,-53.08000002,-172.64995));
#150787=CARTESIAN_POINT('Ctrl Pts',(-50.6496826558917,-52.5104134695225,
-172.51902671195));
#150788=CARTESIAN_POINT('Ctrl Pts',(-50.5696324866503,-53.080000020002,
-172.529650273729));
#150789=CARTESIAN_POINT('Ctrl Pts',(-51.1448166902479,-53.08000002,-172.453565067926));
#150790=CARTESIAN_POINT('Ctrl Pts',(-50.6231450026166,-52.5122246214263,
-172.38820210671));
#150791=CARTESIAN_POINT('Ctrl Pts',(-50.5479627709917,-53.08000002,-172.409726298163));
#150792=CARTESIAN_POINT('Ctrl Pts',(-51.1053920215496,-53.08000002,-172.257328160063));
#150793=CARTESIAN_POINT('Ctrl Pts',(-50.5209943367899,-52.5191962391206,
-172.14633102856));
#150794=CARTESIAN_POINT('Ctrl Pts',(-50.4615294415736,-53.08000002,-172.182182441317));
#150795=CARTESIAN_POINT('Ctrl Pts',(-50.9536357182667,-53.08000002,-171.894521542842));
#150796=CARTESIAN_POINT('Ctrl Pts',(-50.4454214941564,-52.5243539633763,
-172.035403273235));
#150797=CARTESIAN_POINT('Ctrl Pts',(-50.3972583757626,-53.0800000199979,
-172.075215659168));
#150798=CARTESIAN_POINT('Ctrl Pts',(-50.8413637606251,-53.08000002,-171.728129909852));
#150799=CARTESIAN_POINT('Ctrl Pts',(-50.256671675285,-52.537235833176,-171.850283164392));
#150800=CARTESIAN_POINT('Ctrl Pts',(-50.2296016046087,-53.080000020002,
-171.888983273332));
#150801=CARTESIAN_POINT('Ctrl Pts',(-50.5609546754159,-53.08000002,-171.450449746589));
#150802=CARTESIAN_POINT('Ctrl Pts',(-50.1435689235997,-52.5449549130127,
-171.776163607997));
#150803=CARTESIAN_POINT('Ctrl Pts',(-50.1270268918696,-53.0800000200001,
-171.809929875206));
#150804=CARTESIAN_POINT('Ctrl Pts',(-50.3929278167739,-53.08000002,-171.339270411997));
#150805=CARTESIAN_POINT('Ctrl Pts',(-49.8969554005076,-52.561785887019,
-171.675977326981));
#150806=CARTESIAN_POINT('Ctrl Pts',(-49.8942480960507,-53.08000002,-171.69520402023));
#150807=CARTESIAN_POINT('Ctrl Pts',(-50.0265556908409,-53.08000002,-171.18899099047));
#150808=CARTESIAN_POINT('Ctrl Pts',(-49.7635656750098,-52.5708895200013,
-171.64995));
#150809=CARTESIAN_POINT('Ctrl Pts',(-49.7648572777959,-53.08000002,-171.659148653595));
#150810=CARTESIAN_POINT('Ctrl Pts',(-49.8283902508599,-53.08000002,-171.149950000016));
#150811=CARTESIAN_POINT('Ctrl Pts',(-49.6300753314849,-52.58000002,-171.64995));
#150812=CARTESIAN_POINT('Ctrl Pts',(-49.6300753314848,-53.0800000199999,
-171.64995));
#150813=CARTESIAN_POINT('Ctrl Pts',(-49.6300753314849,-53.08000002,-171.14995));
#150814=CARTESIAN_POINT('',(-49.6300753314849,-52.58000002,-171.64995));
#150815=CARTESIAN_POINT('Origin',(-49.6300753314849,-52.58000002,-171.14995));
#150816=CARTESIAN_POINT('Ctrl Pts',(-49.6300753314849,-52.58000002,-171.64995));
#150817=CARTESIAN_POINT('Ctrl Pts',(-49.7635656750098,-52.5708895200013,
-171.64995));
#150818=CARTESIAN_POINT('Ctrl Pts',(-49.8969554005076,-52.561785887019,
-171.675977326981));
#150819=CARTESIAN_POINT('Ctrl Pts',(-50.1435689235997,-52.5449549130127,
-171.776163607997));
#150820=CARTESIAN_POINT('Ctrl Pts',(-50.256671675285,-52.537235833176,-171.850283164392));
#150821=CARTESIAN_POINT('Ctrl Pts',(-50.4454214941564,-52.5243539633763,
-172.035403273235));
#150822=CARTESIAN_POINT('Ctrl Pts',(-50.5209943367899,-52.5191962391206,
-172.14633102856));
#150823=CARTESIAN_POINT('Ctrl Pts',(-50.6231450026166,-52.5122246214263,
-172.38820210671));
#150824=CARTESIAN_POINT('Ctrl Pts',(-50.6496826558917,-52.5104134695225,
-172.51902671195));
#150825=CARTESIAN_POINT('Ctrl Pts',(-50.6496826558921,-52.51041346952,-172.64995));
#150826=CARTESIAN_POINT('Origin',(83.2809572255632,-52.5800000199999,-171.14995));
#150827=CARTESIAN_POINT('',(-43.9094855672884,-52.58000002,-171.64995));
#150828=CARTESIAN_POINT('Origin',(-43.9094855672884,-52.58000002,-171.14995));
#150829=CARTESIAN_POINT('',(-49.5598049141337,-52.58000002,-171.64995));
#150830=CARTESIAN_POINT('Ctrl Pts',(-43.2972503047852,-53.08000002,-170.861259130871));
#150831=CARTESIAN_POINT('Ctrl Pts',(-42.4360603595898,-53.08000002,-171.405549026075));
#150832=CARTESIAN_POINT('Ctrl Pts',(-42.9629113790828,-52.2741145284007,
-171.07256826174));
#150833=CARTESIAN_POINT('Ctrl Pts',(-43.3290496999002,-53.08000002,-170.911572751073));
#150834=CARTESIAN_POINT('Ctrl Pts',(-42.5775224401932,-53.080000020001,
-171.535704796364));
#150835=CARTESIAN_POINT('Ctrl Pts',(-43.0118891450524,-52.2900672717484,
-171.173154953435));
#150836=CARTESIAN_POINT('Ctrl Pts',(-43.3692611707715,-53.08000002,-170.954112611118));
#150837=CARTESIAN_POINT('Ctrl Pts',(-42.7308220084871,-53.0800000200015,
-171.613444114474));
#150838=CARTESIAN_POINT('Ctrl Pts',(-43.073894673874,-52.3102438041593,
-171.258275237078));
#150839=CARTESIAN_POINT('Ctrl Pts',(-43.4620142194198,-53.08000002,-171.027622760172));
#150840=CARTESIAN_POINT('Ctrl Pts',(-43.0212179754289,-53.0800000199986,
-171.708873691595));
#150841=CARTESIAN_POINT('Ctrl Pts',(-43.2170017360461,-52.3567135560047,
-171.405295505501));
#150842=CARTESIAN_POINT('Ctrl Pts',(-43.512966485493,-53.08000002,-171.057128671245));
#150843=CARTESIAN_POINT('Ctrl Pts',(-43.154321777956,-53.080000020001,-171.728961938884));
#150844=CARTESIAN_POINT('Ctrl Pts',(-43.2956718648015,-52.3822166623249,
-171.464307358546));
#150845=CARTESIAN_POINT('Ctrl Pts',(-43.6204035532382,-53.08000002,-171.104030585588));
#150846=CARTESIAN_POINT('Ctrl Pts',(-43.3978292274293,-53.080000019999,
-171.740357884216));
#150847=CARTESIAN_POINT('Ctrl Pts',(-43.4617135157955,-52.4359237144093,
-171.55811115512));
#150848=CARTESIAN_POINT('Ctrl Pts',(-43.6774556997061,-53.08000002,-171.121458138538));
#150849=CARTESIAN_POINT('Ctrl Pts',(-43.5113479697337,-53.080000019999,
-171.733309812026));
#150850=CARTESIAN_POINT('Ctrl Pts',(-43.5499633272225,-52.4644105712997,
-171.592966290451));
#150851=CARTESIAN_POINT('Ctrl Pts',(-43.7921030708942,-53.08000002,-171.144263427359));
#150852=CARTESIAN_POINT('Ctrl Pts',(-43.718452515944,-53.080000020001,-171.702758245039));
#150853=CARTESIAN_POINT('Ctrl Pts',(-43.7274774238083,-52.5215797867686,
-171.638576841342));
#150854=CARTESIAN_POINT('Ctrl Pts',(-43.8503459614229,-53.08000002,-171.149949987963));
#150855=CARTESIAN_POINT('Ctrl Pts',(-43.8149201055142,-53.08000002,-171.680268286151));
#150856=CARTESIAN_POINT('Ctrl Pts',(-43.8177416070106,-52.5505863340359,
-171.64995));
#150857=CARTESIAN_POINT('Ctrl Pts',(-43.9094855672884,-53.08000002,-171.14995));
#150858=CARTESIAN_POINT('Ctrl Pts',(-43.9094855672884,-53.0800000199999,
-171.64995));
#150859=CARTESIAN_POINT('Ctrl Pts',(-43.9094855672884,-52.58000002,-171.64995));
#150860=CARTESIAN_POINT('',(-42.9629113790828,-52.2741145284007,-171.07256826174));
#150861=CARTESIAN_POINT('Origin',(-43.2972503047852,-52.58000002,-170.861259130871));
#150862=CARTESIAN_POINT('Ctrl Pts',(-42.9629113790828,-52.2741145284007,
-171.07256826174));
#150863=CARTESIAN_POINT('Ctrl Pts',(-43.0118891450524,-52.2900672717484,
-171.173154953435));
#150864=CARTESIAN_POINT('Ctrl Pts',(-43.073894673874,-52.3102438041593,
-171.258275237078));
#150865=CARTESIAN_POINT('Ctrl Pts',(-43.2170017360461,-52.3567135560047,
-171.405295505501));
#150866=CARTESIAN_POINT('Ctrl Pts',(-43.2956718648015,-52.3822166623249,
-171.464307358546));
#150867=CARTESIAN_POINT('Ctrl Pts',(-43.4617135157955,-52.4359237144093,
-171.55811115512));
#150868=CARTESIAN_POINT('Ctrl Pts',(-43.5499633272225,-52.4644105712997,
-171.592966290451));
#150869=CARTESIAN_POINT('Ctrl Pts',(-43.7274774238083,-52.5215797867686,
-171.638576841342));
#150870=CARTESIAN_POINT('Ctrl Pts',(-43.8177416070106,-52.5505863340359,
-171.64995));
#150871=CARTESIAN_POINT('Ctrl Pts',(-43.9094855672884,-52.58000002,-171.64995));
#150872=CARTESIAN_POINT('Ctrl Pts',(-42.9629113790828,-52.2741145284007,
-171.07256826174));
#150873=CARTESIAN_POINT('Ctrl Pts',(-42.4360603595898,-53.08000002,-171.405549026075));
#150874=CARTESIAN_POINT('Ctrl Pts',(-43.2972503047852,-53.08000002,-170.861259130871));
#150875=CARTESIAN_POINT('Ctrl Pts',(-42.2277314430405,-52.2712772274341,
-169.905239816447));
#150876=CARTESIAN_POINT('Ctrl Pts',(-41.6869083931944,-53.0800000201158,
-170.237641125793));
#150877=CARTESIAN_POINT('Ctrl Pts',(-42.5594745131554,-53.08000002,-169.693930655453));
#150878=CARTESIAN_POINT('Ctrl Pts',(-41.4865768015737,-52.2683704772926,
-168.741816047102));
#150879=CARTESIAN_POINT('Ctrl Pts',(-40.9363322060061,-53.08000002,-169.082082669019));
#150880=CARTESIAN_POINT('Ctrl Pts',(-41.8155944388483,-53.08000002,-168.530506878352));
#150881=CARTESIAN_POINT('Ctrl Pts',(-40.738568473807,-52.2653905871942,
-167.582872774143));
#150882=CARTESIAN_POINT('Ctrl Pts',(-40.1851006582006,-53.0800000199999,
-167.941466238826));
#150883=CARTESIAN_POINT('Ctrl Pts',(-41.0647116264263,-53.08000002,-167.371563643272));
#150884=CARTESIAN_POINT('',(-40.7385684496897,-52.2653907651306,-167.582872680651));
#150885=CARTESIAN_POINT('Origin',(-41.0647116264263,-52.58000002,-167.371563643272));
#150886=CARTESIAN_POINT('Ctrl Pts',(-40.738568473807,-52.2653905871942,
-167.582872774143));
#150887=CARTESIAN_POINT('Ctrl Pts',(-41.4866208523709,-52.2683706527206,
-168.741884298091));
#150888=CARTESIAN_POINT('Ctrl Pts',(-42.2277810204719,-52.2712774187735,
-169.905318536155));
#150889=CARTESIAN_POINT('Ctrl Pts',(-42.9629113790828,-52.2741145284007,
-171.07256826174));
#150890=CARTESIAN_POINT('Ctrl Pts',(-39.5145387173472,-53.08000002,-160.691745630313));
#150891=CARTESIAN_POINT('Ctrl Pts',(-39.046518301009,-53.0800000200001,
-160.669925623174));
#150892=CARTESIAN_POINT('Ctrl Pts',(-39.0160991280449,-52.6123983573548,
-160.668484445457));
#150893=CARTESIAN_POINT('Ctrl Pts',(-39.4806000144733,-53.08000002,-161.437914207565));
#150894=CARTESIAN_POINT('Ctrl Pts',(-38.9718867651858,-53.0800000199999,
-161.469235957258));
#150895=CARTESIAN_POINT('Ctrl Pts',(-38.9784549947027,-52.5734683914883,
-161.44194359172));
#150896=CARTESIAN_POINT('Ctrl Pts',(-39.5061329414855,-53.08000002,-162.175995192901));
#150897=CARTESIAN_POINT('Ctrl Pts',(-38.9628527118104,-53.08000002,-162.240077797041));
#150898=CARTESIAN_POINT('Ctrl Pts',(-39.0068863115613,-52.534969993258,
-162.206646800233));
#150899=CARTESIAN_POINT('Ctrl Pts',(-39.650908257113,-53.08000002,-163.427315362947));
#150900=CARTESIAN_POINT('Ctrl Pts',(-39.0343477235682,-53.0800000199999,
-163.540394308862));
#150901=CARTESIAN_POINT('Ctrl Pts',(-39.1678790396063,-52.4697392824198,
-163.502497688872));
#150902=CARTESIAN_POINT('Ctrl Pts',(-39.7412068397501,-53.08000002,-163.944571422167));
#150903=CARTESIAN_POINT('Ctrl Pts',(-39.0953266270306,-53.08000002,-164.09147487193));
#150904=CARTESIAN_POINT('Ctrl Pts',(-39.2682617425407,-52.4427876651683,
-164.03795625844));
#150905=CARTESIAN_POINT('Ctrl Pts',(-39.9897001844459,-53.08000002,-164.969734884811));
#150906=CARTESIAN_POINT('Ctrl Pts',(-39.2768635558283,-53.0800000199999,
-165.197823788181));
#150907=CARTESIAN_POINT('Ctrl Pts',(-39.5444749164239,-52.3894029704394,
-165.098845393713));
#150908=CARTESIAN_POINT('Ctrl Pts',(-40.1483999357838,-53.08000002,-165.477859388262));
#150909=CARTESIAN_POINT('Ctrl Pts',(-39.4036485964169,-53.08000002,-165.757191206274));
#150910=CARTESIAN_POINT('Ctrl Pts',(-39.7208567629119,-52.362959099468,
-165.624494361306));
#150911=CARTESIAN_POINT('Ctrl Pts',(-40.6198461801496,-53.08000002,-166.648725872017));
#150912=CARTESIAN_POINT('Ctrl Pts',(-39.8000071452162,-53.08000002,-167.111931394921));
#150913=CARTESIAN_POINT('Ctrl Pts',(-40.2447869076871,-52.3020702250487,
-166.835340537707));
#150914=CARTESIAN_POINT('Ctrl Pts',(-40.9685974766509,-53.08000002,-167.299349676832));
#150915=CARTESIAN_POINT('Ctrl Pts',(-40.1181633100728,-53.0800000199999,
-167.894540549612));
#150916=CARTESIAN_POINT('Ctrl Pts',(-40.6323757317604,-52.2682680312788,
-167.507958491073));
#150917=CARTESIAN_POINT('Ctrl Pts',(-41.4396558833968,-53.08000002,-167.895156212719));
#150918=CARTESIAN_POINT('Ctrl Pts',(-40.5374626513414,-53.0800000200001,
-168.618271993387));
#150919=CARTESIAN_POINT('Ctrl Pts',(-41.1557083615592,-52.2373619998033,
-168.123490399267));
#150920=CARTESIAN_POINT('',(-39.0000000106387,-52.5800000199908,-161.329336741014));
#150921=CARTESIAN_POINT('Origin',(-39.5,-52.58000002,-161.329336741016));
#150922=CARTESIAN_POINT('Ctrl Pts',(-39.0000000425548,-52.580000019989,
-161.329336741012));
#150923=CARTESIAN_POINT('Ctrl Pts',(-39.0000143473941,-52.5710036001899,
-161.508212762828));
#150924=CARTESIAN_POINT('Ctrl Pts',(-39.0036315660785,-52.5620200854199,
-161.686619320982));
#150925=CARTESIAN_POINT('Ctrl Pts',(-39.0107951000132,-52.5530670619587,
-161.86454449438));
#150926=CARTESIAN_POINT('Ctrl Pts',(-39.0182046362212,-52.5438065835258,
-162.048579780123));
#150927=CARTESIAN_POINT('Ctrl Pts',(-39.029407468258,-52.5345779583329,
-162.232100602006));
#150928=CARTESIAN_POINT('Ctrl Pts',(-39.044392703487,-52.5253784540501,
-162.415108947356));
#150929=CARTESIAN_POINT('Ctrl Pts',(-39.0593779387159,-52.5161789497673,
-162.598117292706));
#150930=CARTESIAN_POINT('Ctrl Pts',(-39.078145305281,-52.5070075369497,
-162.780613878806));
#150931=CARTESIAN_POINT('Ctrl Pts',(-39.1007423131417,-52.4978535392319,
-162.962605828642));
#150932=CARTESIAN_POINT('Ctrl Pts',(-39.1217650408907,-52.4893372788923,
-163.131918829615));
#150933=CARTESIAN_POINT('Ctrl Pts',(-39.1460968222467,-52.4808601821505,
-163.300781307826));
#150934=CARTESIAN_POINT('Ctrl Pts',(-39.1738223729434,-52.4723997023487,
-163.469192662811));
#150935=CARTESIAN_POINT('Ctrl Pts',(-39.2011086577874,-52.4640732649655,
-163.634935816242));
#150936=CARTESIAN_POINT('Ctrl Pts',(-39.2316823007795,-52.4557621613023,
-163.800242538063));
#150937=CARTESIAN_POINT('Ctrl Pts',(-39.2656696239975,-52.447461845679,
-163.965100428973));
#150938=CARTESIAN_POINT('Ctrl Pts',(-39.2987592557448,-52.4393807624587,
-164.125604004552));
#150939=CARTESIAN_POINT('Ctrl Pts',(-39.3350850983342,-52.4313092877518,
-164.285682551043));
#150940=CARTESIAN_POINT('Ctrl Pts',(-39.3748016229351,-52.423269407278,
-164.445306693126));
#150941=CARTESIAN_POINT('Ctrl Pts',(-39.3850253517464,-52.4211998012773,
-164.486396742086));
#150942=CARTESIAN_POINT('Ctrl Pts',(-39.3954739382909,-52.4191324533597,
-164.527456568598));
#150943=CARTESIAN_POINT('Ctrl Pts',(-39.4061503736799,-52.4170681050358,
-164.568485422985));
#150944=CARTESIAN_POINT('Ctrl Pts',(-39.4495891091557,-52.4086689832778,
-164.735417689015));
#150945=CARTESIAN_POINT('Ctrl Pts',(-39.4968013767408,-52.4003263288354,
-164.901856686214));
#150946=CARTESIAN_POINT('Ctrl Pts',(-39.5479233092373,-52.3920184089943,
-165.067322106566));
#150947=CARTESIAN_POINT('Ctrl Pts',(-39.5979804671909,-52.3838835276343,
-165.229341190702));
#150948=CARTESIAN_POINT('Ctrl Pts',(-39.6517867720346,-52.3757819588673,
-165.390426824107));
#150949=CARTESIAN_POINT('Ctrl Pts',(-39.7094542224162,-52.3677335878383,
-165.550104007737));
#150950=CARTESIAN_POINT('Ctrl Pts',(-39.7655755217695,-52.3599010057347,
-165.705500006053));
#150951=CARTESIAN_POINT('Ctrl Pts',(-39.8253542902578,-52.3521189747995,
-165.85956196005));
#150952=CARTESIAN_POINT('Ctrl Pts',(-39.8888695985127,-52.344443005944,
-166.011829898773));
#150953=CARTESIAN_POINT('Ctrl Pts',(-39.905244671204,-52.3424640413221,
-166.051086554116));
#150954=CARTESIAN_POINT('Ctrl Pts',(-39.9218679486955,-52.340492315133,
-166.090223853525));
#150955=CARTESIAN_POINT('Ctrl Pts',(-39.9387404404432,-52.3385291686761,
-166.129233683518));
#150956=CARTESIAN_POINT('Ctrl Pts',(-39.9865386305692,-52.3329677584828,
-166.23974488119));
#150957=CARTESIAN_POINT('Ctrl Pts',(-40.0363615889745,-52.3275249298668,
-166.349379781195));
#150958=CARTESIAN_POINT('Ctrl Pts',(-40.0883918199408,-52.3221245794599,
-166.458102843919));
#150959=CARTESIAN_POINT('Ctrl Pts',(-40.1391791878068,-52.3168532289849,
-166.564228803376));
#150960=CARTESIAN_POINT('Ctrl Pts',(-40.1920702020519,-52.3116221321699,
-166.669486100781));
#150961=CARTESIAN_POINT('Ctrl Pts',(-40.2472524480337,-52.3063985864397,
-166.773815992306));
#150962=CARTESIAN_POINT('Ctrl Pts',(-40.3015855872307,-52.3012554170705,
-166.87654052658));
#150963=CARTESIAN_POINT('Ctrl Pts',(-40.358140555795,-52.2961193585579,
-166.978366102817));
#150964=CARTESIAN_POINT('Ctrl Pts',(-40.4171056645871,-52.2909997877437,
-167.079209477833));
#150965=CARTESIAN_POINT('Ctrl Pts',(-40.4746249147384,-52.2860057517729,
-167.17758011485));
#150966=CARTESIAN_POINT('Ctrl Pts',(-40.5344381405214,-52.2810273360842,
-167.275016162333));
#150967=CARTESIAN_POINT('Ctrl Pts',(-40.5967205896074,-52.2761141036865,
-167.371413190652));
#150968=CARTESIAN_POINT('Ctrl Pts',(-40.6426385298221,-52.2724918069592,
-167.442482216489));
#150969=CARTESIAN_POINT('Ctrl Pts',(-40.6898986641975,-52.2689057716457,
-167.512985937728));
#150970=CARTESIAN_POINT('Ctrl Pts',(-40.7385684573717,-52.2653908962638,
-167.582872566557));
#150971=CARTESIAN_POINT('Origin',(-39.5,-52.58000002,-55.2499500000008));
#150972=CARTESIAN_POINT('',(-39.0000000110462,-52.5800000200017,-70.7293062304698));
#150973=CARTESIAN_POINT('Origin',(-39.5,-52.58000002,-70.7293062304687));
#150974=CARTESIAN_POINT('',(-39.,-52.58000002,-129.34995));
#150975=CARTESIAN_POINT('Ctrl Pts',(-41.4399683837798,-53.08000002,-64.1630432687404));
#150976=CARTESIAN_POINT('Ctrl Pts',(-40.5377494244216,-53.08000002,-63.4397598124973));
#150977=CARTESIAN_POINT('Ctrl Pts',(-41.1560619801497,-52.2373289603819,
-63.9347016803424));
#150978=CARTESIAN_POINT('Ctrl Pts',(-40.9682919256936,-53.08000002,-64.7596776730624));
#150979=CARTESIAN_POINT('Ctrl Pts',(-40.1178821818991,-53.08000002,-64.1644517527562));
#150980=CARTESIAN_POINT('Ctrl Pts',(-40.6320437640006,-52.2682772301857,
-64.5510855653446));
#150981=CARTESIAN_POINT('Ctrl Pts',(-40.6198991642287,-53.08000002,-65.4100287027235));
#150982=CARTESIAN_POINT('Ctrl Pts',(-39.7999900770068,-53.0800000199999,
-64.9469795070795));
#150983=CARTESIAN_POINT('Ctrl Pts',(-40.2448521881318,-52.3020649540327,
-65.2234219261584));
#150984=CARTESIAN_POINT('Ctrl Pts',(-40.2472081238925,-53.08000002,-66.3353006309098));
#150985=CARTESIAN_POINT('Ctrl Pts',(-39.4791379317096,-53.0800000199999,
-66.0432454126586));
#150986=CARTESIAN_POINT('Ctrl Pts',(-39.830683046914,-52.3501802308807,
-66.1802561999853));
#150987=CARTESIAN_POINT('Ctrl Pts',(-40.158849529204,-53.08000002,-66.5829654036754));
#150988=CARTESIAN_POINT('Ctrl Pts',(-39.4079361487702,-53.0800000199999,
-66.3190163717637));
#150989=CARTESIAN_POINT('Ctrl Pts',(-39.7324818893101,-52.3630645171375,
-66.4364231780381));
#150990=CARTESIAN_POINT('Ctrl Pts',(-39.9995673126391,-53.08000002,-67.0857801567948));
#150991=CARTESIAN_POINT('Ctrl Pts',(-39.283551683371,-53.0800000199999,
-66.871958046892));
#150992=CARTESIAN_POINT('Ctrl Pts',(-39.5554484391419,-52.3892314658149,
-66.9565858557632));
#150993=CARTESIAN_POINT('Ctrl Pts',(-39.9284899861158,-53.08000002,-67.341717845364));
#150994=CARTESIAN_POINT('Ctrl Pts',(-39.2293907876001,-53.08000002,-67.1504035968485));
#150995=CARTESIAN_POINT('Ctrl Pts',(-39.4764466553468,-52.4025551469199,
-67.2213966334271));
#150996=CARTESIAN_POINT('Ctrl Pts',(-39.7415458247801,-53.08000002,-68.1121058873989));
#150997=CARTESIAN_POINT('Ctrl Pts',(-39.0955485045717,-53.08000002,-67.9649896902694));
#150998=CARTESIAN_POINT('Ctrl Pts',(-39.2686417135216,-52.4426736449394,
-68.0186529598151));
#150999=CARTESIAN_POINT('Ctrl Pts',(-39.6510782949347,-53.08000002,-68.6301060216833));
#151000=CARTESIAN_POINT('Ctrl Pts',(-39.0344334320403,-53.08000002,-68.5169196669116));
#151001=CARTESIAN_POINT('Ctrl Pts',(-39.1680706108451,-52.4696640994698,
-68.554881198313));
#151002=CARTESIAN_POINT('Ctrl Pts',(-39.5060965949729,-53.08000002,-69.8826150276831));
#151003=CARTESIAN_POINT('Ctrl Pts',(-38.9628098506121,-53.0800000199999,
-69.8184703936588));
#151004=CARTESIAN_POINT('Ctrl Pts',(-39.0068468087641,-52.5349571571294,
-69.8519627949666));
#151005=CARTESIAN_POINT('Ctrl Pts',(-39.4806156445371,-53.08000002,-70.6208998773124));
#151006=CARTESIAN_POINT('Ctrl Pts',(-38.9718949651596,-53.0800000199999,
-70.5896094886226));
#151007=CARTESIAN_POINT('Ctrl Pts',(-38.9784724981306,-52.5734665632027,
-70.6168773255623));
#151008=CARTESIAN_POINT('Ctrl Pts',(-39.5145320287584,-53.08000002,-71.3667542047957));
#151009=CARTESIAN_POINT('Ctrl Pts',(-39.0464983325853,-53.0800000199999,
-71.3885691567561));
#151010=CARTESIAN_POINT('Ctrl Pts',(-39.0160910311445,-52.6123805775276,
-71.3900101945721));
#151011=CARTESIAN_POINT('',(-40.7385684498172,-52.2653907681885,-64.4757702925262));
#151012=CARTESIAN_POINT('Origin',(-41.0647116264214,-52.58000002,-64.687079328241));
#151013=CARTESIAN_POINT('Ctrl Pts',(-40.7385684580933,-52.265390901695,
-64.4757704085913));
#151014=CARTESIAN_POINT('Ctrl Pts',(-40.6731577382874,-52.2701147931979,
-64.5696959221107));
#151015=CARTESIAN_POINT('Ctrl Pts',(-40.6103086685504,-52.2749654591829,
-64.6647119718094));
#151016=CARTESIAN_POINT('Ctrl Pts',(-40.5498529666727,-52.2798625896157,
-64.7606962119301));
#151017=CARTESIAN_POINT('Ctrl Pts',(-40.4876384745571,-52.2849021884166,
-64.859472846139));
#151018=CARTESIAN_POINT('Ctrl Pts',(-40.4279579901574,-52.2899909785542,
-64.959274801201));
#151019=CARTESIAN_POINT('Ctrl Pts',(-40.3706215165111,-52.2950875642308,
-65.0599992822958));
#151020=CARTESIAN_POINT('Ctrl Pts',(-40.3124161847234,-52.3002613818974,
-65.1622501091852));
#151021=CARTESIAN_POINT('Ctrl Pts',(-40.2566258082699,-52.3054434096775,
-65.26545173734));
#151022=CARTESIAN_POINT('Ctrl Pts',(-40.2030547740074,-52.3106358110184,
-65.369526925024));
#151023=CARTESIAN_POINT('Ctrl Pts',(-40.1482748098001,-52.3159453885452,
-65.4759507627318));
#151024=CARTESIAN_POINT('Ctrl Pts',(-40.0958148612012,-52.3212660160675,
-65.5832881526308));
#151025=CARTESIAN_POINT('Ctrl Pts',(-40.0454787270805,-52.3266443567245,
-65.6914862715604));
#151026=CARTESIAN_POINT('Ctrl Pts',(-40.0089709584569,-52.3305451572074,
-65.7699601543962));
#151027=CARTESIAN_POINT('Ctrl Pts',(-39.9735806395691,-52.3344772730378,
-65.8488874483287));
#151028=CARTESIAN_POINT('Ctrl Pts',(-39.9392396956596,-52.3384715084012,
-65.9282567948704));
#151029=CARTESIAN_POINT('Ctrl Pts',(-39.8822675889028,-52.3450980007926,
-66.0599316520412));
#151030=CARTESIAN_POINT('Ctrl Pts',(-39.8282521243597,-52.35179330575,-66.1928019679309));
#151031=CARTESIAN_POINT('Ctrl Pts',(-39.7770250192551,-52.3585357064663,
-66.326792421969));
#151032=CARTESIAN_POINT('Ctrl Pts',(-39.7302756747203,-52.3646887540264,
-66.4490707722176));
#151033=CARTESIAN_POINT('Ctrl Pts',(-39.6858483481945,-52.3708818419249,
-66.5722825351572));
#151034=CARTESIAN_POINT('Ctrl Pts',(-39.643630310403,-52.3771272309155,
-66.6963898596616));
#151035=CARTESIAN_POINT('Ctrl Pts',(-39.5964607848755,-52.3841051022434,
-66.8350529505487));
#151036=CARTESIAN_POINT('Ctrl Pts',(-39.5519844690044,-52.3911513115055,
-66.9750591381598));
#151037=CARTESIAN_POINT('Ctrl Pts',(-39.5102573480315,-52.3982348943555,
-67.1158335539574));
#151038=CARTESIAN_POINT('Ctrl Pts',(-39.4737134245086,-52.404438579247,
-67.2391214627551));
#151039=CARTESIAN_POINT('Ctrl Pts',(-39.4392772647425,-52.4106706781818,
-67.3629983817228));
#151040=CARTESIAN_POINT('Ctrl Pts',(-39.4069537833937,-52.4169136927106,
-67.4870781002419));
#151041=CARTESIAN_POINT('Ctrl Pts',(-39.3653073114868,-52.4249573661746,
-67.6469458587845));
#151042=CARTESIAN_POINT('Ctrl Pts',(-39.3271258249076,-52.4330430184609,
-67.8072556992434));
#151043=CARTESIAN_POINT('Ctrl Pts',(-39.2922411274965,-52.4411393696389,
-67.9679723407774));
#151044=CARTESIAN_POINT('Ctrl Pts',(-39.2567093388435,-52.4493859035137,
-68.1316701843534));
#151045=CARTESIAN_POINT('Ctrl Pts',(-39.2245972902298,-52.4576442124894,
-68.2957905034026));
#151046=CARTESIAN_POINT('Ctrl Pts',(-39.1957663841659,-52.4659126791799,
-68.4603174774834));
#151047=CARTESIAN_POINT('Ctrl Pts',(-39.1662932678576,-52.4743653264855,
-68.6285093002511));
#151048=CARTESIAN_POINT('Ctrl Pts',(-39.1402487174386,-52.4828293495748,
-68.7971266032564));
#151049=CARTESIAN_POINT('Ctrl Pts',(-39.1175319575409,-52.4913245467436,
-68.9661674216048));
#151050=CARTESIAN_POINT('Ctrl Pts',(-39.1117517651853,-52.4934861170537,
-69.0091792089545));
#151051=CARTESIAN_POINT('Ctrl Pts',(-39.1061872722816,-52.4956497790532,
-69.0522184676471));
#151052=CARTESIAN_POINT('Ctrl Pts',(-39.1008373305186,-52.4978159816229,
-69.0952852526225));
#151053=CARTESIAN_POINT('Ctrl Pts',(-39.0789398766013,-52.5066823063506,
-69.2715587488873));
#151054=CARTESIAN_POINT('Ctrl Pts',(-39.060639025291,-52.5155639508941,
-69.4482775535725));
#151055=CARTESIAN_POINT('Ctrl Pts',(-39.0458873913583,-52.5244699995587,
-69.6254473411904));
#151056=CARTESIAN_POINT('Ctrl Pts',(-39.0306492988374,-52.5336697393413,
-69.8084595843056));
#151057=CARTESIAN_POINT('Ctrl Pts',(-39.019198308061,-52.5428965372875,
-69.9919537511656));
#151058=CARTESIAN_POINT('Ctrl Pts',(-39.0115396379574,-52.5521535968908,
-70.1759317271015));
#151059=CARTESIAN_POINT('Ctrl Pts',(-39.0038809678538,-52.561410656494,
-70.3599097030374));
#151060=CARTESIAN_POINT('Ctrl Pts',(-39.0000151139767,-52.5706989155813,
-70.5443721556157));
#151061=CARTESIAN_POINT('Ctrl Pts',(-39.0000000441847,-52.5800000200048,
-70.729306230472));
#151062=CARTESIAN_POINT('Ctrl Pts',(-40.7385684738022,-52.2653905871942,
-64.4757701973706));
#151063=CARTESIAN_POINT('Ctrl Pts',(-40.1851006581956,-53.08000002,-64.1171767326871));
#151064=CARTESIAN_POINT('Ctrl Pts',(-41.0647116264215,-53.08000002,-64.6870793282409));
#151065=CARTESIAN_POINT('Ctrl Pts',(-41.4350320326697,-52.2681651349568,
-63.3966889540178));
#151066=CARTESIAN_POINT('Ctrl Pts',(-40.8849497704992,-53.0800000200001,
-63.0545757298723));
#151067=CARTESIAN_POINT('Ctrl Pts',(-41.7638515954828,-53.08000002,-63.6079981134234));
#151068=CARTESIAN_POINT('Ctrl Pts',(-42.125553749702,-52.2708762823431,
-62.3137201227713));
#151069=CARTESIAN_POINT('Ctrl Pts',(-41.584202382955,-53.08000002,-61.9790488279059));
#151070=CARTESIAN_POINT('Ctrl Pts',(-42.4569204735311,-53.08000002,-62.5250292766735));
#151071=CARTESIAN_POINT('Ctrl Pts',(-42.8108476403353,-52.2735270043159,
-61.2273317382593));
#151072=CARTESIAN_POINT('Ctrl Pts',(-42.2822348911901,-53.08000002,-60.8926985768511));
#151073=CARTESIAN_POINT('Ctrl Pts',(-43.1446480925044,-53.08000002,-61.4386408691297));
#151074=CARTESIAN_POINT('',(-42.8108476403353,-52.2735270043159,-61.2273317382593));
#151075=CARTESIAN_POINT('Origin',(-43.1446480925044,-52.58000002,-61.4386408691297));
#151076=CARTESIAN_POINT('Ctrl Pts',(-42.8108476403353,-52.2735270043159,
-61.2273317382593));
#151077=CARTESIAN_POINT('Ctrl Pts',(-42.1255968220058,-52.2708764489536,
-62.3136518407425));
#151078=CARTESIAN_POINT('Ctrl Pts',(-41.4350707133446,-52.2681652890367,
-63.3966290232794));
#151079=CARTESIAN_POINT('Ctrl Pts',(-40.7385684738071,-52.2653905871969,
-64.475770197359));
#151080=CARTESIAN_POINT('Ctrl Pts',(-43.7578534463097,-53.08000002,-61.14995));
#151081=CARTESIAN_POINT('Ctrl Pts',(-43.7578534463096,-53.0800000199999,
-60.64995));
#151082=CARTESIAN_POINT('Ctrl Pts',(-43.7578534463097,-52.58000002,-60.64995));
#151083=CARTESIAN_POINT('Ctrl Pts',(-43.6407450400032,-53.08000002,-61.1499500212049));
#151084=CARTESIAN_POINT('Ctrl Pts',(-43.5651337625656,-53.08000002,-60.5880729855648));
#151085=CARTESIAN_POINT('Ctrl Pts',(-43.5763740160895,-52.5217319642193,
-60.64995));
#151086=CARTESIAN_POINT('Ctrl Pts',(-43.5216142225441,-53.08000002,-61.1725879738646));
#151087=CARTESIAN_POINT('Ctrl Pts',(-43.3529851647999,-53.0800000199999,
-60.5541186415154));
#151088=CARTESIAN_POINT('Ctrl Pts',(-43.3921532801741,-52.4622997588847,
-60.6952259861921));
#151089=CARTESIAN_POINT('Ctrl Pts',(-43.3605400154948,-53.08000002,-61.2428714356874));
#151090=CARTESIAN_POINT('Ctrl Pts',(-43.0017618884342,-53.08000002,-60.5701748148313));
#151091=CARTESIAN_POINT('Ctrl Pts',(-43.1434985367023,-52.3817526273734,
-60.8357928521433));
#151092=CARTESIAN_POINT('Ctrl Pts',(-43.3089610591665,-53.08000002,-61.2727843293231));
#151093=CARTESIAN_POINT('Ctrl Pts',(-42.8669014498658,-53.0800000199996,
-60.5905012094869));
#151094=CARTESIAN_POINT('Ctrl Pts',(-43.0639517713831,-52.3559271119108,
-60.8956186757958));
#151095=CARTESIAN_POINT('Ctrl Pts',(-43.2167397054761,-53.08000002,-61.3458748887128));
#151096=CARTESIAN_POINT('Ctrl Pts',(-42.577778492926,-53.0800000200004,
-60.6851892310921));
#151097=CARTESIAN_POINT('Ctrl Pts',(-42.9218280041301,-52.3097083637374,
-61.0417997602761));
#151098=CARTESIAN_POINT('Ctrl Pts',(-43.1765485703954,-53.08000002,-61.3882486178711));
#151099=CARTESIAN_POINT('Ctrl Pts',(-42.4244093202802,-53.0800000199984,
-60.7623557509217));
#151100=CARTESIAN_POINT('Ctrl Pts',(-42.8599235980017,-52.2895352828276,
-61.126589843371));
#151101=CARTESIAN_POINT('Ctrl Pts',(-43.1446480925044,-53.08000002,-61.4386408691297));
#151102=CARTESIAN_POINT('Ctrl Pts',(-42.2822348911901,-53.08000002,-60.8926985768511));
#151103=CARTESIAN_POINT('Ctrl Pts',(-42.8108476403352,-52.2735270043159,
-61.2273317382593));
#151104=CARTESIAN_POINT('Origin',(-43.7578534463097,-52.58000002,-61.14995));
#151105=CARTESIAN_POINT('Ctrl Pts',(-43.7578534463097,-52.58000002,-60.64995));
#151106=CARTESIAN_POINT('Ctrl Pts',(-43.5763740160895,-52.5217319642193,
-60.64995));
#151107=CARTESIAN_POINT('Ctrl Pts',(-43.3921532801741,-52.4622997588847,
-60.6952259861921));
#151108=CARTESIAN_POINT('Ctrl Pts',(-43.1434985367023,-52.3817526273734,
-60.8357928521433));
#151109=CARTESIAN_POINT('Ctrl Pts',(-43.0639517713831,-52.3559271119108,
-60.8956186757958));
#151110=CARTESIAN_POINT('Ctrl Pts',(-42.9218280041301,-52.3097083637374,
-61.0417997602761));
#151111=CARTESIAN_POINT('Ctrl Pts',(-42.8599235980017,-52.2895352828276,
-61.126589843371));
#151112=CARTESIAN_POINT('Ctrl Pts',(-42.8108476403353,-52.2735270043159,
-61.2273317382593));
#151113=CARTESIAN_POINT('Origin',(1.65582490824295E-14,-52.58000002,-61.14995));
#151114=CARTESIAN_POINT('Origin',(-59.5,-53.58000002,-55.2499500000008));
#151115=CARTESIAN_POINT('',(-60.,-53.58000002,-174.34995));
#151116=CARTESIAN_POINT('Origin',(-59.5,-53.58000002,-174.34995));
#151117=CARTESIAN_POINT('',(-60.,-53.58000002,-58.24995));
#151118=CARTESIAN_POINT('Origin',(-57.,-53.58000002,-174.34995));
#151119=CARTESIAN_POINT('Origin',(-57.,-53.58000002,-174.34995));
#151120=CARTESIAN_POINT('Origin',(0.,-12.9675000200281,-61.64995));
#151121=CARTESIAN_POINT('',(-47.3503956976423,-46.6672397853475,-61.2273317382593));
#151122=CARTESIAN_POINT('Origin',(0.,-12.9675000200281,-61.2273317382593));
#151123=CARTESIAN_POINT('Ctrl Pts',(-47.3503956976423,-46.6672397853475,
-61.2273317382593));
#151124=CARTESIAN_POINT('Ctrl Pts',(-47.4408676817955,-46.6931677917013,
-61.0370194599865));
#151125=CARTESIAN_POINT('Ctrl Pts',(-47.5839744124439,-46.7341093359256,
-60.8908220076151));
#151126=CARTESIAN_POINT('Ctrl Pts',(-47.9099463828816,-46.8268793795224,
-60.6975716107228));
#151127=CARTESIAN_POINT('Ctrl Pts',(-48.0917170178641,-46.8783971335546,
-60.64995));
#151128=CARTESIAN_POINT('Ctrl Pts',(-48.2747189347426,-46.93000002,-60.64995));
#151129=CARTESIAN_POINT('Origin',(83.2809572255632,-46.9300000199999,-61.14995));
#151130=CARTESIAN_POINT('Origin',(-48.2747189347426,-46.93000002,-61.14995));
#151131=CARTESIAN_POINT('Ctrl Pts',(-47.7195914591242,-46.43000002,-61.4386408691297));
#151132=CARTESIAN_POINT('Ctrl Pts',(-47.4775784747621,-46.4300000199999,
-61.3001247789676));
#151133=CARTESIAN_POINT('Ctrl Pts',(-47.3503956976423,-46.6672397853475,
-61.2273317382593));
#151134=CARTESIAN_POINT('Ctrl Pts',(-47.7740598678193,-46.43000002,-61.3434749301835));
#151135=CARTESIAN_POINT('Ctrl Pts',(-47.5485238823607,-46.43000002,-61.1353180501949));
#151136=CARTESIAN_POINT('Ctrl Pts',(-47.4408676817955,-46.6931677917013,
-61.0370194599865));
#151137=CARTESIAN_POINT('Ctrl Pts',(-47.8601584717208,-46.43000002,-61.2703860128396));
#151138=CARTESIAN_POINT('Ctrl Pts',(-47.6638566779936,-46.43000002,-60.997955986762));
#151139=CARTESIAN_POINT('Ctrl Pts',(-47.5839744124439,-46.7341093359256,
-60.8908220076151));
#151140=CARTESIAN_POINT('Ctrl Pts',(-48.0559929527306,-46.43000002,-61.1737607963294));
#151141=CARTESIAN_POINT('Ctrl Pts',(-47.9370084437089,-46.4300000199999,
-60.7796218648572));
#151142=CARTESIAN_POINT('Ctrl Pts',(-47.9099463828816,-46.8268793795224,
-60.6975716107228));
#151143=CARTESIAN_POINT('Ctrl Pts',(-48.1650685977726,-46.43000002,-61.1499500105546));
#151144=CARTESIAN_POINT('Ctrl Pts',(-48.1007647709628,-46.43000002,-60.6990016989097));
#151145=CARTESIAN_POINT('Ctrl Pts',(-48.0917170178641,-46.8783971335546,
-60.64995));
#151146=CARTESIAN_POINT('Ctrl Pts',(-48.2747189347426,-46.43000002,-61.14995));
#151147=CARTESIAN_POINT('Ctrl Pts',(-48.2747189347426,-46.43000002,-60.64995));
#151148=CARTESIAN_POINT('Ctrl Pts',(-48.2747189347426,-46.93000002,-60.64995));
#151149=CARTESIAN_POINT('Origin',(-47.7195914591242,-46.93000002,-61.4386408691297));
#151150=CARTESIAN_POINT('Ctrl Pts',(-47.3503956976423,-46.6672397853475,
-61.2273317382593));
#151151=CARTESIAN_POINT('Ctrl Pts',(-47.4775784747622,-46.43000002,-61.3001247789676));
#151152=CARTESIAN_POINT('Ctrl Pts',(-47.7195914591242,-46.43000002,-61.4386408691297));
#151153=CARTESIAN_POINT('Ctrl Pts',(-45.1164556950575,-46.6590534862623,
-65.1406137191269));
#151154=CARTESIAN_POINT('Ctrl Pts',(-45.2561496318399,-46.43000002,-65.1939977276857));
#151155=CARTESIAN_POINT('Ctrl Pts',(-45.4798241095785,-46.43000002,-65.3519247333759));
#151156=CARTESIAN_POINT('Ctrl Pts',(-42.8446532485491,-46.6501540216799,
-69.0311826437503));
#151157=CARTESIAN_POINT('Ctrl Pts',(-42.9872821964954,-46.43000002,-69.082946811334));
#151158=CARTESIAN_POINT('Ctrl Pts',(-43.2012981267977,-46.43000002,-69.2424952559608));
#151159=CARTESIAN_POINT('Ctrl Pts',(-40.5149864073608,-46.6403532458042,
-72.8868173744763));
#151160=CARTESIAN_POINT('Ctrl Pts',(-40.6428186202086,-46.43000002,-72.9643267243714));
#151161=CARTESIAN_POINT('Ctrl Pts',(-40.8634877666247,-46.43000002,-73.0981265053466));
#151162=CARTESIAN_POINT('',(-40.5149645407348,-46.6407620497281,-72.8871156726096));
#151163=CARTESIAN_POINT('Origin',(-40.8634877666247,-46.93000002,-73.0981265053466));
#151164=CARTESIAN_POINT('Ctrl Pts',(-40.5149864073608,-46.6403532458042,
-72.8868173744763));
#151165=CARTESIAN_POINT('Ctrl Pts',(-42.8446532485491,-46.6501540216799,
-69.0311826437503));
#151166=CARTESIAN_POINT('Ctrl Pts',(-45.1164556950575,-46.6590534862623,
-65.1406137191269));
#151167=CARTESIAN_POINT('Ctrl Pts',(-47.3503956976423,-46.6672397853475,
-61.2273317382593));
#151168=CARTESIAN_POINT('Ctrl Pts',(-39.5009150908472,-46.43000002,-78.6483012309456));
#151169=CARTESIAN_POINT('Ctrl Pts',(-38.9925996219358,-46.43000002,-78.6546392690997));
#151170=CARTESIAN_POINT('Ctrl Pts',(-39.0010185398262,-46.9382906476586,
-78.6545545088046));
#151171=CARTESIAN_POINT('Ctrl Pts',(-39.4889961719126,-46.43000002,-77.6521831848818));
#151172=CARTESIAN_POINT('Ctrl Pts',(-39.0322289013405,-46.43000002,-77.6697878581646));
#151173=CARTESIAN_POINT('Ctrl Pts',(-38.9877635814871,-46.8849139645486,
-77.6175842987478));
#151174=CARTESIAN_POINT('Ctrl Pts',(-39.5933371710426,-46.43000002,-76.6722018120623));
#151175=CARTESIAN_POINT('Ctrl Pts',(-39.1763256032396,-46.43000002,-76.6493249295432));
#151176=CARTESIAN_POINT('Ctrl Pts',(-39.1036909811623,-46.8323255651553,
-76.5984538753872));
#151177=CARTESIAN_POINT('Ctrl Pts',(-39.9334371785153,-46.43000002,-75.2543998581027));
#151178=CARTESIAN_POINT('Ctrl Pts',(-39.5965010051026,-46.4300000199999,
-75.16683002555));
#151179=CARTESIAN_POINT('Ctrl Pts',(-39.4815683506526,-46.7562077909153,
-75.125263078053));
#151180=CARTESIAN_POINT('Ctrl Pts',(-40.0729487155202,-46.43000002,-74.8007807728849));
#151181=CARTESIAN_POINT('Ctrl Pts',(-39.7579862728477,-46.43000002,-74.7028397032788));
#151182=CARTESIAN_POINT('Ctrl Pts',(-39.6365790276958,-46.7318484038351,
-74.6541180909925));
#151183=CARTESIAN_POINT('Ctrl Pts',(-40.4336795368199,-46.43000002,-73.8793270924814));
#151184=CARTESIAN_POINT('Ctrl Pts',(-40.1657218306395,-46.4300000199999,
-73.7660901072993));
#151185=CARTESIAN_POINT('Ctrl Pts',(-40.0373881727514,-46.6823634194217,
-73.6974136443781));
#151186=CARTESIAN_POINT('Ctrl Pts',(-40.6620683669064,-46.43000002,-73.411923037355));
#151187=CARTESIAN_POINT('Ctrl Pts',(-40.4182099778731,-46.4300000199999,
-73.2894241672258));
#151188=CARTESIAN_POINT('Ctrl Pts',(-40.2911698500431,-46.6572594632896,
-73.2123128660115));
#151189=CARTESIAN_POINT('Ctrl Pts',(-40.9442174875933,-46.43000002,-72.9681042608037));
#151190=CARTESIAN_POINT('Ctrl Pts',(-40.7310707477149,-46.43000002,-72.8323985218523));
#151191=CARTESIAN_POINT('Ctrl Pts',(-40.6046466716213,-46.6334277480432,
-72.7519083427877));
#151192=CARTESIAN_POINT('',(-39.,-46.93000002,-78.4955841262963));
#151193=CARTESIAN_POINT('Origin',(-39.5,-46.93000002,-78.4955841262963));
#151194=CARTESIAN_POINT('Ctrl Pts',(-39.,-46.93000002,-78.4955841262963));
#151195=CARTESIAN_POINT('Ctrl Pts',(-39.0000000114043,-46.9212366188075,
-78.325357772545));
#151196=CARTESIAN_POINT('Ctrl Pts',(-39.0036424523548,-46.9124870586774,
-78.1556109785247));
#151197=CARTESIAN_POINT('Ctrl Pts',(-39.0108614956953,-46.9037692487272,
-77.9863659895749));
#151198=CARTESIAN_POINT('Ctrl Pts',(-39.0181149087956,-46.8950099334112,
-77.8163152277052));
#151199=CARTESIAN_POINT('Ctrl Pts',(-39.0289785903128,-46.8862819126589,
-77.6467704601483));
#151200=CARTESIAN_POINT('Ctrl Pts',(-39.043431653744,-46.877583067065,-77.477738864482));
#151201=CARTESIAN_POINT('Ctrl Pts',(-39.0578119415107,-46.8689280228611,
-77.309558395414));
#151202=CARTESIAN_POINT('Ctrl Pts',(-39.0757453657993,-46.8603010136457,
-77.1418852932464));
#151203=CARTESIAN_POINT('Ctrl Pts',(-39.0972614984966,-46.851692008831,
-76.9747208445981));
#151204=CARTESIAN_POINT('Ctrl Pts',(-39.1185331932699,-46.8431808081755,
-76.809455497957));
#151205=CARTESIAN_POINT('Ctrl Pts',(-39.1433067271124,-46.8346863590143,
-76.6446866806331));
#151206=CARTESIAN_POINT('Ctrl Pts',(-39.1716605727341,-46.826203771819,
-76.4804194998339));
#151207=CARTESIAN_POINT('Ctrl Pts',(-39.1992826999361,-46.8179400919769,
-76.3203915084399));
#151208=CARTESIAN_POINT('Ctrl Pts',(-39.2303030938182,-46.8096869394463,
-76.1608390644509));
#151209=CARTESIAN_POINT('Ctrl Pts',(-39.264838514336,-46.8014558784949,
-76.001779067251));
#151210=CARTESIAN_POINT('Ctrl Pts',(-39.2940438168355,-46.7944951807135,
-75.8672680271612));
#151211=CARTESIAN_POINT('Ctrl Pts',(-39.3257637466383,-46.7875503001958,
-75.7331091835309));
#151212=CARTESIAN_POINT('Ctrl Pts',(-39.3600912437891,-46.7806433619661,
-75.5993240027414));
#151213=CARTESIAN_POINT('Ctrl Pts',(-39.4012359993546,-46.7723647425283,
-75.4389697963834));
#151214=CARTESIAN_POINT('Ctrl Pts',(-39.4461824058822,-46.7641247054021,
-75.2789598860371));
#151215=CARTESIAN_POINT('Ctrl Pts',(-39.4950323080936,-46.7559182016718,
-75.1198288925915));
#151216=CARTESIAN_POINT('Ctrl Pts',(-39.5428091296028,-46.7478919693522,
-74.9641935130659));
#151217=CARTESIAN_POINT('Ctrl Pts',(-39.5943203183166,-46.7398980605529,
-74.8093990261248));
#151218=CARTESIAN_POINT('Ctrl Pts',(-39.6496298273295,-46.7319643620929,
-74.6559650168446));
#151219=CARTESIAN_POINT('Ctrl Pts',(-39.7049393363425,-46.7240306636329,
-74.5025310075644));
#151220=CARTESIAN_POINT('Ctrl Pts',(-39.7640477566345,-46.7161574167842,
-74.3504576467527));
#151221=CARTESIAN_POINT('Ctrl Pts',(-39.8269791847324,-46.7084020374917,
-74.2002817725628));
#151222=CARTESIAN_POINT('Ctrl Pts',(-39.8745311201513,-46.7025419560283,
-74.0868066189424));
#151223=CARTESIAN_POINT('Ctrl Pts',(-39.9242976680265,-46.6967835306671,
-73.9742725680164));
#151224=CARTESIAN_POINT('Ctrl Pts',(-39.9764418349066,-46.6910703067992,
-73.8627159546544));
#151225=CARTESIAN_POINT('Ctrl Pts',(-40.0277693349268,-46.6854465617911,
-73.752906508705));
#151226=CARTESIAN_POINT('Ctrl Pts',(-40.0814011405111,-46.6798663222219,
-73.644043931816));
#151227=CARTESIAN_POINT('Ctrl Pts',(-40.1375110305611,-46.6743128514715,
-73.5361901580596));
#151228=CARTESIAN_POINT('Ctrl Pts',(-40.1949600591147,-46.6686268396217,
-73.4257623079495));
#151229=CARTESIAN_POINT('Ctrl Pts',(-40.2550075097591,-46.6629683413473,
-73.3163916130317));
#151230=CARTESIAN_POINT('Ctrl Pts',(-40.317850220895,-46.6573653423464,
-73.2081779482056));
#151231=CARTESIAN_POINT('Ctrl Pts',(-40.3769396861228,-46.6520969793389,
-73.1064272842168));
#151232=CARTESIAN_POINT('Ctrl Pts',(-40.438501162163,-46.6468778743449,
-73.005699727026));
#151233=CARTESIAN_POINT('Ctrl Pts',(-40.5026976064787,-46.6417729019327,
-72.9061082583841));
#151234=CARTESIAN_POINT('Ctrl Pts',(-40.5067752375929,-46.6414486441865,
-72.8997824053626));
#151235=CARTESIAN_POINT('Ctrl Pts',(-40.5108634973868,-46.641124861076,
-72.8934611460772));
#151236=CARTESIAN_POINT('Ctrl Pts',(-40.5149624265548,-46.6408015750335,
-72.8871445136361));
#151237=CARTESIAN_POINT('Origin',(-39.5,-46.93000002,-55.2499500000008));
#151238=CARTESIAN_POINT('',(-39.,-46.9300000199928,-153.563058845201));
#151239=CARTESIAN_POINT('Origin',(-39.5,-46.9300000199999,-153.563058845195));
#151240=CARTESIAN_POINT('',(-39.,-46.93000002,-129.34995));
#151241=CARTESIAN_POINT('Ctrl Pts',(-40.9139483721511,-46.43000002,-159.04250796345));
#151242=CARTESIAN_POINT('Ctrl Pts',(-40.6980070138923,-46.43000002,-159.177513727936));
#151243=CARTESIAN_POINT('Ctrl Pts',(-40.5710289585984,-46.6359863492877,
-159.256899712053));
#151244=CARTESIAN_POINT('Ctrl Pts',(-40.6453734355539,-46.43000002,-158.612545232755));
#151245=CARTESIAN_POINT('Ctrl Pts',(-40.4000491853353,-46.43000002,-158.734901860446));
#151246=CARTESIAN_POINT('Ctrl Pts',(-40.2726319701784,-46.6590723862912,
-158.810854977709));
#151247=CARTESIAN_POINT('Ctrl Pts',(-40.4272411167408,-46.43000002,-158.162404667172));
#151248=CARTESIAN_POINT('Ctrl Pts',(-40.1587308612842,-46.43000002,-158.276021182203));
#151249=CARTESIAN_POINT('Ctrl Pts',(-40.0302467855321,-46.6832471055803,
-158.343663631397));
#151250=CARTESIAN_POINT('Ctrl Pts',(-40.0748112905834,-46.43000002,-157.263052526127));
#151251=CARTESIAN_POINT('Ctrl Pts',(-39.7601657220121,-46.43000002,-157.361162449029));
#151252=CARTESIAN_POINT('Ctrl Pts',(-39.6386598952534,-46.7315414595573,
-157.409909939755));
#151253=CARTESIAN_POINT('Ctrl Pts',(-39.936491307137,-46.43000002,-156.81535457804));
#151254=CARTESIAN_POINT('Ctrl Pts',(-39.6001021971278,-46.43000002,-156.903067496752));
#151255=CARTESIAN_POINT('Ctrl Pts',(-39.484972353656,-46.7555812340755,
-156.944919216257));
#151256=CARTESIAN_POINT('Ctrl Pts',(-39.5977060048933,-46.43000002,-155.407958919601));
#151257=CARTESIAN_POINT('Ctrl Pts',(-39.18209163777,-46.43000002,-155.432505947607));
#151258=CARTESIAN_POINT('Ctrl Pts',(-39.1085513924158,-46.8311357158264,
-155.482548023534));
#151259=CARTESIAN_POINT('Ctrl Pts',(-39.4929946038571,-46.43000002,-154.44272705014));
#151260=CARTESIAN_POINT('Ctrl Pts',(-39.0379952988168,-46.4300000199999,
-154.42847000153));
#151261=CARTESIAN_POINT('Ctrl Pts',(-38.9922097725462,-46.8829301245063,
-154.478770282061));
#151262=CARTESIAN_POINT('Ctrl Pts',(-39.5003628921561,-46.43000002,-153.467040782265));
#151263=CARTESIAN_POINT('Ctrl Pts',(-38.9951403347308,-46.4300000199999,
-153.463084491498));
#151264=CARTESIAN_POINT('Ctrl Pts',(-39.0004039132295,-46.9352126230012,
-153.463110895003));
#151265=CARTESIAN_POINT('',(-40.5149651533753,-46.6407282068896,-159.171551992371));
#151266=CARTESIAN_POINT('Origin',(-40.8634877666247,-46.93000002,-158.96051646616));
#151267=CARTESIAN_POINT('Ctrl Pts',(-40.5149614839772,-46.640792942112,
-159.171504755847));
#151268=CARTESIAN_POINT('Ctrl Pts',(-40.4511923171114,-46.645823490987,
-159.07323460075));
#151269=CARTESIAN_POINT('Ctrl Pts',(-40.3900526489562,-46.6509693267882,
-158.973921789425));
#151270=CARTESIAN_POINT('Ctrl Pts',(-40.331374886992,-46.6561622609605,
-158.87367813627));
#151271=CARTESIAN_POINT('Ctrl Pts',(-40.2710812776531,-46.6614981963103,
-158.770674008987));
#151272=CARTESIAN_POINT('Ctrl Pts',(-40.2133863650166,-46.6668839079942,
-158.6666870514));
#151273=CARTESIAN_POINT('Ctrl Pts',(-40.1581069327706,-46.6722900646723,
-158.561806464956));
#151274=CARTESIAN_POINT('Ctrl Pts',(-40.1019927837822,-46.6777778540536,
-158.45534218675));
#151275=CARTESIAN_POINT('Ctrl Pts',(-40.0483669724133,-46.6832869376886,
-158.347956944359));
#151276=CARTESIAN_POINT('Ctrl Pts',(-39.9970465019613,-46.6888297686089,
-158.239712731665));
#151277=CARTESIAN_POINT('Ctrl Pts',(-39.944733925413,-46.6944797512428,
-158.129375986647));
#151278=CARTESIAN_POINT('Ctrl Pts',(-39.8948160656533,-46.7001650767535,
-158.018146559171));
#151279=CARTESIAN_POINT('Ctrl Pts',(-39.8471176835924,-46.7059395833958,
-157.906060277828));
#151280=CARTESIAN_POINT('Ctrl Pts',(-39.8407923129947,-46.7067053513937,
-157.891196308909));
#151281=CARTESIAN_POINT('Ctrl Pts',(-39.8345060078927,-46.7074727414294,
-157.87631723173));
#151282=CARTESIAN_POINT('Ctrl Pts',(-39.8282583922396,-46.7082419270457,
-157.861423094293));
#151283=CARTESIAN_POINT('Ctrl Pts',(-39.7717626884057,-46.7151974898055,
-157.726738948491));
#151284=CARTESIAN_POINT('Ctrl Pts',(-39.7184638218149,-46.7222433276003,
-157.590841615228));
#151285=CARTESIAN_POINT('Ctrl Pts',(-39.6682083051711,-46.7293360118737,
-157.453806541317));
#151286=CARTESIAN_POINT('Ctrl Pts',(-39.6171120060077,-46.7365473578454,
-157.314478849553));
#151287=CARTESIAN_POINT('Ctrl Pts',(-39.5691610368222,-46.7438075845872,
-157.173974722644));
#151288=CARTESIAN_POINT('Ctrl Pts',(-39.5242175974619,-46.7511105793801,
-157.03234443406));
#151289=CARTESIAN_POINT('Ctrl Pts',(-39.4783447495199,-46.758564596572,
-156.88778529963));
#151290=CARTESIAN_POINT('Ctrl Pts',(-39.4356044625501,-46.7660637202736,
-156.742052563172));
#151291=CARTESIAN_POINT('Ctrl Pts',(-39.3958849012062,-46.7736346178437,
-156.595174950523));
#151292=CARTESIAN_POINT('Ctrl Pts',(-39.3844661816561,-46.7758111261729,
-156.552950056534));
#151293=CARTESIAN_POINT('Ctrl Pts',(-39.3732973633793,-46.7779937423037,
-156.510630409542));
#151294=CARTESIAN_POINT('Ctrl Pts',(-39.3623764117127,-46.7801834881411,
-156.468216397628));
#151295=CARTESIAN_POINT('Ctrl Pts',(-39.3213886065209,-46.7884018997361,
-156.309030887905));
#151296=CARTESIAN_POINT('Ctrl Pts',(-39.2841032524674,-46.7966765801414,
-156.149349043185));
#151297=CARTESIAN_POINT('Ctrl Pts',(-39.2503661597731,-46.8049680101138,
-155.98922493615));
#151298=CARTESIAN_POINT('Ctrl Pts',(-39.2158556778871,-46.8134495128462,
-155.82543014371));
#151299=CARTESIAN_POINT('Ctrl Pts',(-39.1850574748408,-46.8219492572809,
-155.661172069128));
#151300=CARTESIAN_POINT('Ctrl Pts',(-39.157847363523,-46.830454388723,-155.496486938258));
#151301=CARTESIAN_POINT('Ctrl Pts',(-39.1298994391238,-46.8391901402154,
-155.327336304014));
#151302=CARTESIAN_POINT('Ctrl Pts',(-39.1057364276871,-46.847932409478,
-155.157734529226));
#151303=CARTESIAN_POINT('Ctrl Pts',(-39.0852736729076,-46.8566860190199,
-154.987706928931));
#151304=CARTESIAN_POINT('Ctrl Pts',(-39.064673617634,-46.8654983633181,
-154.81653848158));
#151305=CARTESIAN_POINT('Ctrl Pts',(-39.0478236262521,-46.8743231257662,
-154.644937780829));
#151306=CARTESIAN_POINT('Ctrl Pts',(-39.034690197654,-46.8831704349881,
-154.472926755722));
#151307=CARTESIAN_POINT('Ctrl Pts',(-39.0215514753255,-46.8920213103216,
-154.300846397615));
#151308=CARTESIAN_POINT('Ctrl Pts',(-39.0121325773116,-46.9008956262777,
-154.12835470933));
#151309=CARTESIAN_POINT('Ctrl Pts',(-39.0064507305479,-46.9097951391645,
-153.955480082265));
#151310=CARTESIAN_POINT('Ctrl Pts',(-39.0021584937233,-46.9165180971254,
-153.824885423315));
#151311=CARTESIAN_POINT('Ctrl Pts',(-39.0000000085995,-46.9232553328191,
-153.694072304413));
#151312=CARTESIAN_POINT('Ctrl Pts',(-39.,-46.9300000199928,-153.563058845201));
#151313=CARTESIAN_POINT('Ctrl Pts',(-40.5149864073608,-46.6403532458042,
-159.17182559703));
#151314=CARTESIAN_POINT('Ctrl Pts',(-40.6428186202086,-46.43000002,-159.094316247135));
#151315=CARTESIAN_POINT('Ctrl Pts',(-40.8634877666247,-46.43000002,-158.96051646616));
#151316=CARTESIAN_POINT('Ctrl Pts',(-42.8925295367156,-46.6503554345072,
-163.106696326736));
#151317=CARTESIAN_POINT('Ctrl Pts',(-43.0357695446718,-46.4300000199999,
-163.055969456472));
#151318=CARTESIAN_POINT('Ctrl Pts',(-43.2493416424527,-46.43000002,-162.895383432653));
#151319=CARTESIAN_POINT('Ctrl Pts',(-45.2098379840441,-46.6594189992588,
-167.077916061371));
#151320=CARTESIAN_POINT('Ctrl Pts',(-45.3499681200706,-46.4300000200635,
-167.025403443097));
#151321=CARTESIAN_POINT('Ctrl Pts',(-45.5734830336511,-46.43000002,-166.866604917879));
#151322=CARTESIAN_POINT('Ctrl Pts',(-47.4880541505298,-46.6677435098469,
-171.07256826174));
#151323=CARTESIAN_POINT('Ctrl Pts',(-47.6152001643476,-46.4300000199999,
-170.99986675708));
#151324=CARTESIAN_POINT('Ctrl Pts',(-47.8576079004676,-46.43000002,-170.861259130871));
#151325=CARTESIAN_POINT('',(-47.4880541505298,-46.6677435098469,-171.07256826174));
#151326=CARTESIAN_POINT('Origin',(-47.8576079004676,-46.93000002,-170.861259130871));
#151327=CARTESIAN_POINT('Ctrl Pts',(-47.4880541505298,-46.6677435098469,
-171.07256826174));
#151328=CARTESIAN_POINT('Ctrl Pts',(-45.2098379840441,-46.6594189992588,
-167.077916061371));
#151329=CARTESIAN_POINT('Ctrl Pts',(-42.8925295367156,-46.6503554345072,
-163.106696326736));
#151330=CARTESIAN_POINT('Ctrl Pts',(-40.5149864073608,-46.6403532458042,
-159.17182559703));
#151331=CARTESIAN_POINT('Ctrl Pts',(-48.4122058243951,-46.43000002,-171.14995));
#151332=CARTESIAN_POINT('Ctrl Pts',(-48.4122058243951,-46.43000002,-171.64995));
#151333=CARTESIAN_POINT('Ctrl Pts',(-48.4122058243951,-46.93000002,-171.64995));
#151334=CARTESIAN_POINT('Ctrl Pts',(-48.3039317427638,-46.43000002,-171.149949965311));
#151335=CARTESIAN_POINT('Ctrl Pts',(-48.2401145573434,-46.43000002,-171.601506869702));
#151336=CARTESIAN_POINT('Ctrl Pts',(-48.231362292365,-46.8790932958503,
-171.64995));
#151337=CARTESIAN_POINT('Ctrl Pts',(-48.1935717932631,-46.43000002,-171.125988974658));
#151338=CARTESIAN_POINT('Ctrl Pts',(-48.0743475333484,-46.4300000200007,
-171.520103948478));
#151339=CARTESIAN_POINT('Ctrl Pts',(-48.0473109525228,-46.8270214030016,
-171.602027929987));
#151340=CARTESIAN_POINT('Ctrl Pts',(-47.9990582077163,-46.43000002,-171.030110581883));
#151341=CARTESIAN_POINT('Ctrl Pts',(-47.8027749187994,-46.4300000199993,
-171.303307031957));
#151342=CARTESIAN_POINT('Ctrl Pts',(-47.7232867546241,-46.734966787668,
-171.410271183096));
#151343=CARTESIAN_POINT('Ctrl Pts',(-47.9126814701194,-46.43000002,-170.95757572435));
#151344=CARTESIAN_POINT('Ctrl Pts',(-47.6869922690936,-46.43000002,-171.166719195593));
#151345=CARTESIAN_POINT('Ctrl Pts',(-47.5795866952779,-46.693929642055,
-171.265147156144));
#151346=CARTESIAN_POINT('Ctrl Pts',(-47.8576079004676,-46.43000002,-170.861259130871));
#151347=CARTESIAN_POINT('Ctrl Pts',(-47.6152001643476,-46.43000002,-170.99986675708));
#151348=CARTESIAN_POINT('Ctrl Pts',(-47.4880541505298,-46.6677435098469,
-171.07256826174));
#151349=CARTESIAN_POINT('',(-48.4122058243951,-46.93000002,-171.64995));
#151350=CARTESIAN_POINT('Origin',(-48.4122058243951,-46.93000002,-171.14995));
#151351=CARTESIAN_POINT('Ctrl Pts',(-48.4122058243951,-46.93000002,-171.64995));
#151352=CARTESIAN_POINT('Ctrl Pts',(-48.231362292365,-46.8790932958503,
-171.64995));
#151353=CARTESIAN_POINT('Ctrl Pts',(-48.0473109525228,-46.8270214030016,
-171.602027929987));
#151354=CARTESIAN_POINT('Ctrl Pts',(-47.7232867546241,-46.734966787668,
-171.410271183096));
#151355=CARTESIAN_POINT('Ctrl Pts',(-47.5795866952779,-46.693929642055,
-171.265147156144));
#151356=CARTESIAN_POINT('Ctrl Pts',(-47.4880541505298,-46.6677435098469,
-171.07256826174));
#151357=CARTESIAN_POINT('Origin',(1.41965171211599E-14,-46.93000002,-171.14995));
#151358=CARTESIAN_POINT('',(-50.4241310475534,-46.93000002,-171.64995));
#151359=CARTESIAN_POINT('Origin',(-50.4241310475534,-46.93000002,-171.14995));
#151360=CARTESIAN_POINT('',(-48.7591445042216,-46.93000002,-171.64995));
#151361=CARTESIAN_POINT('Ctrl Pts',(-50.4241310475534,-46.93000002,-171.64995));
#151362=CARTESIAN_POINT('Ctrl Pts',(-50.4241310475535,-46.43000002,-171.64995));
#151363=CARTESIAN_POINT('Ctrl Pts',(-50.4241310475534,-46.43000002,-171.14995));
#151364=CARTESIAN_POINT('Ctrl Pts',(-50.5576213910783,-46.9208895200013,
-171.64995));
#151365=CARTESIAN_POINT('Ctrl Pts',(-50.5563794763166,-46.43000002,-171.640924254979));
#151366=CARTESIAN_POINT('Ctrl Pts',(-50.6224459669284,-46.43000002,-171.149950000016));
#151367=CARTESIAN_POINT('Ctrl Pts',(-50.6910111165761,-46.911785887019,
-171.675977326981));
#151368=CARTESIAN_POINT('Ctrl Pts',(-50.6936490544688,-46.43000002,-171.658003579003));
#151369=CARTESIAN_POINT('Ctrl Pts',(-50.8206114069094,-46.43000002,-171.18899099047));
#151370=CARTESIAN_POINT('Ctrl Pts',(-50.9376246396682,-46.8949549130127,
-171.776163607997));
#151371=CARTESIAN_POINT('Ctrl Pts',(-50.9520843153697,-46.4300000199999,
-171.746711574348));
#151372=CARTESIAN_POINT('Ctrl Pts',(-51.1869835328424,-46.43000002,-171.339270411997));
#151373=CARTESIAN_POINT('Ctrl Pts',(-51.0507273913534,-46.887235833176,
-171.850283164392));
#151374=CARTESIAN_POINT('Ctrl Pts',(-51.0736480315269,-46.4300000199987,
-171.817687494207));
#151375=CARTESIAN_POINT('Ctrl Pts',(-51.3550103914843,-46.43000002,-171.450449746589));
#151376=CARTESIAN_POINT('Ctrl Pts',(-51.239477210225,-46.8743539633763,
-172.035403273235));
#151377=CARTESIAN_POINT('Ctrl Pts',(-51.2780932509,-46.4300000200014,-172.003556970023));
#151378=CARTESIAN_POINT('Ctrl Pts',(-51.6354194766937,-46.43000002,-171.728129909852));
#151379=CARTESIAN_POINT('Ctrl Pts',(-51.3150500528584,-46.8691962391206,
-172.14633102856));
#151380=CARTESIAN_POINT('Ctrl Pts',(-51.3616623431659,-46.43000002,-172.118296873734));
#151381=CARTESIAN_POINT('Ctrl Pts',(-51.7476914343352,-46.43000002,-171.894521542842));
#151382=CARTESIAN_POINT('Ctrl Pts',(-51.4172007186852,-46.8622246214263,
-172.38820210671));
#151383=CARTESIAN_POINT('Ctrl Pts',(-51.4744733522994,-46.43000002,-172.371853931892));
#151384=CARTESIAN_POINT('Ctrl Pts',(-51.8994477376182,-46.43000002,-172.257328160063));
#151385=CARTESIAN_POINT('Ctrl Pts',(-51.4437383719602,-46.8604134695225,
-172.51902671195));
#151386=CARTESIAN_POINT('Ctrl Pts',(-51.5042290374097,-46.43000002,-172.511015867073));
#151387=CARTESIAN_POINT('Ctrl Pts',(-51.9388724063164,-46.43000002,-172.453565067926));
#151388=CARTESIAN_POINT('Ctrl Pts',(-51.4437383719606,-46.86041346952,-172.64995));
#151389=CARTESIAN_POINT('Ctrl Pts',(-51.5042290374232,-46.43000002,-172.64995));
#151390=CARTESIAN_POINT('Ctrl Pts',(-51.9388724063314,-46.43000002,-172.64995));
#151391=CARTESIAN_POINT('Origin',(-51.9388724063314,-46.93000002,-172.64995));
#151392=CARTESIAN_POINT('Ctrl Pts',(-51.4437383719606,-46.86041346952,-172.64995));
#151393=CARTESIAN_POINT('Ctrl Pts',(-51.4437383719602,-46.8604134695225,
-172.51902671195));
#151394=CARTESIAN_POINT('Ctrl Pts',(-51.4172007186852,-46.8622246214263,
-172.38820210671));
#151395=CARTESIAN_POINT('Ctrl Pts',(-51.3150500528584,-46.8691962391206,
-172.14633102856));
#151396=CARTESIAN_POINT('Ctrl Pts',(-51.239477210225,-46.8743539633763,
-172.035403273235));
#151397=CARTESIAN_POINT('Ctrl Pts',(-51.0507273913534,-46.887235833176,
-171.850283164392));
#151398=CARTESIAN_POINT('Ctrl Pts',(-50.9376246396682,-46.8949549130127,
-171.776163607997));
#151399=CARTESIAN_POINT('Ctrl Pts',(-50.6910111165761,-46.911785887019,
-171.675977326981));
#151400=CARTESIAN_POINT('Ctrl Pts',(-50.5576213910783,-46.9208895200013,
-171.64995));
#151401=CARTESIAN_POINT('Ctrl Pts',(-50.4241310475534,-46.93000002,-171.64995));
#151402=CARTESIAN_POINT('Origin',(-51.9388724063314,-46.93000002,-171.64995));
#151403=CARTESIAN_POINT('Origin',(-51.9388724063314,-46.93000002,-176.84995));
#151404=CARTESIAN_POINT('Origin',(83.2809572255632,-45.9300000199999,-176.84995));
#151405=CARTESIAN_POINT('',(-57.,-45.93000002,-177.34995));
#151406=CARTESIAN_POINT('Origin',(-57.,-45.93000002,-176.84995));
#151407=CARTESIAN_POINT('',(-52.0794132410337,-45.93000002,-177.34995));
#151408=CARTESIAN_POINT('',(-60.,-45.93000002,-177.34995));
#151409=CARTESIAN_POINT('Ctrl Pts',(-51.9388724063314,-46.43000002,-176.84995));
#151410=CARTESIAN_POINT('Ctrl Pts',(-51.9388724063423,-46.43000002,-176.981217345763));
#151411=CARTESIAN_POINT('Ctrl Pts',(-51.9540189315504,-46.3761134565303,
-177.110943344657));
#151412=CARTESIAN_POINT('Ctrl Pts',(-52.0060527960138,-46.1909933646562,
-177.296063436531));
#151413=CARTESIAN_POINT('Ctrl Pts',(-52.0425163963479,-46.0612673657634,
-177.34995));
#151414=CARTESIAN_POINT('Ctrl Pts',(-52.0794132410337,-45.93000002,-177.34995));
#151415=CARTESIAN_POINT('Origin',(-57.,-45.93000002,-174.34995));
#151416=CARTESIAN_POINT('',(-60.,-45.93000002,-174.34995));
#151417=CARTESIAN_POINT('Origin',(-59.5,-45.93000002,-174.34995));
#151418=CARTESIAN_POINT('Origin',(-57.,-45.93000002,-174.34995));
#151419=CARTESIAN_POINT('Origin',(-59.5,-45.93000002,-55.2499500000008));
#151420=CARTESIAN_POINT('',(-60.,-45.93000002,-58.24995));
#151421=CARTESIAN_POINT('Origin',(-59.5,-45.93000002,-58.24995));
#151422=CARTESIAN_POINT('',(-60.,-45.93000002,-174.34995));
#151423=CARTESIAN_POINT('Origin',(-57.,-45.93000002,-58.24995));
#151424=CARTESIAN_POINT('Origin',(-57.,-45.93000002,-58.24995));
#151425=CARTESIAN_POINT('Origin',(-57.,-2.42462934179819E-14,-58.24995));
#151426=CARTESIAN_POINT('',(-60.,-45.43000002,-58.24995));
#151427=CARTESIAN_POINT('Origin',(-57.,-45.43000002,-58.24995));
#151428=CARTESIAN_POINT('',(-60.,-54.58000002,-58.24995));
#151429=CARTESIAN_POINT('Origin',(-57.,-45.43000002,-58.24995));
#151430=CARTESIAN_POINT('Origin',(-59.5,-45.43000002,-58.24995));
#151431=CARTESIAN_POINT('Origin',(83.2809572255632,-44.43000002,-61.14995));
#151432=CARTESIAN_POINT('Origin',(-60.,-45.43000002,-176.84995));
#151433=CARTESIAN_POINT('',(-52.1496836583849,-45.43000002,-177.34995));
#151434=CARTESIAN_POINT('',(-57.,-45.43000002,-177.34995));
#151435=CARTESIAN_POINT('',(-60.,-45.43000002,-177.34995));
#151436=CARTESIAN_POINT('Origin',(-57.,-45.43000002,-176.84995));
#151437=CARTESIAN_POINT('Ctrl Pts',(-52.1496836583849,-45.43000002,-177.34995));
#151438=CARTESIAN_POINT('Ctrl Pts',(-52.1865805030705,-45.2987326742378,
-177.34995));
#151439=CARTESIAN_POINT('Ctrl Pts',(-52.2230441034049,-45.1690066753419,
-177.296063436528));
#151440=CARTESIAN_POINT('Ctrl Pts',(-52.2750779678683,-44.9838865834715,
-177.110943344658));
#151441=CARTESIAN_POINT('Ctrl Pts',(-52.2902244930764,-44.93000002,-176.981217345763));
#151442=CARTESIAN_POINT('Ctrl Pts',(-52.2902244930873,-44.93000002,-176.84995));
#151443=CARTESIAN_POINT('Origin',(-52.2902244930873,-44.43000002,-171.64995));
#151444=CARTESIAN_POINT('',(-51.7902244930873,-44.43000002,-172.64995));
#151445=CARTESIAN_POINT('Origin',(-52.2902244930873,-44.43000002,-172.64995));
#151446=CARTESIAN_POINT('Origin',(-52.2902244930873,-44.43000002,-176.84995));
#151447=CARTESIAN_POINT('Origin',(-52.2902244930873,-44.43000002,-172.64995));
#151448=CARTESIAN_POINT('Ctrl Pts',(-51.7950904587165,-44.36041346952,-172.64995));
#151449=CARTESIAN_POINT('Ctrl Pts',(-51.7150402894768,-44.93000002,-172.64995));
#151450=CARTESIAN_POINT('Ctrl Pts',(-52.2902244930873,-44.93000002,-172.64995));
#151451=CARTESIAN_POINT('Ctrl Pts',(-51.7950904587162,-44.3604134695225,
-172.51902671195));
#151452=CARTESIAN_POINT('Ctrl Pts',(-51.7150402894748,-44.9300000200027,
-172.529650273729));
#151453=CARTESIAN_POINT('Ctrl Pts',(-52.2902244930723,-44.93000002,-172.453565067926));
#151454=CARTESIAN_POINT('Ctrl Pts',(-51.7685528054411,-44.3622246214263,
-172.38820210671));
#151455=CARTESIAN_POINT('Ctrl Pts',(-51.6933705738162,-44.93000002,-172.409726298163));
#151456=CARTESIAN_POINT('Ctrl Pts',(-52.2507998243741,-44.93000002,-172.257328160063));
#151457=CARTESIAN_POINT('Ctrl Pts',(-51.6664021396144,-44.3691962391205,
-172.14633102856));
#151458=CARTESIAN_POINT('Ctrl Pts',(-51.6069372443981,-44.93000002,-172.182182441317));
#151459=CARTESIAN_POINT('Ctrl Pts',(-52.0990435210912,-44.93000002,-171.894521542842));
#151460=CARTESIAN_POINT('Ctrl Pts',(-51.5908292969809,-44.3743539633763,
-172.035403273235));
#151461=CARTESIAN_POINT('Ctrl Pts',(-51.5426661785871,-44.9300000199979,
-172.075215659168));
#151462=CARTESIAN_POINT('Ctrl Pts',(-51.9867715634496,-44.93000002,-171.728129909852));
#151463=CARTESIAN_POINT('Ctrl Pts',(-51.4020794781095,-44.387235833176,
-171.850283164392));
#151464=CARTESIAN_POINT('Ctrl Pts',(-51.3750094074331,-44.930000020002,
-171.888983273332));
#151465=CARTESIAN_POINT('Ctrl Pts',(-51.7063624782404,-44.93000002,-171.450449746589));
#151466=CARTESIAN_POINT('Ctrl Pts',(-51.2889767264242,-44.3949549130127,
-171.776163607997));
#151467=CARTESIAN_POINT('Ctrl Pts',(-51.2724346946947,-44.9300000200007,
-171.809929875206));
#151468=CARTESIAN_POINT('Ctrl Pts',(-51.5383356195984,-44.93000002,-171.339270411997));
#151469=CARTESIAN_POINT('Ctrl Pts',(-51.0423632033321,-44.411785887019,
-171.675977326981));
#151470=CARTESIAN_POINT('Ctrl Pts',(-51.0396558988745,-44.9300000199993,
-171.69520402023));
#151471=CARTESIAN_POINT('Ctrl Pts',(-51.1719634936654,-44.93000002,-171.18899099047));
#151472=CARTESIAN_POINT('Ctrl Pts',(-50.9089734778343,-44.4208895200012,
-171.64995));
#151473=CARTESIAN_POINT('Ctrl Pts',(-50.9102650806209,-44.93000002,-171.659148653595));
#151474=CARTESIAN_POINT('Ctrl Pts',(-50.9737980536844,-44.93000002,-171.149950000016));
#151475=CARTESIAN_POINT('Ctrl Pts',(-50.7754831343094,-44.43000002,-171.64995));
#151476=CARTESIAN_POINT('Ctrl Pts',(-50.7754831343094,-44.9300000199999,
-171.64995));
#151477=CARTESIAN_POINT('Ctrl Pts',(-50.7754831343094,-44.93000002,-171.14995));
#151478=CARTESIAN_POINT('',(-50.7754831343094,-44.43000002,-171.64995));
#151479=CARTESIAN_POINT('Origin',(-50.7754831343094,-44.43000002,-171.14995));
#151480=CARTESIAN_POINT('Ctrl Pts',(-50.7754831343094,-44.43000002,-171.64995));
#151481=CARTESIAN_POINT('Ctrl Pts',(-50.9089734778343,-44.4208895200012,
-171.64995));
#151482=CARTESIAN_POINT('Ctrl Pts',(-51.0423632033321,-44.411785887019,
-171.675977326981));
#151483=CARTESIAN_POINT('Ctrl Pts',(-51.2889767264242,-44.3949549130127,
-171.776163607997));
#151484=CARTESIAN_POINT('Ctrl Pts',(-51.4020794781095,-44.387235833176,
-171.850283164392));
#151485=CARTESIAN_POINT('Ctrl Pts',(-51.5908292969809,-44.3743539633763,
-172.035403273235));
#151486=CARTESIAN_POINT('Ctrl Pts',(-51.6664021396144,-44.3691962391205,
-172.14633102856));
#151487=CARTESIAN_POINT('Ctrl Pts',(-51.7685528054411,-44.3622246214263,
-172.38820210671));
#151488=CARTESIAN_POINT('Ctrl Pts',(-51.7950904587162,-44.3604134695225,
-172.51902671195));
#151489=CARTESIAN_POINT('Ctrl Pts',(-51.7950904587165,-44.36041346952,-172.64995));
#151490=CARTESIAN_POINT('Origin',(1.31515029790052E-14,-44.43000002,-171.14995));
#151491=CARTESIAN_POINT('',(-50.0729884546894,-44.43000002,-171.64995));
#151492=CARTESIAN_POINT('Origin',(-50.0729884546894,-44.43000002,-171.14995));
#151493=CARTESIAN_POINT('',(-50.7052127169582,-44.43000002,-171.64995));
#151494=CARTESIAN_POINT('Ctrl Pts',(-49.5369875341119,-44.93000002,-170.861259130871));
#151495=CARTESIAN_POINT('Ctrl Pts',(-48.7929216289437,-44.9300000199999,
-171.272289063137));
#151496=CARTESIAN_POINT('Ctrl Pts',(-49.1544657093286,-44.1870483688939,
-171.07256826174));
#151497=CARTESIAN_POINT('Ctrl Pts',(-49.5629323055535,-44.93000002,-170.908225431312));
#151498=CARTESIAN_POINT('Ctrl Pts',(-48.8869683938206,-44.93000002,-171.389208114715));
#151499=CARTESIAN_POINT('Ctrl Pts',(-49.1988333494309,-44.1988790013969,
-171.166486883581));
#151500=CARTESIAN_POINT('Ctrl Pts',(-49.5959607588443,-44.93000002,-170.94944826591));
#151501=CARTESIAN_POINT('Ctrl Pts',(-48.9974211832039,-44.93000002,-171.47664075754));
#151502=CARTESIAN_POINT('Ctrl Pts',(-49.2553422033029,-44.2139336491638,
-171.248946535323));
#151503=CARTESIAN_POINT('Ctrl Pts',(-49.673955990897,-44.93000002,-171.02211105853));
#151504=CARTESIAN_POINT('Ctrl Pts',(-49.2286028218105,-44.93000002,-171.604363908288));
#151505=CARTESIAN_POINT('Ctrl Pts',(-49.3888358236751,-44.249424483408,
-171.394272113556));
#151506=CARTESIAN_POINT('Ctrl Pts',(-49.7179930277929,-44.93000002,-171.052463257479));
#151507=CARTESIAN_POINT('Ctrl Pts',(-49.3448677594853,-44.9300000199992,
-171.644582495821));
#151508=CARTESIAN_POINT('Ctrl Pts',(-49.4642369070823,-44.2694386569593,
-171.45497652175));
#151509=CARTESIAN_POINT('Ctrl Pts',(-49.8597665056525,-44.93000002,-171.125547207032));
#151510=CARTESIAN_POINT('Ctrl Pts',(-49.6719308335793,-44.9300000200013,
-171.711639121533));
#151511=CARTESIAN_POINT('Ctrl Pts',(-49.7071198591548,-44.3337582466603,
-171.601144400479));
#151512=CARTESIAN_POINT('Ctrl Pts',(-49.9661358829125,-44.93000002,-171.149949988199));
#151513=CARTESIAN_POINT('Ctrl Pts',(-49.8809090309114,-44.93000002,-171.700346637809));
#151514=CARTESIAN_POINT('Ctrl Pts',(-49.8895242589787,-44.3818638633066,
-171.64995));
#151515=CARTESIAN_POINT('Ctrl Pts',(-50.0729884546894,-44.93000002,-171.14995));
#151516=CARTESIAN_POINT('Ctrl Pts',(-50.0729884546893,-44.93000002,-171.64995));
#151517=CARTESIAN_POINT('Ctrl Pts',(-50.0729884546894,-44.43000002,-171.64995));
#151518=CARTESIAN_POINT('',(-49.1544657093286,-44.1870483688939,-171.07256826174));
#151519=CARTESIAN_POINT('Origin',(-49.5369875341119,-44.43000002,-170.861259130871));
#151520=CARTESIAN_POINT('Ctrl Pts',(-49.1544657093286,-44.1870483688939,
-171.07256826174));
#151521=CARTESIAN_POINT('Ctrl Pts',(-49.1988333494309,-44.1988790013969,
-171.166486883581));
#151522=CARTESIAN_POINT('Ctrl Pts',(-49.2553422033029,-44.2139336491638,
-171.248946535323));
#151523=CARTESIAN_POINT('Ctrl Pts',(-49.3888358236751,-44.249424483408,
-171.394272113556));
#151524=CARTESIAN_POINT('Ctrl Pts',(-49.4642369070823,-44.2694386569593,
-171.45497652175));
#151525=CARTESIAN_POINT('Ctrl Pts',(-49.7071198591548,-44.3337582466603,
-171.601144400479));
#151526=CARTESIAN_POINT('Ctrl Pts',(-49.8895242589787,-44.3818638633066,
-171.64995));
#151527=CARTESIAN_POINT('Ctrl Pts',(-50.0729884546894,-44.43000002,-171.64995));
#151528=CARTESIAN_POINT('Ctrl Pts',(-49.1544657093286,-44.1870483688939,
-171.07256826174));
#151529=CARTESIAN_POINT('Ctrl Pts',(-48.7929216289437,-44.9300000199999,
-171.272289063137));
#151530=CARTESIAN_POINT('Ctrl Pts',(-49.5369875341119,-44.93000002,-170.861259130871));
#151531=CARTESIAN_POINT('Ctrl Pts',(-46.303473398785,-44.1770628106394,
-165.900085726624));
#151532=CARTESIAN_POINT('Ctrl Pts',(-45.8620651160177,-44.9300000199373,
-166.013584137672));
#151533=CARTESIAN_POINT('Ctrl Pts',(-46.6796506810215,-44.93000002,-165.688772250388));
#151534=CARTESIAN_POINT('Ctrl Pts',(-43.4017256360502,-44.1659184128467,
-160.756986066495));
#151535=CARTESIAN_POINT('Ctrl Pts',(-42.9064403928045,-44.93000002,-160.851370978315));
#151536=CARTESIAN_POINT('Ctrl Pts',(-43.7703248719811,-44.93000002,-160.54566797298));
#151537=CARTESIAN_POINT('Ctrl Pts',(-40.4124516249929,-44.1531545436406,
-155.665156257244));
#151538=CARTESIAN_POINT('Ctrl Pts',(-39.9673804148566,-44.93000002,-155.927306340695));
#151539=CARTESIAN_POINT('Ctrl Pts',(-40.7712064624936,-44.93000002,-155.453847126373));
#151540=CARTESIAN_POINT('',(-40.4124515954294,-44.1531546078393,-155.665156239121));
#151541=CARTESIAN_POINT('Origin',(-40.7712064624936,-44.43000002,-155.453847126373));
#151542=CARTESIAN_POINT('Ctrl Pts',(-40.4124516249929,-44.1531545436406,
-155.665156257244));
#151543=CARTESIAN_POINT('Ctrl Pts',(-43.4017256360502,-44.1659184128467,
-160.756986066495));
#151544=CARTESIAN_POINT('Ctrl Pts',(-46.303473398785,-44.1770628106394,
-165.900085726624));
#151545=CARTESIAN_POINT('Ctrl Pts',(-49.1544657093286,-44.1870483688939,
-171.07256826174));
#151546=CARTESIAN_POINT('Ctrl Pts',(-39.5,-44.93000002,-150.364854264666));
#151547=CARTESIAN_POINT('Ctrl Pts',(-39.0000000000006,-44.93000002,-150.364854264666));
#151548=CARTESIAN_POINT('Ctrl Pts',(-39.,-44.4300000200006,-150.364854264665));
#151549=CARTESIAN_POINT('Ctrl Pts',(-39.5000000014677,-44.93000002,-151.253598202975));
#151550=CARTESIAN_POINT('Ctrl Pts',(-38.9493378739027,-44.93000002,-151.339754274397));
#151551=CARTESIAN_POINT('Ctrl Pts',(-38.9999999999989,-44.3818073757215,
-151.292233578463));
#151552=CARTESIAN_POINT('Ctrl Pts',(-39.5994072100806,-44.93000002,-152.128156158989));
#151553=CARTESIAN_POINT('Ctrl Pts',(-39.0101446877546,-44.93000002,-152.270659170967));
#151554=CARTESIAN_POINT('Ctrl Pts',(-39.1104524571481,-44.3342708908056,
-152.203846600498));
#151555=CARTESIAN_POINT('Ctrl Pts',(-39.9069198952433,-44.93000002,-153.416428338509));
#151556=CARTESIAN_POINT('Ctrl Pts',(-39.2308584472657,-44.93000002,-153.622795365418));
#151557=CARTESIAN_POINT('Ctrl Pts',(-39.4521332161855,-44.2641615099952,
-153.545498595041));
#151558=CARTESIAN_POINT('Ctrl Pts',(-40.0374208080396,-44.93000002,-153.8438516675));
#151559=CARTESIAN_POINT('Ctrl Pts',(-39.336211428575,-44.93000002,-154.093302098276));
#151560=CARTESIAN_POINT('Ctrl Pts',(-39.5971342320646,-44.2408855884987,
-153.990424071582));
#151561=CARTESIAN_POINT('Ctrl Pts',(-40.356527124461,-44.93000002,-154.669573645042));
#151562=CARTESIAN_POINT('Ctrl Pts',(-39.6029233414186,-44.9300000199999,
-155.022603846473));
#151563=CARTESIAN_POINT('Ctrl Pts',(-39.9516968040472,-44.1959019617888,
-154.849602863721));
#151564=CARTESIAN_POINT('Ctrl Pts',(-40.5450613770689,-44.93000002,-155.069904201826));
#151565=CARTESIAN_POINT('Ctrl Pts',(-39.7696946227985,-44.93000002,-155.485741538253));
#151566=CARTESIAN_POINT('Ctrl Pts',(-40.1611888206879,-44.1740829716026,
-155.265988433439));
#151567=CARTESIAN_POINT('Ctrl Pts',(-40.7712064624936,-44.93000002,-155.453847126373));
#151568=CARTESIAN_POINT('Ctrl Pts',(-39.9673804148566,-44.93000002,-155.927306340695));
#151569=CARTESIAN_POINT('Ctrl Pts',(-40.4124516249929,-44.1531545436406,
-155.665156257244));
#151570=CARTESIAN_POINT('',(-39.,-44.4300000199906,-150.364854264666));
#151571=CARTESIAN_POINT('Origin',(-39.5,-44.43000002,-150.364854264666));
#151572=CARTESIAN_POINT('Ctrl Pts',(-39.,-44.4300000200006,-150.364854264666));
#151573=CARTESIAN_POINT('Ctrl Pts',(-38.999999999999,-44.3818073757215,
-151.292233578463));
#151574=CARTESIAN_POINT('Ctrl Pts',(-39.1104524571481,-44.3342708908056,
-152.203846600499));
#151575=CARTESIAN_POINT('Ctrl Pts',(-39.3382396298397,-44.2875313035987,
-153.098281263527));
#151576=CARTESIAN_POINT('Ctrl Pts',(-39.4521332161855,-44.2641615099952,
-153.545498595041));
#151577=CARTESIAN_POINT('Ctrl Pts',(-39.5971342320646,-44.2408855884987,
-153.990424071582));
#151578=CARTESIAN_POINT('Ctrl Pts',(-39.7744155180559,-44.2183937751437,
-154.420013467651));
#151579=CARTESIAN_POINT('Ctrl Pts',(-39.9516967998039,-44.1959019623272,
-154.849602853438));
#151580=CARTESIAN_POINT('Ctrl Pts',(-40.1611888106594,-44.1740829726471,
-155.265988413506));
#151581=CARTESIAN_POINT('Ctrl Pts',(-40.4124516069506,-44.1531545451434,
-155.665156228581));
#151582=CARTESIAN_POINT('Origin',(-39.5,-44.43000002,-55.2499500000007));
#151583=CARTESIAN_POINT('',(-39.,-44.43000002,-81.6937887068282));
#151584=CARTESIAN_POINT('Origin',(-39.5,-44.43000002,-81.6937887068282));
#151585=CARTESIAN_POINT('',(-39.,-44.43000002,-129.34995));
#151586=CARTESIAN_POINT('Ctrl Pts',(-41.0619056481271,-44.93000002,-76.1510528072502));
#151587=CARTESIAN_POINT('Ctrl Pts',(-40.2383013915693,-44.9300000200001,
-75.5735325535681));
#151588=CARTESIAN_POINT('Ctrl Pts',(-40.7356761305387,-44.1280183635067,
-75.9220149346039));
#151589=CARTESIAN_POINT('Ctrl Pts',(-40.6997637919875,-44.93000002,-76.6715445325856));
#151590=CARTESIAN_POINT('Ctrl Pts',(-39.915133580973,-44.9300000199999,
-76.1827431658708));
#151591=CARTESIAN_POINT('Ctrl Pts',(-40.3333152536302,-44.1563776140685,
-76.4629140546281));
#151592=CARTESIAN_POINT('Ctrl Pts',(-40.4205675940477,-44.93000002,-77.2240865411077));
#151593=CARTESIAN_POINT('Ctrl Pts',(-39.660816170609,-44.93000002,-76.8319017752828));
#151594=CARTESIAN_POINT('Ctrl Pts',(-40.023059761065,-44.186488846014,-77.037491401942));
#151595=CARTESIAN_POINT('Ctrl Pts',(-40.039661195993,-44.93000002,-78.208477386432));
#151596=CARTESIAN_POINT('Ctrl Pts',(-39.3372827309322,-44.93000002,-77.9582690332229));
#151597=CARTESIAN_POINT('Ctrl Pts',(-39.5997881972139,-44.2401083817187,
-78.0617130018949));
#151598=CARTESIAN_POINT('Ctrl Pts',(-39.9103339554084,-44.93000002,-78.6298739674098));
#151599=CARTESIAN_POINT('Ctrl Pts',(-39.2328733408237,-44.93000002,-78.4220178024824));
#151600=CARTESIAN_POINT('Ctrl Pts',(-39.4560716552024,-44.2630556348417,
-78.5003466592746));
#151601=CARTESIAN_POINT('Ctrl Pts',(-39.558721486255,-44.93000002,-80.0963039522294));
#151602=CARTESIAN_POINT('Ctrl Pts',(-38.9834353962971,-44.93000002,-79.9425516378539));
#151603=CARTESIAN_POINT('Ctrl Pts',(-39.0653053548081,-44.3428691652806,
-80.0275378636304));
#151604=CARTESIAN_POINT('Ctrl Pts',(-39.4642346663104,-44.93000002,-81.1617889688827));
#151605=CARTESIAN_POINT('Ctrl Pts',(-38.9290061700283,-44.9300000199999,
-81.0769866725498));
#151606=CARTESIAN_POINT('Ctrl Pts',(-38.9602847906733,-44.4007851791287,
-81.1383456746059));
#151607=CARTESIAN_POINT('Ctrl Pts',(-39.5119572736767,-44.93000002,-82.225747614569));
#151608=CARTESIAN_POINT('Ctrl Pts',(-39.0403511889319,-44.9300000199999,
-82.2482379714646));
#151609=CARTESIAN_POINT('Ctrl Pts',(-39.0132635226448,-44.4584456120789,
-82.2489957256636));
#151610=CARTESIAN_POINT('Origin',(-40.7712064624936,-44.43000002,-76.6047958451324));
#151611=CARTESIAN_POINT('Ctrl Pts',(-40.4124516186295,-44.153154649867,
-76.3934867953418));
#151612=CARTESIAN_POINT('Ctrl Pts',(-40.3492687471321,-44.1584174362915,
-76.4938623552029));
#151613=CARTESIAN_POINT('Ctrl Pts',(-40.2887972234514,-44.1637790836454,
-76.5952597648493));
#151614=CARTESIAN_POINT('Ctrl Pts',(-40.2308619735706,-44.1691773515359,
-76.6975721748967));
#151615=CARTESIAN_POINT('Ctrl Pts',(-40.1720233715351,-44.1746597916175,
-76.8014798854953));
#151616=CARTESIAN_POINT('Ctrl Pts',(-40.1158000723182,-44.1801801717817,
-76.9063314571057));
#151617=CARTESIAN_POINT('Ctrl Pts',(-40.062010544316,-44.1857172779623,
-77.0120479770336));
#151618=CARTESIAN_POINT('Ctrl Pts',(-40.0069033106055,-44.1913900290666,
-77.1203542810132));
#151619=CARTESIAN_POINT('Ctrl Pts',(-39.9543498747492,-44.1970805363738,
-77.2295685571082));
#151620=CARTESIAN_POINT('Ctrl Pts',(-39.904167438306,-44.2028090487481,
-77.3396386298012));
#151621=CARTESIAN_POINT('Ctrl Pts',(-39.859605995182,-44.2078959037604,
-77.4373796250899));
#151622=CARTESIAN_POINT('Ctrl Pts',(-39.8169140795409,-44.213013530734,
-77.5357960364665));
#151623=CARTESIAN_POINT('Ctrl Pts',(-39.7759776294699,-44.2182010663734,
-77.6348705097609));
#151624=CARTESIAN_POINT('Ctrl Pts',(-39.7206873277629,-44.2252075461762,
-77.7686842017251));
#151625=CARTESIAN_POINT('Ctrl Pts',(-39.6686277251655,-44.2322979157729,
-77.9036835094696));
#151626=CARTESIAN_POINT('Ctrl Pts',(-39.6196506088544,-44.2394333017539,
-78.0397988921473));
#151627=CARTESIAN_POINT('Ctrl Pts',(-39.5698722791269,-44.2466854150436,
-78.1781409773952));
#151628=CARTESIAN_POINT('Ctrl Pts',(-39.5232774197431,-44.2539845156844,
-78.3176362948157));
#151629=CARTESIAN_POINT('Ctrl Pts',(-39.479736648919,-44.2613273210185,
-78.4582406896765));
#151630=CARTESIAN_POINT('Ctrl Pts',(-39.435371602894,-44.2688091338215,
-78.6015068820576));
#151631=CARTESIAN_POINT('Ctrl Pts',(-39.3941767593022,-44.2763369097495,
-78.745924967725));
#151632=CARTESIAN_POINT('Ctrl Pts',(-39.3560523315242,-44.2839376143512,
-78.8914720771512));
#151633=CARTESIAN_POINT('Ctrl Pts',(-39.3509935172703,-44.284946168578,
-78.9107850435271));
#151634=CARTESIAN_POINT('Ctrl Pts',(-39.3459888245001,-44.285956042194,
-78.9301179169555));
#151635=CARTESIAN_POINT('Ctrl Pts',(-39.3410380762978,-44.2869673285108,
-78.9494706682134));
#151636=CARTESIAN_POINT('Ctrl Pts',(-39.2980051492431,-44.2957576382831,
-79.1176887837713));
#151637=CARTESIAN_POINT('Ctrl Pts',(-39.2592198938221,-44.3046155600241,
-79.2867252680673));
#151638=CARTESIAN_POINT('Ctrl Pts',(-39.224550515281,-44.3134982487801,
-79.4564303829574));
#151639=CARTESIAN_POINT('Ctrl Pts',(-39.1889042723014,-44.3226312213062,
-79.6309172072047));
#151640=CARTESIAN_POINT('Ctrl Pts',(-39.1576084892969,-44.3317911714413,
-79.8061114784507));
#151641=CARTESIAN_POINT('Ctrl Pts',(-39.1305597703672,-44.3409620370165,
-79.9818724566913));
#151642=CARTESIAN_POINT('Ctrl Pts',(-39.1026629400711,-44.3504204546697,
-80.1631444125051));
#151643=CARTESIAN_POINT('Ctrl Pts',(-39.0792832454589,-44.3598914595052,
-80.3450199391458));
#151644=CARTESIAN_POINT('Ctrl Pts',(-39.0603574905697,-44.3693756778076,
-80.5273570717227));
#151645=CARTESIAN_POINT('Ctrl Pts',(-39.0412931899528,-44.3789293251993,
-80.7110290007639));
#151646=CARTESIAN_POINT('Ctrl Pts',(-39.0267483551842,-44.3884974622236,
-80.8951701896708));
#151647=CARTESIAN_POINT('Ctrl Pts',(-39.0167110904471,-44.3980830680851,
-81.0796353183193));
#151648=CARTESIAN_POINT('Ctrl Pts',(-39.0067015411556,-44.4076422056464,
-81.2635910917448));
#151649=CARTESIAN_POINT('Ctrl Pts',(-39.0011751817154,-44.4172196919994,
-81.4478698295068));
#151650=CARTESIAN_POINT('Ctrl Pts',(-39.0001681003861,-44.4268053025559,
-81.6323145412984));
#151651=CARTESIAN_POINT('Ctrl Pts',(-39.0000562265889,-44.4278701407374,
-81.6528039791229));
#151652=CARTESIAN_POINT('Ctrl Pts',(-39.0000001661476,-44.4289350571871,
-81.6732954448402));
#151653=CARTESIAN_POINT('Ctrl Pts',(-39.0000000003688,-44.43000002,-81.6937887068282));
#151654=CARTESIAN_POINT('Ctrl Pts',(-40.4124516249929,-44.1531545436406,
-76.3934867142621));
#151655=CARTESIAN_POINT('Ctrl Pts',(-39.9673804148565,-44.93000002,-76.1313366308109));
#151656=CARTESIAN_POINT('Ctrl Pts',(-40.7712064624936,-44.93000002,-76.6047958451324));
#151657=CARTESIAN_POINT('Ctrl Pts',(-43.3552388512871,-44.1657199195518,
-71.3808409460202));
#151658=CARTESIAN_POINT('Ctrl Pts',(-42.8619820924489,-44.9300000200589,
-71.2817568775718));
#151659=CARTESIAN_POINT('Ctrl Pts',(-43.7236852143189,-44.93000002,-71.5921585277583));
#151660=CARTESIAN_POINT('Ctrl Pts',(-46.2131449010667,-44.1767154324357,
-66.3184583453296));
#151661=CARTESIAN_POINT('Ctrl Pts',(-45.7723278216974,-44.9300000200823,
-66.2016926213901));
#151662=CARTESIAN_POINT('Ctrl Pts',(-46.5890843541627,-44.93000002,-66.5297716146547));
#151663=CARTESIAN_POINT('Ctrl Pts',(-49.0214378669496,-44.1865817238571,
-61.2273317382593));
#151664=CARTESIAN_POINT('Ctrl Pts',(-48.6588221091936,-44.93000002,-61.026863396898));
#151665=CARTESIAN_POINT('Ctrl Pts',(-49.4036629110189,-44.93000002,-61.4386408691297));
#151666=CARTESIAN_POINT('Origin',(-59.5,-45.43000002,-55.2499500000007));
#151667=CARTESIAN_POINT('',(-60.,-45.43000002,-174.34995));
#151668=CARTESIAN_POINT('Origin',(-59.5,-45.43000002,-174.34995));
#151669=CARTESIAN_POINT('',(-60.,-45.43000002,-58.24995));
#151670=CARTESIAN_POINT('Origin',(-57.,-45.43000002,-174.34995));
#151671=CARTESIAN_POINT('Origin',(-57.,-45.43000002,-174.34995));
#151672=CARTESIAN_POINT('Origin',(0.,-12.9675000200281,-60.64995));
#151673=CARTESIAN_POINT('Origin',(-42.5,-55.58000002,-60.64995));
#151674=CARTESIAN_POINT('Origin',(0.,-12.9675000200281,-179.64995));
#151675=CARTESIAN_POINT('Origin',(3.54807775957937E-14,-73.08000002,3.11172719585489E-30));
#151676=CARTESIAN_POINT('',(-41.5,-73.08000002,-174.34995));
#151677=CARTESIAN_POINT('Ctrl Pts',(-30.800186642726,28.4199999800001,-78.2835659239152));
#151678=CARTESIAN_POINT('Ctrl Pts',(-29.3719438459593,28.4199999800001,
-77.079545860612));
#151679=CARTESIAN_POINT('Ctrl Pts',(-28.2935777143944,29.6448500754942,
-76.1704746152117));
#151680=CARTESIAN_POINT('Ctrl Pts',(-29.4908802242649,28.4199999800001,
-79.8367023859018));
#151681=CARTESIAN_POINT('Ctrl Pts',(-28.1162846817441,28.4199999799895,
-78.6350614606686));
#151682=CARTESIAN_POINT('Ctrl Pts',(-27.0582328538907,29.5957479131388,
-77.7235993982802));
#151683=CARTESIAN_POINT('Ctrl Pts',(-28.1443442258615,28.41999998,-81.3659786124399));
#151684=CARTESIAN_POINT('Ctrl Pts',(-26.8231903788109,28.41999998,-80.171186708314));
#151685=CARTESIAN_POINT('Ctrl Pts',(-25.7920491676122,29.54547115812,-79.2528873037006));
#151686=CARTESIAN_POINT('Ctrl Pts',(-25.359343066053,28.41999998,-84.349696566808));
#151687=CARTESIAN_POINT('Ctrl Pts',(-24.151734271497,28.41999998,-83.168456079353));
#151688=CARTESIAN_POINT('Ctrl Pts',(-23.1839068120671,29.4434760286189,
-82.2366052581402));
#151689=CARTESIAN_POINT('Ctrl Pts',(-23.928985790681,28.41999998,-85.7957524739721));
#151690=CARTESIAN_POINT('Ctrl Pts',(-22.7816855628193,28.4199999799965,
-84.621550748069));
#151691=CARTESIAN_POINT('Ctrl Pts',(-21.8495491428221,29.3920399293098,
-83.6826429630518));
#151692=CARTESIAN_POINT('Ctrl Pts',(-22.4473146057945,28.41999998,-87.1798147710383));
#151693=CARTESIAN_POINT('Ctrl Pts',(-21.3602588054756,28.41999998,-86.0160960137185));
#151694=CARTESIAN_POINT('Ctrl Pts',(-20.4734286051771,29.3409536236015,
-85.0667234623348));
#151695=CARTESIAN_POINT('Ctrl Pts',(-39.6993756576748,28.41999998,-66.758245524204));
#151696=CARTESIAN_POINT('Ctrl Pts',(-37.9544308619569,28.41999998,-65.5068366539031));
#151697=CARTESIAN_POINT('Ctrl Pts',(-36.7529144574179,29.9771506489281,
-64.6451542155005));
#151698=CARTESIAN_POINT('Ctrl Pts',(-38.3090750828473,28.41999998,-68.6968587227942));
#151699=CARTESIAN_POINT('Ctrl Pts',(-36.6139893647491,28.41999998,-67.4471428080873));
#151700=CARTESIAN_POINT('Ctrl Pts',(-35.4221830133223,29.9261764058054,
-66.5837572422386));
#151701=CARTESIAN_POINT('Ctrl Pts',(-36.8898270007225,28.4199999800001,
-70.617650456175));
#151702=CARTESIAN_POINT('Ctrl Pts',(-35.2435893151229,28.41999998,-69.3754183593105));
#151703=CARTESIAN_POINT('Ctrl Pts',(-34.0676680572731,29.8734031042169,
-68.5045591474479));
#151704=CARTESIAN_POINT('Ctrl Pts',(-33.9748337796689,28.4199999800001,
-74.4122216515051));
#151705=CARTESIAN_POINT('Ctrl Pts',(-32.4319411374915,28.41999998,-73.1856180617498));
#151706=CARTESIAN_POINT('Ctrl Pts',(-31.2955902801573,29.7642394885798,
-72.2991303428252));
#151707=CARTESIAN_POINT('Ctrl Pts',(-32.4811021033977,28.41999998,-76.2833884926716));
#151708=CARTESIAN_POINT('Ctrl Pts',(-30.9935194672858,28.4199999799959,
-75.0646492888563));
#151709=CARTESIAN_POINT('Ctrl Pts',(-29.8799523105758,29.7079117212239,
-74.1702869851635));
#151710=CARTESIAN_POINT('Ctrl Pts',(-30.9453615210646,28.41999998,-78.1110740930249));
#151711=CARTESIAN_POINT('Ctrl Pts',(-29.5115669185301,28.41999998,-76.9063064032585));
#151712=CARTESIAN_POINT('Ctrl Pts',(-28.4305705461597,29.6502955521147,
-75.9979827843214));
#151713=CARTESIAN_POINT('Ctrl Pts',(-36.7055660855173,29.9753365749746,
-64.7141089388348));
#151714=CARTESIAN_POINT('Ctrl Pts',(-35.3900556592162,29.9249246093161,
-66.6293066030352));
#151715=CARTESIAN_POINT('Ctrl Pts',(-34.0512327947874,29.8727558883661,
-68.5270566307911));
#151716=CARTESIAN_POINT('Ctrl Pts',(-32.6816291687152,29.8188212963983,
-70.4018447451366));
#151717=CARTESIAN_POINT('Ctrl Pts',(-32.0393671155873,29.7935292037721,
-71.2810080596735));
#151718=CARTESIAN_POINT('Ctrl Pts',(-31.3907503317202,29.7678616196868,
-72.1545609864309));
#151719=CARTESIAN_POINT('Ctrl Pts',(-30.7353640256462,29.7418658638091,
-73.0207789414145));
#151720=CARTESIAN_POINT('Origin',(-42.,28.91999998,-171.14995));
#151721=CARTESIAN_POINT('Origin',(-45.4220505312374,35.8460962305468,-172.64995));
#151722=CARTESIAN_POINT('Origin',(-44.489435756687,35.9771666894179,-172.64995));
#151723=CARTESIAN_POINT('Origin',(-44.2110895547669,33.9966305519348,-172.64995));
#151724=CARTESIAN_POINT('Origin',(-45.5819760525891,35.4528826626933,-172.64995));
#151725=CARTESIAN_POINT('Origin',(0.,-12.9675000200281,-172.64995));
#151726=CARTESIAN_POINT('Origin',(-48.4203826827217,32.6144760325608,-172.64995));
#151727=CARTESIAN_POINT('Origin',(-46.9641305719631,31.2435895347386,-172.64995));
#151728=CARTESIAN_POINT('Origin',(-48.9446667094463,31.5219357366587,-172.64995));
#151729=CARTESIAN_POINT('Origin',(-51.6222122422086,12.4702093225365,-172.64995));
#151730=CARTESIAN_POINT('Ctrl Pts',(-50.4704930916386,27.85041342952,-177.84995));
#151731=CARTESIAN_POINT('Ctrl Pts',(-50.4704930916386,27.85041342952,-177.34995));
#151732=CARTESIAN_POINT('Ctrl Pts',(-50.9656271260094,27.91999998,-177.34995));
#151733=CARTESIAN_POINT('Ctrl Pts',(-50.4335962469534,28.1129481210447,
-177.849949999941));
#151734=CARTESIAN_POINT('Ctrl Pts',(-50.4520556784241,27.9816024412645,
-177.367861075731));
#151735=CARTESIAN_POINT('Ctrl Pts',(-50.9287302813235,28.0512673257631,
-177.34995));
#151736=CARTESIAN_POINT('Ctrl Pts',(-50.3971326466187,28.3724001188352,
-177.742176873059));
#151737=CARTESIAN_POINT('Ctrl Pts',(-50.4311035247778,28.1306847609584,
-177.32958965968));
#151738=CARTESIAN_POINT('Ctrl Pts',(-50.8922666809894,28.1809933246567,
-177.29606343653));
#151739=CARTESIAN_POINT('Ctrl Pts',(-50.3450987821552,28.7426403025778,
-177.371936689315));
#151740=CARTESIAN_POINT('Ctrl Pts',(-50.4002116209072,28.3504920783889,
-177.142957948487));
#151741=CARTESIAN_POINT('Ctrl Pts',(-50.840232816526,28.3661134165298,-177.110943344657));
#151742=CARTESIAN_POINT('Ctrl Pts',(-50.3299522569454,28.8504134294547,
-177.112484691526));
#151743=CARTESIAN_POINT('Ctrl Pts',(-50.3904429224034,28.4199999799438,
-176.997671841187));
#151744=CARTESIAN_POINT('Ctrl Pts',(-50.8250862913143,28.41999998,-176.981217345763));
#151745=CARTESIAN_POINT('Ctrl Pts',(-50.3299522569362,28.85041342952,-176.84995));
#151746=CARTESIAN_POINT('Ctrl Pts',(-50.3904429223989,28.41999998,-176.84995));
#151747=CARTESIAN_POINT('Ctrl Pts',(-50.825086291307,28.41999998,-176.84995));
#151748=CARTESIAN_POINT('Origin',(-50.9656271260094,27.91999998,-177.84995));
#151749=CARTESIAN_POINT('Origin',(-53.107614345321,12.6789689739766,-177.84995));
#151750=CARTESIAN_POINT('Origin',(-51.0358975433606,27.41999998,-177.84995));
#151751=CARTESIAN_POINT('',(-51.0717059287548,27.1652100787588,-177.34995));
#151752=CARTESIAN_POINT('Ctrl Pts',(-50.6813043436922,26.35041342952,-176.84995));
#151753=CARTESIAN_POINT('Ctrl Pts',(-50.6012541744525,26.9199999800001,
-176.84995));
#151754=CARTESIAN_POINT('Ctrl Pts',(-51.176438378063,26.91999998,-176.84995));
#151755=CARTESIAN_POINT('Ctrl Pts',(-50.681304343683,26.3504134295853,-177.112484691526));
#151756=CARTESIAN_POINT('Ctrl Pts',(-50.6012541744552,26.9199999799806,
-176.958917254526));
#151757=CARTESIAN_POINT('Ctrl Pts',(-51.1764383780557,26.91999998,-176.981217345763));
#151758=CARTESIAN_POINT('Ctrl Pts',(-50.6661578184733,26.4581865564618,
-177.371936689315));
#151759=CARTESIAN_POINT('Ctrl Pts',(-50.5965693573617,26.9533341856637,
-177.069891898465));
#151760=CARTESIAN_POINT('Ctrl Pts',(-51.161291852844,26.9738865434699,-177.110943344657));
#151761=CARTESIAN_POINT('Ctrl Pts',(-50.6141239540097,26.8284267402052,
-177.742176873059));
#151762=CARTESIAN_POINT('Ctrl Pts',(-50.5759178325036,27.1002774203984,
-177.257255781812));
#151763=CARTESIAN_POINT('Ctrl Pts',(-51.1092579883806,27.1590066353435,
-177.29606343653));
#151764=CARTESIAN_POINT('Ctrl Pts',(-50.5776603536751,27.0878787379949,
-177.849949999941));
#151765=CARTESIAN_POINT('Ctrl Pts',(-50.5600601550379,27.2131106584802,
-177.331204220089));
#151766=CARTESIAN_POINT('Ctrl Pts',(-51.0727943880466,27.2887326342368,
-177.34995));
#151767=CARTESIAN_POINT('Ctrl Pts',(-50.5407635089898,27.3504134295199,
-177.84995));
#151768=CARTESIAN_POINT('Ctrl Pts',(-50.5407635089898,27.35041342952,-177.34995));
#151769=CARTESIAN_POINT('Ctrl Pts',(-51.0358975433606,27.41999998,-177.34995));
#151770=CARTESIAN_POINT('Origin',(-51.6222122422086,12.4702093225365,-172.64995));
#151771=CARTESIAN_POINT('',(-49.6109861057109,26.78082687904,-171.64995));
#151772=CARTESIAN_POINT('Ctrl Pts',(-51.6159008944631,19.70041342952,-177.84995));
#151773=CARTESIAN_POINT('Ctrl Pts',(-51.6159008944631,19.70041342952,-177.34995));
#151774=CARTESIAN_POINT('Ctrl Pts',(-52.1110349288339,19.76999998,-177.34995));
#151775=CARTESIAN_POINT('Ctrl Pts',(-51.5790040497779,19.9629481210451,
-177.849949999941));
#151776=CARTESIAN_POINT('Ctrl Pts',(-51.5974634812487,19.8316024412644,
-177.367861075732));
#151777=CARTESIAN_POINT('Ctrl Pts',(-52.0741380841476,19.9012673257632,
-177.34995));
#151778=CARTESIAN_POINT('Ctrl Pts',(-51.5425404494433,20.2224001188348,
-177.742176873059));
#151779=CARTESIAN_POINT('Ctrl Pts',(-51.5765113276013,19.980684760958,-177.329589659683));
#151780=CARTESIAN_POINT('Ctrl Pts',(-52.0376744838139,20.0309933246565,
-177.29606343653));
#151781=CARTESIAN_POINT('Ctrl Pts',(-51.4905065849796,20.5926403025782,
-177.371936689315));
#151782=CARTESIAN_POINT('Ctrl Pts',(-51.5456194237325,20.2004920783894,
-177.142957948484));
#151783=CARTESIAN_POINT('Ctrl Pts',(-51.9856406193506,20.2161134165301,
-177.110943344657));
#151784=CARTESIAN_POINT('Ctrl Pts',(-51.4753600597699,20.7004134294547,
-177.112484691526));
#151785=CARTESIAN_POINT('Ctrl Pts',(-51.5358507252279,20.2699999799402,
-176.997671841189));
#151786=CARTESIAN_POINT('Ctrl Pts',(-51.9704940941388,20.26999998,-176.981217345763));
#151787=CARTESIAN_POINT('Ctrl Pts',(-51.4753600597607,20.70041342952,-176.84995));
#151788=CARTESIAN_POINT('Ctrl Pts',(-51.5358507252234,20.26999998,-176.84995));
#151789=CARTESIAN_POINT('Ctrl Pts',(-51.9704940941315,20.26999998,-176.84995));
#151790=CARTESIAN_POINT('Origin',(-52.1110349288339,19.76999998,-177.84995));
#151791=CARTESIAN_POINT('Origin',(-53.107614345321,12.6789689739766,-177.84995));
#151792=CARTESIAN_POINT('Origin',(-52.1813053461851,19.26999998,-177.84995));
#151793=CARTESIAN_POINT('',(-51.0717059287548,27.1652100787588,-177.34995));
#151794=CARTESIAN_POINT('Ctrl Pts',(-51.8267121465167,18.20041342952,-176.84995));
#151795=CARTESIAN_POINT('Ctrl Pts',(-51.746661977277,18.76999998,-176.84995));
#151796=CARTESIAN_POINT('Ctrl Pts',(-52.3218461808875,18.76999998,-176.84995));
#151797=CARTESIAN_POINT('Ctrl Pts',(-51.8267121465076,18.2004134295853,
-177.112484691526));
#151798=CARTESIAN_POINT('Ctrl Pts',(-51.7466619772798,18.7699999799806,
-176.958917254526));
#151799=CARTESIAN_POINT('Ctrl Pts',(-52.3218461808802,18.76999998,-176.981217345763));
#151800=CARTESIAN_POINT('Ctrl Pts',(-51.8115656212979,18.3081865564618,
-177.371936689315));
#151801=CARTESIAN_POINT('Ctrl Pts',(-51.7419771601862,18.8033341856637,
-177.069891898465));
#151802=CARTESIAN_POINT('Ctrl Pts',(-52.3066996556685,18.8238865434699,
-177.110943344657));
#151803=CARTESIAN_POINT('Ctrl Pts',(-51.7595317568342,18.6784267402051,
-177.742176873059));
#151804=CARTESIAN_POINT('Ctrl Pts',(-51.721325635328,18.9502774203983,-177.257255781811));
#151805=CARTESIAN_POINT('Ctrl Pts',(-52.2546657912052,19.0090066353435,
-177.29606343653));
#151806=CARTESIAN_POINT('Ctrl Pts',(-51.7230681564996,18.9378787379949,
-177.849949999941));
#151807=CARTESIAN_POINT('Ctrl Pts',(-51.7054679578625,19.0631106584802,
-177.331204220089));
#151808=CARTESIAN_POINT('Ctrl Pts',(-52.2182021908711,19.1387326342368,
-177.34995));
#151809=CARTESIAN_POINT('Ctrl Pts',(-51.6861713118143,19.20041342952,-177.84995));
#151810=CARTESIAN_POINT('Ctrl Pts',(-51.6861713118143,19.2004134295199,
-177.34995));
#151811=CARTESIAN_POINT('Ctrl Pts',(-52.1813053461851,19.26999998,-177.34995));
#151812=CARTESIAN_POINT('Origin',(-51.6222122422086,12.4702093225365,-172.64995));
#151813=CARTESIAN_POINT('',(-50.9867892914963,16.9914785469432,-171.64995));
#151814=CARTESIAN_POINT('Origin',(-50.9867892914963,16.9914785469432,-172.64995));
#151815=CARTESIAN_POINT('',(-50.7563939085354,18.6308268790399,-171.64995));
#151816=CARTESIAN_POINT('Ctrl Pts',(-52.1126146143195,13.5388501432916,
-171.391638125813));
#151817=CARTESIAN_POINT('Ctrl Pts',(-52.4864722882118,13.5059760932665,
-171.679515584751));
#151818=CARTESIAN_POINT('Ctrl Pts',(-52.5050296388285,13.3739336825608,
-172.133326251627));
#151819=CARTESIAN_POINT('Ctrl Pts',(-51.9336694513028,14.1125756396742,
-171.482621144035));
#151820=CARTESIAN_POINT('Ctrl Pts',(-52.3988291636435,14.129589328176,-171.781794156641));
#151821=CARTESIAN_POINT('Ctrl Pts',(-52.4188787332531,13.9869292276479,
-172.315208572937));
#151822=CARTESIAN_POINT('Ctrl Pts',(-51.7497860966453,14.6887611591208,
-171.543915907757));
#151823=CARTESIAN_POINT('Ctrl Pts',(-52.3125022740344,14.7438370647052,
-171.821280489149));
#151824=CARTESIAN_POINT('Ctrl Pts',(-52.3315472405275,14.6083250867988,
-172.437881815118));
#151825=CARTESIAN_POINT('Ctrl Pts',(-51.3741578990745,15.8404043177988,
-171.628003076365));
#151826=CARTESIAN_POINT('Ctrl Pts',(-52.1416679592957,15.9593863754288,
-171.81403941883));
#151827=CARTESIAN_POINT('Ctrl Pts',(-52.1554800333145,15.861108362107,-172.606056153125));
#151828=CARTESIAN_POINT('Ctrl Pts',(-51.1823572933404,16.4160730441958,
-171.64995));
#151829=CARTESIAN_POINT('Ctrl Pts',(-52.0557320324868,16.5708522670934,
-171.757498535929));
#151830=CARTESIAN_POINT('Ctrl Pts',(-52.0666747393889,16.4929908616926,
-172.649949997757));
#151831=CARTESIAN_POINT('Ctrl Pts',(-50.9867892914963,16.9914785469432,
-171.64995));
#151832=CARTESIAN_POINT('Ctrl Pts',(-51.9770573602378,17.1306516479032,
-171.64995));
#151833=CARTESIAN_POINT('Ctrl Pts',(-51.9770573602378,17.1306516479033,
-172.64995));
#151834=CARTESIAN_POINT('',(-52.1126146143195,13.5388501432916,-171.391638125813));
#151835=CARTESIAN_POINT('Origin',(-51.5147615700869,13.2347605816008,-172.133326251627));
#151836=CARTESIAN_POINT('Ctrl Pts',(-52.1126146143195,13.5388501432916,
-171.391638125813));
#151837=CARTESIAN_POINT('Ctrl Pts',(-51.9336694513434,14.1125756396757,
-171.482621144061));
#151838=CARTESIAN_POINT('Ctrl Pts',(-51.7497860966928,14.6887611591254,
-171.54391590778));
#151839=CARTESIAN_POINT('Ctrl Pts',(-51.3741578991343,15.8404043178081,
-171.628003076379));
#151840=CARTESIAN_POINT('Ctrl Pts',(-51.1823572934054,16.4160730442074,
-171.649950000008));
#151841=CARTESIAN_POINT('Ctrl Pts',(-50.9867892914963,16.9914785469432,
-171.64995));
#151842=CARTESIAN_POINT('Ctrl Pts',(-53.1963133798215,12.11999998,-176.84995));
#151843=CARTESIAN_POINT('Ctrl Pts',(-52.8383133487074,12.11999998,-176.84995));
#151844=CARTESIAN_POINT('Ctrl Pts',(-52.7229737572976,12.4589111791821,
-176.84995));
#151845=CARTESIAN_POINT('Ctrl Pts',(-53.1963133903003,12.11999998,-176.935788696125));
#151846=CARTESIAN_POINT('Ctrl Pts',(-52.8383133592413,12.1199999570555,
-176.956623424753));
#151847=CARTESIAN_POINT('Ctrl Pts',(-52.7229737689762,12.4589111448658,
-177.021627393075));
#151848=CARTESIAN_POINT('Ctrl Pts',(-53.2113113817619,12.0970286741326,
-177.021779308321));
#151849=CARTESIAN_POINT('Ctrl Pts',(-52.8537691267412,12.0857563897115,
-177.064307914426));
#151850=CARTESIAN_POINT('Ctrl Pts',(-52.7396382131267,12.4078638336875,
-177.193608615338));
#151851=CARTESIAN_POINT('Ctrl Pts',(-53.2731270360347,12.0145014233151,
-177.168462633103));
#151852=CARTESIAN_POINT('Ctrl Pts',(-52.9137267746853,11.9605670475505,
-177.241607460489));
#151853=CARTESIAN_POINT('Ctrl Pts',(-52.8083222549725,12.2244699412272,
-177.486975267512));
#151854=CARTESIAN_POINT('Ctrl Pts',(-53.3209180569567,11.9546120038032,
-177.230014853822));
#151855=CARTESIAN_POINT('Ctrl Pts',(-52.9598970865314,11.8669832265648,
-177.312681927597));
#151856=CARTESIAN_POINT('Ctrl Pts',(-52.8614762873877,12.0912699189313,
-177.610143591528));
#151857=CARTESIAN_POINT('Ctrl Pts',(-53.3846587239315,11.8868850448361,
-177.272764808359));
#151858=CARTESIAN_POINT('Ctrl Pts',(-53.0160258826804,11.7628399725939,
-177.351063336446));
#151859=CARTESIAN_POINT('Ctrl Pts',(-52.9322463618642,11.9408779899289,
-177.695579616717));
#151860=CARTESIAN_POINT('Origin',(-53.3846587239314,12.1537701096722,-177.695579616717));
#151861=CARTESIAN_POINT('Ctrl Pts',(-52.5050296388285,13.3739336825608,
-172.133326251627));
#151862=CARTESIAN_POINT('Ctrl Pts',(-52.4864722882118,13.5059760932666,
-171.679515584751));
#151863=CARTESIAN_POINT('Ctrl Pts',(-52.1126146143195,13.5388501432916,
-171.391638125813));
#151864=CARTESIAN_POINT('Ctrl Pts',(-52.5511257748791,13.045942631788,-172.016544094259));
#151865=CARTESIAN_POINT('Ctrl Pts',(-52.5259488232545,13.1630178119759,
-171.621133646225));
#151866=CARTESIAN_POINT('Ctrl Pts',(-52.2275734081837,13.1702746923549,
-171.333188379966));
#151867=CARTESIAN_POINT('Ctrl Pts',(-52.6287970696452,12.7242148673197,
-171.90506362857));
#151868=CARTESIAN_POINT('Ctrl Pts',(-52.6036316644729,12.8055197818763,
-171.550813695775));
#151869=CARTESIAN_POINT('Ctrl Pts',(-52.3625569744519,12.7995634785289,
-171.277518845311));
#151870=CARTESIAN_POINT('Ctrl Pts',(-52.7423614633688,12.4030287528935,
-171.844601961512));
#151871=CARTESIAN_POINT('Ctrl Pts',(-52.7259743335333,12.4493753091149,
-171.512222020089));
#151872=CARTESIAN_POINT('Ctrl Pts',(-52.521634376552,12.4186874453849,-171.247275980756));
#151873=CARTESIAN_POINT('Ctrl Pts',(-52.5103993792155,12.4456688476555,
-171.249463186897));
#151874=CARTESIAN_POINT('Ctrl Pts',(-52.3561903484674,12.8170807700125,
-171.280152290009));
#151875=CARTESIAN_POINT('Ctrl Pts',(-52.2248583846995,13.1789834261216,
-171.33457063385));
#151876=CARTESIAN_POINT('Ctrl Pts',(-52.1126146143195,13.5388501432916,
-171.391638125813));
#151877=CARTESIAN_POINT('Ctrl Pts',(-53.3764151395101,11.8956579446144,
-177.267099525666));
#151878=CARTESIAN_POINT('Ctrl Pts',(-53.0100887119116,11.775605096064,-177.346426173794));
#151879=CARTESIAN_POINT('Ctrl Pts',(-52.9240620597106,11.958262205024,-177.68425748122));
#151880=CARTESIAN_POINT('Ctrl Pts',(-53.456953595738,11.8101639377045,-177.323569657212));
#151881=CARTESIAN_POINT('Ctrl Pts',(-53.0700075125763,11.6468244366821,
-177.3949635665));
#151882=CARTESIAN_POINT('Ctrl Pts',(-53.0038949723879,11.7887688205011,
-177.797166892916));
#151883=CARTESIAN_POINT('Ctrl Pts',(-53.5494992446435,11.7107497255641,
-177.351908350358));
#151884=CARTESIAN_POINT('Ctrl Pts',(-53.1326802282722,11.5106994843395,
-177.38870977272));
#151885=CARTESIAN_POINT('Ctrl Pts',(-53.0956839028775,11.5915634526764,
-177.853871009894));
#151886=CARTESIAN_POINT('Ctrl Pts',(-53.6420451768198,11.6097057706468,
-177.349844870837));
#151887=CARTESIAN_POINT('Ctrl Pts',(-53.1835178900119,11.3997623969134,
-177.345484998328));
#151888=CARTESIAN_POINT('Ctrl Pts',(-53.1874365908317,11.3912058852591,
-177.849739369046));
#151889=CARTESIAN_POINT('Origin',(-53.6325912458891,11.61999998,-177.84995));
#151890=CARTESIAN_POINT('Origin',(0.,-12.9675000200281,-177.84995));
#151891=CARTESIAN_POINT('Origin',(-53.8590042959267,11.11999998,-177.84995));
#151892=CARTESIAN_POINT('Origin',(0.,-12.9675000200281,-177.34995));
#151893=CARTESIAN_POINT('Ctrl Pts',(-53.8590042959257,11.1199999800011,
-177.34995));
#151894=CARTESIAN_POINT('Ctrl Pts',(-53.4025720561301,10.9158686240688,
-177.34995));
#151895=CARTESIAN_POINT('Ctrl Pts',(-53.4025720561297,10.9158686240697,
-177.84995));
#151896=CARTESIAN_POINT('Ctrl Pts',(-53.9152095126149,11.0571633006792,
-177.34995));
#151897=CARTESIAN_POINT('Ctrl Pts',(-53.4357429270681,10.8416994438452,
-177.323612898224));
#151898=CARTESIAN_POINT('Ctrl Pts',(-53.4583000366404,10.7912623535259,
-177.849949984912));
#151899=CARTESIAN_POINT('Ctrl Pts',(-53.9700011606116,10.9953079956486,
-177.338340413074));
#151900=CARTESIAN_POINT('Ctrl Pts',(-53.4634087021834,10.7796461652398,
-177.282275394088));
#151901=CARTESIAN_POINT('Ctrl Pts',(-53.5126282698489,10.6685980808388,
-177.826730821509));
#151902=CARTESIAN_POINT('Ctrl Pts',(-54.0742219292009,10.8766241714759,
-177.291358543608));
#151903=CARTESIAN_POINT('Ctrl Pts',(-53.5073796187504,10.6816635307577,
-177.18321412648));
#151904=CARTESIAN_POINT('Ctrl Pts',(-53.6159658107279,10.4332420187126,
-177.732767091856));
#151905=CARTESIAN_POINT('Ctrl Pts',(-54.1215658763003,10.8221729031368,
-177.256908861057));
#151906=CARTESIAN_POINT('Ctrl Pts',(-53.5219518286219,10.649686808137,-177.127170956772));
#151907=CARTESIAN_POINT('Ctrl Pts',(-53.6629085389549,10.3252623899094,
-177.663867719202));
#151908=CARTESIAN_POINT('Ctrl Pts',(-54.2036611796727,10.7271494012897,
-177.166153898004));
#151909=CARTESIAN_POINT('Ctrl Pts',(-53.5394251697822,10.6131024574854,
-177.020421798311));
#151910=CARTESIAN_POINT('Ctrl Pts',(-53.7443081182388,10.1368259480206,
-177.482357798918));
#151911=CARTESIAN_POINT('Ctrl Pts',(-54.2369068974943,10.6883272976786,
-177.111149481396));
#151912=CARTESIAN_POINT('Ctrl Pts',(-53.5413185515592,10.6107526879388,
-176.973405437982));
#151913=CARTESIAN_POINT('Ctrl Pts',(-53.7772720937282,10.0598397490546,
-177.372348961349));
#151914=CARTESIAN_POINT('Ctrl Pts',(-54.282897054019,10.6344777440414,-176.987189324297));
#151915=CARTESIAN_POINT('Ctrl Pts',(-53.5410688387025,10.6146700040362,
-176.899444869037));
#151916=CARTESIAN_POINT('Ctrl Pts',(-53.8228725022638,9.95305333910152,
-177.124428650036));
#151917=CARTESIAN_POINT('Ctrl Pts',(-54.2951871094022,10.61999998,-176.919796282647));
#151918=CARTESIAN_POINT('Ctrl Pts',(-53.5392499462662,10.6199999783344,
-176.8744703999));
#151919=CARTESIAN_POINT('Ctrl Pts',(-53.8350584050868,9.92434321115133,
-176.989642564215));
#151920=CARTESIAN_POINT('Ctrl Pts',(-54.2951871140408,10.61999998,-176.84995));
#151921=CARTESIAN_POINT('Ctrl Pts',(-53.5392499457278,10.61999998,-176.84995));
#151922=CARTESIAN_POINT('Ctrl Pts',(-53.8350584096845,9.92434320033874,
-176.84995));
#151923=CARTESIAN_POINT('Origin',(0.,-12.9675000200281,-171.871644662643));
#151924=CARTESIAN_POINT('Origin',(0.,-12.9675000200281,-171.449026400902));
#151925=CARTESIAN_POINT('Ctrl Pts',(-56.3647818444065,3.96926413137802,
-176.823236869191));
#151926=CARTESIAN_POINT('Ctrl Pts',(-55.9959340274937,3.96888359130611,
-176.817122088667));
#151927=CARTESIAN_POINT('Ctrl Pts',(-55.8870828276465,4.32076528003782,
-176.796522687734));
#151928=CARTESIAN_POINT('Ctrl Pts',(-56.3621914406401,3.97343752384164,
-176.898676428268));
#151929=CARTESIAN_POINT('Ctrl Pts',(-55.9940683565767,3.97509020000321,
-176.909738482033));
#151930=CARTESIAN_POINT('Ctrl Pts',(-55.8845144046578,4.32904163576369,
-176.94740476072));
#151931=CARTESIAN_POINT('Ctrl Pts',(-56.3706829146393,3.95977275889743,
-176.975561795614));
#151932=CARTESIAN_POINT('Ctrl Pts',(-56.0002448138047,3.95455861174371,
-177.005108600189));
#151933=CARTESIAN_POINT('Ctrl Pts',(-55.8929338246199,4.30194256512436,
-177.101178646029));
#151934=CARTESIAN_POINT('Ctrl Pts',(-56.4046489137991,3.9046063492797,-177.105916142434));
#151935=CARTESIAN_POINT('Ctrl Pts',(-56.0238513574191,3.87557171406294,
-177.159000770829));
#151936=CARTESIAN_POINT('Ctrl Pts',(-55.9266115295683,4.19254080857125,
-177.361891255001));
#151937=CARTESIAN_POINT('Ctrl Pts',(-56.4280565527281,3.86646604036506,
-177.161475370894));
#151938=CARTESIAN_POINT('Ctrl Pts',(-56.0401276640061,3.82096319617762,
-177.221565174049));
#151939=CARTESIAN_POINT('Ctrl Pts',(-55.9498205047936,4.11690393979646,
-177.473010794577));
#151940=CARTESIAN_POINT('Ctrl Pts',(-56.4844776989127,3.77353560122462,
-177.252565826982));
#151941=CARTESIAN_POINT('Ctrl Pts',(-56.0775874017679,3.6944039842704,-177.314195789872));
#151942=CARTESIAN_POINT('Ctrl Pts',(-56.0057627129126,3.93261288273155,
-177.655191732052));
#151943=CARTESIAN_POINT('Ctrl Pts',(-56.5179433552169,3.71797632916513,
-177.288846704038));
#151944=CARTESIAN_POINT('Ctrl Pts',(-56.0992917633819,3.62064831431513,
-177.344699390005));
#151945=CARTESIAN_POINT('Ctrl Pts',(-56.0389442880078,3.82243329271981,
-177.727752411286));
#151946=CARTESIAN_POINT('Ctrl Pts',(-56.5933952273326,3.59109438829976,
-177.340494166071));
#151947=CARTESIAN_POINT('Ctrl Pts',(-56.1453765257444,3.46307334244855,
-177.373495736382));
#151948=CARTESIAN_POINT('Ctrl Pts',(-56.1137555688082,3.57081571968701,
-177.8310434768));
#151949=CARTESIAN_POINT('Ctrl Pts',(-56.6369998249196,3.51682557412558,
-177.353132613067));
#151950=CARTESIAN_POINT('Ctrl Pts',(-56.1703907360266,3.37693361833867,
-177.366019145535));
#151951=CARTESIAN_POINT('Ctrl Pts',(-56.1569874820333,3.42354388148881,
-177.856317178204));
#151952=CARTESIAN_POINT('Ctrl Pts',(-56.6789110795914,3.44432084323002,
-177.349268724474));
#151953=CARTESIAN_POINT('Ctrl Pts',(-56.1915749927218,3.30386891072904,
-177.341992013576));
#151954=CARTESIAN_POINT('Ctrl Pts',(-56.1985461365938,3.27975188714757,
-177.848586370252));
#151955=CARTESIAN_POINT('Origin',(-56.6639973329545,3.46999998000001,-177.84995));
#151956=CARTESIAN_POINT('Origin',(0.,-12.9675000200281,-177.84995));
#151957=CARTESIAN_POINT('',(-56.8066553649227,2.96999998000001,-177.34995));
#151958=CARTESIAN_POINT('Origin',(-56.8066553649227,2.96999998000001,-177.84995));
#151959=CARTESIAN_POINT('Origin',(0.,-12.9675000200281,-177.34995));
#151960=CARTESIAN_POINT('Ctrl Pts',(-56.8066553649227,2.96999998000003,
-177.34995));
#151961=CARTESIAN_POINT('Ctrl Pts',(-56.3252430313216,2.83493642067775,
-177.34995));
#151962=CARTESIAN_POINT('Ctrl Pts',(-56.3252430313217,2.83493642067777,
-177.84995));
#151963=CARTESIAN_POINT('Ctrl Pts',(-56.8796685247676,2.83987814625872,
-177.34995));
#151964=CARTESIAN_POINT('Ctrl Pts',(-56.3657038976309,2.69072016585578,
-177.313059794074));
#151965=CARTESIAN_POINT('Ctrl Pts',(-56.3976379760506,2.57689628418379,
-177.849949962148));
#151966=CARTESIAN_POINT('Ctrl Pts',(-56.9495585329053,2.71140496526165,
-177.298153784266));
#151967=CARTESIAN_POINT('Ctrl Pts',(-56.393446522619,2.59195606221812,-177.219869815671));
#151968=CARTESIAN_POINT('Ctrl Pts',(-56.4669147992933,2.32220551629932,
-177.746434148089));
#151969=CARTESIAN_POINT('Ctrl Pts',(-57.,2.61702308584988,-177.204078948543));
#151970=CARTESIAN_POINT('Ctrl Pts',(-56.409292540301,2.5378414548249,-177.125154911669));
#151971=CARTESIAN_POINT('Ctrl Pts',(-56.5169491525424,2.13496529160036,
-177.558207897086));
#151972=CARTESIAN_POINT('Origin',(-57.,2.26404619169977,-177.558207897086));
#151973=CARTESIAN_POINT('Ctrl Pts',(-57.,2.61702308584989,-177.204078948543));
#151974=CARTESIAN_POINT('Ctrl Pts',(-56.9495585329053,2.71140496526165,
-177.298153784266));
#151975=CARTESIAN_POINT('Ctrl Pts',(-56.8796685247676,2.83987814625872,
-177.34995));
#151976=CARTESIAN_POINT('Ctrl Pts',(-56.8066553649227,2.96999998000001,
-177.34995));
#151977=CARTESIAN_POINT('Ctrl Pts',(-57.,2.61702308584989,-177.204078948543));
#151978=CARTESIAN_POINT('Ctrl Pts',(-56.409292540301,2.53784145482491,-177.125154911669));
#151979=CARTESIAN_POINT('Ctrl Pts',(-56.5169491525423,2.13496529160038,
-177.558207897086));
#151980=CARTESIAN_POINT('Ctrl Pts',(-57.043897408659,2.52469464001198,-177.112050866152));
#151981=CARTESIAN_POINT('Ctrl Pts',(-56.4267635932219,2.4778594556634,-177.032282865396));
#151982=CARTESIAN_POINT('Ctrl Pts',(-56.5659347005564,1.95164994081541,
-177.37392715461));
#151983=CARTESIAN_POINT('Ctrl Pts',(-57.0736014896981,2.46999998000001,
-176.982739539051));
#151984=CARTESIAN_POINT('Ctrl Pts',(-56.4314543935154,2.46472012384626,
-176.935564924353));
#151985=CARTESIAN_POINT('Ctrl Pts',(-56.5940537017931,1.84341101199667,
-177.116606872607));
#151986=CARTESIAN_POINT('Ctrl Pts',(-57.077763566464,2.46999998000001,-176.848740272858));
#151987=CARTESIAN_POINT('Ctrl Pts',(-56.430072632376,2.46999998,-176.848740272858));
#151988=CARTESIAN_POINT('Ctrl Pts',(-56.5940537057312,1.84341099694892,
-176.848740272858));
#151989=CARTESIAN_POINT('Origin',(0.,-12.9675000200281,-171.871644662643));
#151990=CARTESIAN_POINT('Origin',(0.,-12.9675000200281,-171.449026400902));
#151991=CARTESIAN_POINT('Ctrl Pts',(-58.2644174754153,-4.18000001999999,
-176.647241333324));
#151992=CARTESIAN_POINT('Ctrl Pts',(-57.8378063278744,-4.18000001999999,
-176.647241333323));
#151993=CARTESIAN_POINT('Ctrl Pts',(-57.7706512256236,-3.75870764711888,
-176.647241333324));
#151994=CARTESIAN_POINT('Ctrl Pts',(-58.2063099446428,-4.18000001999999,
-176.814456128226));
#151995=CARTESIAN_POINT('Ctrl Pts',(-57.8302553406283,-4.13262948514164,
-176.819875027464));
#151996=CARTESIAN_POINT('Ctrl Pts',(-57.7706512234859,-3.7587076337082,
-176.91349018761));
#151997=CARTESIAN_POINT('Ctrl Pts',(-58.1740867503666,-4.22134717274183,
-176.965019674666));
#151998=CARTESIAN_POINT('Ctrl Pts',(-57.8337414661451,-4.15737968364172,
-177.016619266697));
#151999=CARTESIAN_POINT('Ctrl Pts',(-57.7839302828914,-3.84070116554495,
-177.179630564281));
#152000=CARTESIAN_POINT('Ctrl Pts',(-58.1596733704946,-4.39698767568444,
-177.184652644663));
#152001=CARTESIAN_POINT('Ctrl Pts',(-57.8638647108401,-4.36170500598442,
-177.299461859543));
#152002=CARTESIAN_POINT('Ctrl Pts',(-57.8378689508709,-4.18900518947036,
-177.581280960616));
#152003=CARTESIAN_POINT('Ctrl Pts',(-58.1766173277935,-4.52496538336098,
-177.243973427637));
#152004=CARTESIAN_POINT('Ctrl Pts',(-57.8889218715383,-4.53236075126195,
-177.380206838676));
#152005=CARTESIAN_POINT('Ctrl Pts',(-57.8761547096863,-4.44264996470081,
-177.698192218067));
#152006=CARTESIAN_POINT('Ctrl Pts',(-58.2078173720827,-4.6591771252004,
-177.236349008085));
#152007=CARTESIAN_POINT('Ctrl Pts',(-57.9133432880527,-4.70343927025971,
-177.368016692624));
#152008=CARTESIAN_POINT('Ctrl Pts',(-57.914127722791,-4.70894021166886,
-177.693561815623));
#152009=CARTESIAN_POINT('Origin',(-58.4091202674301,-4.63835423039998,-177.693561815623));
#152010=CARTESIAN_POINT('Ctrl Pts',(-57.9826110754301,-5.20432973493151,
-177.68524973918));
#152011=CARTESIAN_POINT('Ctrl Pts',(-57.9819403936438,-5.19932045653815,
-177.367360689003));
#152012=CARTESIAN_POINT('Ctrl Pts',(-58.2670190981741,-5.15898893607704,
-177.232518219478));
#152013=CARTESIAN_POINT('Ctrl Pts',(-57.9604889110946,-5.0391007365056,
-177.687922734557));
#152014=CARTESIAN_POINT('Ctrl Pts',(-57.9597329881765,-5.03356356782781,
-177.367569378206));
#152015=CARTESIAN_POINT('Ctrl Pts',(-58.2478951756903,-4.99233199195458,
-177.233703806904));
#152016=CARTESIAN_POINT('Ctrl Pts',(-57.9376611104107,-4.87397087657654,
-177.690692163097));
#152017=CARTESIAN_POINT('Ctrl Pts',(-57.936860143276,-4.86824210971035,
-177.367787815378));
#152018=CARTESIAN_POINT('Ctrl Pts',(-58.2281612527228,-4.82572915883349,
-177.234977247299));
#152019=CARTESIAN_POINT('Ctrl Pts',(-57.9141277227909,-4.70894021166782,
-177.693561815623));
#152020=CARTESIAN_POINT('Ctrl Pts',(-57.9133432880526,-4.70343927025946,
-177.368016692624));
#152021=CARTESIAN_POINT('Ctrl Pts',(-58.207817372083,-4.65917712520044,
-177.236349008084));
#152022=CARTESIAN_POINT('Origin',(-58.4781889478697,-5.13797785215286,-177.68524973918));
#152023=CARTESIAN_POINT('Origin',(8.72896884135842,-12.9196247869585,-187.477148715837));
#152024=CARTESIAN_POINT('Ctrl Pts',(-58.250127507179,-5.06968783385529,
-177.226728198848));
#152025=CARTESIAN_POINT('Ctrl Pts',(-57.9662855289687,-5.08328249329522,
-177.360292478972));
#152026=CARTESIAN_POINT('Ctrl Pts',(-57.9585760313018,-5.02718307168404,
-177.669186903823));
#152027=CARTESIAN_POINT('Ctrl Pts',(-58.267275359726,-5.17241111264655,
-177.245973878017));
#152028=CARTESIAN_POINT('Ctrl Pts',(-57.984552359372,-5.21769695918899,
-177.385890323218));
#152029=CARTESIAN_POINT('Ctrl Pts',(-57.986638158118,-5.23110018896161,
-177.710636685369));
#152030=CARTESIAN_POINT('Ctrl Pts',(-58.2949532186373,-5.28245544896484,
-177.219964260301));
#152031=CARTESIAN_POINT('Ctrl Pts',(-58.0035760854518,-5.36150223388792,
-177.347296528341));
#152032=CARTESIAN_POINT('Ctrl Pts',(-58.0151803280234,-5.44931573531903,
-177.670490460791));
#152033=CARTESIAN_POINT('Ctrl Pts',(-58.3517502627772,-5.44113379045571,
-177.116208062583));
#152034=CARTESIAN_POINT('Ctrl Pts',(-58.0288335651954,-5.55441367376,-177.210693506391));
#152035=CARTESIAN_POINT('Ctrl Pts',(-58.0549536715593,-5.76404075854571,
-177.499799765465));
#152036=CARTESIAN_POINT('Ctrl Pts',(-58.3785597083963,-5.49933671141672,
-177.055067358297));
#152037=CARTESIAN_POINT('Ctrl Pts',(-58.0374810804384,-5.6211131042901,
-177.130197562223));
#152038=CARTESIAN_POINT('Ctrl Pts',(-58.0690822624578,-5.87947228735883,
-177.397969070777));
#152039=CARTESIAN_POINT('Ctrl Pts',(-58.4367803399072,-5.59139596273917,
-176.908361465886));
#152040=CARTESIAN_POINT('Ctrl Pts',(-58.049441388405,-5.71232355105524,
-176.947605119838));
#152041=CARTESIAN_POINT('Ctrl Pts',(-58.0910734645313,-6.0620213485957,
-177.158256835825));
#152042=CARTESIAN_POINT('Ctrl Pts',(-58.4681676012925,-5.62547497424865,
-176.823186408681));
#152043=CARTESIAN_POINT('Ctrl Pts',(-58.0527112965688,-5.73640373079481,
-176.8437834687));
#152044=CARTESIAN_POINT('Ctrl Pts',(-58.0990088104622,-6.12958052854701,
-177.021022282342));
#152045=CARTESIAN_POINT('Ctrl Pts',(-58.549399705635,-5.67884101979599,
-176.597416893918));
#152046=CARTESIAN_POINT('Ctrl Pts',(-58.0542110412498,-5.74228297193106,
-176.586646322505));
#152047=CARTESIAN_POINT('Ctrl Pts',(-58.1113726902199,-6.23532200623141,
-176.671138683684));
#152048=CARTESIAN_POINT('Ctrl Pts',(-58.5996921096123,-5.68603239881912,
-176.453921402976));
#152049=CARTESIAN_POINT('Ctrl Pts',(-58.0492158141453,-5.69790226417634,
-176.435349477229));
#152050=CARTESIAN_POINT('Ctrl Pts',(-58.1129608923341,-6.24950165634564,
-176.458921147922));
#152051=CARTESIAN_POINT('Ctrl Pts',(-58.6547670071737,-5.67538447778071,
-176.294472036962));
#152052=CARTESIAN_POINT('Ctrl Pts',(-58.0397058063333,-5.61759270411258,
-176.307417995075));
#152053=CARTESIAN_POINT('Ctrl Pts',(-58.1105363664048,-6.22828871330273,
-176.243722845542));
#152054=CARTESIAN_POINT('Origin',(0.,-12.9675000200281,-171.871644662643));
#152055=CARTESIAN_POINT('Origin',(0.,-12.9675000200281,-171.449026400902));
#152056=CARTESIAN_POINT('Ctrl Pts',(-58.9890336736409,-12.33000002,-176.26629097911));
#152057=CARTESIAN_POINT('Ctrl Pts',(-58.4985823439911,-12.33000002,-176.26629097911));
#152058=CARTESIAN_POINT('Ctrl Pts',(-58.48912660861,-11.8396398505087,-176.26629097911));
#152059=CARTESIAN_POINT('Ctrl Pts',(-58.9511729872876,-12.33000002,-176.394565470062));
#152060=CARTESIAN_POINT('Ctrl Pts',(-58.4978924302213,-12.2942221356206,
-176.390394119799));
#152061=CARTESIAN_POINT('Ctrl Pts',(-58.4891266082067,-11.8396398295935,
-176.423373313634));
#152062=CARTESIAN_POINT('Ctrl Pts',(-58.9148079297158,-12.3367286443605,
-176.512401023853));
#152063=CARTESIAN_POINT('Ctrl Pts',(-58.4973632374244,-12.2720420811237,
-176.51680491203));
#152064=CARTESIAN_POINT('Ctrl Pts',(-58.4893923301638,-11.8529830432079,
-176.578231191384));
#152065=CARTESIAN_POINT('Ctrl Pts',(-58.8482938287677,-12.3711206280572,
-176.731313674606));
#152066=CARTESIAN_POINT('Ctrl Pts',(-58.4968786243544,-12.2700692006727,
-176.761217862814));
#152067=CARTESIAN_POINT('Ctrl Pts',(-58.4906521273108,-11.9211841187055,
-176.880933630382));
#152068=CARTESIAN_POINT('Ctrl Pts',(-58.817725908538,-12.3995214017445,
-176.833790628028));
#152069=CARTESIAN_POINT('Ctrl Pts',(-58.4969059340918,-12.2890138650664,
-176.883349034336));
#152070=CARTESIAN_POINT('Ctrl Pts',(-58.4916809553489,-11.9775042760042,
-177.031063990607));
#152071=CARTESIAN_POINT('Ctrl Pts',(-58.7801197877863,-12.4620381958002,
-176.965157505607));
#152072=CARTESIAN_POINT('Ctrl Pts',(-58.4973396692349,-12.3546251483512,
-177.045101981496));
#152073=CARTESIAN_POINT('Ctrl Pts',(-58.4936040475389,-12.1014782716709,
-177.230049861356));
#152074=CARTESIAN_POINT('Ctrl Pts',(-58.7686983660461,-12.486608549538,
-177.006030037118));
#152075=CARTESIAN_POINT('Ctrl Pts',(-58.4975444264886,-12.3825831770725,
-177.096147908481));
#152076=CARTESIAN_POINT('Ctrl Pts',(-58.494315776837,-12.1502025268642,
-177.293200512009));
#152077=CARTESIAN_POINT('Ctrl Pts',(-58.7491768361659,-12.5414135007217,
-177.077379300711));
#152078=CARTESIAN_POINT('Ctrl Pts',(-58.4980148214299,-12.4487602363349,
-177.186076538859));
#152079=CARTESIAN_POINT('Ctrl Pts',(-58.4957333150688,-12.2588835334819,
-177.404811094274));
#152080=CARTESIAN_POINT('Ctrl Pts',(-58.7409598721377,-12.5716812769085,
-177.108237839695));
#152081=CARTESIAN_POINT('Ctrl Pts',(-58.4982801309887,-12.4869468894055,
-177.22572537075));
#152082=CARTESIAN_POINT('Ctrl Pts',(-58.4964422014533,-12.3189060674576,
-177.453832155185));
#152083=CARTESIAN_POINT('Ctrl Pts',(-58.7207402303504,-12.6723026604245,
-177.185595547246));
#152084=CARTESIAN_POINT('Ctrl Pts',(-58.4990784570061,-12.6167275534409,
-177.325053017822));
#152085=CARTESIAN_POINT('Ctrl Pts',(-58.4984277184057,-12.5184434004461,
-177.577650852379));
#152086=CARTESIAN_POINT('Ctrl Pts',(-58.71386124121,-12.7496539972645,-177.213921724807));
#152087=CARTESIAN_POINT('Ctrl Pts',(-58.499584494838,-12.7220101607261,
-177.363144865607));
#152088=CARTESIAN_POINT('Ctrl Pts',(-58.4994668010734,-12.6718351617761,
-177.62421726441));
#152089=CARTESIAN_POINT('Ctrl Pts',(-58.7141461350374,-12.8294402383603,
-177.213832217126));
#152090=CARTESIAN_POINT('Ctrl Pts',(-58.4998383709333,-12.8299842764724,
-177.363039831107));
#152091=CARTESIAN_POINT('Ctrl Pts',(-58.4998385375645,-12.8300551987826,
-177.624173936067));
#152092=CARTESIAN_POINT('Origin',(-58.9998371575436,-12.8288804567203,-177.624173936068));
#152093=CARTESIAN_POINT('Ctrl Pts',(-58.4988777713114,-13.3298527448209,
-177.624285947696));
#152094=CARTESIAN_POINT('Ctrl Pts',(-58.4988766126948,-13.3300397939931,
-177.363046991769));
#152095=CARTESIAN_POINT('Ctrl Pts',(-58.7133155825256,-13.3314748983275,
-177.213850156091));
#152096=CARTESIAN_POINT('Ctrl Pts',(-58.4999097084608,-13.1632549492482,
-177.624165638205));
#152097=CARTESIAN_POINT('Ctrl Pts',(-58.4999095201947,-13.1633713364571,
-177.363039299942));
#152098=CARTESIAN_POINT('Ctrl Pts',(-58.7142076600563,-13.1641303210821,
-177.213830854253));
#152099=CARTESIAN_POINT('Ctrl Pts',(-58.500229964035,-12.996655767065,-177.624128301462));
#152100=CARTESIAN_POINT('Ctrl Pts',(-58.5002301876544,-12.9966649765953,
-177.363036914652));
#152101=CARTESIAN_POINT('Ctrl Pts',(-58.7144845107404,-12.9967863561848,
-177.213824921703));
#152102=CARTESIAN_POINT('Ctrl Pts',(-58.4998385375645,-12.8300551987823,
-177.624173936067));
#152103=CARTESIAN_POINT('Ctrl Pts',(-58.4998383709332,-12.8299842764725,
-177.363039831106));
#152104=CARTESIAN_POINT('Ctrl Pts',(-58.7141461350386,-12.8294402383605,
-177.213832217124));
#152105=CARTESIAN_POINT('Origin',(-58.9988681796133,-13.3329497766555,-177.624285947696));
#152106=CARTESIAN_POINT('Origin',(9.53286718169884,-12.9674995361125,-178.689058801762));
#152107=CARTESIAN_POINT('Ctrl Pts',(-58.7171412311507,-13.2450064259713,
-177.201718344835));
#152108=CARTESIAN_POINT('Ctrl Pts',(-58.499487866025,-13.2129797427744,
-177.346623311491));
#152109=CARTESIAN_POINT('Ctrl Pts',(-58.4996466434616,-13.1583683303841,
-177.604649432751));
#152110=CARTESIAN_POINT('Ctrl Pts',(-58.7088369592429,-13.350481719734,
-177.231562795809));
#152111=CARTESIAN_POINT('Ctrl Pts',(-58.4989011425798,-13.3549568592449,
-177.387243781406));
#152112=CARTESIAN_POINT('Ctrl Pts',(-58.4990964462207,-13.3675412254732,
-177.653635589973));
#152113=CARTESIAN_POINT('Ctrl Pts',(-58.7142302220621,-13.4630034042927,
-177.204888879754));
#152114=CARTESIAN_POINT('Ctrl Pts',(-58.4976201073564,-13.5106559619976,
-177.34946224375));
#152115=CARTESIAN_POINT('Ctrl Pts',(-58.4969599356141,-13.5907093707611,
-177.608451413633));
#152116=CARTESIAN_POINT('Ctrl Pts',(-58.744734365864,-13.6207444397399,
-177.084931957504));
#152117=CARTESIAN_POINT('Ctrl Pts',(-58.4955856783522,-13.714544547136,
-177.195108413244));
#152118=CARTESIAN_POINT('Ctrl Pts',(-58.4926597506031,-13.9035447147552,
-177.415964369801));
#152119=CARTESIAN_POINT('Ctrl Pts',(-58.7643257211001,-13.6767548657761,
-177.011378635403));
#152120=CARTESIAN_POINT('Ctrl Pts',(-58.4947863265944,-13.7828140187279,
-177.100057626205));
#152121=CARTESIAN_POINT('Ctrl Pts',(-58.4906864354198,-14.0146226773921,
-177.299459860577));
#152122=CARTESIAN_POINT('Ctrl Pts',(-58.8477271879271,-13.8175445314543,
-176.717566432405));
#152123=CARTESIAN_POINT('Ctrl Pts',(-58.4932080623643,-13.9334183953258,
-176.732015957667));
#152124=CARTESIAN_POINT('Ctrl Pts',(-58.4852925969465,-14.2938175741563,
-176.853564982499));
#152125=CARTESIAN_POINT('Ctrl Pts',(-58.9364557612147,-13.8384035340429,
-176.439823404047));
#152126=CARTESIAN_POINT('Ctrl Pts',(-58.4944709305922,-13.886285675068,
-176.399510353928));
#152127=CARTESIAN_POINT('Ctrl Pts',(-58.4839076510609,-14.3351427387709,
-176.459952278612));
#152128=CARTESIAN_POINT('Ctrl Pts',(-59.0262805694248,-13.8273207647541,
-176.128850259174));
#152129=CARTESIAN_POINT('Ctrl Pts',(-58.4967342962639,-13.7830237188745,
-176.132987895578));
#152130=CARTESIAN_POINT('Ctrl Pts',(-58.4845502518446,-14.3131195259793,
-176.102153175423));
#152131=CARTESIAN_POINT('Origin',(0.,-12.9675000200281,-171.871644662643));
#152132=CARTESIAN_POINT('Origin',(0.,-12.9675000200281,-171.449026400902));
#152133=CARTESIAN_POINT('Ctrl Pts',(-58.627582591745,-20.4849178106967,
-176.310058991613));
#152134=CARTESIAN_POINT('Ctrl Pts',(-58.0107588300312,-20.5427919605405,
-176.323555907706));
#152135=CARTESIAN_POINT('Ctrl Pts',(-58.0841784519436,-19.9304621405658,
-176.259519378371));
#152136=CARTESIAN_POINT('Ctrl Pts',(-58.5358479429026,-20.4652520455798,
-176.572045320709));
#152137=CARTESIAN_POINT('Ctrl Pts',(-58.0269718314754,-20.409820708043,
-176.521171997891));
#152138=CARTESIAN_POINT('Ctrl Pts',(-58.0887038582403,-19.8911762730753,
-176.615064002266));
#152139=CARTESIAN_POINT('Ctrl Pts',(-58.453312463316,-20.5037323072241,
-176.810599719082));
#152140=CARTESIAN_POINT('Ctrl Pts',(-58.0300429255414,-20.3800147773311,
-176.815173598683));
#152141=CARTESIAN_POINT('Ctrl Pts',(-58.0801409030891,-19.9672777568629,
-176.996564457697));
#152142=CARTESIAN_POINT('Ctrl Pts',(-58.3536773083228,-20.6617143273459,
-177.059070718027));
#152143=CARTESIAN_POINT('Ctrl Pts',(-58.008419009151,-20.5399861299023,
-177.132937218036));
#152144=CARTESIAN_POINT('Ctrl Pts',(-58.0411746905458,-20.2805473548039,
-177.404658872083));
#152145=CARTESIAN_POINT('Ctrl Pts',(-58.3273152468094,-20.7187423212865,
-177.118370177225));
#152146=CARTESIAN_POINT('Ctrl Pts',(-57.9997262186439,-20.6050332455159,
-177.211134013007));
#152147=CARTESIAN_POINT('Ctrl Pts',(-58.0268899075637,-20.3936565135702,
-177.503861519498));
#152148=CARTESIAN_POINT('Ctrl Pts',(-58.2694539592074,-20.878594537362,
-177.222018588675));
#152149=CARTESIAN_POINT('Ctrl Pts',(-57.9736236814238,-20.7985247659916,
-177.347834553946));
#152150=CARTESIAN_POINT('Ctrl Pts',(-57.9855747517757,-20.7107497140498,
-177.674988342283));
#152151=CARTESIAN_POINT('Ctrl Pts',(-58.2424846982626,-20.9834338367789,
-177.246739433871));
#152152=CARTESIAN_POINT('Ctrl Pts',(-57.9549828795132,-20.9354006234089,
-177.384906431077));
#152153=CARTESIAN_POINT('Ctrl Pts',(-57.9575440958208,-20.9188769733095,
-177.71328609301));
#152154=CARTESIAN_POINT('Ctrl Pts',(-58.2224054091628,-21.0947200667586,
-177.228981500926));
#152155=CARTESIAN_POINT('Ctrl Pts',(-57.9347942321424,-21.0799781740437,
-177.361546823285));
#152156=CARTESIAN_POINT('Ctrl Pts',(-57.9264125504997,-21.1393961655747,
-177.673640454257));
#152157=CARTESIAN_POINT('Origin',(-58.4476369465814,-21.0219233613115,-177.688917160843));
#152158=CARTESIAN_POINT('Ctrl Pts',(-57.8819282087167,-21.4487963148739,
-177.697497252237));
#152159=CARTESIAN_POINT('Ctrl Pts',(-57.8810878095005,-21.4545317502846,
-177.368333266163));
#152160=CARTESIAN_POINT('Ctrl Pts',(-58.1799818947148,-21.5006430233976,
-177.238261718413));
#152161=CARTESIAN_POINT('Ctrl Pts',(-57.906096697535,-21.2838546967462,
-177.694536471641));
#152162=CARTESIAN_POINT('Ctrl Pts',(-57.9052384907138,-21.2898253143233,
-177.368094235677));
#152163=CARTESIAN_POINT('Ctrl Pts',(-58.2008748005355,-21.3341357689658,
-177.236799145875));
#152164=CARTESIAN_POINT('Ctrl Pts',(-57.9295599753438,-21.1188110827801,
-177.691677811931));
#152165=CARTESIAN_POINT('Ctrl Pts',(-57.9287492734302,-21.1245836426315,
-177.367866070024));
#152166=CARTESIAN_POINT('Ctrl Pts',(-58.2211580737071,-21.1675764425397,
-177.235439894836));
#152167=CARTESIAN_POINT('Ctrl Pts',(-57.952317989407,-20.9536655363853,
-177.688917160843));
#152168=CARTESIAN_POINT('Ctrl Pts',(-57.9515978527783,-20.958891271667,
-177.367648026607));
#152169=CARTESIAN_POINT('Ctrl Pts',(-58.2408316684984,-21.0009616906551,
-177.234173073119));
#152170=CARTESIAN_POINT('Origin',(-58.376645543834,-21.5212860267954,-177.697497252237));
#152171=CARTESIAN_POINT('Origin',(8.61202340367822,-13.0253612208376,-187.990299917396));
#152172=CARTESIAN_POINT('Ctrl Pts',(-58.1799818947148,-21.5006430233977,
-177.238261718413));
#152173=CARTESIAN_POINT('Ctrl Pts',(-57.8810878095005,-21.4545317502846,
-177.368333266163));
#152174=CARTESIAN_POINT('Ctrl Pts',(-57.8819282087167,-21.4487963148736,
-177.697497252237));
#152175=CARTESIAN_POINT('Ctrl Pts',(-58.1643305096628,-21.5659716479372,
-177.242027715059));
#152176=CARTESIAN_POINT('Ctrl Pts',(-57.868876514339,-21.5377805372773,
-177.374493960823));
#152177=CARTESIAN_POINT('Ctrl Pts',(-57.8629489711247,-21.5783230793646,
-177.699822299871));
#152178=CARTESIAN_POINT('Ctrl Pts',(-58.1516959167317,-21.6321056009482,
-177.229926261063));
#152179=CARTESIAN_POINT('Ctrl Pts',(-57.8561193903755,-21.6237742374893,
-177.3594824509));
#152180=CARTESIAN_POINT('Ctrl Pts',(-57.8432533717849,-21.7094932883126,
-177.67338127456));
#152181=CARTESIAN_POINT('Ctrl Pts',(-58.135834617463,-21.751763745641,-177.175847704912));
#152182=CARTESIAN_POINT('Ctrl Pts',(-57.833274341657,-21.7763737806991,
-177.289541220421));
#152183=CARTESIAN_POINT('Ctrl Pts',(-57.8068932864249,-21.9467814783138,
-177.56730490578));
#152184=CARTESIAN_POINT('Ctrl Pts',(-58.1325374345936,-21.8059684297317,
-177.133613057603));
#152185=CARTESIAN_POINT('Ctrl Pts',(-57.822969521998,-21.8444848229842,
-177.233860492204));
#152186=CARTESIAN_POINT('Ctrl Pts',(-57.7900355525622,-22.0542721190802,
-177.487158575097));
#152187=CARTESIAN_POINT('Ctrl Pts',(-58.1379476084663,-21.8930112710375,
-177.027055273752));
#152188=CARTESIAN_POINT('Ctrl Pts',(-57.8075855468967,-21.9461185785114,
-177.096669117024));
#152189=CARTESIAN_POINT('Ctrl Pts',(-57.7626304144021,-22.2268825024457,
-177.290851905635));
#152190=CARTESIAN_POINT('Ctrl Pts',(-58.1467121091855,-21.9264637442851,
-176.962169933093));
#152191=CARTESIAN_POINT('Ctrl Pts',(-57.8023886323833,-21.9804905067127,
-177.013273949454));
#152192=CARTESIAN_POINT('Ctrl Pts',(-57.7519076537925,-22.2932204551335,
-177.173672169064));
#152193=CARTESIAN_POINT('Ctrl Pts',(-58.1775901524469,-21.9698497118448,
-176.818815489061));
#152194=CARTESIAN_POINT('Ctrl Pts',(-57.7982009932088,-22.0095200736329,
-176.838338250264));
#152195=CARTESIAN_POINT('Ctrl Pts',(-57.7379487783882,-22.3792570371924,
-176.923566462093));
#152196=CARTESIAN_POINT('Ctrl Pts',(-58.1997838724148,-21.98000002,-176.740111438881));
#152197=CARTESIAN_POINT('Ctrl Pts',(-57.7993206334297,-22.0035077749888,
-176.744992431703));
#152198=CARTESIAN_POINT('Ctrl Pts',(-57.7346476044917,-22.3993856207533,
-176.79021969384));
#152199=CARTESIAN_POINT('Ctrl Pts',(-58.2281061322669,-21.98000002,-176.657965001855));
#152200=CARTESIAN_POINT('Ctrl Pts',(-57.8031610044997,-21.98000002,-176.657965001855));
#152201=CARTESIAN_POINT('Ctrl Pts',(-57.7346476057222,-22.3993856132206,
-176.657965001855));
#152202=CARTESIAN_POINT('Origin',(0.,-12.9675000200281,-171.871644662643));
#152203=CARTESIAN_POINT('Origin',(0.,-12.9675000200281,-171.449026400902));
#152204=CARTESIAN_POINT('Ctrl Pts',(-57.0184057454332,-28.63000002,-176.849882244789));
#152205=CARTESIAN_POINT('Ctrl Pts',(-56.3680674991214,-28.63000002,-176.849882244789));
#152206=CARTESIAN_POINT('Ctrl Pts',(-56.5351989170821,-28.0015042572884,
-176.849882244789));
#152207=CARTESIAN_POINT('Ctrl Pts',(-57.0179413444383,-28.63000002,-176.912963832989));
#152208=CARTESIAN_POINT('Ctrl Pts',(-56.3682278310667,-28.6293970924019,
-176.891072637881));
#152209=CARTESIAN_POINT('Ctrl Pts',(-56.5351989103125,-28.0015042827455,
-176.976072722839));
#152210=CARTESIAN_POINT('Ctrl Pts',(-57.0114676733044,-28.6416054347749,
-176.974087537723));
#152211=CARTESIAN_POINT('Ctrl Pts',(-56.3671971691575,-28.6322312586769,
-176.931422425923));
#152212=CARTESIAN_POINT('Ctrl Pts',(-56.5290979719196,-28.024501614784,
-177.098181890721));
#152213=CARTESIAN_POINT('Ctrl Pts',(-57.,-28.664523125878,-177.032518510534));
#152214=CARTESIAN_POINT('Ctrl Pts',(-56.364125065416,-28.6418687251214,
-176.974758823107));
#152215=CARTESIAN_POINT('Ctrl Pts',(-56.5169491525423,-28.0699653316567,
-177.215087021068));
#152216=CARTESIAN_POINT('Origin',(-57.,-28.199046231756,-177.215087021068));
#152217=CARTESIAN_POINT('Ctrl Pts',(-56.262175563026,-28.9930296810172,
-177.84995));
#152218=CARTESIAN_POINT('Ctrl Pts',(-56.262175563026,-28.9930296810172,
-177.34995));
#152219=CARTESIAN_POINT('Ctrl Pts',(-56.7430488584365,-29.13000002,-177.34995));
#152220=CARTESIAN_POINT('Ctrl Pts',(-56.3176963010821,-28.7981083537361,
-177.849949971516));
#152221=CARTESIAN_POINT('Ctrl Pts',(-56.2928119947094,-28.8854717787751,
-177.322103214377));
#152222=CARTESIAN_POINT('Ctrl Pts',(-56.799051006553,-29.0316942919675,
-177.34995));
#152223=CARTESIAN_POINT('Ctrl Pts',(-56.3721096851181,-28.6028436438479,
-177.790491903933));
#152224=CARTESIAN_POINT('Ctrl Pts',(-56.3169386704035,-28.8006430758332,
-177.261063208671));
#152225=CARTESIAN_POINT('Ctrl Pts',(-56.8539225877547,-28.933239542368,
-177.320220947896));
#152226=CARTESIAN_POINT('Ctrl Pts',(-56.4617523202342,-28.2759697513382,
-177.568612620023));
#152227=CARTESIAN_POINT('Ctrl Pts',(-56.3506671101773,-28.684579593959,
-177.121256964593));
#152228=CARTESIAN_POINT('Ctrl Pts',(-56.9443314005494,-28.7684056938368,
-177.209281314082));
#152229=CARTESIAN_POINT('Ctrl Pts',(-56.4972682976465,-28.1436156829388,
-177.404470992826));
#152230=CARTESIAN_POINT('Ctrl Pts',(-56.3596918685657,-28.6555519736166,
-177.043271150691));
#152231=CARTESIAN_POINT('Ctrl Pts',(-56.9801582405499,-28.7016493747432,
-177.12717563931));
#152232=CARTESIAN_POINT('Ctrl Pts',(-56.5169491525423,-28.0699653316567,
-177.215087021068));
#152233=CARTESIAN_POINT('Ctrl Pts',(-56.364125065416,-28.6418687251214,
-176.974758823107));
#152234=CARTESIAN_POINT('Ctrl Pts',(-57.,-28.664523125878,-177.032518510534));
#152235=CARTESIAN_POINT('',(-56.7430488584365,-29.13000002,-177.34995));
#152236=CARTESIAN_POINT('Origin',(-56.7430488584365,-29.13000002,-177.84995));
#152237=CARTESIAN_POINT('Ctrl Pts',(-56.7430488584365,-29.13000002,-177.34995));
#152238=CARTESIAN_POINT('Ctrl Pts',(-56.799051006553,-29.0316942919675,
-177.34995));
#152239=CARTESIAN_POINT('Ctrl Pts',(-56.8539225877547,-28.933239542368,
-177.320220947896));
#152240=CARTESIAN_POINT('Ctrl Pts',(-56.9443314005494,-28.7684056938368,
-177.209281314082));
#152241=CARTESIAN_POINT('Ctrl Pts',(-56.9801582405499,-28.7016493747432,
-177.12717563931));
#152242=CARTESIAN_POINT('Ctrl Pts',(-57.,-28.664523125878,-177.032518510534));
#152243=CARTESIAN_POINT('Origin',(0.,-12.9675000200281,-177.84995));
#152244=CARTESIAN_POINT('Origin',(-56.5982428503831,-29.63000002,-177.84995));
#152245=CARTESIAN_POINT('Origin',(0.,-12.9675000200281,-177.34995));
#152246=CARTESIAN_POINT('Ctrl Pts',(-56.598242850383,-29.6300000200001,
-177.34995));
#152247=CARTESIAN_POINT('Ctrl Pts',(-56.1185967245324,-29.4887923928816,
-177.34995));
#152248=CARTESIAN_POINT('Ctrl Pts',(-56.1185967245323,-29.4887923928817,
-177.84995));
#152249=CARTESIAN_POINT('Ctrl Pts',(-56.5603834356575,-29.6942993846806,
-177.34995));
#152250=CARTESIAN_POINT('Ctrl Pts',(-56.0988447287815,-29.5558848630778,
-177.36777816462));
#152251=CARTESIAN_POINT('Ctrl Pts',(-56.0810569766533,-29.6163052971279,
-177.849949980253));
#152252=CARTESIAN_POINT('Ctrl Pts',(-56.5223271856603,-29.7580969359688,
-177.337570500007));
#152253=CARTESIAN_POINT('Ctrl Pts',(-56.076826602317,-29.6305362885491,
-177.372218485688));
#152254=CARTESIAN_POINT('Ctrl Pts',(-56.04332441336,-29.7428150883777,-177.825190994024));
#152255=CARTESIAN_POINT('Ctrl Pts',(-56.4500227583409,-29.8779487295679,
-177.288930648015));
#152256=CARTESIAN_POINT('Ctrl Pts',(-56.0326216659297,-29.7794711155594,
-177.345478783924));
#152257=CARTESIAN_POINT('Ctrl Pts',(-55.9716327345056,-29.9804872937887,
-177.727911302019));
#152258=CARTESIAN_POINT('Ctrl Pts',(-56.4164036466448,-29.9329688836733,
-177.253030654974));
#152259=CARTESIAN_POINT('Ctrl Pts',(-56.010729181878,-29.8527767454272,
-177.315352245562));
#152260=CARTESIAN_POINT('Ctrl Pts',(-55.9382985315747,-30.0895950523083,
-177.656111307255));
#152261=CARTESIAN_POINT('Ctrl Pts',(-56.3301688951883,-30.0730055436657,
-177.116037754475));
#152262=CARTESIAN_POINT('Ctrl Pts',(-55.9539368540439,-30.0418512098301,
-177.177649819729));
#152263=CARTESIAN_POINT('Ctrl Pts',(-55.8527945813582,-30.367294876883,
-177.382125514336));
#152264=CARTESIAN_POINT('Ctrl Pts',(-56.2941923707649,-30.1300000200003,
-176.98587944854));
#152265=CARTESIAN_POINT('Ctrl Pts',(-55.9270363771194,-30.1300000005971,
-177.017952895974));
#152266=CARTESIAN_POINT('Ctrl Pts',(-55.8171229439391,-30.4803177904842,
-177.121808892945));
#152267=CARTESIAN_POINT('Ctrl Pts',(-56.294192362543,-30.1300000200003,
-176.84995));
#152268=CARTESIAN_POINT('Ctrl Pts',(-55.9270363712659,-30.1300000200003,
-176.84995));
#152269=CARTESIAN_POINT('Ctrl Pts',(-55.8171229357418,-30.4803178166107,
-176.84995));
#152270=CARTESIAN_POINT('Origin',(0.,-12.9675000200281,-171.871644662643));
#152271=CARTESIAN_POINT('Origin',(0.,-12.9675000200281,-171.449026400902));
#152272=CARTESIAN_POINT('Ctrl Pts',(-54.1989607257493,-36.78000002,-176.84995));
#152273=CARTESIAN_POINT('Ctrl Pts',(-53.4396057593646,-36.78000002,-176.84995));
#152274=CARTESIAN_POINT('Ctrl Pts',(-53.7396474992599,-36.0824364606782,
-176.84995));
#152275=CARTESIAN_POINT('Ctrl Pts',(-54.1989607146972,-36.78000002,-176.918317891383));
#152276=CARTESIAN_POINT('Ctrl Pts',(-53.4396057606977,-36.7800000160094,
-176.873130497251));
#152277=CARTESIAN_POINT('Ctrl Pts',(-53.7396474882981,-36.0824364861631,
-176.986685785392));
#152278=CARTESIAN_POINT('Ctrl Pts',(-54.1865253922149,-36.7944813746413,
-176.987117359946));
#152279=CARTESIAN_POINT('Ctrl Pts',(-53.4415801188845,-36.7743609339043,
-176.898046003587));
#152280=CARTESIAN_POINT('Ctrl Pts',(-53.7273175494953,-36.1111537311933,
-177.124284716345));
#152281=CARTESIAN_POINT('Ctrl Pts',(-54.1401753140075,-36.8481352183371,
-177.110787176626));
#152282=CARTESIAN_POINT('Ctrl Pts',(-53.4422054158915,-36.7696056006871,
-176.971124353297));
#152283=CARTESIAN_POINT('Ctrl Pts',(-53.6813602693863,-36.2175520155611,
-177.371624356797));
#152284=CARTESIAN_POINT('Ctrl Pts',(-54.1061105508192,-36.8874586360784,
-177.16641977034));
#152285=CARTESIAN_POINT('Ctrl Pts',(-53.4404233153528,-36.7716343519663,
-177.018743720143));
#152286=CARTESIAN_POINT('Ctrl Pts',(-53.64758418971,-36.2955323627627,-177.48288953791));
#152287=CARTESIAN_POINT('Ctrl Pts',(-54.0238234872226,-36.9816277442484,
-177.25641751247));
#152288=CARTESIAN_POINT('Ctrl Pts',(-53.4231809570326,-36.8072884980391,
-177.124958325117));
#152289=CARTESIAN_POINT('Ctrl Pts',(-53.565994475128,-36.4822744877163,
-177.662885027711));
#152290=CARTESIAN_POINT('Ctrl Pts',(-53.9751511105352,-37.0369743252984,
-177.291477883886));
#152291=CARTESIAN_POINT('Ctrl Pts',(-53.408253154931,-36.8396793680934,
-177.182243847129));
#152292=CARTESIAN_POINT('Ctrl Pts',(-53.5177345753394,-36.5920295740937,
-177.73300576859));
#152293=CARTESIAN_POINT('Ctrl Pts',(-53.8706043508049,-37.1546953024018,
-177.33811707005));
#152294=CARTESIAN_POINT('Ctrl Pts',(-53.3641465670514,-36.936877735883,
-177.281217994791));
#152295=CARTESIAN_POINT('Ctrl Pts',(-53.4140738058199,-36.825476258465,
-177.826284139284));
#152296=CARTESIAN_POINT('Ctrl Pts',(-53.8142255012181,-37.2176314844153,
-177.34995));
#152297=CARTESIAN_POINT('Ctrl Pts',(-53.3356547273387,-37.0000719000691,
-177.323538819178));
#152298=CARTESIAN_POINT('Ctrl Pts',(-53.3581698892714,-36.9502882170505,
-177.849949987733));
#152299=CARTESIAN_POINT('Ctrl Pts',(-53.7578119323263,-37.28000002,-177.34995));
#152300=CARTESIAN_POINT('Ctrl Pts',(-53.3022372549337,-37.073961884407,
-177.34995));
#152301=CARTESIAN_POINT('Ctrl Pts',(-53.3022372549337,-37.073961884407,
-177.84995));
#152302=CARTESIAN_POINT('Origin',(-53.7578119323263,-37.28000002,-177.84995));
#152303=CARTESIAN_POINT('Origin',(0.,-12.9675000200281,-177.84995));
#152304=CARTESIAN_POINT('Origin',(-53.5288692553037,-37.78000002,-177.84995));
#152305=CARTESIAN_POINT('Origin',(0.,-12.9675000200281,-177.34995));
#152306=CARTESIAN_POINT('Ctrl Pts',(-53.5288692553037,-37.78000002,-177.34995));
#152307=CARTESIAN_POINT('Ctrl Pts',(-53.0752347700892,-37.5697245962714,
-177.34995));
#152308=CARTESIAN_POINT('Ctrl Pts',(-53.0752347700893,-37.5697245962714,
-177.84995));
#152309=CARTESIAN_POINT('Ctrl Pts',(-53.4801386760123,-37.8325641065285,
-177.34995));
#152310=CARTESIAN_POINT('Ctrl Pts',(-53.0475810937503,-37.6293828354337,
-177.371580332169));
#152311=CARTESIAN_POINT('Ctrl Pts',(-53.0269261151962,-37.673942537699,
-177.849949988053));
#152312=CARTESIAN_POINT('Ctrl Pts',(-53.4320050770023,-37.884077740683,
-177.341849758034));
#152313=CARTESIAN_POINT('Ctrl Pts',(-53.0170937964823,-37.6950135347464,
-177.382936820891));
#152314=CARTESIAN_POINT('Ctrl Pts',(-52.9791793012708,-37.7761418725299,
-177.833741031442));
#152315=CARTESIAN_POINT('Ctrl Pts',(-53.3846587239314,-37.9343850848642,
-177.325518346031));
#152316=CARTESIAN_POINT('Ctrl Pts',(-52.9848137611505,-37.764168205744,
-177.380776321343));
#152317=CARTESIAN_POINT('Ctrl Pts',(-52.9322463618642,-37.8758780299853,
-177.801086692062));
#152318=CARTESIAN_POINT('Origin',(-53.3846587239314,-38.0887701497285,-177.801086692062));
#152319=CARTESIAN_POINT('Ctrl Pts',(-53.3846587239314,-37.9343850848642,
-177.325518346031));
#152320=CARTESIAN_POINT('Ctrl Pts',(-52.9848137611506,-37.764168205744,
-177.380776321343));
#152321=CARTESIAN_POINT('Ctrl Pts',(-52.9322463618642,-37.8758780299853,
-177.801086692062));
#152322=CARTESIAN_POINT('Ctrl Pts',(-53.2963306348783,-38.0282371456548,
-177.295050892481));
#152323=CARTESIAN_POINT('Ctrl Pts',(-52.9134668198848,-37.9027770181211,
-177.371916826896));
#152324=CARTESIAN_POINT('Ctrl Pts',(-52.8342434317084,-38.0841419017282,
-177.740238340822));
#152325=CARTESIAN_POINT('Ctrl Pts',(-53.2302250969522,-38.1165826570878,
-177.234494972704));
#152326=CARTESIAN_POINT('Ctrl Pts',(-52.85052657881,-38.040124740984,-177.309543897189));
#152327=CARTESIAN_POINT('Ctrl Pts',(-52.7606534316743,-38.2807615372527,
-177.619039957031));
#152328=CARTESIAN_POINT('Ctrl Pts',(-53.1455750275301,-38.2433781645652,
-177.065457314865));
#152329=CARTESIAN_POINT('Ctrl Pts',(-52.7690004592735,-38.2275535486387,
-177.113060004592));
#152330=CARTESIAN_POINT('Ctrl Pts',(-52.6665978216312,-38.5625293047724,
-177.280964618108));
#152331=CARTESIAN_POINT('Ctrl Pts',(-53.1262583407606,-38.28000002,-176.958526013972));
#152332=CARTESIAN_POINT('Ctrl Pts',(-52.7480693868922,-38.2799999991994,
-176.98145090087));
#152333=CARTESIAN_POINT('Ctrl Pts',(-52.6451348250506,-38.6439111866979,
-177.06710203648));
#152334=CARTESIAN_POINT('Ctrl Pts',(-53.1262583325313,-38.28000002,-176.84995));
#152335=CARTESIAN_POINT('Ctrl Pts',(-52.748069378376,-38.28000002,-176.84995));
#152336=CARTESIAN_POINT('Ctrl Pts',(-52.6451348158641,-38.6439112191758,
-176.84995));
#152337=CARTESIAN_POINT('Ctrl Pts',(-52.1126146143194,-39.4738501833479,
-171.391638125813));
#152338=CARTESIAN_POINT('Ctrl Pts',(-52.4864722882118,-39.4409761333229,
-171.679515584751));
#152339=CARTESIAN_POINT('Ctrl Pts',(-52.5050296388285,-39.3089337226171,
-172.133326251627));
#152340=CARTESIAN_POINT('Ctrl Pts',(-52.2029436074416,-39.18424163534,-171.345711176575));
#152341=CARTESIAN_POINT('Ctrl Pts',(-52.5176461244299,-39.1701487854048,
-171.633412526629));
#152342=CARTESIAN_POINT('Ctrl Pts',(-52.541270746464,-39.0510648426419,
-172.04151129494));
#152343=CARTESIAN_POINT('Ctrl Pts',(-52.3057718899875,-38.8932964873464,
-171.301698499895));
#152344=CARTESIAN_POINT('Ctrl Pts',(-52.5724535929286,-38.8910154875477,
-171.580271166833));
#152345=CARTESIAN_POINT('Ctrl Pts',(-52.5971684400779,-38.7973422647502,
-171.953442620307));
#152346=CARTESIAN_POINT('Ctrl Pts',(-52.4226914394942,-38.5972250898729,
-171.270067206297));
#152347=CARTESIAN_POINT('Ctrl Pts',(-52.6539547691069,-38.61136117722,-171.540761416572));
#152348=CARTESIAN_POINT('Ctrl Pts',(-52.6743159902015,-38.5446760769969,
-171.890184412595));
#152349=CARTESIAN_POINT('',(-52.1126146143194,-39.473850183348,-171.391638125813));
#152350=CARTESIAN_POINT('Origin',(-51.5147615700869,-39.1697606216571,-172.133326251627));
#152351=CARTESIAN_POINT('Ctrl Pts',(-52.1126146143194,-39.473850183348,
-171.391638125813));
#152352=CARTESIAN_POINT('Ctrl Pts',(-52.2018635968859,-39.1877043141331,
-171.34626029805));
#152353=CARTESIAN_POINT('Ctrl Pts',(-52.3033147624415,-38.900253615735,
-171.302751240844));
#152354=CARTESIAN_POINT('Ctrl Pts',(-52.418503743379,-38.6078427661481,
-171.27120723903));
#152355=CARTESIAN_POINT('Origin',(-51.6222122422086,-38.4052093625928,-172.64995));
#152356=CARTESIAN_POINT('',(-50.5139609686817,-46.2908269190399,-171.64995));
#152357=CARTESIAN_POINT('Ctrl Pts',(-50.5091418211897,-53.5104134695199,
-177.84995));
#152358=CARTESIAN_POINT('Ctrl Pts',(-50.5091418211897,-53.51041346952,-177.34995));
#152359=CARTESIAN_POINT('Ctrl Pts',(-51.0042758555605,-53.58000002,-177.34995));
#152360=CARTESIAN_POINT('Ctrl Pts',(-50.546038665875,-53.2478787779945,
-177.849949999941));
#152361=CARTESIAN_POINT('Ctrl Pts',(-50.5284384672378,-53.3731106984804,
-177.33120422009));
#152362=CARTESIAN_POINT('Ctrl Pts',(-51.0411727002473,-53.4487326742368,
-177.34995));
#152363=CARTESIAN_POINT('Ctrl Pts',(-50.5825022662094,-52.9884267802056,
-177.742176873059));
#152364=CARTESIAN_POINT('Ctrl Pts',(-50.5442961447015,-53.2602774603979,
-177.257255781812));
#152365=CARTESIAN_POINT('Ctrl Pts',(-51.0776363005805,-53.3190066753437,
-177.296063436531));
#152366=CARTESIAN_POINT('Ctrl Pts',(-50.6345361306733,-52.6181865964612,
-177.371936689315));
#152367=CARTESIAN_POINT('Ctrl Pts',(-50.5649476695633,-53.1133342256642,
-177.069891898465));
#152368=CARTESIAN_POINT('Ctrl Pts',(-51.1296701650438,-53.1338865834697,
-177.110943344657));
#152369=CARTESIAN_POINT('Ctrl Pts',(-50.6496826558828,-52.5104134695857,
-177.112484691526));
#152370=CARTESIAN_POINT('Ctrl Pts',(-50.5696324866514,-53.0800000199829,
-176.958917254526));
#152371=CARTESIAN_POINT('Ctrl Pts',(-51.1448166902519,-53.08000002,-176.981217345763));
#152372=CARTESIAN_POINT('Ctrl Pts',(-50.6496826558921,-52.5104134695199,
-176.84995));
#152373=CARTESIAN_POINT('Ctrl Pts',(-50.5696324866524,-53.08000002,-176.84995));
#152374=CARTESIAN_POINT('Ctrl Pts',(-51.1448166902628,-53.08000002,-176.84995));
#152375=CARTESIAN_POINT('Origin',(-51.0042758555605,-53.58000002,-177.84995));
#152376=CARTESIAN_POINT('Origin',(-53.1076143453209,-38.6139690140329,-177.84995));
#152377=CARTESIAN_POINT('Origin',(-50.9340054382093,-54.0800000199999,-177.84995));
#152378=CARTESIAN_POINT('',(-62.4796469926385,28.0715083218873,-177.34995));
#152379=CARTESIAN_POINT('Ctrl Pts',(-50.2983305691361,-55.0104134695199,
-176.84995));
#152380=CARTESIAN_POINT('Ctrl Pts',(-50.3588212345988,-54.58000002,-176.84995));
#152381=CARTESIAN_POINT('Ctrl Pts',(-50.7934646035069,-54.58000002,-176.84995));
#152382=CARTESIAN_POINT('Ctrl Pts',(-50.2983305691453,-55.0104134694541,
-177.112484691526));
#152383=CARTESIAN_POINT('Ctrl Pts',(-50.358821234607,-54.5800000199424,
-176.997671841189));
#152384=CARTESIAN_POINT('Ctrl Pts',(-50.7934646035178,-54.58000002,-176.981217345763));
#152385=CARTESIAN_POINT('Ctrl Pts',(-50.313477094355,-54.9026403425777,
-177.371936689315));
#152386=CARTESIAN_POINT('Ctrl Pts',(-50.3685899331079,-54.5104921183889,
-177.142957948483));
#152387=CARTESIAN_POINT('Ctrl Pts',(-50.8086111287259,-54.5261134565302,
-177.110943344657));
#152388=CARTESIAN_POINT('Ctrl Pts',(-50.3655109588186,-54.5324001588352,
-177.742176873059));
#152389=CARTESIAN_POINT('Ctrl Pts',(-50.3994818369767,-54.2906848009584,
-177.329589659683));
#152390=CARTESIAN_POINT('Ctrl Pts',(-50.8606449931892,-54.3409933646562,
-177.296063436531));
#152391=CARTESIAN_POINT('Ctrl Pts',(-50.4019745591532,-54.2729481610447,
-177.849949999941));
#152392=CARTESIAN_POINT('Ctrl Pts',(-50.420433990624,-54.1416024812641,
-177.367861075731));
#152393=CARTESIAN_POINT('Ctrl Pts',(-50.8971085935234,-54.2112673657634,
-177.34995));
#152394=CARTESIAN_POINT('Ctrl Pts',(-50.4388714038385,-54.0104134695199,
-177.84995));
#152395=CARTESIAN_POINT('Ctrl Pts',(-50.4388714038384,-54.0104134695199,
-177.34995));
#152396=CARTESIAN_POINT('Ctrl Pts',(-50.9340054382093,-54.08000002,-177.34995));
#152397=CARTESIAN_POINT('Origin',(-51.6222122422086,-38.4052093625928,-172.64995));
#152398=CARTESIAN_POINT('Origin',(-48.9446667094463,-57.4569357767149,-172.64995));
#152399=CARTESIAN_POINT('Ctrl Pts',(-50.9867892914962,-42.9264785869994,
-171.64995));
#152400=CARTESIAN_POINT('Ctrl Pts',(-51.9770573602378,-43.0656516879595,
-171.64995));
#152401=CARTESIAN_POINT('Ctrl Pts',(-51.9770573602378,-43.0656516879596,
-172.64995));
#152402=CARTESIAN_POINT('Ctrl Pts',(-51.1823572933545,-42.3510730842576,
-171.64995));
#152403=CARTESIAN_POINT('Ctrl Pts',(-52.0557320324863,-42.5058523071511,
-171.757498535929));
#152404=CARTESIAN_POINT('Ctrl Pts',(-52.0666747393887,-42.4279909017497,
-172.649949997757));
#152405=CARTESIAN_POINT('Ctrl Pts',(-51.3741578990751,-41.7754043578546,
-171.628003076365));
#152406=CARTESIAN_POINT('Ctrl Pts',(-52.1416679592955,-41.8943864154851,
-171.81403941883));
#152407=CARTESIAN_POINT('Ctrl Pts',(-52.1554800333146,-41.7961084021622,
-172.606056153133));
#152408=CARTESIAN_POINT('Ctrl Pts',(-51.7497860966445,-40.6237611991777,
-171.543915907757));
#152409=CARTESIAN_POINT('Ctrl Pts',(-52.3125022740342,-40.6788371047634,
-171.821280489149));
#152410=CARTESIAN_POINT('Ctrl Pts',(-52.3315472405273,-40.5433251268562,
-172.43788181511));
#152411=CARTESIAN_POINT('Ctrl Pts',(-51.9336694513069,-40.0475756797307,
-171.482621144039));
#152412=CARTESIAN_POINT('Ctrl Pts',(-52.3988291636532,-40.0645893682337,
-171.781794156641));
#152413=CARTESIAN_POINT('Ctrl Pts',(-52.4188787332529,-39.9219292677054,
-172.315208572937));
#152414=CARTESIAN_POINT('Ctrl Pts',(-52.1126146143194,-39.473850183348,
-171.391638125813));
#152415=CARTESIAN_POINT('Ctrl Pts',(-52.4864722882118,-39.4409761333229,
-171.679515584751));
#152416=CARTESIAN_POINT('Ctrl Pts',(-52.5050296388285,-39.3089337226171,
-172.133326251627));
#152417=CARTESIAN_POINT('',(-50.9867892914962,-42.9264785869994,-171.64995));
#152418=CARTESIAN_POINT('Origin',(-50.9867892914962,-42.9264785869994,-172.64995));
#152419=CARTESIAN_POINT('Ctrl Pts',(-50.9867892914962,-42.9264785869994,
-171.64995));
#152420=CARTESIAN_POINT('Ctrl Pts',(-51.1823574302578,-42.3510731085196,
-171.649950016858));
#152421=CARTESIAN_POINT('Ctrl Pts',(-51.3741580251093,-41.7754043773928,
-171.628003106914));
#152422=CARTESIAN_POINT('Ctrl Pts',(-51.7497861967124,-40.6237612089719,
-171.543915957081));
#152423=CARTESIAN_POINT('Ctrl Pts',(-51.9336695368887,-40.0475756828609,
-171.482621199082));
#152424=CARTESIAN_POINT('Ctrl Pts',(-52.1126146143194,-39.473850183348,
-171.391638125813));
#152425=CARTESIAN_POINT('Origin',(-51.6222122422086,-38.4052093625928,-172.64995));
#152426=CARTESIAN_POINT('',(-51.3476245933058,-40.3590020057362,-171.64995));
#152427=CARTESIAN_POINT('Ctrl Pts',(-51.6545496240141,-45.3604134695199,
-177.84995));
#152428=CARTESIAN_POINT('Ctrl Pts',(-51.6545496240142,-45.3604134695199,
-177.34995));
#152429=CARTESIAN_POINT('Ctrl Pts',(-52.1496836583849,-45.43000002,-177.34995));
#152430=CARTESIAN_POINT('Ctrl Pts',(-51.6914464686995,-45.0978787779945,
-177.849949999941));
#152431=CARTESIAN_POINT('Ctrl Pts',(-51.6738462700621,-45.2231106984802,
-177.331204220089));
#152432=CARTESIAN_POINT('Ctrl Pts',(-52.1865805030705,-45.2987326742378,
-177.34995));
#152433=CARTESIAN_POINT('Ctrl Pts',(-51.7279100690339,-44.8384267802056,
-177.742176873059));
#152434=CARTESIAN_POINT('Ctrl Pts',(-51.6897039475278,-45.1102774603978,
-177.257255781811));
#152435=CARTESIAN_POINT('Ctrl Pts',(-52.2230441034049,-45.1690066753419,
-177.296063436528));
#152436=CARTESIAN_POINT('Ctrl Pts',(-51.7799439334977,-44.4681865964612,
-177.371936689315));
#152437=CARTESIAN_POINT('Ctrl Pts',(-51.710355472386,-44.963334225664,-177.069891898465));
#152438=CARTESIAN_POINT('Ctrl Pts',(-52.2750779678683,-44.9838865834715,
-177.110943344658));
#152439=CARTESIAN_POINT('Ctrl Pts',(-51.7950904587073,-44.3604134695857,
-177.112484691526));
#152440=CARTESIAN_POINT('Ctrl Pts',(-51.7150402894787,-44.9300000199802,
-176.958917254526));
#152441=CARTESIAN_POINT('Ctrl Pts',(-52.2902244930764,-44.93000002,-176.981217345763));
#152442=CARTESIAN_POINT('Ctrl Pts',(-51.7950904587165,-44.36041346952,-176.84995));
#152443=CARTESIAN_POINT('Ctrl Pts',(-51.7150402894768,-44.93000002,-176.84995));
#152444=CARTESIAN_POINT('Ctrl Pts',(-52.2902244930873,-44.93000002,-176.84995));
#152445=CARTESIAN_POINT('Origin',(-52.1496836583849,-45.43000002,-177.84995));
#152446=CARTESIAN_POINT('Origin',(-53.1076143453209,-38.6139690140329,-177.84995));
#152447=CARTESIAN_POINT('Origin',(-52.0794132410337,-45.93000002,-177.84995));
#152448=CARTESIAN_POINT('',(-62.4796469926385,28.0715083218873,-177.34995));
#152449=CARTESIAN_POINT('Ctrl Pts',(-51.4437383719606,-46.86041346952,-176.84995));
#152450=CARTESIAN_POINT('Ctrl Pts',(-51.5042290374232,-46.43000002,-176.84995));
#152451=CARTESIAN_POINT('Ctrl Pts',(-51.9388724063314,-46.43000002,-176.84995));
#152452=CARTESIAN_POINT('Ctrl Pts',(-51.4437383719698,-46.8604134694541,
-177.112484691526));
#152453=CARTESIAN_POINT('Ctrl Pts',(-51.5042290374242,-46.4300000199415,
-176.997671841189));
#152454=CARTESIAN_POINT('Ctrl Pts',(-51.9388724063423,-46.43000002,-176.981217345763));
#152455=CARTESIAN_POINT('Ctrl Pts',(-51.4588848971795,-46.7526403425778,
-177.371936689315));
#152456=CARTESIAN_POINT('Ctrl Pts',(-51.5139977359314,-46.3604921183892,
-177.142957948483));
#152457=CARTESIAN_POINT('Ctrl Pts',(-51.9540189315504,-46.3761134565303,
-177.110943344657));
#152458=CARTESIAN_POINT('Ctrl Pts',(-51.5109187616431,-46.3824001588352,
-177.742176873059));
#152459=CARTESIAN_POINT('Ctrl Pts',(-51.5448896398021,-46.1406848009587,
-177.329589659683));
#152460=CARTESIAN_POINT('Ctrl Pts',(-52.0060527960138,-46.1909933646562,
-177.296063436531));
#152461=CARTESIAN_POINT('Ctrl Pts',(-51.5473823619777,-46.1229481610447,
-177.849949999941));
#152462=CARTESIAN_POINT('Ctrl Pts',(-51.5658417934483,-45.9916024812643,
-177.367861075732));
#152463=CARTESIAN_POINT('Ctrl Pts',(-52.0425163963479,-46.0612673657634,
-177.34995));
#152464=CARTESIAN_POINT('Ctrl Pts',(-51.584279206663,-45.86041346952,-177.84995));
#152465=CARTESIAN_POINT('Ctrl Pts',(-51.584279206663,-45.8604134695199,
-177.34995));
#152466=CARTESIAN_POINT('Ctrl Pts',(-52.0794132410337,-45.93000002,-177.34995));
#152467=CARTESIAN_POINT('Origin',(-46.9641305719631,-57.1785895747948,-172.64995));
#152468=CARTESIAN_POINT('Origin',(-48.4203826827217,-58.549476072617,-172.64995));
#152469=CARTESIAN_POINT('Origin',(0.,-12.9675000200281,-172.64995));
#152470=CARTESIAN_POINT('Origin',(-45.5819760525891,-61.3878827027496,-172.64995));
#152471=CARTESIAN_POINT('Origin',(-44.2110895547669,-59.9316305919911,-172.64995));
#152472=CARTESIAN_POINT('Origin',(-44.489435756687,-61.9121667294742,-172.64995));
#152473=CARTESIAN_POINT('Origin',(-45.4220505312374,-61.7810962706031,-172.64995));
#152474=CARTESIAN_POINT('Ctrl Pts',(-40.9304134495199,-63.4221822677665,
-177.84995));
#152475=CARTESIAN_POINT('Ctrl Pts',(-40.9304134495199,-63.4221822677665,
-177.34995));
#152476=CARTESIAN_POINT('Ctrl Pts',(-41.,-63.9173163021373,-177.34995));
#152477=CARTESIAN_POINT('Ctrl Pts',(-41.1929481410454,-63.3852854230811,
-177.849949999941));
#152478=CARTESIAN_POINT('Ctrl Pts',(-41.0616024612649,-63.4037448545523,
-177.367861075732));
#152479=CARTESIAN_POINT('Ctrl Pts',(-41.1312673457634,-63.8804194574513,
-177.34995));
#152480=CARTESIAN_POINT('Ctrl Pts',(-41.4524001388343,-63.3488218227467,
-177.742176873059));
#152481=CARTESIAN_POINT('Ctrl Pts',(-41.2106847809575,-63.3827927009057,
-177.329589659683));
#152482=CARTESIAN_POINT('Ctrl Pts',(-41.2609933446562,-63.8439558571173,
-177.296063436531));
#152483=CARTESIAN_POINT('Ctrl Pts',(-41.8226403225787,-63.2967879582829,
-177.371936689315));
#152484=CARTESIAN_POINT('Ctrl Pts',(-41.4304920983899,-63.3519007970349,
-177.142957948483));
#152485=CARTESIAN_POINT('Ctrl Pts',(-41.4461134365302,-63.7919219926539,
-177.110943344657));
#152486=CARTESIAN_POINT('Ctrl Pts',(-41.9304134494542,-63.2816414330733,
-177.112484691526));
#152487=CARTESIAN_POINT('Ctrl Pts',(-41.4999999999415,-63.342132098545,
-176.997671841189));
#152488=CARTESIAN_POINT('Ctrl Pts',(-41.5,-63.7767754674458,-176.981217345763));
#152489=CARTESIAN_POINT('Ctrl Pts',(-41.9304134495199,-63.2816414330641,
-176.84995));
#152490=CARTESIAN_POINT('Ctrl Pts',(-41.5,-63.3421320985267,-176.84995));
#152491=CARTESIAN_POINT('Ctrl Pts',(-41.5,-63.7767754674349,-176.84995));
#152492=CARTESIAN_POINT('Origin',(-41.,-63.9173163021373,-177.84995));
#152493=CARTESIAN_POINT('Origin',(-45.6308101826775,-63.2664983737155,-177.84995));
#152494=CARTESIAN_POINT('Origin',(-40.5,-63.9875867194884,-177.84995));
#152495=CARTESIAN_POINT('',(-40.227526467895,-64.0258803771248,-177.34995));
#152496=CARTESIAN_POINT('Ctrl Pts',(-39.43041344952,-63.63299351982,-176.84995));
#152497=CARTESIAN_POINT('Ctrl Pts',(-40.,-63.5529433505803,-176.84995));
#152498=CARTESIAN_POINT('Ctrl Pts',(-40.,-64.1281275541908,-176.84995));
#152499=CARTESIAN_POINT('Ctrl Pts',(-39.4304134495858,-63.6329935198108,
-177.112484691526));
#152500=CARTESIAN_POINT('Ctrl Pts',(-39.9999999999783,-63.5529433505767,
-176.958917254529));
#152501=CARTESIAN_POINT('Ctrl Pts',(-40.,-64.1281275541799,-176.981217345763));
#152502=CARTESIAN_POINT('Ctrl Pts',(-39.5381865764622,-63.6178469946011,
-177.371936689315));
#152503=CARTESIAN_POINT('Ctrl Pts',(-40.033334205665,-63.5482585334886,
-177.069891898461));
#152504=CARTESIAN_POINT('Ctrl Pts',(-40.0538865634702,-64.1129810289718,
-177.110943344657));
#152505=CARTESIAN_POINT('Ctrl Pts',(-39.9084267602046,-63.5658131301376,
-177.742176873059));
#152506=CARTESIAN_POINT('Ctrl Pts',(-40.1802774403969,-63.5276070086322,
-177.257255781815));
#152507=CARTESIAN_POINT('Ctrl Pts',(-40.2390066553433,-64.0609471645084,
-177.29606343653));
#152508=CARTESIAN_POINT('Ctrl Pts',(-40.1678787579952,-63.5293495298029,
-177.849949999941));
#152509=CARTESIAN_POINT('Ctrl Pts',(-40.293110678481,-63.5117493311661,
-177.331204220089));
#152510=CARTESIAN_POINT('Ctrl Pts',(-40.3687326542369,-64.0244835641743,
-177.34995));
#152511=CARTESIAN_POINT('Ctrl Pts',(-40.4304134495199,-63.4924526851176,
-177.84995));
#152512=CARTESIAN_POINT('Ctrl Pts',(-40.4304134495199,-63.4924526851176,
-177.34995));
#152513=CARTESIAN_POINT('Ctrl Pts',(-40.5,-63.9875867194884,-177.34995));
#152514=CARTESIAN_POINT('Origin',(-45.4220505312374,-61.7810962706031,-172.64995));
#152515=CARTESIAN_POINT('',(-39.8608268990399,-62.5626752818388,-171.64995));
#152516=CARTESIAN_POINT('Ctrl Pts',(-32.7804134495199,-64.5675900705909,
-177.84995));
#152517=CARTESIAN_POINT('Ctrl Pts',(-32.7804134495199,-64.5675900705908,
-177.34995));
#152518=CARTESIAN_POINT('Ctrl Pts',(-32.85,-65.0627241049617,-177.34995));
#152519=CARTESIAN_POINT('Ctrl Pts',(-33.0429481410447,-64.5306932259057,
-177.849949999941));
#152520=CARTESIAN_POINT('Ctrl Pts',(-32.9116024612643,-64.5491526573769,
-177.367861075732));
#152521=CARTESIAN_POINT('Ctrl Pts',(-32.9812673457631,-65.0258272602758,
-177.34995));
#152522=CARTESIAN_POINT('Ctrl Pts',(-33.3024001388352,-64.494229625571,
-177.742176873059));
#152523=CARTESIAN_POINT('Ctrl Pts',(-33.0606847809584,-64.52820050373,-177.329589659683));
#152524=CARTESIAN_POINT('Ctrl Pts',(-33.1109933446567,-64.9893636599417,
-177.29606343653));
#152525=CARTESIAN_POINT('Ctrl Pts',(-33.6726403225778,-64.4421957611075,
-177.371936689315));
#152526=CARTESIAN_POINT('Ctrl Pts',(-33.280492098389,-64.4973085998594,
-177.142957948483));
#152527=CARTESIAN_POINT('Ctrl Pts',(-33.2961134365298,-64.9373297954784,
-177.110943344657));
#152528=CARTESIAN_POINT('Ctrl Pts',(-33.7804134494542,-64.4270492358978,
-177.112484691526));
#152529=CARTESIAN_POINT('Ctrl Pts',(-33.3499999999424,-64.4875399013621,
-176.997671841189));
#152530=CARTESIAN_POINT('Ctrl Pts',(-33.35,-64.9221832702703,-176.981217345763));
#152531=CARTESIAN_POINT('Ctrl Pts',(-33.7804134495199,-64.4270492358885,
-176.84995));
#152532=CARTESIAN_POINT('Ctrl Pts',(-33.35,-64.4875399013512,-176.84995));
#152533=CARTESIAN_POINT('Ctrl Pts',(-33.35,-64.9221832702593,-176.84995));
#152534=CARTESIAN_POINT('Origin',(-32.85,-65.0627241049617,-177.84995));
#152535=CARTESIAN_POINT('Origin',(-45.6308101826775,-63.2664983737155,-177.84995));
#152536=CARTESIAN_POINT('Origin',(-32.35,-65.1329945223129,-177.84995));
#152537=CARTESIAN_POINT('',(-40.227526467895,-64.0258803771248,-177.34995));
#152538=CARTESIAN_POINT('Ctrl Pts',(-31.28041344952,-64.7784013226445,-176.84995));
#152539=CARTESIAN_POINT('Ctrl Pts',(-31.8499999999999,-64.6983511534047,
-176.84995));
#152540=CARTESIAN_POINT('Ctrl Pts',(-31.85,-65.2735353570153,-176.84995));
#152541=CARTESIAN_POINT('Ctrl Pts',(-31.2804134495858,-64.7784013226352,
-177.112484691526));
#152542=CARTESIAN_POINT('Ctrl Pts',(-31.8499999999783,-64.6983511534012,
-176.958917254529));
#152543=CARTESIAN_POINT('Ctrl Pts',(-31.85,-65.2735353570043,-176.981217345763));
#152544=CARTESIAN_POINT('Ctrl Pts',(-31.3881865764622,-64.7632547974255,
-177.371936689315));
#152545=CARTESIAN_POINT('Ctrl Pts',(-31.883334205664,-64.6936663363131,
-177.069891898462));
#152546=CARTESIAN_POINT('Ctrl Pts',(-31.9038865634697,-65.2583888317962,
-177.110943344657));
#152547=CARTESIAN_POINT('Ctrl Pts',(-31.7584267602047,-64.711220932962,
-177.742176873059));
#152548=CARTESIAN_POINT('Ctrl Pts',(-32.0302774403978,-64.6730148114567,
-177.257255781815));
#152549=CARTESIAN_POINT('Ctrl Pts',(-32.0890066553437,-65.2063549673329,
-177.296063436531));
#152550=CARTESIAN_POINT('Ctrl Pts',(-32.0178787579952,-64.6747573326273,
-177.849949999941));
#152551=CARTESIAN_POINT('Ctrl Pts',(-32.1431106784802,-64.6571571339907,
-177.331204220089));
#152552=CARTESIAN_POINT('Ctrl Pts',(-32.2187326542366,-65.1698913669989,
-177.34995));
#152553=CARTESIAN_POINT('Ctrl Pts',(-32.28041344952,-64.6378604879421,-177.84995));
#152554=CARTESIAN_POINT('Ctrl Pts',(-32.28041344952,-64.637860487942,-177.34995));
#152555=CARTESIAN_POINT('Ctrl Pts',(-32.35,-65.1329945223129,-177.34995));
#152556=CARTESIAN_POINT('Origin',(-45.4220505312374,-61.7810962706031,-172.64995));
#152557=CARTESIAN_POINT('',(-29.958978566972,-63.954289311524,-171.64995));
#152558=CARTESIAN_POINT('Origin',(-29.958978566972,-63.954289311524,-172.64995));
#152559=CARTESIAN_POINT('',(-31.7108268990399,-63.7080830846632,-171.64995));
#152560=CARTESIAN_POINT('Ctrl Pts',(-26.2234488624093,-65.1680142434972,
-171.34400271074));
#152561=CARTESIAN_POINT('Ctrl Pts',(-26.1751497442534,-65.4958993451584,
-171.625426858395));
#152562=CARTESIAN_POINT('Ctrl Pts',(-26.0394480946395,-65.5149709682656,
-172.038055421481));
#152563=CARTESIAN_POINT('Ctrl Pts',(-26.5325022452051,-65.072358231615,
-171.399245459895));
#152564=CARTESIAN_POINT('Ctrl Pts',(-26.5059850091802,-65.4494034808673,
-171.691392643103));
#152565=CARTESIAN_POINT('Ctrl Pts',(-26.3688360080808,-65.4686785159697,
-172.14852124047));
#152566=CARTESIAN_POINT('Ctrl Pts',(-26.843027692162,-64.9750314285332,
-171.444032296926));
#152567=CARTESIAN_POINT('Ctrl Pts',(-26.8344935945357,-65.4032346100804,
-171.736704292719));
#152568=CARTESIAN_POINT('Ctrl Pts',(-26.7013989289162,-65.4219398454845,
-172.23811459301));
#152569=CARTESIAN_POINT('Ctrl Pts',(-27.4650077428683,-64.7776672125821,
-171.519686348695));
#152570=CARTESIAN_POINT('Ctrl Pts',(-27.4914924972326,-65.3108994359038,
-171.799283317704));
#152571=CARTESIAN_POINT('Ctrl Pts',(-27.3705571684413,-65.3278957879536,
-172.38942269823));
#152572=CARTESIAN_POINT('Ctrl Pts',(-27.7764978537267,-64.6776202239548,
-171.550373470332));
#152573=CARTESIAN_POINT('Ctrl Pts',(-27.8213068579945,-65.2645470503453,
-171.81528847728));
#152574=CARTESIAN_POINT('Ctrl Pts',(-27.7072474293082,-65.2805770576552,
-172.450796940493));
#152575=CARTESIAN_POINT('Ctrl Pts',(-28.7113572324553,-64.3737932440126,
-171.624291948599));
#152576=CARTESIAN_POINT('Ctrl Pts',(-28.8291547927028,-65.1229032603379,
-171.822805263071));
#152577=CARTESIAN_POINT('Ctrl Pts',(-28.7226827355371,-65.1378669321315,
-172.598633897542));
#152578=CARTESIAN_POINT('Ctrl Pts',(-29.3350621276793,-64.1663451413114,
-171.64995));
#152579=CARTESIAN_POINT('Ctrl Pts',(-29.4938163229,-65.0294911740669,-171.766054775631));
#152580=CARTESIAN_POINT('Ctrl Pts',(-29.4067311934443,-65.0417301908804,
-172.64994999751));
#152581=CARTESIAN_POINT('Ctrl Pts',(-29.958978566972,-63.954289311524,-171.64995));
#152582=CARTESIAN_POINT('Ctrl Pts',(-30.098151667932,-64.9445573802655,
-171.64995));
#152583=CARTESIAN_POINT('Ctrl Pts',(-30.098151667932,-64.9445573802656,
-172.64995));
#152584=CARTESIAN_POINT('Ctrl Pts',(-26.2234488624093,-65.1680142434972,
-171.34400271074));
#152585=CARTESIAN_POINT('Ctrl Pts',(-26.5325022452051,-65.072358231615,
-171.399245459895));
#152586=CARTESIAN_POINT('Ctrl Pts',(-26.843027692162,-64.9750314285332,
-171.444032296926));
#152587=CARTESIAN_POINT('Ctrl Pts',(-27.4650077428683,-64.7776672125821,
-171.519686348695));
#152588=CARTESIAN_POINT('Ctrl Pts',(-27.7764978537267,-64.6776202239548,
-171.550373470332));
#152589=CARTESIAN_POINT('Ctrl Pts',(-28.7113572324553,-64.3737932440126,
-171.624291948599));
#152590=CARTESIAN_POINT('Ctrl Pts',(-29.3350621276793,-64.1663451413114,
-171.64995));
#152591=CARTESIAN_POINT('Ctrl Pts',(-29.958978566972,-63.954289311524,-171.64995));
#152592=CARTESIAN_POINT('Ctrl Pts',(-42.5,-54.58000002,-171.14995));
#152593=CARTESIAN_POINT('Ctrl Pts',(-41.5,-54.58000002,-171.14995));
#152594=CARTESIAN_POINT('Ctrl Pts',(-41.5,-55.58000002,-171.14995));
#152595=CARTESIAN_POINT('Ctrl Pts',(-42.5,-54.58000002,-171.64995));
#152596=CARTESIAN_POINT('Ctrl Pts',(-41.5,-54.58000002,-171.64995));
#152597=CARTESIAN_POINT('Ctrl Pts',(-41.5,-55.58000002,-171.64995));
#152598=CARTESIAN_POINT('Ctrl Pts',(-42.5,-55.08000002,-171.64995));
#152599=CARTESIAN_POINT('Ctrl Pts',(-42.,-55.08000002,-171.64995));
#152600=CARTESIAN_POINT('Ctrl Pts',(-42.,-55.58000002,-171.64995));
#152601=CARTESIAN_POINT('Ctrl Pts',(-25.1782808829885,-54.58000002,-147.977025477683));
#152602=CARTESIAN_POINT('Ctrl Pts',(-23.9800829025888,-54.5800000200001,
-149.152655882413));
#152603=CARTESIAN_POINT('Ctrl Pts',(-23.0246263600192,-55.5929437980769,
-150.090116786386));
#152604=CARTESIAN_POINT('Ctrl Pts',(-23.9836910796608,-54.58000002,-146.759504150767));
#152605=CARTESIAN_POINT('Ctrl Pts',(-22.8379194752343,-54.5800000199763,
-147.932452641776));
#152606=CARTESIAN_POINT('Ctrl Pts',(-21.9091489271198,-55.5502169050949,
-148.872607854072));
#152607=CARTESIAN_POINT('Ctrl Pts',(-22.7503247929853,-54.58000002,-145.568800995698));
#152608=CARTESIAN_POINT('Ctrl Pts',(-21.6573291961429,-54.58000002,-146.736008441848));
#152609=CARTESIAN_POINT('Ctrl Pts',(-20.7612402155903,-55.5070450251362,
-147.681892304448));
#152610=CARTESIAN_POINT('Ctrl Pts',(-20.1860325764608,-54.58000002,-143.268341382183));
#152611=CARTESIAN_POINT('Ctrl Pts',(-19.2052975266984,-54.58000002,-144.424597244368));
#152612=CARTESIAN_POINT('Ctrl Pts',(-18.3837542309683,-55.4210082419989,
-145.38143269084));
#152613=CARTESIAN_POINT('Ctrl Pts',(-18.8677311043704,-54.58000002,-142.169807438416));
#152614=CARTESIAN_POINT('Ctrl Pts',(-17.9461389525456,-54.58000002,-143.320329501862));
#152615=CARTESIAN_POINT('Ctrl Pts',(-17.165895474142,-55.3785603713206,
-144.282911778325));
#152616=CARTESIAN_POINT('Ctrl Pts',(-17.5014165897211,-54.58000002,-141.139869854338));
#152617=CARTESIAN_POINT('Ctrl Pts',(-16.6396978513013,-54.5800000199999,
-142.283025361002));
#152618=CARTESIAN_POINT('Ctrl Pts',(-15.9085533562516,-55.3376384323294,
-143.252961163042));
#152619=CARTESIAN_POINT('Ctrl Pts',(-17.55,-54.58000002,-141.176536909659));
#152620=CARTESIAN_POINT('Ctrl Pts',(-17.9693769714652,-54.5800000200003,
-141.49343498957));
#152621=CARTESIAN_POINT('Ctrl Pts',(-18.3834419174563,-54.5800000200088,
-141.816182952557));
#152622=CARTESIAN_POINT('Ctrl Pts',(-18.7928766486271,-54.5800000200341,
-142.14446893926));
#152623=CARTESIAN_POINT('Ctrl Pts',(-19.2164906824831,-54.5800000200604,
-142.48412393308));
#152624=CARTESIAN_POINT('Ctrl Pts',(-19.635148044907,-54.5800000201049,
-142.829707458939));
#152625=CARTESIAN_POINT('Ctrl Pts',(-20.0495713966389,-54.5800000201721,
-143.180920598249));
#152626=CARTESIAN_POINT('Ctrl Pts',(-20.488326023268,-54.5800000202432,
-143.552753867686));
#152627=CARTESIAN_POINT('Ctrl Pts',(-20.9223347029624,-54.58000002034,-143.930897445283));
#152628=CARTESIAN_POINT('Ctrl Pts',(-21.3524219961151,-54.5800000204563,
-144.315043885279));
#152629=CARTESIAN_POINT('Ctrl Pts',(-21.3910234228925,-54.5800000204667,
-144.349522003818));
#152630=CARTESIAN_POINT('Ctrl Pts',(-21.4295932412714,-54.5800000204773,
-144.384048506611));
#152631=CARTESIAN_POINT('Ctrl Pts',(-21.4681320362146,-54.580000020488,
-144.418623187423));
#152632=CARTESIAN_POINT('Ctrl Pts',(-21.9304021275721,-54.5800000206166,
-144.83334401305));
#152633=CARTESIAN_POINT('Ctrl Pts',(-22.3865711849682,-54.5800000207665,
-145.253534976228));
#152634=CARTESIAN_POINT('Ctrl Pts',(-22.8375326449957,-54.580000020912,
-145.679007211413));
#152635=CARTESIAN_POINT('Ctrl Pts',(-22.9587258346797,-54.5800000209511,
-145.793350324682));
#152636=CARTESIAN_POINT('Ctrl Pts',(-23.0795426741296,-54.5800000209898,
-145.90807504421));
#152637=CARTESIAN_POINT('Ctrl Pts',(-23.2,-54.5800000210274,-146.023178055809));
#152638=CARTESIAN_POINT('Origin',(3.3975957231091E-14,-70.08000002,-174.34995));
#152639=CARTESIAN_POINT('',(-41.5,-73.08000002,-174.34995));
#152640=CARTESIAN_POINT('Ctrl Pts',(-16.443141398898,-54.58000002,-140.363430177307));
#152641=CARTESIAN_POINT('Ctrl Pts',(-15.630331507009,-54.5800000199999,
-141.502754952306));
#152642=CARTESIAN_POINT('Ctrl Pts',(-14.935633130959,-55.3065630024253,
-142.47652148601));
#152643=CARTESIAN_POINT('Ctrl Pts',(-15.3397373006696,-54.58000002,-139.576246587186));
#152644=CARTESIAN_POINT('Ctrl Pts',(-14.5800220275964,-54.580000020014,
-140.713030388695));
#152645=CARTESIAN_POINT('Ctrl Pts',(-13.9222087476243,-55.2748272571858,
-141.68934947009));
#152646=CARTESIAN_POINT('Ctrl Pts',(-14.2001096642283,-54.58000002,-138.832914681508));
#152647=CARTESIAN_POINT('Ctrl Pts',(-13.4942101985199,-54.5800000200048,
-139.965671699013));
#152648=CARTESIAN_POINT('Ctrl Pts',(-12.8784929287096,-55.2441433795399,
-140.946005990295));
#152649=CARTESIAN_POINT('Ctrl Pts',(-11.8242610588971,-54.58000002,-137.462982383337));
#152650=CARTESIAN_POINT('Ctrl Pts',(-11.2325518044464,-54.5800000199952,
-138.58879503276));
#152651=CARTESIAN_POINT('Ctrl Pts',(-10.7090288904129,-55.1865297732718,
-139.576073691957));
#152652=CARTESIAN_POINT('Ctrl Pts',(-10.6074840054802,-54.58000002,-136.847973525117));
#152653=CARTESIAN_POINT('Ctrl Pts',(-10.0748797157148,-54.5800000199999,
-137.970225859417));
#152654=CARTESIAN_POINT('Ctrl Pts',(-9.6010395318864,-55.1600903081647,
-138.961065386249));
#152655=CARTESIAN_POINT('Ctrl Pts',(-9.35547519799418,-54.58000002,-136.31962263586));
#152656=CARTESIAN_POINT('Ctrl Pts',(-8.88330739463766,-54.58000002,-137.438496970103));
#152657=CARTESIAN_POINT('Ctrl Pts',(-8.46374531288877,-55.1370659744517,
-138.432713944563));
#152658=CARTESIAN_POINT('Ctrl Pts',(-9.4,-54.58000002,-136.338455187671));
#152659=CARTESIAN_POINT('Ctrl Pts',(-9.92110496058458,-54.5800000200001,
-136.559368584537));
#152660=CARTESIAN_POINT('Ctrl Pts',(-10.4350703325249,-54.5800000200483,
-136.794854049277));
#152661=CARTESIAN_POINT('Ctrl Pts',(-10.9425445776727,-54.5800000201757,
-137.043577637514));
#152662=CARTESIAN_POINT('Ctrl Pts',(-11.3976304732259,-54.58000002029,-137.266624615721));
#152663=CARTESIAN_POINT('Ctrl Pts',(-11.8474960215409,-54.5800000203574,
-137.500318485596));
#152664=CARTESIAN_POINT('Ctrl Pts',(-12.2925996107723,-54.5800000201853,
-137.743731583458));
#152665=CARTESIAN_POINT('Ctrl Pts',(-12.5336925965022,-54.5800000200921,
-137.875577724331));
#152666=CARTESIAN_POINT('Ctrl Pts',(-12.7734820900616,-54.5800000201101,
-138.010349990831));
#152667=CARTESIAN_POINT('Ctrl Pts',(-13.0121639376423,-54.580000020184,
-138.147985687537));
#152668=CARTESIAN_POINT('Ctrl Pts',(-13.3646805607945,-54.580000020293,
-138.351264116625));
#152669=CARTESIAN_POINT('Ctrl Pts',(-13.713070843513,-54.5800000206454,
-138.55976634471));
#152670=CARTESIAN_POINT('Ctrl Pts',(-14.058084756869,-54.5800000210433,
-138.77339084118));
#152671=CARTESIAN_POINT('Ctrl Pts',(-14.3916633624478,-54.580000021428,
-138.979934864164));
#152672=CARTESIAN_POINT('Ctrl Pts',(-14.7220850961472,-54.5800000217332,
-139.191268004988));
#152673=CARTESIAN_POINT('Ctrl Pts',(-15.05,-54.580000021344,-139.407335470919));
#152674=CARTESIAN_POINT('Ctrl Pts',(-1.09388780931665,-55.0499912502469,
-136.472972564846));
#152675=CARTESIAN_POINT('Ctrl Pts',(-1.14986049246831,-54.5800000199999,
-135.468532548998));
#152676=CARTESIAN_POINT('Ctrl Pts',(-1.21164037634558,-54.58000002,-134.359881256142));
#152677=CARTESIAN_POINT('Ctrl Pts',(-2.06753743423328,-55.0527136176872,
-136.533065609844));
#152678=CARTESIAN_POINT('Ctrl Pts',(-2.1734236725105,-54.580000019985,-135.528951041927));
#152679=CARTESIAN_POINT('Ctrl Pts',(-2.29002416952399,-54.58000002,-134.419974475838));
#152680=CARTESIAN_POINT('Ctrl Pts',(-3.03750542044518,-55.059063567472,
-136.673166196403));
#152681=CARTESIAN_POINT('Ctrl Pts',(-3.19311650329436,-54.58000002,-135.669893399192));
#152682=CARTESIAN_POINT('Ctrl Pts',(-3.36400336137312,-54.58000002,-134.560074887715));
#152683=CARTESIAN_POINT('Ctrl Pts',(-4.48820368733454,-55.0737025194561,
-136.999007240366));
#152684=CARTESIAN_POINT('Ctrl Pts',(-4.71607294932927,-54.5800000199999,
-135.997360222398));
#152685=CARTESIAN_POINT('Ctrl Pts',(-4.96860300664728,-54.58000002,-134.885915931654));
#152686=CARTESIAN_POINT('Ctrl Pts',(-4.97306841018422,-55.0794633322322,
-137.127585972214));
#152687=CARTESIAN_POINT('Ctrl Pts',(-5.22506238654006,-54.5800000199999,
-136.126634241129));
#152688=CARTESIAN_POINT('Ctrl Pts',(-5.50462478218054,-54.58000002,-135.014494663549));
#152689=CARTESIAN_POINT('Ctrl Pts',(-5.92682186653397,-55.0923918960893,
-137.417551068811));
#152690=CARTESIAN_POINT('Ctrl Pts',(-6.22569420503589,-54.58000002,-136.418114793059));
#152691=CARTESIAN_POINT('Ctrl Pts',(-6.5582931505392,-54.58000002,-135.304459760069));
#152692=CARTESIAN_POINT('Ctrl Pts',(-6.39676634858691,-55.099562033378,
-137.578988956132));
#152693=CARTESIAN_POINT('Ctrl Pts',(-6.71851642939749,-54.58000002,-136.580417857494));
#152694=CARTESIAN_POINT('Ctrl Pts',(-7.07711031169138,-54.58000002,-135.46589761626));
#152695=CARTESIAN_POINT('Ctrl Pts',(-6.86052929923582,-55.1073474746665,
-137.755279275981));
#152696=CARTESIAN_POINT('Ctrl Pts',(-7.20434315889942,-54.58000002,-136.757552063338));
#152697=CARTESIAN_POINT('Ctrl Pts',(-7.58869434220596,-54.58000002,-135.642187967278));
#152698=CARTESIAN_POINT('Ctrl Pts',(-1.24999999852556,-54.58000002,-134.362052703156));
#152699=CARTESIAN_POINT('Ctrl Pts',(-1.8558687299695,-54.58000002,-134.396884061811));
#152700=CARTESIAN_POINT('Ctrl Pts',(-2.45821169814561,-54.5800000199999,
-134.456836856573));
#152701=CARTESIAN_POINT('Ctrl Pts',(-3.05717008780528,-54.5800000200001,
-134.540898522254));
#152702=CARTESIAN_POINT('Ctrl Pts',(-3.40705616968019,-54.5800000200002,
-134.590003781231));
#152703=CARTESIAN_POINT('Ctrl Pts',(-3.75578723672687,-54.5800000200004,
-134.647336949705));
#152704=CARTESIAN_POINT('Ctrl Pts',(-4.10339093154591,-54.5800000200016,
-134.712704370428));
#152705=CARTESIAN_POINT('Ctrl Pts',(-4.21364342719022,-54.580000020002,
-134.733437525386));
#152706=CARTESIAN_POINT('Ctrl Pts',(-4.32374689616092,-54.5800000200024,
-134.754971981414));
#152707=CARTESIAN_POINT('Ctrl Pts',(-4.43373542753185,-54.5800000200027,
-134.777307325963));
#152708=CARTESIAN_POINT('Ctrl Pts',(-4.67988879728086,-54.5800000200034,
-134.827293631415));
#152709=CARTESIAN_POINT('Ctrl Pts',(-4.92593529130837,-54.5800000200038,
-134.881432381241));
#152710=CARTESIAN_POINT('Ctrl Pts',(-5.17124777564329,-54.5800000200039,
-134.939444408488));
#152711=CARTESIAN_POINT('Ctrl Pts',(-5.41900393393831,-54.580000020004,
-134.998034321043));
#152712=CARTESIAN_POINT('Ctrl Pts',(-5.6660135363309,-54.5800000200037,
-135.060575714351));
#152713=CARTESIAN_POINT('Ctrl Pts',(-5.91161937020563,-54.5800000200032,
-135.126829777541));
#152714=CARTESIAN_POINT('Ctrl Pts',(-5.95160365908193,-54.5800000200032,
-135.137615847073));
#152715=CARTESIAN_POINT('Ctrl Pts',(-5.99155067840898,-54.5800000200031,
-135.148500406429));
#152716=CARTESIAN_POINT('Ctrl Pts',(-6.03145750349794,-54.580000020003,
-135.159482527522));
#152717=CARTESIAN_POINT('Ctrl Pts',(-6.28934481311126,-54.5800000200026,
-135.230451582474));
#152718=CARTESIAN_POINT('Ctrl Pts',(-6.54583590336334,-54.580000020002,
-135.305503306745));
#152719=CARTESIAN_POINT('Ctrl Pts',(-6.80143368808723,-54.5800000200016,
-135.384644793435));
#152720=CARTESIAN_POINT('Ctrl Pts',(-6.83430358210449,-54.5800000200015,
-135.394822394476));
#152721=CARTESIAN_POINT('Ctrl Pts',(-6.86715867181465,-54.5800000200014,
-135.405067695209));
#152722=CARTESIAN_POINT('Ctrl Pts',(-6.9,-54.5800000200014,-135.415380765739));
#152723=CARTESIAN_POINT('Origin',(0.,-12.9675000200281,-170.64995));
#152724=CARTESIAN_POINT('Origin',(0.,-12.9675000200281,-171.64995));
#152725=CARTESIAN_POINT('Origin',(0.,-12.9675000200281,-171.07256826174));
#152726=CARTESIAN_POINT('Origin',(3.3975957231091E-14,-70.08000002,-174.34995));
#152727=CARTESIAN_POINT('Origin',(-60.,-54.58000002,-55.24995));
#152728=CARTESIAN_POINT('Origin',(-60.,-54.58000002,-55.24995));
#152729=CARTESIAN_POINT('Origin',(3.54807775957937E-14,-73.08000002,3.11172719585489E-30));
#152730=CARTESIAN_POINT('Origin',(-60.,-54.58000002,-55.24995));
#152731=CARTESIAN_POINT('Origin',(-60.,-2.55003103885676E-14,0.));
#152732=CARTESIAN_POINT('',(-60.,28.41999998,-174.34995));
#152733=CARTESIAN_POINT('Origin',(-60.,-2.55003103885676E-14,0.));
#152734=CARTESIAN_POINT('',(-60.,28.41999998,-174.34995));
#152735=CARTESIAN_POINT('Origin',(-60.,28.41999998,-177.34995));
#152736=CARTESIAN_POINT('',(-57.,-54.58000002,-177.34995));
#152737=CARTESIAN_POINT('Origin',(0.,-12.9675000200281,-171.64995));
#152738=CARTESIAN_POINT('Ctrl Pts',(-39.8501516349278,-30.4480624610812,
-139.515559008643));
#152739=CARTESIAN_POINT('Ctrl Pts',(-39.8776986028551,-31.1793494861265,
-140.199588507397));
#152740=CARTESIAN_POINT('Ctrl Pts',(-39.905579888437,-31.8977486430871,
-140.90539342064));
#152741=CARTESIAN_POINT('Ctrl Pts',(-39.9335715388522,-32.6056681732837,
-141.62920925267));
#152742=CARTESIAN_POINT('Ctrl Pts',(-39.9805442496755,-33.7936259708707,
-142.843842590218));
#152743=CARTESIAN_POINT('Ctrl Pts',(-40.0273699621533,-34.9400872995304,
-144.097130127809));
#152744=CARTESIAN_POINT('Ctrl Pts',(-40.0734472049714,-36.0537916893395,
-145.374999488024));
#152745=CARTESIAN_POINT('Ctrl Pts',(-40.0751063896396,-36.0938885093696,
-145.421033595465));
#152746=CARTESIAN_POINT('Ctrl Pts',(-39.,-37.0899493427105,-144.4917610531));
#152747=CARTESIAN_POINT('Ctrl Pts',(-39.,-38.3588510407228,-143.307942286761));
#152748=CARTESIAN_POINT('Ctrl Pts',(-40.0284942517968,-34.9676084789312,
-144.127227814579));
#152749=CARTESIAN_POINT('Ctrl Pts',(-39.,-35.9377773398718,-143.195151285356));
#152750=CARTESIAN_POINT('Ctrl Pts',(-39.,-37.1517836400886,-142.014121037894));
#152751=CARTESIAN_POINT('Ctrl Pts',(-39.98110816979,-33.8078877259523,-142.858424592381));
#152752=CARTESIAN_POINT('Ctrl Pts',(-38.9999999999999,-34.7456377245003,
-141.920028658586));
#152753=CARTESIAN_POINT('Ctrl Pts',(-39.,-35.9043030651865,-140.745333283629));
#152754=CARTESIAN_POINT('Ctrl Pts',(-39.8860349079144,-31.4034486206149,
-140.399993912959));
#152755=CARTESIAN_POINT('Ctrl Pts',(-39.,-32.2660355551645,-139.44936091542));
#152756=CARTESIAN_POINT('Ctrl Pts',(-39.,-33.3065355961441,-138.286902604304));
#152757=CARTESIAN_POINT('Ctrl Pts',(-39.838820917574,-30.1709959811911,
-139.222722930622));
#152758=CARTESIAN_POINT('Ctrl Pts',(-39.,-30.991536347315,-138.265657625916));
#152759=CARTESIAN_POINT('Ctrl Pts',(-39.,-31.969482004655,-137.109613636004));
#152760=CARTESIAN_POINT('Ctrl Pts',(-39.7930043034378,-28.8965637495112,
-138.115832334683));
#152761=CARTESIAN_POINT('Ctrl Pts',(-38.9999999999999,-29.666065684619,
-137.150287618997));
#152762=CARTESIAN_POINT('Ctrl Pts',(-39.,-30.5806161032665,-136.00274102598));
#152763=CARTESIAN_POINT('Ctrl Pts',(-39.0000000012919,-36.28000002,-141.149515588739));
#152764=CARTESIAN_POINT('Ctrl Pts',(-39.0000000010156,-35.8345332337773,
-140.70226392125));
#152765=CARTESIAN_POINT('Ctrl Pts',(-39.0000000008023,-35.3840176213637,
-140.260002181398));
#152766=CARTESIAN_POINT('Ctrl Pts',(-39.0000000006337,-34.9275493437178,
-139.822886348177));
#152767=CARTESIAN_POINT('Ctrl Pts',(-39.0000000005941,-34.8204877683556,
-139.720363758959));
#152768=CARTESIAN_POINT('Ctrl Pts',(-39.0000000005571,-34.7130985462023,
-139.618124369438));
#152769=CARTESIAN_POINT('Ctrl Pts',(-39.0000000005223,-34.6053696556425,
-139.516170434427));
#152770=CARTESIAN_POINT('Ctrl Pts',(-39.0000000003865,-34.1849244503591,
-139.118263773436));
#152771=CARTESIAN_POINT('Ctrl Pts',(-39.0000000002855,-33.7606942182181,
-138.725996583524));
#152772=CARTESIAN_POINT('Ctrl Pts',(-39.0000000002095,-33.3318521218421,
-138.33965468812));
#152773=CARTESIAN_POINT('Ctrl Pts',(-39.0000000001368,-32.9217240240916,
-137.970172149018));
#152774=CARTESIAN_POINT('Ctrl Pts',(-39.000000000087,-32.5073780349993,
-137.606108713902));
#152775=CARTESIAN_POINT('Ctrl Pts',(-39.000000000054,-32.0880629354048,
-137.247752417324));
#152776=CARTESIAN_POINT('Ctrl Pts',(-39.0000000000227,-31.6891890378919,
-136.906865640642));
#152777=CARTESIAN_POINT('Ctrl Pts',(-39.0000000000065,-31.285818826212,
-136.571142959481));
#152778=CARTESIAN_POINT('Ctrl Pts',(-39.0000000000016,-30.8772772476494,
-136.240870924102));
#152779=CARTESIAN_POINT('Ctrl Pts',(-39.0000000000006,-30.7950629150974,
-136.174407444314));
#152780=CARTESIAN_POINT('Ctrl Pts',(-39.0000000000001,-30.7126390581343,
-136.108164834603));
#152781=CARTESIAN_POINT('Ctrl Pts',(-39.,-30.63000002,-136.04214564125));
#152782=CARTESIAN_POINT('Origin',(-39.,46.91999998,-129.34995));
#152783=CARTESIAN_POINT('Origin',(-57.,-2.42462934179819E-14,-174.34995));
#152784=CARTESIAN_POINT('Origin',(-60.,28.41999998,-177.34995));
#152785=CARTESIAN_POINT('',(-57.,-54.58000002,-177.34995));
#152786=CARTESIAN_POINT('',(-60.,-29.13000002,-177.34995));
#152787=CARTESIAN_POINT('Origin',(-57.,-2.42462934179819E-14,-174.34995));
#152788=CARTESIAN_POINT('',(-60.,28.41999998,-174.34995));
#152789=CARTESIAN_POINT('Origin',(-60.,-2.55003103885676E-14,0.));
#152790=CARTESIAN_POINT('Origin',(-60.,-29.13000002,-176.84995));
#152791=CARTESIAN_POINT('Origin',(0.,-12.9675000200281,-171.64995));
#152792=CARTESIAN_POINT('Ctrl Pts',(-39.5912209089345,-22.3752378108182,
-133.464034181247));
#152793=CARTESIAN_POINT('Ctrl Pts',(-39.6121374457797,-23.2156616534414,
-133.924199547062));
#152794=CARTESIAN_POINT('Ctrl Pts',(-39.6349219111963,-24.0387135538522,
-134.431982361478));
#152795=CARTESIAN_POINT('Ctrl Pts',(-39.6912633163793,-25.928116182914,
-135.710428138755));
#152796=CARTESIAN_POINT('Ctrl Pts',(-39.7252977745181,-26.9648643074353,
-136.499221044835));
#152797=CARTESIAN_POINT('Ctrl Pts',(-39.7602371906927,-27.9700232578782,
-137.330324735012));
#152798=CARTESIAN_POINT('Ctrl Pts',(-39.7614953849933,-28.006195589491,
-137.360262497367));
#152799=CARTESIAN_POINT('Ctrl Pts',(-38.9999999999999,-28.7416759820709,
-136.390803950004));
#152800=CARTESIAN_POINT('Ctrl Pts',(-39.,-29.6092937616716,-135.247171188664));
#152801=CARTESIAN_POINT('Ctrl Pts',(-39.7261148635016,-26.9897399838167,
-136.518160398014));
#152802=CARTESIAN_POINT('Ctrl Pts',(-38.9999999999855,-27.6876355340531,
-135.545932666416));
#152803=CARTESIAN_POINT('Ctrl Pts',(-39.,-28.4992718278429,-134.405052285569));
#152804=CARTESIAN_POINT('Ctrl Pts',(-39.6916499750401,-25.9410827372237,
-135.719201830687));
#152805=CARTESIAN_POINT('Ctrl Pts',(-39.,-26.5955422649145,-134.742448815396));
#152806=CARTESIAN_POINT('Ctrl Pts',(-39.,-27.350294560115,-133.606110521891));
#152807=CARTESIAN_POINT('Ctrl Pts',(-39.6264336205064,-23.7540596888349,
-134.239374112649));
#152808=CARTESIAN_POINT('Ctrl Pts',(-38.9999999999999,-24.3121967691435,
-133.254719568795));
#152809=CARTESIAN_POINT('Ctrl Pts',(-39.,-24.9455608509554,-132.126282804037));
#152810=CARTESIAN_POINT('Ctrl Pts',(-39.5962661790751,-22.6346054925691,
-133.57169567032));
#152811=CARTESIAN_POINT('Ctrl Pts',(-38.9999999999854,-23.1403713306369,
-132.582946581795));
#152812=CARTESIAN_POINT('Ctrl Pts',(-39.,-23.7105874730482,-131.458602080542));
#152813=CARTESIAN_POINT('Ctrl Pts',(-39.5698471421185,-21.4814250807741,
-132.996116063158));
#152814=CARTESIAN_POINT('Ctrl Pts',(-39.,-21.9292251340083,-132.003415558585));
#152815=CARTESIAN_POINT('Ctrl Pts',(-39.,-22.4346253623973,-130.883024754454));
#152816=CARTESIAN_POINT('Ctrl Pts',(-39.0000000022172,-28.13000002,-134.169022080262));
#152817=CARTESIAN_POINT('Ctrl Pts',(-39.0000000027011,-27.7992138900224,
-133.937908100891));
#152818=CARTESIAN_POINT('Ctrl Pts',(-39.0000000021338,-27.4657185053518,
-133.711655036842));
#152819=CARTESIAN_POINT('Ctrl Pts',(-39.00000000154,-27.1287626917303,-133.490292823799));
#152820=CARTESIAN_POINT('Ctrl Pts',(-39.0000000009697,-26.8052287127277,
-133.277748048811));
#152821=CARTESIAN_POINT('Ctrl Pts',(-39.0000000004972,-26.4785047877958,
-133.06971193157));
#152822=CARTESIAN_POINT('Ctrl Pts',(-39.0000000003364,-26.1478973077855,
-132.866246059588));
#152823=CARTESIAN_POINT('Ctrl Pts',(-39.0000000002123,-25.8927164902428,
-132.709200043712));
#152824=CARTESIAN_POINT('Ctrl Pts',(-39.0000000001809,-25.6361572010218,
-132.555471936139));
#152825=CARTESIAN_POINT('Ctrl Pts',(-39.0000000003918,-25.3779449003587,
-132.405146018542));
#152826=CARTESIAN_POINT('Ctrl Pts',(-39.0000000007921,-24.887736647026,
-132.11975680468));
#152827=CARTESIAN_POINT('Ctrl Pts',(-39.000000000553,-24.3912688192601,
-131.846323735541));
#152828=CARTESIAN_POINT('Ctrl Pts',(-39.0000000002964,-23.8878019342432,
-131.586247706168));
#152829=CARTESIAN_POINT('Ctrl Pts',(-39.0000000000603,-23.42465277012,-131.346998613135));
#152830=CARTESIAN_POINT('Ctrl Pts',(-39.0000000000002,-22.9555805746405,
-131.119053182003));
#152831=CARTESIAN_POINT('Ctrl Pts',(-39.,-22.48000002,-130.903539806302));
#152832=CARTESIAN_POINT('Origin',(-39.,46.91999998,-129.34995));
#152833=CARTESIAN_POINT('Ctrl Pts',(-58.2228448679712,-20.997722377502,
-177.242431000705));
#152834=CARTESIAN_POINT('Ctrl Pts',(-59.9999999999999,-20.9611893120647,
-176.449983597595));
#152835=CARTESIAN_POINT('Ctrl Pts',(-60.,-20.8715629014036,-174.505875827596));
#152836=CARTESIAN_POINT('Ctrl Pts',(-58.19761253134,-21.2014273832679,-177.244315088819));
#152837=CARTESIAN_POINT('Ctrl Pts',(-59.9999999999924,-21.1661125646404,
-176.460241938351));
#152838=CARTESIAN_POINT('Ctrl Pts',(-60.,-21.0755801285197,-174.496470313984));
#152839=CARTESIAN_POINT('Ctrl Pts',(-58.1714292060953,-21.40462514847,-177.246332126402));
#152840=CARTESIAN_POINT('Ctrl Pts',(-60.0000000000095,-21.3701601153011,
-176.471395106131));
#152841=CARTESIAN_POINT('Ctrl Pts',(-60.,-21.2796010327843,-174.487167894352));
#152842=CARTESIAN_POINT('Ctrl Pts',(-58.1443031111633,-21.607263174561,
-177.248493339178));
#152843=CARTESIAN_POINT('Ctrl Pts',(-60.,-21.5731259515601,-176.483536694353));
#152844=CARTESIAN_POINT('Ctrl Pts',(-60.,-21.4836289747507,-174.478062871828));
#152845=CARTESIAN_POINT('Origin',(0.,-12.9675000200281,-171.64995));
#152846=CARTESIAN_POINT('Ctrl Pts',(-39.4710976496822,-14.3145440753934,
-130.89161549018));
#152847=CARTESIAN_POINT('Ctrl Pts',(-39.4728125648223,-14.7530413219124,
-130.92736520195));
#152848=CARTESIAN_POINT('Ctrl Pts',(-39.4753639075638,-15.1920614442498,
-130.980586110252));
#152849=CARTESIAN_POINT('Ctrl Pts',(-39.4825355718676,-16.1247177471361,
-131.130598723552));
#152850=CARTESIAN_POINT('Ctrl Pts',(-39.4873750954154,-16.6176732832087,
-131.232022056041));
#152851=CARTESIAN_POINT('Ctrl Pts',(-39.5043768621473,-18.0582508435763,
-131.589922098221));
#152852=CARTESIAN_POINT('Ctrl Pts',(-39.5191347956219,-18.9899841315148,
-131.902314804673));
#152853=CARTESIAN_POINT('Ctrl Pts',(-39.5365899624517,-19.9017174575869,
-132.27695566545));
#152854=CARTESIAN_POINT('Ctrl Pts',(-39.5372195035444,-19.9345312052232,
-132.290469469449));
#152855=CARTESIAN_POINT('Ctrl Pts',(-39.,-20.3054116348924,-131.293905860767));
#152856=CARTESIAN_POINT('Ctrl Pts',(-39.,-20.720937818584,-130.177378160746));
#152857=CARTESIAN_POINT('Ctrl Pts',(-39.5194895810462,-19.0123420478084,
-131.90982316175));
#152858=CARTESIAN_POINT('Ctrl Pts',(-39.,-19.3374585219745,-130.911526747764));
#152859=CARTESIAN_POINT('Ctrl Pts',(-39.,-19.698133940161,-129.796732169428));
#152860=CARTESIAN_POINT('Ctrl Pts',(-39.5045124277029,-18.0697294738066,
-131.592774070923));
#152861=CARTESIAN_POINT('Ctrl Pts',(-38.9999999999923,-18.3454434179522,
-130.592508390753));
#152862=CARTESIAN_POINT('Ctrl Pts',(-39.,-18.6506584423116,-129.479682762144));
#152863=CARTESIAN_POINT('Ctrl Pts',(-39.4873751859149,-16.6176732464254,
-131.23202224217));
#152864=CARTESIAN_POINT('Ctrl Pts',(-39.0000000000038,-16.8157658206047,
-130.229644160077));
#152865=CARTESIAN_POINT('Ctrl Pts',(-39.,-17.0348936577371,-129.118930933505));
#152866=CARTESIAN_POINT('Ctrl Pts',(-39.4825356614912,-16.1247177152636,
-131.130598909837));
#152867=CARTESIAN_POINT('Ctrl Pts',(-39.,-16.2963199259075,-130.127635847669));
#152868=CARTESIAN_POINT('Ctrl Pts',(-39.,-16.4860091127214,-129.017507601134));
#152869=CARTESIAN_POINT('Ctrl Pts',(-39.4749533438571,-15.1386572025492,
-130.9719965231));
#152870=CARTESIAN_POINT('Ctrl Pts',(-39.,-15.2570331695429,-129.96814976082));
#152871=CARTESIAN_POINT('Ctrl Pts',(-39.,-15.3875914977103,-128.858905214396));
#152872=CARTESIAN_POINT('Ctrl Pts',(-39.4722050319315,-14.6463890166082,
-130.914693311714));
#152873=CARTESIAN_POINT('Ctrl Pts',(-38.9999999999999,-14.7379707288414,
-129.910514022628));
#152874=CARTESIAN_POINT('Ctrl Pts',(-39.,-14.8389953875779,-128.801602009569));
#152875=CARTESIAN_POINT('Ctrl Pts',(-39.4705097325996,-14.1547657662532,
-130.879360876185));
#152876=CARTESIAN_POINT('Ctrl Pts',(-39.,-14.2195253716732,-129.874981182379));
#152877=CARTESIAN_POINT('Ctrl Pts',(-39.,-14.2910120087967,-128.766269567481));
#152878=CARTESIAN_POINT('Ctrl Pts',(-39.0000000000669,-19.98000002,-129.914446011788));
#152879=CARTESIAN_POINT('Ctrl Pts',(-39.0000000001518,-19.6367327840719,
-129.798586081307));
#152880=CARTESIAN_POINT('Ctrl Pts',(-39.0000000002631,-19.2913217887157,
-129.690298412947));
#152881=CARTESIAN_POINT('Ctrl Pts',(-39.0000000003003,-18.9438276300824,
-129.590011167477));
#152882=CARTESIAN_POINT('Ctrl Pts',(-39.0000000003366,-18.6049646905725,
-129.492214902559));
#152883=CARTESIAN_POINT('Ctrl Pts',(-39.0000000003094,-18.2641207496911,
-129.402026657411));
#152884=CARTESIAN_POINT('Ctrl Pts',(-39.0000000002472,-17.9213701519491,
-129.319797180689));
#152885=CARTESIAN_POINT('Ctrl Pts',(-39.0000000002263,-17.8056205245996,
-129.292027626528));
#152886=CARTESIAN_POINT('Ctrl Pts',(-39.0000000002019,-17.6896536077084,
-129.265165339737));
#152887=CARTESIAN_POINT('Ctrl Pts',(-39.0000000001767,-17.5734727602674,
-129.239222565105));
#152888=CARTESIAN_POINT('Ctrl Pts',(-39.0000000001494,-17.4477751466172,
-129.211154730048));
#152889=CARTESIAN_POINT('Ctrl Pts',(-39.0000000001211,-17.3216708975945,
-129.184146383705));
#152890=CARTESIAN_POINT('Ctrl Pts',(-39.0000000000953,-17.1952995452482,
-129.158233426905));
#152891=CARTESIAN_POINT('Ctrl Pts',(-39.0000000000407,-16.9274823440481,
-129.103316426838));
#152892=CARTESIAN_POINT('Ctrl Pts',(-39.0000000000228,-16.6579107580322,
-129.053205467123));
#152893=CARTESIAN_POINT('Ctrl Pts',(-39.0000000000127,-16.3874479062815,
-129.008231038422));
#152894=CARTESIAN_POINT('Ctrl Pts',(-39.0000000000071,-16.2374573286252,
-128.983289570501));
#152895=CARTESIAN_POINT('Ctrl Pts',(-39.0000000000044,-16.0871922946702,
-128.959928670237));
#152896=CARTESIAN_POINT('Ctrl Pts',(-39.0000000000028,-15.9367995435377,
-128.938211682847));
#152897=CARTESIAN_POINT('Ctrl Pts',(-39.,-15.6676875947363,-128.899351426921));
#152898=CARTESIAN_POINT('Ctrl Pts',(-39.0000000000001,-15.3983918170305,
-128.865722188253));
#152899=CARTESIAN_POINT('Ctrl Pts',(-39.,-15.1285853320425,-128.837337411665));
#152900=CARTESIAN_POINT('Ctrl Pts',(-39.,-14.8629886325447,-128.809395522211));
#152901=CARTESIAN_POINT('Ctrl Pts',(-39.,-14.5968970408721,-128.786535808696));
#152902=CARTESIAN_POINT('Ctrl Pts',(-39.,-14.3300000191853,-128.768820409992));
#152903=CARTESIAN_POINT('Origin',(-39.,46.91999998,-129.34995));
#152904=CARTESIAN_POINT('Ctrl Pts',(-58.6998841333603,-12.8234825355735,
-177.223692421544));
#152905=CARTESIAN_POINT('Ctrl Pts',(-59.9999999999999,-12.8247546893956,
-176.329633102893));
#152906=CARTESIAN_POINT('Ctrl Pts',(-60.,-12.8269998197496,-174.751773822184));
#152907=CARTESIAN_POINT('Ctrl Pts',(-58.7002617769471,-12.996381211483,
-177.22367874123));
#152908=CARTESIAN_POINT('Ctrl Pts',(-59.9999999999968,-12.9961202462228,
-176.329584396716));
#152909=CARTESIAN_POINT('Ctrl Pts',(-60.,-12.9956778161511,-174.752013833507));
#152910=CARTESIAN_POINT('Ctrl Pts',(-58.6999592969537,-13.1692782682892,
-177.223689661345));
#152911=CARTESIAN_POINT('Ctrl Pts',(-60.,-13.16751068744,-176.329623133207));
#152912=CARTESIAN_POINT('Ctrl Pts',(-60.,-13.1643444677208,-174.751821305086));
#152913=CARTESIAN_POINT('Ctrl Pts',(-58.6989770498873,-13.3421437200247,
-177.22372531347));
#152914=CARTESIAN_POINT('Ctrl Pts',(-60.,-13.338837622507,-176.329750343386));
#152915=CARTESIAN_POINT('Ctrl Pts',(-60.,-13.3329998199577,-174.75119758399));
#152916=CARTESIAN_POINT('Origin',(0.,-12.9675000200281,-171.64995));
#152917=CARTESIAN_POINT('Ctrl Pts',(-39.532390596256,-6.25584930059378,
-132.186909005141));
#152918=CARTESIAN_POINT('Ctrl Pts',(-39.5154906923694,-7.16492474321995,
-131.82486600692));
#152919=CARTESIAN_POINT('Ctrl Pts',(-39.5012062751564,-8.10027061565897,
-131.522946484679));
#152920=CARTESIAN_POINT('Ctrl Pts',(-39.4801155592828,-9.98786863920294,
-131.0794868627));
#152921=CARTESIAN_POINT('Ctrl Pts',(-39.4733327199609,-10.9147757068085,
-130.938171698301));
#152922=CARTESIAN_POINT('Ctrl Pts',(-39.4702993039609,-11.842906113671,
-130.874975449521));
#152923=CARTESIAN_POINT('Ctrl Pts',(-39.4698735679011,-11.9817787569958,
-130.866104166164));
#152924=CARTESIAN_POINT('Ctrl Pts',(-39.,-11.9280000478899,-129.861650462511));
#152925=CARTESIAN_POINT('Ctrl Pts',(-39.,-11.8686433059622,-128.75301285746));
#152926=CARTESIAN_POINT('Ctrl Pts',(-39.4726650480512,-11.0072303515572,
-130.924266220454));
#152927=CARTESIAN_POINT('Ctrl Pts',(-39.,-10.9001842769389,-129.920145931085));
#152928=CARTESIAN_POINT('Ctrl Pts',(-39.,-10.7823162329457,-128.811175087855));
#152929=CARTESIAN_POINT('Ctrl Pts',(-39.4795992973311,-10.0340735686833,
-131.068631786405));
#152930=CARTESIAN_POINT('Ctrl Pts',(-39.0000000000038,-9.87380260099891,
-130.065440410241));
#152931=CARTESIAN_POINT('Ctrl Pts',(-39.,-9.69789923172707,-128.955540477711));
#152932=CARTESIAN_POINT('Ctrl Pts',(-39.5013352696214,-8.08872573977277,
-131.525658760403));
#152933=CARTESIAN_POINT('Ctrl Pts',(-38.9999999999961,-7.82478234255028,
-130.525007038766));
#152934=CARTESIAN_POINT('Ctrl Pts',(-39.,-7.5328018765656,-129.41256745169));
#152935=CARTESIAN_POINT('Ctrl Pts',(-39.5158343666262,-7.14245811524402,
-131.8321301746));
#152936=CARTESIAN_POINT('Ctrl Pts',(-39.000000000015,-6.82873706011098,
-130.833383690437));
#152937=CARTESIAN_POINT('Ctrl Pts',(-39.,-6.48098994967646,-129.719043469502));
#152938=CARTESIAN_POINT('Ctrl Pts',(-39.5330007209533,-6.22310181331709,
-132.199981346222));
#152939=CARTESIAN_POINT('Ctrl Pts',(-39.,-5.86351575546646,-131.202920178865));
#152940=CARTESIAN_POINT('Ctrl Pts',(-39.,-5.4610240206487,-130.086890037519));
#152941=CARTESIAN_POINT('Ctrl Pts',(-39.,-11.8300000219165,-128.755118230443));
#152942=CARTESIAN_POINT('Ctrl Pts',(-39.,-11.2456383392957,-128.787506003178));
#152943=CARTESIAN_POINT('Ctrl Pts',(-38.9999999999998,-10.6643296819666,
-128.844689763199));
#152944=CARTESIAN_POINT('Ctrl Pts',(-39.0000000000002,-10.0859609278487,
-128.925742270509));
#152945=CARTESIAN_POINT('Ctrl Pts',(-39.0000000000004,-9.71348092877506,
-128.977941559687));
#152946=CARTESIAN_POINT('Ctrl Pts',(-39.0000000000007,-9.34222031417317,
-129.040041718412));
#152947=CARTESIAN_POINT('Ctrl Pts',(-39.0000000000031,-8.97214920379055,
-129.111806478628));
#152948=CARTESIAN_POINT('Ctrl Pts',(-39.0000000000039,-8.85321569986176,
-129.134870247055));
#152949=CARTESIAN_POINT('Ctrl Pts',(-39.0000000000046,-8.73429069407208,
-129.1589539896));
#152950=CARTESIAN_POINT('Ctrl Pts',(-39.0000000000049,-8.61535199981085,
-129.184060813321));
#152951=CARTESIAN_POINT('Ctrl Pts',(-39.0000000000057,-8.3170598050556,
-129.247027450022));
#152952=CARTESIAN_POINT('Ctrl Pts',(-39.0000000000046,-8.02087151391859,
-129.315956118525));
#152953=CARTESIAN_POINT('Ctrl Pts',(-39.0000000000032,-7.72648278144854,
-129.390626430169));
#152954=CARTESIAN_POINT('Ctrl Pts',(-39.0000000000018,-7.42024264682867,
-129.468302793997));
#152955=CARTESIAN_POINT('Ctrl Pts',(-39.0000000000006,-7.11594965101859,
-129.552192661458));
#152956=CARTESIAN_POINT('Ctrl Pts',(-39.0000000000002,-6.81328756599581,
-129.642098960196));
#152957=CARTESIAN_POINT('Ctrl Pts',(-39.,-6.60142553226265,-129.705032945781));
#152958=CARTESIAN_POINT('Ctrl Pts',(-39.,-6.39036319103641,-129.770916038733));
#152959=CARTESIAN_POINT('Ctrl Pts',(-39.,-6.18000018270165,-129.839693348042));
#152960=CARTESIAN_POINT('Origin',(-39.,46.91999998,-129.34995));
#152961=CARTESIAN_POINT('Ctrl Pts',(-58.1727505513103,-4.55147683639116,
-177.246631327017));
#152962=CARTESIAN_POINT('Ctrl Pts',(-59.9999999999999,-4.58657792455373,
-176.471369022158));
#152963=CARTESIAN_POINT('Ctrl Pts',(-60.,-4.67636962353871,-174.488179236421));
#152964=CARTESIAN_POINT('Ctrl Pts',(-58.1991963791488,-4.75453073304115,
-177.244581482931));
#152965=CARTESIAN_POINT('Ctrl Pts',(-60.,-4.78987454640717,-176.45995577904));
#152966=CARTESIAN_POINT('Ctrl Pts',(-60.,-4.88047860745801,-174.497420557097));
#152967=CARTESIAN_POINT('Ctrl Pts',(-58.224696806329,-4.95813196877357,
-177.242671121043));
#152968=CARTESIAN_POINT('Ctrl Pts',(-59.9999999999904,-4.99421808034748,
-176.449490545983));
#152969=CARTESIAN_POINT('Ctrl Pts',(-60.,-5.08458311893969,-174.506824441727));
#152970=CARTESIAN_POINT('Ctrl Pts',(-58.2492435654384,-5.16222748868144,
-177.240889086276));
#152971=CARTESIAN_POINT('Ctrl Pts',(-60.,-5.19940519654632,-176.439881014021));
#152972=CARTESIAN_POINT('Ctrl Pts',(-60.,-5.28868572332295,-174.51629758862));
#152973=CARTESIAN_POINT('Origin',(0.,-12.9675000200281,-171.64995));
#152974=CARTESIAN_POINT('Ctrl Pts',(-39.7525219240432,1.81208306781682,
-137.147133758372));
#152975=CARTESIAN_POINT('Ctrl Pts',(-39.7179607657458,0.808996392073229,
-136.328011452488));
#152976=CARTESIAN_POINT('Ctrl Pts',(-39.6844054587038,-0.224294744540098,
-135.552952869904));
#152977=CARTESIAN_POINT('Ctrl Pts',(-39.6367679612577,-1.84279784212966,
-134.475122839821));
#152978=CARTESIAN_POINT('Ctrl Pts',(-39.6212800791283,-2.39690688691799,
-134.128738792364));
#152979=CARTESIAN_POINT('Ctrl Pts',(-39.5994686586584,-3.23005227649636,
-133.645552385194));
#152980=CARTESIAN_POINT('Ctrl Pts',(-39.5924947647291,-3.50534889940371,
-133.491838360679));
#152981=CARTESIAN_POINT('Ctrl Pts',(-39.5857308656309,-3.78242429107441,
-133.34341275263));
#152982=CARTESIAN_POINT('Ctrl Pts',(-39.5652399075022,-4.65674474020595,
-132.895844604925));
#152983=CARTESIAN_POINT('Ctrl Pts',(-39.,-4.21888391538426,-131.902596984872));
#152984=CARTESIAN_POINT('Ctrl Pts',(-39.,-3.72521479271581,-130.782753296221));
#152985=CARTESIAN_POINT('Ctrl Pts',(-39.5781306671204,-4.08236536173137,
-133.176106520795));
#152986=CARTESIAN_POINT('Ctrl Pts',(-39.,-3.6159206095068,-132.184581657476));
#152987=CARTESIAN_POINT('Ctrl Pts',(-39.,-3.08946624372919,-131.063015115075));
#152988=CARTESIAN_POINT('Ctrl Pts',(-39.5919846958087,-3.51592220196165,
-133.479760839166));
#152989=CARTESIAN_POINT('Ctrl Pts',(-39.,-3.02226593965722,-132.489948109969));
#152990=CARTESIAN_POINT('Ctrl Pts',(-39.,-2.46339239509573,-131.366669530497));
#152991=CARTESIAN_POINT('Ctrl Pts',(-39.6212800791283,-2.39690688691799,
-134.128738792364));
#152992=CARTESIAN_POINT('Ctrl Pts',(-39.,-1.85088554063804,-133.142434340475));
#152993=CARTESIAN_POINT('Ctrl Pts',(-39.,-1.22847641296741,-132.015647483627));
#152994=CARTESIAN_POINT('Ctrl Pts',(-39.6367679612577,-1.84279784212966,
-134.475122839821));
#152995=CARTESIAN_POINT('Ctrl Pts',(-39.,-1.27148303561927,-133.490738119779));
#152996=CARTESIAN_POINT('Ctrl Pts',(-39.,-0.61794440595705,-132.362031531162));
#152997=CARTESIAN_POINT('Ctrl Pts',(-39.6847850431059,-0.21139821211329,
-135.561541219197));
#152998=CARTESIAN_POINT('Ctrl Pts',(-39.,0.433753695599259,-134.583900592971));
#152999=CARTESIAN_POINT('Ctrl Pts',(-39.,1.17663045280609,-133.448449910404));
#153000=CARTESIAN_POINT('Ctrl Pts',(-39.7187663759592,0.83378959624966,
-136.346621542847));
#153001=CARTESIAN_POINT('Ctrl Pts',(-39.,1.52263602949375,-135.373451527487));
#153002=CARTESIAN_POINT('Ctrl Pts',(-39.,2.32236925604725,-134.233515370373));
#153003=CARTESIAN_POINT('Ctrl Pts',(-39.7537665531305,1.84818159949203,
-137.176641147095));
#153004=CARTESIAN_POINT('Ctrl Pts',(-39.,2.57493359537216,-136.206226648817));
#153005=CARTESIAN_POINT('Ctrl Pts',(-39.,3.43069435955708,-135.063549838392));
#153006=CARTESIAN_POINT('Ctrl Pts',(-39.,-3.68000001999998,-130.802732351058));
#153007=CARTESIAN_POINT('Ctrl Pts',(-39.,-3.33509769381514,-130.955490419457));
#153008=CARTESIAN_POINT('Ctrl Pts',(-38.999999999995,-2.99379560771467,
-131.114791966817));
#153009=CARTESIAN_POINT('Ctrl Pts',(-39.0000000000322,-2.65562532357943,
-131.280281718424));
#153010=CARTESIAN_POINT('Ctrl Pts',(-39.0000000000621,-2.38378986674371,
-131.413309321204));
#153011=CARTESIAN_POINT('Ctrl Pts',(-39.0000000001226,-2.11397851849314,
-131.550336634986));
#153012=CARTESIAN_POINT('Ctrl Pts',(-39.0000000002374,-1.84595706992345,
-131.691201637143));
#153013=CARTESIAN_POINT('Ctrl Pts',(-39.0000000003908,-1.48773653906914,
-131.879472897226));
#153014=CARTESIAN_POINT('Ctrl Pts',(-39.0000000006483,-1.13214453284296,
-132.074954501691));
#153015=CARTESIAN_POINT('Ctrl Pts',(-39.0000000009742,-0.77990354390592,
-132.276609948051));
#153016=CARTESIAN_POINT('Ctrl Pts',(-39.0000000012103,-0.524689202150672,
-132.422718332994));
#153017=CARTESIAN_POINT('Ctrl Pts',(-39.000000001479,-0.271234086134615,
-132.572069210975));
#153018=CARTESIAN_POINT('Ctrl Pts',(-39.0000000017246,-0.0198207958907409,
-132.724283330851));
#153019=CARTESIAN_POINT('Ctrl Pts',(-39.0000000020985,0.362997438679579,
-132.956054453974));
#153020=CARTESIAN_POINT('Ctrl Pts',(-39.0000000024107,0.740951650742127,
-133.194233184148));
#153021=CARTESIAN_POINT('Ctrl Pts',(-39.0000000024159,1.11485984244746,
-133.438609986291));
#153022=CARTESIAN_POINT('Ctrl Pts',(-39.00000000242,1.40217712996276,-133.626393194792));
#153023=CARTESIAN_POINT('Ctrl Pts',(-39.0000000022332,1.68710447741373,
-133.817837252074));
#153024=CARTESIAN_POINT('Ctrl Pts',(-39.0000000018622,1.96999998000005,
-134.012863078852));
#153025=CARTESIAN_POINT('Origin',(-39.,46.91999998,-129.34995));
#153026=CARTESIAN_POINT('Origin',(83.2809572255632,2.96999998000007,-176.84995));
#153027=CARTESIAN_POINT('',(-60.,2.96999998000001,-177.34995));
#153028=CARTESIAN_POINT('Origin',(-57.,-2.42462934179819E-14,-174.34995));
#153029=CARTESIAN_POINT('',(-60.,28.41999998,-174.34995));
#153030=CARTESIAN_POINT('',(-57.,-54.58000002,-177.34995));
#153031=CARTESIAN_POINT('Origin',(-60.,-2.55003103885676E-14,0.));
#153032=CARTESIAN_POINT('Origin',(-60.,28.41999998,-177.34995));
#153033=CARTESIAN_POINT('Origin',(0.,-12.9675000200281,-171.64995));
#153034=CARTESIAN_POINT('Ctrl Pts',(-40.0642139728404,9.89540198157303,
-145.11953138824));
#153035=CARTESIAN_POINT('Ctrl Pts',(-40.0183499110469,8.78469917332298,
-143.853535251546));
#153036=CARTESIAN_POINT('Ctrl Pts',(-39.9717745968192,7.64117779462799,
-142.61251748975));
#153037=CARTESIAN_POINT('Ctrl Pts',(-39.925101121935,6.45601873886266,-141.410634166036));
#153038=CARTESIAN_POINT('Ctrl Pts',(-39.8971179105603,5.74545333844114,
-140.69004168436));
#153039=CARTESIAN_POINT('Ctrl Pts',(-39.8692646256818,5.02426042253766,
-139.987850959434));
#153040=CARTESIAN_POINT('Ctrl Pts',(-39.8417723415181,4.28998417285319,
-139.307926707528));
#153041=CARTESIAN_POINT('Ctrl Pts',(-39.,12.1842637898263,-143.052046612136));
#153042=CARTESIAN_POINT('Ctrl Pts',(-39.,10.9256789631914,-144.234640911918));
#153043=CARTESIAN_POINT('Ctrl Pts',(-40.0658654912634,9.93539056346401,
-145.16513792084));
#153044=CARTESIAN_POINT('Ctrl Pts',(-39.,10.979841755805,-141.770231455688));
#153045=CARTESIAN_POINT('Ctrl Pts',(-39.,9.77621097937933,-142.950028280238));
#153046=CARTESIAN_POINT('Ctrl Pts',(-40.0194681925347,8.81214966903568,
-143.883338323671));
#153047=CARTESIAN_POINT('Ctrl Pts',(-39.,9.73492905398707,-140.513855077087));
#153048=CARTESIAN_POINT('Ctrl Pts',(-38.9999999999938,8.58671680832509,
-141.687354928893));
#153049=CARTESIAN_POINT('Ctrl Pts',(-39.9723349230223,7.65540591189065,
-142.62694638584));
#153050=CARTESIAN_POINT('Ctrl Pts',(-39.,7.14197626750154,-138.081230637578));
#153051=CARTESIAN_POINT('Ctrl Pts',(-39.0000000000061,6.11210401876312,
-139.242594351665));
#153052=CARTESIAN_POINT('Ctrl Pts',(-39.8778673208479,5.25663156583475,
-140.194321946232));
#153053=CARTESIAN_POINT('Ctrl Pts',(-39.,5.8072721390059,-136.917329731646));
#153054=CARTESIAN_POINT('Ctrl Pts',(-39.,4.84002931498563,-138.072328953201));
#153055=CARTESIAN_POINT('Ctrl Pts',(-39.831007995706,4.02695578189988,-139.030438856635));
#153056=CARTESIAN_POINT('Ctrl Pts',(-39.,4.42069758591766,-135.824477851673));
#153057=CARTESIAN_POINT('Ctrl Pts',(-39.,3.51696512827391,-136.971103897255));
#153058=CARTESIAN_POINT('Ctrl Pts',(-39.7856126378568,2.75522939862341,
-137.937569160376));
#153059=CARTESIAN_POINT('Ctrl Pts',(-39.,4.46999998000001,-135.863383986541));
#153060=CARTESIAN_POINT('Ctrl Pts',(-39.0000000000005,4.88328157550107,
-136.189917146855));
#153061=CARTESIAN_POINT('Ctrl Pts',(-39.0000000000119,5.29116221661458,
-136.522117224196));
#153062=CARTESIAN_POINT('Ctrl Pts',(-39.0000000000389,5.69434025783345,
-136.859675625829));
#153063=CARTESIAN_POINT('Ctrl Pts',(-39.0000000000669,6.11191405992085,
-137.209286792078));
#153064=CARTESIAN_POINT('Ctrl Pts',(-39.0000000001116,6.52444323385465,
-137.564646050771));
#153065=CARTESIAN_POINT('Ctrl Pts',(-39.0000000001789,6.93266997764253,
-137.925456663921));
#153066=CARTESIAN_POINT('Ctrl Pts',(-39.0000000002504,7.36643947054107,
-138.308843198685));
#153067=CARTESIAN_POINT('Ctrl Pts',(-39.0000000003473,7.79535110451708,
-138.698384855332));
#153068=CARTESIAN_POINT('Ctrl Pts',(-39.0000000004772,8.22026082374413,
-139.093772869082));
#153069=CARTESIAN_POINT('Ctrl Pts',(-39.0000000004994,8.29309080497359,
-139.161542798356));
#153070=CARTESIAN_POINT('Ctrl Pts',(-39.0000000005226,8.36580314364496,
-139.229484583884));
#153071=CARTESIAN_POINT('Ctrl Pts',(-39.0000000005469,8.43840206333326,
-139.297596789496));
#153072=CARTESIAN_POINT('Ctrl Pts',(-39.0000000006997,8.8960899600184,-139.726998938435));
#153073=CARTESIAN_POINT('Ctrl Pts',(-39.0000000008925,9.34761173377698,
-140.161633014643));
#153074=CARTESIAN_POINT('Ctrl Pts',(-39.0000000011355,9.79388080738361,
-140.601330848477));
#153075=CARTESIAN_POINT('Ctrl Pts',(-39.0000000011949,9.90289654250056,
-140.708741344565));
#153076=CARTESIAN_POINT('Ctrl Pts',(-39.0000000012573,10.0115986221443,
-140.816454152322));
#153077=CARTESIAN_POINT('Ctrl Pts',(-39.0000000013228,10.11999998,-140.924467062102));
#153078=CARTESIAN_POINT('Origin',(-39.,46.91999998,-129.34995));
#153079=CARTESIAN_POINT('Origin',(-60.,28.41999998,-177.34995));
#153080=CARTESIAN_POINT('',(-57.,-54.58000002,-177.34995));
#153081=CARTESIAN_POINT('Origin',(-57.,-2.42462934179819E-14,-174.34995));
#153082=CARTESIAN_POINT('Ctrl Pts',(-38.9841065328395,-56.2141391785318,
-61.0006103127042));
#153083=CARTESIAN_POINT('Ctrl Pts',(-40.2048288919875,-54.58000002,-61.850776413383));
#153084=CARTESIAN_POINT('Ctrl Pts',(-42.0182169324382,-54.58000002,-63.1137016214078));
#153085=CARTESIAN_POINT('Ctrl Pts',(-36.4598290914011,-56.1197282395838,
-64.7755113243629));
#153086=CARTESIAN_POINT('Ctrl Pts',(-37.6731521867469,-54.5800000199842,
-65.6186857176609));
#153087=CARTESIAN_POINT('Ctrl Pts',(-39.3891852844759,-54.58000002,-66.8886318537073));
#153088=CARTESIAN_POINT('Ctrl Pts',(-33.8526449461492,-56.018427265929,
-68.5041285748648));
#153089=CARTESIAN_POINT('Ctrl Pts',(-35.039043742113,-54.58000002,-69.3609187351473));
#153090=CARTESIAN_POINT('Ctrl Pts',(-36.6602985783386,-54.58000002,-70.6173011253171));
#153091=CARTESIAN_POINT('Ctrl Pts',(-31.1389734555133,-55.9114071812081,
-72.1061129617773));
#153092=CARTESIAN_POINT('Ctrl Pts',(-32.2647524970408,-54.5800000199999,
-73.0003840144137));
#153093=CARTESIAN_POINT('Ctrl Pts',(-33.7990997127136,-54.58000002,-74.2192042704808));
#153094=CARTESIAN_POINT('Ctrl Pts',(-39.4999999999959,-54.58000002,-66.6681042685264));
#153095=CARTESIAN_POINT('Ctrl Pts',(-37.6706537603941,-54.58000002,-69.204359231621));
#153096=CARTESIAN_POINT('Ctrl Pts',(-35.7938421862428,-54.58000002,-71.7056198678132));
#153097=CARTESIAN_POINT('Ctrl Pts',(-33.8499999999899,-54.58000002,-74.1550953619836));
#153098=CARTESIAN_POINT('Ctrl Pts',(-33.5716649926242,-56.0068714410799,
-68.806691265109));
#153099=CARTESIAN_POINT('Ctrl Pts',(-35.3684223959548,-56.0769674434306,
-66.3189008836144));
#153100=CARTESIAN_POINT('Ctrl Pts',(-37.1195284786874,-56.1442949465457,
-63.7841134204858));
#153101=CARTESIAN_POINT('Ctrl Pts',(-38.8323589160537,-56.2084590974991,
-61.2273337386071));
#153102=CARTESIAN_POINT('Origin',(0.,-12.9675000200281,-60.64995));
#153103=CARTESIAN_POINT('Origin',(-41.5,-73.08000002,-177.34995));
#153104=CARTESIAN_POINT('',(41.5,-70.08000002,-177.34995));
#153105=CARTESIAN_POINT('Origin',(3.3975957231091E-14,-70.08000002,-174.34995));
#153106=CARTESIAN_POINT('',(-41.5,-73.08000002,-174.34995));
#153107=CARTESIAN_POINT('Origin',(3.54807775957937E-14,-73.08000002,3.11172719585489E-30));
#153108=CARTESIAN_POINT('Origin',(-60.,-54.58000002,-55.24995));
#153109=CARTESIAN_POINT('Ctrl Pts',(-33.85,-54.58000002,-157.903547609535));
#153110=CARTESIAN_POINT('Ctrl Pts',(-35.7938424480564,-54.58000002,-160.35302343361));
#153111=CARTESIAN_POINT('Ctrl Pts',(-37.6706534886586,-54.58000002,-162.854283363144));
#153112=CARTESIAN_POINT('Ctrl Pts',(-39.5,-54.58000002,-165.390538702986));
#153113=CARTESIAN_POINT('Ctrl Pts',(-42.1374590345468,-54.58000002,-169.116290576972));
#153114=CARTESIAN_POINT('Ctrl Pts',(-40.320307620846,-54.58000002,-170.379862235888));
#153115=CARTESIAN_POINT('Ctrl Pts',(-39.0986073542357,-56.2184192034566,
-171.229381885675));
#153116=CARTESIAN_POINT('Ctrl Pts',(-39.4714760509134,-54.58000002,-165.282321435755));
#153117=CARTESIAN_POINT('Ctrl Pts',(-37.7530684146655,-54.5800000201611,
-166.553337438667));
#153118=CARTESIAN_POINT('Ctrl Pts',(-36.5384467754252,-56.1227754271583,
-167.395443178417));
#153119=CARTESIAN_POINT('Ctrl Pts',(-36.7030946909167,-54.58000002,-161.495162061412));
#153120=CARTESIAN_POINT('Ctrl Pts',(-35.0808115183431,-54.5800000200163,
-162.752463904168));
#153121=CARTESIAN_POINT('Ctrl Pts',(-33.8932339485135,-56.0200282137318,
-163.608339894981));
#153122=CARTESIAN_POINT('Ctrl Pts',(-33.7983252138975,-54.58000002,-157.838463708057));
#153123=CARTESIAN_POINT('Ctrl Pts',(-32.2640061692936,-54.5800000199999,
-159.057279891091));
#153124=CARTESIAN_POINT('Ctrl Pts',(-31.1382389079697,-55.9113782125501,
-159.951555016761));
#153125=CARTESIAN_POINT('',(-38.9938267385724,-56.214502484065,-171.072567687954));
#153126=CARTESIAN_POINT('Origin',(-42.7058184423063,-60.0992226028014,-170.703547390513));
#153127=CARTESIAN_POINT('Ctrl Pts',(-38.9938273364047,-56.2145025937637,
-171.072567271539));
#153128=CARTESIAN_POINT('Ctrl Pts',(-37.2296100808616,-56.148520626844,
-168.433870605279));
#153129=CARTESIAN_POINT('Ctrl Pts',(-35.4249314550332,-56.0791684505653,
-165.817913090769));
#153130=CARTESIAN_POINT('Ctrl Pts',(-33.5716804653412,-56.0068706353672,
-163.251940550002));
#153131=CARTESIAN_POINT('Ctrl Pts',(-39.4023695343916,-56.667607408721,
-171.60507092612));
#153132=CARTESIAN_POINT('Ctrl Pts',(-39.1191457108045,-56.3534914900074,
-171.473900235605));
#153133=CARTESIAN_POINT('Ctrl Pts',(-38.9938259143948,-56.2145026772597,
-171.07256826174));
#153134=CARTESIAN_POINT('Ctrl Pts',(-39.4667323101199,-56.6069363160445,
-171.604463274963));
#153135=CARTESIAN_POINT('Ctrl Pts',(-39.1873296781659,-56.2851199488468,
-171.471360601804));
#153136=CARTESIAN_POINT('Ctrl Pts',(-39.0656324591812,-56.1451830708436,
-171.065281773562));
#153137=CARTESIAN_POINT('Ctrl Pts',(-39.532372953365,-56.5484198596326,
-171.603842231026));
#153138=CARTESIAN_POINT('Ctrl Pts',(-39.256852764825,-56.2190926208658,
-171.468759835437));
#153139=CARTESIAN_POINT('Ctrl Pts',(-39.1389029748433,-56.0783561940248,
-171.057850262871));
#153140=CARTESIAN_POINT('Ctrl Pts',(-39.59920642547,-56.4919352618991,-171.603208415545));
#153141=CARTESIAN_POINT('Ctrl Pts',(-39.3276146389594,-56.1552707341152,
-171.46610011903));
#153142=CARTESIAN_POINT('Ctrl Pts',(-39.2135563963028,-56.0138844098186,
-171.050282355671));
#153143=CARTESIAN_POINT('Origin',(-39.6007286333569,-56.8876021458077,-170.64995));
#153144=CARTESIAN_POINT('Origin',(0.,-12.9675000200281,-170.64995));
#153145=CARTESIAN_POINT('Origin',(0.,-12.9675000200281,-171.64995));
#153146=CARTESIAN_POINT('Origin',(0.,-12.9675000200281,-171.07256826174));
#153147=CARTESIAN_POINT('Origin',(0.,-12.9675000200281,-171.64995));
#153148=CARTESIAN_POINT('Ctrl Pts',(-42.5,-55.08000002,-60.64995));
#153149=CARTESIAN_POINT('Ctrl Pts',(-42.,-55.08000002,-60.64995));
#153150=CARTESIAN_POINT('Ctrl Pts',(-42.,-55.58000002,-60.64995));
#153151=CARTESIAN_POINT('Ctrl Pts',(-42.5,-54.58000002,-60.64995));
#153152=CARTESIAN_POINT('Ctrl Pts',(-41.5,-54.58000002,-60.64995));
#153153=CARTESIAN_POINT('Ctrl Pts',(-41.5,-55.58000002,-60.64995));
#153154=CARTESIAN_POINT('Ctrl Pts',(-42.5,-54.58000002,-61.14995));
#153155=CARTESIAN_POINT('Ctrl Pts',(-41.5,-54.58000002,-61.14995));
#153156=CARTESIAN_POINT('Ctrl Pts',(-41.5,-55.58000002,-61.14995));
#153157=CARTESIAN_POINT('Origin',(0.,-12.9675000200281,-171.64995));
#153158=CARTESIAN_POINT('Ctrl Pts',(-31.0842854211463,-55.9092502161047,
-159.87997642591));
#153159=CARTESIAN_POINT('Ctrl Pts',(-29.278906722612,-55.8380360188005,
-157.486006234072));
#153160=CARTESIAN_POINT('Ctrl Pts',(-27.4082502462316,-55.7634592463117,
-155.123448236681));
#153161=CARTESIAN_POINT('Ctrl Pts',(-25.4683317949416,-55.6876147613919,
-152.854279668282));
#153162=CARTESIAN_POINT('Ctrl Pts',(-33.7871193355851,-54.58000002,-157.824358608005));
#153163=CARTESIAN_POINT('Ctrl Pts',(-32.2532079260876,-54.58000002,-159.043115862826));
#153164=CARTESIAN_POINT('Ctrl Pts',(-31.1276111727346,-55.910959075446,
-159.937449916708));
#153165=CARTESIAN_POINT('Ctrl Pts',(-31.2221573047513,-54.58000002,-154.596132061548));
#153166=CARTESIAN_POINT('Ctrl Pts',(-29.7951706706339,-54.580000020057,
-155.819252869408));
#153167=CARTESIAN_POINT('Ctrl Pts',(-28.6950259327511,-55.8150212418279,
-156.709250494305));
#153168=CARTESIAN_POINT('Ctrl Pts',(-28.5157861483817,-54.58000002,-151.424072006624));
#153169=CARTESIAN_POINT('Ctrl Pts',(-27.1955413535409,-54.5800000200432,
-152.632731094419));
#153170=CARTESIAN_POINT('Ctrl Pts',(-26.143809437084,-55.7129653866513,
-153.537246733037));
#153171=CARTESIAN_POINT('Ctrl Pts',(-25.6489783375839,-54.58000002,-148.460215214005));
#153172=CARTESIAN_POINT('Ctrl Pts',(-24.4312618773724,-54.5800000199999,
-149.638058579956));
#153173=CARTESIAN_POINT('Ctrl Pts',(-23.4643533331708,-55.6098289013737,
-150.573306522708));
#153174=CARTESIAN_POINT('Ctrl Pts',(-25.7,-54.58000002,-148.513004346424));
#153175=CARTESIAN_POINT('Ctrl Pts',(-27.6634746333275,-54.58000002,-150.546045135875));
#153176=CARTESIAN_POINT('Ctrl Pts',(-29.537631721855,-54.58000002,-152.662307251431));
#153177=CARTESIAN_POINT('Ctrl Pts',(-31.35,-54.58000002,-154.831379798159));
#153178=CARTESIAN_POINT('Origin',(-60.,-54.58000002,-55.24995));
#153179=CARTESIAN_POINT('Ctrl Pts',(-31.3499999999855,-54.58000002,-77.227263173365));
#153180=CARTESIAN_POINT('Ctrl Pts',(-29.5376330958494,-54.58000002,-79.396334075655));
#153181=CARTESIAN_POINT('Ctrl Pts',(-27.6634733215002,-54.58000002,-81.5125991939361));
#153182=CARTESIAN_POINT('Ctrl Pts',(-25.7,-54.58000002,-83.5456386250818));
#153183=CARTESIAN_POINT('Ctrl Pts',(-31.127610916576,-55.9109590653435,
-72.1211933947368));
#153184=CARTESIAN_POINT('Ctrl Pts',(-32.2532076658177,-54.58000002,-73.0155274500394));
#153185=CARTESIAN_POINT('Ctrl Pts',(-33.787119065489,-54.58000002,-74.2342847034403));
#153186=CARTESIAN_POINT('Ctrl Pts',(-28.6950527991335,-55.8150223013088,
-75.3493568083322));
#153187=CARTESIAN_POINT('Ctrl Pts',(-29.7951976773991,-54.58000002,-76.2393546649833));
#153188=CARTESIAN_POINT('Ctrl Pts',(-31.2221856658751,-54.58000002,-77.4624751982426));
#153189=CARTESIAN_POINT('Ctrl Pts',(-26.1438256035288,-55.7129660087519,
-78.5213783677229));
#153190=CARTESIAN_POINT('Ctrl Pts',(-27.1955581318452,-54.5800000200432,
-79.425893713097));
#153191=CARTESIAN_POINT('Ctrl Pts',(-28.5158034471915,-54.58000002,-80.6345530934811));
#153192=CARTESIAN_POINT('Ctrl Pts',(-23.4643531971916,-55.6098288961396,
-81.485336599214));
#153193=CARTESIAN_POINT('Ctrl Pts',(-24.4312617378937,-54.58000002,-82.420584542654));
#153194=CARTESIAN_POINT('Ctrl Pts',(-25.6489781920928,-54.58000002,-83.5984279079175));
#153195=CARTESIAN_POINT('Origin',(0.,-12.9675000200281,-171.64995));
#153196=CARTESIAN_POINT('Origin',(-41.5,-73.08000002,-177.34995));
#153197=CARTESIAN_POINT('',(41.5,-70.08000002,-177.34995));
#153198=CARTESIAN_POINT('Origin',(3.3975957231091E-14,-70.08000002,-174.34995));
#153199=CARTESIAN_POINT('',(-41.5,-73.08000002,-174.34995));
#153200=CARTESIAN_POINT('Origin',(3.54807775957937E-14,-73.08000002,3.11172719585489E-30));
#153201=CARTESIAN_POINT('Origin',(0.,-12.9675000200281,-171.64995));
#153202=CARTESIAN_POINT('Origin',(0.,-12.9675000200281,-60.64995));
#153203=CARTESIAN_POINT('Origin',(0.,-12.9675000200281,-60.64995));
#153204=CARTESIAN_POINT('Ctrl Pts',(-40.5058072670198,20.4819096056616,
-73.2085628001111));
#153205=CARTESIAN_POINT('Ctrl Pts',(-40.5844085651433,22.403893278843,-70.4548680070988));
#153206=CARTESIAN_POINT('Ctrl Pts',(-40.6592141342549,24.2755389287606,
-67.6497302110104));
#153207=CARTESIAN_POINT('Ctrl Pts',(-40.7299249270772,26.1062893712319,
-64.8223085129012));
#153208=CARTESIAN_POINT('Origin',(-60.,28.41999998,-177.34995));
#153209=CARTESIAN_POINT('',(-57.,-54.58000002,-177.34995));
#153210=CARTESIAN_POINT('Origin',(-57.,-2.42462934179819E-14,-174.34995));
#153211=CARTESIAN_POINT('',(-60.,28.41999998,-174.34995));
#153212=CARTESIAN_POINT('Origin',(-60.,-2.55003103885676E-14,0.));
#153213=CARTESIAN_POINT('Ctrl Pts',(-40.7317364547463,26.153205244256,-64.7498326746213));
#153214=CARTESIAN_POINT('Ctrl Pts',(-39.,27.3939818002346,-65.5850914026758));
#153215=CARTESIAN_POINT('Ctrl Pts',(-39.,29.2922016634715,-66.8629239833248));
#153216=CARTESIAN_POINT('Ctrl Pts',(-40.6299764732755,23.5169744919048,
-68.8233420843703));
#153217=CARTESIAN_POINT('Ctrl Pts',(-39.,24.7554556194404,-69.6493391078479));
#153218=CARTESIAN_POINT('Ctrl Pts',(-39.,26.5499956507371,-70.9364700811645));
#153219=CARTESIAN_POINT('Ctrl Pts',(-40.5197426374407,20.7960159162511,
-72.851125470798));
#153220=CARTESIAN_POINT('Ctrl Pts',(-38.9999999999314,22.0110957235223,
-73.6915951012831));
#153221=CARTESIAN_POINT('Ctrl Pts',(-39.,23.7045900978902,-74.9643266004363));
#153222=CARTESIAN_POINT('Ctrl Pts',(-40.401808630759,17.9622434922255,-76.7460261035824));
#153223=CARTESIAN_POINT('Ctrl Pts',(-39.,19.1149982396193,-77.6303175298695));
#153224=CARTESIAN_POINT('Ctrl Pts',(-39.,20.7168512667374,-78.8591174122859));
#153225=CARTESIAN_POINT('Ctrl Pts',(-39.,26.4199999800115,-71.0516396909898));
#153226=CARTESIAN_POINT('Ctrl Pts',(-39.,24.5896727691867,-73.6696133337874));
#153227=CARTESIAN_POINT('Ctrl Pts',(-39.,22.7129807779577,-76.2544280814611));
#153228=CARTESIAN_POINT('Ctrl Pts',(-39.,20.769999979994,-78.7897987614735));
#153229=CARTESIAN_POINT('Origin',(-39.,46.91999998,-129.34995));
#153230=CARTESIAN_POINT('Ctrl Pts',(-39.,20.76999998,-153.26884421004));
#153231=CARTESIAN_POINT('Ctrl Pts',(-39.,22.7129810391408,-155.80421523086));
#153232=CARTESIAN_POINT('Ctrl Pts',(-39.,24.5896725049001,-158.389029259702));
#153233=CARTESIAN_POINT('Ctrl Pts',(-39.,26.4199999800001,-161.0070032805));
#153234=CARTESIAN_POINT('Ctrl Pts',(-39.,29.2922017208088,-165.195719073356));
#153235=CARTESIAN_POINT('Ctrl Pts',(-39.,27.3939818557438,-166.473551654334));
#153236=CARTESIAN_POINT('Ctrl Pts',(-40.731736456874,26.153205299378,-167.30881038206));
#153237=CARTESIAN_POINT('Ctrl Pts',(-39.,26.5499900188717,-161.122164521183));
#153238=CARTESIAN_POINT('Ctrl Pts',(-39.,24.7554502364948,-162.409295569185));
#153239=CARTESIAN_POINT('Ctrl Pts',(-40.6299762644379,23.5169690803201,
-163.235292522563));
#153240=CARTESIAN_POINT('Ctrl Pts',(-39.,23.7045860616975,-157.09431111324));
#153241=CARTESIAN_POINT('Ctrl Pts',(-39.,22.0110917831004,-158.367042514669));
#153242=CARTESIAN_POINT('Ctrl Pts',(-40.5197424781718,20.796012087217,-159.207512241208));
#153243=CARTESIAN_POINT('Ctrl Pts',(-39.,20.7168513145423,-153.199525621538));
#153244=CARTESIAN_POINT('Ctrl Pts',(-39.,19.1149982856394,-154.428325504224));
#153245=CARTESIAN_POINT('Ctrl Pts',(-40.4018086326459,17.9622435375657,
-155.312616930242));
#153246=CARTESIAN_POINT('Ctrl Pts',(-40.7299249270775,26.1062893712214,
-167.236334458579));
#153247=CARTESIAN_POINT('Ctrl Pts',(-40.6592140226013,24.2755360362191,
-164.408908292578));
#153248=CARTESIAN_POINT('Ctrl Pts',(-40.5844084705175,22.4038909152615,
-161.603771549441));
#153249=CARTESIAN_POINT('Ctrl Pts',(-40.5058072685341,20.48190961327,-158.850080166024));
#153250=CARTESIAN_POINT('Origin',(0.,-12.9675000200281,-171.64995));
#153251=CARTESIAN_POINT('Origin',(0.,-12.9675000200281,-171.07256826174));
#153252=CARTESIAN_POINT('Origin',(0.,-12.9675000200281,-170.64995));
#153253=CARTESIAN_POINT('Origin',(0.,-12.9675000200281,-171.64995));
#153254=CARTESIAN_POINT('Origin',(0.,-12.9675000200281,-171.64995));
#153255=CARTESIAN_POINT('Origin',(0.,-12.9675000200281,-170.64995));
#153256=CARTESIAN_POINT('Origin',(0.,-12.9675000200281,-171.64995));
#153257=CARTESIAN_POINT('Origin',(0.,-12.9675000200281,-171.07256826174));
#153258=CARTESIAN_POINT('Origin',(0.,-12.9675000200281,-171.64995));
#153259=CARTESIAN_POINT('Ctrl Pts',(-40.4031453084766,17.9943647936175,
-155.356778662625));
#153260=CARTESIAN_POINT('Ctrl Pts',(-40.352516489763,16.7776395477168,-153.683470409173));
#153261=CARTESIAN_POINT('Ctrl Pts',(-40.3002588807393,15.5341707784358,
-152.02728304762));
#153262=CARTESIAN_POINT('Ctrl Pts',(-40.2466286890062,14.2587895844586,
-150.39951644339));
#153263=CARTESIAN_POINT('Ctrl Pts',(-40.2205532005948,13.6386876144874,
-149.608081472651));
#153264=CARTESIAN_POINT('Ctrl Pts',(-40.194198830347,13.0122318389436,-148.824806848577));
#153265=CARTESIAN_POINT('Ctrl Pts',(-40.1676234671339,12.3782653572084,
-148.051087554039));
#153266=CARTESIAN_POINT('Ctrl Pts',(-39.,20.7969022442792,-153.303957440565));
#153267=CARTESIAN_POINT('Ctrl Pts',(-39.,19.1920625442621,-154.533208999946));
#153268=CARTESIAN_POINT('Ctrl Pts',(-40.4049679555898,18.0381725147214,
-155.417048749269));
#153269=CARTESIAN_POINT('Ctrl Pts',(-39.,19.4994946787828,-151.61013720275));
#153270=CARTESIAN_POINT('Ctrl Pts',(-38.9999999999926,17.9467387756658,
-152.837123072001));
#153271=CARTESIAN_POINT('Ctrl Pts',(-40.3537709661131,16.8074898953919,
-153.723238579969));
#153272=CARTESIAN_POINT('Ctrl Pts',(-39.,18.1688145972663,-149.933732593));
#153273=CARTESIAN_POINT('Ctrl Pts',(-39.,16.6677293129161,-151.153378312361));
#153274=CARTESIAN_POINT('Ctrl Pts',(-40.3009026952457,15.549481350471,-152.046823901733));
#153275=CARTESIAN_POINT('Ctrl Pts',(-39.,15.4269724929124,-146.639117676373));
#153276=CARTESIAN_POINT('Ctrl Pts',(-39.,14.0355026731613,-147.843763736059));
#153277=CARTESIAN_POINT('Ctrl Pts',(-40.1923546827668,12.9680978184463,
-148.752208985047));
#153278=CARTESIAN_POINT('Ctrl Pts',(-39.,14.0212803181596,-145.027145257042));
#153279=CARTESIAN_POINT('Ctrl Pts',(-39.0000000000223,12.6882757758116,
-146.224143705887));
#153280=CARTESIAN_POINT('Ctrl Pts',(-40.1368768832445,11.6498727042044,
-147.140254909589));
#153281=CARTESIAN_POINT('Ctrl Pts',(-39.,12.5683345334111,-143.463140153395));
#153282=CARTESIAN_POINT('Ctrl Pts',(-39.,11.293230102484,-144.64769997634));
#153283=CARTESIAN_POINT('Ctrl Pts',(-40.0806897728025,10.2937241351084,
-145.576231462098));
#153284=CARTESIAN_POINT('Ctrl Pts',(-39.,12.61999998,-143.518796834034));
#153285=CARTESIAN_POINT('Ctrl Pts',(-39.0000000000004,13.1830701012425,
-144.125823176785));
#153286=CARTESIAN_POINT('Ctrl Pts',(-39.000000000008,13.7383356437293,-144.739255401572));
#153287=CARTESIAN_POINT('Ctrl Pts',(-39.0000000000126,14.2868563031727,
-145.358644195211));
#153288=CARTESIAN_POINT('Ctrl Pts',(-39.0000000000176,14.874877526446,-146.022636972598));
#153289=CARTESIAN_POINT('Ctrl Pts',(-39.0000000000202,15.4551472634138,
-146.693475297455));
#153290=CARTESIAN_POINT('Ctrl Pts',(-39.0000000000369,16.0289279109256,
-147.370648869846));
#153291=CARTESIAN_POINT('Ctrl Pts',(-39.0000000000444,16.2865138368672,
-147.674650725649));
#153292=CARTESIAN_POINT('Ctrl Pts',(-39.000000000055,16.5427914446669,-147.979929896415));
#153293=CARTESIAN_POINT('Ctrl Pts',(-39.0000000000741,16.7978726164159,
-148.286442551932));
#153294=CARTESIAN_POINT('Ctrl Pts',(-39.0000000001113,17.2936331206748,
-148.88216221097));
#153295=CARTESIAN_POINT('Ctrl Pts',(-39.0000000001696,17.7841600789861,
-149.481724824065));
#153296=CARTESIAN_POINT('Ctrl Pts',(-39.0000000003777,18.2699999799999,
-150.084863924608));
#153297=CARTESIAN_POINT('Origin',(-39.,46.91999998,-129.34995));
#153298=CARTESIAN_POINT('Ctrl Pts',(-39.000000000374,18.2699999799838,-81.9737790469184));
#153299=CARTESIAN_POINT('Ctrl Pts',(-39.0000000001679,17.7841524775854,
-82.5769275834792));
#153300=CARTESIAN_POINT('Ctrl Pts',(-39.0000000001103,17.2936169434169,
-83.1765007297742));
#153301=CARTESIAN_POINT('Ctrl Pts',(-39.0000000000735,16.7978518736795,
-83.7722255217958));
#153302=CARTESIAN_POINT('Ctrl Pts',(-39.0000000000309,16.2234293967169,
-84.462467193728));
#153303=CARTESIAN_POINT('Ctrl Pts',(-39.0000000000258,15.6429390502857,
-85.1464596076279));
#153304=CARTESIAN_POINT('Ctrl Pts',(-39.0000000000195,15.0550950356354,
-85.8236901162035));
#153305=CARTESIAN_POINT('Ctrl Pts',(-39.0000000000137,14.5092314506924,
-86.4525567271254));
#153306=CARTESIAN_POINT('Ctrl Pts',(-39.0000000000098,13.957027196594,-87.0755929306387));
#153307=CARTESIAN_POINT('Ctrl Pts',(-39.0000000000048,13.3974208289947,
-87.6923562596142));
#153308=CARTESIAN_POINT('Ctrl Pts',(-39.0000000000025,13.1398841264358,
-87.9761971935281));
#153309=CARTESIAN_POINT('Ctrl Pts',(-39.0000000000002,12.8807792236243,
-88.2587090915689));
#153310=CARTESIAN_POINT('Ctrl Pts',(-39.,12.61999998,-88.5398461374725));
#153311=CARTESIAN_POINT('Ctrl Pts',(-40.4049679656207,18.0381727558475,
-76.6415938903714));
#153312=CARTESIAN_POINT('Ctrl Pts',(-39.,19.1920627889827,-77.5254336382597));
#153313=CARTESIAN_POINT('Ctrl Pts',(-39.,20.796902498477,-78.7546851990749));
#153314=CARTESIAN_POINT('Ctrl Pts',(-40.3537711092786,16.8074933352464,
-78.3353996644624));
#153315=CARTESIAN_POINT('Ctrl Pts',(-39.0000000000074,17.9467422700577,
-79.2215151478833));
#153316=CARTESIAN_POINT('Ctrl Pts',(-39.,19.4994983593746,-80.4485009715931));
#153317=CARTESIAN_POINT('Ctrl Pts',(-40.3009014559381,15.5494518783308,
-80.0118574083956));
#153318=CARTESIAN_POINT('Ctrl Pts',(-39.,16.6676992320686,-80.9053032515377));
#153319=CARTESIAN_POINT('Ctrl Pts',(-39.,18.1687833493074,-82.1249487171281));
#153320=CARTESIAN_POINT('Ctrl Pts',(-40.1923542727721,12.9680880684791,
-83.3064457069268));
#153321=CARTESIAN_POINT('Ctrl Pts',(-39.,14.0354926345166,-84.2148910918098));
#153322=CARTESIAN_POINT('Ctrl Pts',(-39.,15.4269620807205,-85.4195370156013));
#153323=CARTESIAN_POINT('Ctrl Pts',(-40.136876773061,11.6498700440212,-84.9183911253513));
#153324=CARTESIAN_POINT('Ctrl Pts',(-39.,12.6882730287539,-85.8345023651596));
#153325=CARTESIAN_POINT('Ctrl Pts',(-39.,14.0212774653657,-87.0315007804442));
#153326=CARTESIAN_POINT('Ctrl Pts',(-40.0806897769273,10.2937242346666,
-86.4824113945889));
#153327=CARTESIAN_POINT('Ctrl Pts',(-39.,11.2932302045755,-87.4109428798));
#153328=CARTESIAN_POINT('Ctrl Pts',(-39.,12.5683346400766,-88.5955027032924));
#153329=CARTESIAN_POINT('Origin',(0.,-12.9675000200281,-171.64995));
#153330=CARTESIAN_POINT('Origin',(-60.,28.41999998,-177.34995));
#153331=CARTESIAN_POINT('',(-57.,-54.58000002,-177.34995));
#153332=CARTESIAN_POINT('Origin',(-57.,-2.42462934179819E-14,-174.34995));
#153333=CARTESIAN_POINT('',(-60.,28.41999998,-174.34995));
#153334=CARTESIAN_POINT('Origin',(-60.,-2.55003103885676E-14,0.));
#153335=CARTESIAN_POINT('Ctrl Pts',(-39.,-46.9678746292626,-78.4459379002929));
#153336=CARTESIAN_POINT('Ctrl Pts',(-39.,-45.3542557512738,-77.2153536750926));
#153337=CARTESIAN_POINT('Ctrl Pts',(-40.4142759779013,-44.1970573566106,
-76.3328465915894));
#153338=CARTESIAN_POINT('Ctrl Pts',(-39.,-45.6681795295713,-80.1501792727118));
#153339=CARTESIAN_POINT('Ctrl Pts',(-38.9999999999777,-44.1065399853887,
-78.9218422882493));
#153340=CARTESIAN_POINT('Ctrl Pts',(-40.3630303964688,-42.9636869888089,
-78.0370779308685));
#153341=CARTESIAN_POINT('Ctrl Pts',(-39.,-44.3354733849924,-81.8371103170565));
#153342=CARTESIAN_POINT('Ctrl Pts',(-39.0000000000075,-42.8253754175223,
-80.6161315734671));
#153343=CARTESIAN_POINT('Ctrl Pts',(-40.3100980841279,-41.7032148714377,
-79.7240190083239));
#153344=CARTESIAN_POINT('Ctrl Pts',(-39.,-41.5900648068412,-85.1534256657242));
#153345=CARTESIAN_POINT('Ctrl Pts',(-38.9999999999925,-40.1892936959721,
-83.9475037984034));
#153346=CARTESIAN_POINT('Ctrl Pts',(-40.2013644254228,-39.117307479239,
-83.0403343570498));
#153347=CARTESIAN_POINT('Ctrl Pts',(-39.,-40.1827113458493,-86.7766805524391));
#153348=CARTESIAN_POINT('Ctrl Pts',(-39.0000000000224,-38.8402604870948,
-85.5784283533127));
#153349=CARTESIAN_POINT('Ctrl Pts',(-40.1457604305377,-37.7969103286269,
-84.6635709993291));
#153350=CARTESIAN_POINT('Ctrl Pts',(-39.,-38.7282817023213,-88.3525652913338));
#153351=CARTESIAN_POINT('Ctrl Pts',(-38.9999999999999,-37.4435485041586,
-87.1668478324999));
#153352=CARTESIAN_POINT('Ctrl Pts',(-40.0893978453286,-36.4387324215761,
-86.2394739826303));
#153353=CARTESIAN_POINT('Ctrl Pts',(-39.,-38.7800000199999,-88.296486260558));
#153354=CARTESIAN_POINT('Ctrl Pts',(-39.0000000000004,-39.3488675990385,
-87.6791933887653));
#153355=CARTESIAN_POINT('Ctrl Pts',(-39.0000000000079,-39.9098343204478,
-87.055447933957));
#153356=CARTESIAN_POINT('Ctrl Pts',(-39.0000000000125,-40.4639767641388,
-86.4257067262301));
#153357=CARTESIAN_POINT('Ctrl Pts',(-39.0000000000174,-41.0582242765977,
-85.75038912433));
#153358=CARTESIAN_POINT('Ctrl Pts',(-39.0000000000199,-41.6446237826485,
-85.0681763071405));
#153359=CARTESIAN_POINT('Ctrl Pts',(-39.0000000000371,-42.2244596706239,
-84.3795886418692));
#153360=CARTESIAN_POINT('Ctrl Pts',(-39.0000000000445,-42.4717173644235,
-84.0859562510071));
#153361=CARTESIAN_POINT('Ctrl Pts',(-39.0000000000547,-42.7177810382264,
-83.7911641691168));
#153362=CARTESIAN_POINT('Ctrl Pts',(-39.0000000000728,-42.9627483114232,
-83.4952507849665));
#153363=CARTESIAN_POINT('Ctrl Pts',(-39.0000000001092,-43.4568057616665,
-82.8984436680065));
#153364=CARTESIAN_POINT('Ctrl Pts',(-39.0000000001663,-43.9457116736056,
-82.2978701296067));
#153365=CARTESIAN_POINT('Ctrl Pts',(-39.0000000003688,-44.43000002,-81.6937887068282));
#153366=CARTESIAN_POINT('Origin',(-39.,46.91999998,-129.34995));
#153367=CARTESIAN_POINT('Ctrl Pts',(-39.0000000003644,-44.4300000199906,
-150.364854264666));
#153368=CARTESIAN_POINT('Ctrl Pts',(-39.0000000001644,-43.9457023551939,
-149.760761216984));
#153369=CARTESIAN_POINT('Ctrl Pts',(-39.000000000108,-43.4567859620687,
-149.160174741698));
#153370=CARTESIAN_POINT('Ctrl Pts',(-39.0000000000721,-42.9627229131801,
-148.563361289672));
#153371=CARTESIAN_POINT('Ctrl Pts',(-39.0000000000298,-42.3819947837029,
-147.861859000802));
#153372=CARTESIAN_POINT('Ctrl Pts',(-39.000000000025,-41.795103731089,-147.166651435239));
#153373=CARTESIAN_POINT('Ctrl Pts',(-39.0000000000189,-41.2007410723699,
-146.478263131247));
#153374=CARTESIAN_POINT('Ctrl Pts',(-39.0000000000133,-40.6489795609292,
-145.839215294884));
#153375=CARTESIAN_POINT('Ctrl Pts',(-39.0000000000093,-40.0907793123423,
-145.206044014044));
#153376=CARTESIAN_POINT('Ctrl Pts',(-39.0000000000044,-39.5250612454855,
-144.579200831309));
#153377=CARTESIAN_POINT('Ctrl Pts',(-39.0000000000023,-39.2781704674615,
-144.305633819486));
#153378=CARTESIAN_POINT('Ctrl Pts',(-39.0000000000002,-39.0298473782501,
-144.033272518857));
#153379=CARTESIAN_POINT('Ctrl Pts',(-39.,-38.7800000199999,-143.762156710948));
#153380=CARTESIAN_POINT('Ctrl Pts',(-40.4142759901646,-44.1970576517619,
-155.725796787747));
#153381=CARTESIAN_POINT('Ctrl Pts',(-38.9999999999999,-45.3542560507482,
-154.843289706001));
#153382=CARTESIAN_POINT('Ctrl Pts',(-39.,-46.9678749402838,-153.612705479043));
#153383=CARTESIAN_POINT('Ctrl Pts',(-40.3630305742695,-42.9636912658246,
-154.021570941673));
#153384=CARTESIAN_POINT('Ctrl Pts',(-39.,-44.1065443282322,-153.136806613681));
#153385=CARTESIAN_POINT('Ctrl Pts',(-39.,-45.668184102287,-151.908469685114));
#153386=CARTESIAN_POINT('Ctrl Pts',(-40.3100965640753,-41.7031787097929,
-152.33457670764));
#153387=CARTESIAN_POINT('Ctrl Pts',(-39.0000000000074,-42.8253385188873,
-151.442463829735));
#153388=CARTESIAN_POINT('Ctrl Pts',(-39.,-44.3354350613925,-150.221485398912));
#153389=CARTESIAN_POINT('Ctrl Pts',(-40.2013639252015,-39.117295594665,
-149.018294252799));
#153390=CARTESIAN_POINT('Ctrl Pts',(-38.9999999999925,-40.1892814621382,
-148.11112464401));
#153391=CARTESIAN_POINT('Ctrl Pts',(-39.,-41.5900521206853,-146.90520294412));
#153392=CARTESIAN_POINT('Ctrl Pts',(-40.1457602981154,-37.7969071359042,
-147.395068273086));
#153393=CARTESIAN_POINT('Ctrl Pts',(-39.,-38.8402571910301,-146.480210875403));
#153394=CARTESIAN_POINT('Ctrl Pts',(-39.,-40.1827079235241,-145.281958716849));
#153395=CARTESIAN_POINT('Ctrl Pts',(-40.0893978502897,-36.4387325411231,
-145.819169127587));
#153396=CARTESIAN_POINT('Ctrl Pts',(-38.9999999999999,-37.4435486267092,
-144.891795278378));
#153397=CARTESIAN_POINT('Ctrl Pts',(-39.,-38.728281830342,-143.706077818883));
#153398=CARTESIAN_POINT('Ctrl Pts',(-40.1769969654089,-38.5367854528866,
-148.32464784256));
#153399=CARTESIAN_POINT('Ctrl Pts',(-40.2034881200521,-39.168290402203,
-149.099701330404));
#153400=CARTESIAN_POINT('Ctrl Pts',(-40.2297509497426,-39.7923967253814,
-149.884082045736));
#153401=CARTESIAN_POINT('Ctrl Pts',(-40.2557302446384,-40.410237152229,
-150.67643548022));
#153402=CARTESIAN_POINT('Ctrl Pts',(-40.3094516567182,-41.6878415022836,
-152.314907407094));
#153403=CARTESIAN_POINT('Ctrl Pts',(-40.3617745388197,-42.9337816491534,
-153.981551875682));
#153404=CARTESIAN_POINT('Ctrl Pts',(-40.4124516185963,-44.1531546492747,
-155.665156176616));
#153405=CARTESIAN_POINT('Origin',(0.,-12.9675000200281,-171.64995));
#153406=CARTESIAN_POINT('Origin',(0.,-12.9675000200281,-171.07256826174));
#153407=CARTESIAN_POINT('Origin',(0.,-12.9675000200281,-170.64995));
#153408=CARTESIAN_POINT('Origin',(0.,-12.9675000200281,-171.64995));
#153409=CARTESIAN_POINT('Origin',(-60.,28.41999998,-177.34995));
#153410=CARTESIAN_POINT('',(-57.,-54.58000002,-177.34995));
#153411=CARTESIAN_POINT('Origin',(-57.,-2.42462934179819E-14,-174.34995));
#153412=CARTESIAN_POINT('',(-60.,28.41999998,-174.34995));
#153413=CARTESIAN_POINT('Origin',(-60.,-2.55003103885676E-14,0.));
#153414=CARTESIAN_POINT('Origin',(0.,-12.9675000200281,-171.64995));
#153415=CARTESIAN_POINT('Origin',(0.,-12.9675000200281,-171.64995));
#153416=CARTESIAN_POINT('Origin',(0.,-12.9675000200281,-170.64995));
#153417=CARTESIAN_POINT('Origin',(0.,-12.9675000200281,-171.07256826174));
#153418=CARTESIAN_POINT('Origin',(0.,-12.9675000200281,-171.64995));
#153419=CARTESIAN_POINT('Ctrl Pts',(-40.5149617844426,-46.6408003024225,
-159.171515337561));
#153420=CARTESIAN_POINT('Ctrl Pts',(-40.5934042533475,-48.5623552413193,
-161.934081688328));
#153421=CARTESIAN_POINT('Ctrl Pts',(-40.668031895784,-50.4341179794481,
-164.747447196893));
#153422=CARTESIAN_POINT('Ctrl Pts',(-40.7385684573717,-52.2653908962638,
-167.582872566557));
#153423=CARTESIAN_POINT('Ctrl Pts',(-40.7403779325784,-52.3123829231466,
-167.655650590757));
#153424=CARTESIAN_POINT('Ctrl Pts',(-39.,-53.5547145065899,-166.821728771562));
#153425=CARTESIAN_POINT('Ctrl Pts',(-39.,-55.460351966619,-165.542559282053));
#153426=CARTESIAN_POINT('Ctrl Pts',(-40.6387326052879,-49.6718481371244,
-163.565128292503));
#153427=CARTESIAN_POINT('Ctrl Pts',(-38.9999999999999,-50.9123394210222,
-162.740555198018));
#153428=CARTESIAN_POINT('Ctrl Pts',(-39.,-52.7145421899793,-161.452000516006));
#153429=CARTESIAN_POINT('Ctrl Pts',(-40.5285982996977,-46.9471996283483,
-159.51999555488));
#153430=CARTESIAN_POINT('Ctrl Pts',(-38.9999999999311,-48.1648205365349,
-158.680980229719));
#153431=CARTESIAN_POINT('Ctrl Pts',(-39.,-49.8662825279046,-157.406795875704));
#153432=CARTESIAN_POINT('Ctrl Pts',(-40.4106852206046,-44.110656513925,
-155.606501037481));
#153433=CARTESIAN_POINT('Ctrl Pts',(-39.,-45.2665850600662,-154.723479509065));
#153434=CARTESIAN_POINT('Ctrl Pts',(-39.,-46.8768207417856,-153.493409728778));
#153435=CARTESIAN_POINT('Ctrl Pts',(-39.,-52.5800000199845,-161.329336741015));
#153436=CARTESIAN_POINT('Ctrl Pts',(-39.,-50.7492254978239,-158.702450591995));
#153437=CARTESIAN_POINT('Ctrl Pts',(-39.,-48.8724582313882,-156.108353723945));
#153438=CARTESIAN_POINT('Ctrl Pts',(-39.,-46.9300000199928,-153.563058845201));
#153439=CARTESIAN_POINT('Origin',(-39.,46.91999998,-129.34995));
#153440=CARTESIAN_POINT('Ctrl Pts',(-39.,-46.93000002,-78.4955841262963));
#153441=CARTESIAN_POINT('Ctrl Pts',(-39.,-48.8725599414451,-75.9501559720627));
#153442=CARTESIAN_POINT('Ctrl Pts',(-39.,-50.7491289418203,-73.3563309228582));
#153443=CARTESIAN_POINT('Ctrl Pts',(-39.,-52.58000002,-70.7293062304687));
#153444=CARTESIAN_POINT('Ctrl Pts',(-39.,-55.4603726203092,-66.5160529206996));
#153445=CARTESIAN_POINT('Ctrl Pts',(-39.,-53.5547345046268,-65.2368833127815));
#153446=CARTESIAN_POINT('Ctrl Pts',(-40.7403786971506,-52.3124027851469,
-64.4029616119961));
#153447=CARTESIAN_POINT('Ctrl Pts',(-39.,-52.7124559353729,-70.609751474253));
#153448=CARTESIAN_POINT('Ctrl Pts',(-38.9999999999999,-50.9103452005084,
-69.3211688367401));
#153449=CARTESIAN_POINT('Ctrl Pts',(-40.6386554420727,-49.6698429482511,
-68.4966218848756));
#153450=CARTESIAN_POINT('Ctrl Pts',(-39.,-49.8653057974222,-74.6531246748237));
#153451=CARTESIAN_POINT('Ctrl Pts',(-39.,-48.1638674451749,-73.378963184763));
#153452=CARTESIAN_POINT('Ctrl Pts',(-40.5285598162873,-46.9462740729553,
-72.5399234557376));
#153453=CARTESIAN_POINT('Ctrl Pts',(-39.,-46.8768348378863,-78.5652147900786));
#153454=CARTESIAN_POINT('Ctrl Pts',(-39.,-45.266598631985,-77.3351449301694));
#153455=CARTESIAN_POINT('Ctrl Pts',(-40.4106857765804,-44.1106698886037,
-76.4521234813751));
#153456=CARTESIAN_POINT('Ctrl Pts',(-40.7385684580933,-52.265390901695,
-64.4757704085913));
#153457=CARTESIAN_POINT('Ctrl Pts',(-40.6679883556503,-50.4329865209081,
-67.3129485767829));
#153458=CARTESIAN_POINT('Ctrl Pts',(-40.5933737163056,-48.561586044698,
-70.1257010194362));
#153459=CARTESIAN_POINT('Ctrl Pts',(-40.5149627320849,-46.6408090593808,
-72.8871337536569));
#153460=CARTESIAN_POINT('Origin',(0.,-12.9675000200281,-60.64995));
#153461=CARTESIAN_POINT('Origin',(-60.,28.41999998,-177.34995));
#153462=CARTESIAN_POINT('',(-57.,-54.58000002,-177.34995));
#153463=CARTESIAN_POINT('Origin',(-57.,-2.42462934179819E-14,-174.34995));
#153464=CARTESIAN_POINT('',(-60.,28.41999998,-174.34995));
#153465=CARTESIAN_POINT('Origin',(-60.,-2.55003103885676E-14,0.));
#153466=CARTESIAN_POINT('Origin',(0.,-12.9675000200281,-171.64995));
#153467=CARTESIAN_POINT('Origin',(0.,-12.9675000200281,-171.64995));
#153468=CARTESIAN_POINT('',(50.9867892914962,-42.9264785869994,-171.64995));
#153469=CARTESIAN_POINT('',(50.0729884546894,-44.43000002,-171.64995));
#153470=CARTESIAN_POINT('Origin',(0.,-12.9675000200281,-171.64995));
#153471=CARTESIAN_POINT('',(50.7754831343094,-44.43000002,-171.64995));
#153472=CARTESIAN_POINT('',(50.7052127169582,-44.43000002,-171.64995));
#153473=CARTESIAN_POINT('',(51.3476245933058,-40.3590020057362,-171.64995));
#153474=CARTESIAN_POINT('Origin',(60.,-2.55003103885676E-14,0.));
#153475=CARTESIAN_POINT('',(60.,-45.43000002,-58.24995));
#153476=CARTESIAN_POINT('',(60.,-45.93000002,-58.24995));
#153477=CARTESIAN_POINT('',(60.,-54.58000002,-58.24995));
#153478=CARTESIAN_POINT('',(60.,-45.93000002,-174.34995));
#153479=CARTESIAN_POINT('',(60.,-45.93000002,-174.34995));
#153480=CARTESIAN_POINT('',(60.,-45.43000002,-174.34995));
#153481=CARTESIAN_POINT('',(60.,28.41999998,-174.34995));
#153482=CARTESIAN_POINT('',(60.,-45.43000002,-58.24995));
#153483=CARTESIAN_POINT('Origin',(57.,-2.42462934179819E-14,-174.34995));
#153484=CARTESIAN_POINT('',(57.,-45.93000002,-177.34995));
#153485=CARTESIAN_POINT('Origin',(57.,-45.93000002,-174.34995));
#153486=CARTESIAN_POINT('',(57.,-45.43000002,-177.34995));
#153487=CARTESIAN_POINT('',(57.,-54.58000002,-177.34995));
#153488=CARTESIAN_POINT('Origin',(57.,-45.43000002,-174.34995));
#153489=CARTESIAN_POINT('Origin',(60.,28.41999998,-177.34995));
#153490=CARTESIAN_POINT('',(52.0794132410337,-45.93000002,-177.34995));
#153491=CARTESIAN_POINT('',(60.,-45.93000002,-177.34995));
#153492=CARTESIAN_POINT('',(52.1496836583849,-45.43000002,-177.34995));
#153493=CARTESIAN_POINT('',(62.4796469926385,28.0715083218873,-177.34995));
#153494=CARTESIAN_POINT('',(60.,-45.43000002,-177.34995));
#153495=CARTESIAN_POINT('Origin',(0.,-12.9675000200281,-60.64995));
#153496=CARTESIAN_POINT('',(40.7385684290383,-52.2653907132467,-64.4757702425922));
#153497=CARTESIAN_POINT('',(40.5149254648566,-46.6404784163578,-72.8869718390768));
#153498=CARTESIAN_POINT('Ctrl Pts',(40.7385684580933,-52.265390901695,-64.4757704085913));
#153499=CARTESIAN_POINT('Ctrl Pts',(40.7211666822863,-51.8136050708653,
-65.175286797751));
#153500=CARTESIAN_POINT('Ctrl Pts',(40.7037330721709,-51.3649633742573,
-65.8647723839272));
#153501=CARTESIAN_POINT('Ctrl Pts',(40.6862834285501,-50.9193769960497,
-66.5441356808015));
#153502=CARTESIAN_POINT('Ctrl Pts',(40.6682155292875,-50.4580031153458,
-67.2475693942546));
#153503=CARTESIAN_POINT('Ctrl Pts',(40.6501304434355,-49.9999049480625,
-67.940150902046));
#153504=CARTESIAN_POINT('Ctrl Pts',(40.6320442475958,-49.5449972740905,
-68.6218329826322));
#153505=CARTESIAN_POINT('Ctrl Pts',(40.6135558867345,-49.0799742637535,
-69.3186729599381));
#153506=CARTESIAN_POINT('Ctrl Pts',(40.5950663659317,-48.618285303638,-70.0041236119615));
#153507=CARTESIAN_POINT('Ctrl Pts',(40.5765913348633,-48.1598519228023,
-70.6781879312868));
#153508=CARTESIAN_POINT('Ctrl Pts',(40.5575179493113,-47.6865711694347,
-71.3740833049765));
#153509=CARTESIAN_POINT('Ctrl Pts',(40.5384600096633,-47.2167603716574,
-72.057843011644));
#153510=CARTESIAN_POINT('Ctrl Pts',(40.5194331080602,-46.7503450984622,
-72.729523983642));
#153511=CARTESIAN_POINT('Ctrl Pts',(40.5179427908006,-46.7138122595236,
-72.7821346380918));
#153512=CARTESIAN_POINT('Ctrl Pts',(40.5164526631504,-46.6773002579314,
-72.8346712140457));
#153513=CARTESIAN_POINT('Ctrl Pts',(40.5149627321913,-46.6408090606421,
-72.887133751753));
#153514=CARTESIAN_POINT('',(47.3503956976423,-46.6672397853475,-61.2273317382593));
#153515=CARTESIAN_POINT('Ctrl Pts',(40.5149864073608,-46.6403532458042,
-72.8868173744763));
#153516=CARTESIAN_POINT('Ctrl Pts',(41.0609560613025,-46.6426501090734,
-71.9832291349818));
#153517=CARTESIAN_POINT('Ctrl Pts',(41.6128385796135,-46.644935702693,-71.0626686770773));
#153518=CARTESIAN_POINT('Ctrl Pts',(42.170607592867,-46.6472077166882,-70.1250927592573));
#153519=CARTESIAN_POINT('Ctrl Pts',(42.7172794741845,-46.649434527672,-69.2061704478816));
#153520=CARTESIAN_POINT('Ctrl Pts',(43.269605809916,-46.6516482924861,-68.2709029203465));
#153521=CARTESIAN_POINT('Ctrl Pts',(43.8276034398616,-46.6538471636059,
-67.3192749993308));
#153522=CARTESIAN_POINT('Ctrl Pts',(44.4025916272084,-46.6561129884974,
-66.3386708104082));
#153523=CARTESIAN_POINT('Ctrl Pts',(44.9836011759049,-46.6583629939592,
-65.3406943944767));
#153524=CARTESIAN_POINT('Ctrl Pts',(45.5707010314966,-46.6605955623318,
-64.3253600969817));
#153525=CARTESIAN_POINT('Ctrl Pts',(46.1180853657563,-46.6626771042377,
-63.3787100796264));
#153526=CARTESIAN_POINT('Ctrl Pts',(46.6707641600523,-46.6647434902106,
-62.4169713275415));
#153527=CARTESIAN_POINT('Ctrl Pts',(47.2288372631003,-46.6667937657809,
-61.440182400038));
#153528=CARTESIAN_POINT('Ctrl Pts',(47.2693283090469,-46.6669425237158,
-61.3693113884668));
#153529=CARTESIAN_POINT('Ctrl Pts',(47.3098477714336,-46.667091197001,-61.2983611610774));
#153530=CARTESIAN_POINT('Ctrl Pts',(47.3503956976423,-46.6672397853475,
-61.2273317382593));
#153531=CARTESIAN_POINT('',(42.8108476403353,-52.2735270043159,-61.2273317382593));
#153532=CARTESIAN_POINT('Origin',(0.,-12.9675000200281,-61.2273317382593));
#153533=CARTESIAN_POINT('Ctrl Pts',(42.8108476403353,-52.2735270043159,
-61.2273317382593));
#153534=CARTESIAN_POINT('Ctrl Pts',(42.1255968220058,-52.2708764489536,
-62.3136518407425));
#153535=CARTESIAN_POINT('Ctrl Pts',(41.4350707133446,-52.2681652890367,
-63.3966290232794));
#153536=CARTESIAN_POINT('Ctrl Pts',(40.7385684738071,-52.2653905871969,
-64.475770197359));
#153537=CARTESIAN_POINT('Ctrl Pts',(40.7403786971506,-52.3124027851469,
-64.4029616119961));
#153538=CARTESIAN_POINT('Ctrl Pts',(39.,-53.5547345046268,-65.2368833127815));
#153539=CARTESIAN_POINT('Ctrl Pts',(39.,-55.4603726203092,-66.5160529206996));
#153540=CARTESIAN_POINT('Ctrl Pts',(40.6386554420727,-49.6698429482511,
-68.4966218848756));
#153541=CARTESIAN_POINT('Ctrl Pts',(38.9999999999999,-50.9103452005084,
-69.3211688367401));
#153542=CARTESIAN_POINT('Ctrl Pts',(39.,-52.7124559353729,-70.609751474253));
#153543=CARTESIAN_POINT('Ctrl Pts',(40.5285598162873,-46.9462740729553,
-72.5399234557376));
#153544=CARTESIAN_POINT('Ctrl Pts',(39.,-48.1638674451749,-73.378963184763));
#153545=CARTESIAN_POINT('Ctrl Pts',(39.,-49.8653057974222,-74.6531246748237));
#153546=CARTESIAN_POINT('Ctrl Pts',(40.4106857765804,-44.1106698886037,
-76.4521234813751));
#153547=CARTESIAN_POINT('Ctrl Pts',(39.,-45.266598631985,-77.3351449301694));
#153548=CARTESIAN_POINT('Ctrl Pts',(39.,-46.8768348378863,-78.5652147900786));
#153549=CARTESIAN_POINT('',(39.,-46.93000002,-78.4955841262963));
#153550=CARTESIAN_POINT('',(39.,-52.5800000200005,-70.729306230469));
#153551=CARTESIAN_POINT('Ctrl Pts',(39.,-46.93000002,-78.4955841262963));
#153552=CARTESIAN_POINT('Ctrl Pts',(39.,-48.8725599414451,-75.9501559720627));
#153553=CARTESIAN_POINT('Ctrl Pts',(39.,-50.7491289418203,-73.3563309228582));
#153554=CARTESIAN_POINT('Ctrl Pts',(39.,-52.58000002,-70.7293062304687));
#153555=CARTESIAN_POINT('Ctrl Pts',(39.,-46.93000002,-78.4955841262963));
#153556=CARTESIAN_POINT('Ctrl Pts',(39.,-46.9255842492519,-78.4098091472741));
#153557=CARTESIAN_POINT('Ctrl Pts',(39.0008866619218,-46.920902618172,-78.3188865334045));
#153558=CARTESIAN_POINT('Ctrl Pts',(39.0030201782254,-46.9159544489267,
-78.2228086756993));
#153559=CARTESIAN_POINT('Ctrl Pts',(39.0050468444063,-46.9112540924074,
-78.1315425604054));
#153560=CARTESIAN_POINT('Ctrl Pts',(39.0081988100488,-46.9063132273459,
-78.0356246635966));
#153561=CARTESIAN_POINT('Ctrl Pts',(39.0128290773931,-46.90113159526,-77.9350548628545));
#153562=CARTESIAN_POINT('Ctrl Pts',(39.0175116979026,-46.8958913758787,
-77.8333479469085));
#153563=CARTESIAN_POINT('Ctrl Pts',(39.0237064111757,-46.8904046922954,
-77.7268790460392));
#153564=CARTESIAN_POINT('Ctrl Pts',(39.0318235339305,-46.8846730593421,
-77.6156825960158));
#153565=CARTESIAN_POINT('Ctrl Pts',(39.0384789387151,-46.8799735693215,
-77.524510217837));
#153566=CARTESIAN_POINT('Ctrl Pts',(39.046427676054,-46.8751093489263,-77.430158523236));
#153567=CARTESIAN_POINT('Ctrl Pts',(39.0559186572753,-46.8700818656153,
-77.3326586488547));
#153568=CARTESIAN_POINT('Ctrl Pts',(39.060664147886,-46.8675681239597,-77.283908711664));
#153569=CARTESIAN_POINT('Ctrl Pts',(39.065795502557,-46.8650135847254,-77.2343720793742));
#153570=CARTESIAN_POINT('Ctrl Pts',(39.0713456567497,-46.8624185135539,
-77.1840542212292));
#153571=CARTESIAN_POINT('Ctrl Pts',(39.0741207338461,-46.8611209779682,
-77.1588952921567));
#153572=CARTESIAN_POINT('Ctrl Pts',(39.0770005267778,-46.8598133115467,
-77.1335410980723));
#153573=CARTESIAN_POINT('Ctrl Pts',(39.0799892582902,-46.8584955542634,
-77.1079924524725));
#153574=CARTESIAN_POINT('Ctrl Pts',(39.0814836240464,-46.8578366756218,
-77.0952181296726));
#153575=CARTESIAN_POINT('Ctrl Pts',(39.0830052255386,-46.8571752743318,
-77.0823951952784));
#153576=CARTESIAN_POINT('Ctrl Pts',(39.0845545972427,-46.8565113557256,
-77.0695237573806));
#153577=CARTESIAN_POINT('Ctrl Pts',(39.0853292830947,-46.8561793964225,
-77.0630880384317));
#153578=CARTESIAN_POINT('Ctrl Pts',(39.0861109115594,-46.8558468077976,
-77.0566401937475));
#153579=CARTESIAN_POINT('Ctrl Pts',(39.0868995498376,-46.855513590546,-77.0501802373859));
#153580=CARTESIAN_POINT('Ctrl Pts',(39.0870967094071,-46.8554302862331,
-77.0485652482955));
#153581=CARTESIAN_POINT('Ctrl Pts',(39.0872943070911,-46.8553469426312,
-77.0469495022282));
#153582=CARTESIAN_POINT('Ctrl Pts',(39.087492343942,-46.8552635597513,-77.0453329994072));
#153583=CARTESIAN_POINT('Ctrl Pts',(39.0875504129536,-46.8552391099512,
-77.0448590031764));
#153584=CARTESIAN_POINT('Ctrl Pts',(39.0876090913764,-46.8552144165552,
-77.0443802848915));
#153585=CARTESIAN_POINT('Ctrl Pts',(39.0876650419913,-46.8551908825852,
-77.0439240441796));
#153586=CARTESIAN_POINT('Ctrl Pts',(39.0881815283767,-46.8549736378756,
-77.0397124351284));
#153587=CARTESIAN_POINT('Ctrl Pts',(39.0885201817289,-46.8548313832274,
-77.0369546251899));
#153588=CARTESIAN_POINT('Ctrl Pts',(39.0892865615655,-46.8545120536274,
-77.0307640477345));
#153589=CARTESIAN_POINT('Ctrl Pts',(39.1038378949207,-46.848448909429,-76.9132229122347));
#153590=CARTESIAN_POINT('Ctrl Pts',(39.1193530923716,-46.8426772179598,
-76.8027648546542));
#153591=CARTESIAN_POINT('Ctrl Pts',(39.1352365569654,-46.8372437726699,
-76.6993778537452));
#153592=CARTESIAN_POINT('Ctrl Pts',(39.1507083793338,-46.8319511427227,
-76.5986702717307));
#153593=CARTESIAN_POINT('Ctrl Pts',(39.1665293605593,-46.8269793809776,
-76.5046719635031));
#153594=CARTESIAN_POINT('Ctrl Pts',(39.1821968310681,-46.8223675906343,
-76.4173774322885));
#153595=CARTESIAN_POINT('Ctrl Pts',(39.1973614587387,-46.8179038143398,
-76.3328845932689));
#153596=CARTESIAN_POINT('Ctrl Pts',(39.2123821550198,-46.8137771916607,
-76.2546720979176));
#153597=CARTESIAN_POINT('Ctrl Pts',(39.2268511484975,-46.8100203816861,
-76.1827406339065));
#153598=CARTESIAN_POINT('Ctrl Pts',(39.2365066710429,-46.8075133680874,
-76.1347389623633));
#153599=CARTESIAN_POINT('Ctrl Pts',(39.2459174917404,-46.8051709836293,
-76.0895344918327));
#153600=CARTESIAN_POINT('Ctrl Pts',(39.2549753268259,-46.8030024901304,
-76.0471290191523));
#153601=CARTESIAN_POINT('Ctrl Pts',(39.2679244690509,-46.799902397176,-75.9865058689541));
#153602=CARTESIAN_POINT('Ctrl Pts',(39.2801621316059,-46.7971290289103,
-75.9315791013882));
#153603=CARTESIAN_POINT('Ctrl Pts',(39.2914380950645,-46.7946619198934,
-75.8823160645738));
#153604=CARTESIAN_POINT('Ctrl Pts',(39.3023895019119,-46.7922658217968,
-75.8344709681726));
#153605=CARTESIAN_POINT('Ctrl Pts',(39.3124339752469,-46.7901586455784,
-75.7919682881292));
#153606=CARTESIAN_POINT('Ctrl Pts',(39.3213888254142,-46.7883231875921,
-75.7547850060667));
#153607=CARTESIAN_POINT('Ctrl Pts',(39.3304763688448,-46.7864605317292,
-75.7170507409117));
#153608=CARTESIAN_POINT('Ctrl Pts',(39.3384424825747,-46.784876170525,-75.684792861159));
#153609=CARTESIAN_POINT('Ctrl Pts',(39.3451473014964,-46.7835508487111,
-75.6579881481457));
#153610=CARTESIAN_POINT('Ctrl Pts',(39.3484997109572,-46.7828881878041,
-75.6445857916391));
#153611=CARTESIAN_POINT('Ctrl Pts',(39.3515375662882,-46.7822903315084,
-75.632546809234));
#153612=CARTESIAN_POINT('Ctrl Pts',(39.3542479292085,-46.7817552642262,
-75.6218688811627));
#153613=CARTESIAN_POINT('Ctrl Pts',(39.3556031106687,-46.7814877305851,
-75.6165299171271));
#153614=CARTESIAN_POINT('Ctrl Pts',(39.3568764620696,-46.7812359081476,
-75.6115312270711));
#153615=CARTESIAN_POINT('Ctrl Pts',(39.3580666487484,-46.7809995683565,
-75.6068725597214));
#153616=CARTESIAN_POINT('Ctrl Pts',(39.3586617420878,-46.7808813984609,
-75.6045432260465));
#153617=CARTESIAN_POINT('Ctrl Pts',(39.3592360469333,-46.7807671000885,
-75.6022988986903));
#153618=CARTESIAN_POINT('Ctrl Pts',(39.3597894130148,-46.7806566486229,
-75.6001395497628));
#153619=CARTESIAN_POINT('Ctrl Pts',(39.3598612372675,-46.7806423125545,
-75.5998592766699));
#153620=CARTESIAN_POINT('Ctrl Pts',(39.3599327087539,-46.7806280413271,
-75.5995804352823));
#153621=CARTESIAN_POINT('Ctrl Pts',(39.3600038271003,-46.7806138349341,
-75.599303025727));
#153622=CARTESIAN_POINT('Ctrl Pts',(39.3602066724863,-46.7805733151326,
-75.5985117918037));
#153623=CARTESIAN_POINT('Ctrl Pts',(39.3604066500891,-46.7805333225372,
-75.5977322016091));
#153624=CARTESIAN_POINT('Ctrl Pts',(39.3606037509506,-46.7804938570154,
-75.5969642585609));
#153625=CARTESIAN_POINT('Ctrl Pts',(39.3607368535288,-46.7804672058752,
-75.5964456651928));
#153626=CARTESIAN_POINT('Ctrl Pts',(39.3608686444778,-46.7804407949061,
-75.5959323825031));
#153627=CARTESIAN_POINT('Ctrl Pts',(39.3609991215663,-46.7804146237221,
-75.5954244100684));
#153628=CARTESIAN_POINT('Ctrl Pts',(39.3610317408384,-46.7804080809262,
-75.5952974169597));
#153629=CARTESIAN_POINT('Ctrl Pts',(39.3610375440812,-46.7804069284516,
-75.5952748130406));
#153630=CARTESIAN_POINT('Ctrl Pts',(39.361036578518,-46.780407134699,-75.5952785550563));
#153631=CARTESIAN_POINT('Ctrl Pts',(39.3610358543456,-46.7804072893846,
-75.595281361568));
#153632=CARTESIAN_POINT('Ctrl Pts',(39.3610313231803,-46.7804082083531,
-75.5952989877083));
#153633=CARTESIAN_POINT('Ctrl Pts',(39.3610314438366,-46.7804081907787,
-75.5952985091008));
#153634=CARTESIAN_POINT('Ctrl Pts',(39.3610318058053,-46.7804081380554,
-75.5952970732781));
#153635=CARTESIAN_POINT('Ctrl Pts',(39.3610739620456,-46.780399656151,-75.595132688387));
#153636=CARTESIAN_POINT('Ctrl Pts',(39.3613866106273,-46.780336824024,-75.5939164234912));
#153637=CARTESIAN_POINT('Ctrl Pts',(39.3887993237504,-46.7748277663454,
-75.4872755409908));
#153638=CARTESIAN_POINT('Ctrl Pts',(39.4171239171424,-46.769455425969,-75.3838529125325));
#153639=CARTESIAN_POINT('Ctrl Pts',(39.4461119121629,-46.7642454946395,
-75.2836839374329));
#153640=CARTESIAN_POINT('Ctrl Pts',(39.4765319614061,-46.758778184207,-75.1785664516249));
#153641=CARTESIAN_POINT('Ctrl Pts',(39.5076823703915,-46.7534897219875,
-75.0770317440789));
#153642=CARTESIAN_POINT('Ctrl Pts',(39.5392965492066,-46.7484034641376,
-74.9790667613441));
#153643=CARTESIAN_POINT('Ctrl Pts',(39.5557430115697,-46.7457574694785,
-74.9281030019857));
#153644=CARTESIAN_POINT('Ctrl Pts',(39.5723153365704,-46.7431660963815,
-74.8781044890794));
#153645=CARTESIAN_POINT('Ctrl Pts',(39.5889783035331,-46.7406320190629,
-74.8290644524599));
#153646=CARTESIAN_POINT('Ctrl Pts',(39.6235154268386,-46.7353796686853,
-74.7274197816498));
#153647=CARTESIAN_POINT('Ctrl Pts',(39.6584382421912,-46.7303660691318,
-74.6299124838824));
#153648=CARTESIAN_POINT('Ctrl Pts',(39.6934473281028,-46.725573431974,-74.5365127275556));
#153649=CARTESIAN_POINT('Ctrl Pts',(39.6985874062929,-46.7248697709361,
-74.5227996574207));
#153650=CARTESIAN_POINT('Ctrl Pts',(39.7037293874539,-46.7241708730641,
-74.5091750510547));
#153651=CARTESIAN_POINT('Ctrl Pts',(39.7088723685335,-46.7234766821404,
-74.4956387342263));
#153652=CARTESIAN_POINT('Ctrl Pts',(39.7289582878229,-46.7207655185856,
-74.4427726312636));
#153653=CARTESIAN_POINT('Ctrl Pts',(39.7490592722323,-46.718125479337,-74.3912543559002));
#153654=CARTESIAN_POINT('Ctrl Pts',(39.7691234113894,-46.7155495625879,
-74.3410753456657));
#153655=CARTESIAN_POINT('Ctrl Pts',(39.7791554809679,-46.7142616042133,
-74.3159858405485));
#153656=CARTESIAN_POINT('Ctrl Pts',(39.7891783519126,-46.7129896836072,
-74.2912311569872));
#153657=CARTESIAN_POINT('Ctrl Pts',(39.7991858392501,-46.7117326802967,
-74.2668100718185));
#153658=CARTESIAN_POINT('Ctrl Pts',(39.8041895829188,-46.7111041786415,
-74.2545995292341));
#153659=CARTESIAN_POINT('Ctrl Pts',(39.8091894816777,-46.7104794068406,
-74.2424723866395));
#153660=CARTESIAN_POINT('Ctrl Pts',(39.8141847735823,-46.709858221149,-74.2304284891786));
#153661=CARTESIAN_POINT('Ctrl Pts',(39.8166824195346,-46.7095476283031,
-74.2244065404481));
#153662=CARTESIAN_POINT('Ctrl Pts',(39.819178913834,-46.7092379320185,-74.218405403026));
#153663=CARTESIAN_POINT('Ctrl Pts',(39.821674162369,-46.7089291135509,-74.2124250570812));
#153664=CARTESIAN_POINT('Ctrl Pts',(39.8234983881871,-46.7087033426052,
-74.2080529469205));
#153665=CARTESIAN_POINT('Ctrl Pts',(39.824874199419,-46.70853337947,-74.2047617703752));
#153666=CARTESIAN_POINT('Ctrl Pts',(39.826783209619,-46.7082978312743,-74.200205025373));
#153667=CARTESIAN_POINT('Ctrl Pts',(39.8274854193994,-46.7082111872916,
-74.1985288735604));
#153668=CARTESIAN_POINT('Ctrl Pts',(39.8282598940434,-46.7081156703967,
-74.1966815054939));
#153669=CARTESIAN_POINT('Ctrl Pts',(39.8291560336875,-46.7080052503693,
-74.1945463609026));
#153670=CARTESIAN_POINT('Ctrl Pts',(39.877269842631,-46.7020767902931,-74.0799102775538));
#153671=CARTESIAN_POINT('Ctrl Pts',(39.9264740604984,-46.6963385369307,
-73.968962778436));
#153672=CARTESIAN_POINT('Ctrl Pts',(39.9765878889061,-46.6907908225711,
-73.8617077695641));
#153673=CARTESIAN_POINT('Ctrl Pts',(40.0290875437083,-46.6849789918235,
-73.7493465487097));
#153674=CARTESIAN_POINT('Ctrl Pts',(40.0825853967005,-46.6793762726923,
-73.641037739188));
#153675=CARTESIAN_POINT('Ctrl Pts',(40.1368204676907,-46.6739818538525,
-73.5367631931971));
#153676=CARTESIAN_POINT('Ctrl Pts',(40.1929501737492,-46.6683989876682,
-73.4288459450216));
#153677=CARTESIAN_POINT('Ctrl Pts',(40.2498691844757,-46.6630392225076,
-73.3252496142913));
#153678=CARTESIAN_POINT('Ctrl Pts',(40.307235899747,-46.6579004797244,-73.2259317454814));
#153679=CARTESIAN_POINT('Ctrl Pts',(40.3682935377067,-46.6524311148681,
-73.1202238546246));
#153680=CARTESIAN_POINT('Ctrl Pts',(40.4298580477627,-46.6472121219459,
-73.0193625605604));
#153681=CARTESIAN_POINT('Ctrl Pts',(40.4914637898166,-46.6422397754793,
-72.9232736363168));
#153682=CARTESIAN_POINT('Ctrl Pts',(40.4992739249393,-46.6416094008342,
-72.9110918581721));
#153683=CARTESIAN_POINT('Ctrl Pts',(40.5070846601786,-46.6409829889087,
-72.8989867555173));
#153684=CARTESIAN_POINT('Ctrl Pts',(40.5148949946051,-46.6403605309214,
-72.886958154682));
#153685=CARTESIAN_POINT('Ctrl Pts',(40.7385684350658,-52.2653905899946,
-64.4757702529885));
#153686=CARTESIAN_POINT('Ctrl Pts',(40.6741963269159,-52.2700392402486,
-64.5682036154681));
#153687=CARTESIAN_POINT('Ctrl Pts',(40.6099114015966,-52.2749116374814,
-64.6650832096111));
#153688=CARTESIAN_POINT('Ctrl Pts',(40.546116711937,-52.2800128685024,-64.7665086919945));
#153689=CARTESIAN_POINT('Ctrl Pts',(40.4863184179071,-52.2847945347216,
-64.8615804111306));
#153690=CARTESIAN_POINT('Ctrl Pts',(40.4269511124508,-52.2897772674399,
-64.9606464072725));
#153691=CARTESIAN_POINT('Ctrl Pts',(40.368303754201,-52.2949643181793,-65.0637700989948));
#153692=CARTESIAN_POINT('Ctrl Pts',(40.3557054842752,-52.2960785689706,
-65.0859225052212));
#153693=CARTESIAN_POINT('Ctrl Pts',(40.3431402620066,-52.2972022442298,
-65.1082620785195));
#153694=CARTESIAN_POINT('Ctrl Pts',(40.3306106542808,-52.298335369721,-65.1307893189901));
#153695=CARTESIAN_POINT('Ctrl Pts',(40.2770643860162,-52.3031778710076,
-65.2270612604503));
#153696=CARTESIAN_POINT('Ctrl Pts',(40.2241778798164,-52.3081925187233,
-65.3267522112761));
#153697=CARTESIAN_POINT('Ctrl Pts',(40.172142097124,-52.3133789242405,-65.4298540962228));
#153698=CARTESIAN_POINT('Ctrl Pts',(40.1219281349228,-52.3183837489425,
-65.529346289589));
#153699=CARTESIAN_POINT('Ctrl Pts',(40.0725061689381,-52.3235485541602,
-65.6320155327409));
#153700=CARTESIAN_POINT('Ctrl Pts',(40.0240065700531,-52.328871683927,-65.737828636263));
#153701=CARTESIAN_POINT('Ctrl Pts',(39.9998035685206,-52.3315281124515,
-65.7906330875486));
#153702=CARTESIAN_POINT('Ctrl Pts',(39.9758295582964,-52.3342239524705,
-65.844220135671));
#153703=CARTESIAN_POINT('Ctrl Pts',(39.9520962441108,-52.3369588990613,
-65.8985836900181));
#153704=CARTESIAN_POINT('Ctrl Pts',(39.9501823456376,-52.3371794502268,
-65.9029676678667));
#153705=CARTESIAN_POINT('Ctrl Pts',(39.9478022209924,-52.3374543749929,
-65.9084324421974));
#153706=CARTESIAN_POINT('Ctrl Pts',(39.9463591924207,-52.3376214165691,
-65.9117507464063));
#153707=CARTESIAN_POINT('Ctrl Pts',(39.9439751906999,-52.3378973829726,
-65.9172328575015));
#153708=CARTESIAN_POINT('Ctrl Pts',(39.9415904249564,-52.338174107732,-65.9227302078874));
#153709=CARTESIAN_POINT('Ctrl Pts',(39.939204947652,-52.338451591336,-65.9282428006076));
#153710=CARTESIAN_POINT('Ctrl Pts',(39.8843720007904,-52.3448298719774,
-66.0549561016047));
#153711=CARTESIAN_POINT('Ctrl Pts',(39.8292508260476,-52.3516114098802,
-66.1897692462162));
#153712=CARTESIAN_POINT('Ctrl Pts',(39.77466324876,-52.3588065544525,-66.3328057530256));
#153713=CARTESIAN_POINT('Ctrl Pts',(39.7396281633994,-52.3634245008206,
-66.4246086223736));
#153714=CARTESIAN_POINT('Ctrl Pts',(39.7048123077817,-52.3682128157311,
-66.5197986983745));
#153715=CARTESIAN_POINT('Ctrl Pts',(39.6704219083266,-52.3731740475517,
-66.6184044463493));
#153716=CARTESIAN_POINT('Ctrl Pts',(39.6614376543415,-52.3744701350488,
-66.6441645159683));
#153717=CARTESIAN_POINT('Ctrl Pts',(39.6524843264061,-52.3757776790693,
-66.6701521715622));
#153718=CARTESIAN_POINT('Ctrl Pts',(39.6435649121351,-52.3770967667731,
-66.6963691459274));
#153719=CARTESIAN_POINT('Ctrl Pts',(39.6183188111944,-52.3808303999811,
-66.7705754066834));
#153720=CARTESIAN_POINT('Ctrl Pts',(39.5933299861079,-52.3846599397822,
-66.8466869090993));
#153721=CARTESIAN_POINT('Ctrl Pts',(39.5686982123625,-52.3885833393951,
-66.9246630559015));
#153722=CARTESIAN_POINT('Ctrl Pts',(39.5549282412021,-52.3907766487393,
-66.9682542850093));
#153723=CARTESIAN_POINT('Ctrl Pts',(39.541270848872,-52.3929991243851,-67.0124249390758));
#153724=CARTESIAN_POINT('Ctrl Pts',(39.5277411825347,-52.3952507861725,
-67.0571754321711));
#153725=CARTESIAN_POINT('Ctrl Pts',(39.4894213492339,-52.4016281278001,
-67.1839214577418));
#153726=CARTESIAN_POINT('Ctrl Pts',(39.4521147917285,-52.4082409660612,
-67.3153460673175));
#153727=CARTESIAN_POINT('Ctrl Pts',(39.4162038270705,-52.4150881216699,
-67.4514264537781));
#153728=CARTESIAN_POINT('Ctrl Pts',(39.4149453563048,-52.4153280747106,
-67.4561952810646));
#153729=CARTESIAN_POINT('Ctrl Pts',(39.4133617691025,-52.4156309953993,
-67.4622146571144));
#153730=CARTESIAN_POINT('Ctrl Pts',(39.4124335754226,-52.415808885988,-67.4657500795878));
#153731=CARTESIAN_POINT('Ctrl Pts',(39.4105797736013,-52.4161641716408,
-67.4728110764051));
#153732=CARTESIAN_POINT('Ctrl Pts',(39.4087222991178,-52.4165215150904,
-67.4799129639208));
#153733=CARTESIAN_POINT('Ctrl Pts',(39.4068613946353,-52.4168809133824,
-67.4870556836734));
#153734=CARTESIAN_POINT('Ctrl Pts',(39.381911700939,-52.4216994719838,-67.5828202280981));
#153735=CARTESIAN_POINT('Ctrl Pts',(39.3563089921541,-52.4268890153023,
-67.6859566474392));
#153736=CARTESIAN_POINT('Ctrl Pts',(39.3306172745555,-52.4324518255431,
-67.7965112043874));
#153737=CARTESIAN_POINT('Ctrl Pts',(39.3275224908695,-52.4331219128704,
-67.8098284315418));
#153738=CARTESIAN_POINT('Ctrl Pts',(39.3244264768482,-52.4337974167592,
-67.8232533055113));
#153739=CARTESIAN_POINT('Ctrl Pts',(39.3213302670964,-52.4344783414944,
-67.8367859134954));
#153740=CARTESIAN_POINT('Ctrl Pts',(39.2961897811093,-52.4400072882182,
-67.9466674682555));
#153741=CARTESIAN_POINT('Ctrl Pts',(39.2710330665147,-52.4458937489998,
-68.0636542200436));
#153742=CARTESIAN_POINT('Ctrl Pts',(39.2464418816062,-52.4521384400037,
-68.1877613272645));
#153743=CARTESIAN_POINT('Ctrl Pts',(39.241222042281,-52.4534639671711,-68.214104879282));
#153744=CARTESIAN_POINT('Ctrl Pts',(39.2360278299045,-52.4548056270789,
-68.2407690954401));
#153745=CARTESIAN_POINT('Ctrl Pts',(39.2308650220214,-52.4561634144658,
-68.267753883504));
#153746=CARTESIAN_POINT('Ctrl Pts',(39.2306328542106,-52.4562244732021,
-68.2689673702946));
#153747=CARTESIAN_POINT('Ctrl Pts',(39.230169613006,-52.4563464505562,-68.2713915594693));
#153748=CARTESIAN_POINT('Ctrl Pts',(39.2301687096753,-52.4563466885112,
-68.2713962886104));
#153749=CARTESIAN_POINT('Ctrl Pts',(39.2301344730456,-52.4563557071123,
-68.2715755251274));
#153750=CARTESIAN_POINT('Ctrl Pts',(39.2289672002148,-52.4566620223187,
-68.2776632593741));
#153751=CARTESIAN_POINT('Ctrl Pts',(39.2266941231712,-52.4572656889597,
-68.2896605972969));
#153752=CARTESIAN_POINT('Ctrl Pts',(39.2244113996309,-52.4578719174444,
-68.3017088495876));
#153753=CARTESIAN_POINT('Ctrl Pts',(39.2210134842536,-52.4587780266544,
-68.3197169721931));
#153754=CARTESIAN_POINT('Ctrl Pts',(39.2165803307865,-52.4599844003236,
-68.3436926461029));
#153755=CARTESIAN_POINT('Ctrl Pts',(39.2121153103965,-52.4611994457921,
-68.3678406648138));
#153756=CARTESIAN_POINT('Ctrl Pts',(39.2066001604335,-52.4627190883533,
-68.3980423412379));
#153757=CARTESIAN_POINT('Ctrl Pts',(39.2001691540676,-52.4645440491351,
-68.4343121208314));
#153758=CARTESIAN_POINT('Ctrl Pts',(39.1936237674451,-52.466401468209,-68.4712269855738));
#153759=CARTESIAN_POINT('Ctrl Pts',(39.1861293377007,-52.4685752693127,
-68.5144298402431));
#153760=CARTESIAN_POINT('Ctrl Pts',(39.1778832003543,-52.4710659880907,
-68.5639315451791));
#153761=CARTESIAN_POINT('Ctrl Pts',(39.1695997515529,-52.4735679766715,
-68.6136572314238));
#153762=CARTESIAN_POINT('Ctrl Pts',(39.1605581534571,-52.4763897165832,
-68.6697380841339));
#153763=CARTESIAN_POINT('Ctrl Pts',(39.1510103356013,-52.4795319125527,
-68.7321884721531));
#153764=CARTESIAN_POINT('Ctrl Pts',(39.1410905312248,-52.4827965296411,
-68.7970719504247));
#153765=CARTESIAN_POINT('Ctrl Pts',(39.1306246335061,-52.486407000624,-68.8688297769009));
#153766=CARTESIAN_POINT('Ctrl Pts',(39.1199512244241,-52.4903634279064,
-68.9474646303329));
#153767=CARTESIAN_POINT('Ctrl Pts',(39.1145062226234,-52.492381785257,-68.9875799220123));
#153768=CARTESIAN_POINT('Ctrl Pts',(39.1090080835936,-52.494490167789,-69.029484766641));
#153769=CARTESIAN_POINT('Ctrl Pts',(39.1035067882548,-52.4966885089909,
-69.0731779591835));
#153770=CARTESIAN_POINT('Ctrl Pts',(39.1029771369556,-52.4969001599207,
-69.077384633207));
#153771=CARTESIAN_POINT('Ctrl Pts',(39.1022508807535,-52.4971918158444,
-69.0831814548162));
#153772=CARTESIAN_POINT('Ctrl Pts',(39.1019177992675,-52.4973259667241,
-69.0858477071385));
#153773=CARTESIAN_POINT('Ctrl Pts',(39.1015249019274,-52.4974842088542,
-69.088992773704));
#153774=CARTESIAN_POINT('Ctrl Pts',(39.1011335086494,-52.4976423082182,
-69.0921350054727));
#153775=CARTESIAN_POINT('Ctrl Pts',(39.1007436120715,-52.4978002647885,
-69.0952744018884));
#153776=CARTESIAN_POINT('Ctrl Pts',(39.0832836734639,-52.5048737098396,
-69.235859551369));
#153777=CARTESIAN_POINT('Ctrl Pts',(39.0688275953131,-52.5116608692955,
-69.3707601805461));
#153778=CARTESIAN_POINT('Ctrl Pts',(39.0568219586142,-52.518159855566,-69.4999384882442));
#153779=CARTESIAN_POINT('Ctrl Pts',(39.0447636431752,-52.5246873583091,
-69.629683608905));
#153780=CARTESIAN_POINT('Ctrl Pts',(39.0351773266671,-52.5309241541674,
-69.7536560848756));
#153781=CARTESIAN_POINT('Ctrl Pts',(39.0275544970134,-52.5368686996032,
-69.8718244174154));
#153782=CARTESIAN_POINT('Ctrl Pts',(39.0199123078435,-52.5428283422574,
-69.9902928592144));
#153783=CARTESIAN_POINT('Ctrl Pts',(39.0142436155034,-52.5484942489622,
-70.1029276450134));
#153784=CARTESIAN_POINT('Ctrl Pts',(39.0100881477389,-52.5538652225379,
-70.209703776616));
#153785=CARTESIAN_POINT('Ctrl Pts',(39.0059150397578,-52.5592589962272,
-70.3169331794721));
#153786=CARTESIAN_POINT('Ctrl Pts',(39.0032680425101,-52.5643553280888,
-70.4182540860612));
#153787=CARTESIAN_POINT('Ctrl Pts',(39.0017332526658,-52.5691533557067,
-70.5136478931993));
#153788=CARTESIAN_POINT('Ctrl Pts',(39.0005167345971,-52.5729564088175,
-70.5892597370394));
#153789=CARTESIAN_POINT('Ctrl Pts',(39.,-52.5765720563163,-70.6611479548761));
#153790=CARTESIAN_POINT('Ctrl Pts',(39.,-52.58000002,-70.7293062304687));
#153791=CARTESIAN_POINT('Origin',(39.,46.91999998,-129.34995));
#153792=CARTESIAN_POINT('',(39.,-52.5800000199938,-161.329336741015));
#153793=CARTESIAN_POINT('',(39.,-46.9300000199928,-153.563058845201));
#153794=CARTESIAN_POINT('Ctrl Pts',(39.,-52.5800000199845,-161.329336741015));
#153795=CARTESIAN_POINT('Ctrl Pts',(39.,-50.7492254978239,-158.702450591995));
#153796=CARTESIAN_POINT('Ctrl Pts',(39.,-48.8724582313882,-156.108353723945));
#153797=CARTESIAN_POINT('Ctrl Pts',(39.,-46.9300000199928,-153.563058845201));
#153798=CARTESIAN_POINT('',(39.,-46.93000002,-129.34995));
#153799=CARTESIAN_POINT('',(39.,-52.58000002,-129.34995));
#153800=CARTESIAN_POINT('Ctrl Pts',(39.,-55.460351966619,-165.542559282053));
#153801=CARTESIAN_POINT('Ctrl Pts',(39.,-53.5547145065899,-166.821728771562));
#153802=CARTESIAN_POINT('Ctrl Pts',(40.7403779325784,-52.3123829231466,
-167.655650590757));
#153803=CARTESIAN_POINT('Ctrl Pts',(39.,-52.7145421899793,-161.452000516006));
#153804=CARTESIAN_POINT('Ctrl Pts',(38.9999999999999,-50.9123394210222,
-162.740555198018));
#153805=CARTESIAN_POINT('Ctrl Pts',(40.6387326052879,-49.6718481371244,
-163.565128292503));
#153806=CARTESIAN_POINT('Ctrl Pts',(39.,-49.8662825279046,-157.406795875704));
#153807=CARTESIAN_POINT('Ctrl Pts',(38.9999999999311,-48.1648205365349,
-158.680980229719));
#153808=CARTESIAN_POINT('Ctrl Pts',(40.5285982996977,-46.9471996283483,
-159.51999555488));
#153809=CARTESIAN_POINT('Ctrl Pts',(39.,-46.8768207417856,-153.493409728778));
#153810=CARTESIAN_POINT('Ctrl Pts',(39.,-45.2665850600662,-154.723479509065));
#153811=CARTESIAN_POINT('Ctrl Pts',(40.4106852206046,-44.110656513925,-155.606501037481));
#153812=CARTESIAN_POINT('',(40.5149261503614,-46.6404760392329,-159.171673926022));
#153813=CARTESIAN_POINT('',(40.7385684294474,-52.2653907112048,-167.582872729716));
#153814=CARTESIAN_POINT('Ctrl Pts',(40.5149617845453,-46.6408003036389,
-159.171515339397));
#153815=CARTESIAN_POINT('Ctrl Pts',(40.5335538982914,-47.0961591011677,
-159.826177485735));
#153816=CARTESIAN_POINT('Ctrl Pts',(40.5521766465686,-47.5547531683496,
-160.492365990833));
#153817=CARTESIAN_POINT('Ctrl Pts',(40.5708158550091,-48.0166562803791,
-161.170144960962));
#153818=CARTESIAN_POINT('Ctrl Pts',(40.5888975189152,-48.4647427350991,
-161.827649896304));
#153819=CARTESIAN_POINT('Ctrl Pts',(40.6069946714345,-48.9159431551024,
-162.496062436473));
#153820=CARTESIAN_POINT('Ctrl Pts',(40.6250928445344,-49.3703312806777,
-163.175393596044));
#153821=CARTESIAN_POINT('Ctrl Pts',(40.6427823317295,-49.8144585903571,
-163.839384363628));
#153822=CARTESIAN_POINT('Ctrl Pts',(40.6604727941326,-50.2616311860377,
-164.51380640413));
#153823=CARTESIAN_POINT('Ctrl Pts',(40.6781492466715,-50.7119252600374,
-165.198621116253));
#153824=CARTESIAN_POINT('Ctrl Pts',(40.6953050861943,-51.1489571166631,
-165.863266427761));
#153825=CARTESIAN_POINT('Ctrl Pts',(40.7124477273092,-51.5889292289694,
-166.53770137231));
#153826=CARTESIAN_POINT('Ctrl Pts',(40.729562078012,-52.0319192326658,-167.221841789087));
#153827=CARTESIAN_POINT('Ctrl Pts',(40.7325651077245,-52.1096500310188,
-167.341886892448));
#153828=CARTESIAN_POINT('Ctrl Pts',(40.7355672628713,-52.1874737695562,
-167.462230691843));
#153829=CARTESIAN_POINT('Ctrl Pts',(40.7385684573717,-52.2653908962637,
-167.582872566557));
#153830=CARTESIAN_POINT('Ctrl Pts',(40.5148965271728,-46.6403604087803,
-159.171687177116));
#153831=CARTESIAN_POINT('Ctrl Pts',(40.485505880482,-46.6427027446008,-159.126423040234));
#153832=CARTESIAN_POINT('Ctrl Pts',(40.4561230470032,-46.6450999497777,
-159.08009741564));
#153833=CARTESIAN_POINT('Ctrl Pts',(40.4267943476046,-46.6475528831212,
-159.032693440355));
#153834=CARTESIAN_POINT('Ctrl Pts',(40.3643789077675,-46.6527730571033,
-158.931811368252));
#153835=CARTESIAN_POINT('Ctrl Pts',(40.3022274691506,-46.6582166938404,
-158.826032696424));
#153836=CARTESIAN_POINT('Ctrl Pts',(40.2407519168729,-46.6639145603451,
-158.71523194619));
#153837=CARTESIAN_POINT('Ctrl Pts',(40.2154779760741,-46.6662570775797,
-158.669679340347));
#153838=CARTESIAN_POINT('Ctrl Pts',(40.1903177355716,-46.6686426274371,
-158.623278069988));
#153839=CARTESIAN_POINT('Ctrl Pts',(40.1652973161143,-46.6710736223053,
-158.57602023873));
#153840=CARTESIAN_POINT('Ctrl Pts',(40.1129408815272,-46.6761605963274,
-158.477130947318));
#153841=CARTESIAN_POINT('Ctrl Pts',(40.061187910713,-46.6814753763527,-158.374503906099));
#153842=CARTESIAN_POINT('Ctrl Pts',(40.0102983583742,-46.6870051091517,
-158.268129054487));
#153843=CARTESIAN_POINT('Ctrl Pts',(40.0055391015154,-46.6875222569265,
-158.258180740563));
#153844=CARTESIAN_POINT('Ctrl Pts',(40.000787361602,-46.6880412815843,-158.248199662502));
#153845=CARTESIAN_POINT('Ctrl Pts',(39.9960433292924,-46.688562170626,-158.238185821595));
#153846=CARTESIAN_POINT('Ctrl Pts',(39.9683079331311,-46.6916074837661,
-158.179641143458));
#153847=CARTESIAN_POINT('Ctrl Pts',(39.9408370839521,-46.6947156646751,
-158.11997668449));
#153848=CARTESIAN_POINT('Ctrl Pts',(39.9136694264136,-46.6978784774708,
-158.059195198908));
#153849=CARTESIAN_POINT('Ctrl Pts',(39.9000855976443,-46.6994598838686,
-158.028804456117));
#153850=CARTESIAN_POINT('Ctrl Pts',(39.8865774905551,-46.7010549168859,
-157.998134479889));
#153851=CARTESIAN_POINT('Ctrl Pts',(39.8731496300776,-46.7026621221226,
-157.967185912099));
#153852=CARTESIAN_POINT('Ctrl Pts',(39.8664356998389,-46.703465724741,-157.951711628204));
#153853=CARTESIAN_POINT('Ctrl Pts',(39.8597418255558,-46.7042723684712,
-157.936167697887));
#153854=CARTESIAN_POINT('Ctrl Pts',(39.8530685429161,-46.7050818534694,
-157.920554214528));
#153855=CARTESIAN_POINT('Ctrl Pts',(39.8497319015962,-46.7054865959685,
-157.912747472849));
#153856=CARTESIAN_POINT('Ctrl Pts',(39.8464004078077,-46.7058920486704,
-157.904923342997));
#153857=CARTESIAN_POINT('Ctrl Pts',(39.8430741268868,-46.7062981850526,
-157.897081837744));
#153858=CARTESIAN_POINT('Ctrl Pts',(39.8399222509519,-46.706683026718,-157.889651481654));
#153859=CARTESIAN_POINT('Ctrl Pts',(39.8360309238232,-46.7071598659057,
-157.880439145401));
#153860=CARTESIAN_POINT('Ctrl Pts',(39.8335156236791,-46.7074688074295,
-157.874466100708));
#153861=CARTESIAN_POINT('Ctrl Pts',(39.8333764427928,-46.7074859023099,
-157.874135589991));
#153862=CARTESIAN_POINT('Ctrl Pts',(39.8332414629469,-46.7075024828872,
-157.873815001909));
#153863=CARTESIAN_POINT('Ctrl Pts',(39.8331110389128,-46.7075185050603,
-157.873505188529));
#153864=CARTESIAN_POINT('Ctrl Pts',(39.8314301064126,-46.7077250022113,
-157.869512248248));
#153865=CARTESIAN_POINT('Ctrl Pts',(39.8297484996322,-46.7079318944916,
-157.86550999177));
#153866=CARTESIAN_POINT('Ctrl Pts',(39.8280662447799,-46.7081391851734,
-157.861498417039));
#153867=CARTESIAN_POINT('Ctrl Pts',(39.7687531704664,-46.7154478563873,
-157.720057998646));
#153868=CARTESIAN_POINT('Ctrl Pts',(39.7086758947724,-46.7232497705536,
-157.567010082113));
#153869=CARTESIAN_POINT('Ctrl Pts',(39.6492710002084,-46.731714411294,-157.40213520183));
#153870=CARTESIAN_POINT('Ctrl Pts',(39.6305758096956,-46.7343783007332,
-157.35024777201));
#153871=CARTESIAN_POINT('Ctrl Pts',(39.6119473744286,-46.7371081401241,
-157.297188794001));
#153872=CARTESIAN_POINT('Ctrl Pts',(39.5934307084091,-46.7399101225425,
-157.242950994996));
#153873=CARTESIAN_POINT('Ctrl Pts',(39.5539191783334,-46.7458890937288,
-157.127216422457));
#153874=CARTESIAN_POINT('Ctrl Pts',(39.5149265146814,-46.7521844764172,
-157.006122027191));
#153875=CARTESIAN_POINT('Ctrl Pts',(39.4769284603091,-46.7587734088497,
-156.879651340181));
#153876=CARTESIAN_POINT('Ctrl Pts',(39.4579294331229,-46.7620678750659,
-156.816415996676));
#153877=CARTESIAN_POINT('Ctrl Pts',(39.439179259145,-46.7654347814872,-156.751837220508));
#153878=CARTESIAN_POINT('Ctrl Pts',(39.4207374191931,-46.7688651930717,
-156.685917108977));
#153879=CARTESIAN_POINT('Ctrl Pts',(39.4115164992172,-46.7705803988639,
-156.652957053211));
#153880=CARTESIAN_POINT('Ctrl Pts',(39.4023726231759,-46.7723114718034,
-156.619661670513));
#153881=CARTESIAN_POINT('Ctrl Pts',(39.3933131608115,-46.7740568258333,
-156.586031547249));
#153882=CARTESIAN_POINT('Ctrl Pts',(39.3887834296293,-46.7749295028482,
-156.569216485616));
#153883=CARTESIAN_POINT('Ctrl Pts',(39.3842747984955,-46.7758057495308,
-156.552317739308));
#153884=CARTESIAN_POINT('Ctrl Pts',(39.3797881736941,-46.7766853518933,
-156.535335392793));
#153885=CARTESIAN_POINT('Ctrl Pts',(39.3775448612934,-46.7771251530745,
-156.526844219535));
#153886=CARTESIAN_POINT('Ctrl Pts',(39.3753070502474,-46.7775657931418,
-156.518332146253));
#153887=CARTESIAN_POINT('Ctrl Pts',(39.3730748531502,-46.7780072437074,
-156.509799184646));
#153888=CARTESIAN_POINT('Ctrl Pts',(39.3714007053272,-46.7783383316315,
-156.503399463442));
#153889=CARTESIAN_POINT('Ctrl Pts',(39.369729715331,-46.7786698754583,-156.496987992557));
#153890=CARTESIAN_POINT('Ctrl Pts',(39.3680619304574,-46.7790018628477,
-156.490564777184));
#153891=CARTESIAN_POINT('Ctrl Pts',(39.3675060021662,-46.7791125253109,
-156.488423705393));
#153892=CARTESIAN_POINT('Ctrl Pts',(39.3665115797823,-46.7793107839559,
-156.484586928693));
#153893=CARTESIAN_POINT('Ctrl Pts',(39.3663952165149,-46.779333994977,-156.484137647));
#153894=CARTESIAN_POINT('Ctrl Pts',(39.3651798359371,-46.7795764273605,
-156.479445030019));
#153895=CARTESIAN_POINT('Ctrl Pts',(39.3638113809044,-46.7798472112542,
-156.474145034342));
#153896=CARTESIAN_POINT('Ctrl Pts',(39.3622924024584,-46.7801465392495,
-156.468236627594));
#153897=CARTESIAN_POINT('Ctrl Pts',(39.3576875062211,-46.7810539743506,
-156.450324852692));
#153898=CARTESIAN_POINT('Ctrl Pts',(39.3516969630454,-46.7822232088955,
-156.42683241472));
#153899=CARTESIAN_POINT('Ctrl Pts',(39.3444292371885,-46.7836586304216,
-156.397743787219));
#153900=CARTESIAN_POINT('Ctrl Pts',(39.3394045741733,-46.7846510329414,
-156.377632881325));
#153901=CARTESIAN_POINT('Ctrl Pts',(39.3337705197713,-46.7857706667138,
-156.35484692661));
#153902=CARTESIAN_POINT('Ctrl Pts',(39.3275773655646,-46.7870189843683,
-156.329378991889));
#153903=CARTESIAN_POINT('Ctrl Pts',(39.3185244421424,-46.7888437288775,
-156.292150908258));
#153904=CARTESIAN_POINT('Ctrl Pts',(39.3082739032971,-46.7909453929226,
-156.249193109022));
#153905=CARTESIAN_POINT('Ctrl Pts',(39.2970184933079,-46.7933577839599,
-156.200472151143));
#153906=CARTESIAN_POINT('Ctrl Pts',(39.2857630833188,-46.7957701749971,
-156.151751193264));
#153907=CARTESIAN_POINT('Ctrl Pts',(39.2735027903882,-46.7984932254866,
-156.097267063491));
#153908=CARTESIAN_POINT('Ctrl Pts',(39.2604851284931,-46.8015632964374,
-156.036979329678));
#153909=CARTESIAN_POINT('Ctrl Pts',(39.247467466598,-46.8046333673881,-155.976691595865));
#153910=CARTESIAN_POINT('Ctrl Pts',(39.2336957527102,-46.8080429288287,
-155.910603676852));
#153911=CARTESIAN_POINT('Ctrl Pts',(39.2194870997902,-46.8117851407561,
-155.838698731947));
#153912=CARTESIAN_POINT('Ctrl Pts',(39.2052784468702,-46.8155273526834,
-155.766793787042));
#153913=CARTESIAN_POINT('Ctrl Pts',(39.1906327815456,-46.8196025971396,
-155.689071535734));
#153914=CARTESIAN_POINT('Ctrl Pts',(39.1759121851943,-46.824014590861,-155.605507258466));
#153915=CARTESIAN_POINT('Ctrl Pts',(39.161191588843,-46.8284265845825,-155.521942981197));
#153916=CARTESIAN_POINT('Ctrl Pts',(39.1463992322883,-46.833168409848,-155.432540854273));
#153917=CARTESIAN_POINT('Ctrl Pts',(39.1319534122398,-46.838197824685,-155.337304509702));
#153918=CARTESIAN_POINT('Ctrl Pts',(39.1247305022156,-46.8407125321035,
-155.289686337417));
#153919=CARTESIAN_POINT('Ctrl Pts',(39.1175949803997,-46.8432985882358,
-155.24060995796));
#153920=CARTESIAN_POINT('Ctrl Pts',(39.1106031571093,-46.8459469127866,
-155.190078297287));
#153921=CARTESIAN_POINT('Ctrl Pts',(39.1071072454641,-46.847271075062,-155.164812466951));
#153922=CARTESIAN_POINT('Ctrl Pts',(39.1036472844893,-46.8486108069295,
-155.139182814454));
#153923=CARTESIAN_POINT('Ctrl Pts',(39.1002305329326,-46.8499646445616,
-155.113189925138));
#153924=CARTESIAN_POINT('Ctrl Pts',(39.0985221571543,-46.8506415633776,
-155.10019348048));
#153925=CARTESIAN_POINT('Ctrl Pts',(39.096824584886,-46.8513220087368,-155.087106226545));
#153926=CARTESIAN_POINT('Ctrl Pts',(39.0951387325872,-46.8520057872307,
-155.073928243663));
#153927=CARTESIAN_POINT('Ctrl Pts',(39.0942958064377,-46.8523476764776,
-155.067339252221));
#153928=CARTESIAN_POINT('Ctrl Pts',(39.0934558103441,-46.8526903990116,
-155.060727578541));
#153929=CARTESIAN_POINT('Ctrl Pts',(39.0926188595233,-46.8530339294089,
-155.054093233508));
#153930=CARTESIAN_POINT('Ctrl Pts',(39.0917819087025,-46.8533774598063,
-155.047458888474));
#153931=CARTESIAN_POINT('Ctrl Pts',(39.0906930029478,-46.853827734122,-155.038751520483));
#153932=CARTESIAN_POINT('Ctrl Pts',(39.0901172584079,-46.854066918385,-155.034122195496));
#153933=CARTESIAN_POINT('Ctrl Pts',(39.0742562772155,-46.8606561204245,
-154.906590570869));
#153934=CARTESIAN_POINT('Ctrl Pts',(39.061129990202,-46.8670036349,-154.783735029668));
#153935=CARTESIAN_POINT('Ctrl Pts',(39.0502431981267,-46.8731065605454,
-154.665599454386));
#153936=CARTESIAN_POINT('Ctrl Pts',(39.0391497064693,-46.8793253579895,
-154.545220925085));
#153937=CARTESIAN_POINT('Ctrl Pts',(39.0303815861069,-46.8852901921471,
-154.429743243621));
#153938=CARTESIAN_POINT('Ctrl Pts',(39.0234682960032,-46.8909984573606,
-154.319202785664));
#153939=CARTESIAN_POINT('Ctrl Pts',(39.0164819666703,-46.8967670306597,
-154.207494462663));
#153940=CARTESIAN_POINT('Ctrl Pts',(39.0113899664732,-46.9022735872273,
-154.10082817691));
#153941=CARTESIAN_POINT('Ctrl Pts',(39.0077596161897,-46.9075158793827,
-153.999232157633));
#153942=CARTESIAN_POINT('Ctrl Pts',(39.004072963734,-46.9128394729037,-153.89606051173));
#153943=CARTESIAN_POINT('Ctrl Pts',(39.0018937009545,-46.9178905436415,
-153.79811756574));
#153944=CARTESIAN_POINT('Ctrl Pts',(39.000821918352,-46.9226671591535,-153.705424192369));
#153945=CARTESIAN_POINT('Ctrl Pts',(39.0002562987361,-46.9251879571451,
-153.65650644531));
#153946=CARTESIAN_POINT('Ctrl Pts',(39.,-46.9276323243641,-153.609050599416));
#153947=CARTESIAN_POINT('Ctrl Pts',(39.,-46.9300000199928,-153.563058845201));
#153948=CARTESIAN_POINT('Ctrl Pts',(39.,-52.5800000200011,-161.329336741015));
#153949=CARTESIAN_POINT('Ctrl Pts',(38.9999999999999,-52.5757636289944,
-161.413568993848));
#153950=CARTESIAN_POINT('Ctrl Pts',(39.0007875208437,-52.5712939085953,
-161.50340414571));
#153951=CARTESIAN_POINT('Ctrl Pts',(39.002705436195,-52.5665523334981,-161.598853214538));
#153952=CARTESIAN_POINT('Ctrl Pts',(39.0045946757477,-52.5618816522765,
-161.692875172275));
#153953=CARTESIAN_POINT('Ctrl Pts',(39.007580711382,-52.556947197286,-161.792344453901));
#153954=CARTESIAN_POINT('Ctrl Pts',(39.0120413122437,-52.5517104751597,
-161.897265269322));
#153955=CARTESIAN_POINT('Ctrl Pts',(39.014128447874,-52.549260188825,-161.94635820075));
#153956=CARTESIAN_POINT('Ctrl Pts',(39.0165391409009,-52.5467437004451,
-161.996644569051));
#153957=CARTESIAN_POINT('Ctrl Pts',(39.0193159959949,-52.5441569358408,
-162.048124286934));
#153958=CARTESIAN_POINT('Ctrl Pts',(39.0255457440389,-52.5383536471604,
-162.163616691443));
#153959=CARTESIAN_POINT('Ctrl Pts',(39.0336143349312,-52.5322056713611,
-162.285112131259));
#153960=CARTESIAN_POINT('Ctrl Pts',(39.0440353236384,-52.5257342581849,
-162.412568556975));
#153961=CARTESIAN_POINT('Ctrl Pts',(39.0459395812387,-52.5245517180179,
-162.435859040652));
#153962=CARTESIAN_POINT('Ctrl Pts',(39.0479225271856,-52.5233583822674,
-162.459348549214));
#153963=CARTESIAN_POINT('Ctrl Pts',(39.0499874806663,-52.522154386545,-162.483036799005));
#153964=CARTESIAN_POINT('Ctrl Pts',(39.0566701532884,-52.5182579746761,
-162.559697517917));
#153965=CARTESIAN_POINT('Ctrl Pts',(39.0642111230617,-52.5142513212459,
-162.63843891517));
#153966=CARTESIAN_POINT('Ctrl Pts',(39.0727245161976,-52.510148860684,-162.719244903039));
#153967=CARTESIAN_POINT('Ctrl Pts',(39.0769812127655,-52.5080976304031,
-162.759647896974));
#153968=CARTESIAN_POINT('Ctrl Pts',(39.0814810954767,-52.5060224564948,
-162.80056703288));
#153969=CARTESIAN_POINT('Ctrl Pts',(39.0862386725614,-52.5039259762791,
-162.841999704965));
#153970=CARTESIAN_POINT('Ctrl Pts',(39.0886174611038,-52.5028777361712,
-162.862716041008));
#153971=CARTESIAN_POINT('Ctrl Pts',(39.0910606769942,-52.501824169324,-162.883560761195));
#153972=CARTESIAN_POINT('Ctrl Pts',(39.0935701478725,-52.5007656343161,
-162.904533519597));
#153973=CARTESIAN_POINT('Ctrl Pts',(39.0948248833117,-52.5002363668122,
-162.915019898798));
#153974=CARTESIAN_POINT('Ctrl Pts',(39.0960961827068,-52.4997058572543,
-162.925538287561));
#153975=CARTESIAN_POINT('Ctrl Pts',(39.0973842749376,-52.4991741535183,
-162.936088640481));
#153976=CARTESIAN_POINT('Ctrl Pts',(39.0984281101808,-52.4987432751346,
-162.944638362265));
#153977=CARTESIAN_POINT('Ctrl Pts',(39.0996604129328,-52.4982394633436,
-162.954643068411));
#153978=CARTESIAN_POINT('Ctrl Pts',(39.1006502213987,-52.497838153136,-162.962616485939));
#153979=CARTESIAN_POINT('Ctrl Pts',(39.1008818361442,-52.497744246724,-162.964482262133));
#153980=CARTESIAN_POINT('Ctrl Pts',(39.1011000517209,-52.4976559520504,
-162.966236829985));
#153981=CARTESIAN_POINT('Ctrl Pts',(39.1012991554483,-52.4975755156648,
-162.967835546034));
#153982=CARTESIAN_POINT('Ctrl Pts',(39.1180987707534,-52.4907885993556,
-163.102729126186));
#153983=CARTESIAN_POINT('Ctrl Pts',(39.1369594452229,-52.4840212715504,
-163.23723004872));
#153984=CARTESIAN_POINT('Ctrl Pts',(39.158020961122,-52.477252165749,-163.37176382442));
#153985=CARTESIAN_POINT('Ctrl Pts',(39.179082477021,-52.4704830599476,-163.506297600119));
#153986=CARTESIAN_POINT('Ctrl Pts',(39.2023460261632,-52.4637119611059,
-163.640864383156));
#153987=CARTESIAN_POINT('Ctrl Pts',(39.2279803894119,-52.4570117183738,
-163.775880236838));
#153988=CARTESIAN_POINT('Ctrl Pts',(39.2536147526607,-52.4503114756418,
-163.910896090521));
#153989=CARTESIAN_POINT('Ctrl Pts',(39.2814446348001,-52.4435537149193,
-164.045151495395));
#153990=CARTESIAN_POINT('Ctrl Pts',(39.3114635522106,-52.4367950352887,
-164.178546542087));
#153991=CARTESIAN_POINT('Ctrl Pts',(39.3264730109159,-52.4334156954734,
-164.245244065433));
#153992=CARTESIAN_POINT('Ctrl Pts',(39.3420294553905,-52.4300359823671,
-164.311726457118));
#153993=CARTESIAN_POINT('Ctrl Pts',(39.3581260665589,-52.4266736702452,
-164.377982223013));
#153994=CARTESIAN_POINT('Ctrl Pts',(39.3661743721431,-52.4249925141843,
-164.41111010596));
#153995=CARTESIAN_POINT('Ctrl Pts',(39.3743576845704,-52.4233156920952,
-164.444181343468));
#153996=CARTESIAN_POINT('Ctrl Pts',(39.3826749315158,-52.4216453552344,
-164.477194551363));
#153997=CARTESIAN_POINT('Ctrl Pts',(39.3868335549885,-52.4208101868041,
-164.49370115531));
#153998=CARTESIAN_POINT('Ctrl Pts',(39.391025659974,-52.4199766385722,-164.510193252601));
#153999=CARTESIAN_POINT('Ctrl Pts',(39.3952510996912,-52.4191449731968,
-164.526670674556));
#154000=CARTESIAN_POINT('Ctrl Pts',(39.3973638195498,-52.4187291405091,
-164.534909385534));
#154001=CARTESIAN_POINT('Ctrl Pts',(39.3994848729635,-52.4183137784622,
-164.543144427728));
#154002=CARTESIAN_POINT('Ctrl Pts',(39.4016142407734,-52.4178989195526,
-164.551375780296));
#154003=CARTESIAN_POINT('Ctrl Pts',(39.4031446790737,-52.417600748442,-164.557291891724));
#154004=CARTESIAN_POINT('Ctrl Pts',(39.4044913051618,-52.4173392624714,
-164.562482058706));
#154005=CARTESIAN_POINT('Ctrl Pts',(39.4060594277002,-52.4170359365337,
-164.568507465127));
#154006=CARTESIAN_POINT('Ctrl Pts',(39.4066731047513,-52.4169172314182,
-164.570865478326));
#154007=CARTESIAN_POINT('Ctrl Pts',(39.4073208144597,-52.4167921189192,
-164.57335140041));
#154008=CARTESIAN_POINT('Ctrl Pts',(39.4080272966066,-52.4166558955955,
-164.576058742277));
#154009=CARTESIAN_POINT('Ctrl Pts',(39.4389568787749,-52.4106920782465,
-164.694585378933));
#154010=CARTESIAN_POINT('Ctrl Pts',(39.4709489777983,-52.4049043173862,
-164.80961245767));
#154011=CARTESIAN_POINT('Ctrl Pts',(39.5037549717153,-52.3992948524888,
-164.921096659683));
#154012=CARTESIAN_POINT('Ctrl Pts',(39.5382493737183,-52.3933966883399,
-165.038318557941));
#154013=CARTESIAN_POINT('Ctrl Pts',(39.5736433997348,-52.3876956313425,
-165.151623787289));
#154014=CARTESIAN_POINT('Ctrl Pts',(39.6096648516938,-52.3821914670209,
-165.261017822325));
#154015=CARTESIAN_POINT('Ctrl Pts',(39.6284113105696,-52.3793269631076,
-165.317949197034));
#154016=CARTESIAN_POINT('Ctrl Pts',(39.647327993138,-52.3765157420429,-165.373822126896));
#154017=CARTESIAN_POINT('Ctrl Pts',(39.6663784661277,-52.3737575148381,
-165.428642508953));
#154018=CARTESIAN_POINT('Ctrl Pts',(39.7053741027461,-52.3681115224344,
-165.540857869648));
#154019=CARTESIAN_POINT('Ctrl Pts',(39.7449238922867,-52.3626884946953,
-165.648643856583));
#154020=CARTESIAN_POINT('Ctrl Pts',(39.7847063969893,-52.3574869652637,
-165.752029633127));
#154021=CARTESIAN_POINT('Ctrl Pts',(39.8102919510438,-52.354141675332,-165.818520730005));
#154022=CARTESIAN_POINT('Ctrl Pts',(39.8359743201574,-52.3508879221915,
-165.88319338533));
#154023=CARTESIAN_POINT('Ctrl Pts',(39.8616696526033,-52.3477250660392,
-165.946060288054));
#154024=CARTESIAN_POINT('Ctrl Pts',(39.8745173188263,-52.3461436379631,
-165.977493739416));
#154025=CARTESIAN_POINT('Ctrl Pts',(39.8873682812456,-52.344584926784,-166.008475898349));
#154026=CARTESIAN_POINT('Ctrl Pts',(39.9002122316688,-52.3430488303558,
-166.039008789559));
#154027=CARTESIAN_POINT('Ctrl Pts',(39.9066342068805,-52.3422807821417,
-166.054275235164));
#154028=CARTESIAN_POINT('Ctrl Pts',(39.9130544350819,-52.3415183868975,
-166.069429378085));
#154029=CARTESIAN_POINT('Ctrl Pts',(39.9194716392171,-52.3407616305627,
-166.084471496975));
#154030=CARTESIAN_POINT('Ctrl Pts',(39.9226802412847,-52.3403832523953,
-166.09199255642));
#154031=CARTESIAN_POINT('Ctrl Pts',(39.9258880875008,-52.3400062839368,
-166.099485610224));
#154032=CARTESIAN_POINT('Ctrl Pts',(39.9290950189449,-52.3396307233536,
-166.106950694721));
#154033=CARTESIAN_POINT('Ctrl Pts',(39.930698484667,-52.339442943062,-166.11068323697));
#154034=CARTESIAN_POINT('Ctrl Pts',(39.9323017216999,-52.3392555147389,
-166.114408786899));
#154035=CARTESIAN_POINT('Ctrl Pts',(39.9339047102407,-52.3390684381484,
-166.118127349181));
#154036=CARTESIAN_POINT('Ctrl Pts',(39.9347062045111,-52.3389748998532,
-166.119986630323));
#154037=CARTESIAN_POINT('Ctrl Pts',(39.935507636658,-52.3388814494912,-166.121844164551));
#154038=CARTESIAN_POINT('Ctrl Pts',(39.9363090042075,-52.3387880870328,
-166.123699952453));
#154039=CARTESIAN_POINT('Ctrl Pts',(39.9367096879822,-52.3387414058036,
-166.124627846405));
#154040=CARTESIAN_POINT('Ctrl Pts',(39.9371103556077,-52.3386947465503,
-166.125555303774));
#154041=CARTESIAN_POINT('Ctrl Pts',(39.9375110067751,-52.3386481092691,
-166.126482324637));
#154042=CARTESIAN_POINT('Ctrl Pts',(39.9378016553992,-52.3386142766918,
-166.12715482321));
#154043=CARTESIAN_POINT('Ctrl Pts',(39.938092295362,-52.3385804556776,-166.127827092064));
#154044=CARTESIAN_POINT('Ctrl Pts',(39.9383829265455,-52.3385466462252,
-166.128499131229));
#154045=CARTESIAN_POINT('Ctrl Pts',(39.938492922488,-52.3385338502735,-166.128753479646));
#154046=CARTESIAN_POINT('Ctrl Pts',(39.9386010220686,-52.3385212764432,
-166.129003412917));
#154047=CARTESIAN_POINT('Ctrl Pts',(39.9387065331371,-52.3385090050618,
-166.129247334349));
#154048=CARTESIAN_POINT('Ctrl Pts',(39.9399964501902,-52.3383589822787,
-166.132229376132));
#154049=CARTESIAN_POINT('Ctrl Pts',(39.9409610502249,-52.3382468715858,
-166.134457830407));
#154050=CARTESIAN_POINT('Ctrl Pts',(39.9427463071851,-52.3380398161657,
-166.138573531837));
#154051=CARTESIAN_POINT('Ctrl Pts',(39.9909131807542,-52.3324533866124,
-166.249616633677));
#154052=CARTESIAN_POINT('Ctrl Pts',(40.040074614134,-52.3270302476623,-166.357417513742));
#154053=CARTESIAN_POINT('Ctrl Pts',(40.0901271983721,-52.3217716839405,
-166.461950306206));
#154054=CARTESIAN_POINT('Ctrl Pts',(40.1422107221744,-52.3162997481167,
-166.570724633593));
#154055=CARTESIAN_POINT('Ctrl Pts',(40.1952591438407,-52.3110060133846,
-166.675960294702));
#154056=CARTESIAN_POINT('Ctrl Pts',(40.249103194939,-52.3058907626207,-166.777651247629));
#154057=CARTESIAN_POINT('Ctrl Pts',(40.3044083654476,-52.3006367037243,
-166.882101699928));
#154058=CARTESIAN_POINT('Ctrl Pts',(40.360552693577,-52.2955709418491,-166.982812555586));
#154059=CARTESIAN_POINT('Ctrl Pts',(40.4173004895395,-52.2906926276812,
-167.079800199658));
#154060=CARTESIAN_POINT('Ctrl Pts',(40.4772368637466,-52.2855402079526,
-167.18223744202));
#154061=CARTESIAN_POINT('Ctrl Pts',(40.5378462972357,-52.2805968899478,
-167.280521365932));
#154062=CARTESIAN_POINT('Ctrl Pts',(40.59879608483,-52.27586045319,-167.374695481386));
#154063=CARTESIAN_POINT('Ctrl Pts',(40.645245648188,-52.2722508357007,-167.446465157953));
#154064=CARTESIAN_POINT('Ctrl Pts',(40.6918916531602,-52.268761345407,-167.515848441831));
#154065=CARTESIAN_POINT('Ctrl Pts',(40.7385684356245,-52.2653905899516,
-167.582872719316));
#154066=CARTESIAN_POINT('Origin',(0.,-12.9675000200281,-171.64995));
#154067=CARTESIAN_POINT('',(42.9629113790828,-52.2741145284007,-171.07256826174));
#154068=CARTESIAN_POINT('',(47.4880541505298,-46.6677435098469,-171.07256826174));
#154069=CARTESIAN_POINT('Origin',(0.,-12.9675000200281,-171.07256826174));
#154070=CARTESIAN_POINT('Ctrl Pts',(47.4880541505298,-46.6677435098469,
-171.07256826174));
#154071=CARTESIAN_POINT('Ctrl Pts',(46.9283768635402,-46.6656984714656,
-170.091223234496));
#154072=CARTESIAN_POINT('Ctrl Pts',(46.3741127719638,-46.6636372134722,
-169.12492957485));
#154073=CARTESIAN_POINT('Ctrl Pts',(45.8251573705305,-46.6615606438201,
-168.173728787141));
#154074=CARTESIAN_POINT('Ctrl Pts',(45.2609461023282,-46.6594263647987,
-167.196093443092));
#154075=CARTESIAN_POINT('Ctrl Pts',(44.7023427412084,-46.6572759119971,
-166.234401479565));
#154076=CARTESIAN_POINT('Ctrl Pts',(44.149280897441,-46.6551106551776,-165.288669126662));
#154077=CARTESIAN_POINT('Ctrl Pts',(43.5865485868871,-46.652907538136,-164.326400335003));
#154078=CARTESIAN_POINT('Ctrl Pts',(43.0295534282823,-46.6506890964257,
-163.380654060043));
#154079=CARTESIAN_POINT('Ctrl Pts',(42.4782718898617,-46.6484571462022,
-162.45141897123));
#154080=CARTESIAN_POINT('Ctrl Pts',(41.912450579805,-46.6461663294209,-161.497675777128));
#154081=CARTESIAN_POINT('Ctrl Pts',(41.3526483592774,-46.6438612834653,
-160.561326137806));
#154082=CARTESIAN_POINT('Ctrl Pts',(40.7988863618209,-46.6415443404656,
-159.642329260554));
#154083=CARTESIAN_POINT('Ctrl Pts',(40.7040758002953,-46.6411476525964,
-159.484986195532));
#154084=CARTESIAN_POINT('Ctrl Pts',(40.6094424040048,-46.6407506168077,
-159.32815173549));
#154085=CARTESIAN_POINT('Ctrl Pts',(40.5149864073608,-46.6403532458042,
-159.17182559703));
#154086=CARTESIAN_POINT('Ctrl Pts',(40.738568473807,-52.2653905871942,-167.582872774143));
#154087=CARTESIAN_POINT('Ctrl Pts',(41.4866208523709,-52.2683706527206,
-168.741884298091));
#154088=CARTESIAN_POINT('Ctrl Pts',(42.2277810204719,-52.2712774187735,
-169.905318536155));
#154089=CARTESIAN_POINT('Ctrl Pts',(42.9629113790828,-52.2741145284007,
-171.07256826174));
#154090=CARTESIAN_POINT('Origin',(0.,-12.9675000200281,-170.64995));
#154091=CARTESIAN_POINT('',(48.4122058243951,-46.93000002,-171.64995));
#154092=CARTESIAN_POINT('',(43.9094855672884,-52.58000002,-171.64995));
#154093=CARTESIAN_POINT('Origin',(0.,-12.9675000200281,-171.64995));
#154094=CARTESIAN_POINT('Ctrl Pts',(48.4122058243951,-46.93000002,-171.64995));
#154095=CARTESIAN_POINT('Ctrl Pts',(48.3795547379479,-46.9208088710473,
-171.64995));
#154096=CARTESIAN_POINT('Ctrl Pts',(48.3480259720962,-46.9118688891517,
-171.648414023011));
#154097=CARTESIAN_POINT('Ctrl Pts',(48.3177156961692,-46.9032522569107,
-171.645643509378));
#154098=CARTESIAN_POINT('Ctrl Pts',(48.2866802541381,-46.8944294738036,
-171.642806711868));
#154099=CARTESIAN_POINT('Ctrl Pts',(48.2569219491055,-46.8859454642817,
-171.63867615571));
#154100=CARTESIAN_POINT('Ctrl Pts',(48.2284995614569,-46.8778463555618,
-171.63356011004));
#154101=CARTESIAN_POINT('Ctrl Pts',(48.198916697874,-46.869416563126,-171.628235178053));
#154102=CARTESIAN_POINT('Ctrl Pts',(48.1707807231883,-46.8614035157324,
-171.621843200721));
#154103=CARTESIAN_POINT('Ctrl Pts',(48.1441156179165,-46.8538291316514,
-171.61470651212));
#154104=CARTESIAN_POINT('Ctrl Pts',(48.12245452578,-46.8476761677015,-171.608909105069));
#154105=CARTESIAN_POINT('Ctrl Pts',(48.101763104914,-46.8418120039883,-171.602619822146));
#154106=CARTESIAN_POINT('Ctrl Pts',(48.0820376369122,-46.8362364896225,
-171.595996656439));
#154107=CARTESIAN_POINT('Ctrl Pts',(48.0562396073805,-46.8289445316193,
-171.587334523582));
#154108=CARTESIAN_POINT('Ctrl Pts',(48.0320944146206,-46.8221467489661,
-171.578102851547));
#154109=CARTESIAN_POINT('Ctrl Pts',(48.0095649832056,-46.8158219187507,
-171.568617968669));
#154110=CARTESIAN_POINT('Ctrl Pts',(47.9927425203933,-46.811099242038,-171.561535717611));
#154111=CARTESIAN_POINT('Ctrl Pts',(47.9768201788659,-46.8066397235393,
-171.554311410389));
#154112=CARTESIAN_POINT('Ctrl Pts',(47.9617741294179,-46.8024283376171,
-171.547061058122));
#154113=CARTESIAN_POINT('Ctrl Pts',(47.944175917045,-46.7975026018549,-171.538580876037));
#154114=CARTESIAN_POINT('Ctrl Pts',(47.9277764289289,-46.7929162833264,
-171.530065584821));
#154115=CARTESIAN_POINT('Ctrl Pts',(47.9125296815332,-46.7886393940512,
-171.521677794724));
#154116=CARTESIAN_POINT('Ctrl Pts',(47.9049063078353,-46.7865009494136,
-171.517483899676));
#154117=CARTESIAN_POINT('Ctrl Pts',(47.8975710137052,-46.7844397807934,
-171.513321495654));
#154118=CARTESIAN_POINT('Ctrl Pts',(47.8905175870556,-46.7824517721236,
-171.509208644575));
#154119=CARTESIAN_POINT('Ctrl Pts',(47.8869908737309,-46.7814577677886,
-171.507152219036));
#154120=CARTESIAN_POINT('Ctrl Pts',(47.8835346346846,-46.7804820586724,
-171.505108166637));
#154121=CARTESIAN_POINT('Ctrl Pts',(47.8801480654843,-46.7795241076621,
-171.503078598546));
#154122=CARTESIAN_POINT('Ctrl Pts',(47.8784547808841,-46.7790451321569,
-171.5020638145));
#154123=CARTESIAN_POINT('Ctrl Pts',(47.8767789142175,-46.7785705965115,
-171.501052650544));
#154124=CARTESIAN_POINT('Ctrl Pts',(47.8751203661658,-46.7781004343759,
-171.500045363464));
#154125=CARTESIAN_POINT('Ctrl Pts',(47.8737467023028,-46.7777110306835,
-171.499211095286));
#154126=CARTESIAN_POINT('Ctrl Pts',(47.8732028318327,-46.7775573985475,
-171.498880505616));
#154127=CARTESIAN_POINT('Ctrl Pts',(47.8714562342584,-46.7770609996115,
-171.497809237805));
#154128=CARTESIAN_POINT('Ctrl Pts',(47.8710940073364,-46.7769580514217,
-171.497587067542));
#154129=CARTESIAN_POINT('Ctrl Pts',(47.8706801156592,-46.7768404051464,
-171.49733291326));
#154130=CARTESIAN_POINT('Ctrl Pts',(47.8701965793844,-46.7767030026997,
-171.497035384937));
#154131=CARTESIAN_POINT('Ctrl Pts',(47.836561660035,-46.7671452498347,-171.476339231072));
#154132=CARTESIAN_POINT('Ctrl Pts',(47.8047036022027,-46.7580497202331,
-171.454035671718));
#154133=CARTESIAN_POINT('Ctrl Pts',(47.7746907554855,-46.7494720426908,
-171.430440242212));
#154134=CARTESIAN_POINT('Ctrl Pts',(47.744142879704,-46.7407414537359,-171.40642418481));
#154135=CARTESIAN_POINT('Ctrl Pts',(47.7155063657762,-46.7325472033367,
-171.381070282487));
#154136=CARTESIAN_POINT('Ctrl Pts',(47.6888109308635,-46.7249172690417,
-171.354698000924));
#154137=CARTESIAN_POINT('Ctrl Pts',(47.6613862780346,-46.7170789139135,
-171.327605328767));
#154138=CARTESIAN_POINT('Ctrl Pts',(47.6360099672327,-46.709835977306,-171.299438368667));
#154139=CARTESIAN_POINT('Ctrl Pts',(47.6126733279724,-46.7031888660082,
-171.270521985313));
#154140=CARTESIAN_POINT('Ctrl Pts',(47.5889579777984,-46.6964338842684,
-171.241136342017));
#154141=CARTESIAN_POINT('Ctrl Pts',(47.5673486778549,-46.6902939779218,
-171.210977135119));
#154142=CARTESIAN_POINT('Ctrl Pts',(47.547799316212,-46.6847421919371,-171.180356754921));
#154143=CARTESIAN_POINT('Ctrl Pts',(47.5277922694594,-46.6790604288296,
-171.1490194975));
#154144=CARTESIAN_POINT('Ctrl Pts',(47.5099423764393,-46.6739943919686,
-171.117199563618));
#154145=CARTESIAN_POINT('Ctrl Pts',(47.4941672862597,-46.669490540989,-171.085196501643));
#154146=CARTESIAN_POINT('Ctrl Pts',(47.4920938454406,-46.6688985653896,
-171.080990094308));
#154147=CARTESIAN_POINT('Ctrl Pts',(47.4900562077632,-46.6683162712008,
-171.076780470406));
#154148=CARTESIAN_POINT('Ctrl Pts',(47.4880541505297,-46.6677435098468,
-171.072568261741));
#154149=CARTESIAN_POINT('Ctrl Pts',(42.9629113790828,-52.2741145284007,
-171.07256826174));
#154150=CARTESIAN_POINT('Ctrl Pts',(42.9756222718615,-52.2782546634559,
-171.098672923949));
#154151=CARTESIAN_POINT('Ctrl Pts',(42.9897028705913,-52.2828396112092,
-171.124738297516));
#154152=CARTESIAN_POINT('Ctrl Pts',(43.0052476387318,-52.2878991708896,
-171.150543690017));
#154153=CARTESIAN_POINT('Ctrl Pts',(43.013330346337,-52.290529955803,-171.163961544844));
#154154=CARTESIAN_POINT('Ctrl Pts',(43.0218083812408,-52.293288881294,-171.177309700215));
#154155=CARTESIAN_POINT('Ctrl Pts',(43.0306913485009,-52.2961789110827,
-171.190561243996));
#154156=CARTESIAN_POINT('Ctrl Pts',(43.0470490146324,-52.3015007974534,
-171.214963487364));
#154157=CARTESIAN_POINT('Ctrl Pts',(43.064778803995,-52.3072669331714,-171.23903038737));
#154158=CARTESIAN_POINT('Ctrl Pts',(43.0839005275333,-52.31348256218,-171.262607653843));
#154159=CARTESIAN_POINT('Ctrl Pts',(43.0949669386116,-52.3170797643665,
-171.276252643657));
#154160=CARTESIAN_POINT('Ctrl Pts',(43.1064988617158,-52.3208272871931,
-171.289734426472));
#154161=CARTESIAN_POINT('Ctrl Pts',(43.1184942836132,-52.3247242103712,
-171.303029756078));
#154162=CARTESIAN_POINT('Ctrl Pts',(43.1272258290788,-52.3275608060489,
-171.312707512804));
#154163=CARTESIAN_POINT('Ctrl Pts',(43.1362057486528,-52.3304774679509,
-171.322290183655));
#154164=CARTESIAN_POINT('Ctrl Pts',(43.14544820496,-52.333478680082,-171.331785371289));
#154165=CARTESIAN_POINT('Ctrl Pts',(43.1595109854538,-52.3380451487795,
-171.346232692977));
#154166=CARTESIAN_POINT('Ctrl Pts',(43.1740872867586,-52.3427767262898,
-171.360366229518));
#154167=CARTESIAN_POINT('Ctrl Pts',(43.1892239439584,-52.3476882653286,
-171.374181494434));
#154168=CARTESIAN_POINT('Ctrl Pts',(43.1988301566281,-52.3508052870011,
-171.382949108783));
#154169=CARTESIAN_POINT('Ctrl Pts',(43.2086621092605,-52.3539948050664,
-171.391588325689));
#154170=CARTESIAN_POINT('Ctrl Pts',(43.2187321357514,-52.3572607157877,
-171.400095850004));
#154171=CARTESIAN_POINT('Ctrl Pts',(43.2278830511384,-52.3602285404205,
-171.407826875858));
#154172=CARTESIAN_POINT('Ctrl Pts',(43.2372323602375,-52.3632600301537,
-171.415450206072));
#154173=CARTESIAN_POINT('Ctrl Pts',(43.2467668483314,-52.3663508159467,
-171.422945451982));
#154174=CARTESIAN_POINT('Ctrl Pts',(43.2728213692292,-52.3747968848117,
-171.443427415909));
#154175=CARTESIAN_POINT('Ctrl Pts',(43.3002828482488,-52.3836935947796,
-171.462969026633));
#154176=CARTESIAN_POINT('Ctrl Pts',(43.3291050777233,-52.3930240911597,
-171.481391787822));
#154177=CARTESIAN_POINT('Ctrl Pts',(43.332995320062,-52.3942834625797,-171.48387837567));
#154178=CARTESIAN_POINT('Ctrl Pts',(43.3369103005577,-52.3955507194566,
-171.486344636295));
#154179=CARTESIAN_POINT('Ctrl Pts',(43.3408498612603,-52.3968258055869,
-171.488790186207));
#154180=CARTESIAN_POINT('Ctrl Pts',(43.3444738260935,-52.3979987453243,
-171.491039824568));
#154181=CARTESIAN_POINT('Ctrl Pts',(43.348619785142,-52.3993405084081,-171.493577576822));
#154182=CARTESIAN_POINT('Ctrl Pts',(43.352338286152,-52.4005438861322,-171.495820868468));
#154183=CARTESIAN_POINT('Ctrl Pts',(43.3545029203103,-52.4012444029587,
-171.497126745677));
#154184=CARTESIAN_POINT('Ctrl Pts',(43.3565222632456,-52.401897888212,-171.498333988034));
#154185=CARTESIAN_POINT('Ctrl Pts',(43.3582062180294,-52.4024428669334,
-171.499335182402));
#154186=CARTESIAN_POINT('Ctrl Pts',(43.3649105815967,-52.4046126018451,
-171.503321257986));
#154187=CARTESIAN_POINT('Ctrl Pts',(43.3717389531774,-52.4068219286436,
-171.507281191728));
#154188=CARTESIAN_POINT('Ctrl Pts',(43.3786925372967,-52.4090712396164,
-171.51120960731));
#154189=CARTESIAN_POINT('Ctrl Pts',(43.4008365800392,-52.4162342849567,
-171.523719846788));
#154190=CARTESIAN_POINT('Ctrl Pts',(43.4243162170495,-52.423824032754,-171.535916815119));
#154191=CARTESIAN_POINT('Ctrl Pts',(43.4491265174689,-52.4318390452238,
-171.547571669372));
#154192=CARTESIAN_POINT('Ctrl Pts',(43.4590725867668,-52.435052140918,-171.552243921867));
#154193=CARTESIAN_POINT('Ctrl Pts',(43.4692320307583,-52.4383334238362,
-171.556828799921));
#154194=CARTESIAN_POINT('Ctrl Pts',(43.4796024564523,-52.4416821170203,
-171.561310538145));
#154195=CARTESIAN_POINT('Ctrl Pts',(43.5054793388387,-52.4500379687691,
-171.572493629016));
#154196=CARTESIAN_POINT('Ctrl Pts',(43.5326922691112,-52.4588199433374,
-171.583046072084));
#154197=CARTESIAN_POINT('Ctrl Pts',(43.5612393729964,-52.4680256720035,
-171.592719713033));
#154198=CARTESIAN_POINT('Ctrl Pts',(43.57551499012,-52.4726292023059,-171.597557233327));
#154199=CARTESIAN_POINT('Ctrl Pts',(43.5901240191453,-52.4773386219235,
-171.602174491315));
#154200=CARTESIAN_POINT('Ctrl Pts',(43.6050638744462,-52.4821528303647,
-171.606536419614));
#154201=CARTESIAN_POINT('Ctrl Pts',(43.6082649632574,-52.4831843469668,
-171.60747102839));
#154202=CARTESIAN_POINT('Ctrl Pts',(43.6114812396548,-52.4842206741277,
-171.608393905187));
#154203=CARTESIAN_POINT('Ctrl Pts',(43.614712668377,-52.4852618572514,-171.609304696318));
#154204=CARTESIAN_POINT('Ctrl Pts',(43.6171456120831,-52.4860457643543,
-171.609990431249));
#154205=CARTESIAN_POINT('Ctrl Pts',(43.6204559687148,-52.4871122872049,
-171.610908827037));
#154206=CARTESIAN_POINT('Ctrl Pts',(43.6226813902947,-52.4878292091908,
-171.611517580204));
#154207=CARTESIAN_POINT('Ctrl Pts',(43.6234117671554,-52.4880645008919,
-171.611717371216));
#154208=CARTESIAN_POINT('Ctrl Pts',(43.6240252456133,-52.4882621270372,
-171.611884340861));
#154209=CARTESIAN_POINT('Ctrl Pts',(43.6244523866038,-52.4883997220079,
-171.612000396047));
#154210=CARTESIAN_POINT('Ctrl Pts',(43.6289479545664,-52.4898478797731,
-171.61322185216));
#154211=CARTESIAN_POINT('Ctrl Pts',(43.6337045827901,-52.4913799689085,
-171.614482833112));
#154212=CARTESIAN_POINT('Ctrl Pts',(43.6387203708674,-52.49299531386,-171.615771589263));
#154213=CARTESIAN_POINT('Ctrl Pts',(43.6521489264918,-52.4973200080455,
-171.619221921174));
#154214=CARTESIAN_POINT('Ctrl Pts',(43.6674571356465,-52.5022486368226,
-171.622889155636));
#154215=CARTESIAN_POINT('Ctrl Pts',(43.6846428372704,-52.5077791164167,
-171.626522702309));
#154216=CARTESIAN_POINT('Ctrl Pts',(43.702262529913,-52.5134492573716,-171.630248007041));
#154217=CARTESIAN_POINT('Ctrl Pts',(43.7218557516377,-52.5197520367826,
-171.633937845606));
#154218=CARTESIAN_POINT('Ctrl Pts',(43.7434271305591,-52.5266870794093,
-171.6372677803));
#154219=CARTESIAN_POINT('Ctrl Pts',(43.7653502121052,-52.5337351918914,
-171.640652006691));
#154220=CARTESIAN_POINT('Ctrl Pts',(43.7893165109233,-52.5414363642839,
-171.643664337744));
#154221=CARTESIAN_POINT('Ctrl Pts',(43.8153376259069,-52.549791966158,-171.64591050217));
#154222=CARTESIAN_POINT('Ctrl Pts',(43.8419949736875,-52.5583518678077,
-171.648211586744));
#154223=CARTESIAN_POINT('Ctrl Pts',(43.8708088768737,-52.5675986046511,
-171.649708459496));
#154224=CARTESIAN_POINT('Ctrl Pts',(43.9017983937575,-52.577535306748,-171.649923358981));
#154225=CARTESIAN_POINT('Ctrl Pts',(43.9043460731332,-52.5783522130292,
-171.649941026084));
#154226=CARTESIAN_POINT('Ctrl Pts',(43.9069084601724,-52.5791737833863,
-171.64995));
#154227=CARTESIAN_POINT('Ctrl Pts',(43.9094855672884,-52.58000002,-171.64995));
#154228=CARTESIAN_POINT('Origin',(0.,-12.9675000200281,-171.64995));
#154229=CARTESIAN_POINT('',(49.6300753314849,-52.58000002,-171.64995));
#154230=CARTESIAN_POINT('',(50.4241310475534,-46.93000002,-171.64995));
#154231=CARTESIAN_POINT('',(50.5139609686817,-46.2908269190399,-171.64995));
#154232=CARTESIAN_POINT('',(48.7591445042216,-46.93000002,-171.64995));
#154233=CARTESIAN_POINT('',(49.5598049141337,-52.58000002,-171.64995));
#154234=CARTESIAN_POINT('Origin',(60.,-2.55003103885676E-14,0.));
#154235=CARTESIAN_POINT('',(60.,-53.58000002,-58.24995));
#154236=CARTESIAN_POINT('',(60.,-54.08000002,-58.24995));
#154237=CARTESIAN_POINT('',(60.,-54.58000002,-58.24995));
#154238=CARTESIAN_POINT('',(60.,-54.08000002,-174.34995));
#154239=CARTESIAN_POINT('',(60.,-54.08000002,-174.34995));
#154240=CARTESIAN_POINT('',(60.,-53.58000002,-174.34995));
#154241=CARTESIAN_POINT('',(60.,28.41999998,-174.34995));
#154242=CARTESIAN_POINT('',(60.,-53.58000002,-58.24995));
#154243=CARTESIAN_POINT('Origin',(57.,-2.42462934179819E-14,-174.34995));
#154244=CARTESIAN_POINT('',(57.,-54.08000002,-177.34995));
#154245=CARTESIAN_POINT('Origin',(57.,-54.08000002,-174.34995));
#154246=CARTESIAN_POINT('',(57.,-53.58000002,-177.34995));
#154247=CARTESIAN_POINT('',(57.,-54.58000002,-177.34995));
#154248=CARTESIAN_POINT('Origin',(57.,-53.58000002,-174.34995));
#154249=CARTESIAN_POINT('Origin',(60.,28.41999998,-177.34995));
#154250=CARTESIAN_POINT('',(50.9340054382093,-54.08000002,-177.34995));
#154251=CARTESIAN_POINT('',(60.,-54.08000002,-177.34995));
#154252=CARTESIAN_POINT('',(51.0042758555605,-53.58000002,-177.34995));
#154253=CARTESIAN_POINT('',(62.4796469926385,28.0715083218873,-177.34995));
#154254=CARTESIAN_POINT('',(60.,-53.58000002,-177.34995));
#154255=CARTESIAN_POINT('Origin',(0.,-12.9675000200281,-170.64995));
#154256=CARTESIAN_POINT('',(52.1126146143194,-39.473850183348,-171.391638125813));
#154257=CARTESIAN_POINT('',(52.4185037493065,-38.6078427690472,-171.271207233798));
#154258=CARTESIAN_POINT('Ctrl Pts',(52.1126146143194,-39.473850183348,-171.391638125813));
#154259=CARTESIAN_POINT('Ctrl Pts',(52.1380831145661,-39.3921942843444,
-171.378688901202));
#154260=CARTESIAN_POINT('Ctrl Pts',(52.1640396477339,-39.3120540081033,
-171.366154150429));
#154261=CARTESIAN_POINT('Ctrl Pts',(52.1904049108065,-39.233350279785,-171.354220830313));
#154262=CARTESIAN_POINT('Ctrl Pts',(52.21740941517,-39.1527383333408,-171.341998179841));
#154263=CARTESIAN_POINT('Ctrl Pts',(52.2448426634599,-39.0736335235921,
-171.33040624582));
#154264=CARTESIAN_POINT('Ctrl Pts',(52.2726181340388,-38.9959696675765,
-171.319592910656));
#154265=CARTESIAN_POINT('Ctrl Pts',(52.3015399982203,-38.9151003448007,
-171.308333270246));
#154266=CARTESIAN_POINT('Ctrl Pts',(52.3308328658517,-38.8357934271155,
-171.297917697251));
#154267=CARTESIAN_POINT('Ctrl Pts',(52.3603984063869,-38.7579933413912,
-171.288458976171));
#154268=CARTESIAN_POINT('Ctrl Pts',(52.3796601931508,-38.7073070141901,
-171.2822966715));
#154269=CARTESIAN_POINT('Ctrl Pts',(52.3990377034992,-38.657260644957,-171.27653939255));
#154270=CARTESIAN_POINT('Ctrl Pts',(52.4185037670893,-38.6078427777457,
-171.271207218103));
#154271=CARTESIAN_POINT('',(52.2951895046066,-38.58067735034,-171.07256826174));
#154272=CARTESIAN_POINT('Origin',(53.1718788440769,-38.7731638601678,-170.641452709883));
#154273=CARTESIAN_POINT('',(49.1544657093286,-44.1870483688939,-171.07256826174));
#154274=CARTESIAN_POINT('Origin',(0.,-12.9675000200281,-171.07256826174));
#154275=CARTESIAN_POINT('Ctrl Pts',(49.1544657093286,-44.1870483688939,
-171.07256826174));
#154276=CARTESIAN_POINT('Ctrl Pts',(49.1674099450031,-44.1904999604323,
-171.099968982618));
#154277=CARTESIAN_POINT('Ctrl Pts',(49.1818195618825,-44.1943411562328,
-171.12729943789));
#154278=CARTESIAN_POINT('Ctrl Pts',(49.1977879406042,-44.1985958890317,
-171.154324681996));
#154279=CARTESIAN_POINT('Ctrl Pts',(49.2047680888881,-44.2004557313089,
-171.166138042298));
#154280=CARTESIAN_POINT('Ctrl Pts',(49.2120456036907,-44.2023944608238,
-171.177893516791));
#154281=CARTESIAN_POINT('Ctrl Pts',(49.2196259920141,-44.2044134518367,
-171.189573569196));
#154282=CARTESIAN_POINT('Ctrl Pts',(49.2343858775653,-44.2083446589212,
-171.212315970954));
#154283=CARTESIAN_POINT('Ctrl Pts',(49.2502933549397,-44.2125799775673,
-171.234767669611));
#154284=CARTESIAN_POINT('Ctrl Pts',(49.2673661857556,-44.2171233653378,
-171.256807716226));
#154285=CARTESIAN_POINT('Ctrl Pts',(49.2780167292262,-44.2199576667771,
-171.27055695776));
#154286=CARTESIAN_POINT('Ctrl Pts',(49.2891203199703,-44.2229117312905,
-171.284146427066));
#154287=CARTESIAN_POINT('Ctrl Pts',(49.3006765847195,-44.2259852536784,
-171.297551077901));
#154288=CARTESIAN_POINT('Ctrl Pts',(49.3076450228149,-44.2278385904581,
-171.305634094477));
#154289=CARTESIAN_POINT('Ctrl Pts',(49.3147792321624,-44.2297356757576,
-171.31365165429));
#154290=CARTESIAN_POINT('Ctrl Pts',(49.322089013489,-44.2316790662859,-171.321609324439));
#154291=CARTESIAN_POINT('Ctrl Pts',(49.3361254166797,-44.2354108076054,
-171.336889818026));
#154292=CARTESIAN_POINT('Ctrl Pts',(49.3507349332876,-44.2392935037787,
-171.351849549341));
#154293=CARTESIAN_POINT('Ctrl Pts',(49.3659444071017,-44.2433339581765,
-171.366466996183));
#154294=CARTESIAN_POINT('Ctrl Pts',(49.3768819596723,-44.2462395604955,
-171.376978805811));
#154295=CARTESIAN_POINT('Ctrl Pts',(49.3881298096026,-44.2492267542621,
-171.387313431887));
#154296=CARTESIAN_POINT('Ctrl Pts',(49.3996980831345,-44.2522980875319,
-171.397460025651));
#154297=CARTESIAN_POINT('Ctrl Pts',(49.4100384253246,-44.2550434096321,
-171.406529594355));
#154298=CARTESIAN_POINT('Ctrl Pts',(49.420635347381,-44.2578561071891,-171.415448967782));
#154299=CARTESIAN_POINT('Ctrl Pts',(49.4314773883421,-44.2607330292976,
-171.424194851323));
#154300=CARTESIAN_POINT('Ctrl Pts',(49.4582917280625,-44.2678481810523,
-171.445825012401));
#154301=CARTESIAN_POINT('Ctrl Pts',(49.4866223506434,-44.275360699466,-171.466406988852));
#154302=CARTESIAN_POINT('Ctrl Pts',(49.5164137343661,-44.283254020249,-171.485716798992));
#154303=CARTESIAN_POINT('Ctrl Pts',(49.5199598905896,-44.2841935854897,
-171.488015302615));
#154304=CARTESIAN_POINT('Ctrl Pts',(49.5239976875963,-44.2852633080731,
-171.490595498519));
#154305=CARTESIAN_POINT('Ctrl Pts',(49.5276130959414,-44.2862210486011,
-171.492872353817));
#154306=CARTESIAN_POINT('Ctrl Pts',(49.5295802652792,-44.2867421620191,
-171.494111206943));
#154307=CARTESIAN_POINT('Ctrl Pts',(49.531421900296,-44.2872299980374,-171.49526124167));
#154308=CARTESIAN_POINT('Ctrl Pts',(49.5329880148365,-44.2876448451646,
-171.496233960813));
#154309=CARTESIAN_POINT('Ctrl Pts',(49.5370095623471,-44.2887101104364,
-171.498731757843));
#154310=CARTESIAN_POINT('Ctrl Pts',(49.5410793863111,-44.2897880343388,
-171.501220670594));
#154311=CARTESIAN_POINT('Ctrl Pts',(49.5451978658055,-44.2908787108092,
-171.503699197074));
#154312=CARTESIAN_POINT('Ctrl Pts',(49.5699429400149,-44.2974318259181,
-171.518590936068));
#154313=CARTESIAN_POINT('Ctrl Pts',(49.5964058211158,-44.3044348265418,
-171.533094285846));
#154314=CARTESIAN_POINT('Ctrl Pts',(49.6246582855736,-44.3119055301866,
-171.54685574217));
#154315=CARTESIAN_POINT('Ctrl Pts',(49.6332772021546,-44.3141846011545,
-171.551053919085));
#154316=CARTESIAN_POINT('Ctrl Pts',(49.6420624484702,-44.3165071389794,
-171.555182772464));
#154317=CARTESIAN_POINT('Ctrl Pts',(49.6510154288811,-44.3188734756713,
-171.559231527241));
#154318=CARTESIAN_POINT('Ctrl Pts',(49.6726079214831,-44.3245805257451,
-171.568996175831));
#154319=CARTESIAN_POINT('Ctrl Pts',(49.6951721931324,-44.3305411806568,
-171.578293225514));
#154320=CARTESIAN_POINT('Ctrl Pts',(49.7187075835833,-44.3367544577215,
-171.586960972345));
#154321=CARTESIAN_POINT('Ctrl Pts',(49.7304752788088,-44.3398610962538,
-171.59129484576));
#154322=CARTESIAN_POINT('Ctrl Pts',(49.7424854973315,-44.3430308211926,
-171.595471243433));
#154323=CARTESIAN_POINT('Ctrl Pts',(49.7547365163585,-44.3462630678917,
-171.599469109271));
#154324=CARTESIAN_POINT('Ctrl Pts',(49.760862025872,-44.3478791912413,-171.601468042189));
#154325=CARTESIAN_POINT('Ctrl Pts',(49.7670477359762,-44.3495109450574,
-171.603422339684));
#154326=CARTESIAN_POINT('Ctrl Pts',(49.7732933004513,-44.3511582236526,
-171.605329314684));
#154327=CARTESIAN_POINT('Ctrl Pts',(49.7764160826888,-44.3519818629502,
-171.606282802184));
#154328=CARTESIAN_POINT('Ctrl Pts',(49.77955382855,-44.3528093834448,-171.607224458979));
#154329=CARTESIAN_POINT('Ctrl Pts',(49.7827064904596,-44.3536407707549,
-171.608153947255));
#154330=CARTESIAN_POINT('Ctrl Pts',(49.7851118263354,-44.3542750809921,
-171.608863104012));
#154331=CARTESIAN_POINT('Ctrl Pts',(49.7883547859396,-44.3551302199853,
-171.60980415202));
#154332=CARTESIAN_POINT('Ctrl Pts',(49.7905382446473,-44.3557059426006,
-171.610428960928));
#154333=CARTESIAN_POINT('Ctrl Pts',(49.7912166345354,-44.3558848167874,
-171.610623085984));
#154334=CARTESIAN_POINT('Ctrl Pts',(49.791792643767,-44.356036692665,-171.610787142201));
#154335=CARTESIAN_POINT('Ctrl Pts',(49.7922091744941,-44.3561465181287,
-171.610905567567));
#154336=CARTESIAN_POINT('Ctrl Pts',(49.8044703717807,-44.3593793928967,
-171.614391593156));
#154337=CARTESIAN_POINT('Ctrl Pts',(49.8184706367615,-44.3630698175465,
-171.618127956761));
#154338=CARTESIAN_POINT('Ctrl Pts',(49.8342418983615,-44.3672252172811,
-171.621894685085));
#154339=CARTESIAN_POINT('Ctrl Pts',(49.8498640564744,-44.3713413313448,
-171.625625802286));
#154340=CARTESIAN_POINT('Ctrl Pts',(49.8672244691343,-44.3759138263744,
-171.629386605));
#154341=CARTESIAN_POINT('Ctrl Pts',(49.8863472451527,-44.3809478076652,
-171.632913171055));
#154342=CARTESIAN_POINT('Ctrl Pts',(49.9052048010337,-44.385911970996,-171.636390825993));
#154343=CARTESIAN_POINT('Ctrl Pts',(49.9257768087209,-44.3913250774835,
-171.639640560882));
#154344=CARTESIAN_POINT('Ctrl Pts',(49.9480705932716,-44.3971875545849,
-171.64236215772));
#154345=CARTESIAN_POINT('Ctrl Pts',(49.969627485023,-44.4028562549342,-171.644993795623));
#154346=CARTESIAN_POINT('Ctrl Pts',(49.9927947579018,-44.4089452546521,
-171.647131375962));
#154347=CARTESIAN_POINT('Ctrl Pts',(50.0175556679848,-44.4154484770367,
-171.64846219077));
#154348=CARTESIAN_POINT('Ctrl Pts',(50.0352273714949,-44.4200897853511,
-171.649411984806));
#154349=CARTESIAN_POINT('Ctrl Pts',(50.0537103637574,-44.4249419583976,
-171.64995));
#154350=CARTESIAN_POINT('Ctrl Pts',(50.0729884546894,-44.43000002,-171.64995));
#154351=CARTESIAN_POINT('Ctrl Pts',(50.9867892914962,-42.9264785869994,
-171.64995));
#154352=CARTESIAN_POINT('Ctrl Pts',(51.0240482415051,-42.8168542892489,
-171.64995));
#154353=CARTESIAN_POINT('Ctrl Pts',(51.0922171107721,-42.6180583252229,
-171.649619189927));
#154354=CARTESIAN_POINT('Ctrl Pts',(51.2371844845627,-42.18600352108,-171.638403047895));
#154355=CARTESIAN_POINT('Ctrl Pts',(51.2926025880972,-42.0196813435606,
-171.632782871465));
#154356=CARTESIAN_POINT('Ctrl Pts',(51.385977497022,-41.7369244128409,-171.619483440323));
#154357=CARTESIAN_POINT('Ctrl Pts',(51.4188123620423,-41.6371286285496,
-171.614233886791));
#154358=CARTESIAN_POINT('Ctrl Pts',(51.4706089315109,-41.4791663653461,
-171.604841992257));
#154359=CARTESIAN_POINT('Ctrl Pts',(51.4971436791054,-41.3981183730614,
-171.599766324506));
#154360=CARTESIAN_POINT('Ctrl Pts',(51.5292150542645,-41.2999588202135,
-171.593113195487));
#154361=CARTESIAN_POINT('Ctrl Pts',(51.5455297532666,-41.2499800948475,
-171.58959521104));
#154362=CARTESIAN_POINT('Ctrl Pts',(51.5525816181663,-41.2283682241181,
-171.588045568303));
#154363=CARTESIAN_POINT('Ctrl Pts',(51.5572961698944,-41.2139175755746,
-171.587003052042));
#154364=CARTESIAN_POINT('Ctrl Pts',(51.5601091265564,-41.2052942020437,
-171.586376554727));
#154365=CARTESIAN_POINT('Ctrl Pts',(51.8079906336108,-40.4453081581786,
-171.53088053051));
#154366=CARTESIAN_POINT('Ctrl Pts',(51.9887431992002,-39.8710008464974,
-171.454619407075));
#154367=CARTESIAN_POINT('Ctrl Pts',(52.1126146143194,-39.473850183348,-171.391638125813));
#154368=CARTESIAN_POINT('Origin',(0.,-12.9675000200281,-171.64995));
#154369=CARTESIAN_POINT('',(40.1769968691492,-38.5367831582149,-148.324645026283));
#154370=CARTESIAN_POINT('Ctrl Pts',(52.2951895046066,-38.58067735034,-171.07256826174));
#154371=CARTESIAN_POINT('Ctrl Pts',(51.611967682992,-38.5785901798911,-169.754773540737));
#154372=CARTESIAN_POINT('Ctrl Pts',(50.9382354286579,-38.5764745002471,
-168.460090147878));
#154373=CARTESIAN_POINT('Ctrl Pts',(50.2739302308651,-38.5743305031011,
-167.188544893716));
#154374=CARTESIAN_POINT('Ctrl Pts',(49.5884175161196,-38.5721180602227,
-165.876406373652));
#154375=CARTESIAN_POINT('Ctrl Pts',(48.9129436968084,-38.5698754660624,
-164.588907334074));
#154376=CARTESIAN_POINT('Ctrl Pts',(48.2474886948655,-38.5676040651517,
-163.32604780964));
#154377=CARTESIAN_POINT('Ctrl Pts',(47.5987203612334,-38.5653896209301,
-162.094855216772));
#154378=CARTESIAN_POINT('Ctrl Pts',(46.9594752653591,-38.5631478085241,
-160.887081815245));
#154379=CARTESIAN_POINT('Ctrl Pts',(46.3297741930984,-38.5608808096086,
-159.702700873047));
#154380=CARTESIAN_POINT('Ctrl Pts',(46.3223172763666,-38.5608539638196,
-159.68867544026));
#154381=CARTESIAN_POINT('Ctrl Pts',(46.31576784214,-38.5608303787607,-159.676357433767));
#154382=CARTESIAN_POINT('Ctrl Pts',(46.3074074634252,-38.5608002522641,
-159.660634412727));
#154383=CARTESIAN_POINT('Ctrl Pts',(46.3072537239608,-38.5607996982663,
-159.660345281227));
#154384=CARTESIAN_POINT('Ctrl Pts',(46.3070999849996,-38.5607991442668,
-159.660056150999));
#154385=CARTESIAN_POINT('Ctrl Pts',(46.3069462465417,-38.5607985902656,
-159.65976702204));
#154386=CARTESIAN_POINT('Ctrl Pts',(45.7108946304494,-38.5586507000882,
-158.538799730412));
#154387=CARTESIAN_POINT('Ctrl Pts',(45.1224208024696,-38.5564771811492,
-157.436924140047));
#154388=CARTESIAN_POINT('Ctrl Pts',(44.5414447167035,-38.55427822462,-156.354171396456));
#154389=CARTESIAN_POINT('Ctrl Pts',(43.9496124781868,-38.5520381782619,
-155.251186272456));
#154390=CARTESIAN_POINT('Ctrl Pts',(43.3655609703394,-38.5497717381949,
-154.168045243083));
#154391=CARTESIAN_POINT('Ctrl Pts',(42.7892537562729,-38.5474800295275,
-153.104754637799));
#154392=CARTESIAN_POINT('Ctrl Pts',(42.1951910911732,-38.5451177155995,
-152.008705108427));
#154393=CARTESIAN_POINT('Ctrl Pts',(41.6093573588218,-38.542728554327,-150.933747933629));
#154394=CARTESIAN_POINT('Ctrl Pts',(41.0317614677954,-38.5403147086464,
-149.879863096509));
#154395=CARTESIAN_POINT('Ctrl Pts',(40.744805903117,-38.5391154853468,-149.356282296784));
#154396=CARTESIAN_POINT('Ctrl Pts',(40.45988434067,-38.5379101834035,-148.837902175));
#154397=CARTESIAN_POINT('Ctrl Pts',(40.1770020116941,-38.5366991465431,
-148.324717991527));
#154398=CARTESIAN_POINT('',(40.4124516162331,-44.1531546061648,-155.665156220206));
#154399=CARTESIAN_POINT('Ctrl Pts',(40.1769969654164,-38.5367854529716,
-148.324647842671));
#154400=CARTESIAN_POINT('Ctrl Pts',(40.1948823687306,-38.9631265319537,
-148.847902586266));
#154401=CARTESIAN_POINT('Ctrl Pts',(40.2129052771572,-39.3918670421897,
-149.382496639157));
#154402=CARTESIAN_POINT('Ctrl Pts',(40.2310530620268,-39.8234241172529,
-149.928744356201));
#154403=CARTESIAN_POINT('Ctrl Pts',(40.2392538151749,-40.0184392701975,
-150.175586751426));
#154404=CARTESIAN_POINT('Ctrl Pts',(40.2474800182096,-40.2140300019281,
-150.424808356685));
#154405=CARTESIAN_POINT('Ctrl Pts',(40.2557302446384,-40.410237152229,-150.67643548022));
#154406=CARTESIAN_POINT('Ctrl Pts',(40.2737019599345,-40.8376410634674,
-151.224562378794));
#154407=CARTESIAN_POINT('Ctrl Pts',(40.2917665359898,-41.2674257878512,
-151.783444601094));
#154408=CARTESIAN_POINT('Ctrl Pts',(40.3099131424047,-41.6997961521597,
-152.353294054308));
#154409=CARTESIAN_POINT('Ctrl Pts',(40.326999464829,-42.106903645561,-152.889847901806));
#154410=CARTESIAN_POINT('Ctrl Pts',(40.3441585036013,-42.516303297068,-153.436124940354));
#154411=CARTESIAN_POINT('Ctrl Pts',(40.361378696468,-42.9281717249953,-153.99225788082));
#154412=CARTESIAN_POINT('Ctrl Pts',(40.3783481518696,-43.3340430745853,
-154.540293155664));
#154413=CARTESIAN_POINT('Ctrl Pts',(40.3953770040522,-43.7423116398837,
-155.097899842787));
#154414=CARTESIAN_POINT('Ctrl Pts',(40.4124516185963,-44.1531546492746,
-155.665156176616));
#154415=CARTESIAN_POINT('Ctrl Pts',(40.4124516249929,-44.1531545436406,
-155.665156257244));
#154416=CARTESIAN_POINT('Ctrl Pts',(40.9798621708435,-44.1555773238801,
-156.631664486591));
#154417=CARTESIAN_POINT('Ctrl Pts',(41.5543790914707,-44.1579855398722,
-157.617504781648));
#154418=CARTESIAN_POINT('Ctrl Pts',(42.1359452197555,-44.1603762923632,
-158.622735508298));
#154419=CARTESIAN_POINT('Ctrl Pts',(42.696413965657,-44.1626803159045,-159.59149963899));
#154420=CARTESIAN_POINT('Ctrl Pts',(43.2634297031817,-44.1649681190063,
-160.57827289928));
#154421=CARTESIAN_POINT('Ctrl Pts',(43.8369823248252,-44.167237552928,-161.58308298225));
#154422=CARTESIAN_POINT('Ctrl Pts',(44.4001337756382,-44.1694658314804,
-162.569671195192));
#154423=CARTESIAN_POINT('Ctrl Pts',(44.9695870210121,-44.1716763989756,
-163.57364806962));
#154424=CARTESIAN_POINT('Ctrl Pts',(45.5453744486588,-44.1738676841351,
-164.595014746654));
#154425=CARTESIAN_POINT('Ctrl Pts',(46.1335504926022,-44.1761061168871,
-165.638357102996));
#154426=CARTESIAN_POINT('Ctrl Pts',(46.7283357453045,-44.178324422888,-166.699845913526));
#154427=CARTESIAN_POINT('Ctrl Pts',(47.3298140619878,-44.1805214778239,
-167.779452924363));
#154428=CARTESIAN_POINT('Ctrl Pts',(47.8957945550262,-44.1825888677885,
-168.795344090068));
#154429=CARTESIAN_POINT('Ctrl Pts',(48.4677016046433,-44.1846374429551,
-169.827277858276));
#154430=CARTESIAN_POINT('Ctrl Pts',(49.0456491794116,-44.1866667637444,
-170.875204350381));
#154431=CARTESIAN_POINT('Ctrl Pts',(49.081897568424,-44.1867940410488,-170.940929424419));
#154432=CARTESIAN_POINT('Ctrl Pts',(49.1181697337045,-44.1869212427789,
-171.00671740016));
#154433=CARTESIAN_POINT('Ctrl Pts',(49.1544657093286,-44.1870483688939,
-171.07256826174));
#154434=CARTESIAN_POINT('Ctrl Pts',(39.,-46.9678749402838,-153.612705479043));
#154435=CARTESIAN_POINT('Ctrl Pts',(38.9999999999999,-45.3542560507482,
-154.843289706001));
#154436=CARTESIAN_POINT('Ctrl Pts',(40.4142759901646,-44.1970576517619,
-155.725796787747));
#154437=CARTESIAN_POINT('Ctrl Pts',(39.,-45.668184102287,-151.908469685114));
#154438=CARTESIAN_POINT('Ctrl Pts',(39.,-44.1065443282322,-153.136806613681));
#154439=CARTESIAN_POINT('Ctrl Pts',(40.3630305742695,-42.9636912658246,
-154.021570941673));
#154440=CARTESIAN_POINT('Ctrl Pts',(39.,-44.3354350613925,-150.221485398912));
#154441=CARTESIAN_POINT('Ctrl Pts',(39.0000000000074,-42.8253385188873,
-151.442463829735));
#154442=CARTESIAN_POINT('Ctrl Pts',(40.3100965640753,-41.7031787097929,
-152.33457670764));
#154443=CARTESIAN_POINT('Ctrl Pts',(39.,-41.5900521206853,-146.90520294412));
#154444=CARTESIAN_POINT('Ctrl Pts',(38.9999999999925,-40.1892814621382,
-148.11112464401));
#154445=CARTESIAN_POINT('Ctrl Pts',(40.2013639252015,-39.117295594665,-149.018294252799));
#154446=CARTESIAN_POINT('Ctrl Pts',(39.,-40.1827079235241,-145.281958716849));
#154447=CARTESIAN_POINT('Ctrl Pts',(39.,-38.8402571910301,-146.480210875403));
#154448=CARTESIAN_POINT('Ctrl Pts',(40.1457602981154,-37.7969071359042,
-147.395068273086));
#154449=CARTESIAN_POINT('Ctrl Pts',(39.,-38.728281830342,-143.706077818883));
#154450=CARTESIAN_POINT('Ctrl Pts',(38.9999999999999,-37.4435486267092,
-144.891795278378));
#154451=CARTESIAN_POINT('Ctrl Pts',(40.0893978502897,-36.4387325411231,
-145.819169127587));
#154452=CARTESIAN_POINT('',(39.,-38.78000002,-143.762156710948));
#154453=CARTESIAN_POINT('Ctrl Pts',(40.1769968691492,-38.5367831582149,
-148.324645026283));
#154454=CARTESIAN_POINT('Ctrl Pts',(40.1355273735409,-38.5405885510441,
-148.253998247274));
#154455=CARTESIAN_POINT('Ctrl Pts',(40.0931293305385,-38.5444852864301,
-148.178893064488));
#154456=CARTESIAN_POINT('Ctrl Pts',(40.050116838129,-38.5485760914372,-148.099208883115));
#154457=CARTESIAN_POINT('Ctrl Pts',(40.0079564572523,-38.5525858543579,
-148.02110330847));
#154458=CARTESIAN_POINT('Ctrl Pts',(39.9652058213465,-38.5567825344687,
-147.938597973455));
#154459=CARTESIAN_POINT('Ctrl Pts',(39.9222048827104,-38.5612440999661,
-147.851590185633));
#154460=CARTESIAN_POINT('Ctrl Pts',(39.880442017431,-38.5655772090728,-147.767087506475));
#154461=CARTESIAN_POINT('Ctrl Pts',(39.8384433132321,-38.5701605578681,
-147.678337561074));
#154462=CARTESIAN_POINT('Ctrl Pts',(39.7965596110765,-38.575041557274,-147.585261996377));
#154463=CARTESIAN_POINT('Ctrl Pts',(39.7703977220409,-38.578090384342,-147.527124046047));
#154464=CARTESIAN_POINT('Ctrl Pts',(39.744281479466,-38.581254848957,-147.467298719482));
#154465=CARTESIAN_POINT('Ctrl Pts',(39.718303767535,-38.5845404963934,-147.405771116491));
#154466=CARTESIAN_POINT('Ctrl Pts',(39.6781910428581,-38.589613932859,-147.310765066484));
#154467=CARTESIAN_POINT('Ctrl Pts',(39.6384072401214,-38.59497820995,-147.21169883425));
#154468=CARTESIAN_POINT('Ctrl Pts',(39.5993186657284,-38.60062759641,-147.108536628033));
#154469=CARTESIAN_POINT('Ctrl Pts',(39.5612326590572,-38.6061320839423,
-147.008020389331));
#154470=CARTESIAN_POINT('Ctrl Pts',(39.5238071296623,-38.6119074732402,
-146.903615357461));
#154471=CARTESIAN_POINT('Ctrl Pts',(39.4874039909042,-38.6179142095375,
-146.795314311961));
#154472=CARTESIAN_POINT('Ctrl Pts',(39.4535378615888,-38.623502324056,-146.694560988565));
#154473=CARTESIAN_POINT('Ctrl Pts',(39.4205571104765,-38.6292905412101,
-146.590435817828));
#154474=CARTESIAN_POINT('Ctrl Pts',(39.3887661995631,-38.635216720523,-146.48295663282));
#154475=CARTESIAN_POINT('Ctrl Pts',(39.3719269697633,-38.638355740212,-146.426026313963));
#154476=CARTESIAN_POINT('Ctrl Pts',(39.3554217533661,-38.6415329535104,
-146.368155370693));
#154477=CARTESIAN_POINT('Ctrl Pts',(39.3392966976341,-38.6447354631592,
-146.309349381664));
#154478=CARTESIAN_POINT('Ctrl Pts',(39.3312341697681,-38.6463367179837,
-146.27994638715));
#154479=CARTESIAN_POINT('Ctrl Pts',(39.3232666707404,-38.6479442936562,
-146.250309634084));
#154480=CARTESIAN_POINT('Ctrl Pts',(39.3154000216331,-38.6495562849387,
-146.220440057212));
#154481=CARTESIAN_POINT('Ctrl Pts',(39.3114666970794,-38.65036228058,-146.205505268776));
#154482=CARTESIAN_POINT('Ctrl Pts',(39.307558584028,-38.6511693798373,-146.190512274645));
#154483=CARTESIAN_POINT('Ctrl Pts',(39.3036764077864,-38.6519773352297,
-146.175461199439));
#154484=CARTESIAN_POINT('Ctrl Pts',(39.3017353196656,-38.6523813129259,
-146.167935661836));
#154485=CARTESIAN_POINT('Ctrl Pts',(39.2998007156842,-38.6527855046386,
-146.16039560398));
#154486=CARTESIAN_POINT('Ctrl Pts',(39.2978726865716,-38.6531898783562,
-146.152841042329));
#154487=CARTESIAN_POINT('Ctrl Pts',(39.2959446574589,-38.6535942520737,
-146.145286480678));
#154488=CARTESIAN_POINT('Ctrl Pts',(39.2936380176904,-38.6540802197939,
-146.136191881702));
#154489=CARTESIAN_POINT('Ctrl Pts',(39.2921084144363,-38.654403513146,-146.130133862755));
#154490=CARTESIAN_POINT('Ctrl Pts',(39.2559675721066,-38.6620421567188,
-145.986997459891));
#154491=CARTESIAN_POINT('Ctrl Pts',(39.2232049408543,-38.6699359481944,
-145.843120322114));
#154492=CARTESIAN_POINT('Ctrl Pts',(39.1938520119094,-38.6778211466036,
-145.698765413825));
#154493=CARTESIAN_POINT('Ctrl Pts',(39.1643011830174,-38.6857595076921,
-145.553437252449));
#154494=CARTESIAN_POINT('Ctrl Pts',(39.1382061063453,-38.6936886972171,
-145.407625253192));
#154495=CARTESIAN_POINT('Ctrl Pts',(39.1155464093657,-38.7013467251314,
-145.261596960813));
#154496=CARTESIAN_POINT('Ctrl Pts',(39.0997468350803,-38.706686319082,-145.15977808586));
#154497=CARTESIAN_POINT('Ctrl Pts',(39.0856163027924,-38.7118942339117,
-145.057854041734));
#154498=CARTESIAN_POINT('Ctrl Pts',(39.0731335090665,-38.7168854313741,
-144.9559137805));
#154499=CARTESIAN_POINT('Ctrl Pts',(39.0548053657282,-38.7242138695852,
-144.806237693489));
#154500=CARTESIAN_POINT('Ctrl Pts',(39.0398124881451,-38.7320390883622,
-144.655702496367));
#154501=CARTESIAN_POINT('Ctrl Pts',(39.0282916457397,-38.7400909159274,
-144.504532299893));
#154502=CARTESIAN_POINT('Ctrl Pts',(39.0168061959963,-38.7481180078351,
-144.353826506583));
#154503=CARTESIAN_POINT('Ctrl Pts',(39.0087717144706,-38.756369895014,-144.202489956612));
#154504=CARTESIAN_POINT('Ctrl Pts',(39.004275703363,-38.7645674845392,-144.050760362076));
#154505=CARTESIAN_POINT('Ctrl Pts',(39.001429135968,-38.7697576387672,-143.954695537878));
#154506=CARTESIAN_POINT('Ctrl Pts',(39.0000000038998,-38.7749258178196,
-143.858473458816));
#154507=CARTESIAN_POINT('Ctrl Pts',(39.,-38.78000002,-143.762156710948));
#154508=CARTESIAN_POINT('',(39.,-44.4300000199906,-150.364854264666));
#154509=CARTESIAN_POINT('Ctrl Pts',(39.0000000003644,-44.4300000199906,
-150.364854264666));
#154510=CARTESIAN_POINT('Ctrl Pts',(39.0000000001644,-43.9457023551939,
-149.760761216984));
#154511=CARTESIAN_POINT('Ctrl Pts',(39.000000000108,-43.4567859620687,-149.160174741698));
#154512=CARTESIAN_POINT('Ctrl Pts',(39.0000000000721,-42.9627229131801,
-148.563361289672));
#154513=CARTESIAN_POINT('Ctrl Pts',(39.0000000000298,-42.3819947837034,
-147.861859000803));
#154514=CARTESIAN_POINT('Ctrl Pts',(39.0000000000251,-41.7951037310901,
-147.166651435241));
#154515=CARTESIAN_POINT('Ctrl Pts',(39.000000000019,-41.2007410723715,-146.478263131248));
#154516=CARTESIAN_POINT('Ctrl Pts',(39.0000000000133,-40.6489795609409,
-145.839215294898));
#154517=CARTESIAN_POINT('Ctrl Pts',(39.0000000000093,-40.0907793123645,
-145.206044014069));
#154518=CARTESIAN_POINT('Ctrl Pts',(39.0000000000044,-39.5250612455183,
-144.579200831346));
#154519=CARTESIAN_POINT('Ctrl Pts',(39.0000000000023,-39.2781704674834,
-144.30563381951));
#154520=CARTESIAN_POINT('Ctrl Pts',(39.0000000000002,-39.0298473782612,
-144.033272518869));
#154521=CARTESIAN_POINT('Ctrl Pts',(39.,-38.7800000199999,-143.762156710948));
#154522=CARTESIAN_POINT('Ctrl Pts',(39.0000000003644,-44.4300000199906,
-150.364854264666));
#154523=CARTESIAN_POINT('Ctrl Pts',(39.0000007052026,-44.4254451266292,
-150.452504858533));
#154524=CARTESIAN_POINT('Ctrl Pts',(39.0010202384484,-44.4206877726529,
-150.544931342509));
#154525=CARTESIAN_POINT('Ctrl Pts',(39.0034067297545,-44.4156797092475,
-150.642139337907));
#154526=CARTESIAN_POINT('Ctrl Pts',(39.0057191759491,-44.4108270298623,
-150.736331283407));
#154527=CARTESIAN_POINT('Ctrl Pts',(39.0093152859151,-44.4057385176752,
-150.835012944067));
#154528=CARTESIAN_POINT('Ctrl Pts',(39.0145518042182,-44.4003915136932,
-150.938169957597));
#154529=CARTESIAN_POINT('Ctrl Pts',(39.0154416112397,-44.3994829325689,
-150.955698748607));
#154530=CARTESIAN_POINT('Ctrl Pts',(39.0163788749113,-44.3985669479675,
-150.973356707516));
#154531=CARTESIAN_POINT('Ctrl Pts',(39.0173654574034,-44.397643526823,-150.991143695347));
#154532=CARTESIAN_POINT('Ctrl Pts',(39.0229730021521,-44.3923949790017,
-151.092241506225));
#154533=CARTESIAN_POINT('Ctrl Pts',(39.0301712126243,-44.386903742455,-151.197509750464));
#154534=CARTESIAN_POINT('Ctrl Pts',(39.0393212707034,-44.3811807618817,
-151.306908428555));
#154535=CARTESIAN_POINT('Ctrl Pts',(39.0406017698706,-44.3803798629372,
-151.322218158282));
#154536=CARTESIAN_POINT('Ctrl Pts',(39.0419205457929,-44.379574476212,-151.337608737534));
#154537=CARTESIAN_POINT('Ctrl Pts',(39.0432786373157,-44.3787646832776,
-151.353080013601));
#154538=CARTESIAN_POINT('Ctrl Pts',(39.0488099378183,-44.3754665196488,
-151.416092171215));
#154539=CARTESIAN_POINT('Ctrl Pts',(39.0549931721796,-44.3720949468472,
-151.480443195579));
#154540=CARTESIAN_POINT('Ctrl Pts',(39.0619004408812,-44.3686579749138,
-151.54612071821));
#154541=CARTESIAN_POINT('Ctrl Pts',(39.0653540752321,-44.3669394889471,
-151.578959479526));
#154542=CARTESIAN_POINT('Ctrl Pts',(39.0689887775362,-44.3652046607912,
-151.612129859391));
#154543=CARTESIAN_POINT('Ctrl Pts',(39.0728138179726,-44.363454962206,-151.645629929068));
#154544=CARTESIAN_POINT('Ctrl Pts',(39.0747263381908,-44.3625801129134,
-151.662379963907));
#154545=CARTESIAN_POINT('Ctrl Pts',(39.0766864464293,-44.3617015464156,
-151.679212420879));
#154546=CARTESIAN_POINT('Ctrl Pts',(39.0786953190885,-44.3608194643872,
-151.696127044875));
#154547=CARTESIAN_POINT('Ctrl Pts',(39.0796997554181,-44.3603784233729,
-151.704584356872));
#154548=CARTESIAN_POINT('Ctrl Pts',(39.080716383072,-44.3599365035074,-151.713062210601));
#154549=CARTESIAN_POINT('Ctrl Pts',(39.0817453500286,-44.3594937318188,
-151.721560572708));
#154550=CARTESIAN_POINT('Ctrl Pts',(39.0827743169852,-44.3590509601302,
-151.730058934815));
#154551=CARTESIAN_POINT('Ctrl Pts',(39.0839942168393,-44.3585320129597,
-151.740025025291));
#154552=CARTESIAN_POINT('Ctrl Pts',(39.0848694175268,-44.3581628889547,
-151.747117150299));
#154553=CARTESIAN_POINT('Ctrl Pts',(39.105124915675,-44.3496199447983,-151.911256103819));
#154554=CARTESIAN_POINT('Ctrl Pts',(39.1291136383777,-44.3407950403259,
-152.075349215586));
#154555=CARTESIAN_POINT('Ctrl Pts',(39.1568906940477,-44.3319910570048,
-152.239164594126));
#154556=CARTESIAN_POINT('Ctrl Pts',(39.1675198003644,-44.3286221443367,
-152.301849822377));
#154557=CARTESIAN_POINT('Ctrl Pts',(39.1787031089135,-44.3252564505626,
-152.364494303024));
#154558=CARTESIAN_POINT('Ctrl Pts',(39.190441757935,-44.321911449593,-152.427084805163));
#154559=CARTESIAN_POINT('Ctrl Pts',(39.211649394889,-44.3158682016823,-152.540163971575));
#154560=CARTESIAN_POINT('Ctrl Pts',(39.2346703636018,-44.3098924130758,
-152.653066963499));
#154561=CARTESIAN_POINT('Ctrl Pts',(39.2595020395869,-44.3040887056269,
-152.765715249301));
#154562=CARTESIAN_POINT('Ctrl Pts',(39.2719178775795,-44.3011868519025,
-152.822039392202));
#154563=CARTESIAN_POINT('Ctrl Pts',(39.2847862305988,-44.2983279746361,
-152.878299892895));
#154564=CARTESIAN_POINT('Ctrl Pts',(39.298105589975,-44.2955253459415,-152.934486886189));
#154565=CARTESIAN_POINT('Ctrl Pts',(39.3047652696632,-44.2941240315943,
-152.962580382836));
#154566=CARTESIAN_POINT('Ctrl Pts',(39.311537690051,-44.2927367766557,-152.990655504777));
#154567=CARTESIAN_POINT('Ctrl Pts',(39.3184225947996,-44.2913652303238,
-153.018711029337));
#154568=CARTESIAN_POINT('Ctrl Pts',(39.3218650471739,-44.2906794571578,
-153.032738791617));
#154569=CARTESIAN_POINT('Ctrl Pts',(39.3253356199727,-44.2899976109454,
-153.046761654706));
#154570=CARTESIAN_POINT('Ctrl Pts',(39.3288342765372,-44.2893198980638,
-153.060779465937));
#154571=CARTESIAN_POINT('Ctrl Pts',(39.3305836048194,-44.2889810416229,
-153.067788371552));
#154572=CARTESIAN_POINT('Ctrl Pts',(39.3323399540012,-44.2886432185021,
-153.074796014213));
#154573=CARTESIAN_POINT('Ctrl Pts',(39.3341033192103,-44.2883064545096,
-153.081802374849));
#154574=CARTESIAN_POINT('Ctrl Pts',(39.3358666844194,-44.2879696905171,
-153.088808735485));
#154575=CARTESIAN_POINT('Ctrl Pts',(39.337254200393,-44.2877060656016,-153.094305141372));
#154576=CARTESIAN_POINT('Ctrl Pts',(39.3394144578684,-44.2872993656993,
-153.102817591642));
#154577=CARTESIAN_POINT('Ctrl Pts',(39.3748573788217,-44.2806267201212,
-153.242479694645));
#154578=CARTESIAN_POINT('Ctrl Pts',(39.412489111862,-44.2738186133137,-153.378383004324));
#154579=CARTESIAN_POINT('Ctrl Pts',(39.4519769629075,-44.2670316716111,
-153.510443256863));
#154580=CARTESIAN_POINT('Ctrl Pts',(39.4918829156408,-44.260172869027,-153.643901777807));
#154581=CARTESIAN_POINT('Ctrl Pts',(39.5336838923085,-44.2533356595528,
-153.773435489427));
#154582=CARTESIAN_POINT('Ctrl Pts',(39.5770317524979,-44.2466382972547,
-153.898989281955));
#154583=CARTESIAN_POINT('Ctrl Pts',(39.6212491945741,-44.2398065821899,
-154.027061752529));
#154584=CARTESIAN_POINT('Ctrl Pts',(39.6670756075795,-44.2331203235828,
-154.150993109346));
#154585=CARTESIAN_POINT('Ctrl Pts',(39.7141457934817,-44.2266606244434,
-154.270756794082));
#154586=CARTESIAN_POINT('Ctrl Pts',(39.7533855876433,-44.2212755328039,
-154.370597112257));
#154587=CARTESIAN_POINT('Ctrl Pts',(39.7934897051191,-44.216047010482,-154.46754169698));
#154588=CARTESIAN_POINT('Ctrl Pts',(39.8342530369782,-44.2110000715016,
-154.561590642464));
#154589=CARTESIAN_POINT('Ctrl Pts',(39.8848733950829,-44.2047327266387,
-154.678381667206));
#154590=CARTESIAN_POINT('Ctrl Pts',(39.9365093609633,-44.198746358527,-154.790706718198));
#154591=CARTESIAN_POINT('Ctrl Pts',(39.9887873165752,-44.1930504805605,
-154.898592431591));
#154592=CARTESIAN_POINT('Ctrl Pts',(40.0418796117349,-44.1872658772674,
-155.008158692779));
#154593=CARTESIAN_POINT('Ctrl Pts',(40.0956336285611,-44.1817805384754,
-155.113146519742));
#154594=CARTESIAN_POINT('Ctrl Pts',(40.1496863776524,-44.1765656542448,
-155.213609846438));
#154595=CARTESIAN_POINT('Ctrl Pts',(40.2051589771905,-44.1712137861266,
-155.31671213048));
#154596=CARTESIAN_POINT('Ctrl Pts',(40.2609458166902,-44.1661464111464,
-155.41504938527));
#154597=CARTESIAN_POINT('Ctrl Pts',(40.3166905863262,-44.161297194854,-155.508702734244));
#154598=CARTESIAN_POINT('Ctrl Pts',(40.3486445042757,-44.1585175356943,
-155.562386540784));
#154599=CARTESIAN_POINT('Ctrl Pts',(40.3805852951185,-44.1558089457943,
-155.61453170595));
#154600=CARTESIAN_POINT('Ctrl Pts',(40.4124516185963,-44.1531546492747,
-155.665156176616));
#154601=CARTESIAN_POINT('Origin',(39.,46.91999998,-129.34995));
#154602=CARTESIAN_POINT('',(39.,-38.78000002,-88.296486260558));
#154603=CARTESIAN_POINT('',(39.,-38.78000002,-129.34995));
#154604=CARTESIAN_POINT('',(39.,-44.43000002,-81.6937887068282));
#154605=CARTESIAN_POINT('Ctrl Pts',(39.,-38.7800000199999,-88.296486260558));
#154606=CARTESIAN_POINT('Ctrl Pts',(39.0000000000004,-39.3488675990358,
-87.6791933887682));
#154607=CARTESIAN_POINT('Ctrl Pts',(39.0000000000079,-39.9098343204423,
-87.055447933963));
#154608=CARTESIAN_POINT('Ctrl Pts',(39.0000000000125,-40.4639767641308,
-86.4257067262392));
#154609=CARTESIAN_POINT('Ctrl Pts',(39.0000000000174,-41.0582242765816,
-85.7503891243484));
#154610=CARTESIAN_POINT('Ctrl Pts',(39.0000000000199,-41.6446237826245,
-85.0681763071684));
#154611=CARTESIAN_POINT('Ctrl Pts',(39.0000000000371,-42.2244596705921,
-84.3795886419069));
#154612=CARTESIAN_POINT('Ctrl Pts',(39.0000000000444,-42.4717173644025,
-84.0859562510322));
#154613=CARTESIAN_POINT('Ctrl Pts',(39.0000000000547,-42.7177810382159,
-83.7911641691294));
#154614=CARTESIAN_POINT('Ctrl Pts',(39.0000000000728,-42.9627483114232,
-83.4952507849665));
#154615=CARTESIAN_POINT('Ctrl Pts',(39.0000000001092,-43.4568057616665,
-82.8984436680065));
#154616=CARTESIAN_POINT('Ctrl Pts',(39.0000000001663,-43.9457116736055,
-82.2978701296066));
#154617=CARTESIAN_POINT('Ctrl Pts',(39.0000000003688,-44.43000002,-81.6937887068282));
#154618=CARTESIAN_POINT('',(39.,-44.43000002,-129.34995));
#154619=CARTESIAN_POINT('Ctrl Pts',(40.4142759779013,-44.1970573566106,
-76.3328465915894));
#154620=CARTESIAN_POINT('Ctrl Pts',(39.,-45.3542557512738,-77.2153536750926));
#154621=CARTESIAN_POINT('Ctrl Pts',(39.,-46.9678746292626,-78.4459379002929));
#154622=CARTESIAN_POINT('Ctrl Pts',(40.3630303964688,-42.9636869888089,
-78.0370779308685));
#154623=CARTESIAN_POINT('Ctrl Pts',(39.,-44.1065399853887,-78.9218422882493));
#154624=CARTESIAN_POINT('Ctrl Pts',(39.,-45.6681795295713,-80.1501792727118));
#154625=CARTESIAN_POINT('Ctrl Pts',(40.3100980841279,-41.7032148714377,
-79.7240190083239));
#154626=CARTESIAN_POINT('Ctrl Pts',(39.0000000000075,-42.8253754175223,
-80.6161315734671));
#154627=CARTESIAN_POINT('Ctrl Pts',(39.,-44.3354733849924,-81.8371103170565));
#154628=CARTESIAN_POINT('Ctrl Pts',(40.2013644254228,-39.117307479239,-83.0403343570498));
#154629=CARTESIAN_POINT('Ctrl Pts',(38.9999999999925,-40.1892936959721,
-83.9475037984034));
#154630=CARTESIAN_POINT('Ctrl Pts',(39.,-41.5900648068412,-85.1534256657242));
#154631=CARTESIAN_POINT('Ctrl Pts',(40.1457604305377,-37.7969103286269,
-84.6635709993291));
#154632=CARTESIAN_POINT('Ctrl Pts',(39.0000000000224,-38.8402604870948,
-85.5784283533127));
#154633=CARTESIAN_POINT('Ctrl Pts',(39.,-40.1827113458493,-86.7766805524391));
#154634=CARTESIAN_POINT('Ctrl Pts',(40.0893978453286,-36.4387324215761,
-86.2394739826303));
#154635=CARTESIAN_POINT('Ctrl Pts',(38.9999999999999,-37.4435485041586,
-87.1668478324999));
#154636=CARTESIAN_POINT('Ctrl Pts',(39.,-38.7282817023213,-88.3525652913338));
#154637=CARTESIAN_POINT('',(40.1769830712292,-38.5367008846094,-83.7339572460004));
#154638=CARTESIAN_POINT('Ctrl Pts',(39.,-38.78000002,-88.296486260558));
#154639=CARTESIAN_POINT('Ctrl Pts',(39.,-38.7751322708569,-88.2040883348799));
#154640=CARTESIAN_POINT('Ctrl Pts',(39.0012719050489,-38.770015943568,-88.1070513397817));
#154641=CARTESIAN_POINT('Ctrl Pts',(39.0042443556417,-38.7646505825313,
-88.0053892224477));
#154642=CARTESIAN_POINT('Ctrl Pts',(39.006951468088,-38.7597641646792,-87.9128020541979));
#154643=CARTESIAN_POINT('Ctrl Pts',(39.0110696448286,-38.7546711367464,
-87.8163776816512));
#154644=CARTESIAN_POINT('Ctrl Pts',(39.0169597134217,-38.7493716191513,
-87.7161359772685));
#154645=CARTESIAN_POINT('Ctrl Pts',(39.0225041669748,-38.7443830644857,
-87.621776214686));
#154646=CARTESIAN_POINT('Ctrl Pts',(39.0296189198416,-38.7392117734668,
-87.5240383765513));
#154647=CARTESIAN_POINT('Ctrl Pts',(39.0386310058382,-38.7338594124382,
-87.4229686929037));
#154648=CARTESIAN_POINT('Ctrl Pts',(39.0431370488365,-38.731183231924,-87.3724338510799));
#154649=CARTESIAN_POINT('Ctrl Pts',(39.0481177945266,-38.7284618151407,
-87.3210666362513));
#154650=CARTESIAN_POINT('Ctrl Pts',(39.0536162553258,-38.7256955139037,
-87.2688755073787));
#154651=CARTESIAN_POINT('Ctrl Pts',(39.0563654857254,-38.7243123632852,
-87.2427799429424));
#154652=CARTESIAN_POINT('Ctrl Pts',(39.0592441664584,-38.7229179928732,
-87.2164784244485));
#154653=CARTESIAN_POINT('Ctrl Pts',(39.0622577885059,-38.7215124585059,
-87.1899722295901));
#154654=CARTESIAN_POINT('Ctrl Pts',(39.0630111940177,-38.721161074914,-87.1833456808756));
#154655=CARTESIAN_POINT('Ctrl Pts',(39.0637730337606,-38.7208089935898,
-87.1767063401531));
#154656=CARTESIAN_POINT('Ctrl Pts',(39.0645433942633,-38.7204562154624,
-87.1700542284318));
#154657=CARTESIAN_POINT('Ctrl Pts',(39.0651211646403,-38.7201916318669,
-87.1650651446408));
#154658=CARTESIAN_POINT('Ctrl Pts',(39.0657037279515,-38.7199266563198,
-87.1600688771641));
#154659=CARTESIAN_POINT('Ctrl Pts',(39.0662911208221,-38.7196612892144,
-87.1550654348854));
#154660=CARTESIAN_POINT('Ctrl Pts',(39.0664133853009,-38.71960605366,-87.1540239798509));
#154661=CARTESIAN_POINT('Ctrl Pts',(39.0665355793354,-38.7195509271128,
-87.1529845890894));
#154662=CARTESIAN_POINT('Ctrl Pts',(39.0666586113654,-38.7194955005559,
-87.1519395508262));
#154663=CARTESIAN_POINT('Ctrl Pts',(39.0680442608999,-38.718871258374,-87.1401697963779));
#154664=CARTESIAN_POINT('Ctrl Pts',(39.0696269835109,-38.7181701779564,
-87.1269526878292));
#154665=CARTESIAN_POINT('Ctrl Pts',(39.07096982888,-38.7175841665058,-87.1159059528804));
#154666=CARTESIAN_POINT('Ctrl Pts',(39.071226215998,-38.7174722803643,-87.1137968190948));
#154667=CARTESIAN_POINT('Ctrl Pts',(39.0714737027787,-38.7173645880403,
-87.1117667787753));
#154668=CARTESIAN_POINT('Ctrl Pts',(39.0717090468188,-38.7172624241003,
-87.1098409798219));
#154669=CARTESIAN_POINT('Ctrl Pts',(39.0875044445527,-38.7104055686412,
-86.9805886715101));
#154670=CARTESIAN_POINT('Ctrl Pts',(39.1060041069199,-38.7033702850715,
-86.8512458769073));
#154671=CARTESIAN_POINT('Ctrl Pts',(39.1272339734381,-38.6963344387826,
-86.7219659415845));
#154672=CARTESIAN_POINT('Ctrl Pts',(39.1378819023615,-38.6928055804575,
-86.6571250457942));
#154673=CARTESIAN_POINT('Ctrl Pts',(39.1492158695168,-38.6892762956135,
-86.592299827051));
#154674=CARTESIAN_POINT('Ctrl Pts',(39.1612346902753,-38.6857671564475,
-86.5275086253275));
#154675=CARTESIAN_POINT('Ctrl Pts',(39.170230183961,-38.6831407391106,-86.4790156111036));
#154676=CARTESIAN_POINT('Ctrl Pts',(39.1796091474621,-38.6805260462456,
-86.4305417811094));
#154677=CARTESIAN_POINT('Ctrl Pts',(39.1893697299427,-38.6779321756499,
-86.3820948719549));
#154678=CARTESIAN_POINT('Ctrl Pts',(39.1991303124233,-38.6753383050542,
-86.3336479628005));
#154679=CARTESIAN_POINT('Ctrl Pts',(39.2092725094359,-38.672765261147,-86.2852279785019));
#154680=CARTESIAN_POINT('Ctrl Pts',(39.2197935457867,-38.6702217598244,
-86.2368423218951));
#154681=CARTESIAN_POINT('Ctrl Pts',(39.2303145821375,-38.6676782585017,
-86.1884566652882));
#154682=CARTESIAN_POINT('Ctrl Pts',(39.2412144573617,-38.6651642995807,
-86.1401053366775));
#154683=CARTESIAN_POINT('Ctrl Pts',(39.2524893947787,-38.6626885282162,
-86.0917955706138));
#154684=CARTESIAN_POINT('Ctrl Pts',(39.2581268634872,-38.6614506425339,
-86.067640687582));
#154685=CARTESIAN_POINT('Ctrl Pts',(39.2638580840871,-38.6602222971366,
-86.0434961893031));
#154686=CARTESIAN_POINT('Ctrl Pts',(39.2696825029684,-38.6590045387141,
-86.0193629463918));
#154687=CARTESIAN_POINT('Ctrl Pts',(39.272594712409,-38.6583956595029,-86.0072963249361));
#154688=CARTESIAN_POINT('Ctrl Pts',(39.2755302206201,-38.6577894266009,
-85.9952325169264));
#154689=CARTESIAN_POINT('Ctrl Pts',(39.2784889532421,-38.6571859693317,
-85.983171629405));
#154690=CARTESIAN_POINT('Ctrl Pts',(39.2799683195532,-38.6568842406971,
-85.9771411856443));
#154691=CARTESIAN_POINT('Ctrl Pts',(39.2814534919182,-38.6565832059434,
-85.9711114719805));
#154692=CARTESIAN_POINT('Ctrl Pts',(39.2829444607249,-38.6562828811408,
-85.9650825016789));
#154693=CARTESIAN_POINT('Ctrl Pts',(39.2842286592038,-38.6560242059406,
-85.959889640195));
#154694=CARTESIAN_POINT('Ctrl Pts',(39.2852757225972,-38.6558141697005,
-85.9556680182126));
#154695=CARTESIAN_POINT('Ctrl Pts',(39.2867135640682,-38.6555118292067,
-85.9499104143363));
#154696=CARTESIAN_POINT('Ctrl Pts',(39.2869450726374,-38.6554631490033,
-85.9489833756727));
#154697=CARTESIAN_POINT('Ctrl Pts',(39.2871867538787,-38.6554120757498,
-85.9480165163723));
#154698=CARTESIAN_POINT('Ctrl Pts',(39.2874412782136,-38.6553580214243,
-85.9469993764742));
#154699=CARTESIAN_POINT('Ctrl Pts',(39.3168062531781,-38.6491216671837,
-85.8296499385384));
#154700=CARTESIAN_POINT('Ctrl Pts',(39.347813897775,-38.6430183085598,-85.7153946198998));
#154701=CARTESIAN_POINT('Ctrl Pts',(39.3802038090334,-38.6370773642453,
-85.6042576441525));
#154702=CARTESIAN_POINT('Ctrl Pts',(39.4044962424771,-38.6326216560094,
-85.5209049123421));
#154703=CARTESIAN_POINT('Ctrl Pts',(39.4295662524833,-38.6282571384398,
-85.4393063176715));
#154704=CARTESIAN_POINT('Ctrl Pts',(39.4553071010921,-38.6239848770771,
-85.3594741229853));
#154705=CARTESIAN_POINT('Ctrl Pts',(39.4939183740053,-38.6175764850329,
-85.239725830956));
#154706=CARTESIAN_POINT('Ctrl Pts',(39.5340443755693,-38.6113746546872,
-85.1239378544272));
#154707=CARTESIAN_POINT('Ctrl Pts',(39.5753182817589,-38.6053655234179,
-85.0121853429442));
#154708=CARTESIAN_POINT('Ctrl Pts',(39.6165921879486,-38.5993563921486,
-84.9004328314613));
#154709=CARTESIAN_POINT('Ctrl Pts',(39.659013902461,-38.5935399471999,-84.7927151573769));
#154710=CARTESIAN_POINT('Ctrl Pts',(39.7022266257688,-38.587902347965,-84.6890544727167));
#154711=CARTESIAN_POINT('Ctrl Pts',(39.7486087077317,-38.5818512692602,
-84.5777909835356));
#154712=CARTESIAN_POINT('Ctrl Pts',(39.7958609030512,-38.576108580013,-84.4711866585353));
#154713=CARTESIAN_POINT('Ctrl Pts',(39.8435692192616,-38.5706418472248,
-84.3691732753572));
#154714=CARTESIAN_POINT('Ctrl Pts',(39.8748801633873,-38.5670540332235,
-84.3022219428749));
#154715=CARTESIAN_POINT('Ctrl Pts',(39.9063880806255,-38.5635851184899,
-84.2372469507177));
#154716=CARTESIAN_POINT('Ctrl Pts',(39.937981857019,-38.5602263972235,-84.1742185506446));
#154717=CARTESIAN_POINT('Ctrl Pts',(39.9905251860152,-38.5546405377075,
-84.0693965781175));
#154718=CARTESIAN_POINT('Ctrl Pts',(40.043308659147,-38.5493483797232,-83.9699663358905));
#154719=CARTESIAN_POINT('Ctrl Pts',(40.0958052372803,-38.5443134355034,
-83.8758305147684));
#154720=CARTESIAN_POINT('Ctrl Pts',(40.122964392795,-38.5417086022374,-83.8271292565859));
#154721=CARTESIAN_POINT('Ctrl Pts',(40.1500471338584,-38.5391726650493,
-83.7798442200289));
#154722=CARTESIAN_POINT('Ctrl Pts',(40.1769830712292,-38.5367008846094,
-83.7339572460004));
#154723=CARTESIAN_POINT('',(40.4124515952943,-44.1531546081811,-76.3934867324882));
#154724=CARTESIAN_POINT('Ctrl Pts',(40.4124516186295,-44.153154649867,-76.3934867953418));
#154725=CARTESIAN_POINT('Ctrl Pts',(40.3952460398817,-43.7391604247703,
-76.9650940777494));
#154726=CARTESIAN_POINT('Ctrl Pts',(40.3780870787012,-43.3277837645271,
-77.5268985486059));
#154727=CARTESIAN_POINT('Ctrl Pts',(40.3609885419993,-42.9188402155611,
-78.0789845047923));
#154728=CARTESIAN_POINT('Ctrl Pts',(40.3428805261513,-42.4857530809918,
-78.6636650197566));
#154729=CARTESIAN_POINT('Ctrl Pts',(40.3248402889955,-42.055395000472,-79.2374457299862));
#154730=CARTESIAN_POINT('Ctrl Pts',(40.3068810516774,-41.6275578066968,
-79.8004867094309));
#154731=CARTESIAN_POINT('Ctrl Pts',(40.2897545069958,-41.2195575845354,
-80.3374218988947));
#154732=CARTESIAN_POINT('Ctrl Pts',(40.2727015872578,-40.8138501719484,
-80.8645911001279));
#154733=CARTESIAN_POINT('Ctrl Pts',(40.2557312547753,-40.4102611753384,
-81.3821766826868));
#154734=CARTESIAN_POINT('Ctrl Pts',(40.2374822795637,-39.97626345594,-81.9387601483187));
#154735=CARTESIAN_POINT('Ctrl Pts',(40.2193511533291,-39.5452803790655,
-82.4835699879066));
#154736=CARTESIAN_POINT('Ctrl Pts',(40.2013522628222,-39.1168809520225,
-83.0169014070057));
#154737=CARTESIAN_POINT('Ctrl Pts',(40.193206439655,-38.9229986693181,-83.258273141993));
#154738=CARTESIAN_POINT('Ctrl Pts',(40.1850876474775,-38.7296460713902,
-83.4972944027484));
#154739=CARTESIAN_POINT('Ctrl Pts',(40.1769969653824,-38.5367854415877,
-83.7339951195581));
#154740=CARTESIAN_POINT('Ctrl Pts',(40.4124516068581,-44.1531545451511,
-76.3934867430719));
#154741=CARTESIAN_POINT('Ctrl Pts',(40.3510699177843,-44.158267238669,-76.4910005227811));
#154742=CARTESIAN_POINT('Ctrl Pts',(40.2897374695193,-44.1636365976902,
-76.5934241275335));
#154743=CARTESIAN_POINT('Ctrl Pts',(40.2289388806379,-44.1692681835667,
-76.7008689731916));
#154744=CARTESIAN_POINT('Ctrl Pts',(40.1815905139172,-44.1736539168247,
-76.784544236846));
#154745=CARTESIAN_POINT('Ctrl Pts',(40.1345654049276,-44.178198675974,-76.8712646231758));
#154746=CARTESIAN_POINT('Ctrl Pts',(40.0880717165451,-44.1829046417643,
-76.9610747878389));
#154747=CARTESIAN_POINT('Ctrl Pts',(40.0366336021373,-44.1881110690267,
-77.0604359201913));
#154748=CARTESIAN_POINT('Ctrl Pts',(39.9858518633865,-44.1935143925675,
-77.1635711601288));
#154749=CARTESIAN_POINT('Ctrl Pts',(39.9359915641101,-44.199114610184,-77.2704856845705));
#154750=CARTESIAN_POINT('Ctrl Pts',(39.8861312648337,-44.2047148278006,
-77.3774002090122));
#154751=CARTESIAN_POINT('Ctrl Pts',(39.837193200328,-44.2105119454377,-77.4880941304441));
#154752=CARTESIAN_POINT('Ctrl Pts',(39.7893996906518,-44.2165040019749,
-77.6025360228382));
#154753=CARTESIAN_POINT('Ctrl Pts',(39.7863162384146,-44.2168905862676,
-77.6099193707346));
#154754=CARTESIAN_POINT('Ctrl Pts',(39.7824541929345,-44.2173769096022,
-77.6192077850968));
#154755=CARTESIAN_POINT('Ctrl Pts',(39.7801635931124,-44.2176662577561,
-77.6247328089195));
#154756=CARTESIAN_POINT('Ctrl Pts',(39.7787661541334,-44.2178427819944,
-77.6281034909458));
#154757=CARTESIAN_POINT('Ctrl Pts',(39.777367957483,-44.2180196929799,-77.6314816136799));
#154758=CARTESIAN_POINT('Ctrl Pts',(39.775969023752,-44.2181969908901,-77.6348671799205));
#154759=CARTESIAN_POINT('Ctrl Pts',(39.7180520552975,-44.225537265303,-77.7750323134183));
#154760=CARTESIAN_POINT('Ctrl Pts',(39.6589014044892,-44.2335417463499,
-77.9279743185955));
#154761=CARTESIAN_POINT('Ctrl Pts',(39.6002641254276,-44.2422288610516,
-78.0940075633862));
#154762=CARTESIAN_POINT('Ctrl Pts',(39.5860275451542,-44.2443380108582,
-78.1343188748137));
#154763=CARTESIAN_POINT('Ctrl Pts',(39.5718214669483,-44.2464874033966,
-78.1754019794697));
#154764=CARTESIAN_POINT('Ctrl Pts',(39.5576712214515,-44.2486773058874,
-78.2172615215681));
#154765=CARTESIAN_POINT('Ctrl Pts',(39.5182563748059,-44.2547771767953,
-78.3338593171923));
#154766=CARTESIAN_POINT('Ctrl Pts',(39.4792798091834,-44.2611901671226,
-78.4564714249827));
#154767=CARTESIAN_POINT('Ctrl Pts',(39.4413055250383,-44.2679169956396,
-78.5851235840438));
#154768=CARTESIAN_POINT('Ctrl Pts',(39.4103620351911,-44.273398377438,-78.6899562851032));
#154769=CARTESIAN_POINT('Ctrl Pts',(39.3800846623711,-44.2790880796353,
-78.7987983155533));
#154770=CARTESIAN_POINT('Ctrl Pts',(39.3507730694842,-44.2849849651986,
-78.9116354894448));
#154771=CARTESIAN_POINT('Ctrl Pts',(39.3486671601221,-44.2854086305573,
-78.9197423453843));
#154772=CARTESIAN_POINT('Ctrl Pts',(39.3462781123095,-44.2858919006434,
-78.9289899433011));
#154773=CARTESIAN_POINT('Ctrl Pts',(39.344470382315,-44.2862592024284,-78.9360178765697));
#154774=CARTESIAN_POINT('Ctrl Pts',(39.3433176190757,-44.2864934254578,
-78.9404994878422));
#154775=CARTESIAN_POINT('Ctrl Pts',(39.3421676157945,-44.2867279189475,
-78.9449823374088));
#154776=CARTESIAN_POINT('Ctrl Pts',(39.3410203725809,-44.2869626764882,
-78.9494664233533));
#154777=CARTESIAN_POINT('Ctrl Pts',(39.3046430590299,-44.2944064761663,
-79.0916498753526));
#154778=CARTESIAN_POINT('Ctrl Pts',(39.2711308927383,-44.3020903706652,
-79.2345947225894));
#154779=CARTESIAN_POINT('Ctrl Pts',(39.240557058843,-44.3098085083895,-79.3781902552231));
#154780=CARTESIAN_POINT('Ctrl Pts',(39.2237092792686,-44.3140616054511,
-79.4573188947637));
#154781=CARTESIAN_POINT('Ctrl Pts',(39.2077529091826,-44.3183251085781,
-79.5366446976344));
#154782=CARTESIAN_POINT('Ctrl Pts',(39.1926939224873,-44.3225650371283,
-79.6161466581915));
#154783=CARTESIAN_POINT('Ctrl Pts',(39.1818817918178,-44.3256092433848,
-79.673227895025));
#154784=CARTESIAN_POINT('Ctrl Pts',(39.1715328096908,-44.3286406374731,
-79.73039721567));
#154785=CARTESIAN_POINT('Ctrl Pts',(39.1616480262631,-44.3316460088623,
-79.7876447784984));
#154786=CARTESIAN_POINT('Ctrl Pts',(39.1517632428354,-44.3346513802515,
-79.8448923413267));
#154787=CARTESIAN_POINT('Ctrl Pts',(39.1423426585283,-44.3376307202623,
-79.9022181402485));
#154788=CARTESIAN_POINT('Ctrl Pts',(39.1333861528049,-44.3405704642751,
-79.9596120521454));
#154789=CARTESIAN_POINT('Ctrl Pts',(39.1230624498265,-44.3439589558317,
-80.0257670591857));
#154790=CARTESIAN_POINT('Ctrl Pts',(39.1132917639146,-44.3473158048929,
-80.0924491279359));
#154791=CARTESIAN_POINT('Ctrl Pts',(39.1041771551082,-44.35064350333,-80.158887585486));
#154792=CARTESIAN_POINT('Ctrl Pts',(39.0974766932732,-44.3530898086899,
-80.2077287764401));
#154793=CARTESIAN_POINT('Ctrl Pts',(39.0911296815406,-44.3555203400116,
-80.2564381655058));
#154794=CARTESIAN_POINT('Ctrl Pts',(39.0851592100358,-44.3579356581365,
-80.3047076554924));
#154795=CARTESIAN_POINT('Ctrl Pts',(39.0710671323645,-44.3636365228988,
-80.4186379207139));
#154796=CARTESIAN_POINT('Ctrl Pts',(39.0586668014923,-44.3696038383643,
-80.5331343405056));
#154797=CARTESIAN_POINT('Ctrl Pts',(39.0480243009804,-44.3755933655321,
-80.6481162160745));
#154798=CARTESIAN_POINT('Ctrl Pts',(39.0400424255965,-44.3800855109081,
-80.7343526227512));
#154799=CARTESIAN_POINT('Ctrl Pts',(39.03304753109,-44.3845906292611,-80.8208617423929));
#154800=CARTESIAN_POINT('Ctrl Pts',(39.0270467496741,-44.3891067880273,
-80.9076077919212));
#154801=CARTESIAN_POINT('Ctrl Pts',(39.0130892771956,-44.399611113601,-81.1093741145068));
#154802=CARTESIAN_POINT('Ctrl Pts',(39.0045137146899,-44.4101748983392,
-81.3124170949888));
#154803=CARTESIAN_POINT('Ctrl Pts',(39.0013677367083,-44.4207753411466,
-81.5163151311992));
#154804=CARTESIAN_POINT('Ctrl Pts',(39.0004560331356,-44.42384734662,-81.5754047272333));
#154805=CARTESIAN_POINT('Ctrl Pts',(39.,-44.426922427187,-81.6345660607426));
#154806=CARTESIAN_POINT('Ctrl Pts',(39.,-44.43000002,-81.6937887068282));
#154807=CARTESIAN_POINT('Origin',(60.,-2.55003103885676E-14,0.));
#154808=CARTESIAN_POINT('',(60.,19.76999998,-58.24995));
#154809=CARTESIAN_POINT('',(60.,19.26999998,-58.24995));
#154810=CARTESIAN_POINT('',(60.,-54.58000002,-58.24995));
#154811=CARTESIAN_POINT('',(60.,19.26999998,-174.34995));
#154812=CARTESIAN_POINT('',(60.,19.26999998,-174.34995));
#154813=CARTESIAN_POINT('',(60.,19.76999998,-174.34995));
#154814=CARTESIAN_POINT('',(60.,28.41999998,-174.34995));
#154815=CARTESIAN_POINT('',(60.,19.76999998,-58.24995));
#154816=CARTESIAN_POINT('Origin',(57.,-2.42462934179819E-14,-174.34995));
#154817=CARTESIAN_POINT('',(57.,19.26999998,-177.34995));
#154818=CARTESIAN_POINT('Origin',(57.,19.26999998,-174.34995));
#154819=CARTESIAN_POINT('',(57.,19.76999998,-177.34995));
#154820=CARTESIAN_POINT('',(57.,-54.58000002,-177.34995));
#154821=CARTESIAN_POINT('Origin',(57.,19.76999998,-174.34995));
#154822=CARTESIAN_POINT('Origin',(60.,28.41999998,-177.34995));
#154823=CARTESIAN_POINT('',(52.1813053461851,19.26999998,-177.34995));
#154824=CARTESIAN_POINT('',(60.,19.26999998,-177.34995));
#154825=CARTESIAN_POINT('',(52.1110349288339,19.76999998,-177.34995));
#154826=CARTESIAN_POINT('',(51.0717059287548,27.1652100787588,-177.34995));
#154827=CARTESIAN_POINT('',(60.,19.76999998,-177.34995));
#154828=CARTESIAN_POINT('Origin',(0.,-12.9675000200281,-171.64995));
#154829=CARTESIAN_POINT('',(50.9867892914963,16.9914785469432,-171.64995));
#154830=CARTESIAN_POINT('',(50.8071048221096,18.26999998,-171.64995));
#154831=CARTESIAN_POINT('',(50.7563939085354,18.6308268790399,-171.64995));
#154832=CARTESIAN_POINT('',(50.2136602208993,18.26999998,-171.64995));
#154833=CARTESIAN_POINT('',(49.8991400004038,18.26999998,-171.64995));
#154834=CARTESIAN_POINT('Origin',(0.,-12.9675000200281,-171.64995));
#154835=CARTESIAN_POINT('Ctrl Pts',(39.,20.796902498477,-78.7546851990749));
#154836=CARTESIAN_POINT('Ctrl Pts',(39.,19.1920627889827,-77.5254336382597));
#154837=CARTESIAN_POINT('Ctrl Pts',(40.4049679656207,18.0381727558475,-76.6415938903714));
#154838=CARTESIAN_POINT('Ctrl Pts',(39.,19.4994983593746,-80.4485009715931));
#154839=CARTESIAN_POINT('Ctrl Pts',(39.0000000000074,17.9467422700577,-79.2215151478833));
#154840=CARTESIAN_POINT('Ctrl Pts',(40.3537711092786,16.8074933352464,-78.3353996644624));
#154841=CARTESIAN_POINT('Ctrl Pts',(39.,18.1687833493074,-82.1249487171281));
#154842=CARTESIAN_POINT('Ctrl Pts',(39.,16.6676992320686,-80.9053032515377));
#154843=CARTESIAN_POINT('Ctrl Pts',(40.3009014559381,15.5494518783308,-80.0118574083956));
#154844=CARTESIAN_POINT('Ctrl Pts',(39.,15.4269620807205,-85.4195370156013));
#154845=CARTESIAN_POINT('Ctrl Pts',(39.,14.0354926345166,-84.2148910918098));
#154846=CARTESIAN_POINT('Ctrl Pts',(40.1923542727721,12.9680880684791,-83.3064457069268));
#154847=CARTESIAN_POINT('Ctrl Pts',(39.,14.0212774653657,-87.0315007804442));
#154848=CARTESIAN_POINT('Ctrl Pts',(39.,12.6882730287539,-85.8345023651596));
#154849=CARTESIAN_POINT('Ctrl Pts',(40.136876773061,11.6498700440212,-84.9183911253513));
#154850=CARTESIAN_POINT('Ctrl Pts',(39.,12.5683346400766,-88.5955027032924));
#154851=CARTESIAN_POINT('Ctrl Pts',(39.,11.2932302045755,-87.4109428798));
#154852=CARTESIAN_POINT('Ctrl Pts',(40.0806897769273,10.2937242346666,-86.4824113945889));
#154853=CARTESIAN_POINT('',(39.,18.2699999799838,-81.9737790469184));
#154854=CARTESIAN_POINT('',(39.,12.61999998,-88.5398461374725));
#154855=CARTESIAN_POINT('Ctrl Pts',(39.000000000374,18.2699999799838,-81.9737790469184));
#154856=CARTESIAN_POINT('Ctrl Pts',(39.0000000001679,17.7841524775854,-82.5769275834792));
#154857=CARTESIAN_POINT('Ctrl Pts',(39.0000000001103,17.2936169434169,-83.1765007297742));
#154858=CARTESIAN_POINT('Ctrl Pts',(39.0000000000735,16.7978518736795,-83.7722255217958));
#154859=CARTESIAN_POINT('Ctrl Pts',(39.0000000000309,16.2234293967186,-84.462467193726));
#154860=CARTESIAN_POINT('Ctrl Pts',(39.0000000000258,15.6429390502891,-85.1464596076239));
#154861=CARTESIAN_POINT('Ctrl Pts',(39.0000000000195,15.0550950356406,-85.8236901161975));
#154862=CARTESIAN_POINT('Ctrl Pts',(39.0000000000137,14.5092314506736,-86.4525567271471));
#154863=CARTESIAN_POINT('Ctrl Pts',(39.0000000000098,13.9570271965508,-87.0755929306875));
#154864=CARTESIAN_POINT('Ctrl Pts',(39.0000000000048,13.3974208289264,-87.6923562596894));
#154865=CARTESIAN_POINT('Ctrl Pts',(39.0000000000025,13.13988412639,-87.976197193578));
#154866=CARTESIAN_POINT('Ctrl Pts',(39.0000000000002,12.8807792236012,-88.2587090915938));
#154867=CARTESIAN_POINT('Ctrl Pts',(39.,12.61999998,-88.5398461374725));
#154868=CARTESIAN_POINT('',(40.4031452851324,17.9943647515726,-76.7018642453134));
#154869=CARTESIAN_POINT('Ctrl Pts',(39.,18.269999980001,-81.9737790469175));
#154870=CARTESIAN_POINT('Ctrl Pts',(38.9999999999998,18.2654156915697,-81.8856318368241));
#154871=CARTESIAN_POINT('Ctrl Pts',(39.0009991608804,18.26061957816,-81.7926846809007));
#154872=CARTESIAN_POINT('Ctrl Pts',(39.0033630480626,18.2555755018158,-81.6949391084757));
#154873=CARTESIAN_POINT('Ctrl Pts',(39.0056805350309,18.2506304345201,-81.5991121620725));
#154874=CARTESIAN_POINT('Ctrl Pts',(39.0093096132162,18.2454470421538,-81.498673282606));
#154875=CARTESIAN_POINT('Ctrl Pts',(39.0146446230652,18.2399896740651,-81.3936309537436));
#154876=CARTESIAN_POINT('Ctrl Pts',(39.0153733661184,18.2392442173188,-81.3792825514694));
#154877=CARTESIAN_POINT('Ctrl Pts',(39.0161340182114,18.2384936461679,-81.3648482669779));
#154878=CARTESIAN_POINT('Ctrl Pts',(39.0169276600567,18.2377378675041,-81.3503281331421));
#154879=CARTESIAN_POINT('Ctrl Pts',(39.0231927688791,18.2317716554125,-81.2357043653457));
#154880=CARTESIAN_POINT('Ctrl Pts',(39.0315081702222,18.2254891630288,-81.1157344332212));
#154881=CARTESIAN_POINT('Ctrl Pts',(39.0424313701074,18.2189126895613,-80.9904826023971));
#154882=CARTESIAN_POINT('Ctrl Pts',(39.04789297005,18.2156244528275,-80.927856686985));
#154883=CARTESIAN_POINT('Ctrl Pts',(39.0540073612066,18.2122635841095,-80.863911025723));
#154884=CARTESIAN_POINT('Ctrl Pts',(39.060848407193,18.2088387139701,-80.7986584961791));
#154885=CARTESIAN_POINT('Ctrl Pts',(39.0642689301862,18.2071262789005,-80.7660322314072));
#154886=CARTESIAN_POINT('Ctrl Pts',(39.0678711648011,18.2053978544484,-80.7330792582658));
#154887=CARTESIAN_POINT('Ctrl Pts',(39.0716645132203,18.203654996908,-80.6998015756023));
#154888=CARTESIAN_POINT('Ctrl Pts',(39.0735611874298,18.2027835681379,-80.6831627342706));
#154889=CARTESIAN_POINT('Ctrl Pts',(39.0755056424577,18.201908531612,-80.6664427159685));
#154890=CARTESIAN_POINT('Ctrl Pts',(39.0774990638269,18.2010300996946,-80.6496417847185));
#154891=CARTESIAN_POINT('Ctrl Pts',(39.0784957745116,18.200590883736,-80.6412413190935));
#154892=CARTESIAN_POINT('Ctrl Pts',(39.0795047269169,18.2001508189632,-80.6328206252585));
#154893=CARTESIAN_POINT('Ctrl Pts',(39.0805260696444,18.1997099337144,-80.624379737664));
#154894=CARTESIAN_POINT('Ctrl Pts',(39.0815474123718,18.1992690484656,-80.6159388500695));
#154895=CARTESIAN_POINT('Ctrl Pts',(39.0827573834569,18.1987528067232,-80.6060491570009));
#154896=CARTESIAN_POINT('Ctrl Pts',(39.0836274177688,18.1983848455065,-80.5989965285573));
#154897=CARTESIAN_POINT('Ctrl Pts',(39.1051352614155,18.1892885923952,-80.4246507265768));
#154898=CARTESIAN_POINT('Ctrl Pts',(39.1309066704761,18.1801885513109,-80.2503500624807));
#154899=CARTESIAN_POINT('Ctrl Pts',(39.1610112640735,18.1711018501782,-80.0763839135592));
#154900=CARTESIAN_POINT('Ctrl Pts',(39.1698759392603,18.1684261570551,-80.0251573989507));
#154901=CARTESIAN_POINT('Ctrl Pts',(39.1791159978341,18.1657516191816,-79.9739598404955));
#154902=CARTESIAN_POINT('Ctrl Pts',(39.1887323599578,18.1630786698777,-79.9227985019606));
#154903=CARTESIAN_POINT('Ctrl Pts',(39.220134300174,18.1543502346169,-79.7557326954332));
#154904=CARTESIAN_POINT('Ctrl Pts',(39.2555525447006,18.1456378884788,-79.589054911354));
#154905=CARTESIAN_POINT('Ctrl Pts',(39.2949852319104,18.1369559053374,-79.4230299972133));
#154906=CARTESIAN_POINT('Ctrl Pts',(39.3069784381681,18.1343153342298,-79.3725345534556));
#154907=CARTESIAN_POINT('Ctrl Pts',(39.3193426296427,18.1316775749095,-79.3220995551001));
#154908=CARTESIAN_POINT('Ctrl Pts',(39.3320767843687,18.1290430353581,-79.2717325590862));
#154909=CARTESIAN_POINT('Ctrl Pts',(39.3335084096053,18.1287468497541,-79.2660700974515));
#154910=CARTESIAN_POINT('Ctrl Pts',(39.3346928938226,18.1285025254522,-79.2613992073983));
#154911=CARTESIAN_POINT('Ctrl Pts',(39.3362385925853,18.1282026907361,-79.2553029077291));
#154912=CARTESIAN_POINT('Ctrl Pts',(39.3365946309511,18.1281336263977,-79.2538986777304));
#154913=CARTESIAN_POINT('Ctrl Pts',(39.3369699173628,18.1280616163234,-79.2524188090918));
#154914=CARTESIAN_POINT('Ctrl Pts',(39.3373720289107,18.1279853490152,-79.2508337742336));
#154915=CARTESIAN_POINT('Ctrl Pts',(39.3664342551112,18.1224732025065,-79.1362769010717));
#154916=CARTESIAN_POINT('Ctrl Pts',(39.3969619678381,18.1169261390775,-79.0242808226136));
#154917=CARTESIAN_POINT('Ctrl Pts',(39.428775919443,18.1113778371804,-78.9148742209707));
#154918=CARTESIAN_POINT('Ctrl Pts',(39.43458111554,18.1103654203351,-78.8949104395223));
#154919=CARTESIAN_POINT('Ctrl Pts',(39.4404291962516,18.1093529632644,-78.8750327509934));
#154920=CARTESIAN_POINT('Ctrl Pts',(39.4463191483709,18.108340671569,-78.8552411650393));
#154921=CARTESIAN_POINT('Ctrl Pts',(39.4749454395885,18.1034207407643,-78.7590502806814));
#154922=CARTESIAN_POINT('Ctrl Pts',(39.5045596054427,18.0985048054926,-78.6648976879518));
#154923=CARTESIAN_POINT('Ctrl Pts',(39.5350352637485,18.0936321430839,-78.5728004536459));
#154924=CARTESIAN_POINT('Ctrl Pts',(39.571899290306,18.0877380634667,-78.4613976134759));
#154925=CARTESIAN_POINT('Ctrl Pts',(39.6100411528787,18.0819102751752,-78.3529478782708));
#154926=CARTESIAN_POINT('Ctrl Pts',(39.649204178819,18.076223152307,-78.24756060623));
#154927=CARTESIAN_POINT('Ctrl Pts',(39.6883672047593,18.0705360294389,-78.1421733341892));
#154928=CARTESIAN_POINT('Ctrl Pts',(39.7285512433921,18.0649896536414,-78.039848263612));
#154929=CARTESIAN_POINT('Ctrl Pts',(39.7694967206528,18.0596550895294,-77.9406424526632));
#154930=CARTESIAN_POINT('Ctrl Pts',(39.7891552025899,18.0570938925608,-77.8930123901248));
#154931=CARTESIAN_POINT('Ctrl Pts',(39.8089883024401,18.0545801164714,-77.8460748119818));
#154932=CARTESIAN_POINT('Ctrl Pts',(39.8289779243427,18.0521207730912,-77.799822102316));
#154933=CARTESIAN_POINT('Ctrl Pts',(39.8812607387598,18.0456883656069,-77.6788482366005));
#154934=CARTESIAN_POINT('Ctrl Pts',(39.9345962223184,18.039559426019,-77.5627033684304));
#154935=CARTESIAN_POINT('Ctrl Pts',(39.9886489788594,18.0337023607363,-77.4513444300145));
#154936=CARTESIAN_POINT('Ctrl Pts',(40.0294901638302,18.0292768790051,-77.3672038367675));
#154937=CARTESIAN_POINT('Ctrl Pts',(40.0707395862103,18.0250065798345,-77.2857950222072));
#154938=CARTESIAN_POINT('Ctrl Pts',(40.112234287026,18.0208776696245,-77.2070925617702));
#154939=CARTESIAN_POINT('Ctrl Pts',(40.1739111069978,18.0147405473728,-77.090110937893));
#154940=CARTESIAN_POINT('Ctrl Pts',(40.2361301260653,18.0089161027968,-76.9791130352856));
#154941=CARTESIAN_POINT('Ctrl Pts',(40.2982915106338,18.0033979264447,-76.8739688586284));
#154942=CARTESIAN_POINT('Ctrl Pts',(40.3332999615727,18.0002901641669,-76.8147530806086));
#154943=CARTESIAN_POINT('Ctrl Pts',(40.3682890824644,17.9972795185705,-76.7573935352408));
#154944=CARTESIAN_POINT('Ctrl Pts',(40.4031452967415,17.9943646881396,-76.7018642559303));
#154945=CARTESIAN_POINT('',(40.1676094225648,12.3781800338281,-84.0075170117514));
#154946=CARTESIAN_POINT('Ctrl Pts',(40.1676234671554,12.3782653665599,-84.0075554249296));
#154947=CARTESIAN_POINT('Ctrl Pts',(40.1854904141354,12.8044715491944,-83.4873941951976));
#154948=CARTESIAN_POINT('Ctrl Pts',(40.2034989189839,13.2330557803372,-82.9558646413233));
#154949=CARTESIAN_POINT('Ctrl Pts',(40.221636439171,13.6644456562588,-82.4126443566806));
#154950=CARTESIAN_POINT('Ctrl Pts',(40.2299404179379,13.8619507359476,-82.1639394806617));
#154951=CARTESIAN_POINT('Ctrl Pts',(40.2382713875396,14.0600443482884,-81.9127845855315));
#154952=CARTESIAN_POINT('Ctrl Pts',(40.2466278643551,14.258769973405,-81.6591515576612));
#154953=CARTESIAN_POINT('Ctrl Pts',(40.2645132823419,14.6841036335584,-81.1162992505338));
#154954=CARTESIAN_POINT('Ctrl Pts',(40.2824940000457,15.1117784931431,-80.5627632534198));
#154955=CARTESIAN_POINT('Ctrl Pts',(40.3005593524997,15.5420020743483,-79.9983299955263));
#154956=CARTESIAN_POINT('Ctrl Pts',(40.3175555231764,15.9467632565014,-79.4673022167339));
#154957=CARTESIAN_POINT('Ctrl Pts',(40.3346265987071,16.3537802388756,-78.9266287711736));
#154958=CARTESIAN_POINT('Ctrl Pts',(40.351761140265,16.7632308195706,-78.3761759459867));
#154959=CARTESIAN_POINT('Ctrl Pts',(40.3688308672064,17.1711325766644,-77.8278053118314));
#154960=CARTESIAN_POINT('Ctrl Pts',(40.3859635974491,17.581449344521,-77.2697285875284));
#154961=CARTESIAN_POINT('Ctrl Pts',(40.4031453084497,17.9943647931319,-76.7018643085084));
#154962=CARTESIAN_POINT('Ctrl Pts',(40.1676094225648,12.3781800338281,-84.0075170117514));
#154963=CARTESIAN_POINT('Ctrl Pts',(40.0228549897639,12.3915973180658,-84.254864531227));
#154964=CARTESIAN_POINT('Ctrl Pts',(39.8658980290371,12.4063586860731,-84.557511956544));
#154965=CARTESIAN_POINT('Ctrl Pts',(39.6366325098753,12.4354191976067,-85.1013040029903));
#154966=CARTESIAN_POINT('Ctrl Pts',(39.5613574468262,12.4462035443194,-85.2975097823435));
#154967=CARTESIAN_POINT('Ctrl Pts',(39.4541753102143,12.4637879130523,-85.6144735095455));
#154968=CARTESIAN_POINT('Ctrl Pts',(39.4194087915838,12.4698763705169,-85.723898191007));
#154969=CARTESIAN_POINT('Ctrl Pts',(39.3692414744553,12.4792413419471,-85.8936607669787));
#154970=CARTESIAN_POINT('Ctrl Pts',(39.3446537532988,12.4839810030478,-85.9799477336672));
#154971=CARTESIAN_POINT('Ctrl Pts',(39.3169568710184,12.4895770893797,-86.0830613712933));
#154972=CARTESIAN_POINT('Ctrl Pts',(39.3033708464989,12.4923867809843,-86.1352271323001));
#154973=CARTESIAN_POINT('Ctrl Pts',(39.2976061261076,12.4935928782,-86.1577140972523));
#154974=CARTESIAN_POINT('Ctrl Pts',(39.2937760184904,12.4943973114159,-86.172734310248));
#154975=CARTESIAN_POINT('Ctrl Pts',(39.2914838099539,12.4948809191622,-86.1817797064966));
#154976=CARTESIAN_POINT('Ctrl Pts',(39.1927975915771,12.5157684085442,-86.5729597638327));
#154977=CARTESIAN_POINT('Ctrl Pts',(39.1204470384713,12.5381366398829,-86.9632929573707));
#154978=CARTESIAN_POINT('Ctrl Pts',(39.0247795673145,12.5764456511043,-87.744877974384));
#154979=CARTESIAN_POINT('Ctrl Pts',(39.0000000163315,12.5990133424068,-88.1415519987986));
#154980=CARTESIAN_POINT('Ctrl Pts',(39.,12.61999998,-88.5398461374725));
#154981=CARTESIAN_POINT('Origin',(39.,46.91999998,-129.34995));
#154982=CARTESIAN_POINT('',(39.,12.61999998,-143.518796834034));
#154983=CARTESIAN_POINT('',(39.,18.26999998,-150.084863924608));
#154984=CARTESIAN_POINT('Ctrl Pts',(39.,12.61999998,-143.518796834034));
#154985=CARTESIAN_POINT('Ctrl Pts',(39.0000000000004,13.1830701012418,-144.125823176784));
#154986=CARTESIAN_POINT('Ctrl Pts',(39.000000000008,13.738335643728,-144.73925540157));
#154987=CARTESIAN_POINT('Ctrl Pts',(39.0000000000126,14.2868563031708,-145.358644195209));
#154988=CARTESIAN_POINT('Ctrl Pts',(39.0000000000176,14.8748775264481,-146.0226369726));
#154989=CARTESIAN_POINT('Ctrl Pts',(39.0000000000202,15.4551472634197,-146.693475297462));
#154990=CARTESIAN_POINT('Ctrl Pts',(39.0000000000369,16.0289279109354,-147.370648869858));
#154991=CARTESIAN_POINT('Ctrl Pts',(39.0000000000444,16.2865138368738,-147.674650725657));
#154992=CARTESIAN_POINT('Ctrl Pts',(39.000000000055,16.5427914446702,-147.979929896419));
#154993=CARTESIAN_POINT('Ctrl Pts',(39.0000000000741,16.7978726164159,-148.286442551932));
#154994=CARTESIAN_POINT('Ctrl Pts',(39.0000000001113,17.2936331206748,-148.88216221097));
#154995=CARTESIAN_POINT('Ctrl Pts',(39.0000000001696,17.7841600789862,-149.481724824065));
#154996=CARTESIAN_POINT('Ctrl Pts',(39.0000000003777,18.26999998,-150.084863924608));
#154997=CARTESIAN_POINT('',(39.,18.26999998,-129.34995));
#154998=CARTESIAN_POINT('',(39.,12.61999998,-129.34995));
#154999=CARTESIAN_POINT('Ctrl Pts',(40.4049679555898,18.0381725147214,-155.417048749269));
#155000=CARTESIAN_POINT('Ctrl Pts',(39.,19.1920625442621,-154.533208999946));
#155001=CARTESIAN_POINT('Ctrl Pts',(39.,20.7969022442792,-153.303957440565));
#155002=CARTESIAN_POINT('Ctrl Pts',(40.3537709661131,16.8074898953919,-153.723238579969));
#155003=CARTESIAN_POINT('Ctrl Pts',(38.9999999999926,17.9467387756562,-152.837123072008));
#155004=CARTESIAN_POINT('Ctrl Pts',(39.,19.4994946787828,-151.61013720275));
#155005=CARTESIAN_POINT('Ctrl Pts',(40.3009026952457,15.549481350471,-152.046823901733));
#155006=CARTESIAN_POINT('Ctrl Pts',(38.9999999999925,16.6677293129161,-151.153378312361));
#155007=CARTESIAN_POINT('Ctrl Pts',(39.,18.1688145972663,-149.933732593));
#155008=CARTESIAN_POINT('Ctrl Pts',(40.1923546827668,12.9680978184463,-148.752208985047));
#155009=CARTESIAN_POINT('Ctrl Pts',(39.0000000000073,14.0355026731613,-147.843763736059));
#155010=CARTESIAN_POINT('Ctrl Pts',(39.,15.4269724929124,-146.639117676373));
#155011=CARTESIAN_POINT('Ctrl Pts',(40.1368768832445,11.6498727042044,-147.140254909589));
#155012=CARTESIAN_POINT('Ctrl Pts',(39.0000000000223,12.6882757758116,-146.224143705887));
#155013=CARTESIAN_POINT('Ctrl Pts',(39.,14.0212803181596,-145.027145257042));
#155014=CARTESIAN_POINT('Ctrl Pts',(40.0806897728025,10.2937241351084,-145.576231462098));
#155015=CARTESIAN_POINT('Ctrl Pts',(39.,11.293230102484,-144.64769997634));
#155016=CARTESIAN_POINT('Ctrl Pts',(39.,12.5683345334111,-143.463140153395));
#155017=CARTESIAN_POINT('',(40.4031452850214,17.9943647518538,-155.356778726108));
#155018=CARTESIAN_POINT('',(40.1676094240942,12.378180022345,-148.051125971627));
#155019=CARTESIAN_POINT('Ctrl Pts',(40.4031453084766,17.9943647936175,-155.356778662625));
#155020=CARTESIAN_POINT('Ctrl Pts',(40.3860321140814,17.5830959513313,-154.791178868832));
#155021=CARTESIAN_POINT('Ctrl Pts',(40.3689676275558,17.1744079304129,-154.235292309724));
#155022=CARTESIAN_POINT('Ctrl Pts',(40.3519656027356,16.7681166958106,-153.689035359578));
#155023=CARTESIAN_POINT('Ctrl Pts',(40.3339478834236,16.3375537774879,-153.110145227137));
#155024=CARTESIAN_POINT('Ctrl Pts',(40.316000320502,15.9096827342591,-152.542069480784));
#155025=CARTESIAN_POINT('Ctrl Pts',(40.2981360458695,15.4842945621373,-151.984648335164));
#155026=CARTESIAN_POINT('Ctrl Pts',(40.2808862495354,15.0735384870678,-151.446400831022));
#155027=CARTESIAN_POINT('Ctrl Pts',(40.2637140755375,14.665097672676,-150.918086687449));
#155028=CARTESIAN_POINT('Ctrl Pts',(40.2466286890062,14.2587895844586,-150.39951644339));
#155029=CARTESIAN_POINT('Ctrl Pts',(40.2283833140916,13.8248957777965,-149.845738599086));
#155030=CARTESIAN_POINT('Ctrl Pts',(40.210259843033,13.3940133909222,-149.30377834175));
#155031=CARTESIAN_POINT('Ctrl Pts',(40.1922726412517,12.9657005449508,-148.773332424983));
#155032=CARTESIAN_POINT('Ctrl Pts',(40.1840273016278,12.7693617856903,-148.530175830143));
#155033=CARTESIAN_POINT('Ctrl Pts',(40.1758105398716,12.5735634700978,-148.289438170232));
#155034=CARTESIAN_POINT('Ctrl Pts',(40.1676234671417,12.3782653572967,-148.051087554154));
#155035=CARTESIAN_POINT('Ctrl Pts',(40.4031452966654,17.994364688146,-155.356778715455));
#155036=CARTESIAN_POINT('Ctrl Pts',(40.3417594471859,17.9994980567657,-155.258985209779));
#155037=CARTESIAN_POINT('Ctrl Pts',(40.280419765882,18.0048901664367,-155.156247032814));
#155038=CARTESIAN_POINT('Ctrl Pts',(40.2196167541285,18.0105466339004,-155.04845145244));
#155039=CARTESIAN_POINT('Ctrl Pts',(40.173064781723,18.01487733578,-154.965921052411));
#155040=CARTESIAN_POINT('Ctrl Pts',(40.1268268322551,18.0193629844826,-154.880426356048));
#155041=CARTESIAN_POINT('Ctrl Pts',(40.081103453352,18.0240056787045,-154.791924271342));
#155042=CARTESIAN_POINT('Ctrl Pts',(40.0300289459692,18.0291917197627,-154.69306455259));
#155043=CARTESIAN_POINT('Ctrl Pts',(39.9796023466813,18.0345733014836,-154.590459987357));
#155044=CARTESIAN_POINT('Ctrl Pts',(39.9300871858588,18.0401504376233,-154.484104885994));
#155045=CARTESIAN_POINT('Ctrl Pts',(39.8805720250364,18.045727573763,-154.37774978463));
#155046=CARTESIAN_POINT('Ctrl Pts',(39.8319690807585,18.0515002708413,-154.267644023757));
#155047=CARTESIAN_POINT('Ctrl Pts',(39.7845003415924,18.0574666071742,-154.153818005325));
#155048=CARTESIAN_POINT('Ctrl Pts',(39.7814378422914,18.0578515320989,-154.146474391232));
#155049=CARTESIAN_POINT('Ctrl Pts',(39.7776001357721,18.0583360042348,-154.13723144672));
#155050=CARTESIAN_POINT('Ctrl Pts',(39.7753269786915,18.0586238608678,-154.131740764591));
#155051=CARTESIAN_POINT('Ctrl Pts',(39.77395412672,18.0587977091907,-154.128424718441));
#155052=CARTESIAN_POINT('Ctrl Pts',(39.772580519514,18.0589719361886,-154.125101397286));
#155053=CARTESIAN_POINT('Ctrl Pts',(39.7712061770303,18.0591465420297,-154.121770798376));
#155054=CARTESIAN_POINT('Ctrl Pts',(39.7147134503032,18.0663237632711,-153.984865611844));
#155055=CARTESIAN_POINT('Ctrl Pts',(39.6570058671139,18.0741420356517,-153.835646393747));
#155056=CARTESIAN_POINT('Ctrl Pts',(39.5997365496176,18.0826184704731,-153.673814403576));
#155057=CARTESIAN_POINT('Ctrl Pts',(39.5845780628911,18.0848620789243,-153.630979458405));
#155058=CARTESIAN_POINT('Ctrl Pts',(39.5694505681787,18.0871518019538,-153.587260749271));
#155059=CARTESIAN_POINT('Ctrl Pts',(39.5543851687262,18.0894879617595,-153.542652542234));
#155060=CARTESIAN_POINT('Ctrl Pts',(39.5151902756828,18.0955658313842,-153.426597610589));
#155061=CARTESIAN_POINT('Ctrl Pts',(39.4764206630589,18.1019568988266,-153.304531892792));
#155062=CARTESIAN_POINT('Ctrl Pts',(39.4386411928737,18.1086618989044,-153.176428855199));
#155063=CARTESIAN_POINT('Ctrl Pts',(39.4068074123412,18.1143116737662,-153.06848652662));
#155064=CARTESIAN_POINT('Ctrl Pts',(39.3756773812159,18.120184284672,-152.956258735352));
#155065=CARTESIAN_POINT('Ctrl Pts',(39.3455832861018,18.1262784534442,-152.839761180211));
#155066=CARTESIAN_POINT('Ctrl Pts',(39.3445386995356,18.1264899861986,-152.835717470619));
#155067=CARTESIAN_POINT('Ctrl Pts',(39.3431410854322,18.1267738816604,-152.830290388621));
#155068=CARTESIAN_POINT('Ctrl Pts',(39.3424532775621,18.1269138636721,-152.827614629636));
#155069=CARTESIAN_POINT('Ctrl Pts',(39.3413285750048,18.1271427620804,-152.823239231935));
#155070=CARTESIAN_POINT('Ctrl Pts',(39.3401977921499,18.1273735054214,-152.818828478333));
#155071=CARTESIAN_POINT('Ctrl Pts',(39.3390610558454,18.1276060961256,-152.814382322845));
#155072=CARTESIAN_POINT('Ctrl Pts',(39.3244959323229,18.130586305629,-152.757413258302));
#155073=CARTESIAN_POINT('Ctrl Pts',(39.3089685134929,18.1338668144423,-152.694689316399));
#155074=CARTESIAN_POINT('Ctrl Pts',(39.2927900726882,18.1374504392791,-152.626156872866));
#155075=CARTESIAN_POINT('Ctrl Pts',(39.2855217920503,18.1390604084554,-152.595368180778));
#155076=CARTESIAN_POINT('Ctrl Pts',(39.2781228183628,18.1407315528484,-152.563407190484));
#155077=CARTESIAN_POINT('Ctrl Pts',(39.2706247681685,18.142464101305,-152.530269443939));
#155078=CARTESIAN_POINT('Ctrl Pts',(39.2578795193265,18.1454091017568,-152.473941623395));
#155079=CARTESIAN_POINT('Ctrl Pts',(39.2448479300532,18.1485312638142,-152.414216824096));
#155080=CARTESIAN_POINT('Ctrl Pts',(39.2316997667936,18.1518310602961,-152.351082418171));
#155081=CARTESIAN_POINT('Ctrl Pts',(39.2251256851638,18.1534809585371,-152.319515215208));
#155082=CARTESIAN_POINT('Ctrl Pts',(39.2185227175705,18.1551752605691,-152.287095693681));
#155083=CARTESIAN_POINT('Ctrl Pts',(39.2119135922845,18.1569139918642,-152.253822861645));
#155084=CARTESIAN_POINT('Ctrl Pts',(39.2086090296414,18.1577833575118,-152.237186445627));
#155085=CARTESIAN_POINT('Ctrl Pts',(39.2053029411143,18.1586638305792,-152.220336699373));
#155086=CARTESIAN_POINT('Ctrl Pts',(39.2019982610058,18.1595554112169,-152.203273553159));
#155087=CARTESIAN_POINT('Ctrl Pts',(39.2003459209516,18.1600012015357,-152.194741980052));
#155088=CARTESIAN_POINT('Ctrl Pts',(39.198693933812,18.1604497687537,-152.186157056788));
#155089=CARTESIAN_POINT('Ctrl Pts',(39.1970426716466,18.1609011128083,-152.177518775964));
#155090=CARTESIAN_POINT('Ctrl Pts',(39.1962170405639,18.1611267848356,-152.173199635552));
#155091=CARTESIAN_POINT('Ctrl Pts',(39.1953915907749,18.1613531510724,-152.16886715574));
#155092=CARTESIAN_POINT('Ctrl Pts',(39.1945663691362,18.1615802114996,-152.164521335805));
#155093=CARTESIAN_POINT('Ctrl Pts',(39.1937411474975,18.1618072719268,-152.160175515869));
#155094=CARTESIAN_POINT('Ctrl Pts',(39.1931776325701,18.1619625964041,-152.157202665874));
#155095=CARTESIAN_POINT('Ctrl Pts',(39.1920914357414,18.1622634753302,-152.15144385495));
#155096=CARTESIAN_POINT('Ctrl Pts',(39.1788631156134,18.1659277492899,-152.081309794124));
#155097=CARTESIAN_POINT('Ctrl Pts',(39.1672931884971,18.1693409956331,-152.016198167235));
#155098=CARTESIAN_POINT('Ctrl Pts',(39.1570953546843,18.1724913915801,-151.956153037642));
#155099=CARTESIAN_POINT('Ctrl Pts',(39.1467171302433,18.1756975152351,-151.895045763004));
#155100=CARTESIAN_POINT('Ctrl Pts',(39.1377599277363,18.1786314258552,-151.83918548891));
#155101=CARTESIAN_POINT('Ctrl Pts',(39.1299726355725,18.1812818179602,-151.788599497983));
#155102=CARTESIAN_POINT('Ctrl Pts',(39.1253058882552,18.1828701377491,-151.758284462604));
#155103=CARTESIAN_POINT('Ctrl Pts',(39.1210602663186,18.1843566573616,-151.729863257325));
#155104=CARTESIAN_POINT('Ctrl Pts',(39.1171902972612,18.1857390937416,-151.703339248921));
#155105=CARTESIAN_POINT('Ctrl Pts',(39.1106448931655,18.188077253197,-151.658478333843));
#155106=CARTESIAN_POINT('Ctrl Pts',(39.1051703967782,18.1901236336778,-151.619046015605));
#155107=CARTESIAN_POINT('Ctrl Pts',(39.1005859920701,18.1918842844985,-151.585053901893));
#155108=CARTESIAN_POINT('Ctrl Pts',(39.0993314455262,18.1923660958879,-151.575751780573));
#155109=CARTESIAN_POINT('Ctrl Pts',(39.0981438522368,18.1928265117298,-151.566857005841));
#155110=CARTESIAN_POINT('Ctrl Pts',(39.097020173279,18.193265659932,-151.558369702141));
#155111=CARTESIAN_POINT('Ctrl Pts',(39.0944052417367,18.1942876088418,-151.538618759936));
#155112=CARTESIAN_POINT('Ctrl Pts',(39.092135864911,18.1951945362373,-151.521074619786));
#155113=CARTESIAN_POINT('Ctrl Pts',(39.0901796603349,18.1959884327771,-151.50573856626));
#155114=CARTESIAN_POINT('Ctrl Pts',(39.0892015580469,18.196385381047,-151.498070539497));
#155115=CARTESIAN_POINT('Ctrl Pts',(39.0883018748229,18.1967540904593,-151.490954519409));
#155116=CARTESIAN_POINT('Ctrl Pts',(39.0874773395217,18.1970947718093,-151.484390616359));
#155117=CARTESIAN_POINT('Ctrl Pts',(39.0870650718711,18.1972651124842,-151.481108664835));
#155118=CARTESIAN_POINT('Ctrl Pts',(39.0866715989482,18.1974284473239,-151.477964741632));
#155119=CARTESIAN_POINT('Ctrl Pts',(39.086296559352,18.1975848038151,-151.474958857364));
#155120=CARTESIAN_POINT('Ctrl Pts',(39.0861090395539,18.1976629820607,-151.473455915231));
#155121=CARTESIAN_POINT('Ctrl Pts',(39.0859261285695,18.19773941579,-151.471987482775));
#155122=CARTESIAN_POINT('Ctrl Pts',(39.0857477842125,18.197814108305,-151.470553561156));
#155123=CARTESIAN_POINT('Ctrl Pts',(39.085658612034,18.1978514545625,-151.469836600346));
#155124=CARTESIAN_POINT('Ctrl Pts',(39.0855705815424,18.1978883655208,-151.469128267242));
#155125=CARTESIAN_POINT('Ctrl Pts',(39.0854836876517,18.1979248415804,-151.468428561981));
#155126=CARTESIAN_POINT('Ctrl Pts',(39.0854619641791,18.1979339605953,-151.468253635665));
#155127=CARTESIAN_POINT('Ctrl Pts',(39.0854515340338,18.197938339297,-151.4681696234));
#155128=CARTESIAN_POINT('Ctrl Pts',(39.0854439756643,18.1979415118432,-151.468108744634));
#155129=CARTESIAN_POINT('Ctrl Pts',(39.0854326381102,18.1979462706624,-151.468017426485));
#155130=CARTESIAN_POINT('Ctrl Pts',(39.0854277616982,18.1979483155799,-151.46797815875));
#155131=CARTESIAN_POINT('Ctrl Pts',(39.0854009525399,18.1979595786092,-151.467762178707));
#155132=CARTESIAN_POINT('Ctrl Pts',(39.0853741433817,18.1979708416385,-151.467546198663));
#155133=CARTESIAN_POINT('Ctrl Pts',(39.0853253870772,18.1979913212022,-151.467153507985));
#155134=CARTESIAN_POINT('Ctrl Pts',(39.085226410725,18.1980329661159,-151.466355329862));
#155135=CARTESIAN_POINT('Ctrl Pts',(39.0849289026081,18.1981581445001,-151.463956125758));
#155136=CARTESIAN_POINT('Ctrl Pts',(39.0846323917651,18.1982832354517,-151.46155857911));
#155137=CARTESIAN_POINT('Ctrl Pts',(39.0843368746301,18.1984082389251,-151.459162690843));
#155138=CARTESIAN_POINT('Ctrl Pts',(39.0670855857401,18.2057055180914,-151.319298852997));
#155139=CARTESIAN_POINT('Ctrl Pts',(39.0531814282618,18.2127125095008,-151.184936931341));
#155140=CARTESIAN_POINT('Ctrl Pts',(39.0420026133318,18.2194266697535,-151.056136661796));
#155141=CARTESIAN_POINT('Ctrl Pts',(39.0308452663617,18.2261279360345,-150.927583742174));
#155142=CARTESIAN_POINT('Ctrl Pts',(39.0224027838946,18.2325374963608,-150.804571134108));
#155143=CARTESIAN_POINT('Ctrl Pts',(39.0161084260695,18.238653156518,-150.687152448744));
#155144=CARTESIAN_POINT('Ctrl Pts',(39.0098304711397,18.2447528794603,-150.570039752719));
#155145=CARTESIAN_POINT('Ctrl Pts',(39.0056894504988,18.2505602334755,-150.458491861449));
#155146=CARTESIAN_POINT('Ctrl Pts',(39.0031745103681,18.2560733519913,-150.352556215922));
#155147=CARTESIAN_POINT('Ctrl Pts',(39.000951854371,18.2609457407142,-150.258932318096));
#155148=CARTESIAN_POINT('Ctrl Pts',(39.,18.2655883162516,-150.169691888134));
#155149=CARTESIAN_POINT('Ctrl Pts',(39.,18.26999998,-150.084863924608));
#155150=CARTESIAN_POINT('Ctrl Pts',(39.,12.61999998,-143.518796834034));
#155151=CARTESIAN_POINT('Ctrl Pts',(39.,12.6151217916977,-143.611377351187));
#155152=CARTESIAN_POINT('Ctrl Pts',(39.001285417222,12.6099953737847,-143.708586401381));
#155153=CARTESIAN_POINT('Ctrl Pts',(39.0042875091668,12.6046202721211,-143.810409212199));
#155154=CARTESIAN_POINT('Ctrl Pts',(39.0070158061698,12.5997353871711,-143.902945641696));
#155155=CARTESIAN_POINT('Ctrl Pts',(39.0111625213286,12.5946450511523,-143.999293736081));
#155156=CARTESIAN_POINT('Ctrl Pts',(39.0170880852875,12.5893494102396,-144.099432636865));
#155157=CARTESIAN_POINT('Ctrl Pts',(39.0226020020085,12.5844216559904,-144.192614916778));
#155158=CARTESIAN_POINT('Ctrl Pts',(39.0296564835121,12.5793163599211,-144.289075241998));
#155159=CARTESIAN_POINT('Ctrl Pts',(39.0385666744866,12.5740351371479,-144.388768460183));
#155160=CARTESIAN_POINT('Ctrl Pts',(39.0430217699738,12.5713945257613,-144.438615069276));
#155161=CARTESIAN_POINT('Ctrl Pts',(39.0479411388294,12.5687099636132,-144.489269319451));
#155162=CARTESIAN_POINT('Ctrl Pts',(39.0533661791931,12.5659817900504,-144.540723001229));
#155163=CARTESIAN_POINT('Ctrl Pts',(39.056078699375,12.564617703269,-144.566449842117));
#155164=CARTESIAN_POINT('Ctrl Pts',(39.0589176574687,12.5632427150076,-144.592376515436));
#155165=CARTESIAN_POINT('Ctrl Pts',(39.0618883354043,12.5618568790563,-144.618501783899));
#155166=CARTESIAN_POINT('Ctrl Pts',(39.0626310048883,12.5615104200685,-144.625033101014));
#155167=CARTESIAN_POINT('Ctrl Pts',(39.0633819072345,12.5611632831152,-144.631576830055));
#155168=CARTESIAN_POINT('Ctrl Pts',(39.0641411256594,12.5608154690912,-144.638132950689));
#155169=CARTESIAN_POINT('Ctrl Pts',(39.0647105394781,12.5605546085733,-144.643050041165));
#155170=CARTESIAN_POINT('Ctrl Pts',(39.0652846310973,12.5602933672032,-144.647974101911));
#155171=CARTESIAN_POINT('Ctrl Pts',(39.0658634357377,12.5600317453597,-144.652905124331));
#155172=CARTESIAN_POINT('Ctrl Pts',(39.0660384936335,12.5599526185417,-144.654396498707));
#155173=CARTESIAN_POINT('Ctrl Pts',(39.0662133034635,12.559873761637,-144.655882766897));
#155174=CARTESIAN_POINT('Ctrl Pts',(39.0663916080063,12.5597934932929,-144.65739561764));
#155175=CARTESIAN_POINT('Ctrl Pts',(39.0677898358322,12.5591640453241,-144.669259084336));
#155176=CARTESIAN_POINT('Ctrl Pts',(39.0693646538055,12.5584672545937,-144.682390329012));
#155177=CARTESIAN_POINT('Ctrl Pts',(39.0706765465421,12.5578951255962,-144.693171271542));
#155178=CARTESIAN_POINT('Ctrl Pts',(39.070856771342,12.5578165278334,-144.694652332574));
#155179=CARTESIAN_POINT('Ctrl Pts',(39.0710319534679,12.5577402823252,-144.696089049905));
#155180=CARTESIAN_POINT('Ctrl Pts',(39.0712008829784,12.5576668864921,-144.697472054104));
#155181=CARTESIAN_POINT('Ctrl Pts',(39.0869456209749,12.5508261743042,-144.826372201183));
#155182=CARTESIAN_POINT('Ctrl Pts',(39.1053961392304,12.5438077204206,-144.955367405366));
#155183=CARTESIAN_POINT('Ctrl Pts',(39.126578585198,12.5367888738498,-145.084303731865));
#155184=CARTESIAN_POINT('Ctrl Pts',(39.1370708909132,12.5333122270027,-145.148169791408));
#155185=CARTESIAN_POINT('Ctrl Pts',(39.1482327304231,12.5298352050449,-145.212021539346));
#155186=CARTESIAN_POINT('Ctrl Pts',(39.1600630009103,12.5263775808316,-145.275841235295));
#155187=CARTESIAN_POINT('Ctrl Pts',(39.1689914693088,12.5237680641214,-145.324006840561));
#155188=CARTESIAN_POINT('Ctrl Pts',(39.1783005066348,12.521170027977,-145.37215406157));
#155189=CARTESIAN_POINT('Ctrl Pts',(39.187988311637,12.5185924412067,-145.42027522266));
#155190=CARTESIAN_POINT('Ctrl Pts',(39.1976761166393,12.5160148544364,-145.468396383749));
#155191=CARTESIAN_POINT('Ctrl Pts',(39.2077426849771,12.5134577213724,-145.516491480961));
#155192=CARTESIAN_POINT('Ctrl Pts',(39.2181853048246,12.5109296373551,-145.564553167133));
#155193=CARTESIAN_POINT('Ctrl Pts',(39.228627924672,12.5084015533379,-145.612614853305));
#155194=CARTESIAN_POINT('Ctrl Pts',(39.2394465955928,12.5059025182058,-145.660643128128));
#155195=CARTESIAN_POINT('Ctrl Pts',(39.2506376189685,12.5034410609666,-145.70863080923));
#155196=CARTESIAN_POINT('Ctrl Pts',(39.2562331306563,12.5022103323471,-145.732624649781));
#155197=CARTESIAN_POINT('Ctrl Pts',(39.2619217169944,12.5009889917376,-145.756608347695));
#155198=CARTESIAN_POINT('Ctrl Pts',(39.2677028352578,12.4997780721034,-145.780581038343));
#155199=CARTESIAN_POINT('Ctrl Pts',(39.2705933943894,12.4991726122863,-145.792567383666));
#155200=CARTESIAN_POINT('Ctrl Pts',(39.2735070857133,12.4985697572877,-145.804550977563));
#155201=CARTESIAN_POINT('Ctrl Pts',(39.2764438363011,12.4979696347552,-145.81653171371));
#155202=CARTESIAN_POINT('Ctrl Pts',(39.2779122115949,12.497669573489,-145.822522081783));
#155203=CARTESIAN_POINT('Ctrl Pts',(39.2793863516566,12.4973701953126,-145.828511735444));
#155204=CARTESIAN_POINT('Ctrl Pts',(39.2808662470572,12.4970715160892,-145.834500661514));
#155205=CARTESIAN_POINT('Ctrl Pts',(39.282143744699,12.4968136857024,-145.83967051266));
#155206=CARTESIAN_POINT('Ctrl Pts',(39.2831842318061,12.4966045567679,-145.843868940243));
#155207=CARTESIAN_POINT('Ctrl Pts',(39.2846166008847,12.496302858648,-145.849609262975));
#155208=CARTESIAN_POINT('Ctrl Pts',(39.2848435353867,12.4962550597157,-145.850518719414));
#155209=CARTESIAN_POINT('Ctrl Pts',(39.2850803473589,12.4962049370979,-145.851466879967));
#155210=CARTESIAN_POINT('Ctrl Pts',(39.2853295849969,12.4961519292614,-145.85246373439));
#155211=CARTESIAN_POINT('Ctrl Pts',(39.3144876655075,12.4899505915487,-145.96908481043));
#155212=CARTESIAN_POINT('Ctrl Pts',(39.3452757917139,12.4838818138653,-146.082626080962));
#155213=CARTESIAN_POINT('Ctrl Pts',(39.377433242888,12.4779746135799,-146.193064054807));
#155214=CARTESIAN_POINT('Ctrl Pts',(39.4015513312685,12.4735442133658,-146.27589253519));
#155215=CARTESIAN_POINT('Ctrl Pts',(39.4264397287502,12.4692045367127,-146.356975344281));
#155216=CARTESIAN_POINT('Ctrl Pts',(39.451991679228,12.4649566420713,-146.436300560345));
#155217=CARTESIAN_POINT('Ctrl Pts',(39.4903196049447,12.4585848001093,-146.55528838444));
#155218=CARTESIAN_POINT('Ctrl Pts',(39.5301458154197,12.452418499751,-146.670335595739));
#155219=CARTESIAN_POINT('Ctrl Pts',(39.5711029864092,12.4464465664109,-146.78136878618));
#155220=CARTESIAN_POINT('Ctrl Pts',(39.6120601573987,12.4404746330708,-146.89240197662));
#155221=CARTESIAN_POINT('Ctrl Pts',(39.6541481889008,12.4346970509066,-146.999421769204));
#155222=CARTESIAN_POINT('Ctrl Pts',(39.697010140157,12.4291022091382,-147.102407485838));
#155223=CARTESIAN_POINT('Ctrl Pts',(39.7351096523847,12.4241290164551,-147.193950345067));
#155224=CARTESIAN_POINT('Ctrl Pts',(39.7738018023959,12.4193428417345,-147.282307078856));
#155225=CARTESIAN_POINT('Ctrl Pts',(39.8128440602613,12.4147562936274,-147.367529588044));
#155226=CARTESIAN_POINT('Ctrl Pts',(39.8618865683454,12.4089949510485,-147.474580917149));
#155227=CARTESIAN_POINT('Ctrl Pts',(39.9114819117157,12.4035479278012,-147.576688885594));
#155228=CARTESIAN_POINT('Ctrl Pts',(39.9611833644274,12.3983649064512,-147.673940637116));
#155229=CARTESIAN_POINT('Ctrl Pts',(39.97083216751,12.3973586993959,-147.692820628519));
#155230=CARTESIAN_POINT('Ctrl Pts',(39.9804850491675,12.3963624584099,-147.711517731987));
#155231=CARTESIAN_POINT('Ctrl Pts',(39.9901388560831,12.3953758384233,-147.730032771159));
#155232=CARTESIAN_POINT('Ctrl Pts',(40.042584448648,12.3900158938656,-147.830618188829));
#155233=CARTESIAN_POINT('Ctrl Pts',(40.0950616995403,12.3849250467423,-147.925821963176));
#155234=CARTESIAN_POINT('Ctrl Pts',(40.1470365111874,12.380085203232,-148.015755916064));
#155235=CARTESIAN_POINT('Ctrl Pts',(40.1539032839609,12.3794457760827,-148.027637748812));
#155236=CARTESIAN_POINT('Ctrl Pts',(40.1607613212998,12.3788107298062,-148.039427662383));
#155237=CARTESIAN_POINT('Ctrl Pts',(40.1676094240942,12.378180022345,-148.051125971627));
#155238=CARTESIAN_POINT('Origin',(0.,-12.9675000200281,-171.64995));
#155239=CARTESIAN_POINT('',(52.4039495302269,12.4224147476539,-171.07256826174));
#155240=CARTESIAN_POINT('',(49.2955572616308,18.0287857662077,-171.07256826174));
#155241=CARTESIAN_POINT('Origin',(0.,-12.9675000200281,-171.07256826174));
#155242=CARTESIAN_POINT('Ctrl Pts',(49.2955572616308,18.0287857662076,-171.07256826174));
#155243=CARTESIAN_POINT('Ctrl Pts',(48.7132630683598,18.0267551266955,-170.013127987308));
#155244=CARTESIAN_POINT('Ctrl Pts',(48.1371153371835,18.0247048552528,-168.969866266346));
#155245=CARTESIAN_POINT('Ctrl Pts',(47.5669953586077,18.0226353122181,-167.942835850289));
#155246=CARTESIAN_POINT('Ctrl Pts',(46.9862239296856,18.0205271042783,-166.896617607296));
#155247=CARTESIAN_POINT('Ctrl Pts',(46.4117077069108,18.0183988996116,-165.86724275765));
#155248=CARTESIAN_POINT('Ctrl Pts',(45.8433676787677,18.0162516178655,-164.854739370262));
#155249=CARTESIAN_POINT('Ctrl Pts',(45.2580605358242,18.0140402315798,-163.812008899861));
#155250=CARTESIAN_POINT('Ctrl Pts',(44.6793039153065,18.0118086131983,-162.787172249637));
#155251=CARTESIAN_POINT('Ctrl Pts',(44.1070591167068,18.0095583137349,-161.78023170509));
#155252=CARTESIAN_POINT('Ctrl Pts',(43.5239608645021,18.0072653340743,-160.754193070863));
#155253=CARTESIAN_POINT('Ctrl Pts',(42.9476239530702,18.004952960289,-159.746735734167));
#155254=CARTESIAN_POINT('Ctrl Pts',(42.3780543128992,18.0026233653842,-158.757834162611));
#155255=CARTESIAN_POINT('Ctrl Pts',(41.7921767666784,18.0002270695668,-157.740618381898));
#155256=CARTESIAN_POINT('Ctrl Pts',(41.2134596804323,17.9978125542456,-156.743036083865));
#155257=CARTESIAN_POINT('Ctrl Pts',(40.641956554655,17.9953827110471,-155.765031415368));
#155258=CARTESIAN_POINT('Ctrl Pts',(40.5622122112717,17.9950436643444,-155.628566124808));
#155259=CARTESIAN_POINT('Ctrl Pts',(40.4826083936333,17.9947043199976,-155.492481965325));
#155260=CARTESIAN_POINT('Ctrl Pts',(40.4031453149964,17.9943646866131,-155.356778744658));
#155261=CARTESIAN_POINT('Ctrl Pts',(40.1676286103913,12.3781782553038,-148.05115874653));
#155262=CARTESIAN_POINT('Ctrl Pts',(40.7369146152135,12.3806129238374,-149.086420661532));
#155263=CARTESIAN_POINT('Ctrl Pts',(41.3145214278423,12.3830242794477,-150.142821070685));
#155264=CARTESIAN_POINT('Ctrl Pts',(41.9004187180735,12.3854095614278,-151.220396408575));
#155265=CARTESIAN_POINT('Ctrl Pts',(42.4720688158783,12.387736840799,-152.271768479359));
#155266=CARTESIAN_POINT('Ctrl Pts',(43.0516112855504,12.3900392971675,-153.343298885691));
#155267=CARTESIAN_POINT('Ctrl Pts',(43.639059311913,12.3923151748205,-154.434995860215));
#155268=CARTESIAN_POINT('Ctrl Pts',(44.2115536547062,12.394533119256,-155.498903327619));
#155269=CARTESIAN_POINT('Ctrl Pts',(44.7915556819794,12.3967258166804,-156.581963045714));
#155270=CARTESIAN_POINT('Ctrl Pts',(45.3791183645239,12.3988924598231,-157.684155326372));
#155271=CARTESIAN_POINT('Ctrl Pts',(45.69458603494,12.4000557499454,-158.275932240494));
#155272=CARTESIAN_POINT('Ctrl Pts',(46.0122339467694,12.401211543745,-158.873224061255));
#155273=CARTESIAN_POINT('Ctrl Pts',(46.3320756406617,12.402359822038,-159.476024489131));
#155274=CARTESIAN_POINT('Ctrl Pts',(46.3403466525113,12.4023895161759,-159.491612730368));
#155275=CARTESIAN_POINT('Ctrl Pts',(46.349506689406,12.4024223895878,-159.508877614243));
#155276=CARTESIAN_POINT('Ctrl Pts',(46.3569477569657,12.4024490777728,-159.522903319776));
#155277=CARTESIAN_POINT('Ctrl Pts',(46.3571037555989,12.4024496372785,-159.523197362381));
#155278=CARTESIAN_POINT('Ctrl Pts',(46.3572589987558,12.4024501940669,-159.52348998131));
#155279=CARTESIAN_POINT('Ctrl Pts',(46.3574134624099,12.4024507480515,-159.523781131265));
#155280=CARTESIAN_POINT('Ctrl Pts',(47.0115330056625,12.4047967511373,-160.756737044912));
#155281=CARTESIAN_POINT('Ctrl Pts',(47.6760241215332,12.4071159777989,-162.015036767565));
#155282=CARTESIAN_POINT('Ctrl Pts',(48.3508610839072,12.4094057510675,-163.298706080169));
#155283=CARTESIAN_POINT('Ctrl Pts',(49.0067945063899,12.411631383184,-164.54641723486));
#155284=CARTESIAN_POINT('Ctrl Pts',(49.6725021575915,12.4138291854533,-165.818096645811));
#155285=CARTESIAN_POINT('Ctrl Pts',(50.3480029624884,12.4159976714344,-167.113744493829));
#155286=CARTESIAN_POINT('Ctrl Pts',(51.0235037673853,12.4181661574155,-168.409392341847));
#155287=CARTESIAN_POINT('Ctrl Pts',(51.7087974034322,12.4203053190432,-169.729008804884));
#155288=CARTESIAN_POINT('Ctrl Pts',(52.4039495302269,12.4224147476539,-171.07256826174));
#155289=CARTESIAN_POINT('Origin',(0.,-12.9675000200281,-170.64995));
#155290=CARTESIAN_POINT('Ctrl Pts',(50.2136602208993,18.26999998,-171.64995));
#155291=CARTESIAN_POINT('Ctrl Pts',(50.0851229429831,18.23650101235,-171.64995));
#155292=CARTESIAN_POINT('Ctrl Pts',(49.9746389296368,18.2070601321017,-171.626166638551));
#155293=CARTESIAN_POINT('Ctrl Pts',(49.8399940956355,18.1718227588537,-171.580545385988));
#155294=CARTESIAN_POINT('Ctrl Pts',(49.8001480569663,18.1614733076846,-171.563607489984));
#155295=CARTESIAN_POINT('Ctrl Pts',(49.7475533787961,18.1478385799374,-171.538010641032));
#155296=CARTESIAN_POINT('Ctrl Pts',(49.7312137127225,18.1436060874251,-171.52944037697));
#155297=CARTESIAN_POINT('Ctrl Pts',(49.7084205773179,18.1376844316008,-171.516772700281));
#155298=CARTESIAN_POINT('Ctrl Pts',(49.6974529329991,18.1348302609285,-171.510485215015));
#155299=CARTESIAN_POINT('Ctrl Pts',(49.6853910445521,18.1316770648567,-171.503278490686));
#155300=CARTESIAN_POINT('Ctrl Pts',(49.6803770252153,18.1303624489092,-171.500222192265));
#155301=CARTESIAN_POINT('Ctrl Pts',(49.6770686640073,18.1294940830886,-171.498192352673));
#155302=CARTESIAN_POINT('Ctrl Pts',(49.6765960425098,18.1293702666764,-171.497905072835));
#155303=CARTESIAN_POINT('Ctrl Pts',(49.4956122808246,18.08175492675,-171.38540529848));
#155304=CARTESIAN_POINT('Ctrl Pts',(49.3699326913236,18.0484851821909,-171.23007999248));
#155305=CARTESIAN_POINT('Ctrl Pts',(49.2955572616308,18.0287857662077,-171.07256826174));
#155306=CARTESIAN_POINT('',(52.5103993912271,12.4456688534684,-171.249463176903));
#155307=CARTESIAN_POINT('Origin',(53.2802565113079,12.6131588410718,-170.642164399514));
#155308=CARTESIAN_POINT('',(52.1126146143195,13.5388501432916,-171.391638125813));
#155309=CARTESIAN_POINT('Ctrl Pts',(52.5103994272594,12.4456688709067,-171.249463146917));
#155310=CARTESIAN_POINT('Ctrl Pts',(52.4789249293047,12.5214873830577,-171.255734050496));
#155311=CARTESIAN_POINT('Ctrl Pts',(52.4475912597577,12.5988603052281,-171.263156330074));
#155312=CARTESIAN_POINT('Ctrl Pts',(52.4165030218133,12.6778243900594,-171.271682853797));
#155313=CARTESIAN_POINT('Ctrl Pts',(52.387020598463,12.7527097078642,-171.279768953194));
#155314=CARTESIAN_POINT('Ctrl Pts',(52.3577589616042,12.8290260178364,-171.288848248172));
#155315=CARTESIAN_POINT('Ctrl Pts',(52.3288066421888,12.9068196706831,-171.298836409739));
#155316=CARTESIAN_POINT('Ctrl Pts',(52.3006266608301,12.9825380839679,-171.308558125043));
#155317=CARTESIAN_POINT('Ctrl Pts',(52.2727397648527,13.0596559839818,-171.319141098433));
#155318=CARTESIAN_POINT('Ctrl Pts',(52.2452261612323,13.1382317037553,-171.330462085915));
#155319=CARTESIAN_POINT('Ctrl Pts',(52.2187662336855,13.2137982446139,-171.341349518645));
#155320=CARTESIAN_POINT('Ctrl Pts',(52.1926515942531,13.2907130439262,-171.352919627189));
#155321=CARTESIAN_POINT('Ctrl Pts',(52.1669516021167,13.3690434713394,-171.365017856694));
#155322=CARTESIAN_POINT('Ctrl Pts',(52.1486202360554,13.4249152292384,-171.373647317457));
#155323=CARTESIAN_POINT('Ctrl Pts',(52.1304997930493,13.4815075305005,-171.382544571252));
#155324=CARTESIAN_POINT('Ctrl Pts',(52.1126146143195,13.5388501432916,-171.391638125813));
#155325=CARTESIAN_POINT('Ctrl Pts',(52.1126146143195,13.5388501432916,-171.391638125814));
#155326=CARTESIAN_POINT('Ctrl Pts',(52.0803920632866,13.6421605599748,-171.408021385403));
#155327=CARTESIAN_POINT('Ctrl Pts',(52.0443154341228,13.7573997650724,-171.425325387943));
#155328=CARTESIAN_POINT('Ctrl Pts',(52.0042475791589,13.8846776632875,-171.442931430639));
#155329=CARTESIAN_POINT('Ctrl Pts',(51.9673088889449,14.0020155856068,-171.459162500599));
#155330=CARTESIAN_POINT('Ctrl Pts',(51.926977620903,14.1295858261524,-171.475647125295));
#155331=CARTESIAN_POINT('Ctrl Pts',(51.8831362090135,14.2674563385285,-171.491883525028));
#155332=CARTESIAN_POINT('Ctrl Pts',(51.8417138631109,14.3977194803224,-171.507224038415));
#155333=CARTESIAN_POINT('Ctrl Pts',(51.7971595353686,14.5371723996994,-171.522339825733));
#155334=CARTESIAN_POINT('Ctrl Pts',(51.7493757816615,14.6858287519608,-171.536828313229));
#155335=CARTESIAN_POINT('Ctrl Pts',(51.7077663335838,14.8152766979877,-171.549444692676));
#155336=CARTESIAN_POINT('Ctrl Pts',(51.6637081429747,14.9517026484988,-171.561584593079));
#155337=CARTESIAN_POINT('Ctrl Pts',(51.617135700075,15.0950969115951,-171.57301932221));
#155338=CARTESIAN_POINT('Ctrl Pts',(51.6010267119545,15.144695694415,-171.576974491925));
#155339=CARTESIAN_POINT('Ctrl Pts',(51.584616911503,15.1951280068941,-171.580845702717));
#155340=CARTESIAN_POINT('Ctrl Pts',(51.5679035198677,15.2463930815758,-171.584624968275));
#155341=CARTESIAN_POINT('Ctrl Pts',(51.5659904551147,15.2522610352249,-171.585057554304));
#155342=CARTESIAN_POINT('Ctrl Pts',(51.5645241366347,15.2567580002418,-171.58538800781));
#155343=CARTESIAN_POINT('Ctrl Pts',(51.5621523934156,15.2640296730528,-171.585919105761));
#155344=CARTESIAN_POINT('Ctrl Pts',(51.5620922592179,15.264214042173,-171.585932571447));
#155345=CARTESIAN_POINT('Ctrl Pts',(51.5620321292168,15.2643983974826,-171.585946034188));
#155346=CARTESIAN_POINT('Ctrl Pts',(51.5619720034126,15.2645827389817,-171.585959493986));
#155347=CARTESIAN_POINT('Ctrl Pts',(51.5100296192924,15.4238344458647,-171.597587346801));
#155348=CARTESIAN_POINT('Ctrl Pts',(51.4612187298276,15.5727959713245,-171.606956492029));
#155349=CARTESIAN_POINT('Ctrl Pts',(51.4156249289144,15.7114071757297,-171.614568164852));
#155350=CARTESIAN_POINT('Ctrl Pts',(51.370285212554,15.8492459293811,-171.62213741944));
#155351=CARTESIAN_POINT('Ctrl Pts',(51.3281260757772,15.9768490948217,-171.627969257248));
#155352=CARTESIAN_POINT('Ctrl Pts',(51.2891960739576,16.0941513344784,-171.632521761146));
#155353=CARTESIAN_POINT('Ctrl Pts',(51.2529325860679,16.2034189468185,-171.636762440885));
#155354=CARTESIAN_POINT('Ctrl Pts',(51.2194703342734,16.3037482407608,-171.639893258602));
#155355=CARTESIAN_POINT('Ctrl Pts',(51.1888281668638,16.3950846110292,-171.642249337767));
#155356=CARTESIAN_POINT('Ctrl Pts',(51.1597260909545,16.4818303671407,-171.644486999149));
#155357=CARTESIAN_POINT('Ctrl Pts',(51.1332014685273,16.5604778447485,-171.646031796051));
#155358=CARTESIAN_POINT('Ctrl Pts',(51.1093286900604,16.6310287376919,-171.647132271588));
#155359=CARTESIAN_POINT('Ctrl Pts',(51.0855300937576,16.701360401109,-171.648229327512));
#155360=CARTESIAN_POINT('Ctrl Pts',(51.0643670215595,16.7636457950945,-171.648884851425));
#155361=CARTESIAN_POINT('Ctrl Pts',(51.0459071806312,16.8178871170319,-171.649293646808));
#155362=CARTESIAN_POINT('Ctrl Pts',(51.0273959299895,16.8722794982784,-171.649703580665));
#155363=CARTESIAN_POINT('Ctrl Pts',(51.0116030939921,16.9185829775746,-171.649865392466));
#155364=CARTESIAN_POINT('Ctrl Pts',(50.9985891037783,16.9567994635462,-171.649923556513));
#155365=CARTESIAN_POINT('Ctrl Pts',(50.9943621183234,16.9692122998618,-171.649942448381));
#155366=CARTESIAN_POINT('Ctrl Pts',(50.9904282251185,16.9807719773071,-171.64995));
#155367=CARTESIAN_POINT('Ctrl Pts',(50.9867892914963,16.9914785469432,-171.64995));
#155368=CARTESIAN_POINT('Origin',(0.,-12.9675000200281,-171.64995));
#155369=CARTESIAN_POINT('',(50.4557527353536,20.76999998,-171.64995));
#155370=CARTESIAN_POINT('',(49.6616970192851,26.41999998,-171.64995));
#155371=CARTESIAN_POINT('',(49.6109861057109,26.78082687904,-171.64995));
#155372=CARTESIAN_POINT('',(44.1114262156583,26.41999998,-171.64995));
#155373=CARTESIAN_POINT('',(43.6598261881496,26.41999998,-171.64995));
#155374=CARTESIAN_POINT('',(48.5692718988023,20.76999998,-171.64995));
#155375=CARTESIAN_POINT('Origin',(0.,-12.9675000200281,-171.64995));
#155376=CARTESIAN_POINT('',(50.5260231527048,20.76999998,-171.64995));
#155377=CARTESIAN_POINT('Origin',(0.,-12.9675000200281,-170.64995));
#155378=CARTESIAN_POINT('',(43.1661128544364,26.1158519257145,-171.07256826174));
#155379=CARTESIAN_POINT('Ctrl Pts',(44.1114262156583,26.41999998,-171.64995));
#155380=CARTESIAN_POINT('Ctrl Pts',(44.0862354544475,26.4119589516213,-171.64995));
#155381=CARTESIAN_POINT('Ctrl Pts',(44.062424087661,26.4043528118249,-171.649077188494));
#155382=CARTESIAN_POINT('Ctrl Pts',(44.0400096738348,26.3971890622453,-171.647602355793));
#155383=CARTESIAN_POINT('Ctrl Pts',(44.0325064360514,26.3947909929969,-171.647108654707));
#155384=CARTESIAN_POINT('Ctrl Pts',(44.0251594468187,26.3924424007436,-171.646547173762));
#155385=CARTESIAN_POINT('Ctrl Pts',(44.0179685608018,26.3901433003913,-171.645927118434));
#155386=CARTESIAN_POINT('Ctrl Pts',(43.9954109094669,26.3829310731345,-171.643982018503));
#155387=CARTESIAN_POINT('Ctrl Pts',(43.9743934989977,26.3762072089724,-171.641463268277));
#155388=CARTESIAN_POINT('Ctrl Pts',(43.9549327642172,26.3699786174128,-171.638633940813));
#155389=CARTESIAN_POINT('Ctrl Pts',(43.9350172655692,26.3636044743919,-171.635738496838));
#155390=CARTESIAN_POINT('Ctrl Pts',(43.9167355998369,26.3577501595336,-171.63251895689));
#155391=CARTESIAN_POINT('Ctrl Pts',(43.900061978668,26.3524088423955,-171.629213691978));
#155392=CARTESIAN_POINT('Ctrl Pts',(43.8823343709119,26.3467298855471,-171.625699491956));
#155393=CARTESIAN_POINT('Ctrl Pts',(43.8664272902322,26.3416317152979,-171.622089275396));
#155394=CARTESIAN_POINT('Ctrl Pts',(43.8523110704409,26.337106169398,-171.618620938174));
#155395=CARTESIAN_POINT('Ctrl Pts',(43.8473291598941,26.335509009168,-171.617396889099));
#155396=CARTESIAN_POINT('Ctrl Pts',(43.8425702599821,26.3339831528831,-171.616190046819));
#155397=CARTESIAN_POINT('Ctrl Pts',(43.8380328957014,26.3325281766859,-171.615009325804));
#155398=CARTESIAN_POINT('Ctrl Pts',(43.8361555194993,26.3319261669027,-171.614520791625));
#155399=CARTESIAN_POINT('Ctrl Pts',(43.834316044768,26.3313369484831,-171.614036835203));
#155400=CARTESIAN_POINT('Ctrl Pts',(43.8325143893445,26.3307598347951,-171.613557935536));
#155401=CARTESIAN_POINT('Ctrl Pts',(43.8310448450428,26.3302891043099,-171.613167314628));
#155402=CARTESIAN_POINT('Ctrl Pts',(43.8306220292784,26.3301538547414,-171.613054933854));
#155403=CARTESIAN_POINT('Ctrl Pts',(43.8287460529606,26.3295522868089,-171.61254888948));
#155404=CARTESIAN_POINT('Ctrl Pts',(43.8283220898321,26.3294163348674,-171.61243452548));
#155405=CARTESIAN_POINT('Ctrl Pts',(43.8278239364058,26.3292565744529,-171.612299893551));
#155406=CARTESIAN_POINT('Ctrl Pts',(43.8272228179699,26.3290637741874,-171.612136790524));
#155407=CARTESIAN_POINT('Ctrl Pts',(43.7945831106783,26.3185950481281,-171.603280573905));
#155408=CARTESIAN_POINT('Ctrl Pts',(43.7634524938468,26.3086018031985,-171.593184647393));
#155409=CARTESIAN_POINT('Ctrl Pts',(43.7338613831768,26.2990964255035,-171.582169375343));
#155410=CARTESIAN_POINT('Ctrl Pts',(43.7161500744003,26.2934071264004,-171.575576351961));
#155411=CARTESIAN_POINT('Ctrl Pts',(43.6989893210903,26.287892288612,-171.568653540263));
#155412=CARTESIAN_POINT('Ctrl Pts',(43.682378199249,26.2825521351849,-171.561465632265));
#155413=CARTESIAN_POINT('Ctrl Pts',(43.6621217355773,26.2760400750766,-171.55270032438));
#155414=CARTESIAN_POINT('Ctrl Pts',(43.6426836268837,26.2697877829703,-171.543541205931));
#155415=CARTESIAN_POINT('Ctrl Pts',(43.6240553138662,26.2637931585035,-171.534100818898));
#155416=CARTESIAN_POINT('Ctrl Pts',(43.6118890679869,26.2598780388064,-171.52793525416));
#155417=CARTESIAN_POINT('Ctrl Pts',(43.6000684354351,26.2560728887536,-171.521649806639));
#155418=CARTESIAN_POINT('Ctrl Pts',(43.5885882565054,26.2523762161258,-171.515273953786));
#155419=CARTESIAN_POINT('Ctrl Pts',(43.5858376819236,26.2514905179298,-171.513746341812));
#155420=CARTESIAN_POINT('Ctrl Pts',(43.5831063120073,26.2506109376294,-171.512213345091));
#155421=CARTESIAN_POINT('Ctrl Pts',(43.58039516952,26.2497378068516,-171.510675985829));
#155422=CARTESIAN_POINT('Ctrl Pts',(43.5785452743591,26.249142043107,-171.509626998742));
#155423=CARTESIAN_POINT('Ctrl Pts',(43.5767041725523,26.2485490825943,-171.508575561719));
#155424=CARTESIAN_POINT('Ctrl Pts',(43.5748722248338,26.2479590424451,-171.507522020905));
#155425=CARTESIAN_POINT('Ctrl Pts',(43.5718287594684,26.246978792441,-171.505771744438));
#155426=CARTESIAN_POINT('Ctrl Pts',(43.5693369349477,26.2461761716096,-171.504322744292));
#155427=CARTESIAN_POINT('Ctrl Pts',(43.5663723957617,26.2452212663088,-171.502580705527));
#155428=CARTESIAN_POINT('Ctrl Pts',(43.5647615530418,26.2447023990733,-171.501634133298));
#155429=CARTESIAN_POINT('Ctrl Pts',(43.5630113134971,26.2441386224429,-171.50060039331));
#155430=CARTESIAN_POINT('Ctrl Pts',(43.5609591548336,26.243477566168,-171.499377888939));
#155431=CARTESIAN_POINT('Ctrl Pts',(43.5328624030456,26.2344268361218,-171.482640195843));
#155432=CARTESIAN_POINT('Ctrl Pts',(43.5058766871946,26.2257272700079,-171.464782106444));
#155433=CARTESIAN_POINT('Ctrl Pts',(43.4801111596735,26.2174158381575,-171.445999348312));
#155434=CARTESIAN_POINT('Ctrl Pts',(43.4531619571471,26.2087225769759,-171.426353705408));
#155435=CARTESIAN_POINT('Ctrl Pts',(43.4275474816989,26.2004538833673,-171.405696571767));
#155436=CARTESIAN_POINT('Ctrl Pts',(43.4033381150423,26.1926341561568,-171.384240314257));
#155437=CARTESIAN_POINT('Ctrl Pts',(43.3837824064608,26.1863175800693,-171.366908496987));
#155438=CARTESIAN_POINT('Ctrl Pts',(43.365142364827,26.1802935715868,-171.349055028029));
#155439=CARTESIAN_POINT('Ctrl Pts',(43.3474322736918,26.1745674931452,-171.330786171197));
#155440=CARTESIAN_POINT('Ctrl Pts',(43.3226113547606,26.1665423210721,-171.305182135005));
#155441=CARTESIAN_POINT('Ctrl Pts',(43.2997031859874,26.1591304014692,-171.278951913314));
#155442=CARTESIAN_POINT('Ctrl Pts',(43.2786212075764,26.1523059918628,-171.252199761598));
#155443=CARTESIAN_POINT('Ctrl Pts',(43.2554014801638,26.1447895753422,-171.222734895519));
#155444=CARTESIAN_POINT('Ctrl Pts',(43.2343969539159,26.1379858217079,-171.192637063565));
#155445=CARTESIAN_POINT('Ctrl Pts',(43.2154467008627,26.1318449539662,-171.162094734958));
#155446=CARTESIAN_POINT('Ctrl Pts',(43.1971455897184,26.12591444197,-171.132598635414));
#155447=CARTESIAN_POINT('Ctrl Pts',(43.1807594970827,26.1206018686274,-171.102689012713));
#155448=CARTESIAN_POINT('Ctrl Pts',(43.1661128544364,26.1158519257145,-171.07256826174));
#155449=CARTESIAN_POINT('',(47.6457075325507,20.5094809071607,-171.07256826174));
#155450=CARTESIAN_POINT('Origin',(0.,-12.9675000200281,-171.07256826174));
#155451=CARTESIAN_POINT('Ctrl Pts',(47.6457075325506,20.5094809071606,-171.072568261741));
#155452=CARTESIAN_POINT('Ctrl Pts',(47.6608054793214,20.5137743424238,-171.104353673586));
#155453=CARTESIAN_POINT('Ctrl Pts',(47.6779305040385,20.5186086512811,-171.135995650035));
#155454=CARTESIAN_POINT('Ctrl Pts',(47.6971672417547,20.5240387499795,-171.167206713736));
#155455=CARTESIAN_POINT('Ctrl Pts',(47.7160784704467,20.5293769647964,-171.197889648237));
#155456=CARTESIAN_POINT('Ctrl Pts',(47.7370309269822,20.5352912371008,-171.228155855593));
#155457=CARTESIAN_POINT('Ctrl Pts',(47.7600754969573,20.5418118265715,-171.257699199741));
#155458=CARTESIAN_POINT('Ctrl Pts',(47.7825293088982,20.548165257765,-171.286485186822));
#155459=CARTESIAN_POINT('Ctrl Pts',(47.8069696244586,20.5550945051755,-171.314584515203));
#155460=CARTESIAN_POINT('Ctrl Pts',(47.8334105302321,20.5626033659202,-171.341687271229));
#155461=CARTESIAN_POINT('Ctrl Pts',(47.8549943997946,20.568732893867,-171.363811413112));
#155462=CARTESIAN_POINT('Ctrl Pts',(47.8779108659171,20.5752482720292,-171.385270896185));
#155463=CARTESIAN_POINT('Ctrl Pts',(47.9021486191345,20.5821377906669,-171.405886271163));
#155464=CARTESIAN_POINT('Ctrl Pts',(47.9213820600628,20.5876048464848,-171.422245237825));
#155465=CARTESIAN_POINT('Ctrl Pts',(47.9414471996244,20.5933072712984,-171.438072451705));
#155466=CARTESIAN_POINT('Ctrl Pts',(47.9623296966163,20.5992329574236,-171.453274815853));
#155467=CARTESIAN_POINT('Ctrl Pts',(47.9727709451122,20.6021958004862,-171.460875997927));
#155468=CARTESIAN_POINT('Ctrl Pts',(47.9834165059242,20.6052144399543,-171.468321013392));
#155469=CARTESIAN_POINT('Ctrl Pts',(47.9942636985228,20.6082867262198,-171.475597912193));
#155470=CARTESIAN_POINT('Ctrl Pts',(47.9996872948221,20.6098228693525,-171.479236361594));
#155471=CARTESIAN_POINT('Ctrl Pts',(48.0051612966878,20.6113724225186,-171.482832785671));
#155472=CARTESIAN_POINT('Ctrl Pts',(48.0106853331332,20.6129350916101,-171.486385694791));
#155473=CARTESIAN_POINT('Ctrl Pts',(48.0142592323965,20.613946095424,-171.488684329026));
#155474=CARTESIAN_POINT('Ctrl Pts',(48.0183353267973,20.6150974528436,-171.49126815362));
#155475=CARTESIAN_POINT('Ctrl Pts',(48.0219806198629,20.6161281188114,-171.493545641964));
#155476=CARTESIAN_POINT('Ctrl Pts',(48.0239697138534,20.6166905129581,-171.494788378364));
#155477=CARTESIAN_POINT('Ctrl Pts',(48.0258300378168,20.6172166329018,-171.495940836679));
#155478=CARTESIAN_POINT('Ctrl Pts',(48.0274071543696,20.617662137765,-171.496912392695));
#155479=CARTESIAN_POINT('Ctrl Pts',(48.0507475253393,20.6242553402511,-171.511290834034));
#155480=CARTESIAN_POINT('Ctrl Pts',(48.0756840369207,20.6312829116219,-171.525353615259));
#155481=CARTESIAN_POINT('Ctrl Pts',(48.1022649324158,20.6387735189811,-171.538797793285));
#155482=CARTESIAN_POINT('Ctrl Pts',(48.127917677585,20.6460025697022,-171.551772528201));
#155483=CARTESIAN_POINT('Ctrl Pts',(48.155102381514,20.6536631594268,-171.56417076011));
#155484=CARTESIAN_POINT('Ctrl Pts',(48.1838328927653,20.6617597777488,-171.575687929238));
#155485=CARTESIAN_POINT('Ctrl Pts',(48.193709004373,20.6645429898362,-171.57964695547));
#155486=CARTESIAN_POINT('Ctrl Pts',(48.2037674836592,20.6673775162118,-171.58350160808));
#155487=CARTESIAN_POINT('Ctrl Pts',(48.2140079119365,20.6702628383739,-171.587238716541));
#155488=CARTESIAN_POINT('Ctrl Pts',(48.2258244062378,20.6735922296808,-171.59155098939));
#155489=CARTESIAN_POINT('Ctrl Pts',(48.2378831914308,20.6769892737823,-171.595706763012));
#155490=CARTESIAN_POINT('Ctrl Pts',(48.2501826687628,20.6804524954123,-171.599685179414));
#155491=CARTESIAN_POINT('Ctrl Pts',(48.2563324074288,20.6821841062273,-171.601674387615));
#155492=CARTESIAN_POINT('Ctrl Pts',(48.2625423199986,20.6839322620305,-171.603619253238));
#155493=CARTESIAN_POINT('Ctrl Pts',(48.2688120843098,20.6856966917931,-171.605517102748));
#155494=CARTESIAN_POINT('Ctrl Pts',(48.2719469664653,20.6865789066744,-171.606466027504));
#155495=CARTESIAN_POINT('Ctrl Pts',(48.2750968115901,20.6874651900693,-171.60740319812));
#155496=CARTESIAN_POINT('Ctrl Pts',(48.2782615753499,20.6883555052367,-171.608328278083));
#155497=CARTESIAN_POINT('Ctrl Pts',(48.2806789487674,20.6890355636495,-171.609034891241));
#155498=CARTESIAN_POINT('Ctrl Pts',(48.2839466163799,20.6899543743648,-171.609974943678));
#155499=CARTESIAN_POINT('Ctrl Pts',(48.2861362745438,20.6905703569427,-171.610596209647));
#155500=CARTESIAN_POINT('Ctrl Pts',(48.2868132611247,20.69076080308,-171.610788289274));
#155501=CARTESIAN_POINT('Ctrl Pts',(48.2873870926172,20.6909222321912,-171.610950345128));
#155502=CARTESIAN_POINT('Ctrl Pts',(48.2878005760434,20.6910385077935,-171.611066908152));
#155503=CARTESIAN_POINT('Ctrl Pts',(48.2998125318058,20.6944163877819,-171.614453137937));
#155504=CARTESIAN_POINT('Ctrl Pts',(48.3135201354276,20.6982563100554,-171.618084608787));
#155505=CARTESIAN_POINT('Ctrl Pts',(48.3289584082396,20.7025797409342,-171.621757482605));
#155506=CARTESIAN_POINT('Ctrl Pts',(48.3440560181388,20.7068077704313,-171.625349310317));
#155507=CARTESIAN_POINT('Ctrl Pts',(48.3608093202089,20.7114985927589,-171.628980616122));
#155508=CARTESIAN_POINT('Ctrl Pts',(48.3792439438551,20.7166665888665,-171.632412351309));
#155509=CARTESIAN_POINT('Ctrl Pts',(48.3973413375453,20.7217400453114,-171.63578130876));
#155510=CARTESIAN_POINT('Ctrl Pts',(48.4170597039694,20.7272737927182,-171.638957768871));
#155511=CARTESIAN_POINT('Ctrl Pts',(48.4384078208194,20.7332699884129,-171.641670360648));
#155512=CARTESIAN_POINT('Ctrl Pts',(48.4590004972892,20.7390539982559,-171.644286962629));
#155513=CARTESIAN_POINT('Ctrl Pts',(48.4811101375688,20.7452686573897,-171.646471581729));
#155514=CARTESIAN_POINT('Ctrl Pts',(48.5047220649505,20.7518996505501,-171.647942204836));
#155515=CARTESIAN_POINT('Ctrl Pts',(48.5251264176098,20.7576298529491,-171.649213050372));
#155516=CARTESIAN_POINT('Ctrl Pts',(48.5466525424873,20.7636708901536,-171.64995));
#155517=CARTESIAN_POINT('Ctrl Pts',(48.5692718988023,20.76999998,-171.64995));
#155518=CARTESIAN_POINT('Origin',(0.,-12.9675000200281,-171.64995));
#155519=CARTESIAN_POINT('',(40.7299248988704,26.1062891840346,-167.236334624234));
#155520=CARTESIAN_POINT('Ctrl Pts',(43.1661128544364,26.1158519257145,-171.07256826174));
#155521=CARTESIAN_POINT('Ctrl Pts',(42.3615449736022,26.1127499922191,-169.789073851883));
#155522=CARTESIAN_POINT('Ctrl Pts',(41.5498582787394,26.1095640229222,-168.510069248237));
#155523=CARTESIAN_POINT('Ctrl Pts',(40.7299249439363,26.1062890581356,-167.236334669465));
#155524=CARTESIAN_POINT('',(40.5057713939776,20.481582219525,-158.850240721809));
#155525=CARTESIAN_POINT('Ctrl Pts',(40.7299249270775,26.1062893712214,-167.236334458579));
#155526=CARTESIAN_POINT('Ctrl Pts',(40.7128753097134,25.6648631996692,-166.554593295561));
#155527=CARTESIAN_POINT('Ctrl Pts',(40.6957961482183,25.2264331174374,-165.882453706378));
#155528=CARTESIAN_POINT('Ctrl Pts',(40.6787028125346,24.7909199131761,-165.220009030196));
#155529=CARTESIAN_POINT('Ctrl Pts',(40.6609759030339,24.3392641742899,-164.533010480519));
#155530=CARTESIAN_POINT('Ctrl Pts',(40.6432337524935,23.8907456085251,-163.856438781572));
#155531=CARTESIAN_POINT('Ctrl Pts',(40.6254919034664,23.4452850207497,-163.190342549082));
#155532=CARTESIAN_POINT('Ctrl Pts',(40.607340392364,22.9895386781693,-162.508866050162));
#155533=CARTESIAN_POINT('Ctrl Pts',(40.589189196447,22.5369932474311,-161.838354137871));
#155534=CARTESIAN_POINT('Ctrl Pts',(40.5710532970034,22.0875722018093,-161.178804354429));
#155535=CARTESIAN_POINT('Ctrl Pts',(40.5522933111462,21.6226858317652,-160.496558367787));
#155536=CARTESIAN_POINT('Ctrl Pts',(40.5335496951665,21.1611426591172,-159.826041783126));
#155537=CARTESIAN_POINT('Ctrl Pts',(40.5148372507287,20.7028654660488,-159.167197042055));
#155538=CARTESIAN_POINT('Ctrl Pts',(40.5118264342186,20.6291290526335,-159.061189479517));
#155539=CARTESIAN_POINT('Ctrl Pts',(40.5088164210288,20.5554772043327,-158.955483975447));
#155540=CARTESIAN_POINT('Ctrl Pts',(40.5058072686407,20.4819096145309,-158.850080167922));
#155541=CARTESIAN_POINT('Ctrl Pts',(40.5058324224781,20.4814581622042,-158.850394545255));
#155542=CARTESIAN_POINT('Ctrl Pts',(41.0748559880981,20.4838558671134,-159.794595142241));
#155543=CARTESIAN_POINT('Ctrl Pts',(41.6503757590613,20.4862411501968,-160.757331383121));
#155544=CARTESIAN_POINT('Ctrl Pts',(42.2323582161204,20.488611368542,-161.738653725408));
#155545=CARTESIAN_POINT('Ctrl Pts',(42.7807997999503,20.4908449862182,-162.663420396849));
#155546=CARTESIAN_POINT('Ctrl Pts',(43.3349807509714,20.49306522617,-163.604692509208));
#155547=CARTESIAN_POINT('Ctrl Pts',(43.8949153576922,20.4952702209769,-164.562486402209));
#155548=CARTESIAN_POINT('Ctrl Pts',(44.4451875767377,20.4974371657787,-165.503752336773));
#155549=CARTESIAN_POINT('Ctrl Pts',(45.0010164490219,20.4995893855044,-166.460974849504));
#155550=CARTESIAN_POINT('Ctrl Pts',(45.5624581798033,20.5017254605505,-167.434143383494));
#155551=CARTESIAN_POINT('Ctrl Pts',(46.1111612276046,20.5038130696894,-168.385231468596));
#155552=CARTESIAN_POINT('Ctrl Pts',(46.6652252369269,20.5058852574484,-169.35155022864));
#155553=CARTESIAN_POINT('Ctrl Pts',(47.2247453462289,20.5079410566878,-170.333063732337));
#155554=CARTESIAN_POINT('Ctrl Pts',(47.3647237291413,20.5084553678775,-170.578614644217));
#155555=CARTESIAN_POINT('Ctrl Pts',(47.5050438144344,20.5089686551722,-170.825116431323));
#155556=CARTESIAN_POINT('Ctrl Pts',(47.6457075325507,20.5094809071607,-171.07256826174));
#155557=CARTESIAN_POINT('Ctrl Pts',(40.731736456874,26.153205299378,-167.30881038206));
#155558=CARTESIAN_POINT('Ctrl Pts',(39.,27.3939818557438,-166.473551654334));
#155559=CARTESIAN_POINT('Ctrl Pts',(39.,29.2922017208088,-165.195719073356));
#155560=CARTESIAN_POINT('Ctrl Pts',(40.6299762644379,23.5169690803201,-163.235292522563));
#155561=CARTESIAN_POINT('Ctrl Pts',(39.,24.7554502365011,-162.409295569182));
#155562=CARTESIAN_POINT('Ctrl Pts',(39.,26.5499900188717,-161.122164521183));
#155563=CARTESIAN_POINT('Ctrl Pts',(40.5197424781718,20.796012087217,-159.207512241208));
#155564=CARTESIAN_POINT('Ctrl Pts',(39.,22.0110917831,-158.367042514669));
#155565=CARTESIAN_POINT('Ctrl Pts',(39.,23.7045860616975,-157.09431111324));
#155566=CARTESIAN_POINT('Ctrl Pts',(40.4018086326459,17.9622435375657,-155.312616930242));
#155567=CARTESIAN_POINT('Ctrl Pts',(39.,19.1149982856394,-154.428325504224));
#155568=CARTESIAN_POINT('Ctrl Pts',(39.,20.7168513145423,-153.199525621538));
#155569=CARTESIAN_POINT('',(39.,26.4199999800005,-161.0070032805));
#155570=CARTESIAN_POINT('Ctrl Pts',(40.7299249051676,26.1062890609606,-167.236334613664));
#155571=CARTESIAN_POINT('Ctrl Pts',(40.6655599724143,26.1109551454916,-167.143655159795));
#155572=CARTESIAN_POINT('Ctrl Pts',(40.6012807827827,26.1158462415184,-167.04650897417));
#155573=CARTESIAN_POINT('Ctrl Pts',(40.537493215085,26.1209674811084,-166.944795556906));
#155574=CARTESIAN_POINT('Ctrl Pts',(40.4777242273763,26.1257660855567,-166.849490026288));
#155575=CARTESIAN_POINT('Ctrl Pts',(40.4183871223425,26.1307667543264,-166.750174501842));
#155576=CARTESIAN_POINT('Ctrl Pts',(40.3597727647597,26.1359727718707,-166.646784924028));
#155577=CARTESIAN_POINT('Ctrl Pts',(40.3479006562068,26.1370272303339,-166.625843769989));
#155578=CARTESIAN_POINT('Ctrl Pts',(40.3360580421242,26.1380901098204,-166.604735545593));
#155579=CARTESIAN_POINT('Ctrl Pts',(40.3242470923055,26.1391614322574,-166.583459825004));
#155580=CARTESIAN_POINT('Ctrl Pts',(40.2707276546541,26.144015959222,-166.487052286319));
#155581=CARTESIAN_POINT('Ctrl Pts',(40.2178676814488,26.149043399969,-166.387213933017));
#155582=CARTESIAN_POINT('Ctrl Pts',(40.1658599746533,26.1542433904085,-166.283952280357));
#155583=CARTESIAN_POINT('Ctrl Pts',(40.1156927673743,26.1592593585082,-166.184344951902));
#155584=CARTESIAN_POINT('Ctrl Pts',(40.0663183755085,26.1644359186199,-166.081551558006));
#155585=CARTESIAN_POINT('Ctrl Pts',(40.0178686966096,26.1697714290785,-165.975604902816));
#155586=CARTESIAN_POINT('Ctrl Pts',(39.9942719299905,26.1723700179225,-165.924005004665));
#155587=CARTESIAN_POINT('Ctrl Pts',(39.970893821805,26.1750062938622,-165.871657468398));
#155588=CARTESIAN_POINT('Ctrl Pts',(39.947745464702,26.1776799753113,-165.818567904404));
#155589=CARTESIAN_POINT('Ctrl Pts',(39.9458414957153,26.1778998875296,-165.81420124966));
#155590=CARTESIAN_POINT('Ctrl Pts',(39.9434731024443,26.1781740861158,-165.808756672598));
#155591=CARTESIAN_POINT('Ctrl Pts',(39.9420381705474,26.1783405694635,-165.805452905768));
#155592=CARTESIAN_POINT('Ctrl Pts',(39.9396836723283,26.1786137425294,-165.800031942491));
#155593=CARTESIAN_POINT('Ctrl Pts',(39.9373283981638,26.1788876628891,-165.794595981622));
#155594=CARTESIAN_POINT('Ctrl Pts',(39.9349723995142,26.1791623310232,-165.789145019958));
#155595=CARTESIAN_POINT('Ctrl Pts',(39.8799745860375,26.1855741117791,-165.661899203024));
#155596=CARTESIAN_POINT('Ctrl Pts',(39.8246694294618,26.1923956775984,-165.526432930152));
#155597=CARTESIAN_POINT('Ctrl Pts',(39.7698978587332,26.1996375838493,-165.38261840114));
#155598=CARTESIAN_POINT('Ctrl Pts',(39.7354995937025,26.2041857282102,-165.292298364332));
#155599=CARTESIAN_POINT('Ctrl Pts',(39.7013112109897,26.208899657812,-165.198685786783));
#155600=CARTESIAN_POINT('Ctrl Pts',(39.6675307141268,26.2137818117656,-165.101752901681));
#155601=CARTESIAN_POINT('Ctrl Pts',(39.6585869831338,26.2150744118065,-165.076088931958));
#155602=CARTESIAN_POINT('Ctrl Pts',(39.6496737175069,26.2163784633357,-165.050197692129));
#155603=CARTESIAN_POINT('Ctrl Pts',(39.6407939407845,26.2176940491621,-165.024077536311));
#155604=CARTESIAN_POINT('Ctrl Pts',(39.6156806967495,26.2214147089198,-164.9502061015));
#155605=CARTESIAN_POINT('Ctrl Pts',(39.5908206081619,26.2252310634679,-164.874435432396));
#155606=CARTESIAN_POINT('Ctrl Pts',(39.5663133697914,26.2291410756515,-164.796805863973));
#155607=CARTESIAN_POINT('Ctrl Pts',(39.5524797752985,26.2313481592157,-164.7529863216));
#155608=CARTESIAN_POINT('Ctrl Pts',(39.53875962603,26.2335849133149,-164.708577884265));
#155609=CARTESIAN_POINT('Ctrl Pts',(39.5251684492104,26.2358513676767,-164.663579935738));
#155610=CARTESIAN_POINT('Ctrl Pts',(39.4871369769279,26.2421934672154,-164.537664552922));
#155611=CARTESIAN_POINT('Ctrl Pts',(39.4501045438397,26.2487694405955,-164.407107098214));
#155612=CARTESIAN_POINT('Ctrl Pts',(39.4144495932088,26.2555781438501,-164.271929512584));
#155613=CARTESIAN_POINT('Ctrl Pts',(39.4131963919402,26.2558174563553,-164.267178286771));
#155614=CARTESIAN_POINT('Ctrl Pts',(39.411617445666,26.2561199480258,-164.261173555401));
#155615=CARTESIAN_POINT('Ctrl Pts',(39.4106951136031,26.2562969839952,-164.257658721375));
#155616=CARTESIAN_POINT('Ctrl Pts',(39.4088599785172,26.2566492268935,-164.250665366703));
#155617=CARTESIAN_POINT('Ctrl Pts',(39.4070210670069,26.2570035280093,-164.243631152948));
#155618=CARTESIAN_POINT('Ctrl Pts',(39.4051786186454,26.2573598846844,-164.236556132581));
#155619=CARTESIAN_POINT('Ctrl Pts',(39.3805910621168,26.2621154805938,-164.142139666509));
#155620=CARTESIAN_POINT('Ctrl Pts',(39.3553405852739,26.2672382778453,-164.040433634314));
#155621=CARTESIAN_POINT('Ctrl Pts',(39.3299788857907,26.2727306896172,-163.931389102773));
#155622=CARTESIAN_POINT('Ctrl Pts',(39.3266758216188,26.273446011891,-163.917187330312));
#155623=CARTESIAN_POINT('Ctrl Pts',(39.3233709423668,26.274167604002,-163.902861072933));
#155624=CARTESIAN_POINT('Ctrl Pts',(39.3200655291253,26.2748954716567,-163.888410214473));
#155625=CARTESIAN_POINT('Ctrl Pts',(39.3047720495629,26.2782631683074,-163.821549010632));
#155626=CARTESIAN_POINT('Ctrl Pts',(39.2894667835075,26.2817651925946,-163.752020734357));
#155627=CARTESIAN_POINT('Ctrl Pts',(39.2742814104456,26.2854018053583,-163.679819977838));
#155628=CARTESIAN_POINT('Ctrl Pts',(39.2666887239147,26.2872201117401,-163.643719599579));
#155629=CARTESIAN_POINT('Ctrl Pts',(39.2591260938889,26.2890720658277,-163.606951088395));
#155630=CARTESIAN_POINT('Ctrl Pts',(39.251610560464,26.2909576680051,-163.569514400177));
#155631=CARTESIAN_POINT('Ctrl Pts',(39.2478527937515,26.2919004690937,-163.550796056068));
#155632=CARTESIAN_POINT('Ctrl Pts',(39.2441068051003,26.2928516822406,-163.531910666905));
#155633=CARTESIAN_POINT('Ctrl Pts',(39.2403747510816,26.2938113064648,-163.512858247065));
#155634=CARTESIAN_POINT('Ctrl Pts',(39.2385087240722,26.2942911185769,-163.503332037144));
#155635=CARTESIAN_POINT('Ctrl Pts',(39.236646180934,26.29477303346,-163.493764069515));
#155636=CARTESIAN_POINT('Ctrl Pts',(39.2347873929698,26.2952570508672,-163.484154348409));
#155637=CARTESIAN_POINT('Ctrl Pts',(39.2329286050057,26.2957410682743,-163.474544627303));
#155638=CARTESIAN_POINT('Ctrl Pts',(39.2308289096148,26.2962917205444,-163.463611919718));
#155639=CARTESIAN_POINT('Ctrl Pts',(39.229222566815,26.2967154103779,-163.455199929581));
#155640=CARTESIAN_POINT('Ctrl Pts',(39.2035210820178,26.3034944477151,-163.320608087395));
#155641=CARTESIAN_POINT('Ctrl Pts',(39.1800429123288,26.3103754712095,-163.185641273895));
#155642=CARTESIAN_POINT('Ctrl Pts',(39.1587671982296,26.3172370503909,-163.050400347168));
#155643=CARTESIAN_POINT('Ctrl Pts',(39.14812934118,26.3206678399816,-162.982779883805));
#155644=CARTESIAN_POINT('Ctrl Pts',(39.1380423077006,26.324090233778,-162.915090776103));
#155645=CARTESIAN_POINT('Ctrl Pts',(39.1285006561278,26.3274858217589,-162.847345445333));
#155646=CARTESIAN_POINT('Ctrl Pts',(39.1237298303414,26.3291836157494,-162.813472779947));
#155647=CARTESIAN_POINT('Ctrl Pts',(39.1190953150477,26.3308747058532,-162.77958606057));
#155648=CARTESIAN_POINT('Ctrl Pts',(39.1145962130836,26.3325568340628,-162.745686816459));
#155649=CARTESIAN_POINT('Ctrl Pts',(39.1123466621015,26.3333978981676,-162.728737194403));
#155650=CARTESIAN_POINT('Ctrl Pts',(39.1101309623961,26.3342367217452,-162.711784441201));
#155651=CARTESIAN_POINT('Ctrl Pts',(39.1079489892389,26.3350730241177,-162.694828747083));
#155652=CARTESIAN_POINT('Ctrl Pts',(39.1068580026604,26.3354911753039,-162.686350900024));
#155653=CARTESIAN_POINT('Ctrl Pts',(39.1057754475934,26.3359086961896,-162.677872317734));
#155654=CARTESIAN_POINT('Ctrl Pts',(39.1047013076557,26.3363255518907,-162.669393023875));
#155655=CARTESIAN_POINT('Ctrl Pts',(39.1036271677181,26.3367424075918,-162.660913730015));
#155656=CARTESIAN_POINT('Ctrl Pts',(39.1027440700184,26.3370868304298,-162.653898670079));
#155657=CARTESIAN_POINT('Ctrl Pts',(39.1015019249879,26.3375872893148,-162.643953286364));
#155658=CARTESIAN_POINT('Ctrl Pts',(39.1011118171303,26.3377444633473,-162.640829840841));
#155659=CARTESIAN_POINT('Ctrl Pts',(39.1007231163658,26.337901530053,-162.63770854998));
#155660=CARTESIAN_POINT('Ctrl Pts',(39.1003358168758,26.338058489386,-162.634589414424));
#155661=CARTESIAN_POINT('Ctrl Pts',(39.0803022287851,26.3461774224188,-162.473247924084));
#155662=CARTESIAN_POINT('Ctrl Pts',(39.0640224933764,26.3540091540096,-162.317671311841));
#155663=CARTESIAN_POINT('Ctrl Pts',(39.050841126827,26.3615481992926,-162.16793193425));
#155664=CARTESIAN_POINT('Ctrl Pts',(39.038312448885,26.3687139411743,-162.025607052378));
#155665=CARTESIAN_POINT('Ctrl Pts',(39.028583270636,26.3756152663121,-161.888555596263));
#155666=CARTESIAN_POINT('Ctrl Pts',(39.0211340241148,26.3822478553176,-161.756834054055));
#155667=CARTESIAN_POINT('Ctrl Pts',(39.0132828087732,26.389238345484,-161.618004685198));
#155668=CARTESIAN_POINT('Ctrl Pts',(39.0079635979443,26.3959305221126,-161.485092013288));
#155669=CARTESIAN_POINT('Ctrl Pts',(39.004619214619,26.4023211247915,-161.358161599385));
#155670=CARTESIAN_POINT('Ctrl Pts',(39.0013874364463,26.4084965563252,-161.235504923639));
#155671=CARTESIAN_POINT('Ctrl Pts',(39.,26.4143903824311,-161.118434406696));
#155672=CARTESIAN_POINT('Ctrl Pts',(39.,26.4199999800001,-161.0070032805));
#155673=CARTESIAN_POINT('',(39.,20.76999998,-153.26884421004));
#155674=CARTESIAN_POINT('Ctrl Pts',(39.,20.76999998,-153.26884421004));
#155675=CARTESIAN_POINT('Ctrl Pts',(39.,22.7129810391408,-155.80421523086));
#155676=CARTESIAN_POINT('Ctrl Pts',(39.,24.5896725049001,-158.389029259702));
#155677=CARTESIAN_POINT('Ctrl Pts',(39.,26.4199999800001,-161.0070032805));
#155678=CARTESIAN_POINT('Ctrl Pts',(39.,20.76999998,-153.26884421004));
#155679=CARTESIAN_POINT('Ctrl Pts',(39.,20.765569632395,-153.354826102789));
#155680=CARTESIAN_POINT('Ctrl Pts',(39.000895533927,20.7608738301319,-153.445942320504));
#155681=CARTESIAN_POINT('Ctrl Pts',(39.0030485079457,20.7559119024773,-153.542200055545));
#155682=CARTESIAN_POINT('Ctrl Pts',(39.0050920925181,20.7512020830759,-153.633567076506));
#155683=CARTESIAN_POINT('Ctrl Pts',(39.0082687993418,20.7462524949737,-153.729566394896));
#155684=CARTESIAN_POINT('Ctrl Pts',(39.0129322676218,20.7410628868451,-153.830197762011));
#155685=CARTESIAN_POINT('Ctrl Pts',(39.0176588317899,20.7358030642508,-153.932190653446));
#155686=CARTESIAN_POINT('Ctrl Pts',(39.0239128232778,20.7302964639597,-154.038946012008));
#155687=CARTESIAN_POINT('Ctrl Pts',(39.0321077416871,20.7245446460313,-154.150428276652));
#155688=CARTESIAN_POINT('Ctrl Pts',(39.0387151242647,20.7199070816687,-154.2403139761));
#155689=CARTESIAN_POINT('Ctrl Pts',(39.0465852621392,20.7151100444308,-154.333273737209));
#155690=CARTESIAN_POINT('Ctrl Pts',(39.0559563911723,20.7101549630931,-154.429277186451));
#155691=CARTESIAN_POINT('Ctrl Pts',(39.0606419556888,20.7076774224243,-154.477278911072));
#155692=CARTESIAN_POINT('Ctrl Pts',(39.0657030530557,20.7051603870308,-154.526041243959));
#155693=CARTESIAN_POINT('Ctrl Pts',(39.0711711665567,20.7026041131822,-154.575558899896));
#155694=CARTESIAN_POINT('Ctrl Pts',(39.0739052233071,20.701325976258,-154.600317727865));
#155695=CARTESIAN_POINT('Ctrl Pts',(39.0767410490255,20.7000380317247,-154.625265347961));
#155696=CARTESIAN_POINT('Ctrl Pts',(39.0796826780972,20.6987403179556,-154.650400978073));
#155697=CARTESIAN_POINT('Ctrl Pts',(39.0811534926331,20.698091461071,-154.66296879313));
#155698=CARTESIAN_POINT('Ctrl Pts',(39.0826507590311,20.6974401619388,-154.675583609516));
#155699=CARTESIAN_POINT('Ctrl Pts',(39.0841749877846,20.6967864256737,-154.688245323403));
#155700=CARTESIAN_POINT('Ctrl Pts',(39.0849371021613,20.6964595575411,-154.694576180347));
#155701=CARTESIAN_POINT('Ctrl Pts',(39.085705957183,20.6961320801321,-154.700918761536));
#155702=CARTESIAN_POINT('Ctrl Pts',(39.0864816170269,20.6958039941128,-154.707273053476));
#155703=CARTESIAN_POINT('Ctrl Pts',(39.0866755319878,20.695721972608,-154.708861626461));
#155704=CARTESIAN_POINT('Ctrl Pts',(39.0868698722512,20.6956399130652,-154.710450931365));
#155705=CARTESIAN_POINT('Ctrl Pts',(39.0870646388221,20.695557815495,-154.712040967975));
#155706=CARTESIAN_POINT('Ctrl Pts',(39.0871154522388,20.695536396737,-154.71245579888));
#155707=CARTESIAN_POINT('Ctrl Pts',(39.0871666636068,20.6955148202132,-154.712873684999));
#155708=CARTESIAN_POINT('Ctrl Pts',(39.0872155866559,20.6954942166411,-154.71327272705));
#155709=CARTESIAN_POINT('Ctrl Pts',(39.0877292261227,20.6952779012655,-154.717462239963));
#155710=CARTESIAN_POINT('Ctrl Pts',(39.0880559398794,20.6951404556704,-154.720124228289));
#155711=CARTESIAN_POINT('Ctrl Pts',(39.0888290754381,20.6948179109104,-154.726371047678));
#155712=CARTESIAN_POINT('Ctrl Pts',(39.1032547849822,20.6887996428716,-154.842928617782));
#155713=CARTESIAN_POINT('Ctrl Pts',(39.1186282597997,20.6830712546896,-154.952455676747));
#155714=CARTESIAN_POINT('Ctrl Pts',(39.134360699675,20.6776783755399,-155.054965099396));
#155715=CARTESIAN_POINT('Ctrl Pts',(39.149697365566,20.6724211626496,-155.154895738147));
#155716=CARTESIAN_POINT('Ctrl Pts',(39.1653749029401,20.6674827203699,-155.248157397457));
#155717=CARTESIAN_POINT('Ctrl Pts',(39.1808956676299,20.6629012978552,-155.334756337397));
#155718=CARTESIAN_POINT('Ctrl Pts',(39.1959260131881,20.6584646373607,-155.41861895746));
#155719=CARTESIAN_POINT('Ctrl Pts',(39.2108092257903,20.6543627114732,-155.496233284115));
#155720=CARTESIAN_POINT('Ctrl Pts',(39.2251413518476,20.6506275356373,-155.567599290605));
#155721=CARTESIAN_POINT('Ctrl Pts',(39.2355153047439,20.6479239215311,-155.619255798981));
#155722=CARTESIAN_POINT('Ctrl Pts',(39.2456015006244,20.6454123949607,-155.667638558048));
#155723=CARTESIAN_POINT('Ctrl Pts',(39.2552637406475,20.643104533941,-155.712745444566));
#155724=CARTESIAN_POINT('Ctrl Pts',(39.2680118953415,20.640059591027,-155.772258514591));
#155725=CARTESIAN_POINT('Ctrl Pts',(39.2800324810176,20.6373401949117,-155.826093537767));
#155726=CARTESIAN_POINT('Ctrl Pts',(39.2910799593509,20.6349262020915,-155.874282959093));
#155727=CARTESIAN_POINT('Ctrl Pts',(39.3021027512786,20.6325176035164,-155.922364697602));
#155728=CARTESIAN_POINT('Ctrl Pts',(39.3121567697338,20.6304130796149,-155.964826035607));
#155729=CARTESIAN_POINT('Ctrl Pts',(39.3210492571792,20.6285942725498,-156.001691614201));
#155730=CARTESIAN_POINT('Ctrl Pts',(39.3299517023356,20.6267734288042,-156.038598474471));
#155731=CARTESIAN_POINT('Ctrl Pts',(39.337690840516,20.6252374529696,-156.069898858172));
#155732=CARTESIAN_POINT('Ctrl Pts',(39.3441271348021,20.6239671595869,-156.095616105163));
#155733=CARTESIAN_POINT('Ctrl Pts',(39.3473452819451,20.6233320128956,-156.108474728658));
#155734=CARTESIAN_POINT('Ctrl Pts',(39.3502385260851,20.6227633384985,-156.119937477056));
#155735=CARTESIAN_POINT('Ctrl Pts',(39.3527941980629,20.622259172562,-156.130006632794));
#155736=CARTESIAN_POINT('Ctrl Pts',(39.3540720340518,20.6220070895937,-156.135041210662));
#155737=CARTESIAN_POINT('Ctrl Pts',(39.3552655223485,20.6217711483625,-156.139727379426));
#155738=CARTESIAN_POINT('Ctrl Pts',(39.3563733761272,20.621551129286,-156.144065382332));
#155739=CARTESIAN_POINT('Ctrl Pts',(39.3569273030166,20.6214411197478,-156.146234383785));
#155740=CARTESIAN_POINT('Ctrl Pts',(39.3574598241068,20.6213350916515,-156.148316343098));
#155741=CARTESIAN_POINT('Ctrl Pts',(39.3579707959811,20.6212330217096,-156.150311286952));
#155742=CARTESIAN_POINT('Ctrl Pts',(39.3580064486167,20.6212258998647,-156.150450482492));
#155743=CARTESIAN_POINT('Ctrl Pts',(39.3580419963212,20.6212187973118,-156.150589254327));
#155744=CARTESIAN_POINT('Ctrl Pts',(39.3580774390432,20.6212117140468,-156.150727602449));
#155745=CARTESIAN_POINT('Ctrl Pts',(39.3582959780233,20.6211680388036,-156.151580653676));
#155746=CARTESIAN_POINT('Ctrl Pts',(39.358510531579,20.6211250965916,-156.152417601068));
#155747=CARTESIAN_POINT('Ctrl Pts',(39.3587210872467,20.6210828864843,-156.153238442282));
#155748=CARTESIAN_POINT('Ctrl Pts',(39.3588434390735,20.6210583586063,-156.153715425035));
#155749=CARTESIAN_POINT('Ctrl Pts',(39.3589644411211,20.6210340778222,-156.154186969809));
#155750=CARTESIAN_POINT('Ctrl Pts',(39.35908409128,20.62101004377,-156.154653077003));
#155751=CARTESIAN_POINT('Ctrl Pts',(39.3591140038197,20.621004035257,-156.154769603802));
#155752=CARTESIAN_POINT('Ctrl Pts',(39.3591165961832,20.6210035274588,-156.154779716518));
#155753=CARTESIAN_POINT('Ctrl Pts',(39.3591122924758,20.6210044063111,-156.154762971055));
#155754=CARTESIAN_POINT('Ctrl Pts',(39.3591090646952,20.6210050654502,-156.154750411958));
#155755=CARTESIAN_POINT('Ctrl Pts',(39.35910195833,20.6210065045819,-156.154722745096));
#155756=CARTESIAN_POINT('Ctrl Pts',(39.3590995907982,20.6210069880885,-156.154713533031));
#155757=CARTESIAN_POINT('Ctrl Pts',(39.3590924882029,20.6210084386082,-156.154685896836));
#155758=CARTESIAN_POINT('Ctrl Pts',(39.3591279622065,20.6210012882107,-156.15482436012));
#155759=CARTESIAN_POINT('Ctrl Pts',(39.3594389855587,20.6209386764191,-156.156035085875));
#155760=CARTESIAN_POINT('Ctrl Pts',(39.3867193814463,20.6154468879403,-156.262229934837));
#155761=CARTESIAN_POINT('Ctrl Pts',(39.4149051829703,20.6100918526737,-156.365212269418));
#155762=CARTESIAN_POINT('Ctrl Pts',(39.4437478087531,20.6048990924637,-156.464947028467));
#155763=CARTESIAN_POINT('Ctrl Pts',(39.4740165754652,20.599449573111,-156.56961323249));
#155764=CARTESIAN_POINT('Ctrl Pts',(39.5050085204789,20.5941787690805,-156.670703053005));
#155765=CARTESIAN_POINT('Ctrl Pts',(39.5364571470437,20.5891098870968,-156.768229841553));
#155766=CARTESIAN_POINT('Ctrl Pts',(39.5527864562365,20.5864779330112,-156.818869416591));
#155767=CARTESIAN_POINT('Ctrl Pts',(39.5692392444004,20.5839003179835,-156.868549206904));
#155768=CARTESIAN_POINT('Ctrl Pts',(39.585780524855,20.5813796851227,-156.917275972421));
#155769=CARTESIAN_POINT('Ctrl Pts',(39.6201299951416,20.576145362194,-157.018461523858));
#155770=CARTESIAN_POINT('Ctrl Pts',(39.6548573299948,20.5711493957629,-157.115517731783));
#155771=CARTESIAN_POINT('Ctrl Pts',(39.6896634736143,20.5663740905208,-157.20847470014));
#155772=CARTESIAN_POINT('Ctrl Pts',(39.6947578637932,20.5656751544825,-157.222080317351));
#155773=CARTESIAN_POINT('Ctrl Pts',(39.699853985679,20.5649809455337,-157.235598197776));
#155774=CARTESIAN_POINT('Ctrl Pts',(39.7049509461478,20.5642914082257,-157.249028514624));
#155775=CARTESIAN_POINT('Ctrl Pts',(39.7249112786228,20.5615910941841,-157.301623309337));
#155776=CARTESIAN_POINT('Ctrl Pts',(39.7448842807308,20.5589617603203,-157.352874077829));
#155777=CARTESIAN_POINT('Ctrl Pts',(39.7648181882144,20.5563964561493,-157.402789407317));
#155778=CARTESIAN_POINT('Ctrl Pts',(39.7747851419562,20.5551138040638,-157.427747072061));
#155779=CARTESIAN_POINT('Ctrl Pts',(39.7847423349863,20.5538471666677,-157.45237087167));
#155780=CARTESIAN_POINT('Ctrl Pts',(39.7946836004314,20.5525954318246,-157.47666203141));
#155781=CARTESIAN_POINT('Ctrl Pts',(39.7996542331539,20.5519695644031,-157.488807611281));
#155782=CARTESIAN_POINT('Ctrl Pts',(39.8046208849858,20.5513474231558,-157.500870030787));
#155783=CARTESIAN_POINT('Ctrl Pts',(39.809582796279,20.5507288654499,-157.512849444999));
#155784=CARTESIAN_POINT('Ctrl Pts',(39.8120637519256,20.5504195865969,-157.518839152105));
#155785=CARTESIAN_POINT('Ctrl Pts',(39.8145435224991,20.5501112036634,-157.524808107863));
#155786=CARTESIAN_POINT('Ctrl Pts',(39.8170220141739,20.5498036980508,-157.530756332126));
#155787=CARTESIAN_POINT('Ctrl Pts',(39.8188462490901,20.54957736585,-157.535134381284));
#155788=CARTESIAN_POINT('Ctrl Pts',(39.8202180487261,20.5494074771205,-157.538420409514));
#155789=CARTESIAN_POINT('Ctrl Pts',(39.8221344968241,20.5491704280015,-157.543001012365));
#155790=CARTESIAN_POINT('Ctrl Pts',(39.8228218255829,20.549085410997,-157.544643832787));
#155791=CARTESIAN_POINT('Ctrl Pts',(39.823579329211,20.5489917564752,-157.546453148038));
#155792=CARTESIAN_POINT('Ctrl Pts',(39.8244535178766,20.5488837732778,-157.548538842568));
#155793=CARTESIAN_POINT('Ctrl Pts',(39.8725663581697,20.5429406873756,-157.663329495599));
#155794=CARTESIAN_POINT('Ctrl Pts',(39.9217743356622,20.5371890374606,-157.774410745202));
#155795=CARTESIAN_POINT('Ctrl Pts',(39.971892926282,20.5316291232997,-157.881779625474));
#155796=CARTESIAN_POINT('Ctrl Pts',(40.0244146734342,20.5258026145705,-157.994296779528));
#155797=CARTESIAN_POINT('Ctrl Pts',(40.0779363679974,20.5201866679455,-158.102737051431));
#155798=CARTESIAN_POINT('Ctrl Pts',(40.1321925265671,20.5147804320522,-158.207119649317));
#155799=CARTESIAN_POINT('Ctrl Pts',(40.1883659720449,20.509183152311,-158.315190886312));
#155800=CARTESIAN_POINT('Ctrl Pts',(40.2453263822506,20.5038106595684,-158.418912739766));
#155801=CARTESIAN_POINT('Ctrl Pts',(40.3027268245705,20.4986608268383,-158.518328841652));
#155802=CARTESIAN_POINT('Ctrl Pts',(40.3638454627555,20.4931774063171,-158.62418476393));
#155803=CARTESIAN_POINT('Ctrl Pts',(40.4254626820068,20.4879464200038,-158.725159169806));
#155804=CARTESIAN_POINT('Ctrl Pts',(40.4871059726323,20.4829640792563,-158.821327714668));
#155805=CARTESIAN_POINT('Ctrl Pts',(40.4933177444275,20.4824620106059,-158.831018583674));
#155806=CARTESIAN_POINT('Ctrl Pts',(40.4995297413823,20.4819624659268,-158.840660668463));
#155807=CARTESIAN_POINT('Ctrl Pts',(40.5057414544625,20.4814654407574,-158.850254057419));
#155808=CARTESIAN_POINT('Origin',(39.,46.91999998,-129.34995));
#155809=CARTESIAN_POINT('',(39.,26.419999980009,-71.0516396909899));
#155810=CARTESIAN_POINT('',(39.,26.41999998,-129.34995));
#155811=CARTESIAN_POINT('',(39.,20.769999979994,-78.7897987614735));
#155812=CARTESIAN_POINT('Ctrl Pts',(39.,26.4199999800115,-71.0516396909898));
#155813=CARTESIAN_POINT('Ctrl Pts',(39.,24.5896727691867,-73.6696133337874));
#155814=CARTESIAN_POINT('Ctrl Pts',(39.,22.7129807779577,-76.2544280814611));
#155815=CARTESIAN_POINT('Ctrl Pts',(39.,20.769999979994,-78.7897987614735));
#155816=CARTESIAN_POINT('',(39.,20.76999998,-129.34995));
#155817=CARTESIAN_POINT('Ctrl Pts',(39.,29.2922016634715,-66.8629239833248));
#155818=CARTESIAN_POINT('Ctrl Pts',(39.,27.39376514223,-65.5849455541034));
#155819=CARTESIAN_POINT('Ctrl Pts',(40.7320633148745,26.1529710718006,-64.749675035773));
#155820=CARTESIAN_POINT('Ctrl Pts',(39.,26.5499956507371,-70.9364700811645));
#155821=CARTESIAN_POINT('Ctrl Pts',(39.,24.7552520476619,-69.6491930963147));
#155822=CARTESIAN_POINT('Ctrl Pts',(40.6302860195927,23.5167393131936,-68.8231852344136));
#155823=CARTESIAN_POINT('Ctrl Pts',(39.,23.7045900978902,-74.9643266004363));
#155824=CARTESIAN_POINT('Ctrl Pts',(38.9999999999314,22.0109048679673,-73.6914516653908));
#155825=CARTESIAN_POINT('Ctrl Pts',(40.5200331454484,20.7957836646288,-72.8509648236473));
#155826=CARTESIAN_POINT('Ctrl Pts',(39.,20.7168512667374,-78.8591174122859));
#155827=CARTESIAN_POINT('Ctrl Pts',(39.,19.1148189506652,-77.6301799952506));
#155828=CARTESIAN_POINT('Ctrl Pts',(40.402078446557,17.9620216308036,-76.7458559111338));
#155829=CARTESIAN_POINT('',(40.7299248988739,26.1062891840432,-64.8223083472515));
#155830=CARTESIAN_POINT('Ctrl Pts',(39.,26.4199999800114,-71.0516396909892));
#155831=CARTESIAN_POINT('Ctrl Pts',(39.,26.4157490575532,-70.9671977910182));
#155832=CARTESIAN_POINT('Ctrl Pts',(39.0007946432884,26.4112648461199,-70.8771641690186));
#155833=CARTESIAN_POINT('Ctrl Pts',(39.0027282692707,26.4065088388894,-70.7815280985075));
#155834=CARTESIAN_POINT('Ctrl Pts',(39.0046332133543,26.4018233785582,-70.687310618824));
#155835=CARTESIAN_POINT('Ctrl Pts',(39.007643552267,26.3968741379737,-70.5876556369414));
#155836=CARTESIAN_POINT('Ctrl Pts',(39.0121385956576,26.391622622828,-70.4825592333295));
#155837=CARTESIAN_POINT('Ctrl Pts',(39.0141929022949,26.389222596514,-70.4345284979758));
#155838=CARTESIAN_POINT('Ctrl Pts',(39.0165580098215,26.3867594115903,-70.3853613380078));
#155839=CARTESIAN_POINT('Ctrl Pts',(39.0192737374602,26.3842292724267,-70.3350578600083));
#155840=CARTESIAN_POINT('Ctrl Pts',(39.0255147686812,26.3784147432784,-70.2194551124234));
#155841=CARTESIAN_POINT('Ctrl Pts',(39.0336033940894,26.3722556372242,-70.0978543729413));
#155842=CARTESIAN_POINT('Ctrl Pts',(39.0440550436964,26.3657732814451,-69.9702982548804));
#155843=CARTESIAN_POINT('Ctrl Pts',(39.0459036608686,26.364626726149,-69.947736990474));
#155844=CARTESIAN_POINT('Ctrl Pts',(39.0478263334364,26.3634700624251,-69.9249894362222));
#155845=CARTESIAN_POINT('Ctrl Pts',(39.0498260809213,26.3623034136746,-69.9020558523985));
#155846=CARTESIAN_POINT('Ctrl Pts',(39.0564790072074,26.3584221095613,-69.8257584979552));
#155847=CARTESIAN_POINT('Ctrl Pts',(39.0639844336357,26.3544316715932,-69.7474029129631));
#155848=CARTESIAN_POINT('Ctrl Pts',(39.072455105127,26.3503463271069,-69.6670050750542));
#155849=CARTESIAN_POINT('Ctrl Pts',(39.0766904408726,26.3483036548637,-69.6268061560997));
#155850=CARTESIAN_POINT('Ctrl Pts',(39.0811671665333,26.3462372639141,-69.5860966794539));
#155851=CARTESIAN_POINT('Ctrl Pts',(39.0858996117955,26.3441497520647,-69.5448792292923));
#155852=CARTESIAN_POINT('Ctrl Pts',(39.0882658344266,26.34310599614,-69.5242705042115));
#155853=CARTESIAN_POINT('Ctrl Pts',(39.0906959906315,26.3420569598266,-69.503534785651));
#155854=CARTESIAN_POINT('Ctrl Pts',(39.0931918854002,26.3410029962426,-69.4826724165355));
#155855=CARTESIAN_POINT('Ctrl Pts',(39.0944398327845,26.3404760144507,-69.4722412319778));
#155856=CARTESIAN_POINT('Ctrl Pts',(39.0957042150142,26.3399478008273,-69.4617783847725));
#155857=CARTESIAN_POINT('Ctrl Pts',(39.0969852581247,26.3394184025146,-69.4512839199201));
#155858=CARTESIAN_POINT('Ctrl Pts',(39.0980249587679,26.3389887403419,-69.4427665626448));
#155859=CARTESIAN_POINT('Ctrl Pts',(39.0992517705288,26.3384865966415,-69.4328046918058));
#155860=CARTESIAN_POINT('Ctrl Pts',(39.1002372416259,26.3380865818,-69.4248647839529));
#155861=CARTESIAN_POINT('Ctrl Pts',(39.1004659959578,26.3379937276025,-69.423021717909));
#155862=CARTESIAN_POINT('Ctrl Pts',(39.1006816275985,26.3379063756034,-69.4212875849205));
#155863=CARTESIAN_POINT('Ctrl Pts',(39.1008785926738,26.3378267085406,-69.419705717698));
#155864=CARTESIAN_POINT('Ctrl Pts',(39.1176064072507,26.3310607585165,-69.2853611819927));
#155865=CARTESIAN_POINT('Ctrl Pts',(39.1363872223018,26.3243138583997,-69.1513989218022));
#155866=CARTESIAN_POINT('Ctrl Pts',(39.1573589564869,26.3175651137247,-69.0174031985853));
#155867=CARTESIAN_POINT('Ctrl Pts',(39.1783306906719,26.3108163690497,-68.8834074753684));
#155868=CARTESIAN_POINT('Ctrl Pts',(39.2014945270825,26.3040655661428,-68.7493781443013));
#155869=CARTESIAN_POINT('Ctrl Pts',(39.2270164024943,26.2973852620386,-68.6149087107991));
#155870=CARTESIAN_POINT('Ctrl Pts',(39.2525382779062,26.2907049579344,-68.4804392772969));
#155871=CARTESIAN_POINT('Ctrl Pts',(39.2802448812632,26.2839676825278,-68.346725706618));
#155872=CARTESIAN_POINT('Ctrl Pts',(39.3101294150359,26.2772295950935,-68.2138673363941));
#155873=CARTESIAN_POINT('Ctrl Pts',(39.3250716819223,26.2738605513764,-68.1474381512822));
#155874=CARTESIAN_POINT('Ctrl Pts',(39.3405581607619,26.2704911619849,-68.0812228072504));
#155875=CARTESIAN_POINT('Ctrl Pts',(39.3565820575716,26.2671390609516,-68.0152327345648));
#155876=CARTESIAN_POINT('Ctrl Pts',(39.3645940059764,26.265463010435,-67.982237698222));
#155877=CARTESIAN_POINT('Ctrl Pts',(39.3727402743783,26.2637912659535,-67.9492989688229));
#155878=CARTESIAN_POINT('Ctrl Pts',(39.3810197959113,26.2621259619583,-67.916417922894));
#155879=CARTESIAN_POINT('Ctrl Pts',(39.3851595566778,26.2612933099607,-67.8999773999296));
#155880=CARTESIAN_POINT('Ctrl Pts',(39.3893326286307,26.2604622669912,-67.8835512970938));
#155881=CARTESIAN_POINT('Ctrl Pts',(39.3935388657984,26.2596330936854,-67.8671397821491));
#155882=CARTESIAN_POINT('Ctrl Pts',(39.3956419843822,26.2592185070325,-67.8589340246768));
#155883=CARTESIAN_POINT('Ctrl Pts',(39.3977533941432,26.2588043877234,-67.8507319141284));
#155884=CARTESIAN_POINT('Ctrl Pts',(39.3998730760318,26.2583907680051,-67.8425334712319));
#155885=CARTESIAN_POINT('Ctrl Pts',(39.4014018607501,26.2580924517776,-67.8366204829287));
#155886=CARTESIAN_POINT('Ctrl Pts',(39.4027461781225,26.2578310056885,-67.8314363746657));
#155887=CARTESIAN_POINT('Ctrl Pts',(39.4043141873651,26.2575272307581,-67.8254081776661));
#155888=CARTESIAN_POINT('Ctrl Pts',(39.4049202453754,26.2574098174006,-67.823078193263));
#155889=CARTESIAN_POINT('Ctrl Pts',(39.4055598310341,26.2572860807778,-67.8206221151732));
#155890=CARTESIAN_POINT('Ctrl Pts',(39.4062569470272,26.2571514505613,-67.8179491721346));
#155891=CARTESIAN_POINT('Ctrl Pts',(39.4370469433536,26.2512051461987,-67.6998914784915));
#155892=CARTESIAN_POINT('Ctrl Pts',(39.4688929423544,26.2454344417139,-67.5853212411314));
#155893=CARTESIAN_POINT('Ctrl Pts',(39.5015465506626,26.239841569324,-67.4742814563482));
#155894=CARTESIAN_POINT('Ctrl Pts',(39.5358806442963,26.2339608653447,-67.3575271199869));
#155895=CARTESIAN_POINT('Ctrl Pts',(39.5711074099235,26.2282767546822,-67.2446756972104));
#155896=CARTESIAN_POINT('Ctrl Pts',(39.6069552370405,26.2227890155487,-67.1357214352314));
#155897=CARTESIAN_POINT('Ctrl Pts',(39.6256220886793,26.2199314138341,-67.0789862518927));
#155898=CARTESIAN_POINT('Ctrl Pts',(39.6444576394001,26.217127015129,-67.0233069304515));
#155899=CARTESIAN_POINT('Ctrl Pts',(39.6634255058615,26.2143755290716,-66.9686775345326));
#155900=CARTESIAN_POINT('Ctrl Pts',(39.7022382760887,26.2087453335856,-66.8568927855324));
#155901=CARTESIAN_POINT('Ctrl Pts',(39.7415986105878,26.2033376046449,-66.7495233055924));
#155902=CARTESIAN_POINT('Ctrl Pts',(39.781186051756,26.1981508743513,-66.6465398341847));
#155903=CARTESIAN_POINT('Ctrl Pts',(39.8066514637351,26.1948144065258,-66.5802936599174));
#155904=CARTESIAN_POINT('Ctrl Pts',(39.8322114175671,26.1915693068131,-66.5158608089899));
#155905=CARTESIAN_POINT('Ctrl Pts',(39.8577823212076,26.1884149365567,-66.4532286057725));
#155906=CARTESIAN_POINT('Ctrl Pts',(39.8705677730279,26.1868377514286,-66.4219125041639));
#155907=CARTESIAN_POINT('Ctrl Pts',(39.8833560183902,26.1852832413074,-66.3910464188101));
#155908=CARTESIAN_POINT('Ctrl Pts',(39.8961367846945,26.1837513043075,-66.3606283296588));
#155909=CARTESIAN_POINT('Ctrl Pts',(39.9025271678466,26.1829853358075,-66.3454192850831));
#155910=CARTESIAN_POINT('Ctrl Pts',(39.9089156872528,26.1822250098702,-66.3303222253317));
#155911=CARTESIAN_POINT('Ctrl Pts',(39.9153010704457,26.1814703124786,-66.3153368725879));
#155912=CARTESIAN_POINT('Ctrl Pts',(39.9184937620421,26.1810929637827,-66.307844196216));
#155913=CARTESIAN_POINT('Ctrl Pts',(39.9216856697547,26.1807170222045,-66.3003794462247));
#155914=CARTESIAN_POINT('Ctrl Pts',(39.924876635247,26.1803424859162,-66.2929425863946));
#155915=CARTESIAN_POINT('Ctrl Pts',(39.9264721179931,26.1801552177721,-66.2892241564795));
#155916=CARTESIAN_POINT('Ctrl Pts',(39.9280673651883,26.1799683009501,-66.2855126990972));
#155917=CARTESIAN_POINT('Ctrl Pts',(39.9296623571035,26.179781735215,-66.2818082095887));
#155918=CARTESIAN_POINT('Ctrl Pts',(39.9304598530611,26.1796884523475,-66.2799559648344));
#155919=CARTESIAN_POINT('Ctrl Pts',(39.931257285198,26.1795952572518,-66.2781054620504));
#155920=CARTESIAN_POINT('Ctrl Pts',(39.9320546510499,26.1795021498985,-66.2762567006511));
#155921=CARTESIAN_POINT('Ctrl Pts',(39.9324533339758,26.1794555962218,-66.2753323199515));
#155922=CARTESIAN_POINT('Ctrl Pts',(39.9328520003305,26.1794090644806,-66.2744083745979));
#155923=CARTESIAN_POINT('Ctrl Pts',(39.9332506498063,26.1793625546713,-66.2734848645166));
#155924=CARTESIAN_POINT('Ctrl Pts',(39.9334710477516,26.1793368411886,-66.2729742913521));
#155925=CARTESIAN_POINT('Ctrl Pts',(39.9336914405377,26.1793111344095,-66.2724638512311));
#155926=CARTESIAN_POINT('Ctrl Pts',(39.9339118281128,26.1792854343334,-66.2719535441411));
#155927=CARTESIAN_POINT('Ctrl Pts',(39.9340602477085,26.1792681266657,-66.271609878796));
#155928=CARTESIAN_POINT('Ctrl Pts',(39.9342090065607,26.1792507822761,-66.2712654842615));
#155929=CARTESIAN_POINT('Ctrl Pts',(39.9343519252519,26.1792341213463,-66.2709346606505));
#155930=CARTESIAN_POINT('Ctrl Pts',(39.9343806434435,26.1792307734863,-66.2708681846999));
#155931=CARTESIAN_POINT('Ctrl Pts',(39.9344091968868,26.1792274449355,-66.2708020921554));
#155932=CARTESIAN_POINT('Ctrl Pts',(39.9344375981603,26.179224134224,-66.2707363538339));
#155933=CARTESIAN_POINT('Ctrl Pts',(39.9356927533187,26.1790778218918,-66.26783113927));
#155934=CARTESIAN_POINT('Ctrl Pts',(39.936649858508,26.1789663271907,-66.2656172715509));
#155935=CARTESIAN_POINT('Ctrl Pts',(39.9383996878686,26.1787629094249,-66.2615781509511));
#155936=CARTESIAN_POINT('Ctrl Pts',(39.986566302021,26.1731635377039,-66.150395444895));
#155937=CARTESIAN_POINT('Ctrl Pts',(40.0357321248214,26.1677282386571,-66.0424674068876));
#155938=CARTESIAN_POINT('Ctrl Pts',(40.0857914406382,26.1624582752379,-65.9378193737947));
#155939=CARTESIAN_POINT('Ctrl Pts',(40.1378864073397,26.1569740099346,-65.8289158518348));
#155940=CARTESIAN_POINT('Ctrl Pts',(40.1909489716211,26.1516687995635,-65.7235645048982));
#155941=CARTESIAN_POINT('Ctrl Pts',(40.2448072385024,26.1465429026494,-65.6217708150873));
#155942=CARTESIAN_POINT('Ctrl Pts',(40.3001348611089,26.1412771615403,-65.5172000002484));
#155943=CARTESIAN_POINT('Ctrl Pts',(40.3563019551941,26.1362006462319,-65.4163835080774));
#155944=CARTESIAN_POINT('Ctrl Pts',(40.4130699166274,26.1313124810063,-65.3193043818183));
#155945=CARTESIAN_POINT('Ctrl Pts',(40.4730292450883,26.1261495141332,-65.2167676855708));
#155946=CARTESIAN_POINT('Ctrl Pts',(40.5336587646811,26.1211966671277,-65.1184003258764));
#155947=CARTESIAN_POINT('Ctrl Pts',(40.594622373623,26.1164516892111,-65.0241581730242));
#155948=CARTESIAN_POINT('Ctrl Pts',(40.6395930973415,26.1129514848327,-64.9546390305044));
#155949=CARTESIAN_POINT('Ctrl Pts',(40.6847443924467,26.1095643652524,-64.8873640810613));
#155950=CARTESIAN_POINT('Ctrl Pts',(40.7299249051783,26.1062890609598,-64.8223083578266));
#155951=CARTESIAN_POINT('',(40.5057713943428,20.4815822174724,-73.2084022473292));
#155952=CARTESIAN_POINT('Ctrl Pts',(40.5058072671264,20.4819096069224,-73.2085627982137));
#155953=CARTESIAN_POINT('Ctrl Pts',(40.524433110837,20.9372732015992,-72.5561415754388));
#155954=CARTESIAN_POINT('Ctrl Pts',(40.5430920718079,21.3958644703476,-71.8921575025155));
#155955=CARTESIAN_POINT('Ctrl Pts',(40.5617698100191,21.8577586494764,-71.2165453906544));
#155956=CARTESIAN_POINT('Ctrl Pts',(40.579811750967,22.3039297762911,-70.5639313702585));
#155957=CARTESIAN_POINT('Ctrl Pts',(40.5978712100053,22.753182702484,-69.9004673459997));
#155958=CARTESIAN_POINT('Ctrl Pts',(40.6159337007597,23.2055915895099,-69.2261421324262));
#155959=CARTESIAN_POINT('Ctrl Pts',(40.6335867547941,23.6477453675777,-68.5671023801613));
#155960=CARTESIAN_POINT('Ctrl Pts',(40.6512427049893,24.0929135723843,-67.8976880494934));
#155961=CARTESIAN_POINT('Ctrl Pts',(40.6688865216948,24.5411727272614,-67.2179375596961));
#155962=CARTESIAN_POINT('Ctrl Pts',(40.6860071352838,24.9761393734549,-66.5583441357168));
#155963=CARTESIAN_POINT('Ctrl Pts',(40.7031163227297,25.4140163111681,-65.8890183497114));
#155964=CARTESIAN_POINT('Ctrl Pts',(40.7201989295779,25.8548813945471,-65.2100441331028));
#155965=CARTESIAN_POINT('Ctrl Pts',(40.7234419274554,25.9385761457275,-65.0811462451561));
#155966=CARTESIAN_POINT('Ctrl Pts',(40.7266839631706,26.0223786149058,-64.9519007760722));
#155967=CARTESIAN_POINT('Ctrl Pts',(40.7299249270772,26.1062893712319,-64.8223085129012));
#155968=CARTESIAN_POINT('Ctrl Pts',(40.5057175975614,20.4815025603645,-73.2083776836381));
#155969=CARTESIAN_POINT('Ctrl Pts',(40.5054644120188,20.4815748935818,-73.2086976157026));
#155970=CARTESIAN_POINT('Ctrl Pts',(40.5049011999628,20.4816397337449,-73.2095404184828));
#155971=CARTESIAN_POINT('Ctrl Pts',(40.5040075187888,20.4817138168114,-73.2109184929233));
#155972=CARTESIAN_POINT('Ctrl Pts',(40.5039405013756,20.4817193723222,-73.2110218351295));
#155973=CARTESIAN_POINT('Ctrl Pts',(40.5038716257255,20.4817249801809,-73.2111281875613));
#155974=CARTESIAN_POINT('Ctrl Pts',(40.5038008833269,20.4817306475902,-73.2112375555082));
#155975=CARTESIAN_POINT('Ctrl Pts',(40.5036682413297,20.4817412739827,-73.2114426204088));
#155976=CARTESIAN_POINT('Ctrl Pts',(40.5035290365313,20.4817521097208,-73.2116582867215));
#155977=CARTESIAN_POINT('Ctrl Pts',(40.5033832129991,20.4817632024457,-73.2118845894146));
#155978=CARTESIAN_POINT('Ctrl Pts',(40.5023624482738,20.4818408515203,-73.2134687082665));
#155979=CARTESIAN_POINT('Ctrl Pts',(40.5010173195751,20.4819310487397,-73.2155739780529));
#155980=CARTESIAN_POINT('Ctrl Pts',(40.4993289612953,20.4820504367294,-73.2182126034611));
#155981=CARTESIAN_POINT('Ctrl Pts',(40.4972707721543,20.4821959763739,-73.2214292134824));
#155982=CARTESIAN_POINT('Ctrl Pts',(40.4947024442687,20.482384902843,-73.225438450215));
#155983=CARTESIAN_POINT('Ctrl Pts',(40.4916267542034,20.482620024983,-73.2302425124976));
#155984=CARTESIAN_POINT('Ctrl Pts',(40.4900889091707,20.4827375860529,-73.232644543639));
#155985=CARTESIAN_POINT('Ctrl Pts',(40.4884242433347,20.4828667122259,-73.2352452930148));
#155986=CARTESIAN_POINT('Ctrl Pts',(40.4866332081492,20.4830078607953,-73.2380451199897));
#155987=CARTESIAN_POINT('Ctrl Pts',(40.4848421729637,20.4831490093648,-73.2408449469647));
#155988=CARTESIAN_POINT('Ctrl Pts',(40.4819068550032,20.483384737091,-73.2454372432251));
#155989=CARTESIAN_POINT('Ctrl Pts',(40.4808815266029,20.4834678959463,-73.2470422411145));
#155990=CARTESIAN_POINT('Ctrl Pts',(40.4726788994003,20.4841331667888,-73.2598822242301));
#155991=CARTESIAN_POINT('Ctrl Pts',(40.4643047119547,20.484816592624,-73.2730804680188));
#155992=CARTESIAN_POINT('Ctrl Pts',(40.4561952554549,20.4854831988743,-73.2859475813571));
#155993=CARTESIAN_POINT('Ctrl Pts',(40.442730688993,20.4865900010578,-73.3073115411638));
#155994=CARTESIAN_POINT('Ctrl Pts',(40.4290118058235,20.4877298937745,-73.3293255323986));
#155995=CARTESIAN_POINT('Ctrl Pts',(40.4157123730281,20.4888477046274,-73.3509081883742));
#155996=CARTESIAN_POINT('Ctrl Pts',(40.4129918066602,20.4890763669064,-73.3553231922979));
#155997=CARTESIAN_POINT('Ctrl Pts',(40.4102886284986,20.4893041021319,-73.3597200850662));
#155998=CARTESIAN_POINT('Ctrl Pts',(40.4076083565512,20.4895304334342,-73.3640895164659));
#155999=CARTESIAN_POINT('Ctrl Pts',(40.3918256302552,20.4908631806573,-73.3898188234937));
#156000=CARTESIAN_POINT('Ctrl Pts',(40.3760899149249,20.4922092776769,-73.4158150871827));
#156001=CARTESIAN_POINT('Ctrl Pts',(40.3604066409036,20.4935692425358,-73.442079018916));
#156002=CARTESIAN_POINT('Ctrl Pts',(40.3491586948822,20.4945446008253,-73.4609153464609));
#156003=CARTESIAN_POINT('Ctrl Pts',(40.337580168363,20.4955585440772,-73.4804966048277));
#156004=CARTESIAN_POINT('Ctrl Pts',(40.3264437516604,20.496543538312,-73.4995169658499));
#156005=CARTESIAN_POINT('Ctrl Pts',(40.3220524022774,20.4969319445598,-73.5070171387395));
#156006=CARTESIAN_POINT('Ctrl Pts',(40.3177292467201,20.4973158389473,-73.5144298906698));
#156007=CARTESIAN_POINT('Ctrl Pts',(40.3135195919864,20.4976910410416,-73.5216743800284));
#156008=CARTESIAN_POINT('Ctrl Pts',(40.2837490006234,20.5003444625053,-73.5729072591995));
#156009=CARTESIAN_POINT('Ctrl Pts',(40.2541443566281,20.5030513930188,-73.6252024652474));
#156010=CARTESIAN_POINT('Ctrl Pts',(40.2247473538148,20.5058144906767,-73.6785646287757));
#156011=CARTESIAN_POINT('Ctrl Pts',(40.2100488524082,20.5071960395057,-73.7052457105399));
#156012=CARTESIAN_POINT('Ctrl Pts',(40.1954022357644,20.5085916032087,-73.7321935119101));
#156013=CARTESIAN_POINT('Ctrl Pts',(40.1808127130061,20.5100011562159,-73.7594083654028));
#156014=CARTESIAN_POINT('Ctrl Pts',(40.173517951627,20.5107059327196,-73.7730157921491));
#156015=CARTESIAN_POINT('Ctrl Pts',(40.1662374614079,20.5114142046086,-73.7866899804991));
#156016=CARTESIAN_POINT('Ctrl Pts',(40.1589718843034,20.5121259510964,-73.8004309595697));
#156017=CARTESIAN_POINT('Ctrl Pts',(40.1528035177503,20.5127302132447,-73.8120968457736));
#156018=CARTESIAN_POINT('Ctrl Pts',(40.1461485986819,20.5133861915882,-73.8247609414863));
#156019=CARTESIAN_POINT('Ctrl Pts',(40.1402744482112,20.5139685326086,-73.8360036008295));
#156020=CARTESIAN_POINT('Ctrl Pts',(40.1392295719346,20.5140721176836,-73.838003411371));
#156021=CARTESIAN_POINT('Ctrl Pts',(40.1382092722869,20.5141733704156,-73.8399581997929));
#156022=CARTESIAN_POINT('Ctrl Pts',(40.1372205265763,20.5142715823243,-73.8418542900697));
#156023=CARTESIAN_POINT('Ctrl Pts',(40.0848418236023,20.5194743481513,-73.9422994787208));
#156024=CARTESIAN_POINT('Ctrl Pts',(40.0326909735655,20.5249042925461,-74.0473968589734));
#156025=CARTESIAN_POINT('Ctrl Pts',(39.9811106489698,20.53059114945,-74.15719227979));
#156026=CARTESIAN_POINT('Ctrl Pts',(39.955320486672,20.533434577902,-74.2120899901983));
#156027=CARTESIAN_POINT('Ctrl Pts',(39.9296729235851,20.5363414040528,-74.2681616497415));
#156028=CARTESIAN_POINT('Ctrl Pts',(39.9042093277617,20.5393099926147,-74.3254093376965));
#156029=CARTESIAN_POINT('Ctrl Pts',(39.89147752985,20.5407942868957,-74.354033181674));
#156030=CARTESIAN_POINT('Ctrl Pts',(39.8787916677988,20.5422939996947,-74.3829510163953));
#156031=CARTESIAN_POINT('Ctrl Pts',(39.8661567482737,20.5438085282331,-74.4121628275136));
#156032=CARTESIAN_POINT('Ctrl Pts',(39.8598392885112,20.5445657925023,-74.4267687330727));
#156033=CARTESIAN_POINT('Ctrl Pts',(39.8535345599658,20.5453267592658,-74.4414481316369));
#156034=CARTESIAN_POINT('Ctrl Pts',(39.8472431670729,20.546091336907,-74.4562010097231));
#156035=CARTESIAN_POINT('Ctrl Pts',(39.8440974706264,20.5464736257276,-74.4635774487662));
#156036=CARTESIAN_POINT('Ctrl Pts',(39.8409551077943,20.5468568171812,-74.4709722576226));
#156037=CARTESIAN_POINT('Ctrl Pts',(39.8378161530651,20.5472408983346,-74.4783854335678));
#156038=CARTESIAN_POINT('Ctrl Pts',(39.834677198336,20.5476249794881,-74.485798609513));
#156039=CARTESIAN_POINT('Ctrl Pts',(39.8308803749233,20.5480914147653,-74.4948030605568));
#156040=CARTESIAN_POINT('Ctrl Pts',(39.8284095866455,20.5483957973263,-74.5006800594813));
#156041=CARTESIAN_POINT('Ctrl Pts',(39.8267548791063,20.5485996448687,-74.5046159347301));
#156042=CARTESIAN_POINT('Ctrl Pts',(39.8250994988266,20.5488038771736,-74.5085609314176));
#156043=CARTESIAN_POINT('Ctrl Pts',(39.8234434712545,20.5490084974887,-74.5125150515796));
#156044=CARTESIAN_POINT('Ctrl Pts',(39.7650787544711,20.5562200964616,-74.6518733009648));
#156045=CARTESIAN_POINT('Ctrl Pts',(39.705949287917,20.5639116601681,-74.8025864915926));
#156046=CARTESIAN_POINT('Ctrl Pts',(39.6474445414473,20.5722505834299,-74.9648672153215));
#156047=CARTESIAN_POINT('Ctrl Pts',(39.6282911439158,20.5749805963238,-75.0179949938496));
#156048=CARTESIAN_POINT('Ctrl Pts',(39.6092048952496,20.5777803184013,-75.0723627785656));
#156049=CARTESIAN_POINT('Ctrl Pts',(39.590234879732,20.5806566307811,-75.1279785331065));
#156050=CARTESIAN_POINT('Ctrl Pts',(39.5509555186119,20.5866123303195,-75.2431366522207));
#156051=CARTESIAN_POINT('Ctrl Pts',(39.5121846907435,20.5928834855924,-75.3636377971847));
#156052=CARTESIAN_POINT('Ctrl Pts',(39.4743970636933,20.5994474513941,-75.4894988803743));
#156053=CARTESIAN_POINT('Ctrl Pts',(39.4555032501681,20.602729434295,-75.5524294219692));
#156054=CARTESIAN_POINT('Ctrl Pts',(39.4368554442729,20.6060836803313,-75.616699311578));
#156055=CARTESIAN_POINT('Ctrl Pts',(39.4185130435008,20.6095013265868,-75.682306527728));
#156056=CARTESIAN_POINT('Ctrl Pts',(39.4093418431147,20.6112101497145,-75.715110135803));
#156057=CARTESIAN_POINT('Ctrl Pts',(39.4002469552407,20.6129348140017,-75.7482480687642));
#156058=CARTESIAN_POINT('Ctrl Pts',(39.3912357431359,20.6146737452512,-75.7817197508287));
#156059=CARTESIAN_POINT('Ctrl Pts',(39.3867301370835,20.615543210876,-75.798455591861));
#156060=CARTESIAN_POINT('Ctrl Pts',(39.3822454466591,20.616416242651,-75.8152748697134));
#156061=CARTESIAN_POINT('Ctrl Pts',(39.3777825776534,20.6172926281855,-75.8321775012889));
#156062=CARTESIAN_POINT('Ctrl Pts',(39.3755511431506,20.6177308209527,-75.8406288170767));
#156063=CARTESIAN_POINT('Ctrl Pts',(39.3733251637777,20.6181698521267,-75.8491009712693));
#156064=CARTESIAN_POINT('Ctrl Pts',(39.3711047520856,20.6186096935286,-75.8575939523402));
#156065=CARTESIAN_POINT('Ctrl Pts',(39.3694394433164,20.6189395745801,-75.8639636881434));
#156066=CARTESIAN_POINT('Ctrl Pts',(39.3677772663487,20.6192699113821,-75.8703451390635));
#156067=CARTESIAN_POINT('Ctrl Pts',(39.3661182684645,20.6196006916848,-75.876738299984));
#156068=CARTESIAN_POINT('Ctrl Pts',(39.3655652691698,20.6197109517858,-75.8788693536241));
#156069=CARTESIAN_POINT('Ctrl Pts',(39.364566060937,20.6199104927054,-75.882726903527));
#156070=CARTESIAN_POINT('Ctrl Pts',(39.3644603320247,20.6199316193372,-75.883135364027));
#156071=CARTESIAN_POINT('Ctrl Pts',(39.3632886423492,20.6201657450447,-75.8876619305092));
#156072=CARTESIAN_POINT('Ctrl Pts',(39.3619401943855,20.6204326391343,-75.8928872274733));
#156073=CARTESIAN_POINT('Ctrl Pts',(39.3604179112815,20.6207325043951,-75.8988123848571));
#156074=CARTESIAN_POINT('Ctrl Pts',(39.3561202061195,20.6215790831136,-75.915540271678));
#156075=CARTESIAN_POINT('Ctrl Pts',(39.3504345352844,20.6226880046764,-75.9378370320484));
#156076=CARTESIAN_POINT('Ctrl Pts',(39.3434643999225,20.6240629515274,-75.9657169873842));
#156077=CARTESIAN_POINT('Ctrl Pts',(39.338645331914,20.6250135732928,-75.9849928541872));
#156078=CARTESIAN_POINT('Ctrl Pts',(39.3332133533839,20.6260913571462,-76.0069377298266));
#156079=CARTESIAN_POINT('Ctrl Pts',(39.3272171126794,20.6272975187254,-76.0315582073714));
#156080=CARTESIAN_POINT('Ctrl Pts',(39.3183466318018,20.6290818422292,-76.0679802734658));
#156081=CARTESIAN_POINT('Ctrl Pts',(39.3082381023201,20.6311490838876,-76.1102569728201));
#156082=CARTESIAN_POINT('Ctrl Pts',(39.2970861361385,20.6335337862126,-76.1584224289575));
#156083=CARTESIAN_POINT('Ctrl Pts',(39.2859341699569,20.6359184885376,-76.2065878850949));
#156084=CARTESIAN_POINT('Ctrl Pts',(39.2737387538673,20.638620581188,-76.2606421223469));
#156085=CARTESIAN_POINT('Ctrl Pts',(39.2607519274271,20.6416772034245,-76.320626599082));
#156086=CARTESIAN_POINT('Ctrl Pts',(39.2477651009869,20.6447338256609,-76.3806110758172));
#156087=CARTESIAN_POINT('Ctrl Pts',(39.2339901728747,20.6481374432729,-76.4465224823002));
#156088=CARTESIAN_POINT('Ctrl Pts',(39.2197517386379,20.6518811490863,-76.5183784626765));
#156089=CARTESIAN_POINT('Ctrl Pts',(39.2055133044011,20.6556248548996,-76.5902344430528));
#156090=CARTESIAN_POINT('Ctrl Pts',(39.1908112827616,20.6597090490522,-76.668035292015));
#156091=CARTESIAN_POINT('Ctrl Pts',(39.1760175660153,20.6641379750649,-76.7518070063022));
#156092=CARTESIAN_POINT('Ctrl Pts',(39.1612238492691,20.6685669010776,-76.8355787205894));
#156093=CARTESIAN_POINT('Ctrl Pts',(39.1463417152349,20.6733334101818,-76.9253169916379));
#156094=CARTESIAN_POINT('Ctrl Pts',(39.1318020793478,20.6783942558663,-77.0210185553126));
#156095=CARTESIAN_POINT('Ctrl Pts',(39.1245322614042,20.6809246787086,-77.0688693371499));
#156096=CARTESIAN_POINT('Ctrl Pts',(39.1173488620745,20.6835281179723,-77.1182105829694));
#156097=CARTESIAN_POINT('Ctrl Pts',(39.1103099921676,20.6861952262397,-77.1690393189886));
#156098=CARTESIAN_POINT('Ctrl Pts',(39.1067905572142,20.6875287803734,-77.1944536869981));
#156099=CARTESIAN_POINT('Ctrl Pts',(39.1033072823559,20.6888782545145,-77.2202399296267));
#156100=CARTESIAN_POINT('Ctrl Pts',(39.0998676643283,20.6902421382148,-77.2463974463625));
#156101=CARTESIAN_POINT('Ctrl Pts',(39.0981478553145,20.6909240800649,-77.2594762047304));
#156102=CARTESIAN_POINT('Ctrl Pts',(39.0964389617509,20.6916096244217,-77.2726477817081));
#156103=CARTESIAN_POINT('Ctrl Pts',(39.0947419304685,20.6922985716316,-77.2859120947703));
#156104=CARTESIAN_POINT('Ctrl Pts',(39.0938934148273,20.6926430452366,-77.2925442513014));
#156105=CARTESIAN_POINT('Ctrl Pts',(39.0930478648249,20.6929883695589,-77.2991995918563));
#156106=CARTESIAN_POINT('Ctrl Pts',(39.0922053995177,20.6933345183431,-77.305878105238));
#156107=CARTESIAN_POINT('Ctrl Pts',(39.0913629342106,20.6936806671272,-77.3125566186197));
#156108=CARTESIAN_POINT('Ctrl Pts',(39.0902593691714,20.6941375164164,-77.3213829757033));
#156109=CARTESIAN_POINT('Ctrl Pts',(39.0896873770723,20.6943754114281,-77.3259831523947));
#156110=CARTESIAN_POINT('Ctrl Pts',(39.073847709233,20.700963226138,-77.4533717490315));
#156111=CARTESIAN_POINT('Ctrl Pts',(39.0607443555278,20.70730974043,-77.576098400105));
#156112=CARTESIAN_POINT('Ctrl Pts',(39.0498825952953,20.7134119697754,-77.6941169307647));
#156113=CARTESIAN_POINT('Ctrl Pts',(39.0388132758123,20.7196308076743,-77.8143906978918));
#156114=CARTESIAN_POINT('Ctrl Pts',(39.0300720643756,20.7255959375135,-77.9297747532434));
#156115=CARTESIAN_POINT('Ctrl Pts',(39.0231884656326,20.7313047362494,-78.0402316284843));
#156116=CARTESIAN_POINT('Ctrl Pts',(39.0162316052384,20.7370742933238,-78.1518640883824));
#156117=CARTESIAN_POINT('Ctrl Pts',(39.0111722044164,20.7425820371733,-78.2584640096062));
#156118=CARTESIAN_POINT('Ctrl Pts',(39.007577304562,20.7478257600228,-78.3600031367658));
#156119=CARTESIAN_POINT('Ctrl Pts',(39.0039265968346,20.7531508873704,-78.4631185756265));
#156120=CARTESIAN_POINT('Ctrl Pts',(39.0017862622086,20.7582037355828,-78.5610149408692));
#156121=CARTESIAN_POINT('Ctrl Pts',(39.0007559038223,20.7629824596714,-78.6536722122545));
#156122=CARTESIAN_POINT('Ctrl Pts',(39.0002365147002,20.7653913470468,-78.7003794351757));
#156123=CARTESIAN_POINT('Ctrl Pts',(39.,20.7677305858192,-78.745755534165));
#156124=CARTESIAN_POINT('Ctrl Pts',(39.,20.769999979994,-78.7897987614735));
#156125=CARTESIAN_POINT('Origin',(60.,-2.55003103885676E-14,0.));
#156126=CARTESIAN_POINT('',(60.,27.41999998,-174.34995));
#156127=CARTESIAN_POINT('',(60.,27.91999998,-174.34995));
#156128=CARTESIAN_POINT('',(60.,28.41999998,-174.34995));
#156129=CARTESIAN_POINT('',(60.,27.91999998,-58.24995));
#156130=CARTESIAN_POINT('',(60.,27.91999998,-58.24995));
#156131=CARTESIAN_POINT('',(60.,27.41999998,-58.24995));
#156132=CARTESIAN_POINT('',(60.,-54.58000002,-58.24995));
#156133=CARTESIAN_POINT('',(60.,27.41999998,-174.34995));
#156134=CARTESIAN_POINT('Origin',(57.,-2.42462934179819E-14,-174.34995));
#156135=CARTESIAN_POINT('',(57.,27.91999998,-177.34995));
#156136=CARTESIAN_POINT('',(57.,27.41999998,-177.34995));
#156137=CARTESIAN_POINT('',(57.,-54.58000002,-177.34995));
#156138=CARTESIAN_POINT('Origin',(57.,27.91999998,-174.34995));
#156139=CARTESIAN_POINT('Origin',(57.,27.41999998,-174.34995));
#156140=CARTESIAN_POINT('Origin',(60.,28.41999998,-177.34995));
#156141=CARTESIAN_POINT('',(51.0358975433606,27.41999998,-177.34995));
#156142=CARTESIAN_POINT('',(60.,27.41999998,-177.34995));
#156143=CARTESIAN_POINT('',(50.9656271260094,27.91999998,-177.34995));
#156144=CARTESIAN_POINT('',(51.0717059287548,27.1652100787588,-177.34995));
#156145=CARTESIAN_POINT('',(60.,27.91999998,-177.34995));
#156146=CARTESIAN_POINT('Origin',(0.,-12.9675000200281,-60.64995));
#156147=CARTESIAN_POINT('',(43.0147613882085,26.1152677387813,-61.2273317382593));
#156148=CARTESIAN_POINT('Ctrl Pts',(40.7299249439368,26.1062890581501,-64.8223083020179));
#156149=CARTESIAN_POINT('Ctrl Pts',(41.4984715481572,26.1093587748547,-63.6284010127));
#156150=CARTESIAN_POINT('Ctrl Pts',(42.2597732523974,26.1123503129199,-62.4298580866994));
#156151=CARTESIAN_POINT('Ctrl Pts',(43.0147613882085,26.1152677387813,-61.2273317382593));
#156152=CARTESIAN_POINT('',(47.508501172308,20.508980519813,-61.2273317382593));
#156153=CARTESIAN_POINT('Origin',(0.,-12.9675000200281,-61.2273317382593));
#156154=CARTESIAN_POINT('Ctrl Pts',(47.508501172308,20.508980519813,-61.2273317382593));
#156155=CARTESIAN_POINT('Ctrl Pts',(46.9479652028759,20.506933294733,-62.2124897267371));
#156156=CARTESIAN_POINT('Ctrl Pts',(46.3928886767053,20.5048696025693,-63.1825198713977));
#156157=CARTESIAN_POINT('Ctrl Pts',(45.8431672210077,20.5027903324153,-64.1373805839133));
#156158=CARTESIAN_POINT('Ctrl Pts',(45.2781159650936,20.5006530787213,-65.1188690072553));
#156159=CARTESIAN_POINT('Ctrl Pts',(44.718722664361,20.4984993668521,-66.0843301889488));
#156160=CARTESIAN_POINT('Ctrl Pts',(44.1649210893552,20.4963305571374,-67.0337477577078));
#156161=CARTESIAN_POINT('Ctrl Pts',(43.6014124126742,20.494123732261,-67.9998068336205));
#156162=CARTESIAN_POINT('Ctrl Pts',(43.0436933549281,20.4919012772471,-68.9492550300463));
#156163=CARTESIAN_POINT('Ctrl Pts',(42.4917405921862,20.4896650090889,-69.8821034900559));
#156164=CARTESIAN_POINT('Ctrl Pts',(41.9251450970919,20.4873694150639,-70.8396994488505));
#156165=CARTESIAN_POINT('Ctrl Pts',(41.3646260097972,20.4850592665968,-71.7798033059479));
#156166=CARTESIAN_POINT('Ctrl Pts',(40.810204740074,20.4827369083245,-72.7024556292253));
#156167=CARTESIAN_POINT('Ctrl Pts',(40.7085420530185,20.4823110639438,-72.8716398209669));
#156168=CARTESIAN_POINT('Ctrl Pts',(40.6070845166736,20.4818848099951,-73.0402373040993));
#156169=CARTESIAN_POINT('Ctrl Pts',(40.5058324224785,20.4814581622114,-73.2082484262411));
#156170=CARTESIAN_POINT('Origin',(0.,-12.9675000200281,-60.64995));
#156171=CARTESIAN_POINT('',(36.7055660333102,29.9753365541058,-64.7141088836342));
#156172=CARTESIAN_POINT('',(30.7353086514483,29.741858118838,-73.0207560182717));
#156173=CARTESIAN_POINT('Ctrl Pts',(36.7055660855173,29.9753365749746,-64.7141089388348));
#156174=CARTESIAN_POINT('Ctrl Pts',(36.2220584843733,29.9568079733785,-65.4180278206773));
#156175=CARTESIAN_POINT('Ctrl Pts',(35.7419772179904,29.9382942623995,-66.1100086426196));
#156176=CARTESIAN_POINT('Ctrl Pts',(35.2650854674007,29.9198082912173,-66.7901977895291));
#156177=CARTESIAN_POINT('Ctrl Pts',(34.7683249631423,29.9005521385268,-67.4987256749291));
#156178=CARTESIAN_POINT('Ctrl Pts',(34.2750253842728,29.8813260904984,-68.1944589405539));
#156179=CARTESIAN_POINT('Ctrl Pts',(33.7849656074347,29.8621435250255,-68.8775972447204));
#156180=CARTESIAN_POINT('Ctrl Pts',(33.4153693887468,29.8476763028648,-69.3928105839785));
#156181=CARTESIAN_POINT('Ctrl Pts',(33.0476169663231,29.8332337892929,-69.9008606940659));
#156182=CARTESIAN_POINT('Ctrl Pts',(32.6816291687152,29.8188212963983,-70.4018447451366));
#156183=CARTESIAN_POINT('Ctrl Pts',(32.2720987954213,29.8026941095528,-70.9624322477535));
#156184=CARTESIAN_POINT('Ctrl Pts',(31.8649468060184,29.7866101193311,-71.5139406969673));
#156185=CARTESIAN_POINT('Ctrl Pts',(31.4601541744911,29.7705870470778,-72.0562568439028));
#156186=CARTESIAN_POINT('Ctrl Pts',(31.2177120993998,29.760990363285,-72.3810657504347));
#156187=CARTESIAN_POINT('Ctrl Pts',(30.9761164695227,29.7514154886983,-72.7025782839012));
#156188=CARTESIAN_POINT('Ctrl Pts',(30.7353640256726,29.7418658638113,-73.0207789413775));
#156189=CARTESIAN_POINT('',(30.7601599624812,36.3431985357226,-61.2273317382593));
#156190=CARTESIAN_POINT('Ctrl Pts',(30.7353076117298,29.7418701453522,-73.0207363867594));
#156191=CARTESIAN_POINT('Ctrl Pts',(30.7376555198548,30.3201755188477,-72.011174247587));
#156192=CARTESIAN_POINT('Ctrl Pts',(30.7399863123607,30.9057127448615,-70.982250645273));
#156193=CARTESIAN_POINT('Ctrl Pts',(30.7422975783267,31.4984542632869,-69.933929106915));
#156194=CARTESIAN_POINT('Ctrl Pts',(30.7445647962615,32.0798993332709,-68.9055864460945));
#156195=CARTESIAN_POINT('Ctrl Pts',(30.7468132224327,32.6682765545812,-67.8585780816147));
#156196=CARTESIAN_POINT('Ctrl Pts',(30.7490411044641,33.2636023728865,-66.792894370105));
#156197=CARTESIAN_POINT('Ctrl Pts',(30.7512077501492,33.8425648571132,-65.7565024145669));
#156198=CARTESIAN_POINT('Ctrl Pts',(30.7533549642696,34.4280991321017,-64.7024475949364));
#156199=CARTESIAN_POINT('Ctrl Pts',(30.7554816601947,35.0202624568943,-63.6307456284999));
#156200=CARTESIAN_POINT('Ctrl Pts',(30.7570523555171,35.4576113761063,-62.839228023281));
#156201=CARTESIAN_POINT('Ctrl Pts',(30.7586118691448,35.8985771000441,-62.0380848686548));
#156202=CARTESIAN_POINT('Ctrl Pts',(30.7601599624812,36.3431985357226,-61.2273317382593));
#156203=CARTESIAN_POINT('',(36.7137393100582,32.0861766206928,-61.2273317382593));
#156204=CARTESIAN_POINT('Origin',(0.,-12.9675000200281,-61.2273317382593));
#156205=CARTESIAN_POINT('Ctrl Pts',(36.7137393100582,32.0861766206928,-61.2273317382593));
#156206=CARTESIAN_POINT('Ctrl Pts',(36.7110837808245,31.3874382843756,-62.3925373065787));
#156207=CARTESIAN_POINT('Ctrl Pts',(36.7083607806502,30.6840320430885,-63.5549321813014));
#156208=CARTESIAN_POINT('Ctrl Pts',(36.7055659807394,29.9753365781839,-64.7141088636381));
#156209=CARTESIAN_POINT('Origin',(0.,-12.9675000200281,-171.64995));
#156210=CARTESIAN_POINT('',(38.9938267385724,-56.214502484065,-171.072567687954));
#156211=CARTESIAN_POINT('',(33.5713998621727,-56.0068402847832,-163.25208226359));
#156212=CARTESIAN_POINT('Ctrl Pts',(38.9938273364047,-56.2145025937637,
-171.072567271539));
#156213=CARTESIAN_POINT('Ctrl Pts',(38.5540171403421,-56.1980536322107,
-170.41475390162));
#156214=CARTESIAN_POINT('Ctrl Pts',(38.1169660650788,-56.1815933299574,
-169.766247994682));
#156215=CARTESIAN_POINT('Ctrl Pts',(37.6825967520171,-56.165136805697,-169.127138796781));
#156216=CARTESIAN_POINT('Ctrl Pts',(37.2317386940273,-56.1480555885249,
-168.463768887479));
#156217=CARTESIAN_POINT('Ctrl Pts',(36.7837699246781,-56.1309784443151,
-167.810522543182));
#156218=CARTESIAN_POINT('Ctrl Pts',(36.3386107368843,-56.1139204163073,
-167.167443811692));
#156219=CARTESIAN_POINT('Ctrl Pts',(35.871378908884,-56.0960165881337,-166.492478856456));
#156220=CARTESIAN_POINT('Ctrl Pts',(35.4072422564642,-56.0781338251636,
-165.828714783957));
#156221=CARTESIAN_POINT('Ctrl Pts',(34.9461149698614,-56.0602874301248,
-165.176142950611));
#156222=CARTESIAN_POINT('Ctrl Pts',(34.4849876832587,-56.042441035086,-164.523571117264));
#156223=CARTESIAN_POINT('Ctrl Pts',(34.0268698769957,-56.0246309977758,
-163.882191037155));
#156224=CARTESIAN_POINT('Ctrl Pts',(33.5716804663548,-56.0068706354489,
-163.251940551477));
#156225=CARTESIAN_POINT('',(33.5886122085038,-60.5345771657123,-171.07256826174));
#156226=CARTESIAN_POINT('Ctrl Pts',(33.5712930253539,-56.0068938993568,
-163.252219719633));
#156227=CARTESIAN_POINT('Ctrl Pts',(33.5735544942697,-56.5714984856234,
-164.209913770145));
#156228=CARTESIAN_POINT('Ctrl Pts',(33.5758020709476,-57.1422670958701,
-165.18499894682));
#156229=CARTESIAN_POINT('Ctrl Pts',(33.5780337735611,-57.7192031690627,
-166.177497602729));
#156230=CARTESIAN_POINT('Ctrl Pts',(33.5802053064641,-58.2805842680772,
-167.143237157098));
#156231=CARTESIAN_POINT('Ctrl Pts',(33.5823618086959,-58.8478046711717,
-168.125463912336));
#156232=CARTESIAN_POINT('Ctrl Pts',(33.5845018265016,-59.4209095564351,
-169.124173270749));
#156233=CARTESIAN_POINT('Ctrl Pts',(33.5858788715011,-59.7896874303229,
-169.766816394718));
#156234=CARTESIAN_POINT('Ctrl Pts',(33.5872490985137,-60.1609026711095,
-170.416283768652));
#156235=CARTESIAN_POINT('Ctrl Pts',(33.5886122085038,-60.5345771657124,
-171.07256826174));
#156236=CARTESIAN_POINT('Origin',(0.,-12.9675000200281,-171.07256826174));
#156237=CARTESIAN_POINT('Origin',(-3.54807775957937E-14,-73.08000002,3.11172719585489E-30));
#156238=CARTESIAN_POINT('',(32.85,-73.08000002,-58.24995));
#156239=CARTESIAN_POINT('',(32.35,-73.08000002,-58.24995));
#156240=CARTESIAN_POINT('',(-41.5,-73.0800000199999,-58.24995));
#156241=CARTESIAN_POINT('',(32.35,-73.08000002,-174.34995));
#156242=CARTESIAN_POINT('',(32.35,-73.08000002,-174.34995));
#156243=CARTESIAN_POINT('',(32.85,-73.08000002,-174.34995));
#156244=CARTESIAN_POINT('',(41.5,-73.08000002,-174.34995));
#156245=CARTESIAN_POINT('',(32.85,-73.08000002,-58.24995));
#156246=CARTESIAN_POINT('Origin',(-3.3975957231091E-14,-70.08000002,-174.34995));
#156247=CARTESIAN_POINT('',(32.35,-70.08000002,-177.34995));
#156248=CARTESIAN_POINT('Origin',(32.35,-70.08000002,-174.34995));
#156249=CARTESIAN_POINT('',(32.85,-70.08000002,-177.34995));
#156250=CARTESIAN_POINT('',(-41.5,-70.08000002,-177.34995));
#156251=CARTESIAN_POINT('Origin',(32.85,-70.08000002,-174.34995));
#156252=CARTESIAN_POINT('Origin',(41.5,-73.08000002,-177.34995));
#156253=CARTESIAN_POINT('',(32.35,-65.1329945223129,-177.34995));
#156254=CARTESIAN_POINT('',(32.35,-73.08000002,-177.34995));
#156255=CARTESIAN_POINT('',(32.85,-65.0627241049617,-177.34995));
#156256=CARTESIAN_POINT('',(40.227526467895,-64.0258803771248,-177.34995));
#156257=CARTESIAN_POINT('',(32.85,-73.08000002,-177.34995));
#156258=CARTESIAN_POINT('Origin',(0.,-12.9675000200281,-171.64995));
#156259=CARTESIAN_POINT('',(29.958978566972,-63.954289311524,-171.64995));
#156260=CARTESIAN_POINT('',(31.35,-63.7587939982373,-171.64995));
#156261=CARTESIAN_POINT('',(31.7108268990399,-63.7080830846632,-171.64995));
#156262=CARTESIAN_POINT('',(31.35,-63.1109998882233,-171.64995));
#156263=CARTESIAN_POINT('',(31.35,-62.7949079300497,-171.64995));
#156264=CARTESIAN_POINT('Origin',(0.,-12.9675000200281,-171.64995));
#156265=CARTESIAN_POINT('Ctrl Pts',(33.787119065489,-54.58000002,-74.2342847034403));
#156266=CARTESIAN_POINT('Ctrl Pts',(32.2532076658177,-54.58000002,-73.0155274500394));
#156267=CARTESIAN_POINT('Ctrl Pts',(31.127610916576,-55.9109590653435,-72.1211933947368));
#156268=CARTESIAN_POINT('Ctrl Pts',(31.2221856658751,-54.58000002,-77.4624751982426));
#156269=CARTESIAN_POINT('Ctrl Pts',(29.795197677401,-54.58000002,-76.2393546649806));
#156270=CARTESIAN_POINT('Ctrl Pts',(28.6950527991335,-55.8150223013088,
-75.3493568083322));
#156271=CARTESIAN_POINT('Ctrl Pts',(28.5158034471915,-54.58000002,-80.6345530934811));
#156272=CARTESIAN_POINT('Ctrl Pts',(27.1955581318591,-54.5800000200432,
-79.4258937131132));
#156273=CARTESIAN_POINT('Ctrl Pts',(26.1438256035288,-55.7129660087519,
-78.5213783677229));
#156274=CARTESIAN_POINT('Ctrl Pts',(25.6489781920928,-54.58000002,-83.5984279079175));
#156275=CARTESIAN_POINT('Ctrl Pts',(24.4312617378937,-54.58000002,-82.420584542654));
#156276=CARTESIAN_POINT('Ctrl Pts',(23.4643531971916,-55.6098288961396,
-81.485336599214));
#156277=CARTESIAN_POINT('',(31.3499999999941,-54.58000002,-77.227263173365));
#156278=CARTESIAN_POINT('',(25.7,-54.58000002,-83.5456386250818));
#156279=CARTESIAN_POINT('Ctrl Pts',(31.3499999999855,-54.58000002,-77.227263173365));
#156280=CARTESIAN_POINT('Ctrl Pts',(29.5376330958494,-54.58000002,-79.396334075655));
#156281=CARTESIAN_POINT('Ctrl Pts',(27.6634733215002,-54.58000002,-81.5125991939361));
#156282=CARTESIAN_POINT('Ctrl Pts',(25.7,-54.58000002,-83.5456386250818));
#156283=CARTESIAN_POINT('',(31.0842852491211,-55.9092501930853,-72.1786663403249));
#156284=CARTESIAN_POINT('Ctrl Pts',(31.3500000000008,-54.58000002,-77.2272631733646));
#156285=CARTESIAN_POINT('Ctrl Pts',(31.3453107206565,-54.5800000199999,
-77.1375720242367));
#156286=CARTESIAN_POINT('Ctrl Pts',(31.3403970685239,-54.5810786430591,
-77.0428817158067));
#156287=CARTESIAN_POINT('Ctrl Pts',(31.3352210588623,-54.5836402116848,
-76.9431962742989));
#156288=CARTESIAN_POINT('Ctrl Pts',(31.3300450492006,-54.5862017803106,
-76.843510832791));
#156289=CARTESIAN_POINT('Ctrl Pts',(31.3246066855266,-54.5902459987653,
-76.7388301777383));
#156290=CARTESIAN_POINT('Ctrl Pts',(31.3188661644989,-54.5962369768836,
-76.6291669959942));
#156291=CARTESIAN_POINT('Ctrl Pts',(31.3131256434712,-54.6022279550019,
-76.51950381425));
#156292=CARTESIAN_POINT('Ctrl Pts',(31.3070902307353,-54.6101659107058,
-76.4048625539582));
#156293=CARTESIAN_POINT('Ctrl Pts',(31.3007798943886,-54.6205652232166,
-76.2853053463729));
#156294=CARTESIAN_POINT('Ctrl Pts',(31.2976247262152,-54.6257648794721,
-76.2255267425802));
#156295=CARTESIAN_POINT('Ctrl Pts',(31.2944015900026,-54.6315806184543,
-76.164519829024));
#156296=CARTESIAN_POINT('Ctrl Pts',(31.2911181260652,-54.6380804273865,
-76.1022968571952));
#156297=CARTESIAN_POINT('Ctrl Pts',(31.2894763940964,-54.6413303318526,
-76.0711853712808));
#156298=CARTESIAN_POINT('Ctrl Pts',(31.2878195895528,-54.6447512961395,
-76.0397698784925));
#156299=CARTESIAN_POINT('Ctrl Pts',(31.2861490867532,-54.6483519686845,
-76.0080522698309));
#156300=CARTESIAN_POINT('Ctrl Pts',(31.2853138353534,-54.650152304957,-75.9921934655001));
#156301=CARTESIAN_POINT('Ctrl Pts',(31.284475159829,-54.6519975703892,-75.9762591325628));
#156302=CARTESIAN_POINT('Ctrl Pts',(31.2836332475183,-54.6538888551562,
-75.9602495203746));
#156303=CARTESIAN_POINT('Ctrl Pts',(31.283212291363,-54.6548344975397,-75.9522447142805));
#156304=CARTESIAN_POINT('Ctrl Pts',(31.2827905260398,-54.6557916448769,
-75.9442210883976));
#156305=CARTESIAN_POINT('Ctrl Pts',(31.2823679765381,-54.656760433808,-75.9361786752311));
#156306=CARTESIAN_POINT('Ctrl Pts',(31.2819454270365,-54.657729222739,-75.9281362620647));
#156307=CARTESIAN_POINT('Ctrl Pts',(31.2814519788643,-54.6588736933179,
-75.9187392181045));
#156308=CARTESIAN_POINT('Ctrl Pts',(31.2810980010362,-54.6597018623565,
-75.9119951068502));
#156309=CARTESIAN_POINT('Ctrl Pts',(31.2722272916116,-54.6804558370728,
-75.7429872015412));
#156310=CARTESIAN_POINT('Ctrl Pts',(31.2633507615356,-54.705371481956,-75.574005469165));
#156311=CARTESIAN_POINT('Ctrl Pts',(31.2544854003494,-54.7345127723453,
-75.4053367307167));
#156312=CARTESIAN_POINT('Ctrl Pts',(31.2520303003698,-54.7425829208636,
-75.3586270019613));
#156313=CARTESIAN_POINT('Ctrl Pts',(31.2495760556688,-54.7509768357141,
-75.3119412323424));
#156314=CARTESIAN_POINT('Ctrl Pts',(31.2471230238481,-54.7596951726748,
-75.2652854092562));
#156315=CARTESIAN_POINT('Ctrl Pts',(31.2385625508759,-54.7901200074795,
-75.1024681521939));
#156316=CARTESIAN_POINT('Ctrl Pts',(31.2300160506949,-54.8244995244996,
-74.940017336389));
#156317=CARTESIAN_POINT('Ctrl Pts',(31.2214979294548,-54.862827933893,-74.7781981331342));
#156318=CARTESIAN_POINT('Ctrl Pts',(31.2191128026884,-54.8735601261897,
-74.7328877528154));
#156319=CARTESIAN_POINT('Ctrl Pts',(31.2167299031896,-54.8846016101691,
-74.6876269284716));
#156320=CARTESIAN_POINT('Ctrl Pts',(31.2143495510005,-54.8959515162524,
-74.6424215363045));
#156321=CARTESIAN_POINT('Ctrl Pts',(31.2140609162468,-54.8973277736659,
-74.6369400586917));
#156322=CARTESIAN_POINT('Ctrl Pts',(31.2138228813912,-54.8984661601923,
-74.632419632326));
#156323=CARTESIAN_POINT('Ctrl Pts',(31.2135285145844,-54.8999595685782,
-74.6264903392875));
#156324=CARTESIAN_POINT('Ctrl Pts',(31.2134648969398,-54.9002823193833,
-74.6252089188002));
#156325=CARTESIAN_POINT('Ctrl Pts',(31.2133986476546,-54.9006217246293,
-74.6238616838906));
#156326=CARTESIAN_POINT('Ctrl Pts',(31.2133286878654,-54.9009838833262,
-74.6224247205651));
#156327=CARTESIAN_POINT('Ctrl Pts',(31.2078839743254,-54.9291693650911,
-74.5105911405694));
#156328=CARTESIAN_POINT('Ctrl Pts',(31.2024129074911,-54.9587960031325,
-74.4012817764876));
#156329=CARTESIAN_POINT('Ctrl Pts',(31.1969474187156,-54.9896805561478,
-74.2945231806525));
#156330=CARTESIAN_POINT('Ctrl Pts',(31.1960901136078,-54.994525042367,-74.2777772511894));
#156331=CARTESIAN_POINT('Ctrl Pts',(31.1952329460617,-54.999400523412,-74.2610939879282));
#156332=CARTESIAN_POINT('Ctrl Pts',(31.1943760394873,-55.0043063412549,
-74.2444733920645));
#156333=CARTESIAN_POINT('Ctrl Pts',(31.1896361485215,-55.0314423702774,
-74.1525382680613));
#156334=CARTESIAN_POINT('Ctrl Pts',(31.1849043296596,-55.0595054546659,
-74.0625245652527));
#156335=CARTESIAN_POINT('Ctrl Pts',(31.1802158006127,-55.0883755446775,
-73.9744474139547));
#156336=CARTESIAN_POINT('Ctrl Pts',(31.1743848787859,-55.1242800333362,
-73.8649096508721));
#156337=CARTESIAN_POINT('Ctrl Pts',(31.1686235363137,-55.1614471793065,
-73.7583217249963));
#156338=CARTESIAN_POINT('Ctrl Pts',(31.1630045098354,-55.1996179865692,
-73.6547813901237));
#156339=CARTESIAN_POINT('Ctrl Pts',(31.1576629693929,-55.2359037936395,
-73.5563542180359));
#156340=CARTESIAN_POINT('Ctrl Pts',(31.152450076667,-55.2730964685128,-73.4606804383564));
#156341=CARTESIAN_POINT('Ctrl Pts',(31.1474257337304,-55.3109734535205,
-73.3678004487643));
#156342=CARTESIAN_POINT('Ctrl Pts',(31.1449858887296,-55.3293666989023,
-73.3226974808467));
#156343=CARTESIAN_POINT('Ctrl Pts',(31.1425895372687,-55.3479189876124,
-73.2782350785174));
#156344=CARTESIAN_POINT('Ctrl Pts',(31.1402427759134,-55.3666136886743,
-73.2344049908577));
#156345=CARTESIAN_POINT('Ctrl Pts',(31.1336254850984,-55.4193281555054,
-73.1108149053839));
#156346=CARTESIAN_POINT('Ctrl Pts',(31.1273335379019,-55.4731591730317,
-72.9923884427035));
#156347=CARTESIAN_POINT('Ctrl Pts',(31.1213310258052,-55.5277148075479,
-72.8790684585829));
#156348=CARTESIAN_POINT('Ctrl Pts',(31.1174456970023,-55.5630277856362,
-72.8057182693366));
#156349=CARTESIAN_POINT('Ctrl Pts',(31.1136816088053,-55.5986432025572,
-72.7345071180142));
#156350=CARTESIAN_POINT('Ctrl Pts',(31.1100289108462,-55.6344440246039,
-72.6654155838679));
#156351=CARTESIAN_POINT('Ctrl Pts',(31.103673361896,-55.6967360289041,-72.5451990665901));
#156352=CARTESIAN_POINT('Ctrl Pts',(31.0976553569188,-55.7595906037036,
-72.4314038795334));
#156353=CARTESIAN_POINT('Ctrl Pts',(31.0919676912673,-55.8223273129114,
-72.3238825741213));
#156354=CARTESIAN_POINT('Ctrl Pts',(31.0893364096103,-55.8513511624607,
-72.2741400512662));
#156355=CARTESIAN_POINT('Ctrl Pts',(31.0867758098859,-55.8803490121959,
-72.2257399755741));
#156356=CARTESIAN_POINT('Ctrl Pts',(31.0842850954296,-55.9092502064055,
-72.1786663566349));
#156357=CARTESIAN_POINT('',(25.4680306998147,-55.6875937661705,-79.20421297481));
#156358=CARTESIAN_POINT('Ctrl Pts',(25.4683317135053,-55.6876147553279,
-79.2043632295083));
#156359=CARTESIAN_POINT('Ctrl Pts',(25.860615391601,-55.7029545756699,-78.7454945043951));
#156360=CARTESIAN_POINT('Ctrl Pts',(26.2547029404868,-55.7184229037236,
-78.2773837565957));
#156361=CARTESIAN_POINT('Ctrl Pts',(26.6507273376328,-55.7340096395059,
-77.7999327473883));
#156362=CARTESIAN_POINT('Ctrl Pts',(27.0210025496724,-55.7485829383693,
-77.3535252155626));
#156363=CARTESIAN_POINT('Ctrl Pts',(27.3929707792159,-55.7632597430092,
-76.8989523765739));
#156364=CARTESIAN_POINT('Ctrl Pts',(27.7667262123628,-55.778029204186,-76.4361762559085));
#156365=CARTESIAN_POINT('Ctrl Pts',(28.1285322965327,-55.7923264703655,
-75.9881955679608));
#156366=CARTESIAN_POINT('Ctrl Pts',(28.4920130741863,-55.8067105712765,
-75.5325274217445));
#156367=CARTESIAN_POINT('Ctrl Pts',(28.8572413086363,-55.8211691061762,
-75.0691821389535));
#156368=CARTESIAN_POINT('Ctrl Pts',(29.2247961803246,-55.8357197472236,
-74.6028851774929));
#156369=CARTESIAN_POINT('Ctrl Pts',(29.5941208661498,-55.8503458004071,
-74.1288122836977));
#156370=CARTESIAN_POINT('Ctrl Pts',(29.96527663479,-55.8650317084468,-73.6470279022662));
#156371=CARTESIAN_POINT('Ctrl Pts',(30.3095833935785,-55.8786552536649,
-73.2000952857711));
#156372=CARTESIAN_POINT('Ctrl Pts',(30.6554657752219,-55.8923302944832,
-72.7465266201201));
#156373=CARTESIAN_POINT('Ctrl Pts',(31.0029626442895,-55.9060418772438,
-72.286422310765));
#156374=CARTESIAN_POINT('Ctrl Pts',(31.0300604186516,-55.9071111052251,
-72.250543418413));
#156375=CARTESIAN_POINT('Ctrl Pts',(31.0571680056025,-55.9081805540986,
-72.2146248096625));
#156376=CARTESIAN_POINT('Ctrl Pts',(31.0842854210862,-55.9092502160976,
-72.1786665455479));
#156377=CARTESIAN_POINT('Ctrl Pts',(25.4680306998147,-55.6875937661705,
-79.20421297481));
#156378=CARTESIAN_POINT('Ctrl Pts',(25.4683278290903,-55.6871423789816,
-79.205235636863));
#156379=CARTESIAN_POINT('Ctrl Pts',(25.4685596245448,-55.6842213655928,
-79.2103525600497));
#156380=CARTESIAN_POINT('Ctrl Pts',(25.4692817313297,-55.6758960492355,
-79.224980571896));
#156381=CARTESIAN_POINT('Ctrl Pts',(25.4697672929732,-55.6704183548359,
-79.2346152157047));
#156382=CARTESIAN_POINT('Ctrl Pts',(25.4705320388274,-55.66214441212,-79.2492396837741));
#156383=CARTESIAN_POINT('Ctrl Pts',(25.4709043683141,-55.658198381398,-79.2562346877634));
#156384=CARTESIAN_POINT('Ctrl Pts',(25.4711627415284,-55.6554792098156,
-79.2610599241439));
#156385=CARTESIAN_POINT('Ctrl Pts',(25.4713670581236,-55.6533481293772,
-79.2648467294586));
#156386=CARTESIAN_POINT('Ctrl Pts',(25.472547099263,-55.6410978948656,-79.2866308125499));
#156387=CARTESIAN_POINT('Ctrl Pts',(25.4736967231167,-55.6293072323705,
-79.307839175783));
#156388=CARTESIAN_POINT('Ctrl Pts',(25.4770338679804,-55.5955045885169,
-79.3693302774191));
#156389=CARTESIAN_POINT('Ctrl Pts',(25.4793891057231,-55.5722204188109,
-79.4126816839331));
#156390=CARTESIAN_POINT('Ctrl Pts',(25.4838233290034,-55.5293901492856,
-79.4942352738236));
#156391=CARTESIAN_POINT('Ctrl Pts',(25.4872055392468,-55.497440282494,-79.5564379815909));
#156392=CARTESIAN_POINT('Ctrl Pts',(25.490671225521,-55.4658071514793,-79.6202024646101));
#156393=CARTESIAN_POINT('Ctrl Pts',(25.4929998345068,-55.4447953387203,
-79.6630595960062));
#156394=CARTESIAN_POINT('Ctrl Pts',(25.494272991468,-55.4334480988312,-79.6864995491182));
#156395=CARTESIAN_POINT('Ctrl Pts',(25.4996853335514,-55.3857186867812,
-79.7861924995833));
#156396=CARTESIAN_POINT('Ctrl Pts',(25.504170022895,-55.3477170112747,-79.8690767460442));
#156397=CARTESIAN_POINT('Ctrl Pts',(25.5111409036076,-55.291348542635,-79.9981497038913));
#156398=CARTESIAN_POINT('Ctrl Pts',(25.5146868706228,-55.2633232496154,
-80.0638724996628));
#156399=CARTESIAN_POINT('Ctrl Pts',(25.5189273312081,-55.2309885305297,
-80.1426326343882));
#156400=CARTESIAN_POINT('Ctrl Pts',(25.5210727305464,-55.2149222425954,
-80.1825342051072));
#156401=CARTESIAN_POINT('Ctrl Pts',(25.5219974942784,-55.2080595018384,
-80.1997466864495));
#156402=CARTESIAN_POINT('Ctrl Pts',(25.5226151719892,-55.2034895393514,
-80.2112465257512));
#156403=CARTESIAN_POINT('Ctrl Pts',(25.5230043996644,-55.20062028382,-80.2184954847682));
#156404=CARTESIAN_POINT('Ctrl Pts',(25.530600911193,-55.1447563858798,-80.3600047810412));
#156405=CARTESIAN_POINT('Ctrl Pts',(25.5388664494851,-55.0868589761765,
-80.5174942954816));
#156406=CARTESIAN_POINT('Ctrl Pts',(25.5531250311004,-54.9992784182683,
-80.7851227928128));
#156407=CARTESIAN_POINT('Ctrl Pts',(25.5581822585155,-54.9699767299778,
-80.8795612335467));
#156408=CARTESIAN_POINT('Ctrl Pts',(25.5662146791705,-54.9265911279604,
-81.0291346039942));
#156409=CARTESIAN_POINT('Ctrl Pts',(25.5703415777611,-54.9050412831635,
-81.105899507708));
#156410=CARTESIAN_POINT('Ctrl Pts',(25.5753363913883,-54.880321616272,-81.1989275171106));
#156411=CARTESIAN_POINT('Ctrl Pts',(25.5778761532825,-54.8680895188335,
-81.246308880565));
#156412=CARTESIAN_POINT('Ctrl Pts',(25.5789733849926,-54.8628769662688,
-81.2668010318613));
#156413=CARTESIAN_POINT('Ctrl Pts',(25.5797067823245,-54.85940881693,-81.28050376331));
#156414=CARTESIAN_POINT('Ctrl Pts',(25.58013492075,-54.8573947781028,-81.2885068528041));
#156415=CARTESIAN_POINT('Ctrl Pts',(25.6001616759959,-54.7635577145736,
-81.6630099302082));
#156416=CARTESIAN_POINT('Ctrl Pts',(25.6214848628736,-54.6947552928938,
-82.036220275339));
#156417=CARTESIAN_POINT('Ctrl Pts',(25.6583907318718,-54.6035691563163,
-82.7847463047849));
#156418=CARTESIAN_POINT('Ctrl Pts',(25.6799145825718,-54.5800000497493,
-83.1644838191851));
#156419=CARTESIAN_POINT('Ctrl Pts',(25.7,-54.58000002,-83.5456386250818));
#156420=CARTESIAN_POINT('Origin',(60.,-54.58000002,-55.24995));
#156421=CARTESIAN_POINT('',(25.7,-54.58000002,-148.513004346424));
#156422=CARTESIAN_POINT('',(31.3500000000003,-54.58000002,-154.831379798158));
#156423=CARTESIAN_POINT('Ctrl Pts',(25.7,-54.58000002,-148.513004346424));
#156424=CARTESIAN_POINT('Ctrl Pts',(27.6634746333275,-54.58000002,-150.546045135875));
#156425=CARTESIAN_POINT('Ctrl Pts',(29.537631721855,-54.58000002,-152.662307251431));
#156426=CARTESIAN_POINT('Ctrl Pts',(31.35,-54.58000002,-154.831379798159));
#156427=CARTESIAN_POINT('',(31.35,-54.58000002,-76.6255854122387));
#156428=CARTESIAN_POINT('',(25.7,-54.58000002,-147.999168907581));
#156429=CARTESIAN_POINT('Ctrl Pts',(31.1276111727346,-55.910959075446,-159.937449916708));
#156430=CARTESIAN_POINT('Ctrl Pts',(32.2532079260876,-54.58000002,-159.043115862826));
#156431=CARTESIAN_POINT('Ctrl Pts',(33.7871193355851,-54.58000002,-157.824358608005));
#156432=CARTESIAN_POINT('Ctrl Pts',(28.6950259327511,-55.8150212418279,
-156.709250494305));
#156433=CARTESIAN_POINT('Ctrl Pts',(29.7951706706344,-54.5800000200427,
-155.819252869409));
#156434=CARTESIAN_POINT('Ctrl Pts',(31.2221573047513,-54.58000002,-154.596132061548));
#156435=CARTESIAN_POINT('Ctrl Pts',(26.143809437084,-55.7129653866513,-153.537246733037));
#156436=CARTESIAN_POINT('Ctrl Pts',(27.1955413535444,-54.5800000200432,
-152.632731094415));
#156437=CARTESIAN_POINT('Ctrl Pts',(28.5157861483817,-54.58000002,-151.424072006624));
#156438=CARTESIAN_POINT('Ctrl Pts',(23.4643533331708,-55.6098289013737,
-150.573306522708));
#156439=CARTESIAN_POINT('Ctrl Pts',(24.4312618773724,-54.5800000199999,
-149.638058579956));
#156440=CARTESIAN_POINT('Ctrl Pts',(25.6489783375839,-54.58000002,-148.460215214005));
#156441=CARTESIAN_POINT('',(31.0842852491456,-55.9092501930801,-159.879976631169));
#156442=CARTESIAN_POINT('',(25.4680827049418,-55.6876414657738,-152.854491724755));
#156443=CARTESIAN_POINT('Ctrl Pts',(31.0842854211464,-55.9092502161047,
-159.87997642591));
#156444=CARTESIAN_POINT('Ctrl Pts',(30.7346533861529,-55.8954587801339,
-159.4163569811));
#156445=CARTESIAN_POINT('Ctrl Pts',(30.386656089505,-55.8817029991764,-158.959334162683));
#156446=CARTESIAN_POINT('Ctrl Pts',(30.0402547234154,-55.8679982667367,
-158.509013875888));
#156447=CARTESIAN_POINT('Ctrl Pts',(29.6827133608912,-55.8538528008432,
-158.044211641617));
#156448=CARTESIAN_POINT('Ctrl Pts',(29.3268722787328,-55.8397617134658,
-157.586549708062));
#156449=CARTESIAN_POINT('Ctrl Pts',(28.9726777824063,-55.8257391217459,
-157.136090072484));
#156450=CARTESIAN_POINT('Ctrl Pts',(28.5999643590844,-55.8109833640537,
-156.662078323047));
#156451=CARTESIAN_POINT('Ctrl Pts',(28.2290743062977,-55.7963034531147,
-156.196041547281));
#156452=CARTESIAN_POINT('Ctrl Pts',(27.8599317931223,-55.781712801269,-155.737995624991));
#156453=CARTESIAN_POINT('Ctrl Pts',(27.4782730833951,-55.7666274367858,
-155.264419134997));
#156454=CARTESIAN_POINT('Ctrl Pts',(27.0984824976563,-55.7516374773747,
-154.799384179417));
#156455=CARTESIAN_POINT('Ctrl Pts',(26.7204611045877,-55.7367546582871,
-154.342854013806));
#156456=CARTESIAN_POINT('Ctrl Pts',(26.3230166169315,-55.7211071459622,
-153.86286689906));
#156457=CARTESIAN_POINT('Ctrl Pts',(25.9275279292449,-55.7055780633222,
-153.392280661765));
#156458=CARTESIAN_POINT('Ctrl Pts',(25.5338619724156,-55.6901777816033,
-152.930999011426));
#156459=CARTESIAN_POINT('Ctrl Pts',(25.512012978637,-55.68932304511,-152.90539725508));
#156460=CARTESIAN_POINT('Ctrl Pts',(25.4901695948933,-55.688468704589,-152.879824148347));
#156461=CARTESIAN_POINT('Ctrl Pts',(25.468331796778,-55.6876147615411,-152.854279670573));
#156462=CARTESIAN_POINT('Ctrl Pts',(31.0842850954302,-55.909250206398,-159.879976614859));
#156463=CARTESIAN_POINT('Ctrl Pts',(31.0895854115311,-55.8477481146612,
-159.779803440199));
#156464=CARTESIAN_POINT('Ctrl Pts',(31.0951600653657,-55.7862957665143,
-159.6744189526));
#156465=CARTESIAN_POINT('Ctrl Pts',(31.1010151755717,-55.7254297048882,
-159.563699979791));
#156466=CARTESIAN_POINT('Ctrl Pts',(31.1048957464655,-55.6850897183029,
-159.490319153784));
#156467=CARTESIAN_POINT('Ctrl Pts',(31.1088994942666,-55.6450065439528,
-159.414595376028));
#156468=CARTESIAN_POINT('Ctrl Pts',(31.1130279364408,-55.6053242693568,
-159.336497304981));
#156469=CARTESIAN_POINT('Ctrl Pts',(31.1182320407174,-55.5553028118145,
-159.238050847847));
#156470=CARTESIAN_POINT('Ctrl Pts',(31.1236338630895,-55.505924294484,-159.135838743465));
#156471=CARTESIAN_POINT('Ctrl Pts',(31.1292335128526,-55.4574651316412,
-159.029851363251));
#156472=CARTESIAN_POINT('Ctrl Pts',(31.134430377709,-55.412491654549,-158.93148769503));
#156473=CARTESIAN_POINT('Ctrl Pts',(31.1397976024776,-55.3683104260197,
-158.829872916478));
#156474=CARTESIAN_POINT('Ctrl Pts',(31.1453337206069,-55.3251129589623,
-158.725027925676));
#156475=CARTESIAN_POINT('Ctrl Pts',(31.1457047307718,-55.3222180244603,
-158.718001602099));
#156476=CARTESIAN_POINT('Ctrl Pts',(31.1461718442569,-55.3185888253415,
-158.709155023414));
#156477=CARTESIAN_POINT('Ctrl Pts',(31.1464490733754,-55.3164414031806,
-158.703905479327));
#156478=CARTESIAN_POINT('Ctrl Pts',(31.1466037171372,-55.315243529584,-158.700977182148));
#156479=CARTESIAN_POINT('Ctrl Pts',(31.1467586734147,-55.3140450063871,
-158.698042922972));
#156480=CARTESIAN_POINT('Ctrl Pts',(31.1469139423337,-55.3128458487235,
-158.695102699558));
#156481=CARTESIAN_POINT('Ctrl Pts',(31.1533714787286,-55.2629736379607,
-158.572820662532));
#156482=CARTESIAN_POINT('Ctrl Pts',(31.1603704172416,-55.2120214585731,
-158.440211131639));
#156483=CARTESIAN_POINT('Ctrl Pts',(31.1679235634068,-55.1612687635298,
-158.297038080203));
#156484=CARTESIAN_POINT('Ctrl Pts',(31.1706072274891,-55.1432361210005,
-158.246168102674));
#156485=CARTESIAN_POINT('Ctrl Pts',(31.1733608621816,-55.1252291692777,
-158.193964379686));
#156486=CARTESIAN_POINT('Ctrl Pts',(31.1761850567432,-55.1073066058283,
-158.140415804507));
#156487=CARTESIAN_POINT('Ctrl Pts',(31.182154073824,-55.0694267483942,-158.027239338468));
#156488=CARTESIAN_POINT('Ctrl Pts',(31.1884373070365,-55.0319283050599,
-157.908064907983));
#156489=CARTESIAN_POINT('Ctrl Pts',(31.1950355152709,-54.9953865838879,
-157.782861954481));
#156490=CARTESIAN_POINT('Ctrl Pts',(31.200367630056,-54.9658566501828,-157.681683498786));
#156491=CARTESIAN_POINT('Ctrl Pts',(31.2059053736433,-54.9369522328227,
-157.576569309603));
#156492=CARTESIAN_POINT('Ctrl Pts',(31.211647603869,-54.9089746582482,-157.467531218779));
#156493=CARTESIAN_POINT('Ctrl Pts',(31.211851539337,-54.9079810338998,-157.463658727915));
#156494=CARTESIAN_POINT('Ctrl Pts',(31.2121280280077,-54.9066380554768,
-157.458408449884));
#156495=CARTESIAN_POINT('Ctrl Pts',(31.2122601928806,-54.9059973007545,
-157.45589890854));
#156496=CARTESIAN_POINT('Ctrl Pts',(31.212464012248,-54.9050091545155,-157.452028794511));
#156497=CARTESIAN_POINT('Ctrl Pts',(31.2126695003386,-54.9040153265436,
-157.448126913748));
#156498=CARTESIAN_POINT('Ctrl Pts',(31.2128766588162,-54.9030159233487,
-157.444193233984));
#156499=CARTESIAN_POINT('Ctrl Pts',(31.2156323833892,-54.8897213675319,
-157.391865479322));
#156500=CARTESIAN_POINT('Ctrl Pts',(31.2186822770619,-54.8754481380802,
-157.333937612989));
#156501=CARTESIAN_POINT('Ctrl Pts',(31.2220286788944,-54.8604870397,-157.270362719997));
#156502=CARTESIAN_POINT('Ctrl Pts',(31.2236506557137,-54.8532355032798,
-157.239548428142));
#156503=CARTESIAN_POINT('Ctrl Pts',(31.2253422855029,-54.8458231472352,
-157.207407563133));
#156504=CARTESIAN_POINT('Ctrl Pts',(31.2271037881024,-54.8382874305316,
-157.173935514171));
#156505=CARTESIAN_POINT('Ctrl Pts',(31.230750984607,-54.8226847061137,-157.104631534711));
#156506=CARTESIAN_POINT('Ctrl Pts',(31.2346975404456,-54.8065505635224,
-157.02962198736));
#156507=CARTESIAN_POINT('Ctrl Pts',(31.2389443632973,-54.7902552512034,
-156.948879688243));
#156508=CARTESIAN_POINT('Ctrl Pts',(31.2404734082391,-54.7843882146574,
-156.919808872633));
#156509=CARTESIAN_POINT('Ctrl Pts',(31.242041368692,-54.7785007447406,-156.889995055113));
#156510=CARTESIAN_POINT('Ctrl Pts',(31.243648253759,-54.7726116560897,-156.859437531544));
#156511=CARTESIAN_POINT('Ctrl Pts',(31.2440818183164,-54.7710226811428,
-156.851192598878));
#156512=CARTESIAN_POINT('Ctrl Pts',(31.2445182165278,-54.7694335927254,
-156.842893526154));
#156513=CARTESIAN_POINT('Ctrl Pts',(31.244957689739,-54.7678447199691,-156.834540313013));
#156514=CARTESIAN_POINT('Ctrl Pts',(31.2453971629501,-54.7662558472127,
-156.826187099872));
#156515=CARTESIAN_POINT('Ctrl Pts',(31.2457373617316,-54.7650314393738,
-156.819720368753));
#156516=CARTESIAN_POINT('Ctrl Pts',(31.2462842962207,-54.7630793515511,
-156.809318204654));
#156517=CARTESIAN_POINT('Ctrl Pts',(31.2499077279959,-54.7501468026159,
-156.740404042759));
#156518=CARTESIAN_POINT('Ctrl Pts',(31.2532865764462,-54.7388343038513,
-156.676335804936));
#156519=CARTESIAN_POINT('Ctrl Pts',(31.2564089347118,-54.7288613645528,
-156.617160899623));
#156520=CARTESIAN_POINT('Ctrl Pts',(31.2595996255425,-54.718670168262,-156.55669095616));
#156521=CARTESIAN_POINT('Ctrl Pts',(31.2625225020072,-54.709877696298,-156.501330429004));
#156522=CARTESIAN_POINT('Ctrl Pts',(31.2651663049396,-54.7022330407062,
-156.451105263779));
#156523=CARTESIAN_POINT('Ctrl Pts',(31.2661836254125,-54.6992914203054,
-156.431778903174));
#156524=CARTESIAN_POINT('Ctrl Pts',(31.2671596373143,-54.6965202625494,
-156.413212698865));
#156525=CARTESIAN_POINT('Ctrl Pts',(31.2680937422418,-54.6939071725389,
-156.395407391056));
#156526=CARTESIAN_POINT('Ctrl Pts',(31.2705597707236,-54.6870086387644,
-156.348401540974));
#156527=CARTESIAN_POINT('Ctrl Pts',(31.2727389909105,-54.6812076253658,
-156.306702425142));
#156528=CARTESIAN_POINT('Ctrl Pts',(31.2746373151085,-54.6763099699925,
-156.270323611698));
#156529=CARTESIAN_POINT('Ctrl Pts',(31.2749472115869,-54.6755104405157,
-156.264384865203));
#156530=CARTESIAN_POINT('Ctrl Pts',(31.2752496232857,-54.6747350947099,
-156.258587876625));
#156531=CARTESIAN_POINT('Ctrl Pts',(31.2755445770089,-54.6739832155616,
-156.252932676198));
#156532=CARTESIAN_POINT('Ctrl Pts',(31.2765954487601,-54.6713043934435,
-156.232784124375));
#156533=CARTESIAN_POINT('Ctrl Pts',(31.2775517837798,-54.6689230091112,
-156.214435590985));
#156534=CARTESIAN_POINT('Ctrl Pts',(31.2784152401867,-54.6668102998059,
-156.197888377381));
#156535=CARTESIAN_POINT('Ctrl Pts',(31.2788469683902,-54.6657539451532,
-156.189614770579));
#156536=CARTESIAN_POINT('Ctrl Pts',(31.2792554896595,-54.6647648470439,
-156.181791483242));
#156537=CARTESIAN_POINT('Ctrl Pts',(31.2796409993958,-54.6638399472217,
-156.174418629354));
#156538=CARTESIAN_POINT('Ctrl Pts',(31.2798337542639,-54.6633774973106,
-156.170732202409));
#156539=CARTESIAN_POINT('Ctrl Pts',(31.2800207570482,-54.6629311023795,
-156.167158383168));
#156540=CARTESIAN_POINT('Ctrl Pts',(31.2802020332021,-54.6625004132038,
-156.163697183383));
#156541=CARTESIAN_POINT('Ctrl Pts',(31.280292671279,-54.662285068616,-156.161966583491));
#156542=CARTESIAN_POINT('Ctrl Pts',(31.2803818777461,-54.6620736508037,
-156.160264138423));
#156543=CARTESIAN_POINT('Ctrl Pts',(31.2804696557356,-54.6618661181874,
-156.158589849491));
#156544=CARTESIAN_POINT('Ctrl Pts',(31.2805135447303,-54.6617623518792,
-156.157752705025));
#156545=CARTESIAN_POINT('Ctrl Pts',(31.2805570766087,-54.661659556891,-156.15692259959));
#156546=CARTESIAN_POINT('Ctrl Pts',(31.2806002517564,-54.6615577281553,
-156.156099533342));
#156547=CARTESIAN_POINT('Ctrl Pts',(31.2806218393302,-54.6615068137874,
-156.155688000219));
#156548=CARTESIAN_POINT('Ctrl Pts',(31.2806273357613,-54.6614938621523,
-156.155583237424));
#156549=CARTESIAN_POINT('Ctrl Pts',(31.2806407410667,-54.6614622698096,
-156.155327731628));
#156550=CARTESIAN_POINT('Ctrl Pts',(31.2806541463722,-54.6614306774669,
-156.155072225832));
#156551=CARTESIAN_POINT('Ctrl Pts',(31.2806754569608,-54.6613804188924,
-156.154665979994));
#156552=CARTESIAN_POINT('Ctrl Pts',(31.2807287078847,-54.6612551356553,
-156.153651452317));
#156553=CARTESIAN_POINT('Ctrl Pts',(31.2808487333909,-54.6609727521238,
-156.151364746491));
#156554=CARTESIAN_POINT('Ctrl Pts',(31.2809686760916,-54.6606913107074,
-156.149079596605));
#156555=CARTESIAN_POINT('Ctrl Pts',(31.2810885359334,-54.6604108081993,
-156.146796003748));
#156556=CARTESIAN_POINT('Ctrl Pts',(31.2882968648863,-54.6435414854894,
-156.009461528184));
#156557=CARTESIAN_POINT('Ctrl Pts',(31.2952156728382,-54.6300150587062,
-155.877565569711));
#156558=CARTESIAN_POINT('Ctrl Pts',(31.3018424173055,-54.6192049768191,
-155.751171162578));
#156559=CARTESIAN_POINT('Ctrl Pts',(31.3084520725614,-54.6084227722368,
-155.625102704447));
#156560=CARTESIAN_POINT('Ctrl Pts',(31.3147711704004,-54.6003428938458,
-155.504507460173));
#156561=CARTESIAN_POINT('Ctrl Pts',(31.3207975017896,-54.5943950305198,
-155.389442427711));
#156562=CARTESIAN_POINT('Ctrl Pts',(31.3268022969577,-54.5884684229948,
-155.274788601642));
#156563=CARTESIAN_POINT('Ctrl Pts',(31.332516415975,-54.5846586070994,-155.165625531183));
#156564=CARTESIAN_POINT('Ctrl Pts',(31.3379379616093,-54.5824527478572,
-155.062004084437));
#156565=CARTESIAN_POINT('Ctrl Pts',(31.3421341584728,-54.5807454451325,
-154.981802603317));
#156566=CARTESIAN_POINT('Ctrl Pts',(31.3461550941912,-54.58000002,-154.904920740243));
#156567=CARTESIAN_POINT('Ctrl Pts',(31.35,-54.58000002,-154.831379798159));
#156568=CARTESIAN_POINT('Ctrl Pts',(25.7,-54.58000002,-148.513004346424));
#156569=CARTESIAN_POINT('Ctrl Pts',(25.6952401431873,-54.58000002,-148.603330686833));
#156570=CARTESIAN_POINT('Ctrl Pts',(25.690234948237,-54.5812733325853,-148.69822201173));
#156571=CARTESIAN_POINT('Ctrl Pts',(25.6849838077408,-54.5842510816626,
-148.797663422931));
#156572=CARTESIAN_POINT('Ctrl Pts',(25.6802258199289,-54.5869491800714,
-148.887765948818));
#156573=CARTESIAN_POINT('Ctrl Pts',(25.6752658344534,-54.5910472446749,
-148.981605501865));
#156574=CARTESIAN_POINT('Ctrl Pts',(25.6701039419043,-54.5969022494087,
-149.079159958141));
#156575=CARTESIAN_POINT('Ctrl Pts',(25.6654607472659,-54.6021689081641,
-149.166911557778));
#156576=CARTESIAN_POINT('Ctrl Pts',(25.660654398054,-54.608857531153,-149.257664908944));
#156577=CARTESIAN_POINT('Ctrl Pts',(25.6556862558358,-54.6172494896974,
-149.351379263024));
#156578=CARTESIAN_POINT('Ctrl Pts',(25.6532021847266,-54.6214454689696,
-149.398236440063));
#156579=CARTESIAN_POINT('Ctrl Pts',(25.6506776946647,-54.6260675732657,
-149.445833314481));
#156580=CARTESIAN_POINT('Ctrl Pts',(25.6481130758643,-54.6311526793434,
-149.494162543797));
#156581=CARTESIAN_POINT('Ctrl Pts',(25.6468307664641,-54.6336952323822,
-149.518327158455));
#156582=CARTESIAN_POINT('Ctrl Pts',(25.6455384263384,-54.636353552382,-149.542674834613));
#156583=CARTESIAN_POINT('Ctrl Pts',(25.6442361017532,-54.6391323395035,
-149.567204468556));
#156584=CARTESIAN_POINT('Ctrl Pts',(25.6439105206068,-54.6398270362839,
-149.573336877041));
#156585=CARTESIAN_POINT('Ctrl Pts',(25.6435843154472,-54.6405292625706,
-149.579480657608));
#156586=CARTESIAN_POINT('Ctrl Pts',(25.6432574870445,-54.6412390923846,
-149.585635792139));
#156587=CARTESIAN_POINT('Ctrl Pts',(25.6430123657424,-54.6417714647451,
-149.590252143037));
#156588=CARTESIAN_POINT('Ctrl Pts',(25.6427668938662,-54.6423081140951,
-149.594874880539));
#156589=CARTESIAN_POINT('Ctrl Pts',(25.6425210717417,-54.642849071759,-149.599503996986));
#156590=CARTESIAN_POINT('Ctrl Pts',(25.6424595871068,-54.6429843752208,
-149.600661824155));
#156591=CARTESIAN_POINT('Ctrl Pts',(25.642398181581,-54.6431197234208,-149.601818148208));
#156592=CARTESIAN_POINT('Ctrl Pts',(25.6423358274055,-54.6432573912261,
-149.602992322239));
#156593=CARTESIAN_POINT('Ctrl Pts',(25.6417248072865,-54.6446064235565,
-149.614498271108));
#156594=CARTESIAN_POINT('Ctrl Pts',(25.6410477023583,-54.646127792578,-149.627247027373));
#156595=CARTESIAN_POINT('Ctrl Pts',(25.6404953939238,-54.6473869011259,
-149.637644969131));
#156596=CARTESIAN_POINT('Ctrl Pts',(25.6404280329281,-54.6475404653307,
-149.638913129577));
#156597=CARTESIAN_POINT('Ctrl Pts',(25.6403625279329,-54.6476900650441,
-149.640146332103));
#156598=CARTESIAN_POINT('Ctrl Pts',(25.6402992249769,-54.6478348634309,
-149.641338064999));
#156599=CARTESIAN_POINT('Ctrl Pts',(25.6335671479497,-54.6632337318913,
-149.768075237438));
#156600=CARTESIAN_POINT('Ctrl Pts',(25.6266648637635,-54.68134375949,-149.894901757786));
#156601=CARTESIAN_POINT('Ctrl Pts',(25.6197654985376,-54.7021891456976,
-150.021659611439));
#156602=CARTESIAN_POINT('Ctrl Pts',(25.6166209067786,-54.7116900530323,
-150.079433289006));
#156603=CARTESIAN_POINT('Ctrl Pts',(25.6134766834941,-54.7217585222176,
-150.137192825257));
#156604=CARTESIAN_POINT('Ctrl Pts',(25.6103479373083,-54.7323935724098,
-150.194923995243));
#156605=CARTESIAN_POINT('Ctrl Pts',(25.6078496009172,-54.7408857706705,
-150.241022935302));
#156606=CARTESIAN_POINT('Ctrl Pts',(25.6053615108759,-54.749739102678,-150.287103673156));
#156607=CARTESIAN_POINT('Ctrl Pts',(25.6028917781346,-54.7589519149327,
-150.333158921312));
#156608=CARTESIAN_POINT('Ctrl Pts',(25.6004220453934,-54.7681647271875,
-150.379214169468));
#156609=CARTESIAN_POINT('Ctrl Pts',(25.5979706737284,-54.7777370159852,
-150.42524392434));
#156610=CARTESIAN_POINT('Ctrl Pts',(25.5955454527164,-54.787666304305,-150.471241193469));
#156611=CARTESIAN_POINT('Ctrl Pts',(25.5931202317043,-54.7975955926248,
-150.517238462598));
#156612=CARTESIAN_POINT('Ctrl Pts',(25.5907211611064,-54.8078818802587,
-150.563203245825));
#156613=CARTESIAN_POINT('Ctrl Pts',(25.5883559904803,-54.8185217967351,
-150.609128693392));
#156614=CARTESIAN_POINT('Ctrl Pts',(25.586849990668,-54.8252966619559,-150.63837128361));
#156615=CARTESIAN_POINT('Ctrl Pts',(25.5853907429839,-54.832056830242,-150.666933522216));
#156616=CARTESIAN_POINT('Ctrl Pts',(25.5838882239385,-54.8391074038692,
-150.696081713571));
#156617=CARTESIAN_POINT('Ctrl Pts',(25.5830751710654,-54.8429226561036,
-150.711854572358));
#156618=CARTESIAN_POINT('Ctrl Pts',(25.5822494632555,-54.8468237998395,
-150.727798866652));
#156619=CARTESIAN_POINT('Ctrl Pts',(25.5813969566317,-54.8508654682067,
-150.744114196661));
#156620=CARTESIAN_POINT('Ctrl Pts',(25.5813506829308,-54.8510848482654,
-150.74499978591));
#156621=CARTESIAN_POINT('Ctrl Pts',(25.5813043298756,-54.8513046489268,
-150.74588647576));
#156622=CARTESIAN_POINT('Ctrl Pts',(25.5812578952138,-54.8515248793833,
-150.746774298036));
#156623=CARTESIAN_POINT('Ctrl Pts',(25.5762922628235,-54.8750758959192,
-150.841716284895));
#156624=CARTESIAN_POINT('Ctrl Pts',(25.5712705869925,-54.9000065217402,
-150.935491566644));
#156625=CARTESIAN_POINT('Ctrl Pts',(25.5663110036503,-54.9262266483463,
-151.02805147902));
#156626=CARTESIAN_POINT('Ctrl Pts',(25.5573185100371,-54.9737678034748,
-151.195876952141));
#156627=CARTESIAN_POINT('Ctrl Pts',(25.5485269899804,-55.025545197899,-151.359704657308));
#156628=CARTESIAN_POINT('Ctrl Pts',(25.539955871748,-55.0811644018053,-151.519223093345));
#156629=CARTESIAN_POINT('Ctrl Pts',(25.5367090290684,-55.1022336252313,
-151.579650595599));
#156630=CARTESIAN_POINT('Ctrl Pts',(25.5334937784768,-55.1238542107661,
-151.639460298851));
#156631=CARTESIAN_POINT('Ctrl Pts',(25.5303111060527,-55.1460043862931,
-151.698636298518));
#156632=CARTESIAN_POINT('Ctrl Pts',(25.5291526668546,-55.1540666773987,
-151.720175366468));
#156633=CARTESIAN_POINT('Ctrl Pts',(25.5279985351647,-55.1621991258492,
-151.741630495981));
#156634=CARTESIAN_POINT('Ctrl Pts',(25.5268458420758,-55.1704017042082,
-151.763000564696));
#156635=CARTESIAN_POINT('Ctrl Pts',(25.5259639599703,-55.1766771882415,
-151.779350000099));
#156636=CARTESIAN_POINT('Ctrl Pts',(25.5251276462376,-55.1826745046545,
-151.794830293532));
#156637=CARTESIAN_POINT('Ctrl Pts',(25.5242386556593,-55.1891234263154,
-151.811322522395));
#156638=CARTESIAN_POINT('Ctrl Pts',(25.523965661785,-55.1911037803844,-151.81638700515));
#156639=CARTESIAN_POINT('Ctrl Pts',(25.5236877053738,-55.1931270620186,
-151.821546800661));
#156640=CARTESIAN_POINT('Ctrl Pts',(25.5234019553268,-55.1952153541429,
-151.826856060969));
#156641=CARTESIAN_POINT('Ctrl Pts',(25.516907746872,-55.2426757290784,-151.947519009381));
#156642=CARTESIAN_POINT('Ctrl Pts',(25.5103427225298,-55.2927227172219,
-152.066203784139));
#156643=CARTESIAN_POINT('Ctrl Pts',(25.5038940014195,-55.3452199311413,
-152.182765043397));
#156644=CARTESIAN_POINT('Ctrl Pts',(25.5006806324233,-55.3713790589293,
-152.240846999532));
#156645=CARTESIAN_POINT('Ctrl Pts',(25.4974956403295,-55.3981463157476,
-152.298402283602));
#156646=CARTESIAN_POINT('Ctrl Pts',(25.4943591646552,-55.4255036723978,
-152.355416512223));
#156647=CARTESIAN_POINT('Ctrl Pts',(25.4920014436296,-55.4460684787852,
-152.398274694317));
#156648=CARTESIAN_POINT('Ctrl Pts',(25.489671651699,-55.4669661314315,-152.440826470802));
#156649=CARTESIAN_POINT('Ctrl Pts',(25.4873785634058,-55.4881875528084,
-152.483065297136));
#156650=CARTESIAN_POINT('Ctrl Pts',(25.4839389309659,-55.5200196848738,
-152.546423536637));
#156651=CARTESIAN_POINT('Ctrl Pts',(25.4805819867172,-55.5525804217012,
-152.609077547121));
#156652=CARTESIAN_POINT('Ctrl Pts',(25.4773357259928,-55.5858365512146,
-152.671006667056));
#156653=CARTESIAN_POINT('Ctrl Pts',(25.4740921888675,-55.6190647789758,
-152.73288382872));
#156654=CARTESIAN_POINT('Ctrl Pts',(25.4709591638032,-55.6529871939301,
-152.794037301754));
#156655=CARTESIAN_POINT('Ctrl Pts',(25.4679623650184,-55.6875680621891,
-152.854448417611));
#156656=CARTESIAN_POINT('Origin',(0.,-12.9675000200281,-171.64995));
#156657=CARTESIAN_POINT('',(25.5015460489969,-65.317216804244,-171.07256826174));
#156658=CARTESIAN_POINT('',(31.1079170675507,-62.1926886331265,-171.07256826174));
#156659=CARTESIAN_POINT('Origin',(0.,-12.9675000200281,-171.07256826174));
#156660=CARTESIAN_POINT('Ctrl Pts',(31.1079170675507,-62.1926886331265,
-171.07256826174));
#156661=CARTESIAN_POINT('Ctrl Pts',(31.1058138200187,-61.5908885288768,
-169.979184151723));
#156662=CARTESIAN_POINT('Ctrl Pts',(31.1036899128493,-60.9957468863196,
-168.903399109055));
#156663=CARTESIAN_POINT('Ctrl Pts',(31.1015460971806,-60.4071760243875,
-167.845246182439));
#156664=CARTESIAN_POINT('Ctrl Pts',(31.0993650427809,-59.8083815073155,
-166.768712817194));
#156665=CARTESIAN_POINT('Ctrl Pts',(31.0971633844274,-59.216388176699,-165.710429350991));
#156666=CARTESIAN_POINT('Ctrl Pts',(31.094942488845,-58.6311510745784,-164.670402894343));
#156667=CARTESIAN_POINT('Ctrl Pts',(31.0926579405937,-58.0291406023887,
-163.600568435817));
#156668=CARTESIAN_POINT('Ctrl Pts',(31.0903530381058,-57.4342792756791,
-162.550052453581));
#156669=CARTESIAN_POINT('Ctrl Pts',(31.0880298460936,-56.8465661337348,
-161.518834639248));
#156670=CARTESIAN_POINT('Ctrl Pts',(31.0867866957293,-56.5320782211154,
-160.967025406579));
#156671=CARTESIAN_POINT('Ctrl Pts',(31.0855383179793,-56.2196378961364,
-160.420741481362));
#156672=CARTESIAN_POINT('Ctrl Pts',(31.0842850915597,-55.9092502513102,
-159.879976688011));
#156673=CARTESIAN_POINT('Ctrl Pts',(25.4679548160676,-55.6876551762764,
-152.854600597735));
#156674=CARTESIAN_POINT('Ctrl Pts',(25.4704574246668,-56.3163380661018,
-154.015391793635));
#156675=CARTESIAN_POINT('Ctrl Pts',(25.4729351017059,-56.9553314098175,
-155.201562547543));
#156676=CARTESIAN_POINT('Ctrl Pts',(25.4753841249239,-57.6045621956431,
-156.413167418875));
#156677=CARTESIAN_POINT('Ctrl Pts',(25.4777340045614,-58.2275102316101,
-157.575723002255));
#156678=CARTESIAN_POINT('Ctrl Pts',(25.4800575016275,-58.8598835484616,
-158.761695122599));
#156679=CARTESIAN_POINT('Ctrl Pts',(25.4823522232456,-59.5016591213111,
-159.97110891368));
#156680=CARTESIAN_POINT('Ctrl Pts',(25.4846007074484,-60.1305032590741,
-161.156153662694));
#156681=CARTESIAN_POINT('Ctrl Pts',(25.4868215599701,-60.7683743984617,
-162.363705019834));
#156682=CARTESIAN_POINT('Ctrl Pts',(25.4890134549808,-61.4152933901963,
-163.593762998944));
#156683=CARTESIAN_POINT('Ctrl Pts',(25.4911578809512,-62.0482023022682,
-164.797182078134));
#156684=CARTESIAN_POINT('Ctrl Pts',(25.49327458673,-62.6897712831155,-166.022143574981));
#156685=CARTESIAN_POINT('Ctrl Pts',(25.4953632798875,-63.3400631788034,
-167.268623429998));
#156686=CARTESIAN_POINT('Ctrl Pts',(25.497451973045,-63.9903550744914,-168.515103285014));
#156687=CARTESIAN_POINT('Ctrl Pts',(25.4995126467204,-64.6493695892343,
-169.783101662045));
#156688=CARTESIAN_POINT('Ctrl Pts',(25.5015460489969,-65.317216804244,-171.07256826174));
#156689=CARTESIAN_POINT('Ctrl Pts',(42.,-55.58000002,-60.64995));
#156690=CARTESIAN_POINT('Ctrl Pts',(42.,-55.08000002,-60.64995));
#156691=CARTESIAN_POINT('Ctrl Pts',(42.5,-55.08000002,-60.64995));
#156692=CARTESIAN_POINT('Ctrl Pts',(41.5,-55.58000002,-60.64995));
#156693=CARTESIAN_POINT('Ctrl Pts',(41.5,-54.58000002,-60.64995));
#156694=CARTESIAN_POINT('Ctrl Pts',(42.5,-54.58000002,-60.64995));
#156695=CARTESIAN_POINT('Ctrl Pts',(41.5,-55.58000002,-61.14995));
#156696=CARTESIAN_POINT('Ctrl Pts',(41.5,-54.58000002,-61.14995));
#156697=CARTESIAN_POINT('Ctrl Pts',(42.5,-54.58000002,-61.14995));
#156698=CARTESIAN_POINT('',(42.,-55.58000002,-60.64995));
#156699=CARTESIAN_POINT('',(41.5,-55.58000002,-61.14995));
#156700=CARTESIAN_POINT('Origin',(42.,-55.58000002,-61.14995));
#156701=CARTESIAN_POINT('',(42.5,-54.58000002,-61.14995));
#156702=CARTESIAN_POINT('Origin',(42.5,-55.58000002,-61.14995));
#156703=CARTESIAN_POINT('',(42.5,-55.08000002,-60.64995));
#156704=CARTESIAN_POINT('Origin',(42.5,-55.08000002,-61.14995));
#156705=CARTESIAN_POINT('Origin',(42.5,-55.58000002,-60.64995));
#156706=CARTESIAN_POINT('Origin',(0.,-12.9675000200281,-171.64995));
#156707=CARTESIAN_POINT('',(33.85,-63.4074419114814,-171.64995));
#156708=CARTESIAN_POINT('',(39.5,-62.6133861954129,-171.64995));
#156709=CARTESIAN_POINT('',(39.8608268990399,-62.5626752818388,-171.64995));
#156710=CARTESIAN_POINT('',(39.5,-56.978215522411,-171.64995));
#156711=CARTESIAN_POINT('',(39.5,-56.5665827677457,-171.64995));
#156712=CARTESIAN_POINT('',(33.85,-61.4584329769396,-171.64995));
#156713=CARTESIAN_POINT('Origin',(0.,-12.9675000200281,-171.64995));
#156714=CARTESIAN_POINT('',(33.85,-63.4777123288326,-171.64995));
#156715=CARTESIAN_POINT('Origin',(0.,-12.9675000200281,-170.64995));
#156716=CARTESIAN_POINT('',(39.3992713666431,-56.66417131427,-171.60362375617));
#156717=CARTESIAN_POINT('Origin',(39.9831889404834,-58.6893018970301,-160.044295853358));
#156718=CARTESIAN_POINT('Origin',(39.6007286333569,-56.8876021458077,-170.64995));
#156719=CARTESIAN_POINT('Ctrl Pts',(33.5886122085037,-60.5345771657122,
-171.072568261741));
#156720=CARTESIAN_POINT('Ctrl Pts',(33.5929196926425,-60.5496789454406,
-171.104351697009));
#156721=CARTESIAN_POINT('Ctrl Pts',(33.5977697943261,-60.5668084312768,
-171.13599186684));
#156722=CARTESIAN_POINT('Ctrl Pts',(33.6032176264056,-60.5860501581706,
-171.167201320259));
#156723=CARTESIAN_POINT('Ctrl Pts',(33.6085732655045,-60.6049662597278,
-171.197882620002));
#156724=CARTESIAN_POINT('Ctrl Pts',(33.6145068364652,-60.6259240920045,
-171.228147383835));
#156725=CARTESIAN_POINT('Ctrl Pts',(33.6210487151924,-60.6489745030752,
-171.257689498379));
#156726=CARTESIAN_POINT('Ctrl Pts',(33.6274228563078,-60.6714338880711,
-171.28647413576));
#156727=CARTESIAN_POINT('Ctrl Pts',(33.6343746980392,-60.695880197154,-171.314572324815));
#156728=CARTESIAN_POINT('Ctrl Pts',(33.6419080665843,-60.722327544365,-171.341674173059));
#156729=CARTESIAN_POINT('Ctrl Pts',(33.6480621691508,-60.7439327116121,
-171.363814010349));
#156730=CARTESIAN_POINT('Ctrl Pts',(33.6546039728895,-60.7668727584721,
-171.38528835636));
#156731=CARTESIAN_POINT('Ctrl Pts',(33.6615217079334,-60.7911363934354,
-171.405917367214));
#156732=CARTESIAN_POINT('Ctrl Pts',(33.6670079528816,-60.8103791432507,
-171.42227760736));
#156733=CARTESIAN_POINT('Ctrl Pts',(33.6727304167729,-60.8304540680111,
-171.438105942042));
#156734=CARTESIAN_POINT('Ctrl Pts',(33.6786769452906,-60.8513468520672,
-171.453309230289));
#156735=CARTESIAN_POINT('Ctrl Pts',(33.6816502095495,-60.8617932440953,
-171.460910874412));
#156736=CARTESIAN_POINT('Ctrl Pts',(33.6846794709728,-60.8724440739407,
-171.468356302772));
#156737=CARTESIAN_POINT('Ctrl Pts',(33.6877625715685,-60.883296665184,-171.475633559578));
#156738=CARTESIAN_POINT('Ctrl Pts',(33.6893041218664,-60.8887229608057,
-171.479272187981));
#156739=CARTESIAN_POINT('Ctrl Pts',(33.690859130285,-60.8941996943994,-171.482868777341));
#156740=CARTESIAN_POINT('Ctrl Pts',(33.692427301567,-60.8997264955286,-171.486421837307));
#156741=CARTESIAN_POINT('Ctrl Pts',(33.6934416044798,-60.9033012647824,
-171.488719978534));
#156742=CARTESIAN_POINT('Ctrl Pts',(33.6945967894686,-60.907378611323,-171.491303411206));
#156743=CARTESIAN_POINT('Ctrl Pts',(33.6956308892224,-60.9110250428065,
-171.49358056745));
#156744=CARTESIAN_POINT('Ctrl Pts',(33.6961955678179,-60.9130162064263,
-171.49482402717));
#156745=CARTESIAN_POINT('Ctrl Pts',(33.6967238009515,-60.9148783795049,
-171.495977094956));
#156746=CARTESIAN_POINT('Ctrl Pts',(33.6971709938997,-60.9164567102561,
-171.496948943728));
#156747=CARTESIAN_POINT('Ctrl Pts',(33.7037454599816,-60.9396607478684,
-171.51123670657));
#156748=CARTESIAN_POINT('Ctrl Pts',(33.7107503112399,-60.964441558183,-171.525212483463));
#156749=CARTESIAN_POINT('Ctrl Pts',(33.7182138182058,-60.9908464908231,
-171.538579075089));
#156750=CARTESIAN_POINT('Ctrl Pts',(33.722249158874,-61.0051230097589,-171.545806073206));
#156751=CARTESIAN_POINT('Ctrl Pts',(33.7264182463428,-61.0198738554632,
-171.552854348258));
#156752=CARTESIAN_POINT('Ctrl Pts',(33.7307227872848,-61.0351027074787,
-171.559672544505));
#156753=CARTESIAN_POINT('Ctrl Pts',(33.7368557590083,-61.0568002868611,
-171.569386891599));
#156754=CARTESIAN_POINT('Ctrl Pts',(33.7432641867585,-61.0794688883045,
-171.578634643421));
#156755=CARTESIAN_POINT('Ctrl Pts',(33.7499446944048,-61.1031075981544,
-171.587257169257));
#156756=CARTESIAN_POINT('Ctrl Pts',(33.7532849482279,-61.1149269530793,
-171.591568432174));
#156757=CARTESIAN_POINT('Ctrl Pts',(33.7566930603084,-61.1269886097382,
-171.595723207788));
#156758=CARTESIAN_POINT('Ctrl Pts',(33.7601675497484,-61.1392909724596,
-171.599700645306));
#156759=CARTESIAN_POINT('Ctrl Pts',(33.7619047944684,-61.1454421538202,
-171.601689364065));
#156760=CARTESIAN_POINT('Ctrl Pts',(33.7636586341358,-61.1516535125633,
-171.603633745029));
#156761=CARTESIAN_POINT('Ctrl Pts',(33.7654287967637,-61.1579247271646,
-171.605531115606));
#156762=CARTESIAN_POINT('Ctrl Pts',(33.7663138780777,-61.1610603344652,
-171.606479800894));
#156763=CARTESIAN_POINT('Ctrl Pts',(33.7672030401555,-61.1642109057643,
-171.607416733475));
#156764=CARTESIAN_POINT('Ctrl Pts',(33.7680962461282,-61.1673763968156,
-171.608341576954));
#156765=CARTESIAN_POINT('Ctrl Pts',(33.7687784745082,-61.1697941905808,
-171.609047969978));
#156766=CARTESIAN_POINT('Ctrl Pts',(33.7697003191667,-61.1730627912301,
-171.609987833509));
#156767=CARTESIAN_POINT('Ctrl Pts',(33.7703182663326,-61.1752528272204,
-171.610608904528));
#156768=CARTESIAN_POINT('Ctrl Pts',(33.7705093651044,-61.1759300909268,
-171.610800969345));
#156769=CARTESIAN_POINT('Ctrl Pts',(33.7706713306159,-61.1765040977548,
-171.610962995654));
#156770=CARTESIAN_POINT('Ctrl Pts',(33.7707879573347,-61.1769175828282,
-171.611079502341));
#156771=CARTESIAN_POINT('Ctrl Pts',(33.7741748768774,-61.1889254716733,
-171.614462936079));
#156772=CARTESIAN_POINT('Ctrl Pts',(33.778025386712,-61.2026296218794,-171.618091850388));
#156773=CARTESIAN_POINT('Ctrl Pts',(33.7823610153952,-61.2180649959048,
-171.621762516496));
#156774=CARTESIAN_POINT('Ctrl Pts',(33.7866010646012,-61.2331600951773,
-171.62535226231));
#156775=CARTESIAN_POINT('Ctrl Pts',(33.7913054677371,-61.2499114871387,
-171.62898182177));
#156776=CARTESIAN_POINT('Ctrl Pts',(33.7964886563819,-61.2683447777054,
-171.632412230725));
#156777=CARTESIAN_POINT('Ctrl Pts',(33.801577086152,-61.2864410714946,-171.635779925064));
#156778=CARTESIAN_POINT('Ctrl Pts',(33.8071273721981,-61.3061589305378,
-171.638955522725));
#156779=CARTESIAN_POINT('Ctrl Pts',(33.8131416925086,-61.3275071544742,
-171.641667715949));
#156780=CARTESIAN_POINT('Ctrl Pts',(33.8189432281165,-61.348100085169,-171.644283952655));
#156781=CARTESIAN_POINT('Ctrl Pts',(33.8251768962949,-61.370210572944,-171.646468631973));
#156782=CARTESIAN_POINT('Ctrl Pts',(33.8318283554853,-61.3938240136231,
-171.647939780786));
#156783=CARTESIAN_POINT('Ctrl Pts',(33.8375807854589,-61.4142457977842,
-171.649212085146));
#156784=CARTESIAN_POINT('Ctrl Pts',(33.8436456332876,-61.4357916287887,
-171.64995));
#156785=CARTESIAN_POINT('Ctrl Pts',(33.85,-61.4584329769396,-171.64995));
#156786=CARTESIAN_POINT('Ctrl Pts',(38.9938259143948,-56.2145026772597,
-171.07256826174));
#156787=CARTESIAN_POINT('Ctrl Pts',(39.1191457108045,-56.3534914900074,
-171.473900235605));
#156788=CARTESIAN_POINT('Ctrl Pts',(39.4023695343915,-56.6676074087211,
-171.60507092612));
#156789=CARTESIAN_POINT('Ctrl Pts',(39.0656324591812,-56.1451830708436,
-171.065281773562));
#156790=CARTESIAN_POINT('Ctrl Pts',(39.1873296781658,-56.2851199488468,
-171.471360601804));
#156791=CARTESIAN_POINT('Ctrl Pts',(39.4667323101199,-56.6069363160446,
-171.604463274963));
#156792=CARTESIAN_POINT('Ctrl Pts',(39.1389029748433,-56.0783561940248,
-171.057850262871));
#156793=CARTESIAN_POINT('Ctrl Pts',(39.2568527648251,-56.2190926208658,
-171.468759835437));
#156794=CARTESIAN_POINT('Ctrl Pts',(39.532372953365,-56.5484198596326,-171.603842231026));
#156795=CARTESIAN_POINT('Ctrl Pts',(39.2135563963028,-56.0138844098186,
-171.050282355671));
#156796=CARTESIAN_POINT('Ctrl Pts',(39.3276146389594,-56.1552707341152,
-171.46610011903));
#156797=CARTESIAN_POINT('Ctrl Pts',(39.59920642547,-56.4919352618992,-171.603208415545));
#156798=CARTESIAN_POINT('',(39.2122208303137,-56.0150382731948,-171.050417727856));
#156799=CARTESIAN_POINT('Ctrl Pts',(39.3992713666431,-56.6641713142699,
-171.60362375617));
#156800=CARTESIAN_POINT('Ctrl Pts',(39.3906770785271,-56.6361858077295,
-171.595251703632));
#156801=CARTESIAN_POINT('Ctrl Pts',(39.3823718010794,-56.6088835146842,
-171.585840100202));
#156802=CARTESIAN_POINT('Ctrl Pts',(39.3743756985557,-56.5823930069001,
-171.575551092327));
#156803=CARTESIAN_POINT('Ctrl Pts',(39.3659748533384,-56.5545616159241,
-171.564741280628));
#156804=CARTESIAN_POINT('Ctrl Pts',(39.3579151925546,-56.527625972385,-171.552963121434));
#156805=CARTESIAN_POINT('Ctrl Pts',(39.3502074591453,-56.5016806847487,
-171.540389654922));
#156806=CARTESIAN_POINT('Ctrl Pts',(39.344062169692,-56.48099479773,-171.530364971004));
#156807=CARTESIAN_POINT('Ctrl Pts',(39.3381395186297,-56.4609345535854,
-171.519832885525));
#156808=CARTESIAN_POINT('Ctrl Pts',(39.3324428773758,-56.4415362262102,
-171.508879279698));
#156809=CARTESIAN_POINT('Ctrl Pts',(39.3245733723685,-56.4147388156646,
-171.493747651769));
#156810=CARTESIAN_POINT('Ctrl Pts',(39.3171386020042,-56.3892165372729,
-171.477816990192));
#156811=CARTESIAN_POINT('Ctrl Pts',(39.3101422442096,-56.3650383608604,
-171.461323930839));
#156812=CARTESIAN_POINT('Ctrl Pts',(39.3066440653122,-56.3529492726542,
-171.453077401162));
#156813=CARTESIAN_POINT('Ctrl Pts',(39.3032553172147,-56.3411954690074,
-171.444690285293));
#156814=CARTESIAN_POINT('Ctrl Pts',(39.2999755567523,-56.3297816523997,
-171.436192546601));
#156815=CARTESIAN_POINT('Ctrl Pts',(39.2983356765211,-56.3240747440958,
-171.431943677255));
#156816=CARTESIAN_POINT('Ctrl Pts',(39.2967230252678,-56.318452762688,-171.427667134469));
#156817=CARTESIAN_POINT('Ctrl Pts',(39.2951374873227,-56.3129160426783,
-171.423366671635));
#156818=CARTESIAN_POINT('Ctrl Pts',(39.2942934323989,-56.3099685914361,
-171.421077337065));
#156819=CARTESIAN_POINT('Ctrl Pts',(39.2934570590603,-56.3070452947652,
-171.418781220015));
#156820=CARTESIAN_POINT('Ctrl Pts',(39.2926283405029,-56.3041461672385,
-171.416478873257));
#156821=CARTESIAN_POINT('Ctrl Pts',(39.2923552884053,-56.3031909420352,
-171.415720279636));
#156822=CARTESIAN_POINT('Ctrl Pts',(39.2920830672967,-56.3022383405622,
-171.414961009691));
#156823=CARTESIAN_POINT('Ctrl Pts',(39.2918116761374,-56.301288363005,-171.414201083151));
#156824=CARTESIAN_POINT('Ctrl Pts',(39.2916633249908,-56.3007690746823,
-171.413785682834));
#156825=CARTESIAN_POINT('Ctrl Pts',(39.2915170891402,-56.3002571066252,
-171.413375314105));
#156826=CARTESIAN_POINT('Ctrl Pts',(39.2913732225394,-56.2997533552218,
-171.412970764343));
#156827=CARTESIAN_POINT('Ctrl Pts',(39.2910785677092,-56.2987216162118,
-171.412142201349));
#156828=CARTESIAN_POINT('Ctrl Pts',(39.2907927013265,-56.2977203215939,
-171.411334858269));
#156829=CARTESIAN_POINT('Ctrl Pts',(39.2905105668222,-56.2967317999291,
-171.410534859845));
#156830=CARTESIAN_POINT('Ctrl Pts',(39.2895637803088,-56.2934145205245,
-171.407850226428));
#156831=CARTESIAN_POINT('Ctrl Pts',(39.2886580158514,-56.2902380779171,
-171.405249914464));
#156832=CARTESIAN_POINT('Ctrl Pts',(39.287606731647,-56.2865471065203,-171.402183331585));
#156833=CARTESIAN_POINT('Ctrl Pts',(39.2872325193817,-56.2852332783835,
-171.401091759087));
#156834=CARTESIAN_POINT('Ctrl Pts',(39.2868399324184,-56.2838544292433,
-171.399940714715));
#156835=CARTESIAN_POINT('Ctrl Pts',(39.2864208072506,-56.282381690366,-171.398703860458));
#156836=CARTESIAN_POINT('Ctrl Pts',(39.2793207216785,-56.2574331240225,
-171.377751238812));
#156837=CARTESIAN_POINT('Ctrl Pts',(39.2725972793437,-56.2336227224313,
-171.355722284568));
#156838=CARTESIAN_POINT('Ctrl Pts',(39.2662721784007,-56.2110893945002,
-171.33284252015));
#156839=CARTESIAN_POINT('Ctrl Pts',(39.2598102321418,-56.1880685517593,
-171.309467745673));
#156840=CARTESIAN_POINT('Ctrl Pts',(39.2537640388237,-56.1663806024417,
-171.285204989219));
#156841=CARTESIAN_POINT('Ctrl Pts',(39.2481450730767,-56.1461217644991,
-171.260281430404));
#156842=CARTESIAN_POINT('Ctrl Pts',(39.2424446265433,-56.1255691525555,
-171.234996454334));
#156843=CARTESIAN_POINT('Ctrl Pts',(39.2371838522641,-56.1064872560232,
-171.209031394905));
#156844=CARTESIAN_POINT('Ctrl Pts',(39.23236323362,-56.0889251572901,-171.182609447624));
#156845=CARTESIAN_POINT('Ctrl Pts',(39.2274123917834,-56.0708886396635,
-171.155473743339));
#156846=CARTESIAN_POINT('Ctrl Pts',(39.2229257811129,-56.0544550420533,
-171.127856183048));
#156847=CARTESIAN_POINT('Ctrl Pts',(39.2188923243667,-56.0396254214308,
-171.099983271027));
#156848=CARTESIAN_POINT('Ctrl Pts',(39.2165122517984,-56.0308747206147,
-171.083535951155));
#156849=CARTESIAN_POINT('Ctrl Pts',(39.2142897493854,-56.0226815447907,
-171.066999426818));
#156850=CARTESIAN_POINT('Ctrl Pts',(39.2122207971109,-56.0150382320577,
-171.050417750961));
#156851=CARTESIAN_POINT('Origin',(42.7058184422067,-60.0992226026716,-170.70354739068));
#156852=CARTESIAN_POINT('Ctrl Pts',(39.0986073542357,-56.2184192034566,
-171.229381885675));
#156853=CARTESIAN_POINT('Ctrl Pts',(40.320307620846,-54.58000002,-170.379862235888));
#156854=CARTESIAN_POINT('Ctrl Pts',(42.1374590345468,-54.58000002,-169.116290576972));
#156855=CARTESIAN_POINT('Ctrl Pts',(36.5384467754252,-56.1227754271583,
-167.395443178417));
#156856=CARTESIAN_POINT('Ctrl Pts',(37.7530684146654,-54.5800000200966,
-166.553337438667));
#156857=CARTESIAN_POINT('Ctrl Pts',(39.4714760509134,-54.58000002,-165.282321435755));
#156858=CARTESIAN_POINT('Ctrl Pts',(33.8932339485135,-56.0200282137318,
-163.608339894981));
#156859=CARTESIAN_POINT('Ctrl Pts',(35.0808115183432,-54.5800000200163,
-162.752463904168));
#156860=CARTESIAN_POINT('Ctrl Pts',(36.7030946909167,-54.58000002,-161.495162061412));
#156861=CARTESIAN_POINT('Ctrl Pts',(31.1382389079697,-55.9113782125501,
-159.951555016761));
#156862=CARTESIAN_POINT('Ctrl Pts',(32.2640061692936,-54.5800000199999,
-159.057279891091));
#156863=CARTESIAN_POINT('Ctrl Pts',(33.7983252138975,-54.58000002,-157.838463708057));
#156864=CARTESIAN_POINT('',(39.5000000000002,-54.58000002,-165.390538702985));
#156865=CARTESIAN_POINT('Ctrl Pts',(39.2122207971107,-56.015038232057,-171.050417750959));
#156866=CARTESIAN_POINT('Ctrl Pts',(39.217277668066,-55.9551243221841,-170.951014902235));
#156867=CARTESIAN_POINT('Ctrl Pts',(39.2225737764226,-55.8953485378391,
-170.846909763433));
#156868=CARTESIAN_POINT('Ctrl Pts',(39.2281136244437,-55.8361395590084,
-170.738013265696));
#156869=CARTESIAN_POINT('Ctrl Pts',(39.2329744614731,-55.7841877372847,
-170.642464050889));
#156870=CARTESIAN_POINT('Ctrl Pts',(39.2380229477203,-55.732672178747,-170.543226083457));
#156871=CARTESIAN_POINT('Ctrl Pts',(39.2432615363417,-55.6818511882625,
-170.440250573425));
#156872=CARTESIAN_POINT('Ctrl Pts',(39.2486908746011,-55.6291796830242,
-170.333525476877));
#156873=CARTESIAN_POINT('Ctrl Pts',(39.2543239888344,-55.5772600009846,
-170.22279399802));
#156874=CARTESIAN_POINT('Ctrl Pts',(39.2601606430054,-55.5263531464095,
-170.108059909242));
#156875=CARTESIAN_POINT('Ctrl Pts',(39.2655922070714,-55.4789794569764,
-170.001288883325));
#156876=CARTESIAN_POINT('Ctrl Pts',(39.2712000221776,-55.4324830581944,
-169.891051881756));
#156877=CARTESIAN_POINT('Ctrl Pts',(39.2769824136889,-55.3870332559345,
-169.777380931684));
#156878=CARTESIAN_POINT('Ctrl Pts',(39.2774136687668,-55.3836435757349,
-169.768903267325));
#156879=CARTESIAN_POINT('Ctrl Pts',(39.2778458943164,-55.3802596954691,
-169.76040651352));
#156880=CARTESIAN_POINT('Ctrl Pts',(39.2782790893708,-55.3768816747099,
-169.751890688863));
#156881=CARTESIAN_POINT('Ctrl Pts',(39.2786817731338,-55.3737415785869,
-169.743974660545));
#156882=CARTESIAN_POINT('Ctrl Pts',(39.2791846505417,-55.3698374844174,
-169.734088992016));
#156883=CARTESIAN_POINT('Ctrl Pts',(39.2794897333218,-55.3674765853668,
-169.728093195798));
#156884=CARTESIAN_POINT('Ctrl Pts',(39.2796754514722,-55.3660393957464,
-169.724443274347));
#156885=CARTESIAN_POINT('Ctrl Pts',(39.279861545757,-55.3646017242543,-169.720785919229));
#156886=CARTESIAN_POINT('Ctrl Pts',(39.2800480163202,-55.3631635898699,
-169.717121128618));
#156887=CARTESIAN_POINT('Ctrl Pts',(39.2896637468172,-55.2890032912071,
-169.528138812898));
#156888=CARTESIAN_POINT('Ctrl Pts',(39.3002819901101,-55.2136805673814,
-169.319346539255));
#156889=CARTESIAN_POINT('Ctrl Pts',(39.3119342062424,-55.1403994795761,
-169.090262204253));
#156890=CARTESIAN_POINT('Ctrl Pts',(39.3182997955631,-55.1003661241485,
-168.965113753532));
#156891=CARTESIAN_POINT('Ctrl Pts',(39.3249727388327,-55.0609470669007,
-168.833918228421));
#156892=CARTESIAN_POINT('Ctrl Pts',(39.331953351763,-55.0226701436895,-168.69666675457));
#156893=CARTESIAN_POINT('Ctrl Pts',(39.3377950222373,-54.9906384045853,
-168.581808949051));
#156894=CARTESIAN_POINT('Ctrl Pts',(39.3438520987461,-54.9594069518665,
-168.462711233961));
#156895=CARTESIAN_POINT('Ctrl Pts',(39.3501233117751,-54.9292733027628,
-168.339396616846));
#156896=CARTESIAN_POINT('Ctrl Pts',(39.3503418056772,-54.9282234231705,
-168.33510024041));
#156897=CARTESIAN_POINT('Ctrl Pts',(39.3506232405128,-54.9268751667346,
-168.329566206783));
#156898=CARTESIAN_POINT('Ctrl Pts',(39.3507795876923,-54.9261276645024,
-168.326492141633));
#156899=CARTESIAN_POINT('Ctrl Pts',(39.3510206043589,-54.9249753540039,
-168.321753322947));
#156900=CARTESIAN_POINT('Ctrl Pts',(39.3512629457232,-54.9238198292848,
-168.316988402192));
#156901=CARTESIAN_POINT('Ctrl Pts',(39.3515066134264,-54.9226611781907,
-168.312197349974));
#156902=CARTESIAN_POINT('Ctrl Pts',(39.3552892899169,-54.9046743781474,
-168.23782146695));
#156903=CARTESIAN_POINT('Ctrl Pts',(39.3593881459255,-54.8859547368179,
-168.157216109233));
#156904=CARTESIAN_POINT('Ctrl Pts',(39.3638064495819,-54.8668806041018,
-168.070327443506));
#156905=CARTESIAN_POINT('Ctrl Pts',(39.3650116256491,-54.861677772871,-168.046626913035));
#156906=CARTESIAN_POINT('Ctrl Pts',(39.3662405652956,-54.8564488546796,
-168.022458966405));
#156907=CARTESIAN_POINT('Ctrl Pts',(39.3674933237398,-54.8512021679473,
-167.997822720973));
#156908=CARTESIAN_POINT('Ctrl Pts',(39.3705640006804,-54.8383418435663,
-167.93743601905));
#156909=CARTESIAN_POINT('Ctrl Pts',(39.3737775356156,-54.8253747693599,
-167.874238194184));
#156910=CARTESIAN_POINT('Ctrl Pts',(39.3771341911808,-54.8124307390108,
-167.808223412464));
#156911=CARTESIAN_POINT('Ctrl Pts',(39.3788125189633,-54.8059587238362,
-167.775216021605));
#156912=CARTESIAN_POINT('Ctrl Pts',(39.3805266279187,-54.7994925927265,
-167.741504369649));
#156913=CARTESIAN_POINT('Ctrl Pts',(39.3822765218251,-54.7930494106325,
-167.707088286477));
#156914=CARTESIAN_POINT('Ctrl Pts',(39.3831514687782,-54.7898278195855,
-167.689880244891));
#156915=CARTESIAN_POINT('Ctrl Pts',(39.3840353620358,-54.7866119728371,
-167.672496094056));
#156916=CARTESIAN_POINT('Ctrl Pts',(39.3849282011879,-54.7834040498743,
-167.654935829232));
#156917=CARTESIAN_POINT('Ctrl Pts',(39.3853746207639,-54.7818000883929,
-167.64615569682));
#156918=CARTESIAN_POINT('Ctrl Pts',(39.3858232768172,-54.7801981082895,
-167.637331535831));
#156919=CARTESIAN_POINT('Ctrl Pts',(39.386274169183,-54.778598385049,-167.62846334785));
#156920=CARTESIAN_POINT('Ctrl Pts',(39.3867250615487,-54.7769986618084,
-167.61959515987));
#156921=CARTESIAN_POINT('Ctrl Pts',(39.3872461308566,-54.7751632308417,
-167.609346669943));
#156922=CARTESIAN_POINT('Ctrl Pts',(39.3876335550243,-54.7738062632412,
-167.601726705049));
#156923=CARTESIAN_POINT('Ctrl Pts',(39.3938323417077,-54.752094781634,-167.479807266749));
#156924=CARTESIAN_POINT('Ctrl Pts',(39.4001106304159,-54.7322517188799,
-167.357667971969));
#156925=CARTESIAN_POINT('Ctrl Pts',(39.4063626742351,-54.7142658021284,
-167.235386059973));
#156926=CARTESIAN_POINT('Ctrl Pts',(39.4094886961447,-54.7052728437527,
-167.174245103974));
#156927=CARTESIAN_POINT('Ctrl Pts',(39.4126074508743,-54.6967440843976,
-167.113068500334));
#156928=CARTESIAN_POINT('Ctrl Pts',(39.4157054315454,-54.6886767990617,
-167.051865706899));
#156929=CARTESIAN_POINT('Ctrl Pts',(39.4172544218809,-54.6846431563937,
-167.021264310181));
#156930=CARTESIAN_POINT('Ctrl Pts',(39.4187982167228,-54.6807248694948,
-166.990656367443));
#156931=CARTESIAN_POINT('Ctrl Pts',(39.4203351387637,-54.6769215183548,
-166.960043055177));
#156932=CARTESIAN_POINT('Ctrl Pts',(39.4211035997842,-54.6750198427849,
-166.944736399044));
#156933=CARTESIAN_POINT('Ctrl Pts',(39.4218703425289,-54.6731469003953,
-166.929428400584));
#156934=CARTESIAN_POINT('Ctrl Pts',(39.4226351589158,-54.6713026337753,
-166.914119205984));
#156935=CARTESIAN_POINT('Ctrl Pts',(39.4230175671092,-54.6703805004653,
-166.906464608684));
#156936=CARTESIAN_POINT('Ctrl Pts',(39.4233994937091,-54.6694655360523,
-166.898809712353));
#156937=CARTESIAN_POINT('Ctrl Pts',(39.4237809128189,-54.6685577330597,
-166.891154535198));
#156938=CARTESIAN_POINT('Ctrl Pts',(39.4241623319288,-54.6676499300671,
-166.883499358043));
#156939=CARTESIAN_POINT('Ctrl Pts',(39.4244844603489,-54.6668873637392,
-166.877027058665));
#156940=CARTESIAN_POINT('Ctrl Pts',(39.4249334045403,-54.6658543237986,
-166.868188340615));
#156941=CARTESIAN_POINT('Ctrl Pts',(39.4250682094824,-54.6655441318147,
-166.865534329497));
#156942=CARTESIAN_POINT('Ctrl Pts',(39.4252029319403,-54.6652349867371,
-166.862881953684));
#156943=CARTESIAN_POINT('Ctrl Pts',(39.425337571846,-54.6649268850763,-166.860231214349));
#156944=CARTESIAN_POINT('Ctrl Pts',(39.4335179130109,-54.6462074966023,
-166.699179763937));
#156945=CARTESIAN_POINT('Ctrl Pts',(39.4414032837231,-54.6312933688463,
-166.54397705278));
#156946=CARTESIAN_POINT('Ctrl Pts',(39.4489876210276,-54.6195031874319,
-166.394706763715));
#156947=CARTESIAN_POINT('Ctrl Pts',(39.4545816663594,-54.6108070012453,
-166.284608184209));
#156948=CARTESIAN_POINT('Ctrl Pts',(39.4600119506171,-54.6038113708886,
-166.177736867599));
#156949=CARTESIAN_POINT('Ctrl Pts',(39.4652761839798,-54.5982610012924,
-166.074124550311));
#156950=CARTESIAN_POINT('Ctrl Pts',(39.4723661788121,-54.590785631368,-165.934577014416));
#156951=CARTESIAN_POINT('Ctrl Pts',(39.4791552957939,-54.5859295459294,
-165.80093473994));
#156952=CARTESIAN_POINT('Ctrl Pts',(39.4856401196765,-54.5831141206687,
-165.673267756554));
#156953=CARTESIAN_POINT('Ctrl Pts',(39.4906056246988,-54.5809583168219,
-165.575511663456));
#156954=CARTESIAN_POINT('Ctrl Pts',(39.4953927244241,-54.58000002,-165.481258862479));
#156955=CARTESIAN_POINT('Ctrl Pts',(39.5,-54.58000002,-165.390538702986));
#156956=CARTESIAN_POINT('',(33.85,-54.58000002,-157.903547609535));
#156957=CARTESIAN_POINT('Ctrl Pts',(33.85,-54.58000002,-157.903547609535));
#156958=CARTESIAN_POINT('Ctrl Pts',(35.7938424480564,-54.58000002,-160.35302343361));
#156959=CARTESIAN_POINT('Ctrl Pts',(37.6706534886586,-54.58000002,-162.854283363144));
#156960=CARTESIAN_POINT('Ctrl Pts',(39.5,-54.58000002,-165.390538702986));
#156961=CARTESIAN_POINT('Ctrl Pts',(33.85,-54.58000002,-157.903547609535));
#156962=CARTESIAN_POINT('Ctrl Pts',(33.8455842717013,-54.58000002,-157.988668869387));
#156963=CARTESIAN_POINT('Ctrl Pts',(33.840905459912,-54.5809154547948,-158.078838729506));
#156964=CARTESIAN_POINT('Ctrl Pts',(33.8359628860556,-54.5831131147122,
-158.174062541897));
#156965=CARTESIAN_POINT('Ctrl Pts',(33.8312850893789,-54.5851930444324,
-158.264185147261));
#156966=CARTESIAN_POINT('Ctrl Pts',(33.826371034481,-54.5884217416172,-158.358834689519));
#156967=CARTESIAN_POINT('Ctrl Pts',(33.8212204663112,-54.5931538081737,
-158.458009249791));
#156968=CARTESIAN_POINT('Ctrl Pts',(33.8159363095128,-54.5980086088171,
-158.559756068707));
#156969=CARTESIAN_POINT('Ctrl Pts',(33.8104030224301,-54.6044458578897,
-158.666269301579));
#156970=CARTESIAN_POINT('Ctrl Pts',(33.8046223261081,-54.6128946576057,
-158.777508335281));
#156971=CARTESIAN_POINT('Ctrl Pts',(33.8003719093108,-54.6191068711921,
-158.859299910384));
#156972=CARTESIAN_POINT('Ctrl Pts',(33.7959876687427,-54.6264077104841,
-158.943647679002));
#156973=CARTESIAN_POINT('Ctrl Pts',(33.791470801607,-54.634983652183,-159.030525674615));
#156974=CARTESIAN_POINT('Ctrl Pts',(33.7892123680392,-54.6392716230325,
-159.073964672421));
#156975=CARTESIAN_POINT('Ctrl Pts',(33.7869207854566,-54.6438785762368,
-159.118036081396));
#156976=CARTESIAN_POINT('Ctrl Pts',(33.7845962600292,-54.64882901054,-159.162735578489));
#156977=CARTESIAN_POINT('Ctrl Pts',(33.7834339973156,-54.6513042276916,
-159.185085327036));
#156978=CARTESIAN_POINT('Ctrl Pts',(33.7822635001811,-54.6538653257679,
-159.207592072923));
#156979=CARTESIAN_POINT('Ctrl Pts',(33.7810847987406,-54.6565154364382,
-159.230255193116));
#156980=CARTESIAN_POINT('Ctrl Pts',(33.7804954480203,-54.6578404917734,
-159.241586753212));
#156981=CARTESIAN_POINT('Ctrl Pts',(33.7799040462578,-54.6591878009921,
-159.252957406234));
#156982=CARTESIAN_POINT('Ctrl Pts',(33.7793105974546,-54.6605577598491,
-159.264367069807));
#156983=CARTESIAN_POINT('Ctrl Pts',(33.779013873053,-54.6612427392777,-159.270071901593));
#156984=CARTESIAN_POINT('Ctrl Pts',(33.7787166368952,-54.6619333811565,
-159.275786485939));
#156985=CARTESIAN_POINT('Ctrl Pts',(33.7784188895009,-54.6626297352091,
-159.28151081218));
#156986=CARTESIAN_POINT('Ctrl Pts',(33.7783816710766,-54.6627167794657,
-159.28222635296));
#156987=CARTESIAN_POINT('Ctrl Pts',(33.7783444446642,-54.6628039129752,
-159.282942045957));
#156988=CARTESIAN_POINT('Ctrl Pts',(33.7783072102649,-54.6628911358349,
-159.283657891149));
#156989=CARTESIAN_POINT('Ctrl Pts',(33.778284912608,-54.6629433688623,-159.284086571907));
#156990=CARTESIAN_POINT('Ctrl Pts',(33.7782626120867,-54.6629956339321,
-159.284515307244));
#156991=CARTESIAN_POINT('Ctrl Pts',(33.7782403087015,-54.6630479310653,
-159.284944097156));
#156992=CARTESIAN_POINT('Ctrl Pts',(33.7782180028459,-54.6631002339908,
-159.28537293456));
#156993=CARTESIAN_POINT('Ctrl Pts',(33.77819542865,-54.6631531926069,-159.285806930388));
#156994=CARTESIAN_POINT('Ctrl Pts',(33.7781740983071,-54.663203256122,-159.28621701232));
#156995=CARTESIAN_POINT('Ctrl Pts',(33.7779674505323,-54.6636882700773,
-159.290189874781));
#156996=CARTESIAN_POINT('Ctrl Pts',(33.7778502780355,-54.6639632537656,
-159.292442549935));
#156997=CARTESIAN_POINT('Ctrl Pts',(33.7775241141409,-54.6647359837781,
-159.298713005671));
#156998=CARTESIAN_POINT('Ctrl Pts',(33.7717564466018,-54.678400432493,-159.409595615936));
#156999=CARTESIAN_POINT('Ctrl Pts',(33.7662716229799,-54.6929414485542,
-159.513746318479));
#157000=CARTESIAN_POINT('Ctrl Pts',(33.7611094668565,-54.7078021960704,
-159.611181297637));
#157001=CARTESIAN_POINT('Ctrl Pts',(33.7560582805545,-54.7223434851163,
-159.706521736841));
#157002=CARTESIAN_POINT('Ctrl Pts',(33.7513159805723,-54.7371906836515,
-159.795432098454));
#157003=CARTESIAN_POINT('Ctrl Pts',(33.7469165106161,-54.7518701986928,
-159.877921548684));
#157004=CARTESIAN_POINT('Ctrl Pts',(33.7426426249294,-54.7661306823073,
-159.958056311314));
#157005=CARTESIAN_POINT('Ctrl Pts',(33.7386922093325,-54.7802328295328,
-160.032131525696));
#157006=CARTESIAN_POINT('Ctrl Pts',(33.7350940886263,-54.7937904986563,
-160.10014960274));
#157007=CARTESIAN_POINT('Ctrl Pts',(33.7318108902886,-54.8061615446452,
-160.16221445707));
#157008=CARTESIAN_POINT('Ctrl Pts',(33.728820953291,-54.8180796425581,-160.219236030609));
#157009=CARTESIAN_POINT('Ctrl Pts',(33.7261451708852,-54.82928903124,-160.271211282608));
#157010=CARTESIAN_POINT('Ctrl Pts',(33.7232172313475,-54.8415547566755,
-160.328084515266));
#157011=CARTESIAN_POINT('Ctrl Pts',(33.7206338516712,-54.8529843457977,
-160.378943028466));
#157012=CARTESIAN_POINT('Ctrl Pts',(33.7183743345158,-54.8633229976481,
-160.423822117226));
#157013=CARTESIAN_POINT('Ctrl Pts',(33.7161148173604,-54.8736616494985,
-160.468701205986));
#157014=CARTESIAN_POINT('Ctrl Pts',(33.7141792010275,-54.8829093403809,
-160.507600869464));
#157015=CARTESIAN_POINT('Ctrl Pts',(33.7125484587061,-54.8908716103222,
-160.540547336014));
#157016=CARTESIAN_POINT('Ctrl Pts',(33.7109177163846,-54.8988338802635,
-160.573493802564));
#157017=CARTESIAN_POINT('Ctrl Pts',(33.7095906356586,-54.905511485582,-160.600488868346));
#157018=CARTESIAN_POINT('Ctrl Pts',(33.7085494778909,-54.910771945989,-160.621555337921));
#157019=CARTESIAN_POINT('Ctrl Pts',(33.7080288990071,-54.9134021761925,
-160.632088572709));
#157020=CARTESIAN_POINT('Ctrl Pts',(33.7075798767493,-54.9156790556679,
-160.64113953553));
#157021=CARTESIAN_POINT('Ctrl Pts',(33.7072007704359,-54.9175915601511,
-160.648710248803));
#157022=CARTESIAN_POINT('Ctrl Pts',(33.7070112172792,-54.9185478123928,
-160.65249560544));
#157023=CARTESIAN_POINT('Ctrl Pts',(33.7068391595856,-54.9194130241989,
-160.655910886927));
#157024=CARTESIAN_POINT('Ctrl Pts',(33.7066844261339,-54.9201861620642,
-160.658956291836));
#157025=CARTESIAN_POINT('Ctrl Pts',(33.7066271536549,-54.9204723285113,
-160.66008350697));
#157026=CARTESIAN_POINT('Ctrl Pts',(33.7065722544831,-54.9207458838973,
-160.661160051605));
#157027=CARTESIAN_POINT('Ctrl Pts',(33.7065197237176,-54.9210067805742,
-160.662185924984));
#157028=CARTESIAN_POINT('Ctrl Pts',(33.7065012931173,-54.9210983170736,
-160.6625458562));
#157029=CARTESIAN_POINT('Ctrl Pts',(33.7064831539969,-54.9211882964876,
-160.662899551137));
#157030=CARTESIAN_POINT('Ctrl Pts',(33.7064653061515,-54.9212767167715,
-160.663247009611));
#157031=CARTESIAN_POINT('Ctrl Pts',(33.7064309473279,-54.9214469343443,
-160.663915900679));
#157032=CARTESIAN_POINT('Ctrl Pts',(33.7063976681466,-54.9216113735066,
-160.664561678743));
#157033=CARTESIAN_POINT('Ctrl Pts',(33.7063654665511,-54.9217700215039,
-160.66518434624));
#157034=CARTESIAN_POINT('Ctrl Pts',(33.7063493657534,-54.9218493455026,
-160.665495679988));
#157035=CARTESIAN_POINT('Ctrl Pts',(33.7063335343563,-54.9219272217235,
-160.665801236091));
#157036=CARTESIAN_POINT('Ctrl Pts',(33.7063179721145,-54.9220036486581,
-160.666101014837));
#157037=CARTESIAN_POINT('Ctrl Pts',(33.7063101909937,-54.9220418621254,
-160.66625090421));
#157038=CARTESIAN_POINT('Ctrl Pts',(33.7063255851885,-54.921966662831,-160.665956043164));
#157039=CARTESIAN_POINT('Ctrl Pts',(33.7063294920643,-54.921947622701,-160.665881391093));
#157040=CARTESIAN_POINT('Ctrl Pts',(33.7063333989402,-54.9219285825709,
-160.665806739022));
#157041=CARTESIAN_POINT('Ctrl Pts',(33.7063258183025,-54.9219656412912,
-160.66595230046));
#157042=CARTESIAN_POINT('Ctrl Pts',(33.706272088182,-54.9222285814461,-160.666983018974));
#157043=CARTESIAN_POINT('Ctrl Pts',(33.7009078975708,-54.9484794272874,
-160.769885646496));
#157044=CARTESIAN_POINT('Ctrl Pts',(33.6956802612108,-54.975601534076,-160.869638762938));
#157045=CARTESIAN_POINT('Ctrl Pts',(33.6906131147999,-55.0033469705025,
-160.966209592634));
#157046=CARTESIAN_POINT('Ctrl Pts',(33.6852952359268,-55.0324653061955,
-161.067558938667));
#157047=CARTESIAN_POINT('Ctrl Pts',(33.6801541162865,-55.0622699904258,
-161.16540357318));
#157048=CARTESIAN_POINT('Ctrl Pts',(33.675211508873,-55.0924969827791,-161.259758725589));
#157049=CARTESIAN_POINT('Ctrl Pts',(33.6727873622862,-55.1073220850409,
-161.306036064963));
#157050=CARTESIAN_POINT('Ctrl Pts',(33.6704108807543,-55.1222491269139,
-161.351474766905));
#157051=CARTESIAN_POINT('Ctrl Pts',(33.6680841619286,-55.1372490025288,
-161.396080607222));
#157052=CARTESIAN_POINT('Ctrl Pts',(33.6629744949401,-55.1701899700473,
-161.494038721992));
#157053=CARTESIAN_POINT('Ctrl Pts',(33.6580979013176,-55.2034782520868,
-161.587960992612));
#157054=CARTESIAN_POINT('Ctrl Pts',(33.6534377421645,-55.2368194787995,
-161.677878398062));
#157055=CARTESIAN_POINT('Ctrl Pts',(33.6528122575655,-55.241294524208,-161.689947074355));
#157056=CARTESIAN_POINT('Ctrl Pts',(33.652190671613,-55.2457705620805,-161.701943669366));
#157057=CARTESIAN_POINT('Ctrl Pts',(33.651572943776,-55.2502469164948,-161.713868317027));
#157058=CARTESIAN_POINT('Ctrl Pts',(33.6489628960728,-55.2691605834178,
-161.764252802516));
#157059=CARTESIAN_POINT('Ctrl Pts',(33.6464211319758,-55.2880796832181,
-161.813351747981));
#157060=CARTESIAN_POINT('Ctrl Pts',(33.6439413334603,-55.306954917264,-161.861173480295));
#157061=CARTESIAN_POINT('Ctrl Pts',(33.6427014342026,-55.3163925342869,
-161.885084346451));
#157062=CARTESIAN_POINT('Ctrl Pts',(33.6414770339499,-55.3258191988819,
-161.908675903486));
#157063=CARTESIAN_POINT('Ctrl Pts',(33.6402671210953,-55.3352290373697,
-161.93194933418));
#157064=CARTESIAN_POINT('Ctrl Pts',(33.639662164668,-55.3399339566135,-161.943586049527));
#157065=CARTESIAN_POINT('Ctrl Pts',(33.6390608306291,-55.3446346703723,
-161.955143232875));
#157066=CARTESIAN_POINT('Ctrl Pts',(33.6384629894247,-55.349330455341,-161.96662103369));
#157067=CARTESIAN_POINT('Ctrl Pts',(33.6381640688225,-55.3516783478254,
-161.972359934098));
#157068=CARTESIAN_POINT('Ctrl Pts',(33.6378660214631,-55.3540250081756,
-161.978078988847));
#157069=CARTESIAN_POINT('Ctrl Pts',(33.6375688304508,-55.3563703470497,
-161.983778217058));
#157070=CARTESIAN_POINT('Ctrl Pts',(33.6373398167457,-55.3581776518568,
-161.988170009928));
#157071=CARTESIAN_POINT('Ctrl Pts',(33.6371703141945,-55.3595177060693,
-161.991420282418));
#157072=CARTESIAN_POINT('Ctrl Pts',(33.6369239026404,-55.361468542626,-161.996140872168));
#157073=CARTESIAN_POINT('Ctrl Pts',(33.636850545999,-55.3620493060492,-161.997546190237));
#157074=CARTESIAN_POINT('Ctrl Pts',(33.636770374559,-55.3626842991758,-161.999081790039));
#157075=CARTESIAN_POINT('Ctrl Pts',(33.6366797957947,-55.3634022825266,
-162.00081644943));
#157076=CARTESIAN_POINT('Ctrl Pts',(33.6303630969412,-55.4134723474333,
-162.121786536301));
#157077=CARTESIAN_POINT('Ctrl Pts',(33.6242642048687,-55.4647929755218,
-162.238561065914));
#157078=CARTESIAN_POINT('Ctrl Pts',(33.6183832363913,-55.5171199863229,
-162.351143940503));
#157079=CARTESIAN_POINT('Ctrl Pts',(33.6124477006515,-55.5699325194892,
-162.464771428624));
#157080=CARTESIAN_POINT('Ctrl Pts',(33.6067341407565,-55.6237697200541,
-162.574129314741));
#157081=CARTESIAN_POINT('Ctrl Pts',(33.6012414339651,-55.67832637603,-162.679244507083));
#157082=CARTESIAN_POINT('Ctrl Pts',(33.5953685243728,-55.7366594202596,
-162.791635727812));
#157083=CARTESIAN_POINT('Ctrl Pts',(33.5897480982937,-55.7958148333295,
-162.899176624726));
#157084=CARTESIAN_POINT('Ctrl Pts',(33.5843774549044,-55.8553619694533,
-163.001924469437));
#157085=CARTESIAN_POINT('Ctrl Pts',(33.5798407181868,-55.90566314555,-163.088718524814));
#157086=CARTESIAN_POINT('Ctrl Pts',(33.5754821883936,-55.956242546843,-163.172092965307));
#157087=CARTESIAN_POINT('Ctrl Pts',(33.5712996217319,-56.0068141405006,
-163.252093549704));
#157088=CARTESIAN_POINT('Origin',(60.,-54.58000002,-55.24995));
#157089=CARTESIAN_POINT('',(39.4999999999985,-54.58000002,-66.6681042685273));
#157090=CARTESIAN_POINT('',(39.5,-54.58000002,-65.9723506080548));
#157091=CARTESIAN_POINT('',(33.8499999999899,-54.58000002,-74.1550953619836));
#157092=CARTESIAN_POINT('Ctrl Pts',(39.4999999999959,-54.58000002,-66.6681042685264));
#157093=CARTESIAN_POINT('Ctrl Pts',(37.6706537603941,-54.58000002,-69.204359231621));
#157094=CARTESIAN_POINT('Ctrl Pts',(35.7938421862428,-54.58000002,-71.7056198678132));
#157095=CARTESIAN_POINT('Ctrl Pts',(33.8499999999899,-54.58000002,-74.1550953619836));
#157096=CARTESIAN_POINT('',(33.85,-54.58000002,-157.276549545042));
#157097=CARTESIAN_POINT('Origin',(-3.54807775957937E-14,-73.08000002,3.11172719585489E-30));
#157098=CARTESIAN_POINT('',(40.5,-73.08000002,-174.34995));
#157099=CARTESIAN_POINT('',(41.,-73.08000002,-174.34995));
#157100=CARTESIAN_POINT('',(41.5,-73.08000002,-174.34995));
#157101=CARTESIAN_POINT('',(41.,-73.08000002,-58.24995));
#157102=CARTESIAN_POINT('',(41.,-73.08000002,-58.24995));
#157103=CARTESIAN_POINT('',(40.5,-73.08000002,-58.24995));
#157104=CARTESIAN_POINT('',(-41.5,-73.0800000199999,-58.24995));
#157105=CARTESIAN_POINT('',(40.5,-73.08000002,-174.34995));
#157106=CARTESIAN_POINT('Origin',(-3.3975957231091E-14,-70.08000002,-174.34995));
#157107=CARTESIAN_POINT('',(41.,-70.08000002,-177.34995));
#157108=CARTESIAN_POINT('',(40.5,-70.08000002,-177.34995));
#157109=CARTESIAN_POINT('',(-41.5,-70.08000002,-177.34995));
#157110=CARTESIAN_POINT('Origin',(41.,-70.08000002,-174.34995));
#157111=CARTESIAN_POINT('Origin',(40.5,-70.08000002,-174.34995));
#157112=CARTESIAN_POINT('Origin',(41.5,-73.08000002,-177.34995));
#157113=CARTESIAN_POINT('',(40.5,-63.9875867194884,-177.34995));
#157114=CARTESIAN_POINT('',(40.5,-73.08000002,-177.34995));
#157115=CARTESIAN_POINT('',(41.,-63.9173163021373,-177.34995));
#157116=CARTESIAN_POINT('',(40.227526467895,-64.0258803771248,-177.34995));
#157117=CARTESIAN_POINT('',(41.,-73.08000002,-177.34995));
#157118=CARTESIAN_POINT('Origin',(0.,-12.9675000200281,-60.64995));
#157119=CARTESIAN_POINT('',(38.8323576630952,-56.2084583512428,-61.2273323469212));
#157120=CARTESIAN_POINT('',(33.5881101525803,-60.3971457002532,-61.2273317382593));
#157121=CARTESIAN_POINT('Origin',(0.,-12.9675000200281,-61.2273317382593));
#157122=CARTESIAN_POINT('',(33.5713955981572,-56.0068423841383,-68.80655523181));
#157123=CARTESIAN_POINT('Ctrl Pts',(33.5881101525803,-60.3971457002532,
-61.2273317382593));
#157124=CARTESIAN_POINT('Ctrl Pts',(33.5859966234634,-59.8194297837461,
-62.2410161014668));
#157125=CARTESIAN_POINT('Ctrl Pts',(33.5838660751903,-59.2475976035343,
-63.2383627339802));
#157126=CARTESIAN_POINT('Ctrl Pts',(33.5817197112415,-58.6815774556952,
-64.2193509751279));
#157127=CARTESIAN_POINT('Ctrl Pts',(33.579516248939,-58.1004998341978,-65.2264358219469));
#157128=CARTESIAN_POINT('Ctrl Pts',(33.5772961193852,-57.5255476663152,
-66.2162804051611));
#157129=CARTESIAN_POINT('Ctrl Pts',(33.5750610470281,-56.9566908458864,
-67.1888908421399));
#157130=CARTESIAN_POINT('Ctrl Pts',(33.5738095983383,-56.6381798498937,
-67.7334692103161));
#157131=CARTESIAN_POINT('Ctrl Pts',(33.5725534724423,-56.3215806067112,
-68.2726451091889));
#157132=CARTESIAN_POINT('Ctrl Pts',(33.5712930253538,-56.006893899348,-68.8064232518886));
#157133=CARTESIAN_POINT('Ctrl Pts',(33.5716649935586,-56.0068714411552,
-68.8066912637494));
#157134=CARTESIAN_POINT('Ctrl Pts',(34.023338992169,-56.0244950519456,-68.1812988971121));
#157135=CARTESIAN_POINT('Ctrl Pts',(34.477894463698,-56.042167524175,-67.5449502682449));
#157136=CARTESIAN_POINT('Ctrl Pts',(34.9354108072308,-56.0598757513079,
-66.8975869283598));
#157137=CARTESIAN_POINT('Ctrl Pts',(35.3815636085019,-56.0771441511205,
-66.2663024472423));
#157138=CARTESIAN_POINT('Ctrl Pts',(35.8305319442804,-56.094446553343,-65.6245433868767));
#157139=CARTESIAN_POINT('Ctrl Pts',(36.2823935541714,-56.1117690245108,
-64.9723033619553));
#157140=CARTESIAN_POINT('Ctrl Pts',(36.7172567195688,-56.1284398469034,
-64.3445997561884));
#157141=CARTESIAN_POINT('Ctrl Pts',(37.1547995097133,-56.1451292541387,
-63.7071888252589));
#157142=CARTESIAN_POINT('Ctrl Pts',(37.5950960941535,-56.1618231713757,
-63.0601118262641));
#157143=CARTESIAN_POINT('Ctrl Pts',(38.0051074962401,-56.177368820955,-62.4575431101039));
#157144=CARTESIAN_POINT('Ctrl Pts',(38.41750687348,-56.1929183711655,-61.846592510695));
#157145=CARTESIAN_POINT('Ctrl Pts',(38.8323589160537,-56.2084590974991,
-61.2273337386071));
#157146=CARTESIAN_POINT('Ctrl Pts',(42.0182169324382,-54.58000002,-63.1137016214078));
#157147=CARTESIAN_POINT('Ctrl Pts',(40.2048288919875,-54.58000002,-61.850776413383));
#157148=CARTESIAN_POINT('Ctrl Pts',(38.9841065328395,-56.2141391785318,
-61.0006103127042));
#157149=CARTESIAN_POINT('Ctrl Pts',(39.3891852844759,-54.58000002,-66.8886318537073));
#157150=CARTESIAN_POINT('Ctrl Pts',(37.6731521867469,-54.58000002,-65.6186857176609));
#157151=CARTESIAN_POINT('Ctrl Pts',(36.4598290914011,-56.1197282395838,
-64.7755113243629));
#157152=CARTESIAN_POINT('Ctrl Pts',(36.6602985783386,-54.58000002,-70.6173011253171));
#157153=CARTESIAN_POINT('Ctrl Pts',(35.039043742113,-54.58000002,-69.3609187351473));
#157154=CARTESIAN_POINT('Ctrl Pts',(33.8526449461492,-56.018427265929,-68.5041285748648));
#157155=CARTESIAN_POINT('Ctrl Pts',(33.7990997127136,-54.58000002,-74.2192042704808));
#157156=CARTESIAN_POINT('Ctrl Pts',(32.2647524970408,-54.5800000199999,
-73.0003840144137));
#157157=CARTESIAN_POINT('Ctrl Pts',(31.1389734555133,-55.9114071812081,
-72.1061129617773));
#157158=CARTESIAN_POINT('',(39.2253966502056,-55.8655297208509,-61.2672223984388));
#157159=CARTESIAN_POINT('Ctrl Pts',(39.4999999999998,-54.58000002,-66.6681042685264));
#157160=CARTESIAN_POINT('Ctrl Pts',(39.495523236403,-54.58000002,-66.5799539738083));
#157161=CARTESIAN_POINT('Ctrl Pts',(39.4908202961929,-54.5808808281515,
-66.4866281324533));
#157162=CARTESIAN_POINT('Ctrl Pts',(39.4858571267135,-54.5829895419112,
-66.3881202588974));
#157163=CARTESIAN_POINT('Ctrl Pts',(39.480993916126,-54.5850557858959,-66.2915963469858));
#157164=CARTESIAN_POINT('Ctrl Pts',(39.4758808544998,-54.5883008850007,
-66.1900969985362));
#157165=CARTESIAN_POINT('Ctrl Pts',(39.4704844413006,-54.5931012842766,
-66.0836227128787));
#157166=CARTESIAN_POINT('Ctrl Pts',(39.4697336068659,-54.5937691918188,
-66.0688083246691));
#157167=CARTESIAN_POINT('Ctrl Pts',(39.4689772847685,-54.5944672898739,
-66.0538976389502));
#157168=CARTESIAN_POINT('Ctrl Pts',(39.468215382555,-54.595196672676,-66.0388906681808));
#157169=CARTESIAN_POINT('Ctrl Pts',(39.4623021949749,-54.6008574743503,
-65.9224202975833));
#157170=CARTESIAN_POINT('Ctrl Pts',(39.4560603818811,-54.6083970407844,
-65.8001528088562));
#157171=CARTESIAN_POINT('Ctrl Pts',(39.4495103135196,-54.6183556248677,
-65.6721332133175));
#157172=CARTESIAN_POINT('Ctrl Pts',(39.4462352793388,-54.6233349169094,
-65.6081234155481));
#157173=CARTESIAN_POINT('Ctrl Pts',(39.4428839973304,-54.6289198642788,
-65.5426762103419));
#157174=CARTESIAN_POINT('Ctrl Pts',(39.4394645933395,-54.6351826677793,
-65.4758013974786));
#157175=CARTESIAN_POINT('Ctrl Pts',(39.437754891344,-54.6383140695295,-65.442363991047));
#157176=CARTESIAN_POINT('Ctrl Pts',(39.4360281696955,-54.6416149880493,
-65.4085696904452));
#157177=CARTESIAN_POINT('Ctrl Pts',(39.4342859048123,-54.6450946615458,
-65.3744200607822));
#157178=CARTESIAN_POINT('Ctrl Pts',(39.4334147723707,-54.646834498294,-65.3573452459507));
#157179=CARTESIAN_POINT('Ctrl Pts',(39.4325397546503,-54.6486190265432,
-65.3401815992333));
#157180=CARTESIAN_POINT('Ctrl Pts',(39.4316610537463,-54.6504494140905,
-65.3229293289581));
#157181=CARTESIAN_POINT('Ctrl Pts',(39.4312217032943,-54.6513646078642,
-65.3143031938205));
#157182=CARTESIAN_POINT('Ctrl Pts',(39.4307814320818,-54.6522912666236,
-65.305654902819));
#157183=CARTESIAN_POINT('Ctrl Pts',(39.4303402670448,-54.6532295369723,
-65.2969844832221));
#157184=CARTESIAN_POINT('Ctrl Pts',(39.430009393267,-54.6539332397338,-65.2904816685244));
#157185=CARTESIAN_POINT('Ctrl Pts',(39.4296780167157,-54.6546434740272,
-65.2839664064937));
#157186=CARTESIAN_POINT('Ctrl Pts',(39.4293461491344,-54.6553603018509,
-65.2774387089119));
#157187=CARTESIAN_POINT('Ctrl Pts',(39.4292355266072,-54.6555992444588,
-65.2752628097179));
#157188=CARTESIAN_POINT('Ctrl Pts',(39.4291942240796,-54.6556882995562,
-65.274450489437));
#157189=CARTESIAN_POINT('Ctrl Pts',(39.4290141183437,-54.6560793298168,
-65.2709068666062));
#157190=CARTESIAN_POINT('Ctrl Pts',(39.4232507347946,-54.6685922981555,
-65.1575109360216));
#157191=CARTESIAN_POINT('Ctrl Pts',(39.4178450815666,-54.6819071044714,
-65.0511646649134));
#157192=CARTESIAN_POINT('Ctrl Pts',(39.4127966639773,-54.6954925733759,
-64.9518535498794));
#157193=CARTESIAN_POINT('Ctrl Pts',(39.4079368016429,-54.7085706334722,
-64.8562516431812));
#157194=CARTESIAN_POINT('Ctrl Pts',(39.4034079875762,-54.7218995863115,
-64.7671691893792));
#157195=CARTESIAN_POINT('Ctrl Pts',(39.3992100712441,-54.7350554540221,
-64.6845997089738));
#157196=CARTESIAN_POINT('Ctrl Pts',(39.3950616267999,-54.7480562815743,
-64.6030032989584));
#157197=CARTESIAN_POINT('Ctrl Pts',(39.3912363253505,-54.7608879647296,
-64.5277672359874));
#157198=CARTESIAN_POINT('Ctrl Pts',(39.3877343287418,-54.7731916269955,
-64.4588918939396));
#157199=CARTESIAN_POINT('Ctrl Pts',(39.3842823576569,-54.7853195331948,
-64.3910004263623));
#157200=CARTESIAN_POINT('Ctrl Pts',(39.3811445195931,-54.796934330417,-64.3292892396896));
#157201=CARTESIAN_POINT('Ctrl Pts',(39.3783212885897,-54.8077427493247,
-64.2737654283553));
#157202=CARTESIAN_POINT('Ctrl Pts',(39.3778747135099,-54.809452411244,-64.2649827426853));
#157203=CARTESIAN_POINT('Ctrl Pts',(39.3774360107346,-54.8111420022469,
-64.2563548824163));
#157204=CARTESIAN_POINT('Ctrl Pts',(39.3770051829108,-54.8128104810774,
-64.2478818916985));
#157205=CARTESIAN_POINT('Ctrl Pts',(39.3743361892215,-54.8231467667669,
-64.1953914128839));
#157206=CARTESIAN_POINT('Ctrl Pts',(39.371967988214,-54.8326738045252,-64.1488179262381));
#157207=CARTESIAN_POINT('Ctrl Pts',(39.369899295881,-54.8411825869057,-64.1081353024567));
#157208=CARTESIAN_POINT('Ctrl Pts',(39.3678433023701,-54.8496391374912,
-64.0677024119946));
#157209=CARTESIAN_POINT('Ctrl Pts',(39.3660831513506,-54.857089892747,-64.03308828041));
#157210=CARTESIAN_POINT('Ctrl Pts',(39.3646179182847,-54.8633802441861,
-64.0042741362313));
#157211=CARTESIAN_POINT('Ctrl Pts',(39.3631516508793,-54.8696750361198,
-63.9754396515278));
#157212=CARTESIAN_POINT('Ctrl Pts',(39.3619807133368,-54.8748077492079,
-63.9524132576399));
#157213=CARTESIAN_POINT('Ctrl Pts',(39.3611042771126,-54.8786758154394,
-63.9351782941354));
#157214=CARTESIAN_POINT('Ctrl Pts',(39.3602895559443,-54.8822715082603,
-63.9191569463013));
#157215=CARTESIAN_POINT('Ctrl Pts',(39.3597293339265,-54.8847748380768,
-63.9081403809706));
#157216=CARTESIAN_POINT('Ctrl Pts',(39.3594232718812,-54.8861432861055,
-63.9021217828994));
#157217=CARTESIAN_POINT('Ctrl Pts',(39.3593226039518,-54.8865933870957,
-63.9001421849207));
#157218=CARTESIAN_POINT('Ctrl Pts',(39.359249433704,-54.8869210418335,-63.8987033204161));
#157219=CARTESIAN_POINT('Ctrl Pts',(39.3592037570943,-54.8871256249942,
-63.8978051077709));
#157220=CARTESIAN_POINT('Ctrl Pts',(39.3591935404627,-54.8871713847563,
-63.8976042017099));
#157221=CARTESIAN_POINT('Ctrl Pts',(39.3591846993252,-54.8872109892174,
-63.8974303442201));
#157222=CARTESIAN_POINT('Ctrl Pts',(39.3591772336508,-54.8872444346251,
-63.8972835346803));
#157223=CARTESIAN_POINT('Ctrl Pts',(39.3591735008137,-54.8872611573289,
-63.8972101299104));
#157224=CARTESIAN_POINT('Ctrl Pts',(39.3591701118425,-54.8872763402874,
-63.8971434871318));
#157225=CARTESIAN_POINT('Ctrl Pts',(39.3591670667343,-54.887289983141,-63.8970836062849));
#157226=CARTESIAN_POINT('Ctrl Pts',(39.3591655441802,-54.8872968045678,
-63.8970536658614));
#157227=CARTESIAN_POINT('Ctrl Pts',(39.3591900763927,-54.8871869022241,
-63.8975360766884));
#157228=CARTESIAN_POINT('Ctrl Pts',(39.3592017106449,-54.8871347946242,
-63.897764848134));
#157229=CARTESIAN_POINT('Ctrl Pts',(39.359213344897,-54.8870826870244,-63.8979936195796));
#157230=CARTESIAN_POINT('Ctrl Pts',(39.3592120810124,-54.8870883035032,
-63.8979687479432));
#157231=CARTESIAN_POINT('Ctrl Pts',(39.3591589665828,-54.8873262900705,
-63.8969242492737));
#157232=CARTESIAN_POINT('Ctrl Pts',(39.3534773448721,-54.9127835840158,
-63.7851947934758));
#157233=CARTESIAN_POINT('Ctrl Pts',(39.3479856206203,-54.9391109216136,
-63.6772073597653));
#157234=CARTESIAN_POINT('Ctrl Pts',(39.3426855452689,-54.966034304412,-63.5729933103322));
#157235=CARTESIAN_POINT('Ctrl Pts',(39.337116117579,-54.9943259462696,-63.4634830535726));
#157236=CARTESIAN_POINT('Ctrl Pts',(39.3317582956126,-55.0232755056928,
-63.3581391118471));
#157237=CARTESIAN_POINT('Ctrl Pts',(39.3266113718449,-55.052586215412,-63.2569443988532));
#157238=CARTESIAN_POINT('Ctrl Pts',(39.3249343634493,-55.0621364455105,
-63.2239723963631));
#157239=CARTESIAN_POINT('Ctrl Pts',(39.3232797251223,-55.071725193134,-63.1914405077103));
#157240=CARTESIAN_POINT('Ctrl Pts',(39.3216473789753,-55.0813427108627,
-63.159347100086));
#157241=CARTESIAN_POINT('Ctrl Pts',(39.3163246960283,-55.1127030921774,
-63.0546983196863));
#157242=CARTESIAN_POINT('Ctrl Pts',(39.3112522088888,-55.1443595066673,
-62.954726789106));
#157243=CARTESIAN_POINT('Ctrl Pts',(39.3064521227518,-55.1759617601416,
-62.8593924163544));
#157244=CARTESIAN_POINT('Ctrl Pts',(39.306107452178,-55.1782309625117,-62.8525469239979));
#157245=CARTESIAN_POINT('Ctrl Pts',(39.3057641849582,-55.1804998949383,
-62.845725320774));
#157246=CARTESIAN_POINT('Ctrl Pts',(39.3054223287976,-55.1827684321607,
-62.8389275828999));
#157247=CARTESIAN_POINT('Ctrl Pts',(39.3028709552403,-55.1996991958884,
-62.7881940561616));
#157248=CARTESIAN_POINT('Ctrl Pts',(39.3003875354856,-55.2166118918502,
-62.7387919172498));
#157249=CARTESIAN_POINT('Ctrl Pts',(39.2979654360815,-55.2334594185815,
-62.6907137704932));
#157250=CARTESIAN_POINT('Ctrl Pts',(39.2967543863794,-55.2418831819471,
-62.6666746971149));
#157251=CARTESIAN_POINT('Ctrl Pts',(39.2955586742956,-55.250290669231,-62.6429666270713));
#157252=CARTESIAN_POINT('Ctrl Pts',(39.2943772688074,-55.2586762672058,
-62.6195885146807));
#157253=CARTESIAN_POINT('Ctrl Pts',(39.2937865660632,-55.2628690661932,
-62.6078994584855));
#157254=CARTESIAN_POINT('Ctrl Pts',(39.2931994405157,-55.2670563940624,
-62.5962928920887));
#157255=CARTESIAN_POINT('Ctrl Pts',(39.2926157608318,-55.2712375603914,
-62.58476868362));
#157256=CARTESIAN_POINT('Ctrl Pts',(39.2923239209898,-55.2733281435559,
-62.5790065793857));
#157257=CARTESIAN_POINT('Ctrl Pts',(39.2920329426495,-55.2754171864107,
-62.5732650646585));
#157258=CARTESIAN_POINT('Ctrl Pts',(39.2917428087709,-55.2775046036935,
-62.5675441225895));
#157259=CARTESIAN_POINT('Ctrl Pts',(39.2915090535797,-55.2791863949705,
-62.5629348714603));
#157260=CARTESIAN_POINT('Ctrl Pts',(39.2913400018075,-55.2804046703665,
-62.5596019669335));
#157261=CARTESIAN_POINT('Ctrl Pts',(39.2910805711966,-55.2822769572449,
-62.554492614977));
#157262=CARTESIAN_POINT('Ctrl Pts',(39.2910179999347,-55.2827285282922,
-62.5532603062746));
#157263=CARTESIAN_POINT('Ctrl Pts',(39.29095017263,-55.2832182167915,-62.5519246872481));
#157264=CARTESIAN_POINT('Ctrl Pts',(39.2908749168058,-55.2837618804591,
-62.5504429930271));
#157265=CARTESIAN_POINT('Ctrl Pts',(39.2844820573665,-55.3299452216857,
-62.4245754872765));
#157266=CARTESIAN_POINT('Ctrl Pts',(39.2782741629842,-55.3774330170781,
-62.3027126717482));
#157267=CARTESIAN_POINT('Ctrl Pts',(39.2722610566445,-55.4260061918257,
-62.1848677196681));
#157268=CARTESIAN_POINT('Ctrl Pts',(39.2660766425471,-55.4759631707472,
-62.0636654754735));
#157269=CARTESIAN_POINT('Ctrl Pts',(39.26009828666,-55.5270679896246,-61.946713217043));
#157270=CARTESIAN_POINT('Ctrl Pts',(39.254335463863,-55.5790290546349,-61.8340043906321));
#157271=CARTESIAN_POINT('Ctrl Pts',(39.2482258756724,-55.6341167643111,
-61.7145135544448));
#157272=CARTESIAN_POINT('Ctrl Pts',(39.2423585567611,-55.6901667039142,
-61.5997921748508));
#157273=CARTESIAN_POINT('Ctrl Pts',(39.2367431964852,-55.7467753028942,
-61.4898098101459));
#157274=CARTESIAN_POINT('Ctrl Pts',(39.2328382758321,-55.7861409137256,
-61.4133280910202));
#157275=CARTESIAN_POINT('Ctrl Pts',(39.2290551619518,-55.8257754618418,
-61.3391375767458));
#157276=CARTESIAN_POINT('Ctrl Pts',(39.2253966502057,-55.8655297208508,
-61.2672223984388));
#157277=CARTESIAN_POINT('Ctrl Pts',(39.2253966502054,-55.865529720851,-61.2672223984388));
#157278=CARTESIAN_POINT('Ctrl Pts',(39.0894849099381,-55.973106721351,-61.2534405956196));
#157279=CARTESIAN_POINT('Ctrl Pts',(38.9583675005087,-56.087272628509,-61.2401323247394));
#157280=CARTESIAN_POINT('Ctrl Pts',(38.8323573704738,-56.2084579968516,
-61.2273318724241));
#157281=CARTESIAN_POINT('Ctrl Pts',(33.5713705761603,-56.0068466996901,
-68.8065662520943));
#157282=CARTESIAN_POINT('Ctrl Pts',(33.5716407255132,-56.0065270796914,
-68.8073048104027));
#157283=CARTESIAN_POINT('Ctrl Pts',(33.571763596338,-56.0045950124546,-68.8104067087827));
#157284=CARTESIAN_POINT('Ctrl Pts',(33.5721706506023,-55.9991005135222,
-68.8191908544081));
#157285=CARTESIAN_POINT('Ctrl Pts',(33.5724492473124,-55.9954676511144,
-68.8249939058348));
#157286=CARTESIAN_POINT('Ctrl Pts',(33.5728282689527,-55.9907549991229,
-68.8325305810644));
#157287=CARTESIAN_POINT('Ctrl Pts',(33.5731041457865,-55.9873742312304,
-68.8379409991175));
#157288=CARTESIAN_POINT('Ctrl Pts',(33.5733343137518,-55.9846017185724,
-68.8423820318139));
#157289=CARTESIAN_POINT('Ctrl Pts',(33.5740628471358,-55.9759052979108,
-68.8563203448581));
#157290=CARTESIAN_POINT('Ctrl Pts',(33.5747259271068,-55.9680435604782,
-68.8690049728665));
#157291=CARTESIAN_POINT('Ctrl Pts',(33.5766727727727,-55.9451279534846,
-68.9062215166601));
#157292=CARTESIAN_POINT('Ctrl Pts',(33.5780152783015,-55.9295406414513,
-68.9318763717004));
#157293=CARTESIAN_POINT('Ctrl Pts',(33.5806116739953,-55.8998032246295,
-68.9814610011427));
#157294=CARTESIAN_POINT('Ctrl Pts',(33.5819227551623,-55.8849811468815,
-69.0064972151006));
#157295=CARTESIAN_POINT('Ctrl Pts',(33.5845705352917,-55.8554389192834,
-69.0570579760427));
#157296=CARTESIAN_POINT('Ctrl Pts',(33.5859648027717,-55.8400931028538,
-69.0836819419351));
#157297=CARTESIAN_POINT('Ctrl Pts',(33.5898400697109,-55.7979757190093,
-69.1576904032815));
#157298=CARTESIAN_POINT('Ctrl Pts',(33.5937887266916,-55.7560919721939,
-69.2331703700131));
#157299=CARTESIAN_POINT('Ctrl Pts',(33.5985250010602,-55.7077292668964,
-69.3238132173549));
#157300=CARTESIAN_POINT('Ctrl Pts',(33.6005822539447,-55.6871201048491,
-69.3632141538798));
#157301=CARTESIAN_POINT('Ctrl Pts',(33.6019597992385,-55.6734079620416,
-69.3896046055977));
#157302=CARTESIAN_POINT('Ctrl Pts',(33.6027160054383,-55.6659325257803,
-69.4040961057493));
#157303=CARTESIAN_POINT('Ctrl Pts',(33.6083893848232,-55.6101758456577,
-69.5128495384139));
#157304=CARTESIAN_POINT('Ctrl Pts',(33.6136342702573,-55.5608215111131,
-69.613836091737));
#157305=CARTESIAN_POINT('Ctrl Pts',(33.6218546903343,-55.4875927031781,
-69.7718651036816));
#157306=CARTESIAN_POINT('Ctrl Pts',(33.6260524855428,-55.4511796496671,
-69.8525164490197));
#157307=CARTESIAN_POINT('Ctrl Pts',(33.6311062438331,-55.4091644471695,
-69.9494849851258));
#157308=CARTESIAN_POINT('Ctrl Pts',(33.633671936046,-55.3882882683558,-69.9986889872937));
#157309=CARTESIAN_POINT('Ctrl Pts',(33.6347797887555,-55.3793710855899,
-70.0199307304866));
#157310=CARTESIAN_POINT('Ctrl Pts',(33.6355201880339,-55.3734330861315,
-70.0341261927124));
#157311=CARTESIAN_POINT('Ctrl Pts',(33.6359696672266,-55.3698435365156,
-70.0427433731727));
#157312=CARTESIAN_POINT('Ctrl Pts',(33.6456605291765,-55.2926836875688,
-70.228524654433));
#157313=CARTESIAN_POINT('Ctrl Pts',(33.6559356302676,-55.2164164760441,
-70.4286045583069));
#157314=CARTESIAN_POINT('Ctrl Pts',(33.673171806379,-55.1046321197711,-70.7593432066334));
#157315=CARTESIAN_POINT('Ctrl Pts',(33.6792132916678,-55.0678175042389,
-70.8746875304398));
#157316=CARTESIAN_POINT('Ctrl Pts',(33.6886934938914,-55.0139506128507,
-71.0553819190524));
#157317=CARTESIAN_POINT('Ctrl Pts',(33.6935370007537,-54.987356742398,-71.1476478424839));
#157318=CARTESIAN_POINT('Ctrl Pts',(33.6993504871532,-54.9570822780224,
-71.2586472129303));
#157319=CARTESIAN_POINT('Ctrl Pts',(33.7022946123362,-54.9421531363248,
-71.3149848772055));
#157320=CARTESIAN_POINT('Ctrl Pts',(33.7038813586064,-54.9342138292439,
-71.3453900726014));
#157321=CARTESIAN_POINT('Ctrl Pts',(33.704624367107,-54.9305251002979,-71.3596402001894));
#157322=CARTESIAN_POINT('Ctrl Pts',(33.7050495491287,-54.9284213105411,
-71.3677980732163));
#157323=CARTESIAN_POINT('Ctrl Pts',(33.7052491662678,-54.9274352281448,
-71.371628851342));
#157324=CARTESIAN_POINT('Ctrl Pts',(33.7069422801926,-54.9190764485954,
-71.4041231748996));
#157325=CARTESIAN_POINT('Ctrl Pts',(33.7130531741981,-54.884534886557,-71.5342184997344));
#157326=CARTESIAN_POINT('Ctrl Pts',(33.7307728610088,-54.8097058756137,
-71.8787180674662));
#157327=CARTESIAN_POINT('Ctrl Pts',(33.7381334527421,-54.7811877769103,
-72.0184836933547));
#157328=CARTESIAN_POINT('Ctrl Pts',(33.7513335591963,-54.7374161896249,
-72.2658215103054));
#157329=CARTESIAN_POINT('Ctrl Pts',(33.7560887124468,-54.7226759772122,
-72.354546583101));
#157330=CARTESIAN_POINT('Ctrl Pts',(33.7636849639329,-54.7010223535207,
-72.4970490085014));
#157331=CARTESIAN_POINT('Ctrl Pts',(33.7675980837435,-54.6903110456761,
-72.5706533552747));
#157332=CARTESIAN_POINT('Ctrl Pts',(33.7723387369823,-54.678178773344,-72.660635090891));
#157333=CARTESIAN_POINT('Ctrl Pts',(33.7747487362382,-54.6722248501104,
-72.7066518276824));
#157334=CARTESIAN_POINT('Ctrl Pts',(33.7759631018253,-54.6692786047312,
-72.7299164371522));
#157335=CARTESIAN_POINT('Ctrl Pts',(33.7764854891564,-54.6680227978837,
-72.7399418666397));
#157336=CARTESIAN_POINT('Ctrl Pts',(33.7768341725156,-54.6671871520272,
-72.7466376793895));
#157337=CARTESIAN_POINT('Ctrl Pts',(33.7770694365511,-54.6666255109262,
-72.7511589231412));
#157338=CARTESIAN_POINT('Ctrl Pts',(33.8063811783703,-54.5968113004879,
-73.3147231974228));
#157339=CARTESIAN_POINT('Ctrl Pts',(33.8306904602248,-54.5800000405386,
-73.7828685758946));
#157340=CARTESIAN_POINT('Ctrl Pts',(33.8499999999899,-54.58000002,-74.1550953619836));
#157341=CARTESIAN_POINT('Origin',(57.,-2.42462934179819E-14,-174.34995));
#157342=CARTESIAN_POINT('',(60.,11.11999998,-174.34995));
#157343=CARTESIAN_POINT('',(60.,11.61999998,-174.34995));
#157344=CARTESIAN_POINT('',(60.,28.41999998,-174.34995));
#157345=CARTESIAN_POINT('',(57.,11.11999998,-177.34995));
#157346=CARTESIAN_POINT('Origin',(57.,11.11999998,-174.34995));
#157347=CARTESIAN_POINT('',(57.,11.61999998,-177.34995));
#157348=CARTESIAN_POINT('',(57.,-54.58000002,-177.34995));
#157349=CARTESIAN_POINT('Origin',(57.,11.61999998,-174.34995));
#157350=CARTESIAN_POINT('Origin',(60.,28.41999998,-177.34995));
#157351=CARTESIAN_POINT('',(53.8590042959267,11.11999998,-177.34995));
#157352=CARTESIAN_POINT('',(60.,11.11999998,-177.34995));
#157353=CARTESIAN_POINT('',(53.6325912458891,11.61999998,-177.34995));
#157354=CARTESIAN_POINT('Origin',(0.,-12.9675000200281,-177.34995));
#157355=CARTESIAN_POINT('',(60.,11.61999998,-177.34995));
#157356=CARTESIAN_POINT('Origin',(39.,46.91999998,-129.34995));
#157357=CARTESIAN_POINT('',(39.,4.46999998000001,-135.863383986541));
#157358=CARTESIAN_POINT('',(39.0000000003307,10.11999998,-140.924467062102));
#157359=CARTESIAN_POINT('Ctrl Pts',(39.,4.46999998000001,-135.863383986541));
#157360=CARTESIAN_POINT('Ctrl Pts',(39.0000000000005,4.88328157550195,-136.189917146856));
#157361=CARTESIAN_POINT('Ctrl Pts',(39.0000000000119,5.29116221661631,-136.522117224197));
#157362=CARTESIAN_POINT('Ctrl Pts',(39.0000000000389,5.69434025783604,-136.859675625831));
#157363=CARTESIAN_POINT('Ctrl Pts',(39.0000000000669,6.11191405993836,-137.209286792093));
#157364=CARTESIAN_POINT('Ctrl Pts',(39.0000000001116,6.52444323388668,-137.564646050799));
#157365=CARTESIAN_POINT('Ctrl Pts',(39.0000000001789,6.93266997768885,-137.925456663962));
#157366=CARTESIAN_POINT('Ctrl Pts',(39.0000000002504,7.36643947058691,-138.308843198726));
#157367=CARTESIAN_POINT('Ctrl Pts',(39.0000000003473,7.7953511045625,-138.698384855374));
#157368=CARTESIAN_POINT('Ctrl Pts',(39.0000000004772,8.2202608237891,-139.093772869124));
#157369=CARTESIAN_POINT('Ctrl Pts',(39.0000000004994,8.29309080500349,-139.161542798384));
#157370=CARTESIAN_POINT('Ctrl Pts',(39.0000000005226,8.36580314365992,-139.229484583898));
#157371=CARTESIAN_POINT('Ctrl Pts',(39.0000000005469,8.43840206333325,-139.297596789496));
#157372=CARTESIAN_POINT('Ctrl Pts',(39.0000000006997,8.89608996002628,-139.726998938443));
#157373=CARTESIAN_POINT('Ctrl Pts',(39.0000000008925,9.34761173379244,-140.161633014658));
#157374=CARTESIAN_POINT('Ctrl Pts',(39.0000000011356,9.79388080740657,-140.6013308485));
#157375=CARTESIAN_POINT('Ctrl Pts',(39.0000000011949,9.90289654251582,-140.70874134458));
#157376=CARTESIAN_POINT('Ctrl Pts',(39.0000000012573,10.011598622152,-140.816454152329));
#157377=CARTESIAN_POINT('Ctrl Pts',(39.0000000013228,10.1199999800001,-140.924467062102));
#157378=CARTESIAN_POINT('',(39.0000000003509,10.11999998,-91.1341759094044));
#157379=CARTESIAN_POINT('',(39.,10.11999998,-129.34995));
#157380=CARTESIAN_POINT('',(39.,4.46999998000002,-96.1952589849652));
#157381=CARTESIAN_POINT('Ctrl Pts',(39.0000000014036,10.11999998,-91.1341759094044));
#157382=CARTESIAN_POINT('Ctrl Pts',(39.0000000011199,9.67730365007889,-91.575285870475));
#157383=CARTESIAN_POINT('Ctrl Pts',(39.0000000008904,9.22960685190676,-92.0113795711832));
#157384=CARTESIAN_POINT('Ctrl Pts',(39.0000000007062,8.77598048492635,-92.4423316322574));
#157385=CARTESIAN_POINT('Ctrl Pts',(39.0000000006606,8.66387047835803,-92.5488378715646));
#157386=CARTESIAN_POINT('Ctrl Pts',(39.0000000006178,8.55139809477872,-92.6550299299106));
#157387=CARTESIAN_POINT('Ctrl Pts',(39.0000000005776,8.43854888592038,-92.7609056252127));
#157388=CARTESIAN_POINT('Ctrl Pts',(39.0000000004289,8.02088208266706,-93.1527627205917));
#157389=CARTESIAN_POINT('Ctrl Pts',(39.000000000316,7.59947404051456,-93.5389725674448));
#157390=CARTESIAN_POINT('Ctrl Pts',(39.0000000002313,7.17350510090081,-93.9192513866299));
#157391=CARTESIAN_POINT('Ctrl Pts',(39.0000000001502,6.7660803065941,-94.2829751356576));
#157392=CARTESIAN_POINT('Ctrl Pts',(39.000000000095,6.35448332392143,-94.6412733529686));
#157393=CARTESIAN_POINT('Ctrl Pts',(39.0000000000588,5.93796915862382,-94.9938596181638));
#157394=CARTESIAN_POINT('Ctrl Pts',(39.0000000000244,5.54178994073892,-95.3292320074371));
#157395=CARTESIAN_POINT('Ctrl Pts',(39.0000000000072,5.14116207564722,-95.659436734842));
#157396=CARTESIAN_POINT('Ctrl Pts',(39.0000000000019,4.73541621354422,-95.9841886225431));
#157397=CARTESIAN_POINT('Ctrl Pts',(39.0000000000007,4.64718860206996,-96.0548044588332));
#157398=CARTESIAN_POINT('Ctrl Pts',(39.0000000000001,4.55871888397169,-96.1251623138121));
#157399=CARTESIAN_POINT('Ctrl Pts',(39.,4.46999998000004,-96.1952589849652));
#157400=CARTESIAN_POINT('',(39.,4.46999998000002,-129.34995));
#157401=CARTESIAN_POINT('Ctrl Pts',(40.0658656066501,9.93539045625896,-145.165138021572));
#157402=CARTESIAN_POINT('Ctrl Pts',(39.,10.925678886939,-144.234640983567));
#157403=CARTESIAN_POINT('Ctrl Pts',(39.,12.1842637898263,-143.052046612136));
#157404=CARTESIAN_POINT('Ctrl Pts',(40.0194683031852,8.81214956439894,-143.88333842497));
#157405=CARTESIAN_POINT('Ctrl Pts',(39.,9.77621090664518,-142.950028351532));
#157406=CARTESIAN_POINT('Ctrl Pts',(39.,10.979841755805,-141.770231455688));
#157407=CARTESIAN_POINT('Ctrl Pts',(39.9723350288336,7.65540581054358,-142.626946488088));
#157408=CARTESIAN_POINT('Ctrl Pts',(38.9999999999938,8.58671673912124,-141.687354999621));
#157409=CARTESIAN_POINT('Ctrl Pts',(39.,9.73492905398707,-140.513855077087));
#157410=CARTESIAN_POINT('Ctrl Pts',(39.8778674168776,5.25663147225476,-140.194322050342));
#157411=CARTESIAN_POINT('Ctrl Pts',(39.0000000000061,6.11210395701397,-139.242594421298));
#157412=CARTESIAN_POINT('Ctrl Pts',(39.,7.14197626750154,-138.081230637578));
#157413=CARTESIAN_POINT('Ctrl Pts',(39.8310080868429,4.02695569272985,-139.030438961711));
#157414=CARTESIAN_POINT('Ctrl Pts',(39.,4.84002925713993,-138.072329022275));
#157415=CARTESIAN_POINT('Ctrl Pts',(39.,5.8072721390059,-136.917329731646));
#157416=CARTESIAN_POINT('Ctrl Pts',(39.785612724228,2.75522931487726,-137.937569266631));
#157417=CARTESIAN_POINT('Ctrl Pts',(39.,3.51696507435961,-136.97110396566));
#157418=CARTESIAN_POINT('Ctrl Pts',(39.,4.42069758591766,-135.824477851673));
#157419=CARTESIAN_POINT('',(40.0642139599405,9.89540189006471,-145.119531500823));
#157420=CARTESIAN_POINT('',(39.8417543169614,4.28989009289605,-139.307982736423));
#157421=CARTESIAN_POINT('Ctrl Pts',(40.0642139728404,9.89540198157303,-145.11953138824));
#157422=CARTESIAN_POINT('Ctrl Pts',(40.0490672312073,9.52858910434629,-144.701432431427));
#157423=CARTESIAN_POINT('Ctrl Pts',(40.0340775687819,9.16386888011769,-144.292528978177));
#157424=CARTESIAN_POINT('Ctrl Pts',(40.0192554498771,8.80086505585303,-143.892595037891));
#157425=CARTESIAN_POINT('Ctrl Pts',(40.0026735092318,8.39476199416364,-143.445177168527));
#157426=CARTESIAN_POINT('Ctrl Pts',(39.9863012938639,7.99080764660249,-143.008984945727));
#157427=CARTESIAN_POINT('Ctrl Pts',(39.9701472616296,7.5884884611955,-142.583631867571));
#157428=CARTESIAN_POINT('Ctrl Pts',(39.9549376693659,7.20969072938624,-142.183146911676));
#157429=CARTESIAN_POINT('Ctrl Pts',(39.9399213864914,6.83234320991116,-141.792269106813));
#157430=CARTESIAN_POINT('Ctrl Pts',(39.925101121935,6.45601873886265,-141.410634166036));
#157431=CARTESIAN_POINT('Ctrl Pts',(39.9070625690653,5.9979736856591,-140.946125450285));
#157432=CARTESIAN_POINT('Ctrl Pts',(39.8893840622469,5.54324262799147,-140.497110855627));
#157433=CARTESIAN_POINT('Ctrl Pts',(39.872080343996,5.09074233509129,-140.062917663929));
#157434=CARTESIAN_POINT('Ctrl Pts',(39.8618462222629,4.82311528437996,-139.806118176378));
#157435=CARTESIAN_POINT('Ctrl Pts',(39.8517430061508,4.55626932041237,-139.554502279586));
#157436=CARTESIAN_POINT('Ctrl Pts',(39.8417723415372,4.28998417309766,-139.307926707773));
#157437=CARTESIAN_POINT('Ctrl Pts',(40.0642139578498,9.89540181780599,-145.119531498084));
#157438=CARTESIAN_POINT('Ctrl Pts',(39.9837119096533,9.9031049697781,-144.977776866857));
#157439=CARTESIAN_POINT('Ctrl Pts',(39.9033047333671,9.91139396310649,-144.824952312001));
#157440=CARTESIAN_POINT('Ctrl Pts',(39.7852935726608,9.9248259446457,-144.578638079069));
#157441=CARTESIAN_POINT('Ctrl Pts',(39.7463938137604,9.92946595900602,-144.493689828532));
#157442=CARTESIAN_POINT('Ctrl Pts',(39.6890397168151,9.9366461072912,-144.36197286233));
#157443=CARTESIAN_POINT('Ctrl Pts',(39.6606118595104,9.94029076562729,-144.2950410825));
#157444=CARTESIAN_POINT('Ctrl Pts',(39.6279593144707,9.94462815869065,-144.215073303383));
#157445=CARTESIAN_POINT('Ctrl Pts',(39.6117712025815,9.94681650242244,-144.174619255621));
#157446=CARTESIAN_POINT('Ctrl Pts',(39.6048641034372,9.94775838423618,-144.15718106888));
#157447=CARTESIAN_POINT('Ctrl Pts',(39.6002663026222,9.94838717661874,-144.145533226968));
#157448=CARTESIAN_POINT('Ctrl Pts',(39.5972217602901,9.94880504951511,-144.137787256445));
#157449=CARTESIAN_POINT('Ctrl Pts',(39.5463093096446,9.95580814360903,-144.007917527242));
#157450=CARTESIAN_POINT('Ctrl Pts',(39.4916542170312,9.96362771148659,-143.859230612069));
#157451=CARTESIAN_POINT('Ctrl Pts',(39.4071494540781,9.97745077382445,-143.600799527875));
#157452=CARTESIAN_POINT('Ctrl Pts',(39.3785796317958,9.98240180929145,-143.508758121777));
#157453=CARTESIAN_POINT('Ctrl Pts',(39.3359627083911,9.99033143895586,-143.361740135451));
#157454=CARTESIAN_POINT('Ctrl Pts',(39.314715370758,9.99442093206169,-143.285992920656));
#157455=CARTESIAN_POINT('Ctrl Pts',(39.2902343489268,9.99939423749642,-143.193690016968));
#157456=CARTESIAN_POINT('Ctrl Pts',(39.2780969557419,10.0019282957381,-143.14655487039));
#157457=CARTESIAN_POINT('Ctrl Pts',(39.2720573444652,10.0032067423246,-143.122741292126));
#157458=CARTESIAN_POINT('Ctrl Pts',(39.2694755295604,10.0037570444933,-143.112482751614));
#157459=CARTESIAN_POINT('Ctrl Pts',(39.2677558239374,10.004124439372,-143.105632008287));
#157460=CARTESIAN_POINT('Ctrl Pts',(39.2672057147562,10.0042420820058,-143.103438103034));
#157461=CARTESIAN_POINT('Ctrl Pts',(39.1913299145855,10.0205271473602,-142.799601273041));
#157462=CARTESIAN_POINT('Ctrl Pts',(39.1470186327352,10.0338725753239,-142.55835026003));
#157463=CARTESIAN_POINT('Ctrl Pts',(39.1029770738426,10.0481832824593,-142.288135290547));
#157464=CARTESIAN_POINT('Ctrl Pts',(39.0921521568062,10.0520678385991,-142.213264213691));
#157465=CARTESIAN_POINT('Ctrl Pts',(39.0799075063914,10.0566771044917,-142.123910676051));
#157466=CARTESIAN_POINT('Ctrl Pts',(39.0764992482883,10.0580114078987,-142.097949836939));
#157467=CARTESIAN_POINT('Ctrl Pts',(39.0722428292861,10.0597256940649,-142.064751310274));
#157468=CARTESIAN_POINT('Ctrl Pts',(39.0703293336654,10.0605110264876,-142.049587644647));
#157469=CARTESIAN_POINT('Ctrl Pts',(39.0684465687074,10.0613046863452,-142.034409863244));
#157470=CARTESIAN_POINT('Ctrl Pts',(39.0675898962216,10.0616712186324,-142.027449333261));
#157471=CARTESIAN_POINT('Ctrl Pts',(39.0671824151856,10.0618469512748,-142.024126166792));
#157472=CARTESIAN_POINT('Ctrl Pts',(39.0670122165204,10.0619206551731,-142.022735617363));
#157473=CARTESIAN_POINT('Ctrl Pts',(39.0668997329735,10.0619694337677,-142.021816065555));
#157474=CARTESIAN_POINT('Ctrl Pts',(39.0669853751627,10.0619321550857,-142.022517281932));
#157475=CARTESIAN_POINT('Ctrl Pts',(39.0164452565529,10.0839111803066,-141.608863850399));
#157476=CARTESIAN_POINT('Ctrl Pts',(39.0000054549653,10.1032655307119,-141.242483723391));
#157477=CARTESIAN_POINT('Ctrl Pts',(39.,10.11999998,-140.924467062102));
#157478=CARTESIAN_POINT('Ctrl Pts',(39.,4.46999998000002,-135.863383986541));
#157479=CARTESIAN_POINT('Ctrl Pts',(39.,4.4649048304607,-135.964102536252));
#157480=CARTESIAN_POINT('Ctrl Pts',(39.0019791923666,4.45957150846498,-136.069213666802));
#157481=CARTESIAN_POINT('Ctrl Pts',(39.0065120981555,4.45399949430044,-136.178648033205));
#157482=CARTESIAN_POINT('Ctrl Pts',(39.0102594534973,4.44939310757717,-136.269117475238));
#157483=CARTESIAN_POINT('Ctrl Pts',(39.0157536191668,4.44462331813979,-136.362546776375));
#157484=CARTESIAN_POINT('Ctrl Pts',(39.0233429014063,4.4396914744795,-136.458863808463));
#157485=CARTESIAN_POINT('Ctrl Pts',(39.027137542526,4.43722555264935,-136.507022324508));
#157486=CARTESIAN_POINT('Ctrl Pts',(39.0314562808131,4.43471912489781,-136.555902622014));
#157487=CARTESIAN_POINT('Ctrl Pts',(39.0363440945682,4.43217253088145,-136.605492393808));
#157488=CARTESIAN_POINT('Ctrl Pts',(39.0387880014458,4.43089923387327,-136.630287279704));
#157489=CARTESIAN_POINT('Ctrl Pts',(39.0413741920377,4.4296158957776,-136.655259525851));
#157490=CARTESIAN_POINT('Ctrl Pts',(39.0441083522793,4.42832257012126,-136.680407386378));
#157491=CARTESIAN_POINT('Ctrl Pts',(39.0454754324001,4.42767590729309,-136.692981316641));
#157492=CARTESIAN_POINT('Ctrl Pts',(39.0468795052976,4.42702674778821,-136.705599146449));
#157493=CARTESIAN_POINT('Ctrl Pts',(39.0483212846087,4.42637509905493,-136.718260643517));
#157494=CARTESIAN_POINT('Ctrl Pts',(39.0490421742642,4.42604927468829,-136.724591392051));
#157495=CARTESIAN_POINT('Ctrl Pts',(39.0497724905614,4.42572282801754,-136.730933057349));
#157496=CARTESIAN_POINT('Ctrl Pts',(39.050512322863,4.425395760019,-136.737285609543));
#157497=CARTESIAN_POINT('Ctrl Pts',(39.0506203872579,4.42534798648262,-136.738213501861));
#157498=CARTESIAN_POINT('Ctrl Pts',(39.0507286546797,4.42530019969011,-136.739141626453));
#157499=CARTESIAN_POINT('Ctrl Pts',(39.0508371254071,4.42525239964456,-136.740069983224));
#157500=CARTESIAN_POINT('Ctrl Pts',(39.050905139878,4.42522242755084,-136.740652091375));
#157501=CARTESIAN_POINT('Ctrl Pts',(39.0509725129255,4.42519276704729,-136.741228138368));
#157502=CARTESIAN_POINT('Ctrl Pts',(39.0510428967244,4.42516181331133,-136.741829291024));
#157503=CARTESIAN_POINT('Ctrl Pts',(39.051628747135,4.42490416511385,-136.746833077913));
#157504=CARTESIAN_POINT('Ctrl Pts',(39.0523841686075,4.42457546869017,-136.75321552608));
#157505=CARTESIAN_POINT('Ctrl Pts',(39.0527604572301,4.42441269305049,-136.756375896314));
#157506=CARTESIAN_POINT('Ctrl Pts',(39.0588994248826,4.42175708688442,-136.807935814608));
#157507=CARTESIAN_POINT('Ctrl Pts',(39.0661343773194,4.41885667205721,-136.864171648229));
#157508=CARTESIAN_POINT('Ctrl Pts',(39.0747889848578,4.41571105540969,-136.925046284492));
#157509=CARTESIAN_POINT('Ctrl Pts',(39.0830014682778,4.41272613385796,-136.982811115398));
#157510=CARTESIAN_POINT('Ctrl Pts',(39.0924926835029,4.40952042207355,-137.044752833922));
#157511=CARTESIAN_POINT('Ctrl Pts',(39.1035844904071,4.40609375716194,-137.110831569558));
#157512=CARTESIAN_POINT('Ctrl Pts',(39.1155719987269,4.40239037731665,-137.182246389528));
#157513=CARTESIAN_POINT('Ctrl Pts',(39.1294289734821,4.39842885436704,-137.258494527262));
#157514=CARTESIAN_POINT('Ctrl Pts',(39.1456101803986,4.39421132377648,-137.339475634449));
#157515=CARTESIAN_POINT('Ctrl Pts',(39.1617913873151,4.38999379318591,-137.420456741636));
#157516=CARTESIAN_POINT('Ctrl Pts',(39.180298150752,4.38552005634583,-137.506174477798));
#157517=CARTESIAN_POINT('Ctrl Pts',(39.2016291583746,4.38079442929467,-137.596483472856));
#157518=CARTESIAN_POINT('Ctrl Pts',(39.2042389185241,4.38021626846057,-137.607532403155));
#157519=CARTESIAN_POINT('Ctrl Pts',(39.2066394307158,4.37968903599853,-137.617605342405));
#157520=CARTESIAN_POINT('Ctrl Pts',(39.2095655036944,4.37905318437206,-137.629749427704));
#157521=CARTESIAN_POINT('Ctrl Pts',(39.2096485574449,4.37903513633884,-137.630094125816));
#157522=CARTESIAN_POINT('Ctrl Pts',(39.2097320395475,4.3790170007186,-137.630440493425));
#157523=CARTESIAN_POINT('Ctrl Pts',(39.2098159675572,4.37899877386231,-137.630788600126));
#157524=CARTESIAN_POINT('Ctrl Pts',(39.2281276302169,4.37502198416818,-137.70673955509));
#157525=CARTESIAN_POINT('Ctrl Pts',(39.2466813967273,4.37123554737574,-137.778431463205));
#157526=CARTESIAN_POINT('Ctrl Pts',(39.2651044416888,4.36766070800654,-137.845883960537));
#157527=CARTESIAN_POINT('Ctrl Pts',(39.2840409735794,4.3639862307494,-137.915216493215));
#157528=CARTESIAN_POINT('Ctrl Pts',(39.3028391507201,4.36053526087973,-137.980070624068));
#157529=CARTESIAN_POINT('Ctrl Pts',(39.3211407154263,4.35732730003464,-138.040497223528));
#157530=CARTESIAN_POINT('Ctrl Pts',(39.3323413059184,4.35536402223205,-138.077478410997));
#157531=CARTESIAN_POINT('Ctrl Pts',(39.3433568176487,4.35349169612979,-138.11280181407));
#157532=CARTESIAN_POINT('Ctrl Pts',(39.3541139348103,4.35171428876002,-138.146482817966));
#157533=CARTESIAN_POINT('Ctrl Pts',(39.3720039620678,4.34875830475286,-138.202497275065));
#157534=CARTESIAN_POINT('Ctrl Pts',(39.3891776151373,4.34605561713149,-138.253964698044));
#157535=CARTESIAN_POINT('Ctrl Pts',(39.4053429559131,4.34359270394892,-138.300951862157));
#157536=CARTESIAN_POINT('Ctrl Pts',(39.4097047527134,4.34292815087899,-138.313630126409));
#157537=CARTESIAN_POINT('Ctrl Pts',(39.4139934300582,4.34228105444557,-138.325982248389));
#157538=CARTESIAN_POINT('Ctrl Pts',(39.4182038966227,4.34165114941491,-138.338009611435));
#157539=CARTESIAN_POINT('Ctrl Pts',(39.4281113763137,4.34016894519766,-138.366310716144));
#157540=CARTESIAN_POINT('Ctrl Pts',(39.4375853042781,4.33878145855264,-138.392813478883));
#157541=CARTESIAN_POINT('Ctrl Pts',(39.4465655554463,4.33748325874983,-138.417535049933));
#157542=CARTESIAN_POINT('Ctrl Pts',(39.4510556810304,4.33683415884842,-138.429895835458));
#157543=CARTESIAN_POINT('Ctrl Pts',(39.4554224959828,4.33620741251945,-138.441811284974));
#157544=CARTESIAN_POINT('Ctrl Pts',(39.4596592959402,4.33560223077118,-138.453283494151));
#157545=CARTESIAN_POINT('Ctrl Pts',(39.4617776959189,4.33529963989704,-138.45901959874));
#157546=CARTESIAN_POINT('Ctrl Pts',(39.4638635991141,4.33500244217455,-138.464644890844));
#157547=CARTESIAN_POINT('Ctrl Pts',(39.4659162115836,4.33471054561932,-138.470159619889));
#157548=CARTESIAN_POINT('Ctrl Pts',(39.4669425178184,4.3345645973417,-138.472916984412));
#157549=CARTESIAN_POINT('Ctrl Pts',(39.4679605018047,4.33441997448555,-138.475646708015));
#157550=CARTESIAN_POINT('Ctrl Pts',(39.4689700673648,4.33427666540267,-138.478348821464));
#157551=CARTESIAN_POINT('Ctrl Pts',(39.4694748501449,4.33420501086123,-138.479699878188));
#157552=CARTESIAN_POINT('Ctrl Pts',(39.4699775283455,4.33413368477126,-138.481044032364));
#157553=CARTESIAN_POINT('Ctrl Pts',(39.4704780901355,4.33406268566851,-138.482381287809));
#157554=CARTESIAN_POINT('Ctrl Pts',(39.4709786519255,4.33399168656576,-138.483718543254));
#157555=CARTESIAN_POINT('Ctrl Pts',(39.4710360424286,4.33398352830646,-138.483872798879));
#157556=CARTESIAN_POINT('Ctrl Pts',(39.4719734145588,4.33385066787384,-138.486372361736));
#157557=CARTESIAN_POINT('Ctrl Pts',(39.5076868319688,4.32878875069687,-138.581604477941));
#157558=CARTESIAN_POINT('Ctrl Pts',(39.5441541767506,4.3239356277841,-138.67269332793));
#157559=CARTESIAN_POINT('Ctrl Pts',(39.580948614012,4.31929192751637,-138.759679041817));
#157560=CARTESIAN_POINT('Ctrl Pts',(39.6188258809332,4.31451156701532,-138.849224672855));
#157561=CARTESIAN_POINT('Ctrl Pts',(39.65704958739,4.30995310473825,-138.934422681979));
#157562=CARTESIAN_POINT('Ctrl Pts',(39.6951901830099,4.30561446676912,-139.01535983076));
#157563=CARTESIAN_POINT('Ctrl Pts',(39.7348091235138,4.30110766144076,-139.099434136102));
#157564=CARTESIAN_POINT('Ctrl Pts',(39.7743381098534,4.29683801816509,-139.17891148334));
#157565=CARTESIAN_POINT('Ctrl Pts',(39.8133377650709,4.29280078440236,-139.253925691597));
#157566=CARTESIAN_POINT('Ctrl Pts',(39.8228431850076,4.29181678590074,-139.272208969916));
#157567=CARTESIAN_POINT('Ctrl Pts',(39.8323173603756,4.29084658406392,-139.290227256414));
#157568=CARTESIAN_POINT('Ctrl Pts',(39.8417543169614,4.28989009289605,-139.307982736423));
#157569=CARTESIAN_POINT('Origin',(0.,-12.9675000200281,-171.64995));
#157570=CARTESIAN_POINT('',(55.7843555297028,4.33575017898885,-171.449026400902));
#157571=CARTESIAN_POINT('',(53.7255998841352,9.94225131873297,-171.449026400902));
#157572=CARTESIAN_POINT('Origin',(0.,-12.9675000200281,-171.449026400902));
#157573=CARTESIAN_POINT('Ctrl Pts',(53.7255998841352,9.94225131873298,-171.449026400902));
#157574=CARTESIAN_POINT('Ctrl Pts',(53.0048383941293,9.94024676411936,-170.025533543412));
#157575=CARTESIAN_POINT('Ctrl Pts',(52.294948227473,9.93824451327994,-168.627760176666));
#157576=CARTESIAN_POINT('Ctrl Pts',(51.5958827203954,9.9362037934586,-167.255727365281));
#157577=CARTESIAN_POINT('Ctrl Pts',(51.1460015352648,9.93489049528776,-166.372760402993));
#157578=CARTESIAN_POINT('Ctrl Pts',(50.7006043959427,9.93356129347437,-165.50045341864));
#157579=CARTESIAN_POINT('Ctrl Pts',(50.2596888381369,9.93220562599593,-164.638806639518));
#157580=CARTESIAN_POINT('Ctrl Pts',(49.6966641013534,9.93047451374166,-163.53853144526));
#157581=CARTESIAN_POINT('Ctrl Pts',(49.1409444411495,9.92870584879501,-162.455639719489));
#157582=CARTESIAN_POINT('Ctrl Pts',(48.5925279246073,9.92691158097371,-161.390127665526));
#157583=CARTESIAN_POINT('Ctrl Pts',(48.3183196663362,9.92601444706306,-160.857371638545));
#157584=CARTESIAN_POINT('Ctrl Pts',(48.0459373244593,9.92511126710263,-160.328960426286));
#157585=CARTESIAN_POINT('Ctrl Pts',(47.7753813036175,9.92420565463034,-159.804892982715));
#157586=CARTESIAN_POINT('Ctrl Pts',(47.6401032931966,9.9237528483942,-159.542859260929));
#157587=CARTESIAN_POINT('Ctrl Pts',(47.5052818754017,9.92329944091239,-159.281911474732));
#157588=CARTESIAN_POINT('Ctrl Pts',(47.3709171228666,9.92284603234586,-159.022049462581));
#157589=CARTESIAN_POINT('Ctrl Pts',(47.3037347465991,9.92261932806259,-158.892118456506));
#157590=CARTESIAN_POINT('Ctrl Pts',(47.236666537344,9.9223926239238,-158.762458893565));
#157591=CARTESIAN_POINT('Ctrl Pts',(47.1697125068932,9.92216600042275,-158.6330707515));
#157592=CARTESIAN_POINT('Ctrl Pts',(47.1069431033455,9.92195354089051,-158.511769368315));
#157593=CARTESIAN_POINT('Ctrl Pts',(47.0442740522902,9.92174115224678,-158.39070653862));
#157594=CARTESIAN_POINT('Ctrl Pts',(46.9817053643811,9.92152890466437,-158.269882243086));
#157595=CARTESIAN_POINT('Ctrl Pts',(46.9775341185205,9.92151475482554,-158.26182729005));
#157596=CARTESIAN_POINT('Ctrl Pts',(46.9739449851603,9.92150257901683,-158.25489657829));
#157597=CARTESIAN_POINT('Ctrl Pts',(46.969192963075,9.92148646200742,-158.245720565411));
#157598=CARTESIAN_POINT('Ctrl Pts',(46.9690340241742,9.92148592294852,-158.245413659135));
#157599=CARTESIAN_POINT('Ctrl Pts',(46.9688750858378,9.9214853838877,-158.245106754236));
#157600=CARTESIAN_POINT('Ctrl Pts',(46.9687161480657,9.92148484482495,-158.244799850712));
#157601=CARTESIAN_POINT('Ctrl Pts',(46.3446685940074,9.91936828820202,-157.039784889644));
#157602=CARTESIAN_POINT('Ctrl Pts',(45.7293385706448,9.91722214649627,-155.855973727983));
#157603=CARTESIAN_POINT('Ctrl Pts',(45.1226444261086,9.91504615189965,-154.693400464412));
#157604=CARTESIAN_POINT('Ctrl Pts',(44.5040721429633,9.91282755467424,-153.508065803699));
#157605=CARTESIAN_POINT('Ctrl Pts',(43.8944773759627,9.91057792895297,-152.344808699876));
#157606=CARTESIAN_POINT('Ctrl Pts',(43.2938225298004,9.90829822225579,-151.203638927001));
#157607=CARTESIAN_POINT('Ctrl Pts',(42.6723312127876,9.90593943346604,-150.022882441624));
#157608=CARTESIAN_POINT('Ctrl Pts',(42.0604109072536,9.90354844326633,-148.865772219977));
#157609=CARTESIAN_POINT('Ctrl Pts',(41.4580700145246,9.90112755266097,-147.732292127205));
#157610=CARTESIAN_POINT('Ctrl Pts',(40.9875983364426,9.89923666250341,-146.8469624281));
#157611=CARTESIAN_POINT('Ctrl Pts',(40.5229718710177,9.89732755761719,-145.976048274262));
#157612=CARTESIAN_POINT('Ctrl Pts',(40.064213984323,9.8954018152728,-145.1195315447));
#157613=CARTESIAN_POINT('Ctrl Pts',(39.8417798628559,4.28988750369336,-139.308030800137));
#157614=CARTESIAN_POINT('Ctrl Pts',(40.4868859579449,4.29232172358473,-140.57956955374));
#157615=CARTESIAN_POINT('Ctrl Pts',(41.1456653359953,4.2947194009918,-141.882651683976));
#157616=CARTESIAN_POINT('Ctrl Pts',(41.8180607265059,4.29707616997945,-143.217318051408));
#157617=CARTESIAN_POINT('Ctrl Pts',(42.4709012105623,4.29936439834689,-144.5131690487));
#157618=CARTESIAN_POINT('Ctrl Pts',(43.1365771358385,4.30161405421269,-145.838794161371));
#157619=CARTESIAN_POINT('Ctrl Pts',(43.8150777647377,4.30382299667252,-147.194208617093));
#157620=CARTESIAN_POINT('Ctrl Pts',(44.4699896786601,4.30595514316214,-148.502500809534));
#157621=CARTESIAN_POINT('Ctrl Pts',(45.136849288454,4.30804935037138,-149.838545750742));
#157622=CARTESIAN_POINT('Ctrl Pts',(45.8156861354303,4.31010554107007,-151.202330462395));
#157623=CARTESIAN_POINT('Ctrl Pts',(46.4845297539595,4.31213146236976,-152.546038756222));
#157624=CARTESIAN_POINT('Ctrl Pts',(47.1650003076918,4.3141204676528,-153.916676154632));
#157625=CARTESIAN_POINT('Ctrl Pts',(47.8571688879798,4.31607443802584,-155.314205466087));
#157626=CARTESIAN_POINT('Ctrl Pts',(47.8626439628392,4.31608989399187,-155.325259966127));
#157627=CARTESIAN_POINT('Ctrl Pts',(47.8688897641185,4.31610752027897,-155.337870868679));
#157628=CARTESIAN_POINT('Ctrl Pts',(47.8736561032779,4.31612096323088,-155.347494742445));
#157629=CARTESIAN_POINT('Ctrl Pts',(47.8737827560485,4.31612132044153,-155.347750471263));
#157630=CARTESIAN_POINT('Ctrl Pts',(47.8739083642008,4.31612167469916,-155.348004090965));
#157631=CARTESIAN_POINT('Ctrl Pts',(47.8740328855181,4.31612202588467,-155.348255516304));
#157632=CARTESIAN_POINT('Ctrl Pts',(48.6583351081591,4.31833398113315,-156.931867517586));
#157633=CARTESIAN_POINT('Ctrl Pts',(49.4602813144816,4.32050804470002,-158.555378883432));
#157634=CARTESIAN_POINT('Ctrl Pts',(50.2798261127653,4.32264044202089,-160.218817015509));
#157635=CARTESIAN_POINT('Ctrl Pts',(51.0778218667667,4.32471677026001,-161.838516840608));
#157636=CARTESIAN_POINT('Ctrl Pts',(51.8925026843305,4.32675358286625,-163.496071488855));
#157637=CARTESIAN_POINT('Ctrl Pts',(52.7238700838759,4.32874953207866,-165.191483761551));
#157638=CARTESIAN_POINT('Ctrl Pts',(53.5277706787544,4.33067953890847,-166.83088282306));
#157639=CARTESIAN_POINT('Ctrl Pts',(54.3472733569927,4.33257133103891,-168.505679408003));
#157640=CARTESIAN_POINT('Ctrl Pts',(55.1824230680481,4.33442584374162,-170.215853479615));
#157641=CARTESIAN_POINT('Ctrl Pts',(55.3821715796289,4.33486940032455,-170.624887597482));
#157642=CARTESIAN_POINT('Ctrl Pts',(55.582815395474,4.33531083454817,-171.035945398186));
#157643=CARTESIAN_POINT('Ctrl Pts',(55.7843555297028,4.33575017898885,-171.449026400902));
#157644=CARTESIAN_POINT('Origin',(60.,28.41999998,-177.34995));
#157645=CARTESIAN_POINT('',(57.,2.96999998000001,-177.34995));
#157646=CARTESIAN_POINT('',(56.8066553649227,2.96999998000001,-177.34995));
#157647=CARTESIAN_POINT('',(60.,2.96999998000001,-177.34995));
#157648=CARTESIAN_POINT('',(56.6639973329545,3.46999998000001,-177.34995));
#157649=CARTESIAN_POINT('Origin',(0.,-12.9675000200281,-177.34995));
#157650=CARTESIAN_POINT('',(57.,3.46999998000002,-177.34995));
#157651=CARTESIAN_POINT('',(60.,3.46999998000001,-177.34995));
#157652=CARTESIAN_POINT('',(57.,-54.58000002,-177.34995));
#157653=CARTESIAN_POINT('Origin',(60.,-2.55003103885676E-14,0.));
#157654=CARTESIAN_POINT('',(60.,3.46999998000001,-58.24995));
#157655=CARTESIAN_POINT('',(60.,2.96999998000001,-58.24995));
#157656=CARTESIAN_POINT('',(60.,-54.58000002,-58.24995));
#157657=CARTESIAN_POINT('',(60.,2.96999998000001,-174.34995));
#157658=CARTESIAN_POINT('',(60.,2.96999998000001,-174.34995));
#157659=CARTESIAN_POINT('',(60.,3.46999998000001,-174.34995));
#157660=CARTESIAN_POINT('',(60.,28.41999998,-174.34995));
#157661=CARTESIAN_POINT('',(60.,3.46999998000001,-58.24995));
#157662=CARTESIAN_POINT('Origin',(57.,-2.42462934179819E-14,-174.34995));
#157663=CARTESIAN_POINT('Origin',(57.,2.96999998000001,-174.34995));
#157664=CARTESIAN_POINT('Origin',(57.,3.46999998000001,-174.34995));
#157665=CARTESIAN_POINT('Origin',(-83.2809572255632,2.96999998000007,-176.84995));
#157666=CARTESIAN_POINT('',(57.,2.61702308584989,-177.204078948543));
#157667=CARTESIAN_POINT('Origin',(57.,2.96999998000001,-176.84995));
#157668=CARTESIAN_POINT('Ctrl Pts',(57.,2.61702308584994,-177.204078948543));
#157669=CARTESIAN_POINT('Ctrl Pts',(56.9920596731222,2.63188036382227,-177.218887892731));
#157670=CARTESIAN_POINT('Ctrl Pts',(56.9834056339598,2.64801985224532,-177.233109037942));
#157671=CARTESIAN_POINT('Ctrl Pts',(56.9740378825128,2.66543214066919,-177.246483014067));
#157672=CARTESIAN_POINT('Ctrl Pts',(56.9691180761738,2.67457682041948,-177.253506831137));
#157673=CARTESIAN_POINT('Ctrl Pts',(56.9640014139196,2.68407181613746,-177.260296610627));
#157674=CARTESIAN_POINT('Ctrl Pts',(56.9586878957502,2.69391033186455,-177.266812694652));
#157675=CARTESIAN_POINT('Ctrl Pts',(56.9548301627084,2.70105331434672,-177.271543517403));
#157676=CARTESIAN_POINT('Ctrl Pts',(56.9508686652447,2.70837729051018,-177.276130042922));
#157677=CARTESIAN_POINT('Ctrl Pts',(56.9468034033591,2.71587828894132,-177.280556741858));
#157678=CARTESIAN_POINT('Ctrl Pts',(56.9445388538477,2.72005671158906,-177.283022629467));
#157679=CARTESIAN_POINT('Ctrl Pts',(56.942637304404,2.7235662490483,-177.285018059377));
#157680=CARTESIAN_POINT('Ctrl Pts',(56.9408724773909,2.72681209002593,-177.286824867863));
#157681=CARTESIAN_POINT('Ctrl Pts',(56.9394691316813,2.72939310050244,-177.288261596175));
#157682=CARTESIAN_POINT('Ctrl Pts',(56.9381522359377,2.73180827092145,-177.289577706413));
#157683=CARTESIAN_POINT('Ctrl Pts',(56.9368080197773,2.73427291767105,-177.290895293756));
#157684=CARTESIAN_POINT('Ctrl Pts',(56.9307386543405,2.74540121848779,-177.296844425536));
#157685=CARTESIAN_POINT('Ctrl Pts',(56.9241477932597,2.75741692047087,-177.302727797935));
#157686=CARTESIAN_POINT('Ctrl Pts',(56.9170354365348,2.7703598532817,-177.308364462909));
#157687=CARTESIAN_POINT('Ctrl Pts',(56.9095156481655,2.78404422252536,-177.314324024465));
#157688=CARTESIAN_POINT('Ctrl Pts',(56.9014129050262,2.79876611353917,-177.320008025187));
#157689=CARTESIAN_POINT('Ctrl Pts',(56.8927272071169,2.81454408608465,-177.325169386228));
#157690=CARTESIAN_POINT('Ctrl Pts',(56.8843005955034,2.82985141637389,-177.330176788667));
#157691=CARTESIAN_POINT('Ctrl Pts',(56.8753252884202,2.84615339254148,-177.334691867768));
#157692=CARTESIAN_POINT('Ctrl Pts',(56.8658012858673,2.8634291514813,-177.338460653424));
#157693=CARTESIAN_POINT('Ctrl Pts',(56.8567116437613,2.87991701622107,-177.342057556365));
#157694=CARTESIAN_POINT('Ctrl Pts',(56.8471222135273,2.89729223915623,-177.344974141857));
#157695=CARTESIAN_POINT('Ctrl Pts',(56.8370329951653,2.91549476483612,-177.346970302925));
#157696=CARTESIAN_POINT('Ctrl Pts',(56.8273659549057,2.93293561528255,-177.34888293567));
#157697=CARTESIAN_POINT('Ctrl Pts',(56.8172400781582,2.95113622605794,-177.34995));
#157698=CARTESIAN_POINT('Ctrl Pts',(56.8066553649227,2.96999998000001,-177.34995));
#157699=CARTESIAN_POINT('Origin',(39.,46.91999998,-129.34995));
#157700=CARTESIAN_POINT('',(39.0000000012314,1.96999998000004,-98.0457798926543));
#157701=CARTESIAN_POINT('',(39.,-3.68000001999999,-101.255910620448));
#157702=CARTESIAN_POINT('Ctrl Pts',(39.0000000024628,1.96999998000006,-98.0457798926544));
#157703=CARTESIAN_POINT('Ctrl Pts',(39.0000000032442,1.50691588071896,-98.3650262521902));
#157704=CARTESIAN_POINT('Ctrl Pts',(39.0000000016551,1.03814546724657,-98.6748799794054));
#157705=CARTESIAN_POINT('Ctrl Pts',(39.0000000008071,0.562698589411684,
-98.9745405549561));
#157706=CARTESIAN_POINT('Ctrl Pts',(39.0000000004711,0.374284444249737,
-99.0932926044768));
#157707=CARTESIAN_POINT('Ctrl Pts',(39.0000000002453,0.184822272624995,
-99.2104442275613));
#157708=CARTESIAN_POINT('Ctrl Pts',(39.0000000001311,-0.00574774121676395,
-99.3259468990426));
#157709=CARTESIAN_POINT('Ctrl Pts',(38.9999999999777,-0.261894757938799,
-99.4811951677863));
#157710=CARTESIAN_POINT('Ctrl Pts',(39.,-0.520415976845901,-99.6335997492721));
#157711=CARTESIAN_POINT('Ctrl Pts',(39.,-0.780592906922143,-99.7825242060483));
#157712=CARTESIAN_POINT('Ctrl Pts',(39.,-1.12946683952905,-99.9822185482085));
#157713=CARTESIAN_POINT('Ctrl Pts',(39.,-1.48228932648713,-100.176247523887));
#157714=CARTESIAN_POINT('Ctrl Pts',(39.,-1.83764512720228,-100.363126009317));
#157715=CARTESIAN_POINT('Ctrl Pts',(39.0000000000001,-2.17904755464558,
-100.542666538652));
#157716=CARTESIAN_POINT('Ctrl Pts',(39.0000000000001,-2.52330369641992,
-100.715959269876));
#157717=CARTESIAN_POINT('Ctrl Pts',(39.0000000000001,-2.87085998622341,
-100.88265759943));
#157718=CARTESIAN_POINT('Ctrl Pts',(39.0000000000001,-3.13854475841823,
-101.011047174532));
#157719=CARTESIAN_POINT('Ctrl Pts',(39.,-3.40818747901783,-101.135524193408));
#157720=CARTESIAN_POINT('Ctrl Pts',(39.,-3.68000001999998,-101.255910620448));
#157721=CARTESIAN_POINT('',(39.,-3.68000001999998,-130.802732351058));
#157722=CARTESIAN_POINT('',(39.,-3.68000001999999,-129.34995));
#157723=CARTESIAN_POINT('',(39.0000000004655,1.96999998000006,-134.012863078852));
#157724=CARTESIAN_POINT('Ctrl Pts',(39.,-3.68000001999998,-130.802732351058));
#157725=CARTESIAN_POINT('Ctrl Pts',(39.,-3.3350976938153,-130.955490419457));
#157726=CARTESIAN_POINT('Ctrl Pts',(38.999999999995,-2.99379560771499,-131.114791966817));
#157727=CARTESIAN_POINT('Ctrl Pts',(39.0000000000322,-2.6556253235799,-131.280281718424));
#157728=CARTESIAN_POINT('Ctrl Pts',(39.0000000000621,-2.38378986674403,
-131.413309321204));
#157729=CARTESIAN_POINT('Ctrl Pts',(39.0000000001226,-2.1139785184933,-131.550336634986));
#157730=CARTESIAN_POINT('Ctrl Pts',(39.0000000002374,-1.84595706992345,
-131.691201637143));
#157731=CARTESIAN_POINT('Ctrl Pts',(39.0000000003908,-1.48773653906918,
-131.879472897226));
#157732=CARTESIAN_POINT('Ctrl Pts',(39.0000000006483,-1.13214453284304,
-132.074954501691));
#157733=CARTESIAN_POINT('Ctrl Pts',(39.0000000009742,-0.779903543906046,
-132.276609948051));
#157734=CARTESIAN_POINT('Ctrl Pts',(39.0000000012103,-0.524689202150759,
-132.422718332994));
#157735=CARTESIAN_POINT('Ctrl Pts',(39.000000001479,-0.271234086134657,
-132.572069210975));
#157736=CARTESIAN_POINT('Ctrl Pts',(39.0000000017246,-0.0198207958907458,
-132.724283330851));
#157737=CARTESIAN_POINT('Ctrl Pts',(39.0000000020985,0.362997438679328,
-132.956054453973));
#157738=CARTESIAN_POINT('Ctrl Pts',(39.0000000024107,0.740951650741639,
-133.194233184148));
#157739=CARTESIAN_POINT('Ctrl Pts',(39.0000000024159,1.11485984244673,-133.43860998629));
#157740=CARTESIAN_POINT('Ctrl Pts',(39.00000000242,1.40217712996228,-133.626393194792));
#157741=CARTESIAN_POINT('Ctrl Pts',(39.0000000022332,1.68710447741349,-133.817837252074));
#157742=CARTESIAN_POINT('Ctrl Pts',(39.0000000018622,1.96999998000005,-134.012863078852));
#157743=CARTESIAN_POINT('',(39.,1.96999998000002,-129.34995));
#157744=CARTESIAN_POINT('Ctrl Pts',(39.,-3.72521479271581,-130.782753296221));
#157745=CARTESIAN_POINT('Ctrl Pts',(39.,-4.21888391538426,-131.902596984872));
#157746=CARTESIAN_POINT('Ctrl Pts',(39.5652399075022,-4.65674474020595,
-132.895844604925));
#157747=CARTESIAN_POINT('Ctrl Pts',(39.,-3.08946624372919,-131.063015115075));
#157748=CARTESIAN_POINT('Ctrl Pts',(38.9999999999904,-3.61592060950642,
-132.184581657476));
#157749=CARTESIAN_POINT('Ctrl Pts',(39.5781306671204,-4.08236536173137,
-133.176106520795));
#157750=CARTESIAN_POINT('Ctrl Pts',(39.,-2.46339239509573,-131.366669530497));
#157751=CARTESIAN_POINT('Ctrl Pts',(39.,-3.02226593965722,-132.489948109969));
#157752=CARTESIAN_POINT('Ctrl Pts',(39.5919846958087,-3.51592220196165,
-133.479760839166));
#157753=CARTESIAN_POINT('Ctrl Pts',(39.,-1.22847641296741,-132.015647483627));
#157754=CARTESIAN_POINT('Ctrl Pts',(39.,-1.85088554063804,-133.142434340475));
#157755=CARTESIAN_POINT('Ctrl Pts',(39.6212800791283,-2.39690688691799,
-134.128738792364));
#157756=CARTESIAN_POINT('Ctrl Pts',(39.,-0.61794440595705,-132.362031531162));
#157757=CARTESIAN_POINT('Ctrl Pts',(39.,-1.27148303561927,-133.490738119779));
#157758=CARTESIAN_POINT('Ctrl Pts',(39.6367679612577,-1.84279784212966,
-134.475122839821));
#157759=CARTESIAN_POINT('Ctrl Pts',(39.,1.17663045280609,-133.448449910404));
#157760=CARTESIAN_POINT('Ctrl Pts',(39.,0.433753695599258,-134.583900592971));
#157761=CARTESIAN_POINT('Ctrl Pts',(39.6847850431059,-0.21139821211329,
-135.561541219197));
#157762=CARTESIAN_POINT('Ctrl Pts',(39.,2.32236925604725,-134.233515370373));
#157763=CARTESIAN_POINT('Ctrl Pts',(39.,1.52263602949357,-135.373451527488));
#157764=CARTESIAN_POINT('Ctrl Pts',(39.7187663759592,0.83378959624966,-136.346621542847));
#157765=CARTESIAN_POINT('Ctrl Pts',(39.,3.43069435955708,-135.063549838392));
#157766=CARTESIAN_POINT('Ctrl Pts',(39.,2.57493359537216,-136.206226648817));
#157767=CARTESIAN_POINT('Ctrl Pts',(39.7537665531305,1.84818159949203,-137.176641147095));
#157768=CARTESIAN_POINT('',(39.7525218945665,1.81208317188674,-137.147133694481));
#157769=CARTESIAN_POINT('',(39.585730149821,-3.78242344375788,-133.343410042124));
#157770=CARTESIAN_POINT('Ctrl Pts',(39.7525219099498,1.81208323948034,-137.14713352867));
#157771=CARTESIAN_POINT('Ctrl Pts',(39.7388044572068,1.41395416292999,-136.822020786323));
#157772=CARTESIAN_POINT('Ctrl Pts',(39.7254997729288,1.01842473737008,-136.509864953903));
#157773=CARTESIAN_POINT('Ctrl Pts',(39.712614901004,0.624517733625811,-136.210149947402));
#157774=CARTESIAN_POINT('Ctrl Pts',(39.693784203698,0.0488392482247798,
-135.772129096404));
#157775=CARTESIAN_POINT('Ctrl Pts',(39.6758506543709,-0.523370028522445,
-135.360673152285));
#157776=CARTESIAN_POINT('Ctrl Pts',(39.6588130338047,-1.09508430367974,
-134.974099746561));
#157777=CARTESIAN_POINT('Ctrl Pts',(39.6567872693803,-1.16306084036945,
-134.928136365132));
#157778=CARTESIAN_POINT('Ctrl Pts',(39.6547741490203,-1.23103038514879,
-134.882524801265));
#157779=CARTESIAN_POINT('Ctrl Pts',(39.6527736552071,-1.29899796545754,
-134.837262299613));
#157780=CARTESIAN_POINT('Ctrl Pts',(39.6459517210492,-1.53077591681986,
-134.682911506796));
#157781=CARTESIAN_POINT('Ctrl Pts',(39.6392813566793,-1.76247360775619,
-134.53272279422));
#157782=CARTESIAN_POINT('Ctrl Pts',(39.6327764980427,-1.99382554704971,
-134.386891929138));
#157783=CARTESIAN_POINT('Ctrl Pts',(39.6258782044137,-2.23917040356775,
-134.23224073936));
#157784=CARTESIAN_POINT('Ctrl Pts',(39.619166022538,-2.48412652209771,-134.082490044296));
#157785=CARTESIAN_POINT('Ctrl Pts',(39.6126548834015,-2.72843126504667,
-133.937850299462));
#157786=CARTESIAN_POINT('Ctrl Pts',(39.6106277671319,-2.80449078532386,
-133.892819533902));
#157787=CARTESIAN_POINT('Ctrl Pts',(39.6086201268254,-2.88048753715528,
-133.848284024339));
#157788=CARTESIAN_POINT('Ctrl Pts',(39.6066323874685,-2.95641454443982,
-133.804249815765));
#157789=CARTESIAN_POINT('Ctrl Pts',(39.5994131121229,-3.23217402459558,
-133.644321867863));
#157790=CARTESIAN_POINT('Ctrl Pts',(39.5924450145065,-3.50738674925618,
-133.490746661292));
#157791=CARTESIAN_POINT('Ctrl Pts',(39.5857305518838,-3.78242124043357,
-133.343407072386));
#157792=CARTESIAN_POINT('Ctrl Pts',(39.7525218896124,1.81208307130645,-137.147133691772));
#157793=CARTESIAN_POINT('Ctrl Pts',(39.7139087968672,1.81599661082028,-137.07244305817));
#157794=CARTESIAN_POINT('Ctrl Pts',(39.6744474421853,1.82016969113522,-136.992602940359));
#157795=CARTESIAN_POINT('Ctrl Pts',(39.634725153328,1.82460721687045,-136.907430510093));
#157796=CARTESIAN_POINT('Ctrl Pts',(39.6193838930589,1.82632104654174,-136.874535819026));
#157797=CARTESIAN_POINT('Ctrl Pts',(39.6040042538397,1.82807431955759,-136.840845596339));
#157798=CARTESIAN_POINT('Ctrl Pts',(39.5886220325896,1.82986730990165,-136.806348725811));
#157799=CARTESIAN_POINT('Ctrl Pts',(39.5610167425994,1.83308505183843,-136.744439844176));
#157800=CARTESIAN_POINT('Ctrl Pts',(39.5334042639744,1.8364305250442,-136.679936254232));
#157801=CARTESIAN_POINT('Ctrl Pts',(39.5060076808651,1.839904013326,-136.612794432445));
#157802=CARTESIAN_POINT('Ctrl Pts',(39.4923093893105,1.8416407574669,-136.579223521551));
#157803=CARTESIAN_POINT('Ctrl Pts',(39.4786652963206,1.84340948973778,-136.544993284572));
#157804=CARTESIAN_POINT('Ctrl Pts',(39.4651044746358,1.84521014365973,-136.510099833943));
#157805=CARTESIAN_POINT('Ctrl Pts',(39.4583240637933,1.8461104706207,-136.492653108628));
#157806=CARTESIAN_POINT('Ctrl Pts',(39.4515644747565,1.84701877781338,-136.475040579033));
#157807=CARTESIAN_POINT('Ctrl Pts',(39.4448294099773,1.84793504887911,-136.457261889256));
#157808=CARTESIAN_POINT('Ctrl Pts',(39.4414618775878,1.84839318441198,-136.448372544368));
#157809=CARTESIAN_POINT('Ctrl Pts',(39.4381004763634,1.84885331090119,-136.439441659398));
#157810=CARTESIAN_POINT('Ctrl Pts',(39.4347456711397,1.84931542601312,-136.430469193862));
#157811=CARTESIAN_POINT('Ctrl Pts',(39.4330682685279,1.84954648356909,-136.425982961093));
#157812=CARTESIAN_POINT('Ctrl Pts',(39.4313925149198,1.84977803827995,-136.421486333182));
#157813=CARTESIAN_POINT('Ctrl Pts',(39.4297184686102,1.85001008982501,-136.41697930553));
#157814=CARTESIAN_POINT('Ctrl Pts',(39.4288814454554,1.85012611559753,-136.414725791704));
#157815=CARTESIAN_POINT('Ctrl Pts',(39.4280448491253,1.85024226557856,-136.412469677942));
#157816=CARTESIAN_POINT('Ctrl Pts',(39.4272086869189,1.85035853972607,-136.410210963702));
#157817=CARTESIAN_POINT('Ctrl Pts',(39.4263725247124,1.85047481387359,-136.407952249462));
#157818=CARTESIAN_POINT('Ctrl Pts',(39.424817695823,1.85069152670635,-136.403741922849));
#157819=CARTESIAN_POINT('Ctrl Pts',(39.4247015099726,1.8507077346254,-136.403427019011));
#157820=CARTESIAN_POINT('Ctrl Pts',(39.422629125099,1.85099683218914,-136.397810139249));
#157821=CARTESIAN_POINT('Ctrl Pts',(39.4190350978131,1.85149872607394,-136.388058312145));
#157822=CARTESIAN_POINT('Ctrl Pts',(39.4139781513362,1.85221396905478,-136.374151811247));
#157823=CARTESIAN_POINT('Ctrl Pts',(39.4089011553785,1.85293204778847,-136.360190174681));
#157824=CARTESIAN_POINT('Ctrl Pts',(39.4023496341151,1.85386517241038,-136.342040848675));
#157825=CARTESIAN_POINT('Ctrl Pts',(39.3944335185994,1.85501428022268,-136.319668562829));
#157826=CARTESIAN_POINT('Ctrl Pts',(39.3864697665656,1.85617030297894,-136.2971616481));
#157827=CARTESIAN_POINT('Ctrl Pts',(39.3771249826558,1.85754491903973,-136.270380783999));
#157828=CARTESIAN_POINT('Ctrl Pts',(39.3665617445024,1.85913943038351,-136.239274722874));
#157829=CARTESIAN_POINT('Ctrl Pts',(39.3565727512439,1.86064725997442,-136.209859667532));
#157830=CARTESIAN_POINT('Ctrl Pts',(39.3454941464808,1.86235181612195,-136.176575105897));
#157831=CARTESIAN_POINT('Ctrl Pts',(39.3335058501688,1.86425413539818,-136.139371406299));
#157832=CARTESIAN_POINT('Ctrl Pts',(39.3205136229093,1.86631575981201,-136.099052172649));
#157833=CARTESIAN_POINT('Ctrl Pts',(39.3064535772128,1.86860950825767,-136.054132995381));
#157834=CARTESIAN_POINT('Ctrl Pts',(39.2916080338993,1.87113616999862,-136.00455070594));
#157835=CARTESIAN_POINT('Ctrl Pts',(39.2764341215566,1.87371871904832,-135.953871704315));
#157836=CARTESIAN_POINT('Ctrl Pts',(39.2604385453299,1.8765448407645,-135.898316363799));
#157837=CARTESIAN_POINT('Ctrl Pts',(39.2439796575266,1.87961420051954,-135.837827876053));
#157838=CARTESIAN_POINT('Ctrl Pts',(39.2275207697233,1.88268356027457,-135.777339388308));
#157839=CARTESIAN_POINT('Ctrl Pts',(39.2105986989925,1.88599627399723,-135.711915499126));
#157840=CARTESIAN_POINT('Ctrl Pts',(39.1936207585355,1.88955053178332,-135.641515239685));
#157841=CARTESIAN_POINT('Ctrl Pts',(39.1927210714146,1.88973887735814,-135.637784621893));
#157842=CARTESIAN_POINT('Ctrl Pts',(39.1915408777627,1.88998700014396,-135.632869094502));
#157843=CARTESIAN_POINT('Ctrl Pts',(39.1909213209675,1.89011760234143,-135.630281476236));
#157844=CARTESIAN_POINT('Ctrl Pts',(39.1908306970963,1.89013670579862,-135.629902979888));
#157845=CARTESIAN_POINT('Ctrl Pts',(39.1907401153123,1.89015580793797,-135.629524521743));
#157846=CARTESIAN_POINT('Ctrl Pts',(39.1906495755884,1.89017490875729,-135.629146101804));
#157847=CARTESIAN_POINT('Ctrl Pts',(39.1688106141026,1.89478219094973,-135.537867952023));
#157848=CARTESIAN_POINT('Ctrl Pts',(39.1494516718396,1.89931800089657,-135.448695842305));
#157849=CARTESIAN_POINT('Ctrl Pts',(39.1322641903651,1.90374697366022,-135.361758548468));
#157850=CARTESIAN_POINT('Ctrl Pts',(39.1183456696376,1.90733358111656,-135.291356231057));
#157851=CARTESIAN_POINT('Ctrl Pts',(39.1058515634338,1.910850196318,-135.222418328487));
#157852=CARTESIAN_POINT('Ctrl Pts',(39.0946282203871,1.9142795706683,-135.154990566977));
#157853=CARTESIAN_POINT('Ctrl Pts',(39.0794701304433,1.9189112356398,-135.06392357656));
#157854=CARTESIAN_POINT('Ctrl Pts',(39.0666297867406,1.92338527749994,-134.975613379054));
#157855=CARTESIAN_POINT('Ctrl Pts',(39.0557624151109,1.92766357312286,-134.89020734062));
#157856=CARTESIAN_POINT('Ctrl Pts',(39.0486059555491,1.93048094706223,-134.833965143223));
#157857=CARTESIAN_POINT('Ctrl Pts',(39.0423054581754,1.93321351492931,-134.77898124839));
#157858=CARTESIAN_POINT('Ctrl Pts',(39.0367670376279,1.93585124621579,-134.725286427561));
#157859=CARTESIAN_POINT('Ctrl Pts',(39.0280343318381,1.94001028958918,-134.640623107267));
#157860=CARTESIAN_POINT('Ctrl Pts',(39.0211901513801,1.94394587338376,-134.55913268505));
#157861=CARTESIAN_POINT('Ctrl Pts',(39.015888450433,1.94769256523156,-134.480886044911));
#157862=CARTESIAN_POINT('Ctrl Pts',(39.0104340250084,1.95154718688547,-134.400385377742));
#157863=CARTESIAN_POINT('Ctrl Pts',(39.006612106687,1.95520190735825,-134.323317581055));
#157864=CARTESIAN_POINT('Ctrl Pts',(39.0040807323282,1.95869471836818,-134.249716322542));
#157865=CARTESIAN_POINT('Ctrl Pts',(39.0014556000694,1.96231689729392,-134.173388995717));
#157866=CARTESIAN_POINT('Ctrl Pts',(39.0002182001485,1.96576496763912,-134.100789292161));
#157867=CARTESIAN_POINT('Ctrl Pts',(39.000026518969,1.96908130239247,-134.031915960005));
#157868=CARTESIAN_POINT('Ctrl Pts',(39.000008754634,1.96938864858968,-134.025533022726));
#157869=CARTESIAN_POINT('Ctrl Pts',(39.,1.96969486323497,-134.019182067323));
#157870=CARTESIAN_POINT('Ctrl Pts',(39.,1.96999998000015,-134.012863078852));
#157871=CARTESIAN_POINT('Ctrl Pts',(39.,-3.68000001999999,-130.802732351058));
#157872=CARTESIAN_POINT('Ctrl Pts',(39.,-3.68320699217295,-130.887923832903));
#157873=CARTESIAN_POINT('Ctrl Pts',(39.0018493117517,-3.68659779226474,
-130.977410061787));
#157874=CARTESIAN_POINT('Ctrl Pts',(39.006160362258,-3.69017516856669,-131.071072933503));
#157875=CARTESIAN_POINT('Ctrl Pts',(39.009621104999,-3.69304694635053,-131.146261823757));
#157876=CARTESIAN_POINT('Ctrl Pts',(39.0146693161162,-3.6960389628621,-131.224142051601));
#157877=CARTESIAN_POINT('Ctrl Pts',(39.021645013605,-3.69915270994247,-131.304648061783));
#157878=CARTESIAN_POINT('Ctrl Pts',(39.0263019739025,-3.70123144064329,
-131.358393697072));
#157879=CARTESIAN_POINT('Ctrl Pts',(39.0318189308278,-3.70336458614086,
-131.413313609595));
#157880=CARTESIAN_POINT('Ctrl Pts',(39.0382997789448,-3.70555193766198,
-131.469370363117));
#157881=CARTESIAN_POINT('Ctrl Pts',(39.0486691056802,-3.70905168988551,
-131.559060907086));
#157882=CARTESIAN_POINT('Ctrl Pts',(39.0615053548553,-3.7126900014574,-131.651656352322));
#157883=CARTESIAN_POINT('Ctrl Pts',(39.0772366782264,-3.71646510502138,
-131.746979581721));
#157884=CARTESIAN_POINT('Ctrl Pts',(39.0925140114832,-3.72013126290684,
-131.839551878932));
#157885=CARTESIAN_POINT('Ctrl Pts',(39.1105225354627,-3.72392632174515,
-131.934693626701));
#157886=CARTESIAN_POINT('Ctrl Pts',(39.131639726789,-3.72784618719993,-132.032183000023));
#157887=CARTESIAN_POINT('Ctrl Pts',(39.1362592325343,-3.72870368006957,
-132.053509355086));
#157888=CARTESIAN_POINT('Ctrl Pts',(39.1410274043101,-3.72956713592367,
-132.074947836959));
#157889=CARTESIAN_POINT('Ctrl Pts',(39.1459480171903,-3.7304364973889,-132.096495803533));
#157890=CARTESIAN_POINT('Ctrl Pts',(39.1463940915734,-3.73051530868512,
-132.098449217901));
#157891=CARTESIAN_POINT('Ctrl Pts',(39.1471435285986,-3.73064731141171,
-132.101720321296));
#157892=CARTESIAN_POINT('Ctrl Pts',(39.1472900013385,-3.73067307710898,
-132.102358743601));
#157893=CARTESIAN_POINT('Ctrl Pts',(39.1473069993462,-3.73067606719111,
-132.10243283184));
#157894=CARTESIAN_POINT('Ctrl Pts',(39.1473240236054,-3.73067906164339,
-132.10250702793));
#157895=CARTESIAN_POINT('Ctrl Pts',(39.1473410741282,-3.73068206046583,
-132.102581331868));
#157896=CARTESIAN_POINT('Ctrl Pts',(39.1506177864137,-3.73125836410335,
-132.116860813524));
#157897=CARTESIAN_POINT('Ctrl Pts',(39.1548622386872,-3.73199618726408,
-132.135127161461));
#157898=CARTESIAN_POINT('Ctrl Pts',(39.1601911467889,-3.73289584576598,
-132.157352936904));
#157899=CARTESIAN_POINT('Ctrl Pts',(39.1655157741583,-3.73379478156875,
-132.179560858298));
#157900=CARTESIAN_POINT('Ctrl Pts',(39.1719231966379,-3.73485530708176,
-132.205722138333));
#157901=CARTESIAN_POINT('Ctrl Pts',(39.1795804315515,-3.73607783719616,
-132.235797617303));
#157902=CARTESIAN_POINT('Ctrl Pts',(39.1862116453768,-3.73713655600104,
-132.261843172155));
#157903=CARTESIAN_POINT('Ctrl Pts',(39.1937810024339,-3.73831678222952,
-132.290824222945));
#157904=CARTESIAN_POINT('Ctrl Pts',(39.2024269115509,-3.73961870163836,
-132.322705237269));
#157905=CARTESIAN_POINT('Ctrl Pts',(39.2123357614401,-3.74111079735848,
-132.359243232403));
#157906=CARTESIAN_POINT('Ctrl Pts',(39.2236573987929,-3.74276269105182,
-132.399589405842));
#157907=CARTESIAN_POINT('Ctrl Pts',(39.2366415304428,-3.74457397905163,
-132.443662692744));
#157908=CARTESIAN_POINT('Ctrl Pts',(39.2493021068547,-3.74634013105502,
-132.486637704982));
#157909=CARTESIAN_POINT('Ctrl Pts',(39.2635438263983,-3.74825787607168,
-132.533157316448));
#157910=CARTESIAN_POINT('Ctrl Pts',(39.2796379042396,-3.75032602419857,
-132.583117096287));
#157911=CARTESIAN_POINT('Ctrl Pts',(39.2888298631554,-3.75150722468746,
-132.611651085513));
#157912=CARTESIAN_POINT('Ctrl Pts',(39.2986267896565,-3.75273747274754,
-132.64130675528));
#157913=CARTESIAN_POINT('Ctrl Pts',(39.3090846344843,-3.7540163764884,-132.672059341533));
#157914=CARTESIAN_POINT('Ctrl Pts',(39.3124808338629,-3.75443170222344,
-132.682046285884));
#157915=CARTESIAN_POINT('Ctrl Pts',(39.3159467643173,-3.75485215835433,
-132.692148877582));
#157916=CARTESIAN_POINT('Ctrl Pts',(39.3194844958346,-3.75527819196887,
-132.702366145836));
#157917=CARTESIAN_POINT('Ctrl Pts',(39.3212533615932,-3.75549120877614,
-132.707474779963));
#157918=CARTESIAN_POINT('Ctrl Pts',(39.3230401941007,-3.75570572694133,
-132.712612077562));
#157919=CARTESIAN_POINT('Ctrl Pts',(39.3248451944342,-3.75592137730407,
-132.717777933179));
#157920=CARTESIAN_POINT('Ctrl Pts',(39.3266501947677,-3.75613702766681,
-132.722943788797));
#157921=CARTESIAN_POINT('Ctrl Pts',(39.3288894696748,-3.7564030433275,-132.72931830416));
#157922=CARTESIAN_POINT('Ctrl Pts',(39.3303149522011,-3.75657170342897,
-132.733361050105));
#157923=CARTESIAN_POINT('Ctrl Pts',(39.3540564862143,-3.75938075191748,
-132.800693331353));
#157924=CARTESIAN_POINT('Ctrl Pts',(39.3778323091587,-3.76204300277362,
-132.864162372071));
#157925=CARTESIAN_POINT('Ctrl Pts',(39.401268547416,-3.76455722155949,-132.923846293981));
#157926=CARTESIAN_POINT('Ctrl Pts',(39.4251684250805,-3.76712117916839,
-132.984710943696));
#157927=CARTESIAN_POINT('Ctrl Pts',(39.4487151410444,-3.76953121903715,
-133.041639875485));
#157928=CARTESIAN_POINT('Ctrl Pts',(39.4715634783474,-3.77178764461923,
-133.094737153497));
#157929=CARTESIAN_POINT('Ctrl Pts',(39.4949245826598,-3.77409470936084,
-133.149026051368));
#157930=CARTESIAN_POINT('Ctrl Pts',(39.517555574636,-3.77624121630412,-133.199310024175));
#157931=CARTESIAN_POINT('Ctrl Pts',(39.5391409289902,-3.77822871249156,
-133.245712369463));
#157932=CARTESIAN_POINT('Ctrl Pts',(39.5552925697658,-3.7797158932872,-133.280433782879));
#157933=CARTESIAN_POINT('Ctrl Pts',(39.5708598736309,-3.78111407042952,
-133.312982141961));
#157934=CARTESIAN_POINT('Ctrl Pts',(39.5857296458368,-3.78242418360352,
-133.343410256559));
#157935=CARTESIAN_POINT('Origin',(0.,-12.9675000200281,-171.64995));
#157936=CARTESIAN_POINT('',(57.6746235421417,-3.75150367745622,-171.449026400902));
#157937=CARTESIAN_POINT('',(56.4941621559325,1.85499746228791,-171.449026400902));
#157938=CARTESIAN_POINT('Origin',(0.,-12.9675000200281,-171.449026400902));
#157939=CARTESIAN_POINT('Ctrl Pts',(56.4941621559325,1.85499746228791,-171.449026400902));
#157940=CARTESIAN_POINT('Ctrl Pts',(55.5872148662684,1.85328258784851,-169.566813619198));
#157941=CARTESIAN_POINT('Ctrl Pts',(54.6987069265873,1.85157789414912,-167.72566026361));
#157942=CARTESIAN_POINT('Ctrl Pts',(53.8286007394999,1.84982266457049,-165.9255866409));
#157943=CARTESIAN_POINT('Ctrl Pts',(53.2735091105652,1.84870290095956,-164.777214391328));
#157944=CARTESIAN_POINT('Ctrl Pts',(52.7259078414064,1.84756262081415,-163.645560727361));
#157945=CARTESIAN_POINT('Ctrl Pts',(52.1857969712753,1.8463865543554,-162.53062597535));
#157946=CARTESIAN_POINT('Ctrl Pts',(51.492429613171,1.84487677897675,-161.099328428474));
#157947=CARTESIAN_POINT('Ctrl Pts',(50.8114042047774,1.84331606104898,-159.69558475759));
#157948=CARTESIAN_POINT('Ctrl Pts',(50.1427245048726,1.84172122826594,-158.319391243539));
#157949=CARTESIAN_POINT('Ctrl Pts',(49.8083846549203,1.84092381187443,-157.631294486514));
#157950=CARTESIAN_POINT('Ctrl Pts',(49.4771313616882,1.84011838355358,-156.950085170635));
#157951=CARTESIAN_POINT('Ctrl Pts',(49.1489657089356,1.83931015210421,-156.27576229937));
#157952=CARTESIAN_POINT('Ctrl Pts',(48.9848828825593,1.83890603637952,-155.938600863737));
#157953=CARTESIAN_POINT('Ctrl Pts',(48.8215719791454,1.83850122447541,-155.60316103291));
#157954=CARTESIAN_POINT('Ctrl Pts',(48.6590331509111,1.83809659258963,-155.269442654971));
#157955=CARTESIAN_POINT('Ctrl Pts',(48.5777637367939,1.83789427664674,-155.102583466001));
#157956=CARTESIAN_POINT('Ctrl Pts',(48.4966873421834,1.83769200598395,-154.936154639899));
#157957=CARTESIAN_POINT('Ctrl Pts',(48.4158039886763,1.83748989727043,-154.770156155779));
#157958=CARTESIAN_POINT('Ctrl Pts',(48.3753623119227,1.83738884291367,-154.687156913718));
#157959=CARTESIAN_POINT('Ctrl Pts',(48.3349688954873,1.83728782906129,-154.604265257132));
#157960=CARTESIAN_POINT('Ctrl Pts',(48.2946237421284,1.837186871069,-154.521481183311));
#157961=CARTESIAN_POINT('Ctrl Pts',(48.2593217329394,1.83709853282574,-154.449045118718));
#157962=CARTESIAN_POINT('Ctrl Pts',(48.224056675171,1.8370102373514,-154.376691422179));
#157963=CARTESIAN_POINT('Ctrl Pts',(48.1888285707055,1.83692199521058,-154.304420091836));
#157964=CARTESIAN_POINT('Ctrl Pts',(48.1837959843533,1.83690938919046,-154.294095616072));
#157965=CARTESIAN_POINT('Ctrl Pts',(48.1796675061752,1.83689904733514,-154.285626026406));
#157966=CARTESIAN_POINT('Ctrl Pts',(48.1737330726839,1.83688418615863,-154.273451708059));
#157967=CARTESIAN_POINT('Ctrl Pts',(48.1736305779674,1.83688392948846,-154.273241443119));
#157968=CARTESIAN_POINT('Ctrl Pts',(48.1735280835149,1.83688367281755,-154.273031178774));
#157969=CARTESIAN_POINT('Ctrl Pts',(48.1734255893264,1.83688341614592,-154.272820915026));
#157970=CARTESIAN_POINT('Ctrl Pts',(47.4138476394261,1.83498123889893,-152.714569574048));
#157971=CARTESIAN_POINT('Ctrl Pts',(46.6687914400752,1.83303990966285,-151.189068021751));
#157972=CARTESIAN_POINT('Ctrl Pts',(45.938183755171,1.83105643289783,-149.696350512763));
#157973=CARTESIAN_POINT('Ctrl Pts',(45.1949410991184,1.82903865431501,-148.177818270302));
#157974=CARTESIAN_POINT('Ctrl Pts',(44.4666512921154,1.82697727414329,-146.693213656769));
#157975=CARTESIAN_POINT('Ctrl Pts',(43.7532878193704,1.82487206350732,-145.24254696461));
#157976=CARTESIAN_POINT('Ctrl Pts',(43.0079230141743,1.82267241357356,-143.726803675645));
#157977=CARTESIAN_POINT('Ctrl Pts',(42.278853870262,1.82042491917042,-142.248111447343));
#157978=CARTESIAN_POINT('Ctrl Pts',(41.5661022554074,1.81813232414976,-140.806455468107));
#157979=CARTESIAN_POINT('Ctrl Pts',(40.9493421409949,1.81614848975672,-139.558957899297));
#157980=CARTESIAN_POINT('Ctrl Pts',(40.3448013391909,1.81413094379836,-138.339191935329));
#157981=CARTESIAN_POINT('Ctrl Pts',(39.7525219240432,1.81208306781681,-137.147133758372));
#157982=CARTESIAN_POINT('Ctrl Pts',(39.5857308656309,-3.78242429107441,
-133.34341275263));
#157983=CARTESIAN_POINT('Ctrl Pts',(40.9519549067385,-3.77910503324588,
-136.199077491809));
#157984=CARTESIAN_POINT('Ctrl Pts',(42.3907152118192,-3.77572283235729,
-139.21370723183));
#157985=CARTESIAN_POINT('Ctrl Pts',(44.6577376745155,-3.77119731722451,
-143.974099343123));
#157986=CARTESIAN_POINT('Ctrl Pts',(45.4315569217728,-3.76976624204378,
-145.600637963764));
#157987=CARTESIAN_POINT('Ctrl Pts',(46.6194990079656,-3.76769078813001,
-148.100057770041));
#157988=CARTESIAN_POINT('Ctrl Pts',(47.2202732321399,-3.76666954253768,
-149.364670642009));
#157989=CARTESIAN_POINT('Ctrl Pts',(47.933079937314,-3.76548325423015,-150.866132521422));
#157990=CARTESIAN_POINT('Ctrl Pts',(48.2924588112532,-3.76488740822001,
-151.623383509991));
#157991=CARTESIAN_POINT('Ctrl Pts',(48.4954462437539,-3.76455089104309,
-152.051170954804));
#157992=CARTESIAN_POINT('Ctrl Pts',(48.5955948730132,-3.76438477362141,
-152.262252292382));
#157993=CARTESIAN_POINT('Ctrl Pts',(48.6473508980734,-3.76429887944539,
-152.37134303568));
#157994=CARTESIAN_POINT('Ctrl Pts',(48.651123012323,-3.76429261899403,-152.379293884756));
#157995=CARTESIAN_POINT('Ctrl Pts',(51.416797493966,-3.75970237622441,-158.208789756719));
#157996=CARTESIAN_POINT('Ctrl Pts',(54.4237264557334,-3.75540420604071,
-164.563471491086));
#157997=CARTESIAN_POINT('Ctrl Pts',(57.6746235421417,-3.75150367745622,
-171.449026400902));
#157998=CARTESIAN_POINT('Ctrl Pts',(60.,-4.67636962353871,-174.488179236421));
#157999=CARTESIAN_POINT('Ctrl Pts',(60.,-4.58657792455374,-176.471369022159));
#158000=CARTESIAN_POINT('Ctrl Pts',(58.1727505513102,-4.55147683639116,
-177.246631327017));
#158001=CARTESIAN_POINT('Ctrl Pts',(60.,-4.88047860745801,-174.497420557097));
#158002=CARTESIAN_POINT('Ctrl Pts',(60.0000000000001,-4.78987454640719,
-176.45995577904));
#158003=CARTESIAN_POINT('Ctrl Pts',(58.1991963791505,-4.75453073304092,
-177.244581482931));
#158004=CARTESIAN_POINT('Ctrl Pts',(60.,-5.08458311893969,-174.506824441727));
#158005=CARTESIAN_POINT('Ctrl Pts',(59.9999999999904,-4.99421808034747,
-176.449490545983));
#158006=CARTESIAN_POINT('Ctrl Pts',(58.2246968063274,-4.95813196877381,
-177.242671121044));
#158007=CARTESIAN_POINT('Ctrl Pts',(60.,-5.28868572332295,-174.51629758862));
#158008=CARTESIAN_POINT('Ctrl Pts',(60.,-5.19940519654632,-176.439881014021));
#158009=CARTESIAN_POINT('Ctrl Pts',(58.2492435654384,-5.16222748868145,
-177.240889086276));
#158010=CARTESIAN_POINT('',(60.,-5.18000001999999,-174.511260182693));
#158011=CARTESIAN_POINT('',(58.2670184333942,-5.15898900219891,-177.232516794804));
#158012=CARTESIAN_POINT('Ctrl Pts',(60.,-5.18000001999999,-174.511260182693));
#158013=CARTESIAN_POINT('Ctrl Pts',(60.,-5.1799272377721,-174.520713255673));
#158014=CARTESIAN_POINT('Ctrl Pts',(59.9999613146273,-5.17983454997278,
-174.533245214993));
#158015=CARTESIAN_POINT('Ctrl Pts',(59.9997683044872,-5.17971977325836,
-174.548915860866));
#158016=CARTESIAN_POINT('Ctrl Pts',(59.9995874353749,-5.17961221640953,
-174.563600767101));
#158017=CARTESIAN_POINT('Ctrl Pts',(59.9992707239901,-5.17948526269027,
-174.581041858777));
#158018=CARTESIAN_POINT('Ctrl Pts',(59.99867265545,-5.17933717776086,-174.6012798489));
#158019=CARTESIAN_POINT('Ctrl Pts',(59.99808144442,-5.17919079078715,-174.621285788327));
#158020=CARTESIAN_POINT('Ctrl Pts',(59.9972154017306,-5.1790237543439,-174.644024877617));
#158021=CARTESIAN_POINT('Ctrl Pts',(59.9958839884361,-5.17883445369421,
-174.669527960362));
#158022=CARTESIAN_POINT('Ctrl Pts',(59.9945723442879,-5.17864796382631,
-174.69465236717));
#158023=CARTESIAN_POINT('Ctrl Pts',(59.9928091104631,-5.17843986597539,
-174.722459311834));
#158024=CARTESIAN_POINT('Ctrl Pts',(59.9903620933743,-5.17820867615274,
-174.752969724891));
#158025=CARTESIAN_POINT('Ctrl Pts',(59.9897615851697,-5.17815194120554,
-174.760457107571));
#158026=CARTESIAN_POINT('Ctrl Pts',(59.9891196557456,-5.17809381587359,
-174.768107260234));
#158027=CARTESIAN_POINT('Ctrl Pts',(59.988432396927,-5.17803427879222,-174.775920410068));
#158028=CARTESIAN_POINT('Ctrl Pts',(59.9856554152033,-5.17779370947197,
-174.807490720562));
#158029=CARTESIAN_POINT('Ctrl Pts',(59.9821408038309,-5.17752962562884,
-174.841740394733));
#158030=CARTESIAN_POINT('Ctrl Pts',(59.9775984010229,-5.17724229616848,
-174.878666355715));
#158031=CARTESIAN_POINT('Ctrl Pts',(59.9730975147709,-5.17695759283578,
-174.915254821588));
#158032=CARTESIAN_POINT('Ctrl Pts',(59.9675875782563,-5.17665006670961,
-174.954470891117));
#158033=CARTESIAN_POINT('Ctrl Pts',(59.9607357962623,-5.17632004513401,
-174.996302707221));
#158034=CARTESIAN_POINT('Ctrl Pts',(59.9592196006012,-5.17624701635385,
-175.005559455047));
#158035=CARTESIAN_POINT('Ctrl Pts',(59.9576374998204,-5.17617288630168,
-175.014944252933));
#158036=CARTESIAN_POINT('Ctrl Pts',(59.9559855465045,-5.17609765897697,
-175.024456911882));
#158037=CARTESIAN_POINT('Ctrl Pts',(59.9481389578712,-5.17574033781949,
-175.069640949992));
#158038=CARTESIAN_POINT('Ctrl Pts',(59.9387215277951,-5.17535866288732,
-175.117704292394));
#158039=CARTESIAN_POINT('Ctrl Pts',(59.9272892750181,-5.17495659188962,
-175.168559246422));
#158040=CARTESIAN_POINT('Ctrl Pts',(59.9265912438941,-5.17493204221635,
-175.171664351024));
#158041=CARTESIAN_POINT('Ctrl Pts',(59.9258856855017,-5.17490741653123,
-175.174779860105));
#158042=CARTESIAN_POINT('Ctrl Pts',(59.9251724926247,-5.17488271574553,
-175.177905752576));
#158043=CARTESIAN_POINT('Ctrl Pts',(59.9189756112986,-5.17466809240504,
-175.205066406175));
#158044=CARTESIAN_POINT('Ctrl Pts',(59.9122028334488,-5.17444785344947,
-175.233010001163));
#158045=CARTESIAN_POINT('Ctrl Pts',(59.904783763042,-5.1742229673739,-175.261715234116));
#158046=CARTESIAN_POINT('Ctrl Pts',(59.9010742278385,-5.17411052433611,
-175.276067850593));
#158047=CARTESIAN_POINT('Ctrl Pts',(59.8972030676678,-5.17399691988581,
-175.290610868415));
#158048=CARTESIAN_POINT('Ctrl Pts',(59.8931613792453,-5.17388230573763,
-175.305340960976));
#158049=CARTESIAN_POINT('Ctrl Pts',(59.891140535034,-5.17382499866353,-175.312706007257));
#158050=CARTESIAN_POINT('Ctrl Pts',(59.889077056277,-5.17376743915838,-175.320117822345));
#158051=CARTESIAN_POINT('Ctrl Pts',(59.8869698226738,-5.17370964723968,
-175.327575967589));
#158052=CARTESIAN_POINT('Ctrl Pts',(59.8859162058722,-5.17368075128032,
-175.331305040212));
#158053=CARTESIAN_POINT('Ctrl Pts',(59.8848516502199,-5.17365179721695,
-175.335045695386));
#158054=CARTESIAN_POINT('Ctrl Pts',(59.8837760155946,-5.17362278766247,
-175.338797875885));
#158055=CARTESIAN_POINT('Ctrl Pts',(59.8827003809693,-5.17359377810799,
-175.342550056383));
#158056=CARTESIAN_POINT('Ctrl Pts',(59.8812553100241,-5.17355521136971,
-175.347545951429));
#158057=CARTESIAN_POINT('Ctrl Pts',(59.8805157344353,-5.17353559732074,
-175.350088935428));
#158058=CARTESIAN_POINT('Ctrl Pts',(59.8800176333053,-5.17352238733908,
-175.351801624737));
#158059=CARTESIAN_POINT('Ctrl Pts',(59.8795184251299,-5.17350919095032,
-175.353512540531));
#158060=CARTESIAN_POINT('Ctrl Pts',(59.8790181177072,-5.17349600812921,
-175.355221686178));
#158061=CARTESIAN_POINT('Ctrl Pts',(59.8654362414286,-5.17313813327622,
-175.401619967842));
#158062=CARTESIAN_POINT('Ctrl Pts',(59.8509971474762,-5.17279016162673,
-175.446725987013));
#158063=CARTESIAN_POINT('Ctrl Pts',(59.8359110132716,-5.17245277034999,
-175.490454018024));
#158064=CARTESIAN_POINT('Ctrl Pts',(59.8203336981495,-5.17210439414134,
-175.535605765283));
#158065=CARTESIAN_POINT('Ctrl Pts',(59.8040664089156,-5.17176729583692,
-175.579288675368));
#158066=CARTESIAN_POINT('Ctrl Pts',(59.7873050482715,-5.17144188203371,
-175.621452071484));
#158067=CARTESIAN_POINT('Ctrl Pts',(59.7697421073717,-5.17110090593307,
-175.665631851983));
#158068=CARTESIAN_POINT('Ctrl Pts',(59.7516366599007,-5.17077275638255,
-175.70814359908));
#158069=CARTESIAN_POINT('Ctrl Pts',(59.7331769155636,-5.1704575724523,-175.748971379014));
#158070=CARTESIAN_POINT('Ctrl Pts',(59.7318411535293,-5.17043476548812,
-175.7519257102));
#158071=CARTESIAN_POINT('Ctrl Pts',(59.7305035211752,-5.1704120262858,-175.754871240386));
#158072=CARTESIAN_POINT('Ctrl Pts',(59.7291640828256,-5.17038935484021,
-175.757807970983));
#158073=CARTESIAN_POINT('Ctrl Pts',(59.7245308271502,-5.17031093196695,
-175.767966425615));
#158074=CARTESIAN_POINT('Ctrl Pts',(59.7198743116007,-5.17023326574134,
-175.778026603707));
#158075=CARTESIAN_POINT('Ctrl Pts',(59.7151963681919,-5.17015634142143,
-175.787990446344));
#158076=CARTESIAN_POINT('Ctrl Pts',(59.6859083951819,-5.16967472862527,
-175.850372721789));
#158077=CARTESIAN_POINT('Ctrl Pts',(59.6559202772399,-5.16922449040161,
-175.908679583196));
#158078=CARTESIAN_POINT('Ctrl Pts',(59.6259391187632,-5.16880507771954,
-175.962986478089));
#158079=CARTESIAN_POINT('Ctrl Pts',(59.6006389687672,-5.16845114864189,
-176.008814346537));
#158080=CARTESIAN_POINT('Ctrl Pts',(59.5753448613497,-5.16811915863265,
-176.051795357692));
#158081=CARTESIAN_POINT('Ctrl Pts',(59.5504391432744,-5.16780833955879,
-176.092031152333));
#158082=CARTESIAN_POINT('Ctrl Pts',(59.5458311121938,-5.16775083212421,
-176.099475538867));
#158083=CARTESIAN_POINT('Ctrl Pts',(59.5412362469768,-5.16769404861673,
-176.106826053089));
#158084=CARTESIAN_POINT('Ctrl Pts',(59.5366567934599,-5.16763798325383,
-176.11408345595));
#158085=CARTESIAN_POINT('Ctrl Pts',(59.5348607551479,-5.16761599470447,
-176.116929772335));
#158086=CARTESIAN_POINT('Ctrl Pts',(59.5337373392218,-5.16760226626031,
-176.118706848888));
#158087=CARTESIAN_POINT('Ctrl Pts',(59.5313782454486,-5.16757359498196,
-176.122418507681));
#158088=CARTESIAN_POINT('Ctrl Pts',(59.5312518004227,-5.16757205823061,
-176.122617448815));
#158089=CARTESIAN_POINT('Ctrl Pts',(59.5311217942244,-5.16757047859849,
-176.122821941482));
#158090=CARTESIAN_POINT('Ctrl Pts',(59.5309879284935,-5.16756885253193,
-176.123032445711));
#158091=CARTESIAN_POINT('Ctrl Pts',(59.5290762516248,-5.16754563139973,
-176.126038562844));
#158092=CARTESIAN_POINT('Ctrl Pts',(59.5271600421084,-5.16752244583908,
-176.12904004279));
#158093=CARTESIAN_POINT('Ctrl Pts',(59.5252393170933,-5.16749929577026,
-176.132036896267));
#158094=CARTESIAN_POINT('Ctrl Pts',(59.4885613142581,-5.16705722400919,
-176.189264557424));
#158095=CARTESIAN_POINT('Ctrl Pts',(59.4500653841475,-5.16662664608057,
-176.244992491202));
#158096=CARTESIAN_POINT('Ctrl Pts',(59.4101077057974,-5.16620977760933,
-176.298936679342));
#158097=CARTESIAN_POINT('Ctrl Pts',(59.3694359516207,-5.16578545936345,
-176.353844893479));
#158098=CARTESIAN_POINT('Ctrl Pts',(59.3272496939177,-5.16537534434658,
-176.4069051164));
#158099=CARTESIAN_POINT('Ctrl Pts',(59.2838905709168,-5.16498144614305,
-176.457859440189));
#158100=CARTESIAN_POINT('Ctrl Pts',(59.2787049812111,-5.1649343373842,-176.463953387636));
#158101=CARTESIAN_POINT('Ctrl Pts',(59.2735025769242,-5.16488746021233,
-176.470017261057));
#158102=CARTESIAN_POINT('Ctrl Pts',(59.2682839111567,-5.16484081777635,
-176.476050657348));
#158103=CARTESIAN_POINT('Ctrl Pts',(59.198184488061,-5.16421429597941,-176.557093900619));
#158104=CARTESIAN_POINT('Ctrl Pts',(59.1254281377786,-5.16363128018837,
-176.63248959021));
#158105=CARTESIAN_POINT('Ctrl Pts',(59.0504291615598,-5.16308787519053,
-176.702751972211));
#158106=CARTESIAN_POINT('Ctrl Pts',(59.0228175280704,-5.16288781513113,
-176.728619780516));
#158107=CARTESIAN_POINT('Ctrl Pts',(58.994901582676,-5.16269312687973,-176.753791426191));
#158108=CARTESIAN_POINT('Ctrl Pts',(58.966700826357,-5.16250362596014,-176.778291252628));
#158109=CARTESIAN_POINT('Ctrl Pts',(58.9580740402192,-5.16244565645437,
-176.785785901378));
#158110=CARTESIAN_POINT('Ctrl Pts',(58.9494150826379,-5.16238815490271,
-176.79321994001));
#158111=CARTESIAN_POINT('Ctrl Pts',(58.9407254879922,-5.16233112230567,
-176.800593251677));
#158112=CARTESIAN_POINT('Ctrl Pts',(58.8901282302924,-5.16199903627317,
-176.843526134708));
#158113=CARTESIAN_POINT('Ctrl Pts',(58.8387753737899,-5.16168474946931,
-176.884162608041));
#158114=CARTESIAN_POINT('Ctrl Pts',(58.7869638405979,-5.1613877473488,-176.922564128275));
#158115=CARTESIAN_POINT('Ctrl Pts',(58.7327825694257,-5.16107716104806,
-176.962722043955));
#158116=CARTESIAN_POINT('Ctrl Pts',(58.6780996195717,-5.1607854754869,-177.000436045426));
#158117=CARTESIAN_POINT('Ctrl Pts',(58.6231983985429,-5.16051201831244,
-177.035786965185));
#158118=CARTESIAN_POINT('Ctrl Pts',(58.5639650113499,-5.16021698307657,
-177.073927368595));
#158119=CARTESIAN_POINT('Ctrl Pts',(58.5044777230962,-5.15994316516394,
-177.109317211894));
#158120=CARTESIAN_POINT('Ctrl Pts',(58.4450274076812,-5.15968964438824,
-177.142067473344));
#158121=CARTESIAN_POINT('Ctrl Pts',(58.3855770922661,-5.15943612361254,
-177.174817734794));
#158122=CARTESIAN_POINT('Ctrl Pts',(58.3261631370263,-5.15920289782321,
-177.204928688562));
#158123=CARTESIAN_POINT('Ctrl Pts',(58.2670184333942,-5.15898900219891,
-177.232516794804));
#158124=CARTESIAN_POINT('',(58.2078173715129,-4.65917712431111,-177.236349007278));
#158125=CARTESIAN_POINT('Origin',(-8.73110974027571,-12.9198662892988,-187.475563684127));
#158126=CARTESIAN_POINT('',(60.,-4.68000001999999,-174.488343624884));
#158127=CARTESIAN_POINT('Ctrl Pts',(58.2078173713336,-4.65917712527795,
-177.236349006383));
#158128=CARTESIAN_POINT('Ctrl Pts',(58.2680396583105,-4.65937904897621,
-177.209843370633));
#158129=CARTESIAN_POINT('Ctrl Pts',(58.3286061602997,-4.6595903192446,-177.180819390645));
#158130=CARTESIAN_POINT('Ctrl Pts',(58.389247772245,-4.65981829367543,-177.149112865983));
#158131=CARTESIAN_POINT('Ctrl Pts',(58.4488949403758,-4.66004252962116,
-177.117926287218));
#158132=CARTESIAN_POINT('Ctrl Pts',(58.5086145427696,-4.66028295223093,
-177.084143855486));
#158133=CARTESIAN_POINT('Ctrl Pts',(58.5681109624229,-4.66054518977293,
-177.047638867556));
#158134=CARTESIAN_POINT('Ctrl Pts',(58.6261911081638,-4.6608011849193,-177.01200285733));
#158135=CARTESIAN_POINT('Ctrl Pts',(58.6840581776048,-4.66107798952929,
-176.973771908009));
#158136=CARTESIAN_POINT('Ctrl Pts',(58.7414038465745,-4.66137918120361,
-176.932863994594));
#158137=CARTESIAN_POINT('Ctrl Pts',(58.7956818748661,-4.66166426097535,
-176.89414440301));
#158138=CARTESIAN_POINT('Ctrl Pts',(58.8494922433316,-4.66197119389585,
-176.853026464809));
#158139=CARTESIAN_POINT('Ctrl Pts',(58.9025503147113,-4.66230134010155,
-176.809476916618));
#158140=CARTESIAN_POINT('Ctrl Pts',(58.9569411261647,-4.66263977909037,
-176.764833468356));
#158141=CARTESIAN_POINT('Ctrl Pts',(59.0105409839596,-4.66300263959302,
-176.717634115967));
#158142=CARTESIAN_POINT('Ctrl Pts',(59.0630247791536,-4.66338930132797,
-176.667888366361));
#158143=CARTESIAN_POINT('Ctrl Pts',(59.114910853718,-4.66377155949998,-176.618709154687));
#158144=CARTESIAN_POINT('Ctrl Pts',(59.1657055368162,-4.66417709024071,
-176.567040982309));
#158145=CARTESIAN_POINT('Ctrl Pts',(59.2150845173184,-4.66460301486336,
-176.512942701094));
#158146=CARTESIAN_POINT('Ctrl Pts',(59.2637965700052,-4.66502318681605,
-176.459575088032));
#158147=CARTESIAN_POINT('Ctrl Pts',(59.3111302557302,-4.66546320851134,
-176.40384249302));
#158148=CARTESIAN_POINT('Ctrl Pts',(59.356773551464,-4.66591798745967,-176.345852268448));
#158149=CARTESIAN_POINT('Ctrl Pts',(59.3632118699717,-4.66598213733476,
-176.337672325915));
#158150=CARTESIAN_POINT('Ctrl Pts',(59.3696165628679,-4.6660465769791,-176.329447547331));
#158151=CARTESIAN_POINT('Ctrl Pts',(59.3759867651245,-4.6661112882857,-176.321178317415));
#158152=CARTESIAN_POINT('Ctrl Pts',(59.3999226589537,-4.66635443958636,
-176.290106869232));
#158153=CARTESIAN_POINT('Ctrl Pts',(59.4233715104119,-4.66660144104085,
-176.258407507797));
#158154=CARTESIAN_POINT('Ctrl Pts',(59.4462880189083,-4.66685121140858,
-176.226103284235));
#158155=CARTESIAN_POINT('Ctrl Pts',(59.4577462731564,-4.66697609659244,
-176.209951172454));
#158156=CARTESIAN_POINT('Ctrl Pts',(59.4690714829495,-4.66710167269257,
-176.193647874009));
#158157=CARTESIAN_POINT('Ctrl Pts',(59.4802580714741,-4.6672277849629,-176.177196699382));
#158158=CARTESIAN_POINT('Ctrl Pts',(59.4858513657365,-4.66729084109807,
-176.168971112068));
#158159=CARTESIAN_POINT('Ctrl Pts',(59.4914100075004,-4.66735403118273,
-176.160708557756));
#158160=CARTESIAN_POINT('Ctrl Pts',(59.496933313017,-4.66741733507178,-176.152409467875));
#158161=CARTESIAN_POINT('Ctrl Pts',(59.4996949657753,-4.66744898701631,
-176.148259922935));
#158162=CARTESIAN_POINT('Ctrl Pts',(59.5024477846533,-4.66748066740648,
-176.144101244222));
#158163=CARTESIAN_POINT('Ctrl Pts',(59.5051916847113,-4.66751237365184,
-176.139933487251));
#158164=CARTESIAN_POINT('Ctrl Pts',(59.5076606481011,-4.66754090295588,
-176.136183336312));
#158165=CARTESIAN_POINT('Ctrl Pts',(59.5107552332661,-4.66757679218943,
-176.131455884057));
#158166=CARTESIAN_POINT('Ctrl Pts',(59.5127669604926,-4.66760023191263,
-176.128369384483));
#158167=CARTESIAN_POINT('Ctrl Pts',(59.5129909806557,-4.66760284209285,
-176.128025680759));
#158168=CARTESIAN_POINT('Ctrl Pts',(59.5132016187169,-4.66760529661482,
-176.127702354121));
#158169=CARTESIAN_POINT('Ctrl Pts',(59.5133965440667,-4.66760756732954,
-176.127403037814));
#158170=CARTESIAN_POINT('Ctrl Pts',(59.5371312287591,-4.6678840562422,-176.09095740269));
#158171=CARTESIAN_POINT('Ctrl Pts',(59.5613327018925,-4.66817509409086,
-176.052066438838));
#158172=CARTESIAN_POINT('Ctrl Pts',(59.5856916606812,-4.66848486559977,
-176.010634488638));
#158173=CARTESIAN_POINT('Ctrl Pts',(59.6095513371242,-4.66878828776317,
-175.970051763623));
#158174=CARTESIAN_POINT('Ctrl Pts',(59.6335618236263,-4.66910971421667,
-175.927030471272));
#158175=CARTESIAN_POINT('Ctrl Pts',(59.6573936723734,-4.66945172336169,
-175.881509967927));
#158176=CARTESIAN_POINT('Ctrl Pts',(59.6811736782573,-4.66979298851353,
-175.836088488089));
#158177=CARTESIAN_POINT('Ctrl Pts',(59.7047754709015,-4.67015478183408,
-175.788177887775));
#158178=CARTESIAN_POINT('Ctrl Pts',(59.7278372729539,-4.67053780712503,
-175.737758277064));
#158179=CARTESIAN_POINT('Ctrl Pts',(59.7508990750064,-4.67092083241598,
-175.687338666353));
#158180=CARTESIAN_POINT('Ctrl Pts',(59.773420321916,-4.67132512407299,-175.634409283462));
#158181=CARTESIAN_POINT('Ctrl Pts',(59.7950115476719,-4.6717490027353,-175.57900221117));
#158182=CARTESIAN_POINT('Ctrl Pts',(59.8094968549156,-4.67203337809809,
-175.541830237949));
#158183=CARTESIAN_POINT('Ctrl Pts',(59.8235629763428,-4.6723265191891,-175.503544172828));
#158184=CARTESIAN_POINT('Ctrl Pts',(59.8370875679768,-4.67262720060425,
-175.464169412071));
#158185=CARTESIAN_POINT('Ctrl Pts',(59.8438498637937,-4.67277754131183,
-175.444482031693));
#158186=CARTESIAN_POINT('Ctrl Pts',(59.8504767991258,-4.67292976676747,
-175.424522484744));
#158187=CARTESIAN_POINT('Ctrl Pts',(59.856952806083,-4.67308365370076,-175.404295481212));
#158188=CARTESIAN_POINT('Ctrl Pts',(59.8601908095616,-4.6731605971674,-175.394181979446));
#158189=CARTESIAN_POINT('Ctrl Pts',(59.863391084221,-4.67323795595347,-175.384001614636));
#158190=CARTESIAN_POINT('Ctrl Pts',(59.8665516908483,-4.67331569985915,
-175.37375502587));
#158191=CARTESIAN_POINT('Ctrl Pts',(59.868131994162,-4.67335457181198,-175.368631731487));
#158192=CARTESIAN_POINT('Ctrl Pts',(59.8697023806881,-4.67339354004155,
-175.363491881185));
#158193=CARTESIAN_POINT('Ctrl Pts',(59.8712626078616,-4.67343260052121,
-175.35833556037));
#158194=CARTESIAN_POINT('Ctrl Pts',(59.8720427214483,-4.67345213076104,
-175.355757399962));
#158195=CARTESIAN_POINT('Ctrl Pts',(59.8728202952122,-4.67347168406318,
-175.353175121931));
#158196=CARTESIAN_POINT('Ctrl Pts',(59.8735952988247,-4.67349125990757,
-175.350588737318));
#158197=CARTESIAN_POINT('Ctrl Pts',(59.8743703024372,-4.67351083575196,
-175.348002352706));
#158198=CARTESIAN_POINT('Ctrl Pts',(59.8747992527727,-4.67352167993367,
-175.346569510899));
#158199=CARTESIAN_POINT('Ctrl Pts',(59.8759125689141,-4.67355005454189,
-175.342817274903));
#158200=CARTESIAN_POINT('Ctrl Pts',(59.8902666875517,-4.67391589177132,
-175.294439245841));
#158201=CARTESIAN_POINT('Ctrl Pts',(59.9027576717863,-4.67427372815143,
-175.247880000389));
#158202=CARTESIAN_POINT('Ctrl Pts',(59.9136927181814,-4.67461859932685,
-175.203252216413));
#158203=CARTESIAN_POINT('Ctrl Pts',(59.9249587511274,-4.67497390920703,
-175.157273620035));
#158204=CARTESIAN_POINT('Ctrl Pts',(59.9345737413699,-4.6753154806694,-175.113344667922));
#158205=CARTESIAN_POINT('Ctrl Pts',(59.9428469848154,-4.67564005948804,
-175.071540483632));
#158206=CARTESIAN_POINT('Ctrl Pts',(59.9514972186274,-4.67597942852633,
-175.02783139048));
#158207=CARTESIAN_POINT('Ctrl Pts',(59.9586811510616,-4.67630024501819,
-174.986444595862));
#158208=CARTESIAN_POINT('Ctrl Pts',(59.9647154213307,-4.67660076426343,
-174.947422139622));
#158209=CARTESIAN_POINT('Ctrl Pts',(59.970910334806,-4.67690928387539,-174.907360834903));
#158210=CARTESIAN_POINT('Ctrl Pts',(59.9758938379629,-4.67719644344746,
-174.86979072386));
#158211=CARTESIAN_POINT('Ctrl Pts',(59.9799644784539,-4.67746194092389,
-174.834721935552));
#158212=CARTESIAN_POINT('Ctrl Pts',(59.9841355348749,-4.67773398778144,
-174.798788058567));
#158213=CARTESIAN_POINT('Ctrl Pts',(59.9873482802513,-4.67798332297327,
-174.765479724316));
#158214=CARTESIAN_POINT('Ctrl Pts',(59.9898750007537,-4.67821076220642,
-174.734782194308));
#158215=CARTESIAN_POINT('Ctrl Pts',(59.9924851917468,-4.67844571491974,
-174.703070568006));
#158216=CARTESIAN_POINT('Ctrl Pts',(59.9943634066945,-4.67865733157614,
-174.674144423609));
#158217=CARTESIAN_POINT('Ctrl Pts',(59.9957560933403,-4.67884722582315,
-174.647971186912));
#158218=CARTESIAN_POINT('Ctrl Pts',(59.9971686015776,-4.67903982276443,
-174.621425436262));
#158219=CARTESIAN_POINT('Ctrl Pts',(59.9980815614673,-4.67921010288986,
-174.597710889651));
#158220=CARTESIAN_POINT('Ctrl Pts',(59.9986978258392,-4.67936001600106,
-174.576787075096));
#158221=CARTESIAN_POINT('Ctrl Pts',(59.9993246130872,-4.67951248891803,
-174.555505980908));
#158222=CARTESIAN_POINT('Ctrl Pts',(59.9996443925775,-4.67964391657227,
-174.537111225911));
#158223=CARTESIAN_POINT('Ctrl Pts',(59.9998163358512,-4.67975622902168,
-174.521562257855));
#158224=CARTESIAN_POINT('Ctrl Pts',(59.9999609781594,-4.67985070862284,
-174.508482137991));
#158225=CARTESIAN_POINT('Ctrl Pts',(59.9999999999999,-4.67993166335616,
-174.49741579048));
#158226=CARTESIAN_POINT('Ctrl Pts',(60.,-4.68000001999999,-174.488343624884));
#158227=CARTESIAN_POINT('Ctrl Pts',(60.,-5.18000001999999,-174.511260182693));
#158228=CARTESIAN_POINT('Ctrl Pts',(60.,-5.01333573888012,-174.503547232447));
#158229=CARTESIAN_POINT('Ctrl Pts',(60.,-4.84666961885575,-174.495891400547));
#158230=CARTESIAN_POINT('Ctrl Pts',(60.,-4.68000001999999,-174.488343624884));
#158231=CARTESIAN_POINT('Origin',(39.,46.91999998,-129.34995));
#158232=CARTESIAN_POINT('',(39.,-11.8300000206964,-128.75511820843));
#158233=CARTESIAN_POINT('',(39.,-6.180000128392,-129.839693182379));
#158234=CARTESIAN_POINT('Ctrl Pts',(39.,-11.8300000219165,-128.755118230443));
#158235=CARTESIAN_POINT('Ctrl Pts',(39.,-11.2456383392948,-128.787506003178));
#158236=CARTESIAN_POINT('Ctrl Pts',(38.9999999999998,-10.6643296819649,
-128.844689763199));
#158237=CARTESIAN_POINT('Ctrl Pts',(39.0000000000002,-10.0859609278462,
-128.92574227051));
#158238=CARTESIAN_POINT('Ctrl Pts',(39.0000000000004,-9.71348092877341,
-128.977941559688));
#158239=CARTESIAN_POINT('Ctrl Pts',(39.0000000000007,-9.34222031417234,
-129.040041718412));
#158240=CARTESIAN_POINT('Ctrl Pts',(39.0000000000031,-8.97214920379055,
-129.111806478628));
#158241=CARTESIAN_POINT('Ctrl Pts',(39.0000000000039,-8.85321569986176,
-129.134870247055));
#158242=CARTESIAN_POINT('Ctrl Pts',(39.0000000000046,-8.73429069407208,
-129.1589539896));
#158243=CARTESIAN_POINT('Ctrl Pts',(39.0000000000049,-8.61535199981085,
-129.184060813321));
#158244=CARTESIAN_POINT('Ctrl Pts',(39.0000000000057,-8.31705980505462,
-129.247027450022));
#158245=CARTESIAN_POINT('Ctrl Pts',(39.0000000000046,-8.02087151391665,
-129.315956118525));
#158246=CARTESIAN_POINT('Ctrl Pts',(39.0000000000032,-7.72648278144565,
-129.39062643017));
#158247=CARTESIAN_POINT('Ctrl Pts',(39.0000000000018,-7.4202426468251,-129.468302793998));
#158248=CARTESIAN_POINT('Ctrl Pts',(39.0000000000006,-7.11594965101434,
-129.552192661459));
#158249=CARTESIAN_POINT('Ctrl Pts',(39.0000000000002,-6.81328756599089,
-129.642098960197));
#158250=CARTESIAN_POINT('Ctrl Pts',(39.,-6.60142553225938,-129.705032945782));
#158251=CARTESIAN_POINT('Ctrl Pts',(39.,-6.39036319103478,-129.770916038734));
#158252=CARTESIAN_POINT('Ctrl Pts',(39.,-6.18000018270164,-129.839693348042));
#158253=CARTESIAN_POINT('',(39.,-6.18000001999998,-102.218950121094));
#158254=CARTESIAN_POINT('',(39.,-6.18000001999998,-129.34995));
#158255=CARTESIAN_POINT('',(39.,-11.8300000202903,-103.303524781275));
#158256=CARTESIAN_POINT('Ctrl Pts',(39.0000000000558,-6.18000001999998,
-102.218950121094));
#158257=CARTESIAN_POINT('Ctrl Pts',(39.0000000001314,-6.52925246371981,
-102.333137272009));
#158258=CARTESIAN_POINT('Ctrl Pts',(39.0000000002528,-6.88066423663777,
-102.439420790159));
#158259=CARTESIAN_POINT('Ctrl Pts',(39.0000000003133,-7.23418430799431,
-102.537367117889));
#158260=CARTESIAN_POINT('Ctrl Pts',(39.0000000003723,-7.57920291835191,
-102.63295802947));
#158261=CARTESIAN_POINT('Ctrl Pts',(39.0000000003716,-7.92622968242249,
-102.720607819344));
#158262=CARTESIAN_POINT('Ctrl Pts',(39.0000000003073,-8.27519962485344,
-102.799960112761));
#158263=CARTESIAN_POINT('Ctrl Pts',(39.0000000002873,-8.38389527497297,
-102.824676422313));
#158264=CARTESIAN_POINT('Ctrl Pts',(39.0000000002619,-8.49277931386329,
-102.848588085812));
#158265=CARTESIAN_POINT('Ctrl Pts',(39.0000000002334,-8.60184941027751,
-102.871685311886));
#158266=CARTESIAN_POINT('Ctrl Pts',(39.0000000002017,-8.723199010669,-102.897382906795));
#158267=CARTESIAN_POINT('Ctrl Pts',(39.0000000001662,-8.84492476936504,
-102.922084618583));
#158268=CARTESIAN_POINT('Ctrl Pts',(39.0000000001318,-8.96688496783026,
-102.945759157014));
#158269=CARTESIAN_POINT('Ctrl Pts',(39.0000000000546,-9.24095711310763,
-102.998961198483));
#158270=CARTESIAN_POINT('Ctrl Pts',(39.0000000000303,-9.51689579309186,
-103.04710594614));
#158271=CARTESIAN_POINT('Ctrl Pts',(39.0000000000166,-9.7935384256358,-103.08982360864));
#158272=CARTESIAN_POINT('Ctrl Pts',(39.0000000000094,-9.93973590489214,
-103.112398634476));
#158273=CARTESIAN_POINT('Ctrl Pts',(39.0000000000059,-10.0861301614977,
-103.133457170461));
#158274=CARTESIAN_POINT('Ctrl Pts',(39.0000000000038,-10.2325489057379,
-103.152938666286));
#158275=CARTESIAN_POINT('Ctrl Pts',(38.9999999999998,-10.5104673644924,
-103.189916631927));
#158276=CARTESIAN_POINT('Ctrl Pts',(39.0000000000001,-10.7886085240243,
-103.221310636521));
#158277=CARTESIAN_POINT('Ctrl Pts',(39.,-11.0672887212858,-103.24709706551));
#158278=CARTESIAN_POINT('Ctrl Pts',(39.,-11.3209998818248,-103.270573096062));
#158279=CARTESIAN_POINT('Ctrl Pts',(39.,-11.5751577965224,-103.289400790235));
#158280=CARTESIAN_POINT('Ctrl Pts',(39.,-11.8300000206635,-103.303524774541));
#158281=CARTESIAN_POINT('',(39.,-11.83000002,-129.34995));
#158282=CARTESIAN_POINT('Ctrl Pts',(39.,-11.8686433059622,-128.75301285746));
#158283=CARTESIAN_POINT('Ctrl Pts',(39.,-11.928001403163,-129.861675775672));
#158284=CARTESIAN_POINT('Ctrl Pts',(39.4698940168252,-11.9817810974188,
-130.866147879494));
#158285=CARTESIAN_POINT('Ctrl Pts',(39.,-10.7823162329457,-128.811175087855));
#158286=CARTESIAN_POINT('Ctrl Pts',(39.,-10.9001869685749,-129.920171255555));
#158287=CARTESIAN_POINT('Ctrl Pts',(39.4726856154538,-11.0072350094688,
-130.924309912886));
#158288=CARTESIAN_POINT('Ctrl Pts',(39.,-9.69789923172707,-128.955540477711));
#158289=CARTESIAN_POINT('Ctrl Pts',(39.0000000000038,-9.87380661939344,
-130.065465765161));
#158290=CARTESIAN_POINT('Ctrl Pts',(39.4796201588693,-10.0340805400384,
-131.068675422521));
#158291=CARTESIAN_POINT('Ctrl Pts',(39.,-7.5328018765656,-129.41256745169));
#158292=CARTESIAN_POINT('Ctrl Pts',(38.9999999999961,-7.82478902027571,
-130.525032480762));
#158293=CARTESIAN_POINT('Ctrl Pts',(39.5013570517183,-8.08873720748368,
-131.525702236331));
#158294=CARTESIAN_POINT('Ctrl Pts',(39.,-6.48098994967646,-129.719043469502));
#158295=CARTESIAN_POINT('Ctrl Pts',(39.000000000015,-6.82874501931943,-130.833409195368));
#158296=CARTESIAN_POINT('Ctrl Pts',(39.5158567615765,-7.14247173527162,
-131.832173534627));
#158297=CARTESIAN_POINT('Ctrl Pts',(39.,-5.4610240206487,-130.086890037519));
#158298=CARTESIAN_POINT('Ctrl Pts',(39.,-5.86352497601848,-131.202945745636));
#158299=CARTESIAN_POINT('Ctrl Pts',(39.5330238402174,-6.22311741040379,
-132.200024593865));
#158300=CARTESIAN_POINT('',(39.5323905961839,-6.25584930016544,-132.186909003948));
#158301=CARTESIAN_POINT('',(39.4702993039609,-11.842906113671,-130.874975449521));
#158302=CARTESIAN_POINT('Ctrl Pts',(39.5323905962552,-6.25584930063541,
-132.186909005125));
#158303=CARTESIAN_POINT('Ctrl Pts',(39.523857640195,-6.71485178464417,-132.004109523071));
#158304=CARTESIAN_POINT('Ctrl Pts',(39.5161290340393,-7.17254264947844,
-131.839797338281));
#158305=CARTESIAN_POINT('Ctrl Pts',(39.5092514743187,-7.62950902695592,
-131.693972450754));
#158306=CARTESIAN_POINT('Ctrl Pts',(39.5058126944584,-7.85799221570156,
-131.621060006988));
#158307=CARTESIAN_POINT('Ctrl Pts',(39.5025859571867,-8.08629451480858,
-131.55276938753));
#158308=CARTESIAN_POINT('Ctrl Pts',(39.4995726887182,-8.31449060038593,
-131.489100581947));
#158309=CARTESIAN_POINT('Ctrl Pts',(39.498066054484,-8.42858864317462,-131.457266179156));
#158310=CARTESIAN_POINT('Ctrl Pts',(39.4966127484778,-8.54266013706068,
-131.426587248127));
#158311=CARTESIAN_POINT('Ctrl Pts',(39.4952126570643,-8.656714496533,-131.397063765538));
#158312=CARTESIAN_POINT('Ctrl Pts',(39.4945126113576,-8.71374167626916,
-131.382302024243));
#158313=CARTESIAN_POINT('Ctrl Pts',(39.4938258668266,-8.77076457270839,
-131.367829146221));
#158314=CARTESIAN_POINT('Ctrl Pts',(39.4931523927028,-8.82778436533119,
-131.353645131744));
#158315=CARTESIAN_POINT('Ctrl Pts',(39.492815655641,-8.85629426164259,-131.346553124506));
#158316=CARTESIAN_POINT('Ctrl Pts',(39.4924822360254,-8.88480338201596,
-131.339533333227));
#158317=CARTESIAN_POINT('Ctrl Pts',(39.4921521288706,-8.91331187415817,
-131.332585757904));
#158318=CARTESIAN_POINT('Ctrl Pts',(39.4918220217157,-8.94182036630037,
-131.325638182582));
#158319=CARTESIAN_POINT('Ctrl Pts',(39.4915087745014,-8.96913435998962,
-131.319047734368));
#158320=CARTESIAN_POINT('Ctrl Pts',(39.4911717391153,-8.99883561371038,
-131.311959679951));
#158321=CARTESIAN_POINT('Ctrl Pts',(39.4857791729374,-9.47405567324245,
-131.19855080929));
#158322=CARTESIAN_POINT('Ctrl Pts',(39.4813196690077,-9.94820234418142,
-131.105431021423));
#158323=CARTESIAN_POINT('Ctrl Pts',(39.4778365952643,-10.4219783954996,
-131.032600316352));
#158324=CARTESIAN_POINT('Ctrl Pts',(39.4743535215209,-10.8957544468178,
-130.95976961128));
#158325=CARTESIAN_POINT('Ctrl Pts',(39.4718469693993,-11.3691601359334,
-130.907227989003));
#158326=CARTESIAN_POINT('Ctrl Pts',(39.4702993039608,-11.842906113671,-130.874975449521));
#158327=CARTESIAN_POINT('Ctrl Pts',(39.5323905963862,-6.25584929916185,
-132.186909001152));
#158328=CARTESIAN_POINT('Ctrl Pts',(39.5179944370568,-6.25479880330938,
-132.156848952689));
#158329=CARTESIAN_POINT('Ctrl Pts',(39.5020197274459,-6.25361968902792,
-132.122785753625));
#158330=CARTESIAN_POINT('Ctrl Pts',(39.4847061343331,-6.2523014792109,-132.084599485537));
#158331=CARTESIAN_POINT('Ctrl Pts',(39.4684261104329,-6.25106196253827,
-132.048692822312));
#158332=CARTESIAN_POINT('Ctrl Pts',(39.450962599556,-6.24969928622832,-132.0091400591));
#158333=CARTESIAN_POINT('Ctrl Pts',(39.4325663511067,-6.24820853511762,
-131.965832371443));
#158334=CARTESIAN_POINT('Ctrl Pts',(39.4313984292324,-6.24811389186272,
-131.963082898044));
#158335=CARTESIAN_POINT('Ctrl Pts',(39.4302267652109,-6.24801873425826,
-131.960318288634));
#158336=CARTESIAN_POINT('Ctrl Pts',(39.4290514303077,-6.24792306186184,
-131.957538514917));
#158337=CARTESIAN_POINT('Ctrl Pts',(39.4108228025833,-6.2464392494667,-131.914426155958));
#158338=CARTESIAN_POINT('Ctrl Pts',(39.3917069600447,-6.24483093357756,
-131.867665934195));
#158339=CARTESIAN_POINT('Ctrl Pts',(39.3719967225372,-6.24310057463505,
-131.817153403871));
#158340=CARTESIAN_POINT('Ctrl Pts',(39.3704183573035,-6.24296201017607,
-131.813108438826));
#158341=CARTESIAN_POINT('Ctrl Pts',(39.3688362077372,-6.24282266780877,
-131.809039414516));
#158342=CARTESIAN_POINT('Ctrl Pts',(39.3672504385086,-6.24268255138138,
-131.804946279015));
#158343=CARTESIAN_POINT('Ctrl Pts',(39.3557827352194,-6.24166928060638,
-131.775346219556));
#158344=CARTESIAN_POINT('Ctrl Pts',(39.3439645144113,-6.24060098426729,
-131.744058170279));
#158345=CARTESIAN_POINT('Ctrl Pts',(39.3321251353788,-6.23950301199643,
-131.711747849603));
#158346=CARTESIAN_POINT('Ctrl Pts',(39.3218828342703,-6.23855315114849,
-131.683796042978));
#158347=CARTESIAN_POINT('Ctrl Pts',(39.3116243197905,-6.23758115645557,
-131.655079514983));
#158348=CARTESIAN_POINT('Ctrl Pts',(39.3015342098243,-6.23660444805766,
-131.626042903635));
#158349=CARTESIAN_POINT('Ctrl Pts',(39.280893042025,-6.23460641215916,-131.566643197469));
#158350=CARTESIAN_POINT('Ctrl Pts',(39.2624581975365,-6.23271275158796,
-131.510276774682));
#158351=CARTESIAN_POINT('Ctrl Pts',(39.245910507631,-6.23093757224289,-131.457104348278));
#158352=CARTESIAN_POINT('Ctrl Pts',(39.229157708339,-6.22914038946722,-131.403272847174));
#158353=CARTESIAN_POINT('Ctrl Pts',(39.2143386414709,-6.2274644078617,-131.352714546923));
#158354=CARTESIAN_POINT('Ctrl Pts',(39.2011526186406,-6.22591312153527,
-131.30555355468));
#158355=CARTESIAN_POINT('Ctrl Pts',(39.1877850185983,-6.22434047332816,
-131.257743135267));
#158356=CARTESIAN_POINT('Ctrl Pts',(39.1760953442301,-6.22289575183262,
-131.213423757931));
#158357=CARTESIAN_POINT('Ctrl Pts',(39.1658083189928,-6.22157474435082,
-131.172688346465));
#158358=CARTESIAN_POINT('Ctrl Pts',(39.164576028932,-6.22141649992618,-131.167808622589));
#158359=CARTESIAN_POINT('Ctrl Pts',(39.1633639148167,-6.22126002397052,
-131.162980290591));
#158360=CARTESIAN_POINT('Ctrl Pts',(39.162171543294,-6.22110530414493,-131.158203480778));
#158361=CARTESIAN_POINT('Ctrl Pts',(39.1570610239266,-6.22044217302339,
-131.137730013747));
#158362=CARTESIAN_POINT('Ctrl Pts',(39.1523129371346,-6.21981132039893,
-131.118203146671));
#158363=CARTESIAN_POINT('Ctrl Pts',(39.1478950036551,-6.21921161678299,
-131.09963198434));
#158364=CARTESIAN_POINT('Ctrl Pts',(39.1456860369154,-6.21891176497502,
-131.090346403175));
#158365=CARTESIAN_POINT('Ctrl Pts',(39.1435596592823,-6.21861969634864,
-131.081299736341));
#158366=CARTESIAN_POINT('Ctrl Pts',(39.1415121166505,-6.2183352522959,-131.072492943193));
#158367=CARTESIAN_POINT('Ctrl Pts',(39.1404883453346,-6.21819303026953,
-131.068089546618));
#158368=CARTESIAN_POINT('Ctrl Pts',(39.1394842859575,-6.21805271412436,
-131.063746117702));
#158369=CARTESIAN_POINT('Ctrl Pts',(39.1384994880882,-6.21791428326854,
-131.059462770329));
#158370=CARTESIAN_POINT('Ctrl Pts',(39.1380070891535,-6.21784506784063,
-131.057321096642));
#158371=CARTESIAN_POINT('Ctrl Pts',(39.137519505795,-6.21777632371958,-131.055194443296));
#158372=CARTESIAN_POINT('Ctrl Pts',(39.1370366828335,-6.21770804828387,
-131.053082823924));
#158373=CARTESIAN_POINT('Ctrl Pts',(39.1365538598719,-6.21763977284816,
-131.050971204551));
#158374=CARTESIAN_POINT('Ctrl Pts',(39.1364094970497,-6.21761943893419,
-131.050342030326));
#158375=CARTESIAN_POINT('Ctrl Pts',(39.1356024407393,-6.21750462536783,
-131.046793081091));
#158376=CARTESIAN_POINT('Ctrl Pts',(39.1150883146437,-6.21458624167215,
-130.956584267683));
#158377=CARTESIAN_POINT('Ctrl Pts',(39.0973860303671,-6.21172537375338,
-130.868122645569));
#158378=CARTESIAN_POINT('Ctrl Pts',(39.0821843947385,-6.20895207399527,
-130.781623452936));
#158379=CARTESIAN_POINT('Ctrl Pts',(39.0664755042733,-6.20608623355601,
-130.692237917354));
#158380=CARTESIAN_POINT('Ctrl Pts',(39.0534363138107,-6.20331381068036,
-130.604947964263));
#158381=CARTESIAN_POINT('Ctrl Pts',(39.0427217194077,-6.20064908714807,
-130.519937966199));
#158382=CARTESIAN_POINT('Ctrl Pts',(39.0318057827407,-6.19793428972137,
-130.433330510982));
#158383=CARTESIAN_POINT('Ctrl Pts',(39.0233020474348,-6.19533110598602,
-130.349089264251));
#158384=CARTESIAN_POINT('Ctrl Pts',(39.0168531430717,-6.19283746461102,
-130.267356945417));
#158385=CARTESIAN_POINT('Ctrl Pts',(39.0101961559517,-6.19026336247201,
-130.182987421057));
#158386=CARTESIAN_POINT('Ctrl Pts',(39.0057281795345,-6.18780581569125,
-130.10129110459));
#158387=CARTESIAN_POINT('Ctrl Pts',(39.0030730286528,-6.18544701429272,
-130.022373375295));
#158388=CARTESIAN_POINT('Ctrl Pts',(39.0009650480001,-6.18357431178611,
-129.959718914618));
#158389=CARTESIAN_POINT('Ctrl Pts',(39.0000000000003,-6.18176350020245,
-129.898814707424));
#158390=CARTESIAN_POINT('Ctrl Pts',(39.,-6.18000018270164,-129.839693348042));
#158391=CARTESIAN_POINT('Origin',(46.4017469067786,-11.845764450772,-128.222607383819));
#158392=CARTESIAN_POINT('Origin',(0.,-12.9675000200281,-171.64995));
#158393=CARTESIAN_POINT('',(58.3953999019963,-11.8387575339013,-171.449026400902));
#158394=CARTESIAN_POINT('',(58.0166638356104,-6.23225639415715,-171.449026400902));
#158395=CARTESIAN_POINT('Origin',(0.,-12.9675000200281,-171.449026400902));
#158396=CARTESIAN_POINT('Ctrl Pts',(58.0166638356104,-6.23225639415715,
-171.449026400902));
#158397=CARTESIAN_POINT('Ctrl Pts',(56.349577545528,-6.23372673672702,-167.897434994591));
#158398=CARTESIAN_POINT('Ctrl Pts',(54.7469618912178,-6.23517242645505,
-164.485193986989));
#158399=CARTESIAN_POINT('Ctrl Pts',(52.439761917831,-6.23757483085028,-159.575858073651));
#158400=CARTESIAN_POINT('Ctrl Pts',(51.686815584278,-6.23840909492504,-157.974250368882));
#158401=CARTESIAN_POINT('Ctrl Pts',(50.5815758482561,-6.23969494579187,
-155.624095211246));
#158402=CARTESIAN_POINT('Ctrl Pts',(50.0350008862545,-6.24034596867499,
-154.462081732306));
#158403=CARTESIAN_POINT('Ctrl Pts',(49.4079081179195,-6.24111077357991,
-153.129261514999));
#158404=CARTESIAN_POINT('Ctrl Pts',(49.0553674761703,-6.24154416602389,
-152.380081070807));
#158405=CARTESIAN_POINT('Ctrl Pts',(48.8814612455038,-6.24175878610164,
-152.010550217392));
#158406=CARTESIAN_POINT('Ctrl Pts',(48.7933718888155,-6.24186763099907,
-151.823379333081));
#158407=CARTESIAN_POINT('Ctrl Pts',(48.7911832326025,-6.24187033541698,
-151.818728915993));
#158408=CARTESIAN_POINT('Ctrl Pts',(45.3920876839696,-6.24607063796648,
-144.596406262261));
#158409=CARTESIAN_POINT('Ctrl Pts',(42.3069257173847,-6.25073126772922,
-138.054815014792));
#158410=CARTESIAN_POINT('Ctrl Pts',(39.532390596256,-6.25584930059378,-132.186909005141));
#158411=CARTESIAN_POINT('Ctrl Pts',(39.4702993039609,-11.842906113671,-130.874975449521));
#158412=CARTESIAN_POINT('Ctrl Pts',(41.7583572470671,-11.8421670407155,
-135.779786235607));
#158413=CARTESIAN_POINT('Ctrl Pts',(44.2894937407195,-11.8414658913629,
-141.205977562808));
#158414=CARTESIAN_POINT('Ctrl Pts',(47.0636808807324,-11.8408304355432,
-147.153562779003));
#158415=CARTESIAN_POINT('Ctrl Pts',(49.4731957341661,-11.840278511625,-152.319326369276));
#158416=CARTESIAN_POINT('Ctrl Pts',(52.0660617843129,-11.8397764603368,
-157.878417006278));
#158417=CARTESIAN_POINT('Ctrl Pts',(54.8422877286471,-11.8393150124165,
-163.830830224675));
#158418=CARTESIAN_POINT('Ctrl Pts',(55.995043971226,-11.8391234080653,-166.302416339601));
#158419=CARTESIAN_POINT('Ctrl Pts',(57.1794138783212,-11.8389384233643,
-168.841815469919));
#158420=CARTESIAN_POINT('Ctrl Pts',(58.3953999019963,-11.8387575339013,
-171.449026400902));
#158421=CARTESIAN_POINT('Ctrl Pts',(60.,-12.8269998197496,-174.751773822184));
#158422=CARTESIAN_POINT('Ctrl Pts',(60.,-12.8247546893956,-176.329633102893));
#158423=CARTESIAN_POINT('Ctrl Pts',(58.6998841333603,-12.8234825355735,
-177.223692421544));
#158424=CARTESIAN_POINT('Ctrl Pts',(60.,-12.9956778161511,-174.752013833507));
#158425=CARTESIAN_POINT('Ctrl Pts',(59.9999999999984,-12.9961202462228,
-176.329584396716));
#158426=CARTESIAN_POINT('Ctrl Pts',(58.7002617769476,-12.996381211483,-177.22367874123));
#158427=CARTESIAN_POINT('Ctrl Pts',(60.,-13.1643444677208,-174.751821305086));
#158428=CARTESIAN_POINT('Ctrl Pts',(60.,-13.16751068744,-176.329623133207));
#158429=CARTESIAN_POINT('Ctrl Pts',(58.6999592969537,-13.1692782682892,
-177.223689661345));
#158430=CARTESIAN_POINT('Ctrl Pts',(60.,-13.3329998199577,-174.75119758399));
#158431=CARTESIAN_POINT('Ctrl Pts',(60.,-13.338837622507,-176.329750343386));
#158432=CARTESIAN_POINT('Ctrl Pts',(58.6989770498873,-13.3421437200247,
-177.22372531347));
#158433=CARTESIAN_POINT('',(60.,-13.33000002,-174.751208632418));
#158434=CARTESIAN_POINT('',(58.7133156820334,-13.3314748988427,-177.213850299147));
#158435=CARTESIAN_POINT('Ctrl Pts',(60.,-13.33000002,-174.751208632418));
#158436=CARTESIAN_POINT('Ctrl Pts',(60.,-13.3300406632064,-174.817693892478));
#158437=CARTESIAN_POINT('Ctrl Pts',(59.9978175504489,-13.3300830974903,
-174.883676399972));
#158438=CARTESIAN_POINT('Ctrl Pts',(59.9935259312227,-13.33012663432,-174.948960491235));
#158439=CARTESIAN_POINT('Ctrl Pts',(59.9891899816022,-13.3301706208645,
-175.014918936243));
#158440=CARTESIAN_POINT('Ctrl Pts',(59.9827011519673,-13.3302157328684,
-175.080164469868));
#158441=CARTESIAN_POINT('Ctrl Pts',(59.9741881323204,-13.3302612676316,
-175.144504391241));
#158442=CARTESIAN_POINT('Ctrl Pts',(59.965483642566,-13.3303078265375,-175.210291410374));
#158443=CARTESIAN_POINT('Ctrl Pts',(59.9546629379879,-13.3303548274467,
-175.275131623486));
#158444=CARTESIAN_POINT('Ctrl Pts',(59.9419179227273,-13.3304015266371,
-175.338828443807));
#158445=CARTESIAN_POINT('Ctrl Pts',(59.9330492512272,-13.3304340224615,
-175.383152139265));
#158446=CARTESIAN_POINT('Ctrl Pts',(59.9232499582355,-13.3304663723483,
-175.426922389111));
#158447=CARTESIAN_POINT('Ctrl Pts',(59.9125992990762,-13.3304983276908,
-175.470075512945));
#158448=CARTESIAN_POINT('Ctrl Pts',(59.8981332593431,-13.3305417303804,
-175.528687359843));
#158449=CARTESIAN_POINT('Ctrl Pts',(59.8820111888294,-13.3305844310845,
-175.586206570858));
#158450=CARTESIAN_POINT('Ctrl Pts',(59.864531922907,-13.3306256977267,-175.642287543161));
#158451=CARTESIAN_POINT('Ctrl Pts',(59.8603213155855,-13.3306356385117,
-175.655796975057));
#158452=CARTESIAN_POINT('Ctrl Pts',(59.856032061966,-13.3306454962089,-175.66922315738));
#158453=CARTESIAN_POINT('Ctrl Pts',(59.8516685359687,-13.3306552608383,
-175.682561672477));
#158454=CARTESIAN_POINT('Ctrl Pts',(59.8315974156507,-13.3307001756736,
-175.743915481654));
#158455=CARTESIAN_POINT('Ctrl Pts',(59.8098453629079,-13.3307433634398,
-175.803746308069));
#158456=CARTESIAN_POINT('Ctrl Pts',(59.7867216622384,-13.3307845551397,
-175.861801089472));
#158457=CARTESIAN_POINT('Ctrl Pts',(59.7637846813986,-13.3308254142239,
-175.919387088692));
#158458=CARTESIAN_POINT('Ctrl Pts',(59.7394982842042,-13.3308643093334,
-175.975225576071));
#158459=CARTESIAN_POINT('Ctrl Pts',(59.7141598494433,-13.3309010082065,
-176.029120623913));
#158460=CARTESIAN_POINT('Ctrl Pts',(59.6948604672771,-13.3309289604295,
-176.070170559908));
#158461=CARTESIAN_POINT('Ctrl Pts',(59.6749506878815,-13.3309556391615,
-176.110094083364));
#158462=CARTESIAN_POINT('Ctrl Pts',(59.6545592887383,-13.3309809536881,
-176.148824764904));
#158463=CARTESIAN_POINT('Ctrl Pts',(59.6248502631807,-13.3310178354102,
-176.205253007011));
#158464=CARTESIAN_POINT('Ctrl Pts',(59.5939431737811,-13.3310520515032,
-176.259532914652));
#158465=CARTESIAN_POINT('Ctrl Pts',(59.5622506861511,-13.3310833724742,
-176.31154208023));
#158466=CARTESIAN_POINT('Ctrl Pts',(59.5406769550353,-13.3311046933062,
-176.34694579378));
#158467=CARTESIAN_POINT('Ctrl Pts',(59.5187390405221,-13.3311246732112,
-176.381298364634));
#158468=CARTESIAN_POINT('Ctrl Pts',(59.4965632307964,-13.3311432473675,
-176.414574433984));
#158469=CARTESIAN_POINT('Ctrl Pts',(59.4634357414712,-13.3311709945014,
-176.464284124219));
#158470=CARTESIAN_POINT('Ctrl Pts',(59.4297640859701,-13.3311957856679,
-176.511615559249));
#158471=CARTESIAN_POINT('Ctrl Pts',(59.3958538673844,-13.3312180275919,
-176.556637376878));
#158472=CARTESIAN_POINT('Ctrl Pts',(59.3604749618748,-13.3312412328368,
-176.60360913637));
#158473=CARTESIAN_POINT('Ctrl Pts',(59.3248363486428,-13.3312616634009,
-176.648067167108));
#158474=CARTESIAN_POINT('Ctrl Pts',(59.2892362542711,-13.3312797965956,
-176.690119079622));
#158475=CARTESIAN_POINT('Ctrl Pts',(59.2732699473442,-13.3312879291625,
-176.708978966201));
#158476=CARTESIAN_POINT('Ctrl Pts',(59.2573107554705,-13.3312955998131,
-176.727355236389));
#158477=CARTESIAN_POINT('Ctrl Pts',(59.2413826308639,-13.3313028524118,
-176.74525917353));
#158478=CARTESIAN_POINT('Ctrl Pts',(59.1984116798147,-13.3313224184983,
-176.79356047864));
#158479=CARTESIAN_POINT('Ctrl Pts',(59.1558409640565,-13.3313388818287,
-176.83831965251));
#158480=CARTESIAN_POINT('Ctrl Pts',(59.1139642014224,-13.3313532051975,
-176.879933610363));
#158481=CARTESIAN_POINT('Ctrl Pts',(59.1028928301105,-13.3313569920074,
-176.890935501393));
#158482=CARTESIAN_POINT('Ctrl Pts',(59.0918697733653,-13.3313606290969,
-176.901717342555));
#158483=CARTESIAN_POINT('Ctrl Pts',(59.0809000521733,-13.3313641339516,
-176.91228602047));
#158484=CARTESIAN_POINT('Ctrl Pts',(59.037658448174,-13.3313779497574,-176.953946749782));
#158485=CARTESIAN_POINT('Ctrl Pts',(58.9953543728595,-13.3313897838346,
-176.992195992816));
#158486=CARTESIAN_POINT('Ctrl Pts',(58.9543294737028,-13.3314009374072,
-177.027413076148));
#158487=CARTESIAN_POINT('Ctrl Pts',(58.9133506411377,-13.3314120784555,
-177.062590614446));
#158488=CARTESIAN_POINT('Ctrl Pts',(58.8736481149678,-13.3314225404819,
-177.094742812638));
#158489=CARTESIAN_POINT('Ctrl Pts',(58.8355275097074,-13.3314335944421,
-177.12420916681));
#158490=CARTESIAN_POINT('Ctrl Pts',(58.7974621106597,-13.331444632394,-177.153632847846));
#158491=CARTESIAN_POINT('Ctrl Pts',(58.7609740532324,-13.3314562605222,
-177.18037846857));
#158492=CARTESIAN_POINT('Ctrl Pts',(58.7263328221663,-13.331469719106,-177.204745412345));
#158493=CARTESIAN_POINT('Ctrl Pts',(58.7219643842158,-13.3314714163028,
-177.207818209663));
#158494=CARTESIAN_POINT('Ctrl Pts',(58.7176252699974,-13.3314731425762,
-177.210853129469));
#158495=CARTESIAN_POINT('Ctrl Pts',(58.7133159805679,-13.3314749003853,
-177.213850728308));
#158496=CARTESIAN_POINT('',(58.7141461350309,-12.8294402383603,-177.213832217122));
#158497=CARTESIAN_POINT('Origin',(-9.53286718169884,-12.9674995361125,-178.689058801762));
#158498=CARTESIAN_POINT('',(60.,-12.83000002,-174.751778045593));
#158499=CARTESIAN_POINT('Ctrl Pts',(58.7141461350221,-12.8294402383603,
-177.213832217103));
#158500=CARTESIAN_POINT('Ctrl Pts',(58.7755886331233,-12.8294220721977,
-177.171054260417));
#158501=CARTESIAN_POINT('Ctrl Pts',(58.8359427968261,-12.8294076339433,
-177.125614758351));
#158502=CARTESIAN_POINT('Ctrl Pts',(58.8948831125148,-12.8293968304697,
-177.077594979963));
#158503=CARTESIAN_POINT('Ctrl Pts',(58.9533625385092,-12.8293861114749,
-177.029950697036));
#158504=CARTESIAN_POINT('Ctrl Pts',(59.0104494931047,-12.8293789706229,
-176.979766371684));
#158505=CARTESIAN_POINT('Ctrl Pts',(59.0658331174558,-12.8293752468593,
-176.927171986301));
#158506=CARTESIAN_POINT('Ctrl Pts',(59.120872654405,-12.8293715462306,-176.874904359335));
#158507=CARTESIAN_POINT('Ctrl Pts',(59.174229327996,-12.8293712201624,-176.820256697794));
#158508=CARTESIAN_POINT('Ctrl Pts',(59.2256146190754,-12.8293740426676,
-176.763405201032));
#158509=CARTESIAN_POINT('Ctrl Pts',(59.2767636605023,-12.829376852196,-176.706815085418));
#158510=CARTESIAN_POINT('Ctrl Pts',(59.3259588177311,-12.8293827810321,
-176.648041653612));
#158511=CARTESIAN_POINT('Ctrl Pts',(59.3729411440154,-12.8293915431069,
-176.587303496293));
#158512=CARTESIAN_POINT('Ctrl Pts',(59.4197836406822,-12.8294002791039,
-176.526746108936));
#158513=CARTESIAN_POINT('Ctrl Pts',(59.464425943485,-12.829411830954,-176.464236091621));
#158514=CARTESIAN_POINT('Ctrl Pts',(59.5066452026437,-12.8294258590997,
-176.400029364887));
#158515=CARTESIAN_POINT('Ctrl Pts',(59.5488389306529,-12.8294398787623,
-176.335861465731));
#158516=CARTESIAN_POINT('Ctrl Pts',(59.5886121199466,-12.8294563710419,
-176.269999423512));
#158517=CARTESIAN_POINT('Ctrl Pts',(59.6257832108178,-12.8294749501596,
-176.202730993732));
#158518=CARTESIAN_POINT('Ctrl Pts',(59.6629837603696,-12.8294935440016,
-176.135409252651));
#158519=CARTESIAN_POINT('Ctrl Pts',(59.6975777773869,-12.8295142271887,
-176.066679489299));
#158520=CARTESIAN_POINT('Ctrl Pts',(59.7294297692503,-12.8295365772786,
-175.996854153079));
#158521=CARTESIAN_POINT('Ctrl Pts',(59.7613529583115,-12.8295589773266,
-175.926872739705));
#158522=CARTESIAN_POINT('Ctrl Pts',(59.7905216739406,-12.8295830508558,
-175.855791497974));
#158523=CARTESIAN_POINT('Ctrl Pts',(59.8168498754468,-12.8296083493863,
-175.783939712998));
#158524=CARTESIAN_POINT('Ctrl Pts',(59.843274872218,-12.8296337409265,-175.711823765938));
#158525=CARTESIAN_POINT('Ctrl Pts',(59.8668383938283,-12.8296603655722,
-175.638932268924));
#158526=CARTESIAN_POINT('Ctrl Pts',(59.8875057522723,-12.8296877601467,
-175.565603027702));
#158527=CARTESIAN_POINT('Ctrl Pts',(59.908361509043,-12.829715404443,-175.491605335967));
#158528=CARTESIAN_POINT('Ctrl Pts',(59.926268131564,-12.8297438318391,-175.417162555197));
#158529=CARTESIAN_POINT('Ctrl Pts',(59.9412429556759,-12.8297725705227,
-175.342616582038));
#158530=CARTESIAN_POINT('Ctrl Pts',(59.9563048455964,-12.8298014762971,
-175.267637187735));
#158531=CARTESIAN_POINT('Ctrl Pts',(59.9684009949618,-12.8298306961103,
-175.192554025529));
#158532=CARTESIAN_POINT('Ctrl Pts',(59.9775999311467,-12.8298597677861,
-175.117699848986));
#158533=CARTESIAN_POINT('Ctrl Pts',(59.986908142556,-12.8298891848077,-175.041956471043));
#158534=CARTESIAN_POINT('Ctrl Pts',(59.9932502385466,-12.8299184493296,
-174.966448134161));
#158535=CARTESIAN_POINT('Ctrl Pts',(59.9967447710968,-12.8299471137923,
-174.891494881111));
#158536=CARTESIAN_POINT('Ctrl Pts',(59.9989272876026,-12.8299650162334,
-174.844682693903));
#158537=CARTESIAN_POINT('Ctrl Pts',(59.9999999999993,-12.8299826852913,
-174.798086493521));
#158538=CARTESIAN_POINT('Ctrl Pts',(60.,-12.83000002,-174.751778045593));
#158539=CARTESIAN_POINT('Origin',(60.,-12.9674774176428,-75.9457339865586));
#158540=CARTESIAN_POINT('Origin',(39.,46.91999998,-129.34995));
#158541=CARTESIAN_POINT('',(39.,-19.98000002,-129.914446011788));
#158542=CARTESIAN_POINT('',(39.,-14.3300000196436,-128.768820403088));
#158543=CARTESIAN_POINT('Ctrl Pts',(39.0000000000669,-19.98000002,-129.914446011788));
#158544=CARTESIAN_POINT('Ctrl Pts',(39.0000000001518,-19.6367327840738,
-129.798586081307));
#158545=CARTESIAN_POINT('Ctrl Pts',(39.0000000002631,-19.2913217887197,
-129.690298412948));
#158546=CARTESIAN_POINT('Ctrl Pts',(39.0000000003003,-18.9438276300884,
-129.590011167479));
#158547=CARTESIAN_POINT('Ctrl Pts',(39.0000000003366,-18.6049646905776,
-129.49221490256));
#158548=CARTESIAN_POINT('Ctrl Pts',(39.0000000003094,-18.2641207496953,
-129.402026657412));
#158549=CARTESIAN_POINT('Ctrl Pts',(39.0000000002472,-17.9213701519525,
-129.31979718069));
#158550=CARTESIAN_POINT('Ctrl Pts',(39.0000000002263,-17.8056205246018,
-129.292027626528));
#158551=CARTESIAN_POINT('Ctrl Pts',(39.0000000002019,-17.6896536077095,
-129.265165339738));
#158552=CARTESIAN_POINT('Ctrl Pts',(39.0000000001767,-17.5734727602674,
-129.239222565105));
#158553=CARTESIAN_POINT('Ctrl Pts',(39.0000000001494,-17.4477751466172,
-129.211154730048));
#158554=CARTESIAN_POINT('Ctrl Pts',(39.0000000001211,-17.3216708975945,
-129.184146383705));
#158555=CARTESIAN_POINT('Ctrl Pts',(39.0000000000953,-17.1952995452482,
-129.158233426905));
#158556=CARTESIAN_POINT('Ctrl Pts',(39.0000000000407,-16.9274823440487,
-129.103316426838));
#158557=CARTESIAN_POINT('Ctrl Pts',(39.0000000000228,-16.6579107580334,
-129.053205467123));
#158558=CARTESIAN_POINT('Ctrl Pts',(39.0000000000127,-16.3874479062833,
-129.008231038422));
#158559=CARTESIAN_POINT('Ctrl Pts',(39.0000000000071,-16.2374573286264,
-128.983289570501));
#158560=CARTESIAN_POINT('Ctrl Pts',(39.0000000000044,-16.0871922946708,
-128.959928670237));
#158561=CARTESIAN_POINT('Ctrl Pts',(39.0000000000028,-15.9367995435377,
-128.938211682847));
#158562=CARTESIAN_POINT('Ctrl Pts',(39.,-15.6676875947363,-128.899351426921));
#158563=CARTESIAN_POINT('Ctrl Pts',(39.0000000000001,-15.3983918170305,
-128.865722188253));
#158564=CARTESIAN_POINT('Ctrl Pts',(39.,-15.1285853320425,-128.837337411665));
#158565=CARTESIAN_POINT('Ctrl Pts',(39.,-14.8629886325448,-128.809395522211));
#158566=CARTESIAN_POINT('Ctrl Pts',(39.,-14.5968970408721,-128.786535808696));
#158567=CARTESIAN_POINT('Ctrl Pts',(39.,-14.3300000191853,-128.768820409992));
#158568=CARTESIAN_POINT('',(39.0000000000001,-14.330000015482,-103.28982244638));
#158569=CARTESIAN_POINT('',(39.,-14.33000002,-129.34995));
#158570=CARTESIAN_POINT('',(39.,-19.9800000199999,-102.144196959718));
#158571=CARTESIAN_POINT('Ctrl Pts',(39.,-14.3300000071456,-103.289822320808));
#158572=CARTESIAN_POINT('Ctrl Pts',(39.,-14.6503224302969,-103.268556852662));
#158573=CARTESIAN_POINT('Ctrl Pts',(38.9999999999999,-14.9696787697451,
-103.239819970848));
#158574=CARTESIAN_POINT('Ctrl Pts',(39.0000000000001,-15.2880843675587,
-103.203826801699));
#158575=CARTESIAN_POINT('Ctrl Pts',(39.0000000000004,-15.6115732353083,
-103.167259010131));
#158576=CARTESIAN_POINT('Ctrl Pts',(38.9999999999999,-15.9340810135561,
-103.123201376371));
#158577=CARTESIAN_POINT('Ctrl Pts',(39.0000000000089,-16.2556315657715,
-103.071825704718));
#158578=CARTESIAN_POINT('Ctrl Pts',(39.0000000000177,-16.5680888803951,
-103.021902903184));
#158579=CARTESIAN_POINT('Ctrl Pts',(39.0000000000333,-16.8796426042176,
-102.965069752024));
#158580=CARTESIAN_POINT('Ctrl Pts',(39.000000000099,-17.1903180517835,-102.90143687879));
#158581=CARTESIAN_POINT('Ctrl Pts',(39.0000000001251,-17.3140185734884,
-102.87610040731));
#158582=CARTESIAN_POINT('Ctrl Pts',(39.0000000001567,-17.4376802476524,
-102.849665441423));
#158583=CARTESIAN_POINT('Ctrl Pts',(39.0000000001917,-17.5613085289994,
-102.822130971399));
#158584=CARTESIAN_POINT('Ctrl Pts',(39.000000000283,-17.8840119032272,-102.750258530179));
#158585=CARTESIAN_POINT('Ctrl Pts',(39.0000000004,-18.2040368478246,-102.671531783398));
#158586=CARTESIAN_POINT('Ctrl Pts',(39.0000000004561,-18.5218724866243,
-102.586181685713));
#158587=CARTESIAN_POINT('Ctrl Pts',(39.0000000005153,-18.8564962428645,
-102.496323385396));
#158588=CARTESIAN_POINT('Ctrl Pts',(39.0000000004874,-19.1886932216449,
-102.399123389358));
#158589=CARTESIAN_POINT('Ctrl Pts',(39.0000000003521,-19.5190105422359,
-102.294797669285));
#158590=CARTESIAN_POINT('Ctrl Pts',(39.000000000289,-19.6730648764638,-102.246141942362));
#158591=CARTESIAN_POINT('Ctrl Pts',(39.0000000002054,-19.8267100435463,
-102.195935559143));
#158592=CARTESIAN_POINT('Ctrl Pts',(39.000000000131,-19.98000002,-102.144196959718));
#158593=CARTESIAN_POINT('',(39.,-19.98000002,-129.34995));
#158594=CARTESIAN_POINT('Ctrl Pts',(39.,-20.720937818584,-130.177378160746));
#158595=CARTESIAN_POINT('Ctrl Pts',(39.,-20.3054116348924,-131.293905860767));
#158596=CARTESIAN_POINT('Ctrl Pts',(39.5372195035444,-19.9345312052232,
-132.290469469449));
#158597=CARTESIAN_POINT('Ctrl Pts',(39.,-19.698133940161,-129.796732169428));
#158598=CARTESIAN_POINT('Ctrl Pts',(39.,-19.3374585219745,-130.911526747764));
#158599=CARTESIAN_POINT('Ctrl Pts',(39.5194895810462,-19.0123420478084,
-131.90982316175));
#158600=CARTESIAN_POINT('Ctrl Pts',(39.,-18.6506584423116,-129.479682762144));
#158601=CARTESIAN_POINT('Ctrl Pts',(38.9999999999923,-18.3454434179522,
-130.592508390753));
#158602=CARTESIAN_POINT('Ctrl Pts',(39.5045124277029,-18.0697294738066,
-131.592774070923));
#158603=CARTESIAN_POINT('Ctrl Pts',(39.,-17.0348936577371,-129.118930933505));
#158604=CARTESIAN_POINT('Ctrl Pts',(39.0000000000038,-16.8157658206047,
-130.229644160077));
#158605=CARTESIAN_POINT('Ctrl Pts',(39.4873751859149,-16.6176732464254,
-131.23202224217));
#158606=CARTESIAN_POINT('Ctrl Pts',(39.,-16.4860091127214,-129.017507601134));
#158607=CARTESIAN_POINT('Ctrl Pts',(39.,-16.2963199259075,-130.127635847669));
#158608=CARTESIAN_POINT('Ctrl Pts',(39.4825356614912,-16.1247177152636,
-131.130598909837));
#158609=CARTESIAN_POINT('Ctrl Pts',(39.,-15.3875914977103,-128.858905214396));
#158610=CARTESIAN_POINT('Ctrl Pts',(39.,-15.2570331695429,-129.96814976082));
#158611=CARTESIAN_POINT('Ctrl Pts',(39.4749533438571,-15.1386572025492,
-130.9719965231));
#158612=CARTESIAN_POINT('Ctrl Pts',(39.,-14.8389953875779,-128.801602009569));
#158613=CARTESIAN_POINT('Ctrl Pts',(38.9999999999999,-14.7379707288414,
-129.910514022628));
#158614=CARTESIAN_POINT('Ctrl Pts',(39.4722050319315,-14.6463890166082,
-130.914693311714));
#158615=CARTESIAN_POINT('Ctrl Pts',(39.,-14.2910120087967,-128.766269567481));
#158616=CARTESIAN_POINT('Ctrl Pts',(39.,-14.2195253716732,-129.874981182379));
#158617=CARTESIAN_POINT('Ctrl Pts',(39.4705097325996,-14.1547657662532,
-130.879360876185));
#158618=CARTESIAN_POINT('',(39.4710976354407,-14.3145440749074,-130.891615496825));
#158619=CARTESIAN_POINT('',(39.5365899598451,-19.9017174806626,-132.276955615329));
#158620=CARTESIAN_POINT('Ctrl Pts',(39.4710975927162,-14.3145440734493,
-130.89161551676));
#158621=CARTESIAN_POINT('Ctrl Pts',(39.471847193384,-14.5062549022323,-130.907244870022));
#158622=CARTESIAN_POINT('Ctrl Pts',(39.4727537671787,-14.6975339673999,
-130.926164753854));
#158623=CARTESIAN_POINT('Ctrl Pts',(39.4738171268208,-14.888760940223,-130.948378536857));
#158624=CARTESIAN_POINT('Ctrl Pts',(39.474880959685,-15.0800730138931,-130.970602205556));
#158625=CARTESIAN_POINT('Ctrl Pts',(39.4761017195622,-15.2713329311122,
-130.996122712195));
#158626=CARTESIAN_POINT('Ctrl Pts',(39.4774817130348,-15.4629223698792,
-131.024995466283));
#158627=CARTESIAN_POINT('Ctrl Pts',(39.477886687669,-15.5191464494941,-131.033468501305));
#158628=CARTESIAN_POINT('Ctrl Pts',(39.4783053917035,-15.5753989181463,
-131.042230571371));
#158629=CARTESIAN_POINT('Ctrl Pts',(39.4787379239733,-15.6316894498703,
-131.051283927837));
#158630=CARTESIAN_POINT('Ctrl Pts',(39.4802253119557,-15.8252608114915,
-131.082416526602));
#158631=CARTESIAN_POINT('Ctrl Pts',(39.4818769063609,-16.0191549692742,
-131.117009241646));
#158632=CARTESIAN_POINT('Ctrl Pts',(39.4836882348007,-16.2132119285899,
-131.15498469469));
#158633=CARTESIAN_POINT('Ctrl Pts',(39.4854164288744,-16.3983622744101,
-131.191217192038));
#158634=CARTESIAN_POINT('Ctrl Pts',(39.4872900662569,-16.5836618542002,
-131.230529742924));
#158635=CARTESIAN_POINT('Ctrl Pts',(39.4893069555753,-16.7689438009247,
-131.272891706083));
#158636=CARTESIAN_POINT('Ctrl Pts',(39.4905145726718,-16.8798817906742,
-131.298256028499));
#158637=CARTESIAN_POINT('Ctrl Pts',(39.4917735763949,-16.9908128539619,
-131.324714234321));
#158638=CARTESIAN_POINT('Ctrl Pts',(39.4930837333765,-17.1016937426839,
-131.3522649967));
#158639=CARTESIAN_POINT('Ctrl Pts',(39.4933071500142,-17.1206018855207,
-131.356963135003));
#158640=CARTESIAN_POINT('Ctrl Pts',(39.4935320777091,-17.1395124913016,
-131.361693525097));
#158641=CARTESIAN_POINT('Ctrl Pts',(39.4937585203661,-17.1584259087636,
-131.366456272776));
#158642=CARTESIAN_POINT('Ctrl Pts',(39.495180807944,-17.2772211881662,-131.396371117214));
#158643=CARTESIAN_POINT('Ctrl Pts',(39.4966613081908,-17.396083803422,-131.427549347277));
#158644=CARTESIAN_POINT('Ctrl Pts',(39.4981991234424,-17.5150239674286,
-131.459993872874));
#158645=CARTESIAN_POINT('Ctrl Pts',(39.4989402647689,-17.5723465039512,
-131.475630327717));
#158646=CARTESIAN_POINT('Ctrl Pts',(39.4996676909946,-17.6275909302336,
-131.490985006607));
#158647=CARTESIAN_POINT('Ctrl Pts',(39.5003975533504,-17.6821327275196,
-131.506398539652));
#158648=CARTESIAN_POINT('Ctrl Pts',(39.501014492288,-17.7282358841042,-131.519427309566));
#158649=CARTESIAN_POINT('Ctrl Pts',(39.5016332183093,-17.7738366805642,
-131.532499125543));
#158650=CARTESIAN_POINT('Ctrl Pts',(39.5022647440593,-17.8197567988279,
-131.54584706425));
#158651=CARTESIAN_POINT('Ctrl Pts',(39.5023846973585,-17.8284789604902,
-131.548382399168));
#158652=CARTESIAN_POINT('Ctrl Pts',(39.5025051156569,-17.8372126194999,
-131.55092776617));
#158653=CARTESIAN_POINT('Ctrl Pts',(39.5026260789289,-17.8459633741104,
-131.553484861057));
#158654=CARTESIAN_POINT('Ctrl Pts',(39.5027441884728,-17.8545076836315,
-131.555981629755));
#158655=CARTESIAN_POINT('Ctrl Pts',(39.5028628740704,-17.8630723274425,
-131.558490774156));
#158656=CARTESIAN_POINT('Ctrl Pts',(39.5029817892779,-17.8716322053535,
-131.561004974254));
#158657=CARTESIAN_POINT('Ctrl Pts',(39.508478276978,-18.2672860888239,-131.67721609819));
#158658=CARTESIAN_POINT('Ctrl Pts',(39.5146109899203,-18.6633075913778,
-131.807303922318));
#158659=CARTESIAN_POINT('Ctrl Pts',(39.5213644858589,-19.0600784979616,
-131.951274464432));
#158660=CARTESIAN_POINT('Ctrl Pts',(39.5261325711292,-19.3402056398967,
-132.052920164296));
#158661=CARTESIAN_POINT('Ctrl Pts',(39.5312100096328,-19.6207057232028,
-132.161484957873));
#158662=CARTESIAN_POINT('Ctrl Pts',(39.5365899584985,-19.9017174949438,
-132.276955564612));
#158663=CARTESIAN_POINT('Origin',(46.4751157297648,-14.311069215956,-128.224481951383));
#158664=CARTESIAN_POINT('Ctrl Pts',(39.0000000000669,-19.98000002,-129.914446011788));
#158665=CARTESIAN_POINT('Ctrl Pts',(39.0000003661163,-19.9777368568499,
-129.988373295946));
#158666=CARTESIAN_POINT('Ctrl Pts',(39.0015009625459,-19.9753955019565,
-130.065171376428));
#158667=CARTESIAN_POINT('Ctrl Pts',(39.0048608917524,-19.9729474378609,
-130.144774766188));
#158668=CARTESIAN_POINT('Ctrl Pts',(39.0081523964114,-19.9705492282913,
-130.222757042648));
#158669=CARTESIAN_POINT('Ctrl Pts',(39.0132286832547,-19.9680484121296,
-130.303431904837));
#158670=CARTESIAN_POINT('Ctrl Pts',(39.0204492557753,-19.9654302366679,
-130.386695447003));
#158671=CARTESIAN_POINT('Ctrl Pts',(39.0274582141761,-19.9628887923649,
-130.467518775301));
#158672=CARTESIAN_POINT('Ctrl Pts',(39.036488107848,-19.9602366117811,-130.5507814907));
#158673=CARTESIAN_POINT('Ctrl Pts',(39.0478819729243,-19.9574742277174,
-130.636344073164));
#158674=CARTESIAN_POINT('Ctrl Pts',(39.0545620631387,-19.9558546741568,
-130.686508417397));
#158675=CARTESIAN_POINT('Ctrl Pts',(39.062054969042,-19.9541975163494,-130.737462445253));
#158676=CARTESIAN_POINT('Ctrl Pts',(39.0704310879636,-19.9525055342341,
-130.789170171557));
#158677=CARTESIAN_POINT('Ctrl Pts',(39.079165226721,-19.9507412318516,-130.843088037409));
#158678=CARTESIAN_POINT('Ctrl Pts',(39.0888597435241,-19.948939029304,-130.897825485729));
#158679=CARTESIAN_POINT('Ctrl Pts',(39.0995946815592,-19.9471047139459,
-130.953334379507));
#158680=CARTESIAN_POINT('Ctrl Pts',(39.1049621505767,-19.9461875562668,
-130.981088826396));
#158681=CARTESIAN_POINT('Ctrl Pts',(39.1105897492738,-19.9452623720647,
-131.009036129875));
#158682=CARTESIAN_POINT('Ctrl Pts',(39.116487410739,-19.9443302068421,-131.037169407258));
#158683=CARTESIAN_POINT('Ctrl Pts',(39.1194362414716,-19.9438641242308,
-131.05123604595));
#158684=CARTESIAN_POINT('Ctrl Pts',(39.1224525886999,-19.9433962964075,
-131.065349177994));
#158685=CARTESIAN_POINT('Ctrl Pts',(39.1255376923908,-19.9429268649362,
-131.079507915865));
#158686=CARTESIAN_POINT('Ctrl Pts',(39.1270802442362,-19.9426921492006,
-131.0865872848));
#158687=CARTESIAN_POINT('Ctrl Pts',(39.1286399852446,-19.9424570325568,
-131.093678055182));
#158688=CARTESIAN_POINT('Ctrl Pts',(39.1302170699468,-19.9422215338507,
-131.100780113065));
#158689=CARTESIAN_POINT('Ctrl Pts',(39.1310056122978,-19.9421037844977,
-131.104331142007));
#158690=CARTESIAN_POINT('Ctrl Pts',(39.1317984905748,-19.9419859396293,
-131.107884992824));
#158691=CARTESIAN_POINT('Ctrl Pts',(39.1325957240583,-19.941868001679,-131.111441651072));
#158692=CARTESIAN_POINT('Ctrl Pts',(39.1333929575419,-19.9417500637286,
-131.114998309321));
#158693=CARTESIAN_POINT('Ctrl Pts',(39.134531130502,-19.941582703029,-131.120045436292));
#158694=CARTESIAN_POINT('Ctrl Pts',(39.1350005094029,-19.9415139110393,
-131.122120033608));
#158695=CARTESIAN_POINT('Ctrl Pts',(39.1425105718177,-19.9404132392045,
-131.155313590669));
#158696=CARTESIAN_POINT('Ctrl Pts',(39.1512549053093,-19.939183276348,-131.192549999964));
#158697=CARTESIAN_POINT('Ctrl Pts',(39.1614907401956,-19.9378138682254,
-131.233761736226));
#158698=CARTESIAN_POINT('Ctrl Pts',(39.171726575082,-19.9364444601029,-131.274973472488));
#158699=CARTESIAN_POINT('Ctrl Pts',(39.1834541487602,-19.9349353410833,
-131.320161159432));
#158700=CARTESIAN_POINT('Ctrl Pts',(39.1969827572539,-19.9332812983121,
-131.369224668865));
#158701=CARTESIAN_POINT('Ctrl Pts',(39.207442020742,-19.9320025216239,-131.407156742445));
#158702=CARTESIAN_POINT('Ctrl Pts',(39.2188983592693,-19.9306465353236,
-131.447121602909));
#158703=CARTESIAN_POINT('Ctrl Pts',(39.2315999854523,-19.9292039335511,
-131.48938673147));
#158704=CARTESIAN_POINT('Ctrl Pts',(39.2436716909817,-19.9278328757399,
-131.529555775874));
#158705=CARTESIAN_POINT('Ctrl Pts',(39.2568682353366,-19.9263834726761,
-131.571802875789));
#158706=CARTESIAN_POINT('Ctrl Pts',(39.2714424595273,-19.9248510153574,
-131.616333969799));
#158707=CARTESIAN_POINT('Ctrl Pts',(39.2812031361056,-19.9238246951867,
-131.646157417045));
#158708=CARTESIAN_POINT('Ctrl Pts',(39.2915825498145,-19.9227611873571,
-131.677004826585));
#158709=CARTESIAN_POINT('Ctrl Pts',(39.3026674122468,-19.9216604123578,
-131.708930511829));
#158710=CARTESIAN_POINT('Ctrl Pts',(39.3230244720018,-19.9196388678799,
-131.767561197254));
#158711=CARTESIAN_POINT('Ctrl Pts',(39.3432099268556,-19.9177236323538,
-131.822474694915));
#158712=CARTESIAN_POINT('Ctrl Pts',(39.3628888866153,-19.9159285670117,
-131.873757669544));
#158713=CARTESIAN_POINT('Ctrl Pts',(39.3830325254433,-19.9140911148106,
-131.92625158851));
#158714=CARTESIAN_POINT('Ctrl Pts',(39.4026453461985,-19.9123793539091,
-131.974942141252));
#158715=CARTESIAN_POINT('Ctrl Pts',(39.4214203923536,-19.9107967575629,
-132.019933390249));
#158716=CARTESIAN_POINT('Ctrl Pts',(39.4403970415853,-19.9091971675812,
-132.065407747205));
#158717=CARTESIAN_POINT('Ctrl Pts',(39.4585178974063,-19.9077292958912,
-132.107103532241));
#158718=CARTESIAN_POINT('Ctrl Pts',(39.4755189459911,-19.9063887570054,
-132.145129888499));
#158719=CARTESIAN_POINT('Ctrl Pts',(39.4927238794532,-19.9050321417226,
-132.183612275391));
#158720=CARTESIAN_POINT('Ctrl Pts',(39.5087820945746,-19.9038057193559,
-132.218337222793));
#158721=CARTESIAN_POINT('Ctrl Pts',(39.5234725234859,-19.9027002333108,
-132.249410952062));
#158722=CARTESIAN_POINT('Ctrl Pts',(39.5279749265633,-19.9023614178956,
-132.258934598726));
#158723=CARTESIAN_POINT('Ctrl Pts',(39.5323492112491,-19.9020339414172,
-132.268115196008));
#158724=CARTESIAN_POINT('Ctrl Pts',(39.5365899584985,-19.9017174949438,
-132.276955564612));
#158725=CARTESIAN_POINT('Origin',(0.,-12.9675000200281,-171.64995));
#158726=CARTESIAN_POINT('',(57.9903087491627,-19.9260113903464,-171.449026400902));
#158727=CARTESIAN_POINT('',(58.3906572805143,-14.3195102506022,-171.449026400902));
#158728=CARTESIAN_POINT('Origin',(0.,-12.9675000200281,-171.449026400902));
#158729=CARTESIAN_POINT('Ctrl Pts',(58.3906572805143,-14.3195102506022,
-171.449026400902));
#158730=CARTESIAN_POINT('Ctrl Pts',(56.6764429446617,-14.3192048286978,
-167.77385178941));
#158731=CARTESIAN_POINT('Ctrl Pts',(55.0310749604167,-14.318890449637,-164.246346972861));
#158732=CARTESIAN_POINT('Ctrl Pts',(53.4545452629458,-14.318560171184,-160.866515925776));
#158733=CARTESIAN_POINT('Ctrl Pts',(52.6662804142103,-14.3183950319575,
-159.176600402234));
#158734=CARTESIAN_POINT('Ctrl Pts',(51.895225247074,-14.3182260159383,-157.523603253589));
#158735=CARTESIAN_POINT('Ctrl Pts',(51.1413794916545,-14.3180481994016,
-155.907524626682));
#158736=CARTESIAN_POINT('Ctrl Pts',(50.7644566139448,-14.3179592911332,
-155.099485313228));
#158737=CARTESIAN_POINT('Ctrl Pts',(50.391836093189,-14.3178683195607,-154.300675628705));
#158738=CARTESIAN_POINT('Ctrl Pts',(50.0235178752065,-14.317777011786,-153.51109559057));
#158739=CARTESIAN_POINT('Ctrl Pts',(49.8393587662153,-14.3177313578986,
-153.116305571502));
#158740=CARTESIAN_POINT('Ctrl Pts',(49.6562752331921,-14.3176856199487,
-152.723822963869));
#158741=CARTESIAN_POINT('Ctrl Pts',(49.4742672731976,-14.3176399235889,
-152.333647768291));
#158742=CARTESIAN_POINT('Ctrl Pts',(49.3832632932003,-14.317617075409,-152.138560170502));
#158743=CARTESIAN_POINT('Ctrl Pts',(49.2925282064789,-14.317594237627,-151.944049425717));
#158744=CARTESIAN_POINT('Ctrl Pts',(49.2020620127266,-14.3175714278585,
-151.750115533972));
#158745=CARTESIAN_POINT('Ctrl Pts',(49.1144228875291,-14.3175493308953,
-151.562242076344));
#158746=CARTESIAN_POINT('Ctrl Pts',(49.0270361120814,-14.317527260222,-151.374909981773));
#158747=CARTESIAN_POINT('Ctrl Pts',(48.9399016861439,-14.3175052327755,
-151.188119250263));
#158748=CARTESIAN_POINT('Ctrl Pts',(48.9370908982105,-14.3175045222127,
-151.182093742795));
#158749=CARTESIAN_POINT('Ctrl Pts',(48.9348754797666,-14.3175039621476,
-151.177344533669));
#158750=CARTESIAN_POINT('Ctrl Pts',(48.9314701101151,-14.3175031012272,
-151.170044417858));
#158751=CARTESIAN_POINT('Ctrl Pts',(46.2622647123347,-14.3168282924576,
-145.448049298071));
#158752=CARTESIAN_POINT('Ctrl Pts',(43.7885373821752,-14.3160934996481,
-140.145481122769));
#158753=CARTESIAN_POINT('Ctrl Pts',(41.5103050054923,-14.3152949524359,
-135.26233262387));
#158754=CARTESIAN_POINT('Ctrl Pts',(40.812213131252,-14.315050263033,-133.766047028652));
#158755=CARTESIAN_POINT('Ctrl Pts',(40.1324769686662,-14.3147998235171,
-132.309141494925));
#158756=CARTESIAN_POINT('Ctrl Pts',(39.4710976496822,-14.3145440753934,
-130.89161549018));
#158757=CARTESIAN_POINT('Ctrl Pts',(39.5365899624517,-19.9017174575869,
-132.27695566545));
#158758=CARTESIAN_POINT('Ctrl Pts',(40.9222207127391,-19.9043502993893,
-135.204751179876));
#158759=CARTESIAN_POINT('Ctrl Pts',(42.3851075877766,-19.9070565011848,
-138.300261437352));
#158760=CARTESIAN_POINT('Ctrl Pts',(44.6953683528657,-19.9106521746941,
-143.195098938138));
#158761=CARTESIAN_POINT('Ctrl Pts',(45.484775776705,-19.911785330507,-144.868640124163));
#158762=CARTESIAN_POINT('Ctrl Pts',(46.6978643305816,-19.9134223042145,
-147.441844931843));
#158763=CARTESIAN_POINT('Ctrl Pts',(47.3116528834097,-19.914226217965,-148.744170592844));
#158764=CARTESIAN_POINT('Ctrl Pts',(48.0404155449538,-19.9151581515399,
-150.29106623071));
#158765=CARTESIAN_POINT('Ctrl Pts',(48.4079656496442,-19.915625950211,-151.07139297465));
#158766=CARTESIAN_POINT('Ctrl Pts',(48.6156037677501,-19.9158900971054,
-151.512261465775));
#158767=CARTESIAN_POINT('Ctrl Pts',(48.7180581100362,-19.916020478077,-151.729811584573));
#158768=CARTESIAN_POINT('Ctrl Pts',(48.7710084967803,-19.9160878923004,
-151.842249064289));
#158769=CARTESIAN_POINT('Ctrl Pts',(48.774880162121,-19.9160928217188,-151.850470369442));
#158770=CARTESIAN_POINT('Ctrl Pts',(51.5915976683688,-19.919679174478,-157.83165200233));
#158771=CARTESIAN_POINT('Ctrl Pts',(54.6624934339681,-19.9229803733939,
-164.362558913099));
#158772=CARTESIAN_POINT('Ctrl Pts',(57.9903087491627,-19.9260113903464,
-171.449026400902));
#158773=CARTESIAN_POINT('Ctrl Pts',(60.,-20.8715629014036,-174.505875827596));
#158774=CARTESIAN_POINT('Ctrl Pts',(59.9999999999999,-20.9611893120647,
-176.449983597595));
#158775=CARTESIAN_POINT('Ctrl Pts',(58.2228448679712,-20.997722377502,-177.242431000704));
#158776=CARTESIAN_POINT('Ctrl Pts',(60.,-21.0755801285197,-174.496470313984));
#158777=CARTESIAN_POINT('Ctrl Pts',(59.9999999999923,-21.1661125646405,
-176.460241938351));
#158778=CARTESIAN_POINT('Ctrl Pts',(58.1976125313383,-21.2014273832677,
-177.244315088819));
#158779=CARTESIAN_POINT('Ctrl Pts',(60.,-21.2796010327843,-174.487167894352));
#158780=CARTESIAN_POINT('Ctrl Pts',(60.0000000000095,-21.3701601153012,
-176.47139510613));
#158781=CARTESIAN_POINT('Ctrl Pts',(58.1714292060958,-21.40462514847,-177.246332126403));
#158782=CARTESIAN_POINT('Ctrl Pts',(60.,-21.4836289747507,-174.478062871828));
#158783=CARTESIAN_POINT('Ctrl Pts',(60.,-21.57312595156,-176.483536694353));
#158784=CARTESIAN_POINT('Ctrl Pts',(58.1443031111632,-21.607263174561,-177.248493339177));
#158785=CARTESIAN_POINT('',(60.,-21.48000002,-174.47822483969));
#158786=CARTESIAN_POINT('',(58.1799818944376,-21.5006430239275,-177.23826171807));
#158787=CARTESIAN_POINT('Ctrl Pts',(60.,-21.48000002,-174.47822483969));
#158788=CARTESIAN_POINT('Ctrl Pts',(60.,-21.4803505539985,-174.525420140524));
#158789=CARTESIAN_POINT('Ctrl Pts',(60.0001399779557,-21.4809879986116,
-174.619372716533));
#158790=CARTESIAN_POINT('Ctrl Pts',(59.9796633935931,-21.4825721374009,
-174.834540579974));
#158791=CARTESIAN_POINT('Ctrl Pts',(59.9691516993081,-21.4832061865197,
-174.91866280707));
#158792=CARTESIAN_POINT('Ctrl Pts',(59.9428873533568,-21.4843111756952,
-175.063261197871));
#158793=CARTESIAN_POINT('Ctrl Pts',(59.9323654277428,-21.4847047157807,
-175.114519734261));
#158794=CARTESIAN_POINT('Ctrl Pts',(59.9131593178258,-21.4853260452443,
-175.195833730679));
#158795=CARTESIAN_POINT('Ctrl Pts',(59.9026989428284,-21.4856443826443,
-175.237595425077));
#158796=CARTESIAN_POINT('Ctrl Pts',(59.8888111932657,-21.4860267073919,
-175.288192398583));
#158797=CARTESIAN_POINT('Ctrl Pts',(59.8814224077432,-21.4862202024632,
-175.313950381331));
#158798=CARTESIAN_POINT('Ctrl Pts',(59.8781578694836,-21.4863035832901,
-175.325086930002));
#158799=CARTESIAN_POINT('Ctrl Pts',(59.875959462847,-21.4863592661649,-175.332532820678));
#158800=CARTESIAN_POINT('Ctrl Pts',(59.8745119134935,-21.4863955582652,
-175.337392867869));
#158801=CARTESIAN_POINT('Ctrl Pts',(59.8235471264794,-21.4876651097968,
-175.507567331279));
#158802=CARTESIAN_POINT('Ctrl Pts',(59.7625865562566,-21.4888125164959,
-175.657773599687));
#158803=CARTESIAN_POINT('Ctrl Pts',(59.6668100439519,-21.4902869942187,
-175.855173103668));
#158804=CARTESIAN_POINT('Ctrl Pts',(59.6341488192349,-21.4907398771631,
-175.916376608615));
#158805=CARTESIAN_POINT('Ctrl Pts',(59.5853331656683,-21.4913676068731,
-176.001447175398));
#158806=CARTESIAN_POINT('Ctrl Pts',(59.5609666819441,-21.491668721715,-176.042302052764));
#158807=CARTESIAN_POINT('Ctrl Pts',(59.5328610248443,-21.4920003992658,
-176.087088941708));
#158808=CARTESIAN_POINT('Ctrl Pts',(59.5189174770905,-21.4921617429715,
-176.108772671461));
#158809=CARTESIAN_POINT('Ctrl Pts',(59.5129681152444,-21.4922299719197,
-176.117914660496));
#158810=CARTESIAN_POINT('Ctrl Pts',(59.5090080803609,-21.4922752589613,
-176.123975875479));
#158811=CARTESIAN_POINT('Ctrl Pts',(59.5078278775364,-21.4922887416491,
-176.125779857974));
#158812=CARTESIAN_POINT('Ctrl Pts',(59.3277545680046,-21.4943367985525,
-176.399243062079));
#158813=CARTESIAN_POINT('Ctrl Pts',(59.112894255709,-21.4961971427573,-176.62948927359));
#158814=CARTESIAN_POINT('Ctrl Pts',(58.6562287443494,-21.4989602174682,
-176.998436545936));
#158815=CARTESIAN_POINT('Ctrl Pts',(58.4150195201894,-21.4998854333264,
-177.137642938512));
#158816=CARTESIAN_POINT('Ctrl Pts',(58.1799818947148,-21.5006430233981,
-177.238261718413));
#158817=CARTESIAN_POINT('',(58.2408314794355,-21.0009616714991,-177.234172657581));
#158818=CARTESIAN_POINT('Origin',(-8.61422153796722,-13.0251077027817,-187.988562411664));
#158819=CARTESIAN_POINT('',(60.,-20.98000002,-174.500886972636));
#158820=CARTESIAN_POINT('Ctrl Pts',(58.2408309122627,-21.0009616140329,
-177.234171411));
#158821=CARTESIAN_POINT('Ctrl Pts',(58.2980225092941,-21.0007609899858,
-177.208159469229));
#158822=CARTESIAN_POINT('Ctrl Pts',(58.3554746487018,-21.0005425919237,
-177.179810838538));
#158823=CARTESIAN_POINT('Ctrl Pts',(58.4129879890245,-21.0003055852495,
-177.149025012205));
#158824=CARTESIAN_POINT('Ctrl Pts',(58.4687033405938,-21.0000759879055,
-177.119201615964));
#158825=CARTESIAN_POINT('Ctrl Pts',(58.5244764048851,-20.999828925583,-177.087090811604));
#158826=CARTESIAN_POINT('Ctrl Pts',(58.5800794173198,-20.9995636500946,
-177.052602282868));
#158827=CARTESIAN_POINT('Ctrl Pts',(58.63402128412,-20.9993062997384,-177.019144102425));
#158828=CARTESIAN_POINT('Ctrl Pts',(58.6878033716843,-20.9990318066526,
-176.983447946087));
#158829=CARTESIAN_POINT('Ctrl Pts',(58.7411692944488,-20.9987395210302,
-176.945435343265));
#158830=CARTESIAN_POINT('Ctrl Pts',(58.7924353414766,-20.9984587364454,
-176.908918484136));
#158831=CARTESIAN_POINT('Ctrl Pts',(58.8433174795946,-20.9981615307026,
-176.870263722897));
#158832=CARTESIAN_POINT('Ctrl Pts',(58.8935402105985,-20.9978473791949,
-176.829407837885));
#158833=CARTESIAN_POINT('Ctrl Pts',(58.9036719315393,-20.9977840036009,
-176.821165744764));
#158834=CARTESIAN_POINT('Ctrl Pts',(58.9137766493985,-20.9977199385699,
-176.812834097921));
#158835=CARTESIAN_POINT('Ctrl Pts',(58.9238518425652,-20.9976551801365,
-176.804412420825));
#158836=CARTESIAN_POINT('Ctrl Pts',(58.9326728926055,-20.9975984827241,
-176.797039059952));
#158837=CARTESIAN_POINT('Ctrl Pts',(58.9414695595589,-20.9975412674908,
-176.789598141511));
#158838=CARTESIAN_POINT('Ctrl Pts',(58.9502388844965,-20.997483541128,-176.782090523443));
#158839=CARTESIAN_POINT('Ctrl Pts',(58.9984162702457,-20.9971664009531,
-176.74084477029));
#158840=CARTESIAN_POINT('Ctrl Pts',(59.0459429298583,-20.9968333060902,
-176.697517295804));
#158841=CARTESIAN_POINT('Ctrl Pts',(59.0925361026031,-20.9964844704348,
-176.652133568374));
#158842=CARTESIAN_POINT('Ctrl Pts',(59.1264706681046,-20.9962304077535,
-176.619079861566));
#158843=CARTESIAN_POINT('Ctrl Pts',(59.159910744717,-20.9959680013015,-176.58493618398));
#158844=CARTESIAN_POINT('Ctrl Pts',(59.1927590407498,-20.9956974369349,
-176.549725798655));
#158845=CARTESIAN_POINT('Ctrl Pts',(59.2141973373912,-20.9955208542851,
-176.526745894775));
#158846=CARTESIAN_POINT('Ctrl Pts',(59.2353825316704,-20.9953408095841,
-176.503313294377));
#158847=CARTESIAN_POINT('Ctrl Pts',(59.256294110943,-20.995157339527,-176.479432519626));
#158848=CARTESIAN_POINT('Ctrl Pts',(59.2962851015841,-20.9948064741407,
-176.433763284073));
#158849=CARTESIAN_POINT('Ctrl Pts',(59.3352429768689,-20.9944429709512,
-176.38644039433));
#158850=CARTESIAN_POINT('Ctrl Pts',(59.3730217009492,-20.9940675205211,
-176.337552001638));
#158851=CARTESIAN_POINT('Ctrl Pts',(59.3981850918781,-20.9938174430985,
-176.304988759571));
#158852=CARTESIAN_POINT('Ctrl Pts',(59.422824079193,-20.9935620676181,-176.271731280423));
#158853=CARTESIAN_POINT('Ctrl Pts',(59.4468837816017,-20.9933015806725,
-176.237803245043));
#158854=CARTESIAN_POINT('Ctrl Pts',(59.458913632806,-20.9931713371996,-176.220839227352));
#158855=CARTESIAN_POINT('Ctrl Pts',(59.4707984783363,-20.9930398159737,
-176.203707584064));
#158856=CARTESIAN_POINT('Ctrl Pts',(59.4825305150169,-20.9929070384393,
-176.186411021836));
#158857=CARTESIAN_POINT('Ctrl Pts',(59.4883965333572,-20.9928406496721,
-176.177762740722));
#158858=CARTESIAN_POINT('Ctrl Pts',(59.4942243293403,-20.9927739469164,
-176.16907324131));
#158859=CARTESIAN_POINT('Ctrl Pts',(59.5000128525514,-20.9927069328473,
-176.160342860609));
#158860=CARTESIAN_POINT('Ctrl Pts',(59.5029071141569,-20.9926734258127,
-176.155977670259));
#158861=CARTESIAN_POINT('Ctrl Pts',(59.5057915568634,-20.9926398409485,
-176.151602259423));
#158862=CARTESIAN_POINT('Ctrl Pts',(59.5086660442441,-20.9926061785915,
-176.147216670479));
#158863=CARTESIAN_POINT('Ctrl Pts',(59.5101859584498,-20.9925883792806,
-176.144897746075));
#158864=CARTESIAN_POINT('Ctrl Pts',(59.5117030892688,-20.992570558303,-176.142575975924));
#158865=CARTESIAN_POINT('Ctrl Pts',(59.5132174161754,-20.9925527157083,
-176.140251366253));
#158866=CARTESIAN_POINT('Ctrl Pts',(59.5136029453564,-20.9925481732011,
-176.139659548952));
#158867=CARTESIAN_POINT('Ctrl Pts',(59.5139882928002,-20.9925436292928,
-176.139067547608));
#158868=CARTESIAN_POINT('Ctrl Pts',(59.5143734581649,-20.9925390839842,
-176.138475362326));
#158869=CARTESIAN_POINT('Ctrl Pts',(59.5146391908111,-20.9925359480924,
-176.138066802843));
#158870=CARTESIAN_POINT('Ctrl Pts',(59.5149048367898,-20.9925328115342,
-176.137658155807));
#158871=CARTESIAN_POINT('Ctrl Pts',(59.5151703959885,-20.9925296743097,
-176.137249421253));
#158872=CARTESIAN_POINT('Ctrl Pts',(59.5154011012622,-20.9925269488374,
-176.136894332001));
#158873=CARTESIAN_POINT('Ctrl Pts',(59.5156369697105,-20.9925241610901,
-176.13653112869));
#158874=CARTESIAN_POINT('Ctrl Pts',(59.5158771919828,-20.9925213204693,
-176.136161036115));
#158875=CARTESIAN_POINT('Ctrl Pts',(59.5163626876872,-20.9925155794979,
-176.135413069019));
#158876=CARTESIAN_POINT('Ctrl Pts',(59.5168650831917,-20.9925096329291,
-176.13463831307));
#158877=CARTESIAN_POINT('Ctrl Pts',(59.5173723671556,-20.9925036221267,
-176.133855185661));
#158878=CARTESIAN_POINT('Ctrl Pts',(59.5189847061201,-20.992484517539,-176.131366112625));
#158879=CARTESIAN_POINT('Ctrl Pts',(59.5206462689632,-20.9924647590044,
-176.128791809003));
#158880=CARTESIAN_POINT('Ctrl Pts',(59.521976211733,-20.9924489032738,-176.126725977334));
#158881=CARTESIAN_POINT('Ctrl Pts',(59.5223775029386,-20.9924441190339,
-176.126102642179));
#158882=CARTESIAN_POINT('Ctrl Pts',(59.5227486471359,-20.9924396903121,
-176.125525625579));
#158883=CARTESIAN_POINT('Ctrl Pts',(59.5230792754666,-20.9924357426811,
-176.125011289112));
#158884=CARTESIAN_POINT('Ctrl Pts',(59.5232128115734,-20.9924341482888,
-176.124803555886));
#158885=CARTESIAN_POINT('Ctrl Pts',(59.5233389910641,-20.9924326413239,
-176.124607213406));
#158886=CARTESIAN_POINT('Ctrl Pts',(59.5234673634073,-20.992431107786,-176.124407408557));
#158887=CARTESIAN_POINT('Ctrl Pts',(59.5564258070327,-20.9920373857261,
-176.073109311956));
#158888=CARTESIAN_POINT('Ctrl Pts',(59.5902891109346,-20.9916067368321,
-176.016989055202));
#158889=CARTESIAN_POINT('Ctrl Pts',(59.624130621386,-20.9911378554161,-175.955869202696));
#158890=CARTESIAN_POINT('Ctrl Pts',(59.6410513766116,-20.9909034147081,
-175.925309276443));
#158891=CARTESIAN_POINT('Ctrl Pts',(59.6579660208221,-20.9906594132553,
-175.893499084123));
#158892=CARTESIAN_POINT('Ctrl Pts',(59.6747556984726,-20.9904056762572,
-175.860414770979));
#158893=CARTESIAN_POINT('Ctrl Pts',(59.6835884223126,-20.9902721901427,
-175.843009755379));
#158894=CARTESIAN_POINT('Ctrl Pts',(59.6923865345141,-20.9901360095157,
-175.82525209878));
#158895=CARTESIAN_POINT('Ctrl Pts',(59.7011325951197,-20.9899971084505,
-175.807138253296));
#158896=CARTESIAN_POINT('Ctrl Pts',(59.7083460854132,-20.9898825469889,
-175.792198493047));
#158897=CARTESIAN_POINT('Ctrl Pts',(59.7155249023031,-20.9897661213385,
-175.777014659413));
#158898=CARTESIAN_POINT('Ctrl Pts',(59.7226512817366,-20.98964795287,-175.761602485893));
#158899=CARTESIAN_POINT('Ctrl Pts',(59.7233086393773,-20.9896370526721,
-175.760180822885));
#158900=CARTESIAN_POINT('Ctrl Pts',(59.7239655678023,-20.9896261373806,
-175.758757182504));
#158901=CARTESIAN_POINT('Ctrl Pts',(59.7246220603473,-20.9896152069761,
-175.757331562141));
#158902=CARTESIAN_POINT('Ctrl Pts',(59.7426945533578,-20.9893143053719,
-175.718085855172));
#158903=CARTESIAN_POINT('Ctrl Pts',(59.7604642712953,-20.9890011177224,
-175.677230878131));
#158904=CARTESIAN_POINT('Ctrl Pts',(59.7777374148834,-20.9886761769839,
-175.63483458625));
#158905=CARTESIAN_POINT('Ctrl Pts',(59.786590310033,-20.9885096371603,-175.613105482637));
#158906=CARTESIAN_POINT('Ctrl Pts',(59.7953115318292,-20.9883400331687,
-175.590974522494));
#158907=CARTESIAN_POINT('Ctrl Pts',(59.803875922402,-20.988167406105,-175.568446835027));
#158908=CARTESIAN_POINT('Ctrl Pts',(59.8214736860823,-20.98781269899,-175.522157853114));
#158909=CARTESIAN_POINT('Ctrl Pts',(59.8384192713474,-20.9874450703999,
-175.474173290825));
#158910=CARTESIAN_POINT('Ctrl Pts',(59.8544690713476,-20.9870649116206,
-175.424541860454));
#158911=CARTESIAN_POINT('Ctrl Pts',(59.8619224947127,-20.986888368341,-175.401493345036));
#158912=CARTESIAN_POINT('Ctrl Pts',(59.8691821364436,-20.9867091261014,
-175.378090090578));
#158913=CARTESIAN_POINT('Ctrl Pts',(59.8762202767283,-20.9865272376599,
-175.35433870977));
#158914=CARTESIAN_POINT('Ctrl Pts',(59.8764969529595,-20.986520087446,-175.353405019581));
#158915=CARTESIAN_POINT('Ctrl Pts',(59.8767260835289,-20.9865141545933,
-175.352630294314));
#158916=CARTESIAN_POINT('Ctrl Pts',(59.8769595354051,-20.986508101865,-175.351839913648));
#158917=CARTESIAN_POINT('Ctrl Pts',(59.8773656835597,-20.9864975716242,
-175.350464848027));
#158918=CARTESIAN_POINT('Ctrl Pts',(59.8777854130835,-20.9864866791224,
-175.349042476302));
#158919=CARTESIAN_POINT('Ctrl Pts',(59.8784867712533,-20.9864683764864,
-175.346652423526));
#158920=CARTESIAN_POINT('Ctrl Pts',(59.8951524677523,-20.9860334686325,
-175.289859908819));
#158921=CARTESIAN_POINT('Ctrl Pts',(59.9092622647949,-20.9856141796718,
-175.235700841717));
#158922=CARTESIAN_POINT('Ctrl Pts',(59.9213105226927,-20.9852134475942,
-175.184255041104));
#158923=CARTESIAN_POINT('Ctrl Pts',(59.9333080963485,-20.9848144013041,
-175.133025661109));
#158924=CARTESIAN_POINT('Ctrl Pts',(59.9432614521596,-20.9844337557669,
-175.084486756453));
#158925=CARTESIAN_POINT('Ctrl Pts',(59.9516078878375,-20.984074329303,-175.038707777574));
#158926=CARTESIAN_POINT('Ctrl Pts',(59.9599375046911,-20.9837156271159,
-174.993021047486));
#158927=CARTESIAN_POINT('Ctrl Pts',(59.9666666937355,-20.9833780582865,
-174.950083123863));
#158928=CARTESIAN_POINT('Ctrl Pts',(59.9721790686904,-20.9830643460922,
-174.909953824021));
#158929=CARTESIAN_POINT('Ctrl Pts',(59.9776790706391,-20.9827513380522,
-174.869914597891));
#158930=CARTESIAN_POINT('Ctrl Pts',(59.9819677270108,-20.9824620793983,
-174.832671393466));
#158931=CARTESIAN_POINT('Ctrl Pts',(59.9853749488932,-20.9821992015194,
-174.798274559429));
#158932=CARTESIAN_POINT('Ctrl Pts',(59.9862696517874,-20.9821301723786,
-174.789242289731));
#158933=CARTESIAN_POINT('Ctrl Pts',(59.9871033020603,-20.9820629619045,
-174.780406239223));
#158934=CARTESIAN_POINT('Ctrl Pts',(59.9878812857174,-20.9819976169342,
-174.771767216616));
#158935=CARTESIAN_POINT('Ctrl Pts',(59.9907884757324,-20.9817534341119,
-174.739484687239));
#158936=CARTESIAN_POINT('Ctrl Pts',(59.9929279440318,-20.9815324672645,
-174.709892376057));
#158937=CARTESIAN_POINT('Ctrl Pts',(59.9945472810677,-20.9813332116831,
-174.682970861426));
#158938=CARTESIAN_POINT('Ctrl Pts',(59.996197019977,-20.9811302152234,-174.655543914966));
#158939=CARTESIAN_POINT('Ctrl Pts',(59.9973068774898,-20.9809497528969,
-174.630888979004));
#158940=CARTESIAN_POINT('Ctrl Pts',(59.9980852070704,-20.9807901713966,
-174.608976344373));
#158941=CARTESIAN_POINT('Ctrl Pts',(59.9988728010901,-20.9806286904015,
-174.586802884156));
#158942=CARTESIAN_POINT('Ctrl Pts',(59.9993208127642,-20.9804885902046,
-174.567437372749));
#158943=CARTESIAN_POINT('Ctrl Pts',(59.9995921509242,-20.9803680953684,
-174.550840012396));
#158944=CARTESIAN_POINT('Ctrl Pts',(59.9998684942221,-20.9802453778693,
-174.533936495053));
#158945=CARTESIAN_POINT('Ctrl Pts',(59.9999615061132,-20.9801429956864,
-174.519904176989));
#158946=CARTESIAN_POINT('Ctrl Pts',(59.9999900624123,-20.9800590094608,
-174.50869202207));
#158947=CARTESIAN_POINT('Ctrl Pts',(59.9999971274817,-20.9800382305599,
-174.505918040328));
#158948=CARTESIAN_POINT('Ctrl Pts',(60.,-20.9800185773921,-174.503316641764));
#158949=CARTESIAN_POINT('Ctrl Pts',(60.,-20.98000002,-174.500886972636));
#158950=CARTESIAN_POINT('Ctrl Pts',(60.,-21.48000002,-174.47822483969));
#158951=CARTESIAN_POINT('Ctrl Pts',(60.,-21.3133292808184,-174.485664661366));
#158952=CARTESIAN_POINT('Ctrl Pts',(60.,-21.1466632268706,-174.493235890728));
#158953=CARTESIAN_POINT('Ctrl Pts',(60.,-20.98000002,-174.500886972636));
#158954=CARTESIAN_POINT('Origin',(39.,46.91999998,-129.34995));
#158955=CARTESIAN_POINT('',(39.0000000011086,-28.13000002,-134.169022080262));
#158956=CARTESIAN_POINT('',(39.,-22.48000002,-130.903539806302));
#158957=CARTESIAN_POINT('Ctrl Pts',(39.0000000022172,-28.13000002,-134.169022080262));
#158958=CARTESIAN_POINT('Ctrl Pts',(39.0000000027011,-27.7992138900219,
-133.93790810089));
#158959=CARTESIAN_POINT('Ctrl Pts',(39.0000000021338,-27.4657185053507,
-133.711655036841));
#158960=CARTESIAN_POINT('Ctrl Pts',(39.0000000015399,-27.1287626917287,
-133.490292823798));
#158961=CARTESIAN_POINT('Ctrl Pts',(39.0000000009697,-26.8052287127266,
-133.277748048811));
#158962=CARTESIAN_POINT('Ctrl Pts',(39.0000000004972,-26.4785047877952,
-133.069711931569));
#158963=CARTESIAN_POINT('Ctrl Pts',(39.0000000003364,-26.1478973077855,
-132.866246059588));
#158964=CARTESIAN_POINT('Ctrl Pts',(39.0000000002123,-25.8927164902428,
-132.709200043712));
#158965=CARTESIAN_POINT('Ctrl Pts',(39.0000000001809,-25.6361572010218,
-132.555471936139));
#158966=CARTESIAN_POINT('Ctrl Pts',(39.0000000003918,-25.3779449003587,
-132.405146018542));
#158967=CARTESIAN_POINT('Ctrl Pts',(39.0000000007921,-24.8877366470251,
-132.119756804679));
#158968=CARTESIAN_POINT('Ctrl Pts',(39.000000000553,-24.3912688192582,-131.84632373554));
#158969=CARTESIAN_POINT('Ctrl Pts',(39.0000000002964,-23.8878019342404,
-131.586247706167));
#158970=CARTESIAN_POINT('Ctrl Pts',(39.0000000000603,-23.4246527701181,
-131.346998613135));
#158971=CARTESIAN_POINT('Ctrl Pts',(39.0000000000002,-22.9555805746395,
-131.119053182003));
#158972=CARTESIAN_POINT('Ctrl Pts',(39.,-22.48000002,-130.903539806302));
#158973=CARTESIAN_POINT('',(39.,-22.48000002,-101.155103165204));
#158974=CARTESIAN_POINT('',(39.,-22.48000002,-129.34995));
#158975=CARTESIAN_POINT('',(39.,-28.13000002,-97.8896208912436));
#158976=CARTESIAN_POINT('Ctrl Pts',(39.,-22.48000002,-101.155103165204));
#158977=CARTESIAN_POINT('Ctrl Pts',(39.0000000000003,-23.0421399014191,
-100.900364693921));
#158978=CARTESIAN_POINT('Ctrl Pts',(39.0000000001808,-23.5949958654216,
-100.628353151271));
#158979=CARTESIAN_POINT('Ctrl Pts',(39.0000000005377,-24.1395638864455,
-100.340934396652));
#158980=CARTESIAN_POINT('Ctrl Pts',(39.0000000008113,-24.5569439995021,
-100.120644427969));
#158981=CARTESIAN_POINT('Ctrl Pts',(39.0000000009101,-24.9694552602945,
-99.8913025435709));
#158982=CARTESIAN_POINT('Ctrl Pts',(39.0000000004916,-25.3775420853185,
-99.6537285981461));
#158983=CARTESIAN_POINT('Ctrl Pts',(39.0000000002285,-25.6341396980635,
-99.5043463992897));
#158984=CARTESIAN_POINT('Ctrl Pts',(39.0000000001306,-25.8888446969123,
-99.35177201821));
#158985=CARTESIAN_POINT('Ctrl Pts',(39.0000000000752,-26.1419870362595,
-99.1960691366333));
#158986=CARTESIAN_POINT('Ctrl Pts',(39.0000000000073,-26.4522179455436,
-99.0052521968269));
#158987=CARTESIAN_POINT('Ctrl Pts',(39.0000000000056,-26.7601021070994,
-98.8096624723066));
#158988=CARTESIAN_POINT('Ctrl Pts',(39.0000000000023,-27.0653588164942,
-98.6099244013));
#158989=CARTESIAN_POINT('Ctrl Pts',(38.9999999999992,-27.3493059604978,
-98.4241297797058));
#158990=CARTESIAN_POINT('Ctrl Pts',(39.0000000000001,-27.6309803020602,
-98.2347441815217));
#158991=CARTESIAN_POINT('Ctrl Pts',(39.0000000000002,-27.9101240577928,
-98.0422452092007));
#158992=CARTESIAN_POINT('Ctrl Pts',(39.0000000000002,-27.9835605023139,
-97.9916030586567));
#158993=CARTESIAN_POINT('Ctrl Pts',(39.0000000000002,-28.0568495646841,
-97.9407287002963));
#158994=CARTESIAN_POINT('Ctrl Pts',(39.0000000000003,-28.13000002,-97.8896208912436));
#158995=CARTESIAN_POINT('',(39.,-28.13000002,-129.34995));
#158996=CARTESIAN_POINT('Ctrl Pts',(39.,-29.6092937616716,-135.247171188664));
#158997=CARTESIAN_POINT('Ctrl Pts',(38.9999999999999,-28.7416759820709,
-136.390803950004));
#158998=CARTESIAN_POINT('Ctrl Pts',(39.7614953849933,-28.006195589491,-137.360262497367));
#158999=CARTESIAN_POINT('Ctrl Pts',(39.,-28.4992718278429,-134.405052285569));
#159000=CARTESIAN_POINT('Ctrl Pts',(38.9999999999855,-27.6876355340531,
-135.545932666416));
#159001=CARTESIAN_POINT('Ctrl Pts',(39.7261148635016,-26.9897399838167,
-136.518160398014));
#159002=CARTESIAN_POINT('Ctrl Pts',(39.,-27.350294560115,-133.606110521891));
#159003=CARTESIAN_POINT('Ctrl Pts',(39.,-26.5955422649145,-134.742448815396));
#159004=CARTESIAN_POINT('Ctrl Pts',(39.6916499750401,-25.9410827372237,
-135.719201830687));
#159005=CARTESIAN_POINT('Ctrl Pts',(39.,-24.9455608509554,-132.126282804037));
#159006=CARTESIAN_POINT('Ctrl Pts',(38.9999999999999,-24.3121967691435,
-133.254719568795));
#159007=CARTESIAN_POINT('Ctrl Pts',(39.6264336205064,-23.7540596888349,
-134.239374112649));
#159008=CARTESIAN_POINT('Ctrl Pts',(39.,-23.7105874730482,-131.458602080542));
#159009=CARTESIAN_POINT('Ctrl Pts',(38.9999999999854,-23.1403713306369,
-132.582946581795));
#159010=CARTESIAN_POINT('Ctrl Pts',(39.5962661790751,-22.6346054925691,
-133.57169567032));
#159011=CARTESIAN_POINT('Ctrl Pts',(39.,-22.4346253623973,-130.883024754454));
#159012=CARTESIAN_POINT('Ctrl Pts',(39.,-21.9292251340083,-132.003415558585));
#159013=CARTESIAN_POINT('Ctrl Pts',(39.5698471421185,-21.4814250807741,
-132.996116063158));
#159014=CARTESIAN_POINT('',(39.5912209089345,-22.3752378108182,-133.464034181247));
#159015=CARTESIAN_POINT('',(39.7602371761935,-27.9700233746923,-137.330324614952));
#159016=CARTESIAN_POINT('Ctrl Pts',(39.5912176877287,-22.3752677013603,
-133.463979745435));
#159017=CARTESIAN_POINT('Ctrl Pts',(39.5991937056478,-22.6956823003948,
-133.639446472636));
#159018=CARTESIAN_POINT('Ctrl Pts',(39.607504589464,-23.0161431501768,-133.823227767823));
#159019=CARTESIAN_POINT('Ctrl Pts',(39.6161482430768,-23.3372484672009,
-134.015540725654));
#159020=CARTESIAN_POINT('Ctrl Pts',(39.625740246586,-23.6935842790838,-134.228953554191));
#159021=CARTESIAN_POINT('Ctrl Pts',(39.6357421466937,-24.050713523311,-134.452873202772));
#159022=CARTESIAN_POINT('Ctrl Pts',(39.6461511970428,-24.4094330557747,
-134.687659604986));
#159023=CARTESIAN_POINT('Ctrl Pts',(39.6503809255142,-24.5551991121233,
-134.78306530453));
#159024=CARTESIAN_POINT('Ctrl Pts',(39.6546778750575,-24.7012275599844,
-134.880265972657));
#159025=CARTESIAN_POINT('Ctrl Pts',(39.6590417977732,-24.8475712130293,
-134.979287971668));
#159026=CARTESIAN_POINT('Ctrl Pts',(39.6744840567571,-25.3654256156315,
-135.32968907944));
#159027=CARTESIAN_POINT('Ctrl Pts',(39.6906347977313,-25.8829878852576,
-135.699934267346));
#159028=CARTESIAN_POINT('Ctrl Pts',(39.7075008936637,-26.402609425732,-136.091336282031));
#159029=CARTESIAN_POINT('Ctrl Pts',(39.7200778526961,-26.7900884756006,
-136.383202705867));
#159030=CARTESIAN_POINT('Ctrl Pts',(39.7330525286025,-27.1787101201886,
-136.686837180687));
#159031=CARTESIAN_POINT('Ctrl Pts',(39.7464218716113,-27.5694625249137,
-137.00277640538));
#159032=CARTESIAN_POINT('Ctrl Pts',(39.7509812362623,-27.7027213320365,
-137.110521575203));
#159033=CARTESIAN_POINT('Ctrl Pts',(39.755586444335,-27.8362282160821,-137.219697552064));
#159034=CARTESIAN_POINT('Ctrl Pts',(39.7602371757582,-27.9700234449751,
-137.330324487883));
#159035=CARTESIAN_POINT('Ctrl Pts',(39.5912176308748,-22.3752654174111,
-133.46397849469));
#159036=CARTESIAN_POINT('Ctrl Pts',(39.5704459682015,-22.3771166985369,
-133.421559237108));
#159037=CARTESIAN_POINT('Ctrl Pts',(39.5485259522618,-22.3791109149648,
-133.375464310273));
#159038=CARTESIAN_POINT('Ctrl Pts',(39.5257329435558,-22.3812642489227,
-133.325575012736));
#159039=CARTESIAN_POINT('Ctrl Pts',(39.5072761806346,-22.3830079228213,
-133.285176882378));
#159040=CARTESIAN_POINT('Ctrl Pts',(39.4882478794602,-22.3848559043229,
-133.242290536397));
#159041=CARTESIAN_POINT('Ctrl Pts',(39.4688188799045,-22.3868120470417,
-133.196854321189));
#159042=CARTESIAN_POINT('Ctrl Pts',(39.4471075484527,-22.3889979785824,
-133.146080696666));
#159043=CARTESIAN_POINT('Ctrl Pts',(39.4248951791589,-22.3913193770836,
-133.09212240113));
#159044=CARTESIAN_POINT('Ctrl Pts',(39.4024537571075,-22.3937724613011,
-133.034900572149));
#159045=CARTESIAN_POINT('Ctrl Pts',(39.3912330460818,-22.3949990034098,
-133.006289657658));
#159046=CARTESIAN_POINT('Ctrl Pts',(39.3799556321572,-22.3962582955159,
-132.976863015288));
#159047=CARTESIAN_POINT('Ctrl Pts',(39.3686588779053,-22.3975486744013,
-132.946612030522));
#159048=CARTESIAN_POINT('Ctrl Pts',(39.3630105007794,-22.3981938638439,
-132.931486538139));
#159049=CARTESIAN_POINT('Ctrl Pts',(39.3573573118174,-22.3988468290841,
-132.916154951723));
#159050=CARTESIAN_POINT('Ctrl Pts',(39.3517042042225,-22.3995072548015,
-132.900616324401));
#159051=CARTESIAN_POINT('Ctrl Pts',(39.3488776504251,-22.3998374676602,
-132.892847010739));
#159052=CARTESIAN_POINT('Ctrl Pts',(39.3460511183112,-22.4001695458829,
-132.88502593635));
#159053=CARTESIAN_POINT('Ctrl Pts',(39.3432252304613,-22.4005034472795,
-132.877152986039));
#159054=CARTESIAN_POINT('Ctrl Pts',(39.3418122865364,-22.4006703979778,
-132.873216510883));
#159055=CARTESIAN_POINT('Ctrl Pts',(39.3403995037615,-22.4008378044838,
-132.869267066718));
#159056=CARTESIAN_POINT('Ctrl Pts',(39.3389869607814,-22.4010056611205,
-132.865304639651));
#159057=CARTESIAN_POINT('Ctrl Pts',(39.3375744178012,-22.4011735177572,
-132.861342212583));
#159058=CARTESIAN_POINT('Ctrl Pts',(39.3367132897538,-22.4012759517441,
-132.858923697129));
#159059=CARTESIAN_POINT('Ctrl Pts',(39.3347501303002,-22.4015105756498,
-132.853378395947));
#159060=CARTESIAN_POINT('Ctrl Pts',(39.3150826350157,-22.4038611053285,
-132.79782397593));
#159061=CARTESIAN_POINT('Ctrl Pts',(39.2975369800321,-22.4060800233942,
-132.745592029857));
#159062=CARTESIAN_POINT('Ctrl Pts',(39.281813765163,-22.4081460611799,-132.696818181293));
#159063=CARTESIAN_POINT('Ctrl Pts',(39.2659071443645,-22.4102361985906,
-132.647475402449));
#159064=CARTESIAN_POINT('Ctrl Pts',(39.2518653111442,-22.4121701620292,
-132.601671421479));
#159065=CARTESIAN_POINT('Ctrl Pts',(39.2394145627136,-22.4139389110504,
-132.559509824754));
#159066=CARTESIAN_POINT('Ctrl Pts',(39.2268139559692,-22.4157289488919,
-132.516840767305));
#159067=CARTESIAN_POINT('Ctrl Pts',(39.2158426385727,-22.4173500443747,
-132.477901869192));
#159068=CARTESIAN_POINT('Ctrl Pts',(39.2062595192933,-22.418801719556,-132.442769697218));
#159069=CARTESIAN_POINT('Ctrl Pts',(39.1966374578557,-22.4202592937941,
-132.407494761436));
#159070=CARTESIAN_POINT('Ctrl Pts',(39.1884147146853,-22.4215463105877,
-132.376057135563));
#159071=CARTESIAN_POINT('Ctrl Pts',(39.1813937185977,-22.4226672718763,
-132.348509965414));
#159072=CARTESIAN_POINT('Ctrl Pts',(39.174347612458,-22.4237922421966,-132.320864274931));
#159073=CARTESIAN_POINT('Ctrl Pts',(39.1685117471268,-22.424750159556,-132.297136577662));
#159074=CARTESIAN_POINT('Ctrl Pts',(39.1637353846615,-22.4255473035123,
-132.277361832726));
#159075=CARTESIAN_POINT('Ctrl Pts',(39.1614455703549,-22.4259294586877,
-132.267881711778));
#159076=CARTESIAN_POINT('Ctrl Pts',(39.1593999930064,-22.4262746704984,
-132.259309852597));
#159077=CARTESIAN_POINT('Ctrl Pts',(39.1575861139129,-22.4265835945122,
-132.251648900436));
#159078=CARTESIAN_POINT('Ctrl Pts',(39.1561218222149,-22.4268329798601,
-132.245464437157));
#159079=CARTESIAN_POINT('Ctrl Pts',(39.1548085749677,-22.42705871667,-132.239873584309));
#159080=CARTESIAN_POINT('Ctrl Pts',(39.153641039373,-22.4272611070789,-132.234877417562));
#159081=CARTESIAN_POINT('Ctrl Pts',(39.1530572715757,-22.4273623022833,
-132.232379334188));
#159082=CARTESIAN_POINT('Ctrl Pts',(39.1525099491287,-22.427457662781,-132.23002991835));
#159083=CARTESIAN_POINT('Ctrl Pts',(39.1519985118524,-22.42754721861,-132.227829279993));
#159084=CARTESIAN_POINT('Ctrl Pts',(39.1517427932143,-22.4275919965244,
-132.226728960814));
#159085=CARTESIAN_POINT('Ctrl Pts',(39.1514960469557,-22.4276353233905,
-132.225665835756));
#159086=CARTESIAN_POINT('Ctrl Pts',(39.1512582096618,-22.4276772030782,
-132.224639917171));
#159087=CARTESIAN_POINT('Ctrl Pts',(39.1511392910149,-22.4276981429221,
-132.224126957879));
#159088=CARTESIAN_POINT('Ctrl Pts',(39.1510226000849,-22.427718720953,-132.223623300112));
#159089=CARTESIAN_POINT('Ctrl Pts',(39.1509092053933,-22.4277387590788,
-132.223133603284));
#159090=CARTESIAN_POINT('Ctrl Pts',(39.1507958107018,-22.4277587972047,
-132.222643906455));
#159091=CARTESIAN_POINT('Ctrl Pts',(39.1506832277566,-22.4277786733366,
-132.222158917573));
#159092=CARTESIAN_POINT('Ctrl Pts',(39.1502251980778,-22.42785987834,-132.22017626939));
#159093=CARTESIAN_POINT('Ctrl Pts',(39.1289904035728,-22.4316246377878,
-132.128258368202));
#159094=CARTESIAN_POINT('Ctrl Pts',(39.1105424377617,-22.435323922588,-132.038287095715));
#159095=CARTESIAN_POINT('Ctrl Pts',(39.0945601802243,-22.4389133364673,
-131.950468295162));
#159096=CARTESIAN_POINT('Ctrl Pts',(39.0782303612054,-22.4425808082807,
-131.860739724832));
#159097=CARTESIAN_POINT('Ctrl Pts',(39.0644740620208,-22.4461337419189,
-131.773258146502));
#159098=CARTESIAN_POINT('Ctrl Pts',(39.0529498734261,-22.4495490877257,
-131.688194391823));
#159099=CARTESIAN_POINT('Ctrl Pts',(39.0410276477678,-22.4530823970842,
-131.600192597137));
#159100=CARTESIAN_POINT('Ctrl Pts',(39.0314937928809,-22.4564686204929,
-131.514778400783));
#159101=CARTESIAN_POINT('Ctrl Pts',(39.0239807694142,-22.4597054491932,
-131.432091105995));
#159102=CARTESIAN_POINT('Ctrl Pts',(39.0163143777417,-22.4630083533707,
-131.347715861994));
#159103=CARTESIAN_POINT('Ctrl Pts',(39.0107516622859,-22.4661559629513,
-131.266179646715));
#159104=CARTESIAN_POINT('Ctrl Pts',(39.0069213198967,-22.4691661594339,
-131.187583251473));
#159105=CARTESIAN_POINT('Ctrl Pts',(39.0029761663714,-22.4722665839021,
-131.106630998577));
#159106=CARTESIAN_POINT('Ctrl Pts',(39.0008683301356,-22.475221500718,-131.02879708224));
#159107=CARTESIAN_POINT('Ctrl Pts',(39.0002198458126,-22.4780677464764,
-130.954147392188));
#159108=CARTESIAN_POINT('Ctrl Pts',(39.0000718620453,-22.4787172581995,
-130.937112373806));
#159109=CARTESIAN_POINT('Ctrl Pts',(39.0000000007212,-22.4793611705732,
-130.920243010183));
#159110=CARTESIAN_POINT('Ctrl Pts',(39.,-22.48000002,-130.903539806302));
#159111=CARTESIAN_POINT('Ctrl Pts',(39.0000000022172,-28.13000002,-134.169022080262));
#159112=CARTESIAN_POINT('Ctrl Pts',(39.0000022444212,-28.1256876822484,
-134.257859743399));
#159113=CARTESIAN_POINT('Ctrl Pts',(39.0017029362504,-28.1212246324348,
-134.349811093215));
#159114=CARTESIAN_POINT('Ctrl Pts',(39.0054625728427,-28.1165865787746,
-134.444817027622));
#159115=CARTESIAN_POINT('Ctrl Pts',(39.0069704165467,-28.1147264362214,
-134.48292020502));
#159116=CARTESIAN_POINT('Ctrl Pts',(39.0088097443042,-28.1128384071593,
-134.521514303064));
#159117=CARTESIAN_POINT('Ctrl Pts',(39.0110049637423,-28.1109220758294,
-134.560593760958));
#159118=CARTESIAN_POINT('Ctrl Pts',(39.0148393383217,-28.1075748331758,
-134.628853579237));
#159119=CARTESIAN_POINT('Ctrl Pts',(39.0197592533743,-28.104140802429,-134.698594823325));
#159120=CARTESIAN_POINT('Ctrl Pts',(39.0258989313664,-28.1006234906337,
-134.769779548678));
#159121=CARTESIAN_POINT('Ctrl Pts',(39.0289687703624,-28.0988648347361,
-134.805371911355));
#159122=CARTESIAN_POINT('Ctrl Pts',(39.0323436499559,-28.097085364818,-134.841325135559));
#159123=CARTESIAN_POINT('Ctrl Pts',(39.036040744954,-28.0952864067033,-134.877633224531));
#159124=CARTESIAN_POINT('Ctrl Pts',(39.0378892924531,-28.0943869276459,
-134.895787269017));
#159125=CARTESIAN_POINT('Ctrl Pts',(39.0398183990165,-28.0934825767865,
-134.914030029345));
#159126=CARTESIAN_POINT('Ctrl Pts',(39.0418302364931,-28.0925735524499,
-134.932360712653));
#159127=CARTESIAN_POINT('Ctrl Pts',(39.0428361552314,-28.0921190402817,
-134.941526054307));
#159128=CARTESIAN_POINT('Ctrl Pts',(39.0438627570247,-28.0916633597697,
-134.950713376669));
#159129=CARTESIAN_POINT('Ctrl Pts',(39.0449103145788,-28.0912065389918,
-134.959922576108));
#159130=CARTESIAN_POINT('Ctrl Pts',(39.0454340933558,-28.0909781286029,
-134.964527175827));
#159131=CARTESIAN_POINT('Ctrl Pts',(39.0459631110927,-28.090749433149,-134.969137244813));
#159132=CARTESIAN_POINT('Ctrl Pts',(39.0464974019454,-28.0905204563639,
-134.973752769806));
#159133=CARTESIAN_POINT('Ctrl Pts',(39.0470316927981,-28.0902914795789,
-134.9783682948));
#159134=CARTESIAN_POINT('Ctrl Pts',(39.0477179000727,-28.0900004456395,
-134.984234402956));
#159135=CARTESIAN_POINT('Ctrl Pts',(39.0481161280684,-28.0898326858219,
-134.987615699453));
#159136=CARTESIAN_POINT('Ctrl Pts',(39.0550934125024,-28.08689339482,-135.046858815623));
#159137=CARTESIAN_POINT('Ctrl Pts',(39.0632889714829,-28.0837723561849,
-135.109990104035));
#159138=CARTESIAN_POINT('Ctrl Pts',(39.0730296264029,-28.0804454103404,
-135.176965171389));
#159139=CARTESIAN_POINT('Ctrl Pts',(39.0824823950805,-28.0772167927854,
-135.241960782471));
#159140=CARTESIAN_POINT('Ctrl Pts',(39.0933906084473,-28.0737939047369,
-135.310576693437));
#159141=CARTESIAN_POINT('Ctrl Pts',(39.1060896137435,-28.0701698336421,
-135.382744720427));
#159142=CARTESIAN_POINT('Ctrl Pts',(39.1161545441063,-28.0672974808596,
-135.439943386712));
#159143=CARTESIAN_POINT('Ctrl Pts',(39.1273451751191,-28.0642989515184,
-135.499372979695));
#159144=CARTESIAN_POINT('Ctrl Pts',(39.1398433469704,-28.0611802471452,
-135.56098419753));
#159145=CARTESIAN_POINT('Ctrl Pts',(39.1472627659542,-28.0593288584215,
-135.597559101817));
#159146=CARTESIAN_POINT('Ctrl Pts',(39.1551432186097,-28.0574352910613,
-135.634902556301));
#159147=CARTESIAN_POINT('Ctrl Pts',(39.163524700022,-28.0555025618695,-135.673001567496));
#159148=CARTESIAN_POINT('Ctrl Pts',(39.1677154407281,-28.0545361972736,
-135.692051073094));
#159149=CARTESIAN_POINT('Ctrl Pts',(39.1720314685517,-28.0535600468933,
-135.711289461438));
#159150=CARTESIAN_POINT('Ctrl Pts',(39.176477895301,-28.052574648591,-135.730714871549));
#159151=CARTESIAN_POINT('Ctrl Pts',(39.1787011086756,-28.0520819494398,
-135.740427576604));
#159152=CARTESIAN_POINT('Ctrl Pts',(39.180956923569,-28.051586938574,-135.750187036735));
#159153=CARTESIAN_POINT('Ctrl Pts',(39.1832459874,-28.0510896896912,-135.759993010319));
#159154=CARTESIAN_POINT('Ctrl Pts',(39.1843905193155,-28.0508410652498,
-135.764895997111));
#159155=CARTESIAN_POINT('Ctrl Pts',(39.1855433635767,-28.0505918813225,
-135.769810612242));
#159156=CARTESIAN_POINT('Ctrl Pts',(39.1867046015345,-28.050342147721,-135.774736824644));
#159157=CARTESIAN_POINT('Ctrl Pts',(39.1872852205135,-28.0502172809202,
-135.777199930845));
#159158=CARTESIAN_POINT('Ctrl Pts',(39.1878679379234,-28.050092276702,-135.779665936363));
#159159=CARTESIAN_POINT('Ctrl Pts',(39.1884527639581,-28.0499671363333,
-135.782134837256));
#159160=CARTESIAN_POINT('Ctrl Pts',(39.1890375899928,-28.0498419959645,
-135.784603738149));
#159161=CARTESIAN_POINT('Ctrl Pts',(39.1893301170433,-28.0497793997691,
-135.7858386911));
#159162=CARTESIAN_POINT('Ctrl Pts',(39.1902135781519,-28.0495913080571,
-135.7895502221));
#159163=CARTESIAN_POINT('Ctrl Pts',(39.2059227393946,-28.0462467770936,
-135.855546380124));
#159164=CARTESIAN_POINT('Ctrl Pts',(39.221650020651,-28.0430713006495,-135.917319405468));
#159165=CARTESIAN_POINT('Ctrl Pts',(39.2370526053371,-28.0400995402759,
-135.974902972362));
#159166=CARTESIAN_POINT('Ctrl Pts',(39.2526423857115,-28.0370916625402,
-136.033186382538));
#159167=CARTESIAN_POINT('Ctrl Pts',(39.267899310265,-28.034292087431,-136.087178424114));
#159168=CARTESIAN_POINT('Ctrl Pts',(39.2825152847821,-28.0317169129634,
-136.136928250427));
#159169=CARTESIAN_POINT('Ctrl Pts',(39.2973176181395,-28.0291089041111,
-136.187312404608));
#159170=CARTESIAN_POINT('Ctrl Pts',(39.311462418526,-28.0267306714006,-136.233345984635));
#159171=CARTESIAN_POINT('Ctrl Pts',(39.324680631343,-28.024584655685,-136.275086526027));
#159172=CARTESIAN_POINT('Ctrl Pts',(39.3379570787827,-28.0224291854071,
-136.317010961014));
#159173=CARTESIAN_POINT('Ctrl Pts',(39.3502987596337,-28.020507625517,-136.354604895132));
#159174=CARTESIAN_POINT('Ctrl Pts',(39.3614850041212,-28.0188137834241,
-136.387925840271));
#159175=CARTESIAN_POINT('Ctrl Pts',(39.3727121720073,-28.0171137446335,
-136.421368685688));
#159176=CARTESIAN_POINT('Ctrl Pts',(39.3827754798058,-28.0156427969912,
-136.450507583106));
#159177=CARTESIAN_POINT('Ctrl Pts',(39.3915036402467,-28.0143909018923,
-136.475393771548));
#159178=CARTESIAN_POINT('Ctrl Pts',(39.3940272651179,-28.0140289340264,
-136.482589263029));
#159179=CARTESIAN_POINT('Ctrl Pts',(39.3964395993417,-28.0136852698651,
-136.489429167449));
#159180=CARTESIAN_POINT('Ctrl Pts',(39.3987372963114,-28.0133596580246,
-136.495914555584));
#159181=CARTESIAN_POINT('Ctrl Pts',(39.405657219105,-28.0123790200961,-136.515446454598));
#159182=CARTESIAN_POINT('Ctrl Pts',(39.4115352343368,-28.0115620234741,
-136.531763419977));
#159183=CARTESIAN_POINT('Ctrl Pts',(39.4162991112997,-28.010902423024,-136.544889594268));
#159184=CARTESIAN_POINT('Ctrl Pts',(39.4186810497811,-28.010572622799,-136.551452681414));
#159185=CARTESIAN_POINT('Ctrl Pts',(39.420784901807,-28.0102821911499,-136.557217945173));
#159186=CARTESIAN_POINT('Ctrl Pts',(39.4226043068137,-28.010030508285,-136.562187596028));
#159187=CARTESIAN_POINT('Ctrl Pts',(39.423514009317,-28.0099046668525,-136.564672421456));
#159188=CARTESIAN_POINT('Ctrl Pts',(39.4243526262731,-28.0097885194934,
-136.5669583344));
#159189=CARTESIAN_POINT('Ctrl Pts',(39.4251195294557,-28.0096819964926,
-136.56904555736));
#159190=CARTESIAN_POINT('Ctrl Pts',(39.425502981047,-28.0096287349923,-136.57008916884));
#159191=CARTESIAN_POINT('Ctrl Pts',(39.4258685058372,-28.0095778800107,
-136.571083107247));
#159192=CARTESIAN_POINT('Ctrl Pts',(39.4262160353219,-28.0095294246206,
-136.572027396811));
#159193=CARTESIAN_POINT('Ctrl Pts',(39.4263898000642,-28.0095051969255,
-136.572499541593));
#159194=CARTESIAN_POINT('Ctrl Pts',(39.4265590665073,-28.0094815691999,
-136.572959273977));
#159195=CARTESIAN_POINT('Ctrl Pts',(39.4267215489531,-28.0094588375901,
-136.573400400812));
#159196=CARTESIAN_POINT('Ctrl Pts',(39.4268840313989,-28.0094361059803,
-136.573841527647));
#159197=CARTESIAN_POINT('Ctrl Pts',(39.4270438833707,-28.0094136336851,
-136.574276585042));
#159198=CARTESIAN_POINT('Ctrl Pts',(39.4278967242282,-28.009294249711,-136.576588215794));
#159199=CARTESIAN_POINT('Ctrl Pts',(39.4596149084087,-28.0048542151545,
-136.662560562586));
#159200=CARTESIAN_POINT('Ctrl Pts',(39.4919257606152,-28.0005742974956,
-136.744743249651));
#159201=CARTESIAN_POINT('Ctrl Pts',(39.5244183422418,-27.9964886368414,
-136.82314195696));
#159202=CARTESIAN_POINT('Ctrl Pts',(39.557501220046,-27.9923287515567,-136.902964941902));
#159203=CARTESIAN_POINT('Ctrl Pts',(39.5907720426126,-27.9883699287563,
-136.978865697753));
#159204=CARTESIAN_POINT('Ctrl Pts',(39.6238294631346,-27.9846169757305,
-137.050881414756));
#159205=CARTESIAN_POINT('Ctrl Pts',(39.6577842812835,-27.9807621426705,
-137.124852115921));
#159206=CARTESIAN_POINT('Ctrl Pts',(39.6915135537608,-27.9771241573282,
-137.194724506443));
#159207=CARTESIAN_POINT('Ctrl Pts',(39.7246228724876,-27.973680678008,-137.260563754943));
#159208=CARTESIAN_POINT('Ctrl Pts',(39.7365804986175,-27.972437045101,-137.284341988641));
#159209=CARTESIAN_POINT('Ctrl Pts',(39.7484576652078,-27.9712185539927,
-137.307594356029));
#159210=CARTESIAN_POINT('Ctrl Pts',(39.7602371757582,-27.9700234449751,
-137.330324487883));
#159211=CARTESIAN_POINT('Origin',(0.,-12.9675000200281,-171.64995));
#159212=CARTESIAN_POINT('',(56.4351108624337,-28.0132652467914,-171.449026400902));
#159213=CARTESIAN_POINT('',(57.638503474757,-22.4067641070473,-171.449026400902));
#159214=CARTESIAN_POINT('Origin',(0.,-12.9675000200281,-171.449026400902));
#159215=CARTESIAN_POINT('Ctrl Pts',(57.638503474757,-22.4067641070473,-171.449026400902));
#159216=CARTESIAN_POINT('Ctrl Pts',(56.0174734274339,-22.4047732541902,
-168.017725527675));
#159217=CARTESIAN_POINT('Ctrl Pts',(54.4570351795732,-22.4027901572724,
-164.718389532589));
#159218=CARTESIAN_POINT('Ctrl Pts',(52.2072906835069,-22.399520061464,-159.96733285717));
#159219=CARTESIAN_POINT('Ctrl Pts',(51.4725275267282,-22.3983876189532,
-158.416638518232));
#159220=CARTESIAN_POINT('Ctrl Pts',(50.3931082416263,-22.3966483219777,
-156.140083839128));
#159221=CARTESIAN_POINT('Ctrl Pts',(49.8590798993526,-22.3957691535144,
-155.014178206902));
#159222=CARTESIAN_POINT('Ctrl Pts',(49.2459879385832,-22.3947385586366,
-153.722272123792));
#159223=CARTESIAN_POINT('Ctrl Pts',(48.9419270289921,-22.3942240082935,
-153.081731704191));
#159224=CARTESIAN_POINT('Ctrl Pts',(48.7715916624419,-22.3939350767465,
-152.722950018091));
#159225=CARTESIAN_POINT('Ctrl Pts',(48.6879979444904,-22.3937931129051,
-152.546890421963));
#159226=CARTESIAN_POINT('Ctrl Pts',(48.6449082650321,-22.3937199051624,
-152.456141770449));
#159227=CARTESIAN_POINT('Ctrl Pts',(48.6427494969204,-22.3937162374209,
-152.451595325367));
#159228=CARTESIAN_POINT('Ctrl Pts',(45.3353322790861,-22.3880967559532,
-145.486078532289));
#159229=CARTESIAN_POINT('Ctrl Pts',(42.3192392814167,-22.3819993338137,
-139.159156692962));
#159230=CARTESIAN_POINT('Ctrl Pts',(39.5912209089345,-22.3752378108182,
-133.464034181247));
#159231=CARTESIAN_POINT('Ctrl Pts',(39.7602371906927,-27.9700232578782,
-137.330324735012));
#159232=CARTESIAN_POINT('Ctrl Pts',(41.0440760495002,-27.9745032276897,
-139.909644963587));
#159233=CARTESIAN_POINT('Ctrl Pts',(42.3849915594275,-27.9790517553505,
-142.618821730253));
#159234=CARTESIAN_POINT('Ctrl Pts',(44.4821817835909,-27.9852985070288,
-146.877371687389));
#159235=CARTESIAN_POINT('Ctrl Pts',(45.1955448675102,-27.987298498321,-148.329352474291));
#159236=CARTESIAN_POINT('Ctrl Pts',(46.2870402618014,-27.9902150737621,
-150.556019856428));
#159237=CARTESIAN_POINT('Ctrl Pts',(46.8381504361392,-27.9916538177842,
-151.681527597942));
#159238=CARTESIAN_POINT('Ctrl Pts',(47.4904948539634,-27.9933207698379,
-153.015924551323));
#159239=CARTESIAN_POINT('Ctrl Pts',(47.8190123404997,-27.9941552160743,
-153.688449175084));
#159240=CARTESIAN_POINT('Ctrl Pts',(48.0015193211533,-27.9946179773477,
-154.06221379323));
#159241=CARTESIAN_POINT('Ctrl Pts',(48.0900254381751,-27.9948422372974,
-154.243513467762));
#159242=CARTESIAN_POINT('Ctrl Pts',(48.137277552473,-27.9949619482672,-154.34031758891));
#159243=CARTESIAN_POINT('Ctrl Pts',(48.144080578613,-27.9949791830011,-154.354255016688));
#159244=CARTESIAN_POINT('Ctrl Pts',(50.7155543787194,-28.0014936334107,
-159.622532560907));
#159245=CARTESIAN_POINT('Ctrl Pts',(53.477513591401,-28.0075945743212,-165.317366506688));
#159246=CARTESIAN_POINT('Ctrl Pts',(56.4351108624337,-28.0132652467914,
-171.449026400902));
#159247=CARTESIAN_POINT('Origin',(60.,-29.13000002,-176.84995));
#159248=CARTESIAN_POINT('',(56.7430488584365,-29.13000002,-177.34995));
#159249=CARTESIAN_POINT('',(57.,-29.13000002,-177.34995));
#159250=CARTESIAN_POINT('',(60.,-29.13000002,-177.34995));
#159251=CARTESIAN_POINT('',(57.,-28.664523125878,-177.032518510534));
#159252=CARTESIAN_POINT('Ctrl Pts',(56.7430488584365,-29.13000002,-177.34995));
#159253=CARTESIAN_POINT('Ctrl Pts',(56.7774215329782,-29.0696624994766,
-177.34995));
#159254=CARTESIAN_POINT('Ctrl Pts',(56.8073315614797,-29.0157589594499,
-177.339097737931));
#159255=CARTESIAN_POINT('Ctrl Pts',(56.8455026351718,-28.947352143821,-177.316017469029));
#159256=CARTESIAN_POINT('Ctrl Pts',(56.8571106648925,-28.9265627510565,
-177.30717515183));
#159257=CARTESIAN_POINT('Ctrl Pts',(56.8728492172084,-28.8983280728031,
-177.293163830275));
#159258=CARTESIAN_POINT('Ctrl Pts',(56.8803001203001,-28.8849448328683,
-177.285968499567));
#159259=CARTESIAN_POINT('Ctrl Pts',(56.8882606877078,-28.8705728009652,
-177.277425887854));
#159260=CARTESIAN_POINT('Ctrl Pts',(56.8915154695541,-28.8646735743065,
-177.273750819397));
#159261=CARTESIAN_POINT('Ctrl Pts',(56.8936504596961,-28.8607979147461,
-177.271299598116));
#159262=CARTESIAN_POINT('Ctrl Pts',(56.8941472201129,-28.8598965492813,
-177.270730233962));
#159263=CARTESIAN_POINT('Ctrl Pts',(56.9464830121473,-28.7645629228455,
-177.208602031531));
#159264=CARTESIAN_POINT('Ctrl Pts',(56.9812386277457,-28.6996278422223,
-177.122021537563));
#159265=CARTESIAN_POINT('Ctrl Pts',(57.,-28.664523125878,-177.032518510534));
#159266=CARTESIAN_POINT('Origin',(57.,-29.13000002,-176.84995));
#159267=CARTESIAN_POINT('Origin',(60.,-2.55003103885676E-14,0.));
#159268=CARTESIAN_POINT('',(60.,-29.13000002,-58.24995));
#159269=CARTESIAN_POINT('',(60.,-29.63000002,-58.24995));
#159270=CARTESIAN_POINT('',(60.,-54.58000002,-58.24995));
#159271=CARTESIAN_POINT('',(60.,-29.63000002,-174.34995));
#159272=CARTESIAN_POINT('',(60.,-29.63000002,-174.34995));
#159273=CARTESIAN_POINT('',(60.,-29.13000002,-174.34995));
#159274=CARTESIAN_POINT('',(60.,28.41999998,-174.34995));
#159275=CARTESIAN_POINT('',(60.,-29.13000002,-58.24995));
#159276=CARTESIAN_POINT('Origin',(57.,-2.42462934179819E-14,-174.34995));
#159277=CARTESIAN_POINT('',(57.,-29.63000002,-177.34995));
#159278=CARTESIAN_POINT('Origin',(57.,-29.63000002,-174.34995));
#159279=CARTESIAN_POINT('',(57.,-54.58000002,-177.34995));
#159280=CARTESIAN_POINT('Origin',(57.,-29.13000002,-174.34995));
#159281=CARTESIAN_POINT('Origin',(60.,28.41999998,-177.34995));
#159282=CARTESIAN_POINT('',(56.5982428503831,-29.63000002,-177.34995));
#159283=CARTESIAN_POINT('',(60.,-29.63000002,-177.34995));
#159284=CARTESIAN_POINT('Origin',(0.,-12.9675000200281,-177.34995));
#159285=CARTESIAN_POINT('Origin',(57.,-2.42462934179819E-14,-174.34995));
#159286=CARTESIAN_POINT('',(60.,-37.78000002,-174.34995));
#159287=CARTESIAN_POINT('',(60.,-37.28000002,-174.34995));
#159288=CARTESIAN_POINT('',(60.,28.41999998,-174.34995));
#159289=CARTESIAN_POINT('',(57.,-37.78000002,-177.34995));
#159290=CARTESIAN_POINT('Origin',(57.,-37.78000002,-174.34995));
#159291=CARTESIAN_POINT('',(57.,-37.28000002,-177.34995));
#159292=CARTESIAN_POINT('',(57.,-54.58000002,-177.34995));
#159293=CARTESIAN_POINT('Origin',(57.,-37.28000002,-174.34995));
#159294=CARTESIAN_POINT('Origin',(39.,46.91999998,-129.34995));
#159295=CARTESIAN_POINT('',(39.,-30.63000002,-96.0164973302555));
#159296=CARTESIAN_POINT('',(39.0000000003234,-36.28000002,-90.9091273827666));
#159297=CARTESIAN_POINT('Ctrl Pts',(39.,-30.63000002,-96.0164973302555));
#159298=CARTESIAN_POINT('Ctrl Pts',(39.0000000000004,-31.0448154973607,
-95.6851069386958));
#159299=CARTESIAN_POINT('Ctrl Pts',(39.0000000000118,-31.454211737686,-95.3480909235777));
#159300=CARTESIAN_POINT('Ctrl Pts',(39.0000000000377,-31.8588908811793,
-95.0057530542704));
#159301=CARTESIAN_POINT('Ctrl Pts',(39.0000000000646,-32.2780518714171,
-94.6511642828895));
#159302=CARTESIAN_POINT('Ctrl Pts',(39.0000000001072,-32.6921518967125,
-94.2908656551258));
#159303=CARTESIAN_POINT('Ctrl Pts',(39.0000000001713,-33.1019373671843,
-93.9251487646761));
#159304=CARTESIAN_POINT('Ctrl Pts',(39.0000000002394,-33.5373888366211,
-93.5365260124815));
#159305=CARTESIAN_POINT('Ctrl Pts',(39.0000000003318,-33.9679681800838,
-93.1417847771912));
#159306=CARTESIAN_POINT('Ctrl Pts',(39.0000000004578,-34.394536385264,-92.7412278681602));
#159307=CARTESIAN_POINT('Ctrl Pts',(39.0000000004786,-34.4649233358098,
-92.6751329764071));
#159308=CARTESIAN_POINT('Ctrl Pts',(39.0000000005003,-34.5352010051139,
-92.6088796459859));
#159309=CARTESIAN_POINT('Ctrl Pts',(39.000000000523,-34.605373184231,-92.5424691324455));
#159310=CARTESIAN_POINT('Ctrl Pts',(39.0000000006715,-35.0646606142243,
-92.1078023674648));
#159311=CARTESIAN_POINT('Ctrl Pts',(39.0000000008613,-35.5177770523147,
-91.6679502775283));
#159312=CARTESIAN_POINT('Ctrl Pts',(39.0000000011092,-35.965637218633,-91.2230746458943));
#159313=CARTESIAN_POINT('Ctrl Pts',(39.0000000011674,-36.0707105045093,
-91.1187015671131));
#159314=CARTESIAN_POINT('Ctrl Pts',(39.0000000012288,-36.1754942796337,
-91.0140518532023));
#159315=CARTESIAN_POINT('Ctrl Pts',(39.0000000012937,-36.28000002,-90.9091273827667));
#159316=CARTESIAN_POINT('',(39.000000000323,-36.28000002,-141.149515588739));
#159317=CARTESIAN_POINT('',(39.,-36.28000002,-129.34995));
#159318=CARTESIAN_POINT('',(39.,-30.63000002,-136.04214564125));
#159319=CARTESIAN_POINT('Ctrl Pts',(39.0000000012919,-36.28000002,-141.149515588739));
#159320=CARTESIAN_POINT('Ctrl Pts',(39.0000000010156,-35.8345332337807,
-140.702263921253));
#159321=CARTESIAN_POINT('Ctrl Pts',(39.0000000008023,-35.3840176213704,
-140.260002181405));
#159322=CARTESIAN_POINT('Ctrl Pts',(39.0000000006337,-34.9275493437281,
-139.822886348187));
#159323=CARTESIAN_POINT('Ctrl Pts',(39.0000000005941,-34.8204877683625,
-139.720363758965));
#159324=CARTESIAN_POINT('Ctrl Pts',(39.0000000005571,-34.7130985462057,
-139.618124369441));
#159325=CARTESIAN_POINT('Ctrl Pts',(39.0000000005223,-34.6053696556424,
-139.516170434427));
#159326=CARTESIAN_POINT('Ctrl Pts',(39.0000000003866,-34.1849244503587,
-139.118263773436));
#159327=CARTESIAN_POINT('Ctrl Pts',(39.0000000002855,-33.7606942182172,
-138.725996583523));
#159328=CARTESIAN_POINT('Ctrl Pts',(39.0000000002095,-33.3318521218407,
-138.339654688119));
#159329=CARTESIAN_POINT('Ctrl Pts',(39.0000000001368,-32.9217240241196,
-137.970172149043));
#159330=CARTESIAN_POINT('Ctrl Pts',(39.000000000087,-32.5073780350574,-137.606108713954));
#159331=CARTESIAN_POINT('Ctrl Pts',(39.0000000000541,-32.0880629354937,
-137.2477524174));
#159332=CARTESIAN_POINT('Ctrl Pts',(39.0000000000227,-31.6891890379909,
-136.906865640726));
#159333=CARTESIAN_POINT('Ctrl Pts',(39.0000000000065,-31.2858188263214,
-136.571142959571));
#159334=CARTESIAN_POINT('Ctrl Pts',(39.0000000000016,-30.8772772477696,
-136.240870924199));
#159335=CARTESIAN_POINT('Ctrl Pts',(39.0000000000006,-30.7950629151777,
-136.174407444378));
#159336=CARTESIAN_POINT('Ctrl Pts',(39.0000000000001,-30.7126390581746,
-136.108164834635));
#159337=CARTESIAN_POINT('Ctrl Pts',(39.,-30.63000002,-136.04214564125));
#159338=CARTESIAN_POINT('',(39.,-30.63000002,-129.34995));
#159339=CARTESIAN_POINT('Ctrl Pts',(39.,-38.3588510407228,-143.307942286761));
#159340=CARTESIAN_POINT('Ctrl Pts',(39.,-37.0899493427105,-144.4917610531));
#159341=CARTESIAN_POINT('Ctrl Pts',(40.0751063896396,-36.0938885093696,
-145.421033595465));
#159342=CARTESIAN_POINT('Ctrl Pts',(39.,-37.1517836400886,-142.014121037894));
#159343=CARTESIAN_POINT('Ctrl Pts',(39.,-35.9377773398718,-143.195151285356));
#159344=CARTESIAN_POINT('Ctrl Pts',(40.0284942517968,-34.9676084789312,
-144.127227814579));
#159345=CARTESIAN_POINT('Ctrl Pts',(39.,-35.9043030651865,-140.745333283629));
#159346=CARTESIAN_POINT('Ctrl Pts',(38.9999999999999,-34.7456377245003,
-141.920028658586));
#159347=CARTESIAN_POINT('Ctrl Pts',(39.98110816979,-33.8078877259523,-142.858424592381));
#159348=CARTESIAN_POINT('Ctrl Pts',(39.,-33.3065355961441,-138.286902604304));
#159349=CARTESIAN_POINT('Ctrl Pts',(39.,-32.2660355551645,-139.44936091542));
#159350=CARTESIAN_POINT('Ctrl Pts',(39.8860349079144,-31.4034486206149,
-140.399993912959));
#159351=CARTESIAN_POINT('Ctrl Pts',(39.,-31.969482004655,-137.109613636004));
#159352=CARTESIAN_POINT('Ctrl Pts',(39.,-30.9915363473202,-138.26565762591));
#159353=CARTESIAN_POINT('Ctrl Pts',(39.838820917574,-30.1709959811911,-139.222722930622));
#159354=CARTESIAN_POINT('Ctrl Pts',(39.,-30.5806161032665,-136.00274102598));
#159355=CARTESIAN_POINT('Ctrl Pts',(38.9999999999999,-29.666065684619,-137.150287618997));
#159356=CARTESIAN_POINT('Ctrl Pts',(39.7930043034378,-28.8965637495112,
-138.115832334683));
#159357=CARTESIAN_POINT('',(39.8501336360982,-30.4479678253697,-139.515614761957));
#159358=CARTESIAN_POINT('',(40.073447192122,-36.0537915982708,-145.374999599156));
#159359=CARTESIAN_POINT('Ctrl Pts',(39.8501516349467,-30.4480624613224,
-139.515559008888));
#159360=CARTESIAN_POINT('Ctrl Pts',(39.8682496030913,-30.928479243834,-139.964932207816));
#159361=CARTESIAN_POINT('Ctrl Pts',(39.8867711495951,-31.4107613119204,
-140.430651260819));
#159362=CARTESIAN_POINT('Ctrl Pts',(39.9057043691656,-31.8961926581865,
-140.913553018237));
#159363=CARTESIAN_POINT('Ctrl Pts',(39.9148973085922,-32.131891660429,-141.148023790015));
#159364=CARTESIAN_POINT('Ctrl Pts',(39.9241871517812,-32.3683334399629,
-141.386545178378));
#159365=CARTESIAN_POINT('Ctrl Pts',(39.9335715388522,-32.6056681732837,
-141.62920925267));
#159366=CARTESIAN_POINT('Ctrl Pts',(39.9498531623278,-33.0174366496215,
-142.050223971987));
#159367=CARTESIAN_POINT('Ctrl Pts',(39.9663641156002,-33.4304553032117,
-142.482261868868));
#159368=CARTESIAN_POINT('Ctrl Pts',(39.9831005766346,-33.8452748182043,
-142.925794853778));
#159369=CARTESIAN_POINT('Ctrl Pts',(39.9978992507961,-34.2120655528516,
-143.317974545175));
#159370=CARTESIAN_POINT('Ctrl Pts',(40.0128742075591,-34.5802637197622,
-143.719141833042));
#159371=CARTESIAN_POINT('Ctrl Pts',(40.028018889995,-34.950251571756,-144.129584741671));
#159372=CARTESIAN_POINT('Ctrl Pts',(40.0429991025759,-35.3162213897886,
-144.535570278154));
#159373=CARTESIAN_POINT('Ctrl Pts',(40.058145417947,-35.6839417083337,-144.950631978182));
#159374=CARTESIAN_POINT('Ctrl Pts',(40.0734472049714,-36.0537916893395,
-145.374999488024));
#159375=CARTESIAN_POINT('Ctrl Pts',(39.8501336360982,-30.4479678253697,
-139.515614761957));
#159376=CARTESIAN_POINT('Ctrl Pts',(39.8191622083133,-30.4511037081781,
-139.457491138984));
#159377=CARTESIAN_POINT('Ctrl Pts',(39.7879243927985,-30.4543702018603,
-139.396870134181));
#159378=CARTESIAN_POINT('Ctrl Pts',(39.7566167914735,-30.4577697087166,
-139.333684763231));
#159379=CARTESIAN_POINT('Ctrl Pts',(39.725300593464,-30.461170149036,-139.27048204235));
#159380=CARTESIAN_POINT('Ctrl Pts',(39.6939201493324,-30.4646865160787,
-139.204710898193));
#159381=CARTESIAN_POINT('Ctrl Pts',(39.6626726151794,-30.4683465195869,
-139.136305569412));
#159382=CARTESIAN_POINT('Ctrl Pts',(39.6314250810264,-30.472006523095,-139.067900240632));
#159383=CARTESIAN_POINT('Ctrl Pts',(39.6003118730321,-30.4758126014794,
-138.996864100184));
#159384=CARTESIAN_POINT('Ctrl Pts',(39.5695612146119,-30.4797609358057,
-138.923160316523));
#159385=CARTESIAN_POINT('Ctrl Pts',(39.5541858854018,-30.4817351029688,
-138.886308424692));
#159386=CARTESIAN_POINT('Ctrl Pts',(39.5389014254943,-30.4837445705845,
-138.848789863091));
#159387=CARTESIAN_POINT('Ctrl Pts',(39.5237375144895,-30.4857871269164,
-138.810601657135));
#159388=CARTESIAN_POINT('Ctrl Pts',(39.5161555589871,-30.4868084050824,
-138.791507554157));
#159389=CARTESIAN_POINT('Ctrl Pts',(39.5086037389925,-30.4878379536194,
-138.772246042189));
#159390=CARTESIAN_POINT('Ctrl Pts',(39.5010858288046,-30.4888753565829,
-138.752816883547));
#159391=CARTESIAN_POINT('Ctrl Pts',(39.4973268737106,-30.4893940580646,
-138.743102304227));
#159392=CARTESIAN_POINT('Ctrl Pts',(39.4935763957452,-30.4899147229967,
-138.733345813422));
#159393=CARTESIAN_POINT('Ctrl Pts',(39.4898348670455,-30.4904372946442,
-138.723547386211));
#159394=CARTESIAN_POINT('Ctrl Pts',(39.4879641026957,-30.4906985804679,
-138.718648172605));
#159395=CARTESIAN_POINT('Ctrl Pts',(39.486095575638,-30.4909603429601,-138.713738474911));
#159396=CARTESIAN_POINT('Ctrl Pts',(39.4842293450209,-30.491222574526,-138.708818290504));
#159397=CARTESIAN_POINT('Ctrl Pts',(39.4832962297124,-30.491353690309,-138.7063581983));
#159398=CARTESIAN_POINT('Ctrl Pts',(39.4823636885123,-30.4914849233598,
-138.70389548442));
#159399=CARTESIAN_POINT('Ctrl Pts',(39.4814317288226,-30.4916162726957,
-138.701430148567));
#159400=CARTESIAN_POINT('Ctrl Pts',(39.480499769133,-30.4917476220316,-138.698964812714));
#159401=CARTESIAN_POINT('Ctrl Pts',(39.4791346823167,-30.491940398823,-138.69534566852));
#159402=CARTESIAN_POINT('Ctrl Pts',(39.4786376016852,-30.4920106685648,
-138.694026274808));
#159403=CARTESIAN_POINT('Ctrl Pts',(39.4658888577959,-30.4938128931618,
-138.660187473907));
#159404=CARTESIAN_POINT('Ctrl Pts',(39.4517135693882,-30.4958331216217,
-138.621772379626));
#159405=CARTESIAN_POINT('Ctrl Pts',(39.436343196791,-30.4980914029818,-138.578720983754));
#159406=CARTESIAN_POINT('Ctrl Pts',(39.4206728558649,-30.5003937569811,
-138.534829396455));
#159407=CARTESIAN_POINT('Ctrl Pts',(39.4037603945031,-30.5029435136479,
-138.486118765703));
#159408=CARTESIAN_POINT('Ctrl Pts',(39.3859029566423,-30.5057633173538,
-138.432509027361));
#159409=CARTESIAN_POINT('Ctrl Pts',(39.3775676371762,-30.5070795176342,
-138.407485600201));
#159410=CARTESIAN_POINT('Ctrl Pts',(39.3690271533864,-30.5084545769865,
-138.381394552734));
#159411=CARTESIAN_POINT('Ctrl Pts',(39.3603153951006,-30.5098909286504,
-138.354226571495));
#159412=CARTESIAN_POINT('Ctrl Pts',(39.3401293576112,-30.5132191027784,
-138.291275572419));
#159413=CARTESIAN_POINT('Ctrl Pts',(39.3190231670336,-30.5168728189609,
-138.222549326763));
#159414=CARTESIAN_POINT('Ctrl Pts',(39.2974832707415,-30.5208429798159,
-138.147968464029));
#159415=CARTESIAN_POINT('Ctrl Pts',(39.2946500754201,-30.5213651847981,
-138.138158660467));
#159416=CARTESIAN_POINT('Ctrl Pts',(39.2918094470411,-30.5218928638335,
-138.128247546444));
#159417=CARTESIAN_POINT('Ctrl Pts',(39.2889625545045,-30.5224259954821,
-138.118234922939));
#159418=CARTESIAN_POINT('Ctrl Pts',(39.2767170922724,-30.5247191777443,
-138.075167191581));
#159419=CARTESIAN_POINT('Ctrl Pts',(39.2643559286661,-30.5271124131941,
-138.030222414249));
#159420=CARTESIAN_POINT('Ctrl Pts',(39.2519774397925,-30.5295977664338,
-137.983390722815));
#159421=CARTESIAN_POINT('Ctrl Pts',(39.2457881953557,-30.5308404430536,
-137.959974877098));
#159422=CARTESIAN_POINT('Ctrl Pts',(39.2395946713538,-30.5321061642718,
-137.936087285073));
#159423=CARTESIAN_POINT('Ctrl Pts',(39.2334097009524,-30.5333933219195,
-137.9117272282));
#159424=CARTESIAN_POINT('Ctrl Pts',(39.2285848334955,-30.534397427783,-137.89272405793));
#159425=CARTESIAN_POINT('Ctrl Pts',(39.2235931574876,-30.5354511329446,
-137.872738003284));
#159426=CARTESIAN_POINT('Ctrl Pts',(39.2188441690707,-30.5364681053083,
-137.853395850005));
#159427=CARTESIAN_POINT('Ctrl Pts',(39.2175054560001,-30.5367547840863,
-137.847943406003));
#159428=CARTESIAN_POINT('Ctrl Pts',(39.2161857199312,-30.5370385409,-137.842542224786));
#159429=CARTESIAN_POINT('Ctrl Pts',(39.2148934224204,-30.5373174350074,
-137.837228967863));
#159430=CARTESIAN_POINT('Ctrl Pts',(39.2146990458272,-30.5373593839286,
-137.836429792154));
#159431=CARTESIAN_POINT('Ctrl Pts',(39.214504847708,-30.5374013226796,-137.835630793376));
#159432=CARTESIAN_POINT('Ctrl Pts',(39.2143108278165,-30.5374432512608,
-137.834831971547));
#159433=CARTESIAN_POINT('Ctrl Pts',(39.1922239238158,-30.5422163316834,
-137.743895413848));
#159434=CARTESIAN_POINT('Ctrl Pts',(39.1724858756577,-30.5468621133865,
-137.655159254419));
#159435=CARTESIAN_POINT('Ctrl Pts',(39.1547975358758,-30.5513764763546,
-137.568736391554));
#159436=CARTESIAN_POINT('Ctrl Pts',(39.1364521564366,-30.5560585269369,
-137.479103320783));
#159437=CARTESIAN_POINT('Ctrl Pts',(39.1203114766778,-30.5605992305923,
-137.391958310255));
#159438=CARTESIAN_POINT('Ctrl Pts',(39.1060690480999,-30.5649963940464,
-137.307379213395));
#159439=CARTESIAN_POINT('Ctrl Pts',(39.1049881432084,-30.5653301092874,
-137.300960226703));
#159440=CARTESIAN_POINT('Ctrl Pts',(39.1039181848734,-30.5656629988024,
-137.29455599823));
#159441=CARTESIAN_POINT('Ctrl Pts',(39.102859045528,-30.5659950621301,-137.288166551949));
#159442=CARTESIAN_POINT('Ctrl Pts',(39.0868430811912,-30.5710164169082,
-137.191547401492));
#159443=CARTESIAN_POINT('Ctrl Pts',(39.0733000498566,-30.5758480119611,
-137.098324767538));
#159444=CARTESIAN_POINT('Ctrl Pts',(39.061819755875,-30.5804857187884,-137.008629087097));
#159445=CARTESIAN_POINT('Ctrl Pts',(39.0536432573057,-30.5837887877951,
-136.944746001525));
#159446=CARTESIAN_POINT('Ctrl Pts',(39.0465142325881,-30.586993461715,-136.882652782168));
#159447=CARTESIAN_POINT('Ctrl Pts',(39.0402963664581,-30.5900982170105,
-136.822396589877));
#159448=CARTESIAN_POINT('Ctrl Pts',(39.0363915886327,-30.5920479823123,
-136.784556109142));
#159449=CARTESIAN_POINT('Ctrl Pts',(39.0328458135265,-30.593958569049,-136.747435703989));
#159450=CARTESIAN_POINT('Ctrl Pts',(39.0296261138438,-30.5958302989186,
-136.711033325134));
#159451=CARTESIAN_POINT('Ctrl Pts',(39.0222574437438,-30.6001139779211,
-136.627722101395));
#159452=CARTESIAN_POINT('Ctrl Pts',(39.0165956522317,-30.6041933284833,
-136.548187569322));
#159453=CARTESIAN_POINT('Ctrl Pts',(39.01228209515,-30.6080685835929,-136.472473348208));
#159454=CARTESIAN_POINT('Ctrl Pts',(39.0077058481702,-30.6121798365926,
-136.392148231571));
#159455=CARTESIAN_POINT('Ctrl Pts',(39.004646624077,-30.6160614012094,-136.316122548143));
#159456=CARTESIAN_POINT('Ctrl Pts',(39.0027201584472,-30.6197156000662,
-136.244404502519));
#159457=CARTESIAN_POINT('Ctrl Pts',(39.0007936928175,-30.623369798923,-136.172686456895));
#159458=CARTESIAN_POINT('Ctrl Pts',(39.,-30.6267966711481,-136.105275326978));
#159459=CARTESIAN_POINT('Ctrl Pts',(39.,-30.63000002,-136.04214564125));
#159460=CARTESIAN_POINT('Ctrl Pts',(39.,-36.28000002,-141.149515588739));
#159461=CARTESIAN_POINT('Ctrl Pts',(39.0000026845439,-36.271636952727,-141.308381696112));
#159462=CARTESIAN_POINT('Ctrl Pts',(39.0041560645674,-36.2626979527457,
-141.479433937643));
#159463=CARTESIAN_POINT('Ctrl Pts',(39.0196751709712,-36.2481955286276,
-141.754045307826));
#159464=CARTESIAN_POINT('Ctrl Pts',(39.0264019740874,-36.2431828057576,
-141.848583729441));
#159465=CARTESIAN_POINT('Ctrl Pts',(39.0392524022158,-36.2354101945438,
-141.994816669982));
#159466=CARTESIAN_POINT('Ctrl Pts',(39.046368127812,-36.2314610334767,-142.06903892383));
#159467=CARTESIAN_POINT('Ctrl Pts',(39.0559766116434,-36.2267529476897,
-142.157543704131));
#159468=CARTESIAN_POINT('Ctrl Pts',(39.0611201501891,-36.2243753882432,
-142.202270756544));
#159469=CARTESIAN_POINT('Ctrl Pts',(39.0639681937629,-36.2230956375407,
-142.22635834997));
#159470=CARTESIAN_POINT('Ctrl Pts',(39.0653227137038,-36.2224968063035,
-142.237633644024));
#159471=CARTESIAN_POINT('Ctrl Pts',(39.0661029962005,-36.2221542283202,
-142.244085085566));
#159472=CARTESIAN_POINT('Ctrl Pts',(39.0664357352188,-36.2220086145544,
-142.246827511015));
#159473=CARTESIAN_POINT('Ctrl Pts',(39.0740430194889,-36.2186840002108,
-142.309443989598));
#159474=CARTESIAN_POINT('Ctrl Pts',(39.0887631405107,-36.2125697575084,
-142.430607476474));
#159475=CARTESIAN_POINT('Ctrl Pts',(39.1326226546473,-36.1982650817826,
-142.700184720785));
#159476=CARTESIAN_POINT('Ctrl Pts',(39.1509869144791,-36.1926373593803,
-142.804670073255));
#159477=CARTESIAN_POINT('Ctrl Pts',(39.1865588623926,-36.1829503810533,
-142.982962068645));
#159478=CARTESIAN_POINT('Ctrl Pts',(39.1997609500423,-36.179515996477,-143.0459837673));
#159479=CARTESIAN_POINT('Ctrl Pts',(39.2219443680061,-36.1740903581866,
-143.145821485805));
#159480=CARTESIAN_POINT('Ctrl Pts',(39.2336317728787,-36.1713093947294,
-143.197066214847));
#159481=CARTESIAN_POINT('Ctrl Pts',(39.2483952962438,-36.1679576185287,
-143.259149252828));
#159482=CARTESIAN_POINT('Ctrl Pts',(39.2560702744332,-36.1662567791381,
-143.290761895407));
#159483=CARTESIAN_POINT('Ctrl Pts',(39.259423588014,-36.1655227139119,-143.304432193872));
#159484=CARTESIAN_POINT('Ctrl Pts',(39.261673495937,-36.1650322209503,-143.313572801173));
#159485=CARTESIAN_POINT('Ctrl Pts',(39.2630923672526,-36.1647244206623,
-143.319313599113));
#159486=CARTESIAN_POINT('Ctrl Pts',(39.3185147861829,-36.1527413890172,
-143.542939666575));
#159487=CARTESIAN_POINT('Ctrl Pts',(39.376487191619,-36.1419772728173,-143.740335575647));
#159488=CARTESIAN_POINT('Ctrl Pts',(39.4618196356428,-36.1278685716875,
-144.002760783506));
#159489=CARTESIAN_POINT('Ctrl Pts',(39.4900070416244,-36.1234910906176,
-144.084635066894));
#159490=CARTESIAN_POINT('Ctrl Pts',(39.5312015397534,-36.117374661997,-144.199178928827));
#159491=CARTESIAN_POINT('Ctrl Pts',(39.5515286748293,-36.1144280945784,
-144.254384472605));
#159492=CARTESIAN_POINT('Ctrl Pts',(39.5746338810447,-36.111170400366,-144.315208007352));
#159493=CARTESIAN_POINT('Ctrl Pts',(39.5860181263649,-36.1095842181069,
-144.34472838493));
#159494=CARTESIAN_POINT('Ctrl Pts',(39.5908593359132,-36.1089133141243,
-144.35718942879));
#159495=CARTESIAN_POINT('Ctrl Pts',(39.5940782365116,-36.1084679908687,
-144.365454499774));
#159496=CARTESIAN_POINT('Ctrl Pts',(39.5949354491578,-36.1083494362718,
-144.367654752919));
#159497=CARTESIAN_POINT('Ctrl Pts',(39.7476034322303,-36.0872982613274,
-144.757746156936));
#159498=CARTESIAN_POINT('Ctrl Pts',(39.9115823286905,-36.0692299855258,
-145.090746526247));
#159499=CARTESIAN_POINT('Ctrl Pts',(40.0734471901674,-36.0537915266759,
-145.374999596381));
#159500=CARTESIAN_POINT('Origin',(0.,-12.9675000200281,-171.64995));
#159501=CARTESIAN_POINT('',(53.6298444656516,-36.1005191032365,-171.449026400902));
#159502=CARTESIAN_POINT('',(55.7146117108563,-30.4940179634924,-171.449026400902));
#159503=CARTESIAN_POINT('Origin',(0.,-12.9675000200281,-171.449026400902));
#159504=CARTESIAN_POINT('Ctrl Pts',(55.7146117108563,-30.4940179634924,
-171.449026400902));
#159505=CARTESIAN_POINT('Ctrl Pts',(54.8724055325709,-30.4921606112015,
-169.724950356757));
#159506=CARTESIAN_POINT('Ctrl Pts',(54.0458152036748,-30.4902665003795,
-168.036186540547));
#159507=CARTESIAN_POINT('Ctrl Pts',(53.234784597893,-30.4883339514173,-166.382763547322));
#159508=CARTESIAN_POINT('Ctrl Pts',(52.4060857875293,-30.4863593021075,
-164.693320932276));
#159509=CARTESIAN_POINT('Ctrl Pts',(51.5936324329536,-30.4843445334443,
-163.040775976074));
#159510=CARTESIAN_POINT('Ctrl Pts',(50.7974127390484,-30.482290227048,-161.425132437527));
#159511=CARTESIAN_POINT('Ctrl Pts',(49.9722431291296,-30.4801612277018,
-159.750745382452));
#159512=CARTESIAN_POINT('Ctrl Pts',(49.1645092733571,-30.4779897715322,
-158.115991828474));
#159513=CARTESIAN_POINT('Ctrl Pts',(48.3742448639459,-30.4757788795041,
-156.520846084462));
#159514=CARTESIAN_POINT('Ctrl Pts',(48.2015166730246,-30.4752956445566,
-156.17219487945));
#159515=CARTESIAN_POINT('Ctrl Pts',(48.0296232101336,-30.4748105340451,
-155.825435739396));
#159516=CARTESIAN_POINT('Ctrl Pts',(47.8585650914879,-30.4743235932024,
-155.480568209344));
#159517=CARTESIAN_POINT('Ctrl Pts',(47.8537746537233,-30.4743099565518,
-155.470910284583));
#159518=CARTESIAN_POINT('Ctrl Pts',(47.8497874336421,-30.4742986041782,
-155.462871822295));
#159519=CARTESIAN_POINT('Ctrl Pts',(47.8441957454454,-30.4742826727293,
-155.451598884702));
#159520=CARTESIAN_POINT('Ctrl Pts',(47.8440689808494,-30.4742823115604,
-155.451343325141));
#159521=CARTESIAN_POINT('Ctrl Pts',(47.8439422166437,-30.4742819503903,
-155.451087766482));
#159522=CARTESIAN_POINT('Ctrl Pts',(47.8438154528283,-30.4742815892191,
-155.450832208722));
#159523=CARTESIAN_POINT('Ctrl Pts',(47.1281154616227,-30.4722424406397,
-154.00797025836));
#159524=CARTESIAN_POINT('Ctrl Pts',(46.4248779163233,-30.4701660906363,
-152.59381081989));
#159525=CARTESIAN_POINT('Ctrl Pts',(45.7340209887441,-30.4680503695182,
-151.208391024834));
#159526=CARTESIAN_POINT('Ctrl Pts',(45.0434297046247,-30.4659354619224,
-149.823503941679));
#159527=CARTESIAN_POINT('Ctrl Pts',(44.3652099140242,-30.4637812311311,
-148.467334199979));
#159528=CARTESIAN_POINT('Ctrl Pts',(43.6993304940745,-30.4615877238109,
-147.139892688189));
#159529=CARTESIAN_POINT('Ctrl Pts',(43.0059147757672,-30.4593035077674,
-145.757557115364));
#159530=CARTESIAN_POINT('Ctrl Pts',(42.3258812524105,-30.4569767040243,
-144.406374866656));
#159531=CARTESIAN_POINT('Ctrl Pts',(41.6592463874673,-30.4546096167241,
-143.086331517643));
#159532=CARTESIAN_POINT('Ctrl Pts',(41.0448183892133,-30.4524279055834,
-141.869666090743));
#159533=CARTESIAN_POINT('Ctrl Pts',(40.4417734418195,-30.4502120095389,
-140.679452889206));
#159534=CARTESIAN_POINT('Ctrl Pts',(39.850159149164,-30.447965242174,-139.5156626415));
#159535=CARTESIAN_POINT('Ctrl Pts',(40.0734472163172,-36.0537915241817,
-145.374999642303));
#159536=CARTESIAN_POINT('Ctrl Pts',(41.1513629919691,-36.0583266065864,
-147.382840909586));
#159537=CARTESIAN_POINT('Ctrl Pts',(42.2612453872436,-36.0628720322864,
-149.46995218686));
#159538=CARTESIAN_POINT('Ctrl Pts',(43.9743253442819,-36.0693743353693,
-152.719524117757));
#159539=CARTESIAN_POINT('Ctrl Pts',(44.5533923517989,-36.0714955758215,
-153.822532263887));
#159540=CARTESIAN_POINT('Ctrl Pts',(45.4340727076594,-36.0746257587657,
-155.506770736829));
#159541=CARTESIAN_POINT('Ctrl Pts',(45.8774326678813,-36.0761785538904,
-156.356321536736));
#159542=CARTESIAN_POINT('Ctrl Pts',(46.3999730275242,-36.0779791102198,
-157.360469372642));
#159543=CARTESIAN_POINT('Ctrl Pts',(46.6625651604514,-36.0788784372191,
-157.865794599598));
#159544=CARTESIAN_POINT('Ctrl Pts',(46.8082945827096,-36.0793762814646,
-158.146428123263));
#159545=CARTESIAN_POINT('Ctrl Pts',(46.878919483461,-36.0796172170613,-158.282490689921));
#159546=CARTESIAN_POINT('Ctrl Pts',(46.9166136408414,-36.0797457363095,
-158.355125127742));
#159547=CARTESIAN_POINT('Ctrl Pts',(46.9218982679862,-36.0797637527598,
-158.36530862072));
#159548=CARTESIAN_POINT('Ctrl Pts',(49.0459171851673,-36.0870044798771,
-162.458404893256));
#159549=CARTESIAN_POINT('Ctrl Pts',(51.2803555380598,-36.0939327197443,
-166.816984571593));
#159550=CARTESIAN_POINT('Ctrl Pts',(53.6298444656516,-36.1005191032365,
-171.449026400902));
#159551=CARTESIAN_POINT('Origin',(60.,28.41999998,-177.34995));
#159552=CARTESIAN_POINT('',(53.5288692553037,-37.78000002,-177.34995));
#159553=CARTESIAN_POINT('',(60.,-37.78000002,-177.34995));
#159554=CARTESIAN_POINT('',(53.7578119323263,-37.28000002,-177.34995));
#159555=CARTESIAN_POINT('Origin',(0.,-12.9675000200281,-177.34995));
#159556=CARTESIAN_POINT('',(60.,-37.28000002,-177.34995));
#159557=CARTESIAN_POINT('Origin',(60.,-2.55003103885676E-14,0.));
#159558=CARTESIAN_POINT('',(60.,-37.28000002,-58.24995));
#159559=CARTESIAN_POINT('',(60.,-37.78000002,-58.24995));
#159560=CARTESIAN_POINT('',(60.,-54.58000002,-58.24995));
#159561=CARTESIAN_POINT('',(60.,-37.78000002,-174.34995));
#159562=CARTESIAN_POINT('',(60.,-37.28000002,-58.24995));
#159563=CARTESIAN_POINT('Origin',(60.,-2.55003103885676E-14,0.));
#159564=CARTESIAN_POINT('',(60.,11.61999998,-58.24995));
#159565=CARTESIAN_POINT('',(60.,11.11999998,-58.24995));
#159566=CARTESIAN_POINT('',(60.,-54.58000002,-58.24995));
#159567=CARTESIAN_POINT('',(60.,11.11999998,-174.34995));
#159568=CARTESIAN_POINT('',(60.,11.61999998,-58.24995));
#159569=CARTESIAN_POINT('Origin',(60.,-54.58000002,-55.24995));
#159570=CARTESIAN_POINT('',(17.55,-54.58000002,-141.176536909659));
#159571=CARTESIAN_POINT('',(23.2,-54.5800000202568,-146.023178055809));
#159572=CARTESIAN_POINT('Ctrl Pts',(17.55,-54.58000002,-141.176536909659));
#159573=CARTESIAN_POINT('Ctrl Pts',(17.9693769714657,-54.5800000200003,
-141.49343498957));
#159574=CARTESIAN_POINT('Ctrl Pts',(18.3834419174572,-54.5800000200088,
-141.816182952558));
#159575=CARTESIAN_POINT('Ctrl Pts',(18.7928766486286,-54.5800000200341,
-142.144468939261));
#159576=CARTESIAN_POINT('Ctrl Pts',(19.2164906824758,-54.5800000200604,
-142.484123933074));
#159577=CARTESIAN_POINT('Ctrl Pts',(19.635148044891,-54.5800000201049,-142.829707458926));
#159578=CARTESIAN_POINT('Ctrl Pts',(20.0495713966145,-54.5800000201721,
-143.180920598229));
#159579=CARTESIAN_POINT('Ctrl Pts',(20.4883260232375,-54.5800000202432,
-143.55275386766));
#159580=CARTESIAN_POINT('Ctrl Pts',(20.9223347029258,-54.58000002034,-143.930897445251));
#159581=CARTESIAN_POINT('Ctrl Pts',(21.3524219960725,-54.5800000204563,
-144.315043885241));
#159582=CARTESIAN_POINT('Ctrl Pts',(21.3910234228641,-54.5800000204667,
-144.349522003793));
#159583=CARTESIAN_POINT('Ctrl Pts',(21.4295932412572,-54.5800000204773,
-144.384048506598));
#159584=CARTESIAN_POINT('Ctrl Pts',(21.4681320362146,-54.580000020488,-144.418623187422));
#159585=CARTESIAN_POINT('Ctrl Pts',(21.9304021275721,-54.5800000206166,
-144.83334401305));
#159586=CARTESIAN_POINT('Ctrl Pts',(22.3865711849682,-54.5800000207665,
-145.253534976228));
#159587=CARTESIAN_POINT('Ctrl Pts',(22.8375326449957,-54.580000020912,-145.679007211413));
#159588=CARTESIAN_POINT('Ctrl Pts',(22.9587258346798,-54.5800000209511,
-145.793350324682));
#159589=CARTESIAN_POINT('Ctrl Pts',(23.0795426741296,-54.5800000209898,
-145.90807504421));
#159590=CARTESIAN_POINT('Ctrl Pts',(23.2,-54.5800000210274,-146.023178055809));
#159591=CARTESIAN_POINT('',(23.2,-54.58000002,-86.035464915697));
#159592=CARTESIAN_POINT('',(23.2,-54.58000002,-85.5535812563546));
#159593=CARTESIAN_POINT('',(17.55,-54.58000002,-90.8821060618472));
#159594=CARTESIAN_POINT('Ctrl Pts',(23.2,-54.5800000205323,-86.035464915697));
#159595=CARTESIAN_POINT('Ctrl Pts',(22.7416005580064,-54.5800000204569,
-86.473488555251));
#159596=CARTESIAN_POINT('Ctrl Pts',(22.2778852069184,-54.580000020382,-86.9061566638687));
#159597=CARTESIAN_POINT('Ctrl Pts',(21.8082168240834,-54.5800000203146,
-87.3329667340019));
#159598=CARTESIAN_POINT('Ctrl Pts',(21.6948114073334,-54.5800000202983,
-87.4360236474446));
#159599=CARTESIAN_POINT('Ctrl Pts',(21.5810587192868,-54.5800000202825,
-87.5387388946999));
#159600=CARTESIAN_POINT('Ctrl Pts',(21.4669494079305,-54.5800000202671,
-87.6411051232898));
#159601=CARTESIAN_POINT('Ctrl Pts',(21.0322856597372,-54.5800000202087,
-88.0310372688657));
#159602=CARTESIAN_POINT('Ctrl Pts',(20.5935852018712,-54.5800000201577,
-88.4149271477261));
#159603=CARTESIAN_POINT('Ctrl Pts',(20.150033972245,-54.580000020117,-88.7924150855438));
#159604=CARTESIAN_POINT('Ctrl Pts',(19.7265254012934,-54.5800000200782,
-89.152845553139));
#159605=CARTESIAN_POINT('Ctrl Pts',(19.2985947426908,-54.5800000200487,
-89.5074398670458));
#159606=CARTESIAN_POINT('Ctrl Pts',(18.8655062292501,-54.5800000200292,
-89.8558463488876));
#159607=CARTESIAN_POINT('Ctrl Pts',(18.4324177158094,-54.5800000200098,
-90.2042528307294));
#159608=CARTESIAN_POINT('Ctrl Pts',(17.994171750171,-54.5800000200003,-90.5464720515007));
#159609=CARTESIAN_POINT('Ctrl Pts',(17.55,-54.58000002,-90.8821060618472));
#159610=CARTESIAN_POINT('',(17.55,-54.58000002,-140.803447286915));
#159611=CARTESIAN_POINT('Origin',(-3.54807775957937E-14,-73.08000002,3.11172719585489E-30));
#159612=CARTESIAN_POINT('',(16.55,-73.08000002,-58.24995));
#159613=CARTESIAN_POINT('',(16.05,-73.08000002,-58.24995));
#159614=CARTESIAN_POINT('',(-41.5,-73.0800000199999,-58.24995));
#159615=CARTESIAN_POINT('',(16.05,-73.08000002,-174.34995));
#159616=CARTESIAN_POINT('',(16.05,-73.08000002,-174.34995));
#159617=CARTESIAN_POINT('',(16.55,-73.08000002,-174.34995));
#159618=CARTESIAN_POINT('',(41.5,-73.08000002,-174.34995));
#159619=CARTESIAN_POINT('',(16.55,-73.08000002,-58.24995));
#159620=CARTESIAN_POINT('Origin',(60.,-54.58000002,-55.24995));
#159621=CARTESIAN_POINT('',(9.4,-54.58000002,-136.338455187671));
#159622=CARTESIAN_POINT('',(15.05,-54.580000020336,-139.407335470919));
#159623=CARTESIAN_POINT('Ctrl Pts',(9.4,-54.58000002,-136.338455187671));
#159624=CARTESIAN_POINT('Ctrl Pts',(9.92110496058178,-54.5800000200001,
-136.559368584536));
#159625=CARTESIAN_POINT('Ctrl Pts',(10.4350703325194,-54.5800000200483,
-136.794854049275));
#159626=CARTESIAN_POINT('Ctrl Pts',(10.9425445776645,-54.5800000201757,
-137.04357763751));
#159627=CARTESIAN_POINT('Ctrl Pts',(11.3976304732205,-54.58000002029,-137.266624615718));
#159628=CARTESIAN_POINT('Ctrl Pts',(11.8474960215382,-54.5800000203574,
-137.500318485595));
#159629=CARTESIAN_POINT('Ctrl Pts',(12.2925996107723,-54.5800000201853,
-137.743731583458));
#159630=CARTESIAN_POINT('Ctrl Pts',(12.5336925965022,-54.5800000200921,
-137.875577724331));
#159631=CARTESIAN_POINT('Ctrl Pts',(12.7734820900616,-54.5800000201101,
-138.010349990831));
#159632=CARTESIAN_POINT('Ctrl Pts',(13.0121639376423,-54.5800000201839,
-138.147985687537));
#159633=CARTESIAN_POINT('Ctrl Pts',(13.3646805607937,-54.580000020293,-138.351264116624));
#159634=CARTESIAN_POINT('Ctrl Pts',(13.7130708435113,-54.5800000206454,
-138.559766344709));
#159635=CARTESIAN_POINT('Ctrl Pts',(14.0580847568665,-54.5800000210433,
-138.773390841178));
#159636=CARTESIAN_POINT('Ctrl Pts',(14.3916633624461,-54.580000021428,-138.979934864163));
#159637=CARTESIAN_POINT('Ctrl Pts',(14.7220850961464,-54.5800000217332,
-139.191268004987));
#159638=CARTESIAN_POINT('Ctrl Pts',(15.05,-54.5800000213439,-139.407335470919));
#159639=CARTESIAN_POINT('',(15.05,-54.5800000206722,-92.6513075005872));
#159640=CARTESIAN_POINT('',(15.05,-54.58000002,-92.3169104578858));
#159641=CARTESIAN_POINT('',(9.4,-54.58000002,-95.7201877838351));
#159642=CARTESIAN_POINT('Ctrl Pts',(15.05,-54.5800000213444,-92.6513075005872));
#159643=CARTESIAN_POINT('Ctrl Pts',(14.7116749748805,-54.5800000217462,
-92.8742343330664));
#159644=CARTESIAN_POINT('Ctrl Pts',(14.3706840440917,-54.5800000214065,
-93.0921200800065));
#159645=CARTESIAN_POINT('Ctrl Pts',(14.0263093380892,-54.580000021009,-93.3049061919411));
#159646=CARTESIAN_POINT('Ctrl Pts',(13.691663333917,-54.5800000206227,-93.5116810242999));
#159647=CARTESIAN_POINT('Ctrl Pts',(13.3538223587281,-54.5800000202949,
-93.7136406704411));
#159648=CARTESIAN_POINT('Ctrl Pts',(13.0120992871415,-54.5800000201906,
-93.9106936784565));
#159649=CARTESIAN_POINT('Ctrl Pts',(12.7734325857322,-54.5800000201177,
-94.0483197135013));
#159650=CARTESIAN_POINT('Ctrl Pts',(12.5336633488411,-54.5800000201,-94.1830804413658));
#159651=CARTESIAN_POINT('Ctrl Pts',(12.2925916871682,-54.5800000202013,
-94.3149150255473));
#159652=CARTESIAN_POINT('Ctrl Pts',(11.7801234903754,-54.5800000204166,
-94.5951679228046));
#159653=CARTESIAN_POINT('Ctrl Pts',(11.2613422805864,-54.5800000202694,
-94.8625400041996));
#159654=CARTESIAN_POINT('Ctrl Pts',(10.7355463256496,-54.580000020136,-95.1156089775454));
#159655=CARTESIAN_POINT('Ctrl Pts',(10.2954190750541,-54.5800000200243,
-95.3274450527451));
#159656=CARTESIAN_POINT('Ctrl Pts',(9.85037652346006,-54.5800000200001,
-95.5292584793922));
#159657=CARTESIAN_POINT('Ctrl Pts',(9.4,-54.58000002,-95.7201877838351));
#159658=CARTESIAN_POINT('',(9.4,-54.58000002,-136.131917111522));
#159659=CARTESIAN_POINT('Origin',(60.,-54.58000002,-55.24995));
#159660=CARTESIAN_POINT('',(1.24999999943729,-54.58000002,-134.362052687297));
#159661=CARTESIAN_POINT('',(6.9,-54.58000002,-135.415380765739));
#159662=CARTESIAN_POINT('Ctrl Pts',(1.24999999852555,-54.58000002,-134.362052703156));
#159663=CARTESIAN_POINT('Ctrl Pts',(1.85586872996852,-54.58000002,-134.396884061811));
#159664=CARTESIAN_POINT('Ctrl Pts',(2.45821169814366,-54.5800000199999,
-134.456836856573));
#159665=CARTESIAN_POINT('Ctrl Pts',(3.05717008780238,-54.5800000200001,
-134.540898522253));
#159666=CARTESIAN_POINT('Ctrl Pts',(3.40705616967825,-54.5800000200002,
-134.590003781231));
#159667=CARTESIAN_POINT('Ctrl Pts',(3.75578723672591,-54.5800000200004,
-134.647336949705));
#159668=CARTESIAN_POINT('Ctrl Pts',(4.10339093154591,-54.5800000200016,
-134.712704370428));
#159669=CARTESIAN_POINT('Ctrl Pts',(4.21364342719022,-54.580000020002,-134.733437525386));
#159670=CARTESIAN_POINT('Ctrl Pts',(4.32374689616092,-54.5800000200024,
-134.754971981414));
#159671=CARTESIAN_POINT('Ctrl Pts',(4.43373542753185,-54.5800000200027,
-134.777307325963));
#159672=CARTESIAN_POINT('Ctrl Pts',(4.6798887972806,-54.5800000200034,-134.827293631415));
#159673=CARTESIAN_POINT('Ctrl Pts',(4.92593529130785,-54.5800000200038,
-134.881432381241));
#159674=CARTESIAN_POINT('Ctrl Pts',(5.17124777564251,-54.5800000200039,
-134.939444408488));
#159675=CARTESIAN_POINT('Ctrl Pts',(5.41900393393866,-54.580000020004,-134.998034321043));
#159676=CARTESIAN_POINT('Ctrl Pts',(5.66601353633239,-54.5800000200037,
-135.060575714351));
#159677=CARTESIAN_POINT('Ctrl Pts',(5.91161937020824,-54.5800000200032,
-135.126829777541));
#159678=CARTESIAN_POINT('Ctrl Pts',(5.95160365908367,-54.5800000200032,
-135.137615847074));
#159679=CARTESIAN_POINT('Ctrl Pts',(5.99155067840985,-54.5800000200031,
-135.148500406429));
#159680=CARTESIAN_POINT('Ctrl Pts',(6.03145750349794,-54.580000020003,-135.159482527522));
#159681=CARTESIAN_POINT('Ctrl Pts',(6.28934481311032,-54.5800000200026,
-135.230451582474));
#159682=CARTESIAN_POINT('Ctrl Pts',(6.54583590336147,-54.580000020002,-135.305503306744));
#159683=CARTESIAN_POINT('Ctrl Pts',(6.80143368808444,-54.5800000200016,
-135.384644793434));
#159684=CARTESIAN_POINT('Ctrl Pts',(6.83430358210263,-54.5800000200015,
-135.394822394476));
#159685=CARTESIAN_POINT('Ctrl Pts',(6.86715867181372,-54.5800000200014,
-135.405067695209));
#159686=CARTESIAN_POINT('Ctrl Pts',(6.9,-54.5800000200014,-135.415380765739));
#159687=CARTESIAN_POINT('',(6.9,-54.58000002,-96.6432622057672));
#159688=CARTESIAN_POINT('',(6.9,-54.58000002,-96.4806904787158));
#159689=CARTESIAN_POINT('',(1.24999998181185,-54.5800000199993,-97.6965897229033));
#159690=CARTESIAN_POINT('Ctrl Pts',(6.9,-54.5800000200288,-96.6432622057672));
#159691=CARTESIAN_POINT('Ctrl Pts',(6.49061970139211,-54.5800000200775,
-96.7718187571058));
#159692=CARTESIAN_POINT('Ctrl Pts',(6.07861873660016,-54.5800000205753,
-96.8899526380549));
#159693=CARTESIAN_POINT('Ctrl Pts',(5.66396816650171,-54.5800000217474,
-96.9971605311362));
#159694=CARTESIAN_POINT('Ctrl Pts',(5.26447645459898,-54.5800000228767,
-97.100449101863));
#159695=CARTESIAN_POINT('Ctrl Pts',(4.86252531660943,-54.5800000241933,
-97.1935960044572));
#159696=CARTESIAN_POINT('Ctrl Pts',(4.45809517257588,-54.5800000232613,
-97.2761964906685));
#159697=CARTESIAN_POINT('Ctrl Pts',(4.34240961804981,-54.5800000229947,
-97.2998240149577));
#159698=CARTESIAN_POINT('Ctrl Pts',(4.22645442245894,-54.5800000225654,
-97.3225679069059));
#159699=CARTESIAN_POINT('Ctrl Pts',(4.1103033922506,-54.5800000220553,-97.3444205163838));
#159700=CARTESIAN_POINT('Ctrl Pts',(3.87438492650356,-54.5800000210192,
-97.3888061244265));
#159701=CARTESIAN_POINT('Ctrl Pts',(3.63765702198835,-54.580000020604,-97.4294862943975));
#159702=CARTESIAN_POINT('Ctrl Pts',(3.40027293016165,-54.5800000203617,
-97.466451043988));
#159703=CARTESIAN_POINT('Ctrl Pts',(3.16793216733981,-54.5800000201245,
-97.5026304612829));
#159704=CARTESIAN_POINT('Ctrl Pts',(2.93496148468427,-54.5800000200661,
-97.5352507112807));
#159705=CARTESIAN_POINT('Ctrl Pts',(2.70149448625451,-54.5800000200335,
-97.5642527645725));
#159706=CARTESIAN_POINT('Ctrl Pts',(2.47413670469376,-54.5800000200018,
-97.5924959104624));
#159707=CARTESIAN_POINT('Ctrl Pts',(2.2463071385321,-54.580000020002,-97.6173077624549));
#159708=CARTESIAN_POINT('Ctrl Pts',(2.01813705517291,-54.5800000200007,
-97.6385856637381));
#159709=CARTESIAN_POINT('Ctrl Pts',(1.80087152564896,-54.5800000199995,
-97.658846665625));
#159710=CARTESIAN_POINT('Ctrl Pts',(1.58329647023807,-54.58000002,-97.6759032884729));
#159711=CARTESIAN_POINT('Ctrl Pts',(1.36554569823627,-54.58000002,-97.6896238013575));
#159712=CARTESIAN_POINT('Ctrl Pts',(1.32703559408638,-54.58000002,-97.6920503295177));
#159713=CARTESIAN_POINT('Ctrl Pts',(1.2885200646298,-54.58000002,-97.6943724020827));
#159714=CARTESIAN_POINT('Ctrl Pts',(1.24999994858788,-54.58000002,-97.6965891455738));
#159715=CARTESIAN_POINT('',(1.24999999999997,-54.58000002,-134.339054731985));
#159716=CARTESIAN_POINT('Origin',(-3.3975957231091E-14,-70.08000002,-174.34995));
#159717=CARTESIAN_POINT('',(24.2,-73.08000002,-174.34995));
#159718=CARTESIAN_POINT('',(24.7,-73.08000002,-174.34995));
#159719=CARTESIAN_POINT('',(41.5,-73.08000002,-174.34995));
#159720=CARTESIAN_POINT('',(24.2,-70.08000002,-177.34995));
#159721=CARTESIAN_POINT('Origin',(24.2,-70.08000002,-174.34995));
#159722=CARTESIAN_POINT('',(24.7,-70.08000002,-177.34995));
#159723=CARTESIAN_POINT('',(-41.5,-70.08000002,-177.34995));
#159724=CARTESIAN_POINT('Origin',(24.7,-70.08000002,-174.34995));
#159725=CARTESIAN_POINT('Origin',(0.,-12.9675000200281,-170.64995));
#159726=CARTESIAN_POINT('Ctrl Pts',(31.35,-63.1109998882233,-171.64995));
#159727=CARTESIAN_POINT('Ctrl Pts',(31.3163826919509,-62.9824421580757,
-171.64995));
#159728=CARTESIAN_POINT('Ctrl Pts',(31.2868383330336,-62.8719447893433,
-171.626170015677));
#159729=CARTESIAN_POINT('Ctrl Pts',(31.2514775435999,-62.7372823365182,
-171.580557425965));
#159730=CARTESIAN_POINT('Ctrl Pts',(31.2410919380176,-62.6974310527944,
-171.563623005043));
#159731=CARTESIAN_POINT('Ctrl Pts',(31.2274097259629,-62.6448298616196,
-171.538032015327));
#159732=CARTESIAN_POINT('Ctrl Pts',(31.2231625215576,-62.6284882571325,
-171.529463812056));
#159733=CARTESIAN_POINT('Ctrl Pts',(31.2172203289157,-62.6056926604661,
-171.516799359085));
#159734=CARTESIAN_POINT('Ctrl Pts',(31.2143562722305,-62.5947238974589,
-171.51051351882));
#159735=CARTESIAN_POINT('Ctrl Pts',(31.211192177598,-62.5826609240819,-171.503308765418));
#159736=CARTESIAN_POINT('Ctrl Pts',(31.2098730231894,-62.5776464897022,
-171.500253322111));
#159737=CARTESIAN_POINT('Ctrl Pts',(31.2090016607235,-62.5743378631998,
-171.49822405484));
#159738=CARTESIAN_POINT('Ctrl Pts',(31.2088776499101,-62.5738660850072,
-171.497937403819));
#159739=CARTESIAN_POINT('Ctrl Pts',(31.1610829776623,-62.392811385933,-171.385434173695));
#159740=CARTESIAN_POINT('Ctrl Pts',(31.1276890220452,-62.2670868673818,
-171.23009267792));
#159741=CARTESIAN_POINT('Ctrl Pts',(31.1079170675507,-62.1926886331265,
-171.07256826174));
#159742=CARTESIAN_POINT('',(25.5241645866138,-65.4203114476559,-171.244965289362));
#159743=CARTESIAN_POINT('Origin',(25.6930085000554,-66.193075224377,-170.642186607387));
#159744=CARTESIAN_POINT('',(26.2234488624093,-65.1680142434972,-171.34400271074));
#159745=CARTESIAN_POINT('Ctrl Pts',(25.5241645593467,-65.420311391623,-171.244965335496));
#159746=CARTESIAN_POINT('Ctrl Pts',(25.5856266066318,-65.3950097001748,
-171.250561299215));
#159747=CARTESIAN_POINT('Ctrl Pts',(25.6482431903754,-65.3700416388738,
-171.257283842693));
#159748=CARTESIAN_POINT('Ctrl Pts',(25.7120492724639,-65.3455045252255,
-171.26508922401));
#159749=CARTESIAN_POINT('Ctrl Pts',(25.7739841159747,-65.3216870105894,
-171.272665697202));
#159750=CARTESIAN_POINT('Ctrl Pts',(25.8370396117807,-65.2982756083868,
-171.281262680318));
#159751=CARTESIAN_POINT('Ctrl Pts',(25.9012641559865,-65.2753562048817,
-171.290795412438));
#159752=CARTESIAN_POINT('Ctrl Pts',(25.9628302885007,-65.2533854918032,
-171.299933561353));
#159753=CARTESIAN_POINT('Ctrl Pts',(26.0254706465919,-65.231866942171,-171.309931710469));
#159754=CARTESIAN_POINT('Ctrl Pts',(26.0892441669414,-65.2108724395197,
-171.320670985522));
#159755=CARTESIAN_POINT('Ctrl Pts',(26.1334266108244,-65.1963273990365,
-171.328111180366));
#159756=CARTESIAN_POINT('Ctrl Pts',(26.1781532742408,-65.1820338125062,
-171.335906203664));
#159757=CARTESIAN_POINT('Ctrl Pts',(26.2234488624093,-65.1680142434972,
-171.34400271074));
#159758=CARTESIAN_POINT('Ctrl Pts',(26.2234488624093,-65.1680142434972,
-171.34400271074));
#159759=CARTESIAN_POINT('Ctrl Pts',(26.3217167386875,-65.1375990677912,
-171.361567921566));
#159760=CARTESIAN_POINT('Ctrl Pts',(26.4303514143194,-65.1038537466012,
-171.379899641242));
#159761=CARTESIAN_POINT('Ctrl Pts',(26.5494548896309,-65.0666619993164,
-171.39847124772));
#159762=CARTESIAN_POINT('Ctrl Pts',(26.6414327590449,-65.0379406067114,
-171.412813203661));
#159763=CARTESIAN_POINT('Ctrl Pts',(26.7396537921653,-65.0071635777161,
-171.427297276244));
#159764=CARTESIAN_POINT('Ctrl Pts',(26.8441476657696,-64.9742759706334,
-171.441710877444));
#159765=CARTESIAN_POINT('Ctrl Pts',(26.8973144353205,-64.9575426659283,
-171.449044557276));
#159766=CARTESIAN_POINT('Ctrl Pts',(26.9521048251731,-64.9402629709406,
-171.456360592174));
#159767=CARTESIAN_POINT('Ctrl Pts',(27.0085205474515,-64.9224297399861,
-171.46363596587));
#159768=CARTESIAN_POINT('Ctrl Pts',(27.0558749625435,-64.9074608237524,
-171.469742793046));
#159769=CARTESIAN_POINT('Ctrl Pts',(27.104374200011,-64.8921020024936,-171.475820972803));
#159770=CARTESIAN_POINT('Ctrl Pts',(27.1540177175151,-64.8763493205577,
-171.48185932281));
#159771=CARTESIAN_POINT('Ctrl Pts',(27.2981145026722,-64.8306251064268,
-171.499386421359));
#159772=CARTESIAN_POINT('Ctrl Pts',(27.4518624274715,-64.7815805088472,
-171.51653998626));
#159773=CARTESIAN_POINT('Ctrl Pts',(27.6152854898679,-64.729100640996,-171.532829362194));
#159774=CARTESIAN_POINT('Ctrl Pts',(27.762285103335,-64.6818948171925,-171.547481712545));
#159775=CARTESIAN_POINT('Ctrl Pts',(27.9171113129778,-64.6319098298976,
-171.561433561531));
#159776=CARTESIAN_POINT('Ctrl Pts',(28.0797524083188,-64.5790629606593,
-171.574350075366));
#159777=CARTESIAN_POINT('Ctrl Pts',(28.0826324162796,-64.5781271614765,
-171.574578797772));
#159778=CARTESIAN_POINT('Ctrl Pts',(28.0845605503282,-64.5775006128595,
-171.574731707236));
#159779=CARTESIAN_POINT('Ctrl Pts',(28.0881176467749,-64.5763445655939,
-171.575012963699));
#159780=CARTESIAN_POINT('Ctrl Pts',(28.0885065052652,-64.5762181875771,
-171.575043710395));
#159781=CARTESIAN_POINT('Ctrl Pts',(28.088914830995,-64.5760854809111,-171.575075987216));
#159782=CARTESIAN_POINT('Ctrl Pts',(28.0893459957261,-64.5759453491265,
-171.575110057511));
#159783=CARTESIAN_POINT('Ctrl Pts',(28.2453251126488,-64.5252509615012,
-171.587435403764));
#159784=CARTESIAN_POINT('Ctrl Pts',(28.3917855167039,-64.4774693308856,
-171.597568849547));
#159785=CARTESIAN_POINT('Ctrl Pts',(28.5286691085897,-64.4326571475584,
-171.605956388818));
#159786=CARTESIAN_POINT('Ctrl Pts',(28.6375214539492,-64.3970216766547,
-171.612626314036));
#159787=CARTESIAN_POINT('Ctrl Pts',(28.7403173603302,-64.363262690218,-171.618191806933));
#159788=CARTESIAN_POINT('Ctrl Pts',(28.8370242459599,-64.331388662323,-171.622865882341));
#159789=CARTESIAN_POINT('Ctrl Pts',(28.9570429382945,-64.2918311983175,
-171.628666673203));
#159790=CARTESIAN_POINT('Ctrl Pts',(29.0676861505517,-64.2551849334993,
-171.63309896429));
#159791=CARTESIAN_POINT('Ctrl Pts',(29.1688978658542,-64.2215000860559,
-171.636547403149));
#159792=CARTESIAN_POINT('Ctrl Pts',(29.2517930969775,-64.1939112520377,
-171.639371771211));
#159793=CARTESIAN_POINT('Ctrl Pts',(29.3283616429728,-64.1683085580936,
-171.641535544552));
#159794=CARTESIAN_POINT('Ctrl Pts',(29.3985739176396,-64.1447118415866,
-171.643225082614));
#159795=CARTESIAN_POINT('Ctrl Pts',(29.4774723478353,-64.1181959097354,
-171.645123638124));
#159796=CARTESIAN_POINT('Ctrl Pts',(29.5483631757519,-64.0942438437233,
-171.646429379742));
#159797=CARTESIAN_POINT('Ctrl Pts',(29.6112478721861,-64.0729216658316,
-171.647365040175));
#159798=CARTESIAN_POINT('Ctrl Pts',(29.674111806394,-64.051606527743,-171.648300391687));
#159799=CARTESIAN_POINT('Ctrl Pts',(29.7289749630295,-64.0329196552157,
-171.648865922478));
#159800=CARTESIAN_POINT('Ctrl Pts',(29.7758403385976,-64.016920223518,-171.64923249186));
#159801=CARTESIAN_POINT('Ctrl Pts',(29.823015394053,-64.0008150697996,-171.649601483481));
#159802=CARTESIAN_POINT('Ctrl Pts',(29.8620866579719,-63.9874330870119,
-171.649768868419));
#159803=CARTESIAN_POINT('Ctrl Pts',(29.8930579659894,-63.976826170643,-171.649856428699));
#159804=CARTESIAN_POINT('Ctrl Pts',(29.9222033403128,-63.9668445919568,
-171.649938826806));
#159805=CARTESIAN_POINT('Ctrl Pts',(29.9441756977843,-63.9593204895971,
-171.64995));
#159806=CARTESIAN_POINT('Ctrl Pts',(29.958978566972,-63.954289311524,-171.64995));
#159807=CARTESIAN_POINT('Ctrl Pts',(1.21164037634558,-54.58000002,-134.359881256142));
#159808=CARTESIAN_POINT('Ctrl Pts',(1.14985954526071,-54.5800000199999,
-135.468549546812));
#159809=CARTESIAN_POINT('Ctrl Pts',(1.09388617364344,-55.0500049847781,
-136.4730019173));
#159810=CARTESIAN_POINT('Ctrl Pts',(2.29002416952399,-54.58000002,-134.419974475838));
#159811=CARTESIAN_POINT('Ctrl Pts',(2.17342188453964,-54.580000019985,-135.528968047153));
#159812=CARTESIAN_POINT('Ctrl Pts',(2.06753434039226,-55.0527274298038,
-136.533094948603));
#159813=CARTESIAN_POINT('Ctrl Pts',(3.36400336137312,-54.58000002,-134.560074887715));
#159814=CARTESIAN_POINT('Ctrl Pts',(3.19311388201375,-54.58000002,-135.669910423004));
#159815=CARTESIAN_POINT('Ctrl Pts',(3.03750087523273,-55.0590775604595,
-136.673195500792));
#159816=CARTESIAN_POINT('Ctrl Pts',(4.96860300664728,-54.58000002,-134.885915931654));
#159817=CARTESIAN_POINT('Ctrl Pts',(4.71606907271929,-54.5800000199999,
-135.997377284272));
#159818=CARTESIAN_POINT('Ctrl Pts',(4.48819703666783,-55.0737169289411,
-136.999036474763));
#159819=CARTESIAN_POINT('Ctrl Pts',(5.50462478218054,-54.58000002,-135.014494663549));
#159820=CARTESIAN_POINT('Ctrl Pts',(5.22505809365354,-54.5800000199999,
-136.126651318852));
#159821=CARTESIAN_POINT('Ctrl Pts',(4.97306105763453,-55.0794779054381,
-137.127615177464));
#159822=CARTESIAN_POINT('Ctrl Pts',(6.5582931505392,-54.58000002,-135.304459760069));
#159823=CARTESIAN_POINT('Ctrl Pts',(6.22568909425541,-54.58000002,-136.4181319057));
#159824=CARTESIAN_POINT('Ctrl Pts',(5.92681315212766,-55.0924068363451,
-137.417580209995));
#159825=CARTESIAN_POINT('Ctrl Pts',(7.07711031169138,-54.58000002,-135.46589761626));
#159826=CARTESIAN_POINT('Ctrl Pts',(6.71851091709043,-54.58000002,-136.580434989905));
#159827=CARTESIAN_POINT('Ctrl Pts',(6.39675697066589,-55.0995771769741,
-137.579018061084));
#159828=CARTESIAN_POINT('Ctrl Pts',(7.58869434220596,-54.58000002,-135.642187967278));
#159829=CARTESIAN_POINT('Ctrl Pts',(7.2043372482231,-54.58000002,-136.757569215766));
#159830=CARTESIAN_POINT('Ctrl Pts',(6.86051928234731,-55.1073628388699,
-137.755308344391));
#159831=CARTESIAN_POINT('',(6.82752390438729,-55.1067946098355,-137.742762001241));
#159832=CARTESIAN_POINT('',(1.23668893165473,-55.0504165218146,-136.482360813851));
#159833=CARTESIAN_POINT('Ctrl Pts',(6.82752390105444,-55.106794611208,-137.742762010959));
#159834=CARTESIAN_POINT('Ctrl Pts',(6.36691608500268,-55.099096087914,-137.56848291046));
#159835=CARTESIAN_POINT('Ctrl Pts',(5.90746653899706,-55.0921186415656,
-137.411614134422));
#159836=CARTESIAN_POINT('Ctrl Pts',(5.21924575097325,-55.0827917577677,
-137.202426457053));
#159837=CARTESIAN_POINT('Ctrl Pts',(4.87537346097248,-55.0784122257285,
-137.10436149004));
#159838=CARTESIAN_POINT('Ctrl Pts',(4.47443163044212,-55.0738024150764,
-137.001377887286));
#159839=CARTESIAN_POINT('Ctrl Pts',(4.30263256796571,-55.0719335078804,
-136.959690384411));
#159840=CARTESIAN_POINT('Ctrl Pts',(4.1881051325322,-55.0707112308887,-136.932442788467));
#159841=CARTESIAN_POINT('Ctrl Pts',(4.13281892637863,-55.0701321878583,
-136.91954214536));
#159842=CARTESIAN_POINT('Ctrl Pts',(3.12583467092903,-55.059800011716,-136.689517799435));
#159843=CARTESIAN_POINT('Ctrl Pts',(2.18183534213973,-55.0534032173182,
-136.548300970225));
#159844=CARTESIAN_POINT('Ctrl Pts',(1.23668893165476,-55.0504165218146,
-136.482360813851));
#159845=CARTESIAN_POINT('Ctrl Pts',(6.82752391167578,-55.1067946098897,
-137.742761979991));
#159846=CARTESIAN_POINT('Ctrl Pts',(6.82865514233252,-55.0906927749922,
-137.709063966307));
#159847=CARTESIAN_POINT('Ctrl Pts',(6.82989569318454,-55.0733143121305,
-137.671794693994));
#159848=CARTESIAN_POINT('Ctrl Pts',(6.83125496840252,-55.0548926081662,
-137.630841859));
#159849=CARTESIAN_POINT('Ctrl Pts',(6.83251854070202,-55.0377679269163,
-137.59277240316));
#159850=CARTESIAN_POINT('Ctrl Pts',(6.83388482437207,-55.0197420755336,
-137.551519359742));
#159851=CARTESIAN_POINT('Ctrl Pts',(6.83535746783391,-55.0010426501733,
-137.506989171318));
#159852=CARTESIAN_POINT('Ctrl Pts',(6.83688588027598,-54.9816350779259,
-137.460772625494));
#159853=CARTESIAN_POINT('Ctrl Pts',(6.83852910258862,-54.9615015335891,
-137.411025472467));
#159854=CARTESIAN_POINT('Ctrl Pts',(6.84028407605309,-54.9409428817604,
-137.357646873862));
#159855=CARTESIAN_POINT('Ctrl Pts',(6.84116156278532,-54.930663555846,-137.330957574559));
#159856=CARTESIAN_POINT('Ctrl Pts',(6.84206685481821,-54.9202787058626,
-137.303360523525));
#159857=CARTESIAN_POINT('Ctrl Pts',(6.84299862087351,-54.9098305132466,
-137.274844194797));
#159858=CARTESIAN_POINT('Ctrl Pts',(6.84346450390116,-54.9046064169385,
-137.260586030434));
#159859=CARTESIAN_POINT('Ctrl Pts',(6.84393700981204,-54.8993665212808,
-137.24609803364));
#159860=CARTESIAN_POINT('Ctrl Pts',(6.84441587811191,-54.8941164051088,
-137.231378905632));
#159861=CARTESIAN_POINT('Ctrl Pts',(6.84478230404662,-54.8900990610369,
-137.220115954545));
#159862=CARTESIAN_POINT('Ctrl Pts',(6.84512750680533,-54.8863462003223,
-137.20948827454));
#159863=CARTESIAN_POINT('Ctrl Pts',(6.84550863637637,-54.8822386442122,
-137.197726631341));
#159864=CARTESIAN_POINT('Ctrl Pts',(6.8456255907356,-54.8809781894236,-137.194117424529));
#159865=CARTESIAN_POINT('Ctrl Pts',(6.84574593077812,-54.8796846645726,
-137.190401311301));
#159866=CARTESIAN_POINT('Ctrl Pts',(6.84587131312705,-54.8783411245515,
-137.186526810165));
#159867=CARTESIAN_POINT('Ctrl Pts',(6.84770105936456,-54.8587343990471,
-137.129984928968));
#159868=CARTESIAN_POINT('Ctrl Pts',(6.84942928243091,-54.8412633928784,
-137.076574520802));
#159869=CARTESIAN_POINT('Ctrl Pts',(6.85104244637681,-54.8256167780335,
-137.026448311966));
#159870=CARTESIAN_POINT('Ctrl Pts',(6.8526724164755,-54.8098071547105,-136.975799881735));
#159871=CARTESIAN_POINT('Ctrl Pts',(6.85418514107506,-54.7958596699486,
-136.928503953666));
#159872=CARTESIAN_POINT('Ctrl Pts',(6.85557654565148,-54.7834863408097,
-136.884677100533));
#159873=CARTESIAN_POINT('Ctrl Pts',(6.85698425116315,-54.7709680525119,
-136.840336795952));
#159874=CARTESIAN_POINT('Ctrl Pts',(6.85826798681468,-54.7600606486674,
-136.799546849772));
#159875=CARTESIAN_POINT('Ctrl Pts',(6.85943030320443,-54.7505060449436,
-136.762393576608));
#159876=CARTESIAN_POINT('Ctrl Pts',(6.85996390280677,-54.7461196895653,
-136.745337143471));
#159877=CARTESIAN_POINT('Ctrl Pts',(6.8604719860349,-54.7420190332804,-136.729046736211));
#159878=CARTESIAN_POINT('Ctrl Pts',(6.86095509270203,-54.7381821800109,
-136.713528729206));
#159879=CARTESIAN_POINT('Ctrl Pts',(6.86155592605446,-54.7334103365039,
-136.694229189775));
#159880=CARTESIAN_POINT('Ctrl Pts',(6.86211812692543,-54.7290463835956,
-136.676124419269));
#159881=CARTESIAN_POINT('Ctrl Pts',(6.8626429567941,-54.7250525423937,-136.659224428366));
#159882=CARTESIAN_POINT('Ctrl Pts',(6.86290537172844,-54.7230556217927,
-136.650774432914));
#159883=CARTESIAN_POINT('Ctrl Pts',(6.8631584500198,-54.7211513090831,-136.642625613791));
#159884=CARTESIAN_POINT('Ctrl Pts',(6.86340235796966,-54.7193353377099,
-136.634778996657));
#159885=CARTESIAN_POINT('Ctrl Pts',(6.86352431194459,-54.7184273520232,
-136.63085568809));
#159886=CARTESIAN_POINT('Ctrl Pts',(6.86364397372556,-54.7175414566762,
-136.627007928831));
#159887=CARTESIAN_POINT('Ctrl Pts',(6.8637613648426,-54.7166771482468,-136.623235838989));
#159888=CARTESIAN_POINT('Ctrl Pts',(6.86382006040112,-54.716244994032,-136.621349794069));
#159889=CARTESIAN_POINT('Ctrl Pts',(6.86387818831689,-54.7158182368597,
-136.619482666432));
#159890=CARTESIAN_POINT('Ctrl Pts',(6.86393575129393,-54.7153968156136,
-136.617634470333));
#159891=CARTESIAN_POINT('Ctrl Pts',(6.86399331427096,-54.7149753943675,
-136.615786274235));
#159892=CARTESIAN_POINT('Ctrl Pts',(6.86399608221759,-54.7149540623116,
-136.615696574571));
#159893=CARTESIAN_POINT('Ctrl Pts',(6.86410674816117,-54.7141484997746,
-136.612146690543));
#159894=CARTESIAN_POINT('Ctrl Pts',(6.86687027771176,-54.6940321405412,
-136.523499640744));
#159895=CARTESIAN_POINT('Ctrl Pts',(6.86957825832433,-54.6766746954665,
-136.436668295782));
#159896=CARTESIAN_POINT('Ctrl Pts',(6.87220179170381,-54.6617598759321,
-136.351863423873));
#159897=CARTESIAN_POINT('Ctrl Pts',(6.87491477571019,-54.6463365284835,
-136.264167089247));
#159898=CARTESIAN_POINT('Ctrl Pts',(6.8775375463631,-54.6335245857754,-136.178637752116));
#159899=CARTESIAN_POINT('Ctrl Pts',(6.88005612234316,-54.622974273047,-136.095454821509));
#159900=CARTESIAN_POINT('Ctrl Pts',(6.88262252285252,-54.6122236234042,
-136.010692353681));
#159901=CARTESIAN_POINT('Ctrl Pts',(6.88508090180449,-54.6038207305193,
-135.928365983663));
#159902=CARTESIAN_POINT('Ctrl Pts',(6.88743275526135,-54.5974048404534,
-135.848613127078));
#159903=CARTESIAN_POINT('Ctrl Pts',(6.88986235560334,-54.5907768557662,
-135.766223823837));
#159904=CARTESIAN_POINT('Ctrl Pts',(6.8921784369626,-54.5862688512884,-135.686580732264));
#159905=CARTESIAN_POINT('Ctrl Pts',(6.89439732976196,-54.5835019137301,
-135.609783871025));
#159906=CARTESIAN_POINT('Ctrl Pts',(6.89633252386602,-54.5810887456623,
-135.542805947115));
#159907=CARTESIAN_POINT('Ctrl Pts',(6.89819411437535,-54.5800000650814,
-135.477991939119));
#159908=CARTESIAN_POINT('Ctrl Pts',(6.9,-54.5800000200014,-135.415380765739));
#159909=CARTESIAN_POINT('Origin',(1.23493664937611,-61.9785327152568,-133.830076534122));
#159910=CARTESIAN_POINT('Ctrl Pts',(14.935633130959,-55.3065630024253,-142.47652148601));
#159911=CARTESIAN_POINT('Ctrl Pts',(15.630331507009,-54.5800000199999,-141.502754952306));
#159912=CARTESIAN_POINT('Ctrl Pts',(16.443141398898,-54.58000002,-140.363430177307));
#159913=CARTESIAN_POINT('Ctrl Pts',(13.9222087476243,-55.2748272571858,
-141.68934947009));
#159914=CARTESIAN_POINT('Ctrl Pts',(14.5800220275964,-54.580000020014,-140.713030388695));
#159915=CARTESIAN_POINT('Ctrl Pts',(15.3397373006696,-54.58000002,-139.576246587186));
#159916=CARTESIAN_POINT('Ctrl Pts',(12.8784929287096,-55.2441433795399,
-140.946005990295));
#159917=CARTESIAN_POINT('Ctrl Pts',(13.4942101985199,-54.5800000200048,
-139.965671699013));
#159918=CARTESIAN_POINT('Ctrl Pts',(14.2001096642283,-54.58000002,-138.832914681508));
#159919=CARTESIAN_POINT('Ctrl Pts',(10.7090288904129,-55.1865297732718,
-139.576073691957));
#159920=CARTESIAN_POINT('Ctrl Pts',(11.2325518044464,-54.5800000199952,
-138.58879503276));
#159921=CARTESIAN_POINT('Ctrl Pts',(11.8242610588971,-54.58000002,-137.462982383337));
#159922=CARTESIAN_POINT('Ctrl Pts',(9.6010395318864,-55.1600903081647,-138.961065386249));
#159923=CARTESIAN_POINT('Ctrl Pts',(10.0748797157148,-54.5800000199999,
-137.970225859417));
#159924=CARTESIAN_POINT('Ctrl Pts',(10.6074840054802,-54.58000002,-136.847973525117));
#159925=CARTESIAN_POINT('Ctrl Pts',(8.46374531288877,-55.1370659744517,
-138.432713944563));
#159926=CARTESIAN_POINT('Ctrl Pts',(8.88330739463766,-54.58000002,-137.438496970103));
#159927=CARTESIAN_POINT('Ctrl Pts',(9.35547519799418,-54.58000002,-136.31962263586));
#159928=CARTESIAN_POINT('',(14.8995695360959,-55.3054344939376,-142.448537924459));
#159929=CARTESIAN_POINT('',(9.30242220787652,-55.1547652726017,-138.840493482365));
#159930=CARTESIAN_POINT('Ctrl Pts',(14.8995696008972,-55.3054345059085,
-142.448537780858));
#159931=CARTESIAN_POINT('Ctrl Pts',(14.4360425314271,-55.2909407491857,
-142.089227172811));
#159932=CARTESIAN_POINT('Ctrl Pts',(13.9756272852217,-55.276965801663,-141.746453688849));
#159933=CARTESIAN_POINT('Ctrl Pts',(13.5167726538588,-55.2635139066454,
-141.419418449115));
#159934=CARTESIAN_POINT('Ctrl Pts',(13.0608088615625,-55.2501467601756,
-141.094443570512));
#159935=CARTESIAN_POINT('Ctrl Pts',(12.6063898761816,-55.2372957621152,
-140.785004198599));
#159936=CARTESIAN_POINT('Ctrl Pts',(12.1520037917279,-55.2249575381717,
-140.490317118194));
#159937=CARTESIAN_POINT('Ctrl Pts',(12.0325966013581,-55.2217152015208,
-140.412876902674));
#159938=CARTESIAN_POINT('Ctrl Pts',(11.913191572675,-55.2185082497222,-140.336455667304));
#159939=CARTESIAN_POINT('Ctrl Pts',(11.7937609095613,-55.2153365764059,
-140.261039841126));
#159940=CARTESIAN_POINT('Ctrl Pts',(11.4455508439728,-55.206089298155,-140.041158705954));
#159941=CARTESIAN_POINT('Ctrl Pts',(11.0989538321641,-55.1971924514801,
-139.831013919457));
#159942=CARTESIAN_POINT('Ctrl Pts',(10.75329986993,-55.1886468974311,-139.63028506502));
#159943=CARTESIAN_POINT('Ctrl Pts',(10.4339817724706,-55.1807524412442,
-139.444850026204));
#159944=CARTESIAN_POINT('Ctrl Pts',(10.1154686315248,-55.1731577288529,
-139.267450490947));
#159945=CARTESIAN_POINT('Ctrl Pts',(9.79721921732249,-55.1658637037984,
-139.097876598179));
#159946=CARTESIAN_POINT('Ctrl Pts',(9.63224811328577,-55.1620826964738,
-139.00997449669));
#159947=CARTESIAN_POINT('Ctrl Pts',(9.46734764252996,-55.1583824957503,
-138.924175954812));
#159948=CARTESIAN_POINT('Ctrl Pts',(9.302440717147,-55.1547633327525,-138.840457107207));
#159949=CARTESIAN_POINT('Ctrl Pts',(14.8995694581843,-55.3054344861034,
-142.448537924463));
#159950=CARTESIAN_POINT('Ctrl Pts',(14.9033493580002,-55.2678130034392,
-142.375124451206));
#159951=CARTESIAN_POINT('Ctrl Pts',(14.9073778485915,-55.2293881917473,
-142.29668067779));
#159952=CARTESIAN_POINT('Ctrl Pts',(14.911659466542,-55.1907336547858,-142.21302758756));
#159953=CARTESIAN_POINT('Ctrl Pts',(14.9132571196824,-55.1763100086129,
-142.18181307383));
#159954=CARTESIAN_POINT('Ctrl Pts',(14.9148900157128,-55.1618548868074,
-142.149873089003));
#159955=CARTESIAN_POINT('Ctrl Pts',(14.9165583830287,-55.1473998475109,
-142.117197815172));
#159956=CARTESIAN_POINT('Ctrl Pts',(14.9196281312329,-55.1208029881141,
-142.057076244693));
#159957=CARTESIAN_POINT('Ctrl Pts',(14.9228177984541,-55.0942074117109,
-141.994468404112));
#159958=CARTESIAN_POINT('Ctrl Pts',(14.9261276135912,-55.0678250719188,
-141.929332565682));
#159959=CARTESIAN_POINT('Ctrl Pts',(14.9277825211597,-55.0546339020227,
-141.896764646467));
#159960=CARTESIAN_POINT('Ctrl Pts',(14.9294674513146,-55.0414962585256,
-141.863564944585));
#159961=CARTESIAN_POINT('Ctrl Pts',(14.9311823387923,-55.0284397939552,
-141.829729698383));
#159962=CARTESIAN_POINT('Ctrl Pts',(14.9320397825312,-55.02191156167,-141.812812075282));
#159963=CARTESIAN_POINT('Ctrl Pts',(14.9329047154423,-55.0154036283467,
-141.795735565119));
#159964=CARTESIAN_POINT('Ctrl Pts',(14.9337771219422,-55.0089195179454,
-141.778499819894));
#159965=CARTESIAN_POINT('Ctrl Pts',(14.9342133251921,-55.0056774627447,
-141.769881947281));
#159966=CARTESIAN_POINT('Ctrl Pts',(14.9346513968287,-55.0024413634032,
-141.761224265859));
#159967=CARTESIAN_POINT('Ctrl Pts',(14.9350913346392,-54.9992116625344,
-141.752526735865));
#159968=CARTESIAN_POINT('Ctrl Pts',(14.9353113035444,-54.9975968120999,
-141.748177970869));
#159969=CARTESIAN_POINT('Ctrl Pts',(14.9355317389924,-54.9959835612893,
-141.743819243727));
#159970=CARTESIAN_POINT('Ctrl Pts',(14.9357526406798,-54.9943719656216,
-141.739450549905));
#159971=CARTESIAN_POINT('Ctrl Pts',(14.9358630915235,-54.9935661677878,
-141.737266202994));
#159972=CARTESIAN_POINT('Ctrl Pts',(14.935973658927,-54.9927607837399,-141.735079364413));
#159973=CARTESIAN_POINT('Ctrl Pts',(14.9360843428507,-54.9919558204301,
-141.732890033624));
#159974=CARTESIAN_POINT('Ctrl Pts',(14.9361950267743,-54.9911508571203,
-141.730700702836));
#159975=CARTESIAN_POINT('Ctrl Pts',(14.9363961066168,-54.9896918156194,
-141.726722844862));
#159976=CARTESIAN_POINT('Ctrl Pts',(14.9364167441416,-54.9895421996708,
-141.726314564106));
#159977=CARTESIAN_POINT('Ctrl Pts',(14.9368011783469,-54.9867551654281,
-141.718709141974));
#159978=CARTESIAN_POINT('Ctrl Pts',(14.9373927756583,-54.98247714105,-141.707003732738));
#159979=CARTESIAN_POINT('Ctrl Pts',(14.938192167618,-54.9767793478659,-141.691174512061));
#159980=CARTESIAN_POINT('Ctrl Pts',(14.9389948449638,-54.9710581375703,
-141.67528023556));
#159981=CARTESIAN_POINT('Ctrl Pts',(14.9400070303623,-54.963905484254,-141.655228174497));
#159982=CARTESIAN_POINT('Ctrl Pts',(14.9412297078366,-54.9554440189646,
-141.630979039362));
#159983=CARTESIAN_POINT('Ctrl Pts',(14.9424598255056,-54.9469310642593,
-141.606582344228));
#159984=CARTESIAN_POINT('Ctrl Pts',(14.9439030078284,-54.9370933577308,
-141.577937327112));
#159985=CARTESIAN_POINT('Ctrl Pts',(14.9455605682887,-54.926106419147,-141.544988792767));
#159986=CARTESIAN_POINT('Ctrl Pts',(14.9471371826498,-54.9156560219706,
-141.513649282887));
#159987=CARTESIAN_POINT('Ctrl Pts',(14.9489078803818,-54.9041655803484,
-141.478413650684));
#159988=CARTESIAN_POINT('Ctrl Pts',(14.9508734591455,-54.8918308314158,
-141.439232919092));
#159989=CARTESIAN_POINT('Ctrl Pts',(14.952969209833,-54.8786792045088,-141.397457414244));
#159990=CARTESIAN_POINT('Ctrl Pts',(14.9552864041832,-54.8645681869741,
-141.351199207159));
#159991=CARTESIAN_POINT('Ctrl Pts',(14.9578257449883,-54.8497843490626,
-141.300393708248));
#159992=CARTESIAN_POINT('Ctrl Pts',(14.96045217177,-54.8344935036002,-141.247845849083));
#159993=CARTESIAN_POINT('Ctrl Pts',(14.9633163444726,-54.8184826601245,
-141.190431529181));
#159994=CARTESIAN_POINT('Ctrl Pts',(14.966417593519,-54.8021261312926,-141.128095288101));
#159995=CARTESIAN_POINT('Ctrl Pts',(14.9684798402318,-54.7912494821385,
-141.086643374264));
#159996=CARTESIAN_POINT('Ctrl Pts',(14.9706469074253,-54.7802210749185,
-141.043015008737));
#159997=CARTESIAN_POINT('Ctrl Pts',(14.9729182170701,-54.7691629909176,
-140.997198199071));
#159998=CARTESIAN_POINT('Ctrl Pts',(14.9732348851946,-54.7676212624576,
-140.990810376424));
#159999=CARTESIAN_POINT('Ctrl Pts',(14.973638654121,-54.7656694673371,-140.982663044327));
#160000=CARTESIAN_POINT('Ctrl Pts',(14.9738959858372,-54.7644321620716,
-140.977469374413));
#160001=CARTESIAN_POINT('Ctrl Pts',(14.973919883941,-54.764317254939,-140.976987044195));
#160002=CARTESIAN_POINT('Ctrl Pts',(14.9739425188767,-54.7642084743528,
-140.976530198892));
#160003=CARTESIAN_POINT('Ctrl Pts',(14.9739637034869,-54.7641067028186,
-140.976102619019));
#160004=CARTESIAN_POINT('Ctrl Pts',(14.973980599117,-54.7640255356802,-140.975761605838));
#160005=CARTESIAN_POINT('Ctrl Pts',(14.9739974936203,-54.7639444036372,
-140.97542062491));
#160006=CARTESIAN_POINT('Ctrl Pts',(14.9740143869953,-54.7638633066688,
-140.975079676237));
#160007=CARTESIAN_POINT('Ctrl Pts',(14.9784467764848,-54.7425855364503,
-140.885623465218));
#160008=CARTESIAN_POINT('Ctrl Pts',(14.9828067301753,-54.723752431795,-140.798271020784));
#160009=CARTESIAN_POINT('Ctrl Pts',(14.987060775946,-54.707055598208,-140.713150818449));
#160010=CARTESIAN_POINT('Ctrl Pts',(14.9904460357961,-54.6937686888951,
-140.645414357927));
#160011=CARTESIAN_POINT('Ctrl Pts',(14.9937642982209,-54.6818350048517,
-140.579090323978));
#160012=CARTESIAN_POINT('Ctrl Pts',(14.9970000845746,-54.6711088502559,
-140.514222173991));
#160013=CARTESIAN_POINT('Ctrl Pts',(15.0014481308539,-54.6563642327732,
-140.42505172154));
#160014=CARTESIAN_POINT('Ctrl Pts',(15.0057417382206,-54.6439011362337,
-140.338634645609));
#160015=CARTESIAN_POINT('Ctrl Pts',(15.009844873679,-54.6333747825093,-140.255118196318));
#160016=CARTESIAN_POINT('Ctrl Pts',(15.0124918200861,-54.6265841965165,
-140.201241455562));
#160017=CARTESIAN_POINT('Ctrl Pts',(15.0150595760332,-54.6205999746682,
-140.148570745906));
#160018=CARTESIAN_POINT('Ctrl Pts',(15.0175392245295,-54.6153339077643,
-140.097135088049));
#160019=CARTESIAN_POINT('Ctrl Pts',(15.0215328220096,-54.6068526445736,
-140.0142953977));
#160020=CARTESIAN_POINT('Ctrl Pts',(15.0253095877784,-54.6002281891966,
-139.934627798416));
#160021=CARTESIAN_POINT('Ctrl Pts',(15.0289022436262,-54.5951143157021,
-139.858202621515));
#160022=CARTESIAN_POINT('Ctrl Pts',(15.0325973374102,-54.5898546295637,
-139.779598322056));
#160023=CARTESIAN_POINT('Ctrl Pts',(15.0360977006467,-54.586192768118,-139.704423490692));
#160024=CARTESIAN_POINT('Ctrl Pts',(15.0394393505371,-54.5837870670199,
-139.632711391223));
#160025=CARTESIAN_POINT('Ctrl Pts',(15.0429021798406,-54.5812941271455,
-139.55839877093));
#160026=CARTESIAN_POINT('Ctrl Pts',(15.0461945921169,-54.5801499181639,
-139.487804108145));
#160027=CARTESIAN_POINT('Ctrl Pts',(15.0493567599704,-54.5800138479308,
-139.420926064183));
#160028=CARTESIAN_POINT('Ctrl Pts',(15.0495717712766,-54.5800045958481,
-139.416378697866));
#160029=CARTESIAN_POINT('Ctrl Pts',(15.0497861804124,-54.58000002,-139.411848502024));
#160030=CARTESIAN_POINT('Ctrl Pts',(15.05,-54.58000002,-139.407335470919));
#160031=CARTESIAN_POINT('Ctrl Pts',(9.4,-54.58000002,-136.338455187671));
#160032=CARTESIAN_POINT('Ctrl Pts',(9.39704729586323,-54.58000002,-136.419371231505));
#160033=CARTESIAN_POINT('Ctrl Pts',(9.39392227292272,-54.5816877330307,
-136.504488584693));
#160034=CARTESIAN_POINT('Ctrl Pts',(9.39062236601488,-54.5856390342835,
-136.59370256742));
#160035=CARTESIAN_POINT('Ctrl Pts',(9.38788200014251,-54.5889203423347,
-136.66778918878));
#160036=CARTESIAN_POINT('Ctrl Pts',(9.38502102565691,-54.5937636778588,
-136.744700772334));
#160037=CARTESIAN_POINT('Ctrl Pts',(9.38203789209161,-54.6005250600446,
-136.824372403604));
#160038=CARTESIAN_POINT('Ctrl Pts',(9.38011505691329,-54.6048832368531,
-136.875726260872));
#160039=CARTESIAN_POINT('Ctrl Pts',(9.3781413302498,-54.6100392192402,-136.928230353818));
#160040=CARTESIAN_POINT('Ctrl Pts',(9.37611681763369,-54.6160916434082,
-136.981852222139));
#160041=CARTESIAN_POINT('Ctrl Pts',(9.37274205280644,-54.6261807424036,
-137.071237288815));
#160042=CARTESIAN_POINT('Ctrl Pts',(9.36922644791226,-54.6387598086005,
-137.163720894536));
#160043=CARTESIAN_POINT('Ctrl Pts',(9.36557170761357,-54.6542903138158,
-137.259119078051));
#160044=CARTESIAN_POINT('Ctrl Pts',(9.36208319537106,-54.6691144471737,
-137.350178278955));
#160045=CARTESIAN_POINT('Ctrl Pts',(9.35846800862529,-54.6866285757306,
-137.443890153689));
#160046=CARTESIAN_POINT('Ctrl Pts',(9.35473005845707,-54.7072218231019,
-137.540033202452));
#160047=CARTESIAN_POINT('Ctrl Pts',(9.35379931983142,-54.7123494812818,
-137.563972539534));
#160048=CARTESIAN_POINT('Ctrl Pts',(9.35286098194924,-54.717667930619,-137.588062319807));
#160049=CARTESIAN_POINT('Ctrl Pts',(9.35191512681452,-54.7231829278603,
-137.612298620553));
#160050=CARTESIAN_POINT('Ctrl Pts',(9.35183953638586,-54.7236236729493,
-137.614235526423));
#160051=CARTESIAN_POINT('Ctrl Pts',(9.35169854945555,-54.7244483876958,
-137.617847328509));
#160052=CARTESIAN_POINT('Ctrl Pts',(9.35168821144854,-54.7245089317618,
-137.618112143096));
#160053=CARTESIAN_POINT('Ctrl Pts',(9.35168605247973,-54.724521575664,-137.618167446447));
#160054=CARTESIAN_POINT('Ctrl Pts',(9.35168387518485,-54.7245343276891,
-137.618223219001));
#160055=CARTESIAN_POINT('Ctrl Pts',(9.35168167956414,-54.7245471878765,
-137.618279460739));
#160056=CARTESIAN_POINT('Ctrl Pts',(9.35147996024536,-54.7257286980637,
-137.62344658501));
#160057=CARTESIAN_POINT('Ctrl Pts',(9.35112356583562,-54.7278191281679,
-137.63257494496));
#160058=CARTESIAN_POINT('Ctrl Pts',(9.35061244390952,-54.7308764847684,
-137.645648506862));
#160059=CARTESIAN_POINT('Ctrl Pts',(9.35010078023794,-54.7339370819051,
-137.658735925619));
#160060=CARTESIAN_POINT('Ctrl Pts',(9.3494340527294,-54.7379666976379,-137.675777088558));
#160061=CARTESIAN_POINT('Ctrl Pts',(9.34861195666339,-54.7430751320782,
-137.696747673966));
#160062=CARTESIAN_POINT('Ctrl Pts',(9.34779010329173,-54.7481820584367,
-137.717712068561));
#160063=CARTESIAN_POINT('Ctrl Pts',(9.3468129601163,-54.7543672342593,-137.74260384324));
#160064=CARTESIAN_POINT('Ctrl Pts',(9.34568012941133,-54.761791078744,-137.771387080926));
#160065=CARTESIAN_POINT('Ctrl Pts',(9.34531457307779,-54.764186700048,-137.780675225032));
#160066=CARTESIAN_POINT('Ctrl Pts',(9.34493280503381,-54.7667116947109,
-137.790368480995));
#160067=CARTESIAN_POINT('Ctrl Pts',(9.34453481372685,-54.7693725613995,
-137.800465300292));
#160068=CARTESIAN_POINT('Ctrl Pts',(9.34330447756737,-54.777598269965,-137.83167824806));
#160069=CARTESIAN_POINT('Ctrl Pts',(9.34191917788062,-54.7871182467248,
-137.866746870592));
#160070=CARTESIAN_POINT('Ctrl Pts',(9.34037911805495,-54.7981536480039,
-137.905603545057));
#160071=CARTESIAN_POINT('Ctrl Pts',(9.33886990694295,-54.80896800077,-137.943681887146));
#160072=CARTESIAN_POINT('Ctrl Pts',(9.33721203400933,-54.8212380911684,
-137.985398920108));
#160073=CARTESIAN_POINT('Ctrl Pts',(9.33540626469946,-54.8352146572672,
-138.030666056994));
#160074=CARTESIAN_POINT('Ctrl Pts',(9.3336674674978,-54.8486728625257,-138.074254332924));
#160075=CARTESIAN_POINT('Ctrl Pts',(9.33179153704424,-54.8637135838245,
-138.121134219645));
#160076=CARTESIAN_POINT('Ctrl Pts',(9.32978002863578,-54.8805951415112,
-138.171196804022));
#160077=CARTESIAN_POINT('Ctrl Pts',(9.32933487316683,-54.8843311028907,
-138.18227586943));
#160078=CARTESIAN_POINT('Ctrl Pts',(9.32888308122865,-54.8881573501098,
-138.193510690821));
#160079=CARTESIAN_POINT('Ctrl Pts',(9.3284245409003,-54.8920769088252,-138.204899835357));
#160080=CARTESIAN_POINT('Ctrl Pts',(9.32819527073613,-54.8940366881829,
-138.210594407626));
#160081=CARTESIAN_POINT('Ctrl Pts',(9.32796379497366,-54.8960198682933,
-138.216327536038));
#160082=CARTESIAN_POINT('Ctrl Pts',(9.32773086568275,-54.8980267301276,
-138.222099070016));
#160083=CARTESIAN_POINT('Ctrl Pts',(9.32751634870292,-54.8998749559901,
-138.2274143828));
#160084=CARTESIAN_POINT('Ctrl Pts',(9.32723514384213,-54.9023128701556,
-138.234385797297));
#160085=CARTESIAN_POINT('Ctrl Pts',(9.32706811894936,-54.903767122238,-138.238527565011));
#160086=CARTESIAN_POINT('Ctrl Pts',(9.32705378295467,-54.9038919428547,
-138.238883059087));
#160087=CARTESIAN_POINT('Ctrl Pts',(9.32704028811105,-54.9040094863335,
-138.239217715686));
#160088=CARTESIAN_POINT('Ctrl Pts',(9.3270277487768,-54.904118743943,-138.239528702318));
#160089=CARTESIAN_POINT('Ctrl Pts',(9.32430541485895,-54.9278389582856,
-138.307045002644));
#160090=CARTESIAN_POINT('Ctrl Pts',(9.3217228284678,-54.9516402280944,-138.370752091378));
#160091=CARTESIAN_POINT('Ctrl Pts',(9.31928109292825,-54.9751497452016,
-138.430727718388));
#160092=CARTESIAN_POINT('Ctrl Pts',(9.31678872725691,-54.9991467393225,
-138.491946958333));
#160093=CARTESIAN_POINT('Ctrl Pts',(9.31444308648543,-55.0228397485265,
-138.549279020443));
#160094=CARTESIAN_POINT('Ctrl Pts',(9.31224377986652,-55.0458832512665,
-138.602828549886));
#160095=CARTESIAN_POINT('Ctrl Pts',(9.3099917528066,-55.0694791388429,-138.65766173609));
#160096=CARTESIAN_POINT('Ctrl Pts',(9.30789313238485,-55.0923939685203,
-138.708529504678));
#160097=CARTESIAN_POINT('Ctrl Pts',(9.30594629905539,-55.1143100558499,
-138.755557219429));
#160098=CARTESIAN_POINT('Ctrl Pts',(9.30471092027362,-55.1282170857209,
-138.785399034894));
#160099=CARTESIAN_POINT('Ctrl Pts',(9.30353663826253,-55.1417230294578,
-138.813694821712));
#160100=CARTESIAN_POINT('Ctrl Pts',(9.30242287129985,-55.1547575084923,
-138.840477529059));
#160101=CARTESIAN_POINT('Origin',(-3.3975957231091E-14,-70.08000002,-174.34995));
#160102=CARTESIAN_POINT('',(16.05,-70.08000002,-177.34995));
#160103=CARTESIAN_POINT('Origin',(16.05,-70.08000002,-174.34995));
#160104=CARTESIAN_POINT('',(16.55,-70.08000002,-177.34995));
#160105=CARTESIAN_POINT('',(-41.5,-70.08000002,-177.34995));
#160106=CARTESIAN_POINT('Origin',(16.55,-70.08000002,-174.34995));
#160107=CARTESIAN_POINT('Ctrl Pts',(23.0246263600192,-55.5929437980769,
-150.090116786386));
#160108=CARTESIAN_POINT('Ctrl Pts',(23.9800829025888,-54.5800000200001,
-149.152655882413));
#160109=CARTESIAN_POINT('Ctrl Pts',(25.1782808829885,-54.58000002,-147.977025477683));
#160110=CARTESIAN_POINT('Ctrl Pts',(21.9091489271198,-55.5502169050949,
-148.872607854072));
#160111=CARTESIAN_POINT('Ctrl Pts',(22.8379194752343,-54.5800000199763,
-147.932452641776));
#160112=CARTESIAN_POINT('Ctrl Pts',(23.9836910796608,-54.58000002,-146.759504150767));
#160113=CARTESIAN_POINT('Ctrl Pts',(20.7612402155903,-55.5070450251362,
-147.681892304448));
#160114=CARTESIAN_POINT('Ctrl Pts',(21.6573291961429,-54.58000002,-146.736008441848));
#160115=CARTESIAN_POINT('Ctrl Pts',(22.7503247929853,-54.58000002,-145.568800995698));
#160116=CARTESIAN_POINT('Ctrl Pts',(18.3837542309683,-55.4210082419989,
-145.38143269084));
#160117=CARTESIAN_POINT('Ctrl Pts',(19.2052975266984,-54.58000002,-144.424597244368));
#160118=CARTESIAN_POINT('Ctrl Pts',(20.1860325764608,-54.58000002,-143.268341382183));
#160119=CARTESIAN_POINT('Ctrl Pts',(17.165895474142,-55.3785603713206,-144.282911778325));
#160120=CARTESIAN_POINT('Ctrl Pts',(17.9461389525456,-54.58000002,-143.320329501862));
#160121=CARTESIAN_POINT('Ctrl Pts',(18.8677311043704,-54.58000002,-142.169807438416));
#160122=CARTESIAN_POINT('Ctrl Pts',(15.9085533562516,-55.3376384323294,
-143.252961163042));
#160123=CARTESIAN_POINT('Ctrl Pts',(16.6396978513013,-54.5800000199999,
-142.283025361002));
#160124=CARTESIAN_POINT('Ctrl Pts',(17.5014165897211,-54.58000002,-141.139869854338));
#160125=CARTESIAN_POINT('',(22.984916421119,-55.5914230669928,-150.046801054874));
#160126=CARTESIAN_POINT('',(17.3782102443508,-55.3867109640869,-144.502505142991));
#160127=CARTESIAN_POINT('Ctrl Pts',(22.9849164538399,-55.5914231005407,
-150.046800950003));
#160128=CARTESIAN_POINT('Ctrl Pts',(22.6020780769818,-55.5767655125104,
-149.629451903776));
#160129=CARTESIAN_POINT('Ctrl Pts',(22.2213190936165,-55.5622829699053,
-149.221717836613));
#160130=CARTESIAN_POINT('Ctrl Pts',(21.8422215127712,-55.5479851256212,
-148.82334844634));
#160131=CARTESIAN_POINT('Ctrl Pts',(21.4142808369546,-55.5318451409448,
-148.3736529729));
#160132=CARTESIAN_POINT('Ctrl Pts',(20.9884579263804,-55.5159405513025,
-147.935890439072));
#160133=CARTESIAN_POINT('Ctrl Pts',(20.5641624498949,-55.5002788324557,
-147.509629730204));
#160134=CARTESIAN_POINT('Ctrl Pts',(20.2327692252654,-55.4880463487279,
-147.176701573593));
#160135=CARTESIAN_POINT('Ctrl Pts',(19.9023081409924,-55.4759618754942,
-146.850788120774));
#160136=CARTESIAN_POINT('Ctrl Pts',(19.5724972232793,-55.4640266335675,
-146.531662497644));
#160137=CARTESIAN_POINT('Ctrl Pts',(19.0486801775887,-55.4450706717427,
-146.024816204406));
#160138=CARTESIAN_POINT('Ctrl Pts',(18.5287744522527,-55.4265728425626,
-145.537272372091));
#160139=CARTESIAN_POINT('Ctrl Pts',(18.0112485729538,-55.4085493182614,
-145.068100484788));
#160140=CARTESIAN_POINT('Ctrl Pts',(17.7998985115879,-55.4011887724037,
-144.876497492283));
#160141=CARTESIAN_POINT('Ctrl Pts',(17.5889457822771,-55.3939071830409,
-144.687958082283));
#160142=CARTESIAN_POINT('Ctrl Pts',(17.3782871134249,-55.3867051178887,
-144.502418094197));
#160143=CARTESIAN_POINT('Ctrl Pts',(22.9849163130661,-55.5914230820925,
-150.046801040559));
#160144=CARTESIAN_POINT('Ctrl Pts',(22.9923323585403,-55.5151362910079,
-149.910354009793));
#160145=CARTESIAN_POINT('Ctrl Pts',(23.0003039790552,-55.4387315810897,
-149.763483417317));
#160146=CARTESIAN_POINT('Ctrl Pts',(23.0088478791706,-55.3639556534274,
-149.605771335223));
#160147=CARTESIAN_POINT('Ctrl Pts',(23.0145515654438,-55.3140371821896,
-149.500486836855));
#160148=CARTESIAN_POINT('Ctrl Pts',(23.0205099502732,-55.2648492749479,
-149.390375691817));
#160149=CARTESIAN_POINT('Ctrl Pts',(23.0267233715385,-55.2169338992284,
-149.275390145685));
#160150=CARTESIAN_POINT('Ctrl Pts',(23.0294188144066,-55.1961477409682,
-149.225508292028));
#160151=CARTESIAN_POINT('Ctrl Pts',(23.0321622052024,-55.1756010871455,
-149.174709924356));
#160152=CARTESIAN_POINT('Ctrl Pts',(23.0349533325796,-55.1553378636498,
-149.122995219546));
#160153=CARTESIAN_POINT('Ctrl Pts',(23.0350402445946,-55.1547068936707,
-149.121384892037));
#160154=CARTESIAN_POINT('Ctrl Pts',(23.0351272028841,-55.1540761984596,
-149.11977367623));
#160155=CARTESIAN_POINT('Ctrl Pts',(23.0352142074399,-55.1534457793315,
-149.118161572165));
#160156=CARTESIAN_POINT('Ctrl Pts',(23.0352372417001,-55.1532788772866,
-149.117734771243));
#160157=CARTESIAN_POINT('Ctrl Pts',(23.0352602792032,-55.1531119945928,
-149.117307908062));
#160158=CARTESIAN_POINT('Ctrl Pts',(23.035283319949,-55.1529451312743,-149.116880982623));
#160159=CARTESIAN_POINT('Ctrl Pts',(23.0353061707342,-55.1527796436693,
-149.116457576993));
#160160=CARTESIAN_POINT('Ctrl Pts',(23.0353294471293,-55.1526111157677,
-149.116026283041));
#160161=CARTESIAN_POINT('Ctrl Pts',(23.0353532502873,-55.1524388205629,
-149.115585226208));
#160162=CARTESIAN_POINT('Ctrl Pts',(23.035511384165,-55.1512941947592,-149.112655109648));
#160163=CARTESIAN_POINT('Ctrl Pts',(23.0356895098257,-55.1500072136442,
-149.109354439163));
#160164=CARTESIAN_POINT('Ctrl Pts',(23.0358496447262,-55.1488523761523,
-149.106387027815));
#160165=CARTESIAN_POINT('Ctrl Pts',(23.0359290866495,-55.1482794684903,
-149.104914913591));
#160166=CARTESIAN_POINT('Ctrl Pts',(23.0360041000042,-55.1477390217724,
-149.103524837171));
#160167=CARTESIAN_POINT('Ctrl Pts',(23.0360700429472,-55.1472642440113,
-149.102302828729));
#160168=CARTESIAN_POINT('Ctrl Pts',(23.0361056558454,-55.1470078373164,
-149.101642875439));
#160169=CARTESIAN_POINT('Ctrl Pts',(23.0361386232162,-55.1467705806098,
-149.101031941976));
#160170=CARTESIAN_POINT('Ctrl Pts',(23.0361682136977,-55.14655769005,-149.100483583949));
#160171=CARTESIAN_POINT('Ctrl Pts',(23.0361856980364,-55.146431897888,-149.100159571734));
#160172=CARTESIAN_POINT('Ctrl Pts',(23.0362016408016,-55.1463172195784,
-149.099864126125));
#160173=CARTESIAN_POINT('Ctrl Pts',(23.0362178547074,-55.1462006107733,
-149.099563654823));
#160174=CARTESIAN_POINT('Ctrl Pts',(23.0396466113122,-55.1215413326975,
-149.036022952368));
#160175=CARTESIAN_POINT('Ctrl Pts',(23.043400856158,-55.0954814004763,-148.966402766032));
#160176=CARTESIAN_POINT('Ctrl Pts',(23.047485051108,-55.06851563719,-148.890588284903));
#160177=CARTESIAN_POINT('Ctrl Pts',(23.0510706678576,-55.0448417201287,
-148.824028858447));
#160178=CARTESIAN_POINT('Ctrl Pts',(23.0549106126203,-55.0204708888616,
-148.752694757299));
#160179=CARTESIAN_POINT('Ctrl Pts',(23.0590081665062,-54.9957694317052,
-148.676498447966));
#160180=CARTESIAN_POINT('Ctrl Pts',(23.0640392087417,-54.9654405873036,
-148.582943399974));
#160181=CARTESIAN_POINT('Ctrl Pts',(23.0694582576189,-54.9346164108002,
-148.482065220825));
#160182=CARTESIAN_POINT('Ctrl Pts',(23.0752666835093,-54.9040407392492,
-148.373778900728));
#160183=CARTESIAN_POINT('Ctrl Pts',(23.0796325654284,-54.8810586483851,
-148.292385887212));
#160184=CARTESIAN_POINT('Ctrl Pts',(23.0842183659314,-54.8582185778991,
-148.206808519094));
#160185=CARTESIAN_POINT('Ctrl Pts',(23.0890230063924,-54.8358481589629,
-148.117037145628));
#160186=CARTESIAN_POINT('Ctrl Pts',(23.0891989614022,-54.8350289119632,
-148.113749548352));
#160187=CARTESIAN_POINT('Ctrl Pts',(23.0893167643732,-54.8344810902222,
-148.111548434336));
#160188=CARTESIAN_POINT('Ctrl Pts',(23.0895517726634,-54.8333923203654,
-148.107157489765));
#160189=CARTESIAN_POINT('Ctrl Pts',(23.0896456095871,-54.8329575833015,
-148.105404220845));
#160190=CARTESIAN_POINT('Ctrl Pts',(23.0897393535851,-54.8325239285302,
-148.103653010558));
#160191=CARTESIAN_POINT('Ctrl Pts',(23.0898330043309,-54.8320913515626,
-148.101903859584));
#160192=CARTESIAN_POINT('Ctrl Pts',(23.0938754387013,-54.8134191670809,
-148.026401759117));
#160193=CARTESIAN_POINT('Ctrl Pts',(23.0977452975731,-54.7967897346283,
-147.954711586754));
#160194=CARTESIAN_POINT('Ctrl Pts',(23.101415260951,-54.7818805610517,-147.88691339402));
#160195=CARTESIAN_POINT('Ctrl Pts',(23.1044740759873,-54.7694541688457,
-147.830405437396));
#160196=CARTESIAN_POINT('Ctrl Pts',(23.107394083234,-54.7582234867518,-147.776600243719));
#160197=CARTESIAN_POINT('Ctrl Pts',(23.1101606721181,-54.7480218486682,
-147.72552530494));
#160198=CARTESIAN_POINT('Ctrl Pts',(23.1136624974754,-54.735109068192,-147.660876915449));
#160199=CARTESIAN_POINT('Ctrl Pts',(23.1169202344087,-54.7238435469161,
-147.600604046303));
#160200=CARTESIAN_POINT('Ctrl Pts',(23.1199182264117,-54.7139339125423,
-147.544776848901));
#160201=CARTESIAN_POINT('Ctrl Pts',(23.1221963802289,-54.7064036485017,
-147.502354139724));
#160202=CARTESIAN_POINT('Ctrl Pts',(23.1243245925392,-54.6996572049997,
-147.462497765974));
#160203=CARTESIAN_POINT('Ctrl Pts',(23.1262966067565,-54.6935835813359,
-147.42522765844));
#160204=CARTESIAN_POINT('Ctrl Pts',(23.1289486271487,-54.6854156007658,
-147.375105765641));
#160205=CARTESIAN_POINT('Ctrl Pts',(23.1313298271167,-54.6784587434828,
-147.329648473762));
#160206=CARTESIAN_POINT('Ctrl Pts',(23.1334524318317,-54.6724823078343,
-147.28888161716));
#160207=CARTESIAN_POINT('Ctrl Pts',(23.1349852367621,-54.6681665207434,
-147.259442485911));
#160208=CARTESIAN_POINT('Ctrl Pts',(23.1363832071279,-54.6643630279866,
-147.232448787815));
#160209=CARTESIAN_POINT('Ctrl Pts',(23.1376511232448,-54.6610006647087,
-147.207904179543));
#160210=CARTESIAN_POINT('Ctrl Pts',(23.1391629766815,-54.6569914085686,
-147.178637377213));
#160211=CARTESIAN_POINT('Ctrl Pts',(23.1404905826859,-54.653608787909,-147.152853815656));
#160212=CARTESIAN_POINT('Ctrl Pts',(23.1416434646309,-54.6507567724492,
-147.130558272819));
#160213=CARTESIAN_POINT('Ctrl Pts',(23.1422199056034,-54.6493307647194,
-147.1194105014));
#160214=CARTESIAN_POINT('Ctrl Pts',(23.1427526592662,-54.6480378218892,
-147.109134681098));
#160215=CARTESIAN_POINT('Ctrl Pts',(23.1432428112175,-54.6468684071695,
-147.099731151217));
#160216=CARTESIAN_POINT('Ctrl Pts',(23.1434878871932,-54.6462836998097,
-147.095029386276));
#160217=CARTESIAN_POINT('Ctrl Pts',(23.1437223155898,-54.6457298994562,
-147.090545691006));
#160218=CARTESIAN_POINT('Ctrl Pts',(23.1439462156013,-54.6452059677569,
-147.086280097254));
#160219=CARTESIAN_POINT('Ctrl Pts',(23.144058165607,-54.6449440019072,-147.084147300378));
#160220=CARTESIAN_POINT('Ctrl Pts',(23.1441674836954,-54.6446895047668,
-147.082069028698));
#160221=CARTESIAN_POINT('Ctrl Pts',(23.1442741846894,-54.6444423559743,
-147.080045285498));
#160222=CARTESIAN_POINT('Ctrl Pts',(23.1443275351864,-54.644318781578,-147.079033413898));
#160223=CARTESIAN_POINT('Ctrl Pts',(23.1443802314206,-54.6441970443651,
-147.078035174407));
#160224=CARTESIAN_POINT('Ctrl Pts',(23.1444322751837,-54.6440771298857,
-147.0770505674));
#160225=CARTESIAN_POINT('Ctrl Pts',(23.1444452861244,-54.6440471512658,
-147.076804415648));
#160226=CARTESIAN_POINT('Ctrl Pts',(23.144451223023,-54.6440334560348,-147.076691896758));
#160227=CARTESIAN_POINT('Ctrl Pts',(23.1444553594622,-54.6440239044945,
-147.076613426546));
#160228=CARTESIAN_POINT('Ctrl Pts',(23.1444615641209,-54.644009577184,-147.076495721228));
#160229=CARTESIAN_POINT('Ctrl Pts',(23.1444637176774,-54.6440045725571,
-147.076454625506));
#160230=CARTESIAN_POINT('Ctrl Pts',(23.1444796267811,-54.6439679929986,
-147.076154034201));
#160231=CARTESIAN_POINT('Ctrl Pts',(23.1444955358848,-54.6439314134401,
-147.075853442895));
#160232=CARTESIAN_POINT('Ctrl Pts',(23.144525196082,-54.6438632191539,-147.075293360595));
#160233=CARTESIAN_POINT('Ctrl Pts',(23.1445864508551,-54.6437228405878,
-147.074137644174));
#160234=CARTESIAN_POINT('Ctrl Pts',(23.1503046784119,-54.630618284894,-146.966249733404));
#160235=CARTESIAN_POINT('Ctrl Pts',(23.1558442763692,-54.61994345285,-146.86156040566));
#160236=CARTESIAN_POINT('Ctrl Pts',(23.1612011702211,-54.6113286071025,
-146.760176180277));
#160237=CARTESIAN_POINT('Ctrl Pts',(23.1666962989783,-54.6024914548433,
-146.656175730048));
#160238=CARTESIAN_POINT('Ctrl Pts',(23.1719991942556,-54.5958218840169,
-146.555652779676));
#160239=CARTESIAN_POINT('Ctrl Pts',(23.1771079416158,-54.5909508424003,
-146.458674807921));
#160240=CARTESIAN_POINT('Ctrl Pts',(23.1824197384654,-54.5858861990172,
-146.357842402532));
#160241=CARTESIAN_POINT('Ctrl Pts',(23.1875216668299,-54.5827657185001,
-146.260842041119));
#160242=CARTESIAN_POINT('Ctrl Pts',(23.1924139148337,-54.5812088322433,
-146.167704256954));
#160243=CARTESIAN_POINT('Ctrl Pts',(23.1950011320887,-54.580385488254,-146.118449255553));
#160244=CARTESIAN_POINT('Ctrl Pts',(23.1975297444135,-54.58000002,-146.07027379222));
#160245=CARTESIAN_POINT('Ctrl Pts',(23.2,-54.58000002,-146.023178055809));
#160246=CARTESIAN_POINT('Ctrl Pts',(17.55,-54.58000002,-141.176536909659));
#160247=CARTESIAN_POINT('Ctrl Pts',(17.5450917051411,-54.58000002,-141.274872500695));
#160248=CARTESIAN_POINT('Ctrl Pts',(17.5399505125397,-54.5819438994493,
-141.377555492718));
#160249=CARTESIAN_POINT('Ctrl Pts',(17.5345757892522,-54.586403208251,-141.484515818682));
#160250=CARTESIAN_POINT('Ctrl Pts',(17.5299889335016,-54.5902088378856,
-141.575797092152));
#160251=CARTESIAN_POINT('Ctrl Pts',(17.5252317046863,-54.5958480133051,
-141.670199207096));
#160252=CARTESIAN_POINT('Ctrl Pts',(17.5203055297054,-54.6037022322593,
-141.767641241343));
#160253=CARTESIAN_POINT('Ctrl Pts',(17.5179769395429,-54.607414901229,-141.813701838711));
#160254=CARTESIAN_POINT('Ctrl Pts',(17.5156106073861,-54.6116228337644,
-141.860441523156));
#160255=CARTESIAN_POINT('Ctrl Pts',(17.5132068481431,-54.6163676372864,
-141.907848522614));
#160256=CARTESIAN_POINT('Ctrl Pts',(17.5121552034742,-54.6184434888273,
-141.928589084877));
#160257=CARTESIAN_POINT('Ctrl Pts',(17.5110963946809,-54.6206221127213,
-141.949457382844));
#160258=CARTESIAN_POINT('Ctrl Pts',(17.510030454982,-54.6229070275371,-141.970452299473));
#160259=CARTESIAN_POINT('Ctrl Pts',(17.5095307957482,-54.623978081357,-141.980293666643));
#160260=CARTESIAN_POINT('Ctrl Pts',(17.509029569696,-54.6250724904199,-141.990162854726));
#160261=CARTESIAN_POINT('Ctrl Pts',(17.5085267804883,-54.6261906184793,
-142.000059744165));
#160262=CARTESIAN_POINT('Ctrl Pts',(17.5082832419657,-54.626732211758,-142.004853549987));
#160263=CARTESIAN_POINT('Ctrl Pts',(17.5080393366981,-54.627279369982,-142.009653855059));
#160264=CARTESIAN_POINT('Ctrl Pts',(17.5077950651136,-54.6278321345572,
-142.01446064557));
#160265=CARTESIAN_POINT('Ctrl Pts',(17.5076748376931,-54.6281041983715,
-142.016826487775));
#160266=CARTESIAN_POINT('Ctrl Pts',(17.5075545215335,-54.6283776203157,
-142.019193901055));
#160267=CARTESIAN_POINT('Ctrl Pts',(17.5074341166875,-54.6286524053284,
-142.021562883736));
#160268=CARTESIAN_POINT('Ctrl Pts',(17.5074008878149,-54.6287282394536,
-142.022216666587));
#160269=CARTESIAN_POINT('Ctrl Pts',(17.5073676521877,-54.628804177394,-142.022870568969));
#160270=CARTESIAN_POINT('Ctrl Pts',(17.507334409807,-54.6288802192535,-142.023524590846));
#160271=CARTESIAN_POINT('Ctrl Pts',(17.5073152865459,-54.6289239636637,
-142.023900828374));
#160272=CARTESIAN_POINT('Ctrl Pts',(17.5072956614674,-54.6289688853366,
-142.024286934388));
#160273=CARTESIAN_POINT('Ctrl Pts',(17.5072756270475,-54.6290147768759,
-142.024681088858));
#160274=CARTESIAN_POINT('Ctrl Pts',(17.5071508485213,-54.6293005989114,
-142.027135964734));
#160275=CARTESIAN_POINT('Ctrl Pts',(17.5070105236846,-54.6296234749094,
-142.029896478475));
#160276=CARTESIAN_POINT('Ctrl Pts',(17.5068832231264,-54.6299177400483,
-142.032400569581));
#160277=CARTESIAN_POINT('Ctrl Pts',(17.5068200701151,-54.6300637231445,
-142.033642833528));
#160278=CARTESIAN_POINT('Ctrl Pts',(17.5067601224481,-54.6302026255319,
-142.034821996459));
#160279=CARTESIAN_POINT('Ctrl Pts',(17.5067068681503,-54.6303262282003,
-142.035869470081));
#160280=CARTESIAN_POINT('Ctrl Pts',(17.506674018948,-54.6304024708555,-142.036515590195));
#160281=CARTESIAN_POINT('Ctrl Pts',(17.5066437164855,-54.6304728896107,
-142.037111604628));
#160282=CARTESIAN_POINT('Ctrl Pts',(17.506616779378,-54.6305355398635,-142.037641418545));
#160283=CARTESIAN_POINT('Ctrl Pts',(17.5066046036626,-54.6305638581099,
-142.037880897245));
#160284=CARTESIAN_POINT('Ctrl Pts',(17.5065931155187,-54.6305905890773,
-142.038106850617));
#160285=CARTESIAN_POINT('Ctrl Pts',(17.506582390544,-54.6306155528778,-142.038317792377));
#160286=CARTESIAN_POINT('Ctrl Pts',(17.506573757314,-54.630635647865,-142.038487593124));
#160287=CARTESIAN_POINT('Ctrl Pts',(17.5065651450398,-54.6306557000247,
-142.038656980808));
#160288=CARTESIAN_POINT('Ctrl Pts',(17.506556518266,-54.6306757918954,-142.038826652775));
#160289=CARTESIAN_POINT('Ctrl Pts',(17.5040536558753,-54.6365049916146,
-142.088053118458));
#160290=CARTESIAN_POINT('Ctrl Pts',(17.5013190433547,-54.6433710812195,
-142.141762487752));
#160291=CARTESIAN_POINT('Ctrl Pts',(17.4983522495595,-54.6515789268995,
-142.199919204864));
#160292=CARTESIAN_POINT('Ctrl Pts',(17.4954972359002,-54.6594775248973,
-142.255884746523));
#160293=CARTESIAN_POINT('Ctrl Pts',(17.4924272058954,-54.6686189847917,
-142.315968772406));
#160294=CARTESIAN_POINT('Ctrl Pts',(17.4891419225996,-54.679319857396,-142.380131530805));
#160295=CARTESIAN_POINT('Ctrl Pts',(17.4857310844324,-54.690429689156,-142.446746420771));
#160296=CARTESIAN_POINT('Ctrl Pts',(17.4820881710593,-54.703220657768,-142.517758749746));
#160297=CARTESIAN_POINT('Ctrl Pts',(17.4782149173148,-54.7180889605125,
-142.593080227175));
#160298=CARTESIAN_POINT('Ctrl Pts',(17.4745803202652,-54.7320411291163,
-142.663760651876));
#160299=CARTESIAN_POINT('Ctrl Pts',(17.4707427448971,-54.7478238397983,
-142.738238326382));
#160300=CARTESIAN_POINT('Ctrl Pts',(17.4667050220054,-54.7657948260213,
-142.816410456738));
#160301=CARTESIAN_POINT('Ctrl Pts',(17.4659350887227,-54.7692216239439,
-142.831316711218));
#160302=CARTESIAN_POINT('Ctrl Pts',(17.4652069807158,-54.7725054352608,
-142.845407203427));
#160303=CARTESIAN_POINT('Ctrl Pts',(17.464419503232,-54.7761059998999,-142.860639856961));
#160304=CARTESIAN_POINT('Ctrl Pts',(17.4640753193298,-54.7776797037997,
-142.867297614473));
#160305=CARTESIAN_POINT('Ctrl Pts',(17.4637197951665,-54.7793145283239,
-142.874173452564));
#160306=CARTESIAN_POINT('Ctrl Pts',(17.4633444876872,-54.7810519867353,
-142.881430292926));
#160307=CARTESIAN_POINT('Ctrl Pts',(17.4633288972216,-54.7811241616509,
-142.881731745805));
#160308=CARTESIAN_POINT('Ctrl Pts',(17.4633132725516,-54.7811965147846,
-142.882033857305));
#160309=CARTESIAN_POINT('Ctrl Pts',(17.4632976130715,-54.7812690492069,
-142.882336639101));
#160310=CARTESIAN_POINT('Ctrl Pts',(17.4594620331563,-54.7990353844282,
-142.956498984717));
#160311=CARTESIAN_POINT('Ctrl Pts',(17.4558121806766,-54.8170427731732,
-143.026475741498));
#160312=CARTESIAN_POINT('Ctrl Pts',(17.4523678570115,-54.8349227405346,
-143.092287995376));
#160313=CARTESIAN_POINT('Ctrl Pts',(17.4488287514492,-54.8532947340214,
-143.159911289936));
#160314=CARTESIAN_POINT('Ctrl Pts',(17.4455065947382,-54.8715319753916,
-143.223138340297));
#160315=CARTESIAN_POINT('Ctrl Pts',(17.4424195593159,-54.889281955583,-143.282020423993));
#160316=CARTESIAN_POINT('Ctrl Pts',(17.4406460230073,-54.8994795173338,
-143.315848838337));
#160317=CARTESIAN_POINT('Ctrl Pts',(17.4389500348636,-54.9095171355183,
-143.348243606101));
#160318=CARTESIAN_POINT('Ctrl Pts',(17.4373346637261,-54.9193351262199,
-143.379217340403));
#160319=CARTESIAN_POINT('Ctrl Pts',(17.4344710960841,-54.9367394736354,
-143.434124464369));
#160320=CARTESIAN_POINT('Ctrl Pts',(17.4318523790683,-54.9534516177662,
-143.484562021165));
#160321=CARTESIAN_POINT('Ctrl Pts',(17.4294659557099,-54.9691829188542,
-143.530596689604));
#160322=CARTESIAN_POINT('Ctrl Pts',(17.4288674276149,-54.9731284156327,
-143.542142437474));
#160323=CARTESIAN_POINT('Ctrl Pts',(17.4282835109883,-54.9770124679958,
-143.553411265062));
#160324=CARTESIAN_POINT('Ctrl Pts',(17.4277140070979,-54.9808310311818,
-143.564404279982));
#160325=CARTESIAN_POINT('Ctrl Pts',(17.4262939054524,-54.9903529114631,
-143.591816206117));
#160326=CARTESIAN_POINT('Ctrl Pts',(17.4249630047959,-54.9994670858898,
-143.617512975608));
#160327=CARTESIAN_POINT('Ctrl Pts',(17.423716451303,-55.0081165229018,-143.641510951399));
#160328=CARTESIAN_POINT('Ctrl Pts',(17.4230931745566,-55.0124412414077,
-143.653509939294));
#160329=CARTESIAN_POINT('Ctrl Pts',(17.422491013171,-55.0166498780522,-143.665084192978));
#160330=CARTESIAN_POINT('Ctrl Pts',(17.4219092597331,-55.0207360609758,
-143.676235714181));
#160331=CARTESIAN_POINT('Ctrl Pts',(17.4216183830142,-55.0227791524376,
-143.681811474783));
#160332=CARTESIAN_POINT('Ctrl Pts',(17.4213326100765,-55.0247916370273,
-143.687281550016));
#160333=CARTESIAN_POINT('Ctrl Pts',(17.4210518583609,-55.0267727596454,
-143.692646178384));
#160334=CARTESIAN_POINT('Ctrl Pts',(17.4209114825031,-55.0277633209545,
-143.695328492568));
#160335=CARTESIAN_POINT('Ctrl Pts',(17.4207723620668,-55.0287460421781,
-143.697984444891));
#160336=CARTESIAN_POINT('Ctrl Pts',(17.420634486589,-55.0297208317899,-143.700614064785));
#160337=CARTESIAN_POINT('Ctrl Pts',(17.4205655488501,-55.0302082265958,
-143.701928874731));
#160338=CARTESIAN_POINT('Ctrl Pts',(17.4204969223581,-55.0306936385243,
-143.703237101561));
#160339=CARTESIAN_POINT('Ctrl Pts',(17.4204286057972,-55.0311770563127,
-143.704538748928));
#160340=CARTESIAN_POINT('Ctrl Pts',(17.4203602892364,-55.0316604741012,
-143.705840396294));
#160341=CARTESIAN_POINT('Ctrl Pts',(17.4203512686763,-55.0317241749196,
-143.706012785973));
#160342=CARTESIAN_POINT('Ctrl Pts',(17.4202245846065,-55.0326213161048,
-143.708423956259));
#160343=CARTESIAN_POINT('Ctrl Pts',(17.4153263458864,-55.0673092740967,
-143.801651839429));
#160344=CARTESIAN_POINT('Ctrl Pts',(17.4106301495559,-55.1027402694995,
-143.89080847027));
#160345=CARTESIAN_POINT('Ctrl Pts',(17.4061366729319,-55.1384916270083,
-143.975935221091));
#160346=CARTESIAN_POINT('Ctrl Pts',(17.4015130535561,-55.1752784366707,
-144.063527463676));
#160347=CARTESIAN_POINT('Ctrl Pts',(17.3971040350605,-55.2124042647293,
-144.146853581447));
#160348=CARTESIAN_POINT('Ctrl Pts',(17.392907680499,-55.2494458827254,-144.226000408684));
#160349=CARTESIAN_POINT('Ctrl Pts',(17.3885528009809,-55.2878868154835,
-144.308137151852));
#160350=CARTESIAN_POINT('Ctrl Pts',(17.3844269236483,-55.3262368051947,
-144.385773482634));
#160351=CARTESIAN_POINT('Ctrl Pts',(17.3805255402537,-55.364065723145,-144.459041732615));
#160352=CARTESIAN_POINT('Ctrl Pts',(17.3797455324459,-55.3716288996847,
-144.473690333193));
#160353=CARTESIAN_POINT('Ctrl Pts',(17.3789744919001,-55.3791713871413,
-144.488164422799));
#160354=CARTESIAN_POINT('Ctrl Pts',(17.3782123737203,-55.3866899569193,
-144.502465186451));
#160355=CARTESIAN_POINT('Ctrl Pts',(41.5,-55.58000002,-171.14995));
#160356=CARTESIAN_POINT('Ctrl Pts',(41.5,-54.58000002,-171.14995));
#160357=CARTESIAN_POINT('Ctrl Pts',(42.5,-54.58000002,-171.14995));
#160358=CARTESIAN_POINT('Ctrl Pts',(41.5,-55.58000002,-171.64995));
#160359=CARTESIAN_POINT('Ctrl Pts',(41.5,-54.58000002,-171.64995));
#160360=CARTESIAN_POINT('Ctrl Pts',(42.5,-54.58000002,-171.64995));
#160361=CARTESIAN_POINT('Ctrl Pts',(42.,-55.58000002,-171.64995));
#160362=CARTESIAN_POINT('Ctrl Pts',(42.,-55.08000002,-171.64995));
#160363=CARTESIAN_POINT('Ctrl Pts',(42.5,-55.08000002,-171.64995));
#160364=CARTESIAN_POINT('',(41.5,-55.58000002,-171.14995));
#160365=CARTESIAN_POINT('',(42.,-55.58000002,-171.64995));
#160366=CARTESIAN_POINT('Origin',(42.,-55.58000002,-171.14995));
#160367=CARTESIAN_POINT('',(42.5,-55.08000002,-171.64995));
#160368=CARTESIAN_POINT('Origin',(42.5,-55.58000002,-171.64995));
#160369=CARTESIAN_POINT('',(42.5,-54.58000002,-171.14995));
#160370=CARTESIAN_POINT('Origin',(42.5,-55.08000002,-171.14995));
#160371=CARTESIAN_POINT('Origin',(42.5,-55.58000002,-171.14995));
#160372=CARTESIAN_POINT('Ctrl Pts',(26.0394480946395,-65.5149709682656,
-172.038055421481));
#160373=CARTESIAN_POINT('Ctrl Pts',(26.1751497442534,-65.4958993451584,
-171.625426858395));
#160374=CARTESIAN_POINT('Ctrl Pts',(26.2234488624093,-65.1680142434972,
-171.34400271074));
#160375=CARTESIAN_POINT('Ctrl Pts',(26.3688360080808,-65.4686785159697,
-172.14852124047));
#160376=CARTESIAN_POINT('Ctrl Pts',(26.5059850091802,-65.4494034808673,
-171.691392643103));
#160377=CARTESIAN_POINT('Ctrl Pts',(26.5325022452051,-65.072358231615,-171.399245459895));
#160378=CARTESIAN_POINT('Ctrl Pts',(26.7013989289162,-65.4219398454845,
-172.23811459301));
#160379=CARTESIAN_POINT('Ctrl Pts',(26.8344935945357,-65.4032346100804,
-171.736704292719));
#160380=CARTESIAN_POINT('Ctrl Pts',(26.843027692162,-64.9750314285332,-171.444032296926));
#160381=CARTESIAN_POINT('Ctrl Pts',(27.3705571684413,-65.3278957879536,
-172.38942269823));
#160382=CARTESIAN_POINT('Ctrl Pts',(27.4914924972326,-65.3108994359038,
-171.799283317704));
#160383=CARTESIAN_POINT('Ctrl Pts',(27.4650077428683,-64.7776672125821,
-171.519686348695));
#160384=CARTESIAN_POINT('Ctrl Pts',(27.7072474293082,-65.2805770576552,
-172.450796940493));
#160385=CARTESIAN_POINT('Ctrl Pts',(27.8213068579945,-65.2645470503453,
-171.81528847728));
#160386=CARTESIAN_POINT('Ctrl Pts',(27.7764978537267,-64.6776202239548,
-171.550373470332));
#160387=CARTESIAN_POINT('Ctrl Pts',(28.7226827355371,-65.1378669321315,
-172.598633897542));
#160388=CARTESIAN_POINT('Ctrl Pts',(28.8291547927028,-65.1229032603379,
-171.822805263071));
#160389=CARTESIAN_POINT('Ctrl Pts',(28.7113572324553,-64.3737932440126,
-171.624291948599));
#160390=CARTESIAN_POINT('Ctrl Pts',(29.4067311934443,-65.0417301908804,
-172.64994999751));
#160391=CARTESIAN_POINT('Ctrl Pts',(29.4938163229,-65.0294911740669,-171.766054775631));
#160392=CARTESIAN_POINT('Ctrl Pts',(29.3350621276793,-64.1663451413114,
-171.64995));
#160393=CARTESIAN_POINT('Ctrl Pts',(30.098151667932,-64.9445573802656,-172.64995));
#160394=CARTESIAN_POINT('Ctrl Pts',(30.098151667932,-64.9445573802655,-171.64995));
#160395=CARTESIAN_POINT('Ctrl Pts',(29.958978566972,-63.954289311524,-171.64995));
#160396=CARTESIAN_POINT('',(30.098151667932,-64.9445573802656,-172.64995));
#160397=CARTESIAN_POINT('Origin',(29.958978566972,-63.954289311524,-172.64995));
#160398=CARTESIAN_POINT('',(26.0394480946395,-65.5149709682656,-172.038055421481));
#160399=CARTESIAN_POINT('Origin',(25.9002749936795,-64.5247028995241,-172.038055421481));
#160400=CARTESIAN_POINT('Ctrl Pts',(30.098151667932,-64.9445573802656,-172.64995));
#160401=CARTESIAN_POINT('Ctrl Pts',(29.5972390119403,-65.0149560630516,
-172.649949998196));
#160402=CARTESIAN_POINT('Ctrl Pts',(29.1003075630642,-65.0847952236665,
-172.623020954985));
#160403=CARTESIAN_POINT('Ctrl Pts',(28.6071269715803,-65.1541072356527,
-172.570721117633));
#160404=CARTESIAN_POINT('Ctrl Pts',(28.4194541761964,-65.1804829269669,
-172.550819165198));
#160405=CARTESIAN_POINT('Ctrl Pts',(28.2323246108958,-65.2067822722717,
-172.527242787954));
#160406=CARTESIAN_POINT('Ctrl Pts',(28.0457258647366,-65.2330070158113,
-172.500075926044));
#160407=CARTESIAN_POINT('Ctrl Pts',(27.7072474293089,-65.2805770576551,
-172.450796940499));
#160408=CARTESIAN_POINT('Ctrl Pts',(27.3705571686055,-65.3278957879305,
-172.389422697018));
#160409=CARTESIAN_POINT('Ctrl Pts',(27.0359780488069,-65.3749178167011,
-172.313768645042));
#160410=CARTESIAN_POINT('Ctrl Pts',(26.7013989290084,-65.4219398454716,
-172.238114593065));
#160411=CARTESIAN_POINT('Ctrl Pts',(26.3688785032062,-65.4686725436693,
-172.14853549193));
#160412=CARTESIAN_POINT('Ctrl Pts',(26.0394480946395,-65.5149709682656,
-172.038055421481));
#160413=CARTESIAN_POINT('Origin',(45.4220505312374,-61.7810962706031,-172.64995));
#160414=CARTESIAN_POINT('',(31.28041344952,-64.7784013226445,-172.64995));
#160415=CARTESIAN_POINT('',(27.530675086669,-65.3053926820751,-172.64995));
#160416=CARTESIAN_POINT('Ctrl Pts',(31.2804134495199,-64.7784013226445,
-172.64995));
#160417=CARTESIAN_POINT('Ctrl Pts',(31.2804134495199,-64.7784013226445,
-172.608983203817));
#160418=CARTESIAN_POINT('Ctrl Pts',(31.2806213080456,-64.7758267410213,
-172.567620053161));
#160419=CARTESIAN_POINT('Ctrl Pts',(31.2810194383274,-64.7705524414083,
-172.52618728165));
#160420=CARTESIAN_POINT('Ctrl Pts',(31.28141235728,-64.76534717978,-172.485296844715));
#160421=CARTESIAN_POINT('Ctrl Pts',(31.2819905477625,-64.7575120457041,
-172.444338940269));
#160422=CARTESIAN_POINT('Ctrl Pts',(31.2827427524648,-64.7469669392553,
-172.403658150027));
#160423=CARTESIAN_POINT('Ctrl Pts',(31.2834809680707,-64.7366179449949,
-172.363733919128));
#160424=CARTESIAN_POINT('Ctrl Pts',(31.2843867483343,-64.7236585728548,
-172.324077002608));
#160425=CARTESIAN_POINT('Ctrl Pts',(31.2854555737588,-64.7080566649442,
-172.285037095554));
#160426=CARTESIAN_POINT('Ctrl Pts',(31.2865128315013,-64.6926236133354,
-172.246419709538));
#160427=CARTESIAN_POINT('Ctrl Pts',(31.2877295873979,-64.6746046531694,
-172.208406475053));
#160428=CARTESIAN_POINT('Ctrl Pts',(31.2891080729451,-64.6540156623694,
-172.171353409327));
#160429=CARTESIAN_POINT('Ctrl Pts',(31.2904653774001,-64.633743031297,-172.134869681744));
#160430=CARTESIAN_POINT('Ctrl Pts',(31.2919794574909,-64.610978585132,-172.099317309204));
#160431=CARTESIAN_POINT('Ctrl Pts',(31.2936593097591,-64.585786337593,-172.065046652145));
#160432=CARTESIAN_POINT('Ctrl Pts',(31.2944218099435,-64.5743513478863,
-172.049490889995));
#160433=CARTESIAN_POINT('Ctrl Pts',(31.2952185612475,-64.5624168365768,
-172.034199306284));
#160434=CARTESIAN_POINT('Ctrl Pts',(31.2960508993985,-64.54999230786,-172.019204984951));
#160435=CARTESIAN_POINT('Ctrl Pts',(31.2967847052814,-64.539038596013,-172.005985692778));
#160436=CARTESIAN_POINT('Ctrl Pts',(31.2975461754486,-64.527704046776,-171.992997455514));
#160437=CARTESIAN_POINT('Ctrl Pts',(31.2983364317961,-64.515996642854,-171.980262947379));
#160438=CARTESIAN_POINT('Ctrl Pts',(31.2986919487447,-64.5107297689691,
-171.9745340045));
#160439=CARTESIAN_POINT('Ctrl Pts',(31.2990750220731,-64.5051055721233,
-171.968556625651));
#160440=CARTESIAN_POINT('Ctrl Pts',(31.2994555591239,-64.4994990189348,
-171.962743472258));
#160441=CARTESIAN_POINT('Ctrl Pts',(31.2998484999594,-64.4937097174994,
-171.956740836387));
#160442=CARTESIAN_POINT('Ctrl Pts',(31.3002387617528,-64.4879394084972,
-171.950913444372));
#160443=CARTESIAN_POINT('Ctrl Pts',(31.3005989639997,-64.4826418592774,
-171.945675867995));
#160444=CARTESIAN_POINT('Ctrl Pts',(31.3006653264322,-64.4816658568904,
-171.9447109148));
#160445=CARTESIAN_POINT('Ctrl Pts',(31.3007306824748,-64.4807060005262,
-171.943765878233));
#160446=CARTESIAN_POINT('Ctrl Pts',(31.3007948782761,-64.4797652514731,
-171.942843218813));
#160447=CARTESIAN_POINT('Ctrl Pts',(31.3023230365058,-64.4573710546937,
-171.920879639337));
#160448=CARTESIAN_POINT('Ctrl Pts',(31.3039802192176,-64.4332657575141,
-171.899286273904));
#160449=CARTESIAN_POINT('Ctrl Pts',(31.3057568294339,-64.4073810738904,
-171.87835788998));
#160450=CARTESIAN_POINT('Ctrl Pts',(31.3074846180388,-64.3822077066572,
-171.858004622318));
#160451=CARTESIAN_POINT('Ctrl Pts',(31.3093252995898,-64.3553509713006,
-171.838280617927));
#160452=CARTESIAN_POINT('Ctrl Pts',(31.3112753249902,-64.3267856146847,
-171.819487496162));
#160453=CARTESIAN_POINT('Ctrl Pts',(31.3132253503906,-64.2982202580688,
-171.800694374398));
#160454=CARTESIAN_POINT('Ctrl Pts',(31.3152846337614,-64.2679456691333,
-171.782832445245));
#160455=CARTESIAN_POINT('Ctrl Pts',(31.3174561053801,-64.2359826978855,
-171.766229742061));
#160456=CARTESIAN_POINT('Ctrl Pts',(31.3185520676279,-64.2198506842245,
-171.757850200856));
#160457=CARTESIAN_POINT('Ctrl Pts',(31.319676718292,-64.2032893725833,-171.749791815626));
#160458=CARTESIAN_POINT('Ctrl Pts',(31.3208311719887,-64.1863066938707,
-171.742098872734));
#160459=CARTESIAN_POINT('Ctrl Pts',(31.3214083988371,-64.1778153545143,
-171.738252401289));
#160460=CARTESIAN_POINT('Ctrl Pts',(31.321993076794,-64.1692186758832,-171.734497284808));
#160461=CARTESIAN_POINT('Ctrl Pts',(31.3225854050853,-64.1605180755428,
-171.730839196989));
#160462=CARTESIAN_POINT('Ctrl Pts',(31.322881569231,-64.1561677753726,-171.729010153079));
#160463=CARTESIAN_POINT('Ctrl Pts',(31.3231796460049,-64.1517914950928,
-171.727205365633));
#160464=CARTESIAN_POINT('Ctrl Pts',(31.3234796624372,-64.1473894270328,
-171.725425545576));
#160465=CARTESIAN_POINT('Ctrl Pts',(31.3236618137701,-64.1447167648781,
-171.724344949446));
#160466=CARTESIAN_POINT('Ctrl Pts',(31.3238943343951,-64.141314308081,-171.72298693083));
#160467=CARTESIAN_POINT('Ctrl Pts',(31.3240866295113,-64.1384929063,-171.721876575885));
#160468=CARTESIAN_POINT('Ctrl Pts',(31.324211058373,-64.1366672550884,-171.72115809585));
#160469=CARTESIAN_POINT('Ctrl Pts',(31.3243187213849,-64.1350854387713,
-171.720541970086));
#160470=CARTESIAN_POINT('Ctrl Pts',(31.3243855589116,-64.1341060601822,
-171.720161698938));
#160471=CARTESIAN_POINT('Ctrl Pts',(31.3254476052599,-64.1185437629861,
-171.714119201495));
#160472=CARTESIAN_POINT('Ctrl Pts',(31.3266376535648,-64.1013293404877,
-171.707866938349));
#160473=CARTESIAN_POINT('Ctrl Pts',(31.3279469264486,-64.0824003384,-171.701654178638));
#160474=CARTESIAN_POINT('Ctrl Pts',(31.3292273680979,-64.0638881680553,
-171.695578228857));
#160475=CARTESIAN_POINT('Ctrl Pts',(31.3306217347893,-64.0437353416621,
-171.689540171929));
#160476=CARTESIAN_POINT('Ctrl Pts',(31.332124061834,-64.0218994182539,-171.68382031885));
#160477=CARTESIAN_POINT('Ctrl Pts',(31.3335678730231,-64.0009140072203,
-171.678323254875));
#160478=CARTESIAN_POINT('Ctrl Pts',(31.3351113079963,-63.9783734175572,
-171.673120412634));
#160479=CARTESIAN_POINT('Ctrl Pts',(31.3367525763832,-63.9542649101158,
-171.668501297287));
#160480=CARTESIAN_POINT('Ctrl Pts',(31.3383524464309,-63.9307645007625,
-171.66399869165));
#160481=CARTESIAN_POINT('Ctrl Pts',(31.3400451860075,-63.9057736267565,
-171.660051059673));
#160482=CARTESIAN_POINT('Ctrl Pts',(31.3418338549193,-63.8793140597499,
-171.656961460455));
#160483=CARTESIAN_POINT('Ctrl Pts',(31.343555301263,-63.8538489082178,-171.65398797596));
#160484=CARTESIAN_POINT('Ctrl Pts',(31.3453655360519,-63.8270229147674,
-171.651809705469));
#160485=CARTESIAN_POINT('Ctrl Pts',(31.3472728234533,-63.7988948820044,
-171.650723766091));
#160486=CARTESIAN_POINT('Ctrl Pts',(31.3481603393926,-63.7858060955955,
-171.65021844712));
#160487=CARTESIAN_POINT('Ctrl Pts',(31.349068956197,-63.7724359890296,-171.64995));
#160488=CARTESIAN_POINT('Ctrl Pts',(31.35,-63.7587939982373,-171.64995));
#160489=CARTESIAN_POINT('Ctrl Pts',(31.85,-65.2735353570153,-176.84995));
#160490=CARTESIAN_POINT('Ctrl Pts',(31.8499999999999,-64.6983511534047,
-176.84995));
#160491=CARTESIAN_POINT('Ctrl Pts',(31.28041344952,-64.7784013226445,-176.84995));
#160492=CARTESIAN_POINT('Ctrl Pts',(31.85,-65.2735353570043,-176.981217345763));
#160493=CARTESIAN_POINT('Ctrl Pts',(31.8499999999783,-64.6983511534012,
-176.958917254529));
#160494=CARTESIAN_POINT('Ctrl Pts',(31.2804134495858,-64.7784013226352,
-177.112484691526));
#160495=CARTESIAN_POINT('Ctrl Pts',(31.9038865634697,-65.2583888317962,
-177.110943344657));
#160496=CARTESIAN_POINT('Ctrl Pts',(31.883334205664,-64.6936663363131,-177.069891898462));
#160497=CARTESIAN_POINT('Ctrl Pts',(31.3881865764622,-64.7632547974255,
-177.371936689315));
#160498=CARTESIAN_POINT('Ctrl Pts',(32.0890066553437,-65.2063549673329,
-177.296063436531));
#160499=CARTESIAN_POINT('Ctrl Pts',(32.0302774403978,-64.6730148114567,
-177.257255781815));
#160500=CARTESIAN_POINT('Ctrl Pts',(31.7584267602047,-64.711220932962,-177.742176873059));
#160501=CARTESIAN_POINT('Ctrl Pts',(32.2187326542366,-65.1698913669989,
-177.34995));
#160502=CARTESIAN_POINT('Ctrl Pts',(32.1431106784802,-64.6571571339907,
-177.331204220089));
#160503=CARTESIAN_POINT('Ctrl Pts',(32.0178787579952,-64.6747573326273,
-177.849949999941));
#160504=CARTESIAN_POINT('Ctrl Pts',(32.35,-65.1329945223129,-177.34995));
#160505=CARTESIAN_POINT('Ctrl Pts',(32.28041344952,-64.637860487942,-177.34995));
#160506=CARTESIAN_POINT('Ctrl Pts',(32.28041344952,-64.6378604879421,-177.84995));
#160507=CARTESIAN_POINT('',(32.28041344952,-64.6378604879421,-177.84995));
#160508=CARTESIAN_POINT('Origin',(32.35,-65.1329945223129,-177.84995));
#160509=CARTESIAN_POINT('',(31.85,-65.2735353570153,-176.84995));
#160510=CARTESIAN_POINT('Ctrl Pts',(31.85,-65.2735353570153,-176.84995));
#160511=CARTESIAN_POINT('Ctrl Pts',(31.85,-65.2735353570131,-176.875860144879));
#160512=CARTESIAN_POINT('Ctrl Pts',(31.85210178423,-65.272936510976,-176.90206911043));
#160513=CARTESIAN_POINT('Ctrl Pts',(31.8563470810216,-65.2717334581292,
-176.928255280411));
#160514=CARTESIAN_POINT('Ctrl Pts',(31.8606310064401,-65.2705194585142,
-176.954679722494));
#160515=CARTESIAN_POINT('Ctrl Pts',(31.8670976465416,-65.2686902017598,
-176.981080902282));
#160516=CARTESIAN_POINT('Ctrl Pts',(31.8757612620159,-65.2662482275523,
-177.007084282781));
#160517=CARTESIAN_POINT('Ctrl Pts',(31.8790093277216,-65.2653327099256,
-177.016833179033));
#160518=CARTESIAN_POINT('Ctrl Pts',(31.8825659056061,-65.2643311515803,
-177.026525725721));
#160519=CARTESIAN_POINT('Ctrl Pts',(31.8864307190677,-65.2632439750754,
-177.036140639745));
#160520=CARTESIAN_POINT('Ctrl Pts',(31.8965777998919,-65.2603895894823,
-177.061384629059));
#160521=CARTESIAN_POINT('Ctrl Pts',(31.9088564664222,-65.2569417248404,
-177.086112146697));
#160522=CARTESIAN_POINT('Ctrl Pts',(31.9232664008841,-65.2528998905346,
-177.109925913984));
#160523=CARTESIAN_POINT('Ctrl Pts',(31.9261741041008,-65.2520843105163,
-177.114731166078));
#160524=CARTESIAN_POINT('Ctrl Pts',(31.9291685418052,-65.2512445582216,
-177.11949905002));
#160525=CARTESIAN_POINT('Ctrl Pts',(31.9322496425496,-65.2503806488339,
-177.124226050868));
#160526=CARTESIAN_POINT('Ctrl Pts',(31.9414248200636,-65.2478080221507,
-177.138302536998));
#160527=CARTESIAN_POINT('Ctrl Pts',(31.9513686606954,-65.2450209957176,
-177.15201654548));
#160528=CARTESIAN_POINT('Ctrl Pts',(31.9620727243129,-65.2420195372944,
-177.165265493157));
#160529=CARTESIAN_POINT('Ctrl Pts',(31.9674247561217,-65.2405188080827,
-177.171889966996));
#160530=CARTESIAN_POINT('Ctrl Pts',(31.9729667901391,-65.2389644717009,
-177.178398084194));
#160531=CARTESIAN_POINT('Ctrl Pts',(31.9786966345161,-65.2373565305258,
-177.184775824989));
#160532=CARTESIAN_POINT('Ctrl Pts',(31.9815615567046,-65.2365525599382,
-177.187964695387));
#160533=CARTESIAN_POINT('Ctrl Pts',(31.9844734220996,-65.2357351882425,
-177.19112096562));
#160534=CARTESIAN_POINT('Ctrl Pts',(31.9874318783457,-65.2349044161532,
-177.194242832635));
#160535=CARTESIAN_POINT('Ctrl Pts',(31.9891481151571,-65.2344224750587,
-177.196053866042));
#160536=CARTESIAN_POINT('Ctrl Pts',(31.9912379161451,-65.2338354383028,
-177.198223860057));
#160537=CARTESIAN_POINT('Ctrl Pts',(31.9930815352964,-65.2333174589098,
-177.200104597085));
#160538=CARTESIAN_POINT('Ctrl Pts',(31.9944159546055,-65.2329425432427,
-177.201465882471));
#160539=CARTESIAN_POINT('Ctrl Pts',(31.9956200660744,-65.2326041814675,
-177.202676847247));
#160540=CARTESIAN_POINT('Ctrl Pts',(31.9964466064336,-65.2323718572572,
-177.20350338762));
#160541=CARTESIAN_POINT('Ctrl Pts',(32.0062413953876,-65.2296187350626,
-177.213298176739));
#160542=CARTESIAN_POINT('Ctrl Pts',(32.0171766858621,-65.2264997668672,
-177.223386446864));
#160543=CARTESIAN_POINT('Ctrl Pts',(32.0293814740844,-65.2230056156829,
-177.233531412475));
#160544=CARTESIAN_POINT('Ctrl Pts',(32.0410442961724,-65.2196666258643,
-177.243225880487));
#160545=CARTESIAN_POINT('Ctrl Pts',(32.0538670706311,-65.2159848445911,
-177.25297216405));
#160546=CARTESIAN_POINT('Ctrl Pts',(32.0679403417523,-65.2119582399725,
-177.262523160562));
#160547=CARTESIAN_POINT('Ctrl Pts',(32.0811785164908,-65.2081705707742,
-177.271507408763));
#160548=CARTESIAN_POINT('Ctrl Pts',(32.0955236210271,-65.2040776753833,
-177.280318781026));
#160549=CARTESIAN_POINT('Ctrl Pts',(32.111023322083,-65.1996854519068,-177.288715370369));
#160550=CARTESIAN_POINT('Ctrl Pts',(32.1172493121663,-65.1979211636983,
-177.292088150386));
#160551=CARTESIAN_POINT('Ctrl Pts',(32.1236612363228,-65.1961086768998,
-177.29539358477));
#160552=CARTESIAN_POINT('Ctrl Pts',(32.1302605707122,-65.1942488102442,
-177.298614236713));
#160553=CARTESIAN_POINT('Ctrl Pts',(32.1454165064926,-65.1899774674195,
-177.30601073932));
#160554=CARTESIAN_POINT('Ctrl Pts',(32.1615733881405,-65.185464996466,-177.312967023304));
#160555=CARTESIAN_POINT('Ctrl Pts',(32.1787235893757,-65.1806932862225,
-177.31924572228));
#160556=CARTESIAN_POINT('Ctrl Pts',(32.195408897906,-65.1760509233407,-177.325354223758));
#160557=CARTESIAN_POINT('Ctrl Pts',(32.2130347093888,-65.1711630872873,
-177.330821391552));
#160558=CARTESIAN_POINT('Ctrl Pts',(32.2315578626383,-65.166023463016,-177.335399595608));
#160559=CARTESIAN_POINT('Ctrl Pts',(32.2496915443714,-65.1609919055103,
-177.339881537432));
#160560=CARTESIAN_POINT('Ctrl Pts',(32.2686855091775,-65.1557189448577,
-177.343511544964));
#160561=CARTESIAN_POINT('Ctrl Pts',(32.2884598244632,-65.1502101232398,
-177.346028622917));
#160562=CARTESIAN_POINT('Ctrl Pts',(32.3082341397488,-65.1447013016219,
-177.34854570087));
#160563=CARTESIAN_POINT('Ctrl Pts',(32.3287891950344,-65.1389564907821,
-177.34995));
#160564=CARTESIAN_POINT('Ctrl Pts',(32.35,-65.1329945223129,-177.34995));
#160565=CARTESIAN_POINT('',(31.28041344952,-64.7784013226445,-176.84995));
#160566=CARTESIAN_POINT('Origin',(31.35,-65.2735353570153,-176.84995));
#160567=CARTESIAN_POINT('Ctrl Pts',(32.28041344952,-64.6378604879421,-177.84995));
#160568=CARTESIAN_POINT('Ctrl Pts',(32.0178787579952,-64.6747573326273,
-177.849949999941));
#160569=CARTESIAN_POINT('Ctrl Pts',(31.7584267602047,-64.711220932962,-177.742176873059));
#160570=CARTESIAN_POINT('Ctrl Pts',(31.5733066683334,-64.7372378651937,
-177.557056781187));
#160571=CARTESIAN_POINT('Ctrl Pts',(31.3881865764622,-64.7632547974255,
-177.371936689315));
#160572=CARTESIAN_POINT('Ctrl Pts',(31.2804134495858,-64.7784013226352,
-177.112484691526));
#160573=CARTESIAN_POINT('Ctrl Pts',(31.28041344952,-64.7784013226445,-176.84995));
#160574=CARTESIAN_POINT('Origin',(45.6308101826775,-63.2664983737155,-177.84995));
#160575=CARTESIAN_POINT('',(32.7804134495199,-64.5675900705909,-177.84995));
#160576=CARTESIAN_POINT('',(45.5612236321975,-62.7713643393447,-177.84995));
#160577=CARTESIAN_POINT('Origin',(32.85,-65.0627241049617,-177.84995));
#160578=CARTESIAN_POINT('Ctrl Pts',(32.85,-65.0627241049617,-177.34995));
#160579=CARTESIAN_POINT('Ctrl Pts',(32.7804134495199,-64.5675900705908,
-177.34995));
#160580=CARTESIAN_POINT('Ctrl Pts',(32.7804134495199,-64.5675900705909,
-177.84995));
#160581=CARTESIAN_POINT('Ctrl Pts',(32.9812673457631,-65.0258272602758,
-177.34995));
#160582=CARTESIAN_POINT('Ctrl Pts',(32.9116024612643,-64.5491526573769,
-177.367861075732));
#160583=CARTESIAN_POINT('Ctrl Pts',(33.0429481410447,-64.5306932259057,
-177.849949999941));
#160584=CARTESIAN_POINT('Ctrl Pts',(33.1109933446567,-64.9893636599417,
-177.29606343653));
#160585=CARTESIAN_POINT('Ctrl Pts',(33.0606847809584,-64.52820050373,-177.329589659683));
#160586=CARTESIAN_POINT('Ctrl Pts',(33.3024001388352,-64.494229625571,-177.742176873059));
#160587=CARTESIAN_POINT('Ctrl Pts',(33.2961134365298,-64.9373297954784,
-177.110943344657));
#160588=CARTESIAN_POINT('Ctrl Pts',(33.280492098389,-64.4973085998594,-177.142957948483));
#160589=CARTESIAN_POINT('Ctrl Pts',(33.6726403225778,-64.4421957611075,
-177.371936689315));
#160590=CARTESIAN_POINT('Ctrl Pts',(33.35,-64.9221832702703,-176.981217345763));
#160591=CARTESIAN_POINT('Ctrl Pts',(33.3499999999424,-64.4875399013621,
-176.997671841189));
#160592=CARTESIAN_POINT('Ctrl Pts',(33.7804134494542,-64.4270492358978,
-177.112484691526));
#160593=CARTESIAN_POINT('Ctrl Pts',(33.35,-64.9221832702593,-176.84995));
#160594=CARTESIAN_POINT('Ctrl Pts',(33.35,-64.4875399013512,-176.84995));
#160595=CARTESIAN_POINT('Ctrl Pts',(33.7804134495199,-64.4270492358885,
-176.84995));
#160596=CARTESIAN_POINT('',(33.7804134495199,-64.4270492358885,-176.84995));
#160597=CARTESIAN_POINT('Ctrl Pts',(33.7804134495199,-64.4270492358885,
-176.84995));
#160598=CARTESIAN_POINT('Ctrl Pts',(33.7804134494542,-64.4270492358978,
-177.112484691526));
#160599=CARTESIAN_POINT('Ctrl Pts',(33.6726403225778,-64.4421957611075,
-177.371936689315));
#160600=CARTESIAN_POINT('Ctrl Pts',(33.4875202307065,-64.4682126933392,
-177.557056781187));
#160601=CARTESIAN_POINT('Ctrl Pts',(33.3024001388352,-64.494229625571,-177.742176873059));
#160602=CARTESIAN_POINT('Ctrl Pts',(33.0429481410447,-64.5306932259057,
-177.849949999941));
#160603=CARTESIAN_POINT('Ctrl Pts',(32.7804134495199,-64.5675900705909,
-177.84995));
#160604=CARTESIAN_POINT('',(33.35,-64.9221832702593,-176.84995));
#160605=CARTESIAN_POINT('Origin',(33.85,-64.9221832702593,-176.84995));
#160606=CARTESIAN_POINT('Ctrl Pts',(32.85,-65.0627241049617,-177.34995));
#160607=CARTESIAN_POINT('Ctrl Pts',(32.8709105170141,-65.0568465419312,
-177.34995));
#160608=CARTESIAN_POINT('Ctrl Pts',(32.8911797466383,-65.0511492330308,
-177.348585219097));
#160609=CARTESIAN_POINT('Ctrl Pts',(32.9106899838339,-65.0456652629893,
-177.346136042571));
#160610=CARTESIAN_POINT('Ctrl Pts',(32.9306295626821,-65.0400606128794,
-177.343632969545));
#160611=CARTESIAN_POINT('Ctrl Pts',(32.9497766651579,-65.0346787133512,
-177.33999719389));
#160612=CARTESIAN_POINT('Ctrl Pts',(32.9680516974346,-65.0295419367704,
-177.335495637057));
#160613=CARTESIAN_POINT('Ctrl Pts',(32.9869112963546,-65.0242408492217,
-177.330850088141));
#160614=CARTESIAN_POINT('Ctrl Pts',(33.004842416708,-65.0192007399784,-177.32528246904));
#160615=CARTESIAN_POINT('Ctrl Pts',(33.0218018468558,-65.0144337550403,
-177.319052501424));
#160616=CARTESIAN_POINT('Ctrl Pts',(33.0374915731195,-65.0100236605896,
-177.313288953611));
#160617=CARTESIAN_POINT('Ctrl Pts',(33.0523504278524,-65.0058471088959,
-177.306958054963));
#160618=CARTESIAN_POINT('Ctrl Pts',(33.0663727601658,-65.0019056883203,
-177.300241547042));
#160619=CARTESIAN_POINT('Ctrl Pts',(33.0846217845958,-64.9967762220685,
-177.291500510645));
#160620=CARTESIAN_POINT('Ctrl Pts',(33.1014605911939,-64.9920431421992,
-177.282104513304));
#160621=CARTESIAN_POINT('Ctrl Pts',(33.1169358413832,-64.9876933330415,
-177.272394746015));
#160622=CARTESIAN_POINT('Ctrl Pts',(33.1322211818847,-64.983396904016,-177.26280413537));
#160623=CARTESIAN_POINT('Ctrl Pts',(33.1461768441267,-64.9794742231754,
-177.252906955711));
#160624=CARTESIAN_POINT('Ctrl Pts',(33.1588862630228,-64.9759018384949,
-177.242983686098));
#160625=CARTESIAN_POINT('Ctrl Pts',(33.1717549881601,-64.9722846757503,
-177.232936033239));
#160626=CARTESIAN_POINT('Ctrl Pts',(33.1833462719647,-64.9690265783479,
-177.222861820351));
#160627=CARTESIAN_POINT('Ctrl Pts',(33.1937756504663,-64.9660950712279,
-177.21300750887));
#160628=CARTESIAN_POINT('Ctrl Pts',(33.1950359580597,-64.9657408218656,
-177.211816693561));
#160629=CARTESIAN_POINT('Ctrl Pts',(33.1962793259514,-64.9653913339429,
-177.210629037074));
#160630=CARTESIAN_POINT('Ctrl Pts',(33.1975059843104,-64.9650465427636,
-177.209444926089));
#160631=CARTESIAN_POINT('Ctrl Pts',(33.1987673970184,-64.9646919827738,
-177.20822726623));
#160632=CARTESIAN_POINT('Ctrl Pts',(33.1996021366106,-64.9644573527714,
-177.207413007319));
#160633=CARTESIAN_POINT('Ctrl Pts',(33.2007626710069,-64.9641311320666,
-177.206271333214));
#160634=CARTESIAN_POINT('Ctrl Pts',(33.2014998739257,-64.9639239078288,
-177.205546110864));
#160635=CARTESIAN_POINT('Ctrl Pts',(33.2023682910512,-64.9636797953249,
-177.204688490104));
#160636=CARTESIAN_POINT('Ctrl Pts',(33.2035533858467,-64.9633466601626,
-177.20350339534));
#160637=CARTESIAN_POINT('Ctrl Pts',(33.224102627464,-64.9575701813806,-177.182954154274));
#160638=CARTESIAN_POINT('Ctrl Pts',(33.2425303081954,-64.9523902391111,
-177.160790380395));
#160639=CARTESIAN_POINT('Ctrl Pts',(33.258793554525,-64.9478188139827,-177.137499857771));
#160640=CARTESIAN_POINT('Ctrl Pts',(33.2750773096424,-64.9432416240528,
-177.114179964603));
#160641=CARTESIAN_POINT('Ctrl Pts',(33.2891911870376,-64.9392744816987,
-177.089730493789));
#160642=CARTESIAN_POINT('Ctrl Pts',(33.3011153275693,-64.9359229034905,
-177.06459461214));
#160643=CARTESIAN_POINT('Ctrl Pts',(33.3130600466424,-64.9325655411681,
-177.039415351282));
#160644=CARTESIAN_POINT('Ctrl Pts',(33.3228074903105,-64.9298258622901,
-177.013547308706));
#160645=CARTESIAN_POINT('Ctrl Pts',(33.3303606028096,-64.9277029771689,
-176.987389234916));
#160646=CARTESIAN_POINT('Ctrl Pts',(33.3379480469477,-64.9255704427639,
-176.961112263183));
#160647=CARTESIAN_POINT('Ctrl Pts',(33.3433211912071,-64.9240603151624,
-176.934542621745));
#160648=CARTESIAN_POINT('Ctrl Pts',(33.3465057497558,-64.9231653054218,
-176.908037356488));
#160649=CARTESIAN_POINT('Ctrl Pts',(33.3488411540378,-64.9225089477042,
-176.888599651378));
#160650=CARTESIAN_POINT('Ctrl Pts',(33.35,-64.9221832702593,-176.869195583396));
#160651=CARTESIAN_POINT('Ctrl Pts',(33.35,-64.9221832702593,-176.84995));
#160652=CARTESIAN_POINT('Origin',(45.4220505312374,-61.7810962706031,-172.64995));
#160653=CARTESIAN_POINT('',(39.43041344952,-63.6329935198201,-172.64995));
#160654=CARTESIAN_POINT('',(33.7804134495199,-64.4270492358885,-172.64995));
#160655=CARTESIAN_POINT('',(33.35,-64.4875399013512,-172.64995));
#160656=CARTESIAN_POINT('Ctrl Pts',(39.4304134495199,-63.6329935198201,
-172.64995));
#160657=CARTESIAN_POINT('Ctrl Pts',(39.4304134495199,-63.6329935198201,
-172.608983203963));
#160658=CARTESIAN_POINT('Ctrl Pts',(39.4306213080459,-63.6304189382149,
-172.567620053442));
#160659=CARTESIAN_POINT('Ctrl Pts',(39.431019438328,-63.6251446386348,-172.526187282055));
#160660=CARTESIAN_POINT('Ctrl Pts',(39.4314123572806,-63.6199393770401,
-172.485296845251));
#160661=CARTESIAN_POINT('Ctrl Pts',(39.4319905477632,-63.6121042430135,
-172.444338940925));
#160662=CARTESIAN_POINT('Ctrl Pts',(39.4327427524647,-63.6015591366258,
-172.403658150787));
#160663=CARTESIAN_POINT('Ctrl Pts',(39.4334809680696,-63.5912101424279,
-172.36373392));
#160664=CARTESIAN_POINT('Ctrl Pts',(39.4343867483315,-63.578250770363,-172.324077003577));
#160665=CARTESIAN_POINT('Ctrl Pts',(39.435455573753,-63.5626488625364,-172.285037096605));
#160666=CARTESIAN_POINT('Ctrl Pts',(39.4365128314928,-63.5472158110073,
-172.246419710661));
#160667=CARTESIAN_POINT('Ctrl Pts',(39.4377295873855,-63.5291968509287,
-172.208406476233));
#160668=CARTESIAN_POINT('Ctrl Pts',(39.439108072927,-63.5086078602195,-172.171353410548));
#160669=CARTESIAN_POINT('Ctrl Pts',(39.4404653773755,-63.4883352292506,
-172.13486968303));
#160670=CARTESIAN_POINT('Ctrl Pts',(39.4419794574579,-63.465570783196,-172.09931731054));
#160671=CARTESIAN_POINT('Ctrl Pts',(39.4436593097151,-63.4403785357705,
-172.065046653512));
#160672=CARTESIAN_POINT('Ctrl Pts',(39.4444218099166,-63.4289435457853,
-172.049490890928));
#160673=CARTESIAN_POINT('Ctrl Pts',(39.445218561239,-63.4170090341692,-172.034199306794));
#160674=CARTESIAN_POINT('Ctrl Pts',(39.4460508994101,-63.404584505118,-172.019204985054));
#160675=CARTESIAN_POINT('Ctrl Pts',(39.4467847052916,-63.3936307932609,
-172.005985692865));
#160676=CARTESIAN_POINT('Ctrl Pts',(39.4475461754571,-63.3822962440122,
-171.992997455584));
#160677=CARTESIAN_POINT('Ctrl Pts',(39.4483364318027,-63.3705888400765,
-171.980262947432));
#160678=CARTESIAN_POINT('Ctrl Pts',(39.4486919487457,-63.3653219662557,
-171.974534004621));
#160679=CARTESIAN_POINT('Ctrl Pts',(39.4490750220687,-63.3596977694689,
-171.968556625832));
#160680=CARTESIAN_POINT('Ctrl Pts',(39.4494555591141,-63.3540912163381,
-171.962743472495));
#160681=CARTESIAN_POINT('Ctrl Pts',(39.4498484999446,-63.348301914955,-171.956740836674));
#160682=CARTESIAN_POINT('Ctrl Pts',(39.4502387617329,-63.3425316060038,
-171.950913444705));
#160683=CARTESIAN_POINT('Ctrl Pts',(39.4505989639742,-63.3372340568394,
-171.945675868377));
#160684=CARTESIAN_POINT('Ctrl Pts',(39.4506653264156,-63.3362580543183,
-171.944710915048));
#160685=CARTESIAN_POINT('Ctrl Pts',(39.4507306824667,-63.3352981978247,
-171.943765878353));
#160686=CARTESIAN_POINT('Ctrl Pts',(39.4507948782762,-63.3343574486486,
-171.942843218813));
#160687=CARTESIAN_POINT('Ctrl Pts',(39.4523230364769,-63.3119632521963,
-171.920879639657));
#160688=CARTESIAN_POINT('Ctrl Pts',(39.4539802191624,-63.2878579553574,
-171.899286274498));
#160689=CARTESIAN_POINT('Ctrl Pts',(39.4557568293543,-63.2619732720811,
-171.878357890799));
#160690=CARTESIAN_POINT('Ctrl Pts',(39.4574846179602,-63.2367999048249,
-171.858004623066));
#160691=CARTESIAN_POINT('Ctrl Pts',(39.4593252995171,-63.2099431694035,
-171.838280618575));
#160692=CARTESIAN_POINT('Ctrl Pts',(39.4612753249272,-63.1813778126731,
-171.819487496696));
#160693=CARTESIAN_POINT('Ctrl Pts',(39.4632253503372,-63.1528124559428,
-171.800694374818));
#160694=CARTESIAN_POINT('Ctrl Pts',(39.4652846337216,-63.1225378668433,
-171.782832445536));
#160695=CARTESIAN_POINT('Ctrl Pts',(39.4674561053568,-63.0905748953762,
-171.766229742224));
#160696=CARTESIAN_POINT('Ctrl Pts',(39.4685520676076,-63.0744428816831,
-171.757850200996));
#160697=CARTESIAN_POINT('Ctrl Pts',(39.4696767182751,-63.05788157,-171.749791815739));
#160698=CARTESIAN_POINT('Ctrl Pts',(39.4708311719758,-63.0408988912349,
-171.74209887282));
#160699=CARTESIAN_POINT('Ctrl Pts',(39.4714083988261,-63.0324075518524,
-171.73825240136));
#160700=CARTESIAN_POINT('Ctrl Pts',(39.4719930767851,-63.0238108731925,
-171.734497284865));
#160701=CARTESIAN_POINT('Ctrl Pts',(39.4725854050786,-63.0151102728207,
-171.730839197032));
#160702=CARTESIAN_POINT('Ctrl Pts',(39.4728815692253,-63.0107599726348,
-171.729010153115));
#160703=CARTESIAN_POINT('Ctrl Pts',(39.4731796460004,-63.0063836923387,
-171.727205365662));
#160704=CARTESIAN_POINT('Ctrl Pts',(39.4734796624338,-63.0019816242616,
-171.725425545597));
#160705=CARTESIAN_POINT('Ctrl Pts',(39.4736618137668,-62.999308962104,-171.724344949466));
#160706=CARTESIAN_POINT('Ctrl Pts',(39.4738943343923,-62.9959065053002,
-171.722986930847));
#160707=CARTESIAN_POINT('Ctrl Pts',(39.474086629509,-62.9930851035116,-171.721876575899));
#160708=CARTESIAN_POINT('Ctrl Pts',(39.4742110583718,-62.991259452282,-171.721158095857));
#160709=CARTESIAN_POINT('Ctrl Pts',(39.4743187213847,-62.98967763595,-171.720541970087));
#160710=CARTESIAN_POINT('Ctrl Pts',(39.4743855589116,-62.9886982573578,
-171.720161698938));
#160711=CARTESIAN_POINT('Ctrl Pts',(39.4754476052573,-62.9731359601951,
-171.714119201508));
#160712=CARTESIAN_POINT('Ctrl Pts',(39.4766376535597,-62.9559215377298,
-171.707866938373));
#160713=CARTESIAN_POINT('Ctrl Pts',(39.4779469264412,-62.9369925356752,
-171.70165417867));
#160714=CARTESIAN_POINT('Ctrl Pts',(39.4792273680883,-62.9184803653616,
-171.695578228898));
#160715=CARTESIAN_POINT('Ctrl Pts',(39.4806217347776,-62.8983275389991,
-171.689540171976));
#160716=CARTESIAN_POINT('Ctrl Pts',(39.4821240618203,-62.8764916156212,
-171.6838203189));
#160717=CARTESIAN_POINT('Ctrl Pts',(39.4835678730075,-62.8555062046158,
-171.678323254929));
#160718=CARTESIAN_POINT('Ctrl Pts',(39.485111307979,-62.8329656149803,-171.673120412688));
#160719=CARTESIAN_POINT('Ctrl Pts',(39.4867525763642,-62.8088571075656,
-171.66850129734));
#160720=CARTESIAN_POINT('Ctrl Pts',(39.4883524464103,-62.7853566982382,
-171.663998691701));
#160721=CARTESIAN_POINT('Ctrl Pts',(39.4900451859854,-62.7603658242571,
-171.66005105972));
#160722=CARTESIAN_POINT('Ctrl Pts',(39.4918338548956,-62.7339062572745,
-171.656961460496));
#160723=CARTESIAN_POINT('Ctrl Pts',(39.4935553012377,-62.7084411057663,
-171.653987975995));
#160724=CARTESIAN_POINT('Ctrl Pts',(39.4953655360251,-62.6816151123391,
-171.651809705496));
#160725=CARTESIAN_POINT('Ctrl Pts',(39.497272823425,-62.653487079598,-171.650723766108));
#160726=CARTESIAN_POINT('Ctrl Pts',(39.4981603393732,-62.6403982930561,
-171.650218447126));
#160727=CARTESIAN_POINT('Ctrl Pts',(39.499068956187,-62.6270281863508,-171.64995));
#160728=CARTESIAN_POINT('Ctrl Pts',(39.5,-62.6133861954129,-171.64995));
#160729=CARTESIAN_POINT('Ctrl Pts',(33.85,-63.4074419114814,-171.64995));
#160730=CARTESIAN_POINT('Ctrl Pts',(33.8480582289195,-63.4358934441742,
-171.64995));
#160731=CARTESIAN_POINT('Ctrl Pts',(33.8461974246871,-63.4631586213041,
-171.651129585063));
#160732=CARTESIAN_POINT('Ctrl Pts',(33.8444225652799,-63.4891645037474,
-171.653192621539));
#160733=CARTESIAN_POINT('Ctrl Pts',(33.8425545166564,-63.5165358283173,
-171.655363978005));
#160734=CARTESIAN_POINT('Ctrl Pts',(33.8407816512719,-63.5425124936179,
-171.658513818808));
#160735=CARTESIAN_POINT('Ctrl Pts',(33.8391066446573,-63.5670552968023,
-171.66233503357));
#160736=CARTESIAN_POINT('Ctrl Pts',(33.837607521914,-63.589020985843,-171.665755002128));
#160737=CARTESIAN_POINT('Ctrl Pts',(33.8361867195622,-63.6098390961603,
-171.669713339737));
#160738=CARTESIAN_POINT('Ctrl Pts',(33.8348444729116,-63.6295061799083,
-171.674015027606));
#160739=CARTESIAN_POINT('Ctrl Pts',(33.8332381237839,-63.6530429887437,
-171.679163122074));
#160740=CARTESIAN_POINT('Ctrl Pts',(33.8317442597807,-63.6749316248201,
-171.6848021004));
#160741=CARTESIAN_POINT('Ctrl Pts',(33.8303611921804,-63.6951968318997,
-171.690639736311));
#160742=CARTESIAN_POINT('Ctrl Pts',(33.8289186268559,-63.7163338211679,
-171.696728499535));
#160743=CARTESIAN_POINT('Ctrl Pts',(33.8275965325062,-63.7357056261111,
-171.703033282501));
#160744=CARTESIAN_POINT('Ctrl Pts',(33.8263912815561,-63.753365399271,-171.709272496442));
#160745=CARTESIAN_POINT('Ctrl Pts',(33.825874494011,-63.7609375574312,-171.711947746816));
#160746=CARTESIAN_POINT('Ctrl Pts',(33.825379175863,-63.7681951382168,-171.714611542066));
#160747=CARTESIAN_POINT('Ctrl Pts',(33.8249049735087,-63.7751433227486,
-171.717244495107));
#160748=CARTESIAN_POINT('Ctrl Pts',(33.8247845954601,-63.7769071454876,
-171.717912880126));
#160749=CARTESIAN_POINT('Ctrl Pts',(33.8247281084716,-63.7777337764561,
-171.718228248952));
#160750=CARTESIAN_POINT('Ctrl Pts',(33.8246071368902,-63.7795056823664,
-171.71890895899));
#160751=CARTESIAN_POINT('Ctrl Pts',(33.8245512101083,-63.780324858194,-171.719223660355));
#160752=CARTESIAN_POINT('Ctrl Pts',(33.8244815093962,-63.7813459451167,
-171.71961677203));
#160753=CARTESIAN_POINT('Ctrl Pts',(33.8243854515167,-63.7827534613978,
-171.720163005656));
#160754=CARTESIAN_POINT('Ctrl Pts',(33.8240448575363,-63.7877441146917,
-171.72209979508));
#160755=CARTESIAN_POINT('Ctrl Pts',(33.8237064547845,-63.7927026508811,
-171.724069245188));
#160756=CARTESIAN_POINT('Ctrl Pts',(33.8233702655348,-63.7976287443672,
-171.72607046184));
#160757=CARTESIAN_POINT('Ctrl Pts',(33.8210922898814,-63.8310073281163,
-171.739630451674));
#160758=CARTESIAN_POINT('Ctrl Pts',(33.8189167622032,-63.8628843636977,
-171.754642782109));
#160759=CARTESIAN_POINT('Ctrl Pts',(33.816846962281,-63.8932120250278,-171.77077929301));
#160760=CARTESIAN_POINT('Ctrl Pts',(33.8148622623441,-63.9222927621974,
-171.786252350007));
#160761=CARTESIAN_POINT('Ctrl Pts',(33.8129747403056,-63.9499494177769,
-171.802759466717));
#160762=CARTESIAN_POINT('Ctrl Pts',(33.8111851663565,-63.9761709030137,
-171.820043746716));
#160763=CARTESIAN_POINT('Ctrl Pts',(33.8091798424695,-64.0055536344305,
-171.839411808912));
#160764=CARTESIAN_POINT('Ctrl Pts',(33.8072974703405,-64.0331348321881,
-171.859755775727));
#160765=CARTESIAN_POINT('Ctrl Pts',(33.8055364549802,-64.0589378666435,
-171.880757614385));
#160766=CARTESIAN_POINT('Ctrl Pts',(33.8047081977239,-64.0710737917499,
-171.890635396065));
#160767=CARTESIAN_POINT('Ctrl Pts',(33.803906752079,-64.0828168634207,-171.900659292116));
#160768=CARTESIAN_POINT('Ctrl Pts',(33.8031317849169,-64.0941719627785,
-171.910799109343));
#160769=CARTESIAN_POINT('Ctrl Pts',(33.8027566361001,-64.0996687790261,
-171.915707627562));
#160770=CARTESIAN_POINT('Ctrl Pts',(33.8024097468116,-64.1047515263583,
-171.920348851345));
#160771=CARTESIAN_POINT('Ctrl Pts',(33.8020599418533,-64.1098768430549,
-171.925124127276));
#160772=CARTESIAN_POINT('Ctrl Pts',(33.8017205761744,-64.1148492041924,
-171.929756893964));
#160773=CARTESIAN_POINT('Ctrl Pts',(33.8013784560457,-64.1198617813615,
-171.9345159123));
#160774=CARTESIAN_POINT('Ctrl Pts',(33.8010073810434,-64.1252983348553,
-171.939801580717));
#160775=CARTESIAN_POINT('Ctrl Pts',(33.800937583903,-64.1263209202765,-171.940795785495));
#160776=CARTESIAN_POINT('Ctrl Pts',(33.8008667695503,-64.127358400323,-171.941808724667));
#160777=CARTESIAN_POINT('Ctrl Pts',(33.8007947743349,-64.1284131719497,
-171.94284321151));
#160778=CARTESIAN_POINT('Ctrl Pts',(33.7984463931901,-64.1628183166118,
-171.976586695486));
#160779=CARTESIAN_POINT('Ctrl Pts',(33.7962900974017,-64.1944120724635,
-172.012463058108));
#160780=CARTESIAN_POINT('Ctrl Pts',(33.7943343814619,-64.2230682849126,
-172.049959758061));
#160781=CARTESIAN_POINT('Ctrl Pts',(33.7923469358344,-64.2521894179834,
-172.088064807393));
#160782=CARTESIAN_POINT('Ctrl Pts',(33.7905666289932,-64.278276951698,-172.127843232782));
#160783=CARTESIAN_POINT('Ctrl Pts',(33.789000571919,-64.3012249965493,-172.168804472182));
#160784=CARTESIAN_POINT('Ctrl Pts',(33.7877708916472,-64.3192439809744,
-172.200967557951));
#160785=CARTESIAN_POINT('Ctrl Pts',(33.7866732704194,-64.3353278524982,
-172.233860874847));
#160786=CARTESIAN_POINT('Ctrl Pts',(33.785710408276,-64.3494362499387,-172.267266567535));
#160787=CARTESIAN_POINT('Ctrl Pts',(33.7856150487614,-64.350833511157,-172.270574985735));
#160788=CARTESIAN_POINT('Ctrl Pts',(33.7855210125593,-64.3522113735592,
-172.27388835426));
#160789=CARTESIAN_POINT('Ctrl Pts',(33.7854282968075,-64.3535698783134,
-172.277206441635));
#160790=CARTESIAN_POINT('Ctrl Pts',(33.7842160400822,-64.371332302627,-172.320590372142));
#160791=CARTESIAN_POINT('Ctrl Pts',(33.7832297201077,-64.3857842198915,
-172.364775502606));
#160792=CARTESIAN_POINT('Ctrl Pts',(33.7824628528102,-64.3970206371015,
-172.409267414372));
#160793=CARTESIAN_POINT('Ctrl Pts',(33.7816869655113,-64.4083892186358,
-172.454282646281));
#160794=CARTESIAN_POINT('Ctrl Pts',(33.7811357225718,-64.4164662297078,
-172.499611949937));
#160795=CARTESIAN_POINT('Ctrl Pts',(33.7808018218098,-64.4213586645272,
-172.544796240172));
#160796=CARTESIAN_POINT('Ctrl Pts',(33.7805416776482,-64.4251703909416,
-172.579999601885));
#160797=CARTESIAN_POINT('Ctrl Pts',(33.7804134495199,-64.4270492358885,
-172.615116019715));
#160798=CARTESIAN_POINT('Ctrl Pts',(33.7804134495199,-64.4270492358885,
-172.64995));
#160799=CARTESIAN_POINT('Ctrl Pts',(40.,-64.1281275541908,-176.84995));
#160800=CARTESIAN_POINT('Ctrl Pts',(40.,-63.5529433505803,-176.84995));
#160801=CARTESIAN_POINT('Ctrl Pts',(39.43041344952,-63.63299351982,-176.84995));
#160802=CARTESIAN_POINT('Ctrl Pts',(40.,-64.1281275541799,-176.981217345763));
#160803=CARTESIAN_POINT('Ctrl Pts',(39.9999999999783,-63.5529433505767,
-176.958917254529));
#160804=CARTESIAN_POINT('Ctrl Pts',(39.4304134495858,-63.6329935198108,
-177.112484691526));
#160805=CARTESIAN_POINT('Ctrl Pts',(40.0538865634702,-64.1129810289718,
-177.110943344657));
#160806=CARTESIAN_POINT('Ctrl Pts',(40.033334205665,-63.5482585334886,-177.069891898461));
#160807=CARTESIAN_POINT('Ctrl Pts',(39.5381865764622,-63.6178469946011,
-177.371936689315));
#160808=CARTESIAN_POINT('Ctrl Pts',(40.2390066553433,-64.0609471645084,
-177.29606343653));
#160809=CARTESIAN_POINT('Ctrl Pts',(40.1802774403969,-63.5276070086322,
-177.257255781815));
#160810=CARTESIAN_POINT('Ctrl Pts',(39.9084267602046,-63.5658131301376,
-177.742176873059));
#160811=CARTESIAN_POINT('Ctrl Pts',(40.3687326542369,-64.0244835641743,
-177.34995));
#160812=CARTESIAN_POINT('Ctrl Pts',(40.2931106784809,-63.5117493311662,
-177.331204220089));
#160813=CARTESIAN_POINT('Ctrl Pts',(40.1678787579952,-63.5293495298029,
-177.849949999941));
#160814=CARTESIAN_POINT('Ctrl Pts',(40.5,-63.9875867194884,-177.34995));
#160815=CARTESIAN_POINT('Ctrl Pts',(40.4304134495199,-63.4924526851176,
-177.34995));
#160816=CARTESIAN_POINT('Ctrl Pts',(40.4304134495199,-63.4924526851176,
-177.84995));
#160817=CARTESIAN_POINT('',(40.,-64.1281275541909,-176.84995));
#160818=CARTESIAN_POINT('',(39.43041344952,-63.63299351982,-176.84995));
#160819=CARTESIAN_POINT('Origin',(39.5,-64.1281275541909,-176.84995));
#160820=CARTESIAN_POINT('',(40.4304134495199,-63.4924526851176,-177.84995));
#160821=CARTESIAN_POINT('Ctrl Pts',(40.4304134495199,-63.4924526851176,
-177.84995));
#160822=CARTESIAN_POINT('Ctrl Pts',(40.1678787579952,-63.5293495298029,
-177.849949999941));
#160823=CARTESIAN_POINT('Ctrl Pts',(39.9084267602046,-63.5658131301376,
-177.742176873059));
#160824=CARTESIAN_POINT('Ctrl Pts',(39.7233066683334,-63.5918300623693,
-177.557056781187));
#160825=CARTESIAN_POINT('Ctrl Pts',(39.5381865764622,-63.6178469946011,
-177.371936689315));
#160826=CARTESIAN_POINT('Ctrl Pts',(39.4304134495858,-63.6329935198108,
-177.112484691526));
#160827=CARTESIAN_POINT('Ctrl Pts',(39.43041344952,-63.63299351982,-176.84995));
#160828=CARTESIAN_POINT('Origin',(40.5,-63.9875867194884,-177.84995));
#160829=CARTESIAN_POINT('Ctrl Pts',(40.,-64.1281275541908,-176.84995));
#160830=CARTESIAN_POINT('Ctrl Pts',(40.,-64.1281275541887,-176.875860144686));
#160831=CARTESIAN_POINT('Ctrl Pts',(40.0021017841988,-64.1275287081581,
-176.902069110053));
#160832=CARTESIAN_POINT('Ctrl Pts',(40.0063470809329,-64.1263256553243,
-176.928255279864));
#160833=CARTESIAN_POINT('Ctrl Pts',(40.0106310062881,-64.125111655724,-176.954679721742));
#160834=CARTESIAN_POINT('Ctrl Pts',(40.017097646294,-64.1232823989925,-176.981080901339));
#160835=CARTESIAN_POINT('Ctrl Pts',(40.0257612616457,-64.120840424816,-177.007084281669));
#160836=CARTESIAN_POINT('Ctrl Pts',(40.0290093274313,-64.1199249071655,
-177.016833178237));
#160837=CARTESIAN_POINT('Ctrl Pts',(40.032565905416,-64.1189233487908,-177.026525725238));
#160838=CARTESIAN_POINT('Ctrl Pts',(40.0364307189981,-64.117836172251,-177.036140639572));
#160839=CARTESIAN_POINT('Ctrl Pts',(40.0465777997294,-64.1149817866814,
-177.061384628681));
#160840=CARTESIAN_POINT('Ctrl Pts',(40.0588564661358,-64.1115339220729,
-177.086112146133));
#160841=CARTESIAN_POINT('Ctrl Pts',(40.0732664004475,-64.1074920878103,
-177.109925913263));
#160842=CARTESIAN_POINT('Ctrl Pts',(40.0761741037768,-64.1066765077606,
-177.114731165561));
#160843=CARTESIAN_POINT('Ctrl Pts',(40.0791685416013,-64.1058367554325,
-177.119499049704));
#160844=CARTESIAN_POINT('Ctrl Pts',(40.0822496424732,-64.1049728460094,
-177.124226050751));
#160845=CARTESIAN_POINT('Ctrl Pts',(40.0914248199918,-64.1024002193263,
-177.138302536896));
#160846=CARTESIAN_POINT('Ctrl Pts',(40.1013686606316,-64.0996131928932,
-177.152016545396));
#160847=CARTESIAN_POINT('Ctrl Pts',(40.1120727242617,-64.09661173447,-177.165265493094));
#160848=CARTESIAN_POINT('Ctrl Pts',(40.1174247560767,-64.0951110052584,
-177.171889966943));
#160849=CARTESIAN_POINT('Ctrl Pts',(40.1229667901013,-64.0935566688765,
-177.178398084151));
#160850=CARTESIAN_POINT('Ctrl Pts',(40.1286966344869,-64.0919487277014,
-177.184775824956));
#160851=CARTESIAN_POINT('Ctrl Pts',(40.1315615566797,-64.0911447571138,
-177.187964695359));
#160852=CARTESIAN_POINT('Ctrl Pts',(40.1344734220793,-64.0903273854181,
-177.191120965598));
#160853=CARTESIAN_POINT('Ctrl Pts',(40.1374318783303,-64.0894966133288,
-177.194242832619));
#160854=CARTESIAN_POINT('Ctrl Pts',(40.1391481151386,-64.0890146722359,
-177.196053866022));
#160855=CARTESIAN_POINT('Ctrl Pts',(40.1412379161258,-64.0884276354813,
-177.198223860036));
#160856=CARTESIAN_POINT('Ctrl Pts',(40.1430815352768,-64.0879096560891,
-177.200104597065));
#160857=CARTESIAN_POINT('Ctrl Pts',(40.1444159545965,-64.0875347404196,
-177.201465882462));
#160858=CARTESIAN_POINT('Ctrl Pts',(40.1456200660741,-64.0871963786422,
-177.202676847247));
#160859=CARTESIAN_POINT('Ctrl Pts',(40.1464466064337,-64.0869640544319,
-177.20350338762));
#160860=CARTESIAN_POINT('Ctrl Pts',(40.1562413953246,-64.0842109322552,
-177.213298176676));
#160861=CARTESIAN_POINT('Ctrl Pts',(40.1671766857346,-64.0810919640796,
-177.223386446747));
#160862=CARTESIAN_POINT('Ctrl Pts',(40.1793814738916,-64.0775978129156,
-177.233531412315));
#160863=CARTESIAN_POINT('Ctrl Pts',(40.1910442959181,-64.0742588231162,
-177.243225880286));
#160864=CARTESIAN_POINT('Ctrl Pts',(40.2038670703147,-64.0705770418626,
-177.252972163816));
#160865=CARTESIAN_POINT('Ctrl Pts',(40.2179403413746,-64.0665504372626,
-177.262523160305));
#160866=CARTESIAN_POINT('Ctrl Pts',(40.231178516052,-64.062762768083,-177.271507408483));
#160867=CARTESIAN_POINT('Ctrl Pts',(40.2455236205272,-64.0586698727101,
-177.28031878073));
#160868=CARTESIAN_POINT('Ctrl Pts',(40.2610233215231,-64.0542776492498,
-177.288715370066));
#160869=CARTESIAN_POINT('Ctrl Pts',(40.2672493116986,-64.0525133610149,
-177.292088150142));
#160870=CARTESIAN_POINT('Ctrl Pts',(40.2736612359544,-64.050700874188,-177.295393584586));
#160871=CARTESIAN_POINT('Ctrl Pts',(40.2802605704505,-64.0488410075018,
-177.298614236585));
#160872=CARTESIAN_POINT('Ctrl Pts',(40.2954165061835,-64.0445696646893,
-177.306010739179));
#160873=CARTESIAN_POINT('Ctrl Pts',(40.3115733877844,-64.0400571937476,
-177.312967023157));
#160874=CARTESIAN_POINT('Ctrl Pts',(40.3287235889739,-64.0352854835157,
-177.319245722133));
#160875=CARTESIAN_POINT('Ctrl Pts',(40.3454088974569,-64.030643120646,-177.325354223609));
#160876=CARTESIAN_POINT('Ctrl Pts',(40.3630347088931,-64.0257552846044,
-177.330821391408));
#160877=CARTESIAN_POINT('Ctrl Pts',(40.3815578620981,-64.0206156603447,
-177.335399595475));
#160878=CARTESIAN_POINT('Ctrl Pts',(40.3996915438975,-64.0155841028197,
-177.339881537336));
#160879=CARTESIAN_POINT('Ctrl Pts',(40.4186855087824,-64.0103111421447,
-177.343511544901));
#160880=CARTESIAN_POINT('Ctrl Pts',(40.4384598241584,-64.0048023205012,
-177.346028622878));
#160881=CARTESIAN_POINT('Ctrl Pts',(40.4582341395344,-63.9992934988578,
-177.348545700855));
#160882=CARTESIAN_POINT('Ctrl Pts',(40.4787891949221,-63.9935486879891,
-177.34995));
#160883=CARTESIAN_POINT('Ctrl Pts',(40.5,-63.9875867194884,-177.34995));
#160884=CARTESIAN_POINT('Origin',(45.6308101826775,-63.2664983737155,-177.84995));
#160885=CARTESIAN_POINT('',(40.9304134495199,-63.4221822677665,-177.84995));
#160886=CARTESIAN_POINT('',(45.5612236321975,-62.7713643393447,-177.84995));
#160887=CARTESIAN_POINT('Origin',(41.,-63.9173163021373,-177.84995));
#160888=CARTESIAN_POINT('Ctrl Pts',(41.,-63.9173163021373,-177.34995));
#160889=CARTESIAN_POINT('Ctrl Pts',(40.9304134495199,-63.4221822677665,
-177.34995));
#160890=CARTESIAN_POINT('Ctrl Pts',(40.9304134495199,-63.4221822677665,
-177.84995));
#160891=CARTESIAN_POINT('Ctrl Pts',(41.1312673457634,-63.8804194574513,
-177.34995));
#160892=CARTESIAN_POINT('Ctrl Pts',(41.0616024612649,-63.4037448545523,
-177.367861075732));
#160893=CARTESIAN_POINT('Ctrl Pts',(41.1929481410454,-63.3852854230811,
-177.849949999941));
#160894=CARTESIAN_POINT('Ctrl Pts',(41.2609933446562,-63.8439558571173,
-177.296063436531));
#160895=CARTESIAN_POINT('Ctrl Pts',(41.2106847809575,-63.3827927009057,
-177.329589659683));
#160896=CARTESIAN_POINT('Ctrl Pts',(41.4524001388343,-63.3488218227467,
-177.742176873059));
#160897=CARTESIAN_POINT('Ctrl Pts',(41.4461134365302,-63.7919219926539,
-177.110943344657));
#160898=CARTESIAN_POINT('Ctrl Pts',(41.4304920983899,-63.3519007970349,
-177.142957948483));
#160899=CARTESIAN_POINT('Ctrl Pts',(41.8226403225787,-63.2967879582829,
-177.371936689315));
#160900=CARTESIAN_POINT('Ctrl Pts',(41.5,-63.7767754674458,-176.981217345763));
#160901=CARTESIAN_POINT('Ctrl Pts',(41.4999999999415,-63.342132098545,-176.997671841189));
#160902=CARTESIAN_POINT('Ctrl Pts',(41.9304134494542,-63.2816414330733,
-177.112484691526));
#160903=CARTESIAN_POINT('Ctrl Pts',(41.5,-63.7767754674349,-176.84995));
#160904=CARTESIAN_POINT('Ctrl Pts',(41.5,-63.3421320985267,-176.84995));
#160905=CARTESIAN_POINT('Ctrl Pts',(41.9304134495199,-63.2816414330641,
-176.84995));
#160906=CARTESIAN_POINT('',(41.9304134495199,-63.2816414330641,-176.84995));
#160907=CARTESIAN_POINT('Ctrl Pts',(41.9304134495199,-63.2816414330641,
-176.84995));
#160908=CARTESIAN_POINT('Ctrl Pts',(41.9304134494542,-63.2816414330733,
-177.112484691526));
#160909=CARTESIAN_POINT('Ctrl Pts',(41.8226403225787,-63.2967879582829,
-177.371936689315));
#160910=CARTESIAN_POINT('Ctrl Pts',(41.6375202307065,-63.3228048905148,
-177.557056781187));
#160911=CARTESIAN_POINT('Ctrl Pts',(41.4524001388343,-63.3488218227467,
-177.742176873059));
#160912=CARTESIAN_POINT('Ctrl Pts',(41.1929481410454,-63.3852854230811,
-177.849949999941));
#160913=CARTESIAN_POINT('Ctrl Pts',(40.9304134495199,-63.4221822677665,
-177.84995));
#160914=CARTESIAN_POINT('',(41.5,-63.7767754674349,-176.84995));
#160915=CARTESIAN_POINT('Origin',(42.,-63.7767754674349,-176.84995));
#160916=CARTESIAN_POINT('Ctrl Pts',(41.,-63.9173163021373,-177.34995));
#160917=CARTESIAN_POINT('Ctrl Pts',(41.0209105170156,-63.9114387391064,
-177.34995));
#160918=CARTESIAN_POINT('Ctrl Pts',(41.0411797466411,-63.9057414302056,
-177.348585219097));
#160919=CARTESIAN_POINT('Ctrl Pts',(41.0606899838377,-63.9002574601638,
-177.346136042571));
#160920=CARTESIAN_POINT('Ctrl Pts',(41.0806295626856,-63.894652810054,-177.343632969544));
#160921=CARTESIAN_POINT('Ctrl Pts',(41.0997766651611,-63.8892709105259,
-177.33999719389));
#160922=CARTESIAN_POINT('Ctrl Pts',(41.1180516974373,-63.8841341339452,
-177.335495637057));
#160923=CARTESIAN_POINT('Ctrl Pts',(41.1369112963569,-63.8788330463966,
-177.33085008814));
#160924=CARTESIAN_POINT('Ctrl Pts',(41.1548424167097,-63.8737929371535,
-177.32528246904));
#160925=CARTESIAN_POINT('Ctrl Pts',(41.1718018468568,-63.8690259522156,
-177.319052501424));
#160926=CARTESIAN_POINT('Ctrl Pts',(41.1874915731201,-63.864615857765,-177.313288953611));
#160927=CARTESIAN_POINT('Ctrl Pts',(41.2023504278525,-63.8604393060714,
-177.306958054963));
#160928=CARTESIAN_POINT('Ctrl Pts',(41.2163727601653,-63.8564978854959,
-177.300241547043));
#160929=CARTESIAN_POINT('Ctrl Pts',(41.2346217845916,-63.8513684192452,
-177.291500510647));
#160930=CARTESIAN_POINT('Ctrl Pts',(41.2514605911863,-63.8466353393768,
-177.282104513309));
#160931=CARTESIAN_POINT('Ctrl Pts',(41.2669358413727,-63.84228553022,-177.272394746022));
#160932=CARTESIAN_POINT('Ctrl Pts',(41.2822211818629,-63.8379891011976,
-177.262804135385));
#160933=CARTESIAN_POINT('Ctrl Pts',(41.2961768440954,-63.8340664203597,
-177.252906955733));
#160934=CARTESIAN_POINT('Ctrl Pts',(41.3088862629837,-63.8304940356814,
-177.242983686129));
#160935=CARTESIAN_POINT('Ctrl Pts',(41.321754987491,-63.8268768731138,-177.232936033763));
#160936=CARTESIAN_POINT('Ctrl Pts',(41.3333462707914,-63.8236187758533,
-177.222861821372));
#160937=CARTESIAN_POINT('Ctrl Pts',(41.3437756488962,-63.8206872688448,
-177.213007510354));
#160938=CARTESIAN_POINT('Ctrl Pts',(41.3450359570273,-63.8203330193313,
-177.211816694547));
#160939=CARTESIAN_POINT('Ctrl Pts',(41.3462793254426,-63.8199835312615,
-177.210629037565));
#160940=CARTESIAN_POINT('Ctrl Pts',(41.3475059843113,-63.8196387399389,
-177.209444926088));
#160941=CARTESIAN_POINT('Ctrl Pts',(41.348767397019,-63.8192841799492,-177.208227266229));
#160942=CARTESIAN_POINT('Ctrl Pts',(41.3496021366109,-63.8190495499469,
-177.207413007319));
#160943=CARTESIAN_POINT('Ctrl Pts',(41.3507626710068,-63.8187233292422,
-177.206271333214));
#160944=CARTESIAN_POINT('Ctrl Pts',(41.3514998739256,-63.8185161050044,
-177.205546110864));
#160945=CARTESIAN_POINT('Ctrl Pts',(41.3523682910511,-63.8182719925005,
-177.204688490104));
#160946=CARTESIAN_POINT('Ctrl Pts',(41.3535533858468,-63.8179388573381,
-177.20350339534));
#160947=CARTESIAN_POINT('Ctrl Pts',(41.3741026274597,-63.8121623785577,
-177.182954154279));
#160948=CARTESIAN_POINT('Ctrl Pts',(41.3925303081874,-63.8069824362895,
-177.160790380405));
#160949=CARTESIAN_POINT('Ctrl Pts',(41.4087935545141,-63.802411011162,-177.137499857787));
#160950=CARTESIAN_POINT('Ctrl Pts',(41.4250773096292,-63.7978338212329,
-177.114179964625));
#160951=CARTESIAN_POINT('Ctrl Pts',(41.4391911870226,-63.7938666788792,
-177.089730493817));
#160952=CARTESIAN_POINT('Ctrl Pts',(41.4511153275536,-63.7905151006712,
-177.064594612174));
#160953=CARTESIAN_POINT('Ctrl Pts',(41.463060046626,-63.7871577383489,-177.039415351322));
#160954=CARTESIAN_POINT('Ctrl Pts',(41.4728074902942,-63.7844180594708,
-177.013547308752));
#160955=CARTESIAN_POINT('Ctrl Pts',(41.4803606027944,-63.7822951743491,
-176.98738923497));
#160956=CARTESIAN_POINT('Ctrl Pts',(41.4879480469337,-63.7801626399437,
-176.961112263243));
#160957=CARTESIAN_POINT('Ctrl Pts',(41.4933211911952,-63.7786525123415,
-176.934542621811));
#160958=CARTESIAN_POINT('Ctrl Pts',(41.4965057497471,-63.7777575025999,
-176.908037356561));
#160959=CARTESIAN_POINT('Ctrl Pts',(41.498841154035,-63.7771011448806,-176.888599651426));
#160960=CARTESIAN_POINT('Ctrl Pts',(41.5,-63.7767754674349,-176.86919558342));
#160961=CARTESIAN_POINT('Ctrl Pts',(41.5,-63.7767754674349,-176.84995));
#160962=CARTESIAN_POINT('Origin',(45.4220505312374,-61.7810962706031,-172.64995));
#160963=CARTESIAN_POINT('',(42.,-62.2620341086569,-171.64995));
#160964=CARTESIAN_POINT('',(44.489435756687,-61.9121667294742,-171.64995));
#160965=CARTESIAN_POINT('',(44.489435756687,-61.9121667294742,-171.64995));
#160966=CARTESIAN_POINT('',(41.9304134495199,-63.2816414330641,-172.64995));
#160967=CARTESIAN_POINT('Ctrl Pts',(42.,-62.2620341086569,-171.64995));
#160968=CARTESIAN_POINT('Ctrl Pts',(41.9980582289126,-62.2904856414507,
-171.64995));
#160969=CARTESIAN_POINT('Ctrl Pts',(41.9961974246729,-62.3177508186883,
-171.651129585072));
#160970=CARTESIAN_POINT('Ctrl Pts',(41.9944225652579,-62.3437567012451,
-171.653192621565));
#160971=CARTESIAN_POINT('Ctrl Pts',(41.992554516627,-62.3711280259236,-171.655363978048));
#160972=CARTESIAN_POINT('Ctrl Pts',(41.9907816512346,-62.3971046913403,
-171.658513818877));
#160973=CARTESIAN_POINT('Ctrl Pts',(41.9891066446116,-62.4216474946475,
-171.662335033674));
#160974=CARTESIAN_POINT('Ctrl Pts',(41.9876075219068,-62.4436131831248,
-171.665755002159));
#160975=CARTESIAN_POINT('Ctrl Pts',(41.9861867195882,-62.4644312929545,
-171.66971333967));
#160976=CARTESIAN_POINT('Ctrl Pts',(41.9848444729658,-62.48409837629,-171.674015027433));
#160977=CARTESIAN_POINT('Ctrl Pts',(41.9832381238233,-62.5076351853414,
-171.679163121929));
#160978=CARTESIAN_POINT('Ctrl Pts',(41.9817442598049,-62.529523821642,-171.684802100301));
#160979=CARTESIAN_POINT('Ctrl Pts',(41.9803611921887,-62.5497890289526,
-171.690639736275));
#160980=CARTESIAN_POINT('Ctrl Pts',(41.9789186268577,-62.5709260183172,
-171.696728499524));
#160981=CARTESIAN_POINT('Ctrl Pts',(41.9775965324992,-62.5902978233885,
-171.703033282531));
#160982=CARTESIAN_POINT('Ctrl Pts',(41.9763912815383,-62.6079575967058,
-171.709272496533));
#160983=CARTESIAN_POINT('Ctrl Pts',(41.9758744940028,-62.6155297547265,
-171.711947746861));
#160984=CARTESIAN_POINT('Ctrl Pts',(41.9753791758627,-62.6227873353951,
-171.714611542068));
#160985=CARTESIAN_POINT('Ctrl Pts',(41.9749049735149,-62.6297355198322,
-171.717244495073));
#160986=CARTESIAN_POINT('Ctrl Pts',(41.9747845954644,-62.6314993425993,
-171.717912880101));
#160987=CARTESIAN_POINT('Ctrl Pts',(41.9747281084734,-62.6323259736101,
-171.718228248943));
#160988=CARTESIAN_POINT('Ctrl Pts',(41.9746071368898,-62.6340978795566,
-171.718908958995));
#160989=CARTESIAN_POINT('Ctrl Pts',(41.9745512101076,-62.6349170553895,
-171.719223660362));
#160990=CARTESIAN_POINT('Ctrl Pts',(41.9744815093958,-62.6359381423105,
-171.719616772037));
#160991=CARTESIAN_POINT('Ctrl Pts',(41.9743854515175,-62.6373456585733,
-171.720163005656));
#160992=CARTESIAN_POINT('Ctrl Pts',(41.974044857537,-62.6423363118667,-171.72209979508));
#160993=CARTESIAN_POINT('Ctrl Pts',(41.9737064547852,-62.6472948480561,
-171.724069245188));
#160994=CARTESIAN_POINT('Ctrl Pts',(41.9733702655354,-62.6522209415428,
-171.72607046184));
#160995=CARTESIAN_POINT('Ctrl Pts',(41.9710922898651,-62.6855995255356,
-171.739630451773));
#160996=CARTESIAN_POINT('Ctrl Pts',(41.96891676217,-62.7174765613617,-171.754642782338));
#160997=CARTESIAN_POINT('Ctrl Pts',(41.9668469622313,-62.7478042229328,
-171.770779293398));
#160998=CARTESIAN_POINT('Ctrl Pts',(41.9648622623225,-62.7768849596891,
-171.786252350205));
#160999=CARTESIAN_POINT('Ctrl Pts',(41.9629747403081,-62.8045416149154,
-171.802759466707));
#161000=CARTESIAN_POINT('Ctrl Pts',(41.9611851663792,-62.8307630998555,
-171.820043746496));
#161001=CARTESIAN_POINT('Ctrl Pts',(41.9591798424644,-62.8601458316816,
-171.839411808946));
#161002=CARTESIAN_POINT('Ctrl Pts',(41.9572974703087,-62.8877270298286,
-171.85975577606));
#161003=CARTESIAN_POINT('Ctrl Pts',(41.9555364549236,-62.9135300646481,
-171.88075761506));
#161004=CARTESIAN_POINT('Ctrl Pts',(41.954708197691,-62.9256659894071,-171.890635396478));
#161005=CARTESIAN_POINT('Ctrl Pts',(41.9539067520679,-62.9374090607585,
-171.900659292264));
#161006=CARTESIAN_POINT('Ctrl Pts',(41.9531317849258,-62.9487641598237,
-171.910799109226));
#161007=CARTESIAN_POINT('Ctrl Pts',(41.9527566361052,-62.9542609761269,
-171.915707627493));
#161008=CARTESIAN_POINT('Ctrl Pts',(41.9524097468125,-62.9593437235203,
-171.920348851332));
#161009=CARTESIAN_POINT('Ctrl Pts',(41.95205994185,-62.9644690402784,-171.92512412732));
#161010=CARTESIAN_POINT('Ctrl Pts',(41.9517205761669,-62.9694414014787,
-171.929756894068));
#161011=CARTESIAN_POINT('Ctrl Pts',(41.9513784560339,-62.9744539787111,
-171.934515912466));
#161012=CARTESIAN_POINT('Ctrl Pts',(41.9510073810277,-62.9798905322648,
-171.939801580944));
#161013=CARTESIAN_POINT('Ctrl Pts',(41.9509375838925,-62.9809131176108,
-171.94079578565));
#161014=CARTESIAN_POINT('Ctrl Pts',(41.9508667695452,-62.9819505975796,
-171.941808724746));
#161015=CARTESIAN_POINT('Ctrl Pts',(41.9507947743353,-62.9830053691253,
-171.94284321151));
#161016=CARTESIAN_POINT('Ctrl Pts',(41.9484463931933,-63.0174105137634,
-171.976586695463));
#161017=CARTESIAN_POINT('Ctrl Pts',(41.9462900974066,-63.0490042695942,
-172.012463058058));
#161018=CARTESIAN_POINT('Ctrl Pts',(41.9443343814679,-63.077660482026,-172.04995975798));
#161019=CARTESIAN_POINT('Ctrl Pts',(41.9423469358413,-63.1067816150827,
-172.088064807285));
#161020=CARTESIAN_POINT('Ctrl Pts',(41.9405666290003,-63.1328691487862,
-172.127843232645));
#161021=CARTESIAN_POINT('Ctrl Pts',(41.9390005719262,-63.1558171936301,
-172.168804472013));
#161022=CARTESIAN_POINT('Ctrl Pts',(41.9377708916514,-63.1738361780941,
-172.200967557837));
#161023=CARTESIAN_POINT('Ctrl Pts',(41.9366732704211,-63.1899200496495,
-172.23386087479));
#161024=CARTESIAN_POINT('Ctrl Pts',(41.935710408276,-63.2040284471142,-172.267266567535));
#161025=CARTESIAN_POINT('Ctrl Pts',(41.9356150487611,-63.2054257083375,
-172.270574985747));
#161026=CARTESIAN_POINT('Ctrl Pts',(41.9355210125586,-63.2068035707444,
-172.273888354284));
#161027=CARTESIAN_POINT('Ctrl Pts',(41.9354282968065,-63.2081620755033,
-172.27720644167));
#161028=CARTESIAN_POINT('Ctrl Pts',(41.9342160400824,-63.2259244997996,
-172.320590372139));
#161029=CARTESIAN_POINT('Ctrl Pts',(41.9332297201087,-63.240376417052,-172.364775502563));
#161030=CARTESIAN_POINT('Ctrl Pts',(41.9324628528116,-63.2516128342556,
-172.409267414287));
#161031=CARTESIAN_POINT('Ctrl Pts',(41.9316869655132,-63.262981415784,-172.454282646156));
#161032=CARTESIAN_POINT('Ctrl Pts',(41.9311357225737,-63.2710584268555,
-172.49961194977));
#161033=CARTESIAN_POINT('Ctrl Pts',(41.9308018218113,-63.27595086168,-172.544796239962));
#161034=CARTESIAN_POINT('Ctrl Pts',(41.9305416776487,-63.2797625881098,
-172.579999601747));
#161035=CARTESIAN_POINT('Ctrl Pts',(41.9304134495199,-63.2816414330641,
-172.615116019647));
#161036=CARTESIAN_POINT('Ctrl Pts',(41.9304134495199,-63.2816414330641,
-172.64995));
#161037=CARTESIAN_POINT('',(44.628608857647,-62.9024347982158,-172.64995));
#161038=CARTESIAN_POINT('',(41.5,-63.3421320985267,-172.64995));
#161039=CARTESIAN_POINT('Origin',(44.489435756687,-61.9121667294742,-172.64995));
#161040=CARTESIAN_POINT('Origin',(44.2110895547669,-59.9316305919911,-172.64995));
#161041=CARTESIAN_POINT('',(46.2674193015002,-62.1160087581289,-172.64995));
#161042=CARTESIAN_POINT('Origin',(44.2110895547669,-59.9316305919911,-172.64995));
#161043=CARTESIAN_POINT('',(45.5819760525891,-61.3878827027496,-171.64995));
#161044=CARTESIAN_POINT('Origin',(45.5819760525891,-61.3878827027496,-172.64995));
#161045=CARTESIAN_POINT('Origin',(44.2110895547669,-59.9316305919911,-171.64995));
#161046=CARTESIAN_POINT('Origin',(0.,-12.9675000200281,-172.64995));
#161047=CARTESIAN_POINT('',(49.148508738101,-59.2349193215281,-172.64995));
#161048=CARTESIAN_POINT('Origin',(0.,-12.9675000200281,-172.64995));
#161049=CARTESIAN_POINT('',(48.4203826827217,-58.549476072617,-171.64995));
#161050=CARTESIAN_POINT('Origin',(48.4203826827217,-58.549476072617,-172.64995));
#161051=CARTESIAN_POINT('Origin',(0.,-12.9675000200281,-171.64995));
#161052=CARTESIAN_POINT('Origin',(46.9641305719631,-57.1785895747948,-172.64995));
#161053=CARTESIAN_POINT('',(49.9349347781878,-57.596108877675,-172.64995));
#161054=CARTESIAN_POINT('Origin',(46.9641305719631,-57.1785895747948,-172.64995));
#161055=CARTESIAN_POINT('',(48.9446667094463,-57.4569357767149,-171.64995));
#161056=CARTESIAN_POINT('Origin',(48.9446667094463,-57.4569357767149,-172.64995));
#161057=CARTESIAN_POINT('Origin',(46.9641305719631,-57.1785895747948,-171.64995));
#161058=CARTESIAN_POINT('Ctrl Pts',(51.9388724063314,-46.43000002,-176.84995));
#161059=CARTESIAN_POINT('Ctrl Pts',(51.5042290374232,-46.43000002,-176.84995));
#161060=CARTESIAN_POINT('Ctrl Pts',(51.4437383719606,-46.86041346952,-176.84995));
#161061=CARTESIAN_POINT('Ctrl Pts',(51.9388724063423,-46.43000002,-176.981217345763));
#161062=CARTESIAN_POINT('Ctrl Pts',(51.5042290374242,-46.4300000199415,
-176.997671841189));
#161063=CARTESIAN_POINT('Ctrl Pts',(51.4437383719698,-46.8604134694541,
-177.112484691526));
#161064=CARTESIAN_POINT('Ctrl Pts',(51.9540189315504,-46.3761134565303,
-177.110943344657));
#161065=CARTESIAN_POINT('Ctrl Pts',(51.5139977359314,-46.3604921183892,
-177.142957948483));
#161066=CARTESIAN_POINT('Ctrl Pts',(51.4588848971795,-46.7526403425778,
-177.371936689315));
#161067=CARTESIAN_POINT('Ctrl Pts',(52.0060527960138,-46.1909933646562,
-177.296063436531));
#161068=CARTESIAN_POINT('Ctrl Pts',(51.5448896398021,-46.1406848009587,
-177.329589659683));
#161069=CARTESIAN_POINT('Ctrl Pts',(51.5109187616431,-46.3824001588352,
-177.742176873059));
#161070=CARTESIAN_POINT('Ctrl Pts',(52.0425163963479,-46.0612673657634,
-177.34995));
#161071=CARTESIAN_POINT('Ctrl Pts',(51.5658417934483,-45.9916024812643,
-177.367861075732));
#161072=CARTESIAN_POINT('Ctrl Pts',(51.5473823619777,-46.1229481610447,
-177.849949999941));
#161073=CARTESIAN_POINT('Ctrl Pts',(52.0794132410337,-45.93000002,-177.34995));
#161074=CARTESIAN_POINT('Ctrl Pts',(51.584279206663,-45.8604134695199,-177.34995));
#161075=CARTESIAN_POINT('Ctrl Pts',(51.584279206663,-45.86041346952,-177.84995));
#161076=CARTESIAN_POINT('',(51.584279206663,-45.86041346952,-177.84995));
#161077=CARTESIAN_POINT('Origin',(52.0794132410337,-45.93000002,-177.84995));
#161078=CARTESIAN_POINT('',(51.9388724063314,-46.43000002,-176.84995));
#161079=CARTESIAN_POINT('Ctrl Pts',(51.9388724063314,-46.43000002,-176.84995));
#161080=CARTESIAN_POINT('Ctrl Pts',(51.9388724063314,-46.43000002,-176.875800002306));
#161081=CARTESIAN_POINT('Ctrl Pts',(51.939460433088,-46.4279080061138,-176.901947474014));
#161082=CARTESIAN_POINT('Ctrl Pts',(51.9406481740044,-46.4236823982402,
-176.928073316625));
#161083=CARTESIAN_POINT('Ctrl Pts',(51.9418458934022,-46.4194212900745,
-176.954418648378));
#161084=CARTESIAN_POINT('Ctrl Pts',(51.9436534585173,-46.4129905430327,
-176.980741922985));
#161085=CARTESIAN_POINT('Ctrl Pts',(51.9460748639913,-46.4043759454358,
-177.006671795364));
#161086=CARTESIAN_POINT('Ctrl Pts',(51.9469983122141,-46.4010906076739,
-177.016560636708));
#161087=CARTESIAN_POINT('Ctrl Pts',(51.9480109554861,-46.3974879420354,
-177.026391811965));
#161088=CARTESIAN_POINT('Ctrl Pts',(51.9491127083337,-46.3935682526079,
-177.036143091591));
#161089=CARTESIAN_POINT('Ctrl Pts',(51.9519697581159,-46.3834037698484,
-177.06142997094));
#161090=CARTESIAN_POINT('Ctrl Pts',(51.9554279693915,-46.3711005439436,
-177.086198360269));
#161091=CARTESIAN_POINT('Ctrl Pts',(51.9594871634071,-46.3566592108427,
-177.110048753582));
#161092=CARTESIAN_POINT('Ctrl Pts',(51.9627845431406,-46.3449281728812,
-177.129422994686));
#161093=CARTESIAN_POINT('Ctrl Pts',(51.966478933354,-46.3317846967454,-177.148192204337));
#161094=CARTESIAN_POINT('Ctrl Pts',(51.9705652450017,-46.3172468876564,
-177.166105767697));
#161095=CARTESIAN_POINT('Ctrl Pts',(51.9727647076396,-46.3094218927259,
-177.175747766819));
#161096=CARTESIAN_POINT('Ctrl Pts',(51.9750776449811,-46.3011931905608,
-177.185141381874));
#161097=CARTESIAN_POINT('Ctrl Pts',(51.9775020131174,-46.2925680527438,
-177.194242926223));
#161098=CARTESIAN_POINT('Ctrl Pts',(51.977984409055,-46.2908518400194,-177.19605393337));
#161099=CARTESIAN_POINT('Ctrl Pts',(51.978571809157,-46.2887620555822,-177.198223909681));
#161100=CARTESIAN_POINT('Ctrl Pts',(51.9790900053177,-46.2869184469911,
-177.200104635539));
#161101=CARTESIAN_POINT('Ctrl Pts',(51.9794650751736,-46.2855840449618,
-177.201465903008));
#161102=CARTESIAN_POINT('Ctrl Pts',(51.9798035148913,-46.2843799457124,
-177.202676855488));
#161103=CARTESIAN_POINT('Ctrl Pts',(51.9800358214742,-46.2835534076204,
-177.203503393566));
#161104=CARTESIAN_POINT('Ctrl Pts',(51.982778794659,-46.2737940121103,-177.213262788912));
#161105=CARTESIAN_POINT('Ctrl Pts',(51.9858410519141,-46.2628991858342,
-177.223316643279));
#161106=CARTESIAN_POINT('Ctrl Pts',(51.9892581813619,-46.2507420960314,
-177.23342869837));
#161107=CARTESIAN_POINT('Ctrl Pts',(51.9925283434545,-46.2391078706274,
-177.243105843981));
#161108=CARTESIAN_POINT('Ctrl Pts',(51.9961237076887,-46.22631691666,-177.252836300724));
#161109=CARTESIAN_POINT('Ctrl Pts',(52.0000690386848,-46.2122809307154,
-177.262372868916));
#161110=CARTESIAN_POINT('Ctrl Pts',(52.0037880358436,-46.1990501544125,
-177.271362347883));
#161111=CARTESIAN_POINT('Ctrl Pts',(52.0078181206063,-46.1847126616024,
-177.280179445043));
#161112=CARTESIAN_POINT('Ctrl Pts',(52.0121719933272,-46.1692230962462,
-177.288581471766));
#161113=CARTESIAN_POINT('Ctrl Pts',(52.0139487850297,-46.1629018891359,
-177.29201029303));
#161114=CARTESIAN_POINT('Ctrl Pts',(52.0157793940052,-46.1563891942317,
-177.295369566868));
#161115=CARTESIAN_POINT('Ctrl Pts',(52.0176641944465,-46.1496836682356,
-177.298640995833));
#161116=CARTESIAN_POINT('Ctrl Pts',(52.0219346251205,-46.1344908216757,
-177.306053138942));
#161117=CARTESIAN_POINT('Ctrl Pts',(52.0264864211104,-46.1182969659914,
-177.313020714078));
#161118=CARTESIAN_POINT('Ctrl Pts',(52.0313178036988,-46.1011084292979,
-177.319306663921));
#161119=CARTESIAN_POINT('Ctrl Pts',(52.0360111994689,-46.084410806219,-177.325413083744));
#161120=CARTESIAN_POINT('Ctrl Pts',(52.0409685266907,-46.06677419821,-177.330876292405));
#161121=CARTESIAN_POINT('Ctrl Pts',(52.0461782020365,-46.0482398151008,
-177.335449266094));
#161122=CARTESIAN_POINT('Ctrl Pts',(52.0512666586451,-46.0301366900576,
-177.339915835822));
#161123=CARTESIAN_POINT('Ctrl Pts',(52.0565959389366,-46.0111767902437,
-177.343533167656));
#161124=CARTESIAN_POINT('Ctrl Pts',(52.0621443742083,-45.9914372060744,
-177.34604166628));
#161125=CARTESIAN_POINT('Ctrl Pts',(52.06769280948,-45.9716976219051,-177.348550164905));
#161126=CARTESIAN_POINT('Ctrl Pts',(52.0734605256988,-45.9511779052299,
-177.34995));
#161127=CARTESIAN_POINT('Ctrl Pts',(52.0794132410337,-45.93000002,-177.34995));
#161128=CARTESIAN_POINT('',(51.4437383719606,-46.86041346952,-176.84995));
#161129=CARTESIAN_POINT('Origin',(51.9388724063314,-46.93000002,-176.84995));
#161130=CARTESIAN_POINT('Ctrl Pts',(51.584279206663,-45.86041346952,-177.84995));
#161131=CARTESIAN_POINT('Ctrl Pts',(51.5473823619777,-46.1229481610447,
-177.849949999941));
#161132=CARTESIAN_POINT('Ctrl Pts',(51.5109187616431,-46.3824001588352,
-177.742176873059));
#161133=CARTESIAN_POINT('Ctrl Pts',(51.4849018294113,-46.5675202507065,
-177.557056781187));
#161134=CARTESIAN_POINT('Ctrl Pts',(51.4588848971795,-46.7526403425778,
-177.371936689315));
#161135=CARTESIAN_POINT('Ctrl Pts',(51.4437383719698,-46.8604134694541,
-177.112484691526));
#161136=CARTESIAN_POINT('Ctrl Pts',(51.4437383719606,-46.86041346952,-176.84995));
#161137=CARTESIAN_POINT('Origin',(53.1076143453209,-38.6139690140329,-177.84995));
#161138=CARTESIAN_POINT('',(51.6545496240141,-45.3604134695199,-177.84995));
#161139=CARTESIAN_POINT('',(52.6124803109501,-38.5443824635529,-177.84995));
#161140=CARTESIAN_POINT('Origin',(52.1496836583849,-45.43000002,-177.84995));
#161141=CARTESIAN_POINT('Ctrl Pts',(52.1497209086987,-45.4300399704538,
-177.349950000614));
#161142=CARTESIAN_POINT('Ctrl Pts',(51.6545448046101,-45.3604477613618,
-177.349907583593));
#161143=CARTESIAN_POINT('Ctrl Pts',(51.6545402370025,-45.3604802615783,
-177.849949997675));
#161144=CARTESIAN_POINT('Ctrl Pts',(52.1866217328369,-45.2987616698911,
-177.349960874823));
#161145=CARTESIAN_POINT('Ctrl Pts',(51.6738419432767,-45.2231414851577,
-177.331166751555));
#161146=CARTESIAN_POINT('Ctrl Pts',(51.6914402841046,-45.097922783674,-177.849968278574));
#161147=CARTESIAN_POINT('Ctrl Pts',(52.2230902788089,-45.1690198513555,
-177.296074808573));
#161148=CARTESIAN_POINT('Ctrl Pts',(51.6896993598511,-45.1103101034141,
-177.25721607327));
#161149=CARTESIAN_POINT('Ctrl Pts',(51.7279078626935,-44.8384424791336,
-177.742192571987));
#161150=CARTESIAN_POINT('Ctrl Pts',(52.2751299595662,-44.9838805435436,
-177.110939115585));
#161151=CARTESIAN_POINT('Ctrl Pts',(51.7103493697401,-44.9633776482459,
-177.069853325702));
#161152=CARTESIAN_POINT('Ctrl Pts',(51.7799461398382,-44.4681708975332,
-177.371920990387));
#161153=CARTESIAN_POINT('Ctrl Pts',(52.2902773198134,-44.9299908778567,
-176.981197291835));
#161154=CARTESIAN_POINT('Ctrl Pts',(51.7150329623736,-44.9300521550416,
-176.95888267251));
#161155=CARTESIAN_POINT('Ctrl Pts',(51.7950930276016,-44.3603951909531,
-177.112440685846));
#161156=CARTESIAN_POINT('Ctrl Pts',(52.2902747589836,-44.9300000186359,
-176.849916603474));
#161157=CARTESIAN_POINT('Ctrl Pts',(51.7150321621775,-44.9300578487394,
-176.849922286133));
#161158=CARTESIAN_POINT('Ctrl Pts',(51.7950904583897,-44.3604134718452,
-176.849883207942));
#161159=CARTESIAN_POINT('',(51.7950904587165,-44.36041346952,-176.84995));
#161160=CARTESIAN_POINT('Ctrl Pts',(51.7950904587165,-44.36041346952,-176.84995));
#161161=CARTESIAN_POINT('Ctrl Pts',(51.7950904587073,-44.3604134695857,
-177.112484691526));
#161162=CARTESIAN_POINT('Ctrl Pts',(51.7799439334977,-44.4681865964612,
-177.371936689315));
#161163=CARTESIAN_POINT('Ctrl Pts',(51.7539270012658,-44.6533066883334,
-177.557056781187));
#161164=CARTESIAN_POINT('Ctrl Pts',(51.7279100690339,-44.8384267802056,
-177.742176873059));
#161165=CARTESIAN_POINT('Ctrl Pts',(51.6914464686995,-45.0978787779945,
-177.849949999941));
#161166=CARTESIAN_POINT('Ctrl Pts',(51.6545496240141,-45.3604134695199,
-177.84995));
#161167=CARTESIAN_POINT('',(52.2902244930873,-44.93000002,-176.84995));
#161168=CARTESIAN_POINT('Origin',(52.2902244930873,-44.43000002,-176.84995));
#161169=CARTESIAN_POINT('Ctrl Pts',(52.1496836583849,-45.43000002,-177.34995));
#161170=CARTESIAN_POINT('Ctrl Pts',(52.1557508202169,-45.4084149701999,
-177.34995));
#161171=CARTESIAN_POINT('Ctrl Pts',(52.1615771773264,-45.3874879725988,
-177.348552025671));
#161172=CARTESIAN_POINT('Ctrl Pts',(52.1671627297135,-45.367368300209,-177.346011757925));
#161173=CARTESIAN_POINT('Ctrl Pts',(52.172739418816,-45.3472805541836,-177.343475521136));
#161174=CARTESIAN_POINT('Ctrl Pts',(52.1780760668187,-45.3279969954851,
-177.339801327605));
#161175=CARTESIAN_POINT('Ctrl Pts',(52.1831726737217,-45.309608680057,-177.335239527258));
#161176=CARTESIAN_POINT('Ctrl Pts',(52.1884924652697,-45.2904151250394,
-177.33047796189));
#161177=CARTESIAN_POINT('Ctrl Pts',(52.1935507322084,-45.2721966220856,
-177.324750042966));
#161178=CARTESIAN_POINT('Ctrl Pts',(52.1983474745379,-45.2550003525823,
-177.318324974143));
#161179=CARTESIAN_POINT('Ctrl Pts',(52.2027636467357,-45.2391684228957,
-177.31240966572));
#161180=CARTESIAN_POINT('Ctrl Pts',(52.206958146453,-45.2242018844323,-177.305903491103));
#161181=CARTESIAN_POINT('Ctrl Pts',(52.2109309736898,-45.2101026376804,
-177.298999152375));
#161182=CARTESIAN_POINT('Ctrl Pts',(52.2155599839996,-45.1936746495792,
-177.290954439316));
#161183=CARTESIAN_POINT('Ctrl Pts',(52.2198880482107,-45.1784243291713,
-177.282370206816));
#161184=CARTESIAN_POINT('Ctrl Pts',(52.223915166323,-45.1643108658193,-177.273517318558));
#161185=CARTESIAN_POINT('Ctrl Pts',(52.2270926918441,-45.1531748899825,
-177.266532105414));
#161186=CARTESIAN_POINT('Ctrl Pts',(52.2300828568474,-45.1427456090391,
-177.259378907546));
#161187=CARTESIAN_POINT('Ctrl Pts',(52.232885661333,-45.13298799345,-177.252173639391));
#161188=CARTESIAN_POINT('Ctrl Pts',(52.2360631664952,-45.1219259040088,
-177.244005115015));
#161189=CARTESIAN_POINT('Ctrl Pts',(52.238999866935,-45.111726951001,-177.235770093483));
#161190=CARTESIAN_POINT('Ctrl Pts',(52.2416957626522,-45.1023265017848,
-177.227613958382));
#161191=CARTESIAN_POINT('Ctrl Pts',(52.2430437105108,-45.0976262771767,
-177.223535890831));
#161192=CARTESIAN_POINT('Ctrl Pts',(52.2443314571889,-45.0931254933336,
-177.219477157756));
#161193=CARTESIAN_POINT('Ctrl Pts',(52.2455590026863,-45.0888152125502,
-177.215453662315));
#161194=CARTESIAN_POINT('Ctrl Pts',(52.246172775435,-45.0866600721585,-177.213441914594));
#161195=CARTESIAN_POINT('Ctrl Pts',(52.2467714978885,-45.0845525658363,
-177.211438967526));
#161196=CARTESIAN_POINT('Ctrl Pts',(52.2473551700469,-45.0824915202267,
-177.209446651703));
#161197=CARTESIAN_POINT('Ctrl Pts',(52.2477174877031,-45.0812121149925,
-177.208209910855));
#161198=CARTESIAN_POINT('Ctrl Pts',(52.2479568632044,-45.0803718707492,
-177.20738941522));
#161199=CARTESIAN_POINT('Ctrl Pts',(52.2482914474766,-45.0791841923715,
-177.206219918861));
#161200=CARTESIAN_POINT('Ctrl Pts',(52.2484958585334,-45.0784585916408,
-177.20550542626));
#161201=CARTESIAN_POINT('Ctrl Pts',(52.2487358060927,-45.0776035977889,
-177.204660358975));
#161202=CARTESIAN_POINT('Ctrl Pts',(52.2490610356366,-45.0764466294067,
-177.203503390593));
#161203=CARTESIAN_POINT('Ctrl Pts',(52.2541090747794,-45.0584887845861,
-177.185545545773));
#161204=CARTESIAN_POINT('Ctrl Pts',(52.2586928180255,-45.0420748638293,
-177.166390617213));
#161205=CARTESIAN_POINT('Ctrl Pts',(52.2628122653748,-45.027308366338,-177.146327178728));
#161206=CARTESIAN_POINT('Ctrl Pts',(52.2669899506247,-45.0123331103072,
-177.125980097212));
#161207=CARTESIAN_POINT('Ctrl Pts',(52.2706901193928,-44.9990520483592,
-177.104699239602));
#161208=CARTESIAN_POINT('Ctrl Pts',(52.2739127716791,-44.9875196153263,
-177.082782754311));
#161209=CARTESIAN_POINT('Ctrl Pts',(52.2772061377067,-44.9757341293998,
-177.060385361824));
#161210=CARTESIAN_POINT('Ctrl Pts',(52.2800008013202,-44.9657746706807,
-177.037324735901));
#161211=CARTESIAN_POINT('Ctrl Pts',(52.2822967625197,-44.9576461996328,
-177.013906910146));
#161212=CARTESIAN_POINT('Ctrl Pts',(52.2846217509038,-44.9494149626367,
-176.990193019478));
#161213=CARTESIAN_POINT('Ctrl Pts',(52.2864353472564,-44.9430609412307,
-176.966113358338));
#161214=CARTESIAN_POINT('Ctrl Pts',(52.2877375515776,-44.9385396784594,
-176.941964850393));
#161215=CARTESIAN_POINT('Ctrl Pts',(52.2890642583169,-44.9339333431161,
-176.917361961496));
#161216=CARTESIAN_POINT('Ctrl Pts',(52.2898601471524,-44.9312289800572,
-176.892688085414));
#161217=CARTESIAN_POINT('Ctrl Pts',(52.2901252180841,-44.9303342185764,
-176.868228043869));
#161218=CARTESIAN_POINT('Ctrl Pts',(52.2901914014196,-44.9301108130943,
-176.862120821454));
#161219=CARTESIAN_POINT('Ctrl Pts',(52.2902244930873,-44.93000002,-176.856026770997));
#161220=CARTESIAN_POINT('Ctrl Pts',(52.2902244930873,-44.93000002,-176.84995));
#161221=CARTESIAN_POINT('Origin',(51.6222122422086,-38.4052093625928,-172.64995));
#161222=CARTESIAN_POINT('',(51.7950904587165,-44.36041346952,-172.64995));
#161223=CARTESIAN_POINT('Ctrl Pts',(50.7754831343094,-44.43000002,-171.64995));
#161224=CARTESIAN_POINT('Ctrl Pts',(50.8046140710912,-44.4280118806895,
-171.64995));
#161225=CARTESIAN_POINT('Ctrl Pts',(50.8325027036972,-44.4261255344678,
-171.651172745859));
#161226=CARTESIAN_POINT('Ctrl Pts',(50.859069989913,-44.4243298726759,-171.653316375858));
#161227=CARTESIAN_POINT('Ctrl Pts',(50.8868184408941,-44.4224543768949,
-171.655555310293));
#161228=CARTESIAN_POINT('Ctrl Pts',(50.9131258825754,-44.4206778703683,
-171.658798248564));
#161229=CARTESIAN_POINT('Ctrl Pts',(50.9379516616092,-44.4189946396407,
-171.662728774772));
#161230=CARTESIAN_POINT('Ctrl Pts',(50.9633985651933,-44.417269295595,-171.666757640143));
#161231=CARTESIAN_POINT('Ctrl Pts',(50.9872894292095,-44.4156420502453,
-171.671508529141));
#161232=CARTESIAN_POINT('Ctrl Pts',(51.0096221990147,-44.4141126148304,
-171.676676564296));
#161233=CARTESIAN_POINT('Ctrl Pts',(51.0326894620957,-44.4125328784436,
-171.682014568832));
#161234=CARTESIAN_POINT('Ctrl Pts',(51.0540951810777,-44.4110575929876,
-171.687797262872));
#161235=CARTESIAN_POINT('Ctrl Pts',(51.0738701191736,-44.40969108195,-171.693732405553));
#161236=CARTESIAN_POINT('Ctrl Pts',(51.0768409738807,-44.4094857864528,
-171.694624061774));
#161237=CARTESIAN_POINT('Ctrl Pts',(51.0797750688298,-44.4092829526126,
-171.69551924183));
#161238=CARTESIAN_POINT('Ctrl Pts',(51.0826725543606,-44.4090826015581,
-171.696417042979));
#161239=CARTESIAN_POINT('Ctrl Pts',(51.0954249653932,-44.4082008166554,
-171.700368444688));
#161240=CARTESIAN_POINT('Ctrl Pts',(51.1074680002581,-44.407367092164,-171.70436993824));
#161241=CARTESIAN_POINT('Ctrl Pts',(51.1188164928691,-44.4065835128548,
-171.708349867282));
#161242=CARTESIAN_POINT('Ctrl Pts',(51.1244907391747,-44.4061917232002,
-171.710339831803));
#161243=CARTESIAN_POINT('Ctrl Pts',(51.1299913124772,-44.4058124645793,
-171.712324508957));
#161244=CARTESIAN_POINT('Ctrl Pts',(51.1353203844627,-44.4054460422028,
-171.714295777063));
#161245=CARTESIAN_POINT('Ctrl Pts',(51.1379849204555,-44.4052628310145,
-171.715281411117));
#161246=CARTESIAN_POINT('Ctrl Pts',(51.1406065787668,-44.4050828285567,
-171.716263699775));
#161247=CARTESIAN_POINT('Ctrl Pts',(51.143185625721,-44.4049060722589,-171.717241672115));
#161248=CARTESIAN_POINT('Ctrl Pts',(51.1449546614015,-44.4047848304966,
-171.717912488892));
#161249=CARTESIAN_POINT('Ctrl Pts',(51.1457809331891,-44.4047277477496,
-171.718227889236));
#161250=CARTESIAN_POINT('Ctrl Pts',(51.1475638474567,-44.4046060349278,
-171.718913272981));
#161251=CARTESIAN_POINT('Ctrl Pts',(51.1483802134989,-44.404550304702,-171.719227098512));
#161252=CARTESIAN_POINT('Ctrl Pts',(51.1493970225313,-44.4044810069703,
-171.719618819405));
#161253=CARTESIAN_POINT('Ctrl Pts',(51.1507951962543,-44.4043855789116,
-171.720161698938));
#161254=CARTESIAN_POINT('Ctrl Pts',(51.1845048073339,-44.4020848328094,
-171.733250385712));
#161255=CARTESIAN_POINT('Ctrl Pts',(51.2167470072588,-44.3998963013987,
-171.747810336066));
#161256=CARTESIAN_POINT('Ctrl Pts',(51.2474534328981,-44.3978103768682,
-171.763538020509));
#161257=CARTESIAN_POINT('Ctrl Pts',(51.278964188969,-44.3956698132013,-171.779677679156));
#161258=CARTESIAN_POINT('Ctrl Pts',(51.3088579736835,-44.3936373462816,
-171.797046561303));
#161259=CARTESIAN_POINT('Ctrl Pts',(51.337111582541,-44.3917097149291,-171.815335003271));
#161260=CARTESIAN_POINT('Ctrl Pts',(51.3395010289291,-44.3915466925062,
-171.81688168185));
#161261=CARTESIAN_POINT('Ctrl Pts',(51.3418787717478,-44.3913844237635,
-171.818434950475));
#161262=CARTESIAN_POINT('Ctrl Pts',(51.3442448118475,-44.3912229088206,
-171.819994629286));
#161263=CARTESIAN_POINT('Ctrl Pts',(51.3730476143694,-44.3892567194037,
-171.838981256258));
#161264=CARTESIAN_POINT('Ctrl Pts',(51.4001125383987,-44.3874017274751,
-171.858915412102));
#161265=CARTESIAN_POINT('Ctrl Pts',(51.4254654811503,-44.3856615726511,
-171.879488097268));
#161266=CARTESIAN_POINT('Ctrl Pts',(51.4381419525261,-44.3847914952391,
-171.889774439851));
#161267=CARTESIAN_POINT('Ctrl Pts',(51.4503911131589,-44.3839502233142,
-171.900220871966));
#161268=CARTESIAN_POINT('Ctrl Pts',(51.4622199181929,-44.3831387343582,
-171.91079164189));
#161269=CARTESIAN_POINT('Ctrl Pts',(51.4677366951224,-44.3827602681024,
-171.915721690148));
#161270=CARTESIAN_POINT('Ctrl Pts',(51.472836767171,-44.3824082123661,-171.920381836519));
#161271=CARTESIAN_POINT('Ctrl Pts',(51.4779815600685,-44.3820555671411,
-171.925178375141));
#161272=CARTESIAN_POINT('Ctrl Pts',(51.4829853346238,-44.3817125878921,
-171.929843441042));
#161273=CARTESIAN_POINT('Ctrl Pts',(51.4880315628651,-44.3813690722246,
-171.934637611724));
#161274=CARTESIAN_POINT('Ctrl Pts',(51.4935119510881,-44.3809955693083,
-171.93996907612));
#161275=CARTESIAN_POINT('Ctrl Pts',(51.4944786714865,-44.3809296847627,
-171.940909526902));
#161276=CARTESIAN_POINT('Ctrl Pts',(51.4954588090377,-44.3808628542106,
-171.941866786846));
#161277=CARTESIAN_POINT('Ctrl Pts',(51.4964543875452,-44.3807948982762,
-171.942843218813));
#161278=CARTESIAN_POINT('Ctrl Pts',(51.527246566966,-44.378693093839,-171.97304321622));
#161279=CARTESIAN_POINT('Ctrl Pts',(51.5558098726652,-44.3767752596171,
-172.004935794556));
#161280=CARTESIAN_POINT('Ctrl Pts',(51.5820175750055,-44.3750235849214,
-172.038177891501));
#161281=CARTESIAN_POINT('Ctrl Pts',(51.608536381873,-44.3732511165704,-172.071814596365));
#161282=CARTESIAN_POINT('Ctrl Pts',(51.6326434300992,-44.3716487903803,
-172.106832536843));
#161283=CARTESIAN_POINT('Ctrl Pts',(51.6542606346252,-44.3702056322116,
-172.142877708409));
#161284=CARTESIAN_POINT('Ctrl Pts',(51.6761396036481,-44.3687449987228,
-172.179359353905));
#161285=CARTESIAN_POINT('Ctrl Pts',(51.695468239182,-44.3674474359092,-172.216892769522));
#161286=CARTESIAN_POINT('Ctrl Pts',(51.7122176676771,-44.3663088858582,
-172.255120022089));
#161287=CARTESIAN_POINT('Ctrl Pts',(51.7292787416113,-44.3651491515662,
-172.294058543635));
#161288=CARTESIAN_POINT('Ctrl Pts',(51.743663933231,-44.3641544300339,-172.333716479681));
#161289=CARTESIAN_POINT('Ctrl Pts',(51.7553936826929,-44.3633275939378,
-172.373732379002));
#161290=CARTESIAN_POINT('Ctrl Pts',(51.7672496456042,-44.3624918609906,
-172.414178853989));
#161291=CARTESIAN_POINT('Ctrl Pts',(51.7763930408945,-44.361827691907,-172.454990623027));
#161292=CARTESIAN_POINT('Ctrl Pts',(51.7828924549402,-44.3613447258736,
-172.495818301195));
#161293=CARTESIAN_POINT('Ctrl Pts',(51.7894949535036,-44.3608540997158,
-172.537293530278));
#161294=CARTESIAN_POINT('Ctrl Pts',(51.7933692868094,-44.3605505195348,
-172.578784792061));
#161295=CARTESIAN_POINT('Ctrl Pts',(51.7946309645435,-44.3604502191584,
-172.619956446103));
#161296=CARTESIAN_POINT('Ctrl Pts',(51.7949379634072,-44.3604258134796,
-172.629974575665));
#161297=CARTESIAN_POINT('Ctrl Pts',(51.7950904587166,-44.36041346952,-172.639973936947));
#161298=CARTESIAN_POINT('Ctrl Pts',(51.7950904587166,-44.36041346952,-172.64995));
#161299=CARTESIAN_POINT('',(51.9770573602378,-43.0656516879596,-172.64995));
#161300=CARTESIAN_POINT('',(51.7150402894768,-44.93000002,-172.64995));
#161301=CARTESIAN_POINT('Origin',(50.9867892914962,-42.9264785869994,-172.64995));
#161302=CARTESIAN_POINT('Ctrl Pts',(51.9770573602378,-43.0656516879596,
-172.64995));
#161303=CARTESIAN_POINT('Ctrl Pts',(51.9770573602378,-43.0656516879595,
-171.64995));
#161304=CARTESIAN_POINT('Ctrl Pts',(50.9867892914962,-42.9264785869994,
-171.64995));
#161305=CARTESIAN_POINT('Ctrl Pts',(52.0666747393887,-42.4279909017497,
-172.649949997757));
#161306=CARTESIAN_POINT('Ctrl Pts',(52.0557320324863,-42.5058523071511,
-171.757498535929));
#161307=CARTESIAN_POINT('Ctrl Pts',(51.1823572933545,-42.3510730842576,
-171.64995));
#161308=CARTESIAN_POINT('Ctrl Pts',(52.1554800333146,-41.7961084021622,
-172.606056153133));
#161309=CARTESIAN_POINT('Ctrl Pts',(52.1416679592955,-41.8943864154851,
-171.81403941883));
#161310=CARTESIAN_POINT('Ctrl Pts',(51.3741578990751,-41.7754043578546,
-171.628003076365));
#161311=CARTESIAN_POINT('Ctrl Pts',(52.3315472405273,-40.5433251268562,
-172.43788181511));
#161312=CARTESIAN_POINT('Ctrl Pts',(52.3125022740342,-40.6788371047634,
-171.821280489149));
#161313=CARTESIAN_POINT('Ctrl Pts',(51.7497860966445,-40.6237611991777,
-171.543915907757));
#161314=CARTESIAN_POINT('Ctrl Pts',(52.4188787332529,-39.9219292677054,
-172.315208572937));
#161315=CARTESIAN_POINT('Ctrl Pts',(52.3988291636532,-40.0645893682337,
-171.781794156641));
#161316=CARTESIAN_POINT('Ctrl Pts',(51.9336694513069,-40.0475756797307,
-171.482621144039));
#161317=CARTESIAN_POINT('Ctrl Pts',(52.5050296388285,-39.3089337226171,
-172.133326251627));
#161318=CARTESIAN_POINT('Ctrl Pts',(52.4864722882118,-39.4409761333229,
-171.679515584751));
#161319=CARTESIAN_POINT('Ctrl Pts',(52.1126146143194,-39.473850183348,-171.391638125813));
#161320=CARTESIAN_POINT('',(52.5050296388285,-39.3089337226171,-172.133326251627));
#161321=CARTESIAN_POINT('Ctrl Pts',(52.5050296388285,-39.3089337226171,
-172.133326251627));
#161322=CARTESIAN_POINT('Ctrl Pts',(52.4540911811658,-39.6713796819752,
-172.240867836497));
#161323=CARTESIAN_POINT('Ctrl Pts',(52.4027597205579,-40.0366220025906,
-172.327673864957));
#161324=CARTESIAN_POINT('Ctrl Pts',(52.3511170282711,-40.4040788516705,
-172.398058085082));
#161325=CARTESIAN_POINT('Ctrl Pts',(52.3153892921751,-40.6582949033369,
-172.446751689745));
#161326=CARTESIAN_POINT('Ctrl Pts',(52.2795125603003,-40.9135711150572,
-172.487583846606));
#161327=CARTESIAN_POINT('Ctrl Pts',(52.2435136369167,-41.1697167645394,
-172.521968983892));
#161328=CARTESIAN_POINT('Ctrl Pts',(52.1712955694614,-41.6835750151203,
-172.590949606937));
#161329=CARTESIAN_POINT('Ctrl Pts',(52.0985648108855,-42.2010812525765,
-172.632879273599));
#161330=CARTESIAN_POINT('Ctrl Pts',(52.0252827479162,-42.7225102246227,
-172.645720761145));
#161331=CARTESIAN_POINT('Ctrl Pts',(52.0092341999946,-42.8367015765921,
-172.648533007689));
#161332=CARTESIAN_POINT('Ctrl Pts',(51.9931592080447,-42.9510810876001,
-172.649949999597));
#161333=CARTESIAN_POINT('Ctrl Pts',(51.9770573602378,-43.0656516879596,
-172.64995));
#161334=CARTESIAN_POINT('Origin',(51.5147615700869,-39.1697606216571,-172.133326251627));
#161335=CARTESIAN_POINT('Origin',(51.6222122422086,-38.4052093625928,-172.64995));
#161336=CARTESIAN_POINT('',(50.2983305691361,-55.0104134695199,-172.64995));
#161337=CARTESIAN_POINT('',(49.9349347781878,-57.596108877675,-172.64995));
#161338=CARTESIAN_POINT('',(49.2787232447289,-55.08000002,-171.64995));
#161339=CARTESIAN_POINT('Ctrl Pts',(50.2983305691361,-55.0104134695199,
-172.64995));
#161340=CARTESIAN_POINT('Ctrl Pts',(50.2983305691361,-55.0104134695199,
-172.605172304705));
#161341=CARTESIAN_POINT('Ctrl Pts',(50.2952256853384,-55.0106253728164,
-172.559925284473));
#161342=CARTESIAN_POINT('Ctrl Pts',(50.2889016465528,-55.0110569782332,
-172.514629908981));
#161343=CARTESIAN_POINT('Ctrl Pts',(50.2826524098944,-55.0114834785258,
-172.469870297193));
#161344=CARTESIAN_POINT('Ctrl Pts',(50.2732597042546,-55.0121245154913,
-172.425063433793));
#161345=CARTESIAN_POINT('Ctrl Pts',(50.260621229954,-55.0129870709171,-172.380665523989));
#161346=CARTESIAN_POINT('Ctrl Pts',(50.2507110648879,-55.0136634236512,
-172.34585193777));
#161347=CARTESIAN_POINT('Ctrl Pts',(50.2388053749292,-55.0144759677311,
-172.311290758928));
#161348=CARTESIAN_POINT('Ctrl Pts',(50.2248584410366,-55.0154278234074,
-172.277224099798));
#161349=CARTESIAN_POINT('Ctrl Pts',(50.2234976012156,-55.0155206985238,
-172.273900124315));
#161350=CARTESIAN_POINT('Ctrl Pts',(50.2221173289147,-55.0156148998755,
-172.270580868756));
#161351=CARTESIAN_POINT('Ctrl Pts',(50.2207175829473,-55.0157104302734,
-172.267266567635));
#161352=CARTESIAN_POINT('Ctrl Pts',(50.2026895854313,-55.0169408119401,
-172.224580098969));
#161353=CARTESIAN_POINT('Ctrl Pts',(50.1814340508794,-55.0183914677883,
-172.182726614308));
#161354=CARTESIAN_POINT('Ctrl Pts',(50.1570394248576,-55.0200563615513,
-172.142169045314));
#161355=CARTESIAN_POINT('Ctrl Pts',(50.1336253811801,-55.0216543321555,
-172.103241754893));
#161356=CARTESIAN_POINT('Ctrl Pts',(50.1073206492679,-55.0234495875555,
-172.065509332316));
#161357=CARTESIAN_POINT('Ctrl Pts',(50.0782208862319,-55.0254355993083,
-172.029413465929));
#161358=CARTESIAN_POINT('Ctrl Pts',(50.0647174562256,-55.0263571865618,
-172.012663569901));
#161359=CARTESIAN_POINT('Ctrl Pts',(50.0506123834973,-55.0273198349579,
-171.996266629338));
#161360=CARTESIAN_POINT('Ctrl Pts',(50.0359174318355,-55.0283227416369,
-171.980270642));
#161361=CARTESIAN_POINT('Ctrl Pts',(50.0306737152842,-55.0286806168088,
-171.974562666534));
#161362=CARTESIAN_POINT('Ctrl Pts',(50.0250757653012,-55.0290626678437,
-171.968608245928));
#161363=CARTESIAN_POINT('Ctrl Pts',(50.0194929266255,-55.0294436801627,
-171.962815606048));
#161364=CARTESIAN_POINT('Ctrl Pts',(50.0137424541554,-55.0298361329952,
-171.956849032751));
#161365=CARTESIAN_POINT('Ctrl Pts',(50.008008174688,-55.0302274728359,-171.951054248133));
#161366=CARTESIAN_POINT('Ctrl Pts',(50.002735256722,-55.0305873095219,-171.945838282879));
#161367=CARTESIAN_POINT('Ctrl Pts',(50.0017027010506,-55.0306577736204,
-171.944816879826));
#161368=CARTESIAN_POINT('Ctrl Pts',(50.0006879511706,-55.0307270218896,
-171.943817557218));
#161369=CARTESIAN_POINT('Ctrl Pts',(49.9996945037156,-55.0307948156288,
-171.942843213006));
#161370=CARTESIAN_POINT('Ctrl Pts',(49.9775385427164,-55.0323067581414,
-171.921113294381));
#161371=CARTESIAN_POINT('Ctrl Pts',(49.9536976238303,-55.0339338834397,
-171.899758993455));
#161372=CARTESIAN_POINT('Ctrl Pts',(49.9281170980912,-55.0356797757925,
-171.879051282674));
#161373=CARTESIAN_POINT('Ctrl Pts',(49.9029338030088,-55.0373985568197,
-171.858665134382));
#161374=CARTESIAN_POINT('Ctrl Pts',(49.8760642222839,-55.0392324645958,
-171.838905512263));
#161375=CARTESIAN_POINT('Ctrl Pts',(49.8474888776852,-55.0411826856386,
-171.820067900575));
#161376=CARTESIAN_POINT('Ctrl Pts',(49.8203035381361,-55.0430380410853,
-171.802146616433));
#161377=CARTESIAN_POINT('Ctrl Pts',(49.7915729570549,-55.0449988567668,
-171.785058883054));
#161378=CARTESIAN_POINT('Ctrl Pts',(49.7613085510039,-55.0470643535212,
-171.769091901678));
#161379=CARTESIAN_POINT('Ctrl Pts',(49.731938617721,-55.0490688039563,-171.753596828788));
#161380=CARTESIAN_POINT('Ctrl Pts',(49.7011235740018,-55.0511718808408,
-171.739157140893));
#161381=CARTESIAN_POINT('Ctrl Pts',(49.6689100752976,-55.0533704000159,
-171.726070467489));
#161382=CARTESIAN_POINT('Ctrl Pts',(49.6683799863872,-55.0534065777265,
-171.725855119864));
#161383=CARTESIAN_POINT('Ctrl Pts',(49.6678495213746,-55.0534427811054,
-171.725640139907));
#161384=CARTESIAN_POINT('Ctrl Pts',(49.6673186805243,-55.0534790101347,
-171.725425528679));
#161385=CARTESIAN_POINT('Ctrl Pts',(49.6646555879062,-55.0536607618979,
-171.724348879102));
#161386=CARTESIAN_POINT('Ctrl Pts',(49.6612679260877,-55.0538919407015,
-171.722996951244));
#161387=CARTESIAN_POINT('Ctrl Pts',(49.6584523482381,-55.0540840712475,
-171.721889199757));
#161388=CARTESIAN_POINT('Ctrl Pts',(49.6566137537786,-55.0542095340037,
-171.721165829331));
#161389=CARTESIAN_POINT('Ctrl Pts',(49.6550196708291,-55.0543183073482,
-171.720545222463));
#161390=CARTESIAN_POINT('Ctrl Pts',(49.6540347939841,-55.0543855068274,
-171.720163007342));
#161391=CARTESIAN_POINT('Ctrl Pts',(49.6382987468942,-55.0554591986035,
-171.714056096449));
#161392=CARTESIAN_POINT('Ctrl Pts',(49.620874316751,-55.0566482285285,-171.707738814429));
#161393=CARTESIAN_POINT('Ctrl Pts',(49.6016963861777,-55.0579570088307,
-171.701466818893));
#161394=CARTESIAN_POINT('Ctrl Pts',(49.5821836919874,-55.0592886347693,
-171.695085341476));
#161395=CARTESIAN_POINT('Ctrl Pts',(49.5608547090479,-55.0607442990113,
-171.68875040177));
#161396=CARTESIAN_POINT('Ctrl Pts',(49.5376610747394,-55.0623272682998,
-171.682785652347));
#161397=CARTESIAN_POINT('Ctrl Pts',(49.5167527758563,-55.0637542630763,
-171.677408626822));
#161398=CARTESIAN_POINT('Ctrl Pts',(49.4943288267278,-55.0652847355981,
-171.672333011424));
#161399=CARTESIAN_POINT('Ctrl Pts',(49.4703789307845,-55.0669193633298,
-171.667836203527));
#161400=CARTESIAN_POINT('Ctrl Pts',(49.4472084654267,-55.0685007933835,
-171.663485740716));
#161401=CARTESIAN_POINT('Ctrl Pts',(49.4226092365823,-55.0701797452918,
-171.659677091764));
#161402=CARTESIAN_POINT('Ctrl Pts',(49.3966032219418,-55.0719546957534,
-171.656697423783));
#161403=CARTESIAN_POINT('Ctrl Pts',(49.3718021780105,-55.0736474051124,
-171.653855816658));
#161404=CARTESIAN_POINT('Ctrl Pts',(49.3457213525921,-55.0754274463003,
-171.651768285729));
#161405=CARTESIAN_POINT('Ctrl Pts',(49.3184147391538,-55.0772911135977,
-171.650715593428));
#161406=CARTESIAN_POINT('Ctrl Pts',(49.3054566987733,-55.0781754955497,
-171.650216050364));
#161407=CARTESIAN_POINT('Ctrl Pts',(49.2922231788487,-55.0790786713351,
-171.64995));
#161408=CARTESIAN_POINT('Ctrl Pts',(49.2787232447289,-55.08000002,-171.64995));
#161409=CARTESIAN_POINT('',(49.3685531658572,-54.4408269190399,-171.64995));
#161410=CARTESIAN_POINT('Ctrl Pts',(50.7934646035069,-54.58000002,-176.84995));
#161411=CARTESIAN_POINT('Ctrl Pts',(50.3588212345988,-54.58000002,-176.84995));
#161412=CARTESIAN_POINT('Ctrl Pts',(50.2983305691361,-55.0104134695199,
-176.84995));
#161413=CARTESIAN_POINT('Ctrl Pts',(50.7934646035178,-54.58000002,-176.981217345763));
#161414=CARTESIAN_POINT('Ctrl Pts',(50.358821234607,-54.5800000199424,-176.997671841189));
#161415=CARTESIAN_POINT('Ctrl Pts',(50.2983305691453,-55.0104134694541,
-177.112484691526));
#161416=CARTESIAN_POINT('Ctrl Pts',(50.8086111287259,-54.5261134565302,
-177.110943344657));
#161417=CARTESIAN_POINT('Ctrl Pts',(50.3685899331079,-54.5104921183889,
-177.142957948483));
#161418=CARTESIAN_POINT('Ctrl Pts',(50.313477094355,-54.9026403425777,-177.371936689315));
#161419=CARTESIAN_POINT('Ctrl Pts',(50.8606449931892,-54.3409933646562,
-177.296063436531));
#161420=CARTESIAN_POINT('Ctrl Pts',(50.3994818369767,-54.2906848009584,
-177.329589659683));
#161421=CARTESIAN_POINT('Ctrl Pts',(50.3655109588186,-54.5324001588352,
-177.742176873059));
#161422=CARTESIAN_POINT('Ctrl Pts',(50.8971085935234,-54.2112673657634,
-177.34995));
#161423=CARTESIAN_POINT('Ctrl Pts',(50.420433990624,-54.1416024812641,-177.367861075731));
#161424=CARTESIAN_POINT('Ctrl Pts',(50.4019745591532,-54.2729481610447,
-177.849949999941));
#161425=CARTESIAN_POINT('Ctrl Pts',(50.9340054382093,-54.08000002,-177.34995));
#161426=CARTESIAN_POINT('Ctrl Pts',(50.4388714038384,-54.0104134695199,
-177.34995));
#161427=CARTESIAN_POINT('Ctrl Pts',(50.4388714038385,-54.0104134695199,
-177.84995));
#161428=CARTESIAN_POINT('',(50.7934646035069,-54.58000002,-176.84995));
#161429=CARTESIAN_POINT('',(50.2983305691361,-55.0104134695199,-176.84995));
#161430=CARTESIAN_POINT('Origin',(50.7934646035069,-55.08000002,-176.84995));
#161431=CARTESIAN_POINT('',(50.4388714038385,-54.0104134695199,-177.84995));
#161432=CARTESIAN_POINT('Ctrl Pts',(50.4388714038385,-54.0104134695199,
-177.84995));
#161433=CARTESIAN_POINT('Ctrl Pts',(50.4019745591532,-54.2729481610447,
-177.849949999941));
#161434=CARTESIAN_POINT('Ctrl Pts',(50.3655109588186,-54.5324001588352,
-177.742176873059));
#161435=CARTESIAN_POINT('Ctrl Pts',(50.3394940265868,-54.7175202507064,
-177.557056781187));
#161436=CARTESIAN_POINT('Ctrl Pts',(50.313477094355,-54.9026403425777,-177.371936689315));
#161437=CARTESIAN_POINT('Ctrl Pts',(50.2983305691453,-55.0104134694541,
-177.112484691526));
#161438=CARTESIAN_POINT('Ctrl Pts',(50.2983305691361,-55.0104134695199,
-176.84995));
#161439=CARTESIAN_POINT('Origin',(50.9340054382093,-54.0800000199999,-177.84995));
#161440=CARTESIAN_POINT('Ctrl Pts',(50.7934646035069,-54.58000002,-176.84995));
#161441=CARTESIAN_POINT('Ctrl Pts',(50.7934646035069,-54.58000002,-176.875800002307));
#161442=CARTESIAN_POINT('Ctrl Pts',(50.7940526302635,-54.5779080061136,
-176.901947474016));
#161443=CARTESIAN_POINT('Ctrl Pts',(50.79524037118,-54.5736823982397,-176.928073316629));
#161444=CARTESIAN_POINT('Ctrl Pts',(50.7964380905779,-54.5694212900735,
-176.954418648383));
#161445=CARTESIAN_POINT('Ctrl Pts',(50.7982456556932,-54.5629905430313,
-176.980741922991));
#161446=CARTESIAN_POINT('Ctrl Pts',(50.8006670611674,-54.5543759454336,
-177.00667179537));
#161447=CARTESIAN_POINT('Ctrl Pts',(50.8015905093901,-54.5510906076722,
-177.016560636713));
#161448=CARTESIAN_POINT('Ctrl Pts',(50.8026031526618,-54.5474879420343,
-177.026391811967));
#161449=CARTESIAN_POINT('Ctrl Pts',(50.8037049055093,-54.5435682526075,
-177.036143091591));
#161450=CARTESIAN_POINT('Ctrl Pts',(50.8065619552914,-54.5334037698481,
-177.06142997094));
#161451=CARTESIAN_POINT('Ctrl Pts',(50.810020166567,-54.5211005439435,-177.086198360269));
#161452=CARTESIAN_POINT('Ctrl Pts',(50.8140793605825,-54.506659210843,-177.110048753582));
#161453=CARTESIAN_POINT('Ctrl Pts',(50.8173767403582,-54.4949281727313,
-177.129422994933));
#161454=CARTESIAN_POINT('Ctrl Pts',(50.8210711306239,-54.4817846964092,
-177.148192204817));
#161455=CARTESIAN_POINT('Ctrl Pts',(50.825157442334,-54.4672468870987,-177.166105768384));
#161456=CARTESIAN_POINT('Ctrl Pts',(50.827356904925,-54.4594218923349,-177.175747767266));
#161457=CARTESIAN_POINT('Ctrl Pts',(50.8296698422141,-54.4511931903559,
-177.18514138209));
#161458=CARTESIAN_POINT('Ctrl Pts',(50.8320942102929,-54.4425680527437,
-177.194242926223));
#161459=CARTESIAN_POINT('Ctrl Pts',(50.8325766062305,-54.4408518400193,
-177.19605393337));
#161460=CARTESIAN_POINT('Ctrl Pts',(50.8331640063325,-54.4387620555821,
-177.198223909681));
#161461=CARTESIAN_POINT('Ctrl Pts',(50.8336822024932,-54.436918446991,-177.200104635539));
#161462=CARTESIAN_POINT('Ctrl Pts',(50.834057272349,-54.4355840449617,-177.201465903008));
#161463=CARTESIAN_POINT('Ctrl Pts',(50.8343957120667,-54.4343799457124,
-177.202676855488));
#161464=CARTESIAN_POINT('Ctrl Pts',(50.8346280186497,-54.4335534076203,
-177.203503393566));
#161465=CARTESIAN_POINT('Ctrl Pts',(50.8373709918346,-54.4237940121101,
-177.213262788913));
#161466=CARTESIAN_POINT('Ctrl Pts',(50.8404332490898,-54.4128991858337,
-177.22331664328));
#161467=CARTESIAN_POINT('Ctrl Pts',(50.8438503785376,-54.4007420960308,
-177.233428698371));
#161468=CARTESIAN_POINT('Ctrl Pts',(50.8471205406303,-54.3891078706266,
-177.243105843982));
#161469=CARTESIAN_POINT('Ctrl Pts',(50.8507159048646,-54.3763169166589,
-177.252836300725));
#161470=CARTESIAN_POINT('Ctrl Pts',(50.8546612358606,-54.3622809307141,
-177.262372868916));
#161471=CARTESIAN_POINT('Ctrl Pts',(50.8583802330195,-54.349050154411,-177.271362347884));
#161472=CARTESIAN_POINT('Ctrl Pts',(50.8624103177822,-54.3347126616006,
-177.280179445045));
#161473=CARTESIAN_POINT('Ctrl Pts',(50.8667641905032,-54.3192230962442,
-177.288581471767));
#161474=CARTESIAN_POINT('Ctrl Pts',(50.8685409822056,-54.3129018891342,
-177.29201029303));
#161475=CARTESIAN_POINT('Ctrl Pts',(50.8703715911811,-54.3063891942303,
-177.295369566868));
#161476=CARTESIAN_POINT('Ctrl Pts',(50.8722563916222,-54.2996836682345,
-177.298640995834));
#161477=CARTESIAN_POINT('Ctrl Pts',(50.8765268222964,-54.2844908216743,
-177.306053138943));
#161478=CARTESIAN_POINT('Ctrl Pts',(50.8810786182863,-54.2682969659899,
-177.313020714078));
#161479=CARTESIAN_POINT('Ctrl Pts',(50.8859100008748,-54.2511084292962,
-177.319306663922));
#161480=CARTESIAN_POINT('Ctrl Pts',(50.8906033966449,-54.2344108062172,
-177.325413083744));
#161481=CARTESIAN_POINT('Ctrl Pts',(50.8955607238668,-54.2167741982081,
-177.330876292405));
#161482=CARTESIAN_POINT('Ctrl Pts',(50.9007703992126,-54.1982398150987,
-177.335449266095));
#161483=CARTESIAN_POINT('Ctrl Pts',(50.9058588558212,-54.1801366900557,
-177.339915835823));
#161484=CARTESIAN_POINT('Ctrl Pts',(50.9111881361125,-54.1611767902422,
-177.343533167656));
#161485=CARTESIAN_POINT('Ctrl Pts',(50.9167365713841,-54.1414372060732,
-177.34604166628));
#161486=CARTESIAN_POINT('Ctrl Pts',(50.9222850066558,-54.1216976219043,
-177.348550164905));
#161487=CARTESIAN_POINT('Ctrl Pts',(50.9280527228745,-54.1011779052295,
-177.34995));
#161488=CARTESIAN_POINT('Ctrl Pts',(50.9340054382093,-54.08000002,-177.34995));
#161489=CARTESIAN_POINT('Origin',(53.1076143453209,-38.6139690140329,-177.84995));
#161490=CARTESIAN_POINT('',(50.5091418211897,-53.5104134695199,-177.84995));
#161491=CARTESIAN_POINT('',(52.6124803109501,-38.5443824635529,-177.84995));
#161492=CARTESIAN_POINT('Origin',(51.0042758555605,-53.58000002,-177.84995));
#161493=CARTESIAN_POINT('Ctrl Pts',(51.0043131058742,-53.5800399704537,
-177.349950000614));
#161494=CARTESIAN_POINT('Ctrl Pts',(50.5091370017856,-53.5104477613619,
-177.349907583593));
#161495=CARTESIAN_POINT('Ctrl Pts',(50.5091324341781,-53.5104802615782,
-177.849949997675));
#161496=CARTESIAN_POINT('Ctrl Pts',(51.0412139300136,-53.4487616698901,
-177.349960874823));
#161497=CARTESIAN_POINT('Ctrl Pts',(50.5284341404524,-53.3731414851579,
-177.331166751555));
#161498=CARTESIAN_POINT('Ctrl Pts',(50.5460324812801,-53.247922783674,-177.849968278574));
#161499=CARTESIAN_POINT('Ctrl Pts',(51.0776824759844,-53.3190198513573,
-177.296074808575));
#161500=CARTESIAN_POINT('Ctrl Pts',(50.5442915570248,-53.2603101034141,
-177.25721607327));
#161501=CARTESIAN_POINT('Ctrl Pts',(50.582500059869,-52.9884424791336,-177.742192571987));
#161502=CARTESIAN_POINT('Ctrl Pts',(51.1297221567416,-53.1338805435418,
-177.110939115584));
#161503=CARTESIAN_POINT('Ctrl Pts',(50.5649415669174,-53.1133776482461,
-177.069853325703));
#161504=CARTESIAN_POINT('Ctrl Pts',(50.6345383370137,-52.6181708975332,
-177.371920990387));
#161505=CARTESIAN_POINT('Ctrl Pts',(51.1448695169889,-53.0799908778568,
-176.981197291836));
#161506=CARTESIAN_POINT('Ctrl Pts',(50.5696251595464,-53.0800521550443,
-176.95888267251));
#161507=CARTESIAN_POINT('Ctrl Pts',(50.6496852247771,-52.5103951909531,
-177.112440685846));
#161508=CARTESIAN_POINT('Ctrl Pts',(51.144866956159,-53.080000018636,-176.849916603474));
#161509=CARTESIAN_POINT('Ctrl Pts',(50.5696243593531,-53.0800578487393,
-176.849922286134));
#161510=CARTESIAN_POINT('Ctrl Pts',(50.6496826555653,-52.5104134718451,
-176.849883207942));
#161511=CARTESIAN_POINT('',(50.6496826558921,-52.51041346952,-176.84995));
#161512=CARTESIAN_POINT('Ctrl Pts',(50.6496826558921,-52.51041346952,-176.84995));
#161513=CARTESIAN_POINT('Ctrl Pts',(50.6496826558828,-52.5104134695858,
-177.112484691526));
#161514=CARTESIAN_POINT('Ctrl Pts',(50.6345361306733,-52.6181865964613,
-177.371936689314));
#161515=CARTESIAN_POINT('Ctrl Pts',(50.6085191984413,-52.8033066883334,
-177.557056781187));
#161516=CARTESIAN_POINT('Ctrl Pts',(50.5825022662094,-52.9884267802056,
-177.742176873059));
#161517=CARTESIAN_POINT('Ctrl Pts',(50.546038665875,-53.2478787779945,-177.849949999941));
#161518=CARTESIAN_POINT('Ctrl Pts',(50.5091418211897,-53.5104134695199,
-177.84995));
#161519=CARTESIAN_POINT('',(51.1448166902628,-53.08000002,-176.84995));
#161520=CARTESIAN_POINT('Origin',(51.1448166902628,-52.58000002,-176.84995));
#161521=CARTESIAN_POINT('Ctrl Pts',(51.0042758555605,-53.58000002,-177.34995));
#161522=CARTESIAN_POINT('Ctrl Pts',(51.0103430173925,-53.5584149702,-177.34995));
#161523=CARTESIAN_POINT('Ctrl Pts',(51.016169374502,-53.5374879725988,-177.348552025671));
#161524=CARTESIAN_POINT('Ctrl Pts',(51.021754926889,-53.517368300209,-177.346011757925));
#161525=CARTESIAN_POINT('Ctrl Pts',(51.0273316159915,-53.4972805541836,
-177.343475521136));
#161526=CARTESIAN_POINT('Ctrl Pts',(51.0326682639943,-53.4779969954851,
-177.339801327605));
#161527=CARTESIAN_POINT('Ctrl Pts',(51.0377648708973,-53.459608680057,-177.335239527258));
#161528=CARTESIAN_POINT('Ctrl Pts',(51.0430846624452,-53.4404151250393,
-177.33047796189));
#161529=CARTESIAN_POINT('Ctrl Pts',(51.048142929384,-53.4221966220856,-177.324750042966));
#161530=CARTESIAN_POINT('Ctrl Pts',(51.0529396717135,-53.4050003525822,
-177.318324974143));
#161531=CARTESIAN_POINT('Ctrl Pts',(51.0573558439112,-53.3891684228957,
-177.31240966572));
#161532=CARTESIAN_POINT('Ctrl Pts',(51.0615503436285,-53.3742018844323,
-177.305903491103));
#161533=CARTESIAN_POINT('Ctrl Pts',(51.0655231708653,-53.3601026376805,
-177.298999152375));
#161534=CARTESIAN_POINT('Ctrl Pts',(51.070152181175,-53.3436746495795,-177.290954439316));
#161535=CARTESIAN_POINT('Ctrl Pts',(51.0744802453861,-53.3284243291718,
-177.282370206816));
#161536=CARTESIAN_POINT('Ctrl Pts',(51.0785073634984,-53.31431086582,-177.273517318559));
#161537=CARTESIAN_POINT('Ctrl Pts',(51.0816848890195,-53.3031748899829,
-177.266532105414));
#161538=CARTESIAN_POINT('Ctrl Pts',(51.0846750540229,-53.2927456090393,
-177.259378907547));
#161539=CARTESIAN_POINT('Ctrl Pts',(51.0874778585085,-53.28298799345,-177.252173639391));
#161540=CARTESIAN_POINT('Ctrl Pts',(51.0906553636708,-53.2719259040087,
-177.244005115015));
#161541=CARTESIAN_POINT('Ctrl Pts',(51.0935920641105,-53.261726951001,-177.235770093483));
#161542=CARTESIAN_POINT('Ctrl Pts',(51.0962879598278,-53.2523265017848,
-177.227613958382));
#161543=CARTESIAN_POINT('Ctrl Pts',(51.0976359076864,-53.2476262771767,
-177.223535890831));
#161544=CARTESIAN_POINT('Ctrl Pts',(51.0989236543645,-53.2431254933336,
-177.219477157756));
#161545=CARTESIAN_POINT('Ctrl Pts',(51.1001511998619,-53.2388152125502,
-177.215453662315));
#161546=CARTESIAN_POINT('Ctrl Pts',(51.1007649726106,-53.2366600721585,
-177.213441914594));
#161547=CARTESIAN_POINT('Ctrl Pts',(51.1013636950641,-53.2345525658363,
-177.211438967526));
#161548=CARTESIAN_POINT('Ctrl Pts',(51.1019473672225,-53.2324915202267,
-177.209446651703));
#161549=CARTESIAN_POINT('Ctrl Pts',(51.1023096848787,-53.2312121149924,
-177.208209910855));
#161550=CARTESIAN_POINT('Ctrl Pts',(51.10254906038,-53.2303718707492,-177.20738941522));
#161551=CARTESIAN_POINT('Ctrl Pts',(51.1028836446522,-53.2291841923715,
-177.206219918861));
#161552=CARTESIAN_POINT('Ctrl Pts',(51.103088055709,-53.2284585916408,-177.20550542626));
#161553=CARTESIAN_POINT('Ctrl Pts',(51.1033280032683,-53.227603597789,-177.204660358976));
#161554=CARTESIAN_POINT('Ctrl Pts',(51.1036532328122,-53.2264466294068,
-177.203503390593));
#161555=CARTESIAN_POINT('Ctrl Pts',(51.108701271955,-53.2084887845862,-177.185545545773));
#161556=CARTESIAN_POINT('Ctrl Pts',(51.1132850152011,-53.1920748638293,
-177.166390617213));
#161557=CARTESIAN_POINT('Ctrl Pts',(51.1174044625504,-53.177308366338,-177.146327178728));
#161558=CARTESIAN_POINT('Ctrl Pts',(51.1215821478003,-53.1623331103072,
-177.125980097212));
#161559=CARTESIAN_POINT('Ctrl Pts',(51.1252823165684,-53.1490520483592,
-177.104699239602));
#161560=CARTESIAN_POINT('Ctrl Pts',(51.1285049688547,-53.1375196153263,
-177.08278275431));
#161561=CARTESIAN_POINT('Ctrl Pts',(51.1317983348823,-53.1257341293998,
-177.060385361824));
#161562=CARTESIAN_POINT('Ctrl Pts',(51.1345929984958,-53.1157746706807,
-177.037324735901));
#161563=CARTESIAN_POINT('Ctrl Pts',(51.1368889596953,-53.1076461996327,
-177.013906910145));
#161564=CARTESIAN_POINT('Ctrl Pts',(51.1392139480793,-53.0994149626366,
-176.990193019477));
#161565=CARTESIAN_POINT('Ctrl Pts',(51.1410275444319,-53.0930609412306,
-176.966113358338));
#161566=CARTESIAN_POINT('Ctrl Pts',(51.1423297487532,-53.0885396784593,
-176.941964850392));
#161567=CARTESIAN_POINT('Ctrl Pts',(51.1436564554925,-53.0839333431161,
-176.917361961496));
#161568=CARTESIAN_POINT('Ctrl Pts',(51.144452344328,-53.0812289800571,-176.892688085413));
#161569=CARTESIAN_POINT('Ctrl Pts',(51.1447174152596,-53.0803342185763,
-176.868228043868));
#161570=CARTESIAN_POINT('Ctrl Pts',(51.1447835985951,-53.0801108130943,
-176.862120821453));
#161571=CARTESIAN_POINT('Ctrl Pts',(51.1448166902628,-53.08000002,-176.856026770997));
#161572=CARTESIAN_POINT('Ctrl Pts',(51.1448166902628,-53.08000002,-176.84995));
#161573=CARTESIAN_POINT('Origin',(51.6222122422086,-38.4052093625928,-172.64995));
#161574=CARTESIAN_POINT('',(51.4437383719606,-46.86041346952,-172.64995));
#161575=CARTESIAN_POINT('',(50.6496826558921,-52.51041346952,-172.64995));
#161576=CARTESIAN_POINT('',(50.5696324866523,-53.08000002,-172.64995));
#161577=CARTESIAN_POINT('Ctrl Pts',(51.4437383719606,-46.86041346952,-172.64995));
#161578=CARTESIAN_POINT('Ctrl Pts',(51.4437383719606,-46.86041346952,-172.605172304724));
#161579=CARTESIAN_POINT('Ctrl Pts',(51.4406334881656,-46.8606253728163,
-172.559925284512));
#161580=CARTESIAN_POINT('Ctrl Pts',(51.4343094493851,-46.8610569782327,
-172.514629909038));
#161581=CARTESIAN_POINT('Ctrl Pts',(51.428060212732,-46.861483478525,-172.469870297268));
#161582=CARTESIAN_POINT('Ctrl Pts',(51.4186675071001,-46.8621245154899,
-172.425063433886));
#161583=CARTESIAN_POINT('Ctrl Pts',(51.4060290328097,-46.862987070915,-172.380665524099));
#161584=CARTESIAN_POINT('Ctrl Pts',(51.396118867739,-46.8636634236495,-172.345851937849));
#161585=CARTESIAN_POINT('Ctrl Pts',(51.384213177772,-46.86447596773,-172.311290758975));
#161586=CARTESIAN_POINT('Ctrl Pts',(51.3702662438672,-46.8654278234071,
-172.277224099813));
#161587=CARTESIAN_POINT('Ctrl Pts',(51.3689054040442,-46.8655206985236,
-172.273900124325));
#161588=CARTESIAN_POINT('Ctrl Pts',(51.3675251317413,-46.8656148998754,
-172.270580868761));
#161589=CARTESIAN_POINT('Ctrl Pts',(51.3661253857718,-46.8657104302735,
-172.267266567635));
#161590=CARTESIAN_POINT('Ctrl Pts',(51.3480973882623,-46.8669408119397,
-172.224580098984));
#161591=CARTESIAN_POINT('Ctrl Pts',(51.3268418537189,-46.8683914677873,
-172.182726614337));
#161592=CARTESIAN_POINT('Ctrl Pts',(51.3024472277073,-46.8700563615496,
-172.142169045356));
#161593=CARTESIAN_POINT('Ctrl Pts',(51.2790331840628,-46.8716543321515,
-172.103241754985));
#161594=CARTESIAN_POINT('Ctrl Pts',(51.2527284521908,-46.8734495875488,
-172.065509332455));
#161595=CARTESIAN_POINT('Ctrl Pts',(51.2236286892016,-46.8754355992983,
-172.029413466109));
#161596=CARTESIAN_POINT('Ctrl Pts',(51.2101252591521,-46.8763571865548,
-172.01266357002));
#161597=CARTESIAN_POINT('Ctrl Pts',(51.1960201863762,-46.8773198349542,
-171.996266629397));
#161598=CARTESIAN_POINT('Ctrl Pts',(51.1813252346626,-46.8783227416367,
-171.980270642003));
#161599=CARTESIAN_POINT('Ctrl Pts',(51.1760815181382,-46.8786806168068,
-171.974562666566));
#161600=CARTESIAN_POINT('Ctrl Pts',(51.1704835681801,-46.87906266784,-171.968608245986));
#161601=CARTESIAN_POINT('Ctrl Pts',(51.1649007295291,-46.8794436801573,
-171.96281560613));
#161602=CARTESIAN_POINT('Ctrl Pts',(51.1591502570813,-46.8798361329882,
-171.956849032855));
#161603=CARTESIAN_POINT('Ctrl Pts',(51.1534159776358,-46.8802274728275,
-171.951054248257));
#161604=CARTESIAN_POINT('Ctrl Pts',(51.1481430596939,-46.8805873095117,
-171.945838283025));
#161605=CARTESIAN_POINT('Ctrl Pts',(51.1471105039711,-46.8806577736137,
-171.944816879921));
#161606=CARTESIAN_POINT('Ctrl Pts',(51.1460957540418,-46.8807270218863,
-171.943817557264));
#161607=CARTESIAN_POINT('Ctrl Pts',(51.1451023065401,-46.8807948156287,
-171.942843213006));
#161608=CARTESIAN_POINT('Ctrl Pts',(51.1229463457133,-46.8823067581293,
-171.92111329455));
#161609=CARTESIAN_POINT('Ctrl Pts',(51.0991054270076,-46.8839338834152,
-171.89975899377));
#161610=CARTESIAN_POINT('Ctrl Pts',(51.0735249014539,-46.8856797757556,
-171.879051283109));
#161611=CARTESIAN_POINT('Ctrl Pts',(51.0483416062908,-46.8873985567883,
-171.858665134724));
#161612=CARTESIAN_POINT('Ctrl Pts',(51.0214720254546,-46.8892324645722,
-171.8389055125));
#161613=CARTESIAN_POINT('Ctrl Pts',(50.9928966807099,-46.8911826856249,
-171.820067900707));
#161614=CARTESIAN_POINT('Ctrl Pts',(50.9657113411477,-46.8930380410725,
-171.802146616547));
#161615=CARTESIAN_POINT('Ctrl Pts',(50.9369807600363,-46.8949988567561,
-171.785058883141));
#161616=CARTESIAN_POINT('Ctrl Pts',(50.9067163539354,-46.8970643535139,
-171.769091901735));
#161617=CARTESIAN_POINT('Ctrl Pts',(50.877346420633,-46.8990688039503,-171.75359682883));
#161618=CARTESIAN_POINT('Ctrl Pts',(50.8465313768786,-46.9011718808373,
-171.739157140914));
#161619=CARTESIAN_POINT('Ctrl Pts',(50.8143178781222,-46.9033704000159,
-171.726070467489));
#161620=CARTESIAN_POINT('Ctrl Pts',(50.8137877892207,-46.9034065777259,
-171.725855119867));
#161621=CARTESIAN_POINT('Ctrl Pts',(50.8132573242171,-46.9034427811042,
-171.725640139914));
#161622=CARTESIAN_POINT('Ctrl Pts',(50.8127264833758,-46.9034790101329,
-171.72542552869));
#161623=CARTESIAN_POINT('Ctrl Pts',(50.8100633907649,-46.9036607618955,
-171.724348879115));
#161624=CARTESIAN_POINT('Ctrl Pts',(50.8066757289513,-46.903891940699,-171.722996951259));
#161625=CARTESIAN_POINT('Ctrl Pts',(50.8038601511023,-46.9040840712449,
-171.721889199772));
#161626=CARTESIAN_POINT('Ctrl Pts',(50.8020215566215,-46.9042095340026,
-171.721165829338));
#161627=CARTESIAN_POINT('Ctrl Pts',(50.8004274736547,-46.9043183073482,
-171.720545222463));
#161628=CARTESIAN_POINT('Ctrl Pts',(50.7994425968086,-46.9043855068274,
-171.720163007342));
#161629=CARTESIAN_POINT('Ctrl Pts',(50.7837065498889,-46.9054591985905,
-171.714056096515));
#161630=CARTESIAN_POINT('Ctrl Pts',(50.7662821199151,-46.906648228503,-171.707738814551));
#161631=CARTESIAN_POINT('Ctrl Pts',(50.7471041895102,-46.9079570087933,
-171.701466819059));
#161632=CARTESIAN_POINT('Ctrl Pts',(50.7275914953754,-46.9092886347276,
-171.695085341649));
#161633=CARTESIAN_POINT('Ctrl Pts',(50.7062625124688,-46.9107442989673,
-171.688750401938));
#161634=CARTESIAN_POINT('Ctrl Pts',(50.6830688781689,-46.9123272682553,
-171.682785652503));
#161635=CARTESIAN_POINT('Ctrl Pts',(50.6621605794063,-46.9137542630237,
-171.677408626996));
#161636=CARTESIAN_POINT('Ctrl Pts',(50.6397366303949,-46.9152847355379,
-171.672333011606));
#161637=CARTESIAN_POINT('Ctrl Pts',(50.6157867345646,-46.9169193632623,
-171.667836203706));
#161638=CARTESIAN_POINT('Ctrl Pts',(50.5926162693159,-46.9185007933089,
-171.663485740894));
#161639=CARTESIAN_POINT('Ctrl Pts',(50.5680170405766,-46.9201797452105,
-171.65967709193));
#161640=CARTESIAN_POINT('Ctrl Pts',(50.5420110260361,-46.9219546956657,
-171.656697423928));
#161641=CARTESIAN_POINT('Ctrl Pts',(50.5172099822075,-46.9236474050181,
-171.653855816784));
#161642=CARTESIAN_POINT('Ctrl Pts',(50.4911291568878,-46.9254274461996,
-171.651768285827));
#161643=CARTESIAN_POINT('Ctrl Pts',(50.4638225435433,-46.9272911134907,
-171.650715593488));
#161644=CARTESIAN_POINT('Ctrl Pts',(50.4508645026649,-46.9281754954768,
-171.650216050385));
#161645=CARTESIAN_POINT('Ctrl Pts',(50.4376309822184,-46.9290786712979,
-171.64995));
#161646=CARTESIAN_POINT('Ctrl Pts',(50.4241310475534,-46.93000002,-171.64995));
#161647=CARTESIAN_POINT('Ctrl Pts',(49.6300753314849,-52.58000002,-171.64995));
#161648=CARTESIAN_POINT('Ctrl Pts',(49.6592062683373,-52.5780118806847,
-171.64995));
#161649=CARTESIAN_POINT('Ctrl Pts',(49.6870949010184,-52.576125534458,-171.651172745865));
#161650=CARTESIAN_POINT('Ctrl Pts',(49.7136621873133,-52.5743298726611,
-171.653316375876));
#161651=CARTESIAN_POINT('Ctrl Pts',(49.7414106383736,-52.572454376875,-171.655555310323));
#161652=CARTESIAN_POINT('Ctrl Pts',(49.7677180801388,-52.5706778703431,
-171.658798248614));
#161653=CARTESIAN_POINT('Ctrl Pts',(49.7925438592604,-52.5689946396099,
-171.662728774848));
#161654=CARTESIAN_POINT('Ctrl Pts',(49.8179907629401,-52.567269295558,-171.666757640246));
#161655=CARTESIAN_POINT('Ctrl Pts',(49.8418816270552,-52.565642050202,-171.671508529278));
#161656=CARTESIAN_POINT('Ctrl Pts',(49.8642143969623,-52.5641126147803,
-171.676676564475));
#161657=CARTESIAN_POINT('Ctrl Pts',(49.887281660145,-52.5625328783868,-171.682014569053));
#161658=CARTESIAN_POINT('Ctrl Pts',(49.9086873792323,-52.5610575929236,
-171.687797263142));
#161659=CARTESIAN_POINT('Ctrl Pts',(49.9284623174369,-52.5596910818783,
-171.693732405879));
#161660=CARTESIAN_POINT('Ctrl Pts',(49.9314331716388,-52.559485786416,-171.694624061952));
#161661=CARTESIAN_POINT('Ctrl Pts',(49.9343672660957,-52.5592829526098,
-171.69551924186));
#161662=CARTESIAN_POINT('Ctrl Pts',(49.9372647511473,-52.5590826015885,
-171.696417042859));
#161663=CARTESIAN_POINT('Ctrl Pts',(49.9500171622246,-52.5582008166826,
-171.700368444576));
#161664=CARTESIAN_POINT('Ctrl Pts',(49.9620601971446,-52.5573670921872,
-171.704369938142));
#161665=CARTESIAN_POINT('Ctrl Pts',(49.9734086898205,-52.5565835128729,
-171.708349867204));
#161666=CARTESIAN_POINT('Ctrl Pts',(49.9790829361585,-52.5561917232158,
-171.710339831735));
#161667=CARTESIAN_POINT('Ctrl Pts',(49.9845835094961,-52.5558124645922,
-171.7123245089));
#161668=CARTESIAN_POINT('Ctrl Pts',(49.9899125815189,-52.5554460422126,
-171.714295777019));
#161669=CARTESIAN_POINT('Ctrl Pts',(49.9925771175304,-52.5552628310228,
-171.715281411079));
#161670=CARTESIAN_POINT('Ctrl Pts',(49.995198775861,-52.5550828285634,-171.716263699745));
#161671=CARTESIAN_POINT('Ctrl Pts',(49.9977778228351,-52.554906072264,-171.717241672092));
#161672=CARTESIAN_POINT('Ctrl Pts',(49.9995468585359,-52.5547848305001,
-171.717912488876));
#161673=CARTESIAN_POINT('Ctrl Pts',(50.0003731303544,-52.5547277477509,
-171.718227889232));
#161674=CARTESIAN_POINT('Ctrl Pts',(50.0021560446491,-52.5546060349271,
-171.718913272988));
#161675=CARTESIAN_POINT('Ctrl Pts',(50.0029724106939,-52.554550304701,-171.719227098519));
#161676=CARTESIAN_POINT('Ctrl Pts',(50.0039892197234,-52.5544810069693,
-171.719618819411));
#161677=CARTESIAN_POINT('Ctrl Pts',(50.0053873934298,-52.5543855789116,
-171.720161698938));
#161678=CARTESIAN_POINT('Ctrl Pts',(50.0390970047312,-52.5520848327899,
-171.733250385798));
#161679=CARTESIAN_POINT('Ctrl Pts',(50.0713392048815,-52.5498963013618,
-171.747810336266));
#161680=CARTESIAN_POINT('Ctrl Pts',(50.1020456307454,-52.5478103768153,
-171.763538020853));
#161681=CARTESIAN_POINT('Ctrl Pts',(50.1335563870302,-52.5456698131331,
-171.779677679638));
#161682=CARTESIAN_POINT('Ctrl Pts',(50.1634501719592,-52.5436373461994,
-171.797046561953));
#161683=CARTESIAN_POINT('Ctrl Pts',(50.1917037810275,-52.5417097148338,
-171.815335004119));
#161684=CARTESIAN_POINT('Ctrl Pts',(50.1940932268591,-52.541546692449,-171.816881682343));
#161685=CARTESIAN_POINT('Ctrl Pts',(50.1964709691268,-52.541384423744,-171.81843495061));
#161686=CARTESIAN_POINT('Ctrl Pts',(50.1988370086813,-52.5412229088385,
-171.81999462906));
#161687=CARTESIAN_POINT('Ctrl Pts',(50.2276398112107,-52.5392567194225,
-171.83898125602));
#161688=CARTESIAN_POINT('Ctrl Pts',(50.2547047352767,-52.5374017274936,
-171.858915411873));
#161689=CARTESIAN_POINT('Ctrl Pts',(50.2800576780874,-52.535661572667,-171.879488097075));
#161690=CARTESIAN_POINT('Ctrl Pts',(50.2927341494928,-52.5347914952537,
-171.889774439675));
#161691=CARTESIAN_POINT('Ctrl Pts',(50.3049833101608,-52.5339502233269,
-171.900220871814));
#161692=CARTESIAN_POINT('Ctrl Pts',(50.3168121152348,-52.5331387343682,
-171.910791641771));
#161693=CARTESIAN_POINT('Ctrl Pts',(50.3223288922278,-52.5327602681082,
-171.915721690083));
#161694=CARTESIAN_POINT('Ctrl Pts',(50.3274289643461,-52.5324082123672,
-171.920381836518));
#161695=CARTESIAN_POINT('Ctrl Pts',(50.3325737573137,-52.5320555671373,
-171.925178375207));
#161696=CARTESIAN_POINT('Ctrl Pts',(50.3375775319413,-52.5317125878833,
-171.929843441175));
#161697=CARTESIAN_POINT('Ctrl Pts',(50.3426237602553,-52.5313690722106,
-171.934637611929));
#161698=CARTESIAN_POINT('Ctrl Pts',(50.348104148547,-52.5309955692892,-171.939969076396));
#161699=CARTESIAN_POINT('Ctrl Pts',(50.3490708688542,-52.5309296847497,
-171.940909527089));
#161700=CARTESIAN_POINT('Ctrl Pts',(50.3500510063111,-52.530862854204,-171.941866786942));
#161701=CARTESIAN_POINT('Ctrl Pts',(50.3510465847208,-52.5307948982762,
-171.942843218813));
#161702=CARTESIAN_POINT('Ctrl Pts',(50.3818387641553,-52.5286930938358,
-171.973043216233));
#161703=CARTESIAN_POINT('Ctrl Pts',(50.4104020698678,-52.5267752596114,
-172.004935794585));
#161704=CARTESIAN_POINT('Ctrl Pts',(50.43660977222,-52.5250235849138,-172.03817789155));
#161705=CARTESIAN_POINT('Ctrl Pts',(50.4631285790983,-52.5232511165611,
-172.071814596431));
#161706=CARTESIAN_POINT('Ctrl Pts',(50.4872356273342,-52.5216487903698,
-172.10683253693));
#161707=CARTESIAN_POINT('Ctrl Pts',(50.508852831868,-52.5202056322005,-172.14287770852));
#161708=CARTESIAN_POINT('Ctrl Pts',(50.5307318008976,-52.518744998711,-172.179359354038));
#161709=CARTESIAN_POINT('Ctrl Pts',(50.5500604364366,-52.5174474358973,
-172.216892769679));
#161710=CARTESIAN_POINT('Ctrl Pts',(50.5668098649344,-52.5163088858466,
-172.255120022273));
#161711=CARTESIAN_POINT('Ctrl Pts',(50.583870938874,-52.5151491515546,-172.294058543854));
#161712=CARTESIAN_POINT('Ctrl Pts',(50.5982561304957,-52.5141544300228,
-172.333716479937));
#161713=CARTESIAN_POINT('Ctrl Pts',(50.6099858799555,-52.5133275939276,
-172.373732379297));
#161714=CARTESIAN_POINT('Ctrl Pts',(50.6218418428613,-52.5124918609815,
-172.414178854313));
#161715=CARTESIAN_POINT('Ctrl Pts',(50.6309852381434,-52.5118276918993,
-172.454990623381));
#161716=CARTESIAN_POINT('Ctrl Pts',(50.6374846521774,-52.5113447258674,
-172.495818301581));
#161717=CARTESIAN_POINT('Ctrl Pts',(50.6440871507285,-52.5108540997111,
-172.537293530694));
#161718=CARTESIAN_POINT('Ctrl Pts',(50.6479614840189,-52.5105505195319,
-172.578784792508));
#161719=CARTESIAN_POINT('Ctrl Pts',(50.6492231617337,-52.5104502191572,
-172.619956446583));
#161720=CARTESIAN_POINT('Ctrl Pts',(50.6495301605875,-52.5104258134792,
-172.629974575984));
#161721=CARTESIAN_POINT('Ctrl Pts',(50.6496826558921,-52.51041346952,-172.639973937106));
#161722=CARTESIAN_POINT('Ctrl Pts',(50.6496826558921,-52.51041346952,-172.64995));
#161723=CARTESIAN_POINT('Ctrl Pts',(52.5050296388285,-39.3089337226171,
-172.133326251627));
#161724=CARTESIAN_POINT('Ctrl Pts',(52.4864722882118,-39.4409761333229,
-171.679515584751));
#161725=CARTESIAN_POINT('Ctrl Pts',(52.1126146143194,-39.4738501833479,
-171.391638125813));
#161726=CARTESIAN_POINT('Ctrl Pts',(52.541270746464,-39.0510648426419,-172.04151129494));
#161727=CARTESIAN_POINT('Ctrl Pts',(52.5176461244299,-39.1701487854048,
-171.633412526629));
#161728=CARTESIAN_POINT('Ctrl Pts',(52.2029436074416,-39.18424163534,-171.345711176575));
#161729=CARTESIAN_POINT('Ctrl Pts',(52.5971684400779,-38.7973422647502,
-171.953442620307));
#161730=CARTESIAN_POINT('Ctrl Pts',(52.5724535929286,-38.8910154875477,
-171.580271166833));
#161731=CARTESIAN_POINT('Ctrl Pts',(52.3057718899875,-38.8932964873464,
-171.301698499895));
#161732=CARTESIAN_POINT('Ctrl Pts',(52.6743159902015,-38.5446760769969,
-171.890184412595));
#161733=CARTESIAN_POINT('Ctrl Pts',(52.6539547691069,-38.61136117722,-171.540761416572));
#161734=CARTESIAN_POINT('Ctrl Pts',(52.4226914394942,-38.5972250898729,
-171.270067206297));
#161735=CARTESIAN_POINT('',(52.6451353368861,-38.6439093768522,-171.916253407912));
#161736=CARTESIAN_POINT('Ctrl Pts',(52.6451215732066,-38.6439145871468,
-171.916241762849));
#161737=CARTESIAN_POINT('Ctrl Pts',(52.6327200436122,-38.6877262200968,
-171.928258148288));
#161738=CARTESIAN_POINT('Ctrl Pts',(52.6204218089369,-38.7334430503703,
-171.941450676397));
#161739=CARTESIAN_POINT('Ctrl Pts',(52.6083879533182,-38.7810797529306,
-171.955850381936));
#161740=CARTESIAN_POINT('Ctrl Pts',(52.5975991294693,-38.8237879263498,
-171.96876028309));
#161741=CARTESIAN_POINT('Ctrl Pts',(52.5870229477254,-38.8680394620078,
-171.982640380926));
#161742=CARTESIAN_POINT('Ctrl Pts',(52.5767804085671,-38.9138488166889,
-171.997474376372));
#161743=CARTESIAN_POINT('Ctrl Pts',(52.574859932475,-38.9224380706917,-172.000255750518));
#161744=CARTESIAN_POINT('Ctrl Pts',(52.5729511953933,-38.9310821107148,
-172.003070546334));
#161745=CARTESIAN_POINT('Ctrl Pts',(52.5710550072722,-38.9397810591365,
-172.005918494111));
#161746=CARTESIAN_POINT('Ctrl Pts',(52.5701661690904,-38.9438586912092,
-172.007253469632));
#161747=CARTESIAN_POINT('Ctrl Pts',(52.5692800882732,-38.9479483883608,
-172.008595728785));
#161748=CARTESIAN_POINT('Ctrl Pts',(52.5683968484763,-38.9520501640132,
-172.009945239696));
#161749=CARTESIAN_POINT('Ctrl Pts',(52.5682526090381,-38.9527200136028,
-172.010165624574));
#161750=CARTESIAN_POINT('Ctrl Pts',(52.5681091671282,-38.9533868184525,
-172.010385093187));
#161751=CARTESIAN_POINT('Ctrl Pts',(52.5679617607653,-38.9540727644232,
-172.010610953635));
#161752=CARTESIAN_POINT('Ctrl Pts',(52.567091942239,-38.9581204086464,-172.011943715654));
#161753=CARTESIAN_POINT('Ctrl Pts',(52.5661205622637,-38.9626690977524,
-172.013445117389));
#161754=CARTESIAN_POINT('Ctrl Pts',(52.5652406411583,-38.9668167293616,
-172.014817530366));
#161755=CARTESIAN_POINT('Ctrl Pts',(52.5648144293729,-38.9688257384223,
-172.015482292902));
#161756=CARTESIAN_POINT('Ctrl Pts',(52.5644095232376,-38.970740631272,-172.016116692328));
#161757=CARTESIAN_POINT('Ctrl Pts',(52.5640471013215,-38.9724587861977,
-172.016686420464));
#161758=CARTESIAN_POINT('Ctrl Pts',(52.5638603874838,-38.9733439514863,
-172.016979935072));
#161759=CARTESIAN_POINT('Ctrl Pts',(52.5636849424823,-38.9741768987548,
-172.01725628059));
#161760=CARTESIAN_POINT('Ctrl Pts',(52.563523628473,-38.9749435910523,-172.017510745119));
#161761=CARTESIAN_POINT('Ctrl Pts',(52.5634372349735,-38.9753542015808,
-172.017647026409));
#161762=CARTESIAN_POINT('Ctrl Pts',(52.5633560421201,-38.9757403405034,
-172.017775215173));
#161763=CARTESIAN_POINT('Ctrl Pts',(52.5632737953258,-38.9761317175597,
-172.017905169922));
#161764=CARTESIAN_POINT('Ctrl Pts',(52.5564953797729,-39.0083872765447,
-172.028615463309));
#161765=CARTESIAN_POINT('Ctrl Pts',(52.5494159142318,-39.0436596555478,
-172.040521990413));
#161766=CARTESIAN_POINT('Ctrl Pts',(52.5422310058208,-39.0819615094717,
-172.053670741783));
#161767=CARTESIAN_POINT('Ctrl Pts',(52.5357568450765,-39.1164744559038,
-172.065518788423));
#161768=CARTESIAN_POINT('Ctrl Pts',(52.5291975175797,-39.1534471810898,
-172.078375959746));
#161769=CARTESIAN_POINT('Ctrl Pts',(52.5227135897134,-39.192898939103,-172.092240973108));
#161770=CARTESIAN_POINT('Ctrl Pts',(52.5167076842734,-39.2294421476268,
-172.105083799384));
#161771=CARTESIAN_POINT('Ctrl Pts',(52.5107667105805,-39.2681123359778,
-172.118791679458));
#161772=CARTESIAN_POINT('Ctrl Pts',(52.5050296388285,-39.3089337226171,
-172.133326251627));
#161773=CARTESIAN_POINT('Ctrl Pts',(52.6451353368861,-38.6439093768522,
-171.916253407912));
#161774=CARTESIAN_POINT('Ctrl Pts',(52.6464058796499,-38.6394159797481,
-171.881371542694));
#161775=CARTESIAN_POINT('Ctrl Pts',(52.6459390342692,-38.6353252452434,
-171.84657946844));
#161776=CARTESIAN_POINT('Ctrl Pts',(52.6436236858027,-38.6316512514798,
-171.812021915484));
#161777=CARTESIAN_POINT('Ctrl Pts',(52.6416753037096,-38.6285595597699,
-171.782941490513));
#161778=CARTESIAN_POINT('Ctrl Pts',(52.6384182215079,-38.6257624918022,
-171.754024489139));
#161779=CARTESIAN_POINT('Ctrl Pts',(52.633815177568,-38.6232615998417,-171.725358956929));
#161780=CARTESIAN_POINT('Ctrl Pts',(52.6300898783601,-38.6212375976898,
-171.702159594543));
#161781=CARTESIAN_POINT('Ctrl Pts',(52.6254838305633,-38.6194078000763,
-171.67912846901));
#161782=CARTESIAN_POINT('Ctrl Pts',(52.6199955276943,-38.6177699986579,
-171.656318341932));
#161783=CARTESIAN_POINT('Ctrl Pts',(52.6170443172279,-38.6168893080686,
-171.644052713124));
#161784=CARTESIAN_POINT('Ctrl Pts',(52.6137814340186,-38.6160491681525,
-171.631632234766));
#161785=CARTESIAN_POINT('Ctrl Pts',(52.6102740456651,-38.6152700458307,
-171.619352410973));
#161786=CARTESIAN_POINT('Ctrl Pts',(52.6067346866106,-38.6144838216188,
-171.606960653589));
#161787=CARTESIAN_POINT('Ctrl Pts',(52.6029463207216,-38.6137596916157,
-171.594712118775));
#161788=CARTESIAN_POINT('Ctrl Pts',(52.5990294893407,-38.6131080795974,
-171.582899413039));
#161789=CARTESIAN_POINT('Ctrl Pts',(52.5979152610766,-38.6129227143219,
-171.5795390308));
#161790=CARTESIAN_POINT('Ctrl Pts',(52.5967909510326,-38.6127431551648,
-171.576213850961));
#161791=CARTESIAN_POINT('Ctrl Pts',(52.5956600639907,-38.6125694994672,
-171.572930455134));
#161792=CARTESIAN_POINT('Ctrl Pts',(52.5951960360173,-38.6124982446924,
-171.571583205183));
#161793=CARTESIAN_POINT('Ctrl Pts',(52.5947281719133,-38.612427569521,-171.57023506049));
#161794=CARTESIAN_POINT('Ctrl Pts',(52.5942564505892,-38.6123574779562,
-171.568886040307));
#161795=CARTESIAN_POINT('Ctrl Pts',(52.5844642885233,-38.610902491872,-171.540882590844));
#161796=CARTESIAN_POINT('Ctrl Pts',(52.5731590893685,-38.6097161264722,
-171.512940465127));
#161797=CARTESIAN_POINT('Ctrl Pts',(52.560232179002,-38.6088174063243,-171.485293111838));
#161798=CARTESIAN_POINT('Ctrl Pts',(52.5474861932036,-38.607931264631,-171.458032709902));
#161799=CARTESIAN_POINT('Ctrl Pts',(52.5331634401878,-38.6073246921442,
-171.431059045936));
#161800=CARTESIAN_POINT('Ctrl Pts',(52.5172023231265,-38.607001419367,-171.404574211142));
#161801=CARTESIAN_POINT('Ctrl Pts',(52.5014583125321,-38.606682543814,-171.378449628634));
#161802=CARTESIAN_POINT('Ctrl Pts',(52.4841201593532,-38.6066392012133,
-171.352800783014));
#161803=CARTESIAN_POINT('Ctrl Pts',(52.4651717697575,-38.606862192425,-171.327798354999));
#161804=CARTESIAN_POINT('Ctrl Pts',(52.4505678703726,-38.6070340561712,
-171.308528488224));
#161805=CARTESIAN_POINT('Ctrl Pts',(52.435008333388,-38.6073638509613,-171.28964214896));
#161806=CARTESIAN_POINT('Ctrl Pts',(52.418503743379,-38.6078427661477,-171.27120723903));
#161807=CARTESIAN_POINT('Ctrl Pts',(52.9938276306004,-37.7501447842495,
-177.831926349313));
#161808=CARTESIAN_POINT('Ctrl Pts',(53.0290644361633,-37.6768546791036,
-177.379478122309));
#161809=CARTESIAN_POINT('Ctrl Pts',(53.4403098198818,-37.8775685921338,
-177.340139197757));
#161810=CARTESIAN_POINT('Ctrl Pts',(52.8644526083797,-38.0038787899799,
-177.788318381118));
#161811=CARTESIAN_POINT('Ctrl Pts',(52.9387831734984,-37.8445082365119,
-177.396106921235));
#161812=CARTESIAN_POINT('Ctrl Pts',(53.3237240701773,-37.9919010307737,
-177.318314744026));
#161813=CARTESIAN_POINT('Ctrl Pts',(52.7697107392458,-38.2534999676582,
-177.654124612897));
#161814=CARTESIAN_POINT('Ctrl Pts',(52.8575871067054,-38.0208239861393,
-177.3297491457));
#161815=CARTESIAN_POINT('Ctrl Pts',(53.2386901038944,-38.1039031063401,
-177.251398738488));
#161816=CARTESIAN_POINT('Ctrl Pts',(52.6567775733111,-38.592091397267,-177.247773453598));
#161817=CARTESIAN_POINT('Ctrl Pts',(52.7597859066203,-38.2459774998252,
-177.093855210388));
#161818=CARTESIAN_POINT('Ctrl Pts',(53.1371100205879,-38.2560577153129,
-177.048553549081));
#161819=CARTESIAN_POINT('Ctrl Pts',(52.6371617173208,-38.6755874697231,
-176.979974147571));
#161820=CARTESIAN_POINT('Ctrl Pts',(52.7392639513461,-38.2994134985588,
-176.927419692177));
#161821=CARTESIAN_POINT('Ctrl Pts',(53.1194519999705,-38.2935777262418,
-176.914856994736));
#161822=CARTESIAN_POINT('Ctrl Pts',(52.6472666300096,-38.6354176228512,
-176.719388397061));
#161823=CARTESIAN_POINT('Ctrl Pts',(52.7494003756538,-38.2736022260138,
-176.771349933471));
#161824=CARTESIAN_POINT('Ctrl Pts',(53.1285467956633,-38.2755266296908,
-176.784773168118));
#161825=CARTESIAN_POINT('',(53.1262583325313,-38.28000002,-176.84995));
#161826=CARTESIAN_POINT('',(52.6451348158641,-38.6439112191758,-176.84995));
#161827=CARTESIAN_POINT('Origin',(53.1262583325313,-38.78000002,-176.84995));
#161828=CARTESIAN_POINT('',(52.9322463618642,-37.8758780299853,-177.801086692062));
#161829=CARTESIAN_POINT('Ctrl Pts',(52.9322463618642,-37.8758780299853,
-177.801086692062));
#161830=CARTESIAN_POINT('Ctrl Pts',(52.8821502360452,-37.9823362053254,
-177.769982861881));
#161831=CARTESIAN_POINT('Ctrl Pts',(52.8404306738594,-38.0806649492,-177.726394810699));
#161832=CARTESIAN_POINT('Ctrl Pts',(52.7876627669651,-38.2144165753642,
-177.642286402424));
#161833=CARTESIAN_POINT('Ctrl Pts',(52.7717128843553,-38.2567167732527,
-177.611129211082));
#161834=CARTESIAN_POINT('Ctrl Pts',(52.7499450355462,-38.3166003893438,
-177.559711841195));
#161835=CARTESIAN_POINT('Ctrl Pts',(52.743048896851,-38.3359674737686,-177.541792454086));
#161836=CARTESIAN_POINT('Ctrl Pts',(52.7299298022954,-38.3734935229716,
-177.504393152244));
#161837=CARTESIAN_POINT('Ctrl Pts',(52.7239522510328,-38.3909236892047,
-177.485754776825));
#161838=CARTESIAN_POINT('Ctrl Pts',(52.6931841096669,-38.4822980769602,
-177.380246187521));
#161839=CARTESIAN_POINT('Ctrl Pts',(52.6758770663329,-38.5389294441427,
-177.287304310837));
#161840=CARTESIAN_POINT('Ctrl Pts',(52.6511315042833,-38.6222038742842,
-177.073724745201));
#161841=CARTESIAN_POINT('Ctrl Pts',(52.6452799403198,-38.6433981513254,
-176.963536569195));
#161842=CARTESIAN_POINT('Ctrl Pts',(52.6451348158641,-38.6439112191758,
-176.84995));
#161843=CARTESIAN_POINT('',(53.3846587239314,-37.9343850848642,-177.325518346031));
#161844=CARTESIAN_POINT('Origin',(53.3846587239314,-38.0887701497285,-177.801086692062));
#161845=CARTESIAN_POINT('Ctrl Pts',(53.1262583325313,-38.28000002,-176.84995));
#161846=CARTESIAN_POINT('Ctrl Pts',(53.1262583325313,-38.28000002,-176.881246264157));
#161847=CARTESIAN_POINT('Ctrl Pts',(53.1278631222718,-38.2769604420907,
-176.912161979889));
#161848=CARTESIAN_POINT('Ctrl Pts',(53.1310877945824,-38.2712384373324,
-176.942246935877));
#161849=CARTESIAN_POINT('Ctrl Pts',(53.1344117918852,-38.2653401858042,
-176.97325855595));
#161850=CARTESIAN_POINT('Ctrl Pts',(53.1394569106395,-38.2565916101631,
-177.003387789554));
#161851=CARTESIAN_POINT('Ctrl Pts',(53.1462419631605,-38.2453451529124,
-177.032183119753));
#161852=CARTESIAN_POINT('Ctrl Pts',(53.1533750701167,-38.2335217834987,
-177.062455570778));
#161853=CARTESIAN_POINT('Ctrl Pts',(53.1624310737952,-38.2189376813828,
-177.09125406242));
#161854=CARTESIAN_POINT('Ctrl Pts',(53.1734359847931,-38.201960916429,-177.118094373856));
#161855=CARTESIAN_POINT('Ctrl Pts',(53.1779314035387,-38.1950260427687,
-177.129058427921));
#161856=CARTESIAN_POINT('Ctrl Pts',(53.1827520853554,-38.1876914539528,
-177.139696152833));
#161857=CARTESIAN_POINT('Ctrl Pts',(53.1879000622338,-38.1799804108256,
-177.149976143786));
#161858=CARTESIAN_POINT('Ctrl Pts',(53.188619169172,-38.1789032761096,-177.151412127861));
#161859=CARTESIAN_POINT('Ctrl Pts',(53.1893448856165,-38.1778193219541,
-177.152840685413));
#161860=CARTESIAN_POINT('Ctrl Pts',(53.1900771912037,-38.1767286560635,
-177.154261804692));
#161861=CARTESIAN_POINT('Ctrl Pts',(53.2032198647385,-38.1571544974243,
-177.179766603611));
#161862=CARTESIAN_POINT('Ctrl Pts',(53.2185121297572,-38.1353791413438,
-177.202931559866));
#161863=CARTESIAN_POINT('Ctrl Pts',(53.235872888282,-38.1119750815074,-177.223655356482));
#161864=CARTESIAN_POINT('Ctrl Pts',(53.2503574923944,-38.0924483689579,
-177.24094584464));
#161865=CARTESIAN_POINT('Ctrl Pts',(53.2662825550407,-38.0717865852687,
-177.256537463912));
#161866=CARTESIAN_POINT('Ctrl Pts',(53.2836107583403,-38.0503026809971,
-177.270367729685));
#161867=CARTESIAN_POINT('Ctrl Pts',(53.3088054318523,-38.0190657463577,
-177.290476509845));
#161868=CARTESIAN_POINT('Ctrl Pts',(53.3369667492511,-37.9860904738857,
-177.306863401143));
#161869=CARTESIAN_POINT('Ctrl Pts',(53.3679987952442,-37.9523040600082,
-177.319310738459));
#161870=CARTESIAN_POINT('Ctrl Pts',(53.3734631729281,-37.9463546705915,
-177.321502567908));
#161871=CARTESIAN_POINT('Ctrl Pts',(53.3790166292581,-37.9403800305232,
-177.323572190274));
#161872=CARTESIAN_POINT('Ctrl Pts',(53.3846587239314,-37.9343850848643,
-177.325518346031));
#161873=CARTESIAN_POINT('Ctrl Pts',(53.0752347700893,-37.5697245962714,
-177.84995));
#161874=CARTESIAN_POINT('Ctrl Pts',(53.0752347700892,-37.5697245962714,
-177.34995));
#161875=CARTESIAN_POINT('Ctrl Pts',(53.5288692553037,-37.78000002,-177.34995));
#161876=CARTESIAN_POINT('Ctrl Pts',(53.0269261151962,-37.673942537699,-177.849949988053));
#161877=CARTESIAN_POINT('Ctrl Pts',(53.0475810937503,-37.6293828354337,
-177.371580332169));
#161878=CARTESIAN_POINT('Ctrl Pts',(53.4801386760123,-37.8325641065285,
-177.34995));
#161879=CARTESIAN_POINT('Ctrl Pts',(52.9791793012708,-37.7761418725299,
-177.833741031442));
#161880=CARTESIAN_POINT('Ctrl Pts',(53.0170937964823,-37.6950135347464,
-177.382936820891));
#161881=CARTESIAN_POINT('Ctrl Pts',(53.4320050770023,-37.884077740683,-177.341849758034));
#161882=CARTESIAN_POINT('Ctrl Pts',(52.9322463618642,-37.8758780299853,
-177.801086692062));
#161883=CARTESIAN_POINT('Ctrl Pts',(52.9848137611505,-37.764168205744,-177.380776321343));
#161884=CARTESIAN_POINT('Ctrl Pts',(53.3846587239314,-37.9343850848642,
-177.325518346031));
#161885=CARTESIAN_POINT('',(53.0752347700893,-37.5697245962714,-177.84995));
#161886=CARTESIAN_POINT('Origin',(53.46537255433,-36.3098838506748,-168.829790838513));
#161887=CARTESIAN_POINT('Origin',(53.5288692553037,-37.78000002,-177.84995));
#161888=CARTESIAN_POINT('Origin',(54.0849713004979,-36.8984163346077,-171.288907793803));
#161889=CARTESIAN_POINT('Origin',(0.,-12.9675000200281,-177.84995));
#161890=CARTESIAN_POINT('',(53.3022372549338,-37.073961884407,-177.84995));
#161891=CARTESIAN_POINT('Origin',(0.,-12.9675000200281,-177.84995));
#161892=CARTESIAN_POINT('Origin',(53.7578119323263,-37.28000002,-177.84995));
#161893=CARTESIAN_POINT('Ctrl Pts',(53.7396474992599,-36.0824364606782,
-176.84995));
#161894=CARTESIAN_POINT('Ctrl Pts',(53.4396057593646,-36.78000002,-176.84995));
#161895=CARTESIAN_POINT('Ctrl Pts',(54.1989607257493,-36.78000002,-176.84995));
#161896=CARTESIAN_POINT('Ctrl Pts',(53.7396474882981,-36.0824364861631,
-176.986685785392));
#161897=CARTESIAN_POINT('Ctrl Pts',(53.4396057606977,-36.7800000160094,
-176.873130497251));
#161898=CARTESIAN_POINT('Ctrl Pts',(54.1989607146972,-36.78000002,-176.918317891383));
#161899=CARTESIAN_POINT('Ctrl Pts',(53.7273175494953,-36.1111537311933,
-177.124284716345));
#161900=CARTESIAN_POINT('Ctrl Pts',(53.4415801188845,-36.7743609339043,
-176.898046003587));
#161901=CARTESIAN_POINT('Ctrl Pts',(54.1865253922149,-36.7944813746413,
-176.987117359946));
#161902=CARTESIAN_POINT('Ctrl Pts',(53.6813602693863,-36.2175520155611,
-177.371624356797));
#161903=CARTESIAN_POINT('Ctrl Pts',(53.4422054158915,-36.7696056006871,
-176.971124353297));
#161904=CARTESIAN_POINT('Ctrl Pts',(54.1401753140075,-36.8481352183371,
-177.110787176626));
#161905=CARTESIAN_POINT('Ctrl Pts',(53.64758418971,-36.2955323627627,-177.48288953791));
#161906=CARTESIAN_POINT('Ctrl Pts',(53.4404233153528,-36.7716343519663,
-177.018743720143));
#161907=CARTESIAN_POINT('Ctrl Pts',(54.1061105508192,-36.8874586360784,
-177.16641977034));
#161908=CARTESIAN_POINT('Ctrl Pts',(53.565994475128,-36.4822744877163,-177.662885027711));
#161909=CARTESIAN_POINT('Ctrl Pts',(53.4231809570326,-36.8072884980391,
-177.124958325117));
#161910=CARTESIAN_POINT('Ctrl Pts',(54.0238234872226,-36.9816277442484,
-177.25641751247));
#161911=CARTESIAN_POINT('Ctrl Pts',(53.5177345753394,-36.5920295740937,
-177.73300576859));
#161912=CARTESIAN_POINT('Ctrl Pts',(53.408253154931,-36.8396793680934,-177.182243847129));
#161913=CARTESIAN_POINT('Ctrl Pts',(53.9751511105352,-37.0369743252984,
-177.291477883886));
#161914=CARTESIAN_POINT('Ctrl Pts',(53.4140738058199,-36.825476258465,-177.826284139284));
#161915=CARTESIAN_POINT('Ctrl Pts',(53.3641465670514,-36.936877735883,-177.281217994791));
#161916=CARTESIAN_POINT('Ctrl Pts',(53.8706043508049,-37.1546953024018,
-177.33811707005));
#161917=CARTESIAN_POINT('Ctrl Pts',(53.3581698892714,-36.9502882170505,
-177.849949987733));
#161918=CARTESIAN_POINT('Ctrl Pts',(53.3356547273387,-37.0000719000691,
-177.323538819178));
#161919=CARTESIAN_POINT('Ctrl Pts',(53.8142255012181,-37.2176314844153,
-177.34995));
#161920=CARTESIAN_POINT('Ctrl Pts',(53.3022372549337,-37.073961884407,-177.84995));
#161921=CARTESIAN_POINT('Ctrl Pts',(53.3022372549337,-37.073961884407,-177.34995));
#161922=CARTESIAN_POINT('Ctrl Pts',(53.7578119323263,-37.28000002,-177.34995));
#161923=CARTESIAN_POINT('',(53.7396474992599,-36.0824364606782,-176.84995));
#161924=CARTESIAN_POINT('',(54.1989607257493,-36.78000002,-176.84995));
#161925=CARTESIAN_POINT('Origin',(54.1989607257493,-36.28000002,-176.84995));
#161926=CARTESIAN_POINT('Ctrl Pts',(53.7578119323263,-37.28000002,-177.34995));
#161927=CARTESIAN_POINT('Ctrl Pts',(53.7742161642685,-37.2618641718634,
-177.34995));
#161928=CARTESIAN_POINT('Ctrl Pts',(53.7896996386724,-37.2446503004515,
-177.348965174158));
#161929=CARTESIAN_POINT('Ctrl Pts',(53.8042623555378,-37.2284354820834,
-177.347283990825));
#161930=CARTESIAN_POINT('Ctrl Pts',(53.8188250724033,-37.2122206637153,
-177.345602807491));
#161931=CARTESIAN_POINT('Ctrl Pts',(53.8324670317305,-37.1970039098326,
-177.343225742402));
#161932=CARTESIAN_POINT('Ctrl Pts',(53.8451882335193,-37.1828122174664,
-177.340413587883));
#161933=CARTESIAN_POINT('Ctrl Pts',(53.857909435308,-37.1686205251002,-177.337601433363));
#161934=CARTESIAN_POINT('Ctrl Pts',(53.8697098795585,-37.1554529856455,
-177.334354420005));
#161935=CARTESIAN_POINT('Ctrl Pts',(53.8805895662706,-37.1433007895161,
-177.330900434437));
#161936=CARTESIAN_POINT('Ctrl Pts',(53.8860294096267,-37.1372246914513,
-177.329173441653));
#161937=CARTESIAN_POINT('Ctrl Pts',(53.8912390635981,-37.1314019563217,
-177.327394169022));
#161938=CARTESIAN_POINT('Ctrl Pts',(53.896218528185,-37.1258291482413,-177.325587826819));
#161939=CARTESIAN_POINT('Ctrl Pts',(53.8987082604785,-37.123042744201,-177.324684655718));
#161940=CARTESIAN_POINT('Ctrl Pts',(53.9011404454257,-37.1203188302431,
-177.323774692228));
#161941=CARTESIAN_POINT('Ctrl Pts',(53.9035150830269,-37.1176568289441,
-177.322860867202));
#161942=CARTESIAN_POINT('Ctrl Pts',(53.9050269887681,-37.1159619618851,
-177.322279044821));
#161943=CARTESIAN_POINT('Ctrl Pts',(53.9060312701474,-37.1148383391854,
-177.321886952289));
#161944=CARTESIAN_POINT('Ctrl Pts',(53.9074529654649,-37.1132418564841,
-177.32132216178));
#161945=CARTESIAN_POINT('Ctrl Pts',(53.9082642209632,-37.1123308628601,
-177.320999877954));
#161946=CARTESIAN_POINT('Ctrl Pts',(53.9092113920242,-37.11126605107,-177.32062090017));
#161947=CARTESIAN_POINT('Ctrl Pts',(53.9104663537919,-37.1098560275704,
-177.320110634082));
#161948=CARTESIAN_POINT('Ctrl Pts',(53.9286403697806,-37.0894364496314,
-177.312721098969));
#161949=CARTESIAN_POINT('Ctrl Pts',(53.945830114481,-37.0700140267857,-177.30418716129));
#161950=CARTESIAN_POINT('Ctrl Pts',(53.9620355878932,-37.0516626268298,
-177.294766855436));
#161951=CARTESIAN_POINT('Ctrl Pts',(53.9704708009668,-37.0421104240097,
-177.289863432681));
#161952=CARTESIAN_POINT('Ctrl Pts',(53.9786393383145,-37.0328475167389,
-177.284719695117));
#161953=CARTESIAN_POINT('Ctrl Pts',(53.9865411999362,-37.0238789920465,
-177.279370561967));
#161954=CARTESIAN_POINT('Ctrl Pts',(53.9980825382031,-37.0107797020075,
-177.271557699875));
#161955=CARTESIAN_POINT('Ctrl Pts',(54.0090549750916,-36.9983089772956,
-177.263307000333));
#161956=CARTESIAN_POINT('Ctrl Pts',(54.0194585106015,-36.9864704300919,
-177.254722009715));
#161957=CARTESIAN_POINT('Ctrl Pts',(54.0246602783564,-36.9805511564901,
-177.250429514406));
#161958=CARTESIAN_POINT('Ctrl Pts',(54.0297198207667,-36.9747897105812,
-177.24605334149));
#161959=CARTESIAN_POINT('Ctrl Pts',(54.0346371378324,-36.9691853307801,
-177.241605753137));
#161960=CARTESIAN_POINT('Ctrl Pts',(54.0370957963652,-36.9663831408796,
-177.23938195896));
#161961=CARTESIAN_POINT('Ctrl Pts',(54.0395188985619,-36.9636202164527,
-177.237140312228));
#161962=CARTESIAN_POINT('Ctrl Pts',(54.0419064444224,-36.9608963777589,
-177.234882286914));
#161963=CARTESIAN_POINT('Ctrl Pts',(54.043405607905,-36.9591860527052,-177.233464450653));
#161964=CARTESIAN_POINT('Ctrl Pts',(54.0445719721906,-36.9578593946011,
-177.232350366739));
#161965=CARTESIAN_POINT('Ctrl Pts',(54.0460060332577,-36.9562209688304,
-177.230958039316));
#161966=CARTESIAN_POINT('Ctrl Pts',(54.0468558368952,-36.9552500616551,
-177.230132966427));
#161967=CARTESIAN_POINT('Ctrl Pts',(54.0477996442507,-36.954170063335,-177.229209704986));
#161968=CARTESIAN_POINT('Ctrl Pts',(54.0489624129955,-36.9528419344281,
-177.228060548709));
#161969=CARTESIAN_POINT('Ctrl Pts',(54.0658572581406,-36.933544432399,-177.211363490556));
#161970=CARTESIAN_POINT('Ctrl Pts',(54.0813249082697,-36.9157048558455,
-177.193340117963));
#161971=CARTESIAN_POINT('Ctrl Pts',(54.0953653633829,-36.899453296305,-177.174271123402));
#161972=CARTESIAN_POINT('Ctrl Pts',(54.1095973246742,-36.8829800720087,
-177.154942035402));
#161973=CARTESIAN_POINT('Ctrl Pts',(54.1223628927005,-36.8681384062243,
-177.134539220605));
#161974=CARTESIAN_POINT('Ctrl Pts',(54.133662067462,-36.8550100974057,-177.113357603712));
#161975=CARTESIAN_POINT('Ctrl Pts',(54.1452128022232,-36.8415895055282,
-177.091704408349));
#161976=CARTESIAN_POINT('Ctrl Pts',(54.1552311225709,-36.8299592999462,
-177.069237960316));
#161977=CARTESIAN_POINT('Ctrl Pts',(54.1637170285051,-36.8201524333186,
-177.046266573481));
#161978=CARTESIAN_POINT('Ctrl Pts',(54.1723062109049,-36.8102262136684,
-177.023015616773));
#161979=CARTESIAN_POINT('Ctrl Pts',(54.1793254518669,-36.8021676798368,
-176.999247911822));
#161980=CARTESIAN_POINT('Ctrl Pts',(54.1847747513913,-36.7959591590977,
-176.975267376995));
#161981=CARTESIAN_POINT('Ctrl Pts',(54.1903346383764,-36.7896246433495,
-176.95080018394));
#161982=CARTESIAN_POINT('Ctrl Pts',(54.1942602169326,-36.785215650759,-176.926111964466));
#161983=CARTESIAN_POINT('Ctrl Pts',(54.1965514870599,-36.7826646057738,
-176.901500807525));
#161984=CARTESIAN_POINT('Ctrl Pts',(54.1981576461862,-36.7808763468795,
-176.884248614578));
#161985=CARTESIAN_POINT('Ctrl Pts',(54.1989607257493,-36.78000002,-176.867033759598));
#161986=CARTESIAN_POINT('Ctrl Pts',(54.1989607257493,-36.78000002,-176.84995));
#161987=CARTESIAN_POINT('Ctrl Pts',(53.7396474992599,-36.0824364606782,
-176.84995));
#161988=CARTESIAN_POINT('Ctrl Pts',(53.7396474962954,-36.0824364675704,
-176.886929243848));
#161989=CARTESIAN_POINT('Ctrl Pts',(53.7387474700292,-36.084532659728,-176.923734373979));
#161990=CARTESIAN_POINT('Ctrl Pts',(53.7370043459075,-36.0885863209691,
-176.960178957691));
#161991=CARTESIAN_POINT('Ctrl Pts',(53.7352184275947,-36.0927395007422,
-176.997518266259));
#161992=CARTESIAN_POINT('Ctrl Pts',(53.7325474396826,-36.0989476220766,
-177.034480202452));
#161993=CARTESIAN_POINT('Ctrl Pts',(53.7290307937802,-36.1071124473777,
-177.070872685113));
#161994=CARTESIAN_POINT('Ctrl Pts',(53.7254987744607,-36.11531296614,-177.107424261645));
#161995=CARTESIAN_POINT('Ctrl Pts',(53.721113562465,-36.1254876499988,-177.143402563609));
#161996=CARTESIAN_POINT('Ctrl Pts',(53.7158949175063,-36.1375837241688,
-177.178604159827));
#161997=CARTESIAN_POINT('Ctrl Pts',(53.712488356777,-36.1454796457293,-177.201582610408));
#161998=CARTESIAN_POINT('Ctrl Pts',(53.7087262603451,-36.1541952209923,
-177.224229886336));
#161999=CARTESIAN_POINT('Ctrl Pts',(53.7046098856868,-36.1637255131277,
-177.246483747673));
#162000=CARTESIAN_POINT('Ctrl Pts',(53.7045192628111,-36.1639353245641,
-177.246973671229));
#162001=CARTESIAN_POINT('Ctrl Pts',(53.7044284725267,-36.1641455209115,
-177.247463380496));
#162002=CARTESIAN_POINT('Ctrl Pts',(53.7043375149313,-36.1643561019227,
-177.247952874551));
#162003=CARTESIAN_POINT('Ctrl Pts',(53.6892733519024,-36.1992319874284,
-177.329021620976));
#162004=CARTESIAN_POINT('Ctrl Pts',(53.6695548792007,-36.2447904442859,
-177.40484536344));
#162005=CARTESIAN_POINT('Ctrl Pts',(53.6462229782969,-36.2984391069866,
-177.472877385971));
#162006=CARTESIAN_POINT('Ctrl Pts',(53.6342065867359,-36.3260692319555,
-177.507915226427));
#162007=CARTESIAN_POINT('Ctrl Pts',(53.6212319843108,-36.3558446669907,
-177.540885760619));
#162008=CARTESIAN_POINT('Ctrl Pts',(53.6074429005481,-36.3874074842064,
-177.571437587764));
#162009=CARTESIAN_POINT('Ctrl Pts',(53.6072249340652,-36.3879064032337,
-177.571920525892));
#162010=CARTESIAN_POINT('Ctrl Pts',(53.6070067635404,-36.3884057700779,
-177.572402861668));
#162011=CARTESIAN_POINT('Ctrl Pts',(53.6067883895477,-36.3889055833105,
-177.572884593669));
#162012=CARTESIAN_POINT('Ctrl Pts',(53.5821747509553,-36.4452411483475,
-177.627182164609));
#162013=CARTESIAN_POINT('Ctrl Pts',(53.5548118941676,-36.5076136010272,
-177.674313675416));
#162014=CARTESIAN_POINT('Ctrl Pts',(53.5255575781486,-36.573947440762,-177.713411209492));
#162015=CARTESIAN_POINT('Ctrl Pts',(53.5065780536929,-36.6169833036638,
-177.738776786444));
#162016=CARTESIAN_POINT('Ctrl Pts',(53.4868028977424,-36.6616853915005,
-177.760761117544));
#162017=CARTESIAN_POINT('Ctrl Pts',(53.4664703600909,-36.7074778455205,
-177.779132991661));
#162018=CARTESIAN_POINT('Ctrl Pts',(53.4662816165212,-36.7079029292647,
-177.779303534716));
#162019=CARTESIAN_POINT('Ctrl Pts',(53.4660928305315,-36.7083280943329,
-177.779473761639));
#162020=CARTESIAN_POINT('Ctrl Pts',(53.4659040022552,-36.7087533403953,
-177.77964367236));
#162021=CARTESIAN_POINT('Ctrl Pts',(53.4491838139251,-36.7464076281518,
-177.794688766856));
#162022=CARTESIAN_POINT('Ctrl Pts',(53.4320805422693,-36.7848119006859,
-177.807311664152));
#162023=CARTESIAN_POINT('Ctrl Pts',(53.4146874063871,-36.8237527438973,
-177.817537516946));
#162024=CARTESIAN_POINT('Ctrl Pts',(53.3964494296166,-36.8645850698631,
-177.828260072497));
#162025=CARTESIAN_POINT('Ctrl Pts',(53.3778922436239,-36.9060085268254,
-177.836347616446));
#162026=CARTESIAN_POINT('Ctrl Pts',(53.3591168326373,-36.9477888085124,
-177.841770056554));
#162027=CARTESIAN_POINT('Ctrl Pts',(53.341462719104,-36.9870739052212,-177.846868659901));
#162028=CARTESIAN_POINT('Ctrl Pts',(53.3236152017301,-37.0266755174965,
-177.84961057998));
#162029=CARTESIAN_POINT('Ctrl Pts',(53.3056598276503,-37.0663926738597,
-177.849920463284));
#162030=CARTESIAN_POINT('Ctrl Pts',(53.3045193956943,-37.0689153010195,
-177.84994014546));
#162031=CARTESIAN_POINT('Ctrl Pts',(53.3033785305219,-37.0714383891502,
-177.84994999975));
#162032=CARTESIAN_POINT('Ctrl Pts',(53.3022372549337,-37.073961884407,-177.84995));
#162033=CARTESIAN_POINT('Origin',(0.,-12.9675000200281,-171.871644662643));
#162034=CARTESIAN_POINT('',(55.8171229357418,-30.4803178166104,-171.871644662643));
#162035=CARTESIAN_POINT('',(53.7396474992599,-36.0824364606782,-171.871644662643));
#162036=CARTESIAN_POINT('Origin',(0.,-12.9675000200281,-171.871644662643));
#162037=CARTESIAN_POINT('Origin',(54.4948546080238,-30.6573850072952,-171.918810387206));
#162038=CARTESIAN_POINT('Origin',(52.5054720186909,-36.2860506553486,-171.88554415973));
#162039=CARTESIAN_POINT('Ctrl Pts',(56.1493945347971,-29.3837986277054,
-177.844785936526));
#162040=CARTESIAN_POINT('Ctrl Pts',(56.1342142259205,-29.434121619597,-177.331871678519));
#162041=CARTESIAN_POINT('Ctrl Pts',(56.6292894962144,-29.5770787035811,
-177.347150262834));
#162042=CARTESIAN_POINT('Ctrl Pts',(56.1018775093323,-29.5463985702924,
-177.862162411574));
#162043=CARTESIAN_POINT('Ctrl Pts',(56.1107577442959,-29.5139684054722,
-177.363880182749));
#162044=CARTESIAN_POINT('Ctrl Pts',(56.5813906191514,-29.6590318360781,
-177.355839748236));
#162045=CARTESIAN_POINT('Ctrl Pts',(56.0531240578036,-29.7103292972412,
-177.838935726109));
#162046=CARTESIAN_POINT('Ctrl Pts',(56.0827340742419,-29.6092564207282,
-177.376045780878));
#162047=CARTESIAN_POINT('Ctrl Pts',(56.5322373018424,-29.741669930829,-177.344237126135));
#162048=CARTESIAN_POINT('Ctrl Pts',(55.9715766151803,-29.9806728083875,
-177.728264152115));
#162049=CARTESIAN_POINT('Ctrl Pts',(56.0322849866008,-29.7793916826648,
-177.345524396139));
#162050=CARTESIAN_POINT('Ctrl Pts',(56.4500227583409,-29.8779487295679,
-177.288930648015));
#162051=CARTESIAN_POINT('Ctrl Pts',(55.9382308891443,-30.08981673834,-177.656430226304));
#162052=CARTESIAN_POINT('Ctrl Pts',(56.0104065995869,-29.8527129786242,
-177.315401802148));
#162053=CARTESIAN_POINT('Ctrl Pts',(56.4164036466448,-29.9329688836733,
-177.253030654974));
#162054=CARTESIAN_POINT('Ctrl Pts',(55.8448807512244,-30.3929945255238,
-177.357276649046));
#162055=CARTESIAN_POINT('Ctrl Pts',(55.9486579283204,-30.0584540429376,
-177.165590247966));
#162056=CARTESIAN_POINT('Ctrl Pts',(56.3222892817487,-30.0858012522341,
-177.10352016636));
#162057=CARTESIAN_POINT('Ctrl Pts',(55.8076346494222,-30.5102974021064,
-177.049065942077));
#162058=CARTESIAN_POINT('Ctrl Pts',(55.9196838433792,-30.1531627459377,
-176.973586313919));
#162059=CARTESIAN_POINT('Ctrl Pts',(56.2847345577538,-30.1449403478704,
-176.949470753));
#162060=CARTESIAN_POINT('Ctrl Pts',(55.8190628544783,-30.4741856133569,
-176.737644210045));
#162061=CARTESIAN_POINT('Ctrl Pts',(55.928299612176,-30.1249513476889,-176.780220154851));
#162062=CARTESIAN_POINT('Ctrl Pts',(56.2962571325131,-30.1267348532474,
-176.793818000512));
#162063=CARTESIAN_POINT('',(56.1185967245324,-29.4887923928816,-177.84995));
#162064=CARTESIAN_POINT('Origin',(56.5982428503831,-29.63000002,-177.84995));
#162065=CARTESIAN_POINT('',(56.294192362543,-30.13000002,-176.84995));
#162066=CARTESIAN_POINT('Ctrl Pts',(56.294192362543,-30.1300000200003,-176.84995));
#162067=CARTESIAN_POINT('Ctrl Pts',(56.294192362543,-30.1300000200003,-176.872532726662));
#162068=CARTESIAN_POINT('Ctrl Pts',(56.2951871195896,-30.128424325105,-176.895415122225));
#162069=CARTESIAN_POINT('Ctrl Pts',(56.2972200545588,-30.1251924179988,
-176.918380988318));
#162070=CARTESIAN_POINT('Ctrl Pts',(56.2992533574375,-30.1219599259996,
-176.941351010649));
#162071=CARTESIAN_POINT('Ctrl Pts',(56.3023252550559,-30.1170705541272,
-176.96440447796));
#162072=CARTESIAN_POINT('Ctrl Pts',(56.3064575683391,-30.1104754876797,
-176.987289624132));
#162073=CARTESIAN_POINT('Ctrl Pts',(56.3098470935837,-30.1050658919688,
-177.006061139107));
#162074=CARTESIAN_POINT('Ctrl Pts',(56.3139496794318,-30.0985092698674,
-177.024718724667));
#162075=CARTESIAN_POINT('Ctrl Pts',(56.3187663016207,-30.0907949872297,
-177.043106194985));
#162076=CARTESIAN_POINT('Ctrl Pts',(56.3247125232521,-30.0812715426887,
-177.065805914718));
#162077=CARTESIAN_POINT('Ctrl Pts',(56.3317495940632,-30.0699796808652,
-177.088105999951));
#162078=CARTESIAN_POINT('Ctrl Pts',(56.339872577453,-30.0569073841108,-177.109701679162));
#162079=CARTESIAN_POINT('Ctrl Pts',(56.3471147754336,-30.0452525331019,
-177.128955711438));
#162080=CARTESIAN_POINT('Ctrl Pts',(56.3552202898462,-30.0321821766178,
-177.147649859116));
#162081=CARTESIAN_POINT('Ctrl Pts',(56.3641742816089,-30.017703673564,-177.165535027629));
#162082=CARTESIAN_POINT('Ctrl Pts',(56.3713982853061,-30.006022541577,-177.179964628067));
#162083=CARTESIAN_POINT('Ctrl Pts',(56.379174697935,-29.9934245779848,-177.193867303819));
#162084=CARTESIAN_POINT('Ctrl Pts',(56.3874868256334,-29.9799269208526,
-177.207093049855));
#162085=CARTESIAN_POINT('Ctrl Pts',(56.3875437244285,-29.9798345256854,
-177.207183583716));
#162086=CARTESIAN_POINT('Ctrl Pts',(56.387601036394,-29.9797414581918,-177.207274703301));
#162087=CARTESIAN_POINT('Ctrl Pts',(56.3876587294906,-29.9796477703371,
-177.207366354808));
#162088=CARTESIAN_POINT('Ctrl Pts',(56.3889136919176,-29.9776098360883,
-177.209359993644));
#162089=CARTESIAN_POINT('Ctrl Pts',(56.3903497458509,-29.9752768610671,
-177.211601751091));
#162090=CARTESIAN_POINT('Ctrl Pts',(56.3916257120584,-29.9732030439594,
-177.21355908278));
#162091=CARTESIAN_POINT('Ctrl Pts',(56.3923646670942,-29.9720020265766,
-177.214692639532));
#162092=CARTESIAN_POINT('Ctrl Pts',(56.3930494838134,-29.9708886927357,
-177.215731700275));
#162093=CARTESIAN_POINT('Ctrl Pts',(56.3936111551582,-29.9699753935331,
-177.216578542608));
#162094=CARTESIAN_POINT('Ctrl Pts',(56.4016177287422,-29.9569563970344,
-177.228650202519));
#162095=CARTESIAN_POINT('Ctrl Pts',(56.4103290610794,-29.9427602351245,
-177.240522400568));
#162096=CARTESIAN_POINT('Ctrl Pts',(56.4197694089464,-29.927327989156,-177.251935492811));
#162097=CARTESIAN_POINT('Ctrl Pts',(56.4251958207122,-29.9184573710099,
-177.258495858902));
#162098=CARTESIAN_POINT('Ctrl Pts',(56.4308627050949,-29.9091789043299,
-177.264903978388));
#162099=CARTESIAN_POINT('Ctrl Pts',(56.4367709939623,-29.8994866145252,
-177.271105875826));
#162100=CARTESIAN_POINT('Ctrl Pts',(56.4448644739841,-29.8862096140839,
-177.279601556072));
#162101=CARTESIAN_POINT('Ctrl Pts',(56.4533986337169,-29.8721528086074,
-177.287712267273));
#162102=CARTESIAN_POINT('Ctrl Pts',(56.4623751203678,-29.8573176056849,
-177.295286194668));
#162103=CARTESIAN_POINT('Ctrl Pts',(56.4668633636933,-29.8499000042236,
-177.299073158366));
#162104=CARTESIAN_POINT('Ctrl Pts',(56.4714629450669,-29.8422883156734,
-177.302725612065));
#162105=CARTESIAN_POINT('Ctrl Pts',(56.4761738644651,-29.8344848904029,
-177.306223351956));
#162106=CARTESIAN_POINT('Ctrl Pts',(56.4785293241642,-29.8305831777676,
-177.307972221902));
#162107=CARTESIAN_POINT('Ctrl Pts',(56.4809126183669,-29.8266335308248,
-177.309682411394));
#162108=CARTESIAN_POINT('Ctrl Pts',(56.4833237470588,-29.822636425974,-177.311351308538));
#162109=CARTESIAN_POINT('Ctrl Pts',(56.48425029345,-29.8211004220737,-177.311992630849));
#162110=CARTESIAN_POINT('Ctrl Pts',(56.4851808230756,-29.8195576151434,
-177.312627772066));
#162111=CARTESIAN_POINT('Ctrl Pts',(56.4861156809213,-29.8180074786435,
-177.313256809317));
#162112=CARTESIAN_POINT('Ctrl Pts',(56.4863972017675,-29.8175406742613,
-177.313446236083));
#162113=CARTESIAN_POINT('Ctrl Pts',(56.4866790769756,-29.8170732678944,
-177.313635087301));
#162114=CARTESIAN_POINT('Ctrl Pts',(56.4869613159624,-29.8166052453073,
-177.313823365211));
#162115=CARTESIAN_POINT('Ctrl Pts',(56.4878096716068,-29.8151984601995,
-177.314389292088));
#162116=CARTESIAN_POINT('Ctrl Pts',(56.4890156263261,-29.8131986777992,
-177.315181623139));
#162117=CARTESIAN_POINT('Ctrl Pts',(56.4898401272641,-29.8118311447542,
-177.315715538206));
#162118=CARTESIAN_POINT('Ctrl Pts',(56.4902008176112,-29.8112328968372,
-177.315949107389));
#162119=CARTESIAN_POINT('Ctrl Pts',(56.490488387549,-29.8107558902657,-177.316133993143));
#162120=CARTESIAN_POINT('Ctrl Pts',(56.4906406366203,-29.8105033735255,
-177.316231754416));
#162121=CARTESIAN_POINT('Ctrl Pts',(56.4936938884552,-29.805439321616,-177.318192290436));
#162122=CARTESIAN_POINT('Ctrl Pts',(56.4974503833496,-29.7992068257096,
-177.320515037228));
#162123=CARTESIAN_POINT('Ctrl Pts',(56.501924074846,-29.7917729201856,-177.323057554814));
#162124=CARTESIAN_POINT('Ctrl Pts',(56.5063933256274,-29.7843463937703,
-177.325597548624));
#162125=CARTESIAN_POINT('Ctrl Pts',(56.5115787181557,-29.7757202500415,
-177.328356894483));
#162126=CARTESIAN_POINT('Ctrl Pts',(56.517493697644,-29.7658589234036,-177.331141834804));
#162127=CARTESIAN_POINT('Ctrl Pts',(56.5232708007539,-29.7562274612994,
-177.33386185901));
#162128=CARTESIAN_POINT('Ctrl Pts',(56.5297442839822,-29.7454170581434,
-177.336606151603));
#162129=CARTESIAN_POINT('Ctrl Pts',(56.5369204854749,-29.733401340339,-177.339146059258));
#162130=CARTESIAN_POINT('Ctrl Pts',(56.5439111552341,-29.7216962739225,
-177.341620300771));
#162131=CARTESIAN_POINT('Ctrl Pts',(56.5515690870145,-29.7088467394085,
-177.34390045058));
#162132=CARTESIAN_POINT('Ctrl Pts',(56.5598882273037,-29.6948446285046,
-177.345731013883));
#162133=CARTESIAN_POINT('Ctrl Pts',(56.5678117360862,-29.6815084128786,
-177.347474521494));
#162134=CARTESIAN_POINT('Ctrl Pts',(56.5763353622145,-29.6671261312445,
-177.348809934402));
#162135=CARTESIAN_POINT('Ctrl Pts',(56.5854379174801,-29.6517140428296,
-177.34947899318));
#162136=CARTESIAN_POINT('Ctrl Pts',(56.5895873306717,-29.6446884196817,
-177.349783984607));
#162137=CARTESIAN_POINT('Ctrl Pts',(56.5938567934851,-29.6374491756204,
-177.34995));
#162138=CARTESIAN_POINT('Ctrl Pts',(56.598242850383,-29.6300000200001,-177.34995));
#162139=CARTESIAN_POINT('',(55.8171229357418,-30.4803178166104,-176.84995));
#162140=CARTESIAN_POINT('Origin',(56.294192362543,-30.63000002,-176.84995));
#162141=CARTESIAN_POINT('Ctrl Pts',(56.1185967245324,-29.4887923928816,
-177.84995));
#162142=CARTESIAN_POINT('Ctrl Pts',(56.0804686085136,-29.6183038329331,
-177.84995));
#162143=CARTESIAN_POINT('Ctrl Pts',(56.0435105516164,-29.7422083237505,
-177.825637538525));
#162144=CARTESIAN_POINT('Ctrl Pts',(55.9706438254141,-29.983755289409,-177.726373245353));
#162145=CARTESIAN_POINT('Ctrl Pts',(55.9379975051363,-30.0905814889907,
-177.655514525474));
#162146=CARTESIAN_POINT('Ctrl Pts',(55.880677894362,-30.276726517591,-177.471099911401));
#162147=CARTESIAN_POINT('Ctrl Pts',(55.8583243128169,-30.3485429953493,
-177.364626418289));
#162148=CARTESIAN_POINT('Ctrl Pts',(55.8254079947302,-30.4539768569356,
-177.113213750895));
#162149=CARTESIAN_POINT('Ctrl Pts',(55.8171229357418,-30.4803178166104,
-176.983557056031));
#162150=CARTESIAN_POINT('Ctrl Pts',(55.8171229357418,-30.4803178166104,
-176.84995));
#162151=CARTESIAN_POINT('Origin',(0.,-12.9675000200281,-177.84995));
#162152=CARTESIAN_POINT('',(56.262175563026,-28.9930296810172,-177.84995));
#162153=CARTESIAN_POINT('Origin',(56.7430488584365,-29.13000002,-177.84995));
#162154=CARTESIAN_POINT('Origin',(0.,-12.9675000200281,-177.84995));
#162155=CARTESIAN_POINT('Ctrl Pts',(56.7430488584365,-29.13000002,-177.34995));
#162156=CARTESIAN_POINT('Ctrl Pts',(56.262175563026,-28.9930296810172,-177.34995));
#162157=CARTESIAN_POINT('Ctrl Pts',(56.262175563026,-28.9930296810172,-177.84995));
#162158=CARTESIAN_POINT('Ctrl Pts',(56.799051006553,-29.0316942919675,-177.34995));
#162159=CARTESIAN_POINT('Ctrl Pts',(56.2928119947094,-28.8854717787751,
-177.322103214377));
#162160=CARTESIAN_POINT('Ctrl Pts',(56.3176963010821,-28.7981083537361,
-177.849949971516));
#162161=CARTESIAN_POINT('Ctrl Pts',(56.8539225877547,-28.933239542368,-177.320220947896));
#162162=CARTESIAN_POINT('Ctrl Pts',(56.3169386704035,-28.8006430758332,
-177.261063208671));
#162163=CARTESIAN_POINT('Ctrl Pts',(56.3721096851181,-28.6028436438479,
-177.790491903933));
#162164=CARTESIAN_POINT('Ctrl Pts',(56.9443314005494,-28.7684056938368,
-177.209281314082));
#162165=CARTESIAN_POINT('Ctrl Pts',(56.3506671101773,-28.684579593959,-177.121256964593));
#162166=CARTESIAN_POINT('Ctrl Pts',(56.4617523202342,-28.2759697513382,
-177.568612620023));
#162167=CARTESIAN_POINT('Ctrl Pts',(56.9801582405499,-28.7016493747432,
-177.12717563931));
#162168=CARTESIAN_POINT('Ctrl Pts',(56.3596918685657,-28.6555519736166,
-177.043271150691));
#162169=CARTESIAN_POINT('Ctrl Pts',(56.4972682976465,-28.1436156829388,
-177.404470992826));
#162170=CARTESIAN_POINT('Ctrl Pts',(57.,-28.664523125878,-177.032518510534));
#162171=CARTESIAN_POINT('Ctrl Pts',(56.364125065416,-28.6418687251214,-176.974758823107));
#162172=CARTESIAN_POINT('Ctrl Pts',(56.5169491525423,-28.0699653316567,
-177.215087021068));
#162173=CARTESIAN_POINT('',(56.5169491525423,-28.0699653316567,-177.215087021068));
#162174=CARTESIAN_POINT('Origin',(57.,-28.199046231756,-177.215087021068));
#162175=CARTESIAN_POINT('Ctrl Pts',(56.5169491525423,-28.0699653316567,
-177.215087021068));
#162176=CARTESIAN_POINT('Ctrl Pts',(56.5114199834419,-28.0906567725875,
-177.26829284014));
#162177=CARTESIAN_POINT('Ctrl Pts',(56.5046490590763,-28.1159513561152,
-177.319440198101));
#162178=CARTESIAN_POINT('Ctrl Pts',(56.4967764105797,-28.145254791308,-177.367985903784));
#162179=CARTESIAN_POINT('Ctrl Pts',(56.488835970741,-28.1748105582542,-177.416949636328));
#162180=CARTESIAN_POINT('Ctrl Pts',(56.4797745088228,-28.2084455503732,
-177.46326787819));
#162181=CARTESIAN_POINT('Ctrl Pts',(56.4697238291809,-28.2455931588451,
-177.506354841674));
#162182=CARTESIAN_POINT('Ctrl Pts',(56.4600615204675,-28.281305336907,-177.547776870584));
#162183=CARTESIAN_POINT('Ctrl Pts',(56.4494846922707,-28.3202650328622,
-177.586213261633));
#162184=CARTESIAN_POINT('Ctrl Pts',(56.4381034255685,-28.3619923283887,
-177.621103904538));
#162185=CARTESIAN_POINT('Ctrl Pts',(56.4313704755802,-28.3866774360556,
-177.641744573093));
#162186=CARTESIAN_POINT('Ctrl Pts',(56.4243558827027,-28.4123314859347,
-177.661143532174));
#162187=CARTESIAN_POINT('Ctrl Pts',(56.4170817736066,-28.438856914084,-177.679176296163));
#162188=CARTESIAN_POINT('Ctrl Pts',(56.4170314275401,-28.4390405037103,
-177.679301105775));
#162189=CARTESIAN_POINT('Ctrl Pts',(56.4169810706746,-28.4392241291221,
-177.679425845849));
#162190=CARTESIAN_POINT('Ctrl Pts',(56.4169307030184,-28.4394077902846,
-177.679550516358));
#162191=CARTESIAN_POINT('Ctrl Pts',(56.4068381994777,-28.4762092036084,
-177.70453157867));
#162192=CARTESIAN_POINT('Ctrl Pts',(56.3962987764838,-28.5144807857784,
-177.726809957994));
#162193=CARTESIAN_POINT('Ctrl Pts',(56.3853954829433,-28.5539082918042,
-177.746384040078));
#162194=CARTESIAN_POINT('Ctrl Pts',(56.3741127545824,-28.5947078757818,
-177.766639300587));
#162195=CARTESIAN_POINT('Ctrl Pts',(56.3624401562768,-28.6367461405691,
-177.783999255699));
#162196=CARTESIAN_POINT('Ctrl Pts',(56.3504605117084,-28.6797057531804,
-177.798417329991));
#162197=CARTESIAN_POINT('Ctrl Pts',(56.3384882188013,-28.7226390023617,
-177.812826556209));
#162198=CARTESIAN_POINT('Ctrl Pts',(56.3262089639832,-28.7664935773127,
-177.824297783191));
#162199=CARTESIAN_POINT('Ctrl Pts',(56.3137004593873,-28.8109674781278,
-177.832735185289));
#162200=CARTESIAN_POINT('Ctrl Pts',(56.301553921008,-28.8541544105859,-177.840928429144));
#162201=CARTESIAN_POINT('Ctrl Pts',(56.2891909417748,-28.897926340654,-177.846260934398));
#162202=CARTESIAN_POINT('Ctrl Pts',(56.2766821207918,-28.942005178833,-177.848596484849));
#162203=CARTESIAN_POINT('Ctrl Pts',(56.2718668221819,-28.9589734261602,
-177.849495560218));
#162204=CARTESIAN_POINT('Ctrl Pts',(56.2670299262029,-28.9759870597071,
-177.84994999751));
#162205=CARTESIAN_POINT('Ctrl Pts',(56.262175563026,-28.9930296810172,-177.84995));
#162206=CARTESIAN_POINT('Ctrl Pts',(56.5350158381137,-28.0021946997704,
-176.811903784796));
#162207=CARTESIAN_POINT('Ctrl Pts',(56.3679651457268,-28.6303533640722,
-176.837499657378));
#162208=CARTESIAN_POINT('Ctrl Pts',(57.0184194087067,-28.6303484782574,
-176.830899202224));
#162209=CARTESIAN_POINT('Ctrl Pts',(56.5364806901874,-27.9966690056784,
-176.964298400169));
#162210=CARTESIAN_POINT('Ctrl Pts',(56.3684339309491,-28.6288435574528,
-176.887126065441));
#162211=CARTESIAN_POINT('Ctrl Pts',(57.019316568372,-28.6275595516668,-176.907060450972));
#162212=CARTESIAN_POINT('Ctrl Pts',(56.5291525614316,-28.0243358857953,
-177.110977601639));
#162213=CARTESIAN_POINT('Ctrl Pts',(56.367312788345,-28.6317888732642,-176.934996710032));
#162214=CARTESIAN_POINT('Ctrl Pts',(57.0114138500124,-28.6415256904292,
-176.980508103715));
#162215=CARTESIAN_POINT('Ctrl Pts',(56.5131231233502,-28.0842779073417,
-177.250001316319));
#162216=CARTESIAN_POINT('Ctrl Pts',(56.3631318544866,-28.6450072835911,
-176.98772630256));
#162217=CARTESIAN_POINT('Ctrl Pts',(56.9964657809338,-28.6717398279222,
-177.049971678832));
#162218=CARTESIAN_POINT('',(56.5351989170821,-28.0015042572884,-176.849882244789));
#162219=CARTESIAN_POINT('',(57.0184057454332,-28.63000002,-176.849882244789));
#162220=CARTESIAN_POINT('Origin',(57.0184057454332,-28.13000002,-176.849882244789));
#162221=CARTESIAN_POINT('Ctrl Pts',(57.,-28.6645231258781,-177.032518510534));
#162222=CARTESIAN_POINT('Ctrl Pts',(57.0039800912305,-28.6565690730968,
-177.012238847993));
#162223=CARTESIAN_POINT('Ctrl Pts',(57.0072713934122,-28.6501272490681,
-176.991904897329));
#162224=CARTESIAN_POINT('Ctrl Pts',(57.0099157186547,-28.6450662877334,
-176.971747813479));
#162225=CARTESIAN_POINT('Ctrl Pts',(57.0126656382054,-28.6398032299614,
-176.950785808475));
#162226=CARTESIAN_POINT('Ctrl Pts',(57.0147161314663,-28.636032896984,-176.930015335143));
#162227=CARTESIAN_POINT('Ctrl Pts',(57.0161153714143,-28.6335822714496,
-176.909643884951));
#162228=CARTESIAN_POINT('Ctrl Pts',(57.0175146113622,-28.6311316459152,
-176.889272434758));
#162229=CARTESIAN_POINT('Ctrl Pts',(57.018262799339,-28.63000002,-176.869299784457));
#162230=CARTESIAN_POINT('Ctrl Pts',(57.0184057454332,-28.63000002,-176.849882244789));
#162231=CARTESIAN_POINT('Origin',(55.1126545812022,-33.3251112519863,-176.014041861122));
#162232=CARTESIAN_POINT('Origin',(0.,-12.9675000200281,-171.871644662643));
#162233=CARTESIAN_POINT('',(57.7346476057222,-22.3993856132206,-171.871644662643));
#162234=CARTESIAN_POINT('',(56.5351989170821,-28.0015042572884,-171.871644662643));
#162235=CARTESIAN_POINT('Origin',(0.,-12.9675000200281,-171.871644662643));
#162236=CARTESIAN_POINT('Origin',(56.3007888374198,-22.509667514428,-171.959861518035));
#162237=CARTESIAN_POINT('Origin',(55.1752186158567,-28.1616465678281,-171.933521226257));
#162238=CARTESIAN_POINT('Ctrl Pts',(57.8819282087167,-21.4487963148736,
-177.697497252237));
#162239=CARTESIAN_POINT('Ctrl Pts',(57.8810878095005,-21.4545317502846,
-177.368333266163));
#162240=CARTESIAN_POINT('Ctrl Pts',(58.1799818947148,-21.5006430233977,
-177.238261718413));
#162241=CARTESIAN_POINT('Ctrl Pts',(57.8629489711247,-21.5783230793646,
-177.699822299871));
#162242=CARTESIAN_POINT('Ctrl Pts',(57.868876514339,-21.5377805372773,-177.374493960823));
#162243=CARTESIAN_POINT('Ctrl Pts',(58.1643305096628,-21.5659716479372,
-177.242027715059));
#162244=CARTESIAN_POINT('Ctrl Pts',(57.8432533717849,-21.7094932883126,
-177.67338127456));
#162245=CARTESIAN_POINT('Ctrl Pts',(57.8561193903755,-21.6237742374893,
-177.3594824509));
#162246=CARTESIAN_POINT('Ctrl Pts',(58.1516959167317,-21.6321056009482,
-177.229926261063));
#162247=CARTESIAN_POINT('Ctrl Pts',(57.8068932864249,-21.9467814783138,
-177.56730490578));
#162248=CARTESIAN_POINT('Ctrl Pts',(57.833274341657,-21.7763737806991,-177.289541220421));
#162249=CARTESIAN_POINT('Ctrl Pts',(58.135834617463,-21.751763745641,-177.175847704912));
#162250=CARTESIAN_POINT('Ctrl Pts',(57.7900355525622,-22.0542721190802,
-177.487158575097));
#162251=CARTESIAN_POINT('Ctrl Pts',(57.822969521998,-21.8444848229842,-177.233860492204));
#162252=CARTESIAN_POINT('Ctrl Pts',(58.1325374345936,-21.8059684297317,
-177.133613057603));
#162253=CARTESIAN_POINT('Ctrl Pts',(57.7626304144021,-22.2268825024457,
-177.290851905635));
#162254=CARTESIAN_POINT('Ctrl Pts',(57.8075855468967,-21.9461185785114,
-177.096669117024));
#162255=CARTESIAN_POINT('Ctrl Pts',(58.1379476084663,-21.8930112710375,
-177.027055273752));
#162256=CARTESIAN_POINT('Ctrl Pts',(57.7519076537925,-22.2932204551335,
-177.173672169064));
#162257=CARTESIAN_POINT('Ctrl Pts',(57.8023886323833,-21.9804905067127,
-177.013273949454));
#162258=CARTESIAN_POINT('Ctrl Pts',(58.1467121091855,-21.9264637442851,
-176.962169933093));
#162259=CARTESIAN_POINT('Ctrl Pts',(57.7379487783882,-22.3792570371924,
-176.923566462093));
#162260=CARTESIAN_POINT('Ctrl Pts',(57.7982009932088,-22.0095200736329,
-176.838338250264));
#162261=CARTESIAN_POINT('Ctrl Pts',(58.1775901524469,-21.9698497118448,
-176.818815489061));
#162262=CARTESIAN_POINT('Ctrl Pts',(57.7346476044917,-22.3993856207533,
-176.79021969384));
#162263=CARTESIAN_POINT('Ctrl Pts',(57.7993206334297,-22.0035077749888,
-176.744992431703));
#162264=CARTESIAN_POINT('Ctrl Pts',(58.1997838724148,-21.98000002,-176.740111438881));
#162265=CARTESIAN_POINT('Ctrl Pts',(57.7346476057222,-22.3993856132206,
-176.657965001855));
#162266=CARTESIAN_POINT('Ctrl Pts',(57.8031610044997,-21.98000002,-176.657965001855));
#162267=CARTESIAN_POINT('Ctrl Pts',(58.2281061322669,-21.98000002,-176.657965001855));
#162268=CARTESIAN_POINT('',(57.8819282087167,-21.4487963148736,-177.697497252237));
#162269=CARTESIAN_POINT('Origin',(58.376645543834,-21.5212860267954,-177.697497252237));
#162270=CARTESIAN_POINT('',(58.2281061322626,-21.9800000072249,-176.657965001847));
#162271=CARTESIAN_POINT('Ctrl Pts',(58.2281061322669,-21.98000002,-176.657965001855));
#162272=CARTESIAN_POINT('Ctrl Pts',(58.2156432050873,-21.98000002,-176.694112706195));
#162273=CARTESIAN_POINT('Ctrl Pts',(58.2044053428825,-21.9780314444789,
-176.729472360225));
#162274=CARTESIAN_POINT('Ctrl Pts',(58.1944420590819,-21.9740340480493,
-176.763689754096));
#162275=CARTESIAN_POINT('Ctrl Pts',(58.1894604171816,-21.9720353498345,
-176.780798451031));
#162276=CARTESIAN_POINT('Ctrl Pts',(58.1847976426165,-21.9695299941169,
-176.797620591924));
#162277=CARTESIAN_POINT('Ctrl Pts',(58.1804606715693,-21.9665165584178,
-176.814106030133));
#162278=CARTESIAN_POINT('Ctrl Pts',(58.1787278993621,-21.9653125850524,
-176.820692541512));
#162279=CARTESIAN_POINT('Ctrl Pts',(58.1771363661171,-21.9640945924079,
-176.826879459107));
#162280=CARTESIAN_POINT('Ctrl Pts',(58.1755739593543,-21.9627918105726,
-176.833082972166));
#162281=CARTESIAN_POINT('Ctrl Pts',(58.17407480742,-21.9615417725191,-176.839035332859));
#162282=CARTESIAN_POINT('Ctrl Pts',(58.1726025352164,-21.9602135784298,
-176.845003047828));
#162283=CARTESIAN_POINT('Ctrl Pts',(58.1710791571693,-21.9587089640121,
-176.851334149985));
#162284=CARTESIAN_POINT('Ctrl Pts',(58.1702164342252,-21.9578568673295,
-176.854919594256));
#162285=CARTESIAN_POINT('Ctrl Pts',(58.1693376867143,-21.9569475664076,
-176.858621235351));
#162286=CARTESIAN_POINT('Ctrl Pts',(58.1684321549172,-21.9559574019423,
-176.862498842424));
#162287=CARTESIAN_POINT('Ctrl Pts',(58.1662308623925,-21.9535503725674,
-176.871925068526));
#162288=CARTESIAN_POINT('Ctrl Pts',(58.1641348742942,-21.9509516579958,
-176.881260355963));
#162289=CARTESIAN_POINT('Ctrl Pts',(58.1621473919756,-21.9481572100565,
-176.890493088755));
#162290=CARTESIAN_POINT('Ctrl Pts',(58.1566032426735,-21.9403620027998,
-176.916248109862));
#162291=CARTESIAN_POINT('Ctrl Pts',(58.1518943927396,-21.9310133708706,
-176.941234732476));
#162292=CARTESIAN_POINT('Ctrl Pts',(58.1480208458896,-21.9201857317733,
-176.965150077762));
#162293=CARTESIAN_POINT('Ctrl Pts',(58.1463352305236,-21.9154739687441,
-176.975557096202));
#162294=CARTESIAN_POINT('Ctrl Pts',(58.1448350754385,-21.9105702566688,
-176.985577584898));
#162295=CARTESIAN_POINT('Ctrl Pts',(58.1434852751035,-21.9054093827837,
-176.995378681003));
#162296=CARTESIAN_POINT('Ctrl Pts',(58.1421472864369,-21.9002936700451,
-177.005094010869));
#162297=CARTESIAN_POINT('Ctrl Pts',(58.1409571143495,-21.8949250790412,
-177.014594131085));
#162298=CARTESIAN_POINT('Ctrl Pts',(58.1399011290586,-21.8892047551052,
-177.024011615046));
#162299=CARTESIAN_POINT('Ctrl Pts',(58.1388806139833,-21.883676575061,-177.033112768667));
#162300=CARTESIAN_POINT('Ctrl Pts',(58.1379854764992,-21.8778197504792,
-177.042137097446));
#162301=CARTESIAN_POINT('Ctrl Pts',(58.1372216369892,-21.8715145130864,
-177.051170949139));
#162302=CARTESIAN_POINT('Ctrl Pts',(58.1370840173307,-21.8703785092458,
-177.052798562753));
#162303=CARTESIAN_POINT('Ctrl Pts',(58.1369507081154,-21.8692278697024,
-177.054426386573));
#162304=CARTESIAN_POINT('Ctrl Pts',(58.1368218087854,-21.8680617875073,
-177.056054789025));
#162305=CARTESIAN_POINT('Ctrl Pts',(58.1361650523263,-21.8621204687019,
-177.064351681087));
#162306=CARTESIAN_POINT('Ctrl Pts',(58.1356363393907,-21.8559283084116,
-177.07245496925));
#162307=CARTESIAN_POINT('Ctrl Pts',(58.1352380015467,-21.8494904929985,
-177.08033537195));
#162308=CARTESIAN_POINT('Ctrl Pts',(58.1344071771017,-21.83606296032,-177.096771749506));
#162309=CARTESIAN_POINT('Ctrl Pts',(58.1341394415401,-21.8215054517519,
-177.112290333485));
#162310=CARTESIAN_POINT('Ctrl Pts',(58.1344181335807,-21.8059909922371,
-177.126663547938));
#162311=CARTESIAN_POINT('Ctrl Pts',(58.1344801685191,-21.8025375798625,
-177.129862926982));
#162312=CARTESIAN_POINT('Ctrl Pts',(58.1345691972595,-21.7990369110223,
-177.133005658565));
#162313=CARTESIAN_POINT('Ctrl Pts',(58.1346849015299,-21.7954911519696,
-177.136089423575));
#162314=CARTESIAN_POINT('Ctrl Pts',(58.1349931881012,-21.7860437055044,
-177.144305916688));
#162315=CARTESIAN_POINT('Ctrl Pts',(58.1354941233143,-21.7761663325933,
-177.152194777092));
#162316=CARTESIAN_POINT('Ctrl Pts',(58.1361828836554,-21.7659911953573,
-177.159618268632));
#162317=CARTESIAN_POINT('Ctrl Pts',(58.1368690686029,-21.7558541047117,
-177.167014002458));
#162318=CARTESIAN_POINT('Ctrl Pts',(58.1377415390541,-21.7454219712837,
-177.173947428276));
#162319=CARTESIAN_POINT('Ctrl Pts',(58.1387787204352,-21.7348510683059,
-177.180324083576));
#162320=CARTESIAN_POINT('Ctrl Pts',(58.1396881507361,-21.7255821982215,
-177.185915317331));
#162321=CARTESIAN_POINT('Ctrl Pts',(58.1407238858634,-21.7162072526313,
-177.19107901569));
#162322=CARTESIAN_POINT('Ctrl Pts',(58.1418621794207,-21.7068430038689,
-177.195781098596));
#162323=CARTESIAN_POINT('Ctrl Pts',(58.142458961938,-21.701933532219,-177.198246298241));
#162324=CARTESIAN_POINT('Ctrl Pts',(58.1430910223037,-21.6969631041976,
-177.200617659317));
#162325=CARTESIAN_POINT('Ctrl Pts',(58.1437581575669,-21.6919348657256,
-177.202889874908));
#162326=CARTESIAN_POINT('Ctrl Pts',(58.1462286069172,-21.6733149408743,
-177.211304050922));
#162327=CARTESIAN_POINT('Ctrl Pts',(58.1491881991552,-21.6538329623342,
-177.218381304938));
#162328=CARTESIAN_POINT('Ctrl Pts',(58.1526065770555,-21.633732508915,-177.223966894812));
#162329=CARTESIAN_POINT('Ctrl Pts',(58.1562202733795,-21.6124835608022,
-177.229871632727));
#162330=CARTESIAN_POINT('Ctrl Pts',(58.1603466629203,-21.5905439782932,
-177.234108763021));
#162331=CARTESIAN_POINT('Ctrl Pts',(58.1649305053795,-21.5682460893206,
-177.236532779346));
#162332=CARTESIAN_POINT('Ctrl Pts',(58.1695143478386,-21.5459482003481,
-177.23895679567));
#162333=CARTESIAN_POINT('Ctrl Pts',(58.1745553917398,-21.5232931578517,
-177.239567429792));
#162334=CARTESIAN_POINT('Ctrl Pts',(58.1799818945846,-21.5006430239411,
-177.238261718445));
#162335=CARTESIAN_POINT('',(57.7346476057222,-22.3993856132206,-176.657965001855));
#162336=CARTESIAN_POINT('Origin',(58.2281061322669,-22.48000002,-176.657965001855));
#162337=CARTESIAN_POINT('Ctrl Pts',(57.8819282087167,-21.4487963148736,
-177.697497252237));
#162338=CARTESIAN_POINT('Ctrl Pts',(57.8765896421257,-21.4852301944857,
-177.698151252249));
#162339=CARTESIAN_POINT('Ctrl Pts',(57.8712308062151,-21.5215461998528,
-177.696528688191));
#162340=CARTESIAN_POINT('Ctrl Pts',(57.8658871784514,-21.5575327106497,
-177.692745867402));
#162341=CARTESIAN_POINT('Ctrl Pts',(57.8604287549616,-21.5942923100331,
-177.688881781285));
#162342=CARTESIAN_POINT('Ctrl Pts',(57.8549860188209,-21.6307092686159,
-177.682763561799));
#162343=CARTESIAN_POINT('Ctrl Pts',(57.849594035819,-21.6665701891048,-177.674461317079));
#162344=CARTESIAN_POINT('Ctrl Pts',(57.8442188129476,-21.7023196415671,
-177.66618487858));
#162345=CARTESIAN_POINT('Ctrl Pts',(57.8388938392211,-21.737517702457,-177.655737740554));
#162346=CARTESIAN_POINT('Ctrl Pts',(57.8336539589831,-21.7719470718026,
-177.643138949619));
#162347=CARTESIAN_POINT('Ctrl Pts',(57.8307658910941,-21.7909235276622,
-177.63619486657));
#162348=CARTESIAN_POINT('Ctrl Pts',(57.8279036918339,-21.8096662565538,
-177.62859626689));
#162349=CARTESIAN_POINT('Ctrl Pts',(57.8250735265724,-21.8281360946975,
-177.620340114691));
#162350=CARTESIAN_POINT('Ctrl Pts',(57.825000507433,-21.8286126222366,-177.62012710341));
#162351=CARTESIAN_POINT('Ctrl Pts',(57.8249275065196,-21.8290889901148,
-177.619913645942));
#162352=CARTESIAN_POINT('Ctrl Pts',(57.8248545239147,-21.8295651979082,
-177.619699742645));
#162353=CARTESIAN_POINT('Ctrl Pts',(57.8134041423538,-21.904278356602,-177.58614004201));
#162354=CARTESIAN_POINT('Ctrl Pts',(57.8024908179688,-21.9744875656816,
-177.541849255809));
#162355=CARTESIAN_POINT('Ctrl Pts',(57.7925715206938,-22.0376966071709,
-177.489169880472));
#162356=CARTESIAN_POINT('Ctrl Pts',(57.7867917707715,-22.0745270844222,
-177.458474801268));
#162357=CARTESIAN_POINT('Ctrl Pts',(57.7813493744923,-22.1089817246111,
-177.424931754292));
#162358=CARTESIAN_POINT('Ctrl Pts',(57.776333363324,-22.1405749184086,-177.389003065334));
#162359=CARTESIAN_POINT('Ctrl Pts',(57.7762581999322,-22.1410483327462,
-177.388464684929));
#162360=CARTESIAN_POINT('Ctrl Pts',(57.7761831269836,-22.141521141353,-177.387925738145));
#162361=CARTESIAN_POINT('Ctrl Pts',(57.7761081445995,-22.1419933437069,
-177.387386226876));
#162362=CARTESIAN_POINT('Ctrl Pts',(57.7675362470193,-22.1959749590559,
-177.325709935871));
#162363=CARTESIAN_POINT('Ctrl Pts',(57.7601479409397,-22.2420339156115,
-177.256653403133));
#162364=CARTESIAN_POINT('Ctrl Pts',(57.754120051989,-22.2794160573152,-177.182965839566));
#162365=CARTESIAN_POINT('Ctrl Pts',(57.7505729125365,-22.3014137534806,
-177.139604048062));
#162366=CARTESIAN_POINT('Ctrl Pts',(57.7474968850881,-22.3204065587762,
-177.094637483872));
#162367=CARTESIAN_POINT('Ctrl Pts',(57.7449284196372,-22.3362374915981,
-177.048618868861));
#162368=CARTESIAN_POINT('Ctrl Pts',(57.7449026192307,-22.3363965143726,
-177.048156608808));
#162369=CARTESIAN_POINT('Ctrl Pts',(57.7448768691533,-22.3365552239542,
-177.047694236815));
#162370=CARTESIAN_POINT('Ctrl Pts',(57.7448511693847,-22.3367136204909,
-177.04723175335));
#162371=CARTESIAN_POINT('Ctrl Pts',(57.7426315058001,-22.3503941726404,
-177.007287514071));
#162372=CARTESIAN_POINT('Ctrl Pts',(57.740792620676,-22.3617057222206,-176.966623027288));
#162373=CARTESIAN_POINT('Ctrl Pts',(57.7393137106679,-22.3707907309251,
-176.925440939058));
#162374=CARTESIAN_POINT('Ctrl Pts',(57.7377438892451,-22.3804342124164,
-176.881727309435));
#162375=CARTESIAN_POINT('Ctrl Pts',(57.7365796223128,-22.3875691725098,
-176.837429305389));
#162376=CARTESIAN_POINT('Ctrl Pts',(57.7358055387825,-22.3923071177908,
-176.792774052489));
#162377=CARTESIAN_POINT('Ctrl Pts',(57.7350314552522,-22.3970450630717,
-176.748118799589));
#162378=CARTESIAN_POINT('Ctrl Pts',(57.7346476057222,-22.3993856132206,
-176.703104836952));
#162379=CARTESIAN_POINT('Ctrl Pts',(57.7346476057222,-22.3993856132206,
-176.657965001855));
#162380=CARTESIAN_POINT('Ctrl Pts',(58.1799818947148,-21.5006430233976,
-177.238261718413));
#162381=CARTESIAN_POINT('Ctrl Pts',(57.8810878095005,-21.4545317502846,
-177.368333266163));
#162382=CARTESIAN_POINT('Ctrl Pts',(57.8819282087167,-21.4487963148739,
-177.697497252237));
#162383=CARTESIAN_POINT('Ctrl Pts',(58.2008748005355,-21.3341357689658,
-177.236799145875));
#162384=CARTESIAN_POINT('Ctrl Pts',(57.9052384907138,-21.2898253143233,
-177.368094235677));
#162385=CARTESIAN_POINT('Ctrl Pts',(57.906096697535,-21.2838546967462,-177.694536471641));
#162386=CARTESIAN_POINT('Ctrl Pts',(58.2211580737071,-21.1675764425398,
-177.235439894836));
#162387=CARTESIAN_POINT('Ctrl Pts',(57.9287492734302,-21.1245836426315,
-177.367866070024));
#162388=CARTESIAN_POINT('Ctrl Pts',(57.9295599753438,-21.1188110827801,
-177.691677811931));
#162389=CARTESIAN_POINT('Ctrl Pts',(58.2408316684984,-21.0009616906551,
-177.234173073119));
#162390=CARTESIAN_POINT('Ctrl Pts',(57.9515978527783,-20.958891271667,-177.367648026607));
#162391=CARTESIAN_POINT('Ctrl Pts',(57.952317989407,-20.9536655363853,-177.688917160843));
#162392=CARTESIAN_POINT('',(57.9523179894071,-20.9536655363849,-177.688917160843));
#162393=CARTESIAN_POINT('Origin',(1.12335876888057,-12.987558319356,-185.751570788792));
#162394=CARTESIAN_POINT('Origin',(58.4476369465814,-21.0219233613115,-177.688917160843));
#162395=CARTESIAN_POINT('Ctrl Pts',(58.0841784519436,-19.9304621405658,
-176.259519378371));
#162396=CARTESIAN_POINT('Ctrl Pts',(58.0105886540739,-20.5442112516041,
-176.323704335026));
#162397=CARTESIAN_POINT('Ctrl Pts',(58.6287087693006,-20.4848108664684,
-176.310034217439));
#162398=CARTESIAN_POINT('Ctrl Pts',(58.0887038582403,-19.8911762730753,
-176.615064002266));
#162399=CARTESIAN_POINT('Ctrl Pts',(58.0268439039754,-20.4108954967624,
-176.520977425154));
#162400=CARTESIAN_POINT('Ctrl Pts',(58.5368873558551,-20.4653641571308,
-176.572149418256));
#162401=CARTESIAN_POINT('Ctrl Pts',(58.0801409030891,-19.9672777568629,
-176.996564457697));
#162402=CARTESIAN_POINT('Ctrl Pts',(58.0299460242795,-20.3808131077243,
-176.814822746134));
#162403=CARTESIAN_POINT('Ctrl Pts',(58.4542388827497,-20.504002186848,-176.810590092819));
#162404=CARTESIAN_POINT('Ctrl Pts',(58.0411746905458,-20.2805473548039,
-177.404658872083));
#162405=CARTESIAN_POINT('Ctrl Pts',(58.0083595382399,-20.5404571645344,
-177.132443882723));
#162406=CARTESIAN_POINT('Ctrl Pts',(58.3544824851918,-20.6619976365417,
-177.058899043469));
#162407=CARTESIAN_POINT('Ctrl Pts',(58.0268899075637,-20.3936565135702,
-177.503861519498));
#162408=CARTESIAN_POINT('Ctrl Pts',(57.9996775864985,-20.6054116810074,
-177.21060993225));
#162409=CARTESIAN_POINT('Ctrl Pts',(58.3280900169859,-20.7190107839085,
-177.1181514199));
#162410=CARTESIAN_POINT('Ctrl Pts',(57.9855747517757,-20.7107497140498,
-177.674988342283));
#162411=CARTESIAN_POINT('Ctrl Pts',(57.9736028397066,-20.7986778387088,
-177.34726402373));
#162412=CARTESIAN_POINT('Ctrl Pts',(58.2701722703655,-20.8787887637927,
-177.221713795304));
#162413=CARTESIAN_POINT('Ctrl Pts',(57.9575440958208,-20.9188769733095,
-177.71328609301));
#162414=CARTESIAN_POINT('Ctrl Pts',(57.9549784509418,-20.9354291942737,
-177.38433863335));
#162415=CARTESIAN_POINT('Ctrl Pts',(58.243188774626,-20.9835514316547,-177.246401767638));
#162416=CARTESIAN_POINT('Ctrl Pts',(57.9264125504997,-21.1393961655747,
-177.673640454257));
#162417=CARTESIAN_POINT('Ctrl Pts',(57.9348086722084,-21.0798758079841,
-177.36100914447));
#162418=CARTESIAN_POINT('Ctrl Pts',(58.2231123045576,-21.0947564262227,
-177.22865633177));
#162419=CARTESIAN_POINT('',(58.0853233553176,-19.9205720538986,-176.438901946458));
#162420=CARTESIAN_POINT('Ctrl Pts',(58.0853233553176,-19.9205720538985,
-176.438901946458));
#162421=CARTESIAN_POINT('Ctrl Pts',(58.0853233553176,-19.9205720538985,
-176.480417501913));
#162422=CARTESIAN_POINT('Ctrl Pts',(58.0851376391211,-19.9221605933746,
-176.521365344842));
#162423=CARTESIAN_POINT('Ctrl Pts',(58.0847722160181,-19.9252576141166,
-176.561736215164));
#162424=CARTESIAN_POINT('Ctrl Pts',(58.0844515754477,-19.9279750955489,
-176.597159642919));
#162425=CARTESIAN_POINT('Ctrl Pts',(58.08399251563,-19.9318546494952,-176.632139799579));
#162426=CARTESIAN_POINT('Ctrl Pts',(58.0833958455804,-19.9368720425748,
-176.666683991487));
#162427=CARTESIAN_POINT('Ctrl Pts',(58.0826836629924,-19.9428607795499,
-176.707915777809));
#162428=CARTESIAN_POINT('Ctrl Pts',(58.0817755947734,-19.9504692662353,
-176.7485257386));
#162429=CARTESIAN_POINT('Ctrl Pts',(58.0806675194151,-19.9597044874771,
-176.788520564059));
#162430=CARTESIAN_POINT('Ctrl Pts',(58.0804191620121,-19.9617744148938,
-176.797484765736));
#162431=CARTESIAN_POINT('Ctrl Pts',(58.0801607337195,-19.9639262624655,
-176.806418007041));
#162432=CARTESIAN_POINT('Ctrl Pts',(58.0798921481857,-19.9661604475892,
-176.815320243471));
#162433=CARTESIAN_POINT('Ctrl Pts',(58.0797944403183,-19.9669732146084,
-176.818558759425));
#162434=CARTESIAN_POINT('Ctrl Pts',(58.0796953880843,-19.9677968794911,
-176.821793172049));
#162435=CARTESIAN_POINT('Ctrl Pts',(58.079594986812,-19.9686314666135,-176.825023478714));
#162436=CARTESIAN_POINT('Ctrl Pts',(58.0795419300216,-19.9690725020011,
-176.826730525844));
#162437=CARTESIAN_POINT('Ctrl Pts',(58.0794884363611,-19.9695170872346,
-176.828438329814));
#162438=CARTESIAN_POINT('Ctrl Pts',(58.0794346961384,-19.96996363886,-176.8301408435));
#162439=CARTESIAN_POINT('Ctrl Pts',(58.0791314907293,-19.9724831086644,
-176.839746523066));
#162440=CARTESIAN_POINT('Ctrl Pts',(58.0788279335445,-19.9750029926094,
-176.848964250386));
#162441=CARTESIAN_POINT('Ctrl Pts',(58.0785049287239,-19.9776815321688,
-176.858384082359));
#162442=CARTESIAN_POINT('Ctrl Pts',(58.0782649644311,-19.979671452474,-176.865382192523));
#162443=CARTESIAN_POINT('Ctrl Pts',(58.0780141570239,-19.9817498314461,
-176.872491632651));
#162444=CARTESIAN_POINT('Ctrl Pts',(58.077742468928,-19.9839993345726,-176.879948694056));
#162445=CARTESIAN_POINT('Ctrl Pts',(58.0776814788505,-19.9845043157327,
-176.881622697295));
#162446=CARTESIAN_POINT('Ctrl Pts',(58.0776192226438,-19.9850196879432,
-176.883319688304));
#162447=CARTESIAN_POINT('Ctrl Pts',(58.0775567873286,-19.98553644744,-176.885009630243));
#162448=CARTESIAN_POINT('Ctrl Pts',(58.0760209778769,-19.9982479091728,
-176.926579514123));
#162449=CARTESIAN_POINT('Ctrl Pts',(58.0742695942654,-20.01268646212,-176.966883058534));
#162450=CARTESIAN_POINT('Ctrl Pts',(58.0723050521356,-20.0288060439935,
-177.005937009045));
#162451=CARTESIAN_POINT('Ctrl Pts',(58.0703050747586,-20.0452163813369,
-177.045695391583));
#162452=CARTESIAN_POINT('Ctrl Pts',(58.0680841820432,-20.0633690707768,
-177.084159548166));
#162453=CARTESIAN_POINT('Ctrl Pts',(58.0656387397512,-20.0832683280962,
-177.121336601679));
#162454=CARTESIAN_POINT('Ctrl Pts',(58.0640588170965,-20.0961246067136,
-177.145355516077));
#162455=CARTESIAN_POINT('Ctrl Pts',(58.062385084809,-20.1097106147667,-177.16883614858));
#162456=CARTESIAN_POINT('Ctrl Pts',(58.0606154075581,-20.1240370308985,
-177.19177397913));
#162457=CARTESIAN_POINT('Ctrl Pts',(58.0596819789832,-20.1315935987333,
-177.203872697396));
#162458=CARTESIAN_POINT('Ctrl Pts',(58.0587426302185,-20.1391881554284,
-177.215558619911));
#162459=CARTESIAN_POINT('Ctrl Pts',(58.0577743364992,-20.1470064780078,
-177.227139348827));
#162460=CARTESIAN_POINT('Ctrl Pts',(58.056830585,-20.1546266386137,-177.23842655441));
#162461=CARTESIAN_POINT('Ctrl Pts',(58.0558593277325,-20.1624594678433,
-177.249613960001));
#162462=CARTESIAN_POINT('Ctrl Pts',(58.0548338958529,-20.1707182132201,
-177.260961622157));
#162463=CARTESIAN_POINT('Ctrl Pts',(58.0541858470239,-20.1759375460464,
-177.268133077734));
#162464=CARTESIAN_POINT('Ctrl Pts',(58.0535160584687,-20.181327777909,-177.275368058178));
#162465=CARTESIAN_POINT('Ctrl Pts',(58.0528166218735,-20.1869517239637,
-177.282726277947));
#162466=CARTESIAN_POINT('Ctrl Pts',(58.0527562346118,-20.1874372786291,
-177.283361564613));
#162467=CARTESIAN_POINT('Ctrl Pts',(58.052695768784,-20.1879234298963,-177.283996259984));
#162468=CARTESIAN_POINT('Ctrl Pts',(58.0526352243748,-20.1884101777465,
-177.28463036415));
#162469=CARTESIAN_POINT('Ctrl Pts',(58.0495306484098,-20.2133694712422,
-177.317145745527));
#162470=CARTESIAN_POINT('Ctrl Pts',(58.0462539781284,-20.2395848887864,
-177.347770869852));
#162471=CARTESIAN_POINT('Ctrl Pts',(58.0428045171782,-20.2670162191791,
-177.376559123591));
#162472=CARTESIAN_POINT('Ctrl Pts',(58.0397672394745,-20.2911697229848,
-177.401907409157));
#162473=CARTESIAN_POINT('Ctrl Pts',(58.0365959190527,-20.3162667107182,
-177.425831470904));
#162474=CARTESIAN_POINT('Ctrl Pts',(58.0332867315621,-20.3423070408666,
-177.448348708029));
#162475=CARTESIAN_POINT('Ctrl Pts',(58.029716355988,-20.3704026863883,-177.472643189274));
#162476=CARTESIAN_POINT('Ctrl Pts',(58.0259860234872,-20.3995923819501,
-177.495296637396));
#162477=CARTESIAN_POINT('Ctrl Pts',(58.0220887490277,-20.4298923026491,
-177.516296202654));
#162478=CARTESIAN_POINT('Ctrl Pts',(58.0205742820626,-20.4416667438437,
-177.524456558871));
#162479=CARTESIAN_POINT('Ctrl Pts',(58.0190626232285,-20.4533913856618,
-177.532220439175));
#162480=CARTESIAN_POINT('Ctrl Pts',(58.0175217099449,-20.4653139806825,
-177.539766005896));
#162481=CARTESIAN_POINT('Ctrl Pts',(58.0160111045326,-20.4770020729061,
-177.547163160588));
#162482=CARTESIAN_POINT('Ctrl Pts',(58.0144723753573,-20.4888805286016,
-177.554350567559));
#162483=CARTESIAN_POINT('Ctrl Pts',(58.0128709932783,-20.5012113818323,
-177.561456314767));
#162484=CARTESIAN_POINT('Ctrl Pts',(58.0119022679131,-20.5086706949185,
-177.565754800212));
#162485=CARTESIAN_POINT('Ctrl Pts',(58.0109105339349,-20.516296094051,-177.570022646716));
#162486=CARTESIAN_POINT('Ctrl Pts',(58.0098873447433,-20.5241507522577,
-177.574280477352));
#162487=CARTESIAN_POINT('Ctrl Pts',(58.0098166280059,-20.5246936194092,
-177.574574753224));
#162488=CARTESIAN_POINT('Ctrl Pts',(58.0097458731121,-20.525236720801,-177.574868509872));
#162489=CARTESIAN_POINT('Ctrl Pts',(58.0096750800606,-20.5257800563078,
-177.575161747436));
#162490=CARTESIAN_POINT('Ctrl Pts',(58.0048770914619,-20.5626045399239,
-177.595035879935));
#162491=CARTESIAN_POINT('Ctrl Pts',(57.9999760159288,-20.5999426940359,
-177.612257905606));
#162492=CARTESIAN_POINT('Ctrl Pts',(57.9949733613778,-20.6377651830716,
-177.626891543277));
#162493=CARTESIAN_POINT('Ctrl Pts',(57.9900036151859,-20.6753388689884,
-177.641428918254));
#162494=CARTESIAN_POINT('Ctrl Pts',(57.9849335849506,-20.7133909289184,
-177.653412127068));
#162495=CARTESIAN_POINT('Ctrl Pts',(57.9797608952366,-20.7519186238698,
-177.662859907759));
#162496=CARTESIAN_POINT('Ctrl Pts',(57.9746750259199,-20.7897996552932,
-177.672149113294));
#162497=CARTESIAN_POINT('Ctrl Pts',(57.9694898790257,-20.8281408458448,
-177.678987476667));
#162498=CARTESIAN_POINT('Ctrl Pts',(57.9642000006941,-20.8669592766756,
-177.683347065177));
#162499=CARTESIAN_POINT('Ctrl Pts',(57.9602974573845,-20.8955971012205,
-177.686563298501));
#162500=CARTESIAN_POINT('Ctrl Pts',(57.9563378466394,-20.9244950860455,
-177.688429530829));
#162501=CARTESIAN_POINT('Ctrl Pts',(57.9523179894072,-20.9536655363841,
-177.688917160843));
#162502=CARTESIAN_POINT('',(58.5817791104913,-20.48000002,-176.438901946458));
#162503=CARTESIAN_POINT('Origin',(58.5817791104913,-19.98000002,-176.438901946458));
#162504=CARTESIAN_POINT('Ctrl Pts',(58.2408316684982,-21.000961690655,-177.234173073119));
#162505=CARTESIAN_POINT('Ctrl Pts',(58.2576191604414,-20.9259549021678,
-177.229990785726));
#162506=CARTESIAN_POINT('Ctrl Pts',(58.2811129081519,-20.8454420300561,
-177.203239464309));
#162507=CARTESIAN_POINT('Ctrl Pts',(58.3217884188213,-20.7363693827747,
-177.127664840087));
#162508=CARTESIAN_POINT('Ctrl Pts',(58.3362806968749,-20.7020244820194,
-177.096770053335));
#162509=CARTESIAN_POINT('Ctrl Pts',(58.3592272802903,-20.6555911910452,
-177.043321716498));
#162510=CARTESIAN_POINT('Ctrl Pts',(58.3670808352308,-20.6409521412524,
-177.024331107606));
#162511=CARTESIAN_POINT('Ctrl Pts',(58.379170673949,-20.6204149031061,-176.994325460603));
#162512=CARTESIAN_POINT('Ctrl Pts',(58.3852932151404,-20.6105004973145,
-176.978943105286));
#162513=CARTESIAN_POINT('Ctrl Pts',(58.3915345498872,-20.6011376986809,
-176.963039016323));
#162514=CARTESIAN_POINT('Ctrl Pts',(58.3957222043316,-20.5950199469896,
-176.952325670182));
#162515=CARTESIAN_POINT('Ctrl Pts',(58.3983722576607,-20.591272141354,-176.945514912726));
#162516=CARTESIAN_POINT('Ctrl Pts',(58.450443842201,-20.5192322826388,-176.81134072458));
#162517=CARTESIAN_POINT('Ctrl Pts',(58.5136487505111,-20.4800032267732,
-176.633649218076));
#162518=CARTESIAN_POINT('Ctrl Pts',(58.5817791104913,-20.48000002,-176.438901946458));
#162519=CARTESIAN_POINT('Origin',(0.,-12.9675000200281,-171.871644662643));
#162520=CARTESIAN_POINT('',(58.4843989875811,-14.3184534098307,-171.871644662643));
#162521=CARTESIAN_POINT('',(58.0853233553176,-19.9205720538986,-171.871644662643));
#162522=CARTESIAN_POINT('Origin',(0.,-12.9675000200281,-171.871644662643));
#162523=CARTESIAN_POINT('Origin',(56.9993922208425,-14.3352334529356,-171.97869344348));
#162524=CARTESIAN_POINT('Origin',(56.6288585600676,-20.00413998012,-171.968919992346));
#162525=CARTESIAN_POINT('Ctrl Pts',(58.4988784725361,-13.3298521511415,
-177.625121132168));
#162526=CARTESIAN_POINT('Ctrl Pts',(58.4984400659509,-13.3300368724616,
-177.363350721044));
#162527=CARTESIAN_POINT('Ctrl Pts',(58.7133155825256,-13.3314748983277,
-177.213850156091));
#162528=CARTESIAN_POINT('Ctrl Pts',(58.4979162725433,-13.485191578753,-177.625232807249));
#162529=CARTESIAN_POINT('Ctrl Pts',(58.4977839239423,-13.43598157919,-177.363622380296));
#162530=CARTESIAN_POINT('Ctrl Pts',(58.712578798724,-13.4097305125617,-177.214081551648));
#162531=CARTESIAN_POINT('Ctrl Pts',(58.4962858223951,-13.6398775654542,
-177.579193599722));
#162532=CARTESIAN_POINT('Ctrl Pts',(58.4968545902725,-13.5420809464769,
-177.326105364235));
#162533=CARTESIAN_POINT('Ctrl Pts',(58.7189266696638,-13.4876555148705,
-177.186196932532));
#162534=CARTESIAN_POINT('Ctrl Pts',(58.4926514029654,-13.9041359548645,
-177.416655260997));
#162535=CARTESIAN_POINT('Ctrl Pts',(58.4950669867845,-13.7147773263519,
-177.195381605071));
#162536=CARTESIAN_POINT('Ctrl Pts',(58.7446596953841,-13.6207725574733,
-177.084964984215));
#162537=CARTESIAN_POINT('Ctrl Pts',(58.4906746501567,-14.0153382250041,
-177.30007538425));
#162538=CARTESIAN_POINT('Ctrl Pts',(58.4942174562181,-13.7830844191732,
-177.100284844236));
#162539=CARTESIAN_POINT('Ctrl Pts',(58.7642460079756,-13.6767862384015,
-177.011404867089));
#162540=CARTESIAN_POINT('Ctrl Pts',(58.4858641857367,-14.264167834758,-176.902914238843));
#162541=CARTESIAN_POINT('Ctrl Pts',(58.4926218253665,-13.9162949426866,
-176.774744028082));
#162542=CARTESIAN_POINT('Ctrl Pts',(58.8384701265889,-13.8021130095289,
-176.749843894667));
#162543=CARTESIAN_POINT('Ctrl Pts',(58.4843734141373,-14.3196187432775,
-176.581150226222));
#162544=CARTESIAN_POINT('Ctrl Pts',(58.4931402301446,-13.8979533027039,
-176.507351292119));
#162545=CARTESIAN_POINT('Ctrl Pts',(58.9093648689647,-13.8300000199992,
-176.524836788664));
#162546=CARTESIAN_POINT('Ctrl Pts',(58.4843714753642,-14.3197132046691,
-176.2719717603));
#162547=CARTESIAN_POINT('Ctrl Pts',(58.4944487865147,-13.8300000200033,
-176.271971760298));
#162548=CARTESIAN_POINT('Ctrl Pts',(58.9842656455913,-13.83000002,-176.271971760298));
#162549=CARTESIAN_POINT('',(58.4988777713114,-13.3298527448197,-177.624285947696));
#162550=CARTESIAN_POINT('Origin',(58.9988681796133,-13.3329497766555,-177.624285947696));
#162551=CARTESIAN_POINT('',(58.984265645584,-13.8300000195596,-176.2719717603));
#162552=CARTESIAN_POINT('Ctrl Pts',(58.984265645584,-13.83000002,-176.2719717603));
#162553=CARTESIAN_POINT('Ctrl Pts',(58.9679069037307,-13.83000002,-176.327198874233));
#162554=CARTESIAN_POINT('Ctrl Pts',(58.9517045549244,-13.8286735475642,
-176.380696852843));
#162555=CARTESIAN_POINT('Ctrl Pts',(58.9359530227723,-13.8258115631793,
-176.43234588609));
#162556=CARTESIAN_POINT('Ctrl Pts',(58.9219297356961,-13.8232635933533,
-176.478328030139));
#162557=CARTESIAN_POINT('Ctrl Pts',(58.9082644377509,-13.8194986722545,
-176.522845347178));
#162558=CARTESIAN_POINT('Ctrl Pts',(58.8951729075458,-13.814331864178,-176.565820637321));
#162559=CARTESIAN_POINT('Ctrl Pts',(58.893559493195,-13.8136951011589,-176.571116958589));
#162560=CARTESIAN_POINT('Ctrl Pts',(58.8919547470568,-13.8130370072512,
-176.576389834502));
#162561=CARTESIAN_POINT('Ctrl Pts',(58.8903590337597,-13.8123572066797,
-176.581639097253));
#162562=CARTESIAN_POINT('Ctrl Pts',(58.8830872267535,-13.8092592951893,
-176.605560453127));
#162563=CARTESIAN_POINT('Ctrl Pts',(58.8759903846586,-13.8057120618013,
-176.628995175177));
#162564=CARTESIAN_POINT('Ctrl Pts',(58.8690798010049,-13.8016888293515,
-176.651917956065));
#162565=CARTESIAN_POINT('Ctrl Pts',(58.8621692173512,-13.7976655969018,
-176.674840736953));
#162566=CARTESIAN_POINT('Ctrl Pts',(58.8554448348755,-13.7931663671043,
-176.697251516217));
#162567=CARTESIAN_POINT('Ctrl Pts',(58.8489181184766,-13.7881680806183,
-176.719125005848));
#162568=CARTESIAN_POINT('Ctrl Pts',(58.8423914020777,-13.7831697941324,
-176.740998495479));
#162569=CARTESIAN_POINT('Ctrl Pts',(58.8360616849599,-13.777673013475,-176.762332133587));
#162570=CARTESIAN_POINT('Ctrl Pts',(58.8299384580245,-13.7716665856965,
-176.78308775253));
#162571=CARTESIAN_POINT('Ctrl Pts',(58.8268768445568,-13.7686633718073,
-176.793465562002));
#162572=CARTESIAN_POINT('Ctrl Pts',(58.823866884387,-13.7655328586488,-176.803698896827));
#162573=CARTESIAN_POINT('Ctrl Pts',(58.8209097885442,-13.7622749477684,
-176.813782297736));
#162574=CARTESIAN_POINT('Ctrl Pts',(58.8194312406228,-13.7606459923282,
-176.818823998191));
#162575=CARTESIAN_POINT('Ctrl Pts',(58.8179659123987,-13.7589851974192,
-176.82382821912));
#162576=CARTESIAN_POINT('Ctrl Pts',(58.8165139718298,-13.7572926247388,
-176.828794281536));
#162577=CARTESIAN_POINT('Ctrl Pts',(58.8156352418151,-13.7562682615877,
-176.831799795807));
#162578=CARTESIAN_POINT('Ctrl Pts',(58.8149249638452,-13.7554264249111,
-176.834231835516));
#162579=CARTESIAN_POINT('Ctrl Pts',(58.814085451631,-13.75441677938,-176.837108091733));
#162580=CARTESIAN_POINT('Ctrl Pts',(58.8135378235159,-13.7537581704047,
-176.838984322649));
#162581=CARTESIAN_POINT('Ctrl Pts',(58.8129353571127,-13.7530277220208,
-176.841049175964));
#162582=CARTESIAN_POINT('Ctrl Pts',(58.8121984954057,-13.7521196840738,
-176.843577321287));
#162583=CARTESIAN_POINT('Ctrl Pts',(58.8047326216658,-13.7429194547781,
-176.86919245856));
#162584=CARTESIAN_POINT('Ctrl Pts',(58.7976492777345,-13.7328159590292,
-176.893793723174));
#162585=CARTESIAN_POINT('Ctrl Pts',(58.7909628880544,-13.7218493579643,
-176.917269265914));
#162586=CARTESIAN_POINT('Ctrl Pts',(58.7903000239319,-13.7207621694008,
-176.919596545026));
#162587=CARTESIAN_POINT('Ctrl Pts',(58.7896415247005,-13.7196663449181,
-176.921912715834));
#162588=CARTESIAN_POINT('Ctrl Pts',(58.7889873808467,-13.7185618287773,
-176.924217876282));
#162589=CARTESIAN_POINT('Ctrl Pts',(58.7863423110571,-13.7140956517135,
-176.933538930398));
#162590=CARTESIAN_POINT('Ctrl Pts',(58.7837661701099,-13.7094837714519,
-176.942668924438));
#162591=CARTESIAN_POINT('Ctrl Pts',(58.7812577939148,-13.7047306884386,
-176.951606378371));
#162592=CARTESIAN_POINT('Ctrl Pts',(58.778129079127,-13.6988021354804,-176.962754125802));
#162593=CARTESIAN_POINT('Ctrl Pts',(58.7751063849037,-13.6926551088693,
-176.973599905223));
#162594=CARTESIAN_POINT('Ctrl Pts',(58.772182362733,-13.686303335553,-176.984136237167));
#162595=CARTESIAN_POINT('Ctrl Pts',(58.7663343183917,-13.6735997889203,
-177.005208901055));
#162596=CARTESIAN_POINT('Ctrl Pts',(58.7609024431394,-13.6600739570901,
-177.025031703479));
#162597=CARTESIAN_POINT('Ctrl Pts',(58.7559183857717,-13.6458151546945,
-177.04349077111));
#162598=CARTESIAN_POINT('Ctrl Pts',(58.7534263570878,-13.6386857534967,
-177.052720304925));
#162599=CARTESIAN_POINT('Ctrl Pts',(58.7510460967611,-13.6313732492002,
-177.06160869806));
#162600=CARTESIAN_POINT('Ctrl Pts',(58.7487798730375,-13.6238905734078,
-177.070141215375));
#162601=CARTESIAN_POINT('Ctrl Pts',(58.7476467611757,-13.6201492355116,
-177.074407474033));
#162602=CARTESIAN_POINT('Ctrl Pts',(58.7465421602532,-13.6163653600285,
-177.07858476562));
#162603=CARTESIAN_POINT('Ctrl Pts',(58.7454662933704,-13.6125407267456,
-177.082671233078));
#162604=CARTESIAN_POINT('Ctrl Pts',(58.7448786850993,-13.6104518194775,
-177.084903146818));
#162605=CARTESIAN_POINT('Ctrl Pts',(58.744372827281,-13.6086170289023,-177.086828912308));
#162606=CARTESIAN_POINT('Ctrl Pts',(58.7438276832832,-13.6066025097304,
-177.088909271721));
#162607=CARTESIAN_POINT('Ctrl Pts',(58.7433747093129,-13.6049285946708,
-177.090637895106));
#162608=CARTESIAN_POINT('Ctrl Pts',(58.7428946837808,-13.6031304142461,
-177.092473045025));
#162609=CARTESIAN_POINT('Ctrl Pts',(58.7423251299313,-13.6009463862979,
-177.094656337774));
#162610=CARTESIAN_POINT('Ctrl Pts',(58.7384401112559,-13.586048779385,-177.109548929774));
#162611=CARTESIAN_POINT('Ctrl Pts',(58.7349185884774,-13.5704346140225,
-177.123253023635));
#162612=CARTESIAN_POINT('Ctrl Pts',(58.7317901864608,-13.5542149695198,
-177.135582555746));
#162613=CARTESIAN_POINT('Ctrl Pts',(58.7308762483141,-13.5494765274145,
-177.139184531984));
#162614=CARTESIAN_POINT('Ctrl Pts',(58.7299947746698,-13.5446823603777,
-177.142670531144));
#162615=CARTESIAN_POINT('Ctrl Pts',(58.729145971874,-13.5398381541873,-177.146037999423));
#162616=CARTESIAN_POINT('Ctrl Pts',(58.7252281330667,-13.5174786390013,
-177.161581301084));
#162617=CARTESIAN_POINT('Ctrl Pts',(58.7220323680021,-13.4940622836547,
-177.174572918194));
#162618=CARTESIAN_POINT('Ctrl Pts',(58.7195645574954,-13.4700429785437,
-177.184872363911));
#162619=CARTESIAN_POINT('Ctrl Pts',(58.7175984325081,-13.4509066000294,
-177.193078017272));
#162620=CARTESIAN_POINT('Ctrl Pts',(58.716094193839,-13.4313878853066,-177.199575495156));
#162621=CARTESIAN_POINT('Ctrl Pts',(58.7150495463886,-13.4117105994086,
-177.204316500607));
#162622=CARTESIAN_POINT('Ctrl Pts',(58.7137256604449,-13.3867734953148,
-177.210324796013));
#162623=CARTESIAN_POINT('Ctrl Pts',(58.7131400085458,-13.3615857919425,
-177.213511143853));
#162624=CARTESIAN_POINT('Ctrl Pts',(58.7132776892154,-13.3365560747486,
-177.213825716594));
#162625=CARTESIAN_POINT('Ctrl Pts',(58.7132870100049,-13.3348615977753,
-177.21384701273));
#162626=CARTESIAN_POINT('Ctrl Pts',(58.7132996430622,-13.3331678319628,
-177.213855162194));
#162627=CARTESIAN_POINT('Ctrl Pts',(58.7133155825256,-13.3314748983292,
-177.213850156091));
#162628=CARTESIAN_POINT('',(58.4843989875811,-14.3184534098307,-176.2719717603));
#162629=CARTESIAN_POINT('Origin',(58.9842656455946,-14.33000002,-176.2719717603));
#162630=CARTESIAN_POINT('Ctrl Pts',(58.4988777713114,-13.3298527448197,
-177.624285947696));
#162631=CARTESIAN_POINT('Ctrl Pts',(58.4983908181541,-13.4084673412756,
-177.624342719651));
#162632=CARTESIAN_POINT('Ctrl Pts',(58.4974447796673,-13.5228546462299,
-177.608365198208));
#162633=CARTESIAN_POINT('Ctrl Pts',(58.4960362646421,-13.6501200351752,
-177.561615067615));
#162634=CARTESIAN_POINT('Ctrl Pts',(58.4953746377398,-13.7033366219318,
-177.535555792594));
#162635=CARTESIAN_POINT('Ctrl Pts',(58.4949214728157,-13.7385197366069,
-177.516844385966));
#162636=CARTESIAN_POINT('Ctrl Pts',(58.4946730914668,-13.7571080789305,
-177.506112042692));
#162637=CARTESIAN_POINT('Ctrl Pts',(58.4935605637375,-13.8378723566693,
-177.456177551313));
#162638=CARTESIAN_POINT('Ctrl Pts',(58.4921730279003,-13.9270164501794,
-177.384838642241));
#162639=CARTESIAN_POINT('Ctrl Pts',(58.4905865207784,-14.017416254816,-177.281629256011));
#162640=CARTESIAN_POINT('Ctrl Pts',(58.4898144182803,-14.0592159333627,
-177.22502939815));
#162641=CARTESIAN_POINT('Ctrl Pts',(58.4894893930172,-14.0764014812318,
-177.199701923765));
#162642=CARTESIAN_POINT('Ctrl Pts',(58.4892741579113,-14.0876966042115,
-177.182579075853));
#162643=CARTESIAN_POINT('Ctrl Pts',(58.489149697308,-14.0941715098239,-177.172441758713));
#162644=CARTESIAN_POINT('Ctrl Pts',(58.4862281559377,-14.2452242270742,
-176.930144926363));
#162645=CARTESIAN_POINT('Ctrl Pts',(58.4843989875812,-14.3184534098306,
-176.632435702977));
#162646=CARTESIAN_POINT('Ctrl Pts',(58.4843989875811,-14.3184534098307,
-176.2719717603));
#162647=CARTESIAN_POINT('Ctrl Pts',(58.7133155825256,-13.3314748983275,
-177.213850156091));
#162648=CARTESIAN_POINT('Ctrl Pts',(58.4988766126948,-13.3300397939931,
-177.363046991769));
#162649=CARTESIAN_POINT('Ctrl Pts',(58.4988777713114,-13.3298527448209,
-177.624285947696));
#162650=CARTESIAN_POINT('Ctrl Pts',(58.7142076600563,-13.1641303210821,
-177.213830854253));
#162651=CARTESIAN_POINT('Ctrl Pts',(58.4999095201947,-13.1633713364571,
-177.363039299942));
#162652=CARTESIAN_POINT('Ctrl Pts',(58.4999097084608,-13.1632549492482,
-177.624165638205));
#162653=CARTESIAN_POINT('Ctrl Pts',(58.7144845107404,-12.9967863561848,
-177.213824921703));
#162654=CARTESIAN_POINT('Ctrl Pts',(58.5002301876544,-12.9966649765953,
-177.363036914652));
#162655=CARTESIAN_POINT('Ctrl Pts',(58.500229964035,-12.996655767065,-177.624128301462));
#162656=CARTESIAN_POINT('Ctrl Pts',(58.7141461350386,-12.8294402383605,
-177.213832217124));
#162657=CARTESIAN_POINT('Ctrl Pts',(58.4998383709332,-12.8299842764725,
-177.363039831106));
#162658=CARTESIAN_POINT('Ctrl Pts',(58.4998385375645,-12.8300551987823,
-177.624173936067));
#162659=CARTESIAN_POINT('',(58.4998385375645,-12.8300551987823,-177.624173936067));
#162660=CARTESIAN_POINT('Origin',(0.784740066134875,-12.9675005363404,-184.352939507241));
#162661=CARTESIAN_POINT('Origin',(58.9998371575436,-12.8288804567203,-177.624173936068));
#162662=CARTESIAN_POINT('Ctrl Pts',(58.48912660861,-11.8396398505087,-176.26629097911));
#162663=CARTESIAN_POINT('Ctrl Pts',(58.4985823439911,-12.33000002,-176.26629097911));
#162664=CARTESIAN_POINT('Ctrl Pts',(58.9890336736409,-12.33000002,-176.26629097911));
#162665=CARTESIAN_POINT('Ctrl Pts',(58.4891266082067,-11.8396398295935,
-176.423373313634));
#162666=CARTESIAN_POINT('Ctrl Pts',(58.4978924302213,-12.2942221356202,
-176.390394119799));
#162667=CARTESIAN_POINT('Ctrl Pts',(58.9511729872871,-12.33000002,-176.394565470062));
#162668=CARTESIAN_POINT('Ctrl Pts',(58.4893923301638,-11.8529830432079,
-176.578231191384));
#162669=CARTESIAN_POINT('Ctrl Pts',(58.4973632374244,-12.2720420811237,
-176.51680491203));
#162670=CARTESIAN_POINT('Ctrl Pts',(58.9148079297158,-12.3367286443605,
-176.512401023853));
#162671=CARTESIAN_POINT('Ctrl Pts',(58.4906521273108,-11.9211841187055,
-176.880933630382));
#162672=CARTESIAN_POINT('Ctrl Pts',(58.4968786243544,-12.2700692006727,
-176.761217862814));
#162673=CARTESIAN_POINT('Ctrl Pts',(58.8482938287677,-12.3711206280572,
-176.731313674606));
#162674=CARTESIAN_POINT('Ctrl Pts',(58.4916809553489,-11.9775042760042,
-177.031063990607));
#162675=CARTESIAN_POINT('Ctrl Pts',(58.4969059340918,-12.2890138650664,
-176.883349034336));
#162676=CARTESIAN_POINT('Ctrl Pts',(58.817725908538,-12.3995214017445,-176.833790628028));
#162677=CARTESIAN_POINT('Ctrl Pts',(58.4936040475389,-12.1014782716709,
-177.230049861356));
#162678=CARTESIAN_POINT('Ctrl Pts',(58.4973396692349,-12.3546251483512,
-177.045101981496));
#162679=CARTESIAN_POINT('Ctrl Pts',(58.7801197877863,-12.4620381958002,
-176.965157505607));
#162680=CARTESIAN_POINT('Ctrl Pts',(58.494315776837,-12.1502025268642,-177.293200512009));
#162681=CARTESIAN_POINT('Ctrl Pts',(58.4975444264886,-12.3825831770725,
-177.096147908481));
#162682=CARTESIAN_POINT('Ctrl Pts',(58.7686983660461,-12.486608549538,-177.006030037118));
#162683=CARTESIAN_POINT('Ctrl Pts',(58.4957333150688,-12.2588835334819,
-177.404811094274));
#162684=CARTESIAN_POINT('Ctrl Pts',(58.4980148214299,-12.4487602363349,
-177.186076538859));
#162685=CARTESIAN_POINT('Ctrl Pts',(58.7491768361659,-12.5414135007217,
-177.077379300711));
#162686=CARTESIAN_POINT('Ctrl Pts',(58.4964422014533,-12.3189060674576,
-177.453832155185));
#162687=CARTESIAN_POINT('Ctrl Pts',(58.4982801309887,-12.4869468894055,
-177.22572537075));
#162688=CARTESIAN_POINT('Ctrl Pts',(58.7409598721377,-12.5716812769085,
-177.108237839695));
#162689=CARTESIAN_POINT('Ctrl Pts',(58.4984277184057,-12.5184434004461,
-177.577650852379));
#162690=CARTESIAN_POINT('Ctrl Pts',(58.4990784570061,-12.6167275534409,
-177.325053017822));
#162691=CARTESIAN_POINT('Ctrl Pts',(58.7207402303504,-12.6723026604245,
-177.185595547246));
#162692=CARTESIAN_POINT('Ctrl Pts',(58.4994668010734,-12.6718351617763,
-177.624217264241));
#162693=CARTESIAN_POINT('Ctrl Pts',(58.4995844948381,-12.722010160726,-177.363144865678));
#162694=CARTESIAN_POINT('Ctrl Pts',(58.7138612409819,-12.7496539972653,
-177.213921724966));
#162695=CARTESIAN_POINT('Ctrl Pts',(58.4998385375645,-12.8300551987826,
-177.624173936067));
#162696=CARTESIAN_POINT('Ctrl Pts',(58.4998383709333,-12.8299842764724,
-177.363039831107));
#162697=CARTESIAN_POINT('Ctrl Pts',(58.7141461350374,-12.8294402383603,
-177.213832217126));
#162698=CARTESIAN_POINT('',(58.48912660861,-11.8396398505087,-176.26629097911));
#162699=CARTESIAN_POINT('Ctrl Pts',(58.48912660861,-11.8396398505087,-176.26629097911));
#162700=CARTESIAN_POINT('Ctrl Pts',(58.48912660861,-11.8396398505087,-176.409811534268));
#162701=CARTESIAN_POINT('Ctrl Pts',(58.4893483896326,-11.850776103237,-176.551488494012));
#162702=CARTESIAN_POINT('Ctrl Pts',(58.4898674690038,-11.8787272918346,
-176.690381503724));
#162703=CARTESIAN_POINT('Ctrl Pts',(58.4899146582257,-11.8812683191145,
-176.703008191331));
#162704=CARTESIAN_POINT('Ctrl Pts',(58.4899643050978,-11.8839483504648,
-176.715611866645));
#162705=CARTESIAN_POINT('Ctrl Pts',(58.4900164667572,-11.8867716762097,
-176.728191820333));
#162706=CARTESIAN_POINT('Ctrl Pts',(58.4900183886416,-11.8868757010012,
-176.72865532585));
#162707=CARTESIAN_POINT('Ctrl Pts',(58.4900203139396,-11.8869799203049,
-176.72911879896));
#162708=CARTESIAN_POINT('Ctrl Pts',(58.4900222426542,-11.8870843343361,
-176.729582239632));
#162709=CARTESIAN_POINT('Ctrl Pts',(58.4904143757935,-11.9083130858161,
-176.82380584864));
#162710=CARTESIAN_POINT('Ctrl Pts',(58.4909611779827,-11.9381550632001,
-176.917576442103));
#162711=CARTESIAN_POINT('Ctrl Pts',(58.491628008076,-11.9776372784523,-177.007000513355));
#162712=CARTESIAN_POINT('Ctrl Pts',(58.4920261001825,-12.0012078377276,
-177.060385951801));
#162713=CARTESIAN_POINT('Ctrl Pts',(58.4924669768134,-12.0282147910086,
-177.112221932541));
#162714=CARTESIAN_POINT('Ctrl Pts',(58.4929432955759,-12.0588830464209,
-177.16167335862));
#162715=CARTESIAN_POINT('Ctrl Pts',(58.4929498715258,-12.0593064454722,
-177.16235607391));
#162716=CARTESIAN_POINT('Ctrl Pts',(58.4929564542504,-12.0597305436947,
-177.163038337515));
#162717=CARTESIAN_POINT('Ctrl Pts',(58.4929630437302,-12.0601553416844,
-177.163720147168));
#162718=CARTESIAN_POINT('Ctrl Pts',(58.4935968230333,-12.1010126145907,
-177.229296924179));
#162719=CARTESIAN_POINT('Ctrl Pts',(58.4943004033954,-12.1491458631888,
-177.291840545738));
#162720=CARTESIAN_POINT('Ctrl Pts',(58.4950024041184,-12.2028473374637,
-177.347256942163));
#162721=CARTESIAN_POINT('Ctrl Pts',(58.4950097920195,-12.203412495261,-177.347840147912));
#162722=CARTESIAN_POINT('Ctrl Pts',(58.4950171797681,-12.2039782717463,
-177.348422567924));
#162723=CARTESIAN_POINT('Ctrl Pts',(58.4950245672806,-12.2045446649403,
-177.349004197405));
#162724=CARTESIAN_POINT('Ctrl Pts',(58.4957264419677,-12.2583566950054,
-177.404263800622));
#162725=CARTESIAN_POINT('Ctrl Pts',(58.4964292592559,-12.3178002283294,
-177.452938198817));
#162726=CARTESIAN_POINT('Ctrl Pts',(58.4970868450185,-12.3836929510146,
-177.494029767074));
#162727=CARTESIAN_POINT('Ctrl Pts',(58.497092582954,-12.3842679150954,-177.494388322234));
#162728=CARTESIAN_POINT('Ctrl Pts',(58.4970983175096,-12.3848433769923,
-177.494746304328));
#162729=CARTESIAN_POINT('Ctrl Pts',(58.4971040486531,-12.3854193371859,
-177.495103712595));
#162730=CARTESIAN_POINT('Ctrl Pts',(58.4975789393159,-12.4331442135456,
-177.524719067147));
#162731=CARTESIAN_POINT('Ctrl Pts',(58.4980179792089,-12.4835732800606,
-177.549749276722));
#162732=CARTESIAN_POINT('Ctrl Pts',(58.4984026087055,-12.5359391558249,
-177.569640300795));
#162733=CARTESIAN_POINT('Ctrl Pts',(58.4987756724465,-12.5867303969686,
-177.588933204532));
#162734=CARTESIAN_POINT('Ctrl Pts',(58.4990975247222,-12.6393425576463,
-177.603390836161));
#162735=CARTESIAN_POINT('Ctrl Pts',(58.4993516232989,-12.6930550659192,
-177.612550490846));
#162736=CARTESIAN_POINT('Ctrl Pts',(58.499564677447,-12.7380914169331,-177.620230590637));
#162737=CARTESIAN_POINT('Ctrl Pts',(58.4997300980036,-12.7839007002384,
-177.624186575364));
#162738=CARTESIAN_POINT('Ctrl Pts',(58.4998385375645,-12.8300551987823,
-177.624173936067));
#162739=CARTESIAN_POINT('',(58.9890336736409,-12.3300000204739,-176.26629097911));
#162740=CARTESIAN_POINT('Origin',(58.9890336736409,-11.83000002,-176.26629097911));
#162741=CARTESIAN_POINT('Ctrl Pts',(58.7141461350374,-12.8294402383603,
-177.213832217126));
#162742=CARTESIAN_POINT('Ctrl Pts',(58.7140819296199,-12.811459412521,-177.21385238952));
#162743=CARTESIAN_POINT('Ctrl Pts',(58.7143816551427,-12.7933544705259,
-177.212425421223));
#162744=CARTESIAN_POINT('Ctrl Pts',(58.7150632987668,-12.7752997321945,
-177.209516903944));
#162745=CARTESIAN_POINT('Ctrl Pts',(58.7152846118919,-12.7694377972727,
-177.208572579042));
#162746=CARTESIAN_POINT('Ctrl Pts',(58.7155460928643,-12.7635812153741,
-177.207472475417));
#162747=CARTESIAN_POINT('Ctrl Pts',(58.7158480917974,-12.7577360874582,
-177.206216550884));
#162748=CARTESIAN_POINT('Ctrl Pts',(58.716816069541,-12.7390010751397,-177.202191016809));
#162749=CARTESIAN_POINT('Ctrl Pts',(58.7182010244667,-12.7203874846099,
-177.196561750169));
#162750=CARTESIAN_POINT('Ctrl Pts',(58.7200061839669,-12.7020882148015,
-177.189361547879));
#162751=CARTESIAN_POINT('Ctrl Pts',(58.7216704793852,-12.6852169129054,
-177.182723207234));
#162752=CARTESIAN_POINT('Ctrl Pts',(58.723691597054,-12.6686147413198,-177.174751108997));
#162753=CARTESIAN_POINT('Ctrl Pts',(58.7260634953738,-12.6524255210882,
-177.165504848793));
#162754=CARTESIAN_POINT('Ctrl Pts',(58.727449441156,-12.6429658485087,-177.160102081219));
#162755=CARTESIAN_POINT('Ctrl Pts',(58.7289550679102,-12.6336465746835,
-177.154264608281));
#162756=CARTESIAN_POINT('Ctrl Pts',(58.7305781768371,-12.6244942829079,
-177.148008033313));
#162757=CARTESIAN_POINT('Ctrl Pts',(58.7317328456457,-12.6179834038989,
-177.143557147828));
#162758=CARTESIAN_POINT('Ctrl Pts',(58.732946110831,-12.6115611006134,-177.138897443365));
#162759=CARTESIAN_POINT('Ctrl Pts',(58.7342199915419,-12.6052217380805,
-177.134023742212));
#162760=CARTESIAN_POINT('Ctrl Pts',(58.735402267938,-12.5993382368829,-177.129500507198));
#162761=CARTESIAN_POINT('Ctrl Pts',(58.7366319475121,-12.5935452263529,
-177.124813678365));
#162762=CARTESIAN_POINT('Ctrl Pts',(58.7379129452138,-12.5878291335991,
-177.119951431684));
#162763=CARTESIAN_POINT('Ctrl Pts',(58.7387647963682,-12.5840279868799,
-177.116718084393));
#162764=CARTESIAN_POINT('Ctrl Pts',(58.7396386693894,-12.5802640997989,
-177.113409732084));
#162765=CARTESIAN_POINT('Ctrl Pts',(58.7405344197273,-12.5765391217875,
-177.110027828988));
#162766=CARTESIAN_POINT('Ctrl Pts',(58.7407707132952,-12.5755564949246,
-177.10913570323));
#162767=CARTESIAN_POINT('Ctrl Pts',(58.7410085288087,-12.5745765746215,
-177.108238460817));
#162768=CARTESIAN_POINT('Ctrl Pts',(58.74124786267,-12.5735993889851,-177.107336131755));
#162769=CARTESIAN_POINT('Ctrl Pts',(58.7413598187595,-12.5731422790637,
-177.106914038398));
#162770=CARTESIAN_POINT('Ctrl Pts',(58.7414736198389,-12.5726795881164,
-177.106485128439));
#162771=CARTESIAN_POINT('Ctrl Pts',(58.74158951008,-12.5722104964838,-177.106048495697));
#162772=CARTESIAN_POINT('Ctrl Pts',(58.7422420312352,-12.5695692713822,
-177.103590030701));
#162773=CARTESIAN_POINT('Ctrl Pts',(58.7429540566299,-12.5667591487054,
-177.100912580599));
#162774=CARTESIAN_POINT('Ctrl Pts',(58.7436251133995,-12.5641756692348,
-177.098394190095));
#162775=CARTESIAN_POINT('Ctrl Pts',(58.7439823525257,-12.5628003460278,
-177.097053517199));
#162776=CARTESIAN_POINT('Ctrl Pts',(58.7443277438613,-12.5614887596861,
-177.095758708694));
#162777=CARTESIAN_POINT('Ctrl Pts',(58.7446447061254,-12.5602976725631,
-177.09457147636));
#162778=CARTESIAN_POINT('Ctrl Pts',(58.7447641846295,-12.5598486938555,
-177.094123950709));
#162779=CARTESIAN_POINT('Ctrl Pts',(58.744879615129,-12.5594168198056,-177.093691738289));
#162780=CARTESIAN_POINT('Ctrl Pts',(58.7449900830053,-12.5590050376963,
-177.093278230413));
#162781=CARTESIAN_POINT('Ctrl Pts',(58.7450575067238,-12.55875370779,-177.093025847191));
#162782=CARTESIAN_POINT('Ctrl Pts',(58.7451231516292,-12.5585095853754,
-177.092780168902));
#162783=CARTESIAN_POINT('Ctrl Pts',(58.7451895613975,-12.5582631790804,
-177.092531673465));
#162784=CARTESIAN_POINT('Ctrl Pts',(58.7493441098919,-12.5428481742039,
-177.076985973327));
#162785=CARTESIAN_POINT('Ctrl Pts',(58.7539230266605,-12.5280889949087,
-177.060032443229));
#162786=CARTESIAN_POINT('Ctrl Pts',(58.758937601106,-12.5140110251299,-177.041704668915));
#162787=CARTESIAN_POINT('Ctrl Pts',(58.7637684671953,-12.5004488001493,
-177.024048330497));
#162788=CARTESIAN_POINT('Ctrl Pts',(58.7690325800979,-12.4875098220423,
-177.005022325128));
#162789=CARTESIAN_POINT('Ctrl Pts',(58.7746562065322,-12.4753590626234,
-176.984935558188));
#162790=CARTESIAN_POINT('Ctrl Pts',(58.7760519396443,-12.4723433542623,
-176.979950204687));
#162791=CARTESIAN_POINT('Ctrl Pts',(58.7774703718805,-12.469374709313,-176.974897500936));
#162792=CARTESIAN_POINT('Ctrl Pts',(58.7789129322744,-12.4664507071385,
-176.969773145284));
#162793=CARTESIAN_POINT('Ctrl Pts',(58.7832826727381,-12.4575934484255,
-176.954250672645));
#162794=CARTESIAN_POINT('Ctrl Pts',(58.7878685478042,-12.4491565790701,
-176.93808929468));
#162795=CARTESIAN_POINT('Ctrl Pts',(58.7926551613702,-12.4411992644483,
-176.921368546414));
#162796=CARTESIAN_POINT('Ctrl Pts',(58.7932827345557,-12.4401559804613,
-176.919176288128));
#162797=CARTESIAN_POINT('Ctrl Pts',(58.7939144101258,-12.4391199222591,
-176.91697239607));
#162798=CARTESIAN_POINT('Ctrl Pts',(58.7945501814039,-12.4380910843739,
-176.914756880988));
#162799=CARTESIAN_POINT('Ctrl Pts',(58.7979343273103,-12.4326146848608,
-176.902963919341));
#162800=CARTESIAN_POINT('Ctrl Pts',(58.80142242488,-12.4273626370271,-176.89088421705));
#162801=CARTESIAN_POINT('Ctrl Pts',(58.8049977587502,-12.4223299660034,
-176.878537167771));
#162802=CARTESIAN_POINT('Ctrl Pts',(58.8067854256853,-12.4198136304916,
-176.872363643132));
#162803=CARTESIAN_POINT('Ctrl Pts',(58.8085966099864,-12.4173527374792,
-176.866122892953));
#162804=CARTESIAN_POINT('Ctrl Pts',(58.8104321298967,-12.4149474978988,
-176.859816564017));
#162805=CARTESIAN_POINT('Ctrl Pts',(58.8115041159289,-12.4135427824174,
-176.856133522228));
#162806=CARTESIAN_POINT('Ctrl Pts',(58.8127336302357,-12.4119666704472,
-176.851916809599));
#162807=CARTESIAN_POINT('Ctrl Pts',(58.8138602537382,-12.4105555372891,
-176.848059758556));
#162808=CARTESIAN_POINT('Ctrl Pts',(58.8146627037572,-12.409550442129,-176.845312531398));
#162809=CARTESIAN_POINT('Ctrl Pts',(58.8154125443209,-12.408627963248,-176.842748880392));
#162810=CARTESIAN_POINT('Ctrl Pts',(58.8160115760595,-12.4078985515024,
-176.840702677788));
#162811=CARTESIAN_POINT('Ctrl Pts',(58.8244081864246,-12.397674408391,-176.812021115717));
#162812=CARTESIAN_POINT('Ctrl Pts',(58.8333248152985,-12.3884835890777,
-176.78188929717));
#162813=CARTESIAN_POINT('Ctrl Pts',(58.8426847877196,-12.3803541547745,
-176.750536379343));
#162814=CARTESIAN_POINT('Ctrl Pts',(58.8525227202813,-12.371809596859,-176.717582447717));
#162815=CARTESIAN_POINT('Ctrl Pts',(58.8628503464016,-12.3644376787052,
-176.68327982788));
#162816=CARTESIAN_POINT('Ctrl Pts',(58.8735611615879,-12.3582406628378,
-176.647940399611));
#162817=CARTESIAN_POINT('Ctrl Pts',(58.8761776845034,-12.3567268066333,
-176.639307403683));
#162818=CARTESIAN_POINT('Ctrl Pts',(58.8788170008591,-12.3552829261018,
-176.630612725113));
#162819=CARTESIAN_POINT('Ctrl Pts',(58.8814774221998,-12.3539087910943,
-176.62186125809));
#162820=CARTESIAN_POINT('Ctrl Pts',(58.8939117687074,-12.3474863231306,
-176.580958423731));
#162821=CARTESIAN_POINT('Ctrl Pts',(58.9068669263435,-12.3424881234721,
-176.538617876985));
#162822=CARTESIAN_POINT('Ctrl Pts',(58.9202241992701,-12.3387709208172,
-176.494828120573));
#162823=CARTESIAN_POINT('Ctrl Pts',(58.9340586940389,-12.3349209118397,
-176.449473866052));
#162824=CARTESIAN_POINT('Ctrl Pts',(58.9483242256657,-12.3324443653281,
-176.402564210775));
#162825=CARTESIAN_POINT('Ctrl Pts',(58.962873779728,-12.331138362007,-176.354117959566));
#162826=CARTESIAN_POINT('Ctrl Pts',(58.9715048174126,-12.3303636190952,
-176.325378836835));
#162827=CARTESIAN_POINT('Ctrl Pts',(58.9802355398853,-12.33000002,-176.296099633879));
#162828=CARTESIAN_POINT('Ctrl Pts',(58.9890336736409,-12.33000002,-176.26629097911));
#162829=CARTESIAN_POINT('Origin',(0.,-12.9675000200281,-171.871644662643));
#162830=CARTESIAN_POINT('',(58.1115942404669,-6.23752120644091,-171.871644662643));
#162831=CARTESIAN_POINT('',(58.48912660861,-11.8396398505087,-171.871644662643));
#162832=CARTESIAN_POINT('Origin',(0.,-12.9675000200281,-171.871644662643));
#162833=CARTESIAN_POINT('Origin',(56.6526047464346,-6.15642511055022,-171.969110145006));
#162834=CARTESIAN_POINT('Origin',(57.0042957475178,-11.8256297436875,-171.97932653822));
#162835=CARTESIAN_POINT('Ctrl Pts',(57.9826110754301,-5.20432973493148,
-177.68524973918));
#162836=CARTESIAN_POINT('Ctrl Pts',(57.9819403936437,-5.19932045653773,
-177.367360689002));
#162837=CARTESIAN_POINT('Ctrl Pts',(58.267019098174,-5.15898893607643,-177.232518219478));
#162838=CARTESIAN_POINT('Ctrl Pts',(58.0025119651788,-5.35296817875971,
-177.682845100084));
#162839=CARTESIAN_POINT('Ctrl Pts',(57.9949888374176,-5.2966803543509,-177.360992500472));
#162840=CARTESIAN_POINT('Ctrl Pts',(58.2832677496941,-5.23392550092992,
-177.228417054074));
#162841=CARTESIAN_POINT('Ctrl Pts',(58.0218092186127,-5.50176990585681,
-177.64204201157));
#162842=CARTESIAN_POINT('Ctrl Pts',(58.0077051406755,-5.39303977887496,
-177.325226539032));
#162843=CARTESIAN_POINT('Ctrl Pts',(58.3041451880796,-5.30898013469752,
-177.202784454736));
#162844=CARTESIAN_POINT('Ctrl Pts',(58.0549536715593,-5.76404075854571,
-177.499799765465));
#162845=CARTESIAN_POINT('Ctrl Pts',(58.0288513197851,-5.5545561633354,-177.210890020253));
#162846=CARTESIAN_POINT('Ctrl Pts',(58.3514580290103,-5.44123637401812,
-177.116293661504));
#162847=CARTESIAN_POINT('Ctrl Pts',(58.0690822624578,-5.87947228735883,
-177.397969070777));
#162848=CARTESIAN_POINT('Ctrl Pts',(58.0375028694103,-5.62129124259478,
-177.130382190313));
#162849=CARTESIAN_POINT('Ctrl Pts',(58.3782554149277,-5.49944543725108,
-177.055134470277));
#162850=CARTESIAN_POINT('Ctrl Pts',(58.0910734645313,-6.0620213485957,-177.158256835825));
#162851=CARTESIAN_POINT('Ctrl Pts',(58.049471160706,-5.71257363005819,-176.947755762969));
#162852=CARTESIAN_POINT('Ctrl Pts',(58.4364471667621,-5.59150009130694,
-176.908395287787));
#162853=CARTESIAN_POINT('Ctrl Pts',(58.0990088104622,-6.12958052854701,
-177.021022282342));
#162854=CARTESIAN_POINT('Ctrl Pts',(58.0527451569459,-5.73669128650856,
-176.84391309495));
#162855=CARTESIAN_POINT('Ctrl Pts',(58.4678181796127,-5.62556839623242,
-176.823203787185));
#162856=CARTESIAN_POINT('Ctrl Pts',(58.1093120435936,-6.21769842661734,
-176.729452616794));
#162857=CARTESIAN_POINT('Ctrl Pts',(58.0539894201321,-5.74161490543249,
-176.632064657874));
#162858=CARTESIAN_POINT('Ctrl Pts',(58.5354785511785,-5.67000391722627,
-176.63504101192));
#162859=CARTESIAN_POINT('Ctrl Pts',(58.1115942412421,-6.23752121313465,
-176.57952555449));
#162860=CARTESIAN_POINT('Ctrl Pts',(58.0517037498764,-5.72038259956876,
-176.525060913865));
#162861=CARTESIAN_POINT('Ctrl Pts',(58.5707923905479,-5.68000002000002,
-176.534945859098));
#162862=CARTESIAN_POINT('Ctrl Pts',(58.1115942404669,-6.2375212064409,-176.427328712824));
#162863=CARTESIAN_POINT('Ctrl Pts',(58.0470269915055,-5.68000001999982,
-176.427328712824));
#162864=CARTESIAN_POINT('Ctrl Pts',(58.6082745331206,-5.68000001999999,
-176.427328712824));
#162865=CARTESIAN_POINT('',(57.9826110754301,-5.20432973493148,-177.68524973918));
#162866=CARTESIAN_POINT('Origin',(58.4781889478697,-5.13797785215286,-177.68524973918));
#162867=CARTESIAN_POINT('',(58.6082745331212,-5.68000001999999,-176.427328712824));
#162868=CARTESIAN_POINT('Ctrl Pts',(58.6082745331206,-5.68000001999999,
-176.427328712824));
#162869=CARTESIAN_POINT('Ctrl Pts',(58.5970324095344,-5.68000002,-176.459606623727));
#162870=CARTESIAN_POINT('Ctrl Pts',(58.5859083959314,-5.67909758005478,
-176.491428394012));
#162871=CARTESIAN_POINT('Ctrl Pts',(58.5749508380644,-5.67721411211561,
-176.522640354069));
#162872=CARTESIAN_POINT('Ctrl Pts',(58.5641075990386,-5.67535029416368,
-176.553526683621));
#162873=CARTESIAN_POINT('Ctrl Pts',(58.5534272139788,-5.67252542423281,
-176.583816198249));
#162874=CARTESIAN_POINT('Ctrl Pts',(58.5429485109152,-5.66870453919802,
-176.613388490099));
#162875=CARTESIAN_POINT('Ctrl Pts',(58.5357937630411,-5.66609567921663,
-176.633580138909));
#162876=CARTESIAN_POINT('Ctrl Pts',(58.5287328734313,-5.66302333872094,
-176.65343800953));
#162877=CARTESIAN_POINT('Ctrl Pts',(58.5217765613204,-5.65948888494477,
-176.672930259477));
#162878=CARTESIAN_POINT('Ctrl Pts',(58.5172529280574,-5.65719045836277,
-176.685605911291));
#162879=CARTESIAN_POINT('Ctrl Pts',(58.5127742345477,-5.65469728174271,
-176.698124986584));
#162880=CARTESIAN_POINT('Ctrl Pts',(58.5083407613764,-5.65201071061408,
-176.710486547715));
#162881=CARTESIAN_POINT('Ctrl Pts',(58.5060990024534,-5.65065226215459,
-176.716737096415));
#162882=CARTESIAN_POINT('Ctrl Pts',(58.5038683421279,-5.64924411240428,
-176.72294866782));
#162883=CARTESIAN_POINT('Ctrl Pts',(58.5016483653956,-5.64778615672935,
-176.729122399553));
#162884=CARTESIAN_POINT('Ctrl Pts',(58.4898362654193,-5.64002863479541,
-176.761971724228));
#162885=CARTESIAN_POINT('Ctrl Pts',(58.4784451172372,-5.63090809605689,
-176.793399371308));
#162886=CARTESIAN_POINT('Ctrl Pts',(58.4674297681207,-5.62048392576165,
-176.823405937733));
#162887=CARTESIAN_POINT('Ctrl Pts',(58.4631068061411,-5.61639297127818,
-176.835181982634));
#162888=CARTESIAN_POINT('Ctrl Pts',(58.4588444780111,-5.61210324517753,
-176.846731684525));
#162889=CARTESIAN_POINT('Ctrl Pts',(58.454647608505,-5.60762712545288,-176.858035618715));
#162890=CARTESIAN_POINT('Ctrl Pts',(58.4481504254091,-5.60069763446731,
-176.875535264589));
#162891=CARTESIAN_POINT('Ctrl Pts',(58.4418083102892,-5.59331915800136,
-176.892450478896));
#162892=CARTESIAN_POINT('Ctrl Pts',(58.4356299325352,-5.58553811454111,
-176.908739450309));
#162893=CARTESIAN_POINT('Ctrl Pts',(58.4339980164171,-5.58348288083035,
-176.913041912226));
#162894=CARTESIAN_POINT('Ctrl Pts',(58.432377517179,-5.58139962042743,-176.917300718298));
#162895=CARTESIAN_POINT('Ctrl Pts',(58.4307664293617,-5.57928998993657,
-176.921515480085));
#162896=CARTESIAN_POINT('Ctrl Pts',(58.4297367314208,-5.57794165736942,
-176.924209269639));
#162897=CARTESIAN_POINT('Ctrl Pts',(58.428884895563,-5.57681225945347,-176.926433647857));
#162898=CARTESIAN_POINT('Ctrl Pts',(58.4278796327049,-5.57546258463045,
-176.929055357636));
#162899=CARTESIAN_POINT('Ctrl Pts',(58.4273120394084,-5.57470052883984,
-176.930535632058));
#162900=CARTESIAN_POINT('Ctrl Pts',(58.4266956310907,-5.57386775174087,
-176.932142116037));
#162901=CARTESIAN_POINT('Ctrl Pts',(58.4259718144521,-5.5728798358495,-176.934025799901));
#162902=CARTESIAN_POINT('Ctrl Pts',(58.4196479910485,-5.56424863659143,
-176.950483122753));
#162903=CARTESIAN_POINT('Ctrl Pts',(58.4134394553127,-5.55510712130321,
-176.9664084859));
#162904=CARTESIAN_POINT('Ctrl Pts',(58.4073502234499,-5.54547311803255,
-176.98176505197));
#162905=CARTESIAN_POINT('Ctrl Pts',(58.3979885804448,-5.53066170973654,
-177.005374382763));
#162906=CARTESIAN_POINT('Ctrl Pts',(58.3889117915324,-5.51466287933301,
-177.027596666233));
#162907=CARTESIAN_POINT('Ctrl Pts',(58.3801633276821,-5.49770409370011,
-177.048237284276));
#162908=CARTESIAN_POINT('Ctrl Pts',(58.372943899417,-5.48370932405424,-177.06527038447));
#162909=CARTESIAN_POINT('Ctrl Pts',(58.3659447782497,-5.46905542971186,
-177.081234299931));
#162910=CARTESIAN_POINT('Ctrl Pts',(58.3591786862378,-5.45387223042539,
-177.096045819018));
#162911=CARTESIAN_POINT('Ctrl Pts',(58.3557956402319,-5.44628063078215,
-177.103451578561));
#162912=CARTESIAN_POINT('Ctrl Pts',(58.3524730577879,-5.43855609988564,
-177.110568847175));
#162913=CARTESIAN_POINT('Ctrl Pts',(58.3492141964119,-5.43071541842866,
-177.117387967907));
#162914=CARTESIAN_POINT('Ctrl Pts',(58.3477437626597,-5.42717761754519,
-177.120464829463));
#162915=CARTESIAN_POINT('Ctrl Pts',(58.3464013095158,-5.42389707592293,
-177.123242460199));
#162916=CARTESIAN_POINT('Ctrl Pts',(58.3450298856348,-5.42049936370148,
-177.126050672046));
#162917=CARTESIAN_POINT('Ctrl Pts',(58.3437250496098,-5.41726662335737,
-177.128722534506));
#162918=CARTESIAN_POINT('Ctrl Pts',(58.342393972099,-5.41392771186506,-177.13142219143));
#162919=CARTESIAN_POINT('Ctrl Pts',(58.3409084629875,-5.41013924246599,
-177.134394284005));
#162920=CARTESIAN_POINT('Ctrl Pts',(58.3404950069453,-5.4090848123374,-177.13522149511));
#162921=CARTESIAN_POINT('Ctrl Pts',(58.3400696340722,-5.40799542616371,
-177.136069548477));
#162922=CARTESIAN_POINT('Ctrl Pts',(58.3396296994008,-5.40686335247274,
-177.136943044253));
#162923=CARTESIAN_POINT('Ctrl Pts',(58.3355952543372,-5.39648160852046,
-177.144953485235));
#162924=CARTESIAN_POINT('Ctrl Pts',(58.3316482276062,-5.38588752655005,
-177.152494532144));
#162925=CARTESIAN_POINT('Ctrl Pts',(58.3277942727314,-5.37511057187182,
-177.159541643791));
#162926=CARTESIAN_POINT('Ctrl Pts',(58.3203781128629,-5.35437249335602,
-177.173102390681));
#162927=CARTESIAN_POINT('Ctrl Pts',(58.3132716974141,-5.33285868715332,
-177.184860820779));
#162928=CARTESIAN_POINT('Ctrl Pts',(58.3065400889278,-5.31093152612779,
-177.194732398229));
#162929=CARTESIAN_POINT('Ctrl Pts',(58.3000030628719,-5.28963818691342,
-177.20431862998));
#162930=CARTESIAN_POINT('Ctrl Pts',(58.2938195924287,-5.26795588312359,
-177.212125463235));
#162931=CARTESIAN_POINT('Ctrl Pts',(58.2880381913187,-5.24620561892136,
-177.218121248799));
#162932=CARTESIAN_POINT('Ctrl Pts',(58.2824668436432,-5.22524559874663,
-177.223899191781));
#162933=CARTESIAN_POINT('Ctrl Pts',(58.2772689190291,-5.20422301863945,
-177.227995395089));
#162934=CARTESIAN_POINT('Ctrl Pts',(58.2724764146032,-5.18340504051878,
-177.230424191671));
#162935=CARTESIAN_POINT('Ctrl Pts',(58.2705944502693,-5.17523004706118,
-177.231377953658));
#162936=CARTESIAN_POINT('Ctrl Pts',(58.2687748732832,-5.16708633698723,
-177.232075061476));
#162937=CARTESIAN_POINT('Ctrl Pts',(58.267019098174,-5.15898893607643,-177.232518219478));
#162938=CARTESIAN_POINT('',(58.1115942404669,-6.2375212064409,-176.427328712824));
#162939=CARTESIAN_POINT('Origin',(58.6082745331205,-6.18000001999999,-176.427328712824));
#162940=CARTESIAN_POINT('Ctrl Pts',(57.9826110754301,-5.20432973493148,
-177.68524973918));
#162941=CARTESIAN_POINT('Ctrl Pts',(57.9864133803307,-5.23272890152749,
-177.684790303892));
#162942=CARTESIAN_POINT('Ctrl Pts',(57.9901585317883,-5.26087114190313,
-177.682937908873));
#162943=CARTESIAN_POINT('Ctrl Pts',(57.9938499513603,-5.28876235919758,
-177.679797008529));
#162944=CARTESIAN_POINT('Ctrl Pts',(57.9976152499095,-5.31721178304886,
-177.676593247137));
#162945=CARTESIAN_POINT('Ctrl Pts',(58.0013246616446,-5.34540021247657,
-177.672048874718));
#162946=CARTESIAN_POINT('Ctrl Pts',(58.0049820412409,-5.37334248086366,
-177.666219172833));
#162947=CARTESIAN_POINT('Ctrl Pts',(58.0071009194111,-5.38953064535426,
-177.662841774414));
#162948=CARTESIAN_POINT('Ctrl Pts',(58.0092023028964,-5.40563608053747,
-177.659031970271));
#162949=CARTESIAN_POINT('Ctrl Pts',(58.0112866328472,-5.42166024630227,
-177.654792733909));
#162950=CARTESIAN_POINT('Ctrl Pts',(58.0127082279006,-5.43258935797033,
-177.651901407879));
#162951=CARTESIAN_POINT('Ctrl Pts',(58.0141227858999,-5.44348757569641,
-177.648808284626));
#162952=CARTESIAN_POINT('Ctrl Pts',(58.0155294925108,-5.45434822190824,
-177.645514358109));
#162953=CARTESIAN_POINT('Ctrl Pts',(58.0189462259726,-5.48072752022124,
-177.637513777986));
#162954=CARTESIAN_POINT('Ctrl Pts',(58.0223147701654,-5.50687103546922,
-177.628330087141));
#162955=CARTESIAN_POINT('Ctrl Pts',(58.0256102732283,-5.5325791664003,-177.618027059099));
#162956=CARTESIAN_POINT('Ctrl Pts',(58.0292381208969,-5.56087990867951,
-177.606684992183));
#162957=CARTESIAN_POINT('Ctrl Pts',(58.0327774052014,-5.58865274716744,
-177.593984257917));
#162958=CARTESIAN_POINT('Ctrl Pts',(58.0361953413919,-5.61562914495522,
-177.580061370296));
#162959=CARTESIAN_POINT('Ctrl Pts',(58.0369297082257,-5.62142520746961,
-177.57706994321));
#162960=CARTESIAN_POINT('Ctrl Pts',(58.0376584880585,-5.62718459988006,
-177.57402226185));
#162961=CARTESIAN_POINT('Ctrl Pts',(58.0383813818279,-5.63290483163267,
-177.570919942798));
#162962=CARTESIAN_POINT('Ctrl Pts',(58.0384493306635,-5.63344250826458,
-177.570628338448));
#162963=CARTESIAN_POINT('Ctrl Pts',(58.0385172322329,-5.63397987194777,
-177.570336244847));
#162964=CARTESIAN_POINT('Ctrl Pts',(58.0385850863885,-5.63451692127423,
-177.570043663697));
#162965=CARTESIAN_POINT('Ctrl Pts',(58.0490694432024,-5.71749808456103,
-177.524836039378));
#162966=CARTESIAN_POINT('Ctrl Pts',(58.058560690856,-5.79407235500778,-177.467381876558));
#162967=CARTESIAN_POINT('Ctrl Pts',(58.0668921625494,-5.86215495272362,
-177.400951487669));
#162968=CARTESIAN_POINT('Ctrl Pts',(58.0716810779975,-5.90128871155427,
-177.362767415601));
#162969=CARTESIAN_POINT('Ctrl Pts',(58.076086829394,-5.93761722714732,-177.32161665146));
#162970=CARTESIAN_POINT('Ctrl Pts',(58.0800778613687,-5.97074680033053,
-177.278112939551));
#162971=CARTESIAN_POINT('Ctrl Pts',(58.0801358840197,-5.97122844660027,
-177.27748047138));
#162972=CARTESIAN_POINT('Ctrl Pts',(58.0801938210413,-5.97170942905892,
-177.276847523818));
#162973=CARTESIAN_POINT('Ctrl Pts',(58.0802516724784,-5.97218974777174,
-177.276214098177));
#162974=CARTESIAN_POINT('Ctrl Pts',(58.0863462475121,-6.02279071087329,
-177.209483515684));
#162975=CARTESIAN_POINT('Ctrl Pts',(58.091488245137,-6.06600199005368,-177.137485615194));
#162976=CARTESIAN_POINT('Ctrl Pts',(58.0957336562474,-6.10193041986059,
-177.061710183542));
#162977=CARTESIAN_POINT('Ctrl Pts',(58.0990967930802,-6.13039226312736,
-177.001682276096));
#162978=CARTESIAN_POINT('Ctrl Pts',(58.1018971540569,-6.15428295037301,
-176.939282520674));
#162979=CARTESIAN_POINT('Ctrl Pts',(58.1041602520257,-6.17363798086329,
-176.875236987128));
#162980=CARTESIAN_POINT('Ctrl Pts',(58.1041777800786,-6.17378788864584,
-176.874740944307));
#162981=CARTESIAN_POINT('Ctrl Pts',(58.1041952749008,-6.17393751574848,
-176.874244853752));
#162982=CARTESIAN_POINT('Ctrl Pts',(58.104212736516,-6.17408686234949,-176.873748715522));
#162983=CARTESIAN_POINT('Ctrl Pts',(58.1067717090136,-6.19597337403404,
-176.801040431038));
#162984=CARTESIAN_POINT('Ctrl Pts',(58.1086155525892,-6.21181886439977,
-176.72738700765));
#162985=CARTESIAN_POINT('Ctrl Pts',(58.1098212142836,-6.22220604020925,
-176.652935850911));
#162986=CARTESIAN_POINT('Ctrl Pts',(58.1110268759779,-6.23259321601873,
-176.578484694172));
#162987=CARTESIAN_POINT('Ctrl Pts',(58.1115942404669,-6.23752120644093,
-176.50323543809));
#162988=CARTESIAN_POINT('Ctrl Pts',(58.1115942404669,-6.2375212064409,-176.427328712824));
#162989=CARTESIAN_POINT('Ctrl Pts',(58.2670190981741,-5.15898893607704,
-177.232518219478));
#162990=CARTESIAN_POINT('Ctrl Pts',(57.9819403936438,-5.19932045653815,
-177.367360689003));
#162991=CARTESIAN_POINT('Ctrl Pts',(57.9826110754301,-5.20432973493151,
-177.68524973918));
#162992=CARTESIAN_POINT('Ctrl Pts',(58.2478951756903,-4.99233199195458,
-177.233703806904));
#162993=CARTESIAN_POINT('Ctrl Pts',(57.9597329881765,-5.03356356782781,
-177.367569378206));
#162994=CARTESIAN_POINT('Ctrl Pts',(57.9604889110946,-5.0391007365056,-177.687922734557));
#162995=CARTESIAN_POINT('Ctrl Pts',(58.2281612527228,-4.82572915883349,
-177.234977247299));
#162996=CARTESIAN_POINT('Ctrl Pts',(57.936860143276,-4.86824210971035,-177.367787815378));
#162997=CARTESIAN_POINT('Ctrl Pts',(57.9376611104107,-4.87397087657654,
-177.690692163097));
#162998=CARTESIAN_POINT('Ctrl Pts',(58.207817372083,-4.65917712520044,-177.236349008084));
#162999=CARTESIAN_POINT('Ctrl Pts',(57.9133432880526,-4.70343927025946,
-177.368016692624));
#163000=CARTESIAN_POINT('Ctrl Pts',(57.9141277227909,-4.70894021166782,
-177.693561815623));
#163001=CARTESIAN_POINT('',(57.914127722791,-4.70894021166827,-177.693561815623));
#163002=CARTESIAN_POINT('Origin',(1.08576145822724,-12.9503575433999,-185.613344152246));
#163003=CARTESIAN_POINT('Origin',(58.4091202674301,-4.63835423039998,-177.693561815623));
#163004=CARTESIAN_POINT('Ctrl Pts',(57.7719896917998,-3.76686746433079,
-176.487816214668));
#163005=CARTESIAN_POINT('Ctrl Pts',(57.8426304086464,-4.22014242411439,
-176.540115608276));
#163006=CARTESIAN_POINT('Ctrl Pts',(58.3023950569127,-4.18492067076111,
-176.54510707307));
#163007=CARTESIAN_POINT('Ctrl Pts',(57.7656488319951,-3.72809386701247,
-176.804681178765));
#163008=CARTESIAN_POINT('Ctrl Pts',(57.8281144931389,-4.12556715300443,
-176.735939864345));
#163009=CARTESIAN_POINT('Ctrl Pts',(58.2201998825318,-4.16532008285243,
-176.752600827192));
#163010=CARTESIAN_POINT('Ctrl Pts',(57.7783333144461,-3.80457033547739,
-177.140063733512));
#163011=CARTESIAN_POINT('Ctrl Pts',(57.8296205489137,-4.13610505104128,
-176.987574312776));
#163012=CARTESIAN_POINT('Ctrl Pts',(58.1755280883538,-4.20378312244756,
-176.943056377667));
#163013=CARTESIAN_POINT('Ctrl Pts',(57.8431686999111,-4.22319358998163,
-177.622644986573));
#163014=CARTESIAN_POINT('Ctrl Pts',(57.8659572284752,-4.38142129799194,
-177.327226280779));
#163015=CARTESIAN_POINT('Ctrl Pts',(58.1582320325074,-4.41455172597864,
-177.206615941663));
#163016=CARTESIAN_POINT('Ctrl Pts',(57.8918930477109,-4.54705885986191,
-177.742945331961));
#163017=CARTESIAN_POINT('Ctrl Pts',(57.8985608374326,-4.60362668953059,
-177.410684031821));
#163018=CARTESIAN_POINT('Ctrl Pts',(58.1843609366024,-4.57776276467961,
-177.265681912745));
#163019=CARTESIAN_POINT('Ctrl Pts',(57.9368177485324,-4.86994787109087,
-177.677206679151));
#163020=CARTESIAN_POINT('Ctrl Pts',(57.9271674646007,-4.80719227924389,
-177.349355107446));
#163021=CARTESIAN_POINT('Ctrl Pts',(58.228168972613,-4.74018086702697,-177.223609336047));
#163022=CARTESIAN_POINT('',(57.7706512256236,-3.75870764711888,-176.647241333324));
#163023=CARTESIAN_POINT('Ctrl Pts',(57.7706512256236,-3.75870764711887,
-176.647241333324));
#163024=CARTESIAN_POINT('Ctrl Pts',(57.7706512256236,-3.75870764711892,
-176.716132142105));
#163025=CARTESIAN_POINT('Ctrl Pts',(57.7714731229875,-3.76385932402702,
-176.783073604645));
#163026=CARTESIAN_POINT('Ctrl Pts',(57.7731127828381,-3.77416333624056,
-176.848065720941));
#163027=CARTESIAN_POINT('Ctrl Pts',(57.7739326127634,-3.77931534234734,
-176.880561779089));
#163028=CARTESIAN_POINT('Ctrl Pts',(57.7749567540909,-3.78575545282719,
-176.912570500677));
#163029=CARTESIAN_POINT('Ctrl Pts',(57.7761839145684,-3.79348387278035,
-176.944091885703));
#163030=CARTESIAN_POINT('Ctrl Pts',(57.777411075046,-3.80121229273351,-176.97561327073));
#163031=CARTESIAN_POINT('Ctrl Pts',(57.778746960844,-3.80963337741544,-177.004881728095));
#163032=CARTESIAN_POINT('Ctrl Pts',(57.7804726441157,-3.8205343470524,-177.037194031102));
#163033=CARTESIAN_POINT('Ctrl Pts',(57.7839240106591,-3.84233628632631,
-177.101818637114));
#163034=CARTESIAN_POINT('Ctrl Pts',(57.7881819478627,-3.86930866299404,
-177.16259800506));
#163035=CARTESIAN_POINT('Ctrl Pts',(57.7932247359729,-3.90145487248269,
-177.219532134939));
#163036=CARTESIAN_POINT('Ctrl Pts',(57.795746130028,-3.91752797722698,-177.247999199879));
#163037=CARTESIAN_POINT('Ctrl Pts',(57.7984636067391,-3.93489456053134,
-177.275504955302));
#163038=CARTESIAN_POINT('Ctrl Pts',(57.8013736694665,-3.95355516093848,
-177.302049401209));
#163039=CARTESIAN_POINT('Ctrl Pts',(57.8042837321939,-3.97221576134561,
-177.328593847115));
#163040=CARTESIAN_POINT('Ctrl Pts',(57.8072614019285,-3.99136347062015,
-177.353242005971));
#163041=CARTESIAN_POINT('Ctrl Pts',(57.8106775980806,-4.01341962890035,
-177.378798810378));
#163042=CARTESIAN_POINT('Ctrl Pts',(57.820877452893,-4.07927346227552,-177.455104643772));
#163043=CARTESIAN_POINT('Ctrl Pts',(57.8322332475662,-4.15330818745427,
-177.51785062654));
#163044=CARTESIAN_POINT('Ctrl Pts',(57.8448789412148,-4.23709451534444,
-177.567745265917));
#163045=CARTESIAN_POINT('Ctrl Pts',(57.8491747318432,-4.26555705224762,
-177.584694666258));
#163046=CARTESIAN_POINT('Ctrl Pts',(57.8536189541738,-4.29514496864859,
-177.600161038337));
#163047=CARTESIAN_POINT('Ctrl Pts',(57.8582154512499,-4.32592002579372,
-177.614172156613));
#163048=CARTESIAN_POINT('Ctrl Pts',(57.8763428437788,-4.44728887075097,
-177.669428373808));
#163049=CARTESIAN_POINT('Ctrl Pts',(57.8950217283446,-4.57495716519149,
-177.695891593478));
#163050=CARTESIAN_POINT('Ctrl Pts',(57.914127722791,-4.70894021166828,-177.693561815623));
#163051=CARTESIAN_POINT('',(58.2644174754116,-4.18000003136422,-176.647241333317));
#163052=CARTESIAN_POINT('Origin',(58.2644174754153,-3.68000001999999,-176.647241333324));
#163053=CARTESIAN_POINT('Ctrl Pts',(58.2078173718681,-4.65917712427737,
-177.236349008137));
#163054=CARTESIAN_POINT('Ctrl Pts',(58.1948301492149,-4.60331060815716,
-177.23952272256));
#163055=CARTESIAN_POINT('Ctrl Pts',(58.1843326939393,-4.54860640735877,
-177.231092666144));
#163056=CARTESIAN_POINT('Ctrl Pts',(58.1770121417029,-4.49749087444241,
-177.212340891078));
#163057=CARTESIAN_POINT('Ctrl Pts',(58.1744085339799,-4.47931126285495,
-177.205671685695));
#163058=CARTESIAN_POINT('Ctrl Pts',(58.1722067390647,-4.46158638555533,
-177.197697525224));
#163059=CARTESIAN_POINT('Ctrl Pts',(58.1704367005146,-4.44441968451078,
-177.188473620115));
#163060=CARTESIAN_POINT('Ctrl Pts',(58.1685748231361,-4.4263622855139,-177.178771130719));
#163061=CARTESIAN_POINT('Ctrl Pts',(58.1671922722601,-4.40892606256636,
-177.167682895421));
#163062=CARTESIAN_POINT('Ctrl Pts',(58.1663236940235,-4.39229679467997,
-177.155335364104));
#163063=CARTESIAN_POINT('Ctrl Pts',(58.1655193809276,-4.3768979078848,-177.143901412938));
#163064=CARTESIAN_POINT('Ctrl Pts',(58.1651557313076,-4.3621915965796,-177.131388762485));
#163065=CARTESIAN_POINT('Ctrl Pts',(58.1652462837178,-4.3483007781872,-177.117926071166));
#163066=CARTESIAN_POINT('Ctrl Pts',(58.1652984126327,-4.34030415736272,
-177.110175913132));
#163067=CARTESIAN_POINT('Ctrl Pts',(58.1655008078473,-4.33257711780437,
-177.102111193057));
#163068=CARTESIAN_POINT('Ctrl Pts',(58.1658539559977,-4.32513860657448,
-177.093759366692));
#163069=CARTESIAN_POINT('Ctrl Pts',(58.1661142565689,-4.31965578379691,
-177.08760335208));
#163070=CARTESIAN_POINT('Ctrl Pts',(58.1664559934947,-4.31433507611524,
-177.081298147169));
#163071=CARTESIAN_POINT('Ctrl Pts',(58.1668800604306,-4.30916742421314,
-177.074836159665));
#163072=CARTESIAN_POINT('Ctrl Pts',(58.16695135481,-4.3082986355757,-177.073749766575));
#163073=CARTESIAN_POINT('Ctrl Pts',(58.167025065974,-4.3074347774271,-177.072659864222));
#163074=CARTESIAN_POINT('Ctrl Pts',(58.1671011947531,-4.30657576506413,
-177.071566398619));
#163075=CARTESIAN_POINT('Ctrl Pts',(58.1673524923837,-4.30374020439798,
-177.067956918493));
#163076=CARTESIAN_POINT('Ctrl Pts',(58.1676478381592,-4.3007629757407,-177.06405441704));
#163077=CARTESIAN_POINT('Ctrl Pts',(58.1679620654409,-4.29793615717124,
-177.060231622647));
#163078=CARTESIAN_POINT('Ctrl Pts',(58.1682762927225,-4.29510933860178,
-177.056408828254));
#163079=CARTESIAN_POINT('Ctrl Pts',(58.1686091516182,-4.29243243934732,
-177.052666252106));
#163080=CARTESIAN_POINT('Ctrl Pts',(58.1689138852836,-4.29015774532314,
-177.049410570726));
#163081=CARTESIAN_POINT('Ctrl Pts',(58.1694279402103,-4.28632056616321,
-177.04391856494));
#163082=CARTESIAN_POINT('Ctrl Pts',(58.1700074737126,-4.28257531700519,
-177.038318568171));
#163083=CARTESIAN_POINT('Ctrl Pts',(58.1706463882517,-4.27892301202666,
-177.032614290244));
#163084=CARTESIAN_POINT('Ctrl Pts',(58.1727964644394,-4.26663226970529,
-177.013418245402));
#163085=CARTESIAN_POINT('Ctrl Pts',(58.175618532156,-4.25539973890795,-176.993043260651));
#163086=CARTESIAN_POINT('Ctrl Pts',(58.1791407681495,-4.24530419939267,
-176.971613968747));
#163087=CARTESIAN_POINT('Ctrl Pts',(58.1827233690694,-4.2350356400965,-176.949817416491));
#163088=CARTESIAN_POINT('Ctrl Pts',(58.1870304587187,-4.22594345645078,
-176.92693044205));
#163089=CARTESIAN_POINT('Ctrl Pts',(58.1920726605442,-4.21807418246598,
-176.903119223703));
#163090=CARTESIAN_POINT('Ctrl Pts',(58.1972784148855,-4.20994965500221,
-176.878535647406));
#163091=CARTESIAN_POINT('Ctrl Pts',(58.2032679068386,-4.20312878672857,
-176.852967296043));
#163092=CARTESIAN_POINT('Ctrl Pts',(58.2100304868865,-4.19762260354405,
-176.826628541868));
#163093=CARTESIAN_POINT('Ctrl Pts',(58.2169370087538,-4.19199922100361,
-176.79972916613));
#163094=CARTESIAN_POINT('Ctrl Pts',(58.2246499872768,-4.18774708342058,
-176.772026842204));
#163095=CARTESIAN_POINT('Ctrl Pts',(58.2331330995294,-4.18483579450576,
-176.743774442892));
#163096=CARTESIAN_POINT('Ctrl Pts',(58.241867148002,-4.18183838768823,-176.714686318427));
#163097=CARTESIAN_POINT('Ctrl Pts',(58.2514176874185,-4.18026231439924,
-176.685015815368));
#163098=CARTESIAN_POINT('Ctrl Pts',(58.2617170359672,-4.18003022393884,
-176.655054447656));
#163099=CARTESIAN_POINT('Ctrl Pts',(58.2626115695454,-4.18001006609011,
-176.652452200598));
#163100=CARTESIAN_POINT('Ctrl Pts',(58.2635117341523,-4.18000001999999,
-176.649847764673));
#163101=CARTESIAN_POINT('Ctrl Pts',(58.2644174754153,-4.18000001999999,
-176.647241333323));
#163102=CARTESIAN_POINT('Origin',(0.,-12.9675000200281,-171.871644662643));
#163103=CARTESIAN_POINT('',(56.5940537057312,1.84341099694893,-171.871644662643));
#163104=CARTESIAN_POINT('',(57.7706512256236,-3.75870764711888,-171.871644662643));
#163105=CARTESIAN_POINT('Origin',(0.,-12.9675000200281,-171.871644662643));
#163106=CARTESIAN_POINT('Origin',(55.2297899960015,2.001980827273,-171.934292975586));
#163107=CARTESIAN_POINT('Origin',(56.3352965291918,-3.65078706877886,-171.961175715908));
#163108=CARTESIAN_POINT('Ctrl Pts',(56.5169491525423,2.13496529160038,-177.558207897086));
#163109=CARTESIAN_POINT('Ctrl Pts',(56.409292540301,2.53784145482491,-177.125154911669));
#163110=CARTESIAN_POINT('Ctrl Pts',(57.,2.61702308584989,-177.204078948543));
#163111=CARTESIAN_POINT('Ctrl Pts',(56.5659347005564,1.95164994081541,-177.37392715461));
#163112=CARTESIAN_POINT('Ctrl Pts',(56.4267635932219,2.4778594556634,-177.032282865396));
#163113=CARTESIAN_POINT('Ctrl Pts',(57.043897408659,2.52469464001198,-177.112050866152));
#163114=CARTESIAN_POINT('Ctrl Pts',(56.5940537017931,1.84341101199667,-177.116606872607));
#163115=CARTESIAN_POINT('Ctrl Pts',(56.4314543935154,2.46472012384626,-176.935564924353));
#163116=CARTESIAN_POINT('Ctrl Pts',(57.0736014896981,2.46999998000001,-176.982739539051));
#163117=CARTESIAN_POINT('Ctrl Pts',(56.5940537057312,1.84341099694892,-176.848740272858));
#163118=CARTESIAN_POINT('Ctrl Pts',(56.430072632376,2.46999998,-176.848740272858));
#163119=CARTESIAN_POINT('Ctrl Pts',(57.077763566464,2.46999998000001,-176.848740272858));
#163120=CARTESIAN_POINT('',(56.5169491525423,2.13496529160038,-177.558207897086));
#163121=CARTESIAN_POINT('Origin',(57.,2.26404619169977,-177.558207897086));
#163122=CARTESIAN_POINT('',(57.077763566464,2.46999998000001,-176.848740272858));
#163123=CARTESIAN_POINT('Ctrl Pts',(57.077763566464,2.46999998000001,-176.848740272858));
#163124=CARTESIAN_POINT('Ctrl Pts',(57.0760574119627,2.46999998000001,-176.903670626367));
#163125=CARTESIAN_POINT('Ctrl Pts',(57.069539132854,2.47909807637283,-176.964460625587));
#163126=CARTESIAN_POINT('Ctrl Pts',(57.0443985826942,2.52546697496909,-177.087725761396));
#163127=CARTESIAN_POINT('Ctrl Pts',(57.0257001863846,2.56296846543371,-177.150200178938));
#163128=CARTESIAN_POINT('Ctrl Pts',(57.,2.61702308584989,-177.204078948543));
#163129=CARTESIAN_POINT('',(56.5940537057312,1.84341099694892,-176.848740272858));
#163130=CARTESIAN_POINT('Origin',(57.077763566464,1.96999998000001,-176.848740272858));
#163131=CARTESIAN_POINT('Ctrl Pts',(56.5169491525423,2.13496529160038,-177.558207897086));
#163132=CARTESIAN_POINT('Ctrl Pts',(56.5229386918135,2.11255103806931,-177.535675603609));
#163133=CARTESIAN_POINT('Ctrl Pts',(56.528571815665,2.09142571598422,-177.512223964754));
#163134=CARTESIAN_POINT('Ctrl Pts',(56.5338654144839,2.07153817047639,-177.487923467016));
#163135=CARTESIAN_POINT('Ctrl Pts',(56.5392385869434,2.0513516743957,-177.463257682989));
#163136=CARTESIAN_POINT('Ctrl Pts',(56.5442620552539,2.03244001840271,-177.437717820727));
#163137=CARTESIAN_POINT('Ctrl Pts',(56.5489480395883,2.01476843117717,-177.41132463543));
#163138=CARTESIAN_POINT('Ctrl Pts',(56.5536246352264,1.99713225020854,-177.38498433072));
#163139=CARTESIAN_POINT('Ctrl Pts',(56.5579650856442,1.98073116282666,-177.357794129274));
#163140=CARTESIAN_POINT('Ctrl Pts',(56.561970784984,1.96557003493501,-177.329742709106));
#163141=CARTESIAN_POINT('Ctrl Pts',(56.565631524691,1.95171454100795,-177.304106998851));
#163142=CARTESIAN_POINT('Ctrl Pts',(56.5690127023447,1.93889452819214,-177.277750345696));
#163143=CARTESIAN_POINT('Ctrl Pts',(56.5721056483258,1.92715023624348,-177.250654113369));
#163144=CARTESIAN_POINT('Ctrl Pts',(56.572670163045,1.92500670521764,-177.245708594735));
#163145=CARTESIAN_POINT('Ctrl Pts',(56.5732250495913,1.92289910945411,-177.240738434495));
#163146=CARTESIAN_POINT('Ctrl Pts',(56.5737702212793,1.9208278227753,-177.235743502986));
#163147=CARTESIAN_POINT('Ctrl Pts',(56.5742136264815,1.91914318047097,-177.231680968807));
#163148=CARTESIAN_POINT('Ctrl Pts',(56.5746500692504,1.91748459286997,-177.227606869171));
#163149=CARTESIAN_POINT('Ctrl Pts',(56.5750788200599,1.91585486103934,-177.223528406682));
#163150=CARTESIAN_POINT('Ctrl Pts',(56.5782241786983,1.90389898602246,-177.193608399685));
#163151=CARTESIAN_POINT('Ctrl Pts',(56.5809693098902,1.89344399206872,-177.163338973001));
#163152=CARTESIAN_POINT('Ctrl Pts',(56.5833278536963,1.88444881109869,-177.132732821239));
#163153=CARTESIAN_POINT('Ctrl Pts',(56.5857124029625,1.87535444866779,-177.101789204022));
#163154=CARTESIAN_POINT('Ctrl Pts',(56.5877019367001,1.86775166258739,-177.070499522563));
#163155=CARTESIAN_POINT('Ctrl Pts',(56.5892981114555,1.86164434117929,-177.038856203194));
#163156=CARTESIAN_POINT('Ctrl Pts',(56.5899925100869,1.85898741679645,-177.025090118004));
#163157=CARTESIAN_POINT('Ctrl Pts',(56.5906123032695,1.85661411889969,-177.011256862245));
#163158=CARTESIAN_POINT('Ctrl Pts',(56.5911568728243,1.85452762189294,-176.997354903683));
#163159=CARTESIAN_POINT('Ctrl Pts',(56.592110679146,1.85087315017689,-176.97300580843));
#163160=CARTESIAN_POINT('Ctrl Pts',(56.5928339105565,1.84809776611721,-176.948446283833));
#163161=CARTESIAN_POINT('Ctrl Pts',(56.593315736919,1.8462472490988,-176.923675152294));
#163162=CARTESIAN_POINT('Ctrl Pts',(56.5935566501002,1.8453219905896,-176.911289586525));
#163163=CARTESIAN_POINT('Ctrl Pts',(56.5937366253393,1.84463019464051,-176.898851402341));
#163164=CARTESIAN_POINT('Ctrl Pts',(56.5938590328877,1.84415954091471,-176.886362089455));
#163165=CARTESIAN_POINT('Ctrl Pts',(56.5939814404361,1.84368888718891,-176.87387277657));
#163166=CARTESIAN_POINT('Ctrl Pts',(56.5940462830325,1.84343935986365,-176.861332171026));
#163167=CARTESIAN_POINT('Ctrl Pts',(56.5940537057312,1.84341099694892,-176.848740272859));
#163168=CARTESIAN_POINT('Ctrl Pts',(56.3252430313217,2.83493642067777,-177.84995));
#163169=CARTESIAN_POINT('Ctrl Pts',(56.3252430313216,2.83493642067775,-177.34995));
#163170=CARTESIAN_POINT('Ctrl Pts',(56.8066553649227,2.96999998000003,-177.34995));
#163171=CARTESIAN_POINT('Ctrl Pts',(56.3976379760506,2.57689628418379,-177.849949962148));
#163172=CARTESIAN_POINT('Ctrl Pts',(56.3657038976309,2.69072016585579,-177.313059794074));
#163173=CARTESIAN_POINT('Ctrl Pts',(56.8796685247676,2.83987814625872,-177.34995));
#163174=CARTESIAN_POINT('Ctrl Pts',(56.4669147992933,2.32220551629932,-177.746434148089));
#163175=CARTESIAN_POINT('Ctrl Pts',(56.393446522619,2.59195606221812,-177.219869815671));
#163176=CARTESIAN_POINT('Ctrl Pts',(56.9495585329053,2.71140496526165,-177.298153784266));
#163177=CARTESIAN_POINT('Ctrl Pts',(56.5169491525424,2.13496529160036,-177.558207897086));
#163178=CARTESIAN_POINT('Ctrl Pts',(56.409292540301,2.5378414548249,-177.125154911669));
#163179=CARTESIAN_POINT('Ctrl Pts',(57.,2.61702308584988,-177.204078948543));
#163180=CARTESIAN_POINT('',(56.3252430313217,2.83493642067774,-177.84995));
#163181=CARTESIAN_POINT('Origin',(56.8066553649227,2.96999998000001,-177.84995));
#163182=CARTESIAN_POINT('Ctrl Pts',(56.3252430313217,2.83493642067774,-177.84995));
#163183=CARTESIAN_POINT('Ctrl Pts',(56.3337905757477,2.80447007335715,-177.849949995531));
#163184=CARTESIAN_POINT('Ctrl Pts',(56.3422168470079,2.77432812514565,-177.848511343748));
#163185=CARTESIAN_POINT('Ctrl Pts',(56.3505347180946,2.74447917084385,-177.845717295416));
#163186=CARTESIAN_POINT('Ctrl Pts',(56.3586925281077,2.71520460097504,-177.84297701305));
#163187=CARTESIAN_POINT('Ctrl Pts',(56.3667461939752,2.68621137428779,-177.838933157927));
#163188=CARTESIAN_POINT('Ctrl Pts',(56.3747119330389,2.65745132354449,-177.833612584578));
#163189=CARTESIAN_POINT('Ctrl Pts',(56.3826465426729,2.62880366462976,-177.828312803577));
#163190=CARTESIAN_POINT('Ctrl Pts',(56.3904942639185,2.60038604323579,-177.821746106604));
#163191=CARTESIAN_POINT('Ctrl Pts',(56.3982693165815,2.5721540750335,-177.813887718037));
#163192=CARTESIAN_POINT('Ctrl Pts',(56.4059472278018,2.54427483680477,-177.806127512112));
#163193=CARTESIAN_POINT('Ctrl Pts',(56.4135548018023,2.51657466550273,-177.797106929139));
#163194=CARTESIAN_POINT('Ctrl Pts',(56.4210985479533,2.48903439318015,-177.786757501498));
#163195=CARTESIAN_POINT('Ctrl Pts',(56.4239423298017,2.47865247881527,-177.782856055998));
#163196=CARTESIAN_POINT('Ctrl Pts',(56.426776958486,2.4682935670556,-177.778765345278));
#163197=CARTESIAN_POINT('Ctrl Pts',(56.4296024917091,2.45795762024076,-177.774480127077));
#163198=CARTESIAN_POINT('Ctrl Pts',(56.4379967235467,2.42725108558959,-177.761749391951));
#163199=CARTESIAN_POINT('Ctrl Pts',(56.4461165623565,2.39745763002353,-177.747600314328));
#163200=CARTESIAN_POINT('Ctrl Pts',(56.4539709812586,2.36855912289836,-177.73209578844));
#163201=CARTESIAN_POINT('Ctrl Pts',(56.4618532758604,2.33955805362101,-177.716536236265));
#163202=CARTESIAN_POINT('Ctrl Pts',(56.4694684313471,2.31145762034201,-177.699611308859));
#163203=CARTESIAN_POINT('Ctrl Pts',(56.4768213142896,2.28425147073979,-177.681333396443));
#163204=CARTESIAN_POINT('Ctrl Pts',(56.4840747389559,2.25741332328893,-177.663302718978));
#163205=CARTESIAN_POINT('Ctrl Pts',(56.4910730820105,2.23144484455675,-177.643955073003));
#163206=CARTESIAN_POINT('Ctrl Pts',(56.4978146447403,2.20636084783545,-177.623257500239));
#163207=CARTESIAN_POINT('Ctrl Pts',(56.5044442829978,2.18169329952633,-177.602903551794));
#163208=CARTESIAN_POINT('Ctrl Pts',(56.5108257274528,2.15788057710433,-177.581243854425));
#163209=CARTESIAN_POINT('Ctrl Pts',(56.5169491525424,2.13496529160041,-177.558207897086));
#163210=CARTESIAN_POINT('Origin',(0.,-12.9675000200281,-177.84995));
#163211=CARTESIAN_POINT('',(56.1837939657261,3.33069913254215,-177.84995));
#163212=CARTESIAN_POINT('Origin',(56.6639973329545,3.46999998000001,-177.84995));
#163213=CARTESIAN_POINT('Origin',(0.,-12.9675000200281,-177.84995));
#163214=CARTESIAN_POINT('Ctrl Pts',(55.8907344288187,4.30901060783351,-176.690850240902));
#163215=CARTESIAN_POINT('Ctrl Pts',(55.9989092657488,3.95901908419397,-176.752404542197));
#163216=CARTESIAN_POINT('Ctrl Pts',(56.3697825056489,3.96335046636153,-176.770466133952));
#163217=CARTESIAN_POINT('Ctrl Pts',(55.8810800353191,4.34006612171963,-176.874277739409));
#163218=CARTESIAN_POINT('Ctrl Pts',(55.9918208819094,3.98257552011186,-176.864245565378));
#163219=CARTESIAN_POINT('Ctrl Pts',(56.360041241732,3.97898206969736,-176.862106001368));
#163220=CARTESIAN_POINT('Ctrl Pts',(55.8887283478319,4.31560402300748,-177.06862236504));
#163221=CARTESIAN_POINT('Ctrl Pts',(55.9976409365186,3.96330447540303,-176.985952090623));
#163222=CARTESIAN_POINT('Ctrl Pts',(56.3677577343663,3.96667187476728,-176.959188328205));
#163223=CARTESIAN_POINT('Ctrl Pts',(55.9266115295683,4.19254080857125,-177.361891255001));
#163224=CARTESIAN_POINT('Ctrl Pts',(56.0241238299815,3.87468354526111,-177.158432257995));
#163225=CARTESIAN_POINT('Ctrl Pts',(56.4059865293426,3.90470993307104,-177.105730604552));
#163226=CARTESIAN_POINT('Ctrl Pts',(55.9498205047936,4.11690393979646,-177.473010794577));
#163227=CARTESIAN_POINT('Ctrl Pts',(56.0403831092186,3.82012609038464,-177.220853928335));
#163228=CARTESIAN_POINT('Ctrl Pts',(56.4294064346049,3.866625884224,-177.161267442876));
#163229=CARTESIAN_POINT('Ctrl Pts',(56.0057627129126,3.93261288273155,-177.655191732052));
#163230=CARTESIAN_POINT('Ctrl Pts',(56.0777953809631,3.69371421455791,-177.313208384807));
#163231=CARTESIAN_POINT('Ctrl Pts',(56.4858608229818,3.7738058294262,-177.252357953738));
#163232=CARTESIAN_POINT('Ctrl Pts',(56.0389442880078,3.82243329271981,-177.727752411286));
#163233=CARTESIAN_POINT('Ctrl Pts',(56.0994690237907,3.6200556053818,-177.343574237135));
#163234=CARTESIAN_POINT('Ctrl Pts',(56.51934628745,3.71830354331151,-177.288661380879));
#163235=CARTESIAN_POINT('Ctrl Pts',(56.1230975683705,3.53939517412226,-177.843941866969));
#163236=CARTESIAN_POINT('Ctrl Pts',(56.1514384840657,3.44234559640889,-177.375806045407));
#163237=CARTESIAN_POINT('Ctrl Pts',(56.6042740428564,3.57567859252058,-177.346848135714));
#163238=CARTESIAN_POINT('Ctrl Pts',(56.1775019211747,3.35356550968309,-177.866562127611));
#163239=CARTESIAN_POINT('Ctrl Pts',(56.1824782924758,3.33526976742397,-177.359497704487));
#163240=CARTESIAN_POINT('Ctrl Pts',(56.6591858730236,3.48199543258953,-177.358249465165));
#163241=CARTESIAN_POINT('Ctrl Pts',(56.2275049818161,3.17916207692579,-177.837621610915));
#163242=CARTESIAN_POINT('Ctrl Pts',(56.2060958053042,3.25377207835719,-177.320175302413));
#163243=CARTESIAN_POINT('Ctrl Pts',(56.7096544558747,3.39403127791385,-177.343857300475));
#163244=CARTESIAN_POINT('',(55.8866301012659,4.32222455627096,-176.84995));
#163245=CARTESIAN_POINT('',(56.3642936064049,3.96999998000001,-176.84995));
#163246=CARTESIAN_POINT('Origin',(56.3642936064049,4.46999998000001,-176.84995));
#163247=CARTESIAN_POINT('Ctrl Pts',(56.6639973329545,3.46999998000001,-177.34995));
#163248=CARTESIAN_POINT('Ctrl Pts',(56.6132926555039,3.55739556046625,-177.34995));
#163249=CARTESIAN_POINT('Ctrl Pts',(56.5711004619007,3.63103186791303,-177.32741150463));
#163250=CARTESIAN_POINT('Ctrl Pts',(56.5205808972673,3.71540754291555,-177.2866997194));
#163251=CARTESIAN_POINT('Ctrl Pts',(56.5058691633514,3.73942485859416,-177.271891810804));
#163252=CARTESIAN_POINT('Ctrl Pts',(56.4869937439203,3.76997568356519,-177.250163369964));
#163253=CARTESIAN_POINT('Ctrl Pts',(56.4812339676837,3.77925206162339,-177.242992983045));
#163254=CARTESIAN_POINT('Ctrl Pts',(56.4733923486896,3.79192114453357,-177.232568181681));
#163255=CARTESIAN_POINT('Ctrl Pts',(56.4696710505327,3.79794447782133,-177.227437770765));
#163256=CARTESIAN_POINT('Ctrl Pts',(56.4656786808617,3.80445324466831,-177.221637219552));
#163257=CARTESIAN_POINT('Ctrl Pts',(56.4640424820409,3.80713442288003,-177.21919490467));
#163258=CARTESIAN_POINT('Ctrl Pts',(56.4629683087721,3.80889811921587,-177.217576826329));
#163259=CARTESIAN_POINT('Ctrl Pts',(56.4629360063793,3.80894940169979,-177.217534734494));
#163260=CARTESIAN_POINT('Ctrl Pts',(56.3968354290769,3.91795014829009,-177.116097367134));
#163261=CARTESIAN_POINT('Ctrl Pts',(56.3642936064049,3.96999998000001,-176.977117050922));
#163262=CARTESIAN_POINT('Ctrl Pts',(56.3642936064049,3.96999998000001,-176.84995));
#163263=CARTESIAN_POINT('Ctrl Pts',(55.8866301012659,4.32222455627096,-176.84995));
#163264=CARTESIAN_POINT('Ctrl Pts',(55.8866301033422,4.3222245495596,-176.887711783017));
#163265=CARTESIAN_POINT('Ctrl Pts',(55.8873019941254,4.32005750494367,-176.925285001291));
#163266=CARTESIAN_POINT('Ctrl Pts',(55.8886053322676,4.31584578460431,-176.962497615251));
#163267=CARTESIAN_POINT('Ctrl Pts',(55.8899346297675,4.31155017693619,-177.000451414885));
#163268=CARTESIAN_POINT('Ctrl Pts',(55.8919208352951,4.30512748218138,-177.038031169975));
#163269=CARTESIAN_POINT('Ctrl Pts',(55.8945372498695,4.2966554166734,-177.075061157623));
#163270=CARTESIAN_POINT('Ctrl Pts',(55.8971529093906,4.28818579606139,-177.112080459038));
#163271=CARTESIAN_POINT('Ctrl Pts',(55.9003985106906,4.27766770883152,-177.148551411106));
#163272=CARTESIAN_POINT('Ctrl Pts',(55.9042621819464,4.26513074059417,-177.184288779349));
#163273=CARTESIAN_POINT('Ctrl Pts',(55.9062291959159,4.25874810862931,-177.202482848646));
#163274=CARTESIAN_POINT('Ctrl Pts',(55.9083566338582,4.25184146461301,-177.22048652526));
#163275=CARTESIAN_POINT('Ctrl Pts',(55.9106442880651,4.24441025685161,-177.238272995257));
#163276=CARTESIAN_POINT('Ctrl Pts',(55.9107052688196,4.24421216718633,-177.238747119518));
#163277=CARTESIAN_POINT('Ctrl Pts',(55.9107663607186,4.2440137135512,-177.239221068301));
#163278=CARTESIAN_POINT('Ctrl Pts',(55.9108275637053,4.24381489610749,-177.239694840879));
#163279=CARTESIAN_POINT('Ctrl Pts',(55.9214558682229,4.20928892853583,-177.321968590921));
#163280=CARTESIAN_POINT('Ctrl Pts',(55.9354579988728,4.16369334127204,-177.399293819936));
#163281=CARTESIAN_POINT('Ctrl Pts',(55.9520401750176,4.10936168614259,-177.468909678493));
#163282=CARTESIAN_POINT('Ctrl Pts',(55.9599200188449,4.08354330419055,-177.501991108129));
#163283=CARTESIAN_POINT('Ctrl Pts',(55.9683824151874,4.05575233687934,-177.533330971157));
#163284=CARTESIAN_POINT('Ctrl Pts',(55.977341715845,4.02624042822255,-177.562628970791));
#163285=CARTESIAN_POINT('Ctrl Pts',(55.9774917411594,4.02574624530113,-177.563119571762));
#163286=CARTESIAN_POINT('Ctrl Pts',(55.9776419059241,4.025251579432,-177.563609601226));
#163287=CARTESIAN_POINT('Ctrl Pts',(55.9777922097306,4.02475643181778,-177.564099057738));
#163288=CARTESIAN_POINT('Ctrl Pts',(55.9952457911942,3.96725889118211,-177.620935736125));
#163289=CARTESIAN_POINT('Ctrl Pts',(56.01475026219,3.90266672703547,-177.67062951941));
#163290=CARTESIAN_POINT('Ctrl Pts',(56.0354959803716,3.83347839359387,-177.711737746814));
#163291=CARTESIAN_POINT('Ctrl Pts',(56.0478214929256,3.79237199925456,-177.736161098587));
#163292=CARTESIAN_POINT('Ctrl Pts',(56.0605847921289,3.74964437877247,-177.757554032042));
#163293=CARTESIAN_POINT('Ctrl Pts',(56.0736137591996,3.70582717944107,-177.775616713982));
#163294=CARTESIAN_POINT('Ctrl Pts',(56.0737452759341,3.7053848807584,-177.775799041938));
#163295=CARTESIAN_POINT('Ctrl Pts',(56.0738768160358,3.70494248350759,-177.775981025699));
#163296=CARTESIAN_POINT('Ctrl Pts',(56.0740083793673,3.7044999881052,-177.776162665075));
#163297=CARTESIAN_POINT('Ctrl Pts',(56.0854652800848,3.66596625811822,-177.791980326975));
#163298=CARTESIAN_POINT('Ctrl Pts',(56.0971863579253,3.62638912180278,-177.805308764985));
#163299=CARTESIAN_POINT('Ctrl Pts',(56.1090759206044,3.58608423515434,-177.816113161796));
#163300=CARTESIAN_POINT('Ctrl Pts',(56.1213067753347,3.54462238943049,-177.827227700776));
#163301=CARTESIAN_POINT('Ctrl Pts',(56.1337163559748,3.502389009303,-177.835671763787));
#163302=CARTESIAN_POINT('Ctrl Pts',(56.1462034955942,3.45971409454014,-177.841352247251));
#163303=CARTESIAN_POINT('Ctrl Pts',(56.1579134207248,3.41969531745755,-177.846679170638));
#163304=CARTESIAN_POINT('Ctrl Pts',(56.1696918925472,3.37928709608564,-177.849575574952));
#163305=CARTESIAN_POINT('Ctrl Pts',(56.1814524996762,3.33876843673258,-177.849916077404));
#163306=CARTESIAN_POINT('Ctrl Pts',(56.182233078045,3.33607912072376,-177.84993867733));
#163307=CARTESIAN_POINT('Ctrl Pts',(56.1830135754985,3.33338932446759,-177.849949999684));
#163308=CARTESIAN_POINT('Ctrl Pts',(56.1837939657261,3.33069913254215,-177.84995));
#163309=CARTESIAN_POINT('Origin',(0.,-12.9675000200281,-171.871644662643));
#163310=CARTESIAN_POINT('',(53.8350584096845,9.92434320033876,-171.871644662643));
#163311=CARTESIAN_POINT('',(55.8866301012659,4.32222455627096,-171.871644662643));
#163312=CARTESIAN_POINT('Origin',(0.,-12.9675000200281,-171.871644662643));
#163313=CARTESIAN_POINT('Origin',(52.5977860076314,10.1271303560196,-171.886170842901));
#163314=CARTESIAN_POINT('Origin',(54.5615907362999,4.49781486075725,-171.920628921479));
#163315=CARTESIAN_POINT('Ctrl Pts',(53.4025720561297,10.9158686240697,-177.84995));
#163316=CARTESIAN_POINT('Ctrl Pts',(53.4025720561301,10.9158686240688,-177.34995));
#163317=CARTESIAN_POINT('Ctrl Pts',(53.8590042959257,11.1199999800011,-177.34995));
#163318=CARTESIAN_POINT('Ctrl Pts',(53.4583000366404,10.7912623535259,-177.849949984912));
#163319=CARTESIAN_POINT('Ctrl Pts',(53.4357429270681,10.8416994438452,-177.323612898224));
#163320=CARTESIAN_POINT('Ctrl Pts',(53.9152095126149,11.0571633006792,-177.34995));
#163321=CARTESIAN_POINT('Ctrl Pts',(53.5126282698489,10.6685980808388,-177.826730821509));
#163322=CARTESIAN_POINT('Ctrl Pts',(53.4634087021834,10.7796461652398,-177.282275394088));
#163323=CARTESIAN_POINT('Ctrl Pts',(53.9700011606116,10.9953079956486,-177.338340413074));
#163324=CARTESIAN_POINT('Ctrl Pts',(53.6159658107279,10.4332420187126,-177.732767091856));
#163325=CARTESIAN_POINT('Ctrl Pts',(53.5073796187504,10.6816635307577,-177.18321412648));
#163326=CARTESIAN_POINT('Ctrl Pts',(54.0742219292009,10.8766241714759,-177.291358543608));
#163327=CARTESIAN_POINT('Ctrl Pts',(53.6629085389549,10.3252623899094,-177.663867719202));
#163328=CARTESIAN_POINT('Ctrl Pts',(53.5219518286219,10.649686808137,-177.127170956772));
#163329=CARTESIAN_POINT('Ctrl Pts',(54.1215658763003,10.8221729031368,-177.256908861057));
#163330=CARTESIAN_POINT('Ctrl Pts',(53.7443081182388,10.1368259480206,-177.482357798918));
#163331=CARTESIAN_POINT('Ctrl Pts',(53.5394251697822,10.6131024574854,-177.020421798311));
#163332=CARTESIAN_POINT('Ctrl Pts',(54.2036611796727,10.7271494012897,-177.166153898004));
#163333=CARTESIAN_POINT('Ctrl Pts',(53.7772720937282,10.0598397490546,-177.372348961349));
#163334=CARTESIAN_POINT('Ctrl Pts',(53.5413185515592,10.6107526879388,-176.973405437982));
#163335=CARTESIAN_POINT('Ctrl Pts',(54.2369068974943,10.6883272976786,-177.111149481396));
#163336=CARTESIAN_POINT('Ctrl Pts',(53.8228725022638,9.95305333910152,-177.124428650036));
#163337=CARTESIAN_POINT('Ctrl Pts',(53.5410688387025,10.6146700040362,-176.899444869037));
#163338=CARTESIAN_POINT('Ctrl Pts',(54.282897054019,10.6344777440414,-176.987189324297));
#163339=CARTESIAN_POINT('Ctrl Pts',(53.8350584050868,9.92434321115133,-176.989642564215));
#163340=CARTESIAN_POINT('Ctrl Pts',(53.5392499462662,10.6199999783344,-176.8744703999));
#163341=CARTESIAN_POINT('Ctrl Pts',(54.2951871094022,10.61999998,-176.919796282647));
#163342=CARTESIAN_POINT('Ctrl Pts',(53.8350584096845,9.92434320033874,-176.84995));
#163343=CARTESIAN_POINT('Ctrl Pts',(53.5392499457278,10.61999998,-176.84995));
#163344=CARTESIAN_POINT('Ctrl Pts',(54.2951871140408,10.61999998,-176.84995));
#163345=CARTESIAN_POINT('',(54.2951871140408,10.61999998,-176.84995));
#163346=CARTESIAN_POINT('',(53.8350584096845,9.92434320033876,-176.84995));
#163347=CARTESIAN_POINT('Origin',(54.2951871140408,10.11999998,-176.84995));
#163348=CARTESIAN_POINT('',(53.4025720561307,10.9158686240676,-177.84995));
#163349=CARTESIAN_POINT('Ctrl Pts',(53.4025720561307,10.9158686240675,-177.84995));
#163350=CARTESIAN_POINT('Ctrl Pts',(53.4256992941538,10.8641567398107,-177.849949993739));
#163351=CARTESIAN_POINT('Ctrl Pts',(53.4485179803107,10.8129304526924,-177.845955353724));
#163352=CARTESIAN_POINT('Ctrl Pts',(53.4709798749291,10.7623159210356,-177.837971298851));
#163353=CARTESIAN_POINT('Ctrl Pts',(53.4932283385006,10.7121823244322,-177.8300631078));
#163354=CARTESIAN_POINT('Ctrl Pts',(53.5151269426183,10.6626484619091,-177.818240932981));
#163355=CARTESIAN_POINT('Ctrl Pts',(53.5366259143439,10.613840772558,-177.80245915115));
#163356=CARTESIAN_POINT('Ctrl Pts',(53.5459258227761,10.5927278073638,-177.795632353674));
#163357=CARTESIAN_POINT('Ctrl Pts',(53.5551508985508,10.5717508130024,-177.788063986787));
#163358=CARTESIAN_POINT('Ctrl Pts',(53.5642968110718,10.5509205718341,-177.77974738364));
#163359=CARTESIAN_POINT('Ctrl Pts',(53.5644850520156,10.5504918443291,-177.779576211522));
#163360=CARTESIAN_POINT('Ctrl Pts',(53.5646732319863,10.5500632415521,-177.779404746864));
#163361=CARTESIAN_POINT('Ctrl Pts',(53.5648613509312,10.5496347636521,-177.779232989633));
#163362=CARTESIAN_POINT('Ctrl Pts',(53.5997722939237,10.4701182239948,-177.747358438588));
#163363=CARTESIAN_POINT('Ctrl Pts',(53.6324973478409,10.3950941639631,-177.705483670659));
#163364=CARTESIAN_POINT('Ctrl Pts',(53.662565751538,10.3258245179345,-177.653697116807));
#163365=CARTESIAN_POINT('Ctrl Pts',(53.6768635990437,10.292886060487,-177.629072056652));
#163366=CARTESIAN_POINT('Ctrl Pts',(53.6905609342839,10.2612483121622,-177.602206386713));
#163367=CARTESIAN_POINT('Ctrl Pts',(53.7036082895117,10.2310442594454,-177.573112646646));
#163368=CARTESIAN_POINT('Ctrl Pts',(53.7038266840866,10.2305386856232,-177.572625657913));
#163369=CARTESIAN_POINT('Ctrl Pts',(53.7040448535835,10.2300336133805,-177.572138119876));
#163370=CARTESIAN_POINT('Ctrl Pts',(53.7042627976345,10.2295290436849,-177.571650033405));
#163371=CARTESIAN_POINT('Ctrl Pts',(53.7326736221979,10.1637541760665,-177.508023891492));
#163372=CARTESIAN_POINT('Ctrl Pts',(53.7572655280445,10.1064913273751,-177.435049789256));
#163373=CARTESIAN_POINT('Ctrl Pts',(53.7772301637647,10.0598657379883,-177.354607724291));
#163374=CARTESIAN_POINT('Ctrl Pts',(53.7856960958606,10.0400943242139,-177.320496555463));
#163375=CARTESIAN_POINT('Ctrl Pts',(53.7933301997489,10.0222350963587,-177.28504246553));
#163376=CARTESIAN_POINT('Ctrl Pts',(53.8000719149495,10.0064474410942,-177.248388344963));
#163377=CARTESIAN_POINT('Ctrl Pts',(53.8001626051628,10.0062350640088,-177.247895270142));
#163378=CARTESIAN_POINT('Ctrl Pts',(53.8002531267728,10.006023079014,-177.247402027608));
#163379=CARTESIAN_POINT('Ctrl Pts',(53.800343479687,10.005811486348,-177.246908617746));
#163380=CARTESIAN_POINT('Ctrl Pts',(53.8073717082883,9.98935245300704,-177.208528037134));
#163381=CARTESIAN_POINT('Ctrl Pts',(53.8133972227366,9.97522506645289,-177.169027476767));
#163382=CARTESIAN_POINT('Ctrl Pts',(53.8183528652338,9.96359686430571,-177.128668162154));
#163383=CARTESIAN_POINT('Ctrl Pts',(53.8232487909443,9.95210878503228,-177.088795187826));
#163384=CARTESIAN_POINT('Ctrl Pts',(53.8271003741327,9.94306028562344,-177.048084581928));
#163385=CARTESIAN_POINT('Ctrl Pts',(53.829861825915,9.93656859429008,-177.006803377711));
#163386=CARTESIAN_POINT('Ctrl Pts',(53.8325710248907,9.93019974018788,-176.966303305646));
#163387=CARTESIAN_POINT('Ctrl Pts',(53.8342309082794,9.92629199069111,-176.925254528035));
#163388=CARTESIAN_POINT('Ctrl Pts',(53.8348176649726,9.92491022336675,-176.883916088102));
#163389=CARTESIAN_POINT('Ctrl Pts',(53.8349780875801,9.92453244034421,-176.872613924192));
#163390=CARTESIAN_POINT('Ctrl Pts',(53.8350584093113,9.92434320121651,-176.861290124361));
#163391=CARTESIAN_POINT('Ctrl Pts',(53.8350584096845,9.92434320033876,-176.84995));
#163392=CARTESIAN_POINT('Origin',(53.8590042959267,11.11999998,-177.84995));
#163393=CARTESIAN_POINT('Ctrl Pts',(54.2951871140408,10.61999998,-176.84995));
#163394=CARTESIAN_POINT('Ctrl Pts',(54.295187112658,10.61999998,-176.870771477027));
#163395=CARTESIAN_POINT('Ctrl Pts',(54.2940343032734,10.6212900755915,-176.891794363281));
#163396=CARTESIAN_POINT('Ctrl Pts',(54.2916911849701,10.6239505106872,-176.912836670541));
#163397=CARTESIAN_POINT('Ctrl Pts',(54.2893026016019,10.6266625679541,-176.934287275524));
#163398=CARTESIAN_POINT('Ctrl Pts',(54.2856770724215,10.630798428608,-176.955757775013));
#163399=CARTESIAN_POINT('Ctrl Pts',(54.280809897557,10.6364012547725,-176.977053069232));
#163400=CARTESIAN_POINT('Ctrl Pts',(54.2757855218655,10.6421850419525,-176.999036162422));
#163401=CARTESIAN_POINT('Ctrl Pts',(54.2694380093634,10.649531872693,-177.020832355256));
#163402=CARTESIAN_POINT('Ctrl Pts',(54.2617991887197,10.6584484085697,-177.042228441581));
#163403=CARTESIAN_POINT('Ctrl Pts',(54.2609825719224,10.6594016176199,-177.044515758473));
#163404=CARTESIAN_POINT('Ctrl Pts',(54.260151231088,10.660372730439,-177.046798505411));
#163405=CARTESIAN_POINT('Ctrl Pts',(54.2593052287969,10.6613617303426,-177.049076423852));
#163406=CARTESIAN_POINT('Ctrl Pts',(54.2589052193173,10.6618293524056,-177.050153476455));
#163407=CARTESIAN_POINT('Ctrl Pts',(54.2585020693351,10.66230080757,-177.051228977642));
#163408=CARTESIAN_POINT('Ctrl Pts',(54.2580957907476,10.6627760870642,-177.052302900297));
#163409=CARTESIAN_POINT('Ctrl Pts',(54.2504067447387,10.67177101323,-177.072627477953));
#163410=CARTESIAN_POINT('Ctrl Pts',(54.2415263947062,10.6822029113807,-177.092532024772));
#163411=CARTESIAN_POINT('Ctrl Pts',(54.2314451843677,10.6940494493327,-177.111801613672));
#163412=CARTESIAN_POINT('Ctrl Pts',(54.2253160858662,10.7012518184505,-177.123516993521));
#163413=CARTESIAN_POINT('Ctrl Pts',(54.2187437276912,10.7089763005547,-177.134997409078));
#163414=CARTESIAN_POINT('Ctrl Pts',(54.2117316348916,10.7172105764342,-177.146192801267));
#163415=CARTESIAN_POINT('Ctrl Pts',(54.2024588038328,10.7280996292896,-177.160997651028));
#163416=CARTESIAN_POINT('Ctrl Pts',(54.192413237421,10.7398811588086,-177.175304855698));
#163417=CARTESIAN_POINT('Ctrl Pts',(54.1815949348861,10.752515497233,-177.188999491326));
#163418=CARTESIAN_POINT('Ctrl Pts',(54.1761857836187,10.7588326664453,-177.19584680914));
#163419=CARTESIAN_POINT('Ctrl Pts',(54.1705834483029,10.765362824047,-177.202540970492));
#163420=CARTESIAN_POINT('Ctrl Pts',(54.1647879289713,10.7720997079721,-177.209067514237));
#163421=CARTESIAN_POINT('Ctrl Pts',(54.1640579820703,10.7729482199452,-177.209889533819));
#163422=CARTESIAN_POINT('Ctrl Pts',(54.1633248766812,10.7738001056606,-177.210708987479));
#163423=CARTESIAN_POINT('Ctrl Pts',(54.1625884803548,10.7746554933064,-177.211525975779));
#163424=CARTESIAN_POINT('Ctrl Pts',(54.1604015139413,10.7771958428235,-177.213952286052));
#163425=CARTESIAN_POINT('Ctrl Pts',(54.158189835222,10.779762066631,-177.216353164041));
#163426=CARTESIAN_POINT('Ctrl Pts',(54.1559497621978,10.7823577707401,-177.218731355435));
#163427=CARTESIAN_POINT('Ctrl Pts',(54.1544525864815,10.7840926361293,-177.220320843977));
#163428=CARTESIAN_POINT('Ctrl Pts',(54.1529433368185,10.7858400389663,-177.221899598547));
#163429=CARTESIAN_POINT('Ctrl Pts',(54.1514220132121,10.7875999079006,-177.223467359814));
#163430=CARTESIAN_POINT('Ctrl Pts',(54.1502918620496,10.7889072680923,-177.22463200829));
#163431=CARTESIAN_POINT('Ctrl Pts',(54.1487914911753,10.7906414389948,-177.226158503531));
#163432=CARTESIAN_POINT('Ctrl Pts',(54.1477305915031,10.7918671107764,-177.22722583738));
#163433=CARTESIAN_POINT('Ctrl Pts',(54.147363388662,10.7922913451995,-177.227595267244));
#163434=CARTESIAN_POINT('Ctrl Pts',(54.147049085478,10.7926543863909,-177.227910135178));
#163435=CARTESIAN_POINT('Ctrl Pts',(54.146821820558,10.7929168335172,-177.228137406876));
#163436=CARTESIAN_POINT('Ctrl Pts',(54.1342953618731,10.8073824760096,-177.240664239137));
#163437=CARTESIAN_POINT('Ctrl Pts',(54.1198488297753,10.8238052428689,-177.25344441977));
#163438=CARTESIAN_POINT('Ctrl Pts',(54.1034633204787,10.842370556489,-177.265842564197));
#163439=CARTESIAN_POINT('Ctrl Pts',(54.088970645158,10.8587912278061,-177.276808490156));
#163440=CARTESIAN_POINT('Ctrl Pts',(54.0729605932981,10.8768889662157,-177.287474913187));
#163441=CARTESIAN_POINT('Ctrl Pts',(54.0554395607018,10.8967687287218,-177.297375727477));
#163442=CARTESIAN_POINT('Ctrl Pts',(54.0480420828295,10.905162075543,-177.301555906597));
#163443=CARTESIAN_POINT('Ctrl Pts',(54.0403755551798,10.913872699112,-177.305599307741));
#163444=CARTESIAN_POINT('Ctrl Pts',(54.0324419334657,10.9229063569136,-177.309469503735));
#163445=CARTESIAN_POINT('Ctrl Pts',(54.0287742229151,10.9270826137637,-177.311258693993));
#163446=CARTESIAN_POINT('Ctrl Pts',(54.0250526063655,10.9313257163362,-177.313010020251));
#163447=CARTESIAN_POINT('Ctrl Pts',(54.0212673431407,10.9356453298748,-177.314723399853));
#163448=CARTESIAN_POINT('Ctrl Pts',(54.0188642208532,10.938387691225,-177.315811160589));
#163449=CARTESIAN_POINT('Ctrl Pts',(54.0164398861093,10.9411558257346,-177.316881633396));
#163450=CARTESIAN_POINT('Ctrl Pts',(54.0139919510376,10.9439520922684,-177.317934517196));
#163451=CARTESIAN_POINT('Ctrl Pts',(53.9984512906739,10.9617041270301,-177.324618726156));
#163452=CARTESIAN_POINT('Ctrl Pts',(53.9819783775985,10.9805730655438,-177.330584054845));
#163453=CARTESIAN_POINT('Ctrl Pts',(53.9645670843843,11.0004694748766,-177.33549234988));
#163454=CARTESIAN_POINT('Ctrl Pts',(53.9572593724224,11.0088202175061,-177.337552415488));
#163455=CARTESIAN_POINT('Ctrl Pts',(53.9497866998397,11.01735154001,-177.339426565227));
#163456=CARTESIAN_POINT('Ctrl Pts',(53.9421501581125,11.0260550554856,-177.341091294699));
#163457=CARTESIAN_POINT('Ctrl Pts',(53.9232699100964,11.0475732422071,-177.345207098219));
#163458=CARTESIAN_POINT('Ctrl Pts',(53.903385736146,11.0701430681308,-177.348040800477));
#163459=CARTESIAN_POINT('Ctrl Pts',(53.8824911975385,11.0936551403296,-177.349265802689));
#163460=CARTESIAN_POINT('Ctrl Pts',(53.8747985514822,11.102311471674,-177.349716806112));
#163461=CARTESIAN_POINT('Ctrl Pts',(53.8669692913113,11.1110952218607,-177.34995));
#163462=CARTESIAN_POINT('Ctrl Pts',(53.8590042959267,11.11999998,-177.34995));
#163463=CARTESIAN_POINT('Origin',(0.,-12.9675000200281,-177.84995));
#163464=CARTESIAN_POINT('',(53.1780777607544,11.411631335932,-177.84995));
#163465=CARTESIAN_POINT('Origin',(0.,-12.9675000200281,-177.84995));
#163466=CARTESIAN_POINT('Origin',(53.6325912458891,11.61999998,-177.84995));
#163467=CARTESIAN_POINT('Ctrl Pts',(52.9099958749003,11.9881018181948,-177.663675223808));
#163468=CARTESIAN_POINT('Ctrl Pts',(52.9997517486903,11.797676512519,-177.337555142414));
#163469=CARTESIAN_POINT('Ctrl Pts',(53.3622278820666,11.9106883715865,-177.256778275814));
#163470=CARTESIAN_POINT('Ctrl Pts',(52.9976548387626,11.8022980130591,-177.797387815582));
#163471=CARTESIAN_POINT('Ctrl Pts',(53.0664188011436,11.6545589022485,-177.39893190434));
#163472=CARTESIAN_POINT('Ctrl Pts',(53.4506644997516,11.8169620310944,-177.323650098968));
#163473=CARTESIAN_POINT('Ctrl Pts',(53.1011582398324,11.5800093343372,-177.861139569353));
#163474=CARTESIAN_POINT('Ctrl Pts',(53.1375549029137,11.499963173746,-177.390455278679));
#163475=CARTESIAN_POINT('Ctrl Pts',(53.5550086872502,11.7049144813144,-177.355501814437));
#163476=CARTESIAN_POINT('Ctrl Pts',(53.2037302934161,11.3555915204785,-177.848448015576));
#163477=CARTESIAN_POINT('Ctrl Pts',(53.1927421255947,11.3794221790895,-177.337053842004));
#163478=CARTESIAN_POINT('Ctrl Pts',(53.6584638339975,11.5917397245118,-177.349157933747));
#163479=CARTESIAN_POINT('',(52.9322463618642,11.9408779899289,-177.695579616717));
#163480=CARTESIAN_POINT('Ctrl Pts',(52.9322463618642,11.940877989929,-177.695579616717));
#163481=CARTESIAN_POINT('Ctrl Pts',(52.9695658609497,11.861571143096,-177.746066773083));
#163482=CARTESIAN_POINT('Ctrl Pts',(53.009594439893,11.7760355127808,-177.784659368904));
#163483=CARTESIAN_POINT('Ctrl Pts',(53.0510018552188,11.6869357301078,-177.810630175633));
#163484=CARTESIAN_POINT('Ctrl Pts',(53.0924092705445,11.5978359474347,-177.836600982362));
#163485=CARTESIAN_POINT('Ctrl Pts',(53.1351948005685,11.5051717233266,-177.84995));
#163486=CARTESIAN_POINT('Ctrl Pts',(53.1780777607544,11.411631335932,-177.84995));
#163487=CARTESIAN_POINT('',(53.3846587239314,11.8868850448361,-177.272764808359));
#163488=CARTESIAN_POINT('Origin',(53.3846587239314,12.1537701096722,-177.695579616717));
#163489=CARTESIAN_POINT('Ctrl Pts',(53.6325912458891,11.61999998,-177.34995));
#163490=CARTESIAN_POINT('Ctrl Pts',(53.6193902496202,11.6343976136465,-177.34995));
#163491=CARTESIAN_POINT('Ctrl Pts',(53.6071216945481,11.647745990074,-177.349336222758));
#163492=CARTESIAN_POINT('Ctrl Pts',(53.5958029190205,11.6600403513377,-177.348353185436));
#163493=CARTESIAN_POINT('Ctrl Pts',(53.5831048880715,11.6738328485423,-177.347250359578));
#163494=CARTESIAN_POINT('Ctrl Pts',(53.5715986168778,11.6863027073468,-177.345682762576));
#163495=CARTESIAN_POINT('Ctrl Pts',(53.5613057001372,11.6974417930555,-177.343941078924));
#163496=CARTESIAN_POINT('Ctrl Pts',(53.5514335858369,11.7081254826343,-177.342270600037));
#163497=CARTESIAN_POINT('Ctrl Pts',(53.5426828084495,11.7175793620638,-177.34044118093));
#163498=CARTESIAN_POINT('Ctrl Pts',(53.535036882964,11.7258313494675,-177.338656510057));
#163499=CARTESIAN_POINT('Ctrl Pts',(53.5312693392627,11.7298975312822,-177.337777110235));
#163500=CARTESIAN_POINT('Ctrl Pts',(53.5277703317232,11.7336715434635,-177.33690786316));
#163501=CARTESIAN_POINT('Ctrl Pts',(53.5245383140635,11.7371559990051,-177.336068813023));
#163502=CARTESIAN_POINT('Ctrl Pts',(53.5207506930954,11.7412394534479,-177.335085525112));
#163503=CARTESIAN_POINT('Ctrl Pts',(53.5173269143261,11.7449241460667,-177.334144097169));
#163504=CARTESIAN_POINT('Ctrl Pts',(53.5142595429646,11.7482126391687,-177.333272132227));
#163505=CARTESIAN_POINT('Ctrl Pts',(53.5127258572839,11.7498568857197,-177.332836149756));
#163506=CARTESIAN_POINT('Ctrl Pts',(53.5112838669721,11.7514031852974,-177.332417154949));
#163507=CARTESIAN_POINT('Ctrl Pts',(53.5099335719791,11.752852238671,-177.332017926533));
#163508=CARTESIAN_POINT('Ctrl Pts',(53.5092584244826,11.7535767653578,-177.331818312325));
#163509=CARTESIAN_POINT('Ctrl Pts',(53.5086062008165,11.7542769791225,-177.331623634357));
#163510=CARTESIAN_POINT('Ctrl Pts',(53.507976900977,11.7549529596041,-177.331434207795));
#163511=CARTESIAN_POINT('Ctrl Pts',(53.5076622510572,11.7552909498449,-177.331339494514));
#163512=CARTESIAN_POINT('Ctrl Pts',(53.5075769762504,11.7553821019031,-177.331313791835));
#163513=CARTESIAN_POINT('Ctrl Pts',(53.507385610281,11.7555876789724,-177.331255890439));
#163514=CARTESIAN_POINT('Ctrl Pts',(53.5071942443116,11.7557932560417,-177.331197989043));
#163515=CARTESIAN_POINT('Ctrl Pts',(53.5068967871326,11.7561133566317,-177.331108233285));
#163516=CARTESIAN_POINT('Ctrl Pts',(53.5061577729354,11.7569082763594,-177.330881975835));
#163517=CARTESIAN_POINT('Ctrl Pts',(53.4886819350222,11.7757061402844,-177.325531552884));
#163518=CARTESIAN_POINT('Ctrl Pts',(53.4721182870987,11.7934851338263,-177.31927585382));
#163519=CARTESIAN_POINT('Ctrl Pts',(53.4564928503932,11.8102233474837,-177.312383460726));
#163520=CARTESIAN_POINT('Ctrl Pts',(53.4400282994755,11.8278604334882,-177.305120933657));
#163521=CARTESIAN_POINT('Ctrl Pts',(53.4246052146097,11.8443421754681,-177.297151753489));
#163522=CARTESIAN_POINT('Ctrl Pts',(53.4102166329,11.8596818104284,-177.28876587707));
#163523=CARTESIAN_POINT('Ctrl Pts',(53.4013036283722,11.8691839447327,-177.283571247327));
#163524=CARTESIAN_POINT('Ctrl Pts',(53.3927868566238,11.8782485868146,-177.278216229675));
#163525=CARTESIAN_POINT('Ctrl Pts',(53.3846587239315,11.8868850448361,-177.272764808359));
#163526=CARTESIAN_POINT('Ctrl Pts',(52.1126146143195,13.5388501432916,-171.391638125813));
#163527=CARTESIAN_POINT('Ctrl Pts',(52.4864722882118,13.5059760932666,-171.679515584751));
#163528=CARTESIAN_POINT('Ctrl Pts',(52.5050296388285,13.3739336825608,-172.133326251627));
#163529=CARTESIAN_POINT('Ctrl Pts',(52.2275734081837,13.1702746923549,-171.333188379966));
#163530=CARTESIAN_POINT('Ctrl Pts',(52.5259488232545,13.163017811976,-171.621133646225));
#163531=CARTESIAN_POINT('Ctrl Pts',(52.5511257748791,13.045942631788,-172.016544094259));
#163532=CARTESIAN_POINT('Ctrl Pts',(52.3625569744519,12.7995634785289,-171.277518845311));
#163533=CARTESIAN_POINT('Ctrl Pts',(52.6036316644729,12.8055197818762,-171.550813695775));
#163534=CARTESIAN_POINT('Ctrl Pts',(52.6287970696452,12.7242148673197,-171.90506362857));
#163535=CARTESIAN_POINT('Ctrl Pts',(52.521634376552,12.4186874453849,-171.247275980756));
#163536=CARTESIAN_POINT('Ctrl Pts',(52.7259743335333,12.4493753091149,-171.512222020089));
#163537=CARTESIAN_POINT('Ctrl Pts',(52.7423614633688,12.4030287528935,-171.844601961512));
#163538=CARTESIAN_POINT('',(52.7229719177955,12.458911061641,-171.855631342512));
#163539=CARTESIAN_POINT('Ctrl Pts',(52.5103993792154,12.4456688476555,-171.249463186897));
#163540=CARTESIAN_POINT('Ctrl Pts',(52.5297066417322,12.4444102902161,-171.271932598649));
#163541=CARTESIAN_POINT('Ctrl Pts',(52.5475880394989,12.4433468997068,-171.294915021113));
#163542=CARTESIAN_POINT('Ctrl Pts',(52.5640300074807,12.442495320782,-171.318251747026));
#163543=CARTESIAN_POINT('Ctrl Pts',(52.5803556661806,12.4416497658643,-171.341423390643));
#163544=CARTESIAN_POINT('Ctrl Pts',(52.5952623602387,12.441013117922,-171.364944185641));
#163545=CARTESIAN_POINT('Ctrl Pts',(52.6087807058339,12.4405907657944,-171.388635430273));
#163546=CARTESIAN_POINT('Ctrl Pts',(52.623312668846,12.4401367453337,-171.414103065219));
#163547=CARTESIAN_POINT('Ctrl Pts',(52.6362425608597,12.4399303027981,-171.439769352997));
#163548=CARTESIAN_POINT('Ctrl Pts',(52.647675798678,12.4399636610286,-171.465430214553));
#163549=CARTESIAN_POINT('Ctrl Pts',(52.6522530291883,12.4399770158029,-171.475703391785));
#163550=CARTESIAN_POINT('Ctrl Pts',(52.6565910749825,12.4400286515715,-171.485976052153));
#163551=CARTESIAN_POINT('Ctrl Pts',(52.6606989661368,12.4401175158482,-171.49623639269));
#163552=CARTESIAN_POINT('Ctrl Pts',(52.6630824957991,12.44016907774,-171.502189770006));
#163553=CARTESIAN_POINT('Ctrl Pts',(52.6652494160276,12.4402293235166,-171.507780348161));
#163554=CARTESIAN_POINT('Ctrl Pts',(52.6674149000463,12.4403025724068,-171.513538486835));
#163555=CARTESIAN_POINT('Ctrl Pts',(52.6695392899826,12.4403744312632,-171.519187354131));
#163556=CARTESIAN_POINT('Ctrl Pts',(52.6716624958677,12.4404587371184,-171.524997386882));
#163557=CARTESIAN_POINT('Ctrl Pts',(52.6739462816228,12.4405683544587,-171.531492117076));
#163558=CARTESIAN_POINT('Ctrl Pts',(52.6740124707888,12.4405715314118,-171.531680348732));
#163559=CARTESIAN_POINT('Ctrl Pts',(52.6740787844409,12.4405747302306,-171.53186913741));
#163560=CARTESIAN_POINT('Ctrl Pts',(52.6741452257962,12.4405779513586,-171.532058495837));
#163561=CARTESIAN_POINT('Ctrl Pts',(52.6846243513975,12.4410859874213,-171.561924092684));
#163562=CARTESIAN_POINT('Ctrl Pts',(52.6933788831336,12.4419134247877,-171.592007876766));
#163563=CARTESIAN_POINT('Ctrl Pts',(52.7004429961507,12.4430787347014,-171.622183769804));
#163564=CARTESIAN_POINT('Ctrl Pts',(52.7075705499667,12.4442545099334,-171.652630663993));
#163565=CARTESIAN_POINT('Ctrl Pts',(52.712977310938,12.4457744135457,-171.683171329686));
#163566=CARTESIAN_POINT('Ctrl Pts',(52.7167490255101,12.4476434139055,-171.713665889365));
#163567=CARTESIAN_POINT('Ctrl Pts',(52.7205968921899,12.4495501499725,-171.74477614383));
#163568=CARTESIAN_POINT('Ctrl Pts',(52.722743139262,12.4518203906959,-171.77583841498));
#163569=CARTESIAN_POINT('Ctrl Pts',(52.7233295870902,12.4544423301942,-171.806693370106));
#163570=CARTESIAN_POINT('Ctrl Pts',(52.7236409084908,12.4558342116845,-171.823073016147));
#163571=CARTESIAN_POINT('Ctrl Pts',(52.7235135000264,12.4573249035982,-171.839394056547));
#163572=CARTESIAN_POINT('Ctrl Pts',(52.7229739807576,12.4589105225087,-171.855631463706));
#163573=CARTESIAN_POINT('',(52.5050296388285,13.3739336825608,-172.133326251627));
#163574=CARTESIAN_POINT('Ctrl Pts',(52.5050296388285,13.3739336825608,-172.133326251627));
#163575=CARTESIAN_POINT('Ctrl Pts',(52.5113922936146,13.3286610413417,-172.117206797456));
#163576=CARTESIAN_POINT('Ctrl Pts',(52.5180677265498,13.2855571710499,-172.101923158766));
#163577=CARTESIAN_POINT('Ctrl Pts',(52.5249057325846,13.2445934907971,-172.087543541658));
#163578=CARTESIAN_POINT('Ctrl Pts',(52.5320889680496,13.2015616830932,-172.072437942883));
#163579=CARTESIAN_POINT('Ctrl Pts',(52.5394513985051,13.1608916606645,-172.058329381205));
#163580=CARTESIAN_POINT('Ctrl Pts',(52.5468293681514,13.1225611963807,-172.045238297065));
#163581=CARTESIAN_POINT('Ctrl Pts',(52.5548629048856,13.0808248911878,-172.030984008911));
#163582=CARTESIAN_POINT('Ctrl Pts',(52.5629143627139,13.0418628361347,-172.017935616994));
#163583=CARTESIAN_POINT('Ctrl Pts',(52.570789876164,13.0056574082241,-172.006060015165));
#163584=CARTESIAN_POINT('Ctrl Pts',(52.5742287729683,12.9898480605375,-172.000874452415));
#163585=CARTESIAN_POINT('Ctrl Pts',(52.5776343821988,12.9745644067251,-171.995911826329));
#163586=CARTESIAN_POINT('Ctrl Pts',(52.5809918470595,12.9598053140195,-171.991166699342));
#163587=CARTESIAN_POINT('Ctrl Pts',(52.5827654361525,12.9520087868984,-171.988660074309));
#163588=CARTESIAN_POINT('Ctrl Pts',(52.5845256033797,12.9443586463142,-171.986214119865));
#163589=CARTESIAN_POINT('Ctrl Pts',(52.5862702312371,12.9368548371707,-171.983827461247));
#163590=CARTESIAN_POINT('Ctrl Pts',(52.5871425451659,12.9331029325989,-171.982634131938));
#163591=CARTESIAN_POINT('Ctrl Pts',(52.588010880141,12.9293880210105,-171.981453986818));
#163592=CARTESIAN_POINT('Ctrl Pts',(52.5888751232003,12.9257094662639,-171.980289358009));
#163593=CARTESIAN_POINT('Ctrl Pts',(52.5896959593966,12.9222156680164,-171.979183223026));
#163594=CARTESIAN_POINT('Ctrl Pts',(52.5901687724434,12.9202071686556,-171.978548012444));
#163595=CARTESIAN_POINT('Ctrl Pts',(52.5912744272476,12.9155453298856,-171.977081560367));
#163596=CARTESIAN_POINT('Ctrl Pts',(52.5913328956812,12.9152988059168,-171.977004012514));
#163597=CARTESIAN_POINT('Ctrl Pts',(52.5913931436171,12.9150448631177,-171.976924147958));
#163598=CARTESIAN_POINT('Ctrl Pts',(52.5914553200437,12.9147828898895,-171.976841777287));
#163599=CARTESIAN_POINT('Ctrl Pts',(52.6038700340288,12.8624749192527,-171.960394895763));
#163600=CARTESIAN_POINT('Ctrl Pts',(52.6168327657393,12.8116557021248,-171.945092080409));
#163601=CARTESIAN_POINT('Ctrl Pts',(52.6302178818164,12.7623034905211,-171.9309914502));
#163602=CARTESIAN_POINT('Ctrl Pts',(52.6439822275001,12.7115530228484,-171.916491318305));
#163603=CARTESIAN_POINT('Ctrl Pts',(52.6581931596669,12.6623538907316,-171.903262171156));
#163604=CARTESIAN_POINT('Ctrl Pts',(52.6727149251186,12.6146907174398,-171.891312060373));
#163605=CARTESIAN_POINT('Ctrl Pts',(52.6878982669679,12.5648561256253,-171.878817531538));
#163606=CARTESIAN_POINT('Ctrl Pts',(52.7034213118224,12.5167006425706,-171.867720993698));
#163607=CARTESIAN_POINT('Ctrl Pts',(52.7191311438969,12.4702153439479,-171.857976087372));
#163608=CARTESIAN_POINT('Ctrl Pts',(52.7204083062534,12.4664362282162,-171.857183855637));
#163609=CARTESIAN_POINT('Ctrl Pts',(52.7216867047946,12.4626681555264,-171.856400529307));
#163610=CARTESIAN_POINT('Ctrl Pts',(52.7229662582911,12.4589111234036,-171.855626069084));
#163611=CARTESIAN_POINT('Origin',(51.5147615700869,13.2347605816008,-172.133326251627));
#163612=CARTESIAN_POINT('Ctrl Pts',(52.7228616924159,12.4592197450689,-176.820632909447));
#163613=CARTESIAN_POINT('Ctrl Pts',(52.8378230805615,12.1196543833272,-176.831752638987));
#163614=CARTESIAN_POINT('Ctrl Pts',(53.1964757989599,12.1197761140302,-176.835304824703));
#163615=CARTESIAN_POINT('Ctrl Pts',(52.7208610202525,12.4653983050582,-177.002115882214));
#163616=CARTESIAN_POINT('Ctrl Pts',(52.8359625560594,12.1237916221297,-176.944353244896));
#163617=CARTESIAN_POINT('Ctrl Pts',(53.1946754990687,12.1225542377913,-176.925963491801));
#163618=CARTESIAN_POINT('Ctrl Pts',(52.7374134643798,12.4138498331152,-177.18556360953));
#163619=CARTESIAN_POINT('Ctrl Pts',(52.8514409345781,12.0892511690341,-177.059386795892));
#163620=CARTESIAN_POINT('Ctrl Pts',(53.2095700879098,12.099376493835,-177.017605185139));
#163621=CARTESIAN_POINT('Ctrl Pts',(52.8100292410526,12.2198706620515,-177.495904173093));
#163622=CARTESIAN_POINT('Ctrl Pts',(52.9147988673353,11.9568596714106,-177.246828041132));
#163623=CARTESIAN_POINT('Ctrl Pts',(53.2749021302737,12.0121566707775,-177.172631305935));
#163624=CARTESIAN_POINT('Ctrl Pts',(52.867357957607,12.0764932764824,-177.624786878572));
#163625=CARTESIAN_POINT('Ctrl Pts',(52.9645940841351,11.8559530379094,-177.320932244844));
#163626=CARTESIAN_POINT('Ctrl Pts',(53.3264267869461,11.9477421916568,-177.236975784533));
#163627=CARTESIAN_POINT('Ctrl Pts',(52.9443095206334,11.9154395316641,-177.710596296728));
#163628=CARTESIAN_POINT('Ctrl Pts',(53.0251950686999,11.7443762835566,-177.357540682165));
#163629=CARTESIAN_POINT('Ctrl Pts',(53.3957081880351,11.8752586579091,-177.279873126825));
#163630=CARTESIAN_POINT('',(52.7229737572976,12.4589111791821,-176.84995));
#163631=CARTESIAN_POINT('',(53.1963133798215,12.11999998,-176.84995));
#163632=CARTESIAN_POINT('Origin',(53.1963133798215,12.61999998,-176.84995));
#163633=CARTESIAN_POINT('Ctrl Pts',(53.3846587239314,11.8868850448361,-177.272764808359));
#163634=CARTESIAN_POINT('Ctrl Pts',(53.3218769425614,11.9535931363301,-177.230657973471));
#163635=CARTESIAN_POINT('Ctrl Pts',(53.2747906065339,12.0124550402845,-177.170935103968));
#163636=CARTESIAN_POINT('Ctrl Pts',(53.2120088251639,12.0957858369083,-177.025107728));
#163637=CARTESIAN_POINT('Ctrl Pts',(53.1963133798215,12.11999998,-176.939021563529));
#163638=CARTESIAN_POINT('Ctrl Pts',(53.1963133798215,12.11999998,-176.84995));
#163639=CARTESIAN_POINT('Ctrl Pts',(52.7229737572976,12.4589111791821,-176.84995));
#163640=CARTESIAN_POINT('Ctrl Pts',(52.7230767593181,12.458608520417,-176.940255331482));
#163641=CARTESIAN_POINT('Ctrl Pts',(52.7273331507401,12.4459433761744,-177.027109684591));
#163642=CARTESIAN_POINT('Ctrl Pts',(52.7403923566312,12.4085558894172,-177.152214746696));
#163643=CARTESIAN_POINT('Ctrl Pts',(52.7458669121792,12.3930315358947,-177.193053689472));
#163644=CARTESIAN_POINT('Ctrl Pts',(52.7558971321586,12.365201810831,-177.253017986745));
#163645=CARTESIAN_POINT('Ctrl Pts',(52.7595441580411,12.3551682611144,-177.272790399688));
#163646=CARTESIAN_POINT('Ctrl Pts',(52.7674747337066,12.3335983394208,-177.311903853277));
#163647=CARTESIAN_POINT('Ctrl Pts',(52.7720465255225,12.3212955152219,-177.332438473495));
#163648=CARTESIAN_POINT('Ctrl Pts',(52.8110199539533,12.2176628634023,-177.493824447827));
#163649=CARTESIAN_POINT('Ctrl Pts',(52.8604414114892,12.0934691109458,-177.608894237259));
#163650=CARTESIAN_POINT('Ctrl Pts',(52.9322463618642,11.9408779899289,-177.695579616717));
#163651=CARTESIAN_POINT('Ctrl Pts',(52.5050296388285,13.3739336825608,-172.133326251627));
#163652=CARTESIAN_POINT('Ctrl Pts',(52.4864722882118,13.5059760932665,-171.679515584751));
#163653=CARTESIAN_POINT('Ctrl Pts',(52.1126146143195,13.5388501432916,-171.391638125813));
#163654=CARTESIAN_POINT('Ctrl Pts',(52.4188787332531,13.9869292276479,-172.315208572937));
#163655=CARTESIAN_POINT('Ctrl Pts',(52.3988291636435,14.129589328176,-171.781794156641));
#163656=CARTESIAN_POINT('Ctrl Pts',(51.9336694513028,14.1125756396742,-171.482621144035));
#163657=CARTESIAN_POINT('Ctrl Pts',(52.3315472405275,14.6083250867988,-172.437881815118));
#163658=CARTESIAN_POINT('Ctrl Pts',(52.3125022740344,14.7438370647052,-171.821280489149));
#163659=CARTESIAN_POINT('Ctrl Pts',(51.7497860966453,14.6887611591208,-171.543915907757));
#163660=CARTESIAN_POINT('Ctrl Pts',(52.1554800333145,15.861108362107,-172.606056153125));
#163661=CARTESIAN_POINT('Ctrl Pts',(52.1416679592957,15.9593863754288,-171.81403941883));
#163662=CARTESIAN_POINT('Ctrl Pts',(51.3741578990745,15.8404043177988,-171.628003076365));
#163663=CARTESIAN_POINT('Ctrl Pts',(52.0666747393889,16.4929908616926,-172.649949997757));
#163664=CARTESIAN_POINT('Ctrl Pts',(52.0557320324868,16.5708522670934,-171.757498535929));
#163665=CARTESIAN_POINT('Ctrl Pts',(51.1823572933404,16.4160730441958,-171.64995));
#163666=CARTESIAN_POINT('Ctrl Pts',(51.9770573602378,17.1306516479033,-172.64995));
#163667=CARTESIAN_POINT('Ctrl Pts',(51.9770573602378,17.1306516479032,-171.64995));
#163668=CARTESIAN_POINT('Ctrl Pts',(50.9867892914963,16.9914785469432,-171.64995));
#163669=CARTESIAN_POINT('',(51.9770573602378,17.1306516479033,-172.64995));
#163670=CARTESIAN_POINT('Origin',(50.9867892914963,16.9914785469432,-172.64995));
#163671=CARTESIAN_POINT('Ctrl Pts',(51.9770573602378,17.1306516479033,-172.64995));
#163672=CARTESIAN_POINT('Ctrl Pts',(52.0505828082768,16.6074909011026,-172.64994999816));
#163673=CARTESIAN_POINT('Ctrl Pts',(52.1235483666999,16.0883139759218,-172.620408747532));
#163674=CARTESIAN_POINT('Ctrl Pts',(52.1959928599553,15.5728446220586,-172.563374785654));
#163675=CARTESIAN_POINT('Ctrl Pts',(52.2118579788213,15.4599584356373,-172.550884525264));
#163676=CARTESIAN_POINT('Ctrl Pts',(52.2276981039083,15.3472500891946,-172.537075526609));
#163677=CARTESIAN_POINT('Ctrl Pts',(52.2435136369168,15.2347167244825,-172.521968983896));
#163678=CARTESIAN_POINT('Ctrl Pts',(52.2955483171871,14.8644707359736,-172.472266952379));
#163679=CARTESIAN_POINT('Ctrl Pts',(52.3473277334916,14.4960410449573,-172.409096799907));
#163680=CARTESIAN_POINT('Ctrl Pts',(52.39877081545,14.1300044971647,-172.328180486669));
#163681=CARTESIAN_POINT('Ctrl Pts',(52.4343604559388,13.8767710467997,-172.272200510582));
#163682=CARTESIAN_POINT('Ctrl Pts',(52.4697891103105,13.6246830721786,-172.207726272012));
#163683=CARTESIAN_POINT('Ctrl Pts',(52.5050296388285,13.3739336825608,-172.133326251627));
#163684=CARTESIAN_POINT('Origin',(51.6222122422086,12.4702093225365,-172.64995));
#163685=CARTESIAN_POINT('',(51.8267121465167,18.20041342952,-172.64995));
#163686=CARTESIAN_POINT('',(52.3378926620474,14.5631750666398,-172.64995));
#163687=CARTESIAN_POINT('Ctrl Pts',(51.8267121465167,18.20041342952,-172.64995));
#163688=CARTESIAN_POINT('Ctrl Pts',(51.8267121465167,18.20041342952,-172.608983203783));
#163689=CARTESIAN_POINT('Ctrl Pts',(51.8241375648893,18.2006212880455,-172.567620053095));
#163690=CARTESIAN_POINT('Ctrl Pts',(51.8188632652687,18.2010194183273,-172.526187281556));
#163691=CARTESIAN_POINT('Ctrl Pts',(51.8136580036326,18.2014123372798,-172.48529684459));
#163692=CARTESIAN_POINT('Ctrl Pts',(51.8058228695452,18.2019905277624,-172.444338940117));
#163693=CARTESIAN_POINT('Ctrl Pts',(51.7952777630821,18.2027427324649,-172.403658149851));
#163694=CARTESIAN_POINT('Ctrl Pts',(51.7849287688052,18.2034809480711,-172.363733918918));
#163695=CARTESIAN_POINT('Ctrl Pts',(51.7719693966446,18.2043867283353,-172.324077002367));
#163696=CARTESIAN_POINT('Ctrl Pts',(51.7563674887103,18.2054555537608,-172.285037095287));
#163697=CARTESIAN_POINT('Ctrl Pts',(51.7409344370744,18.2065128115045,-172.246419709235));
#163698=CARTESIAN_POINT('Ctrl Pts',(51.7229154768771,18.2077295674027,-172.20840647472));
#163699=CARTESIAN_POINT('Ctrl Pts',(51.7023264860424,18.2091080529521,-172.171353408967));
#163700=CARTESIAN_POINT('Ctrl Pts',(51.68205385491,18.2104653574111,-172.134869681311));
#163701=CARTESIAN_POINT('Ctrl Pts',(51.6592894086755,18.2119794375068,-172.099317308706));
#163702=CARTESIAN_POINT('Ctrl Pts',(51.6340971610588,18.2136592897809,-172.065046651591));
#163703=CARTESIAN_POINT('Ctrl Pts',(51.6226621714695,18.2144217899579,-172.049490889624));
#163704=CARTESIAN_POINT('Ctrl Pts',(51.6107276602892,18.2152185412537,-172.034199306089));
#163705=CARTESIAN_POINT('Ctrl Pts',(51.598303131713,18.2160508793958,-172.019204984927));
#163706=CARTESIAN_POINT('Ctrl Pts',(51.5873494198683,18.2167846852791,-172.005985692758));
#163707=CARTESIAN_POINT('Ctrl Pts',(51.5760148706341,18.2175461554467,-171.992997455498));
#163708=CARTESIAN_POINT('Ctrl Pts',(51.5643074667153,18.2183364117946,-171.980262947367));
#163709=CARTESIAN_POINT('Ctrl Pts',(51.5590405928199,18.2186919287442,-171.974534004477));
#163710=CARTESIAN_POINT('Ctrl Pts',(51.5534163959643,18.2190750020736,-171.968556625618));
#163711=CARTESIAN_POINT('Ctrl Pts',(51.5478098427664,18.2194555391254,-171.962743472216));
#163712=CARTESIAN_POINT('Ctrl Pts',(51.5420205413225,18.2198484799619,-171.956740836337));
#163713=CARTESIAN_POINT('Ctrl Pts',(51.536250232312,18.2202387417562,-171.950913444314));
#163714=CARTESIAN_POINT('Ctrl Pts',(51.5309526830832,18.220598944004,-171.945675867929));
#163715=CARTESIAN_POINT('Ctrl Pts',(51.5299766807193,18.2206653064351,-171.944710914757));
#163716=CARTESIAN_POINT('Ctrl Pts',(51.5290168243772,18.2207306624763,-171.943765878212));
#163717=CARTESIAN_POINT('Ctrl Pts',(51.5280760753453,18.2207948582762,-171.942843218813));
#163718=CARTESIAN_POINT('Ctrl Pts',(51.5058324918989,18.2223127387999,-171.921027356531));
#163719=CARTESIAN_POINT('Ctrl Pts',(51.4819007881196,18.2239579199193,-171.899576783543));
#163720=CARTESIAN_POINT('Ctrl Pts',(51.4562139231078,18.2257209796507,-171.878780245327));
#163721=CARTESIAN_POINT('Ctrl Pts',(51.4311267483435,18.2274428786671,-171.858469226895));
#163722=CARTESIAN_POINT('Ctrl Pts',(51.4043649569905,18.2292771530807,-171.838782360866));
#163723=CARTESIAN_POINT('Ctrl Pts',(51.3759031475289,18.2312202329405,-171.820018775919));
#163724=CARTESIAN_POINT('Ctrl Pts',(51.3471011588778,18.2331865367396,-171.801030926204));
#163725=CARTESIAN_POINT('Ctrl Pts',(51.3165575490232,18.2352641608903,-171.782988824438));
#163726=CARTESIAN_POINT('Ctrl Pts',(51.2842935217107,18.2374560853849,-171.766229742036));
#163727=CARTESIAN_POINT('Ctrl Pts',(51.2681615080545,18.2385520476321,-171.757850200836));
#163728=CARTESIAN_POINT('Ctrl Pts',(51.2516001964196,18.2396766982955,-171.749791815609));
#163729=CARTESIAN_POINT('Ctrl Pts',(51.2346175177148,18.2408311519914,-171.742098872722));
#163730=CARTESIAN_POINT('Ctrl Pts',(51.2261261783623,18.2414083788394,-171.738252401278));
#163731=CARTESIAN_POINT('Ctrl Pts',(51.2175294997355,18.2419930567959,-171.734497284799));
#163732=CARTESIAN_POINT('Ctrl Pts',(51.2088288993997,18.2425853850868,-171.730839196982));
#163733=CARTESIAN_POINT('Ctrl Pts',(51.2044785992318,18.2428815492322,-171.729010153074));
#163734=CARTESIAN_POINT('Ctrl Pts',(51.2001023189545,18.2431796260059,-171.727205365629));
#163735=CARTESIAN_POINT('Ctrl Pts',(51.195700250897,18.243479642438,-171.725425545573));
#163736=CARTESIAN_POINT('Ctrl Pts',(51.1930275887413,18.2436617937708,-171.724344949442));
#163737=CARTESIAN_POINT('Ctrl Pts',(51.1896251319421,18.243894314396,-171.722986930825));
#163738=CARTESIAN_POINT('Ctrl Pts',(51.1868037301612,18.2440866095122,-171.721876575881));
#163739=CARTESIAN_POINT('Ctrl Pts',(51.1849780789541,18.2442110383735,-171.721158095848));
#163740=CARTESIAN_POINT('Ctrl Pts',(51.1833962626412,18.2443187013851,-171.720541970085));
#163741=CARTESIAN_POINT('Ctrl Pts',(51.1824168840543,18.2443855389116,-171.720161698938));
#163742=CARTESIAN_POINT('Ctrl Pts',(51.1668545868817,18.2454475852581,-171.714119201504));
#163743=CARTESIAN_POINT('Ctrl Pts',(51.1496401644066,18.2466376335613,-171.707866938366));
#163744=CARTESIAN_POINT('Ctrl Pts',(51.1307111623421,18.2479469064434,-171.701654178661));
#163745=CARTESIAN_POINT('Ctrl Pts',(51.1121989920192,18.2492273480912,-171.695578228886));
#163746=CARTESIAN_POINT('Ctrl Pts',(51.0920461656476,18.2506217147811,-171.689540171962));
#163747=CARTESIAN_POINT('Ctrl Pts',(51.0702102422606,18.2521240418244,-171.683820318885));
#163748=CARTESIAN_POINT('Ctrl Pts',(51.0492248312468,18.2535678530122,-171.678323254913));
#163749=CARTESIAN_POINT('Ctrl Pts',(51.026684241603,18.2551112879842,-171.673120412672));
#163750=CARTESIAN_POINT('Ctrl Pts',(51.0025757341803,18.2567525563699,-171.668501297324));
#163751=CARTESIAN_POINT('Ctrl Pts',(50.9790753248452,18.2583524264164,-171.663998691686));
#163752=CARTESIAN_POINT('Ctrl Pts',(50.9540844508566,18.260045165992,-171.660051059706));
#163753=CARTESIAN_POINT('Ctrl Pts',(50.9276248838668,18.2618338349027,-171.656961460484));
#163754=CARTESIAN_POINT('Ctrl Pts',(50.9021597323515,18.2635552812453,-171.653987975984));
#163755=CARTESIAN_POINT('Ctrl Pts',(50.8753337389174,18.2653655160331,-171.651809705488));
#163756=CARTESIAN_POINT('Ctrl Pts',(50.8472057061698,18.2672728034334,-171.650723766103));
#163757=CARTESIAN_POINT('Ctrl Pts',(50.8341169196676,18.268160319379,-171.650218447125));
#163758=CARTESIAN_POINT('Ctrl Pts',(50.820746813004,18.26906893619,-171.64995));
#163759=CARTESIAN_POINT('Ctrl Pts',(50.8071048221096,18.26999998,-171.64995));
#163760=CARTESIAN_POINT('Ctrl Pts',(52.3218461808875,18.76999998,-176.84995));
#163761=CARTESIAN_POINT('Ctrl Pts',(51.746661977277,18.76999998,-176.84995));
#163762=CARTESIAN_POINT('Ctrl Pts',(51.8267121465167,18.20041342952,-176.84995));
#163763=CARTESIAN_POINT('Ctrl Pts',(52.3218461808802,18.76999998,-176.981217345763));
#163764=CARTESIAN_POINT('Ctrl Pts',(51.7466619772798,18.7699999799806,-176.958917254526));
#163765=CARTESIAN_POINT('Ctrl Pts',(51.8267121465076,18.2004134295853,-177.112484691526));
#163766=CARTESIAN_POINT('Ctrl Pts',(52.3066996556685,18.8238865434699,-177.110943344657));
#163767=CARTESIAN_POINT('Ctrl Pts',(51.7419771601862,18.8033341856637,-177.069891898465));
#163768=CARTESIAN_POINT('Ctrl Pts',(51.8115656212979,18.3081865564618,-177.371936689315));
#163769=CARTESIAN_POINT('Ctrl Pts',(52.2546657912052,19.0090066353435,-177.29606343653));
#163770=CARTESIAN_POINT('Ctrl Pts',(51.721325635328,18.9502774203983,-177.257255781811));
#163771=CARTESIAN_POINT('Ctrl Pts',(51.7595317568342,18.6784267402051,-177.742176873059));
#163772=CARTESIAN_POINT('Ctrl Pts',(52.2182021908711,19.1387326342368,-177.34995));
#163773=CARTESIAN_POINT('Ctrl Pts',(51.7054679578625,19.0631106584802,-177.331204220089));
#163774=CARTESIAN_POINT('Ctrl Pts',(51.7230681564996,18.9378787379949,-177.849949999941));
#163775=CARTESIAN_POINT('Ctrl Pts',(52.1813053461851,19.26999998,-177.34995));
#163776=CARTESIAN_POINT('Ctrl Pts',(51.6861713118143,19.2004134295199,-177.34995));
#163777=CARTESIAN_POINT('Ctrl Pts',(51.6861713118143,19.20041342952,-177.84995));
#163778=CARTESIAN_POINT('',(51.6861713118143,19.20041342952,-177.84995));
#163779=CARTESIAN_POINT('Origin',(52.1813053461851,19.26999998,-177.84995));
#163780=CARTESIAN_POINT('',(52.3218461808875,18.76999998,-176.84995));
#163781=CARTESIAN_POINT('Ctrl Pts',(52.3218461808875,18.76999998,-176.84995));
#163782=CARTESIAN_POINT('Ctrl Pts',(52.3218461808861,18.76999998,-176.875860144688));
#163783=CARTESIAN_POINT('Ctrl Pts',(52.3212473348555,18.7721017641991,-176.902069110057));
#163784=CARTESIAN_POINT('Ctrl Pts',(52.3200442820214,18.7763470609339,-176.92825527987));
#163785=CARTESIAN_POINT('Ctrl Pts',(52.3188302824207,18.7806309862899,-176.954679721752));
#163786=CARTESIAN_POINT('Ctrl Pts',(52.3170010256884,18.7870976262972,-176.981080901352));
#163787=CARTESIAN_POINT('Ctrl Pts',(52.3145590515113,18.7957612416509,-177.007084281685));
#163788=CARTESIAN_POINT('Ctrl Pts',(52.313643533861,18.7990093074351,-177.016833178247));
#163789=CARTESIAN_POINT('Ctrl Pts',(52.3126419754868,18.802565885418,-177.026525725243));
#163790=CARTESIAN_POINT('Ctrl Pts',(52.3115547989476,18.8064306989981,-177.036140639572));
#163791=CARTESIAN_POINT('Ctrl Pts',(52.3087004133778,18.8165777797304,-177.061384628684));
#163792=CARTESIAN_POINT('Ctrl Pts',(52.3052525487689,18.8288564461382,-177.086112146138));
#163793=CARTESIAN_POINT('Ctrl Pts',(52.3012107145058,18.8432663804517,-177.10992591327));
#163794=CARTESIAN_POINT('Ctrl Pts',(52.3003951344565,18.8461740837797,-177.114731165565));
#163795=CARTESIAN_POINT('Ctrl Pts',(52.2995553821288,18.8491685216028,-177.119499049706));
#163796=CARTESIAN_POINT('Ctrl Pts',(52.2986914727062,18.8522496224732,-177.124226050751));
#163797=CARTESIAN_POINT('Ctrl Pts',(52.296118846023,18.8614247999918,-177.138302536896));
#163798=CARTESIAN_POINT('Ctrl Pts',(52.2933318195899,18.8713686406316,-177.152016545396));
#163799=CARTESIAN_POINT('Ctrl Pts',(52.2903303611667,18.8820727042616,-177.165265493094));
#163800=CARTESIAN_POINT('Ctrl Pts',(52.2888296319551,18.8874247360766,-177.171889966943));
#163801=CARTESIAN_POINT('Ctrl Pts',(52.2872752955732,18.8929667701014,-177.178398084151));
#163802=CARTESIAN_POINT('Ctrl Pts',(52.2856673543981,18.898696614487,-177.184775824956));
#163803=CARTESIAN_POINT('Ctrl Pts',(52.2848633838106,18.9015615366797,-177.187964695359));
#163804=CARTESIAN_POINT('Ctrl Pts',(52.2840460121149,18.9044734020793,-177.191120965597));
#163805=CARTESIAN_POINT('Ctrl Pts',(52.2832152400256,18.9074318583303,-177.194242832619));
#163806=CARTESIAN_POINT('Ctrl Pts',(52.2827332989327,18.9091480951386,-177.196053866022));
#163807=CARTESIAN_POINT('Ctrl Pts',(52.2821462621781,18.9112378961258,-177.198223860036));
#163808=CARTESIAN_POINT('Ctrl Pts',(52.2816282827859,18.9130815152767,-177.200104597065));
#163809=CARTESIAN_POINT('Ctrl Pts',(52.2812533671164,18.9144159345966,-177.201465882462));
#163810=CARTESIAN_POINT('Ctrl Pts',(52.280915005339,18.9156200460742,-177.202676847247));
#163811=CARTESIAN_POINT('Ctrl Pts',(52.2806826811287,18.9164465864338,-177.20350338762));
#163812=CARTESIAN_POINT('Ctrl Pts',(52.277929558952,18.9262413753247,-177.213298176676));
#163813=CARTESIAN_POINT('Ctrl Pts',(52.2748105907763,18.9371766657348,-177.223386446747));
#163814=CARTESIAN_POINT('Ctrl Pts',(52.2713164396122,18.9493814538919,-177.233531412315));
#163815=CARTESIAN_POINT('Ctrl Pts',(52.2679774498128,18.9610442759185,-177.243225880286));
#163816=CARTESIAN_POINT('Ctrl Pts',(52.2642956685592,18.9738670503152,-177.252972163816));
#163817=CARTESIAN_POINT('Ctrl Pts',(52.2602690639592,18.9879403213751,-177.262523160306));
#163818=CARTESIAN_POINT('Ctrl Pts',(52.2564813947795,19.0011784960526,-177.271507408483));
#163819=CARTESIAN_POINT('Ctrl Pts',(52.2523884994066,19.0155236005279,-177.28031878073));
#163820=CARTESIAN_POINT('Ctrl Pts',(52.2479962759463,19.031023301524,-177.288715370066));
#163821=CARTESIAN_POINT('Ctrl Pts',(52.2462319877114,19.0372492916992,-177.292088150143));
#163822=CARTESIAN_POINT('Ctrl Pts',(52.2444195008846,19.0436612159548,-177.295393584586));
#163823=CARTESIAN_POINT('Ctrl Pts',(52.2425596341985,19.0502605504507,-177.298614236585));
#163824=CARTESIAN_POINT('Ctrl Pts',(52.2382882913859,19.0654164861837,-177.306010739179));
#163825=CARTESIAN_POINT('Ctrl Pts',(52.2337758204442,19.0815733677847,-177.312967023157));
#163826=CARTESIAN_POINT('Ctrl Pts',(52.2290041102122,19.0987235689744,-177.319245722133));
#163827=CARTESIAN_POINT('Ctrl Pts',(52.2243617473424,19.1154088774575,-177.325354223609));
#163828=CARTESIAN_POINT('Ctrl Pts',(52.2194739113008,19.1330346888939,-177.330821391408));
#163829=CARTESIAN_POINT('Ctrl Pts',(52.214334287041,19.1515578420991,-177.335399595475));
#163830=CARTESIAN_POINT('Ctrl Pts',(52.2093027295161,19.1696915238984,-177.339881537337));
#163831=CARTESIAN_POINT('Ctrl Pts',(52.2040297688411,19.1886854887831,-177.343511544901));
#163832=CARTESIAN_POINT('Ctrl Pts',(52.1985209471977,19.2084598041589,-177.346028622878));
#163833=CARTESIAN_POINT('Ctrl Pts',(52.1930121255543,19.2282341195348,-177.348545700856));
#163834=CARTESIAN_POINT('Ctrl Pts',(52.1872673146857,19.2487891749223,-177.34995));
#163835=CARTESIAN_POINT('Ctrl Pts',(52.1813053461851,19.26999998,-177.34995));
#163836=CARTESIAN_POINT('',(51.8267121465167,18.20041342952,-176.84995));
#163837=CARTESIAN_POINT('Origin',(52.3218461808875,18.26999998,-176.84995));
#163838=CARTESIAN_POINT('Ctrl Pts',(51.6861713118143,19.20041342952,-177.84995));
#163839=CARTESIAN_POINT('Ctrl Pts',(51.7230681564996,18.9378787379949,-177.849949999941));
#163840=CARTESIAN_POINT('Ctrl Pts',(51.7595317568342,18.6784267402051,-177.742176873059));
#163841=CARTESIAN_POINT('Ctrl Pts',(51.7855486890661,18.4933066483335,-177.557056781187));
#163842=CARTESIAN_POINT('Ctrl Pts',(51.8115656212979,18.3081865564618,-177.371936689315));
#163843=CARTESIAN_POINT('Ctrl Pts',(51.8267121465076,18.2004134295853,-177.112484691526));
#163844=CARTESIAN_POINT('Ctrl Pts',(51.8267121465167,18.20041342952,-176.84995));
#163845=CARTESIAN_POINT('Origin',(53.107614345321,12.6789689739766,-177.84995));
#163846=CARTESIAN_POINT('',(51.6159008944631,19.70041342952,-177.84995));
#163847=CARTESIAN_POINT('',(52.6124803109502,12.6093824234965,-177.84995));
#163848=CARTESIAN_POINT('Origin',(52.1110349288339,19.76999998,-177.84995));
#163849=CARTESIAN_POINT('Ctrl Pts',(52.1110349288339,19.76999998,-177.34995));
#163850=CARTESIAN_POINT('Ctrl Pts',(51.6159008944631,19.70041342952,-177.34995));
#163851=CARTESIAN_POINT('Ctrl Pts',(51.6159008944631,19.70041342952,-177.84995));
#163852=CARTESIAN_POINT('Ctrl Pts',(52.0741380841476,19.9012673257632,-177.34995));
#163853=CARTESIAN_POINT('Ctrl Pts',(51.5974634812487,19.8316024412644,-177.367861075732));
#163854=CARTESIAN_POINT('Ctrl Pts',(51.5790040497779,19.9629481210451,-177.849949999941));
#163855=CARTESIAN_POINT('Ctrl Pts',(52.0376744838139,20.0309933246565,-177.29606343653));
#163856=CARTESIAN_POINT('Ctrl Pts',(51.5765113276013,19.980684760958,-177.329589659683));
#163857=CARTESIAN_POINT('Ctrl Pts',(51.5425404494433,20.2224001188348,-177.742176873059));
#163858=CARTESIAN_POINT('Ctrl Pts',(51.9856406193506,20.2161134165301,-177.110943344657));
#163859=CARTESIAN_POINT('Ctrl Pts',(51.5456194237325,20.2004920783894,-177.142957948484));
#163860=CARTESIAN_POINT('Ctrl Pts',(51.4905065849796,20.5926403025782,-177.371936689315));
#163861=CARTESIAN_POINT('Ctrl Pts',(51.9704940941388,20.26999998,-176.981217345763));
#163862=CARTESIAN_POINT('Ctrl Pts',(51.5358507252279,20.2699999799402,-176.997671841189));
#163863=CARTESIAN_POINT('Ctrl Pts',(51.4753600597699,20.7004134294547,-177.112484691526));
#163864=CARTESIAN_POINT('Ctrl Pts',(51.9704940941315,20.26999998,-176.84995));
#163865=CARTESIAN_POINT('Ctrl Pts',(51.5358507252234,20.26999998,-176.84995));
#163866=CARTESIAN_POINT('Ctrl Pts',(51.4753600597607,20.70041342952,-176.84995));
#163867=CARTESIAN_POINT('',(51.4753600597607,20.70041342952,-176.84995));
#163868=CARTESIAN_POINT('Ctrl Pts',(51.4753600597607,20.70041342952,-176.84995));
#163869=CARTESIAN_POINT('Ctrl Pts',(51.4753600597699,20.7004134294547,-177.112484691526));
#163870=CARTESIAN_POINT('Ctrl Pts',(51.4905065849796,20.5926403025782,-177.371936689315));
#163871=CARTESIAN_POINT('Ctrl Pts',(51.5165235172115,20.4075202107065,-177.557056781187));
#163872=CARTESIAN_POINT('Ctrl Pts',(51.5425404494433,20.2224001188348,-177.742176873059));
#163873=CARTESIAN_POINT('Ctrl Pts',(51.5790040497779,19.9629481210451,-177.849949999941));
#163874=CARTESIAN_POINT('Ctrl Pts',(51.6159008944631,19.70041342952,-177.84995));
#163875=CARTESIAN_POINT('',(51.9704940941315,20.26999998,-176.84995));
#163876=CARTESIAN_POINT('Origin',(51.9704940941315,20.76999998,-176.84995));
#163877=CARTESIAN_POINT('Ctrl Pts',(52.1110349288339,19.76999998,-177.34995));
#163878=CARTESIAN_POINT('Ctrl Pts',(52.1051573658154,19.790910496971,-177.34995));
#163879=CARTESIAN_POINT('Ctrl Pts',(52.0994600569256,19.8111797265574,-177.348585219103));
#163880=CARTESIAN_POINT('Ctrl Pts',(52.0939760868931,19.8306899637212,-177.346136042585));
#163881=CARTESIAN_POINT('Ctrl Pts',(52.0883714367758,19.8506295425955,-177.34363296956));
#163882=CARTESIAN_POINT('Ctrl Pts',(52.0829895372398,19.8697766450989,-177.339997193904));
#163883=CARTESIAN_POINT('Ctrl Pts',(52.077852760651,19.8880516774042,-177.335495637065));
#163884=CARTESIAN_POINT('Ctrl Pts',(52.0725516730947,19.9069112763512,-177.330850088143));
#163885=CARTESIAN_POINT('Ctrl Pts',(52.0675115638435,19.9248423967328,-177.325282469033));
#163886=CARTESIAN_POINT('Ctrl Pts',(52.0627445788973,19.9418018269093,-177.319052501404));
#163887=CARTESIAN_POINT('Ctrl Pts',(52.0583344844422,19.9574915531887,-177.313288953584));
#163888=CARTESIAN_POINT('Ctrl Pts',(52.0541579327436,19.972350407939,-177.306958054925));
#163889=CARTESIAN_POINT('Ctrl Pts',(52.0502165121628,19.986372740271,-177.300241546992));
#163890=CARTESIAN_POINT('Ctrl Pts',(52.0450870458873,20.0046217647853,-177.291500510549));
#163891=CARTESIAN_POINT('Ctrl Pts',(52.0403539659962,20.0214605714607,-177.282104513154));
#163892=CARTESIAN_POINT('Ctrl Pts',(52.036004156819,20.0369358217199,-177.272394745804));
#163893=CARTESIAN_POINT('Ctrl Pts',(52.0317077277822,20.0522211622615,-177.262804135117));
#163894=CARTESIAN_POINT('Ctrl Pts',(52.027785046931,20.0661768245414,-177.25290695541));
#163895=CARTESIAN_POINT('Ctrl Pts',(52.0242126622406,20.0788862434728,-177.242983685746));
#163896=CARTESIAN_POINT('Ctrl Pts',(52.0205954994723,20.0917549686943,-177.232936032798));
#163897=CARTESIAN_POINT('Ctrl Pts',(52.0173374020497,20.103346252571,-177.222861819816));
#163898=CARTESIAN_POINT('Ctrl Pts',(52.0144058949125,20.1137756311337,-177.213007508239));
#163899=CARTESIAN_POINT('Ctrl Pts',(52.0140516456167,20.1150359384904,-177.211816693149));
#163900=CARTESIAN_POINT('Ctrl Pts',(52.0137021577588,20.1162793061519,-177.21062903688));
#163901=CARTESIAN_POINT('Ctrl Pts',(52.0133573666424,20.1175059642869,-177.209444926111));
#163902=CARTESIAN_POINT('Ctrl Pts',(52.0130028066504,20.1187673770028,-177.208227266245));
#163903=CARTESIAN_POINT('Ctrl Pts',(52.012768176645,20.1196021166056,-177.207413007324));
#163904=CARTESIAN_POINT('Ctrl Pts',(52.0124419559371,20.120762651012,-177.206271333209));
#163905=CARTESIAN_POINT('Ctrl Pts',(52.0122347316986,20.1214998539325,-177.205546110857));
#163906=CARTESIAN_POINT('Ctrl Pts',(52.0119906191944,20.1223682710577,-177.204688490097));
#163907=CARTESIAN_POINT('Ctrl Pts',(52.0116574840334,20.1235533658466,-177.20350339534));
#163908=CARTESIAN_POINT('Ctrl Pts',(52.0058810051988,20.1441026076184,-177.18295415412));
#163909=CARTESIAN_POINT('Ctrl Pts',(52.0007010628878,20.1625302884788,-177.160790380055));
#163910=CARTESIAN_POINT('Ctrl Pts',(51.9961296377291,20.1787935349074,-177.137499857223));
#163911=CARTESIAN_POINT('Ctrl Pts',(51.9915524477765,20.1950772900965,-177.114179963887));
#163912=CARTESIAN_POINT('Ctrl Pts',(51.9875853054089,20.2091911675404,-177.089730492885));
#163913=CARTESIAN_POINT('Ctrl Pts',(51.9842337271962,20.2211153080935,-177.064594611035));
#163914=CARTESIAN_POINT('Ctrl Pts',(51.9808763648716,20.23306002718,-177.039415349994));
#163915=CARTESIAN_POINT('Ctrl Pts',(51.9781366859997,20.2428074708371,-177.013547307222));
#163916=CARTESIAN_POINT('Ctrl Pts',(51.9760138008928,20.2503605832966,-176.98738923323));
#163917=CARTESIAN_POINT('Ctrl Pts',(51.9738812665038,20.2579480273889,-176.961112261315));
#163918=CARTESIAN_POINT('Ctrl Pts',(51.9723711389257,20.2633211715772,-176.934542619689));
#163919=CARTESIAN_POINT('Ctrl Pts',(51.9714761292155,20.2665057300255,-176.908037354243));
#163920=CARTESIAN_POINT('Ctrl Pts',(51.9708197715504,20.2688411341264,-176.88859964989));
#163921=CARTESIAN_POINT('Ctrl Pts',(51.9704940941315,20.26999998,-176.869195582661));
#163922=CARTESIAN_POINT('Ctrl Pts',(51.9704940941315,20.26999998,-176.84995));
#163923=CARTESIAN_POINT('Origin',(51.6222122422086,12.4702093225365,-172.64995));
#163924=CARTESIAN_POINT('',(50.6813043436922,26.35041342952,-172.64995));
#163925=CARTESIAN_POINT('',(51.4753600597607,20.70041342952,-172.64995));
#163926=CARTESIAN_POINT('',(51.5358507252234,20.26999998,-172.64995));
#163927=CARTESIAN_POINT('Ctrl Pts',(50.6813043436922,26.35041342952,-172.64995));
#163928=CARTESIAN_POINT('Ctrl Pts',(50.6813043436922,26.35041342952,-172.608927207252));
#163929=CARTESIAN_POINT('Ctrl Pts',(50.6787227100171,26.3506218554067,-172.567506968074));
#163930=CARTESIAN_POINT('Ctrl Pts',(50.6734338193897,26.35102105198,-172.5260173808));
#163931=CARTESIAN_POINT('Ctrl Pts',(50.6682470560006,26.3514125401611,-172.485328947731));
#163932=CARTESIAN_POINT('Ctrl Pts',(50.660456259095,26.3519874576975,-172.444574188382));
#163933=CARTESIAN_POINT('Ctrl Pts',(50.649982463067,26.3527347066972,-172.404092569325));
#163934=CARTESIAN_POINT('Ctrl Pts',(50.6396244504326,26.3534736951746,-172.364058457478));
#163935=CARTESIAN_POINT('Ctrl Pts',(50.626642107556,26.3543811808045,-172.324291861792));
#163936=CARTESIAN_POINT('Ctrl Pts',(50.6110029101186,26.355452592592,-172.285145271694));
#163937=CARTESIAN_POINT('Ctrl Pts',(50.5956188188146,26.3565065275415,-172.246637239636));
#163938=CARTESIAN_POINT('Ctrl Pts',(50.5776636255519,26.357719053777,-172.20872959003));
#163939=CARTESIAN_POINT('Ctrl Pts',(50.5571529561684,26.3590923673666,-172.171775260274));
#163940=CARTESIAN_POINT('Ctrl Pts',(50.5438380830478,26.3599838787969,-172.147785686714));
#163941=CARTESIAN_POINT('Ctrl Pts',(50.5294472385948,26.3609432834134,-172.124198204066));
#163942=CARTESIAN_POINT('Ctrl Pts',(50.513996097651,26.3619727841711,-172.10111200409));
#163943=CARTESIAN_POINT('Ctrl Pts',(50.4951854859102,26.3632261245628,-172.073006277406));
#163944=CARTESIAN_POINT('Ctrl Pts',(50.4748027525668,26.3645832676277,-172.045643569251));
#163945=CARTESIAN_POINT('Ctrl Pts',(50.4528953288796,26.3660508793946,-172.019204984916));
#163946=CARTESIAN_POINT('Ctrl Pts',(50.4419416170359,26.366784685278,-172.005985692749));
#163947=CARTESIAN_POINT('Ctrl Pts',(50.430607067803,26.3675461554458,-171.99299745549));
#163948=CARTESIAN_POINT('Ctrl Pts',(50.4188996638857,26.3683364117939,-171.980262947361));
#163949=CARTESIAN_POINT('Ctrl Pts',(50.4136327899799,26.3686919287444,-171.97453400446));
#163950=CARTESIAN_POINT('Ctrl Pts',(50.4080085931148,26.3690750020745,-171.968556625591));
#163951=CARTESIAN_POINT('Ctrl Pts',(50.4024020399075,26.3694555391271,-171.96274347218));
#163952=CARTESIAN_POINT('Ctrl Pts',(50.396612738455,26.3698484799643,-171.956740836293));
#163953=CARTESIAN_POINT('Ctrl Pts',(50.3908424294362,26.3702387417594,-171.950913444262));
#163954=CARTESIAN_POINT('Ctrl Pts',(50.3855448801983,26.370598944008,-171.945675867869));
#163955=CARTESIAN_POINT('Ctrl Pts',(50.3845688778554,26.3706653064377,-171.944710914718));
#163956=CARTESIAN_POINT('Ctrl Pts',(50.3836090215335,26.3707306624775,-171.943765878193));
#163957=CARTESIAN_POINT('Ctrl Pts',(50.3826682725208,26.3707948582762,-171.942843218813));
#163958=CARTESIAN_POINT('Ctrl Pts',(50.3602740756354,26.3723230165153,-171.920879639234));
#163959=CARTESIAN_POINT('Ctrl Pts',(50.3361687783455,26.3739801992357,-171.899286273711));
#163960=CARTESIAN_POINT('Ctrl Pts',(50.3102840946091,26.37575680946,-171.878357889714));
#163961=CARTESIAN_POINT('Ctrl Pts',(50.2851107273834,26.3774845980647,-171.858004622076));
#163962=CARTESIAN_POINT('Ctrl Pts',(50.2582539920478,26.3793252796138,-171.838280617717));
#163963=CARTESIAN_POINT('Ctrl Pts',(50.229688635469,26.3812753050111,-171.819487495989));
#163964=CARTESIAN_POINT('Ctrl Pts',(50.2011232788901,26.3832253304083,-171.800694374262));
#163965=CARTESIAN_POINT('Ctrl Pts',(50.1708486900078,26.3852846137747,-171.782832445151));
#163966=CARTESIAN_POINT('Ctrl Pts',(50.138885718831,26.3874560853879,-171.766229742008));
#163967=CARTESIAN_POINT('Ctrl Pts',(50.1227537051804,26.3885520476348,-171.757850200811));
#163968=CARTESIAN_POINT('Ctrl Pts',(50.1061923935528,26.3896766982976,-171.749791815589));
#163969=CARTESIAN_POINT('Ctrl Pts',(50.0892097148571,26.3908311519931,-171.742098872707));
#163970=CARTESIAN_POINT('Ctrl Pts',(50.0807183755093,26.3914083788408,-171.738252401266));
#163971=CARTESIAN_POINT('Ctrl Pts',(50.0721216968875,26.391993056797,-171.734497284789));
#163972=CARTESIAN_POINT('Ctrl Pts',(50.0634210965573,26.3925853850876,-171.730839196975));
#163973=CARTESIAN_POINT('Ctrl Pts',(50.0590707963921,26.3928815492329,-171.729010153068));
#163974=CARTESIAN_POINT('Ctrl Pts',(50.0546945161177,26.3931796260065,-171.727205365624));
#163975=CARTESIAN_POINT('Ctrl Pts',(50.0502924480632,26.3934796424384,-171.725425545569));
#163976=CARTESIAN_POINT('Ctrl Pts',(50.0476197859243,26.3936617937702,-171.724344949445));
#163977=CARTESIAN_POINT('Ctrl Pts',(50.0442173291523,26.3938943143935,-171.722986930839));
#163978=CARTESIAN_POINT('Ctrl Pts',(50.0413959273829,26.3940866095089,-171.721876575899));
#163979=CARTESIAN_POINT('Ctrl Pts',(50.0395702761572,26.3942110383716,-171.721158095858));
#163980=CARTESIAN_POINT('Ctrl Pts',(50.0379884598262,26.3943187013844,-171.720541970088));
#163981=CARTESIAN_POINT('Ctrl Pts',(50.0370090812298,26.3943855389116,-171.720161698938));
#163982=CARTESIAN_POINT('Ctrl Pts',(50.0214467840286,26.3954475852603,-171.714119201493));
#163983=CARTESIAN_POINT('Ctrl Pts',(50.004232361525,26.3966376335655,-171.707866938345));
#163984=CARTESIAN_POINT('Ctrl Pts',(49.9853033594322,26.3979469064497,-171.701654178633));
#163985=CARTESIAN_POINT('Ctrl Pts',(49.9667911890826,26.3992273480994,-171.695578228851));
#163986=CARTESIAN_POINT('Ctrl Pts',(49.9466383626846,26.4006217147911,-171.689540171922));
#163987=CARTESIAN_POINT('Ctrl Pts',(49.9248024392717,26.4021240418361,-171.683820318842));
#163988=CARTESIAN_POINT('Ctrl Pts',(49.9038170282338,26.4035678530255,-171.678323254867));
#163989=CARTESIAN_POINT('Ctrl Pts',(49.8812764385664,26.405111287999,-171.673120412625));
#163990=CARTESIAN_POINT('Ctrl Pts',(49.8571679311208,26.4067525563862,-171.668501297279));
#163991=CARTESIAN_POINT('Ctrl Pts',(49.8336675217635,26.4083524264341,-171.663998691642));
#163992=CARTESIAN_POINT('Ctrl Pts',(49.8086766477535,26.410045166011,-171.660051059665));
#163993=CARTESIAN_POINT('Ctrl Pts',(49.7822170807432,26.411833834923,-171.656961460449));
#163994=CARTESIAN_POINT('Ctrl Pts',(49.7567519292073,26.4135552812669,-171.653987975954));
#163995=CARTESIAN_POINT('Ctrl Pts',(49.7299259357533,26.4153655160561,-171.651809705465));
#163996=CARTESIAN_POINT('Ctrl Pts',(49.701797902987,26.4172728034577,-171.650723766089));
#163997=CARTESIAN_POINT('Ctrl Pts',(49.6887091165988,26.4181603193956,-171.65021844712));
#163998=CARTESIAN_POINT('Ctrl Pts',(49.6753390100547,26.4190689361985,-171.64995));
#163999=CARTESIAN_POINT('Ctrl Pts',(49.6616970192851,26.41999998,-171.64995));
#164000=CARTESIAN_POINT('Ctrl Pts',(50.4557527353536,20.76999998,-171.64995));
#164001=CARTESIAN_POINT('Ctrl Pts',(50.4842042680624,20.7680582089184,-171.64995));
#164002=CARTESIAN_POINT('Ctrl Pts',(50.5114694452097,20.7661974046848,-171.651129585064));
#164003=CARTESIAN_POINT('Ctrl Pts',(50.5374753276717,20.7644225452763,-171.653192621543));
#164004=CARTESIAN_POINT('Ctrl Pts',(50.5648466522595,20.7625544966515,-171.655363978012));
#164005=CARTESIAN_POINT('Ctrl Pts',(50.5908233175796,20.7607816312657,-171.658513818819));
#164006=CARTESIAN_POINT('Ctrl Pts',(50.6153661207849,20.7591066246496,-171.662335033587));
#164007=CARTESIAN_POINT('Ctrl Pts',(50.6373318097271,20.757607501913,-171.665755002132));
#164008=CARTESIAN_POINT('Ctrl Pts',(50.6581499199593,20.756186699567,-171.669713339724));
#164009=CARTESIAN_POINT('Ctrl Pts',(50.6778170036355,20.7548444529213,-171.674015027575));
#164010=CARTESIAN_POINT('Ctrl Pts',(50.7013538125097,20.753238103791,-171.679163122048));
#164011=CARTESIAN_POINT('Ctrl Pts',(50.7232424486265,20.7517442397851,-171.684802100382));
#164012=CARTESIAN_POINT('Ctrl Pts',(50.7435076557478,20.7503611721819,-171.690639736304));
#164013=CARTESIAN_POINT('Ctrl Pts',(50.7646446447714,20.7489186068742,-171.696728499457));
#164014=CARTESIAN_POINT('Ctrl Pts',(50.7840164495197,20.7475965125377,-171.703033282349));
#164015=CARTESIAN_POINT('Ctrl Pts',(50.8016762225318,20.7463912615977,-171.709272496226));
#164016=CARTESIAN_POINT('Ctrl Pts',(50.8092483809043,20.7458744740382,-171.71194774667));
#164017=CARTESIAN_POINT('Ctrl Pts',(50.8165059618879,20.7453791558767,-171.71461154199));
#164018=CARTESIAN_POINT('Ctrl Pts',(50.823454146604,20.7449049535098,-171.717244495101));
#164019=CARTESIAN_POINT('Ctrl Pts',(50.8252179693497,20.7447845754607,-171.717912880122));
#164020=CARTESIAN_POINT('Ctrl Pts',(50.8260446003286,20.7447280884717,-171.718228248952));
#164021=CARTESIAN_POINT('Ctrl Pts',(50.8278165062487,20.7446071168896,-171.718908958993));
#164022=CARTESIAN_POINT('Ctrl Pts',(50.8286356820764,20.7445511901077,-171.719223660358));
#164023=CARTESIAN_POINT('Ctrl Pts',(50.8296567689968,20.7444814893959,-171.719616772033));
#164024=CARTESIAN_POINT('Ctrl Pts',(50.83106428527,20.7443854315169,-171.720163005656));
#164025=CARTESIAN_POINT('Ctrl Pts',(50.8360549385636,20.7440448375364,-171.72209979508));
#164026=CARTESIAN_POINT('Ctrl Pts',(50.841013474753,20.7437064347847,-171.724069245188));
#164027=CARTESIAN_POINT('Ctrl Pts',(50.8459395682395,20.743370245535,-171.72607046184));
#164028=CARTESIAN_POINT('Ctrl Pts',(50.8793181521241,20.7410922698724,-171.739630451729));
#164029=CARTESIAN_POINT('Ctrl Pts',(50.911195187842,20.7389167421848,-171.754642782237));
#164030=CARTESIAN_POINT('Ctrl Pts',(50.9415228493068,20.7368469422535,-171.770779293227));
#164031=CARTESIAN_POINT('Ctrl Pts',(50.9706035862437,20.7348622423324,-171.786252350117));
#164032=CARTESIAN_POINT('Ctrl Pts',(50.9982602416247,20.7329747203074,-171.802759466709));
#164033=CARTESIAN_POINT('Ctrl Pts',(51.0244817266949,20.7311851463697,-171.82004374659));
#164034=CARTESIAN_POINT('Ctrl Pts',(51.0538644581718,20.7291798224786,-171.839411808817));
#164035=CARTESIAN_POINT('Ctrl Pts',(51.0814456559995,20.7272974503447,-171.859755775677));
#164036=CARTESIAN_POINT('Ctrl Pts',(51.1072486905314,20.7255364349792,-171.880757614398));
#164037=CARTESIAN_POINT('Ctrl Pts',(51.1193846156018,20.7247081777253,-171.890635396049));
#164038=CARTESIAN_POINT('Ctrl Pts',(51.1311276872427,20.7239067320825,-171.900659292073));
#164039=CARTESIAN_POINT('Ctrl Pts',(51.1424827865761,20.723131764922,-171.910799109276));
#164040=CARTESIAN_POINT('Ctrl Pts',(51.1479796028623,20.7227566161026,-171.915707627529));
#164041=CARTESIAN_POINT('Ctrl Pts',(51.1530623502369,20.7224097268112,-171.92034885135));
#164042=CARTESIAN_POINT('Ctrl Pts',(51.1581876669761,20.7220599218499,-171.925124127321));
#164043=CARTESIAN_POINT('Ctrl Pts',(51.1631600281573,20.7217205561679,-171.929756894051));
#164044=CARTESIAN_POINT('Ctrl Pts',(51.1681726053704,20.7213784360359,-171.934515912431));
#164045=CARTESIAN_POINT('Ctrl Pts',(51.1736091589058,20.7210073610304,-171.93980158089));
#164046=CARTESIAN_POINT('Ctrl Pts',(51.1746317442697,20.7209375638938,-171.940795785613));
#164047=CARTESIAN_POINT('Ctrl Pts',(51.175669224257,20.7208667495451,-171.941808724727));
#164048=CARTESIAN_POINT('Ctrl Pts',(51.176723995822,20.7207947543338,-171.94284321151));
#164049=CARTESIAN_POINT('Ctrl Pts',(51.2111291405428,20.7184463731819,-171.976586695543));
#164050=CARTESIAN_POINT('Ctrl Pts',(51.2427228964462,20.7162900773892,-172.012463058233));
#164051=CARTESIAN_POINT('Ctrl Pts',(51.2713791089379,20.7143343614467,-172.04995975826));
#164052=CARTESIAN_POINT('Ctrl Pts',(51.3005002420468,20.712346915817,-172.088064807662));
#164053=CARTESIAN_POINT('Ctrl Pts',(51.3265877757913,20.7105666089751,-172.127843233128));
#164054=CARTESIAN_POINT('Ctrl Pts',(51.3495358206626,20.7090005519007,-172.168804472612));
#164055=CARTESIAN_POINT('Ctrl Pts',(51.3675548049889,20.7077708716366,-172.200967558242));
#164056=CARTESIAN_POINT('Ctrl Pts',(51.3836386764324,20.706673250415,-172.233860874994));
#164057=CARTESIAN_POINT('Ctrl Pts',(51.3977470738109,20.705710388276,-172.267266567535));
#164058=CARTESIAN_POINT('Ctrl Pts',(51.399144335016,20.7056150287623,-172.270574985704));
#164059=CARTESIAN_POINT('Ctrl Pts',(51.4005221974052,20.7055209925611,-172.273888354197));
#164060=CARTESIAN_POINT('Ctrl Pts',(51.4018807021469,20.7054282768102,-172.27720644154));
#164061=CARTESIAN_POINT('Ctrl Pts',(51.419643126508,20.7042160200817,-172.320590372151));
#164062=CARTESIAN_POINT('Ctrl Pts',(51.4340950438057,20.7032297001049,-172.364775502726));
#164063=CARTESIAN_POINT('Ctrl Pts',(51.4453314610336,20.7024628328062,-172.40926741461));
#164064=CARTESIAN_POINT('Ctrl Pts',(51.456700042584,20.7016869455063,-172.454282646629));
#164065=CARTESIAN_POINT('Ctrl Pts',(51.4647770536576,20.7011357025666,-172.499611950402));
#164066=CARTESIAN_POINT('Ctrl Pts',(51.4696694884625,20.7008018018056,-172.544796240755));
#164067=CARTESIAN_POINT('Ctrl Pts',(51.4734812148342,20.7005416576469,-172.57999960227));
#164068=CARTESIAN_POINT('Ctrl Pts',(51.4753600597607,20.70041342952,-172.615116019904));
#164069=CARTESIAN_POINT('Ctrl Pts',(51.4753600597607,20.70041342952,-172.64995));
#164070=CARTESIAN_POINT('Ctrl Pts',(51.176438378063,26.91999998,-176.84995));
#164071=CARTESIAN_POINT('Ctrl Pts',(50.6012541744525,26.9199999800001,-176.84995));
#164072=CARTESIAN_POINT('Ctrl Pts',(50.6813043436922,26.35041342952,-176.84995));
#164073=CARTESIAN_POINT('Ctrl Pts',(51.1764383780557,26.91999998,-176.981217345763));
#164074=CARTESIAN_POINT('Ctrl Pts',(50.6012541744552,26.9199999799806,-176.958917254526));
#164075=CARTESIAN_POINT('Ctrl Pts',(50.681304343683,26.3504134295853,-177.112484691526));
#164076=CARTESIAN_POINT('Ctrl Pts',(51.161291852844,26.9738865434699,-177.110943344657));
#164077=CARTESIAN_POINT('Ctrl Pts',(50.5965693573617,26.9533341856637,-177.069891898465));
#164078=CARTESIAN_POINT('Ctrl Pts',(50.6661578184733,26.4581865564618,-177.371936689315));
#164079=CARTESIAN_POINT('Ctrl Pts',(51.1092579883806,27.1590066353435,-177.29606343653));
#164080=CARTESIAN_POINT('Ctrl Pts',(50.5759178325036,27.1002774203984,-177.257255781812));
#164081=CARTESIAN_POINT('Ctrl Pts',(50.6141239540097,26.8284267402052,-177.742176873059));
#164082=CARTESIAN_POINT('Ctrl Pts',(51.0727943880466,27.2887326342368,-177.34995));
#164083=CARTESIAN_POINT('Ctrl Pts',(50.5600601550379,27.2131106584802,-177.331204220089));
#164084=CARTESIAN_POINT('Ctrl Pts',(50.5776603536751,27.0878787379949,-177.849949999941));
#164085=CARTESIAN_POINT('Ctrl Pts',(51.0358975433606,27.41999998,-177.34995));
#164086=CARTESIAN_POINT('Ctrl Pts',(50.5407635089898,27.35041342952,-177.34995));
#164087=CARTESIAN_POINT('Ctrl Pts',(50.5407635089898,27.3504134295199,-177.84995));
#164088=CARTESIAN_POINT('',(51.176438378063,26.91999998,-176.84995));
#164089=CARTESIAN_POINT('',(50.6813043436922,26.35041342952,-176.84995));
#164090=CARTESIAN_POINT('Origin',(51.176438378063,26.41999998,-176.84995));
#164091=CARTESIAN_POINT('',(50.5407635089898,27.3504134295199,-177.84995));
#164092=CARTESIAN_POINT('Ctrl Pts',(50.5407635089898,27.3504134295199,-177.84995));
#164093=CARTESIAN_POINT('Ctrl Pts',(50.5776603536751,27.0878787379949,-177.849949999941));
#164094=CARTESIAN_POINT('Ctrl Pts',(50.6141239540097,26.8284267402052,-177.742176873059));
#164095=CARTESIAN_POINT('Ctrl Pts',(50.6401408862415,26.6433066483335,-177.557056781187));
#164096=CARTESIAN_POINT('Ctrl Pts',(50.6661578184733,26.4581865564618,-177.371936689315));
#164097=CARTESIAN_POINT('Ctrl Pts',(50.681304343683,26.3504134295853,-177.112484691526));
#164098=CARTESIAN_POINT('Ctrl Pts',(50.6813043436922,26.35041342952,-176.84995));
#164099=CARTESIAN_POINT('Origin',(51.0358975433606,27.41999998,-177.84995));
#164100=CARTESIAN_POINT('Ctrl Pts',(51.176438378063,26.91999998,-176.84995));
#164101=CARTESIAN_POINT('Ctrl Pts',(51.1764383780616,26.91999998,-176.875860144656));
#164102=CARTESIAN_POINT('Ctrl Pts',(51.1758395320321,26.9221017641939,-176.902069109994));
#164103=CARTESIAN_POINT('Ctrl Pts',(51.1746364792001,26.9263470609191,-176.928255279779));
#164104=CARTESIAN_POINT('Ctrl Pts',(51.1734224796019,26.9306309862647,-176.954679721627));
#164105=CARTESIAN_POINT('Ctrl Pts',(51.1715932228734,26.9370976262562,-176.981080901196));
#164106=CARTESIAN_POINT('Ctrl Pts',(51.1691512487013,26.9457612415897,-177.007084281502));
#164107=CARTESIAN_POINT('Ctrl Pts',(51.1682357310471,26.9490093073872,-177.016833178116));
#164108=CARTESIAN_POINT('Ctrl Pts',(51.167234172668,26.9525658853867,-177.026525725163));
#164109=CARTESIAN_POINT('Ctrl Pts',(51.1661469961231,26.9564306989867,-177.036140639544));
#164110=CARTESIAN_POINT('Ctrl Pts',(51.1632926105572,26.9665777797031,-177.06138462862));
#164111=CARTESIAN_POINT('Ctrl Pts',(51.1598447459541,26.9788564460896,-177.086112146043));
#164112=CARTESIAN_POINT('Ctrl Pts',(51.1558029116984,26.9932663803772,-177.109925913147));
#164113=CARTESIAN_POINT('Ctrl Pts',(51.1549873316437,26.9961740837246,-177.114731165477));
#164114=CARTESIAN_POINT('Ctrl Pts',(51.1541475793103,26.9991685215683,-177.119499049653));
#164115=CARTESIAN_POINT('Ctrl Pts',(51.1532836698816,27.0022496224607,-177.124226050732));
#164116=CARTESIAN_POINT('Ctrl Pts',(51.1507110431984,27.0114247999801,-177.138302536879));
#164117=CARTESIAN_POINT('Ctrl Pts',(51.1479240167653,27.0213686406213,-177.152016545382));
#164118=CARTESIAN_POINT('Ctrl Pts',(51.1449225583421,27.0320727042533,-177.165265493083));
#164119=CARTESIAN_POINT('Ctrl Pts',(51.1434218291305,27.0374247360693,-177.171889966934));
#164120=CARTESIAN_POINT('Ctrl Pts',(51.1418674927487,27.0429667700952,-177.178398084144));
#164121=CARTESIAN_POINT('Ctrl Pts',(51.1402595515736,27.0486966144822,-177.184775824951));
#164122=CARTESIAN_POINT('Ctrl Pts',(51.139455580986,27.0515615366757,-177.187964695355));
#164123=CARTESIAN_POINT('Ctrl Pts',(51.1386382092902,27.0544734020759,-177.191120965594));
#164124=CARTESIAN_POINT('Ctrl Pts',(51.137807437201,27.0574318583278,-177.194242832616));
#164125=CARTESIAN_POINT('Ctrl Pts',(51.1373254961083,27.0591480951356,-177.196053866019));
#164126=CARTESIAN_POINT('Ctrl Pts',(51.136738459354,27.0612378961227,-177.198223860033));
#164127=CARTESIAN_POINT('Ctrl Pts',(51.1362204799618,27.0630815152736,-177.200104597062));
#164128=CARTESIAN_POINT('Ctrl Pts',(51.135845564292,27.0644159345951,-177.20146588246));
#164129=CARTESIAN_POINT('Ctrl Pts',(51.1355072025142,27.0656200460742,-177.202676847247));
#164130=CARTESIAN_POINT('Ctrl Pts',(51.135274878304,27.0664465864337,-177.20350338762));
#164131=CARTESIAN_POINT('Ctrl Pts',(51.1325217561302,27.0762413753144,-177.213298176666));
#164132=CARTESIAN_POINT('Ctrl Pts',(51.1294027879578,27.087176665714,-177.223386446728));
#164133=CARTESIAN_POINT('Ctrl Pts',(51.125908636797,27.0993814538605,-177.233531412289));
#164134=CARTESIAN_POINT('Ctrl Pts',(51.1225696470007,27.111044275877,-177.243225880253));
#164135=CARTESIAN_POINT('Ctrl Pts',(51.1188878657503,27.1238670502636,-177.252972163778));
#164136=CARTESIAN_POINT('Ctrl Pts',(51.1148612611533,27.1379403213136,-177.262523160264));
#164137=CARTESIAN_POINT('Ctrl Pts',(51.1110735919767,27.1511784959811,-177.271507408437));
#164138=CARTESIAN_POINT('Ctrl Pts',(51.1069806966066,27.1655236004465,-177.280318780682));
#164139=CARTESIAN_POINT('Ctrl Pts',(51.102588473149,27.1810233014328,-177.288715370017));
#164140=CARTESIAN_POINT('Ctrl Pts',(51.1008241849099,27.187249291623,-177.292088150103));
#164141=CARTESIAN_POINT('Ctrl Pts',(51.0990116980784,27.1936612158948,-177.295393584556));
#164142=CARTESIAN_POINT('Ctrl Pts',(51.0971518313873,27.2002605504079,-177.298614236564));
#164143=CARTESIAN_POINT('Ctrl Pts',(51.0928804885768,27.2154164861333,-177.306010739157));
#164144=CARTESIAN_POINT('Ctrl Pts',(51.0883680176369,27.2315733677267,-177.312967023133));
#164145=CARTESIAN_POINT('Ctrl Pts',(51.0835963074068,27.248723568909,-177.319245722109));
#164146=CARTESIAN_POINT('Ctrl Pts',(51.078953944539,27.2654088773845,-177.325354223585));
#164147=CARTESIAN_POINT('Ctrl Pts',(51.0740661084993,27.2830346888134,-177.330821391385));
#164148=CARTESIAN_POINT('Ctrl Pts',(51.0689264842414,27.3015578420114,-177.335399595453));
#164149=CARTESIAN_POINT('Ctrl Pts',(51.0638949267134,27.3196915238215,-177.339881537321));
#164150=CARTESIAN_POINT('Ctrl Pts',(51.0586219660347,27.3386854887189,-177.343511544891));
#164151=CARTESIAN_POINT('Ctrl Pts',(51.0531131443872,27.3584598041094,-177.346028622872));
#164152=CARTESIAN_POINT('Ctrl Pts',(51.0476043227396,27.3782341195,-177.348545700853));
#164153=CARTESIAN_POINT('Ctrl Pts',(51.0418595118664,27.3987891749041,-177.34995));
#164154=CARTESIAN_POINT('Ctrl Pts',(51.0358975433606,27.41999998,-177.34995));
#164155=CARTESIAN_POINT('Origin',(53.107614345321,12.6789689739766,-177.84995));
#164156=CARTESIAN_POINT('',(50.4704930916386,27.85041342952,-177.84995));
#164157=CARTESIAN_POINT('',(52.6124803109502,12.6093824234965,-177.84995));
#164158=CARTESIAN_POINT('Origin',(50.9656271260094,27.91999998,-177.84995));
#164159=CARTESIAN_POINT('Ctrl Pts',(50.9656271260094,27.91999998,-177.34995));
#164160=CARTESIAN_POINT('Ctrl Pts',(50.4704930916386,27.85041342952,-177.34995));
#164161=CARTESIAN_POINT('Ctrl Pts',(50.4704930916386,27.85041342952,-177.84995));
#164162=CARTESIAN_POINT('Ctrl Pts',(50.9287302813235,28.0512673257631,-177.34995));
#164163=CARTESIAN_POINT('Ctrl Pts',(50.4520556784241,27.9816024412645,-177.367861075731));
#164164=CARTESIAN_POINT('Ctrl Pts',(50.4335962469534,28.1129481210447,-177.849949999941));
#164165=CARTESIAN_POINT('Ctrl Pts',(50.8922666809894,28.1809933246567,-177.29606343653));
#164166=CARTESIAN_POINT('Ctrl Pts',(50.4311035247778,28.1306847609584,-177.32958965968));
#164167=CARTESIAN_POINT('Ctrl Pts',(50.3971326466187,28.3724001188352,-177.742176873059));
#164168=CARTESIAN_POINT('Ctrl Pts',(50.840232816526,28.3661134165298,-177.110943344657));
#164169=CARTESIAN_POINT('Ctrl Pts',(50.4002116209072,28.3504920783889,-177.142957948487));
#164170=CARTESIAN_POINT('Ctrl Pts',(50.3450987821552,28.7426403025778,-177.371936689315));
#164171=CARTESIAN_POINT('Ctrl Pts',(50.8250862913143,28.41999998,-176.981217345763));
#164172=CARTESIAN_POINT('Ctrl Pts',(50.3904429224034,28.4199999799438,-176.997671841187));
#164173=CARTESIAN_POINT('Ctrl Pts',(50.3299522569454,28.8504134294547,-177.112484691526));
#164174=CARTESIAN_POINT('Ctrl Pts',(50.825086291307,28.41999998,-176.84995));
#164175=CARTESIAN_POINT('Ctrl Pts',(50.3904429223989,28.41999998,-176.84995));
#164176=CARTESIAN_POINT('Ctrl Pts',(50.3299522569362,28.85041342952,-176.84995));
#164177=CARTESIAN_POINT('',(50.3299522569362,28.85041342952,-176.84995));
#164178=CARTESIAN_POINT('Ctrl Pts',(50.3299522569362,28.85041342952,-176.84995));
#164179=CARTESIAN_POINT('Ctrl Pts',(50.3299522569454,28.8504134294547,-177.112484691526));
#164180=CARTESIAN_POINT('Ctrl Pts',(50.3450987821552,28.7426403025778,-177.371936689315));
#164181=CARTESIAN_POINT('Ctrl Pts',(50.3711157143869,28.5575202107065,-177.557056781187));
#164182=CARTESIAN_POINT('Ctrl Pts',(50.3971326466187,28.3724001188352,-177.742176873059));
#164183=CARTESIAN_POINT('Ctrl Pts',(50.4335962469534,28.1129481210447,-177.849949999941));
#164184=CARTESIAN_POINT('Ctrl Pts',(50.4704930916386,27.85041342952,-177.84995));
#164185=CARTESIAN_POINT('',(50.825086291307,28.41999998,-176.84995));
#164186=CARTESIAN_POINT('Origin',(50.825086291307,28.91999998,-176.84995));
#164187=CARTESIAN_POINT('Ctrl Pts',(50.9656271260094,27.91999998,-177.34995));
#164188=CARTESIAN_POINT('Ctrl Pts',(50.9597495629756,27.9409104970259,-177.34995));
#164189=CARTESIAN_POINT('Ctrl Pts',(50.9540522540723,27.9611797266605,-177.348585219096));
#164190=CARTESIAN_POINT('Ctrl Pts',(50.9485682840283,27.9806899638649,-177.346136042567));
#164191=CARTESIAN_POINT('Ctrl Pts',(50.9429636339204,28.0006295427059,-177.343632969541));
#164192=CARTESIAN_POINT('Ctrl Pts',(50.9375817343943,28.0197766451743,-177.339997193887));
#164193=CARTESIAN_POINT('Ctrl Pts',(50.9324449578157,28.0380516774433,-177.335495637055));
#164194=CARTESIAN_POINT('Ctrl Pts',(50.927143870269,28.056911276356,-177.33085008814));
#164195=CARTESIAN_POINT('Ctrl Pts',(50.9221037610279,28.0748423967018,-177.325282469042));
#164196=CARTESIAN_POINT('Ctrl Pts',(50.917336776092,28.0918018268417,-177.319052501429));
#164197=CARTESIAN_POINT('Ctrl Pts',(50.9129266816434,28.107491553098,-177.31328895362));
#164198=CARTESIAN_POINT('Ctrl Pts',(50.9087501299518,28.1223504078232,-177.306958054975));
#164199=CARTESIAN_POINT('Ctrl Pts',(50.9048087093783,28.1363727401291,-177.30024154706));
#164200=CARTESIAN_POINT('Ctrl Pts',(50.8996792431315,28.1546217645412,-177.291500510673));
#164201=CARTESIAN_POINT('Ctrl Pts',(50.8949461632669,28.1714605711226,-177.282104513345));
#164202=CARTESIAN_POINT('Ctrl Pts',(50.8905963541135,28.1869358212966,-177.27239474607));
#164203=CARTESIAN_POINT('Ctrl Pts',(50.8862999250947,28.2022211617742,-177.262804135444));
#164204=CARTESIAN_POINT('Ctrl Pts',(50.88237724426,28.216176823995,-177.252906955805));
#164205=CARTESIAN_POINT('Ctrl Pts',(50.8788048595848,28.2288862428727,-177.242983686215));
#164206=CARTESIAN_POINT('Ctrl Pts',(50.8751876970077,28.2417549674139,-177.232936033829));
#164207=CARTESIAN_POINT('Ctrl Pts',(50.8719295997398,28.2533462507402,-177.222861821418));
#164208=CARTESIAN_POINT('Ctrl Pts',(50.8689980927258,28.2637756288644,-177.213007510384));
#164209=CARTESIAN_POINT('Ctrl Pts',(50.8686438432088,28.2650359370083,-177.211816694565));
#164210=CARTESIAN_POINT('Ctrl Pts',(50.8682943551355,28.266279305436,-177.210629037571));
#164211=CARTESIAN_POINT('Ctrl Pts',(50.8679495638095,28.2675059643168,-177.209444926082));
#164212=CARTESIAN_POINT('Ctrl Pts',(50.8675950038203,28.2687673770226,-177.208227266226));
#164213=CARTESIAN_POINT('Ctrl Pts',(50.8673603738187,28.2696021166119,-177.207413007318));
#164214=CARTESIAN_POINT('Ctrl Pts',(50.8670341531148,28.2707626510054,-177.206271333216));
#164215=CARTESIAN_POINT('Ctrl Pts',(50.8668269288771,28.2714998539238,-177.205546110866));
#164216=CARTESIAN_POINT('Ctrl Pts',(50.8665828163733,28.2723682710494,-177.204688490105));
#164217=CARTESIAN_POINT('Ctrl Pts',(50.8662496812106,28.2735533658467,-177.20350339534));
#164218=CARTESIAN_POINT('Ctrl Pts',(50.8604732024432,28.2941026074213,-177.182954154317));
#164219=CARTESIAN_POINT('Ctrl Pts',(50.8552932601851,28.312530288117,-177.160790380489));
#164220=CARTESIAN_POINT('Ctrl Pts',(50.8507218350651,28.3287935344193,-177.137499857922));
#164221=CARTESIAN_POINT('Ctrl Pts',(50.8461446451417,28.3450772895161,-177.114179964803));
#164222=CARTESIAN_POINT('Ctrl Pts',(50.8421775027915,28.3591911668972,-177.089730494042));
#164223=CARTESIAN_POINT('Ctrl Pts',(50.8388259245845,28.3711153074227,-177.064594612449));
#164224=CARTESIAN_POINT('Ctrl Pts',(50.8354685622628,28.3830600264916,-177.039415351644));
#164225=CARTESIAN_POINT('Ctrl Pts',(50.8327288833832,28.3928074701625,-177.013547309123));
#164226=CARTESIAN_POINT('Ctrl Pts',(50.8306059982581,28.4003605826727,-176.987389235391));
#164227=CARTESIAN_POINT('Ctrl Pts',(50.8284734638487,28.4079480268235,-176.961112263709));
#164228=CARTESIAN_POINT('Ctrl Pts',(50.8269633362407,28.4133211711029,-176.934542622323));
#164229=CARTESIAN_POINT('Ctrl Pts',(50.8260683264915,28.4165057296799,-176.90803735712));
#164230=CARTESIAN_POINT('Ctrl Pts',(50.8254119687592,28.4188411340129,-176.888599651797));
#164231=CARTESIAN_POINT('Ctrl Pts',(50.825086291307,28.41999998,-176.869195583603));
#164232=CARTESIAN_POINT('Ctrl Pts',(50.825086291307,28.41999998,-176.84995));
#164233=CARTESIAN_POINT('Origin',(51.6222122422086,12.4702093225365,-172.64995));
#164234=CARTESIAN_POINT('',(49.3103449325291,28.91999998,-171.64995));
#164235=CARTESIAN_POINT('',(48.9446667094463,31.5219357366587,-171.64995));
#164236=CARTESIAN_POINT('',(48.9446667094463,31.5219357366587,-171.64995));
#164237=CARTESIAN_POINT('',(50.3299522569362,28.85041342952,-172.64995));
#164238=CARTESIAN_POINT('Ctrl Pts',(49.3103449325291,28.91999998,-171.64995));
#164239=CARTESIAN_POINT('Ctrl Pts',(49.3387697982907,28.9180600288945,-171.64995));
#164240=CARTESIAN_POINT('Ctrl Pts',(49.3660105379016,28.9162008924831,-171.651127379994));
#164241=CARTESIAN_POINT('Ctrl Pts',(49.39199439745,28.9144275361028,-171.653186822974));
#164242=CARTESIAN_POINT('Ctrl Pts',(49.4189288617229,28.9125893024879,-171.655321609504));
#164243=CARTESIAN_POINT('Ctrl Pts',(49.4445132303009,28.91084321072,-171.658404102285));
#164244=CARTESIAN_POINT('Ctrl Pts',(49.4687098143076,28.9091918330042,-171.662141420469));
#164245=CARTESIAN_POINT('Ctrl Pts',(49.4943977208127,28.9074386749403,-171.666109083014));
#164246=CARTESIAN_POINT('Ctrl Pts',(49.5185218170459,28.9057922443977,-171.670814501406));
#164247=CARTESIAN_POINT('Ctrl Pts',(49.5410788798076,28.9042527613546,-171.675950032829));
#164248=CARTESIAN_POINT('Ctrl Pts',(49.5642968214887,28.9026681743944,-171.681236025528));
#164249=CARTESIAN_POINT('Ctrl Pts',(49.58585545163,28.9011968327624,-171.686977732447));
#164250=CARTESIAN_POINT('Ctrl Pts',(49.6057833608668,28.8998367851943,-171.692885218569));
#164251=CARTESIAN_POINT('Ctrl Pts',(49.6265086028921,28.8984223209531,-171.699029068292));
#164252=CARTESIAN_POINT('Ctrl Pts',(49.6454709588003,28.8971281708376,-171.705352160828));
#164253=CARTESIAN_POINT('Ctrl Pts',(49.6627257368561,28.8959505601483,-171.71157813447));
#164254=CARTESIAN_POINT('Ctrl Pts',(49.6679908341232,28.8955912257771,-171.713477918791));
#164255=CARTESIAN_POINT('Ctrl Pts',(49.6730970826779,28.8952427325736,-171.715369016405));
#164256=CARTESIAN_POINT('Ctrl Pts',(49.6780463437716,28.8949049535104,-171.717244495098));
#164257=CARTESIAN_POINT('Ctrl Pts',(49.6798101665193,28.8947845754611,-171.717912880119));
#164258=CARTESIAN_POINT('Ctrl Pts',(49.6806367975012,28.8947280884719,-171.718228248951));
#164259=CARTESIAN_POINT('Ctrl Pts',(49.6824087034236,28.8946071168897,-171.718908958993));
#164260=CARTESIAN_POINT('Ctrl Pts',(49.6832278792519,28.8945511901078,-171.719223660358));
#164261=CARTESIAN_POINT('Ctrl Pts',(49.6842489661727,28.8944814893959,-171.719616772033));
#164262=CARTESIAN_POINT('Ctrl Pts',(49.6856564824454,28.894385431517,-171.720163005656));
#164263=CARTESIAN_POINT('Ctrl Pts',(49.6906471357391,28.8940448375365,-171.72209979508));
#164264=CARTESIAN_POINT('Ctrl Pts',(49.6956056719285,28.8937064347848,-171.724069245188));
#164265=CARTESIAN_POINT('Ctrl Pts',(49.700531765415,28.8933702455351,-171.72607046184));
#164266=CARTESIAN_POINT('Ctrl Pts',(49.7339103492972,28.8910922698726,-171.739630451728));
#164267=CARTESIAN_POINT('Ctrl Pts',(49.7657873850126,28.8889167421851,-171.754642782234));
#164268=CARTESIAN_POINT('Ctrl Pts',(49.7961150464751,28.886846942254,-171.770779293223));
#164269=CARTESIAN_POINT('Ctrl Pts',(49.8251957834159,28.8848622423326,-171.786252350114));
#164270=CARTESIAN_POINT('Ctrl Pts',(49.8528524388002,28.8829747203074,-171.802759466709));
#164271=CARTESIAN_POINT('Ctrl Pts',(49.8790739238732,28.8811851463695,-171.820043746592));
#164272=CARTESIAN_POINT('Ctrl Pts',(49.9084566554647,28.8791798224706,-171.839411808894));
#164273=CARTESIAN_POINT('Ctrl Pts',(49.9360378533926,28.8772974503299,-171.859755775837));
#164274=CARTESIAN_POINT('Ctrl Pts',(49.9618408880107,28.8755364349585,-171.880757614645));
#164275=CARTESIAN_POINT('Ctrl Pts',(49.9739768129737,28.8747081777119,-171.890635396217));
#164276=CARTESIAN_POINT('Ctrl Pts',(49.9857198845137,28.873906732076,-171.900659292158));
#164277=CARTESIAN_POINT('Ctrl Pts',(49.9970749837527,28.8731317649219,-171.910799109277));
#164278=CARTESIAN_POINT('Ctrl Pts',(50.0025718000368,28.8727566161027,-171.915707627528));
#164279=CARTESIAN_POINT('Ctrl Pts',(50.0076545474091,28.8724097268114,-171.920348851347));
#164280=CARTESIAN_POINT('Ctrl Pts',(50.012779864146,28.8720599218503,-171.925124127316));
#164281=CARTESIAN_POINT('Ctrl Pts',(50.0177522253248,28.8717205561685,-171.929756894044));
#164282=CARTESIAN_POINT('Ctrl Pts',(50.0227648025355,28.8713784360368,-171.934515912421));
#164283=CARTESIAN_POINT('Ctrl Pts',(50.0282013560687,28.8710073610315,-171.939801580878));
#164284=CARTESIAN_POINT('Ctrl Pts',(50.0292239414366,28.8709375638947,-171.940795785605));
#164285=CARTESIAN_POINT('Ctrl Pts',(50.0302614214281,28.8708667495457,-171.941808724723));
#164286=CARTESIAN_POINT('Ctrl Pts',(50.0313161929975,28.8707947543342,-171.94284321151));
#164287=CARTESIAN_POINT('Ctrl Pts',(50.0657213376989,28.8684463731845,-171.976586695524));
#164288=CARTESIAN_POINT('Ctrl Pts',(50.0973150935852,28.8662900773931,-172.012463058192));
#164289=CARTESIAN_POINT('Ctrl Pts',(50.1259713060629,28.8643343614516,-172.049959758195));
#164290=CARTESIAN_POINT('Ctrl Pts',(50.1550924391609,28.8623469158224,-172.088064807575));
#164291=CARTESIAN_POINT('Ctrl Pts',(50.1811799728969,28.8605666089807,-172.127843233018));
#164292=CARTESIAN_POINT('Ctrl Pts',(50.2041280177626,28.8590005519064,-172.168804472477));
#164293=CARTESIAN_POINT('Ctrl Pts',(50.2221470021198,28.8577708716399,-172.200967558151));
#164294=CARTESIAN_POINT('Ctrl Pts',(50.2382308735885,28.8566732504164,-172.233860874948));
#164295=CARTESIAN_POINT('Ctrl Pts',(50.2523392709864,28.855710388276,-172.267266567535));
#164296=CARTESIAN_POINT('Ctrl Pts',(50.2537365321953,28.8556150287621,-172.270574985713));
#164297=CARTESIAN_POINT('Ctrl Pts',(50.2551143945883,28.8555209925606,-172.273888354216));
#164298=CARTESIAN_POINT('Ctrl Pts',(50.2564728993336,28.8554282768094,-172.277206441568));
#164299=CARTESIAN_POINT('Ctrl Pts',(50.2742353236811,28.8542160200819,-172.320590372148));
#164300=CARTESIAN_POINT('Ctrl Pts',(50.2886872409692,28.8532297001058,-172.364775502692));
#164301=CARTESIAN_POINT('Ctrl Pts',(50.2999236581919,28.8524628328074,-172.409267414542));
#164302=CARTESIAN_POINT('Ctrl Pts',(50.3112922397379,28.8516869455078,-172.45428264653));
#164303=CARTESIAN_POINT('Ctrl Pts',(50.3193692508111,28.8511357025681,-172.49961195027));
#164304=CARTESIAN_POINT('Ctrl Pts',(50.3242616856201,28.8508018018068,-172.54479624059));
#164305=CARTESIAN_POINT('Ctrl Pts',(50.3280734120039,28.8505416576473,-172.579999602161));
#164306=CARTESIAN_POINT('Ctrl Pts',(50.3299522569362,28.85041342952,-172.615116019851));
#164307=CARTESIAN_POINT('Ctrl Pts',(50.3299522569362,28.85041342952,-172.64995));
#164308=CARTESIAN_POINT('',(49.9349347781878,31.6611088376188,-172.64995));
#164309=CARTESIAN_POINT('',(50.3904429223989,28.41999998,-172.64995));
#164310=CARTESIAN_POINT('Origin',(48.9446667094463,31.5219357366587,-172.64995));
#164311=CARTESIAN_POINT('Origin',(46.9641305719631,31.2435895347386,-172.64995));
#164312=CARTESIAN_POINT('',(49.1485087381009,33.2999192814719,-172.64995));
#164313=CARTESIAN_POINT('Origin',(46.9641305719631,31.2435895347386,-172.64995));
#164314=CARTESIAN_POINT('',(48.4203826827217,32.6144760325608,-171.64995));
#164315=CARTESIAN_POINT('Origin',(48.4203826827217,32.6144760325608,-172.64995));
#164316=CARTESIAN_POINT('Origin',(46.9641305719631,31.2435895347386,-171.64995));
#164317=CARTESIAN_POINT('Origin',(0.,-12.9675000200281,-172.64995));
#164318=CARTESIAN_POINT('',(46.2674193015002,36.1810087180727,-172.64995));
#164319=CARTESIAN_POINT('Origin',(0.,-12.9675000200281,-172.64995));
#164320=CARTESIAN_POINT('',(45.5819760525891,35.4528826626933,-171.64995));
#164321=CARTESIAN_POINT('Origin',(45.5819760525891,35.4528826626933,-172.64995));
#164322=CARTESIAN_POINT('Origin',(0.,-12.9675000200281,-171.64995));
#164323=CARTESIAN_POINT('Origin',(44.2110895547669,33.9966305519348,-172.64995));
#164324=CARTESIAN_POINT('',(44.628608857647,36.9674347581595,-172.64995));
#164325=CARTESIAN_POINT('Origin',(44.2110895547669,33.9966305519348,-172.64995));
#164326=CARTESIAN_POINT('',(44.489435756687,35.9771666894179,-171.64995));
#164327=CARTESIAN_POINT('Origin',(44.489435756687,35.9771666894179,-172.64995));
#164328=CARTESIAN_POINT('Origin',(44.2110895547669,33.9966305519348,-171.64995));
#164329=CARTESIAN_POINT('Origin',(45.4220505312374,35.8460962305468,-172.64995));
#164330=CARTESIAN_POINT('',(41.93041344952,37.3466413930079,-172.64995));
#164331=CARTESIAN_POINT('',(44.628608857647,36.9674347581595,-172.64995));
#164332=CARTESIAN_POINT('',(42.,36.3270340686007,-171.64995));
#164333=CARTESIAN_POINT('Ctrl Pts',(41.93041344952,37.3466413930079,-172.64995));
#164334=CARTESIAN_POINT('Ctrl Pts',(41.93041344952,37.3466413930079,-172.605172304593));
#164335=CARTESIAN_POINT('Ctrl Pts',(41.9306253528176,37.3435365091946,-172.559925284252));
#164336=CARTESIAN_POINT('Ctrl Pts',(41.9310569582364,37.337212470379,-172.514629908656));
#164337=CARTESIAN_POINT('Ctrl Pts',(41.9314834585311,37.3309632336908,-172.469870296763));
#164338=CARTESIAN_POINT('Ctrl Pts',(41.9321244954995,37.321570528007,-172.425063433264));
#164339=CARTESIAN_POINT('Ctrl Pts',(41.9329870509292,37.3089320536492,-172.380665523369));
#164340=CARTESIAN_POINT('Ctrl Pts',(41.9336634036616,37.2990218886089,-172.345851937327));
#164341=CARTESIAN_POINT('Ctrl Pts',(41.9344759477384,37.2871161986963,-172.311290758663));
#164342=CARTESIAN_POINT('Ctrl Pts',(41.93542780341,37.2731692648717,-172.277224099708));
#164343=CARTESIAN_POINT('Ctrl Pts',(41.9355206785256,37.2718084250625,-172.273900124256));
#164344=CARTESIAN_POINT('Ctrl Pts',(41.9356148798764,37.2704281527738,-172.270580868726));
#164345=CARTESIAN_POINT('Ctrl Pts',(41.9357104102735,37.269028406819,-172.267266567635));
#164346=CARTESIAN_POINT('Ctrl Pts',(41.9369407919429,37.2510004092627,-172.224580098873));
#164347=CARTESIAN_POINT('Ctrl Pts',(41.9383914477948,37.2297448746573,-172.182726614124));
#164348=CARTESIAN_POINT('Ctrl Pts',(41.9400563415622,37.2053502485713,-172.142169045052));
#164349=CARTESIAN_POINT('Ctrl Pts',(41.9416543121738,37.1819362047876,-172.103241754481));
#164350=CARTESIAN_POINT('Ctrl Pts',(41.9434495675826,37.1556314727481,-172.065509331767));
#164351=CARTESIAN_POINT('Ctrl Pts',(41.9454355793453,37.1265317095662,-172.029413465262));
#164352=CARTESIAN_POINT('Ctrl Pts',(41.946357166588,37.113028279718,-172.01266356946));
#164353=CARTESIAN_POINT('Ctrl Pts',(41.9473198149722,37.0989232071639,-171.996266629114));
#164354=CARTESIAN_POINT('Ctrl Pts',(41.9483227216382,37.0842282556921,-171.980270641983));
#164355=CARTESIAN_POINT('Ctrl Pts',(41.9486805968113,37.0789845391231,-171.974562666498));
#164356=CARTESIAN_POINT('Ctrl Pts',(41.9490626478473,37.073386589124,-171.968608245876));
#164357=CARTESIAN_POINT('Ctrl Pts',(41.9494436601674,37.0678037504325,-171.96281560598));
#164358=CARTESIAN_POINT('Ctrl Pts',(41.9498361130009,37.0620532779482,-171.95684903267));
#164359=CARTESIAN_POINT('Ctrl Pts',(41.9502274528427,37.0563189984669,-171.951054248039));
#164360=CARTESIAN_POINT('Ctrl Pts',(41.95058728953,37.0510460804859,-171.945838282772));
#164361=CARTESIAN_POINT('Ctrl Pts',(41.950657753626,37.050013524852,-171.944816879757));
#164362=CARTESIAN_POINT('Ctrl Pts',(41.9507270018928,37.0489987750081,-171.943817557184));
#164363=CARTESIAN_POINT('Ctrl Pts',(41.9507947956297,37.0480053275874,-171.942843213006));
#164364=CARTESIAN_POINT('Ctrl Pts',(41.9523067381499,37.025849366502,-171.921113294297));
#164365=CARTESIAN_POINT('Ctrl Pts',(41.953933863454,37.002008447526,-171.899758993298));
#164366=CARTESIAN_POINT('Ctrl Pts',(41.9556797558124,36.9764279216952,-171.879051282457));
#164367=CARTESIAN_POINT('Ctrl Pts',(41.9573985368362,36.9512446266509,-171.85866513421));
#164368=CARTESIAN_POINT('Ctrl Pts',(41.9592324446076,36.9243750459795,-171.838905512141));
#164369=CARTESIAN_POINT('Ctrl Pts',(41.9611826656455,36.8957997014518,-171.820067900506));
#164370=CARTESIAN_POINT('Ctrl Pts',(41.9630380210983,36.8686143618144,-171.80214661631));
#164371=CARTESIAN_POINT('Ctrl Pts',(41.964998836786,36.8398837806431,-171.785058882888));
#164372=CARTESIAN_POINT('Ctrl Pts',(41.9670643335467,36.8096193745015,-171.769091901481));
#164373=CARTESIAN_POINT('Ctrl Pts',(41.9690687839745,36.7802494413244,-171.753596828662));
#164374=CARTESIAN_POINT('Ctrl Pts',(41.9711718608506,36.7494343977296,-171.739157140834));
#164375=CARTESIAN_POINT('Ctrl Pts',(41.9733703800159,36.7172208991694,-171.726070467489));
#164376=CARTESIAN_POINT('Ctrl Pts',(41.9734065577268,36.7166908102542,-171.725855119862));
#164377=CARTESIAN_POINT('Ctrl Pts',(41.9734427611061,36.716160345237,-171.725640139903));
#164378=CARTESIAN_POINT('Ctrl Pts',(41.9734789901357,36.7156295043819,-171.725425528673));
#164379=CARTESIAN_POINT('Ctrl Pts',(41.973660741901,36.7129664117315,-171.724348879083));
#164380=CARTESIAN_POINT('Ctrl Pts',(41.9738919207081,36.709578749863,-171.722996951206));
#164381=CARTESIAN_POINT('Ctrl Pts',(41.9740840512554,36.7067631719946,-171.721889199711));
#164382=CARTESIAN_POINT('Ctrl Pts',(41.9742095140083,36.7049245775841,-171.721165829305));
#164383=CARTESIAN_POINT('Ctrl Pts',(41.9743182873496,36.7033304946806,-171.720545222455));
#164384=CARTESIAN_POINT('Ctrl Pts',(41.9743854868274,36.7023456178558,-171.720163007342));
#164385=CARTESIAN_POINT('Ctrl Pts',(41.9754591786029,36.686609570775,-171.714056096453));
#164386=CARTESIAN_POINT('Ctrl Pts',(41.9766482085272,36.6691851406408,-171.707738814436));
#164387=CARTESIAN_POINT('Ctrl Pts',(41.9779569888288,36.6500072100763,-171.701466818902));
#164388=CARTESIAN_POINT('Ctrl Pts',(41.9792886147671,36.6304945158891,-171.695085341485));
#164389=CARTESIAN_POINT('Ctrl Pts',(41.980744279009,36.6091655329514,-171.688750401779));
#164390=CARTESIAN_POINT('Ctrl Pts',(41.9823272482974,36.5859718986434,-171.682785652356));
#164391=CARTESIAN_POINT('Ctrl Pts',(41.9837542430735,36.5650635997658,-171.677408626831));
#164392=CARTESIAN_POINT('Ctrl Pts',(41.9852847155951,36.5426396506425,-171.672333011434));
#164393=CARTESIAN_POINT('Ctrl Pts',(41.9869193433264,36.518689754704,-171.667836203536));
#164394=CARTESIAN_POINT('Ctrl Pts',(41.9885007733798,36.4955192893508,-171.663485740725));
#164395=CARTESIAN_POINT('Ctrl Pts',(41.9901797252878,36.4709200605105,-171.659677091772));
#164396=CARTESIAN_POINT('Ctrl Pts',(41.9919546757492,36.4449140458738,-171.65669742379));
#164397=CARTESIAN_POINT('Ctrl Pts',(41.993647385108,36.4201130019462,-171.653855816664));
#164398=CARTESIAN_POINT('Ctrl Pts',(41.9954274262957,36.3940321765311,-171.651768285733));
#164399=CARTESIAN_POINT('Ctrl Pts',(41.9972910935929,36.3667255630958,-171.650715593431));
#164400=CARTESIAN_POINT('Ctrl Pts',(41.9981754755464,36.3537675226929,-171.650216050365));
#164401=CARTESIAN_POINT('Ctrl Pts',(41.9990786513334,36.340534002745,-171.64995));
#164402=CARTESIAN_POINT('Ctrl Pts',(42.,36.3270340686007,-171.64995));
#164403=CARTESIAN_POINT('',(41.3608268990399,36.416863989729,-171.64995));
#164404=CARTESIAN_POINT('Origin',(42.,28.91999998,-171.14995));
#164405=CARTESIAN_POINT('',(42.,28.41999998,-171.14995));
#164406=CARTESIAN_POINT('',(41.5,28.91999998,-171.14995));
#164407=CARTESIAN_POINT('Origin',(42.,28.91999998,-171.14995));
#164408=CARTESIAN_POINT('',(42.,28.91999998,-171.64995));
#164409=CARTESIAN_POINT('Origin',(42.,28.91999998,-171.14995));
#164410=CARTESIAN_POINT('Origin',(42.,28.91999998,-171.14995));
#164411=CARTESIAN_POINT('Ctrl Pts',(36.7529144574179,29.9771506489281,-64.6451542155005));
#164412=CARTESIAN_POINT('Ctrl Pts',(37.9544308619569,28.41999998,-65.5068366539031));
#164413=CARTESIAN_POINT('Ctrl Pts',(39.6993756576748,28.41999998,-66.758245524204));
#164414=CARTESIAN_POINT('Ctrl Pts',(35.4221830133223,29.9261764058054,-66.5837572422386));
#164415=CARTESIAN_POINT('Ctrl Pts',(36.6139893647491,28.4199999799959,-67.4471428080874));
#164416=CARTESIAN_POINT('Ctrl Pts',(38.3090750828473,28.41999998,-68.6968587227942));
#164417=CARTESIAN_POINT('Ctrl Pts',(34.0676680572731,29.8734031042169,-68.5045591474479));
#164418=CARTESIAN_POINT('Ctrl Pts',(35.2435893151229,28.41999998,-69.3754183593105));
#164419=CARTESIAN_POINT('Ctrl Pts',(36.8898270007225,28.4199999800001,-70.617650456175));
#164420=CARTESIAN_POINT('Ctrl Pts',(31.2955902801573,29.7642394885798,-72.2991303428252));
#164421=CARTESIAN_POINT('Ctrl Pts',(32.4319411374915,28.41999998,-73.1856180617498));
#164422=CARTESIAN_POINT('Ctrl Pts',(33.9748337796689,28.4199999800001,-74.4122216515051));
#164423=CARTESIAN_POINT('Ctrl Pts',(29.8799523105758,29.7079117212239,-74.1702869851635));
#164424=CARTESIAN_POINT('Ctrl Pts',(30.9935194672858,28.4199999800042,-75.0646492888564));
#164425=CARTESIAN_POINT('Ctrl Pts',(32.4811021033977,28.41999998,-76.2833884926716));
#164426=CARTESIAN_POINT('Ctrl Pts',(28.4305705461597,29.6502955521147,-75.9979827843214));
#164427=CARTESIAN_POINT('Ctrl Pts',(29.5115669185301,28.41999998,-76.9063064032585));
#164428=CARTESIAN_POINT('Ctrl Pts',(30.9453615210646,28.41999998,-78.1110740930249));
#164429=CARTESIAN_POINT('',(31.,28.41999998,-78.0460091084363));
#164430=CARTESIAN_POINT('',(37.,28.41999998,-70.4461836365688));
#164431=CARTESIAN_POINT('Ctrl Pts',(31.,28.41999998,-78.0460091084363));
#164432=CARTESIAN_POINT('Ctrl Pts',(31.6054626504307,28.4199999800001,-77.3245680023315));
#164433=CARTESIAN_POINT('Ctrl Pts',(32.203700232555,28.4199999800031,-76.5972335154402));
#164434=CARTESIAN_POINT('Ctrl Pts',(32.7954596657013,28.4199999800058,-75.8646586780434));
#164435=CARTESIAN_POINT('Ctrl Pts',(33.4345463105989,28.4199999800088,-75.0734946192315));
#164436=CARTESIAN_POINT('Ctrl Pts',(34.0660773010416,28.4199999800106,-74.2762178948239));
#164437=CARTESIAN_POINT('Ctrl Pts',(34.6909510193213,28.4199999800288,-73.4736062556159));
#164438=CARTESIAN_POINT('Ctrl Pts',(34.939102988304,28.4199999800361,-73.15487040104));
#164439=CARTESIAN_POINT('Ctrl Pts',(35.1862046047012,28.4199999800463,-72.8352927773716));
#164440=CARTESIAN_POINT('Ctrl Pts',(35.4323104279066,28.4199999800634,-72.5149207187905));
#164441=CARTESIAN_POINT('Ctrl Pts',(35.9594751118247,28.4199999801002,-71.8286759449022));
#164442=CARTESIAN_POINT('Ctrl Pts',(36.4818085017622,28.4199999801598,-71.1391285306312));
#164443=CARTESIAN_POINT('Ctrl Pts',(37.,28.4199999803545,-70.4461836365688));
#164444=CARTESIAN_POINT('Ctrl Pts',(31.,28.41999998,-78.0460091084363));
#164445=CARTESIAN_POINT('Ctrl Pts',(30.9953507488642,28.41999998,-77.9571322255713));
#164446=CARTESIAN_POINT('Ctrl Pts',(30.9904343156938,28.4210644426645,-77.8631868791632));
#164447=CARTESIAN_POINT('Ctrl Pts',(30.9852500369792,28.4236029528388,-77.7641731707001));
#164448=CARTESIAN_POINT('Ctrl Pts',(30.9804902860296,28.4259335906918,-77.6732674499945));
#164449=CARTESIAN_POINT('Ctrl Pts',(30.9755047623887,28.4295072224175,-77.5780895208821));
#164450=CARTESIAN_POINT('Ctrl Pts',(30.9702932674828,28.4346829171186,-77.4786459095534));
#164451=CARTESIAN_POINT('Ctrl Pts',(30.9647250948557,28.4402128393543,-77.372396320033));
#164452=CARTESIAN_POINT('Ctrl Pts',(30.9588989638651,28.4475712846398,-77.2612772547267));
#164453=CARTESIAN_POINT('Ctrl Pts',(30.9528170728823,28.4572452512149,-77.1453434183624));
#164454=CARTESIAN_POINT('Ctrl Pts',(30.9494041569204,28.4626738975081,-77.0802859482809));
#164455=CARTESIAN_POINT('Ctrl Pts',(30.9459106839778,28.4688326969503,-77.0137119621315));
#164456=CARTESIAN_POINT('Ctrl Pts',(30.942337363506,28.4758143402156,-76.9456372159907));
#164457=CARTESIAN_POINT('Ctrl Pts',(30.9405507032701,28.4793051618483,-76.9115998429203));
#164458=CARTESIAN_POINT('Ctrl Pts',(30.9387440785685,28.483001778153,-76.8771872300242));
#164459=CARTESIAN_POINT('Ctrl Pts',(30.9369176023688,28.4869161892589,-76.8424018044853));
#164460=CARTESIAN_POINT('Ctrl Pts',(30.9360043642689,28.4888733948118,-76.8250090917158));
#164461=CARTESIAN_POINT('Ctrl Pts',(30.9350861633931,28.4908850535414,-76.8075231775984));
#164462=CARTESIAN_POINT('Ctrl Pts',(30.9341630151144,28.4929526905484,-76.7899443889576));
#164463=CARTESIAN_POINT('Ctrl Pts',(30.9337014409751,28.493986509052,-76.7811549946371));
#164464=CARTESIAN_POINT('Ctrl Pts',(30.9332386299823,28.4950343224187,-76.772342381627));
#164465=CARTESIAN_POINT('Ctrl Pts',(30.9327745841645,28.4960963227561,-76.7635065927854));
#164466=CARTESIAN_POINT('Ctrl Pts',(30.9327340001398,28.4961892020499,-76.7627338417804));
#164467=CARTESIAN_POINT('Ctrl Pts',(30.9326934066704,28.4962821898565,-76.7619609135104));
#164468=CARTESIAN_POINT('Ctrl Pts',(30.9326528037575,28.4963752863047,-76.7611878080044));
#164469=CARTESIAN_POINT('Ctrl Pts',(30.9326153917186,28.4964610665529,-76.7604754587855));
#164470=CARTESIAN_POINT('Ctrl Pts',(30.9325775167222,28.4965479821107,-76.7597542967421));
#164471=CARTESIAN_POINT('Ctrl Pts',(30.932539159609,28.4966360826217,-76.759023957238));
#164472=CARTESIAN_POINT('Ctrl Pts',(30.9321431556995,28.4975456439494,-76.7514838356034));
#164473=CARTESIAN_POINT('Ctrl Pts',(30.9317015992017,28.4985703405887,-76.7430766793829));
#164474=CARTESIAN_POINT('Ctrl Pts',(30.9313787443117,28.4993250778052,-76.7369297425032));
#164475=CARTESIAN_POINT('Ctrl Pts',(30.9243094913047,28.5158508561152,-76.6023359873139));
#164476=CARTESIAN_POINT('Ctrl Pts',(30.9170546130173,28.5350544953412,-76.4677566994279));
#164477=CARTESIAN_POINT('Ctrl Pts',(30.9097979232358,28.5569559412352,-76.333337137572));
#164478=CARTESIAN_POINT('Ctrl Pts',(30.9054759833442,28.5700000061663,-76.2532795239633));
#164479=CARTESIAN_POINT('Ctrl Pts',(30.9011530346219,28.5840000959786,-76.1732784199905));
#164480=CARTESIAN_POINT('Ctrl Pts',(30.8968642854843,28.5989526153992,-76.0933627491102));
#164481=CARTESIAN_POINT('Ctrl Pts',(30.8939918578668,28.6089671973573,-76.0398385226402));
#164482=CARTESIAN_POINT('Ctrl Pts',(30.8911353205105,28.6194087482988,-75.9863527556447));
#164483=CARTESIAN_POINT('Ctrl Pts',(30.8883057354998,28.630274392489,-75.9329141284561));
#164484=CARTESIAN_POINT('Ctrl Pts',(30.8854761504891,28.6411400366793,-75.8794755012675));
#164485=CARTESIAN_POINT('Ctrl Pts',(30.8826735236571,28.6524297677877,-75.8260840188183));
#164486=CARTESIAN_POINT('Ctrl Pts',(30.879908391992,28.6641395635773,-75.7727479419548));
#164487=CARTESIAN_POINT('Ctrl Pts',(30.8771432603269,28.6758493593668,-75.7194118650914));
#164488=CARTESIAN_POINT('Ctrl Pts',(30.8744156231211,28.687979218675,-75.6661311939467));
#164489=CARTESIAN_POINT('Ctrl Pts',(30.8717358482434,28.700523890345,-75.6129139541153));
#164490=CARTESIAN_POINT('Ctrl Pts',(30.8703959608046,28.70679622618,-75.5863053341995));
#164491=CARTESIAN_POINT('Ctrl Pts',(30.8690680299892,28.7131722483955,-75.5597125647804));
#164492=CARTESIAN_POINT('Ctrl Pts',(30.8677533039181,28.7196512016491,-75.5331366064521));
#164493=CARTESIAN_POINT('Ctrl Pts',(30.8670959408825,28.7228906782759,-75.519848627288));
#164494=CARTESIAN_POINT('Ctrl Pts',(30.8664418784498,28.7261558866934,-75.5065648504057));
#164495=CARTESIAN_POINT('Ctrl Pts',(30.8657912703874,28.7294467262534,-75.4932853935933));
#164496=CARTESIAN_POINT('Ctrl Pts',(30.8654659663562,28.7310921460333,-75.4866456651871));
#164497=CARTESIAN_POINT('Ctrl Pts',(30.8651415258812,28.7327439735401,-75.4800070167672));
#164498=CARTESIAN_POINT('Ctrl Pts',(30.8648179680418,28.7344021958109,-75.4733694629099));
#164499=CARTESIAN_POINT('Ctrl Pts',(30.8645513322407,28.7357686946863,-75.4678996232866));
#164500=CARTESIAN_POINT('Ctrl Pts',(30.8643311330534,28.7369019898584,-75.4633764419093));
#164501=CARTESIAN_POINT('Ctrl Pts',(30.8640263227981,28.738394063327,-75.4574625920758));
#164502=CARTESIAN_POINT('Ctrl Pts',(30.8639612511876,28.7387125946821,-75.4562000894974));
#164503=CARTESIAN_POINT('Ctrl Pts',(30.8638923228878,28.7390475481913,-75.4548741968345));
#164504=CARTESIAN_POINT('Ctrl Pts',(30.8638182635132,28.7394047935033,-75.4534621817682));
#164505=CARTESIAN_POINT('Ctrl Pts',(30.858008398083,28.7674302420227,-75.3426913634633));
#164506=CARTESIAN_POINT('Ctrl Pts',(30.8523016334403,28.7968590694777,-75.234384024023));
#164507=CARTESIAN_POINT('Ctrl Pts',(30.8467210193799,28.8275021583711,-75.1285627604439));
#164508=CARTESIAN_POINT('Ctrl Pts',(30.8458318845886,28.832384387487,-75.1117027220868));
#164509=CARTESIAN_POINT('Ctrl Pts',(30.8449459413324,28.8372974903014,-75.0949056976548));
#164510=CARTESIAN_POINT('Ctrl Pts',(30.8440632708079,28.8422407586805,-75.0781716749711));
#164511=CARTESIAN_POINT('Ctrl Pts',(30.8392462368768,28.8692178592538,-74.9868484090043));
#164512=CARTESIAN_POINT('Ctrl Pts',(30.8345268703748,28.8970918830449,-74.8974052661039));
#164513=CARTESIAN_POINT('Ctrl Pts',(30.8299062263507,28.9257497007075,-74.8098577609863));
#164514=CARTESIAN_POINT('Ctrl Pts',(30.8239245086087,28.9628490694253,-74.6965219441801));
#164515=CARTESIAN_POINT('Ctrl Pts',(30.8181056496567,29.0012784332636,-74.586316278858));
#164516=CARTESIAN_POINT('Ctrl Pts',(30.8124473228795,29.0407768010215,-74.4793548016011));
#164517=CARTESIAN_POINT('Ctrl Pts',(30.8074704278574,29.07551838411,-74.385274684869));
#164518=CARTESIAN_POINT('Ctrl Pts',(30.8026176973093,29.1110871607376,-74.2937033724066));
#164519=CARTESIAN_POINT('Ctrl Pts',(30.7978867098362,29.1473126769893,-74.2046860321974));
#164520=CARTESIAN_POINT('Ctrl Pts',(30.7955318228038,29.1653442188076,-74.1603769357753));
#164521=CARTESIAN_POINT('Ctrl Pts',(30.7932062256382,29.1835361617856,-74.1166837486454));
#164522=CARTESIAN_POINT('Ctrl Pts',(30.7909090745396,29.2018763553954,-74.073600366696));
#164523=CARTESIAN_POINT('Ctrl Pts',(30.784538562423,29.2527378009856,-73.9541205436641));
#164524=CARTESIAN_POINT('Ctrl Pts',(30.7784374998368,29.3046763395262,-73.8394377704279));
#164525=CARTESIAN_POINT('Ctrl Pts',(30.7726131471017,29.3573237688943,-73.7294995389662));
#164526=CARTESIAN_POINT('Ctrl Pts',(30.7685560771346,29.3939963940342,-73.6529198540828));
#164527=CARTESIAN_POINT('Ctrl Pts',(30.7646331869072,29.4310117754566,-73.5786417333732));
#164528=CARTESIAN_POINT('Ctrl Pts',(30.7608459868074,29.4682320688712,-73.5066413939787));
#164529=CARTESIAN_POINT('Ctrl Pts',(30.7545181321184,29.5304217081824,-73.3863394101293));
#164530=CARTESIAN_POINT('Ctrl Pts',(30.7485612047523,29.5931874761478,-73.2724011812726));
#164531=CARTESIAN_POINT('Ctrl Pts',(30.7429002557377,29.6558866113949,-73.1647049054821));
#164532=CARTESIAN_POINT('Ctrl Pts',(30.7403095914777,29.6845801057894,-73.1154190186269));
#164533=CARTESIAN_POINT('Ctrl Pts',(30.7377811237821,29.7132588940408,-73.0674402016844));
#164534=CARTESIAN_POINT('Ctrl Pts',(30.7353086514483,29.741858118838,-73.0207560182717));
#164535=CARTESIAN_POINT('Ctrl Pts',(36.7055659821298,29.9753365605362,-64.7141088904942));
#164536=CARTESIAN_POINT('Ctrl Pts',(36.7103806723968,29.9138048831183,-64.8077062813706));
#164537=CARTESIAN_POINT('Ctrl Pts',(36.7154239961427,29.8523768893488,-64.9057516538932));
#164538=CARTESIAN_POINT('Ctrl Pts',(36.720700743777,29.7914623159788,-65.0083394071988));
#164539=CARTESIAN_POINT('Ctrl Pts',(36.72586695935,29.731823720507,-65.1087782542803));
#164540=CARTESIAN_POINT('Ctrl Pts',(36.7312569354101,29.6726779118629,-65.2135714316818));
#164541=CARTESIAN_POINT('Ctrl Pts',(36.7368742111855,29.6143645132415,-65.3227893322482));
#164542=CARTESIAN_POINT('Ctrl Pts',(36.7419663316423,29.5615027948742,-65.4217965250528));
#164543=CARTESIAN_POINT('Ctrl Pts',(36.7472447702708,29.5093303810589,-65.5244308868896));
#164544=CARTESIAN_POINT('Ctrl Pts',(36.7527092637514,29.4580763652213,-65.630689057867));
#164545=CARTESIAN_POINT('Ctrl Pts',(36.7579504941924,29.408916436862,-65.7326058342887));
#164546=CARTESIAN_POINT('Ctrl Pts',(36.7633629109637,29.360601408339,-65.8378568245558));
#164547=CARTESIAN_POINT('Ctrl Pts',(36.7689447807834,29.3132934632658,-65.9464101551646));
#164548=CARTESIAN_POINT('Ctrl Pts',(36.7701147474361,29.3033776608683,-65.9691630643058));
#164549=CARTESIAN_POINT('Ctrl Pts',(36.7712921542238,29.2935059409922,-65.9920609696869));
#164550=CARTESIAN_POINT('Ctrl Pts',(36.7724769784619,29.2836795313646,-66.015103448616));
#164551=CARTESIAN_POINT('Ctrl Pts',(36.7728652777524,29.2804591483213,-66.0226550988353));
#164552=CARTESIAN_POINT('Ctrl Pts',(36.7733444989399,29.2765012562496,-66.0319750492162));
#164553=CARTESIAN_POINT('Ctrl Pts',(36.773659114264,29.2739116254867,-66.0380915384093));
#164554=CARTESIAN_POINT('Ctrl Pts',(36.7736772492176,29.2737623548375,-66.0384441030783));
#164555=CARTESIAN_POINT('Ctrl Pts',(36.7736948370056,29.2736176171791,-66.0387860190953));
#164556=CARTESIAN_POINT('Ctrl Pts',(36.7737118286106,29.2734778116659,-66.0391163327188));
#164557=CARTESIAN_POINT('Ctrl Pts',(36.7739318943408,29.2716671291314,-66.0433943693668));
#164558=CARTESIAN_POINT('Ctrl Pts',(36.7741524800775,29.2698557797349,-66.0476826125677));
#164559=CARTESIAN_POINT('Ctrl Pts',(36.7743735861458,29.2680437946507,-66.0519810661563));
#164560=CARTESIAN_POINT('Ctrl Pts',(36.7830263907577,29.1971332447106,-66.2201975214263));
#164561=CARTESIAN_POINT('Ctrl Pts',(36.7924804704293,29.125303390636,-66.4041364543566));
#164562=CARTESIAN_POINT('Ctrl Pts',(36.8027632687972,29.0549146566565,-66.6041834017324));
#164563=CARTESIAN_POINT('Ctrl Pts',(36.8041298320501,29.0455601352671,-66.630769239299));
#164564=CARTESIAN_POINT('Ctrl Pts',(36.8055110279142,29.0362310691301,-66.6576394973203));
#164565=CARTESIAN_POINT('Ctrl Pts',(36.8069069162596,29.026932976743,-66.6847949968068));
#164566=CARTESIAN_POINT('Ctrl Pts',(36.8132112795187,28.98493925123,-66.8074395720736));
#164567=CARTESIAN_POINT('Ctrl Pts',(36.819813780274,28.9435824406279,-66.9358954277359));
#164568=CARTESIAN_POINT('Ctrl Pts',(36.8267147784773,28.9033780952543,-67.0701745666682));
#164569=CARTESIAN_POINT('Ctrl Pts',(36.8330290005385,28.8665922336971,-67.1930362565894));
#164570=CARTESIAN_POINT('Ctrl Pts',(36.839593079154,28.830771907803,-67.320772322381));
#164571=CARTESIAN_POINT('Ctrl Pts',(36.8464052868298,28.7962973206778,-67.4533537498322));
#164572=CARTESIAN_POINT('Ctrl Pts',(36.8465175503647,28.7957291878196,-67.4555386596919));
#164573=CARTESIAN_POINT('Ctrl Pts',(36.8467080818096,28.794766653035,-67.4592468559418));
#164574=CARTESIAN_POINT('Ctrl Pts',(36.8467422843428,28.7945940172133,-67.4599124240971));
#164575=CARTESIAN_POINT('Ctrl Pts',(36.8470175925643,28.7932044107582,-67.4652698162981));
#164576=CARTESIAN_POINT('Ctrl Pts',(36.8473091770429,28.7917368396073,-67.4709441072806));
#164577=CARTESIAN_POINT('Ctrl Pts',(36.8476170703693,28.7901927171027,-67.4769359322928));
#164578=CARTESIAN_POINT('Ctrl Pts',(36.8489153744216,28.7836815642673,-67.5022018605477));
#164579=CARTESIAN_POINT('Ctrl Pts',(36.8505025879075,28.7758079031284,-67.5330928362682));
#164580=CARTESIAN_POINT('Ctrl Pts',(36.8523800154265,28.7667137612429,-67.56963455819));
#164581=CARTESIAN_POINT('Ctrl Pts',(36.8542628670224,28.7575933454673,-67.6062818528199));
#164582=CARTESIAN_POINT('Ctrl Pts',(36.8564376124816,28.7472454102247,-67.6486125967218));
#164583=CARTESIAN_POINT('Ctrl Pts',(36.8589058566037,28.735865441364,-67.6966587851417));
#164584=CARTESIAN_POINT('Ctrl Pts',(36.8613895458258,28.7244142620601,-67.7450056238019));
#164585=CARTESIAN_POINT('Ctrl Pts',(36.8641704189541,28.7119181101614,-67.7991396646537));
#164586=CARTESIAN_POINT('Ctrl Pts',(36.867250395188,28.6986287032735,-67.8590995811083));
#164587=CARTESIAN_POINT('Ctrl Pts',(36.8688433532771,28.6917554462763,-67.8901107405077));
#164588=CARTESIAN_POINT('Ctrl Pts',(36.870516324212,28.6846708525742,-67.9226803849028));
#164589=CARTESIAN_POINT('Ctrl Pts',(36.8722696020682,28.6774151685508,-67.9568144872987));
#164590=CARTESIAN_POINT('Ctrl Pts',(36.8757493427449,28.6630147706079,-68.02456063726));
#164591=CARTESIAN_POINT('Ctrl Pts',(36.8795451946842,28.6479379180227,-68.0984658218493));
#164592=CARTESIAN_POINT('Ctrl Pts',(36.8836579616209,28.6325466976036,-68.178548971691));
#164593=CARTESIAN_POINT('Ctrl Pts',(36.8875264392335,28.618069681877,-68.2538753583012));
#164594=CARTESIAN_POINT('Ctrl Pts',(36.8916753646144,28.6033149445469,-68.3346688134664));
#164595=CARTESIAN_POINT('Ctrl Pts',(36.8961054173322,28.5886254921191,-68.4209460266021));
#164596=CARTESIAN_POINT('Ctrl Pts',(36.9008326532897,28.5729506204786,-68.5130110132352));
#164597=CARTESIAN_POINT('Ctrl Pts',(36.9058797909972,28.5573508491198,-68.6113160918283));
#164598=CARTESIAN_POINT('Ctrl Pts',(36.9112460479487,28.5422930359456,-68.7158512369764));
#164599=CARTESIAN_POINT('Ctrl Pts',(36.9139116353246,28.5348133499989,-68.7677771074236));
#164600=CARTESIAN_POINT('Ctrl Pts',(36.9166559335202,28.5274681519236,-68.8212396433565));
#164601=CARTESIAN_POINT('Ctrl Pts',(36.9194786897652,28.5203187159499,-68.8762346670231));
#164602=CARTESIAN_POINT('Ctrl Pts',(36.9201402732601,28.5186430668936,-68.889124125695));
#164603=CARTESIAN_POINT('Ctrl Pts',(36.9208061659157,28.5169781823619,-68.9020977537259));
#164604=CARTESIAN_POINT('Ctrl Pts',(36.9214763635607,28.5153248700445,-68.9151554800575));
#164605=CARTESIAN_POINT('Ctrl Pts',(36.9215588292865,28.5151214351304,-68.9167621924772));
#164606=CARTESIAN_POINT('Ctrl Pts',(36.9216413601916,28.5149181754348,-68.9183701781779));
#164607=CARTESIAN_POINT('Ctrl Pts',(36.9217239562676,28.5147150924694,-68.9199794370191));
#164608=CARTESIAN_POINT('Ctrl Pts',(36.921774586875,28.5145906045473,-68.9209658973506));
#164609=CARTESIAN_POINT('Ctrl Pts',(36.9218252419709,28.5144661830329,-68.9219528360739));
#164610=CARTESIAN_POINT('Ctrl Pts',(36.9218759215533,28.5143418282747,-68.9229402531568));
#164611=CARTESIAN_POINT('Ctrl Pts',(36.9219012452481,28.5142796903922,-68.9234336480827));
#164612=CARTESIAN_POINT('Ctrl Pts',(36.9219268191552,28.5142169699783,-68.9239319183434));
#164613=CARTESIAN_POINT('Ctrl Pts',(36.9219529250405,28.5141529789799,-68.9244405537663));
#164614=CARTESIAN_POINT('Ctrl Pts',(36.9221227453373,28.5137367138275,-68.9277492566648));
#164615=CARTESIAN_POINT('Ctrl Pts',(36.9223099561208,28.5132794300097,-68.9313968042199));
#164616=CARTESIAN_POINT('Ctrl Pts',(36.9224823318152,28.5128599042257,-68.9347553255715));
#164617=CARTESIAN_POINT('Ctrl Pts',(36.9225681829912,28.51265096072,-68.9364280266354));
#164618=CARTESIAN_POINT('Ctrl Pts',(36.9226503541162,28.5124513467347,-68.9380290303443));
#164619=CARTESIAN_POINT('Ctrl Pts',(36.9227248629765,28.5122706024224,-68.9394807467957));
#164620=CARTESIAN_POINT('Ctrl Pts',(36.9227703374086,28.5121602901063,-68.9403667619736));
#164621=CARTESIAN_POINT('Ctrl Pts',(36.9228129576836,28.5120570042161,-68.941197168337));
#164622=CARTESIAN_POINT('Ctrl Pts',(36.9228518183949,28.5119628977735,-68.9419543246753));
#164623=CARTESIAN_POINT('Ctrl Pts',(36.9228692062893,28.5119207906468,-68.9422931078331));
#164624=CARTESIAN_POINT('Ctrl Pts',(36.9228857465798,28.5118807504019,-68.9426153765461));
#164625=CARTESIAN_POINT('Ctrl Pts',(36.9229025306906,28.5118401334067,-68.9429423959565));
#164626=CARTESIAN_POINT('Ctrl Pts',(36.929440276446,28.4960190040928,-69.0703229754156));
#164627=CARTESIAN_POINT('Ctrl Pts',(36.9357346908991,28.4828904264568,-69.1929838435217));
#164628=CARTESIAN_POINT('Ctrl Pts',(36.9417839751952,28.4719638693738,-69.3108866229627));
#164629=CARTESIAN_POINT('Ctrl Pts',(36.9479506457248,28.4608252826823,-69.4310773033385));
#164630=CARTESIAN_POINT('Ctrl Pts',(36.9538625812405,28.4519750415136,-69.5463234505226));
#164631=CARTESIAN_POINT('Ctrl Pts',(36.9595182310889,28.4449475684845,-69.6565910160207));
#164632=CARTESIAN_POINT('Ctrl Pts',(36.9652344171721,28.4378448756717,-69.7680388496438));
#164633=CARTESIAN_POINT('Ctrl Pts',(36.9706888032379,28.4326042890806,-69.8744009702031));
#164634=CARTESIAN_POINT('Ctrl Pts',(36.9758801287652,28.4287986088424,-69.975648698779));
#164635=CARTESIAN_POINT('Ctrl Pts',(36.9811558032791,28.4249310936702,-70.0785415068729));
#164636=CARTESIAN_POINT('Ctrl Pts',(36.9861598004273,28.4225455482904,-70.1761523856826));
#164637=CARTESIAN_POINT('Ctrl Pts',(36.9908911285026,28.4212473708485,-70.2684576807743));
#164638=CARTESIAN_POINT('Ctrl Pts',(36.9940489481048,28.4203809312129,-70.3300647952238));
#164639=CARTESIAN_POINT('Ctrl Pts',(36.9970853114138,28.41999998,-70.3893086183834));
#164640=CARTESIAN_POINT('Ctrl Pts',(37.,28.41999998,-70.4461836365688));
#164641=CARTESIAN_POINT('Ctrl Pts',(28.2935777143944,29.6448500754942,-76.1704746152117));
#164642=CARTESIAN_POINT('Ctrl Pts',(29.3719438459593,28.4199999800001,-77.079545860612));
#164643=CARTESIAN_POINT('Ctrl Pts',(30.800186642726,28.4199999800001,-78.2835659239152));
#164644=CARTESIAN_POINT('Ctrl Pts',(27.0582328538907,29.5957479131388,-77.7235993982802));
#164645=CARTESIAN_POINT('Ctrl Pts',(28.1162846817441,28.4199999800035,-78.6350614606686));
#164646=CARTESIAN_POINT('Ctrl Pts',(29.4908802242649,28.4199999800001,-79.8367023859018));
#164647=CARTESIAN_POINT('Ctrl Pts',(25.7920491676122,29.54547115812,-79.2528873037006));
#164648=CARTESIAN_POINT('Ctrl Pts',(26.8231903788109,28.41999998,-80.171186708314));
#164649=CARTESIAN_POINT('Ctrl Pts',(28.1443442258615,28.41999998,-81.3659786124399));
#164650=CARTESIAN_POINT('Ctrl Pts',(23.1839068120671,29.4434760286189,-82.2366052581402));
#164651=CARTESIAN_POINT('Ctrl Pts',(24.151734271497,28.41999998,-83.168456079353));
#164652=CARTESIAN_POINT('Ctrl Pts',(25.359343066053,28.41999998,-84.349696566808));
#164653=CARTESIAN_POINT('Ctrl Pts',(21.8495491428221,29.3920399293098,-83.6826429630518));
#164654=CARTESIAN_POINT('Ctrl Pts',(22.7816855628193,28.4199999799965,-84.621550748069));
#164655=CARTESIAN_POINT('Ctrl Pts',(23.928985790681,28.41999998,-85.7957524739721));
#164656=CARTESIAN_POINT('Ctrl Pts',(20.4734286051771,29.3409536236015,-85.0667234623348));
#164657=CARTESIAN_POINT('Ctrl Pts',(21.3602588054756,28.41999998,-86.0160960137185));
#164658=CARTESIAN_POINT('Ctrl Pts',(22.4473146057945,28.41999998,-87.1798147710383));
#164659=CARTESIAN_POINT('',(22.5,28.41999998,-87.1305533863517));
#164660=CARTESIAN_POINT('',(28.5,28.41999998,-80.9397703408579));
#164661=CARTESIAN_POINT('Ctrl Pts',(22.5,28.41999998,-87.1305533863517));
#164662=CARTESIAN_POINT('Ctrl Pts',(22.9996306884473,28.4199999800004,-86.6629501694533));
#164663=CARTESIAN_POINT('Ctrl Pts',(23.492564146587,28.4199999800118,-86.1891300413686));
#164664=CARTESIAN_POINT('Ctrl Pts',(23.9796464830061,28.4199999800316,-85.7094996089096));
#164665=CARTESIAN_POINT('Ctrl Pts',(24.4984981224754,28.4199999800526,-85.1985859140089));
#164666=CARTESIAN_POINT('Ctrl Pts',(25.0107103809196,28.4199999800828,-84.6810791338132));
#164667=CARTESIAN_POINT('Ctrl Pts',(25.5172665601395,28.4199999801285,-84.1574232895664));
#164668=CARTESIAN_POINT('Ctrl Pts',(25.9324040800864,28.419999980166,-83.7282720968575));
#164669=CARTESIAN_POINT('Ctrl Pts',(26.3437419377213,28.4199999802138,-83.294989959686));
#164670=CARTESIAN_POINT('Ctrl Pts',(26.7518048403013,28.4199999802818,-82.85780136844));
#164671=CARTESIAN_POINT('Ctrl Pts',(27.3023421757742,28.4199999803735,-82.2679691621747));
#164672=CARTESIAN_POINT('Ctrl Pts',(27.8456527104564,28.4199999804996,-81.6723376117131));
#164673=CARTESIAN_POINT('Ctrl Pts',(28.38269634666,28.4199999807123,-81.0712589143752));
#164674=CARTESIAN_POINT('Ctrl Pts',(28.4218307391359,28.4199999807278,-81.027458284287));
#164675=CARTESIAN_POINT('Ctrl Pts',(28.4609318358966,28.4199999807438,-80.9836287163286));
#164676=CARTESIAN_POINT('Ctrl Pts',(28.5,28.4199999807603,-80.9397703408579));
#164677=CARTESIAN_POINT('',(22.2890532034791,29.4093902975657,-83.1809305852948));
#164678=CARTESIAN_POINT('Ctrl Pts',(22.5,28.41999998,-87.1305533863517));
#164679=CARTESIAN_POINT('Ctrl Pts',(22.4951047682498,28.41999998,-87.0370152632459));
#164680=CARTESIAN_POINT('Ctrl Pts',(22.489969023803,28.4214973912862,-86.9390314876809));
#164681=CARTESIAN_POINT('Ctrl Pts',(22.4845922316981,28.4249676368345,-86.8366329910864));
#164682=CARTESIAN_POINT('Ctrl Pts',(22.4803327151963,28.4277167794254,-86.7555124869833));
#164683=CARTESIAN_POINT('Ctrl Pts',(22.4759218121537,28.4317051628399,-86.6716193602151));
#164684=CARTESIAN_POINT('Ctrl Pts',(22.471359830805,28.4371915964678,-86.5849805610453));
#164685=CARTESIAN_POINT('Ctrl Pts',(22.4673677205461,28.441992678782,-86.5091644599796));
#164686=CARTESIAN_POINT('Ctrl Pts',(22.4632600604673,28.4479411595211,-86.4312485168285));
#164687=CARTESIAN_POINT('Ctrl Pts',(22.4590378193768,28.4552211396799,-86.3512653363311));
#164688=CARTESIAN_POINT('Ctrl Pts',(22.4569266988316,28.4588611297592,-86.3112737460824));
#164689=CARTESIAN_POINT('Ctrl Pts',(22.4547869543608,28.4628341254629,-86.2707657503527));
#164690=CARTESIAN_POINT('Ctrl Pts',(22.4526187803266,28.4671639280558,-86.2297467972352));
#164691=CARTESIAN_POINT('Ctrl Pts',(22.4515346933096,28.4693288293523,-86.2092373206764));
#164692=CARTESIAN_POINT('Ctrl Pts',(22.4504435002051,28.4715829389777,-86.1886001291912));
#164693=CARTESIAN_POINT('Ctrl Pts',(22.4493452313998,28.4739292712921,-86.1678360170587));
#164694=CARTESIAN_POINT('Ctrl Pts',(22.4487960969971,28.4751024374493,-86.1574539609925));
#164695=CARTESIAN_POINT('Ctrl Pts',(22.4482451937128,28.4762986596964,-86.147040175564));
#164696=CARTESIAN_POINT('Ctrl Pts',(22.4476925255692,28.4775183173404,-86.1365947641351));
#164697=CARTESIAN_POINT('Ctrl Pts',(22.4474161914973,28.4781281461624,-86.1313720584206));
#164698=CARTESIAN_POINT('Ctrl Pts',(22.4471394162153,28.4787438338542,-86.1261414462916));
#164699=CARTESIAN_POINT('Ctrl Pts',(22.4468622002481,28.4793654279613,-86.1209029410792));
#164700=CARTESIAN_POINT('Ctrl Pts',(22.4467928962564,28.479520826488,-86.1195933147761));
#164701=CARTESIAN_POINT('Ctrl Pts',(22.4467235647218,28.4796765941662,-86.1182831951567));
#164702=CARTESIAN_POINT('Ctrl Pts',(22.446654205653,28.4798327317393,-86.1169725824328));
#164703=CARTESIAN_POINT('Ctrl Pts',(22.4466281960021,28.4798912833292,-86.1164811026613));
#164704=CARTESIAN_POINT('Ctrl Pts',(22.4466021824793,28.4799498869356,-86.115989553547));
#164705=CARTESIAN_POINT('Ctrl Pts',(22.4465761650848,28.4800085425977,-86.115497935101));
#164706=CARTESIAN_POINT('Ctrl Pts',(22.446559066732,28.4800470904703,-86.1151748487266));
#164707=CARTESIAN_POINT('Ctrl Pts',(22.4465419667071,28.4800856608257,-86.114851732408));
#164708=CARTESIAN_POINT('Ctrl Pts',(22.4465248650102,28.4801242536749,-86.1145285861484));
#164709=CARTESIAN_POINT('Ctrl Pts',(22.4465111475424,28.4801552094431,-86.1142693868174));
#164710=CARTESIAN_POINT('Ctrl Pts',(22.4464975359983,28.4801859375989,-86.1140121899836));
#164711=CARTESIAN_POINT('Ctrl Pts',(22.4464829918517,28.4802187848952,-86.1137373723805));
#164712=CARTESIAN_POINT('Ctrl Pts',(22.446322533286,28.4805811732965,-86.1107054421114));
#164713=CARTESIAN_POINT('Ctrl Pts',(22.4460801860419,28.4811319103387,-86.1061264923159));
#164714=CARTESIAN_POINT('Ctrl Pts',(22.4460292308326,28.4812479771557,-86.1051637598205));
#164715=CARTESIAN_POINT('Ctrl Pts',(22.4449780310017,28.4836424216106,-86.0853027043907));
#164716=CARTESIAN_POINT('Ctrl Pts',(22.4436696588496,28.4866890992066,-86.0605885877759));
#164717=CARTESIAN_POINT('Ctrl Pts',(22.442103617021,28.490518899134,-86.0310232998984));
#164718=CARTESIAN_POINT('Ctrl Pts',(22.44054125975,28.4943396883708,-86.0015275727468));
#164719=CARTESIAN_POINT('Ctrl Pts',(22.4387224427457,28.4989399023362,-85.9672034699557));
#164720=CARTESIAN_POINT('Ctrl Pts',(22.4366469102226,28.5045005891629,-85.928061544957));
#164721=CARTESIAN_POINT('Ctrl Pts',(22.4345758991035,28.5100491624183,-85.889004887933));
#164722=CARTESIAN_POINT('Ctrl Pts',(22.4322492882742,28.5165540132362,-85.8451513709574));
#164723=CARTESIAN_POINT('Ctrl Pts',(22.4296670800832,28.5242461697488,-85.7965202067969));
#164724=CARTESIAN_POINT('Ctrl Pts',(22.4270880170419,28.5319289571546,-85.7479482757746));
#164725=CARTESIAN_POINT('Ctrl Pts',(22.4242538570598,28.540796561228,-85.6946080669459));
#164726=CARTESIAN_POINT('Ctrl Pts',(22.4211653956423,28.5511287615564,-85.6365371663577));
#164727=CARTESIAN_POINT('Ctrl Pts',(22.4181315437853,28.5612782699737,-85.5794930638834));
#164728=CARTESIAN_POINT('Ctrl Pts',(22.4148523490072,28.5728410679315,-85.517884975594));
#164729=CARTESIAN_POINT('Ctrl Pts',(22.4113291382384,28.5861288281457,-85.4517621039892));
#164730=CARTESIAN_POINT('Ctrl Pts',(22.4077443244978,28.5996489234573,-85.3844830808907));
#164731=CARTESIAN_POINT('Ctrl Pts',(22.4039069812495,28.6149545647562,-85.3125318340768));
#164732=CARTESIAN_POINT('Ctrl Pts',(22.3998201352734,28.6324173313141,-85.2359930321443));
#164733=CARTESIAN_POINT('Ctrl Pts',(22.3979169863125,28.6405493348751,-85.2003506951866));
#164734=CARTESIAN_POINT('Ctrl Pts',(22.3959597547803,28.6491497204908,-85.1637139891818));
#164735=CARTESIAN_POINT('Ctrl Pts',(22.393948882839,28.6582589314929,-85.1260941361953));
#164736=CARTESIAN_POINT('Ctrl Pts',(22.3935500158385,28.6600657912909,-85.1186320409653));
#164737=CARTESIAN_POINT('Ctrl Pts',(22.3930644920505,28.6622797595882,-85.1095498956867));
#164738=CARTESIAN_POINT('Ctrl Pts',(22.392720765649,28.6638553527948,-85.1031208045394));
#164739=CARTESIAN_POINT('Ctrl Pts',(22.3926828656075,28.6640290812243,-85.1024119185758));
#164740=CARTESIAN_POINT('Ctrl Pts',(22.3926466889428,28.6641950072837,-85.1017352740096));
#164741=CARTESIAN_POINT('Ctrl Pts',(22.3926125418634,28.6643516992126,-85.101096595959));
#164742=CARTESIAN_POINT('Ctrl Pts',(22.3877821780164,28.6865169631871,-85.0107507327198));
#164743=CARTESIAN_POINT('Ctrl Pts',(22.3831370999249,28.7092875749723,-84.9245013585229));
#164744=CARTESIAN_POINT('Ctrl Pts',(22.3787041414205,28.7322906723717,-84.8423472438193));
#164745=CARTESIAN_POINT('Ctrl Pts',(22.3740953037289,28.7562064257484,-84.7569336357291));
#164746=CARTESIAN_POINT('Ctrl Pts',(22.3697157117241,28.7803731382638,-84.6759461611083));
#164747=CARTESIAN_POINT('Ctrl Pts',(22.365590291958,28.8044073200015,-84.5993406230004));
#164748=CARTESIAN_POINT('Ctrl Pts',(22.3646452728677,28.8099128835203,-84.5817924218366));
#164749=CARTESIAN_POINT('Ctrl Pts',(22.3637135718636,28.8154116467859,-84.5644740070615));
#164750=CARTESIAN_POINT('Ctrl Pts',(22.3627954557692,28.820899277231,-84.5473845938951));
#164751=CARTESIAN_POINT('Ctrl Pts',(22.3586289219162,28.8458028794692,-84.4698305471638));
#164752=CARTESIAN_POINT('Ctrl Pts',(22.3547334364831,28.8704744451308,-84.397000610347));
#164753=CARTESIAN_POINT('Ctrl Pts',(22.3510910329502,28.8945421918395,-84.3288273774177));
#164754=CARTESIAN_POINT('Ctrl Pts',(22.3508951884565,28.8958362647298,-84.3251618438866));
#164755=CARTESIAN_POINT('Ctrl Pts',(22.3507000755983,28.8971286029019,-84.3215097668994));
#164756=CARTESIAN_POINT('Ctrl Pts',(22.3505056915785,28.8984191522915,-84.3178711340653));
#164757=CARTESIAN_POINT('Ctrl Pts',(22.3486008790756,28.9110655345192,-84.2822153567841));
#164758=CARTESIAN_POINT('Ctrl Pts',(22.3467655974202,28.9235399337527,-84.2478508654111));
#164759=CARTESIAN_POINT('Ctrl Pts',(22.3449949120567,28.9357938806202,-84.2147662769381));
#164760=CARTESIAN_POINT('Ctrl Pts',(22.344109569375,28.941920854054,-84.1982239827016));
#164761=CARTESIAN_POINT('Ctrl Pts',(22.3432403894245,28.9479927535013,-84.1820016780921));
#164762=CARTESIAN_POINT('Ctrl Pts',(22.3423866078272,28.9540039023431,-84.1660978565589));
#164763=CARTESIAN_POINT('Ctrl Pts',(22.3419597170285,28.957009476764,-84.1581459457924));
#164764=CARTESIAN_POINT('Ctrl Pts',(22.3415366767081,28.9599998661409,-84.1502736567013));
#164765=CARTESIAN_POINT('Ctrl Pts',(22.3411173918452,28.9629743794316,-84.14248080323));
#164766=CARTESIAN_POINT('Ctrl Pts',(22.3409077494137,28.964461636077,-84.1385843764944));
#164767=CARTESIAN_POINT('Ctrl Pts',(22.3406990459045,28.9659449238627,-84.1347078087226));
#164768=CARTESIAN_POINT('Ctrl Pts',(22.3404912690254,28.9674241578559,-84.1308510764665));
#164769=CARTESIAN_POINT('Ctrl Pts',(22.3402834921463,28.968903391849,-84.1269943442105));
#164770=CARTESIAN_POINT('Ctrl Pts',(22.3401740841416,28.9696825228617,-84.124963567216));
#164771=CARTESIAN_POINT('Ctrl Pts',(22.3398707060041,28.9718496143136,-84.1193403628843));
#164772=CARTESIAN_POINT('Ctrl Pts',(22.3341418138434,29.0127722507775,-84.0131536366896));
#164773=CARTESIAN_POINT('Ctrl Pts',(22.3286290027088,29.0547685352277,-83.9110986363527));
#164774=CARTESIAN_POINT('Ctrl Pts',(22.3233329971592,29.09743018428,-83.8131653118839));
#164775=CARTESIAN_POINT('Ctrl Pts',(22.3178665094664,29.1414651418176,-83.7120794448276));
#164776=CARTESIAN_POINT('Ctrl Pts',(22.3126309837291,29.186208771893,-83.6153844056887));
#164777=CARTESIAN_POINT('Ctrl Pts',(22.3076242361681,29.2312362706003,-83.5230179678608));
#164778=CARTESIAN_POINT('Ctrl Pts',(22.302380749841,29.2783928469877,-83.426284080656));
#164779=CARTESIAN_POINT('Ctrl Pts',(22.2973881622895,29.3258604388178,-83.334297338755));
#164780=CARTESIAN_POINT('Ctrl Pts',(22.2926411499906,29.3731816212461,-83.2469383796063));
#164781=CARTESIAN_POINT('Ctrl Pts',(22.2914299907881,29.3852552123732,-83.2246494954339));
#164782=CARTESIAN_POINT('Ctrl Pts',(22.2902348052996,29.3973194356256,-83.2026616552453));
#164783=CARTESIAN_POINT('Ctrl Pts',(22.2890554809091,29.4093670318967,-83.1809724699472));
#164784=CARTESIAN_POINT('',(28.2496026321977,29.6431021634044,-76.2257352260018));
#164785=CARTESIAN_POINT('Ctrl Pts',(28.2496026843433,29.6431021904052,-76.2257353081032));
#164786=CARTESIAN_POINT('Ctrl Pts',(27.8439324295553,29.6269781482949,-76.7352715965501));
#164787=CARTESIAN_POINT('Ctrl Pts',(27.4405910184951,29.6109534525765,-77.2351086235097));
#164788=CARTESIAN_POINT('Ctrl Pts',(27.0393215418638,29.5950412497677,-77.7253786106869));
#164789=CARTESIAN_POINT('Ctrl Pts',(26.6071317885992,29.577902914045,-78.2534269102236));
#164790=CARTESIAN_POINT('Ctrl Pts',(26.1773458282904,29.5608950892855,-78.7703771082137));
#164791=CARTESIAN_POINT('Ctrl Pts',(25.7496553125592,29.544029978792,-79.2764572215566));
#164792=CARTESIAN_POINT('Ctrl Pts',(25.3271476948443,29.5273692453994,-79.7764044852826));
#164793=CARTESIAN_POINT('Ctrl Pts',(24.906685430099,29.5108477454557,-80.2657444716429));
#164794=CARTESIAN_POINT('Ctrl Pts',(24.4879779898396,29.4944735933695,-80.7447462809204));
#164795=CARTESIAN_POINT('Ctrl Pts',(24.0419205535757,29.4770298806519,-81.2550365181317));
#164796=CARTESIAN_POINT('Ctrl Pts',(23.5987412348824,29.4597865708662,-81.7526119366807));
#164797=CARTESIAN_POINT('Ctrl Pts',(23.1578556033775,29.4427591879028,-82.2378302632723));
#164798=CARTESIAN_POINT('Ctrl Pts',(22.8673437674819,29.4315393704905,-82.5575541480974));
#164799=CARTESIAN_POINT('Ctrl Pts',(22.5778286446949,29.4204131853293,-82.8719138375261));
#164800=CARTESIAN_POINT('Ctrl Pts',(22.2891503923498,29.4093838642276,-83.1810211213626));
#164801=CARTESIAN_POINT('Ctrl Pts',(28.2496025526968,29.6431021742755,-76.2257352367271));
#164802=CARTESIAN_POINT('Ctrl Pts',(28.255183736006,29.5810914147569,-76.3299584484354));
#164803=CARTESIAN_POINT('Ctrl Pts',(28.2610740674642,29.5190700705727,-76.4400011095444));
#164804=CARTESIAN_POINT('Ctrl Pts',(28.2672804894903,29.4576860819767,-76.5560107358913));
#164805=CARTESIAN_POINT('Ctrl Pts',(28.2704089728608,29.4267441339864,-76.6144879366551));
#164806=CARTESIAN_POINT('Ctrl Pts',(28.2736177556735,29.3959634873014,-76.6744810429466));
#164807=CARTESIAN_POINT('Ctrl Pts',(28.2769076118698,29.3654221838543,-76.7360071763375));
#164808=CARTESIAN_POINT('Ctrl Pts',(28.2821860203022,29.3164202019934,-76.8347227559663));
#164809=CARTESIAN_POINT('Ctrl Pts',(28.2876727741999,29.2680404155082,-76.9373783773371));
#164810=CARTESIAN_POINT('Ctrl Pts',(28.2933680075836,29.2205986057973,-77.0439895897435));
#164811=CARTESIAN_POINT('Ctrl Pts',(28.2979333863715,29.1825685871616,-77.1294506296846));
#164812=CARTESIAN_POINT('Ctrl Pts',(28.3026326762123,29.1451412031537,-77.2174524831978));
#164813=CARTESIAN_POINT('Ctrl Pts',(28.3074648801551,29.108462887641,-77.3079840345561));
#164814=CARTESIAN_POINT('Ctrl Pts',(28.3078152123237,29.1058037296322,-77.3145475229955));
#164815=CARTESIAN_POINT('Ctrl Pts',(28.3082600170683,29.1024416508876,-77.3228812792815));
#164816=CARTESIAN_POINT('Ctrl Pts',(28.3085180026056,29.1004972415241,-77.3277143555029));
#164817=CARTESIAN_POINT('Ctrl Pts',(28.3086435314212,29.0995511442857,-77.33006600025));
#164818=CARTESIAN_POINT('Ctrl Pts',(28.3087692964991,29.0986044393851,-77.3324221074881));
#164819=CARTESIAN_POINT('Ctrl Pts',(28.3088952979202,29.0976571367595,-77.3347826788554));
#164820=CARTESIAN_POINT('Ctrl Pts',(28.3142335624862,29.0575230494133,-77.4347923007826));
#164821=CARTESIAN_POINT('Ctrl Pts',(28.3199963653331,29.0163232038439,-77.5428200375934));
#164822=CARTESIAN_POINT('Ctrl Pts',(28.3261919085518,28.9749251754602,-77.6590324417008));
#164823=CARTESIAN_POINT('Ctrl Pts',(28.3294675063405,28.9530379437128,-77.7204742040247));
#164824=CARTESIAN_POINT('Ctrl Pts',(28.3328640791694,28.931096280647,-77.7842041423692));
#164825=CARTESIAN_POINT('Ctrl Pts',(28.3363829000878,28.9092337070165,-77.8502488180608));
#164826=CARTESIAN_POINT('Ctrl Pts',(28.3420752382563,28.8738669846907,-77.9570881932308));
#164827=CARTESIAN_POINT('Ctrl Pts',(28.3480866891023,28.8387109592594,-78.0699758528063));
#164828=CARTESIAN_POINT('Ctrl Pts',(28.3544180938211,28.804361897349,-78.1889520040999));
#164829=CARTESIAN_POINT('Ctrl Pts',(28.3593985277568,28.7773421061341,-78.282541481911));
#164830=CARTESIAN_POINT('Ctrl Pts',(28.3645768739889,28.7508225548804,-78.3798971860222));
#164831=CARTESIAN_POINT('Ctrl Pts',(28.3699520794374,28.7250966301013,-78.4810129983013));
#164832=CARTESIAN_POINT('Ctrl Pts',(28.3701458646069,28.7241691673761,-78.4846583928838));
#164833=CARTESIAN_POINT('Ctrl Pts',(28.3704257902458,28.7228336879588,-78.4899243609925));
#164834=CARTESIAN_POINT('Ctrl Pts',(28.3705342074466,28.722317348061,-78.4919638340097));
#164835=CARTESIAN_POINT('Ctrl Pts',(28.3706986208292,28.7215343248089,-78.4950566703395));
#164836=CARTESIAN_POINT('Ctrl Pts',(28.3708651149875,28.7207430073931,-78.4981887192797));
#164837=CARTESIAN_POINT('Ctrl Pts',(28.3710336910261,28.7199435124741,-78.5013600047023));
#164838=CARTESIAN_POINT('Ctrl Pts',(28.373006883928,28.7105853752683,-78.538480095648));
#164839=CARTESIAN_POINT('Ctrl Pts',(28.3752653039959,28.7001058776199,-78.5809756952539));
#164840=CARTESIAN_POINT('Ctrl Pts',(28.3778104891178,28.688725450316,-78.6288819284805));
#164841=CARTESIAN_POINT('Ctrl Pts',(28.3796362123637,28.6805619927754,-78.663246235763));
#164842=CARTESIAN_POINT('Ctrl Pts',(28.3816094990746,28.6719360567712,-78.7003947879149));
#164843=CARTESIAN_POINT('Ctrl Pts',(28.383730846252,28.6629455066605,-78.7403399456306));
#164844=CARTESIAN_POINT('Ctrl Pts',(28.3869252065252,28.6494073850304,-78.8004900362284));
#164845=CARTESIAN_POINT('Ctrl Pts',(28.3904835574881,28.6349272591564,-78.867509044862));
#164846=CARTESIAN_POINT('Ctrl Pts',(28.3943564253042,28.620103437781,-78.9404874769925));
#164847=CARTESIAN_POINT('Ctrl Pts',(28.3969472734419,28.6101866856927,-78.9893081556088));
#164848=CARTESIAN_POINT('Ctrl Pts',(28.3996788336818,28.6001162870024,-79.040795056823));
#164849=CARTESIAN_POINT('Ctrl Pts',(28.4025356366335,28.5900659246857,-79.0946635154937));
#164850=CARTESIAN_POINT('Ctrl Pts',(28.4063205663074,28.5767503704769,-79.1660329207915));
#164851=CARTESIAN_POINT('Ctrl Pts',(28.4098729825914,28.5650881944288,-79.2328695271597));
#164852=CARTESIAN_POINT('Ctrl Pts',(28.4131801735685,28.5547889850124,-79.2951206573735));
#164853=CARTESIAN_POINT('Ctrl Pts',(28.416100601828,28.545694226821,-79.3500917676345));
#164854=CARTESIAN_POINT('Ctrl Pts',(28.4188298586093,28.537662889555,-79.4014880882629));
#164855=CARTESIAN_POINT('Ctrl Pts',(28.4213603911671,28.5305215651011,-79.4492940109026));
#164856=CARTESIAN_POINT('Ctrl Pts',(28.4240584874455,28.522907365129,-79.5002654878583));
#164857=CARTESIAN_POINT('Ctrl Pts',(28.4265337063652,28.5163045723416,-79.5471525710561));
#164858=CARTESIAN_POINT('Ctrl Pts',(28.42879051022,28.5105339014271,-79.5899402886357));
#164859=CARTESIAN_POINT('Ctrl Pts',(28.4299189121475,28.5076485659698,-79.6113341474255));
#164860=CARTESIAN_POINT('Ctrl Pts',(28.4309928115677,28.5049717606348,-79.6317033009445));
#164861=CARTESIAN_POINT('Ctrl Pts',(28.4320132245346,28.5024840629928,-79.6510465723521));
#164862=CARTESIAN_POINT('Ctrl Pts',(28.4325234310181,28.5012402141718,-79.6607182080559));
#164863=CARTESIAN_POINT('Ctrl Pts',(28.4330202701749,28.5000436735233,-79.6701333769929));
#164864=CARTESIAN_POINT('Ctrl Pts',(28.4335038854641,28.4988921989618,-79.6792919688879));
#164865=CARTESIAN_POINT('Ctrl Pts',(28.4337456931087,28.4983164616811,-79.6838712648354));
#164866=CARTESIAN_POINT('Ctrl Pts',(28.4339841950586,28.4977519928503,-79.688386416761));
#164867=CARTESIAN_POINT('Ctrl Pts',(28.4342194100622,28.4971985238549,-79.69283741224));
#164868=CARTESIAN_POINT('Ctrl Pts',(28.434337017564,28.4969217893572,-79.6950629099794));
#164869=CARTESIAN_POINT('Ctrl Pts',(28.4344538033452,28.4966478049383,-79.6972723686213));
#164870=CARTESIAN_POINT('Ctrl Pts',(28.4345697697949,28.4963765377427,-79.6994657867326));
#164871=CARTESIAN_POINT('Ctrl Pts',(28.4346857362446,28.4961052705471,-79.7016592048439));
#164872=CARTESIAN_POINT('Ctrl Pts',(28.4347179301366,28.496029621214,-79.7022684074304));
#164873=CARTESIAN_POINT('Ctrl Pts',(28.4349152167509,28.495570855037,-79.7059979180573));
#164874=CARTESIAN_POINT('Ctrl Pts',(28.4350220546971,28.4953224163059,-79.7080175850115));
#164875=CARTESIAN_POINT('Ctrl Pts',(28.4351288270614,28.4950747520133,-79.7100360387155));
#164876=CARTESIAN_POINT('Ctrl Pts',(28.4352355337918,28.4948278599047,-79.7120532781116));
#164877=CARTESIAN_POINT('Ctrl Pts',(28.4424961980171,28.4780285381237,-79.8493126418011));
#164878=CARTESIAN_POINT('Ctrl Pts',(28.4494650758024,28.4647367196518,-79.9811770740478));
#164879=CARTESIAN_POINT('Ctrl Pts',(28.456139456048,28.4542917122619,-80.1075719763809));
#164880=CARTESIAN_POINT('Ctrl Pts',(28.4627813333619,28.4438975700234,-80.2333513601604));
#164881=CARTESIAN_POINT('Ctrl Pts',(28.4691315766389,28.4363225305539,-80.3537143519523));
#164882=CARTESIAN_POINT('Ctrl Pts',(28.475187812645,28.4309666690402,-80.4685926700759));
#164883=CARTESIAN_POINT('Ctrl Pts',(28.4812043109995,28.4256459497102,-80.5827172205828));
#164884=CARTESIAN_POINT('Ctrl Pts',(28.4869306496675,28.4225153561887,-80.6914288347818));
#164885=CARTESIAN_POINT('Ctrl Pts',(28.4923647656175,28.4210378446978,-80.7946657755264));
#164886=CARTESIAN_POINT('Ctrl Pts',(28.4949774611128,28.4203274646375,-80.8443015750761));
#164887=CARTESIAN_POINT('Ctrl Pts',(28.4975226090316,28.41999998,-80.8926719059585));
#164888=CARTESIAN_POINT('Ctrl Pts',(28.5,28.41999998,-80.9397703408579));
#164889=CARTESIAN_POINT('Origin',(-3.54807775957937E-14,-73.08000002,3.11172719585489E-30));
#164890=CARTESIAN_POINT('',(24.7,-73.08000002,-58.24995));
#164891=CARTESIAN_POINT('',(24.2,-73.08000002,-58.24995));
#164892=CARTESIAN_POINT('',(-41.5,-73.0800000199999,-58.24995));
#164893=CARTESIAN_POINT('',(24.2,-73.08000002,-174.34995));
#164894=CARTESIAN_POINT('',(24.7,-73.08000002,-58.24995));
#164895=CARTESIAN_POINT('Origin',(0.,-12.9675000200281,-179.64995));
#164896=CARTESIAN_POINT('',(41.0540572871253,28.7076050220164,-61.14995));
#164897=CARTESIAN_POINT('',(41.0540572871253,28.7076050220164,-93.3976987687948));
#164898=CARTESIAN_POINT('',(41.0540572871253,28.7076050220164,-179.64995));
#164899=CARTESIAN_POINT('',(39.3277310924369,30.3404619167909,-92.0491293459315));
#164900=CARTESIAN_POINT('Ctrl Pts',(41.0540572871253,28.7076050220164,-93.3976987687948));
#164901=CARTESIAN_POINT('Ctrl Pts',(41.0005485183022,28.7603163963106,-93.3173972926641));
#164902=CARTESIAN_POINT('Ctrl Pts',(40.944160634441,28.8156580071379,-93.239741406992));
#164903=CARTESIAN_POINT('Ctrl Pts',(40.8848550499675,28.8736049764068,-93.1647596830525));
#164904=CARTESIAN_POINT('Ctrl Pts',(40.825549465494,28.9315519456757,-93.089777959113));
#164905=CARTESIAN_POINT('Ctrl Pts',(40.7633261602461,28.992104346973,-93.0174706190487));
#164906=CARTESIAN_POINT('Ctrl Pts',(40.6981582073462,29.0552176990714,-92.9478087613683));
#164907=CARTESIAN_POINT('Ctrl Pts',(40.6329902544463,29.1183310511698,-92.8781469036879));
#164908=CARTESIAN_POINT('Ctrl Pts',(40.5648738243989,29.1840092134169,-92.8111449499777));
#164909=CARTESIAN_POINT('Ctrl Pts',(40.4937697303936,29.252209946825,-92.7468029017649));
#164910=CARTESIAN_POINT('Ctrl Pts',(40.4582176833909,29.2863103135291,-92.7146318776585));
#164911=CARTESIAN_POINT('Ctrl Pts',(40.4219186395222,29.3210412388419,-92.6831258300065));
#164912=CARTESIAN_POINT('Ctrl Pts',(40.3848672142056,29.3563968380406,-92.6522847588729));
#164913=CARTESIAN_POINT('Ctrl Pts',(40.3663415015473,29.3740746376399,-92.636864223306));
#164914=CARTESIAN_POINT('Ctrl Pts',(40.3476276875811,29.3919085994207,-92.6216099318634));
#164915=CARTESIAN_POINT('Ctrl Pts',(40.3287250640418,29.4098979464083,-92.6065218845213));
#164916=CARTESIAN_POINT('Ctrl Pts',(40.3174895957419,29.4205905752593,-92.5975537496341));
#164917=CARTESIAN_POINT('Ctrl Pts',(40.3057313639822,29.4317717047969,-92.5882858994004));
#164918=CARTESIAN_POINT('Ctrl Pts',(40.2942617097069,29.4426692733808,-92.5793606574514));
#164919=CARTESIAN_POINT('Ctrl Pts',(40.2864347444641,29.4501058436985,-92.573270015411));
#164920=CARTESIAN_POINT('Ctrl Pts',(40.2787427202192,29.4574099458675,-92.5673379096353));
#164921=CARTESIAN_POINT('Ctrl Pts',(40.2714498226746,29.4643315355271,-92.5617569979654));
#164922=CARTESIAN_POINT('Ctrl Pts',(40.2711504835721,29.4646156341893,-92.5615279278215));
#164923=CARTESIAN_POINT('Ctrl Pts',(40.270851117812,29.4648997520497,-92.5612989110134));
#164924=CARTESIAN_POINT('Ctrl Pts',(40.2705517253855,29.4651838891131,-92.5610699475012));
#164925=CARTESIAN_POINT('Ctrl Pts',(40.2116149290431,29.5211175960337,-92.5159974116276));
#164926=CARTESIAN_POINT('Ctrl Pts',(40.1515495404995,29.5778784346942,-92.4730805866532));
#164927=CARTESIAN_POINT('Ctrl Pts',(40.0903677987547,29.6354412520569,-92.4322300633291));
#164928=CARTESIAN_POINT('Ctrl Pts',(40.0278547511154,29.6942566280402,-92.3904906384971));
#164929=CARTESIAN_POINT('Ctrl Pts',(39.9641756860206,29.7539098610732,-92.3509081401424));
#164930=CARTESIAN_POINT('Ctrl Pts',(39.8993230643698,29.8143876478948,-92.3134354060481));
#164931=CARTESIAN_POINT('Ctrl Pts',(39.83468856135,29.8746620299545,-92.2760887038898));
#164932=CARTESIAN_POINT('Ctrl Pts',(39.7688877366747,29.9357560969925,-92.2408374710607));
#164933=CARTESIAN_POINT('Ctrl Pts',(39.7019020445249,29.9976603583428,-92.2076851487087));
#164934=CARTESIAN_POINT('Ctrl Pts',(39.6368741274445,30.0577553584066,-92.1755017614847));
#164935=CARTESIAN_POINT('Ctrl Pts',(39.5707289868318,30.1186144848593,-92.1452964437428));
#164936=CARTESIAN_POINT('Ctrl Pts',(39.5034483725263,30.1802232711375,-92.1171198578927));
#164937=CARTESIAN_POINT('Ctrl Pts',(39.4457147020241,30.2330899312259,-92.0929414561326));
#164938=CARTESIAN_POINT('Ctrl Pts',(39.3871446932213,30.2865087402759,-92.070257565583));
#164939=CARTESIAN_POINT('Ctrl Pts',(39.3277310924369,30.3404619167909,-92.0491293459315));
#164940=CARTESIAN_POINT('',(39.3277310924369,30.3404619167909,-61.14995));
#164941=CARTESIAN_POINT('',(39.3277310924369,30.340461916791,-179.64995));
#164942=CARTESIAN_POINT('Origin',(0.,-12.9675000200281,-61.14995));
#164943=CARTESIAN_POINT('Origin',(0.,-12.9675000200281,-60.64995));
#164944=CARTESIAN_POINT('',(42.,-56.3473237326805,-60.64995));
#164945=CARTESIAN_POINT('',(43.1572831724516,-55.08000002,-60.64995));
#164946=CARTESIAN_POINT('Origin',(44.5079524583206,-57.4754524783489,-60.64995));
#164947=CARTESIAN_POINT('',(42.,-12.9675000200281,-60.64995));
#164948=CARTESIAN_POINT('',(-1.8445455022812E-14,-55.08000002,-60.64995));
#164949=CARTESIAN_POINT('Origin',(57.,-45.43000002,-174.34995));
#164950=CARTESIAN_POINT('',(57.,-44.93000002,-176.84995));
#164951=CARTESIAN_POINT('Origin',(57.,-45.43000002,-176.84995));
#164952=CARTESIAN_POINT('',(59.5,-44.93000002,-174.34995));
#164953=CARTESIAN_POINT('Origin',(57.,-44.93000002,-174.34995));
#164954=CARTESIAN_POINT('Origin',(59.5,-45.43000002,-174.34995));
#164955=CARTESIAN_POINT('Origin',(59.5,-45.43000002,-55.2499500000007));
#164956=CARTESIAN_POINT('',(59.5,-44.93000002,-58.24995));
#164957=CARTESIAN_POINT('',(59.5,-44.93000002,-174.34995));
#164958=CARTESIAN_POINT('Origin',(59.5,-45.43000002,-58.24995));
#164959=CARTESIAN_POINT('Ctrl Pts',(40.7712064624936,-44.93000002,-76.6047958451324));
#164960=CARTESIAN_POINT('Ctrl Pts',(39.9673804148565,-44.93000002,-76.1313366308109));
#164961=CARTESIAN_POINT('Ctrl Pts',(40.4124516249929,-44.1531545436406,
-76.3934867142621));
#164962=CARTESIAN_POINT('Ctrl Pts',(43.7236852143189,-44.93000002,-71.5921585277583));
#164963=CARTESIAN_POINT('Ctrl Pts',(42.8619820924489,-44.9300000200589,
-71.2817568775718));
#164964=CARTESIAN_POINT('Ctrl Pts',(43.3552388512871,-44.1657199195518,
-71.3808409460202));
#164965=CARTESIAN_POINT('Ctrl Pts',(46.5890843541627,-44.93000002,-66.5297716146547));
#164966=CARTESIAN_POINT('Ctrl Pts',(45.7723278216974,-44.9300000200823,
-66.2016926213901));
#164967=CARTESIAN_POINT('Ctrl Pts',(46.2131449010667,-44.1767154324357,
-66.3184583453296));
#164968=CARTESIAN_POINT('Ctrl Pts',(49.4036629110189,-44.93000002,-61.4386408691297));
#164969=CARTESIAN_POINT('Ctrl Pts',(48.6588221091936,-44.93000002,-61.026863396898));
#164970=CARTESIAN_POINT('Ctrl Pts',(49.0214378669496,-44.1865817238571,
-61.2273317382593));
#164971=CARTESIAN_POINT('',(40.7712064624936,-44.93000002,-76.6047958451324));
#164972=CARTESIAN_POINT('Origin',(40.7712064624936,-44.43000002,-76.6047958451324));
#164973=CARTESIAN_POINT('',(49.0214378669496,-44.1865817238571,-61.2273317382593));
#164974=CARTESIAN_POINT('Ctrl Pts',(49.0214378669496,-44.1865817238571,
-61.2273317382593));
#164975=CARTESIAN_POINT('Ctrl Pts',(48.4420648309483,-44.1845462299615,
-62.2776713982629));
#164976=CARTESIAN_POINT('Ctrl Pts',(47.868763221355,-44.1824913928638,-63.3119433794598));
#164977=CARTESIAN_POINT('Ctrl Pts',(47.3014167078854,-44.180417648187,-64.3300966156723));
#164978=CARTESIAN_POINT('Ctrl Pts',(46.7009617895993,-44.1782228868536,
-65.4076657973598));
#164979=CARTESIAN_POINT('Ctrl Pts',(46.1071770969554,-44.1760069450256,
-66.4671799588015));
#164980=CARTESIAN_POINT('Ctrl Pts',(45.5199776965721,-44.1737709346618,
-67.5086101966259));
#164981=CARTESIAN_POINT('Ctrl Pts',(44.9377500540171,-44.1715538563711,
-68.5412227501437));
#164982=CARTESIAN_POINT('Ctrl Pts',(44.3619970347197,-44.1693170524919,
-69.5560565352758));
#164983=CARTESIAN_POINT('Ctrl Pts',(43.7926841712506,-44.1670621447943,
-70.5531122444581));
#164984=CARTESIAN_POINT('Ctrl Pts',(43.2048774090488,-44.1647339873297,
-71.5825569061823));
#164985=CARTESIAN_POINT('Ctrl Pts',(42.623936078368,-44.1623865319684,-72.5930497443139));
#164986=CARTESIAN_POINT('Ctrl Pts',(42.0498710589263,-44.160022100411,-73.5846206914654));
#164987=CARTESIAN_POINT('Ctrl Pts',(41.4976856632468,-44.1577477856019,
-74.5383994051199));
#164988=CARTESIAN_POINT('Ctrl Pts',(40.9518629506906,-44.1554577703291,
-75.4746714241381));
#164989=CARTESIAN_POINT('Ctrl Pts',(40.4124516249929,-44.1531545436406,
-76.3934867142621));
#164990=CARTESIAN_POINT('',(49.4036629110189,-44.93000002,-61.4386408691297));
#164991=CARTESIAN_POINT('Origin',(49.4036629110189,-44.43000002,-61.4386408691297));
#164992=CARTESIAN_POINT('Ctrl Pts',(40.7712064624936,-44.93000002,-76.6047958451324));
#164993=CARTESIAN_POINT('Ctrl Pts',(43.723712605206,-44.93000002,-71.5921120242627));
#164994=CARTESIAN_POINT('Ctrl Pts',(46.5890589653218,-44.93000002,-66.5298175388285));
#164995=CARTESIAN_POINT('Ctrl Pts',(49.4036629110189,-44.93000002,-61.4386408691297));
#164996=CARTESIAN_POINT('Ctrl Pts',(40.4124516249929,-44.1531545436406,
-76.3934867142621));
#164997=CARTESIAN_POINT('Ctrl Pts',(39.9673804148565,-44.93000002,-76.1313366308109));
#164998=CARTESIAN_POINT('Ctrl Pts',(40.7712064624936,-44.93000002,-76.6047958451324));
#164999=CARTESIAN_POINT('Ctrl Pts',(40.1609837329219,-44.174100053011,-76.7929803513312));
#165000=CARTESIAN_POINT('Ctrl Pts',(39.7695444931039,-44.93000002,-76.5732367689873));
#165001=CARTESIAN_POINT('Ctrl Pts',(40.5448762480367,-44.93000002,-76.9890530774658));
#165002=CARTESIAN_POINT('Ctrl Pts',(39.9523146669981,-44.1958519161918,
-77.2080863135005));
#165003=CARTESIAN_POINT('Ctrl Pts',(39.6033636235116,-44.93000002,-77.035174184732));
#165004=CARTESIAN_POINT('Ctrl Pts',(40.3570832012011,-44.93000002,-77.3881516643461));
#165005=CARTESIAN_POINT('Ctrl Pts',(39.5996235521064,-44.2405416721215,
-78.0616481127407));
#165006=CARTESIAN_POINT('Ctrl Pts',(39.3379923637148,-44.93000002,-77.9585218257824));
#165007=CARTESIAN_POINT('Ctrl Pts',(40.039661195993,-44.93000002,-78.208477386432));
#165008=CARTESIAN_POINT('Ctrl Pts',(39.4559266167971,-44.2634896702644,
-78.5002957502421));
#165009=CARTESIAN_POINT('Ctrl Pts',(39.2335339077575,-44.93000002,-78.4222204753855));
#165010=CARTESIAN_POINT('Ctrl Pts',(39.9103339554084,-44.93000002,-78.6298739674098));
#165011=CARTESIAN_POINT('Ctrl Pts',(39.1112085107541,-44.333906530637,-79.8478079198197));
#165012=CARTESIAN_POINT('Ctrl Pts',(39.010584818663,-44.93000002,-79.7803625539821));
#165013=CARTESIAN_POINT('Ctrl Pts',(39.6000876590965,-44.93000002,-79.9237827775448));
#165014=CARTESIAN_POINT('Ctrl Pts',(39.,-44.381938656112,-80.7689356438042));
#165015=CARTESIAN_POINT('Ctrl Pts',(38.9494857171145,-44.9300000199999,
-80.7217336743568));
#165016=CARTESIAN_POINT('Ctrl Pts',(39.5000000012115,-44.93000002,-80.807470573569));
#165017=CARTESIAN_POINT('Ctrl Pts',(39.,-44.43000002,-81.6937887068282));
#165018=CARTESIAN_POINT('Ctrl Pts',(38.9999999999999,-44.9300000199999,
-81.6937887068281));
#165019=CARTESIAN_POINT('Ctrl Pts',(39.5,-44.93000002,-81.6937887068282));
#165020=CARTESIAN_POINT('',(39.5,-44.93000002,-81.6937887068282));
#165021=CARTESIAN_POINT('Origin',(39.5,-44.43000002,-81.6937887068282));
#165022=CARTESIAN_POINT('Ctrl Pts',(39.5,-44.93000002,-81.6937887068282));
#165023=CARTESIAN_POINT('Ctrl Pts',(39.5,-44.93000002,-81.4715915443628));
#165024=CARTESIAN_POINT('Ctrl Pts',(39.5062851881924,-44.93000002,-81.2500804744028));
#165025=CARTESIAN_POINT('Ctrl Pts',(39.5189031887286,-44.93000002,-81.0292580402079));
#165026=CARTESIAN_POINT('Ctrl Pts',(39.5308326200064,-44.93000002,-80.82048597321));
#165027=CARTESIAN_POINT('Ctrl Pts',(39.548422932141,-44.93000002,-80.6123290364182));
#165028=CARTESIAN_POINT('Ctrl Pts',(39.5717668549556,-44.93000002,-80.404790058523));
#165029=CARTESIAN_POINT('Ctrl Pts',(39.5731142710433,-44.93000002,-80.3928108654859));
#165030=CARTESIAN_POINT('Ctrl Pts',(39.5744808704138,-44.93000002,-80.3808337323854));
#165031=CARTESIAN_POINT('Ctrl Pts',(39.5758666762242,-44.93000002,-80.3688586602484));
#165032=CARTESIAN_POINT('Ctrl Pts',(39.5992261762147,-44.93000002,-80.167003757221));
#165033=CARTESIAN_POINT('Ctrl Pts',(39.6280811656786,-44.93000002,-79.9654411052776));
#165034=CARTESIAN_POINT('Ctrl Pts',(39.6625124125991,-44.93000002,-79.7646415180466));
#165035=CARTESIAN_POINT('Ctrl Pts',(39.6964841131886,-44.93000002,-79.5665219590398));
#165036=CARTESIAN_POINT('Ctrl Pts',(39.7358842319638,-44.93000002,-79.3691455608367));
#165037=CARTESIAN_POINT('Ctrl Pts',(39.780739886981,-44.93000002,-79.1729578992698));
#165038=CARTESIAN_POINT('Ctrl Pts',(39.7892690083243,-44.93000002,-79.1356536090772));
#165039=CARTESIAN_POINT('Ctrl Pts',(39.7979952284866,-44.93000002,-79.0983922704899));
#165040=CARTESIAN_POINT('Ctrl Pts',(39.8069185231454,-44.93000002,-79.0611769040833));
#165041=CARTESIAN_POINT('Ctrl Pts',(39.910333955099,-44.93000002,-78.6298739672844));
#165042=CARTESIAN_POINT('Ctrl Pts',(40.0396611959927,-44.93000002,-78.2084773864585));
#165043=CARTESIAN_POINT('Ctrl Pts',(40.1983721980467,-44.93000002,-77.7983145251761));
#165044=CARTESIAN_POINT('Ctrl Pts',(40.3310078543844,-44.93000002,-77.4555391686635));
#165045=CARTESIAN_POINT('Ctrl Pts',(40.483938162075,-44.93000002,-77.1205226744407));
#165046=CARTESIAN_POINT('Ctrl Pts',(40.662722300217,-44.93000002,-76.7953903626101));
#165047=CARTESIAN_POINT('Ctrl Pts',(40.697870150647,-44.93000002,-76.7314713707748));
#165048=CARTESIAN_POINT('Ctrl Pts',(40.734017377992,-44.93000002,-76.6679344511747));
#165049=CARTESIAN_POINT('Ctrl Pts',(40.7712064624936,-44.93000002,-76.6047958451324));
#165050=CARTESIAN_POINT('Origin',(39.5,-44.43000002,-55.2499500000007));
#165051=CARTESIAN_POINT('',(39.5,-44.93000002,-150.364854264666));
#165052=CARTESIAN_POINT('Origin',(39.5,-44.43000002,-150.364854264666));
#165053=CARTESIAN_POINT('',(39.5,-44.93000002,-55.2499500000007));
#165054=CARTESIAN_POINT('Ctrl Pts',(39.0055150586856,-44.4477113456027,
-150.003379856068));
#165055=CARTESIAN_POINT('Ctrl Pts',(39.0227012659498,-44.93000002,-150.00371437679));
#165056=CARTESIAN_POINT('Ctrl Pts',(39.5049987237219,-44.93000002,-150.018486848937));
#165057=CARTESIAN_POINT('Ctrl Pts',(38.9734136439675,-44.3930232755833,
-151.055460419798));
#165058=CARTESIAN_POINT('Ctrl Pts',(38.9344833976404,-44.93000002,-151.111926007989));
#165059=CARTESIAN_POINT('Ctrl Pts',(39.4760001584505,-44.93000002,-151.026575388255));
#165060=CARTESIAN_POINT('Ctrl Pts',(39.0810964939062,-44.3391675960254,
-152.087737194438));
#165061=CARTESIAN_POINT('Ctrl Pts',(38.9915721940229,-44.93000002,-152.165744946158));
#165062=CARTESIAN_POINT('Ctrl Pts',(39.5728295161603,-44.93000002,-152.016813423143));
#165063=CARTESIAN_POINT('Ctrl Pts',(39.4525277093705,-44.2629792367123,
-153.545360859045));
#165064=CARTESIAN_POINT('Ctrl Pts',(39.2290603541538,-44.93000002,-153.623344231399));
#165065=CARTESIAN_POINT('Ctrl Pts',(39.9069198952433,-44.93000002,-153.416428338509));
#165066=CARTESIAN_POINT('Ctrl Pts',(39.5975827673942,-44.2397053437839,
-153.990247284421));
#165067=CARTESIAN_POINT('Ctrl Pts',(39.3342779655495,-44.93000002,-154.093989914495));
#165068=CARTESIAN_POINT('Ctrl Pts',(40.0374208080396,-44.93000002,-153.8438516675));
#165069=CARTESIAN_POINT('Ctrl Pts',(39.9982241297396,-44.1889106964072,
-154.960684718783));
#165070=CARTESIAN_POINT('Ctrl Pts',(39.638422111897,-44.9300000199999,-155.155380476238));
#165071=CARTESIAN_POINT('Ctrl Pts',(40.3978966779789,-44.93000002,-154.776621822351));
#165072=CARTESIAN_POINT('Ctrl Pts',(40.2725981949087,-44.1616758422127,
-155.480642655351));
#165073=CARTESIAN_POINT('Ctrl Pts',(39.8606808421836,-44.9300000200001,
-155.739479736185));
#165074=CARTESIAN_POINT('Ctrl Pts',(40.6447774862557,-44.93000002,-155.276660282544));
#165075=CARTESIAN_POINT('Ctrl Pts',(40.6171580660072,-44.1359519133608,
-155.971665887251));
#165076=CARTESIAN_POINT('Ctrl Pts',(40.1350091672924,-44.93000002,-156.289052674551));
#165077=CARTESIAN_POINT('Ctrl Pts',(40.9548496935007,-44.93000002,-155.74912533543));
#165078=CARTESIAN_POINT('',(40.7712064624936,-44.93000002,-155.453847126373));
#165079=CARTESIAN_POINT('Origin',(40.7712064624936,-44.43000002,-155.453847126373));
#165080=CARTESIAN_POINT('Ctrl Pts',(40.7712064624936,-44.93000002,-155.453847126373));
#165081=CARTESIAN_POINT('Ctrl Pts',(40.5636969173263,-44.93000002,-155.101543121101));
#165082=CARTESIAN_POINT('Ctrl Pts',(40.3878808276675,-44.93000002,-154.735494168673));
#165083=CARTESIAN_POINT('Ctrl Pts',(40.2370488760061,-44.93000002,-154.35860999499));
#165084=CARTESIAN_POINT('Ctrl Pts',(40.2234902738163,-44.93000002,-154.324731081893));
#165085=CARTESIAN_POINT('Ctrl Pts',(40.2101335892401,-44.93000002,-154.290764600318));
#165086=CARTESIAN_POINT('Ctrl Pts',(40.1969739657515,-44.93000002,-154.256712656464));
#165087=CARTESIAN_POINT('Ctrl Pts',(40.0374208080236,-44.93000002,-153.843851667435));
#165088=CARTESIAN_POINT('Ctrl Pts',(39.9069198944888,-44.93000002,-153.416428338648));
#165089=CARTESIAN_POINT('Ctrl Pts',(39.8044156663649,-44.93000002,-152.987004278786));
#165090=CARTESIAN_POINT('Ctrl Pts',(39.6913863431124,-44.93000002,-152.513487119906));
#165091=CARTESIAN_POINT('Ctrl Pts',(39.6104670975054,-44.93000002,-152.035255380817));
#165092=CARTESIAN_POINT('Ctrl Pts',(39.5605987441789,-44.93000002,-151.552464535406));
#165093=CARTESIAN_POINT('Ctrl Pts',(39.5200177005092,-44.93000002,-151.159586987341));
#165094=CARTESIAN_POINT('Ctrl Pts',(39.4999999999997,-44.93000002,-150.763690175803));
#165095=CARTESIAN_POINT('Ctrl Pts',(39.5,-44.93000002,-150.364854264666));
#165096=CARTESIAN_POINT('Ctrl Pts',(49.5369875341119,-44.93000002,-170.861259130871));
#165097=CARTESIAN_POINT('Ctrl Pts',(48.7929216289437,-44.9300000199999,
-171.272289063137));
#165098=CARTESIAN_POINT('Ctrl Pts',(49.1544657093286,-44.1870483688939,
-171.07256826174));
#165099=CARTESIAN_POINT('Ctrl Pts',(46.6796506810215,-44.93000002,-165.688772250388));
#165100=CARTESIAN_POINT('Ctrl Pts',(45.8620651160177,-44.9300000199373,
-166.013584137672));
#165101=CARTESIAN_POINT('Ctrl Pts',(46.303473398785,-44.1770628106394,-165.900085726624));
#165102=CARTESIAN_POINT('Ctrl Pts',(43.7703248719811,-44.93000002,-160.54566797298));
#165103=CARTESIAN_POINT('Ctrl Pts',(42.9064403928045,-44.93000002,-160.851370978315));
#165104=CARTESIAN_POINT('Ctrl Pts',(43.4017256360502,-44.1659184128467,
-160.756986066495));
#165105=CARTESIAN_POINT('Ctrl Pts',(40.7712064624936,-44.93000002,-155.453847126373));
#165106=CARTESIAN_POINT('Ctrl Pts',(39.9673804148566,-44.93000002,-155.927306340695));
#165107=CARTESIAN_POINT('Ctrl Pts',(40.4124516249929,-44.1531545436406,
-155.665156257244));
#165108=CARTESIAN_POINT('',(49.5369875341119,-44.93000002,-170.861259130871));
#165109=CARTESIAN_POINT('Origin',(49.5369875341119,-44.43000002,-170.861259130871));
#165110=CARTESIAN_POINT('Ctrl Pts',(49.5369875341119,-44.93000002,-170.861259130871));
#165111=CARTESIAN_POINT('Ctrl Pts',(46.6796235355215,-44.93000002,-165.688723110732));
#165112=CARTESIAN_POINT('Ctrl Pts',(43.770354187064,-44.93000002,-160.545717743323));
#165113=CARTESIAN_POINT('Ctrl Pts',(40.7712064624936,-44.93000002,-155.453847126373));
#165114=CARTESIAN_POINT('Ctrl Pts',(49.1544657093286,-44.1870483688939,
-171.07256826174));
#165115=CARTESIAN_POINT('Ctrl Pts',(48.7929216289437,-44.9300000199999,
-171.272289063137));
#165116=CARTESIAN_POINT('Ctrl Pts',(49.5369875341119,-44.93000002,-170.861259130871));
#165117=CARTESIAN_POINT('Ctrl Pts',(49.1988333494309,-44.1988790013969,
-171.166486883581));
#165118=CARTESIAN_POINT('Ctrl Pts',(48.8869683938206,-44.93000002,-171.389208114715));
#165119=CARTESIAN_POINT('Ctrl Pts',(49.5629323055535,-44.93000002,-170.908225431312));
#165120=CARTESIAN_POINT('Ctrl Pts',(49.2553422033029,-44.2139336491638,
-171.248946535323));
#165121=CARTESIAN_POINT('Ctrl Pts',(48.9974211832039,-44.93000002,-171.47664075754));
#165122=CARTESIAN_POINT('Ctrl Pts',(49.5959607588443,-44.93000002,-170.94944826591));
#165123=CARTESIAN_POINT('Ctrl Pts',(49.3888358236751,-44.249424483408,-171.394272113556));
#165124=CARTESIAN_POINT('Ctrl Pts',(49.2286028218105,-44.93000002,-171.604363908288));
#165125=CARTESIAN_POINT('Ctrl Pts',(49.673955990897,-44.93000002,-171.02211105853));
#165126=CARTESIAN_POINT('Ctrl Pts',(49.4642369070823,-44.2694386569593,
-171.45497652175));
#165127=CARTESIAN_POINT('Ctrl Pts',(49.3448677594853,-44.9300000199992,
-171.644582495821));
#165128=CARTESIAN_POINT('Ctrl Pts',(49.7179930277929,-44.93000002,-171.052463257479));
#165129=CARTESIAN_POINT('Ctrl Pts',(49.7071198591548,-44.3337582466603,
-171.601144400479));
#165130=CARTESIAN_POINT('Ctrl Pts',(49.6719308335793,-44.9300000200013,
-171.711639121533));
#165131=CARTESIAN_POINT('Ctrl Pts',(49.8597665056525,-44.93000002,-171.125547207032));
#165132=CARTESIAN_POINT('Ctrl Pts',(49.8895242589787,-44.3818638633066,
-171.64995));
#165133=CARTESIAN_POINT('Ctrl Pts',(49.8809090309114,-44.93000002,-171.700346637809));
#165134=CARTESIAN_POINT('Ctrl Pts',(49.9661358829125,-44.93000002,-171.149949988199));
#165135=CARTESIAN_POINT('Ctrl Pts',(50.0729884546894,-44.43000002,-171.64995));
#165136=CARTESIAN_POINT('Ctrl Pts',(50.0729884546893,-44.93000002,-171.64995));
#165137=CARTESIAN_POINT('Ctrl Pts',(50.0729884546894,-44.93000002,-171.14995));
#165138=CARTESIAN_POINT('',(50.0729884546894,-44.93000002,-171.14995));
#165139=CARTESIAN_POINT('Origin',(50.0729884546894,-44.43000002,-171.14995));
#165140=CARTESIAN_POINT('Ctrl Pts',(50.0729884546894,-44.93000002,-171.14995));
#165141=CARTESIAN_POINT('Ctrl Pts',(50.0168171487347,-44.93000002,-171.14995));
#165142=CARTESIAN_POINT('Ctrl Pts',(49.9608486377796,-44.93000002,-171.143210614633));
#165143=CARTESIAN_POINT('Ctrl Pts',(49.9066731284767,-44.93000002,-171.129767219264));
#165144=CARTESIAN_POINT('Ctrl Pts',(49.8576729639836,-44.93000002,-171.117608061132));
#165145=CARTESIAN_POINT('Ctrl Pts',(49.8101382025079,-44.93000002,-171.099963916563));
#165146=CARTESIAN_POINT('Ctrl Pts',(49.7652508518366,-44.93000002,-171.076824577701));
#165147=CARTESIAN_POINT('Ctrl Pts',(49.7179896877752,-44.93000002,-171.052461542819));
#165148=CARTESIAN_POINT('Ctrl Pts',(49.6739559670876,-44.93000002,-171.022111093102));
#165149=CARTESIAN_POINT('Ctrl Pts',(49.6349583346168,-44.93000002,-170.985779705428));
#165150=CARTESIAN_POINT('Ctrl Pts',(49.5959662083459,-44.93000002,-170.949453447498));
#165151=CARTESIAN_POINT('Ctrl Pts',(49.5629377334322,-44.93000002,-170.908235414179));
#165152=CARTESIAN_POINT('Ctrl Pts',(49.5369875341119,-44.93000002,-170.861259130871));
#165153=CARTESIAN_POINT('Origin',(-1.31515029790052E-14,-44.43000002,-171.14995));
#165154=CARTESIAN_POINT('',(50.7754831343094,-44.93000002,-171.14995));
#165155=CARTESIAN_POINT('Origin',(50.7754831343094,-44.43000002,-171.14995));
#165156=CARTESIAN_POINT('',(49.7553180351958,-44.93000002,-171.14995));
#165157=CARTESIAN_POINT('Ctrl Pts',(52.2902244930873,-44.93000002,-172.64995));
#165158=CARTESIAN_POINT('Ctrl Pts',(51.7150402894768,-44.93000002,-172.64995));
#165159=CARTESIAN_POINT('Ctrl Pts',(51.7950904587165,-44.36041346952,-172.64995));
#165160=CARTESIAN_POINT('Ctrl Pts',(52.2902244930723,-44.93000002,-172.453565067926));
#165161=CARTESIAN_POINT('Ctrl Pts',(51.7150402894748,-44.9300000200027,
-172.529650273729));
#165162=CARTESIAN_POINT('Ctrl Pts',(51.7950904587162,-44.3604134695225,
-172.51902671195));
#165163=CARTESIAN_POINT('Ctrl Pts',(52.2507998243741,-44.93000002,-172.257328160063));
#165164=CARTESIAN_POINT('Ctrl Pts',(51.6933705738162,-44.93000002,-172.409726298163));
#165165=CARTESIAN_POINT('Ctrl Pts',(51.7685528054411,-44.3622246214263,
-172.38820210671));
#165166=CARTESIAN_POINT('Ctrl Pts',(52.0990435210912,-44.93000002,-171.894521542842));
#165167=CARTESIAN_POINT('Ctrl Pts',(51.6069372443981,-44.93000002,-172.182182441317));
#165168=CARTESIAN_POINT('Ctrl Pts',(51.6664021396144,-44.3691962391205,
-172.14633102856));
#165169=CARTESIAN_POINT('Ctrl Pts',(51.9867715634496,-44.93000002,-171.728129909852));
#165170=CARTESIAN_POINT('Ctrl Pts',(51.5426661785871,-44.9300000199979,
-172.075215659168));
#165171=CARTESIAN_POINT('Ctrl Pts',(51.5908292969809,-44.3743539633763,
-172.035403273235));
#165172=CARTESIAN_POINT('Ctrl Pts',(51.7063624782404,-44.93000002,-171.450449746589));
#165173=CARTESIAN_POINT('Ctrl Pts',(51.3750094074331,-44.930000020002,-171.888983273332));
#165174=CARTESIAN_POINT('Ctrl Pts',(51.4020794781095,-44.387235833176,-171.850283164392));
#165175=CARTESIAN_POINT('Ctrl Pts',(51.5383356195984,-44.93000002,-171.339270411997));
#165176=CARTESIAN_POINT('Ctrl Pts',(51.2724346946947,-44.9300000200007,
-171.809929875206));
#165177=CARTESIAN_POINT('Ctrl Pts',(51.2889767264242,-44.3949549130127,
-171.776163607997));
#165178=CARTESIAN_POINT('Ctrl Pts',(51.1719634936654,-44.93000002,-171.18899099047));
#165179=CARTESIAN_POINT('Ctrl Pts',(51.0396558988745,-44.9300000199993,
-171.69520402023));
#165180=CARTESIAN_POINT('Ctrl Pts',(51.0423632033321,-44.411785887019,-171.675977326981));
#165181=CARTESIAN_POINT('Ctrl Pts',(50.9737980536844,-44.93000002,-171.149950000016));
#165182=CARTESIAN_POINT('Ctrl Pts',(50.9102650806209,-44.93000002,-171.659148653595));
#165183=CARTESIAN_POINT('Ctrl Pts',(50.9089734778343,-44.4208895200012,
-171.64995));
#165184=CARTESIAN_POINT('Ctrl Pts',(50.7754831343094,-44.93000002,-171.14995));
#165185=CARTESIAN_POINT('Ctrl Pts',(50.7754831343094,-44.9300000199999,
-171.64995));
#165186=CARTESIAN_POINT('Ctrl Pts',(50.7754831343094,-44.43000002,-171.64995));
#165187=CARTESIAN_POINT('',(52.2902244930873,-44.93000002,-172.64995));
#165188=CARTESIAN_POINT('',(51.7902244930873,-44.43000002,-172.64995));
#165189=CARTESIAN_POINT('Origin',(52.2902244930873,-44.43000002,-172.64995));
#165190=CARTESIAN_POINT('Origin',(52.2902244930873,-44.43000002,-172.64995));
#165191=CARTESIAN_POINT('Ctrl Pts',(52.2902244930873,-44.93000002,-172.64995));
#165192=CARTESIAN_POINT('Ctrl Pts',(52.2902244930723,-44.93000002,-172.453565067926));
#165193=CARTESIAN_POINT('Ctrl Pts',(52.2507998243741,-44.93000002,-172.257328160063));
#165194=CARTESIAN_POINT('Ctrl Pts',(52.0990435210912,-44.93000002,-171.894521542842));
#165195=CARTESIAN_POINT('Ctrl Pts',(51.9867715634496,-44.93000002,-171.728129909852));
#165196=CARTESIAN_POINT('Ctrl Pts',(51.7063624782404,-44.93000002,-171.450449746589));
#165197=CARTESIAN_POINT('Ctrl Pts',(51.5383356195984,-44.93000002,-171.339270411997));
#165198=CARTESIAN_POINT('Ctrl Pts',(51.1719634936654,-44.93000002,-171.18899099047));
#165199=CARTESIAN_POINT('Ctrl Pts',(50.9737980536844,-44.93000002,-171.149950000016));
#165200=CARTESIAN_POINT('Ctrl Pts',(50.7754831343094,-44.93000002,-171.14995));
#165201=CARTESIAN_POINT('Origin',(52.2902244930873,-44.43000002,-171.64995));
#165202=CARTESIAN_POINT('',(52.2902244930873,-44.93000002,-55.2499500000007));
#165203=CARTESIAN_POINT('',(51.7950904587165,-44.36041346952,-171.64995));
#165204=CARTESIAN_POINT('Origin',(60.,-45.43000002,-176.84995));
#165205=CARTESIAN_POINT('',(-83.2809572255632,-44.93000002,-176.84995));
#165206=CARTESIAN_POINT('Origin',(-83.2809572255632,-44.43000002,-61.14995));
#165207=CARTESIAN_POINT('',(49.940073970993,-44.93000002,-61.14995));
#165208=CARTESIAN_POINT('',(49.940073970993,-44.43000002,-60.64995));
#165209=CARTESIAN_POINT('Origin',(49.940073970993,-44.43000002,-61.14995));
#165210=CARTESIAN_POINT('',(51.3752989258075,-44.43000002,-60.64995));
#165211=CARTESIAN_POINT('',(-1.31515029790052E-14,-44.43000002,-60.64995));
#165212=CARTESIAN_POINT('',(51.3752989258075,-44.93000002,-61.14995));
#165213=CARTESIAN_POINT('Origin',(51.3752989258075,-44.43000002,-61.14995));
#165214=CARTESIAN_POINT('',(-83.2809572255632,-44.93000002,-61.14995));
#165215=CARTESIAN_POINT('Origin',(57.,-45.43000002,-58.24995));
#165216=CARTESIAN_POINT('',(57.,-44.93000002,-55.74995));
#165217=CARTESIAN_POINT('Origin',(57.,-44.93000002,-58.24995));
#165218=CARTESIAN_POINT('',(57.,-45.43000002,-55.24995));
#165219=CARTESIAN_POINT('Origin',(57.,-45.43000002,-55.74995));
#165220=CARTESIAN_POINT('Origin',(57.,-45.43000002,-58.24995));
#165221=CARTESIAN_POINT('Origin',(57.,-2.42462934179819E-14,-58.24995));
#165222=CARTESIAN_POINT('',(57.,-45.93000002,-55.24995));
#165223=CARTESIAN_POINT('',(57.,28.41999998,-55.24995));
#165224=CARTESIAN_POINT('Origin',(57.,-45.93000002,-58.24995));
#165225=CARTESIAN_POINT('Origin',(57.,-45.93000002,-58.24995));
#165226=CARTESIAN_POINT('',(57.,-46.43000002,-55.74995));
#165227=CARTESIAN_POINT('Origin',(57.,-45.93000002,-55.74995));
#165228=CARTESIAN_POINT('',(59.5,-46.43000002,-58.24995));
#165229=CARTESIAN_POINT('Origin',(57.,-46.43000002,-58.24995));
#165230=CARTESIAN_POINT('Origin',(59.5,-45.93000002,-58.24995));
#165231=CARTESIAN_POINT('Origin',(59.5,-45.93000002,-55.2499500000008));
#165232=CARTESIAN_POINT('',(59.5,-46.43000002,-174.34995));
#165233=CARTESIAN_POINT('',(59.5,-46.43000002,-58.24995));
#165234=CARTESIAN_POINT('Origin',(59.5,-45.93000002,-174.34995));
#165235=CARTESIAN_POINT('Origin',(57.,-45.93000002,-174.34995));
#165236=CARTESIAN_POINT('',(57.,-46.43000002,-176.84995));
#165237=CARTESIAN_POINT('Origin',(57.,-46.43000002,-174.34995));
#165238=CARTESIAN_POINT('Origin',(57.,-45.93000002,-176.84995));
#165239=CARTESIAN_POINT('Origin',(-83.2809572255632,-45.9300000199999,-176.84995));
#165240=CARTESIAN_POINT('',(-83.2809572255632,-46.4300000199999,-176.84995));
#165241=CARTESIAN_POINT('Origin',(51.9388724063314,-46.93000002,-171.64995));
#165242=CARTESIAN_POINT('',(51.9388724063314,-46.43000002,-172.64995));
#165243=CARTESIAN_POINT('',(51.9388724063314,-46.43000002,-55.2499500000008));
#165244=CARTESIAN_POINT('Origin',(51.9388724063314,-46.93000002,-172.64995));
#165245=CARTESIAN_POINT('',(51.4437383719606,-46.86041346952,-171.64995));
#165246=CARTESIAN_POINT('Ctrl Pts',(50.4241310475534,-46.43000002,-171.14995));
#165247=CARTESIAN_POINT('Ctrl Pts',(50.4241310475535,-46.43000002,-171.64995));
#165248=CARTESIAN_POINT('Ctrl Pts',(50.4241310475534,-46.93000002,-171.64995));
#165249=CARTESIAN_POINT('Ctrl Pts',(50.6224459669284,-46.43000002,-171.149950000016));
#165250=CARTESIAN_POINT('Ctrl Pts',(50.5563794763166,-46.43000002,-171.640924254979));
#165251=CARTESIAN_POINT('Ctrl Pts',(50.5576213910783,-46.9208895200013,
-171.64995));
#165252=CARTESIAN_POINT('Ctrl Pts',(50.8206114069094,-46.43000002,-171.18899099047));
#165253=CARTESIAN_POINT('Ctrl Pts',(50.6936490544688,-46.43000002,-171.658003579003));
#165254=CARTESIAN_POINT('Ctrl Pts',(50.6910111165761,-46.911785887019,-171.675977326981));
#165255=CARTESIAN_POINT('Ctrl Pts',(51.1869835328424,-46.43000002,-171.339270411997));
#165256=CARTESIAN_POINT('Ctrl Pts',(50.9520843153697,-46.4300000199999,
-171.746711574348));
#165257=CARTESIAN_POINT('Ctrl Pts',(50.9376246396682,-46.8949549130127,
-171.776163607997));
#165258=CARTESIAN_POINT('Ctrl Pts',(51.3550103914843,-46.43000002,-171.450449746589));
#165259=CARTESIAN_POINT('Ctrl Pts',(51.0736480315269,-46.4300000199987,
-171.817687494207));
#165260=CARTESIAN_POINT('Ctrl Pts',(51.0507273913534,-46.887235833176,-171.850283164392));
#165261=CARTESIAN_POINT('Ctrl Pts',(51.6354194766937,-46.43000002,-171.728129909852));
#165262=CARTESIAN_POINT('Ctrl Pts',(51.2780932509,-46.4300000200014,-172.003556970023));
#165263=CARTESIAN_POINT('Ctrl Pts',(51.239477210225,-46.8743539633763,-172.035403273235));
#165264=CARTESIAN_POINT('Ctrl Pts',(51.7476914343352,-46.43000002,-171.894521542842));
#165265=CARTESIAN_POINT('Ctrl Pts',(51.3616623431659,-46.43000002,-172.118296873734));
#165266=CARTESIAN_POINT('Ctrl Pts',(51.3150500528584,-46.8691962391206,
-172.14633102856));
#165267=CARTESIAN_POINT('Ctrl Pts',(51.8994477376182,-46.43000002,-172.257328160063));
#165268=CARTESIAN_POINT('Ctrl Pts',(51.4744733522994,-46.43000002,-172.371853931892));
#165269=CARTESIAN_POINT('Ctrl Pts',(51.4172007186852,-46.8622246214263,
-172.38820210671));
#165270=CARTESIAN_POINT('Ctrl Pts',(51.9388724063164,-46.43000002,-172.453565067926));
#165271=CARTESIAN_POINT('Ctrl Pts',(51.5042290374097,-46.43000002,-172.511015867073));
#165272=CARTESIAN_POINT('Ctrl Pts',(51.4437383719602,-46.8604134695225,
-172.51902671195));
#165273=CARTESIAN_POINT('Ctrl Pts',(51.9388724063314,-46.43000002,-172.64995));
#165274=CARTESIAN_POINT('Ctrl Pts',(51.5042290374232,-46.43000002,-172.64995));
#165275=CARTESIAN_POINT('Ctrl Pts',(51.4437383719606,-46.86041346952,-172.64995));
#165276=CARTESIAN_POINT('',(50.4241310475534,-46.43000002,-171.14995));
#165277=CARTESIAN_POINT('Ctrl Pts',(50.4241310475534,-46.43000002,-171.14995));
#165278=CARTESIAN_POINT('Ctrl Pts',(50.6224459669284,-46.43000002,-171.149950000016));
#165279=CARTESIAN_POINT('Ctrl Pts',(50.8206114069094,-46.43000002,-171.18899099047));
#165280=CARTESIAN_POINT('Ctrl Pts',(51.1869835328424,-46.43000002,-171.339270411997));
#165281=CARTESIAN_POINT('Ctrl Pts',(51.3550103914843,-46.43000002,-171.450449746589));
#165282=CARTESIAN_POINT('Ctrl Pts',(51.6354194766937,-46.43000002,-171.728129909852));
#165283=CARTESIAN_POINT('Ctrl Pts',(51.7476914343352,-46.43000002,-171.894521542842));
#165284=CARTESIAN_POINT('Ctrl Pts',(51.8994477376182,-46.43000002,-172.257328160063));
#165285=CARTESIAN_POINT('Ctrl Pts',(51.9388724063164,-46.43000002,-172.453565067926));
#165286=CARTESIAN_POINT('Ctrl Pts',(51.9388724063314,-46.43000002,-172.64995));
#165287=CARTESIAN_POINT('Origin',(50.4241310475534,-46.93000002,-171.14995));
#165288=CARTESIAN_POINT('Origin',(-1.41965171211599E-14,-46.93000002,-171.14995));
#165289=CARTESIAN_POINT('',(48.4122058243951,-46.43000002,-171.14995));
#165290=CARTESIAN_POINT('',(50.4944014649046,-46.43000002,-171.14995));
#165291=CARTESIAN_POINT('Origin',(48.4122058243951,-46.93000002,-171.14995));
#165292=CARTESIAN_POINT('Ctrl Pts',(48.5201235179867,-46.9606462876662,
-171.644181328151));
#165293=CARTESIAN_POINT('Ctrl Pts',(48.5228147479093,-46.4300000200001,
-171.676734375474));
#165294=CARTESIAN_POINT('Ctrl Pts',(48.4767984570328,-46.43000002,-171.147074844096));
#165295=CARTESIAN_POINT('Ctrl Pts',(48.3058611060635,-46.9004466821901,
-171.667220120137));
#165296=CARTESIAN_POINT('Ctrl Pts',(48.311325817959,-46.4300000199996,-171.634847520409));
#165297=CARTESIAN_POINT('Ctrl Pts',(48.3485998488332,-46.43000002,-171.158575233343));
#165298=CARTESIAN_POINT('Ctrl Pts',(48.0796981189137,-46.8364853152072,
-171.621252940216));
#165299=CARTESIAN_POINT('Ctrl Pts',(48.1036590804166,-46.4300000200009,
-171.543768248534));
#165300=CARTESIAN_POINT('Ctrl Pts',(48.2130231518178,-46.43000002,-171.135576813935));
#165301=CARTESIAN_POINT('Ctrl Pts',(47.6908242556552,-46.7259662378658,
-171.391170182407));
#165302=CARTESIAN_POINT('Ctrl Pts',(47.7775505894744,-46.4300000199991,
-171.283378605487));
#165303=CARTESIAN_POINT('Ctrl Pts',(47.9796068491616,-46.43000002,-171.020522742606));
#165304=CARTESIAN_POINT('Ctrl Pts',(47.5227534239133,-46.677891632908,-171.205193874949));
#165305=CARTESIAN_POINT('Ctrl Pts',(47.6425982485164,-46.4300000200003,
-171.112712451737));
#165306=CARTESIAN_POINT('Ctrl Pts',(47.8785659772877,-46.43000002,-170.92757795489));
#165307=CARTESIAN_POINT('Ctrl Pts',(47.4395650454936,-46.654055562307,-170.951379521332));
#165308=CARTESIAN_POINT('Ctrl Pts',(47.5779186181849,-46.4300000199999,
-170.897903745869));
#165309=CARTESIAN_POINT('Ctrl Pts',(47.8284835237321,-46.43000002,-170.800621877871));
#165310=CARTESIAN_POINT('',(47.8576079004676,-46.43000002,-170.861259130871));
#165311=CARTESIAN_POINT('Ctrl Pts',(47.8576079004676,-46.43000002,-170.861259130871));
#165312=CARTESIAN_POINT('Ctrl Pts',(47.8760580377294,-46.43000002,-170.89352615778));
#165313=CARTESIAN_POINT('Ctrl Pts',(47.8980723549739,-46.43000002,-170.923203523829));
#165314=CARTESIAN_POINT('Ctrl Pts',(47.9228861329632,-46.43000002,-170.950192158739));
#165315=CARTESIAN_POINT('Ctrl Pts',(47.9503841163783,-46.43000002,-170.980100262029));
#165316=CARTESIAN_POINT('Ctrl Pts',(47.9813190176472,-46.43000002,-171.00670574507));
#165317=CARTESIAN_POINT('Ctrl Pts',(48.0145941519147,-46.43000002,-171.029912775459));
#165318=CARTESIAN_POINT('Ctrl Pts',(48.0405863852467,-46.43000002,-171.048040502427));
#165319=CARTESIAN_POINT('Ctrl Pts',(48.0680050205664,-46.43000002,-171.06409541242));
#165320=CARTESIAN_POINT('Ctrl Pts',(48.0963149978629,-46.43000002,-171.078049783599));
#165321=CARTESIAN_POINT('Ctrl Pts',(48.1225339813698,-46.43000002,-171.090973475624));
#165322=CARTESIAN_POINT('Ctrl Pts',(48.1495923840829,-46.43000002,-171.102104191555));
#165323=CARTESIAN_POINT('Ctrl Pts',(48.177275111639,-46.43000002,-171.111506345608));
#165324=CARTESIAN_POINT('Ctrl Pts',(48.2055749629088,-46.43000002,-171.121118099391));
#165325=CARTESIAN_POINT('Ctrl Pts',(48.2345286556579,-46.43000002,-171.128923533851));
#165326=CARTESIAN_POINT('Ctrl Pts',(48.2639285033283,-46.43000002,-171.134940493274));
#165327=CARTESIAN_POINT('Ctrl Pts',(48.2928212065519,-46.43000002,-171.140853660745));
#165328=CARTESIAN_POINT('Ctrl Pts',(48.3221462163588,-46.43000002,-171.145039422868));
#165329=CARTESIAN_POINT('Ctrl Pts',(48.35170660164,-46.43000002,-171.147466016794));
#165330=CARTESIAN_POINT('Ctrl Pts',(48.3717866301035,-46.43000002,-171.149114374034));
#165331=CARTESIAN_POINT('Ctrl Pts',(48.3919752683815,-46.43000002,-171.14995));
#165332=CARTESIAN_POINT('Ctrl Pts',(48.4122058243951,-46.43000002,-171.14995));
#165333=CARTESIAN_POINT('Origin',(47.8576079004676,-46.93000002,-170.861259130871));
#165334=CARTESIAN_POINT('Ctrl Pts',(40.8634877666247,-46.43000002,-158.96051646616));
#165335=CARTESIAN_POINT('Ctrl Pts',(40.6428186202086,-46.43000002,-159.094316247135));
#165336=CARTESIAN_POINT('Ctrl Pts',(40.5149864073608,-46.6403532458042,
-159.17182559703));
#165337=CARTESIAN_POINT('Ctrl Pts',(43.2493416424527,-46.43000002,-162.895383432653));
#165338=CARTESIAN_POINT('Ctrl Pts',(43.0357695446718,-46.4300000199999,
-163.055969456472));
#165339=CARTESIAN_POINT('Ctrl Pts',(42.8925295367156,-46.6503554345072,
-163.106696326736));
#165340=CARTESIAN_POINT('Ctrl Pts',(45.5734830336511,-46.43000002,-166.866604917879));
#165341=CARTESIAN_POINT('Ctrl Pts',(45.3499681200706,-46.4300000200635,
-167.025403443097));
#165342=CARTESIAN_POINT('Ctrl Pts',(45.2098379840441,-46.6594189992588,
-167.077916061371));
#165343=CARTESIAN_POINT('Ctrl Pts',(47.8576079004676,-46.43000002,-170.861259130871));
#165344=CARTESIAN_POINT('Ctrl Pts',(47.6152001643476,-46.4300000199999,
-170.99986675708));
#165345=CARTESIAN_POINT('Ctrl Pts',(47.4880541505298,-46.6677435098469,
-171.07256826174));
#165346=CARTESIAN_POINT('',(40.8634877666247,-46.43000002,-158.96051646616));
#165347=CARTESIAN_POINT('Ctrl Pts',(40.8634877666247,-46.43000002,-158.96051646616));
#165348=CARTESIAN_POINT('Ctrl Pts',(43.2493545263947,-46.43000002,-162.895404681481));
#165349=CARTESIAN_POINT('Ctrl Pts',(45.5734709768386,-46.43000002,-166.866583832071));
#165350=CARTESIAN_POINT('Ctrl Pts',(47.8576079004676,-46.43000002,-170.861259130871));
#165351=CARTESIAN_POINT('Origin',(40.8634877666247,-46.93000002,-158.96051646616));
#165352=CARTESIAN_POINT('Ctrl Pts',(40.5149864073608,-46.6403532458042,
-159.17182559703));
#165353=CARTESIAN_POINT('Ctrl Pts',(40.6428186202086,-46.43000002,-159.094316247135));
#165354=CARTESIAN_POINT('Ctrl Pts',(40.8634877666247,-46.43000002,-158.96051646616));
#165355=CARTESIAN_POINT('Ctrl Pts',(40.2420911121462,-46.6621010340167,
-158.751563565514));
#165356=CARTESIAN_POINT('Ctrl Pts',(40.3700931620574,-46.4300000200016,
-158.677563865504));
#165357=CARTESIAN_POINT('Ctrl Pts',(40.6178692894368,-46.43000002,-158.555430440935));
#165358=CARTESIAN_POINT('Ctrl Pts',(40.0174528618108,-46.6847857442649,
-158.313094806771));
#165359=CARTESIAN_POINT('Ctrl Pts',(40.1461325131811,-46.43000002,-158.247022454196));
#165360=CARTESIAN_POINT('Ctrl Pts',(40.4157075765897,-46.43000002,-158.132972668916));
#165361=CARTESIAN_POINT('Ctrl Pts',(39.638679212826,-46.73149352613,-157.409902189902));
#165362=CARTESIAN_POINT('Ctrl Pts',(39.7602015168115,-46.43000002,-157.36115128782));
#165363=CARTESIAN_POINT('Ctrl Pts',(40.0748112905834,-46.43000002,-157.263052526127));
#165364=CARTESIAN_POINT('Ctrl Pts',(39.4849903409058,-46.7555303756697,
-156.944912677889));
#165365=CARTESIAN_POINT('Ctrl Pts',(39.6001411399911,-46.43000002,-156.903057342463));
#165366=CARTESIAN_POINT('Ctrl Pts',(39.936491307137,-46.43000002,-156.81535457804));
#165367=CARTESIAN_POINT('Ctrl Pts',(39.1168883482047,-46.8294056411102,
-155.514886495441));
#165368=CARTESIAN_POINT('Ctrl Pts',(39.1919344928279,-46.43000002,-155.466951428797));
#165369=CARTESIAN_POINT('Ctrl Pts',(39.6051995127405,-46.43000002,-155.439088754162));
#165370=CARTESIAN_POINT('Ctrl Pts',(38.9999999999987,-46.8794682890831,
-154.544622066149));
#165371=CARTESIAN_POINT('Ctrl Pts',(39.0480945221819,-46.4300000199999,
-154.497280022653));
#165372=CARTESIAN_POINT('Ctrl Pts',(39.5000000011581,-46.43000002,-154.50605775913));
#165373=CARTESIAN_POINT('Ctrl Pts',(39.,-46.9300000200008,-153.563058845195));
#165374=CARTESIAN_POINT('Ctrl Pts',(38.9999999999992,-46.4300000199999,
-153.563058845195));
#165375=CARTESIAN_POINT('Ctrl Pts',(39.5,-46.43000002,-153.563058845195));
#165376=CARTESIAN_POINT('',(39.5,-46.43000002,-153.563058845195));
#165377=CARTESIAN_POINT('Ctrl Pts',(39.5,-46.43000002,-153.563058845195));
#165378=CARTESIAN_POINT('Ctrl Pts',(39.4999999999995,-46.43000002,-153.949465551025));
#165379=CARTESIAN_POINT('Ctrl Pts',(39.517659421908,-46.43000002,-154.333958533359));
#165380=CARTESIAN_POINT('Ctrl Pts',(39.5536573145516,-46.43000002,-154.716308049405));
#165381=CARTESIAN_POINT('Ctrl Pts',(39.5886363261002,-46.43000002,-155.087835579357));
#165382=CARTESIAN_POINT('Ctrl Pts',(39.64093030875,-46.43000002,-155.457339415578));
#165383=CARTESIAN_POINT('Ctrl Pts',(39.7112111415895,-46.43000002,-155.82460411365));
#165384=CARTESIAN_POINT('Ctrl Pts',(39.7452479661589,-46.43000002,-156.002469451805));
#165385=CARTESIAN_POINT('Ctrl Pts',(39.7835042486626,-46.43000002,-156.179809528774));
#165386=CARTESIAN_POINT('Ctrl Pts',(39.8260607087682,-46.43000002,-156.356599303471));
#165387=CARTESIAN_POINT('Ctrl Pts',(39.9364913068056,-46.43000002,-156.815354578187));
#165388=CARTESIAN_POINT('Ctrl Pts',(40.0748112905465,-46.43000002,-157.263052526106));
#165389=CARTESIAN_POINT('Ctrl Pts',(40.2452594329879,-46.43000002,-157.698012597756));
#165390=CARTESIAN_POINT('Ctrl Pts',(40.3764895639052,-46.43000002,-158.032893731271));
#165391=CARTESIAN_POINT('Ctrl Pts',(40.5265005955851,-46.43000002,-158.360328778652));
#165392=CARTESIAN_POINT('Ctrl Pts',(40.7006921181186,-46.43000002,-158.678176979737));
#165393=CARTESIAN_POINT('Ctrl Pts',(40.7527491045009,-46.43000002,-158.773165640694));
#165394=CARTESIAN_POINT('Ctrl Pts',(40.8069659798326,-46.43000002,-158.86729796943));
#165395=CARTESIAN_POINT('Ctrl Pts',(40.8634877666246,-46.43000002,-158.960516466159));
#165396=CARTESIAN_POINT('Origin',(39.5,-46.9300000199999,-153.563058845195));
#165397=CARTESIAN_POINT('Origin',(39.5,-46.93000002,-55.2499500000008));
#165398=CARTESIAN_POINT('',(39.5,-46.43000002,-78.4955841262963));
#165399=CARTESIAN_POINT('',(39.5,-46.43000002,-55.2499500000008));
#165400=CARTESIAN_POINT('Origin',(39.5,-46.93000002,-78.4955841262963));
#165401=CARTESIAN_POINT('Ctrl Pts',(39.,-46.93000002,-78.4955841262963));
#165402=CARTESIAN_POINT('Ctrl Pts',(38.9999999999999,-46.43000002,-78.4955841262962));
#165403=CARTESIAN_POINT('Ctrl Pts',(39.5,-46.43000002,-78.4955841262963));
#165404=CARTESIAN_POINT('Ctrl Pts',(39.,-46.8794362305035,-77.5133981771651));
#165405=CARTESIAN_POINT('Ctrl Pts',(39.0481232855841,-46.43000002,-77.5608042317299));
#165406=CARTESIAN_POINT('Ctrl Pts',(39.5000000013422,-46.43000002,-77.5519859229414));
#165407=CARTESIAN_POINT('Ctrl Pts',(39.1168166022506,-46.8295915161778,
-76.5473620219989));
#165408=CARTESIAN_POINT('Ctrl Pts',(39.1918385782378,-46.43000002,-76.5948804619986));
#165409=CARTESIAN_POINT('Ctrl Pts',(39.6051349405938,-46.43000002,-76.623019511696));
#165410=CARTESIAN_POINT('Ctrl Pts',(39.4815968642216,-46.7561268840582,
-75.1252733895882));
#165411=CARTESIAN_POINT('Ctrl Pts',(39.5965629951149,-46.4300000199999,
-75.1668461367765));
#165412=CARTESIAN_POINT('Ctrl Pts',(39.9334371785153,-46.43000002,-75.2543998581027));
#165413=CARTESIAN_POINT('Ctrl Pts',(39.6366096849062,-46.7317722003096,
-74.6541303933052));
#165414=CARTESIAN_POINT('Ctrl Pts',(39.7580432024793,-46.43000002,-74.70285740618));
#165415=CARTESIAN_POINT('Ctrl Pts',(40.0729487155202,-46.43000002,-74.8007807728849));
#165416=CARTESIAN_POINT('Ctrl Pts',(40.0169566636517,-46.6848236156742,
-73.7462796297709));
#165417=CARTESIAN_POINT('Ctrl Pts',(40.1456168964303,-46.4300000199999,
-73.8124084195595));
#165418=CARTESIAN_POINT('Ctrl Pts',(40.4152609981819,-46.43000002,-73.9263755541419));
#165419=CARTESIAN_POINT('Ctrl Pts',(40.242297390109,-46.662084595994,-73.3067617342949));
#165420=CARTESIAN_POINT('Ctrl Pts',(40.3703022790479,-46.4300000199999,
-73.3807595522296));
#165421=CARTESIAN_POINT('Ctrl Pts',(40.6180555307315,-46.43000002,-73.5029053716939));
#165422=CARTESIAN_POINT('Ctrl Pts',(40.5149864073608,-46.6403532458042,
-72.8868173744763));
#165423=CARTESIAN_POINT('Ctrl Pts',(40.6428186202086,-46.43000002,-72.9643267243715));
#165424=CARTESIAN_POINT('Ctrl Pts',(40.8634877666247,-46.43000002,-73.0981265053466));
#165425=CARTESIAN_POINT('',(40.8634877666247,-46.43000002,-73.0981265053466));
#165426=CARTESIAN_POINT('Ctrl Pts',(40.8634877666247,-46.43000002,-73.0981265053466));
#165427=CARTESIAN_POINT('Ctrl Pts',(40.6610441993496,-46.43000002,-73.4320063432836));
#165428=CARTESIAN_POINT('Ctrl Pts',(40.4876415800324,-46.43000002,-73.778541855119));
#165429=CARTESIAN_POINT('Ctrl Pts',(40.3370596438484,-46.43000002,-74.1350223226475));
#165430=CARTESIAN_POINT('Ctrl Pts',(40.3050640471142,-46.43000002,-74.2107671667616));
#165431=CARTESIAN_POINT('Ctrl Pts',(40.2740989238689,-46.43000002,-74.2869610781261));
#165432=CARTESIAN_POINT('Ctrl Pts',(40.2441048562922,-46.43000002,-74.3635781632946));
#165433=CARTESIAN_POINT('Ctrl Pts',(40.0729487154701,-46.43000002,-74.8007807729435));
#165434=CARTESIAN_POINT('Ctrl Pts',(39.9334371777349,-46.43000002,-75.2543998579721));
#165435=CARTESIAN_POINT('Ctrl Pts',(39.8240030986842,-46.43000002,-75.7106064091748));
#165436=CARTESIAN_POINT('Ctrl Pts',(39.7066850117826,-46.43000002,-76.1996796511065));
#165437=CARTESIAN_POINT('Ctrl Pts',(39.6220553949041,-46.43000002,-76.69344465813));
#165438=CARTESIAN_POINT('Ctrl Pts',(39.568767518,-46.43000002,-77.1917081792567));
#165439=CARTESIAN_POINT('Ctrl Pts',(39.5226417428821,-46.43000002,-77.6230031089889));
#165440=CARTESIAN_POINT('Ctrl Pts',(39.5,-46.43000002,-78.057668743091));
#165441=CARTESIAN_POINT('Ctrl Pts',(39.5,-46.43000002,-78.4955841262963));
#165442=CARTESIAN_POINT('Origin',(40.8634877666247,-46.93000002,-73.0981265053466));
#165443=CARTESIAN_POINT('Ctrl Pts',(47.7195914591242,-46.43000002,-61.4386408691297));
#165444=CARTESIAN_POINT('Ctrl Pts',(47.4775784747622,-46.43000002,-61.3001247789676));
#165445=CARTESIAN_POINT('Ctrl Pts',(47.3503956976423,-46.6672397853475,
-61.2273317382593));
#165446=CARTESIAN_POINT('Ctrl Pts',(45.4798241095785,-46.43000002,-65.3519247333759));
#165447=CARTESIAN_POINT('Ctrl Pts',(45.2561496318399,-46.43000002,-65.1939977276857));
#165448=CARTESIAN_POINT('Ctrl Pts',(45.1164556950575,-46.6590534862623,
-65.1406137191269));
#165449=CARTESIAN_POINT('Ctrl Pts',(43.2012981267977,-46.43000002,-69.2424952559608));
#165450=CARTESIAN_POINT('Ctrl Pts',(42.9872821964954,-46.43000002,-69.082946811334));
#165451=CARTESIAN_POINT('Ctrl Pts',(42.8446532485491,-46.6501540216799,
-69.0311826437503));
#165452=CARTESIAN_POINT('Ctrl Pts',(40.8634877666247,-46.43000002,-73.0981265053466));
#165453=CARTESIAN_POINT('Ctrl Pts',(40.6428186202086,-46.43000002,-72.9643267243714));
#165454=CARTESIAN_POINT('Ctrl Pts',(40.5149864073608,-46.6403532458042,
-72.8868173744763));
#165455=CARTESIAN_POINT('',(47.7195914591242,-46.43000002,-61.4386408691297));
#165456=CARTESIAN_POINT('Ctrl Pts',(47.7195914591242,-46.43000002,-61.4386408691297));
#165457=CARTESIAN_POINT('Ctrl Pts',(45.4798130845491,-46.43000002,-65.351943995909));
#165458=CARTESIAN_POINT('Ctrl Pts',(43.2013098945494,-46.43000002,-69.2424758480089));
#165459=CARTESIAN_POINT('Ctrl Pts',(40.8634877666247,-46.43000002,-73.0981265053466));
#165460=CARTESIAN_POINT('Origin',(47.7195914591242,-46.93000002,-61.4386408691297));
#165461=CARTESIAN_POINT('Ctrl Pts',(47.3503956976423,-46.6672397853475,
-61.2273317382593));
#165462=CARTESIAN_POINT('Ctrl Pts',(47.4775784747621,-46.4300000199999,
-61.3001247789676));
#165463=CARTESIAN_POINT('Ctrl Pts',(47.7195914591242,-46.43000002,-61.4386408691297));
#165464=CARTESIAN_POINT('Ctrl Pts',(47.4408676817955,-46.6931677917013,
-61.0370194599865));
#165465=CARTESIAN_POINT('Ctrl Pts',(47.5485238823607,-46.43000002,-61.1353180501949));
#165466=CARTESIAN_POINT('Ctrl Pts',(47.7740598678193,-46.43000002,-61.3434749301835));
#165467=CARTESIAN_POINT('Ctrl Pts',(47.5839744124439,-46.7341093359256,
-60.8908220076151));
#165468=CARTESIAN_POINT('Ctrl Pts',(47.6638566779936,-46.43000002,-60.997955986762));
#165469=CARTESIAN_POINT('Ctrl Pts',(47.8601584717208,-46.43000002,-61.2703860128396));
#165470=CARTESIAN_POINT('Ctrl Pts',(47.9099463828816,-46.8268793795224,
-60.6975716107228));
#165471=CARTESIAN_POINT('Ctrl Pts',(47.9370084437089,-46.4300000199999,
-60.7796218648572));
#165472=CARTESIAN_POINT('Ctrl Pts',(48.0559929527306,-46.43000002,-61.1737607963294));
#165473=CARTESIAN_POINT('Ctrl Pts',(48.0917170178641,-46.8783971335546,
-60.64995));
#165474=CARTESIAN_POINT('Ctrl Pts',(48.1007647709628,-46.43000002,-60.6990016989097));
#165475=CARTESIAN_POINT('Ctrl Pts',(48.1650685977726,-46.43000002,-61.1499500105546));
#165476=CARTESIAN_POINT('Ctrl Pts',(48.2747189347426,-46.93000002,-60.64995));
#165477=CARTESIAN_POINT('Ctrl Pts',(48.2747189347426,-46.43000002,-60.64995));
#165478=CARTESIAN_POINT('Ctrl Pts',(48.2747189347426,-46.43000002,-61.14995));
#165479=CARTESIAN_POINT('',(48.2747189347426,-46.43000002,-61.14995));
#165480=CARTESIAN_POINT('Ctrl Pts',(48.2747189347426,-46.43000002,-61.14995));
#165481=CARTESIAN_POINT('Ctrl Pts',(48.2086234136051,-46.43000002,-61.14995));
#165482=CARTESIAN_POINT('Ctrl Pts',(48.1427915915172,-46.43000002,-61.1585974051143));
#165483=CARTESIAN_POINT('Ctrl Pts',(48.0794858636046,-46.43000002,-61.1760262255644));
#165484=CARTESIAN_POINT('Ctrl Pts',(48.0376978539717,-46.43000002,-61.1875309620373));
#165485=CARTESIAN_POINT('Ctrl Pts',(47.9970101587091,-46.43000002,-61.2028630486499));
#165486=CARTESIAN_POINT('Ctrl Pts',(47.9580757097656,-46.43000002,-61.2220733995985));
#165487=CARTESIAN_POINT('Ctrl Pts',(47.9230818282114,-46.43000002,-61.2393394650997));
#165488=CARTESIAN_POINT('Ctrl Pts',(47.8896549296877,-46.43000002,-61.259737076485));
#165489=CARTESIAN_POINT('Ctrl Pts',(47.8586276391544,-46.43000002,-61.2831656716458));
#165490=CARTESIAN_POINT('Ctrl Pts',(47.8304660966178,-46.43000002,-61.3044303508315));
#165491=CARTESIAN_POINT('Ctrl Pts',(47.804280240527,-46.43000002,-61.328192714375));
#165492=CARTESIAN_POINT('Ctrl Pts',(47.7807177502453,-46.43000002,-61.3544087872415));
#165493=CARTESIAN_POINT('Ctrl Pts',(47.7576005025356,-46.43000002,-61.3801294747914));
#165494=CARTESIAN_POINT('Ctrl Pts',(47.7370072711931,-46.43000002,-61.4082122550318));
#165495=CARTESIAN_POINT('Ctrl Pts',(47.7195914591242,-46.43000002,-61.4386408691297));
#165496=CARTESIAN_POINT('',(48.2747189347426,-46.93000002,-60.64995));
#165497=CARTESIAN_POINT('Origin',(48.2747189347426,-46.93000002,-61.14995));
#165498=CARTESIAN_POINT('Ctrl Pts',(47.3503956976423,-46.6672397853475,
-61.2273317382593));
#165499=CARTESIAN_POINT('Ctrl Pts',(47.3649754155722,-46.6714181287613,
-61.1966625829204));
#165500=CARTESIAN_POINT('Ctrl Pts',(47.381438058307,-46.6761016674855,-61.166101816227));
#165501=CARTESIAN_POINT('Ctrl Pts',(47.399867274259,-46.681341395581,-61.135942748396));
#165502=CARTESIAN_POINT('Ctrl Pts',(47.4051456277002,-46.6828421179609,
-61.1273048215368));
#165503=CARTESIAN_POINT('Ctrl Pts',(47.4105849912208,-46.6843883931268,
-61.1186998973957));
#165504=CARTESIAN_POINT('Ctrl Pts',(47.4161865603661,-46.6859812459015,
-61.1101349958363));
#165505=CARTESIAN_POINT('Ctrl Pts',(47.4287662019821,-46.6895583716198,
-61.0909004939857));
#165506=CARTESIAN_POINT('Ctrl Pts',(47.4421651842185,-46.6933699882567,
-61.0718670663287));
#165507=CARTESIAN_POINT('Ctrl Pts',(47.456397415961,-46.6974246653117,-61.0531100816564));
#165508=CARTESIAN_POINT('Ctrl Pts',(47.4706296477036,-46.7014793423668,
-61.0343530969841));
#165509=CARTESIAN_POINT('Ctrl Pts',(47.4856949747266,-46.7057769703188,
-61.0158724995589));
#165510=CARTESIAN_POINT('Ctrl Pts',(47.5016056905473,-46.710324966154,-60.9977415259233));
#165511=CARTESIAN_POINT('Ctrl Pts',(47.5239116638849,-46.7167010132775,
-60.9723228697762));
#165512=CARTESIAN_POINT('Ctrl Pts',(47.5478688873049,-46.7235628876405,
-60.9476070723277));
#165513=CARTESIAN_POINT('Ctrl Pts',(47.5734743527693,-46.730899683852,-60.9238278542592));
#165514=CARTESIAN_POINT('Ctrl Pts',(47.5843973344877,-46.7340294723341,
-60.9136839275807));
#165515=CARTESIAN_POINT('Ctrl Pts',(47.5956197393021,-46.7372455183854,
-60.9037107396086));
#165516=CARTESIAN_POINT('Ctrl Pts',(47.6071388613982,-46.7405461742288,
-60.893927797046));
#165517=CARTESIAN_POINT('Ctrl Pts',(47.6263998861775,-46.7460651724177,
-60.8775698231016));
#165518=CARTESIAN_POINT('Ctrl Pts',(47.6464923548891,-46.7518206541896,
-60.8617425255592));
#165519=CARTESIAN_POINT('Ctrl Pts',(47.6674021178734,-46.7578004809242,
-60.8465384000143));
#165520=CARTESIAN_POINT('Ctrl Pts',(47.6778569993656,-46.7607903942915,
-60.8389363372419));
#165521=CARTESIAN_POINT('Ctrl Pts',(47.6885162039648,-46.7638363936609,
-60.8314900530784));
#165522=CARTESIAN_POINT('Ctrl Pts',(47.6993772512914,-46.7669364419737,
-60.8242117420372));
#165523=CARTESIAN_POINT('Ctrl Pts',(47.7048077749548,-46.7684864661302,
-60.8205725865165));
#165524=CARTESIAN_POINT('Ctrl Pts',(47.7102887588547,-46.770050002197,-60.8169754248191));
#165525=CARTESIAN_POINT('Ctrl Pts',(47.7158198685113,-46.7716267778854,
-60.813421808391));
#165526=CARTESIAN_POINT('Ctrl Pts',(47.7193727027062,-46.7726395986269,
-60.8111391904815));
#165527=CARTESIAN_POINT('Ctrl Pts',(47.7234224734296,-46.7737934320202,
-60.8085741529328));
#165528=CARTESIAN_POINT('Ctrl Pts',(47.7270524255314,-46.7748272671279,
-60.8063084769865));
#165529=CARTESIAN_POINT('Ctrl Pts',(47.7290736414891,-46.7754029232134,
-60.8050469120267));
#165530=CARTESIAN_POINT('Ctrl Pts',(47.7309642340686,-46.7759412474452,
-60.8038771214381));
#165531=CARTESIAN_POINT('Ctrl Pts',(47.732563241915,-46.7763964389912,-60.8028931958203));
#165532=CARTESIAN_POINT('Ctrl Pts',(47.7372961730498,-46.7777437683652,
-60.7999808572715));
#165533=CARTESIAN_POINT('Ctrl Pts',(47.7420952026095,-46.7791092300362,
-60.7970812943398));
#165534=CARTESIAN_POINT('Ctrl Pts',(47.7469605871675,-46.7804929909258,
-60.7941971932464));
#165535=CARTESIAN_POINT('Ctrl Pts',(47.772543208461,-46.7877689277767,-60.7790323352242));
#165536=CARTESIAN_POINT('Ctrl Pts',(47.7999356062372,-46.7955435956083,
-60.7642777177594));
#165537=CARTESIAN_POINT('Ctrl Pts',(47.8292061473077,-46.8038519743165,
-60.7503187372695));
#165538=CARTESIAN_POINT('Ctrl Pts',(47.8364355740346,-46.8059040311933,
-60.7468710583765));
#165539=CARTESIAN_POINT('Ctrl Pts',(47.8437794265727,-46.8079886144811,
-60.7434721114416));
#165540=CARTESIAN_POINT('Ctrl Pts',(47.8512384246683,-46.8101061839473,
-60.740128093106));
#165541=CARTESIAN_POINT('Ctrl Pts',(47.8729397082559,-46.8162670617104,
-60.730398972748));
#165542=CARTESIAN_POINT('Ctrl Pts',(47.8956133919344,-46.8227056078164,
-60.7211360160641));
#165543=CARTESIAN_POINT('Ctrl Pts',(47.9192598675699,-46.8294193228067,
-60.7125029350349));
#165544=CARTESIAN_POINT('Ctrl Pts',(47.9310831053876,-46.8327761803018,
-60.7081863945204));
#165545=CARTESIAN_POINT('Ctrl Pts',(47.9431492874975,-46.8362016470855,
-60.7040274877552));
#165546=CARTESIAN_POINT('Ctrl Pts',(47.9554568133423,-46.8396942255108,
-60.7000475267255));
#165547=CARTESIAN_POINT('Ctrl Pts',(47.9616105762647,-46.8414405147234,
-60.6980575462106));
#165548=CARTESIAN_POINT('Ctrl Pts',(47.9678246742073,-46.8432035812128,
-60.6961123029493));
#165549=CARTESIAN_POINT('Ctrl Pts',(47.9740987753576,-46.8449831434372,
-60.6942145099447));
#165550=CARTESIAN_POINT('Ctrl Pts',(47.9772358259328,-46.8458729245494,
-60.6932656134423));
#165551=CARTESIAN_POINT('Ctrl Pts',(47.980387877244,-46.8467668295495,-60.6923285794147));
#165552=CARTESIAN_POINT('Ctrl Pts',(47.9835548832028,-46.8476648199627,
-60.6914037480275));
#165553=CARTESIAN_POINT('Ctrl Pts',(47.9859651476109,-46.8483482396846,
-60.6906999008591));
#165554=CARTESIAN_POINT('Ctrl Pts',(47.9892214896772,-46.8492713977441,
-60.6897640113346));
#165555=CARTESIAN_POINT('Ctrl Pts',(47.991412150968,-46.8498923749228,-60.6891431809423));
#165556=CARTESIAN_POINT('Ctrl Pts',(47.992099944563,-46.8500873407662,-60.6889482611849));
#165557=CARTESIAN_POINT('Ctrl Pts',(47.9926825870611,-46.8502524924943,
-60.6887839277128));
#165558=CARTESIAN_POINT('Ctrl Pts',(47.9931007164342,-46.8503710071843,
-60.6886662023885));
#165559=CARTESIAN_POINT('Ctrl Pts',(48.0053033073781,-46.8538297124931,
-60.6852305337442));
#165560=CARTESIAN_POINT('Ctrl Pts',(48.0192692831386,-46.8577875919822,
-60.6815376280838));
#165561=CARTESIAN_POINT('Ctrl Pts',(48.0350282325568,-46.8622516984632,
-60.6778086356672));
#165562=CARTESIAN_POINT('Ctrl Pts',(48.0507543703039,-46.8667065102387,
-60.6740874073769));
#165563=CARTESIAN_POINT('Ctrl Pts',(48.0682665960331,-46.871665608229,-60.6703303471326));
#165564=CARTESIAN_POINT('Ctrl Pts',(48.0875881985635,-46.8771339372435,
-60.6668083564069));
#165565=CARTESIAN_POINT('Ctrl Pts',(48.1067263400268,-46.8825503437803,
-60.6633198074299));
#165566=CARTESIAN_POINT('Ctrl Pts',(48.1276403019889,-46.8884665410566,
-60.6600620547269));
#165567=CARTESIAN_POINT('Ctrl Pts',(48.1503376798541,-46.8948827095381,
-60.6573464342638));
#165568=CARTESIAN_POINT('Ctrl Pts',(48.17240731422,-46.9011214254487,-60.6547059199695));
#165569=CARTESIAN_POINT('Ctrl Pts',(48.1961636602219,-46.9078330051241,
-60.6525782551135));
#165570=CARTESIAN_POINT('Ctrl Pts',(48.2215905577363,-46.9150106839736,
-60.6512917365203));
#165571=CARTESIAN_POINT('Ctrl Pts',(48.238560647475,-46.91980111718,-60.6504331049879));
#165572=CARTESIAN_POINT('Ctrl Pts',(48.2562743795194,-46.9247990237211,
-60.64995));
#165573=CARTESIAN_POINT('Ctrl Pts',(48.2747189347426,-46.93000002,-60.64995));
#165574=CARTESIAN_POINT('Origin',(-83.2809572255632,-46.9300000199999,-61.14995));
#165575=CARTESIAN_POINT('',(51.1565772669927,-46.43000002,-61.14995));
#165576=CARTESIAN_POINT('',(-83.2809572255632,-46.4300000199999,-61.14995));
#165577=CARTESIAN_POINT('',(51.1565772669927,-46.93000002,-60.64995));
#165578=CARTESIAN_POINT('Origin',(51.1565772669927,-46.93000002,-61.14995));
#165579=CARTESIAN_POINT('',(-1.41965171211599E-14,-46.93000002,-60.64995));
#165580=CARTESIAN_POINT('Origin',(0.,-12.9675000200281,-61.64995));
#165581=CARTESIAN_POINT('',(43.7578534463097,-52.58000002,-60.64995));
#165582=CARTESIAN_POINT('Origin',(0.,-12.9675000200281,-60.64995));
#165583=CARTESIAN_POINT('Ctrl Pts',(43.7578534463096,-52.58000002,-60.64995));
#165584=CARTESIAN_POINT('Ctrl Pts',(43.7326047098007,-52.5718933448815,
-60.64995));
#165585=CARTESIAN_POINT('Ctrl Pts',(43.7087430193938,-52.5642265504434,
-60.6508231664889));
#165586=CARTESIAN_POINT('Ctrl Pts',(43.6862857190865,-52.5570071197507,
-60.6522980719393));
#165587=CARTESIAN_POINT('Ctrl Pts',(43.6788113190536,-52.5546042969595,
-60.6527889605678));
#165588=CARTESIAN_POINT('Ctrl Pts',(43.6714922008008,-52.5522509345212,
-60.6533468213481));
#165589=CARTESIAN_POINT('Ctrl Pts',(43.6643282149358,-52.5499470452909,
-60.6539625815365));
#165590=CARTESIAN_POINT('Ctrl Pts',(43.6417273860358,-52.5426787721148,
-60.6559051720056));
#165591=CARTESIAN_POINT('Ctrl Pts',(43.6206746206964,-52.5359042274634,
-60.658421247948));
#165592=CARTESIAN_POINT('Ctrl Pts',(43.6011861995931,-52.5296303175985,
-60.66124704236));
#165593=CARTESIAN_POINT('Ctrl Pts',(43.5812552623538,-52.523213948458,-60.6641370010067));
#165594=CARTESIAN_POINT('Ctrl Pts',(43.5629639926385,-52.5173223267036,
-60.6673497529415));
#165595=CARTESIAN_POINT('Ctrl Pts',(43.5462866787648,-52.5119486088649,
-60.6706467221525));
#165596=CARTESIAN_POINT('Ctrl Pts',(43.5285676330368,-52.5062392270762,
-60.6741496332721));
#165597=CARTESIAN_POINT('Ctrl Pts',(43.5126732014012,-52.5011153502927,
-60.6777467267745));
#165598=CARTESIAN_POINT('Ctrl Pts',(43.4985738697311,-52.496568816543,-60.681200460083));
#165599=CARTESIAN_POINT('Ctrl Pts',(43.493624271658,-52.4949727469411,-60.6824128999439));
#165600=CARTESIAN_POINT('Ctrl Pts',(43.4888958518418,-52.4934478097891,
-60.6836081329837));
#165601=CARTESIAN_POINT('Ctrl Pts',(43.4843871673709,-52.4919935882829,
-60.6847773996288));
#165602=CARTESIAN_POINT('Ctrl Pts',(43.4825117041136,-52.4913886803502,
-60.6852637757869));
#165603=CARTESIAN_POINT('Ctrl Pts',(43.480674260163,-52.490796007527,-60.6857456694553));
#165604=CARTESIAN_POINT('Ctrl Pts',(43.478874708603,-52.4902161677162,-60.6862223751517));
#165605=CARTESIAN_POINT('Ctrl Pts',(43.4774063456389,-52.4897430413429,
-60.686611348163));
#165606=CARTESIAN_POINT('Ctrl Pts',(43.4769880700405,-52.4896084617891,
-60.6867221277077));
#165607=CARTESIAN_POINT('Ctrl Pts',(43.4751110601863,-52.4890030432867,
-60.6872267061947));
#165608=CARTESIAN_POINT('Ctrl Pts',(43.4746877014711,-52.48886649142,-60.687340513642));
#165609=CARTESIAN_POINT('Ctrl Pts',(43.4741901615202,-52.4887059950551,
-60.6874745159787));
#165610=CARTESIAN_POINT('Ctrl Pts',(43.4735897327294,-52.4885122903053,
-60.6876368692356));
#165611=CARTESIAN_POINT('Ctrl Pts',(43.440872946168,-52.4779575050367,-60.6964833418455));
#165612=CARTESIAN_POINT('Ctrl Pts',(43.4096715539944,-52.4678833667465,
-60.7065709859225));
#165613=CARTESIAN_POINT('Ctrl Pts',(43.3800156571783,-52.4583018043552,
-60.717578197336));
#165614=CARTESIAN_POINT('Ctrl Pts',(43.3623552478449,-52.4525958796639,
-60.724133111537));
#165615=CARTESIAN_POINT('Ctrl Pts',(43.3452419651281,-52.4470643237979,
-60.7310145708574));
#165616=CARTESIAN_POINT('Ctrl Pts',(43.328674854676,-52.4417072470008,-60.7381585903407));
#165617=CARTESIAN_POINT('Ctrl Pts',(43.3085530794791,-52.4352007475521,
-60.7468354416517));
#165618=CARTESIAN_POINT('Ctrl Pts',(43.2892379670008,-52.428951803686,-60.7558991768847));
#165619=CARTESIAN_POINT('Ctrl Pts',(43.270721116452,-52.422958340144,-60.7652397187937));
#165620=CARTESIAN_POINT('Ctrl Pts',(43.2585405932486,-52.4190157948634,
-60.7713839973336));
#165621=CARTESIAN_POINT('Ctrl Pts',(43.2467055435055,-52.4151838158481,
-60.7776480399122));
#165622=CARTESIAN_POINT('Ctrl Pts',(43.2352112538791,-52.4114610468223,
-60.7840021349292));
#165623=CARTESIAN_POINT('Ctrl Pts',(43.2322460380483,-52.4105006731057,
-60.7856413195806));
#165624=CARTESIAN_POINT('Ctrl Pts',(43.2293030096678,-52.4095474084892,
-60.7872867762851));
#165625=CARTESIAN_POINT('Ctrl Pts',(43.2263834511929,-52.4086016712105,
-60.7889372301596));
#165626=CARTESIAN_POINT('Ctrl Pts',(43.224616894102,-52.408029427527,-60.7899358815037));
#165627=CARTESIAN_POINT('Ctrl Pts',(43.2228583502841,-52.4074597533364,
-60.7909367527273));
#165628=CARTESIAN_POINT('Ctrl Pts',(43.2211081357598,-52.4068927518434,
-60.7919395425494));
#165629=CARTESIAN_POINT('Ctrl Pts',(43.218074199461,-52.4059098743805,-60.793677843997));
#165630=CARTESIAN_POINT('Ctrl Pts',(43.2155965839684,-52.4051071765678,
-60.7951131541398));
#165631=CARTESIAN_POINT('Ctrl Pts',(43.2126453552502,-52.4041510156181,
-60.7968407012197));
#165632=CARTESIAN_POINT('Ctrl Pts',(43.2110245994186,-52.4036259111334,
-60.7977894355509));
#165633=CARTESIAN_POINT('Ctrl Pts',(43.2092611714391,-52.4030545742235,
-60.7988269575869));
#165634=CARTESIAN_POINT('Ctrl Pts',(43.2071863268825,-52.4023823129085,
-60.8000583398207));
#165635=CARTESIAN_POINT('Ctrl Pts',(43.1791498868442,-52.393298348528,-60.8166974533641));
#165636=CARTESIAN_POINT('Ctrl Pts',(43.1522144188923,-52.3845643830934,
-60.8344485377384));
#165637=CARTESIAN_POINT('Ctrl Pts',(43.1264895714976,-52.3762177436116,
-60.8531177508924));
#165638=CARTESIAN_POINT('Ctrl Pts',(43.0995702971012,-52.3674835624112,
-60.8726537918239));
#165639=CARTESIAN_POINT('Ctrl Pts',(43.0739765262997,-52.359173462109,-60.8931951091248));
#165640=CARTESIAN_POINT('Ctrl Pts',(43.0497792324109,-52.3513121589382,
-60.9145307982532));
#165641=CARTESIAN_POINT('Ctrl Pts',(43.0298661553644,-52.3448427274206,
-60.9320889278279));
#165642=CARTESIAN_POINT('Ctrl Pts',(43.0108976759893,-52.338676858853,-60.9501852458894));
#165643=CARTESIAN_POINT('Ctrl Pts',(42.9928889905782,-52.3328202776169,
-60.9687080860286));
#165644=CARTESIAN_POINT('Ctrl Pts',(42.9682605971059,-52.3248109097041,
-60.9940396293788));
#165645=CARTESIAN_POINT('Ctrl Pts',(42.9455081131276,-52.3174064822144,
-61.0199852010191));
#165646=CARTESIAN_POINT('Ctrl Pts',(42.9245492686285,-52.3105824389046,
-61.0464447313357));
#165647=CARTESIAN_POINT('Ctrl Pts',(42.9014578882856,-52.3030640578437,
-61.0755964853009));
#165648=CARTESIAN_POINT('Ctrl Pts',(42.8805436006627,-52.2962501412606,
-61.1053719350892));
#165649=CARTESIAN_POINT('Ctrl Pts',(42.8616512181442,-52.2900924335603,
-61.1355876054117));
#165650=CARTESIAN_POINT('Ctrl Pts',(42.8427588356257,-52.2839347258599,
-61.1658032757343));
#165651=CARTESIAN_POINT('Ctrl Pts',(42.8258875244576,-52.2784329474316,
-61.1964582058417));
#165652=CARTESIAN_POINT('Ctrl Pts',(42.8108476403352,-52.2735270043159,
-61.2273317382593));
#165653=CARTESIAN_POINT('Origin',(57.,-53.58000002,-174.34995));
#165654=CARTESIAN_POINT('',(57.,-53.08000002,-176.84995));
#165655=CARTESIAN_POINT('Origin',(57.,-53.58000002,-176.84995));
#165656=CARTESIAN_POINT('',(59.5,-53.08000002,-174.34995));
#165657=CARTESIAN_POINT('Origin',(57.,-53.08000002,-174.34995));
#165658=CARTESIAN_POINT('Origin',(59.5,-53.58000002,-174.34995));
#165659=CARTESIAN_POINT('Origin',(59.5,-53.58000002,-55.2499500000008));
#165660=CARTESIAN_POINT('',(59.5,-53.08000002,-58.24995));
#165661=CARTESIAN_POINT('',(59.5,-53.08000002,-174.34995));
#165662=CARTESIAN_POINT('Origin',(59.5,-53.58000002,-58.24995));
#165663=CARTESIAN_POINT('Origin',(-1.65582490824295E-14,-52.58000002,-61.14995));
#165664=CARTESIAN_POINT('',(50.6622663180714,-52.58000002,-60.64995));
#165665=CARTESIAN_POINT('',(50.6622663180714,-53.08000002,-61.14995));
#165666=CARTESIAN_POINT('Origin',(50.6622663180714,-52.58000002,-61.14995));
#165667=CARTESIAN_POINT('',(43.7578534463097,-53.08000002,-61.14995));
#165668=CARTESIAN_POINT('',(-83.2809572255632,-53.0800000199999,-61.14995));
#165669=CARTESIAN_POINT('Origin',(43.7578534463097,-52.58000002,-61.14995));
#165670=CARTESIAN_POINT('',(-1.65582490824295E-14,-52.58000002,-60.64995));
#165671=CARTESIAN_POINT('Ctrl Pts',(43.7578534463097,-52.58000002,-60.64995));
#165672=CARTESIAN_POINT('Ctrl Pts',(43.7578534463096,-53.0800000199999,
-60.64995));
#165673=CARTESIAN_POINT('Ctrl Pts',(43.7578534463097,-53.08000002,-61.14995));
#165674=CARTESIAN_POINT('Ctrl Pts',(43.5763740160895,-52.5217319642193,
-60.64995));
#165675=CARTESIAN_POINT('Ctrl Pts',(43.5651337625656,-53.08000002,-60.5880729855648));
#165676=CARTESIAN_POINT('Ctrl Pts',(43.6407450400032,-53.08000002,-61.1499500212049));
#165677=CARTESIAN_POINT('Ctrl Pts',(43.3921532801741,-52.4622997588847,
-60.6952259861921));
#165678=CARTESIAN_POINT('Ctrl Pts',(43.3529851647999,-53.0800000199999,
-60.5541186415154));
#165679=CARTESIAN_POINT('Ctrl Pts',(43.5216142225441,-53.08000002,-61.1725879738646));
#165680=CARTESIAN_POINT('Ctrl Pts',(43.1434985367023,-52.3817526273734,
-60.8357928521433));
#165681=CARTESIAN_POINT('Ctrl Pts',(43.0017618884342,-53.08000002,-60.5701748148313));
#165682=CARTESIAN_POINT('Ctrl Pts',(43.3605400154948,-53.08000002,-61.2428714356874));
#165683=CARTESIAN_POINT('Ctrl Pts',(43.0639517713831,-52.3559271119108,
-60.8956186757958));
#165684=CARTESIAN_POINT('Ctrl Pts',(42.8669014498658,-53.0800000199996,
-60.5905012094869));
#165685=CARTESIAN_POINT('Ctrl Pts',(43.3089610591665,-53.08000002,-61.2727843293231));
#165686=CARTESIAN_POINT('Ctrl Pts',(42.9218280041301,-52.3097083637374,
-61.0417997602761));
#165687=CARTESIAN_POINT('Ctrl Pts',(42.577778492926,-53.0800000200004,-60.6851892310921));
#165688=CARTESIAN_POINT('Ctrl Pts',(43.2167397054761,-53.08000002,-61.3458748887128));
#165689=CARTESIAN_POINT('Ctrl Pts',(42.8599235980017,-52.2895352828276,
-61.126589843371));
#165690=CARTESIAN_POINT('Ctrl Pts',(42.4244093202802,-53.0800000199984,
-60.7623557509217));
#165691=CARTESIAN_POINT('Ctrl Pts',(43.1765485703954,-53.08000002,-61.3882486178711));
#165692=CARTESIAN_POINT('Ctrl Pts',(42.8108476403352,-52.2735270043159,
-61.2273317382593));
#165693=CARTESIAN_POINT('Ctrl Pts',(42.2822348911901,-53.08000002,-60.8926985768511));
#165694=CARTESIAN_POINT('Ctrl Pts',(43.1446480925044,-53.08000002,-61.4386408691297));
#165695=CARTESIAN_POINT('',(43.1446480925044,-53.08000002,-61.4386408691297));
#165696=CARTESIAN_POINT('Ctrl Pts',(43.1446480925044,-53.08000002,-61.4386408691297));
#165697=CARTESIAN_POINT('Ctrl Pts',(43.1765609373872,-53.08000002,-61.3882288400421));
#165698=CARTESIAN_POINT('Ctrl Pts',(43.2167516388878,-53.08000002,-61.3458652617053));
#165699=CARTESIAN_POINT('Ctrl Pts',(43.2628503174202,-53.08000002,-61.3093295271296));
#165700=CARTESIAN_POINT('Ctrl Pts',(43.3089610210815,-53.08000002,-61.2727842619789));
#165701=CARTESIAN_POINT('Ctrl Pts',(43.3605330051287,-53.08000002,-61.2428744748387));
#165702=CARTESIAN_POINT('Ctrl Pts',(43.414231413078,-53.08000002,-61.2194436041558));
#165703=CARTESIAN_POINT('Ctrl Pts',(43.4456262415641,-53.08000002,-61.205744721927));
#165704=CARTESIAN_POINT('Ctrl Pts',(43.477917759742,-53.08000002,-61.1941576093824));
#165705=CARTESIAN_POINT('Ctrl Pts',(43.5108494925037,-53.08000002,-61.1845858141908));
#165706=CARTESIAN_POINT('Ctrl Pts',(43.5447058226299,-53.08000002,-61.1747452795231));
#165707=CARTESIAN_POINT('Ctrl Pts',(43.5792402145377,-53.08000002,-61.1670347524206));
#165708=CARTESIAN_POINT('Ctrl Pts',(43.6141927055654,-53.08000002,-61.1614020099222));
#165709=CARTESIAN_POINT('Ctrl Pts',(43.648904945801,-53.08000002,-61.1558079848602));
#165710=CARTESIAN_POINT('Ctrl Pts',(43.6840310643504,-53.08000002,-61.1522634649487));
#165711=CARTESIAN_POINT('Ctrl Pts',(43.719312634701,-53.08000002,-61.1507670586125));
#165712=CARTESIAN_POINT('Ctrl Pts',(43.7321435462895,-53.08000002,-61.1502228578524));
#165713=CARTESIAN_POINT('Ctrl Pts',(43.7449948697402,-53.08000002,-61.14995));
#165714=CARTESIAN_POINT('Ctrl Pts',(43.7578534463097,-53.08000002,-61.14995));
#165715=CARTESIAN_POINT('Origin',(43.1446480925044,-52.58000002,-61.4386408691297));
#165716=CARTESIAN_POINT('Ctrl Pts',(41.0647116264215,-53.08000002,-64.6870793282409));
#165717=CARTESIAN_POINT('Ctrl Pts',(40.1851006581956,-53.08000002,-64.1171767326871));
#165718=CARTESIAN_POINT('Ctrl Pts',(40.7385684738022,-52.2653905871942,
-64.4757701973706));
#165719=CARTESIAN_POINT('Ctrl Pts',(41.7638515954828,-53.08000002,-63.6079981134234));
#165720=CARTESIAN_POINT('Ctrl Pts',(40.8849497704992,-53.0800000200001,
-63.0545757298723));
#165721=CARTESIAN_POINT('Ctrl Pts',(41.4350320326697,-52.2681651349568,
-63.3966889540178));
#165722=CARTESIAN_POINT('Ctrl Pts',(42.4569204735311,-53.08000002,-62.5250292766735));
#165723=CARTESIAN_POINT('Ctrl Pts',(41.584202382955,-53.08000002,-61.9790488279059));
#165724=CARTESIAN_POINT('Ctrl Pts',(42.125553749702,-52.2708762823431,-62.3137201227713));
#165725=CARTESIAN_POINT('Ctrl Pts',(43.1446480925044,-53.08000002,-61.4386408691297));
#165726=CARTESIAN_POINT('Ctrl Pts',(42.2822348911901,-53.08000002,-60.8926985768511));
#165727=CARTESIAN_POINT('Ctrl Pts',(42.8108476403353,-52.2735270043159,
-61.2273317382593));
#165728=CARTESIAN_POINT('',(41.0647116264214,-53.08000002,-64.687079328241));
#165729=CARTESIAN_POINT('Ctrl Pts',(41.0647116264215,-53.08000002,-64.6870793282409));
#165730=CARTESIAN_POINT('Ctrl Pts',(41.7638515954828,-53.08000002,-63.6079981134234));
#165731=CARTESIAN_POINT('Ctrl Pts',(42.4569204735311,-53.08000002,-62.5250292766735));
#165732=CARTESIAN_POINT('Ctrl Pts',(43.1446480925044,-53.08000002,-61.4386408691297));
#165733=CARTESIAN_POINT('Origin',(41.0647116264214,-52.58000002,-64.687079328241));
#165734=CARTESIAN_POINT('Ctrl Pts',(40.7385684738017,-52.2653905871946,
-64.4757701973708));
#165735=CARTESIAN_POINT('Ctrl Pts',(40.1851006581961,-53.08000002,-64.117176732689));
#165736=CARTESIAN_POINT('Ctrl Pts',(41.0647116264215,-53.08000002,-64.6870793282409));
#165737=CARTESIAN_POINT('Ctrl Pts',(40.4169533529343,-52.2886158160728,
-64.9375850416414));
#165738=CARTESIAN_POINT('Ctrl Pts',(39.9350648871364,-53.08000002,-64.6424135397739));
#165739=CARTESIAN_POINT('Ctrl Pts',(40.7752331041961,-53.08000002,-65.1338723319862));
#165740=CARTESIAN_POINT('Ctrl Pts',(40.1571532317284,-52.3131117923589,
-65.4245685478069));
#165741=CARTESIAN_POINT('Ctrl Pts',(39.7292916509907,-53.0800000199999,
-65.1967116799));
#165742=CARTESIAN_POINT('Ctrl Pts',(40.5414379096314,-53.08000002,-65.6048227505322));
#165743=CARTESIAN_POINT('Ctrl Pts',(39.8302312493672,-52.3511206237746,
-66.1800801057477));
#165744=CARTESIAN_POINT('Ctrl Pts',(39.4809642231373,-53.0800000199999,
-66.0439398517176));
#165745=CARTESIAN_POINT('Ctrl Pts',(40.2472081238925,-53.08000002,-66.3353006309098));
#165746=CARTESIAN_POINT('Ctrl Pts',(39.7320550320644,-52.3640100073116,
-66.4362687474843));
#165747=CARTESIAN_POINT('Ctrl Pts',(39.4096807156913,-53.08000002,-66.3196295939567));
#165748=CARTESIAN_POINT('Ctrl Pts',(40.158849529204,-53.08000002,-66.5829654036754));
#165749=CARTESIAN_POINT('Ctrl Pts',(39.5550747922058,-52.3901835262345,
-66.9564695443705));
#165750=CARTESIAN_POINT('Ctrl Pts',(39.2851434780251,-53.0800000199999,
-66.8724334008892));
#165751=CARTESIAN_POINT('Ctrl Pts',(39.9995673126391,-53.08000002,-67.0857801567948));
#165752=CARTESIAN_POINT('Ctrl Pts',(39.4760999841222,-52.4035086843654,
-67.2212970006122));
#165753=CARTESIAN_POINT('Ctrl Pts',(39.2309126715885,-53.08000002,-67.1508200729254));
#165754=CARTESIAN_POINT('Ctrl Pts',(39.9284899861158,-53.08000002,-67.341717845364));
#165755=CARTESIAN_POINT('Ctrl Pts',(39.2683842506574,-52.4436252670713,
-68.0185730582879));
#165756=CARTESIAN_POINT('Ctrl Pts',(39.096874254798,-53.08000002,-67.9652916099918));
#165757=CARTESIAN_POINT('Ctrl Pts',(39.7415458247801,-53.08000002,-68.1121058873989));
#165758=CARTESIAN_POINT('Ctrl Pts',(39.1678647718912,-52.4706085083894,
-68.5548226317846));
#165759=CARTESIAN_POINT('Ctrl Pts',(39.0356546500978,-53.08000002,-68.5171438238431));
#165760=CARTESIAN_POINT('Ctrl Pts',(39.6510782949347,-53.08000002,-68.6301060216833));
#165761=CARTESIAN_POINT('Ctrl Pts',(39.0336224576287,-52.5249919887119,
-69.6357261726145));
#165762=CARTESIAN_POINT('Ctrl Pts',(38.9750254916822,-53.0800000199999,
-69.6153526806455));
#165763=CARTESIAN_POINT('Ctrl Pts',(39.5302602116332,-53.08000002,-69.6738635266831));
#165764=CARTESIAN_POINT('Ctrl Pts',(39.,-52.5523936264783,-70.1804078085674));
#165765=CARTESIAN_POINT('Ctrl Pts',(38.9716079589828,-53.0800000199999,
-70.1647867514408));
#165766=CARTESIAN_POINT('Ctrl Pts',(39.500000000531,-53.08000002,-70.1996476853715));
#165767=CARTESIAN_POINT('Ctrl Pts',(39.,-52.58000002,-70.7293062304687));
#165768=CARTESIAN_POINT('Ctrl Pts',(38.9999999999999,-53.08000002,-70.7293062304687));
#165769=CARTESIAN_POINT('Ctrl Pts',(39.5,-53.08000002,-70.7293062304687));
#165770=CARTESIAN_POINT('',(39.5,-53.08000002,-70.7293062304687));
#165771=CARTESIAN_POINT('Ctrl Pts',(39.5,-53.08000002,-70.7293062304687));
#165772=CARTESIAN_POINT('Ctrl Pts',(39.5,-53.08000002,-70.1996325547074));
#165773=CARTESIAN_POINT('Ctrl Pts',(39.5302602116353,-53.08000002,-69.6738635266889));
#165774=CARTESIAN_POINT('Ctrl Pts',(39.5906692531643,-53.08000002,-69.1519847741694));
#165775=CARTESIAN_POINT('Ctrl Pts',(39.6510782946932,-53.08000002,-68.6301060216499));
#165776=CARTESIAN_POINT('Ctrl Pts',(39.7415458248093,-53.08000002,-68.1121058873188));
#165777=CARTESIAN_POINT('Ctrl Pts',(39.8661752652165,-53.08000002,-67.5985138592655));
#165778=CARTESIAN_POINT('Ctrl Pts',(39.9284899854243,-53.08000002,-67.3417178452216));
#165779=CARTESIAN_POINT('Ctrl Pts',(39.9995673120589,-53.08000002,-67.0857801566515));
#165780=CARTESIAN_POINT('Ctrl Pts',(40.0792084204325,-53.08000002,-66.8343727800802));
#165781=CARTESIAN_POINT('Ctrl Pts',(40.1588495287955,-53.08000002,-66.5829654035428));
#165782=CARTESIAN_POINT('Ctrl Pts',(40.2472081235396,-53.08000002,-66.3353006307905));
#165783=CARTESIAN_POINT('Ctrl Pts',(40.3452847184367,-53.08000002,-66.0918080038346));
#165784=CARTESIAN_POINT('Ctrl Pts',(40.4725149961137,-53.08000002,-65.7759361633367));
#165785=CARTESIAN_POINT('Ctrl Pts',(40.6155606032197,-53.08000002,-65.4668542003479));
#165786=CARTESIAN_POINT('Ctrl Pts',(40.7793840759628,-53.08000002,-65.1666925984976));
#165787=CARTESIAN_POINT('Ctrl Pts',(40.868130174949,-53.08000002,-65.0040897017112));
#165788=CARTESIAN_POINT('Ctrl Pts',(40.9629743342362,-53.08000002,-64.8441048248465));
#165789=CARTESIAN_POINT('Ctrl Pts',(41.0647116264214,-53.08000002,-64.687079328241));
#165790=CARTESIAN_POINT('Origin',(39.5,-52.58000002,-70.7293062304687));
#165791=CARTESIAN_POINT('Origin',(39.5,-52.58000002,-55.2499500000008));
#165792=CARTESIAN_POINT('',(39.5,-53.08000002,-161.329336741015));
#165793=CARTESIAN_POINT('',(39.5,-53.08000002,-55.2499500000008));
#165794=CARTESIAN_POINT('Origin',(39.5,-52.58000002,-161.329336741016));
#165795=CARTESIAN_POINT('Ctrl Pts',(39.,-52.5800000200011,-161.329336741014));
#165796=CARTESIAN_POINT('Ctrl Pts',(39.0000000000011,-53.08000002,-161.329336741014));
#165797=CARTESIAN_POINT('Ctrl Pts',(39.5,-53.08000002,-161.329336741015));
#165798=CARTESIAN_POINT('Ctrl Pts',(38.999999999999,-52.5523928630554,-161.878250342061));
#165799=CARTESIAN_POINT('Ctrl Pts',(38.971607175397,-53.08000002,-161.893871800581));
#165800=CARTESIAN_POINT('Ctrl Pts',(39.5000000005568,-53.08000002,-161.859009936371));
#165801=CARTESIAN_POINT('Ctrl Pts',(39.0336246233085,-52.5250040247996,
-162.422677519451));
#165802=CARTESIAN_POINT('Ctrl Pts',(38.9750364187576,-53.08000002,-162.443018289978));
#165803=CARTESIAN_POINT('Ctrl Pts',(39.5302621607567,-53.08000002,-162.384548554576));
#165804=CARTESIAN_POINT('Ctrl Pts',(39.1676758409912,-52.4706721515367,
-163.50255544994));
#165805=CARTESIAN_POINT('Ctrl Pts',(39.0355537948544,-53.0800000199999,
-163.540173111977));
#165806=CARTESIAN_POINT('Ctrl Pts',(39.650908257113,-53.08000002,-163.427315362947));
#165807=CARTESIAN_POINT('Ctrl Pts',(39.2680076006075,-52.4437276611465,
-164.038034987594));
#165808=CARTESIAN_POINT('Ctrl Pts',(39.0966358008681,-53.08000002,-164.091177104404));
#165809=CARTESIAN_POINT('Ctrl Pts',(39.7412068397501,-53.08000002,-163.944571422167));
#165810=CARTESIAN_POINT('Ctrl Pts',(39.5441113151659,-52.3903440317307,
-165.098979928026));
#165811=CARTESIAN_POINT('Ctrl Pts',(39.2784275950098,-53.0800000199999,
-165.197323336931));
#165812=CARTESIAN_POINT('Ctrl Pts',(39.9897001844459,-53.08000002,-164.969734884811));
#165813=CARTESIAN_POINT('Ctrl Pts',(39.7204443742655,-52.3638938128861,
-165.624666922963));
#165814=CARTESIAN_POINT('Ctrl Pts',(39.4053566676027,-53.08000002,-165.756550564755));
#165815=CARTESIAN_POINT('Ctrl Pts',(40.1483999357838,-53.08000002,-165.477859388262));
#165816=CARTESIAN_POINT('Ctrl Pts',(40.1569686920085,-52.3131241972374,
-166.633827745735));
#165817=CARTESIAN_POINT('Ctrl Pts',(39.7291683816592,-53.08000002,-166.861730184891));
#165818=CARTESIAN_POINT('Ctrl Pts',(40.5412718238628,-53.08000002,-166.453581502202));
#165819=CARTESIAN_POINT('Ctrl Pts',(40.4170614047767,-52.2886080120764,
-167.121213082449));
#165820=CARTESIAN_POINT('Ctrl Pts',(39.9351413271735,-53.08000002,-167.416390015348));
#165821=CARTESIAN_POINT('Ctrl Pts',(40.7753307309704,-53.08000002,-166.924921320909));
#165822=CARTESIAN_POINT('Ctrl Pts',(40.7385684738071,-52.2653905871942,
-167.582872774143));
#165823=CARTESIAN_POINT('Ctrl Pts',(40.1851006582006,-53.08000002,-167.941466238826));
#165824=CARTESIAN_POINT('Ctrl Pts',(41.0647116264263,-53.08000002,-167.371563643272));
#165825=CARTESIAN_POINT('',(41.0647116264263,-53.08000002,-167.371563643272));
#165826=CARTESIAN_POINT('Origin',(41.0647116264263,-52.58000002,-167.371563643272));
#165827=CARTESIAN_POINT('Ctrl Pts',(41.0647116264263,-53.08000002,-167.371563643272));
#165828=CARTESIAN_POINT('Ctrl Pts',(40.873027927483,-53.08000002,-167.075711184737));
#165829=CARTESIAN_POINT('Ctrl Pts',(40.7056641754959,-53.08000002,-166.769103902006));
#165830=CARTESIAN_POINT('Ctrl Pts',(40.5574162968375,-53.08000002,-166.454043185673));
#165831=CARTESIAN_POINT('Ctrl Pts',(40.4818120706116,-53.08000002,-166.293366878611));
#165832=CARTESIAN_POINT('Ctrl Pts',(40.4111805199837,-53.08000002,-166.130491546345));
#165833=CARTESIAN_POINT('Ctrl Pts',(40.3448358791345,-53.08000002,-165.965720445509));
#165834=CARTESIAN_POINT('Ctrl Pts',(40.1483999357586,-53.08000002,-165.477859388165));
#165835=CARTESIAN_POINT('Ctrl Pts',(39.9897001835278,-53.08000002,-164.969734884954));
#165836=CARTESIAN_POINT('Ctrl Pts',(39.8654535116526,-53.08000002,-164.457153153597));
#165837=CARTESIAN_POINT('Ctrl Pts',(39.7412068397774,-53.08000002,-163.94457142224));
#165838=CARTESIAN_POINT('Ctrl Pts',(39.6509082568844,-53.08000002,-163.427315362986));
#165839=CARTESIAN_POINT('Ctrl Pts',(39.5905852088212,-53.08000002,-162.905931958774));
#165840=CARTESIAN_POINT('Ctrl Pts',(39.530262160758,-53.08000002,-162.384548554563));
#165841=CARTESIAN_POINT('Ctrl Pts',(39.4999999999991,-53.08000002,-161.85902605313));
#165842=CARTESIAN_POINT('Ctrl Pts',(39.5,-53.08000002,-161.329336741015));
#165843=CARTESIAN_POINT('Ctrl Pts',(43.2972503047852,-53.08000002,-170.861259130871));
#165844=CARTESIAN_POINT('Ctrl Pts',(42.4360603595898,-53.08000002,-171.405549026075));
#165845=CARTESIAN_POINT('Ctrl Pts',(42.9629113790828,-52.2741145284007,
-171.07256826174));
#165846=CARTESIAN_POINT('Ctrl Pts',(42.5594745131554,-53.08000002,-169.693930655453));
#165847=CARTESIAN_POINT('Ctrl Pts',(41.6869083931944,-53.0800000201158,
-170.237641125793));
#165848=CARTESIAN_POINT('Ctrl Pts',(42.2277314430405,-52.2712772274341,
-169.905239816447));
#165849=CARTESIAN_POINT('Ctrl Pts',(41.8155944388483,-53.08000002,-168.530506878352));
#165850=CARTESIAN_POINT('Ctrl Pts',(40.9363322060061,-53.08000002,-169.082082669019));
#165851=CARTESIAN_POINT('Ctrl Pts',(41.4865768015737,-52.2683704772926,
-168.741816047102));
#165852=CARTESIAN_POINT('Ctrl Pts',(41.0647116264263,-53.08000002,-167.371563643272));
#165853=CARTESIAN_POINT('Ctrl Pts',(40.1851006582006,-53.0800000199999,
-167.941466238826));
#165854=CARTESIAN_POINT('Ctrl Pts',(40.738568473807,-52.2653905871942,-167.582872774143));
#165855=CARTESIAN_POINT('',(43.2972503047852,-53.08000002,-170.861259130871));
#165856=CARTESIAN_POINT('Origin',(43.2972503047852,-52.58000002,-170.861259130871));
#165857=CARTESIAN_POINT('Ctrl Pts',(43.2972503047852,-53.08000002,-170.861259130871));
#165858=CARTESIAN_POINT('Ctrl Pts',(42.5594745131554,-53.08000002,-169.693930655453));
#165859=CARTESIAN_POINT('Ctrl Pts',(41.8155944388483,-53.08000002,-168.530506878352));
#165860=CARTESIAN_POINT('Ctrl Pts',(41.0647116264263,-53.08000002,-167.371563643272));
#165861=CARTESIAN_POINT('Ctrl Pts',(42.9629113790828,-52.2741145284007,
-171.07256826174));
#165862=CARTESIAN_POINT('Ctrl Pts',(42.4360603595898,-53.08000002,-171.405549026075));
#165863=CARTESIAN_POINT('Ctrl Pts',(43.2972503047852,-53.08000002,-170.861259130871));
#165864=CARTESIAN_POINT('Ctrl Pts',(43.0118891450524,-52.2900672717484,
-171.173154953435));
#165865=CARTESIAN_POINT('Ctrl Pts',(42.5775224401932,-53.080000020001,-171.535704796364));
#165866=CARTESIAN_POINT('Ctrl Pts',(43.3290496999002,-53.08000002,-170.911572751073));
#165867=CARTESIAN_POINT('Ctrl Pts',(43.073894673874,-52.3102438041593,-171.258275237078));
#165868=CARTESIAN_POINT('Ctrl Pts',(42.7308220084871,-53.0800000200015,
-171.613444114474));
#165869=CARTESIAN_POINT('Ctrl Pts',(43.3692611707715,-53.08000002,-170.954112611118));
#165870=CARTESIAN_POINT('Ctrl Pts',(43.2170017360461,-52.3567135560047,
-171.405295505501));
#165871=CARTESIAN_POINT('Ctrl Pts',(43.0212179754289,-53.0800000199986,
-171.708873691595));
#165872=CARTESIAN_POINT('Ctrl Pts',(43.4620142194198,-53.08000002,-171.027622760172));
#165873=CARTESIAN_POINT('Ctrl Pts',(43.2956718648015,-52.3822166623249,
-171.464307358546));
#165874=CARTESIAN_POINT('Ctrl Pts',(43.154321777956,-53.080000020001,-171.728961938884));
#165875=CARTESIAN_POINT('Ctrl Pts',(43.512966485493,-53.08000002,-171.057128671245));
#165876=CARTESIAN_POINT('Ctrl Pts',(43.4617135157955,-52.4359237144093,
-171.55811115512));
#165877=CARTESIAN_POINT('Ctrl Pts',(43.3978292274293,-53.080000019999,-171.740357884216));
#165878=CARTESIAN_POINT('Ctrl Pts',(43.6204035532382,-53.08000002,-171.104030585588));
#165879=CARTESIAN_POINT('Ctrl Pts',(43.5499633272225,-52.4644105712997,
-171.592966290451));
#165880=CARTESIAN_POINT('Ctrl Pts',(43.5113479697337,-53.080000019999,-171.733309812026));
#165881=CARTESIAN_POINT('Ctrl Pts',(43.6774556997061,-53.08000002,-171.121458138538));
#165882=CARTESIAN_POINT('Ctrl Pts',(43.7274774238083,-52.5215797867686,
-171.638576841342));
#165883=CARTESIAN_POINT('Ctrl Pts',(43.718452515944,-53.080000020001,-171.702758245039));
#165884=CARTESIAN_POINT('Ctrl Pts',(43.7921030708942,-53.08000002,-171.144263427359));
#165885=CARTESIAN_POINT('Ctrl Pts',(43.8177416070106,-52.5505863340359,
-171.64995));
#165886=CARTESIAN_POINT('Ctrl Pts',(43.8149201055142,-53.08000002,-171.680268286151));
#165887=CARTESIAN_POINT('Ctrl Pts',(43.8503459614229,-53.08000002,-171.149949987963));
#165888=CARTESIAN_POINT('Ctrl Pts',(43.9094855672884,-52.58000002,-171.64995));
#165889=CARTESIAN_POINT('Ctrl Pts',(43.9094855672884,-53.0800000199999,
-171.64995));
#165890=CARTESIAN_POINT('Ctrl Pts',(43.9094855672884,-53.08000002,-171.14995));
#165891=CARTESIAN_POINT('',(43.9094855672884,-53.08000002,-171.14995));
#165892=CARTESIAN_POINT('Origin',(43.9094855672884,-52.58000002,-171.14995));
#165893=CARTESIAN_POINT('Ctrl Pts',(43.9094855672884,-53.08000002,-171.14995));
#165894=CARTESIAN_POINT('Ctrl Pts',(43.8503415173364,-53.08000002,-171.14995));
#165895=CARTESIAN_POINT('Ctrl Pts',(43.7921001974326,-53.08000002,-171.144262868806));
#165896=CARTESIAN_POINT('Ctrl Pts',(43.7347793831646,-53.08000002,-171.132860793684));
#165897=CARTESIAN_POINT('Ctrl Pts',(43.6774556974662,-53.08000002,-171.121458147386));
#165898=CARTESIAN_POINT('Ctrl Pts',(43.6204048981063,-53.08000002,-171.104031177905));
#165899=CARTESIAN_POINT('Ctrl Pts',(43.5666850153843,-53.08000002,-171.080579637536));
#165900=CARTESIAN_POINT('Ctrl Pts',(43.5129605101707,-53.08000002,-171.057126079209));
#165901=CARTESIAN_POINT('Ctrl Pts',(43.4620141840633,-53.08000002,-171.02762282191));
#165902=CARTESIAN_POINT('Ctrl Pts',(43.4156376346715,-53.08000002,-170.990867761886));
#165903=CARTESIAN_POINT('Ctrl Pts',(43.3692713886891,-53.08000002,-170.95412086768));
#165904=CARTESIAN_POINT('Ctrl Pts',(43.3290601923967,-53.08000002,-170.911589580894));
#165905=CARTESIAN_POINT('Ctrl Pts',(43.2972503047852,-53.08000002,-170.861259130871));
#165906=CARTESIAN_POINT('Origin',(-83.2809572255632,-52.5800000199999,-171.14995));
#165907=CARTESIAN_POINT('',(49.6300753314849,-53.08000002,-171.14995));
#165908=CARTESIAN_POINT('Origin',(49.6300753314849,-52.58000002,-171.14995));
#165909=CARTESIAN_POINT('',(43.4531980731446,-53.08000002,-171.14995));
#165910=CARTESIAN_POINT('Ctrl Pts',(51.1448166902628,-53.08000002,-172.64995));
#165911=CARTESIAN_POINT('Ctrl Pts',(50.5696324866524,-53.08000002,-172.64995));
#165912=CARTESIAN_POINT('Ctrl Pts',(50.6496826558921,-52.51041346952,-172.64995));
#165913=CARTESIAN_POINT('Ctrl Pts',(51.1448166902479,-53.08000002,-172.453565067926));
#165914=CARTESIAN_POINT('Ctrl Pts',(50.5696324866503,-53.080000020002,-172.529650273729));
#165915=CARTESIAN_POINT('Ctrl Pts',(50.6496826558917,-52.5104134695225,
-172.51902671195));
#165916=CARTESIAN_POINT('Ctrl Pts',(51.1053920215496,-53.08000002,-172.257328160063));
#165917=CARTESIAN_POINT('Ctrl Pts',(50.5479627709917,-53.08000002,-172.409726298163));
#165918=CARTESIAN_POINT('Ctrl Pts',(50.6231450026166,-52.5122246214263,
-172.38820210671));
#165919=CARTESIAN_POINT('Ctrl Pts',(50.9536357182667,-53.08000002,-171.894521542842));
#165920=CARTESIAN_POINT('Ctrl Pts',(50.4615294415736,-53.08000002,-172.182182441317));
#165921=CARTESIAN_POINT('Ctrl Pts',(50.5209943367899,-52.5191962391206,
-172.14633102856));
#165922=CARTESIAN_POINT('Ctrl Pts',(50.8413637606251,-53.08000002,-171.728129909852));
#165923=CARTESIAN_POINT('Ctrl Pts',(50.3972583757626,-53.0800000199979,
-172.075215659168));
#165924=CARTESIAN_POINT('Ctrl Pts',(50.4454214941564,-52.5243539633763,
-172.035403273235));
#165925=CARTESIAN_POINT('Ctrl Pts',(50.5609546754159,-53.08000002,-171.450449746589));
#165926=CARTESIAN_POINT('Ctrl Pts',(50.2296016046087,-53.080000020002,-171.888983273332));
#165927=CARTESIAN_POINT('Ctrl Pts',(50.256671675285,-52.537235833176,-171.850283164392));
#165928=CARTESIAN_POINT('Ctrl Pts',(50.3929278167739,-53.08000002,-171.339270411997));
#165929=CARTESIAN_POINT('Ctrl Pts',(50.1270268918696,-53.0800000200001,
-171.809929875206));
#165930=CARTESIAN_POINT('Ctrl Pts',(50.1435689235997,-52.5449549130127,
-171.776163607997));
#165931=CARTESIAN_POINT('Ctrl Pts',(50.0265556908409,-53.08000002,-171.18899099047));
#165932=CARTESIAN_POINT('Ctrl Pts',(49.8942480960507,-53.08000002,-171.69520402023));
#165933=CARTESIAN_POINT('Ctrl Pts',(49.8969554005076,-52.561785887019,-171.675977326981));
#165934=CARTESIAN_POINT('Ctrl Pts',(49.8283902508599,-53.08000002,-171.149950000016));
#165935=CARTESIAN_POINT('Ctrl Pts',(49.7648572777959,-53.08000002,-171.659148653595));
#165936=CARTESIAN_POINT('Ctrl Pts',(49.7635656750098,-52.5708895200013,
-171.64995));
#165937=CARTESIAN_POINT('Ctrl Pts',(49.6300753314849,-53.08000002,-171.14995));
#165938=CARTESIAN_POINT('Ctrl Pts',(49.6300753314848,-53.0800000199999,
-171.64995));
#165939=CARTESIAN_POINT('Ctrl Pts',(49.6300753314849,-52.58000002,-171.64995));
#165940=CARTESIAN_POINT('',(51.1448166902628,-53.08000002,-172.64995));
#165941=CARTESIAN_POINT('',(50.6448166902628,-52.58000002,-172.64995));
#165942=CARTESIAN_POINT('Origin',(51.1448166902628,-52.58000002,-172.64995));
#165943=CARTESIAN_POINT('Origin',(51.1448166902628,-52.58000002,-172.64995));
#165944=CARTESIAN_POINT('Ctrl Pts',(51.1448166902628,-53.08000002,-172.64995));
#165945=CARTESIAN_POINT('Ctrl Pts',(51.1448166902479,-53.08000002,-172.453565067926));
#165946=CARTESIAN_POINT('Ctrl Pts',(51.1053920215496,-53.08000002,-172.257328160063));
#165947=CARTESIAN_POINT('Ctrl Pts',(50.9536357182667,-53.08000002,-171.894521542842));
#165948=CARTESIAN_POINT('Ctrl Pts',(50.8413637606251,-53.08000002,-171.728129909852));
#165949=CARTESIAN_POINT('Ctrl Pts',(50.5609546754159,-53.08000002,-171.450449746589));
#165950=CARTESIAN_POINT('Ctrl Pts',(50.3929278167739,-53.08000002,-171.339270411997));
#165951=CARTESIAN_POINT('Ctrl Pts',(50.0265556908409,-53.08000002,-171.18899099047));
#165952=CARTESIAN_POINT('Ctrl Pts',(49.8283902508599,-53.08000002,-171.149950000016));
#165953=CARTESIAN_POINT('Ctrl Pts',(49.6300753314849,-53.08000002,-171.14995));
#165954=CARTESIAN_POINT('Origin',(51.1448166902628,-52.58000002,-171.64995));
#165955=CARTESIAN_POINT('',(51.1448166902628,-53.08000002,-55.2499500000008));
#165956=CARTESIAN_POINT('',(50.6496826558921,-52.51041346952,-171.64995));
#165957=CARTESIAN_POINT('Origin',(60.,-53.58000002,-176.84995));
#165958=CARTESIAN_POINT('',(-83.2809572255632,-53.0800000199999,-176.84995));
#165959=CARTESIAN_POINT('Origin',(57.,-53.58000002,-58.24995));
#165960=CARTESIAN_POINT('',(57.,-53.08000002,-55.74995));
#165961=CARTESIAN_POINT('Origin',(57.,-53.08000002,-58.24995));
#165962=CARTESIAN_POINT('',(57.,-53.58000002,-55.24995));
#165963=CARTESIAN_POINT('Origin',(57.,-53.58000002,-55.74995));
#165964=CARTESIAN_POINT('Origin',(57.,-53.58000002,-58.24995));
#165965=CARTESIAN_POINT('Origin',(57.,-2.42462934179819E-14,-58.24995));
#165966=CARTESIAN_POINT('',(57.,-54.08000002,-55.24995));
#165967=CARTESIAN_POINT('',(57.,28.41999998,-55.24995));
#165968=CARTESIAN_POINT('Origin',(57.,-54.08000002,-58.24995));
#165969=CARTESIAN_POINT('Origin',(60.,-55.08000002,-171.14995));
#165970=CARTESIAN_POINT('',(45.8586217441902,-54.58000002,-171.14995));
#165971=CARTESIAN_POINT('',(45.8586217441902,-55.08000002,-171.64995));
#165972=CARTESIAN_POINT('Origin',(45.8586217441902,-55.08000002,-171.14995));
#165973=CARTESIAN_POINT('',(42.5,-55.08000002,-171.64995));
#165974=CARTESIAN_POINT('',(49.2787232447289,-54.58000002,-171.14995));
#165975=CARTESIAN_POINT('Origin',(49.2787232447289,-55.08000002,-171.14995));
#165976=CARTESIAN_POINT('',(49.3489936620801,-54.58000002,-171.14995));
#165977=CARTESIAN_POINT('Origin',(60.,-55.08000002,-171.14995));
#165978=CARTESIAN_POINT('',(43.1572831724514,-55.08000002,-171.64995));
#165979=CARTESIAN_POINT('',(42.5,-55.08000002,-171.64995));
#165980=CARTESIAN_POINT('',(43.1572831724514,-54.58000002,-171.14995));
#165981=CARTESIAN_POINT('Origin',(43.1572831724514,-55.08000002,-171.14995));
#165982=CARTESIAN_POINT('',(49.3489936620801,-54.58000002,-171.14995));
#165983=CARTESIAN_POINT('Origin',(-1.8445455022812E-14,-55.08000002,-61.14995));
#165984=CARTESIAN_POINT('',(43.1572831724516,-54.58000002,-61.14995));
#165985=CARTESIAN_POINT('',(60.,-54.58000002,-61.14995));
#165986=CARTESIAN_POINT('Origin',(43.1572831724516,-55.08000002,-61.14995));
#165987=CARTESIAN_POINT('Ctrl Pts',(43.1572831724516,-55.080148121506,-60.6499500219341));
#165988=CARTESIAN_POINT('Ctrl Pts',(43.1572831724515,-54.58000002,-60.6498018765534));
#165989=CARTESIAN_POINT('Ctrl Pts',(43.1572831724516,-54.58000002,-61.14995));
#165990=CARTESIAN_POINT('Ctrl Pts',(43.3271185292341,-54.9843723315207,
-60.6499212610322));
#165991=CARTESIAN_POINT('Ctrl Pts',(43.3143913613969,-54.58000002,-60.7384339405188));
#165992=CARTESIAN_POINT('Ctrl Pts',(43.3817682803708,-54.58000002,-61.1499499438652));
#165993=CARTESIAN_POINT('Ctrl Pts',(43.5299471737832,-54.8943395876963,
-60.6499049353895));
#165994=CARTESIAN_POINT('Ctrl Pts',(43.5407821982001,-54.58000002,-60.7796882578927));
#165995=CARTESIAN_POINT('Ctrl Pts',(43.6059648750607,-54.58000002,-61.1139843549936));
#165996=CARTESIAN_POINT('Ctrl Pts',(43.9881565230544,-54.764616113509,-60.6498916468796));
#165997=CARTESIAN_POINT('Ctrl Pts',(44.0046317151094,-54.58000002,-60.8040236126605));
#165998=CARTESIAN_POINT('Ctrl Pts',(44.0540062919343,-54.58000002,-61.0395265773532));
#165999=CARTESIAN_POINT('Ctrl Pts',(44.2440095987556,-54.7260645641703,
-60.6498933522812));
#166000=CARTESIAN_POINT('Ctrl Pts',(44.2580491347896,-54.58000002,-60.7962448835176));
#166001=CARTESIAN_POINT('Ctrl Pts',(44.2780419706101,-54.58000002,-61.0029930876918));
#166002=CARTESIAN_POINT('Ctrl Pts',(44.7601884828712,-54.7249655177495,
-60.6498933671498));
#166003=CARTESIAN_POINT('Ctrl Pts',(44.7466180387413,-54.58000002,-60.7961110321462));
#166004=CARTESIAN_POINT('Ctrl Pts',(44.7276655629963,-54.58000002,-61.0020306983307));
#166005=CARTESIAN_POINT('Ctrl Pts',(45.0183788445834,-54.7626525929477,
-60.6498915741979));
#166006=CARTESIAN_POINT('Ctrl Pts',(45.0021140860289,-54.58000002,-60.8040311529128));
#166007=CARTESIAN_POINT('Ctrl Pts',(44.9532637149968,-54.58000002,-61.0380773886891));
#166008=CARTESIAN_POINT('Ctrl Pts',(45.4809398893316,-54.8922510295825,
-60.6499045972125));
#166009=CARTESIAN_POINT('Ctrl Pts',(45.4698465063657,-54.58000002,-60.7804647582867));
#166010=CARTESIAN_POINT('Ctrl Pts',(45.4045230317319,-54.58000002,-61.1130978438444));
#166011=CARTESIAN_POINT('Ctrl Pts',(45.6855420836461,-54.9825427397825,
-60.6499207098429));
#166012=CARTESIAN_POINT('Ctrl Pts',(45.6987517183194,-54.58000002,-60.7399919909284));
#166013=CARTESIAN_POINT('Ctrl Pts',(45.6299507757142,-54.58000002,-61.149949944621));
#166014=CARTESIAN_POINT('Ctrl Pts',(45.8586217441897,-55.080148121506,-60.6499500219341));
#166015=CARTESIAN_POINT('Ctrl Pts',(45.8586217441896,-54.58000002,-60.6498018765534));
#166016=CARTESIAN_POINT('Ctrl Pts',(45.8586217441897,-54.58000002,-61.14995));
#166017=CARTESIAN_POINT('',(45.8586217441897,-54.58000002,-61.14995));
#166018=CARTESIAN_POINT('Ctrl Pts',(45.8586217441897,-54.58000002,-61.14995));
#166019=CARTESIAN_POINT('Ctrl Pts',(45.7594843223744,-54.58000002,-61.1499499759911));
#166020=CARTESIAN_POINT('Ctrl Pts',(45.6608556134178,-54.58000002,-61.1430183938606));
#166021=CARTESIAN_POINT('Ctrl Pts',(45.5625314448154,-54.58000002,-61.1320945152429));
#166022=CARTESIAN_POINT('Ctrl Pts',(45.4342876572929,-54.58000002,-61.1178465476446));
#166023=CARTESIAN_POINT('Ctrl Pts',(45.3065614560444,-54.58000002,-61.0968118490375));
#166024=CARTESIAN_POINT('Ctrl Pts',(45.1788934332666,-54.5800000200001,
-61.075587255946));
#166025=CARTESIAN_POINT('Ctrl Pts',(45.1788516209101,-54.5800000200001,
-61.0755803047123));
#166026=CARTESIAN_POINT('Ctrl Pts',(45.1788098085678,-54.5800000200001,
-61.0755733535311));
#166027=CARTESIAN_POINT('Ctrl Pts',(45.1787679962398,-54.5800000200001,
-61.0755664024026));
#166028=CARTESIAN_POINT('Ctrl Pts',(44.9531807615356,-54.5800000200004,
-61.0380634472604));
#166029=CARTESIAN_POINT('Ctrl Pts',(44.7276252028241,-54.58000002,-61.0020307849363));
#166030=CARTESIAN_POINT('Ctrl Pts',(44.5028537665277,-54.58000002,-61.0025117642945));
#166031=CARTESIAN_POINT('Ctrl Pts',(44.5028486075311,-54.58000002,-61.002511775334));
#166032=CARTESIAN_POINT('Ctrl Pts',(44.5028434485348,-54.58000002,-61.0025117863925));
#166033=CARTESIAN_POINT('Ctrl Pts',(44.502838289539,-54.58000002,-61.00251179747));
#166034=CARTESIAN_POINT('Ctrl Pts',(44.3506760857094,-54.58000002,-61.0028385232137));
#166035=CARTESIAN_POINT('Ctrl Pts',(44.1989241833573,-54.5800000200001,
-61.0196754576622));
#166036=CARTESIAN_POINT('Ctrl Pts',(44.0472833113082,-54.5800000200001,
-61.042061298072));
#166037=CARTESIAN_POINT('Ctrl Pts',(43.9748362264932,-54.5800000200001,
-61.0527562304929));
#166038=CARTESIAN_POINT('Ctrl Pts',(43.9024145037602,-54.58000002,-61.0647186315174));
#166039=CARTESIAN_POINT('Ctrl Pts',(43.8299855489727,-54.58000002,-61.0767552584245));
#166040=CARTESIAN_POINT('Ctrl Pts',(43.7015244308355,-54.58000002,-61.0981036066869));
#166041=CARTESIAN_POINT('Ctrl Pts',(43.5729778197502,-54.58000002,-61.1190439724882));
#166042=CARTESIAN_POINT('Ctrl Pts',(43.4442858805782,-54.58000002,-61.1330238652827));
#166043=CARTESIAN_POINT('Ctrl Pts',(43.3487066835599,-54.58000002,-61.143406698398));
#166044=CARTESIAN_POINT('Ctrl Pts',(43.2530473192975,-54.58000002,-61.1499499760532));
#166045=CARTESIAN_POINT('Ctrl Pts',(43.1572831724516,-54.58000002,-61.14995));
#166046=CARTESIAN_POINT('',(45.8586217441897,-55.08000002,-60.64995));
#166047=CARTESIAN_POINT('Origin',(45.8586217441897,-55.08000002,-61.14995));
#166048=CARTESIAN_POINT('Ctrl Pts',(45.8586217441897,-55.08000002,-60.64995));
#166049=CARTESIAN_POINT('Ctrl Pts',(45.7689536596558,-55.029440916946,-60.64995));
#166050=CARTESIAN_POINT('Ctrl Pts',(45.6765174633164,-54.9839564622373,
-60.6499624250156));
#166051=CARTESIAN_POINT('Ctrl Pts',(45.4778485953844,-54.8996925932592,
-60.6499736157096));
#166052=CARTESIAN_POINT('Ctrl Pts',(45.3713338603102,-54.8620619965581,
-60.649952959783));
#166053=CARTESIAN_POINT('Ctrl Pts',(45.185760202174,-54.8090884744683,-60.6499481945182));
#166054=CARTESIAN_POINT('Ctrl Pts',(45.1077985401425,-54.7904750984749,
-60.6500611432134));
#166055=CARTESIAN_POINT('Ctrl Pts',(44.9203791059894,-54.7542997329155,
-60.6502857315348));
#166056=CARTESIAN_POINT('Ctrl Pts',(44.8104650288099,-54.7398986265098,
-60.6502931678836));
#166057=CARTESIAN_POINT('Ctrl Pts',(44.6361116415848,-54.7276946232681,
-60.6500701126525));
#166058=CARTESIAN_POINT('Ctrl Pts',(44.5721214250066,-54.7254562445459,
-60.6499575033559));
#166059=CARTESIAN_POINT('Ctrl Pts',(44.4919713617192,-54.7254515344577,
-60.6499485324377));
#166060=CARTESIAN_POINT('Ctrl Pts',(44.4758287519404,-54.7255927281287,
-60.6499538101927));
#166061=CARTESIAN_POINT('Ctrl Pts',(44.3973353016915,-54.726970533525,-60.6500007005379));
#166062=CARTESIAN_POINT('Ctrl Pts',(44.3350361171944,-54.7301856687748,
-60.6500992062372));
#166063=CARTESIAN_POINT('Ctrl Pts',(44.2458944853161,-54.7378330706298,
-60.6501868928199));
#166064=CARTESIAN_POINT('Ctrl Pts',(44.2189296557646,-54.7405484163116,
-60.6502073540677));
#166065=CARTESIAN_POINT('Ctrl Pts',(44.1669378685651,-54.746561490262,-60.650229174244));
#166066=CARTESIAN_POINT('Ctrl Pts',(44.141907947471,-54.7498060612269,-60.6502317923741));
#166067=CARTESIAN_POINT('Ctrl Pts',(44.0251905251394,-54.7665726407089,
-60.6502071425432));
#166068=CARTESIAN_POINT('Ctrl Pts',(43.9341908339756,-54.7843774385812,
-60.6500644239801));
#166069=CARTESIAN_POINT('Ctrl Pts',(43.7178584587808,-54.8381778103589,
-60.6498839791579));
#166070=CARTESIAN_POINT('Ctrl Pts',(43.5938526567529,-54.8785531161367,
-60.6499834288654));
#166071=CARTESIAN_POINT('Ctrl Pts',(43.3647423777244,-54.9716018333708,
-60.6499762216949));
#166072=CARTESIAN_POINT('Ctrl Pts',(43.2592299860172,-55.0225175893237,
-60.64995));
#166073=CARTESIAN_POINT('Ctrl Pts',(43.1572831724516,-55.08000002,-60.64995));
#166074=CARTESIAN_POINT('Origin',(57.,-54.08000002,-58.24995));
#166075=CARTESIAN_POINT('',(59.5,-54.58000002,-58.24995));
#166076=CARTESIAN_POINT('Origin',(59.5,-54.08000002,-58.24995));
#166077=CARTESIAN_POINT('',(57.,-54.58000002,-55.74995));
#166078=CARTESIAN_POINT('Origin',(57.,-54.08000002,-55.74995));
#166079=CARTESIAN_POINT('Origin',(57.,-54.58000002,-58.24995));
#166080=CARTESIAN_POINT('Origin',(59.5,-54.08000002,0.));
#166081=CARTESIAN_POINT('',(59.5,-54.58000002,-174.34995));
#166082=CARTESIAN_POINT('Origin',(59.5,-54.08000002,-174.34995));
#166083=CARTESIAN_POINT('',(59.5,-54.58000002,-58.24995));
#166084=CARTESIAN_POINT('Origin',(57.,-54.08000002,-174.34995));
#166085=CARTESIAN_POINT('',(57.,-54.58000002,-176.84995));
#166086=CARTESIAN_POINT('Origin',(57.,-54.08000002,-176.84995));
#166087=CARTESIAN_POINT('Origin',(57.,-54.58000002,-174.34995));
#166088=CARTESIAN_POINT('Origin',(60.,-54.08000002,-176.84995));
#166089=CARTESIAN_POINT('',(60.,-54.58000002,-176.84995));
#166090=CARTESIAN_POINT('Origin',(50.7934646035069,-55.08000002,-171.64995));
#166091=CARTESIAN_POINT('',(50.7934646035069,-54.58000002,-172.64995));
#166092=CARTESIAN_POINT('Origin',(50.7934646035069,-55.08000002,-172.64995));
#166093=CARTESIAN_POINT('',(50.2983305691361,-55.0104134695199,-171.64995));
#166094=CARTESIAN_POINT('',(50.7934646035069,-54.58000002,-55.24995));
#166095=CARTESIAN_POINT('Ctrl Pts',(49.2787232447289,-54.58000002,-171.14995));
#166096=CARTESIAN_POINT('Ctrl Pts',(49.2787232447289,-54.58000002,-171.64995));
#166097=CARTESIAN_POINT('Ctrl Pts',(49.2787232447289,-55.08000002,-171.64995));
#166098=CARTESIAN_POINT('Ctrl Pts',(49.477038164104,-54.58000002,-171.149950000016));
#166099=CARTESIAN_POINT('Ctrl Pts',(49.4109716734917,-54.58000002,-171.640924254979));
#166100=CARTESIAN_POINT('Ctrl Pts',(49.4122135882539,-55.0708895200012,
-171.64995));
#166101=CARTESIAN_POINT('Ctrl Pts',(49.6752036040849,-54.58000002,-171.18899099047));
#166102=CARTESIAN_POINT('Ctrl Pts',(49.548241251645,-54.58000002,-171.658003579003));
#166103=CARTESIAN_POINT('Ctrl Pts',(49.5456033137516,-55.061785887019,-171.675977326981));
#166104=CARTESIAN_POINT('Ctrl Pts',(50.0415757300179,-54.58000002,-171.339270411997));
#166105=CARTESIAN_POINT('Ctrl Pts',(49.8066765125445,-54.5800000199999,
-171.746711574348));
#166106=CARTESIAN_POINT('Ctrl Pts',(49.7922168368437,-55.0449549130127,
-171.776163607997));
#166107=CARTESIAN_POINT('Ctrl Pts',(50.2096025886599,-54.58000002,-171.450449746589));
#166108=CARTESIAN_POINT('Ctrl Pts',(49.9282402287017,-54.5800000199992,
-171.817687494207));
#166109=CARTESIAN_POINT('Ctrl Pts',(49.9053195885289,-55.037235833176,-171.850283164392));
#166110=CARTESIAN_POINT('Ctrl Pts',(50.4900116738692,-54.58000002,-171.728129909852));
#166111=CARTESIAN_POINT('Ctrl Pts',(50.1326854480763,-54.5800000200006,
-172.003556970024));
#166112=CARTESIAN_POINT('Ctrl Pts',(50.0940694074005,-55.0243539633763,
-172.035403273235));
#166113=CARTESIAN_POINT('Ctrl Pts',(50.6022836315107,-54.58000002,-171.894521542842));
#166114=CARTESIAN_POINT('Ctrl Pts',(50.2162545403414,-54.58000002,-172.118296873734));
#166115=CARTESIAN_POINT('Ctrl Pts',(50.1696422500339,-55.0191962391206,
-172.14633102856));
#166116=CARTESIAN_POINT('Ctrl Pts',(50.7540399347937,-54.58000002,-172.257328160063));
#166117=CARTESIAN_POINT('Ctrl Pts',(50.3290655494749,-54.58000002,-172.371853931892));
#166118=CARTESIAN_POINT('Ctrl Pts',(50.2717929158607,-55.0122246214262,
-172.38820210671));
#166119=CARTESIAN_POINT('Ctrl Pts',(50.7934646034919,-54.58000002,-172.453565067926));
#166120=CARTESIAN_POINT('Ctrl Pts',(50.3588212345858,-54.5800000199993,
-172.511015867073));
#166121=CARTESIAN_POINT('Ctrl Pts',(50.2983305691357,-55.0104134695225,
-172.51902671195));
#166122=CARTESIAN_POINT('Ctrl Pts',(50.7934646035069,-54.58000002,-172.64995));
#166123=CARTESIAN_POINT('Ctrl Pts',(50.3588212345988,-54.5800000199999,
-172.64995));
#166124=CARTESIAN_POINT('Ctrl Pts',(50.2983305691361,-55.0104134695199,
-172.64995));
#166125=CARTESIAN_POINT('Ctrl Pts',(49.2787232447289,-54.58000002,-171.14995));
#166126=CARTESIAN_POINT('Ctrl Pts',(49.477038164104,-54.58000002,-171.149950000016));
#166127=CARTESIAN_POINT('Ctrl Pts',(49.6752036040849,-54.58000002,-171.18899099047));
#166128=CARTESIAN_POINT('Ctrl Pts',(50.0415757300179,-54.58000002,-171.339270411997));
#166129=CARTESIAN_POINT('Ctrl Pts',(50.2096025886599,-54.58000002,-171.450449746589));
#166130=CARTESIAN_POINT('Ctrl Pts',(50.4900116738692,-54.58000002,-171.728129909852));
#166131=CARTESIAN_POINT('Ctrl Pts',(50.6022836315107,-54.58000002,-171.894521542842));
#166132=CARTESIAN_POINT('Ctrl Pts',(50.7540399347937,-54.58000002,-172.257328160063));
#166133=CARTESIAN_POINT('Ctrl Pts',(50.7934646034919,-54.58000002,-172.453565067926));
#166134=CARTESIAN_POINT('Ctrl Pts',(50.7934646035069,-54.58000002,-172.64995));
#166135=CARTESIAN_POINT('Ctrl Pts',(52.4185037433787,-38.6078427661476,
-171.271207239029));
#166136=CARTESIAN_POINT('Ctrl Pts',(52.5086485179119,-38.28000002,-171.191647032251));
#166137=CARTESIAN_POINT('Ctrl Pts',(52.7704579175044,-38.28000002,-170.960578619515));
#166138=CARTESIAN_POINT('Ctrl Pts',(52.370156234462,-38.5972036761564,-171.210531232685));
#166139=CARTESIAN_POINT('Ctrl Pts',(52.4702729319568,-38.2800000200013,
-171.135526834247));
#166140=CARTESIAN_POINT('Ctrl Pts',(52.7436831755344,-38.28000002,-170.930241803514));
#166141=CARTESIAN_POINT('Ctrl Pts',(52.3288572922619,-38.5881022353565,
-171.144413209532));
#166142=CARTESIAN_POINT('Ctrl Pts',(52.4376229301059,-38.2800000199995,
-171.075889787111));
#166143=CARTESIAN_POINT('Ctrl Pts',(52.7208049303309,-38.28000002,-170.897181907961));
#166144=CARTESIAN_POINT('Ctrl Pts',(52.2951895046066,-38.58067735034,-171.072568261741));
#166145=CARTESIAN_POINT('Ctrl Pts',(52.4111831155989,-38.28000002,-171.012340412829));
#166146=CARTESIAN_POINT('Ctrl Pts',(52.7021525552272,-38.28000002,-170.861259130871));
#166147=CARTESIAN_POINT('',(52.7021525552272,-38.28000002,-170.861259130871));
#166148=CARTESIAN_POINT('Origin',(52.7021525552272,-38.78000002,-170.861259130871));
#166149=CARTESIAN_POINT('',(52.7704579175045,-38.28000002,-170.960578619515));
#166150=CARTESIAN_POINT('Origin',(52.7704579175045,-38.78000002,-170.960578619515));
#166151=CARTESIAN_POINT('Ctrl Pts',(52.7021525552272,-38.28000002,-170.861259130871));
#166152=CARTESIAN_POINT('Ctrl Pts',(52.7208104423973,-38.28000002,-170.897192602603));
#166153=CARTESIAN_POINT('Ctrl Pts',(52.7436752534113,-38.28000002,-170.930232830913));
#166154=CARTESIAN_POINT('Ctrl Pts',(52.7704579175045,-38.28000002,-170.960578619515));
#166155=CARTESIAN_POINT('Ctrl Pts',(40.5593018105247,-38.28000002,-148.113408860656));
#166156=CARTESIAN_POINT('Ctrl Pts',(40.3021382496555,-38.28000002,-148.255551254414));
#166157=CARTESIAN_POINT('Ctrl Pts',(40.1770020116941,-38.5366991465431,
-148.324717991527));
#166158=CARTESIAN_POINT('Ctrl Pts',(42.6385250759047,-38.28000002,-151.875132894361));
#166159=CARTESIAN_POINT('Ctrl Pts',(42.3869374257262,-38.280000019955,-152.041577619703));
#166160=CARTESIAN_POINT('Ctrl Pts',(42.2505775009144,-38.5455762523402,
-152.086445166823));
#166161=CARTESIAN_POINT('Ctrl Pts',(44.6827387638399,-38.28000002,-155.655552720034));
#166162=CARTESIAN_POINT('Ctrl Pts',(44.4227143745257,-38.2800000199852,
-155.82004311619));
#166163=CARTESIAN_POINT('Ctrl Pts',(44.2901446089557,-38.5535332680681,
-155.866861850893));
#166164=CARTESIAN_POINT('Ctrl Pts',(48.7243729558795,-38.28000002,-163.241363066864));
#166165=CARTESIAN_POINT('Ctrl Pts',(48.4532973709855,-38.280000020015,-163.409015135176));
#166166=CARTESIAN_POINT('Ctrl Pts',(48.3237478755738,-38.5680639323333,
-163.452672197745));
#166167=CARTESIAN_POINT('Ctrl Pts',(50.7215899998133,-38.28000002,-167.046867503852));
#166168=CARTESIAN_POINT('Ctrl Pts',(50.4437502527583,-38.2800000199406,
-167.213058728775));
#166169=CARTESIAN_POINT('Ctrl Pts',(50.3175866645898,-38.5746359826999,
-167.258178117331));
#166170=CARTESIAN_POINT('Ctrl Pts',(52.7021525552272,-38.28000002,-170.861259130871));
#166171=CARTESIAN_POINT('Ctrl Pts',(52.4111831155989,-38.28000002,-171.012340412829));
#166172=CARTESIAN_POINT('Ctrl Pts',(52.2951895046066,-38.58067735034,-171.07256826174));
#166173=CARTESIAN_POINT('',(40.5593018105246,-38.28000002,-148.113408860656));
#166174=CARTESIAN_POINT('Origin',(40.5593018105246,-38.78000002,-148.113408860656));
#166175=CARTESIAN_POINT('Ctrl Pts',(40.5593018105247,-38.28000002,-148.113408860656));
#166176=CARTESIAN_POINT('Ctrl Pts',(42.6385266988695,-38.28000002,-151.875135830624));
#166177=CARTESIAN_POINT('Ctrl Pts',(44.6827387638261,-38.28000002,-155.655552720007));
#166178=CARTESIAN_POINT('Ctrl Pts',(46.7035558598462,-38.28000002,-159.448457893456));
#166179=CARTESIAN_POINT('Ctrl Pts',(48.7243729558662,-38.28000002,-163.241363066904));
#166180=CARTESIAN_POINT('Ctrl Pts',(50.7215893876843,-38.28000002,-167.046866324983));
#166181=CARTESIAN_POINT('Ctrl Pts',(52.7021525552272,-38.28000002,-170.86125913087));
#166182=CARTESIAN_POINT('Ctrl Pts',(40.2402032265086,-38.5310516260855,
-148.430476962511));
#166183=CARTESIAN_POINT('Ctrl Pts',(40.3651906300648,-38.28000002,-148.358692119651));
#166184=CARTESIAN_POINT('Ctrl Pts',(40.6162128330585,-38.28000002,-148.214500674674));
#166185=CARTESIAN_POINT('Ctrl Pts',(39.7977899207324,-38.5702096309806,
-147.703924195849));
#166186=CARTESIAN_POINT('Ctrl Pts',(39.9124625700216,-38.28000002,-147.631198453379));
#166187=CARTESIAN_POINT('Ctrl Pts',(40.2179805560823,-38.28000002,-147.519873800225));
#166188=CARTESIAN_POINT('Ctrl Pts',(39.4932042804462,-38.6117726883092,
-146.929953925225));
#166189=CARTESIAN_POINT('Ctrl Pts',(39.6018856406274,-38.28000002,-146.86744228999));
#166190=CARTESIAN_POINT('Ctrl Pts',(39.9439021523076,-38.28000002,-146.780824095429));
#166191=CARTESIAN_POINT('Ctrl Pts',(39.1932776445035,-38.6754317541046,
-145.737338799595));
#166192=CARTESIAN_POINT('Ctrl Pts',(39.2753128801367,-38.28000002,-145.71515188289));
#166193=CARTESIAN_POINT('Ctrl Pts',(39.6739630147418,-38.28000002,-145.64333076277));
#166194=CARTESIAN_POINT('Ctrl Pts',(39.1206267323737,-38.6963627685879,
-145.344127129863));
#166195=CARTESIAN_POINT('Ctrl Pts',(39.1901218279244,-38.28000002,-145.326713623533));
#166196=CARTESIAN_POINT('Ctrl Pts',(39.6085749933904,-38.28000002,-145.268506383101));
#166197=CARTESIAN_POINT('Ctrl Pts',(39.0193613209311,-38.7402648896269,
-144.516661028813));
#166198=CARTESIAN_POINT('Ctrl Pts',(39.0555238762964,-38.28000002,-144.505704693498));
#166199=CARTESIAN_POINT('Ctrl Pts',(39.5174306634401,-38.28000002,-144.480224304407));
#166200=CARTESIAN_POINT('Ctrl Pts',(38.9953087866826,-38.763347780271,-144.080042595184));
#166201=CARTESIAN_POINT('Ctrl Pts',(39.0120467208245,-38.28000002,-144.07044288467));
#166202=CARTESIAN_POINT('Ctrl Pts',(39.4957803914547,-38.28000002,-144.064560626685));
#166203=CARTESIAN_POINT('Ctrl Pts',(39.0007543400766,-38.7864872879417,
-143.640515939691));
#166204=CARTESIAN_POINT('Ctrl Pts',(38.994184744005,-38.2800000199999,-143.64044055047));
#166205=CARTESIAN_POINT('Ctrl Pts',(39.5006779618633,-38.28000002,-143.646429119223));
#166206=CARTESIAN_POINT('',(39.5,-38.28000002,-143.762156710948));
#166207=CARTESIAN_POINT('Origin',(39.5,-38.78000002,-143.762156710948));
#166208=CARTESIAN_POINT('Ctrl Pts',(39.5,-38.28000002,-143.762156710948));
#166209=CARTESIAN_POINT('Ctrl Pts',(39.5,-38.28000002,-144.141283590664));
#166210=CARTESIAN_POINT('Ctrl Pts',(39.5218408888636,-38.28000002,-144.518367123251));
#166211=CARTESIAN_POINT('Ctrl Pts',(39.5652079410422,-38.28000002,-144.893436753186));
#166212=CARTESIAN_POINT('Ctrl Pts',(39.6085749932207,-38.28000002,-145.26850638312));
#166213=CARTESIAN_POINT('Ctrl Pts',(39.6739630147302,-38.28000002,-145.643330762739));
#166214=CARTESIAN_POINT('Ctrl Pts',(39.7609941006785,-38.28000002,-146.010070025021));
#166215=CARTESIAN_POINT('Ctrl Pts',(39.8480251866268,-38.28000002,-146.376809287303));
#166216=CARTESIAN_POINT('Ctrl Pts',(39.9556757536423,-38.28000002,-146.736297755287));
#166217=CARTESIAN_POINT('Ctrl Pts',(40.0875243805731,-38.28000002,-147.087277124802));
#166218=CARTESIAN_POINT('Ctrl Pts',(40.206517035942,-38.28000002,-147.404034061377));
#166219=CARTESIAN_POINT('Ctrl Pts',(40.3452186968614,-38.28000002,-147.713860479176));
#166220=CARTESIAN_POINT('Ctrl Pts',(40.5063035885383,-38.28000002,-148.015815905681));
#166221=CARTESIAN_POINT('Ctrl Pts',(40.5237072071063,-38.28000002,-148.04843918284));
#166222=CARTESIAN_POINT('Ctrl Pts',(40.5413721449718,-38.28000002,-148.080970567499));
#166223=CARTESIAN_POINT('Ctrl Pts',(40.5593018105246,-38.28000002,-148.113408860656));
#166224=CARTESIAN_POINT('Origin',(39.5,-38.78000002,-55.2499500000007));
#166225=CARTESIAN_POINT('',(39.5,-38.28000002,-88.296486260558));
#166226=CARTESIAN_POINT('Origin',(39.5,-38.78000002,-88.296486260558));
#166227=CARTESIAN_POINT('',(39.5,-38.28000002,-55.2499500000007));
#166228=CARTESIAN_POINT('Ctrl Pts',(39.,-38.78000002,-88.296486260558));
#166229=CARTESIAN_POINT('Ctrl Pts',(39.,-38.2800000199999,-88.296486260558));
#166230=CARTESIAN_POINT('Ctrl Pts',(39.5,-38.28000002,-88.296486260558));
#166231=CARTESIAN_POINT('Ctrl Pts',(39.,-38.7380050653939,-87.4993525996999));
#166232=CARTESIAN_POINT('Ctrl Pts',(39.0402973596559,-38.2800000199999,
-87.5315757932098));
#166233=CARTESIAN_POINT('Ctrl Pts',(39.500000001834,-38.28000002,-87.5380528917837));
#166234=CARTESIAN_POINT('Ctrl Pts',(39.094978232517,-38.6964757448679,-86.7169698827889));
#166235=CARTESIAN_POINT('Ctrl Pts',(39.1607938862687,-38.2800000199999,
-86.7517814461085));
#166236=CARTESIAN_POINT('Ctrl Pts',(39.5854804081441,-38.28000002,-86.7926795341198));
#166237=CARTESIAN_POINT('Ctrl Pts',(39.4784350964048,-38.6146030713812,
-85.1828476912075));
#166238=CARTESIAN_POINT('Ctrl Pts',(39.5865447970557,-38.28000002,-85.2418413411644));
#166239=CARTESIAN_POINT('Ctrl Pts',(39.9305915878855,-38.28000002,-85.3294730611686));
#166240=CARTESIAN_POINT('Ctrl Pts',(39.7704847917915,-38.5740029030169,
-84.4264431605892));
#166241=CARTESIAN_POINT('Ctrl Pts',(39.8855744697273,-38.28000002,-84.495834401995));
#166242=CARTESIAN_POINT('Ctrl Pts',(40.1934239997695,-38.28000002,-84.6071790833831));
#166243=CARTESIAN_POINT('Ctrl Pts',(40.1770020116941,-38.5366991465431,
-83.7339249799794));
#166244=CARTESIAN_POINT('Ctrl Pts',(40.3021382496555,-38.2800000199999,
-83.8030917170923));
#166245=CARTESIAN_POINT('Ctrl Pts',(40.5593018105246,-38.28000002,-83.9452341108497));
#166246=CARTESIAN_POINT('',(40.5593018105246,-38.28000002,-83.9452341108497));
#166247=CARTESIAN_POINT('Origin',(40.5593018105246,-38.78000002,-83.9452341108497));
#166248=CARTESIAN_POINT('Ctrl Pts',(40.5593018105246,-38.28000002,-83.9452341108497));
#166249=CARTESIAN_POINT('Ctrl Pts',(40.495353484328,-38.28000002,-84.0609292165926));
#166250=CARTESIAN_POINT('Ctrl Pts',(40.4347639681506,-38.28000002,-84.1780768945292));
#166251=CARTESIAN_POINT('Ctrl Pts',(40.377316900473,-38.28000002,-84.2965776208551));
#166252=CARTESIAN_POINT('Ctrl Pts',(40.3173964789327,-38.28000002,-84.42018033482));
#166253=CARTESIAN_POINT('Ctrl Pts',(40.2608947873256,-38.28000002,-84.5452556205672));
#166254=CARTESIAN_POINT('Ctrl Pts',(40.2076155462081,-38.28000002,-84.6717210755965));
#166255=CARTESIAN_POINT('Ctrl Pts',(40.1651845073099,-38.28000002,-84.7724368615026));
#166256=CARTESIAN_POINT('Ctrl Pts',(40.1247982681521,-38.28000002,-84.8740350854921));
#166257=CARTESIAN_POINT('Ctrl Pts',(40.086379235959,-38.28000002,-84.9764835369928));
#166258=CARTESIAN_POINT('Ctrl Pts',(40.0265153547945,-38.28000002,-85.1361169680304));
#166259=CARTESIAN_POINT('Ctrl Pts',(39.9714555367521,-38.28000002,-85.2977643783891));
#166260=CARTESIAN_POINT('Ctrl Pts',(39.9211479365403,-38.28000002,-85.4606561619587));
#166261=CARTESIAN_POINT('Ctrl Pts',(39.8688810993165,-38.28000002,-85.6298917903942));
#166262=CARTESIAN_POINT('Ctrl Pts',(39.821743908823,-38.28000002,-85.8004696290636));
#166263=CARTESIAN_POINT('Ctrl Pts',(39.7796250224716,-38.28000002,-85.9715109372544));
#166264=CARTESIAN_POINT('Ctrl Pts',(39.7722762919973,-38.28000002,-86.0013535229146));
#166265=CARTESIAN_POINT('Ctrl Pts',(39.7650802005722,-38.28000002,-86.0312102022424));
#166266=CARTESIAN_POINT('Ctrl Pts',(39.758035997616,-38.28000002,-86.0610762975502));
#166267=CARTESIAN_POINT('Ctrl Pts',(39.6557558157219,-38.28000002,-86.4947250268074));
#166268=CARTESIAN_POINT('Ctrl Pts',(39.5840763701744,-38.28000002,-86.9331589876102));
#166269=CARTESIAN_POINT('Ctrl Pts',(39.5426478307206,-38.28000002,-87.3763235090859));
#166270=CARTESIAN_POINT('Ctrl Pts',(39.5141828100108,-38.28000002,-87.6808161957216));
#166271=CARTESIAN_POINT('Ctrl Pts',(39.5,-38.28000002,-87.9875423033778));
#166272=CARTESIAN_POINT('Ctrl Pts',(39.5,-38.28000002,-88.296486260558));
#166273=CARTESIAN_POINT('Ctrl Pts',(52.5768547844511,-38.28000002,-61.4386408691297));
#166274=CARTESIAN_POINT('Ctrl Pts',(52.2861787013546,-38.28000002,-61.287642251635));
#166275=CARTESIAN_POINT('Ctrl Pts',(52.1700794675439,-38.5802945048887,
-61.2273317382593));
#166276=CARTESIAN_POINT('Ctrl Pts',(50.6164606414324,-38.28000002,-65.2124482077584));
#166277=CARTESIAN_POINT('Ctrl Pts',(50.3387340734665,-38.2800000200587,
-65.0466233854387));
#166278=CARTESIAN_POINT('Ctrl Pts',(50.2126317933694,-38.5742944332221,
-65.0011376410615));
#166279=CARTESIAN_POINT('Ctrl Pts',(48.6396458371624,-38.28000002,-68.9774905161504));
#166280=CARTESIAN_POINT('Ctrl Pts',(48.3685987197966,-38.28000002,-68.8102729799503));
#166281=CARTESIAN_POINT('Ctrl Pts',(48.239176789686,-38.5677719010369,-68.7661813852757));
#166282=CARTESIAN_POINT('Ctrl Pts',(44.6396194153305,-38.28000002,-76.4827983330569));
#166283=CARTESIAN_POINT('Ctrl Pts',(44.3795316629781,-38.28000002,-76.3187098252974));
#166284=CARTESIAN_POINT('Ctrl Pts',(44.247123664849,-38.5533652514423,-76.2714892021909));
#166285=CARTESIAN_POINT('Ctrl Pts',(42.6166022657662,-38.28000002,-80.2231727548289));
#166286=CARTESIAN_POINT('Ctrl Pts',(42.3648252555903,-38.2800000199999,
-80.0572213824928));
#166287=CARTESIAN_POINT('Ctrl Pts',(42.228714191533,-38.5454826541321,-80.0118606023558));
#166288=CARTESIAN_POINT('Ctrl Pts',(40.5593018105246,-38.28000002,-83.9452341108497));
#166289=CARTESIAN_POINT('Ctrl Pts',(40.3021382496555,-38.28000002,-83.8030917170923));
#166290=CARTESIAN_POINT('Ctrl Pts',(40.177002011694,-38.5366991465431,-83.7339249799794));
#166291=CARTESIAN_POINT('',(52.5768547844511,-38.28000002,-61.4386408691297));
#166292=CARTESIAN_POINT('',(52.1700794675439,-38.5802945048887,-61.2273317382593));
#166293=CARTESIAN_POINT('Origin',(52.5768547844511,-38.78000002,-61.4386408691297));
#166294=CARTESIAN_POINT('Ctrl Pts',(40.177002011694,-38.536699146543,-83.7339249799794));
#166295=CARTESIAN_POINT('Ctrl Pts',(40.7446447656533,-38.5391292605099,
-82.7041495102648));
#166296=CARTESIAN_POINT('Ctrl Pts',(41.3204916041055,-38.5415363980795,
-81.6534564475751));
#166297=CARTESIAN_POINT('Ctrl Pts',(41.9045140297048,-38.5439178456464,
-80.5818101170486));
#166298=CARTESIAN_POINT('Ctrl Pts',(42.4744069545298,-38.5462416778483,
-79.536090578017));
#166299=CARTESIAN_POINT('Ctrl Pts',(43.0520848743935,-38.5485410462409,
-78.4704186258952));
#166300=CARTESIAN_POINT('Ctrl Pts',(43.6375626153468,-38.5508142186263,
-77.3847870051934));
#166301=CARTESIAN_POINT('Ctrl Pts',(44.2084182209449,-38.5530306191961,
-76.3262687167217));
#166302=CARTESIAN_POINT('Ctrl Pts',(44.7866884417665,-38.5552221118789,
-75.2487758893125));
#166303=CARTESIAN_POINT('Ctrl Pts',(45.3724279863849,-38.5573878910057,
-74.1523290357761));
#166304=CARTESIAN_POINT('Ctrl Pts',(45.6528382846118,-38.5584247115113,
-73.6274285198132));
#166305=CARTESIAN_POINT('Ctrl Pts',(45.9349610406077,-38.5594556511644,
-73.0981844964864));
#166306=CARTESIAN_POINT('Ctrl Pts',(46.2188059022254,-38.5604806919717,
-72.5646014397013));
#166307=CARTESIAN_POINT('Ctrl Pts',(46.2269016349262,-38.560509927859,-72.5493827537727));
#166308=CARTESIAN_POINT('Ctrl Pts',(46.23585120676,-38.5605422353004,-72.5325579056226));
#166309=CARTESIAN_POINT('Ctrl Pts',(46.2431502305807,-38.5605685685527,
-72.5188352954991));
#166310=CARTESIAN_POINT('Ctrl Pts',(46.2433044757766,-38.5605691250351,
-72.5185453051197));
#166311=CARTESIAN_POINT('Ctrl Pts',(46.2434579839114,-38.5605696788504,
-72.5182567001373));
#166312=CARTESIAN_POINT('Ctrl Pts',(46.2436107313547,-38.5605702299136,
-72.5179695249877));
#166313=CARTESIAN_POINT('Ctrl Pts',(46.8939219586432,-38.562916341634,-71.2953420301694));
#166314=CARTESIAN_POINT('Ctrl Pts',(47.5544270166758,-38.5652360394503,
-70.0477205124839));
#166315=CARTESIAN_POINT('Ctrl Pts',(48.2251016678356,-38.5675266745615,
-68.7750796691625));
#166316=CARTESIAN_POINT('Ctrl Pts',(48.873376566188,-38.5697408051259,-67.5449435488894));
#166317=CARTESIAN_POINT('Ctrl Pts',(49.5311530209752,-38.5719277795132,
-66.2914313855809));
#166318=CARTESIAN_POINT('Ctrl Pts',(50.1984508815467,-38.5740861349683,
-65.0145434284377));
#166319=CARTESIAN_POINT('Ctrl Pts',(50.846656328617,-38.5761827365691,-63.7741891908119));
#166320=CARTESIAN_POINT('Ctrl Pts',(51.5038460529118,-38.5782523311409,
-62.5117776143721));
#166321=CARTESIAN_POINT('Ctrl Pts',(52.1700794675439,-38.5802945048887,
-61.2273317382593));
#166322=CARTESIAN_POINT('Ctrl Pts',(52.5768547844511,-38.28000002,-61.4386408691297));
#166323=CARTESIAN_POINT('Ctrl Pts',(50.6164600523975,-38.28000002,-65.2124493416261));
#166324=CARTESIAN_POINT('Ctrl Pts',(48.6396458371541,-38.28000002,-68.9774905161615));
#166325=CARTESIAN_POINT('Ctrl Pts',(46.6396326262455,-38.28000002,-72.7301444246032));
#166326=CARTESIAN_POINT('Ctrl Pts',(44.6396194153369,-38.28000002,-76.4827983330449));
#166327=CARTESIAN_POINT('Ctrl Pts',(42.6166038138442,-38.28000002,-80.2231699540513));
#166328=CARTESIAN_POINT('Ctrl Pts',(40.5593018105246,-38.28000002,-83.9452341108497));
#166329=CARTESIAN_POINT('Origin',(59.5,-37.78000002,-55.2499500000007));
#166330=CARTESIAN_POINT('',(59.5,-38.28000002,-58.24995));
#166331=CARTESIAN_POINT('Origin',(59.5,-37.78000002,-58.24995));
#166332=CARTESIAN_POINT('',(59.5,-38.28000002,-174.34995));
#166333=CARTESIAN_POINT('',(59.5,-38.28000002,-58.24995));
#166334=CARTESIAN_POINT('Origin',(59.5,-37.78000002,-174.34995));
#166335=CARTESIAN_POINT('Origin',(57.,-37.78000002,-174.34995));
#166336=CARTESIAN_POINT('',(57.,-38.28000002,-176.84995));
#166337=CARTESIAN_POINT('Origin',(57.,-38.28000002,-174.34995));
#166338=CARTESIAN_POINT('Origin',(57.,-37.78000002,-176.84995));
#166339=CARTESIAN_POINT('Origin',(-83.2809572255632,-37.78000002,-176.84995));
#166340=CARTESIAN_POINT('',(-83.2809572255632,-38.28000002,-176.84995));
#166341=CARTESIAN_POINT('Origin',(53.1262583325313,-38.78000002,-179.64995));
#166342=CARTESIAN_POINT('',(53.1262583325313,-38.28000002,-171.916267709546));
#166343=CARTESIAN_POINT('Origin',(53.1262583325313,-38.78000002,-171.916267709546));
#166344=CARTESIAN_POINT('',(52.6451348158641,-38.6439112191758,-179.64995));
#166345=CARTESIAN_POINT('',(53.1262583325313,-38.28000002,-176.84995));
#166346=CARTESIAN_POINT('Ctrl Pts',(52.7704579175044,-38.28000002,-170.960578619515));
#166347=CARTESIAN_POINT('Ctrl Pts',(52.508648517912,-38.28000002,-171.191647032252));
#166348=CARTESIAN_POINT('Ctrl Pts',(52.418503743379,-38.6078427661477,-171.27120723903));
#166349=CARTESIAN_POINT('Ctrl Pts',(52.8865885798003,-38.28000002,-171.092159149585));
#166350=CARTESIAN_POINT('Ctrl Pts',(52.5972087752045,-38.2800000200018,
-171.289280606396));
#166351=CARTESIAN_POINT('Ctrl Pts',(52.4966135335128,-38.6055762491043,
-171.358452481822));
#166352=CARTESIAN_POINT('Ctrl Pts',(52.9752899136351,-38.28000002,-171.24095231752));
#166353=CARTESIAN_POINT('Ctrl Pts',(52.6638881026927,-38.2800000200005,
-171.402873892562));
#166354=CARTESIAN_POINT('Ctrl Pts',(52.5554277399439,-38.6065951776351,
-171.457851777602));
#166355=CARTESIAN_POINT('Ctrl Pts',(53.0969739026007,-38.28000002,-171.570371861396));
#166356=CARTESIAN_POINT('Ctrl Pts',(52.7468873373812,-38.2800000199994,
-171.654013242837));
#166357=CARTESIAN_POINT('Ctrl Pts',(52.6330841414732,-38.6181228329597,
-171.679920679702));
#166358=CARTESIAN_POINT('Ctrl Pts',(53.1262583244907,-38.28000002,-171.740763530748));
#166359=CARTESIAN_POINT('Ctrl Pts',(52.7606056378773,-38.28000002,-171.785522775662));
#166360=CARTESIAN_POINT('Ctrl Pts',(52.6495272179227,-38.6283824768232,
-171.795722243821));
#166361=CARTESIAN_POINT('Ctrl Pts',(53.1262583325313,-38.28000002,-171.916267709546));
#166362=CARTESIAN_POINT('Ctrl Pts',(52.748069378376,-38.28000002,-171.916267709546));
#166363=CARTESIAN_POINT('Ctrl Pts',(52.6451348158641,-38.6439112191758,
-171.916267709546));
#166364=CARTESIAN_POINT('Ctrl Pts',(52.7704579175044,-38.28000002,-170.960578619515));
#166365=CARTESIAN_POINT('Ctrl Pts',(52.8285971612714,-38.28000002,-171.026452630405));
#166366=CARTESIAN_POINT('Ctrl Pts',(52.8797920295936,-38.28000002,-171.096554170654));
#166367=CARTESIAN_POINT('Ctrl Pts',(52.9240704508372,-38.28000002,-171.170767761981));
#166368=CARTESIAN_POINT('Ctrl Pts',(52.9683488720808,-38.28000002,-171.244981353309));
#166369=CARTESIAN_POINT('Ctrl Pts',(53.0057109090821,-38.28000002,-171.323307205357));
#166370=CARTESIAN_POINT('Ctrl Pts',(53.0361319037073,-38.28000002,-171.405662091088));
#166371=CARTESIAN_POINT('Ctrl Pts',(53.0782642785414,-38.28000002,-171.519721705435));
#166372=CARTESIAN_POINT('Ctrl Pts',(53.1052589026234,-38.28000002,-171.636480608475));
#166373=CARTESIAN_POINT('Ctrl Pts',(53.1178820115773,-38.28000002,-171.755802197906));
#166374=CARTESIAN_POINT('Ctrl Pts',(53.1234875228305,-38.28000002,-171.808789026646));
#166375=CARTESIAN_POINT('Ctrl Pts',(53.126258330058,-38.28000002,-171.862281331534));
#166376=CARTESIAN_POINT('Ctrl Pts',(53.1262583325313,-38.28000002,-171.916267709546));
#166377=CARTESIAN_POINT('Ctrl Pts',(49.940073970993,-44.4295309128427,-60.6499502200616));
#166378=CARTESIAN_POINT('Ctrl Pts',(49.940073970993,-44.93000002,-60.6494806725745));
#166379=CARTESIAN_POINT('Ctrl Pts',(49.940073970993,-44.93000002,-61.14995));
#166380=CARTESIAN_POINT('Ctrl Pts',(49.8479774404557,-44.4053128313032,
-60.6499729431522));
#166381=CARTESIAN_POINT('Ctrl Pts',(49.8456458072228,-44.93000002,-60.6246358503761));
#166382=CARTESIAN_POINT('Ctrl Pts',(49.8863992897437,-44.93000002,-61.1499500208808));
#166383=CARTESIAN_POINT('Ctrl Pts',(49.7578649778778,-44.3815585116814,
-60.662149119638));
#166384=CARTESIAN_POINT('Ctrl Pts',(49.7496066417035,-44.93000002,-60.6099006060758));
#166385=CARTESIAN_POINT('Ctrl Pts',(49.8338483436824,-44.93000002,-61.1560263819637));
#166386=CARTESIAN_POINT('Ctrl Pts',(49.5816013859087,-44.3349893071918,
-60.7103063370538));
#166387=CARTESIAN_POINT('Ctrl Pts',(49.5465928271943,-44.93000002,-60.6009208199127));
#166388=CARTESIAN_POINT('Ctrl Pts',(49.7309938571501,-44.93000002,-61.1800821203567));
#166389=CARTESIAN_POINT('Ctrl Pts',(49.4941735011919,-44.3118347483412,
-60.7471802581384));
#166390=CARTESIAN_POINT('Ctrl Pts',(49.4370815776501,-44.9300000199997,
-60.6082512678975));
#166391=CARTESIAN_POINT('Ctrl Pts',(49.6799439551145,-44.93000002,-61.1985082982007));
#166392=CARTESIAN_POINT('Ctrl Pts',(49.3328045849881,-44.269009574368,-60.8440382106835));
#166393=CARTESIAN_POINT('Ctrl Pts',(49.2133831268095,-44.9300000200003,
-60.653509168894));
#166394=CARTESIAN_POINT('Ctrl Pts',(49.5856644732959,-44.93000002,-61.2469206297));
#166395=CARTESIAN_POINT('Ctrl Pts',(49.2582348505417,-44.2491742563957,
-60.9036717632631));
#166396=CARTESIAN_POINT('Ctrl Pts',(49.0983969745462,-44.9300000200002,
-60.6926283936834));
#166397=CARTESIAN_POINT('Ctrl Pts',(49.5420691606389,-44.93000002,-61.2767318781126));
#166398=CARTESIAN_POINT('Ctrl Pts',(49.1235836593332,-44.2132994481138,
-61.0495884892673));
#166399=CARTESIAN_POINT('Ctrl Pts',(48.8650295486972,-44.9300000199998,
-60.8202676220942));
#166400=CARTESIAN_POINT('Ctrl Pts',(49.4633104246523,-44.93000002,-61.3496883835064));
#166401=CARTESIAN_POINT('Ctrl Pts',(49.0660606187868,-44.1979416296537,
-61.1334940119936));
#166402=CARTESIAN_POINT('Ctrl Pts',(48.7523385355526,-44.93000002,-60.9091191391034));
#166403=CARTESIAN_POINT('Ctrl Pts',(49.4296447656355,-44.93000002,-61.3916439172571));
#166404=CARTESIAN_POINT('Ctrl Pts',(49.0216817963636,-44.1860823027988,
-61.2274665920928));
#166405=CARTESIAN_POINT('Ctrl Pts',(48.6578457649038,-44.93000002,-61.0263236351359));
#166406=CARTESIAN_POINT('Ctrl Pts',(49.4036629110189,-44.93000002,-61.4386408691297));
#166407=CARTESIAN_POINT('Ctrl Pts',(49.940073970993,-44.43000002,-60.64995));
#166408=CARTESIAN_POINT('Ctrl Pts',(49.8114787093223,-44.3961999235187,
-60.64995));
#166409=CARTESIAN_POINT('Ctrl Pts',(49.7009578626629,-44.366496043485,-60.6737266630953));
#166410=CARTESIAN_POINT('Ctrl Pts',(49.5662681479033,-44.3309458928829,
-60.7193269101808));
#166411=CARTESIAN_POINT('Ctrl Pts',(49.5264094220829,-44.320504982567,-60.7362560379875));
#166412=CARTESIAN_POINT('Ctrl Pts',(49.4738000033418,-44.306750375621,-60.7618373723648));
#166413=CARTESIAN_POINT('Ctrl Pts',(49.4574561560657,-44.302480786915,-60.7704020732091));
#166414=CARTESIAN_POINT('Ctrl Pts',(49.4346580763186,-44.2965074132954,
-60.7830608683784));
#166415=CARTESIAN_POINT('Ctrl Pts',(49.4236882926368,-44.293628364449,-60.789343778841));
#166416=CARTESIAN_POINT('Ctrl Pts',(49.411624548949,-44.2904477727066,-60.7965449436944));
#166417=CARTESIAN_POINT('Ctrl Pts',(49.4066098784319,-44.2891217552102,
-60.7995988132645));
#166418=CARTESIAN_POINT('Ctrl Pts',(49.4033011158289,-44.2882458627272,
-60.8016270235086));
#166419=CARTESIAN_POINT('Ctrl Pts',(49.4028309549621,-44.2881216419612,
-60.8019125086144));
#166420=CARTESIAN_POINT('Ctrl Pts',(49.2216643765893,-44.2400505684977,
-60.9144220519661));
#166421=CARTESIAN_POINT('Ctrl Pts',(49.0958707926624,-44.2064653114064,
-61.0697892923834));
#166422=CARTESIAN_POINT('Ctrl Pts',(49.0214378669496,-44.1865817238571,
-61.2273317382593));
#166423=CARTESIAN_POINT('Ctrl Pts',(49.4036629110189,-44.93000002,-61.4386408691297));
#166424=CARTESIAN_POINT('Ctrl Pts',(49.421292954971,-44.93000002,-61.4067508873822));
#166425=CARTESIAN_POINT('Ctrl Pts',(49.4424088019263,-44.93000002,-61.3772666862021));
#166426=CARTESIAN_POINT('Ctrl Pts',(49.4663885772137,-44.93000002,-61.3502540659085));
#166427=CARTESIAN_POINT('Ctrl Pts',(49.4778548596161,-44.93000002,-61.33733758404));
#166428=CARTESIAN_POINT('Ctrl Pts',(49.4899767151879,-44.93000002,-61.3249865422103));
#166429=CARTESIAN_POINT('Ctrl Pts',(49.5026897554816,-44.93000002,-61.3132100906898));
#166430=CARTESIAN_POINT('Ctrl Pts',(49.5320647115447,-44.93000002,-61.2859992317605));
#166431=CARTESIAN_POINT('Ctrl Pts',(49.563760885477,-44.93000002,-61.2625146831493));
#166432=CARTESIAN_POINT('Ctrl Pts',(49.597554081752,-44.93000002,-61.2422777750133));
#166433=CARTESIAN_POINT('Ctrl Pts',(49.6090633503044,-44.93000002,-61.2353854997602));
#166434=CARTESIAN_POINT('Ctrl Pts',(49.6208161109919,-44.93000002,-61.2288703265774));
#166435=CARTESIAN_POINT('Ctrl Pts',(49.6328042123455,-44.93000002,-61.2227144603287));
#166436=CARTESIAN_POINT('Ctrl Pts',(49.679945666351,-44.93000002,-61.1985074172725));
#166437=CARTESIAN_POINT('Ctrl Pts',(49.7309938530465,-44.93000002,-61.1800821085049));
#166438=CARTESIAN_POINT('Ctrl Pts',(49.7824210964939,-44.93000002,-61.1680542343897));
#166439=CARTESIAN_POINT('Ctrl Pts',(49.833844605741,-44.93000002,-61.1560272336343));
#166440=CARTESIAN_POINT('Ctrl Pts',(49.8863934436428,-44.93000002,-61.14995));
#166441=CARTESIAN_POINT('Ctrl Pts',(49.940073970993,-44.93000002,-61.14995));
#166442=CARTESIAN_POINT('Ctrl Pts',(52.1700794675439,-38.5802945048887,
-61.2273317382593));
#166443=CARTESIAN_POINT('Ctrl Pts',(52.2861787013546,-38.28000002,-61.287642251635));
#166444=CARTESIAN_POINT('Ctrl Pts',(52.5768547844511,-38.28000002,-61.4386408691297));
#166445=CARTESIAN_POINT('Ctrl Pts',(52.238210979969,-38.595348210897,-61.0819498253042));
#166446=CARTESIAN_POINT('Ctrl Pts',(52.3399181230539,-38.28000002,-61.1584857199633));
#166447=CARTESIAN_POINT('Ctrl Pts',(52.6146146074011,-38.28000002,-61.3659524750795));
#166448=CARTESIAN_POINT('Ctrl Pts',(52.3391546482515,-38.6176244716287,
-60.958102271836));
#166449=CARTESIAN_POINT('Ctrl Pts',(52.4211494089633,-38.28000002,-61.0428817134857));
#166450=CARTESIAN_POINT('Ctrl Pts',(52.6705520955624,-38.28000002,-61.3040259447327));
#166451=CARTESIAN_POINT('Ctrl Pts',(52.4601060488528,-38.6442121687577,
-60.8635779995782));
#166452=CARTESIAN_POINT('Ctrl Pts',(52.5193575501107,-38.28000002,-60.9475523661893));
#166453=CARTESIAN_POINT('Ctrl Pts',(52.7375342894722,-38.28000002,-61.2567639997891));
#166454=CARTESIAN_POINT('',(52.7375342894721,-38.28000002,-61.2567639997892));
#166455=CARTESIAN_POINT('',(52.4601061170824,-38.6442121641745,-60.8635778131262));
#166456=CARTESIAN_POINT('Origin',(52.7375342894721,-38.78000002,-61.2567639997892));
#166457=CARTESIAN_POINT('Origin',(53.0240343600242,-38.7671930235723,-61.6028141108652));
#166458=CARTESIAN_POINT('Origin',(53.0468858549885,-38.28000002,-61.6241485284279));
#166459=CARTESIAN_POINT('Origin',(0.,-12.9675000200281,-60.64995));
#166460=CARTESIAN_POINT('Origin',(0.,-12.9675000200281,-61.2273317382593));
#166461=CARTESIAN_POINT('Origin',(57.,19.76999998,-174.34995));
#166462=CARTESIAN_POINT('',(57.,20.26999998,-176.84995));
#166463=CARTESIAN_POINT('Origin',(57.,19.76999998,-176.84995));
#166464=CARTESIAN_POINT('',(59.5,20.26999998,-174.34995));
#166465=CARTESIAN_POINT('Origin',(57.,20.26999998,-174.34995));
#166466=CARTESIAN_POINT('Origin',(59.5,19.76999998,-174.34995));
#166467=CARTESIAN_POINT('Origin',(59.5,19.76999998,-55.24995));
#166468=CARTESIAN_POINT('',(59.5,20.26999998,-58.24995));
#166469=CARTESIAN_POINT('',(59.5,20.26999998,-174.34995));
#166470=CARTESIAN_POINT('Origin',(59.5,19.76999998,-58.24995));
#166471=CARTESIAN_POINT('Ctrl Pts',(48.5401663778083,20.8005163310888,-60.6557251999476));
#166472=CARTESIAN_POINT('Ctrl Pts',(48.5428568992146,20.2699999800004,-60.6233186082983));
#166473=CARTESIAN_POINT('Ctrl Pts',(48.4967141407694,20.26999998,-61.1528286091218));
#166474=CARTESIAN_POINT('Ctrl Pts',(48.3258603491075,20.7405626834577,-60.6326588680102));
#166475=CARTESIAN_POINT('Ctrl Pts',(48.3312760425999,20.2699999799993,-60.6648966748951));
#166476=CARTESIAN_POINT('Ctrl Pts',(48.368727227854,20.26999998,-61.1413140584609));
#166477=CARTESIAN_POINT('Ctrl Pts',(48.0997023590435,20.6768759439098,-60.6786895616851));
#166478=CARTESIAN_POINT('Ctrl Pts',(48.123617249358,20.2699999800005,-60.7558947672151));
#166479=CARTESIAN_POINT('Ctrl Pts',(48.2334071498883,20.26999998,-61.1643439345927));
#166480=CARTESIAN_POINT('Ctrl Pts',(47.710945097327,20.5668610319491,-60.9089307872898));
#166481=CARTESIAN_POINT('Ctrl Pts',(47.7976044540999,20.2699999799995,-61.0163559243911));
#166482=CARTESIAN_POINT('Ctrl Pts',(48.000500083877,20.26999998,-61.2794769780549));
#166483=CARTESIAN_POINT('Ctrl Pts',(47.5431247912797,20.5190619893355,-61.0949662257924));
#166484=CARTESIAN_POINT('Ctrl Pts',(47.662880268204,20.2699999800005,-61.1871235536955));
#166485=CARTESIAN_POINT('Ctrl Pts',(47.8998003386288,20.26999998,-61.3724531273306));
#166486=CARTESIAN_POINT('Ctrl Pts',(47.4601025565285,20.4953747916186,-61.3483411114119));
#166487=CARTESIAN_POINT('Ctrl Pts',(47.5983464794385,20.2699999799998,-61.4016832893902));
#166488=CARTESIAN_POINT('Ctrl Pts',(47.8499146758921,20.26999998,-61.4991870244405));
#166489=CARTESIAN_POINT('',(47.878929697957,20.26999998,-61.4386408691297));
#166490=CARTESIAN_POINT('Origin',(47.878929697957,20.76999998,-61.4386408691297));
#166491=CARTESIAN_POINT('',(48.4322308821779,20.76999998,-60.64995));
#166492=CARTESIAN_POINT('Ctrl Pts',(48.4322308821779,20.76999998,-60.64995));
#166493=CARTESIAN_POINT('Ctrl Pts',(48.399722578391,20.7608881764303,-60.64995));
#166494=CARTESIAN_POINT('Ctrl Pts',(48.3683266666299,20.7520242857188,-60.6514739673707));
#166495=CARTESIAN_POINT('Ctrl Pts',(48.3381385205148,20.7434793708773,-60.6542240356935));
#166496=CARTESIAN_POINT('Ctrl Pts',(48.3071065638243,20.7346956109777,-60.6570509731531));
#166497=CARTESIAN_POINT('Ctrl Pts',(48.277350510797,20.7262486977711,-60.6611729491662));
#166498=CARTESIAN_POINT('Ctrl Pts',(48.2489294698721,20.7181846607773,-60.6662816822899));
#166499=CARTESIAN_POINT('Ctrl Pts',(48.2196862185314,20.709887334115,-60.6715382092119));
#166500=CARTESIAN_POINT('Ctrl Pts',(48.1918559318809,20.7019950860821,-60.6778389168705));
#166501=CARTESIAN_POINT('Ctrl Pts',(48.1654622162443,20.6945292505851,-60.6848721910989));
#166502=CARTESIAN_POINT('Ctrl Pts',(48.1378677797617,20.6867237742267,-60.6922254278175));
#166503=CARTESIAN_POINT('Ctrl Pts',(48.1118431759175,20.6793841107777,-60.7003788836451));
#166504=CARTESIAN_POINT('Ctrl Pts',(48.0873777720132,20.6725078124747,-60.7090106282434));
#166505=CARTESIAN_POINT('Ctrl Pts',(48.062292478069,20.6654572865626,-60.7178610789184));
#166506=CARTESIAN_POINT('Ctrl Pts',(48.038845789214,20.658893486969,-60.7272140672987));
#166507=CARTESIAN_POINT('Ctrl Pts',(48.016995772979,20.6527917612606,-60.7367639150856));
#166508=CARTESIAN_POINT('Ctrl Pts',(47.9943585023737,20.6464701908538,-60.7466578431389));
#166509=CARTESIAN_POINT('Ctrl Pts',(47.9734344086814,20.6406441600918,-60.756762814792));
#166510=CARTESIAN_POINT('Ctrl Pts',(47.9541541175128,20.6352694937039,-60.7667871712989));
#166511=CARTESIAN_POINT('Ctrl Pts',(47.9467623633479,20.6332089328799,-60.770630348682));
#166512=CARTESIAN_POINT('Ctrl Pts',(47.9396120395958,20.6312145793529,-60.77446218704));
#166513=CARTESIAN_POINT('Ctrl Pts',(47.9326986888512,20.6292835269848,-60.7782681307328));
#166514=CARTESIAN_POINT('Ctrl Pts',(47.9250776896262,20.6271548126834,-60.7824636496649));
#166515=CARTESIAN_POINT('Ctrl Pts',(47.9177446558436,20.6251030197031,-60.7866276814552));
#166516=CARTESIAN_POINT('Ctrl Pts',(47.9106933592237,20.623124049625,-60.7907421586884));
#166517=CARTESIAN_POINT('Ctrl Pts',(47.9071677109137,20.6221345645859,-60.7927993973051));
#166518=CARTESIAN_POINT('Ctrl Pts',(47.9037125043225,20.6211632904805,-60.7948442623793));
#166519=CARTESIAN_POINT('Ctrl Pts',(47.9003269328935,20.6202096924913,-60.7968746421038));
#166520=CARTESIAN_POINT('Ctrl Pts',(47.8986341471789,20.6197328934967,-60.797889831966));
#166521=CARTESIAN_POINT('Ctrl Pts',(47.8969587707282,20.619260513863,-60.7989014014781));
#166522=CARTESIAN_POINT('Ctrl Pts',(47.8953007039598,20.6187924875234,-60.7999090937751));
#166523=CARTESIAN_POINT('Ctrl Pts',(47.8939271861499,20.6184047814762,-60.8007438510618));
#166524=CARTESIAN_POINT('Ctrl Pts',(47.893382665496,20.6182516173075,-60.8010750695854));
#166525=CARTESIAN_POINT('Ctrl Pts',(47.8916362218411,20.6177573754894,-60.8021469852348));
#166526=CARTESIAN_POINT('Ctrl Pts',(47.8912744145753,20.6176549843929,-60.8023690518724));
#166527=CARTESIAN_POINT('Ctrl Pts',(47.8908610878189,20.6175379989838,-60.8026230349715));
#166528=CARTESIAN_POINT('Ctrl Pts',(47.8903783339695,20.6174014028689,-60.8029202868589));
#166529=CARTESIAN_POINT('Ctrl Pts',(47.8567603545224,20.6078891319896,-60.8236202934009));
#166530=CARTESIAN_POINT('Ctrl Pts',(47.8249183854607,20.5988369606764,-60.8459276154961));
#166531=CARTESIAN_POINT('Ctrl Pts',(47.7949209542359,20.5903002472954,-60.8695267047893));
#166532=CARTESIAN_POINT('Ctrl Pts',(47.7643887817459,20.5816113564535,-60.8935464769994));
#166533=CARTESIAN_POINT('Ctrl Pts',(47.7357672715377,20.5734563241395,-60.918903986338));
#166534=CARTESIAN_POINT('Ctrl Pts',(47.7090862256909,20.5658629872418,-60.9452797566578));
#166535=CARTESIAN_POINT('Ctrl Pts',(47.6816764704408,20.558062262072,-60.9723758987336));
#166536=CARTESIAN_POINT('Ctrl Pts',(47.6563143907701,20.5508541852985,-61.0005461949134));
#166537=CARTESIAN_POINT('Ctrl Pts',(47.6329913081009,20.5442391521648,-61.0294657761639));
#166538=CARTESIAN_POINT('Ctrl Pts',(47.6092897534091,20.5375167745173,-61.0588546458253));
#166539=CARTESIAN_POINT('Ctrl Pts',(47.5876935481731,20.5314065997584,-61.089016935168));
#166540=CARTESIAN_POINT('Ctrl Pts',(47.5681564806293,20.5258817901274,-61.1196402525177));
#166541=CARTESIAN_POINT('Ctrl Pts',(47.5481621754662,20.5202276800885,-61.1509802655888));
#166542=CARTESIAN_POINT('Ctrl Pts',(47.5303241501823,20.5151864019244,-61.1828027952977));
#166543=CARTESIAN_POINT('Ctrl Pts',(47.5145598665705,20.5107046588175,-61.2148083010891));
#166544=CARTESIAN_POINT('Ctrl Pts',(47.512505186092,20.510120518726,-61.2189798251225));
#166545=CARTESIAN_POINT('Ctrl Pts',(47.5104856938792,20.5095458537873,-61.2231545095474));
#166546=CARTESIAN_POINT('Ctrl Pts',(47.508501172308,20.508980519813,-61.2273317382593));
#166547=CARTESIAN_POINT('',(48.4322308821779,20.26999998,-61.14995));
#166548=CARTESIAN_POINT('Origin',(48.4322308821779,20.76999998,-61.14995));
#166549=CARTESIAN_POINT('Ctrl Pts',(47.878929697957,20.26999998,-61.4386408691297));
#166550=CARTESIAN_POINT('Ctrl Pts',(47.8974331987387,20.26999998,-61.4062039153374));
#166551=CARTESIAN_POINT('Ctrl Pts',(47.919537961559,20.26999998,-61.3763755387993));
#166552=CARTESIAN_POINT('Ctrl Pts',(47.9444691614871,20.26999998,-61.3492604871255));
#166553=CARTESIAN_POINT('Ctrl Pts',(47.972080538841,20.26999998,-61.319230487531));
#166554=CARTESIAN_POINT('Ctrl Pts',(48.003157746836,20.26999998,-61.2925292835119));
#166555=CARTESIAN_POINT('Ctrl Pts',(48.0365924563169,20.26999998,-61.2692603439464));
#166556=CARTESIAN_POINT('Ctrl Pts',(48.0621704908697,20.26999998,-61.2514592698694));
#166557=CARTESIAN_POINT('Ctrl Pts',(48.0891267715872,20.26999998,-61.2356661036975));
#166558=CARTESIAN_POINT('Ctrl Pts',(48.1169536143029,20.26999998,-61.2219104511051));
#166559=CARTESIAN_POINT('Ctrl Pts',(48.1430951909369,20.26999998,-61.2089878766662));
#166560=CARTESIAN_POINT('Ctrl Pts',(48.1700747212765,20.26999998,-61.1978560977682));
#166561=CARTESIAN_POINT('Ctrl Pts',(48.1976781569078,20.26999998,-61.1884510370574));
#166562=CARTESIAN_POINT('Ctrl Pts',(48.2258927336206,20.26999998,-61.1788377479562));
#166563=CARTESIAN_POINT('Ctrl Pts',(48.2547605141936,20.26999998,-61.171028311645));
#166564=CARTESIAN_POINT('Ctrl Pts',(48.2840750385862,20.26999998,-61.1650052516751));
#166565=CARTESIAN_POINT('Ctrl Pts',(48.3128848180535,20.26999998,-61.1590858982813));
#166566=CARTESIAN_POINT('Ctrl Pts',(48.3421274958275,20.26999998,-61.1548920321836));
#166567=CARTESIAN_POINT('Ctrl Pts',(48.3716073656792,20.26999998,-61.1524557732793));
#166568=CARTESIAN_POINT('Ctrl Pts',(48.391727124007,20.26999998,-61.1507930474726));
#166569=CARTESIAN_POINT('Ctrl Pts',(48.4119573716396,20.26999998,-61.14995));
#166570=CARTESIAN_POINT('Ctrl Pts',(48.4322308821779,20.26999998,-61.14995));
#166571=CARTESIAN_POINT('Ctrl Pts',(40.8552491802306,20.26999998,-73.4195575571114));
#166572=CARTESIAN_POINT('Ctrl Pts',(40.6336903802598,20.26999998,-73.2855702871256));
#166573=CARTESIAN_POINT('Ctrl Pts',(40.5058324224785,20.4814581622114,-73.2082484262411));
#166574=CARTESIAN_POINT('Ctrl Pts',(43.2510347775237,20.26999998,-69.4579320833189));
#166575=CARTESIAN_POINT('Ctrl Pts',(43.0367110660153,20.26999998,-69.2967901887638));
#166576=CARTESIAN_POINT('Ctrl Pts',(42.8933128344149,20.4915183317059,-69.2466191256953));
#166577=CARTESIAN_POINT('Ctrl Pts',(45.5849829096511,20.26999998,-65.4599688790667));
#166578=CARTESIAN_POINT('Ctrl Pts',(45.3606391668745,20.269999980008,-65.3006916020456));
#166579=CARTESIAN_POINT('Ctrl Pts',(45.2204439541918,20.5006239318743,-65.2486577002759));
#166580=CARTESIAN_POINT('Ctrl Pts',(47.878929697957,20.26999998,-61.4386408691297));
#166581=CARTESIAN_POINT('Ctrl Pts',(47.6355531845903,20.26999998,-61.2998079338862));
#166582=CARTESIAN_POINT('Ctrl Pts',(47.508501172308,20.508980519813,-61.2273317382593));
#166583=CARTESIAN_POINT('',(40.8552491802306,20.26999998,-73.4195575571114));
#166584=CARTESIAN_POINT('Origin',(40.8552491802306,20.76999998,-73.4195575571114));
#166585=CARTESIAN_POINT('Ctrl Pts',(40.8552491802306,20.26999998,-73.4195575571114));
#166586=CARTESIAN_POINT('Ctrl Pts',(43.2510477030711,20.26999998,-69.4579107098797));
#166587=CARTESIAN_POINT('Ctrl Pts',(45.5849708137067,20.26999998,-65.4599900833935));
#166588=CARTESIAN_POINT('Ctrl Pts',(47.878929697957,20.26999998,-61.4386408691297));
#166589=CARTESIAN_POINT('Ctrl Pts',(40.5057626875991,20.4815735279761,-73.2082062542032));
#166590=CARTESIAN_POINT('Ctrl Pts',(40.6336137367886,20.26999998,-73.2855239371297));
#166591=CARTESIAN_POINT('Ctrl Pts',(40.8552491802306,20.26999998,-73.4195575571114));
#166592=CARTESIAN_POINT('Ctrl Pts',(40.2348040052479,20.5032631524898,-73.6266590242966));
#166593=CARTESIAN_POINT('Ctrl Pts',(40.36273680226,20.26999998,-73.7004454481632));
#166594=CARTESIAN_POINT('Ctrl Pts',(40.611373197132,20.26999998,-73.8228262549259));
#166595=CARTESIAN_POINT('Ctrl Pts',(40.0115963838279,20.5258775774689,-74.0630752877361));
#166596=CARTESIAN_POINT('Ctrl Pts',(40.140116113121,20.26999998,-74.1289328806859));
#166597=CARTESIAN_POINT('Ctrl Pts',(40.4104980509131,20.26999998,-74.2432272518665));
#166598=CARTESIAN_POINT('Ctrl Pts',(39.6351601117623,20.5724303588935,-74.9618949473625));
#166599=CARTESIAN_POINT('Ctrl Pts',(39.75639920405,20.26999998,-75.0104621522509));
#166600=CARTESIAN_POINT('Ctrl Pts',(40.0717001001047,20.26999998,-75.1087680536759));
#166601=CARTESIAN_POINT('Ctrl Pts',(39.4823650047626,20.5963820683904,-75.4245552669206));
#166602=CARTESIAN_POINT('Ctrl Pts',(39.5971879815112,20.26999998,-75.4662299884762));
#166603=CARTESIAN_POINT('Ctrl Pts',(39.9341806290214,20.26999998,-75.5541367565536));
#166604=CARTESIAN_POINT('Ctrl Pts',(39.116363283268,20.6699824412149,-76.8472597580483));
#166605=CARTESIAN_POINT('Ctrl Pts',(39.1910923623951,20.26999998,-76.8948600995692));
#166606=CARTESIAN_POINT('Ctrl Pts',(39.6047590085956,20.26999998,-76.9230972788123));
#166607=CARTESIAN_POINT('Ctrl Pts',(38.999978189647,20.7198888639429,-77.8132651533063));
#166608=CARTESIAN_POINT('Ctrl Pts',(39.0477122635571,20.2699999800001,-77.8601979059779));
#166609=CARTESIAN_POINT('Ctrl Pts',(39.5000000011617,20.26999998,-77.8518474726923));
#166610=CARTESIAN_POINT('Ctrl Pts',(39.0000000471688,20.7702171638925,-78.7897987614795));
#166611=CARTESIAN_POINT('Ctrl Pts',(38.9997827689182,20.26999998,-78.7897987614795));
#166612=CARTESIAN_POINT('Ctrl Pts',(39.5,20.26999998,-78.7897987614789));
#166613=CARTESIAN_POINT('',(39.5,20.26999998,-78.7897987614789));
#166614=CARTESIAN_POINT('Origin',(39.5,20.76999998,-78.7897987614789));
#166615=CARTESIAN_POINT('Ctrl Pts',(39.5,20.26999998,-78.7897987614789));
#166616=CARTESIAN_POINT('Ctrl Pts',(39.4999999999996,20.26999998,-78.4276754534812));
#166617=CARTESIAN_POINT('Ctrl Pts',(39.5156108303728,20.26999998,-78.0671937952867));
#166618=CARTESIAN_POINT('Ctrl Pts',(39.5473687221686,20.26999998,-77.7085899056868));
#166619=CARTESIAN_POINT('Ctrl Pts',(39.5782679790923,20.26999998,-77.3596815527704));
#166620=CARTESIAN_POINT('Ctrl Pts',(39.6244528955633,20.26999998,-77.0125506150102));
#166621=CARTESIAN_POINT('Ctrl Pts',(39.6864661720935,20.26999998,-76.6674187362214));
#166622=CARTESIAN_POINT('Ctrl Pts',(39.725963031717,20.26999998,-76.4476008821939));
#166623=CARTESIAN_POINT('Ctrl Pts',(39.7718817094829,20.26999998,-76.2285940465882));
#166624=CARTESIAN_POINT('Ctrl Pts',(39.8243734219799,20.26999998,-76.0104569305838));
#166625=CARTESIAN_POINT('Ctrl Pts',(39.9341806286948,20.26999998,-75.5541367564111));
#166626=CARTESIAN_POINT('Ctrl Pts',(40.0717001000673,20.26999998,-75.1087680536983));
#166627=CARTESIAN_POINT('Ctrl Pts',(40.2410990749131,20.26999998,-74.6759976525381));
#166628=CARTESIAN_POINT('Ctrl Pts',(40.3724674808252,20.26999998,-74.3403854814604));
#166629=CARTESIAN_POINT('Ctrl Pts',(40.5227478579286,20.26999998,-74.0122470450776));
#166630=CARTESIAN_POINT('Ctrl Pts',(40.6973553852854,20.26999998,-73.6937223220652));
#166631=CARTESIAN_POINT('Ctrl Pts',(40.7479034874671,20.26999998,-73.60151083216));
#166632=CARTESIAN_POINT('Ctrl Pts',(40.800490685591,20.26999998,-73.510105161834));
#166633=CARTESIAN_POINT('Ctrl Pts',(40.8552491802306,20.26999998,-73.4195575571114));
#166634=CARTESIAN_POINT('Origin',(39.5,20.76999998,-55.24995));
#166635=CARTESIAN_POINT('',(39.5,20.26999998,-153.26884421004));
#166636=CARTESIAN_POINT('Origin',(39.5,20.76999998,-153.26884421004));
#166637=CARTESIAN_POINT('',(39.5,20.26999998,-55.24995));
#166638=CARTESIAN_POINT('Ctrl Pts',(39.,20.76999998,-153.26884421004));
#166639=CARTESIAN_POINT('Ctrl Pts',(39.,20.26999998,-153.26884421004));
#166640=CARTESIAN_POINT('Ctrl Pts',(39.5,20.26999998,-153.26884421004));
#166641=CARTESIAN_POINT('Ctrl Pts',(39.,20.7196410046276,-154.246185133485));
#166642=CARTESIAN_POINT('Ctrl Pts',(39.0479377066243,20.26999998,-154.199194380993));
#166643=CARTESIAN_POINT('Ctrl Pts',(39.5000000013484,20.26999998,-154.20759288104));
#166644=CARTESIAN_POINT('Ctrl Pts',(39.1162573309359,20.6699959324755,-155.207409347787));
#166645=CARTESIAN_POINT('Ctrl Pts',(39.1910773834404,20.26999998,-155.160229045822));
#166646=CARTESIAN_POINT('Ctrl Pts',(39.6046315964214,20.26999998,-155.13174861728));
#166647=CARTESIAN_POINT('Ctrl Pts',(39.4789868412919,20.5968217552646,-156.622386886066));
#166648=CARTESIAN_POINT('Ctrl Pts',(39.5936890623428,20.26999998,-156.580982897093));
#166649=CARTESIAN_POINT('Ctrl Pts',(39.9310881578732,20.26999998,-156.493265246185));
#166650=CARTESIAN_POINT('Ctrl Pts',(39.6331118787012,20.5725600557084,-157.091220397978));
#166651=CARTESIAN_POINT('Ctrl Pts',(39.7543133491109,20.26999998,-157.042666916184));
#166652=CARTESIAN_POINT('Ctrl Pts',(40.0698006899404,20.26999998,-156.944576655439));
#166653=CARTESIAN_POINT('Ctrl Pts',(40.0111570472454,20.5257809479637,-157.994781653225));
#166654=CARTESIAN_POINT('Ctrl Pts',(40.1396850110498,20.26999998,-157.928861059881));
#166655=CARTESIAN_POINT('Ctrl Pts',(40.4100413434116,20.26999998,-157.81469163798));
#166656=CARTESIAN_POINT('Ctrl Pts',(40.2350800433575,20.5031211311407,-158.43226426538));
#166657=CARTESIAN_POINT('Ctrl Pts',(40.3630340966184,20.26999998,-158.358476471872));
#166658=CARTESIAN_POINT('Ctrl Pts',(40.6115602809737,20.26999998,-158.236126075511));
#166659=CARTESIAN_POINT('Ctrl Pts',(40.5058324224674,20.4814581622123,-158.850394545248));
#166660=CARTESIAN_POINT('Ctrl Pts',(40.6336903802489,20.26999998,-158.773072684364));
#166661=CARTESIAN_POINT('Ctrl Pts',(40.8552491802207,20.26999998,-158.639085414378));
#166662=CARTESIAN_POINT('',(40.8552491802207,20.26999998,-158.639085414378));
#166663=CARTESIAN_POINT('Origin',(40.8552491802207,20.76999998,-158.639085414378));
#166664=CARTESIAN_POINT('Ctrl Pts',(40.8552491802207,20.26999998,-158.639085414378));
#166665=CARTESIAN_POINT('Ctrl Pts',(40.6523563183102,20.26999998,-158.303585638821));
#166666=CARTESIAN_POINT('Ctrl Pts',(40.4787269326948,20.26999998,-157.955339387382));
#166667=CARTESIAN_POINT('Ctrl Pts',(40.3280973119772,20.26999998,-157.597074989874));
#166668=CARTESIAN_POINT('Ctrl Pts',(40.2977909470356,20.26999998,-157.524992941704));
#166669=CARTESIAN_POINT('Ctrl Pts',(40.2684157827767,20.26999998,-157.452505284537));
#166670=CARTESIAN_POINT('Ctrl Pts',(40.2399210161217,20.26999998,-157.379634146926));
#166671=CARTESIAN_POINT('Ctrl Pts',(40.0698006898873,20.26999998,-156.944576655372));
#166672=CARTESIAN_POINT('Ctrl Pts',(39.9310881570987,20.26999998,-156.493265246319));
#166673=CARTESIAN_POINT('Ctrl Pts',(39.8222693035354,20.26999998,-156.039426370008));
#166674=CARTESIAN_POINT('Ctrl Pts',(39.7053251420368,20.26999998,-155.551700161656));
#166675=CARTESIAN_POINT('Ctrl Pts',(39.6210196491341,20.26999998,-155.059280307642));
#166676=CARTESIAN_POINT('Ctrl Pts',(39.5680311845015,20.26999998,-154.562356823708));
#166677=CARTESIAN_POINT('Ctrl Pts',(39.5224060219208,20.26999998,-154.134486061611));
#166678=CARTESIAN_POINT('Ctrl Pts',(39.5,20.26999998,-153.703276192992));
#166679=CARTESIAN_POINT('Ctrl Pts',(39.5,20.26999998,-153.26884421004));
#166680=CARTESIAN_POINT('Ctrl Pts',(48.0164881467928,20.26999998,-170.861259130871));
#166681=CARTESIAN_POINT('Ctrl Pts',(47.7727200234913,20.26999998,-171.000183411942));
#166682=CARTESIAN_POINT('Ctrl Pts',(47.6457075325507,20.5094809071607,-171.07256826174));
#166683=CARTESIAN_POINT('Ctrl Pts',(45.6783453674058,20.26999998,-166.758558919217));
#166684=CARTESIAN_POINT('Ctrl Pts',(45.4541703457615,20.2699999799837,-166.918724083766));
#166685=CARTESIAN_POINT('Ctrl Pts',(45.3135333962397,20.5009878795767,-166.96987023406));
#166686=CARTESIAN_POINT('Ctrl Pts',(43.2989471172158,20.26999998,-162.679937821406));
#166687=CARTESIAN_POINT('Ctrl Pts',(43.0850828436089,20.26999998,-162.842145218595));
#166688=CARTESIAN_POINT('Ctrl Pts',(42.941059217223,20.4917195215043,-162.891251079751));
#166689=CARTESIAN_POINT('Ctrl Pts',(40.8552491802207,20.26999998,-158.639085414378));
#166690=CARTESIAN_POINT('Ctrl Pts',(40.6336903802499,20.26999998,-158.773072684364));
#166691=CARTESIAN_POINT('Ctrl Pts',(40.5058324224685,20.4814581622113,-158.850394545248));
#166692=CARTESIAN_POINT('',(48.0164881467928,20.26999998,-170.861259130871));
#166693=CARTESIAN_POINT('Origin',(48.0164881467928,20.76999998,-170.861259130871));
#166694=CARTESIAN_POINT('Ctrl Pts',(48.0164881467928,20.26999998,-170.861259130871));
#166695=CARTESIAN_POINT('Ctrl Pts',(45.678332174125,20.26999998,-166.758535769278));
#166696=CARTESIAN_POINT('Ctrl Pts',(43.29896123138,20.26999998,-162.67996116032));
#166697=CARTESIAN_POINT('Ctrl Pts',(40.8552491802207,20.26999998,-158.639085414378));
#166698=CARTESIAN_POINT('Ctrl Pts',(47.5981304714751,20.4959940009177,-170.953449037984));
#166699=CARTESIAN_POINT('Ctrl Pts',(47.7361803032393,20.2699999799996,-170.899850076481));
#166700=CARTESIAN_POINT('Ctrl Pts',(47.9879536642768,20.26999998,-170.801687503914));
#166701=CARTESIAN_POINT('Ctrl Pts',(47.6795757723456,20.5191819878533,-171.201996012878));
#166702=CARTESIAN_POINT('Ctrl Pts',(47.7994410651643,20.2699999800006,-171.110340027154));
#166703=CARTESIAN_POINT('Ctrl Pts',(48.0368367588952,20.26999998,-170.925976258083));
#166704=CARTESIAN_POINT('Ctrl Pts',(47.8461118288466,20.5665218710759,-171.389416721024));
#166705=CARTESIAN_POINT('Ctrl Pts',(47.9331941373512,20.26999998,-171.282098957825));
#166706=CARTESIAN_POINT('Ctrl Pts',(48.1367170179081,20.26999998,-171.019673785838));
#166707=CARTESIAN_POINT('Ctrl Pts',(48.2369635182516,20.6769092692865,-171.621547588333));
#166708=CARTESIAN_POINT('Ctrl Pts',(48.2608982797316,20.26999998,-171.544336769923));
#166709=CARTESIAN_POINT('Ctrl Pts',(48.370721955878,20.26999998,-171.135742484204));
#166710=CARTESIAN_POINT('Ctrl Pts',(48.4597228298326,20.7395177616212,-171.667100514749));
#166711=CARTESIAN_POINT('Ctrl Pts',(48.4654155591074,20.2699999799989,-171.633931058418));
#166712=CARTESIAN_POINT('Ctrl Pts',(48.5039132591497,20.26999998,-171.158522665518));
#166713=CARTESIAN_POINT('Ctrl Pts',(48.6790987479349,20.8007757752918,-171.644223713054));
#166714=CARTESIAN_POINT('Ctrl Pts',(48.6818136557496,20.2699999800007,-171.676865614123));
#166715=CARTESIAN_POINT('Ctrl Pts',(48.6348374950401,20.26999998,-171.147089237505));
#166716=CARTESIAN_POINT('',(48.5692718988023,20.26999998,-171.14995));
#166717=CARTESIAN_POINT('Origin',(48.5692718988023,20.76999998,-171.14995));
#166718=CARTESIAN_POINT('Ctrl Pts',(48.5692718988023,20.26999998,-171.14995));
#166719=CARTESIAN_POINT('Ctrl Pts',(48.5047948684884,20.26999998,-171.14995));
#166720=CARTESIAN_POINT('Ctrl Pts',(48.4405703346722,20.26999998,-171.141645130582));
#166721=CARTESIAN_POINT('Ctrl Pts',(48.3787338163827,20.26999998,-171.124930042697));
#166722=CARTESIAN_POINT('Ctrl Pts',(48.3356628951308,20.26999998,-171.113287501138));
#166723=CARTESIAN_POINT('Ctrl Pts',(48.2937500450339,20.26999998,-171.097563680329));
#166724=CARTESIAN_POINT('Ctrl Pts',(48.2537194844918,20.26999998,-171.077708139862));
#166725=CARTESIAN_POINT('Ctrl Pts',(48.2190067257616,20.26999998,-171.060490279898));
#166726=CARTESIAN_POINT('Ctrl Pts',(48.1858587814802,20.26999998,-171.04016650214));
#166727=CARTESIAN_POINT('Ctrl Pts',(48.1550885346326,20.26999998,-171.016846515546));
#166728=CARTESIAN_POINT('Ctrl Pts',(48.127107857359,20.26999998,-170.995640672702));
#166729=CARTESIAN_POINT('Ctrl Pts',(48.1010921834753,20.26999998,-170.971956505701));
#166730=CARTESIAN_POINT('Ctrl Pts',(48.0776779540546,20.26999998,-170.945845192496));
#166731=CARTESIAN_POINT('Ctrl Pts',(48.0545175809095,20.26999998,-170.920016977257));
#166732=CARTESIAN_POINT('Ctrl Pts',(48.0339013190985,20.26999998,-170.891813734436));
#166733=CARTESIAN_POINT('Ctrl Pts',(48.0164881467928,20.26999998,-170.861259130871));
#166734=CARTESIAN_POINT('Origin',(1.41024658483895E-14,20.76999998,-171.14995));
#166735=CARTESIAN_POINT('',(50.4557527353536,20.26999998,-171.14995));
#166736=CARTESIAN_POINT('Origin',(50.4557527353536,20.76999998,-171.14995));
#166737=CARTESIAN_POINT('',(48.9127966158122,20.26999998,-171.14995));
#166738=CARTESIAN_POINT('Ctrl Pts',(51.9704940941315,20.26999998,-172.64995));
#166739=CARTESIAN_POINT('Ctrl Pts',(51.5358507252234,20.26999998,-172.64995));
#166740=CARTESIAN_POINT('Ctrl Pts',(51.4753600597607,20.70041342952,-172.64995));
#166741=CARTESIAN_POINT('Ctrl Pts',(51.9704940941145,20.26999998,-172.453565067926));
#166742=CARTESIAN_POINT('Ctrl Pts',(51.5358507252071,20.26999998,-172.511015867074));
#166743=CARTESIAN_POINT('Ctrl Pts',(51.4753600597603,20.7004134295229,-172.51902671195));
#166744=CARTESIAN_POINT('Ctrl Pts',(51.9310694254183,20.26999998,-172.257328160063));
#166745=CARTESIAN_POINT('Ctrl Pts',(51.5060950400989,20.26999998,-172.371853931892));
#166746=CARTESIAN_POINT('Ctrl Pts',(51.4488224064852,20.7022245814263,-172.38820210671));
#166747=CARTESIAN_POINT('Ctrl Pts',(51.7793131221354,20.26999998,-171.894521542842));
#166748=CARTESIAN_POINT('Ctrl Pts',(51.3932840309667,20.26999998,-172.118296873734));
#166749=CARTESIAN_POINT('Ctrl Pts',(51.3466717406587,20.7091961991206,-172.14633102856));
#166750=CARTESIAN_POINT('Ctrl Pts',(51.6670411644938,20.26999998,-171.728129909852));
#166751=CARTESIAN_POINT('Ctrl Pts',(51.3097149387001,20.2699999800017,-172.003556970023));
#166752=CARTESIAN_POINT('Ctrl Pts',(51.2710988980251,20.7143539233764,-172.035403273235));
#166753=CARTESIAN_POINT('Ctrl Pts',(51.3866320792846,20.26999998,-171.450449746589));
#166754=CARTESIAN_POINT('Ctrl Pts',(51.105269719327,20.2699999799983,-171.817687494207));
#166755=CARTESIAN_POINT('Ctrl Pts',(51.0823490791536,20.727235793176,-171.850283164392));
#166756=CARTESIAN_POINT('Ctrl Pts',(51.2186052206426,20.26999998,-171.339270411997));
#166757=CARTESIAN_POINT('Ctrl Pts',(50.9837060031699,20.26999998,-171.746711574348));
#166758=CARTESIAN_POINT('Ctrl Pts',(50.9692463274684,20.7349548730131,-171.776163607997));
#166759=CARTESIAN_POINT('Ctrl Pts',(50.8522330947096,20.26999998,-171.18899099047));
#166760=CARTESIAN_POINT('Ctrl Pts',(50.725270742269,20.26999998,-171.658003579003));
#166761=CARTESIAN_POINT('Ctrl Pts',(50.7226328043762,20.7517858470187,-171.675977326981));
#166762=CARTESIAN_POINT('Ctrl Pts',(50.6540676547286,20.26999998,-171.149950000016));
#166763=CARTESIAN_POINT('Ctrl Pts',(50.5880011641168,20.26999998,-171.640924254979));
#166764=CARTESIAN_POINT('Ctrl Pts',(50.5892430788785,20.760889480001,-171.64995));
#166765=CARTESIAN_POINT('Ctrl Pts',(50.4557527353536,20.26999998,-171.14995));
#166766=CARTESIAN_POINT('Ctrl Pts',(50.4557527353535,20.26999998,-171.64995));
#166767=CARTESIAN_POINT('Ctrl Pts',(50.4557527353536,20.76999998,-171.64995));
#166768=CARTESIAN_POINT('',(51.9704940941315,20.26999998,-172.64995));
#166769=CARTESIAN_POINT('Origin',(51.9704940941315,20.76999998,-172.64995));
#166770=CARTESIAN_POINT('Ctrl Pts',(51.9704940941315,20.26999998,-172.64995));
#166771=CARTESIAN_POINT('Ctrl Pts',(51.9704940941145,20.26999998,-172.453565067926));
#166772=CARTESIAN_POINT('Ctrl Pts',(51.9310694254183,20.26999998,-172.257328160063));
#166773=CARTESIAN_POINT('Ctrl Pts',(51.7793131221354,20.26999998,-171.894521542842));
#166774=CARTESIAN_POINT('Ctrl Pts',(51.6670411644938,20.26999998,-171.728129909852));
#166775=CARTESIAN_POINT('Ctrl Pts',(51.3866320792846,20.26999998,-171.450449746589));
#166776=CARTESIAN_POINT('Ctrl Pts',(51.2186052206426,20.26999998,-171.339270411997));
#166777=CARTESIAN_POINT('Ctrl Pts',(50.8522330947096,20.26999998,-171.18899099047));
#166778=CARTESIAN_POINT('Ctrl Pts',(50.6540676547286,20.26999998,-171.149950000016));
#166779=CARTESIAN_POINT('Ctrl Pts',(50.4557527353536,20.26999998,-171.14995));
#166780=CARTESIAN_POINT('Origin',(51.9704940941315,20.76999998,-171.64995));
#166781=CARTESIAN_POINT('',(51.4753600597607,20.70041342952,-171.64995));
#166782=CARTESIAN_POINT('',(51.9704940941315,20.26999998,-55.24995));
#166783=CARTESIAN_POINT('Origin',(60.,19.76999998,-176.84995));
#166784=CARTESIAN_POINT('',(-83.2809572255632,20.2699999800001,-176.84995));
#166785=CARTESIAN_POINT('Origin',(57.,19.76999998,-58.24995));
#166786=CARTESIAN_POINT('',(57.,20.26999998,-55.74995));
#166787=CARTESIAN_POINT('Origin',(57.,20.26999998,-58.24995));
#166788=CARTESIAN_POINT('',(57.,19.76999998,-55.24995));
#166789=CARTESIAN_POINT('Origin',(57.,19.76999998,-55.74995));
#166790=CARTESIAN_POINT('Origin',(57.,19.76999998,-58.24995));
#166791=CARTESIAN_POINT('Origin',(57.,-2.42462934179819E-14,-58.24995));
#166792=CARTESIAN_POINT('',(57.,19.26999998,-55.24995));
#166793=CARTESIAN_POINT('',(57.,28.41999998,-55.24995));
#166794=CARTESIAN_POINT('Origin',(57.,19.26999998,-58.24995));
#166795=CARTESIAN_POINT('Origin',(57.,19.26999998,-58.24995));
#166796=CARTESIAN_POINT('',(57.,18.76999998,-55.74995));
#166797=CARTESIAN_POINT('Origin',(57.,19.26999998,-55.74995));
#166798=CARTESIAN_POINT('',(59.5,18.76999998,-58.24995));
#166799=CARTESIAN_POINT('Origin',(57.,18.76999998,-58.24995));
#166800=CARTESIAN_POINT('Origin',(59.5,19.26999998,-58.24995));
#166801=CARTESIAN_POINT('Origin',(59.5,19.26999998,-55.24995));
#166802=CARTESIAN_POINT('',(59.5,18.76999998,-174.34995));
#166803=CARTESIAN_POINT('',(59.5,18.76999998,-58.24995));
#166804=CARTESIAN_POINT('Origin',(59.5,19.26999998,-174.34995));
#166805=CARTESIAN_POINT('Origin',(57.,19.26999998,-174.34995));
#166806=CARTESIAN_POINT('',(57.,18.76999998,-176.84995));
#166807=CARTESIAN_POINT('Origin',(57.,18.76999998,-174.34995));
#166808=CARTESIAN_POINT('Origin',(57.,19.26999998,-176.84995));
#166809=CARTESIAN_POINT('Origin',(-83.2809572255632,19.26999998,-176.84995));
#166810=CARTESIAN_POINT('',(-83.2809572255632,18.7699999800001,-176.84995));
#166811=CARTESIAN_POINT('Origin',(52.3218461808875,18.26999998,-171.64995));
#166812=CARTESIAN_POINT('',(52.3218461808875,18.76999998,-172.64995));
#166813=CARTESIAN_POINT('',(52.3218461808875,18.76999998,-55.24995));
#166814=CARTESIAN_POINT('Origin',(52.3218461808875,18.26999998,-172.64995));
#166815=CARTESIAN_POINT('',(51.8267121465167,18.20041342952,-171.64995));
#166816=CARTESIAN_POINT('Ctrl Pts',(50.8069033782914,18.76999998,-171.149950013428));
#166817=CARTESIAN_POINT('Ctrl Pts',(50.8069691716108,18.76999998,-171.65003477338));
#166818=CARTESIAN_POINT('Ctrl Pts',(50.8069692256435,18.2699152183756,-171.649950001854));
#166819=CARTESIAN_POINT('Ctrl Pts',(51.0052855451476,18.76999998,-171.149923566191));
#166820=CARTESIAN_POINT('Ctrl Pts',(50.9417879142081,18.76999998,-171.659221103016));
#166821=CARTESIAN_POINT('Ctrl Pts',(50.9405045947988,18.2608007878192,-171.649930655763));
#166822=CARTESIAN_POINT('Ctrl Pts',(51.2035231560588,18.76999998,-171.188965548735));
#166823=CARTESIAN_POINT('Ctrl Pts',(51.071213531544,18.7699999800004,-171.695281914067));
#166824=CARTESIAN_POINT('Ctrl Pts',(51.0739436419031,18.251693043142,-171.675956808334));
#166825=CARTESIAN_POINT('Ctrl Pts',(51.5699573073986,18.76999998,-171.339270411997));
#166826=CARTESIAN_POINT('Ctrl Pts',(51.3040045310345,18.7699999799997,-171.81002165518));
#166827=CARTESIAN_POINT('Ctrl Pts',(51.3206014184843,18.2348578535175,-171.776157476854));
#166828=CARTESIAN_POINT('Ctrl Pts',(51.7379841660413,18.76999998,-171.450449746589));
#166829=CARTESIAN_POINT('Ctrl Pts',(51.406565936193,18.7699999800021,-171.889069508912));
#166830=CARTESIAN_POINT('Ctrl Pts',(51.4337060393708,18.2271381960672,-171.850276197782));
#166831=CARTESIAN_POINT('Ctrl Pts',(52.0183932512491,18.76999998,-171.728129909852));
#166832=CARTESIAN_POINT('Ctrl Pts',(51.5741992781134,18.769999979998,-172.075284894373));
#166833=CARTESIAN_POINT('Ctrl Pts',(51.6224595301836,18.2142554277381,-172.035396209825));
#166834=CARTESIAN_POINT('Ctrl Pts',(52.1306652088914,18.76999998,-171.894521542842));
#166835=CARTESIAN_POINT('Ctrl Pts',(51.6384601923106,18.76999998,-172.182240159754));
#166836=CARTESIAN_POINT('Ctrl Pts',(51.6980343154967,18.2090973697629,-172.14632470545));
#166837=CARTESIAN_POINT('Ctrl Pts',(52.282447203939,18.76999998,-172.257389581842));
#166838=CARTESIAN_POINT('Ctrl Pts',(51.7248942642808,18.76999998,-172.409795949396));
#166839=CARTESIAN_POINT('Ctrl Pts',(51.8002049408554,18.2021241406569,-172.388239289312));
#166840=CARTESIAN_POINT('Ctrl Pts',(52.3218728744769,18.76999998,-172.453697958274));
#166841=CARTESIAN_POINT('Ctrl Pts',(51.7465600943494,18.769999979999,-172.529747068593));
#166842=CARTESIAN_POINT('Ctrl Pts',(51.8267440903201,18.2003128369917,-172.519113452117));
#166843=CARTESIAN_POINT('Ctrl Pts',(52.3218461673279,18.76999998,-172.650149483381));
#166844=CARTESIAN_POINT('Ctrl Pts',(51.746545387842,18.76999998,-172.650072180543));
#166845=CARTESIAN_POINT('Ctrl Pts',(51.8267261127284,18.2003140627874,-172.650082990805));
#166846=CARTESIAN_POINT('',(50.8071048221096,18.76999998,-171.14995));
#166847=CARTESIAN_POINT('Ctrl Pts',(50.8071048221096,18.76999998,-171.14995));
#166848=CARTESIAN_POINT('Ctrl Pts',(51.0054197414846,18.76999998,-171.149950000016));
#166849=CARTESIAN_POINT('Ctrl Pts',(51.2035851814656,18.76999998,-171.18899099047));
#166850=CARTESIAN_POINT('Ctrl Pts',(51.5699573073986,18.76999998,-171.339270411997));
#166851=CARTESIAN_POINT('Ctrl Pts',(51.7379841660413,18.76999998,-171.450449746589));
#166852=CARTESIAN_POINT('Ctrl Pts',(52.0183932512491,18.76999998,-171.728129909852));
#166853=CARTESIAN_POINT('Ctrl Pts',(52.1306652088914,18.76999998,-171.894521542842));
#166854=CARTESIAN_POINT('Ctrl Pts',(52.2824215121743,18.76999998,-172.257328160063));
#166855=CARTESIAN_POINT('Ctrl Pts',(52.3218461808705,18.76999998,-172.453565067926));
#166856=CARTESIAN_POINT('Ctrl Pts',(52.3218461808875,18.76999998,-172.64995));
#166857=CARTESIAN_POINT('Origin',(50.8071048221096,18.26999998,-171.14995));
#166858=CARTESIAN_POINT('Origin',(1.30574517062348E-14,18.26999998,-171.14995));
#166859=CARTESIAN_POINT('',(50.2136602208993,18.76999998,-171.14995));
#166860=CARTESIAN_POINT('',(50.7368344047584,18.76999998,-171.14995));
#166861=CARTESIAN_POINT('Origin',(50.2136602208993,18.26999998,-171.14995));
#166862=CARTESIAN_POINT('Ctrl Pts',(50.2136602208993,18.2695361161168,-171.64994978483));
#166863=CARTESIAN_POINT('Ctrl Pts',(50.2136602208993,18.76999998,-171.650414079253));
#166864=CARTESIAN_POINT('Ctrl Pts',(50.2136602208993,18.76999998,-171.14995));
#166865=CARTESIAN_POINT('Ctrl Pts',(50.1215246544275,18.2455129162615,-171.649927496752));
#166866=CARTESIAN_POINT('Ctrl Pts',(50.1192121820986,18.769999979997,-171.675053529555));
#166867=CARTESIAN_POINT('Ctrl Pts',(50.1601223770514,18.76999998,-171.149949978729));
#166868=CARTESIAN_POINT('Ctrl Pts',(50.0313961658949,18.2219555745979,-171.637727684223));
#166869=CARTESIAN_POINT('Ctrl Pts',(50.0231831602898,18.76999998,-171.689509542455));
#166870=CARTESIAN_POINT('Ctrl Pts',(50.1077189781947,18.76999998,-171.143861566653));
#166871=CARTESIAN_POINT('Ctrl Pts',(49.8551417349348,18.175783311066,-171.589506214496));
#166872=CARTESIAN_POINT('Ctrl Pts',(49.8203496880657,18.76999998,-171.697765173689));
#166873=CARTESIAN_POINT('Ctrl Pts',(50.005178217729,18.76999998,-171.11977321611));
#166874=CARTESIAN_POINT('Ctrl Pts',(49.7677248232621,18.1528278677084,-171.552585380948));
#166875=CARTESIAN_POINT('Ctrl Pts',(49.7110176447319,18.7699999800001,-171.68998153823));
#166876=CARTESIAN_POINT('Ctrl Pts',(49.9542884930289,18.76999998,-171.101323338366));
#166877=CARTESIAN_POINT('Ctrl Pts',(49.6064083377552,18.1103795873091,-171.455624893693));
#166878=CARTESIAN_POINT('Ctrl Pts',(49.4879820896889,18.7699999799999,-171.643731626876));
#166879=CARTESIAN_POINT('Ctrl Pts',(49.8603247967136,18.76999998,-171.052859322317));
#166880=CARTESIAN_POINT('Ctrl Pts',(49.5319078591071,18.0907307659146,-171.395951487152));
#166881=CARTESIAN_POINT('Ctrl Pts',(49.3735536061473,18.76999998,-171.604097554333));
#166882=CARTESIAN_POINT('Ctrl Pts',(49.8169023670873,18.76999998,-171.023027979234));
#166883=CARTESIAN_POINT('Ctrl Pts',(49.3974552840491,18.0552129145183,-171.250061441532));
#166884=CARTESIAN_POINT('Ctrl Pts',(49.1418918710281,18.76999998,-171.475750795187));
#166885=CARTESIAN_POINT('Ctrl Pts',(49.7384998091177,18.76999998,-170.950084676266));
#166886=CARTESIAN_POINT('Ctrl Pts',(49.3400748423115,18.0400232861332,-171.166250453495));
#166887=CARTESIAN_POINT('Ctrl Pts',(49.0303787392063,18.7699999799994,-171.386822745588));
#166888=CARTESIAN_POINT('Ctrl Pts',(49.7050206304183,18.76999998,-170.908176521547));
#166889=CARTESIAN_POINT('Ctrl Pts',(49.295796129512,18.0282912758315,-171.072436686249));
#166890=CARTESIAN_POINT('Ctrl Pts',(48.9370286803265,18.76999998,-171.270056405085));
#166891=CARTESIAN_POINT('Ctrl Pts',(49.6791770659623,18.76999998,-170.861259130871));
#166892=CARTESIAN_POINT('',(49.6791770659623,18.76999998,-170.861259130871));
#166893=CARTESIAN_POINT('Ctrl Pts',(49.6791770659623,18.76999998,-170.861259130871));
#166894=CARTESIAN_POINT('Ctrl Pts',(49.6968576580123,18.76999998,-170.893357248139));
#166895=CARTESIAN_POINT('Ctrl Pts',(49.7180606234586,18.76999998,-170.923027065572));
#166896=CARTESIAN_POINT('Ctrl Pts',(49.7421669681709,18.76999998,-170.950201836129));
#166897=CARTESIAN_POINT('Ctrl Pts',(49.7534002577178,18.76999998,-170.962864978123));
#166898=CARTESIAN_POINT('Ctrl Pts',(49.7652647303594,18.76999998,-170.974986007307));
#166899=CARTESIAN_POINT('Ctrl Pts',(49.7777010515148,18.76999998,-170.986556367076));
#166900=CARTESIAN_POINT('Ctrl Pts',(49.8071230954839,18.76999998,-171.013929705992));
#166901=CARTESIAN_POINT('Ctrl Pts',(49.8388986066918,18.76999998,-171.037546210365));
#166902=CARTESIAN_POINT('Ctrl Pts',(49.8728019101421,18.76999998,-171.057883544606));
#166903=CARTESIAN_POINT('Ctrl Pts',(49.8840707206928,18.76999998,-171.064643286087));
#166904=CARTESIAN_POINT('Ctrl Pts',(49.8955748425992,18.76999998,-171.071040378572));
#166905=CARTESIAN_POINT('Ctrl Pts',(49.9073066431081,18.76999998,-171.07709133376));
#166906=CARTESIAN_POINT('Ctrl Pts',(49.9542902216173,18.76999998,-171.101324232019));
#166907=CARTESIAN_POINT('Ctrl Pts',(50.0051782135404,18.76999998,-171.119773228098));
#166908=CARTESIAN_POINT('Ctrl Pts',(50.0564485939595,18.76999998,-171.131817408419));
#166909=CARTESIAN_POINT('Ctrl Pts',(50.1077152012182,18.76999998,-171.143860702368));
#166910=CARTESIAN_POINT('Ctrl Pts',(50.1601164670163,18.76999998,-171.14995));
#166911=CARTESIAN_POINT('Ctrl Pts',(50.2136602208993,18.76999998,-171.14995));
#166912=CARTESIAN_POINT('Origin',(49.6791770659623,18.26999998,-170.861259130871));
#166913=CARTESIAN_POINT('Ctrl Pts',(40.7628307834967,18.76999998,-155.145469613787));
#166914=CARTESIAN_POINT('Ctrl Pts',(39.9612665046713,18.76999998,-155.616375074053));
#166915=CARTESIAN_POINT('Ctrl Pts',(40.4031453149964,17.9943646866131,-155.356778744658));
#166916=CARTESIAN_POINT('Ctrl Pts',(43.8140202568649,18.76999998,-160.339133090562));
#166917=CARTESIAN_POINT('Ctrl Pts',(42.9502082118644,18.76999998,-160.637466725898));
#166918=CARTESIAN_POINT('Ctrl Pts',(43.4443793123589,18.0073632340302,-160.550451772752));
#166919=CARTESIAN_POINT('Ctrl Pts',(46.773026135633,18.76999998,-165.585306091383));
#166920=CARTESIAN_POINT('Ctrl Pts',(45.9568836537051,18.7699999799361,-165.904661000913));
#166921=CARTESIAN_POINT('Ctrl Pts',(46.3957674250336,18.0186733043079,-165.796619822254));
#166922=CARTESIAN_POINT('Ctrl Pts',(49.6791770659623,18.76999998,-170.861259130871));
#166923=CARTESIAN_POINT('Ctrl Pts',(48.9379852680023,18.76999998,-171.26952948831));
#166924=CARTESIAN_POINT('Ctrl Pts',(49.2955572616308,18.0287857662076,-171.07256826174));
#166925=CARTESIAN_POINT('',(40.7628307834967,18.76999998,-155.145469613787));
#166926=CARTESIAN_POINT('Ctrl Pts',(40.7628307834967,18.76999998,-155.145469613787));
#166927=CARTESIAN_POINT('Ctrl Pts',(43.8140512781903,18.76999998,-160.339185894338));
#166928=CARTESIAN_POINT('Ctrl Pts',(46.7729974319751,18.76999998,-165.585253981682));
#166929=CARTESIAN_POINT('Ctrl Pts',(49.6791770659623,18.76999998,-170.861259130871));
#166930=CARTESIAN_POINT('Origin',(40.7628307834967,18.26999998,-155.145469613787));
#166931=CARTESIAN_POINT('Ctrl Pts',(40.4031453149963,17.9943646866131,-155.356778744658));
#166932=CARTESIAN_POINT('Ctrl Pts',(39.9612665046713,18.76999998,-155.616375074053));
#166933=CARTESIAN_POINT('Ctrl Pts',(40.7628307834967,18.76999998,-155.145469613787));
#166934=CARTESIAN_POINT('Ctrl Pts',(40.1535949024652,18.0152331222464,-154.959221008645));
#166935=CARTESIAN_POINT('Ctrl Pts',(39.7648410678857,18.76999998,-155.176920406762));
#166936=CARTESIAN_POINT('Ctrl Pts',(40.5382265796732,18.76999998,-154.763153570891));
#166937=CARTESIAN_POINT('Ctrl Pts',(39.9463699385113,18.0368966498548,-154.546270136328));
#166938=CARTESIAN_POINT('Ctrl Pts',(39.5997667004894,18.76999998,-154.717664579548));
#166939=CARTESIAN_POINT('Ctrl Pts',(40.3517329455581,18.76999998,-154.366209991013));
#166940=CARTESIAN_POINT('Ctrl Pts',(39.5960425666541,18.0813960858844,-153.697271402021));
#166941=CARTESIAN_POINT('Ctrl Pts',(39.3360417060011,18.76999998,-153.799575452297));
#166942=CARTESIAN_POINT('Ctrl Pts',(40.0364383090907,18.76999998,-153.550444480173));
#166943=CARTESIAN_POINT('Ctrl Pts',(39.4532556977585,18.1042418116532,-153.261037480867));
#166944=CARTESIAN_POINT('Ctrl Pts',(39.23220455254,18.76999998,-153.338508255374));
#166945=CARTESIAN_POINT('Ctrl Pts',(39.9079301282699,18.76999998,-153.131458232674));
#166946=CARTESIAN_POINT('Ctrl Pts',(39.2248664505887,18.1509702537189,-152.367727156036));
#166947=CARTESIAN_POINT('Ctrl Pts',(39.0797143668984,18.76999998,-152.409570079113));
#166948=CARTESIAN_POINT('Ctrl Pts',(39.7023798052426,18.76999998,-152.273874561686));
#166949=CARTESIAN_POINT('Ctrl Pts',(39.1404609620539,18.1746678021094,-151.914185519153));
#166950=CARTESIAN_POINT('Ctrl Pts',(39.0281802867267,18.76999998,-151.943644934638));
#166951=CARTESIAN_POINT('Ctrl Pts',(39.6264148660465,18.76999998,-151.83867201801));
#166952=CARTESIAN_POINT('Ctrl Pts',(39.0282127872062,18.2221486757409,-151.004139862532));
#166953=CARTESIAN_POINT('Ctrl Pts',(38.9776025606259,18.76999998,-151.019307709025));
#166954=CARTESIAN_POINT('Ctrl Pts',(39.5253915082876,18.76999998,-150.965860868517));
#166955=CARTESIAN_POINT('Ctrl Pts',(39.,18.2460151034934,-150.546047809514));
#166956=CARTESIAN_POINT('Ctrl Pts',(38.9754245522527,18.76999998,-150.557403393481));
#166957=CARTESIAN_POINT('Ctrl Pts',(39.5000000006086,18.76999998,-150.526727576342));
#166958=CARTESIAN_POINT('Ctrl Pts',(39.,18.26999998,-150.084863924608));
#166959=CARTESIAN_POINT('Ctrl Pts',(39.,18.76999998,-150.084863924608));
#166960=CARTESIAN_POINT('Ctrl Pts',(39.5,18.76999998,-150.084863924608));
#166961=CARTESIAN_POINT('',(39.5,18.76999998,-150.084863924608));
#166962=CARTESIAN_POINT('Ctrl Pts',(39.5,18.76999998,-150.084863924608));
#166963=CARTESIAN_POINT('Ctrl Pts',(39.5,18.76999998,-150.526736484781));
#166964=CARTESIAN_POINT('Ctrl Pts',(39.5253915082895,18.76999998,-150.965860868514));
#166965=CARTESIAN_POINT('Ctrl Pts',(39.5759031870658,18.76999998,-151.402266443275));
#166966=CARTESIAN_POINT('Ctrl Pts',(39.6264148658422,18.76999998,-151.838672018036));
#166967=CARTESIAN_POINT('Ctrl Pts',(39.7023798052339,18.76999998,-152.273874561637));
#166968=CARTESIAN_POINT('Ctrl Pts',(39.8051549665991,18.76999998,-152.702666397218));
#166969=CARTESIAN_POINT('Ctrl Pts',(39.9079301279644,18.76999998,-153.131458232799));
#166970=CARTESIAN_POINT('Ctrl Pts',(40.0364383090913,18.76999998,-153.550444480149));
#166971=CARTESIAN_POINT('Ctrl Pts',(40.1940856267786,18.76999998,-153.958327235804));
#166972=CARTESIAN_POINT('Ctrl Pts',(40.3268328904507,18.76999998,-154.301785789407));
#166973=CARTESIAN_POINT('Ctrl Pts',(40.4800174576109,18.76999998,-154.637456687545));
#166974=CARTESIAN_POINT('Ctrl Pts',(40.6592112616996,18.76999998,-154.963216752103));
#166975=CARTESIAN_POINT('Ctrl Pts',(40.6928235206461,18.76999998,-155.024321161935));
#166976=CARTESIAN_POINT('Ctrl Pts',(40.7273510343294,18.76999998,-155.085076813206));
#166977=CARTESIAN_POINT('Ctrl Pts',(40.7628307834967,18.76999998,-155.145469613787));
#166978=CARTESIAN_POINT('Origin',(39.5,18.26999998,-150.084863924608));
#166979=CARTESIAN_POINT('Origin',(39.5,18.26999998,-55.24995));
#166980=CARTESIAN_POINT('',(39.5,18.76999998,-81.9737790469184));
#166981=CARTESIAN_POINT('',(39.5,18.76999998,-55.24995));
#166982=CARTESIAN_POINT('Origin',(39.5,18.26999998,-81.9737790469175));
#166983=CARTESIAN_POINT('Ctrl Pts',(39.,18.2699999800011,-81.9737790469193));
#166984=CARTESIAN_POINT('Ctrl Pts',(39.0000000000011,18.76999998,-81.9737790469193));
#166985=CARTESIAN_POINT('Ctrl Pts',(39.5,18.76999998,-81.9737790469184));
#166986=CARTESIAN_POINT('Ctrl Pts',(38.9999999999983,18.2220313158448,-81.0514322138321));
#166987=CARTESIAN_POINT('Ctrl Pts',(38.9495856510588,18.76999998,-81.0044062795137));
#166988=CARTESIAN_POINT('Ctrl Pts',(39.5000000014778,18.76999998,-81.0900715307985));
#166989=CARTESIAN_POINT('Ctrl Pts',(39.1098638639319,18.1747125385734,-80.1448153615248));
#166990=CARTESIAN_POINT('Ctrl Pts',(39.0100135050444,18.76999998,-80.0786830893324));
#166991=CARTESIAN_POINT('Ctrl Pts',(39.5988774762002,18.76999998,-80.2205083311056));
#166992=CARTESIAN_POINT('Ctrl Pts',(39.4494341483978,18.1049192927842,-78.810548635267));
#166993=CARTESIAN_POINT('Ctrl Pts',(39.229508253648,18.7699999800001,-78.7338553009239));
#166994=CARTESIAN_POINT('Ctrl Pts',(39.9044907342272,18.76999998,-78.9396134649389));
#166995=CARTESIAN_POINT('Ctrl Pts',(39.5935190801229,18.0817455339462,-78.3680408652321));
#166996=CARTESIAN_POINT('Ctrl Pts',(39.3342349384753,18.76999998,-78.2659886991342));
#166997=CARTESIAN_POINT('Ctrl Pts',(40.0341671712988,18.76999998,-78.514605681855));
#166998=CARTESIAN_POINT('Ctrl Pts',(39.9457414385913,18.036947832209,-77.5133471330197));
#166999=CARTESIAN_POINT('Ctrl Pts',(39.5993180096537,18.76999998,-77.3418642254583));
#167000=CARTESIAN_POINT('Ctrl Pts',(40.3511672955439,18.76999998,-77.6933701733068));
#167001=CARTESIAN_POINT('Ctrl Pts',(40.1537986734602,18.0152160834001,-77.0990973343972));
#167002=CARTESIAN_POINT('Ctrl Pts',(39.7649903796933,18.76999998,-76.8813885224012));
#167003=CARTESIAN_POINT('Ctrl Pts',(40.5384105179099,18.76999998,-77.2951763044633));
#167004=CARTESIAN_POINT('Ctrl Pts',(40.4031453149964,17.9943646866131,-76.7018642268486));
#167005=CARTESIAN_POINT('Ctrl Pts',(39.9612665046713,18.76999998,-76.4422678974524));
#167006=CARTESIAN_POINT('Ctrl Pts',(40.7628307834967,18.76999998,-76.913173357719));
#167007=CARTESIAN_POINT('',(40.7628307834967,18.76999998,-76.9131733577189));
#167008=CARTESIAN_POINT('Ctrl Pts',(40.7628307834967,18.76999998,-76.913173357719));
#167009=CARTESIAN_POINT('Ctrl Pts',(40.5548564785643,18.76999998,-77.267182363376));
#167010=CARTESIAN_POINT('Ctrl Pts',(40.3788354530892,18.76999998,-77.6350438334274));
#167011=CARTESIAN_POINT('Ctrl Pts',(40.2280138947792,18.76999998,-78.013829837117));
#167012=CARTESIAN_POINT('Ctrl Pts',(40.2160748553597,18.76999998,-78.043814549384));
#167013=CARTESIAN_POINT('Ctrl Pts',(40.2042937476386,18.76999998,-78.073867728607));
#167014=CARTESIAN_POINT('Ctrl Pts',(40.1926672329271,18.76999998,-78.1039879273901));
#167015=CARTESIAN_POINT('Ctrl Pts',(40.0341671712826,18.76999998,-78.5146056819203));
#167016=CARTESIAN_POINT('Ctrl Pts',(39.9044907334798,18.76999998,-78.9396134648084));
#167017=CARTESIAN_POINT('Ctrl Pts',(39.802619647733,18.76999998,-79.366578420212));
#167018=CARTESIAN_POINT('Ctrl Pts',(39.6899907885241,18.76999998,-79.8386316578581));
#167019=CARTESIAN_POINT('Ctrl Pts',(39.6094172115555,18.76999998,-80.3154017457566));
#167020=CARTESIAN_POINT('Ctrl Pts',(39.5598665237953,18.76999998,-80.7967368113108));
#167021=CARTESIAN_POINT('Ctrl Pts',(39.5197815285328,18.76999998,-81.1861222001839));
#167022=CARTESIAN_POINT('Ctrl Pts',(39.4999999999993,18.76999998,-81.5784952288498));
#167023=CARTESIAN_POINT('Ctrl Pts',(39.5,18.76999998,-81.9737790469184));
#167024=CARTESIAN_POINT('Origin',(40.7628307834967,18.26999998,-76.9131733577189));
#167025=CARTESIAN_POINT('Ctrl Pts',(49.5462350640495,18.76999998,-61.4386408691297));
#167026=CARTESIAN_POINT('Ctrl Pts',(48.8042785465888,18.76999998,-61.0296382684995));
#167027=CARTESIAN_POINT('Ctrl Pts',(49.1629069712534,18.0283224583225,-61.2273317382593));
#167028=CARTESIAN_POINT('Ctrl Pts',(46.6827176097033,18.76999998,-66.6332421622494));
#167029=CARTESIAN_POINT('Ctrl Pts',(45.867410270929,18.769999980105,-66.3106234612426));
#167030=CARTESIAN_POINT('Ctrl Pts',(46.3056933853622,18.0183276393305,-66.4219286454218));
#167031=CARTESIAN_POINT('Ctrl Pts',(43.7675014857899,18.76999998,-71.7986930470318));
#167032=CARTESIAN_POINT('Ctrl Pts',(42.9058979134104,18.76999998004,-71.4956126488948));
#167033=CARTESIAN_POINT('Ctrl Pts',(43.3980120961201,18.0071650557604,-71.5873748987318));
#167034=CARTESIAN_POINT('Ctrl Pts',(40.7628307834967,18.76999998,-76.913173357719));
#167035=CARTESIAN_POINT('Ctrl Pts',(39.9612665046713,18.76999998,-76.4422678974524));
#167036=CARTESIAN_POINT('Ctrl Pts',(40.4031453149964,17.9943646866131,-76.7018642268486));
#167037=CARTESIAN_POINT('',(49.5462350640495,18.76999998,-61.4386408691297));
#167038=CARTESIAN_POINT('Ctrl Pts',(49.5462350640495,18.76999998,-61.4386408691297));
#167039=CARTESIAN_POINT('Ctrl Pts',(46.6826907236407,18.76999998,-66.6332909352423));
#167040=CARTESIAN_POINT('Ctrl Pts',(43.7675305143725,18.76999998,-71.7986436352564));
#167041=CARTESIAN_POINT('Ctrl Pts',(40.7628307834967,18.76999998,-76.9131733577189));
#167042=CARTESIAN_POINT('',(49.1629069712534,18.0283224583225,-61.2273317382593));
#167043=CARTESIAN_POINT('Origin',(49.5462350640495,18.26999998,-61.4386408691297));
#167044=CARTESIAN_POINT('Ctrl Pts',(40.4031453149964,17.9943646866131,-76.7018642268486));
#167045=CARTESIAN_POINT('Ctrl Pts',(40.9712467296026,17.9967928105837,-75.7316879770719));
#167046=CARTESIAN_POINT('Ctrl Pts',(41.5465254248927,17.9992060627235,-74.7420551953058));
#167047=CARTESIAN_POINT('Ctrl Pts',(42.128923600295,18.0016015174866,-73.7329075612711));
#167048=CARTESIAN_POINT('Ctrl Pts',(42.6901148582909,18.0039097463388,-72.7605061112557));
#167049=CARTESIAN_POINT('Ctrl Pts',(43.2579165046237,18.0062014493159,-71.7699850988452));
#167050=CARTESIAN_POINT('Ctrl Pts',(43.8323178965797,18.0084744664279,-70.7613168444979));
#167051=CARTESIAN_POINT('Ctrl Pts',(44.3962696818231,18.0107061324303,-69.7709984526495));
#167052=CARTESIAN_POINT('Ctrl Pts',(44.966583117755,18.0129197841333,-68.7631869984356));
#167053=CARTESIAN_POINT('Ctrl Pts',(45.5432901010871,18.0151138514758,-67.7378813099146));
#167054=CARTESIAN_POINT('Ctrl Pts',(46.1330667662012,18.0173576420969,-66.6893395249608));
#167055=CARTESIAN_POINT('Ctrl Pts',(46.7295295612902,18.0195809446279,-65.6225012995692));
#167056=CARTESIAN_POINT('Ctrl Pts',(47.3327621588231,18.0217826463812,-64.5373949188219));
#167057=CARTESIAN_POINT('Ctrl Pts',(47.8996793987642,18.0238518029325,-63.5176133007002));
#167058=CARTESIAN_POINT('Ctrl Pts',(48.4725760817027,18.0259018832755,-62.481696975236));
#167059=CARTESIAN_POINT('Ctrl Pts',(49.0515658068575,18.0279324735353,-61.4296957260205));
#167060=CARTESIAN_POINT('Ctrl Pts',(49.0886544988738,18.0280625482732,-61.3623070511654));
#167061=CARTESIAN_POINT('Ctrl Pts',(49.1257682082662,18.0281925432139,-61.2948523829536));
#167062=CARTESIAN_POINT('Ctrl Pts',(49.1629069712534,18.0283224583225,-61.2273317382593));
#167063=CARTESIAN_POINT('Origin',(-83.2809572255632,18.26999998,-61.14995));
#167064=CARTESIAN_POINT('',(50.0811190791972,18.26999998,-60.64995));
#167065=CARTESIAN_POINT('',(50.0811190791972,18.76999998,-61.14995));
#167066=CARTESIAN_POINT('Origin',(50.0811190791972,18.26999998,-61.14995));
#167067=CARTESIAN_POINT('',(51.394983875096,18.76999998,-61.14995));
#167068=CARTESIAN_POINT('',(-83.2809572255632,18.7699999800001,-61.14995));
#167069=CARTESIAN_POINT('',(51.394983875096,18.26999998,-60.64995));
#167070=CARTESIAN_POINT('Origin',(51.394983875096,18.26999998,-61.14995));
#167071=CARTESIAN_POINT('',(1.30574517062348E-14,18.26999998,-60.64995));
#167072=CARTESIAN_POINT('Ctrl Pts',(49.1629069712534,18.0283224583225,-61.2273317382593));
#167073=CARTESIAN_POINT('Ctrl Pts',(48.8042785465888,18.76999998,-61.0296382684994));
#167074=CARTESIAN_POINT('Ctrl Pts',(49.5462350640495,18.76999998,-61.4386408691297));
#167075=CARTESIAN_POINT('Ctrl Pts',(49.2072136788996,18.0400790290492,-61.1335104039183));
#167076=CARTESIAN_POINT('Ctrl Pts',(48.8976639972856,18.7699999800003,-60.912976735742));
#167077=CARTESIAN_POINT('Ctrl Pts',(49.5720983755525,18.76999998,-61.3917233465932));
#167078=CARTESIAN_POINT('Ctrl Pts',(49.2636489250068,18.0550404895701,-61.0510932718963));
#167079=CARTESIAN_POINT('Ctrl Pts',(49.0074625403989,18.7699999800005,-60.8254916046238));
#167080=CARTESIAN_POINT('Ctrl Pts',(49.6050257059303,18.76999998,-61.3505216375984));
#167081=CARTESIAN_POINT('Ctrl Pts',(49.3970153298707,18.0903238932961,-60.9057963508575));
#167082=CARTESIAN_POINT('Ctrl Pts',(49.2376424762765,18.7699999799996,-60.6973789326117));
#167083=CARTESIAN_POINT('Ctrl Pts',(49.6828096124638,18.76999998,-61.2778731737785));
#167084=CARTESIAN_POINT('Ctrl Pts',(49.4723725947842,18.1102284712985,-60.8450701877959));
#167085=CARTESIAN_POINT('Ctrl Pts',(49.3535760550633,18.7699999800002,-60.656860805429));
#167086=CARTESIAN_POINT('Ctrl Pts',(49.7267438680042,18.76999998,-61.2475100972213));
#167087=CARTESIAN_POINT('Ctrl Pts',(49.7151670266325,18.1742094267258,-60.6988289354793));
#167088=CARTESIAN_POINT('Ctrl Pts',(49.6800903574717,18.7699999799997,-60.5889551600382));
#167089=CARTESIAN_POINT('Ctrl Pts',(49.8682179142305,18.76999998,-61.1743894610928));
#167090=CARTESIAN_POINT('Ctrl Pts',(49.897617121419,18.2220908968247,-60.64995));
#167091=CARTESIAN_POINT('Ctrl Pts',(49.8890563478339,18.76999998,-60.5998057785282));
#167092=CARTESIAN_POINT('Ctrl Pts',(49.9744290136678,18.76999998,-61.1499500118827));
#167093=CARTESIAN_POINT('Ctrl Pts',(50.0811190791972,18.26999998,-60.64995));
#167094=CARTESIAN_POINT('Ctrl Pts',(50.0811190791972,18.76999998,-60.64995));
#167095=CARTESIAN_POINT('Ctrl Pts',(50.0811190791972,18.76999998,-61.14995));
#167096=CARTESIAN_POINT('Ctrl Pts',(50.0811190791972,18.76999998,-61.14995));
#167097=CARTESIAN_POINT('Ctrl Pts',(50.0253653304668,18.76999998,-61.14995));
#167098=CARTESIAN_POINT('Ctrl Pts',(49.9698122997697,18.76999998,-61.156619759286));
#167099=CARTESIAN_POINT('Ctrl Pts',(49.9160272892494,18.76999998,-61.1699168656484));
#167100=CARTESIAN_POINT('Ctrl Pts',(49.8667673647609,18.76999998,-61.1820952486029));
#167101=CARTESIAN_POINT('Ctrl Pts',(49.8189890147709,18.76999998,-61.1998333372795));
#167102=CARTESIAN_POINT('Ctrl Pts',(49.7739018815407,18.76999998,-61.2231365482226));
#167103=CARTESIAN_POINT('Ctrl Pts',(49.7267405569306,18.76999998,-61.2475118015823));
#167104=CARTESIAN_POINT('Ctrl Pts',(49.6828095888518,18.76999998,-61.2778731395778));
#167105=CARTESIAN_POINT('Ctrl Pts',(49.6439176192587,18.76999998,-61.3141973629269));
#167106=CARTESIAN_POINT('Ctrl Pts',(49.6050311049514,18.76999998,-61.3505164911619));
#167107=CARTESIAN_POINT('Ctrl Pts',(49.572103750808,18.76999998,-61.3917134395509));
#167108=CARTESIAN_POINT('Ctrl Pts',(49.5462350640495,18.76999998,-61.4386408691297));
#167109=CARTESIAN_POINT('Ctrl Pts',(49.1629069712534,18.0283224583225,-61.2273317382593));
#167110=CARTESIAN_POINT('Ctrl Pts',(49.1758556443986,18.0317583367506,-61.1999123610635));
#167111=CARTESIAN_POINT('Ctrl Pts',(49.1902712257389,18.0355823155541,-61.1725636295363));
#167112=CARTESIAN_POINT('Ctrl Pts',(49.2062471139611,18.0398182108422,-61.1455207345201));
#167113=CARTESIAN_POINT('Ctrl Pts',(49.2132121160929,18.0416649325582,-61.1337308534933));
#167114=CARTESIAN_POINT('Ctrl Pts',(49.2204732095182,18.0435898179205,-61.121998672147));
#167115=CARTESIAN_POINT('Ctrl Pts',(49.2280358572725,18.0455942231795,-61.1103416139779));
#167116=CARTESIAN_POINT('Ctrl Pts',(49.242774003619,18.0495004236274,-61.0876242489957));
#167117=CARTESIAN_POINT('Ctrl Pts',(49.2586567334235,18.0537084504928,-61.0651969160208));
#167118=CARTESIAN_POINT('Ctrl Pts',(49.2757017806171,18.0582222363407,-61.0431801156955));
#167119=CARTESIAN_POINT('Ctrl Pts',(49.2863389361599,18.0610391157312,-61.0294402810704));
#167120=CARTESIAN_POINT('Ctrl Pts',(49.297428296039,18.0639749488797,-61.015859905788));
#167121=CARTESIAN_POINT('Ctrl Pts',(49.3089695099989,18.0670294385391,-61.0024639978232));
#167122=CARTESIAN_POINT('Ctrl Pts',(49.3159220123172,18.068869482967,-60.9943942157791));
#167123=CARTESIAN_POINT('Ctrl Pts',(49.3230396086335,18.070752883333,-60.9863896947236));
#167124=CARTESIAN_POINT('Ctrl Pts',(49.3303321274388,18.0726821914331,-60.9784448113769));
#167125=CARTESIAN_POINT('Ctrl Pts',(49.3443907684802,18.0764015442057,-60.9631285309434));
#167126=CARTESIAN_POINT('Ctrl Pts',(49.3590252215099,18.0802718191738,-60.9481340775816));
#167127=CARTESIAN_POINT('Ctrl Pts',(49.3742621817036,18.0842997443489,-60.93348331691));
#167128=CARTESIAN_POINT('Ctrl Pts',(49.3852323673815,18.0871997379504,-60.9229351785118));
#167129=CARTESIAN_POINT('Ctrl Pts',(49.3965149012616,18.0901814586669,-60.9125653703328));
#167130=CARTESIAN_POINT('Ctrl Pts',(49.4081198851036,18.093247433935,-60.9023849264265));
#167131=CARTESIAN_POINT('Ctrl Pts',(49.4184695181154,18.0959817521625,-60.8933057359888));
#167132=CARTESIAN_POINT('Ctrl Pts',(49.4290760983762,18.0987832097414,-60.8843771910698));
#167133=CARTESIAN_POINT('Ctrl Pts',(49.4399282538534,18.1016486941697,-60.8756225366125));
#167134=CARTESIAN_POINT('Ctrl Pts',(49.4666824192631,18.1087130644264,-60.8540394074407));
#167135=CARTESIAN_POINT('Ctrl Pts',(49.4949459316395,18.1161710329613,-60.8335002902348));
#167136=CARTESIAN_POINT('Ctrl Pts',(49.5246636596379,18.1240062279754,-60.8142280794331));
#167137=CARTESIAN_POINT('Ctrl Pts',(49.5282089615409,18.1249409606641,-60.8119289196308));
#167138=CARTESIAN_POINT('Ctrl Pts',(49.5322455216986,18.1260051114224,-60.8093481622553));
#167139=CARTESIAN_POINT('Ctrl Pts',(49.5358597613694,18.1269578466203,-60.8070708522197));
#167140=CARTESIAN_POINT('Ctrl Pts',(49.5378245064206,18.1274757651691,-60.8058328785295));
#167141=CARTESIAN_POINT('Ctrl Pts',(49.5396639643064,18.1279606345221,-60.804683593521));
#167142=CARTESIAN_POINT('Ctrl Pts',(49.5412286251171,18.1283730633644,-60.8037112597476));
#167143=CARTESIAN_POINT('Ctrl Pts',(49.5452063921231,18.1294215627134,-60.8012393392033));
#167144=CARTESIAN_POINT('Ctrl Pts',(49.5492314114211,18.130482391578,-60.7987761186316));
#167145=CARTESIAN_POINT('Ctrl Pts',(49.5533040478086,18.1315556397923,-60.7963230567551));
#167146=CARTESIAN_POINT('Ctrl Pts',(49.5780259154611,18.1380705106986,-60.7814323900504));
#167147=CARTESIAN_POINT('Ctrl Pts',(49.60446489505,18.1450328864082,-60.7669291728874));
#167148=CARTESIAN_POINT('Ctrl Pts',(49.6326921477065,18.1524603198153,-60.7531665994733));
#167149=CARTESIAN_POINT('Ctrl Pts',(49.6413659131076,18.1547426466039,-60.7489375894962));
#167150=CARTESIAN_POINT('Ctrl Pts',(49.6502083083206,18.1570688241963,-60.7447787940001));
#167151=CARTESIAN_POINT('Ctrl Pts',(49.6592207458122,18.1594391838299,-60.7407012135605));
#167152=CARTESIAN_POINT('Ctrl Pts',(49.6808075021014,18.1651167128864,-60.7309345177824));
#167153=CARTESIAN_POINT('Ctrl Pts',(49.7033660875626,18.1710466103037,-60.7216353832497));
#167154=CARTESIAN_POINT('Ctrl Pts',(49.7268958138618,18.177227889774,-60.7129654588309));
#167155=CARTESIAN_POINT('Ctrl Pts',(49.7386606770114,18.1803185295091,-60.7086304966215));
#167156=CARTESIAN_POINT('Ctrl Pts',(49.7506680691111,18.1834719459986,-60.70445298761));
#167157=CARTESIAN_POINT('Ctrl Pts',(49.7629162642643,18.1866875763887,-60.7004539866541));
#167158=CARTESIAN_POINT('Ctrl Pts',(49.7690403618409,18.1882953915837,-60.6984544861761));
#167159=CARTESIAN_POINT('Ctrl Pts',(49.7752246606936,18.1899187602925,-60.6964996152323));
#167160=CARTESIAN_POINT('Ctrl Pts',(49.7814688141369,18.191557577201,-60.6945920612596));
#167161=CARTESIAN_POINT('Ctrl Pts',(49.7845908908586,18.1923769856553,-60.6936382842732));
#167162=CARTESIAN_POINT('Ctrl Pts',(49.7877279312615,18.1932002561623,-60.6926963366154));
#167163=CARTESIAN_POINT('Ctrl Pts',(49.7908798877155,18.1940273743939,-60.6917665561795));
#167164=CARTESIAN_POINT('Ctrl Pts',(49.7932848752266,18.1946584773442,-60.6910571205102));
#167165=CARTESIAN_POINT('Ctrl Pts',(49.7965271499009,18.1955092358784,-60.6901157621523));
#167166=CARTESIAN_POINT('Ctrl Pts',(49.7987102115137,18.1960820260968,-60.6894907266843));
#167167=CARTESIAN_POINT('Ctrl Pts',(49.7993882521346,18.1962599299329,-60.689296595912));
#167168=CARTESIAN_POINT('Ctrl Pts',(49.7999640076789,18.1964109931631,-60.6891325221658));
#167169=CARTESIAN_POINT('Ctrl Pts',(49.80038045534,18.1965202573161,-60.6890140555969));
#167170=CARTESIAN_POINT('Ctrl Pts',(49.8126406245812,18.199736980888,-60.6855264140025));
#167171=CARTESIAN_POINT('Ctrl Pts',(49.8266384353679,18.2034086307252,-60.6817886559558));
#167172=CARTESIAN_POINT('Ctrl Pts',(49.8424059506839,18.2075426297223,-60.6780206105999));
#167173=CARTESIAN_POINT('Ctrl Pts',(49.8580179662976,18.2116358590989,-60.6742897258186));
#167174=CARTESIAN_POINT('Ctrl Pts',(49.8753655394232,18.2161825187496,-60.6705292559762));
#167175=CARTESIAN_POINT('Ctrl Pts',(49.8944728359148,18.2211877040932,-60.6670026654773));
#167176=CARTESIAN_POINT('Ctrl Pts',(49.9133107617609,18.226122327387,-60.6635257921092));
#167177=CARTESIAN_POINT('Ctrl Pts',(49.9338597788633,18.2315028072817,-60.6602763839452));
#167178=CARTESIAN_POINT('Ctrl Pts',(49.9561272211008,18.2373295727274,-60.6575539969875));
#167179=CARTESIAN_POINT('Ctrl Pts',(49.9776524699926,18.2429621269792,-60.6549223495706));
#167180=CARTESIAN_POINT('Ctrl Pts',(50.0007840434222,18.2490118557362,-60.6527834311557));
#167181=CARTESIAN_POINT('Ctrl Pts',(50.0255051992595,18.2554727154041,-60.6514490823613));
#167182=CARTESIAN_POINT('Ctrl Pts',(50.0432317550206,18.2601055404193,-60.6504922740119));
#167183=CARTESIAN_POINT('Ctrl Pts',(50.0617751943528,18.2649496372297,-60.64995));
#167184=CARTESIAN_POINT('Ctrl Pts',(50.0811190791972,18.26999998,-60.64995));
#167185=CARTESIAN_POINT('Origin',(0.,-12.9675000200281,-60.64995));
#167186=CARTESIAN_POINT('',(52.2790965136749,12.4220352393542,-61.2273317382593));
#167187=CARTESIAN_POINT('Origin',(0.,-12.9675000200281,-61.2273317382593));
#167188=CARTESIAN_POINT('Ctrl Pts',(52.2790965136749,12.4220352393542,-61.2273317382593));
#167189=CARTESIAN_POINT('Ctrl Pts',(51.5940499967886,12.4199494071951,-62.5507730638401));
#167190=CARTESIAN_POINT('Ctrl Pts',(50.9185870393202,12.4178348117833,-63.8509234010523));
#167191=CARTESIAN_POINT('Ctrl Pts',(50.2526456556148,12.4156916222119,-65.1277560842965));
#167192=CARTESIAN_POINT('Ctrl Pts',(49.5653893074062,12.413479834997,-66.4454566937362));
#167193=CARTESIAN_POINT('Ctrl Pts',(48.8882741342398,12.4112375970648,-67.7383226701546));
#167194=CARTESIAN_POINT('Ctrl Pts',(48.2212806269929,12.40896625095,-69.0063541135337));
#167195=CARTESIAN_POINT('Ctrl Pts',(47.5767619469032,12.4067714394803,-70.2316583231239));
#167196=CARTESIAN_POINT('Ctrl Pts',(46.9416949320218,12.4045494617144,-71.4337735851211));
#167197=CARTESIAN_POINT('Ctrl Pts',(46.3161001760333,12.4023024545041,-72.6127259072083));
#167198=CARTESIAN_POINT('Ctrl Pts',(46.3086478819023,12.4022756874021,-72.6267699818853));
#167199=CARTESIAN_POINT('Ctrl Pts',(46.3021038939964,12.4022521764144,-72.6391017563987));
#167200=CARTESIAN_POINT('Ctrl Pts',(46.2937473313732,12.4022221332078,-72.654848273595));
#167201=CARTESIAN_POINT('Ctrl Pts',(46.293595489273,12.4022215873107,-72.6551343941387));
#167202=CARTESIAN_POINT('Ctrl Pts',(46.2934436476664,12.4022210414119,-72.6554205134396));
#167203=CARTESIAN_POINT('Ctrl Pts',(46.2932918065534,12.4022204955114,-72.6557066314977));
#167204=CARTESIAN_POINT('Ctrl Pts',(45.6957923828427,12.4000723603874,-73.7815899406001));
#167205=CARTESIAN_POINT('Ctrl Pts',(45.1059485933711,12.3978983023915,-74.888236379866));
#167206=CARTESIAN_POINT('Ctrl Pts',(44.5236810068234,12.3956984861845,-75.9756149755482));
#167207=CARTESIAN_POINT('Ctrl Pts',(43.930487601711,12.3934573920611,-77.0833974225216));
#167208=CARTESIAN_POINT('Ctrl Pts',(43.3451575554821,12.3911895674979,-78.1711822389739));
#167209=CARTESIAN_POINT('Ctrl Pts',(42.7676550803754,12.3888961308826,-79.2389632317658));
#167210=CARTESIAN_POINT('Ctrl Pts',(42.1723207719999,12.3865318786758,-80.3397146332603));
#167211=CARTESIAN_POINT('Ctrl Pts',(41.5853049906506,12.3841404106341,-81.4192078583826));
#167212=CARTESIAN_POINT('Ctrl Pts',(41.0066173579777,12.3817239039064,-82.4774630287889));
#167213=CARTESIAN_POINT('Ctrl Pts',(40.7249794558944,12.3805478292045,-82.9924986874662));
#167214=CARTESIAN_POINT('Ctrl Pts',(40.4453148819667,12.3793658376879,-83.5025042696471));
#167215=CARTESIAN_POINT('Ctrl Pts',(40.1676286103916,12.3781782553103,-84.0074842249685));
#167216=CARTESIAN_POINT('Origin',(57.,11.61999998,-174.34995));
#167217=CARTESIAN_POINT('',(57.,12.11999998,-176.84995));
#167218=CARTESIAN_POINT('Origin',(57.,11.61999998,-176.84995));
#167219=CARTESIAN_POINT('',(59.5,12.11999998,-174.34995));
#167220=CARTESIAN_POINT('Origin',(57.,12.11999998,-174.34995));
#167221=CARTESIAN_POINT('Origin',(59.5,11.61999998,-174.34995));
#167222=CARTESIAN_POINT('Origin',(59.5,11.61999998,-55.24995));
#167223=CARTESIAN_POINT('',(59.5,12.11999998,-58.24995));
#167224=CARTESIAN_POINT('',(59.5,12.11999998,-174.34995));
#167225=CARTESIAN_POINT('Origin',(59.5,11.61999998,-58.24995));
#167226=CARTESIAN_POINT('Ctrl Pts',(52.8224784153175,12.11999998,-61.2752041600839));
#167227=CARTESIAN_POINT('Ctrl Pts',(52.5913010098385,12.11999998,-60.9843891047178));
#167228=CARTESIAN_POINT('Ctrl Pts',(52.5245819708698,12.4756972986233,-60.9004583201698));
#167229=CARTESIAN_POINT('Ctrl Pts',(53.0127900201976,12.11999998,-61.1239198608288));
#167230=CARTESIAN_POINT('Ctrl Pts',(52.7297264322295,12.1199999799996,-60.865773772671));
#167231=CARTESIAN_POINT('Ctrl Pts',(52.6505629615106,12.4839221309077,-60.7971452199062));
#167232=CARTESIAN_POINT('Ctrl Pts',(53.1625689933938,12.11999998,-60.9259844495965));
#167233=CARTESIAN_POINT('Ctrl Pts',(52.8314129775774,12.1199999800002,-60.7072763762979));
#167234=CARTESIAN_POINT('Ctrl Pts',(52.7486445377005,12.4996864767879,-60.660571058145));
#167235=CARTESIAN_POINT('Ctrl Pts',(53.2607580814926,12.11999998,-60.7033966151602));
#167236=CARTESIAN_POINT('Ctrl Pts',(52.8857929788878,12.11999998,-60.5379900686008));
#167237=CARTESIAN_POINT('Ctrl Pts',(52.81219032515,12.5218539749099,-60.5055220850798));
#167238=CARTESIAN_POINT('',(52.81219032515,12.5218539749099,-60.5055220850798));
#167239=CARTESIAN_POINT('',(53.2607580814926,12.11999998,-60.7033966151602));
#167240=CARTESIAN_POINT('Origin',(53.2607580814926,12.61999998,-60.7033966151602));
#167241=CARTESIAN_POINT('',(52.8224784153176,12.11999998,-61.275204160084));
#167242=CARTESIAN_POINT('Origin',(52.0615368275759,12.11999998,-60.1416270042854));
#167243=CARTESIAN_POINT('',(52.5245819708686,12.4756972986232,-60.9004583201709));
#167244=CARTESIAN_POINT('Origin',(52.8224784153158,12.6199999800056,-61.2752041600831));
#167245=CARTESIAN_POINT('Ctrl Pts',(52.81219032515,12.5218539749099,-60.5055220850798));
#167246=CARTESIAN_POINT('Ctrl Pts',(52.7933411307666,12.5152785668795,-60.5515133041606));
#167247=CARTESIAN_POINT('Ctrl Pts',(52.7716003070881,12.5093184856134,-60.5955155162472));
#167248=CARTESIAN_POINT('Ctrl Pts',(52.7473030826718,12.5039798383895,-60.6371999655705));
#167249=CARTESIAN_POINT('Ctrl Pts',(52.7233801432051,12.4987234299955,-60.6782422896143));
#167250=CARTESIAN_POINT('Ctrl Pts',(52.6969791694599,12.4940694538365,-60.7170375441058));
#167251=CARTESIAN_POINT('Ctrl Pts',(52.6684211908199,12.4900172284755,-60.753321423101));
#167252=CARTESIAN_POINT('Ctrl Pts',(52.6403779947413,12.4860380480235,-60.7889512534185));
#167253=CARTESIAN_POINT('Ctrl Pts',(52.6102550306507,12.4826391084701,-60.8221593620841));
#167254=CARTESIAN_POINT('Ctrl Pts',(52.5783544676246,12.4798135521224,-60.8527452424381));
#167255=CARTESIAN_POINT('Ctrl Pts',(52.560943652773,12.4782714088574,-60.8694385246063));
#167256=CARTESIAN_POINT('Ctrl Pts',(52.543003279237,12.4768999569538,-60.8853515771895));
#167257=CARTESIAN_POINT('Ctrl Pts',(52.5245819708698,12.4756972986233,-60.9004583201698));
#167258=CARTESIAN_POINT('Ctrl Pts',(52.5554920964233,12.4824531775908,-60.8743475621314));
#167259=CARTESIAN_POINT('Ctrl Pts',(52.6167804214063,12.1199999799999,-60.9580152164686));
#167260=CARTESIAN_POINT('Ctrl Pts',(52.8395656282165,12.11999998,-61.2621516547499));
#167261=CARTESIAN_POINT('Ctrl Pts',(52.4298097977004,12.4550534422725,-60.9763291407645));
#167262=CARTESIAN_POINT('Ctrl Pts',(52.5149863535236,12.1199999800004,-61.0598572644291));
#167263=CARTESIAN_POINT('Ctrl Pts',(52.7700980531444,12.11999998,-61.3131374124818));
#167264=CARTESIAN_POINT('Ctrl Pts',(52.3281854015479,12.4328072501504,-61.1077415231532));
#167265=CARTESIAN_POINT('Ctrl Pts',(52.4334636056902,12.1199999799999,-61.181393614378));
#167266=CARTESIAN_POINT('Ctrl Pts',(52.7138825713227,12.11999998,-61.378844307496));
#167267=CARTESIAN_POINT('Ctrl Pts',(52.2617577785881,12.4182503522228,-61.266432315258));
#167268=CARTESIAN_POINT('Ctrl Pts',(52.3811794250381,12.11999998,-61.3215576504461));
#167269=CARTESIAN_POINT('Ctrl Pts',(52.6771323647535,12.11999998,-61.4581932772117));
#167270=CARTESIAN_POINT('',(52.6867218473722,12.11999998,-61.4386408691297));
#167271=CARTESIAN_POINT('Origin',(53.5608834560411,12.11999998,-61.897804091577));
#167272=CARTESIAN_POINT('Origin',(52.6867218473722,12.61999998,-61.4386408691297));
#167273=CARTESIAN_POINT('Origin',(53.1708541764071,12.6169987765688,-61.636054659934));
#167274=CARTESIAN_POINT('Ctrl Pts',(40.5508657493525,12.11999998,-84.2187933558389));
#167275=CARTESIAN_POINT('Ctrl Pts',(40.2925576369006,12.11999998,-84.0763675385317));
#167276=CARTESIAN_POINT('Ctrl Pts',(40.1676286103916,12.3781782553103,-84.0074842249685));
#167277=CARTESIAN_POINT('Ctrl Pts',(42.6282131590433,12.11999998,-80.4512482683356));
#167278=CARTESIAN_POINT('Ctrl Pts',(42.3754889509591,12.11999998,-80.2844795011615));
#167279=CARTESIAN_POINT('Ctrl Pts',(42.2393869130494,12.3870385552721,-80.2399360160109));
#167280=CARTESIAN_POINT('Ctrl Pts',(44.6709958246245,12.11999998,-76.6652818249261));
#167281=CARTESIAN_POINT('Ctrl Pts',(44.4098483480378,12.11999998,-76.5004916194052));
#167282=CARTESIAN_POINT('Ctrl Pts',(44.2775738677864,12.39497584134,-76.4539726940548));
#167283=CARTESIAN_POINT('Ctrl Pts',(48.710372157466,12.11999998,-69.0687496953211));
#167284=CARTESIAN_POINT('Ctrl Pts',(48.4382080167511,12.11999998,-68.9007945866128));
#167285=CARTESIAN_POINT('Ctrl Pts',(48.3090097368786,12.4094651694423,-68.8574405644517));
#167286=CARTESIAN_POINT('Ctrl Pts',(50.7067648613536,12.11999998,-65.2580717844373));
#167287=CARTESIAN_POINT('Ctrl Pts',(50.4278516292118,12.1199999800037,-65.0915922935902));
#167288=CARTESIAN_POINT('Ctrl Pts',(50.3020637690764,12.4160155627679,-65.046761180979));
#167289=CARTESIAN_POINT('Ctrl Pts',(52.6867218473722,12.11999998,-61.4386408691297));
#167290=CARTESIAN_POINT('Ctrl Pts',(52.3947118718251,12.11999998,-61.287265650179));
#167291=CARTESIAN_POINT('Ctrl Pts',(52.2790965136749,12.4220352393542,-61.2273317382593));
#167292=CARTESIAN_POINT('',(40.5508657493525,12.11999998,-84.2187933558389));
#167293=CARTESIAN_POINT('Ctrl Pts',(40.5508657493525,12.11999998,-84.2187933558389));
#167294=CARTESIAN_POINT('Ctrl Pts',(42.6282147356021,12.11999998,-80.4512454090371));
#167295=CARTESIAN_POINT('Ctrl Pts',(44.6709958246292,12.11999998,-76.6652818249174));
#167296=CARTESIAN_POINT('Ctrl Pts',(46.6906839910419,12.11999998,-72.8670157601218));
#167297=CARTESIAN_POINT('Ctrl Pts',(48.7103721574547,12.11999998,-69.0687496953263));
#167298=CARTESIAN_POINT('Ctrl Pts',(50.7067642663818,12.11999998,-65.2580729321624));
#167299=CARTESIAN_POINT('Ctrl Pts',(52.6867218473722,12.11999998,-61.4386408691297));
#167300=CARTESIAN_POINT('Origin',(40.5508657493525,12.61999998,-84.2187933558389));
#167301=CARTESIAN_POINT('Ctrl Pts',(40.2331730433337,12.3723044963979,-83.8975858343799));
#167302=CARTESIAN_POINT('Ctrl Pts',(40.3579731063027,12.1199999799991,-83.9691999731268));
#167303=CARTESIAN_POINT('Ctrl Pts',(40.6098865790299,12.11999998,-84.1137766207722));
#167304=CARTESIAN_POINT('Ctrl Pts',(39.7931688569455,12.411333626796,-84.6210795875556));
#167305=CARTESIAN_POINT('Ctrl Pts',(39.9075805796616,12.1199999800059,-84.6935233019318));
#167306=CARTESIAN_POINT('Ctrl Pts',(40.2138237094928,12.11999998,-84.8052710236263));
#167307=CARTESIAN_POINT('Ctrl Pts',(39.4900144732213,12.4527389916394,-85.3915160553928));
#167308=CARTESIAN_POINT('Ctrl Pts',(39.5983305176353,12.11999998,-85.4536873863572));
#167309=CARTESIAN_POINT('Ctrl Pts',(39.9410319396356,12.11999998,-85.5407202621882));
#167310=CARTESIAN_POINT('Ctrl Pts',(39.1919178464122,12.5160949947626,-86.5777828047161));
#167311=CARTESIAN_POINT('Ctrl Pts',(39.2735548943734,12.11999998,-86.5998107325698));
#167312=CARTESIAN_POINT('Ctrl Pts',(39.6727396192083,12.11999998,-86.6717926677035));
#167313=CARTESIAN_POINT('Ctrl Pts',(39.1197796418649,12.5368967075763,-86.9683794640772));
#167314=CARTESIAN_POINT('Ctrl Pts',(39.1889101666761,12.11999998,-86.985650574818));
#167315=CARTESIAN_POINT('Ctrl Pts',(39.6078129604692,12.11999998,-87.0440021565177));
#167316=CARTESIAN_POINT('Ctrl Pts',(39.0190067195619,12.5806200665905,-87.7921667079605));
#167317=CARTESIAN_POINT('Ctrl Pts',(39.0548711280315,12.11999998,-87.8030567622564));
#167318=CARTESIAN_POINT('Ctrl Pts',(39.5171116805788,12.11999998,-87.8285181369117));
#167319=CARTESIAN_POINT('Ctrl Pts',(38.9951427354958,12.6036514403655,-88.2277009984956));
#167320=CARTESIAN_POINT('Ctrl Pts',(39.011598340781,12.11999998,-88.2372397284706));
#167321=CARTESIAN_POINT('Ctrl Pts',(39.495630995299,12.11999998,-88.2430081536419));
#167322=CARTESIAN_POINT('Ctrl Pts',(39.0008182748242,12.6267359883438,-88.6661338308315));
#167323=CARTESIAN_POINT('Ctrl Pts',(38.9939934962203,12.11999998,-88.6662158548394));
#167324=CARTESIAN_POINT('Ctrl Pts',(39.5007354296681,12.11999998,-88.6599531506585));
#167325=CARTESIAN_POINT('',(39.5,12.11999998,-88.5398461374725));
#167326=CARTESIAN_POINT('Ctrl Pts',(39.5,12.11999998,-88.5398461374725));
#167327=CARTESIAN_POINT('Ctrl Pts',(39.5,12.11999998,-88.1633801721072));
#167328=CARTESIAN_POINT('Ctrl Pts',(39.5216886477936,12.11999998,-87.7889298981599));
#167329=CARTESIAN_POINT('Ctrl Pts',(39.5647508040475,12.11999998,-87.4164660273289));
#167330=CARTESIAN_POINT('Ctrl Pts',(39.6078129603014,12.11999998,-87.0440021564979));
#167331=CARTESIAN_POINT('Ctrl Pts',(39.672739619198,12.11999998,-86.6717926677294));
#167332=CARTESIAN_POINT('Ctrl Pts',(39.7591103506482,12.11999998,-86.3076691214426));
#167333=CARTESIAN_POINT('Ctrl Pts',(39.8454810820984,12.11999998,-85.9435455751558));
#167334=CARTESIAN_POINT('Ctrl Pts',(39.9523131981843,12.11999998,-85.5865932598647));
#167335=CARTESIAN_POINT('Ctrl Pts',(40.0830988504763,12.11999998,-85.2380360010512));
#167336=CARTESIAN_POINT('Ctrl Pts',(40.2020523584852,12.11999998,-84.9210126276826));
#167337=CARTESIAN_POINT('Ctrl Pts',(40.3408210453828,12.11999998,-84.6109338991013));
#167338=CARTESIAN_POINT('Ctrl Pts',(40.5020760733001,12.11999998,-84.3087360817111));
#167339=CARTESIAN_POINT('Ctrl Pts',(40.5181158924583,12.11999998,-84.2786768742337));
#167340=CARTESIAN_POINT('Ctrl Pts',(40.5343782322704,12.11999998,-84.248695655134));
#167341=CARTESIAN_POINT('Ctrl Pts',(40.5508657493524,12.11999998,-84.2187933558389));
#167342=CARTESIAN_POINT('Origin',(39.5,12.61999998,-88.5398461374725));
#167343=CARTESIAN_POINT('Origin',(39.5,12.61999998,-55.24995));
#167344=CARTESIAN_POINT('',(39.5,12.11999998,-143.518796834034));
#167345=CARTESIAN_POINT('',(39.5,12.11999998,-55.24995));
#167346=CARTESIAN_POINT('Origin',(39.5,12.61999998,-143.518796834034));
#167347=CARTESIAN_POINT('Ctrl Pts',(39.,12.61999998,-143.518796834034));
#167348=CARTESIAN_POINT('Ctrl Pts',(39.,12.11999998,-143.518796834033));
#167349=CARTESIAN_POINT('Ctrl Pts',(39.5,12.11999998,-143.518796834034));
#167350=CARTESIAN_POINT('Ctrl Pts',(39.,12.5782777425004,-144.310620782824));
#167351=CARTESIAN_POINT('Ctrl Pts',(39.0400461849957,12.11999998,-144.278811846669));
#167352=CARTESIAN_POINT('Ctrl Pts',(39.5000000018526,12.11999998,-144.271919993373));
#167353=CARTESIAN_POINT('Ctrl Pts',(39.0943364399906,12.5370121096574,-145.08773908462));
#167354=CARTESIAN_POINT('Ctrl Pts',(39.1598342511364,12.11999998,-145.053286643925));
#167355=CARTESIAN_POINT('Ctrl Pts',(39.5849027948822,12.11999998,-145.01203141024));
#167356=CARTESIAN_POINT('Ctrl Pts',(39.4748832666623,12.4556479161234,-146.611482622671));
#167357=CARTESIAN_POINT('Ctrl Pts',(39.5826034488757,12.11999998,-146.552938806615));
#167358=CARTESIAN_POINT('Ctrl Pts',(39.9273949411055,12.11999998,-146.464868936119));
#167359=CARTESIAN_POINT('Ctrl Pts',(39.7646907193389,12.4152882936363,-147.362846081219));
#167360=CARTESIAN_POINT('Ctrl Pts',(39.8795078356987,12.11999998,-147.293857468464));
#167361=CARTESIAN_POINT('Ctrl Pts',(40.1882099383814,12.11999998,-147.182125180442));
#167362=CARTESIAN_POINT('Ctrl Pts',(40.1676286103828,12.3781782553111,-148.051158746522));
#167363=CARTESIAN_POINT('Ctrl Pts',(40.2925576368918,12.11999998,-147.98227543296));
#167364=CARTESIAN_POINT('Ctrl Pts',(40.5508657493446,12.11999998,-147.839849615653));
#167365=CARTESIAN_POINT('',(40.5508657493446,12.11999998,-147.839849615653));
#167366=CARTESIAN_POINT('Ctrl Pts',(40.5508657493446,12.11999998,-147.839849615653));
#167367=CARTESIAN_POINT('Ctrl Pts',(40.4872051775684,12.11999998,-147.72439272417));
#167368=CARTESIAN_POINT('Ctrl Pts',(40.4268911487416,12.11999998,-147.607488691345));
#167369=CARTESIAN_POINT('Ctrl Pts',(40.3697096603118,12.11999998,-147.489235888512));
#167370=CARTESIAN_POINT('Ctrl Pts',(40.3100900049243,12.11999998,-147.365940893102));
#167371=CARTESIAN_POINT('Ctrl Pts',(40.2538755845826,12.11999998,-147.241179143609));
#167372=CARTESIAN_POINT('Ctrl Pts',(40.2008730860125,12.11999998,-147.115031779943));
#167373=CARTESIAN_POINT('Ctrl Pts',(40.1592698126766,12.11999998,-147.016014877103));
#167374=CARTESIAN_POINT('Ctrl Pts',(40.1196464719309,12.11999998,-146.916143544358));
#167375=CARTESIAN_POINT('Ctrl Pts',(40.0819301037035,12.11999998,-146.815448147357));
#167376=CARTESIAN_POINT('Ctrl Pts',(40.0215352750628,12.11999998,-146.654205654174));
#167377=CARTESIAN_POINT('Ctrl Pts',(39.9660661346645,12.11999998,-146.490922340265));
#167378=CARTESIAN_POINT('Ctrl Pts',(39.9154672964456,12.11999998,-146.326388038909));
#167379=CARTESIAN_POINT('Ctrl Pts',(39.8629240743821,12.11999998,-146.15553110548));
#167380=CARTESIAN_POINT('Ctrl Pts',(39.8156327203445,12.11999998,-145.983326186387));
#167381=CARTESIAN_POINT('Ctrl Pts',(39.7734780737246,12.11999998,-145.810672966349));
#167382=CARTESIAN_POINT('Ctrl Pts',(39.767602077948,12.11999998,-145.786606589968));
#167383=CARTESIAN_POINT('Ctrl Pts',(39.7618258061273,12.11999998,-145.762531511883));
#167384=CARTESIAN_POINT('Ctrl Pts',(39.7561488675992,12.11999998,-145.738450173272));
#167385=CARTESIAN_POINT('Ctrl Pts',(39.6543246883703,12.11999998,-145.306516213334));
#167386=CARTESIAN_POINT('Ctrl Pts',(39.5830357134782,12.11999998,-144.869793515157));
#167387=CARTESIAN_POINT('Ctrl Pts',(39.5419615359765,12.11999998,-144.428332293124));
#167388=CARTESIAN_POINT('Ctrl Pts',(39.5139579007142,12.11999998,-144.127351974194));
#167389=CARTESIAN_POINT('Ctrl Pts',(39.5,12.11999998,-143.824168887311));
#167390=CARTESIAN_POINT('Ctrl Pts',(39.5,12.11999998,-143.518796834034));
#167391=CARTESIAN_POINT('Origin',(40.5508657493455,12.6199999799991,-147.839849615653));
#167392=CARTESIAN_POINT('Ctrl Pts',(52.811758955289,12.11999998,-170.861259130871));
#167393=CARTESIAN_POINT('Ctrl Pts',(52.5194581681217,12.11999998,-171.0127167027));
#167394=CARTESIAN_POINT('Ctrl Pts',(52.4039495302269,12.4224147476539,-171.07256826174));
#167395=CARTESIAN_POINT('Ctrl Pts',(50.8116692616976,12.11999998,-167.001248800573));
#167396=CARTESIAN_POINT('Ctrl Pts',(50.5326451268968,12.11999998,-167.168095406566));
#167397=CARTESIAN_POINT('Ctrl Pts',(50.4067968770089,12.4163544181458,-167.212559451309));
#167398=CARTESIAN_POINT('Ctrl Pts',(48.7949136859973,12.11999998,-163.150111451781));
#167399=CARTESIAN_POINT('Ctrl Pts',(48.5227235736013,12.1199999799924,-163.318503470872));
#167400=CARTESIAN_POINT('Ctrl Pts',(48.3933978906048,12.4097551621214,-163.361420582663));
#167401=CARTESIAN_POINT('Ctrl Pts',(44.7140165615046,12.11999998,-155.473076929555));
#167402=CARTESIAN_POINT('Ctrl Pts',(44.4529340155615,12.1199999800075,-155.63827143996));
#167403=CARTESIAN_POINT('Ctrl Pts',(44.3204976166945,12.3951430089669,-155.684386060413));
#167404=CARTESIAN_POINT('Ctrl Pts',(42.6500851427248,12.11999998,-151.647062446733));
#167405=CARTESIAN_POINT('Ctrl Pts',(42.3975527923274,12.11999998,-151.814329756678));
#167406=CARTESIAN_POINT('Ctrl Pts',(42.2612000992887,12.3871318438137,-151.858374821466));
#167407=CARTESIAN_POINT('Ctrl Pts',(40.5508657493446,12.11999998,-147.839849615653));
#167408=CARTESIAN_POINT('Ctrl Pts',(40.2925576368927,12.11999998,-147.98227543296));
#167409=CARTESIAN_POINT('Ctrl Pts',(40.1676286103837,12.3781782553102,-148.051158746523));
#167410=CARTESIAN_POINT('',(52.811758955289,12.11999998,-170.861259130871));
#167411=CARTESIAN_POINT('Ctrl Pts',(52.811758955289,12.11999998,-170.861259130871));
#167412=CARTESIAN_POINT('Ctrl Pts',(50.8116686437173,12.11999998,-167.001247608061));
#167413=CARTESIAN_POINT('Ctrl Pts',(48.794913685955,12.11999998,-163.150111451771));
#167414=CARTESIAN_POINT('Ctrl Pts',(46.7544651237368,12.11999998,-159.311594190676));
#167415=CARTESIAN_POINT('Ctrl Pts',(44.7140165615186,12.11999998,-155.47307692958));
#167416=CARTESIAN_POINT('Ctrl Pts',(42.6500867945137,12.11999998,-151.647065442471));
#167417=CARTESIAN_POINT('Ctrl Pts',(40.5508657493446,12.11999998,-147.839849615653));
#167418=CARTESIAN_POINT('Origin',(52.811758955289,12.61999998,-170.861259130871));
#167419=CARTESIAN_POINT('Ctrl Pts',(52.4039495302269,12.4224147476539,-171.07256826174));
#167420=CARTESIAN_POINT('Ctrl Pts',(52.5194581681217,12.11999998,-171.0127167027));
#167421=CARTESIAN_POINT('Ctrl Pts',(52.811758955289,12.11999998,-170.861259130871));
#167422=CARTESIAN_POINT('Ctrl Pts',(52.4335834030071,12.4288943780099,-171.135818022105));
#167423=CARTESIAN_POINT('Ctrl Pts',(52.5427333133061,12.1199999800001,-171.068676662146));
#167424=CARTESIAN_POINT('Ctrl Pts',(52.8281457246307,12.11999998,-170.892884198111));
#167425=CARTESIAN_POINT('Ctrl Pts',(52.4691942899059,12.4366759982665,-171.194717391534));
#167426=CARTESIAN_POINT('Ctrl Pts',(52.5708615508922,12.11999998,-171.121670121752));
#167427=CARTESIAN_POINT('Ctrl Pts',(52.8478360402188,12.11999998,-170.922334416373));
#167428=CARTESIAN_POINT('Ctrl Pts',(52.5103993792154,12.4456688476555,-171.249463186897));
#167429=CARTESIAN_POINT('Ctrl Pts',(52.6035237155536,12.11999998,-171.171968757444));
#167430=CARTESIAN_POINT('Ctrl Pts',(52.8706140943225,12.11999998,-170.949706593448));
#167431=CARTESIAN_POINT('',(52.8706140943225,12.11999998,-170.949706593448));
#167432=CARTESIAN_POINT('Ctrl Pts',(52.8706140943225,12.11999998,-170.949706593448));
#167433=CARTESIAN_POINT('Ctrl Pts',(52.8478318703964,12.11999998,-170.92232940649));
#167434=CARTESIAN_POINT('Ctrl Pts',(52.8281487108054,12.11999998,-170.892890025127));
#167435=CARTESIAN_POINT('Ctrl Pts',(52.811758955289,12.11999998,-170.861259130871));
#167436=CARTESIAN_POINT('Origin',(52.8706140943225,12.61999998,-170.949706593448));
#167437=CARTESIAN_POINT('Ctrl Pts',(53.1963133798215,12.11999998,-171.855638188259));
#167438=CARTESIAN_POINT('Ctrl Pts',(52.8383133487074,12.11999998,-171.855638188259));
#167439=CARTESIAN_POINT('Ctrl Pts',(52.7229737572976,12.4589111791821,-171.855638188259));
#167440=CARTESIAN_POINT('Ctrl Pts',(53.1963133729203,12.11999998,-171.690331848712));
#167441=CARTESIAN_POINT('Ctrl Pts',(52.8469882490941,12.1199999799987,-171.731583871386));
#167442=CARTESIAN_POINT('Ctrl Pts',(52.7266981809109,12.4479674186086,-171.743571468459));
#167443=CARTESIAN_POINT('Ctrl Pts',(53.1690734716394,12.11999998,-171.529660295248));
#167444=CARTESIAN_POINT('Ctrl Pts',(52.8308498854142,12.11999998,-171.608042739796));
#167445=CARTESIAN_POINT('Ctrl Pts',(52.7105385127756,12.4423260364225,-171.635556218068));
#167446=CARTESIAN_POINT('Ctrl Pts',(53.0574449276732,12.11999998,-171.218309959504));
#167447=CARTESIAN_POINT('Ctrl Pts',(52.7491850652078,12.11999998,-171.372054509995));
#167448=CARTESIAN_POINT('Ctrl Pts',(52.6373539450168,12.4388109638705,-171.427428053892));
#167449=CARTESIAN_POINT('Ctrl Pts',(52.9763399384659,12.11999998,-171.076756377445));
#167450=CARTESIAN_POINT('Ctrl Pts',(52.6858882090128,12.1199999799997,-171.265152468682));
#167451=CARTESIAN_POINT('Ctrl Pts',(52.5825160219714,12.4409678748685,-171.333391115642));
#167452=CARTESIAN_POINT('Ctrl Pts',(52.8706140943225,12.11999998,-170.949706593448));
#167453=CARTESIAN_POINT('Ctrl Pts',(52.6035237155536,12.11999998,-171.171968757444));
#167454=CARTESIAN_POINT('Ctrl Pts',(52.5103993792154,12.4456688476555,-171.249463186897));
#167455=CARTESIAN_POINT('',(53.1963133798215,12.11999998,-171.855638188259));
#167456=CARTESIAN_POINT('Ctrl Pts',(53.1963133798215,12.11999998,-171.855638188259));
#167457=CARTESIAN_POINT('Ctrl Pts',(53.196313374732,12.11999998,-171.733726928708));
#167458=CARTESIAN_POINT('Ctrl Pts',(53.1815021190221,12.11999998,-171.614382981078));
#167459=CARTESIAN_POINT('Ctrl Pts',(53.1513539482,12.11999998,-171.497697478305));
#167460=CARTESIAN_POINT('Ctrl Pts',(53.140611776948,12.11999998,-171.456120970701));
#167461=CARTESIAN_POINT('Ctrl Pts',(53.1279219841141,12.11999998,-171.414882055051));
#167462=CARTESIAN_POINT('Ctrl Pts',(53.1132591959952,12.11999998,-171.373985128688));
#167463=CARTESIAN_POINT('Ctrl Pts',(53.0817091112244,12.11999998,-171.285986755994));
#167464=CARTESIAN_POINT('Ctrl Pts',(53.0420949559002,12.11999998,-171.202535400932));
#167465=CARTESIAN_POINT('Ctrl Pts',(52.9945125852617,12.11999998,-171.123638976886));
#167466=CARTESIAN_POINT('Ctrl Pts',(52.9579184729549,12.11999998,-171.062962205985));
#167467=CARTESIAN_POINT('Ctrl Pts',(52.9166104754401,12.11999998,-171.00498002572));
#167468=CARTESIAN_POINT('Ctrl Pts',(52.8706140943225,12.11999998,-170.949706593448));
#167469=CARTESIAN_POINT('Origin',(53.1963133798215,12.61999998,-171.855638188259));
#167470=CARTESIAN_POINT('Origin',(53.1963133798215,12.61999998,-179.64995));
#167471=CARTESIAN_POINT('',(53.1963133798215,12.11999998,-171.806096612245));
#167472=CARTESIAN_POINT('',(52.7229737572976,12.4589111791821,-179.64995));
#167473=CARTESIAN_POINT('Origin',(60.,11.61999998,-176.84995));
#167474=CARTESIAN_POINT('',(-83.2809572255632,12.1199999800001,-176.84995));
#167475=CARTESIAN_POINT('Origin',(60.,28.91999998,-171.14995));
#167476=CARTESIAN_POINT('',(43.6738487993976,28.91999998,-171.64995));
#167477=CARTESIAN_POINT('',(49.3806153498803,28.91999998,-171.64995));
#167478=CARTESIAN_POINT('',(43.6738487993976,28.41999998,-171.14995));
#167479=CARTESIAN_POINT('',(41.7558360441701,28.41999998,-171.14995));
#167480=CARTESIAN_POINT('Origin',(43.6738487993976,28.91999998,-171.14995));
#167481=CARTESIAN_POINT('Origin',(60.,28.91999998,-171.14995));
#167482=CARTESIAN_POINT('',(49.3103449325291,28.41999998,-171.14995));
#167483=CARTESIAN_POINT('Origin',(49.3103449325291,28.91999998,-171.14995));
#167484=CARTESIAN_POINT('',(45.342056117244,28.91999998,-171.64995));
#167485=CARTESIAN_POINT('',(49.3806153498803,28.91999998,-171.64995));
#167486=CARTESIAN_POINT('',(45.342056117244,28.41999998,-171.14995));
#167487=CARTESIAN_POINT('Origin',(45.342056117244,28.91999998,-171.14995));
#167488=CARTESIAN_POINT('',(41.7558360441701,28.41999998,-171.14995));
#167489=CARTESIAN_POINT('Ctrl Pts',(50.825086291307,28.41999998,-172.64995));
#167490=CARTESIAN_POINT('Ctrl Pts',(50.3904429223989,28.41999998,-172.64995));
#167491=CARTESIAN_POINT('Ctrl Pts',(50.3299522569362,28.85041342952,-172.64995));
#167492=CARTESIAN_POINT('Ctrl Pts',(50.82508629129,28.41999998,-172.453565067926));
#167493=CARTESIAN_POINT('Ctrl Pts',(50.3904429223853,28.4199999800017,-172.511015867074));
#167494=CARTESIAN_POINT('Ctrl Pts',(50.3299522569358,28.8504134295228,-172.51902671195));
#167495=CARTESIAN_POINT('Ctrl Pts',(50.7856616225938,28.41999998,-172.257328160063));
#167496=CARTESIAN_POINT('Ctrl Pts',(50.3606872372737,28.41999998,-172.371853931892));
#167497=CARTESIAN_POINT('Ctrl Pts',(50.3034146036607,28.8522245814264,-172.38820210671));
#167498=CARTESIAN_POINT('Ctrl Pts',(50.6339053193109,28.41999998,-171.894521542842));
#167499=CARTESIAN_POINT('Ctrl Pts',(50.247876228143,28.41999998,-172.118296873734));
#167500=CARTESIAN_POINT('Ctrl Pts',(50.2012639378342,28.8591961991206,-172.14633102856));
#167501=CARTESIAN_POINT('Ctrl Pts',(50.5216333616693,28.41999998,-171.728129909852));
#167502=CARTESIAN_POINT('Ctrl Pts',(50.1643071358756,28.4199999800017,-172.003556970023));
#167503=CARTESIAN_POINT('Ctrl Pts',(50.1256910952006,28.8643539233763,-172.035403273235));
#167504=CARTESIAN_POINT('Ctrl Pts',(50.2412242764601,28.41999998,-171.450449746589));
#167505=CARTESIAN_POINT('Ctrl Pts',(49.9598619165025,28.4199999799983,-171.817687494207));
#167506=CARTESIAN_POINT('Ctrl Pts',(49.9369412763291,28.8772357931761,-171.850283164392));
#167507=CARTESIAN_POINT('Ctrl Pts',(50.0731974178181,28.41999998,-171.339270411997));
#167508=CARTESIAN_POINT('Ctrl Pts',(49.8382982003454,28.4199999800004,-171.746711574348));
#167509=CARTESIAN_POINT('Ctrl Pts',(49.8238385246439,28.8849548730131,-171.776163607997));
#167510=CARTESIAN_POINT('Ctrl Pts',(49.7068252918851,28.41999998,-171.18899099047));
#167511=CARTESIAN_POINT('Ctrl Pts',(49.5798629394444,28.4199999799996,-171.658003579003));
#167512=CARTESIAN_POINT('Ctrl Pts',(49.5772250015517,28.9017858470187,-171.675977326981));
#167513=CARTESIAN_POINT('Ctrl Pts',(49.5086598519041,28.41999998,-171.149950000016));
#167514=CARTESIAN_POINT('Ctrl Pts',(49.4425933612922,28.41999998,-171.640924254978));
#167515=CARTESIAN_POINT('Ctrl Pts',(49.443835276054,28.9108894800008,-171.64995));
#167516=CARTESIAN_POINT('Ctrl Pts',(49.3103449325291,28.41999998,-171.14995));
#167517=CARTESIAN_POINT('Ctrl Pts',(49.3103449325291,28.41999998,-171.64995));
#167518=CARTESIAN_POINT('Ctrl Pts',(49.3103449325291,28.91999998,-171.64995));
#167519=CARTESIAN_POINT('',(50.825086291307,28.41999998,-172.64995));
#167520=CARTESIAN_POINT('Origin',(50.825086291307,28.91999998,-172.64995));
#167521=CARTESIAN_POINT('Ctrl Pts',(50.825086291307,28.41999998,-172.64995));
#167522=CARTESIAN_POINT('Ctrl Pts',(50.82508629129,28.41999998,-172.453565067926));
#167523=CARTESIAN_POINT('Ctrl Pts',(50.7856616225938,28.41999998,-172.257328160063));
#167524=CARTESIAN_POINT('Ctrl Pts',(50.6339053193109,28.41999998,-171.894521542842));
#167525=CARTESIAN_POINT('Ctrl Pts',(50.5216333616693,28.41999998,-171.728129909852));
#167526=CARTESIAN_POINT('Ctrl Pts',(50.2412242764601,28.41999998,-171.450449746589));
#167527=CARTESIAN_POINT('Ctrl Pts',(50.0731974178181,28.41999998,-171.339270411997));
#167528=CARTESIAN_POINT('Ctrl Pts',(49.7068252918851,28.41999998,-171.18899099047));
#167529=CARTESIAN_POINT('Ctrl Pts',(49.5086598519041,28.41999998,-171.149950000016));
#167530=CARTESIAN_POINT('Ctrl Pts',(49.3103449325291,28.41999998,-171.14995));
#167531=CARTESIAN_POINT('Origin',(50.825086291307,28.91999998,-171.64995));
#167532=CARTESIAN_POINT('',(50.3299522569362,28.85041342952,-171.64995));
#167533=CARTESIAN_POINT('',(50.825086291307,28.41999998,-55.24995));
#167534=CARTESIAN_POINT('Origin',(60.,27.91999998,-176.84995));
#167535=CARTESIAN_POINT('',(57.,28.41999998,-176.84995));
#167536=CARTESIAN_POINT('',(60.,28.41999998,-176.84995));
#167537=CARTESIAN_POINT('Origin',(57.,27.91999998,-176.84995));
#167538=CARTESIAN_POINT('Origin',(57.,27.91999998,-174.34995));
#167539=CARTESIAN_POINT('',(59.5,28.41999998,-174.34995));
#167540=CARTESIAN_POINT('Origin',(57.,28.41999998,-174.34995));
#167541=CARTESIAN_POINT('Origin',(59.5,27.91999998,-174.34995));
#167542=CARTESIAN_POINT('Origin',(59.5,27.91999998,0.));
#167543=CARTESIAN_POINT('',(59.5,28.41999998,-58.24995));
#167544=CARTESIAN_POINT('',(59.5,28.41999998,-174.34995));
#167545=CARTESIAN_POINT('Origin',(59.5,27.91999998,-58.24995));
#167546=CARTESIAN_POINT('Ctrl Pts',(45.342056117244,28.9200050678813,-60.6499500000259));
#167547=CARTESIAN_POINT('Ctrl Pts',(45.342056117244,28.41999998,-60.6499449120928));
#167548=CARTESIAN_POINT('Ctrl Pts',(45.342056117244,28.41999998,-61.14995));
#167549=CARTESIAN_POINT('Ctrl Pts',(45.2161093325487,28.8799153348109,-60.6499495913736));
#167550=CARTESIAN_POINT('Ctrl Pts',(45.2207546457868,28.41999998,-60.6885563794559));
#167551=CARTESIAN_POINT('Ctrl Pts',(45.2032855852163,28.41999998,-61.1499499725599));
#167552=CARTESIAN_POINT('Ctrl Pts',(45.0809055449378,28.8470468727513,-60.6499493090119));
#167553=CARTESIAN_POINT('Ctrl Pts',(45.0814092233342,28.4199999800006,-60.7134256454893));
#167554=CARTESIAN_POINT('Ctrl Pts',(45.0642313709311,28.41999998,-61.1448442113686));
#167555=CARTESIAN_POINT('Ctrl Pts',(44.7999542633237,28.8023061531432,-60.6499489465081));
#167556=CARTESIAN_POINT('Ctrl Pts',(44.7998786663716,28.4199999799995,-60.7430249240652));
#167557=CARTESIAN_POINT('Ctrl Pts',(44.7862672310244,28.41999998,-61.1362430899869));
#167558=CARTESIAN_POINT('Ctrl Pts',(44.6541596767004,28.7904721518728,-60.6499488654503));
#167559=CARTESIAN_POINT('Ctrl Pts',(44.6527441767019,28.41999998,-60.7493138199263));
#167560=CARTESIAN_POINT('Ctrl Pts',(44.647272115325,28.41999998,-61.1328798677618));
#167561=CARTESIAN_POINT('Ctrl Pts',(44.36232828092,28.7904412154038,-60.6499488652048));
#167562=CARTESIAN_POINT('Ctrl Pts',(44.3637416796284,28.41999998,-60.7493310407855));
#167563=CARTESIAN_POINT('Ctrl Pts',(44.3691883762669,28.41999998,-61.1328719599062));
#167564=CARTESIAN_POINT('Ctrl Pts',(44.2164190292987,28.8022526047183,-60.6499489461074));
#167565=CARTESIAN_POINT('Ctrl Pts',(44.2164931090599,28.41999998,-60.7430562060495));
#167566=CARTESIAN_POINT('Ctrl Pts',(44.2300913879779,28.41999998,-61.1362301431742));
#167567=CARTESIAN_POINT('Ctrl Pts',(43.9353228646302,28.8469743774063,-60.6499493083947));
#167568=CARTESIAN_POINT('Ctrl Pts',(43.9348222136893,28.41999998,-60.7134784063315));
#167569=CARTESIAN_POINT('Ctrl Pts',(43.952003265591,28.41999998,-61.1448329195507));
#167570=CARTESIAN_POINT('Ctrl Pts',(43.800108709594,28.8798156648005,-60.6499495903585));
#167571=CARTESIAN_POINT('Ctrl Pts',(43.7954409326636,28.4199999800005,-60.688648899859));
#167572=CARTESIAN_POINT('Ctrl Pts',(43.812959462792,28.41999998,-61.149949972467));
#167573=CARTESIAN_POINT('Ctrl Pts',(43.6738487993976,28.9200050678813,-60.6499500000259));
#167574=CARTESIAN_POINT('Ctrl Pts',(43.6738487993976,28.41999998,-60.6499449120928));
#167575=CARTESIAN_POINT('Ctrl Pts',(43.6738487993976,28.41999998,-61.14995));
#167576=CARTESIAN_POINT('',(45.342056117244,28.41999998,-61.14995));
#167577=CARTESIAN_POINT('',(45.342056117244,28.91999998,-60.64995));
#167578=CARTESIAN_POINT('Origin',(45.342056117244,28.91999998,-61.14995));
#167579=CARTESIAN_POINT('',(43.6738487993976,28.41999998,-61.14995));
#167580=CARTESIAN_POINT('Ctrl Pts',(43.6738487993976,28.41999998,-61.14995));
#167581=CARTESIAN_POINT('Ctrl Pts',(43.8129691638245,28.41999998,-61.1499499724651));
#167582=CARTESIAN_POINT('Ctrl Pts',(43.9520102350777,28.41999998,-61.1448326154154));
#167583=CARTESIAN_POINT('Ctrl Pts',(44.0910473222173,28.41999998,-61.1405313837273));
#167584=CARTESIAN_POINT('Ctrl Pts',(44.2300643593017,28.41999998,-61.1362307723049));
#167585=CARTESIAN_POINT('Ctrl Pts',(44.3691300592233,28.4199999800001,-61.1328730966358));
#167586=CARTESIAN_POINT('Ctrl Pts',(44.5081446038248,28.41999998,-61.1328757503145));
#167587=CARTESIAN_POINT('Ctrl Pts',(44.5081731511562,28.41999998,-61.1328757508594));
#167588=CARTESIAN_POINT('Ctrl Pts',(44.5082016984814,28.41999998,-61.1328757515461));
#167589=CARTESIAN_POINT('Ctrl Pts',(44.5082302458005,28.41999998,-61.1328757523744));
#167590=CARTESIAN_POINT('Ctrl Pts',(44.6473090834153,28.41999998,-61.1328797881197));
#167591=CARTESIAN_POINT('Ctrl Pts',(44.7862513535664,28.41999998,-61.1362425571023));
#167592=CARTESIAN_POINT('Ctrl Pts',(44.9252493016292,28.41999998,-61.140543629625));
#167593=CARTESIAN_POINT('Ctrl Pts',(45.0447391053956,28.41999998,-61.1442410533561));
#167594=CARTESIAN_POINT('Ctrl Pts',(45.1643332045563,28.41999998,-61.1485385900918));
#167595=CARTESIAN_POINT('Ctrl Pts',(45.283905320582,28.41999998,-61.1496673946892));
#167596=CARTESIAN_POINT('Ctrl Pts',(45.3032896860489,28.41999998,-61.1498503902034));
#167597=CARTESIAN_POINT('Ctrl Pts',(45.3226734672926,28.41999998,-61.1499499961673));
#167598=CARTESIAN_POINT('Ctrl Pts',(45.342056117244,28.41999998,-61.14995));
#167599=CARTESIAN_POINT('',(43.6738487993976,28.91999998,-60.64995));
#167600=CARTESIAN_POINT('Origin',(43.6738487993998,28.91999998,-61.1499500000012));
#167601=CARTESIAN_POINT('',(44.5079483622449,28.7904524382955,-60.6499500000782));
#167602=CARTESIAN_POINT('Ctrl Pts',(43.6738487993976,28.91999998,-60.64995));
#167603=CARTESIAN_POINT('Ctrl Pts',(43.7715300191691,28.8889075392417,-60.64995));
#167604=CARTESIAN_POINT('Ctrl Pts',(43.8708734141984,28.863301217625,-60.6499548134033));
#167605=CARTESIAN_POINT('Ctrl Pts',(44.0765991739498,28.8223766210739,-60.6499497946885));
#167606=CARTESIAN_POINT('Ctrl Pts',(44.1829187602502,28.8076233386194,-60.6499592865054));
#167607=CARTESIAN_POINT('Ctrl Pts',(44.3623912990614,28.7933428984955,-60.6499605228612));
#167608=CARTESIAN_POINT('Ctrl Pts',(44.4351555237859,28.7904525467191,-60.6499500385495));
#167609=CARTESIAN_POINT('Ctrl Pts',(44.5079483622449,28.7904524382955,-60.6499500000782));
#167610=CARTESIAN_POINT('Ctrl Pts',(44.5079524583208,28.7904524382925,-60.6499500000761));
#167611=CARTESIAN_POINT('Ctrl Pts',(44.5807739260483,28.7904524382925,-60.6499499621218));
#167612=CARTESIAN_POINT('Ctrl Pts',(44.6535626787506,28.7933447394316,-60.6499600878182));
#167613=CARTESIAN_POINT('Ctrl Pts',(44.8330844822752,28.8076342035688,-60.6499589653179));
#167614=CARTESIAN_POINT('Ctrl Pts',(44.9394245210754,28.8223946394281,-60.6499497574468));
#167615=CARTESIAN_POINT('Ctrl Pts',(45.1451227360793,28.8633247324819,-60.6499554518237));
#167616=CARTESIAN_POINT('Ctrl Pts',(45.2444197705189,28.8889218225659,-60.64995));
#167617=CARTESIAN_POINT('Ctrl Pts',(45.342056117244,28.91999998,-60.64995));
#167618=CARTESIAN_POINT('Origin',(41.7558360441701,29.41999998,-179.64995));
#167619=CARTESIAN_POINT('',(41.7558360441701,28.41999998,-94.0656090587062));
#167620=CARTESIAN_POINT('',(41.7558360441701,28.41999998,-61.14995));
#167621=CARTESIAN_POINT('',(41.7558360441701,28.41999998,-60.64995));
#167622=CARTESIAN_POINT('Ctrl Pts',(41.7558360441699,28.41999998,-94.0656090587062));
#167623=CARTESIAN_POINT('Ctrl Pts',(41.7308060590876,28.41999998,-94.0338832438937));
#167624=CARTESIAN_POINT('Ctrl Pts',(41.7052809909715,28.4208804787712,-94.0028874559655));
#167625=CARTESIAN_POINT('Ctrl Pts',(41.6793664879697,28.4228182439003,-93.9726174435406));
#167626=CARTESIAN_POINT('Ctrl Pts',(41.6537132083297,28.4247364759703,-93.9426525588816));
#167627=CARTESIAN_POINT('Ctrl Pts',(41.6276783059325,28.4276905003979,-93.9133988823568));
#167628=CARTESIAN_POINT('Ctrl Pts',(41.6013615267512,28.4318016725001,-93.8848511812043));
#167629=CARTESIAN_POINT('Ctrl Pts',(41.5745345322137,28.435992549764,-93.8557500127976));
#167630=CARTESIAN_POINT('Ctrl Pts',(41.5474143379969,28.441386237443,-93.827382397737));
#167631=CARTESIAN_POINT('Ctrl Pts',(41.5201155936462,28.4480570335741,-93.7997531157501));
#167632=CARTESIAN_POINT('Ctrl Pts',(41.4978025199057,28.4535095175445,-93.7771698716841));
#167633=CARTESIAN_POINT('Ctrl Pts',(41.4753698984777,28.4598141851721,-93.7550795761226));
#167634=CARTESIAN_POINT('Ctrl Pts',(41.4528781441728,28.4669860146366,-93.7334824827062));
#167635=CARTESIAN_POINT('Ctrl Pts',(41.4463031679536,28.4690825433261,-93.7271690411804));
#167636=CARTESIAN_POINT('Ctrl Pts',(41.4399116489738,28.4711911056978,-93.7210776132016));
#167637=CARTESIAN_POINT('Ctrl Pts',(41.4334563878741,28.4733895230503,-93.7149684859755));
#167638=CARTESIAN_POINT('Ctrl Pts',(41.4261104488557,28.4758912715558,-93.7080164393634));
#167639=CARTESIAN_POINT('Ctrl Pts',(41.4186813966183,28.4785040045918,-93.7010438416435));
#167640=CARTESIAN_POINT('Ctrl Pts',(41.4107916508638,28.4813867845025,-93.6937059454966));
#167641=CARTESIAN_POINT('Ctrl Pts',(41.4099071063804,28.4817099821246,-93.6928832706273));
#167642=CARTESIAN_POINT('Ctrl Pts',(41.4090167534851,28.4820366245984,-93.6920560131081));
#167643=CARTESIAN_POINT('Ctrl Pts',(41.4081200467408,28.4823669762365,-93.6912236943418));
#167644=CARTESIAN_POINT('Ctrl Pts',(41.3849837120793,28.4908905276703,-93.6697486629028));
#167645=CARTESIAN_POINT('Ctrl Pts',(41.361944000301,28.5002943094801,-93.6489194763972));
#167646=CARTESIAN_POINT('Ctrl Pts',(41.3391424940239,28.5106357860759,-93.6287624230044));
#167647=CARTESIAN_POINT('Ctrl Pts',(41.3154766201132,28.5213692910556,-93.6078412488412));
#167648=CARTESIAN_POINT('Ctrl Pts',(41.2920672370986,28.5331126675112,-93.587644051536));
#167649=CARTESIAN_POINT('Ctrl Pts',(41.2690384601266,28.5458882035334,-93.5681847612561));
#167650=CARTESIAN_POINT('Ctrl Pts',(41.2445672529732,28.5594639478674,-93.5475066191177));
#167651=CARTESIAN_POINT('Ctrl Pts',(41.2205258064017,28.5742050230276,-93.5276616732026));
#167652=CARTESIAN_POINT('Ctrl Pts',(41.1970260426481,28.5900949563365,-93.5086504182702));
#167653=CARTESIAN_POINT('Ctrl Pts',(41.1718083285525,28.6071465232962,-93.4882493454546));
#167654=CARTESIAN_POINT('Ctrl Pts',(41.1472143849228,28.6255208325304,-93.4688082580181));
#167655=CARTESIAN_POINT('Ctrl Pts',(41.1233412664623,28.6451524244045,-93.4503104059951));
#167656=CARTESIAN_POINT('Ctrl Pts',(41.0995082258377,28.6647510590544,-93.4318436078908));
#167657=CARTESIAN_POINT('Ctrl Pts',(41.0763931215648,28.6856020390434,-93.41431663479));
#167658=CARTESIAN_POINT('Ctrl Pts',(41.0540572871253,28.7076050220164,-93.3976987687948));
#167659=CARTESIAN_POINT('Origin',(41.7558360441701,29.41999998,-61.14995));
#167660=CARTESIAN_POINT('Origin',(57.,27.91999998,-58.24995));
#167661=CARTESIAN_POINT('',(57.,28.41999998,-55.74995));
#167662=CARTESIAN_POINT('Origin',(57.,28.41999998,-58.24995));
#167663=CARTESIAN_POINT('',(57.,27.91999998,-55.24995));
#167664=CARTESIAN_POINT('Origin',(57.,27.91999998,-55.74995));
#167665=CARTESIAN_POINT('Origin',(57.,27.91999998,-58.24995));
#167666=CARTESIAN_POINT('Origin',(57.,-2.42462934179819E-14,-58.24995));
#167667=CARTESIAN_POINT('',(57.,27.41999998,-55.24995));
#167668=CARTESIAN_POINT('',(57.,28.41999998,-55.24995));
#167669=CARTESIAN_POINT('Origin',(57.,27.41999998,-58.24995));
#167670=CARTESIAN_POINT('Origin',(-83.2809572255632,26.4199999800001,-171.14995));
#167671=CARTESIAN_POINT('',(44.1114262156583,26.91999998,-171.14995));
#167672=CARTESIAN_POINT('Origin',(44.1114262156583,26.41999998,-171.14995));
#167673=CARTESIAN_POINT('',(49.6616970192851,26.91999998,-171.14995));
#167674=CARTESIAN_POINT('Origin',(49.6616970192851,26.41999998,-171.14995));
#167675=CARTESIAN_POINT('',(49.5914266019339,26.91999998,-171.14995));
#167676=CARTESIAN_POINT('Ctrl Pts',(44.1114262156583,26.41999998,-171.64995));
#167677=CARTESIAN_POINT('Ctrl Pts',(44.1114262156583,26.91999998,-171.64995));
#167678=CARTESIAN_POINT('Ctrl Pts',(44.1114262156583,26.91999998,-171.14995));
#167679=CARTESIAN_POINT('Ctrl Pts',(43.9300489743418,26.362103375035,-171.64995));
#167680=CARTESIAN_POINT('Ctrl Pts',(43.9189401667911,26.91999998,-171.71139261988));
#167681=CARTESIAN_POINT('Ctrl Pts',(43.9948946430299,26.91999998,-171.149949978158));
#167682=CARTESIAN_POINT('Ctrl Pts',(43.7459157865524,26.3030441696697,-171.604534812847));
#167683=CARTESIAN_POINT('Ctrl Pts',(43.7068322349107,26.91999998,-171.744547621103));
#167684=CARTESIAN_POINT('Ctrl Pts',(43.8763450763459,26.91999998,-171.127242425404));
#167685=CARTESIAN_POINT('Ctrl Pts',(43.4976348610037,26.2230846254426,-171.46374657232));
#167686=CARTESIAN_POINT('Ctrl Pts',(43.3564708632233,26.91999998,-171.726334995184));
#167687=CARTESIAN_POINT('Ctrl Pts',(43.7162275365378,26.91999998,-171.05684827667));
#167688=CARTESIAN_POINT('Ctrl Pts',(43.4182794830488,26.1974705898599,-171.403866413424));
#167689=CARTESIAN_POINT('Ctrl Pts',(43.2222824786043,26.91999998,-171.705069685313));
#167690=CARTESIAN_POINT('Ctrl Pts',(43.665002290469,26.91999998,-171.026908215035));
#167691=CARTESIAN_POINT('Ctrl Pts',(43.2765868661323,26.1516592710682,-171.257703672334));
#167692=CARTESIAN_POINT('Ctrl Pts',(42.9355727403744,26.91999998,-171.608576267085));
#167693=CARTESIAN_POINT('Ctrl Pts',(43.5734725485514,26.91999998,-170.953826827844));
#167694=CARTESIAN_POINT('Ctrl Pts',(43.2149501334587,26.1316898999239,-171.173001781957));
#167695=CARTESIAN_POINT('Ctrl Pts',(42.7841822677167,26.9199999800006,-171.530641542159));
#167696=CARTESIAN_POINT('Ctrl Pts',(43.5336346878404,26.91999998,-170.91149625204));
#167697=CARTESIAN_POINT('Ctrl Pts',(43.1661128544364,26.1158519257145,-171.07256826174));
#167698=CARTESIAN_POINT('Ctrl Pts',(42.6444458925863,26.91999998,-171.400720533971));
#167699=CARTESIAN_POINT('Ctrl Pts',(43.5020331013479,26.91999998,-170.861259130871));
#167700=CARTESIAN_POINT('',(43.5020331013479,26.91999998,-170.861259130871));
#167701=CARTESIAN_POINT('Origin',(43.5020331013479,26.41999998,-170.861259130871));
#167702=CARTESIAN_POINT('Ctrl Pts',(43.5020331013479,26.91999998,-170.861259130871));
#167703=CARTESIAN_POINT('Ctrl Pts',(43.5336466193108,26.91999998,-170.911515457779));
#167704=CARTESIAN_POINT('Ctrl Pts',(43.5734840835972,26.91999998,-170.953836204196));
#167705=CARTESIAN_POINT('Ctrl Pts',(43.61923735557,26.91999998,-170.99036760152));
#167706=CARTESIAN_POINT('Ctrl Pts',(43.6650022527906,26.91999998,-171.026908280947));
#167707=CARTESIAN_POINT('Ctrl Pts',(43.7162207484477,26.91999998,-171.056845311872));
#167708=CARTESIAN_POINT('Ctrl Pts',(43.7696000450754,26.91999998,-171.080313003677));
#167709=CARTESIAN_POINT('Ctrl Pts',(43.8006630727512,26.91999998,-171.093969563544));
#167710=CARTESIAN_POINT('Ctrl Pts',(43.8326179990561,26.91999998,-171.105532778688));
#167711=CARTESIAN_POINT('Ctrl Pts',(43.8652115257656,26.91999998,-171.115097339925));
#167712=CARTESIAN_POINT('Ctrl Pts',(43.8987093663281,26.91999998,-171.124927271807));
#167713=CARTESIAN_POINT('Ctrl Pts',(43.9328831236168,26.91999998,-171.132646173148));
#167714=CARTESIAN_POINT('Ctrl Pts',(43.9674767132985,26.91999998,-171.138304320373));
#167715=CARTESIAN_POINT('Ctrl Pts',(44.0018197383426,26.91999998,-171.143921485104));
#167716=CARTESIAN_POINT('Ctrl Pts',(44.0365780353938,26.91999998,-171.147507459409));
#167717=CARTESIAN_POINT('Ctrl Pts',(44.0714975023725,26.91999998,-171.149061689887));
#167718=CARTESIAN_POINT('Ctrl Pts',(44.084788827213,26.91999998,-171.149653273435));
#167719=CARTESIAN_POINT('Ctrl Pts',(44.0981033481739,26.91999998,-171.14995));
#167720=CARTESIAN_POINT('Ctrl Pts',(44.1114262156583,26.91999998,-171.14995));
#167721=CARTESIAN_POINT('Ctrl Pts',(41.0569324495328,26.91999998,-167.025025538602));
#167722=CARTESIAN_POINT('Ctrl Pts',(40.1792441039419,26.91999998,-167.592179375447));
#167723=CARTESIAN_POINT('Ctrl Pts',(40.7299249439265,26.10628905815,-167.236334669472));
#167724=CARTESIAN_POINT('Ctrl Pts',(41.879954591083,26.91999998,-168.29867810854));
#167725=CARTESIAN_POINT('Ctrl Pts',(41.0020315723371,26.9199999800235,-168.844852386549));
#167726=CARTESIAN_POINT('Ctrl Pts',(41.5498055229506,26.1095638122232,-168.509987294195));
#167727=CARTESIAN_POINT('Ctrl Pts',(42.6945981803054,26.91999998,-169.577671730211));
#167728=CARTESIAN_POINT('Ctrl Pts',(41.8241014260219,26.9199999799921,-170.115499778852));
#167729=CARTESIAN_POINT('Ctrl Pts',(42.361486708359,26.1127497675934,-169.788980903725));
#167730=CARTESIAN_POINT('Ctrl Pts',(43.502033101348,26.91999998,-170.861259130871));
#167731=CARTESIAN_POINT('Ctrl Pts',(42.6444458925864,26.91999998,-171.400720533971));
#167732=CARTESIAN_POINT('Ctrl Pts',(43.1661128544364,26.1158519257145,-171.07256826174));
#167733=CARTESIAN_POINT('',(41.0569324495328,26.91999998,-167.025025538602));
#167734=CARTESIAN_POINT('Origin',(41.0569324495328,26.41999998,-167.025025538602));
#167735=CARTESIAN_POINT('Ctrl Pts',(41.0569324495328,26.91999998,-167.025025538602));
#167736=CARTESIAN_POINT('Ctrl Pts',(41.879954591083,26.91999998,-168.29867810854));
#167737=CARTESIAN_POINT('Ctrl Pts',(42.6945981803054,26.91999998,-169.577671730211));
#167738=CARTESIAN_POINT('Ctrl Pts',(43.502033101348,26.91999998,-170.861259130871));
#167739=CARTESIAN_POINT('Ctrl Pts',(40.7299249439254,26.1062890581509,-167.236334669472));
#167740=CARTESIAN_POINT('Ctrl Pts',(40.1792441039429,26.91999998,-167.592179375443));
#167741=CARTESIAN_POINT('Ctrl Pts',(41.0569324495329,26.91999998,-167.025025538602));
#167742=CARTESIAN_POINT('Ctrl Pts',(40.4102462106017,26.1294636129469,-166.776026902216));
#167743=CARTESIAN_POINT('Ctrl Pts',(39.9306704790183,26.9199999799922,-167.069096608359));
#167744=CARTESIAN_POINT('Ctrl Pts',(40.7691972872111,26.91999998,-166.579746336928));
#167745=CARTESIAN_POINT('Ctrl Pts',(40.151813332835,26.1538945559334,-166.290857209798));
#167746=CARTESIAN_POINT('Ctrl Pts',(39.7259665151012,26.91999998,-166.517209541042));
#167747=CARTESIAN_POINT('Ctrl Pts',(40.5366320006225,26.91999998,-166.110608556751));
#167748=CARTESIAN_POINT('Ctrl Pts',(39.8265523607132,26.1917953794806,-165.538288752884));
#167749=CARTESIAN_POINT('Ctrl Pts',(39.4788563322456,26.91999998,-165.67366929337));
#167750=CARTESIAN_POINT('Ctrl Pts',(40.2438971241064,26.91999998,-165.383070268286));
#167751=CARTESIAN_POINT('Ctrl Pts',(39.7288584282001,26.2046468301746,-165.283122127771));
#167752=CARTESIAN_POINT('Ctrl Pts',(39.4079009250289,26.91999998,-165.399136176622));
#167753=CARTESIAN_POINT('Ctrl Pts',(40.1559725857258,26.91999998,-165.136425734968));
#167754=CARTESIAN_POINT('Ctrl Pts',(39.5527294533689,26.2307412681496,-164.765032944851));
#167755=CARTESIAN_POINT('Ctrl Pts',(39.2839209216265,26.91999998,-164.848652791671));
#167756=CARTESIAN_POINT('Ctrl Pts',(39.9974565076864,26.91999998,-164.635718209756));
#167757=CARTESIAN_POINT('Ctrl Pts',(39.4741198514661,26.2440255255985,-164.501291002302));
#167758=CARTESIAN_POINT('Ctrl Pts',(39.2299261071797,26.91999998,-164.57143444594));
#167759=CARTESIAN_POINT('Ctrl Pts',(39.9267078667251,26.91999998,-164.380863661625));
#167760=CARTESIAN_POINT('Ctrl Pts',(39.2672961864197,26.2840285028959,-163.707086385033));
#167761=CARTESIAN_POINT('Ctrl Pts',(39.0964160674726,26.91999998,-163.760078926904));
#167762=CARTESIAN_POINT('Ctrl Pts',(39.7405665669667,26.91999998,-163.613547303229));
#167763=CARTESIAN_POINT('Ctrl Pts',(39.1671866999672,26.3109338019081,-163.172923345691));
#167764=CARTESIAN_POINT('Ctrl Pts',(39.0354484142071,26.919999979999,-163.210393447583));
#167765=CARTESIAN_POINT('Ctrl Pts',(39.6504680302044,26.91999998,-163.097634164455));
#167766=CARTESIAN_POINT('Ctrl Pts',(39.0334891635878,26.3651575479723,-162.096254993545));
#167767=CARTESIAN_POINT('Ctrl Pts',(38.9750776668959,26.9199999800009,-162.116493741208));
#167768=CARTESIAN_POINT('Ctrl Pts',(39.530140246995,26.91999998,-162.058113878045));
#167769=CARTESIAN_POINT('Ctrl Pts',(39.,26.3924773748256,-161.553722423305));
#167770=CARTESIAN_POINT('Ctrl Pts',(38.9716965848467,26.9199999800009,-161.56923273356));
#167771=CARTESIAN_POINT('Ctrl Pts',(39.5000000005343,26.91999998,-161.534480343589));
#167772=CARTESIAN_POINT('Ctrl Pts',(39.,26.41999998,-161.0070032805));
#167773=CARTESIAN_POINT('Ctrl Pts',(39.,26.91999998,-161.0070032805));
#167774=CARTESIAN_POINT('Ctrl Pts',(39.5,26.91999998,-161.0070032805));
#167775=CARTESIAN_POINT('',(39.5,26.91999998,-161.0070032805));
#167776=CARTESIAN_POINT('Origin',(39.5,26.41999998,-161.0070032805));
#167777=CARTESIAN_POINT('Ctrl Pts',(39.5,26.91999998,-161.0070032805));
#167778=CARTESIAN_POINT('Ctrl Pts',(39.5,26.91999998,-161.534495292789));
#167779=CARTESIAN_POINT('Ctrl Pts',(39.5301402469972,26.91999998,-162.058113878039));
#167780=CARTESIAN_POINT('Ctrl Pts',(39.5903041384792,26.91999998,-162.577874021264));
#167781=CARTESIAN_POINT('Ctrl Pts',(39.6504680299611,26.91999998,-163.097634164489));
#167782=CARTESIAN_POINT('Ctrl Pts',(39.7405665669947,26.91999998,-163.613547303305));
#167783=CARTESIAN_POINT('Ctrl Pts',(39.864660766352,26.91999998,-164.12509154227));
#167784=CARTESIAN_POINT('Ctrl Pts',(39.9267078660346,26.91999998,-164.380863661769));
#167785=CARTESIAN_POINT('Ctrl Pts',(39.997456507107,26.91999998,-164.6357182099));
#167786=CARTESIAN_POINT('Ctrl Pts',(40.0767145462179,26.91999998,-164.886071972517));
#167787=CARTESIAN_POINT('Ctrl Pts',(40.1559725853186,26.91999998,-165.136425735101));
#167788=CARTESIAN_POINT('Ctrl Pts',(40.2438971237555,26.91999998,-165.383070268404));
#167789=CARTESIAN_POINT('Ctrl Pts',(40.3414754155803,26.91999998,-165.625583031388));
#167790=CARTESIAN_POINT('Ctrl Pts',(40.4688793539733,26.91999998,-165.942221912198));
#167791=CARTESIAN_POINT('Ctrl Pts',(40.6122052010724,26.91999998,-166.252046258612));
#167792=CARTESIAN_POINT('Ctrl Pts',(40.7764339005761,26.91999998,-166.552924284035));
#167793=CARTESIAN_POINT('Ctrl Pts',(40.863769731484,26.91999998,-166.712929401482));
#167794=CARTESIAN_POINT('Ctrl Pts',(40.9570176103072,26.91999998,-166.870404192076));
#167795=CARTESIAN_POINT('Ctrl Pts',(41.0569324495328,26.91999998,-167.025025538601));
#167796=CARTESIAN_POINT('Origin',(39.5,26.41999998,-55.24995));
#167797=CARTESIAN_POINT('',(39.5,26.91999998,-71.0516396909898));
#167798=CARTESIAN_POINT('Origin',(39.5,26.41999998,-71.0516396909898));
#167799=CARTESIAN_POINT('',(39.5,26.91999998,-55.24995));
#167800=CARTESIAN_POINT('Ctrl Pts',(39.,26.4199999799992,-71.0516396909892));
#167801=CARTESIAN_POINT('Ctrl Pts',(38.9999999999991,26.91999998,-71.0516396909893));
#167802=CARTESIAN_POINT('Ctrl Pts',(39.5,26.91999998,-71.0516396909898));
#167803=CARTESIAN_POINT('Ctrl Pts',(39.0000000000007,26.3924765441606,-70.5049040476121));
#167804=CARTESIAN_POINT('Ctrl Pts',(38.9716957320515,26.91999998,-70.4893932974167));
#167805=CARTESIAN_POINT('Ctrl Pts',(39.5000000005637,26.91999998,-70.5241467046182));
#167806=CARTESIAN_POINT('Ctrl Pts',(39.033491503913,26.3651705337364,-69.9626458947041));
#167807=CARTESIAN_POINT('Ctrl Pts',(38.9750894758337,26.91999998,-69.9424423105591));
#167808=CARTESIAN_POINT('Ctrl Pts',(39.530142353303,26.91999998,-70.0007779304057));
#167809=CARTESIAN_POINT('Ctrl Pts',(39.1669830003526,26.3110025024839,-68.8870836756328));
#167810=CARTESIAN_POINT('Ctrl Pts',(39.0353396916727,26.91999998,-68.8496793569739));
#167811=CARTESIAN_POINT('Ctrl Pts',(39.6502847005361,26.91999998,-68.962325974017));
#167812=CARTESIAN_POINT('Ctrl Pts',(39.2668900453864,26.2841390411479,-68.3537511575017));
#167813=CARTESIAN_POINT('Ctrl Pts',(39.096159008118,26.91999998,-68.300908425027));
#167814=CARTESIAN_POINT('Ctrl Pts',(39.7402010400563,26.91999998,-68.4472152479348));
#167815=CARTESIAN_POINT('Ctrl Pts',(39.5417383881002,26.2309152444135,-67.2970652120671));
#167816=CARTESIAN_POINT('Ctrl Pts',(39.2771671667713,26.9199999800001,-67.1992781955699));
#167817=CARTESIAN_POINT('Ctrl Pts',(39.9875645500817,26.91999998,-67.4263054007275));
#167818=CARTESIAN_POINT('Ctrl Pts',(39.717260119628,26.2045403217606,-66.7734209576797));
#167819=CARTESIAN_POINT('Ctrl Pts',(39.4035340747194,26.91999998,-66.6423091570439));
#167820=CARTESIAN_POINT('Ctrl Pts',(40.1455341066151,26.91999998,-66.9202222962256));
#167821=CARTESIAN_POINT('Ctrl Pts',(40.1516150766926,26.1539079466874,-65.7680517499882));
#167822=CARTESIAN_POINT('Ctrl Pts',(39.7258338602466,26.91999998,-65.5416509613312));
#167823=CARTESIAN_POINT('Ctrl Pts',(40.5364535700734,26.91999998,-65.9482917889975));
#167824=CARTESIAN_POINT('Ctrl Pts',(40.4103610815574,26.1294552845028,-65.2824506673441));
#167825=CARTESIAN_POINT('Ctrl Pts',(39.9307518154148,26.91999998,-64.9893751942709));
#167826=CARTESIAN_POINT('Ctrl Pts',(40.7693010717051,26.91999998,-65.4787360246525));
#167827=CARTESIAN_POINT('Ctrl Pts',(40.7299249439368,26.1062890581501,-64.8223083020179));
#167828=CARTESIAN_POINT('Ctrl Pts',(40.1792441039523,26.91999998,-64.466463596043));
#167829=CARTESIAN_POINT('Ctrl Pts',(41.0569324495432,26.91999998,-65.0336174328882));
#167830=CARTESIAN_POINT('',(41.0569324495432,26.91999998,-65.0336174328882));
#167831=CARTESIAN_POINT('Origin',(41.0569324495432,26.41999998,-65.0336174328882));
#167832=CARTESIAN_POINT('Ctrl Pts',(41.0569324495432,26.91999998,-65.0336174328882));
#167833=CARTESIAN_POINT('Ctrl Pts',(40.8648408575287,26.91999998,-65.3308851945503));
#167834=CARTESIAN_POINT('Ctrl Pts',(40.6972294070544,26.91999998,-65.6389714709824));
#167835=CARTESIAN_POINT('Ctrl Pts',(40.5488568184269,26.91999998,-65.9555599509455));
#167836=CARTESIAN_POINT('Ctrl Pts',(40.4750173837555,26.91999998,-66.1131140827442));
#167837=CARTESIAN_POINT('Ctrl Pts',(40.4059436807378,26.91999998,-66.2727743327563));
#167838=CARTESIAN_POINT('Ctrl Pts',(40.3409938376608,26.91999998,-66.4342570423367));
#167839=CARTESIAN_POINT('Ctrl Pts',(40.1455341065928,26.91999998,-66.9202222963147));
#167840=CARTESIAN_POINT('Ctrl Pts',(39.9875645491708,26.91999998,-67.4263054005813));
#167841=CARTESIAN_POINT('Ctrl Pts',(39.8638827946265,26.91999998,-67.936760324224));
#167842=CARTESIAN_POINT('Ctrl Pts',(39.7402010400822,26.91999998,-68.4472152478667));
#167843=CARTESIAN_POINT('Ctrl Pts',(39.6502847003092,26.91999998,-68.9623259739815));
#167844=CARTESIAN_POINT('Ctrl Pts',(39.5902135268069,26.91999998,-69.4815519521983));
#167845=CARTESIAN_POINT('Ctrl Pts',(39.5301423533046,26.91999998,-70.0007779304152));
#167846=CARTESIAN_POINT('Ctrl Pts',(39.5000000000007,26.91999998,-70.5241306955437));
#167847=CARTESIAN_POINT('Ctrl Pts',(39.5,26.91999998,-71.0516396909898));
#167848=CARTESIAN_POINT('Ctrl Pts',(43.3501517762232,26.91999998,-61.4386408691297));
#167849=CARTESIAN_POINT('Ctrl Pts',(42.4913556541499,26.91999998,-60.8975655472507));
#167850=CARTESIAN_POINT('Ctrl Pts',(43.0147613882085,26.1152677387813,-61.2273317382593));
#167851=CARTESIAN_POINT('Ctrl Pts',(42.5924607769204,26.91999998,-62.641249943458));
#167852=CARTESIAN_POINT('Ctrl Pts',(41.7218722762073,26.9199999800149,-62.1010809579055));
#167853=CARTESIAN_POINT('Ctrl Pts',(42.2597213352523,26.1123501122717,-62.4299407790815));
#167854=CARTESIAN_POINT('Ctrl Pts',(41.828377509759,26.91999998,-63.839782013441));
#167855=CARTESIAN_POINT('Ctrl Pts',(40.950890457431,26.91999998,-63.291651632712));
#167856=CARTESIAN_POINT('Ctrl Pts',(41.4984253110313,26.1093585902154,-63.6284728402189));
#167857=CARTESIAN_POINT('Ctrl Pts',(41.0569324495432,26.91999998,-65.0336174328882));
#167858=CARTESIAN_POINT('Ctrl Pts',(40.1792441039523,26.91999998,-64.466463596043));
#167859=CARTESIAN_POINT('Ctrl Pts',(40.7299249439368,26.1062890581501,-64.8223083020179));
#167860=CARTESIAN_POINT('',(43.3501517762232,26.91999998,-61.4386408691297));
#167861=CARTESIAN_POINT('Origin',(43.3501517762232,26.41999998,-61.4386408691297));
#167862=CARTESIAN_POINT('Ctrl Pts',(43.3501517762232,26.91999998,-61.4386408691297));
#167863=CARTESIAN_POINT('Ctrl Pts',(42.5924607769204,26.91999998,-62.641249943458));
#167864=CARTESIAN_POINT('Ctrl Pts',(41.828377509759,26.91999998,-63.839782013441));
#167865=CARTESIAN_POINT('Ctrl Pts',(41.0569324495432,26.91999998,-65.0336174328882));
#167866=CARTESIAN_POINT('Ctrl Pts',(43.0147613882086,26.1152677387813,-61.2273317382593));
#167867=CARTESIAN_POINT('Ctrl Pts',(42.4913556541499,26.91999998,-60.8975655472507));
#167868=CARTESIAN_POINT('Ctrl Pts',(43.3501517762232,26.91999998,-61.4386408691297));
#167869=CARTESIAN_POINT('Ctrl Pts',(43.0636216624014,26.1311367864154,-61.1268955825468));
#167870=CARTESIAN_POINT('Ctrl Pts',(42.6316122966568,26.9199999800009,-60.7676176413114));
#167871=CARTESIAN_POINT('Ctrl Pts',(43.3818037825525,26.91999998,-61.3884029511195));
#167872=CARTESIAN_POINT('Ctrl Pts',(43.1254911751643,26.1512115744493,-61.0418249229491));
#167873=CARTESIAN_POINT('Ctrl Pts',(42.7839211391678,26.91999998,-60.6895038034116));
#167874=CARTESIAN_POINT('Ctrl Pts',(43.4218378639138,26.91999998,-61.3458874687825));
#167875=CARTESIAN_POINT('Ctrl Pts',(43.2683662178942,26.1974732479793,-60.8948259755643));
#167876=CARTESIAN_POINT('Ctrl Pts',(43.0730867590013,26.91999998,-60.5931776502515));
#167877=CARTESIAN_POINT('Ctrl Pts',(43.5142348068871,26.91999998,-61.2723879804742));
#167878=CARTESIAN_POINT('Ctrl Pts',(43.3469540657763,26.2228767030678,-60.8357750676355));
#167879=CARTESIAN_POINT('Ctrl Pts',(43.2058848140176,26.9199999800003,-60.57262210769));
#167880=CARTESIAN_POINT('Ctrl Pts',(43.5650210354047,26.91999998,-61.2428625417913));
#167881=CARTESIAN_POINT('Ctrl Pts',(43.512870268579,26.2763890014657,-60.7418969884463));
#167882=CARTESIAN_POINT('Ctrl Pts',(43.4490485146957,26.9199999799997,-60.5604852270767));
#167883=CARTESIAN_POINT('Ctrl Pts',(43.6721398787422,26.91999998,-61.1959234862494));
#167884=CARTESIAN_POINT('Ctrl Pts',(43.6010803778225,26.3047810522968,-60.7070015638854));
#167885=CARTESIAN_POINT('Ctrl Pts',(43.5624944559174,26.91999998,-60.5672455602404));
#167886=CARTESIAN_POINT('Ctrl Pts',(43.7290408259741,26.91999998,-61.1784757886431));
#167887=CARTESIAN_POINT('Ctrl Pts',(43.7785234711652,26.3617623367046,-60.6613392327119));
#167888=CARTESIAN_POINT('Ctrl Pts',(43.7695073126827,26.9199999800001,-60.5973801431191));
#167889=CARTESIAN_POINT('Ctrl Pts',(43.8433908708859,26.91999998,-61.1556446096555));
#167890=CARTESIAN_POINT('Ctrl Pts',(43.8687620016371,26.3906766531834,-60.64995));
#167891=CARTESIAN_POINT('Ctrl Pts',(43.8659505814334,26.91999998,-60.6197279239548));
#167892=CARTESIAN_POINT('Ctrl Pts',(43.901489846726,26.91999998,-61.1499500121981));
#167893=CARTESIAN_POINT('Ctrl Pts',(43.9604906504041,26.41999998,-60.64995));
#167894=CARTESIAN_POINT('Ctrl Pts',(43.9604906504041,26.91999998,-60.64995));
#167895=CARTESIAN_POINT('Ctrl Pts',(43.9604906504041,26.91999998,-61.14995));
#167896=CARTESIAN_POINT('',(43.9604906504041,26.91999998,-61.14995));
#167897=CARTESIAN_POINT('',(43.9604906504041,26.41999998,-60.64995));
#167898=CARTESIAN_POINT('Origin',(43.9604906504041,26.41999998,-61.14995));
#167899=CARTESIAN_POINT('Ctrl Pts',(43.0147613882085,26.1152677387814,-61.2273317382593));
#167900=CARTESIAN_POINT('Ctrl Pts',(43.0274763575341,26.1193973798922,-61.2011950859334));
#167901=CARTESIAN_POINT('Ctrl Pts',(43.0415632309696,26.1239712727001,-61.1750984307868));
#167902=CARTESIAN_POINT('Ctrl Pts',(43.0571164447522,26.1290191152281,-61.1492627867981));
#167903=CARTESIAN_POINT('Ctrl Pts',(43.0651699639752,26.131632909226,-61.1358849821584));
#167904=CARTESIAN_POINT('Ctrl Pts',(43.0736161127961,26.1343736036103,-61.1225765741374));
#167905=CARTESIAN_POINT('Ctrl Pts',(43.0824643698387,26.1372441135223,-61.1093641997718));
#167906=CARTESIAN_POINT('Ctrl Pts',(43.0987837821055,26.1425383804549,-61.0849957639026));
#167907=CARTESIAN_POINT('Ctrl Pts',(43.1164700502224,26.148273918697,-61.0609616514732));
#167908=CARTESIAN_POINT('Ctrl Pts',(43.1355429762965,26.1544559569961,-61.0374154010505));
#167909=CARTESIAN_POINT('Ctrl Pts',(43.1465990107172,26.1580395093026,-61.0237663073487));
#167910=CARTESIAN_POINT('Ctrl Pts',(43.1581203006806,26.161772866853,-61.0102803672665));
#167911=CARTESIAN_POINT('Ctrl Pts',(43.1701048827302,26.1656551276577,-60.9969808939406));
#167912=CARTESIAN_POINT('Ctrl Pts',(43.1787950777989,26.1684702115346,-60.9873372520484));
#167913=CARTESIAN_POINT('Ctrl Pts',(43.1877316752268,26.1713644971657,-60.9777879307699));
#167914=CARTESIAN_POINT('Ctrl Pts',(43.1969286965292,26.1743424112143,-60.9683254492567));
#167915=CARTESIAN_POINT('Ctrl Pts',(43.2109826450054,26.1788929552686,-60.9538658516032));
#167916=CARTESIAN_POINT('Ctrl Pts',(43.2255507321307,26.1836083308442,-60.939720140068));
#167917=CARTESIAN_POINT('Ctrl Pts',(43.240679422296,26.1885032267772,-60.92589299095));
#167918=CARTESIAN_POINT('Ctrl Pts',(43.2502919812774,26.1916133754649,-60.917107413019));
#167919=CARTESIAN_POINT('Ctrl Pts',(43.2601309161905,26.1947960145932,-60.9084506542873));
#167920=CARTESIAN_POINT('Ctrl Pts',(43.2702085065296,26.1980550109063,-60.8999260702465));
#167921=CARTESIAN_POINT('Ctrl Pts',(43.2793934354622,26.2010253290599,-60.8921565840934));
#167922=CARTESIAN_POINT('Ctrl Pts',(43.2887784322572,26.2040596634157,-60.8844958212145));
#167923=CARTESIAN_POINT('Ctrl Pts',(43.2983502312506,26.2071536395938,-60.8769643387686));
#167924=CARTESIAN_POINT('Ctrl Pts',(43.3244804473604,26.2155999375393,-60.8564040173416));
#167925=CARTESIAN_POINT('Ctrl Pts',(43.3520269426161,26.2244985424302,-60.8367910129159));
#167926=CARTESIAN_POINT('Ctrl Pts',(43.3809428948479,26.2338324224914,-60.8183059987373));
#167927=CARTESIAN_POINT('Ctrl Pts',(43.384685235144,26.2350404254371,-60.8159136440647));
#167928=CARTESIAN_POINT('Ctrl Pts',(43.3884504656939,26.2362557032945,-60.8135401319426));
#167929=CARTESIAN_POINT('Ctrl Pts',(43.3922384457186,26.2374782060985,-60.8111858058261));
#167930=CARTESIAN_POINT('Ctrl Pts',(43.3958601516481,26.2386470469122,-60.8089348232969));
#167931=CARTESIAN_POINT('Ctrl Pts',(43.4000029195312,26.2399839248036,-60.8063959387213));
#167932=CARTESIAN_POINT('Ctrl Pts',(43.4037184370012,26.2411828803464,-60.8041517225798));
#167933=CARTESIAN_POINT('Ctrl Pts',(43.4058774798864,26.2418795791118,-60.8028476353477));
#167934=CARTESIAN_POINT('Ctrl Pts',(43.4078918169659,26.2425295698655,-60.8016419018772));
#167935=CARTESIAN_POINT('Ctrl Pts',(43.4095725805353,26.2430719505222,-60.8006413710886));
#167936=CARTESIAN_POINT('Ctrl Pts',(43.4162296669324,26.2452201853826,-60.7966785175239));
#167937=CARTESIAN_POINT('Ctrl Pts',(43.4230090840535,26.2474073661611,-60.7927415272842));
#167938=CARTESIAN_POINT('Ctrl Pts',(43.4299120181182,26.24963387702,-60.7888356878748));
#167939=CARTESIAN_POINT('Ctrl Pts',(43.4520200484725,26.2567647244526,-60.7763264540602));
#167940=CARTESIAN_POINT('Ctrl Pts',(43.4754609305302,26.2643201821782,-60.7641300208485));
#167941=CARTESIAN_POINT('Ctrl Pts',(43.5002298509359,26.2722988221321,-60.7524745840402));
#167942=CARTESIAN_POINT('Ctrl Pts',(43.5102299430492,26.2755200822101,-60.7477688705979));
#167943=CARTESIAN_POINT('Ctrl Pts',(43.5204460297338,26.2788101645169,-60.743151597115));
#167944=CARTESIAN_POINT('Ctrl Pts',(43.5308756725033,26.2821682775036,-60.7386388333542));
#167945=CARTESIAN_POINT('Ctrl Pts',(43.5566971886473,26.2904822313576,-60.7274662165276));
#167946=CARTESIAN_POINT('Ctrl Pts',(43.5838500463463,26.299219566432,-60.7169226589352));
#167947=CARTESIAN_POINT('Ctrl Pts',(43.6123323823145,26.3083779270718,-60.7072553544966));
#167948=CARTESIAN_POINT('Ctrl Pts',(43.6266343653468,26.3129766621832,-60.7024010607968));
#167949=CARTESIAN_POINT('Ctrl Pts',(43.6412713379323,26.3176814759652,-60.6977682056505));
#167950=CARTESIAN_POINT('Ctrl Pts',(43.6562406894801,26.3224912600696,-60.6933921846514));
#167951=CARTESIAN_POINT('Ctrl Pts',(43.6594393144061,26.3235190063468,-60.6924571241179));
#167952=CARTESIAN_POINT('Ctrl Pts',(43.6626531147166,26.3245515451493,-60.6915338002814));
#167953=CARTESIAN_POINT('Ctrl Pts',(43.6658820550481,26.3255889226458,-60.6906225673019));
#167954=CARTESIAN_POINT('Ctrl Pts',(43.6683132129433,26.3263699926664,-60.6899364749542));
#167955=CARTESIAN_POINT('Ctrl Pts',(43.6716206439064,26.3274324944764,-60.6890177374869));
#167956=CARTESIAN_POINT('Ctrl Pts',(43.6738444898251,26.3281468390294,-60.6884086503619));
#167957=CARTESIAN_POINT('Ctrl Pts',(43.6745742430091,26.3283812505988,-60.6882087789296));
#167958=CARTESIAN_POINT('Ctrl Pts',(43.6751872771554,26.3285781630476,-60.6880417202069));
#167959=CARTESIAN_POINT('Ctrl Pts',(43.6756142713164,26.3287153133704,-60.6879255590549));
#167960=CARTESIAN_POINT('Ctrl Pts',(43.6800859617517,26.3301516182259,-60.6867090629997));
#167961=CARTESIAN_POINT('Ctrl Pts',(43.6848158056741,26.331670679367,-60.6854534743842));
#167962=CARTESIAN_POINT('Ctrl Pts',(43.6898019198389,26.3332718294864,-60.6841703749843));
#167963=CARTESIAN_POINT('Ctrl Pts',(43.7032213047287,26.3375810869581,-60.6807171037335));
#167964=CARTESIAN_POINT('Ctrl Pts',(43.7185191369564,26.3424921433827,-60.6770466408939));
#167965=CARTESIAN_POINT('Ctrl Pts',(43.735693185848,26.3480028948378,-60.6734097222796));
#167966=CARTESIAN_POINT('Ctrl Pts',(43.7533010892254,26.3536528600713,-60.6696809270516));
#167967=CARTESIAN_POINT('Ctrl Pts',(43.7728812161057,26.3599332090448,-60.6659874477524));
#167968=CARTESIAN_POINT('Ctrl Pts',(43.7944381567387,26.3668435503401,-60.662653882105));
#167969=CARTESIAN_POINT('Ctrl Pts',(43.8163462038058,26.3738664431023,-60.659266021353));
#167970=CARTESIAN_POINT('Ctrl Pts',(43.8402960134949,26.3815400288333,-60.6562500536345));
#167971=CARTESIAN_POINT('Ctrl Pts',(43.8662991796198,26.3898656652239,-60.6540003957982));
#167972=CARTESIAN_POINT('Ctrl Pts',(43.8929368536722,26.3983944569635,-60.651695843657));
#167973=CARTESIAN_POINT('Ctrl Pts',(43.9217293432544,26.4076075212788,-60.6501955756524));
#167974=CARTESIAN_POINT('Ctrl Pts',(43.9526957322241,26.4175079798945,-60.6499774413423));
#167975=CARTESIAN_POINT('Ctrl Pts',(43.9552789029716,26.4183338616306,-60.6499592448981));
#167976=CARTESIAN_POINT('Ctrl Pts',(43.9578772047001,26.419164527574,-60.64995));
#167977=CARTESIAN_POINT('Ctrl Pts',(43.9604906504041,26.41999998,-60.64995));
#167978=CARTESIAN_POINT('Ctrl Pts',(43.9604906504041,26.91999998,-61.14995));
#167979=CARTESIAN_POINT('Ctrl Pts',(43.9014853731981,26.91999998,-61.14995));
#167980=CARTESIAN_POINT('Ctrl Pts',(43.8433879790802,26.91999998,-61.1556451738328));
#167981=CARTESIAN_POINT('Ctrl Pts',(43.7862158462631,26.91999998,-61.1670601882964));
#167982=CARTESIAN_POINT('Ctrl Pts',(43.7290408237003,26.91999998,-61.178475779728));
#167983=CARTESIAN_POINT('Ctrl Pts',(43.6721412316922,26.91999998,-61.1959228882129));
#167984=CARTESIAN_POINT('Ctrl Pts',(43.6185804531072,26.91999998,-61.2193930049692));
#167985=CARTESIAN_POINT('Ctrl Pts',(43.5650151406998,26.91999998,-61.2428651084281));
#167986=CARTESIAN_POINT('Ctrl Pts',(43.5142347717189,26.91999998,-61.2723879193617));
#167987=CARTESIAN_POINT('Ctrl Pts',(43.4680362753946,26.91999998,-61.3091376491944));
#167988=CARTESIAN_POINT('Ctrl Pts',(43.4218479344169,26.91999998,-61.345879300707));
#167989=CARTESIAN_POINT('Ctrl Pts',(43.3818141153598,26.91999998,-61.3883863242137));
#167990=CARTESIAN_POINT('Ctrl Pts',(43.3501517762232,26.91999998,-61.4386408691297));
#167991=CARTESIAN_POINT('Origin',(57.,27.41999998,-58.24995));
#167992=CARTESIAN_POINT('',(57.,26.91999998,-55.74995));
#167993=CARTESIAN_POINT('Origin',(57.,27.41999998,-55.74995));
#167994=CARTESIAN_POINT('',(59.5,26.91999998,-58.24995));
#167995=CARTESIAN_POINT('Origin',(57.,26.91999998,-58.24995));
#167996=CARTESIAN_POINT('Origin',(59.5,27.41999998,-58.24995));
#167997=CARTESIAN_POINT('Origin',(59.5,27.41999998,-55.24995));
#167998=CARTESIAN_POINT('',(59.5,26.91999998,-174.34995));
#167999=CARTESIAN_POINT('',(59.5,26.91999998,-58.24995));
#168000=CARTESIAN_POINT('Origin',(59.5,27.41999998,-174.34995));
#168001=CARTESIAN_POINT('Origin',(57.,27.41999998,-174.34995));
#168002=CARTESIAN_POINT('',(57.,26.91999998,-176.84995));
#168003=CARTESIAN_POINT('Origin',(57.,26.91999998,-174.34995));
#168004=CARTESIAN_POINT('Origin',(57.,27.41999998,-176.84995));
#168005=CARTESIAN_POINT('Origin',(-83.2809572255632,27.41999998,-176.84995));
#168006=CARTESIAN_POINT('',(-83.2809572255632,26.9199999800001,-176.84995));
#168007=CARTESIAN_POINT('Origin',(51.176438378063,26.41999998,-55.24995));
#168008=CARTESIAN_POINT('',(50.676438378063,26.41999998,-172.64995));
#168009=CARTESIAN_POINT('Origin',(51.176438378063,26.41999998,-172.64995));
#168010=CARTESIAN_POINT('',(50.6813043436922,26.35041342952,-171.64995));
#168011=CARTESIAN_POINT('',(51.176438378063,26.91999998,-172.64995));
#168012=CARTESIAN_POINT('',(51.176438378063,26.91999998,-55.24995));
#168013=CARTESIAN_POINT('Origin',(51.176438378063,26.41999998,-172.64995));
#168014=CARTESIAN_POINT('Ctrl Pts',(49.6614955754677,26.91999998,-171.149950013428));
#168015=CARTESIAN_POINT('Ctrl Pts',(49.6615613687869,26.91999998,-171.65003477338));
#168016=CARTESIAN_POINT('Ctrl Pts',(49.6615614228195,26.419915218376,-171.649950001854));
#168017=CARTESIAN_POINT('Ctrl Pts',(49.8598777423236,26.91999998,-171.149923566191));
#168018=CARTESIAN_POINT('Ctrl Pts',(49.7963801113845,26.91999998,-171.659221103016));
#168019=CARTESIAN_POINT('Ctrl Pts',(49.7950967919746,26.4108007878185,-171.649930655763));
#168020=CARTESIAN_POINT('Ctrl Pts',(50.0581153532345,26.91999998,-171.188965548735));
#168021=CARTESIAN_POINT('Ctrl Pts',(49.925805728719,26.91999998,-171.695281914066));
#168022=CARTESIAN_POINT('Ctrl Pts',(49.9285358390788,26.4016930431424,-171.675956808335));
#168023=CARTESIAN_POINT('Ctrl Pts',(50.4245495045741,26.91999998,-171.339270411997));
#168024=CARTESIAN_POINT('Ctrl Pts',(50.158596728211,26.91999998,-171.81002165518));
#168025=CARTESIAN_POINT('Ctrl Pts',(50.1751936156598,26.3848578535179,-171.776157476854));
#168026=CARTESIAN_POINT('Ctrl Pts',(50.5925763632168,26.91999998,-171.450449746589));
#168027=CARTESIAN_POINT('Ctrl Pts',(50.2611581333694,26.9199999800027,-171.889069508911));
#168028=CARTESIAN_POINT('Ctrl Pts',(50.2882982365463,26.3771381960673,-171.850276197782));
#168029=CARTESIAN_POINT('Ctrl Pts',(50.8729854484245,26.91999998,-171.728129909852));
#168030=CARTESIAN_POINT('Ctrl Pts',(50.4287914752885,26.9199999799973,-172.075284894372));
#168031=CARTESIAN_POINT('Ctrl Pts',(50.4770517273591,26.3642554277389,-172.035396209825));
#168032=CARTESIAN_POINT('Ctrl Pts',(50.9852574060669,26.91999998,-171.894521542842));
#168033=CARTESIAN_POINT('Ctrl Pts',(50.4930523894858,26.91999998,-172.182240159756));
#168034=CARTESIAN_POINT('Ctrl Pts',(50.5526265126722,26.3590973697634,-172.14632470545));
#168035=CARTESIAN_POINT('Ctrl Pts',(51.1370394011144,26.91999998,-172.257389581842));
#168036=CARTESIAN_POINT('Ctrl Pts',(50.5794864614573,26.91999998,-172.409795949393));
#168037=CARTESIAN_POINT('Ctrl Pts',(50.6547971380307,26.3521241406573,-172.388239289312));
#168038=CARTESIAN_POINT('Ctrl Pts',(51.1764650716523,26.91999998,-172.453697958273));
#168039=CARTESIAN_POINT('Ctrl Pts',(50.601152291526,26.91999998,-172.529747068595));
#168040=CARTESIAN_POINT('Ctrl Pts',(50.6813362874954,26.350312836992,-172.519113452117));
#168041=CARTESIAN_POINT('Ctrl Pts',(51.1764383645034,26.91999998,-172.65014948338));
#168042=CARTESIAN_POINT('Ctrl Pts',(50.601137585018,26.91999998,-172.650072180543));
#168043=CARTESIAN_POINT('Ctrl Pts',(50.6813183099038,26.3503140627879,-172.650082990804));
#168044=CARTESIAN_POINT('Ctrl Pts',(49.6616970192851,26.91999998,-171.14995));
#168045=CARTESIAN_POINT('Ctrl Pts',(49.8600119386601,26.91999998,-171.149950000016));
#168046=CARTESIAN_POINT('Ctrl Pts',(50.058177378641,26.91999998,-171.18899099047));
#168047=CARTESIAN_POINT('Ctrl Pts',(50.4245495045741,26.91999998,-171.339270411997));
#168048=CARTESIAN_POINT('Ctrl Pts',(50.5925763632168,26.91999998,-171.450449746589));
#168049=CARTESIAN_POINT('Ctrl Pts',(50.8729854484245,26.91999998,-171.728129909852));
#168050=CARTESIAN_POINT('Ctrl Pts',(50.9852574060669,26.91999998,-171.894521542842));
#168051=CARTESIAN_POINT('Ctrl Pts',(51.1370137093498,26.91999998,-172.257328160063));
#168052=CARTESIAN_POINT('Ctrl Pts',(51.176438378046,26.91999998,-172.453565067926));
#168053=CARTESIAN_POINT('Ctrl Pts',(51.176438378063,26.91999998,-172.64995));
#168054=CARTESIAN_POINT('Origin',(-83.2809572255632,20.76999998,-61.14995));
#168055=CARTESIAN_POINT('',(51.1762622162812,20.76999998,-60.64995));
#168056=CARTESIAN_POINT('',(1.41024658483895E-14,20.76999998,-60.64995));
#168057=CARTESIAN_POINT('',(51.1762622162812,20.26999998,-61.14995));
#168058=CARTESIAN_POINT('Origin',(51.1762622162812,20.76999998,-61.14995));
#168059=CARTESIAN_POINT('',(-83.2809572255632,20.2699999800001,-61.14995));
#168060=CARTESIAN_POINT('Origin',(1.64641978096591E-14,26.4199999800001,
-61.14995));
#168061=CARTESIAN_POINT('',(50.6819512673597,26.91999998,-61.14995));
#168062=CARTESIAN_POINT('',(50.6819512673597,26.41999998,-60.64995));
#168063=CARTESIAN_POINT('Origin',(50.6819512673597,26.41999998,-61.14995));
#168064=CARTESIAN_POINT('',(1.64641978096591E-14,26.4199999800001,-60.64995));
#168065=CARTESIAN_POINT('',(-83.2809572255632,26.9199999800001,-61.14995));
#168066=CARTESIAN_POINT('Origin',(0.,-12.9675000200281,-61.64995));
#168067=CARTESIAN_POINT('Origin',(0.,-12.9675000200281,-60.64995));
#168068=CARTESIAN_POINT('Ctrl Pts',(37.,33.02054075664,-60.64995));
#168069=CARTESIAN_POINT('Ctrl Pts',(37.5,33.0205407566399,-60.64995));
#168070=CARTESIAN_POINT('Ctrl Pts',(37.5,33.02054075664,-61.14995));
#168071=CARTESIAN_POINT('Ctrl Pts',(36.9450144953722,32.8396166159335,-60.64995));
#168072=CARTESIAN_POINT('Ctrl Pts',(37.4999999999984,32.829451263505,-60.5918750690658));
#168073=CARTESIAN_POINT('Ctrl Pts',(37.5,32.9079637588407,-61.149950027061));
#168074=CARTESIAN_POINT('Ctrl Pts',(36.8889168804295,32.6559426968113,-60.6963841656953));
#168075=CARTESIAN_POINT('Ctrl Pts',(37.5,32.6176893530803,-60.5649300622629));
#168076=CARTESIAN_POINT('Ctrl Pts',(37.5,32.7934674553098,-61.173167066129));
#168077=CARTESIAN_POINT('Ctrl Pts',(36.8135029743542,32.4100449984504,-60.8387768064376));
#168078=CARTESIAN_POINT('Ctrl Pts',(37.5,32.2741011266166,-60.5989161145872));
#168079=CARTESIAN_POINT('Ctrl Pts',(37.5,32.6399623596936,-61.2443634115781));
#168080=CARTESIAN_POINT('Ctrl Pts',(36.7895122380439,32.3319990572285,-60.8990185151424));
#168081=CARTESIAN_POINT('Ctrl Pts',(37.5,32.1451108386466,-60.6268090630372));
#168082=CARTESIAN_POINT('Ctrl Pts',(37.5,32.5912011068259,-61.27448425119));
#168083=CARTESIAN_POINT('Ctrl Pts',(36.7467810375704,32.1932186054134,-61.0450197081848));
#168084=CARTESIAN_POINT('Ctrl Pts',(37.4999999999999,31.876172903305,-60.7353807030111));
#168085=CARTESIAN_POINT('Ctrl Pts',(37.5,32.5044425233165,-61.3474848604736));
#168086=CARTESIAN_POINT('Ctrl Pts',(36.7283245477951,32.1334017245463,-61.1290643654114));
#168087=CARTESIAN_POINT('Ctrl Pts',(37.5,31.7388049050588,-60.8179479783099));
#168088=CARTESIAN_POINT('Ctrl Pts',(37.5,32.4670287634048,-61.3894925929396));
#168089=CARTESIAN_POINT('Ctrl Pts',(36.7137393100582,32.0861766206928,-61.2273317382593));
#168090=CARTESIAN_POINT('Ctrl Pts',(37.5,31.6156971887288,-60.9443257831194));
#168091=CARTESIAN_POINT('Ctrl Pts',(37.5,32.4374646344434,-61.4386408691296));
#168092=CARTESIAN_POINT('',(37.,33.02054075664,-60.64995));
#168093=CARTESIAN_POINT('',(37.5,33.02054075664,-61.14995));
#168094=CARTESIAN_POINT('Origin',(37.,33.02054075664,-61.14995));
#168095=CARTESIAN_POINT('',(37.5,32.4374646344434,-61.4386408691296));
#168096=CARTESIAN_POINT('Ctrl Pts',(37.5,32.4374646344434,-61.4386408691296));
#168097=CARTESIAN_POINT('Ctrl Pts',(37.5,32.4670379954265,-61.3894770341505));
#168098=CARTESIAN_POINT('Ctrl Pts',(37.5,32.5044515673201,-61.3474771045912));
#168099=CARTESIAN_POINT('Ctrl Pts',(37.5,32.5478217582305,-61.3109844882787));
#168100=CARTESIAN_POINT('Ctrl Pts',(37.5,32.5912010725173,-61.2744841953601));
#168101=CARTESIAN_POINT('Ctrl Pts',(37.5,32.6399569706336,-61.2443658937749));
#168102=CARTESIAN_POINT('Ctrl Pts',(37.5,32.6911307205588,-61.2206312870705));
#168103=CARTESIAN_POINT('Ctrl Pts',(37.5,32.7200261312687,-61.2072294705187));
#168104=CARTESIAN_POINT('Ctrl Pts',(37.5,32.7497820420349,-61.1958060470671));
#168105=CARTESIAN_POINT('Ctrl Pts',(37.5,32.7801663767935,-61.1862777806123));
#168106=CARTESIAN_POINT('Ctrl Pts',(37.5,32.8113193812835,-61.1765084659306));
#168107=CARTESIAN_POINT('Ctrl Pts',(37.5,32.8431343593208,-61.168731309436));
#168108=CARTESIAN_POINT('Ctrl Pts',(37.5,32.8753810744804,-61.1629086143648));
#168109=CARTESIAN_POINT('Ctrl Pts',(37.5,32.9073189135582,-61.1571416921447));
#168110=CARTESIAN_POINT('Ctrl Pts',(37.5,32.9396816981555,-61.1532921099755));
#168111=CARTESIAN_POINT('Ctrl Pts',(37.5,32.9722439056898,-61.1513728702169));
#168112=CARTESIAN_POINT('Ctrl Pts',(37.5,32.9883041294273,-61.1504262691642));
#168113=CARTESIAN_POINT('Ctrl Pts',(37.5,33.0044127038512,-61.14995));
#168114=CARTESIAN_POINT('Ctrl Pts',(37.5,33.02054075664,-61.14995));
#168115=CARTESIAN_POINT('Origin',(37.,32.4374646344434,-61.4386408691297));
#168116=CARTESIAN_POINT('Ctrl Pts',(37.,33.02054075664,-60.64995));
#168117=CARTESIAN_POINT('Ctrl Pts',(36.9924666287437,32.9957529741621,-60.64995));
#168118=CARTESIAN_POINT('Ctrl Pts',(36.985335089206,32.9723043403195,-60.6508183507148));
#168119=CARTESIAN_POINT('Ctrl Pts',(36.9786128679924,32.9502135923693,-60.6522871953885));
#168120=CARTESIAN_POINT('Ctrl Pts',(36.9763217634444,32.942684501688,-60.6527878151398));
#168121=CARTESIAN_POINT('Ctrl Pts',(36.9740781118526,32.9353128465307,-60.6533585216106));
#168122=CARTESIAN_POINT('Ctrl Pts',(36.971881941803,32.9280985200821,-60.6539897266455));
#168123=CARTESIAN_POINT('Ctrl Pts',(36.965231374082,32.9062516842166,-60.6559011778243));
#168124=CARTESIAN_POINT('Ctrl Pts',(36.9590174442728,32.8858515293307,-60.6583648678132));
#168125=CARTESIAN_POINT('Ctrl Pts',(36.9532466191212,32.8669144251051,-60.66113439231));
#168126=CARTESIAN_POINT('Ctrl Pts',(36.9471591964415,32.8469383983284,-60.6640558577488));
#168127=CARTESIAN_POINT('Ctrl Pts',(36.9415662354112,32.8285949580227,-60.6673161203253));
#168128=CARTESIAN_POINT('Ctrl Pts',(36.9364609481188,32.811857241149,-60.6706709359492));
#168129=CARTESIAN_POINT('Ctrl Pts',(36.9310729056594,32.7941925096614,-60.6742115572677));
#168130=CARTESIAN_POINT('Ctrl Pts',(36.9262289085405,32.778319104586,-60.6778566924258));
#168131=CARTESIAN_POINT('Ctrl Pts',(36.9219209635135,32.7642065999614,-60.6813681849314));
#168132=CARTESIAN_POINT('Ctrl Pts',(36.9216127929121,32.7631970561973,-60.6816193809775));
#168133=CARTESIAN_POINT('Ctrl Pts',(36.9213073643478,32.7621965203486,-60.6818699150514));
#168134=CARTESIAN_POINT('Ctrl Pts',(36.9210046743457,32.7612049796934,-60.6821197101778));
#168135=CARTESIAN_POINT('Ctrl Pts',(36.9197702682111,32.7571613579714,-60.6831384046648));
#168136=CARTESIAN_POINT('Ctrl Pts',(36.9185820051841,32.7532673571459,-60.6841446812285));
#168137=CARTESIAN_POINT('Ctrl Pts',(36.9174407986844,32.7495220389772,-60.6851333445339));
#168138=CARTESIAN_POINT('Ctrl Pts',(36.9168701954346,32.7476493798929,-60.6856276761866));
#168139=CARTESIAN_POINT('Ctrl Pts',(36.9163106727964,32.745813915541,-60.6861177217765));
#168140=CARTESIAN_POINT('Ctrl Pts',(36.9157621566578,32.744015541504,-60.6866029019919));
#168141=CARTESIAN_POINT('Ctrl Pts',(36.9153143472532,32.7425473462224,-60.6869990038531));
#168142=CARTESIAN_POINT('Ctrl Pts',(36.9151803653871,32.7421075257166,-60.6871177040467));
#168143=CARTESIAN_POINT('Ctrl Pts',(36.9146094848417,32.7402377771945,-60.687629668855));
#168144=CARTESIAN_POINT('Ctrl Pts',(36.9144811009473,32.7398172941379,-60.6877448033369));
#168145=CARTESIAN_POINT('Ctrl Pts',(36.9143306295394,32.7393245233921,-60.6878799880567));
#168146=CARTESIAN_POINT('Ctrl Pts',(36.9141495553194,32.7387315882737,-60.6880432899671));
#168147=CARTESIAN_POINT('Ctrl Pts',(36.9043380451416,32.7066033872109,-60.696891807198));
#168148=CARTESIAN_POINT('Ctrl Pts',(36.8949659479171,32.6759477413478,-60.7069683211716));
#168149=CARTESIAN_POINT('Ctrl Pts',(36.8860481049607,32.646796740842,-60.7179589785711));
#168150=CARTESIAN_POINT('Ctrl Pts',(36.880623229728,32.6290636924553,-60.7246447820114));
#168151=CARTESIAN_POINT('Ctrl Pts',(36.8753661521547,32.6118864586659,-60.7316693183976));
#168152=CARTESIAN_POINT('Ctrl Pts',(36.870277794653,32.5952643697575,-60.7389662185715));
#168153=CARTESIAN_POINT('Ctrl Pts',(36.8634689774476,32.5730220715484,-60.7487303240677));
#168154=CARTESIAN_POINT('Ctrl Pts',(36.8569610178916,32.5517753515799,-60.7589817870678));
#168155=CARTESIAN_POINT('Ctrl Pts',(36.850751208167,32.5315126220667,-60.7695692092458));
#168156=CARTESIAN_POINT('Ctrl Pts',(36.8469896993187,32.519238745775,-60.7759823980503));
#168157=CARTESIAN_POINT('Ctrl Pts',(36.8433375714303,32.5073258680656,-60.7825189042054));
#168158=CARTESIAN_POINT('Ctrl Pts',(36.8397933289186,32.4957685477639,-60.7891471100307));
#168159=CARTESIAN_POINT('Ctrl Pts',(36.8394079005284,32.4945117152125,-60.789867912485));
#168160=CARTESIAN_POINT('Ctrl Pts',(36.8390237657356,32.4932591453848,-60.790589766835));
#168161=CARTESIAN_POINT('Ctrl Pts',(36.838640943046,32.492010897904,-60.7913125928568));
#168162=CARTESIAN_POINT('Ctrl Pts',(36.8383083204172,32.4909263348163,-60.7919406337175));
#168163=CARTESIAN_POINT('Ctrl Pts',(36.8379766343786,32.4898448569959,-60.7925695226016));
#168164=CARTESIAN_POINT('Ctrl Pts',(36.837645899059,32.4887665099017,-60.7931992041001));
#168165=CARTESIAN_POINT('Ctrl Pts',(36.8367126023148,32.485723539367,-60.7949760923178));
#168166=CARTESIAN_POINT('Ctrl Pts',(36.8359448549989,32.4832205295986,-60.7964541280974));
#168167=CARTESIAN_POINT('Ctrl Pts',(36.8350327265731,32.4802468787299,-60.7982289031365));
#168168=CARTESIAN_POINT('Ctrl Pts',(36.8345500410079,32.4786732644123,-60.799168089186));
#168169=CARTESIAN_POINT('Ctrl Pts',(36.8340269806588,32.4769680487848,-60.8001910085464));
#168170=CARTESIAN_POINT('Ctrl Pts',(36.8334181657035,32.4749833371142,-60.8013915861747));
#168171=CARTESIAN_POINT('Ctrl Pts',(36.8245987446436,32.4462323878243,-60.8187834053606));
#168172=CARTESIAN_POINT('Ctrl Pts',(36.8161386112744,32.4186750863256,-60.8373693003596));
#168173=CARTESIAN_POINT('Ctrl Pts',(36.8080717737016,32.3924160926302,-60.8569388251974));
#168174=CARTESIAN_POINT('Ctrl Pts',(36.7996545921008,32.3650166666973,-60.8773582575852));
#168175=CARTESIAN_POINT('Ctrl Pts',(36.7916655629267,32.3390306165208,-60.8988485370896));
#168176=CARTESIAN_POINT('Ctrl Pts',(36.7841265152786,32.3145232383288,-60.9211850004421));
#168177=CARTESIAN_POINT('Ctrl Pts',(36.778553909317,32.296408223251,-60.9376953495804));
#168178=CARTESIAN_POINT('Ctrl Pts',(36.7732267926098,32.2790999388228,-60.9546683305905));
#168179=CARTESIAN_POINT('Ctrl Pts',(36.7681487604643,32.2626081160615,-60.9720182616034));
#168180=CARTESIAN_POINT('Ctrl Pts',(36.7599928054858,32.2361201852846,-60.9998844215971));
#168181=CARTESIAN_POINT('Ctrl Pts',(36.7525209698787,32.2118726247007,-61.0284772793722));
#168182=CARTESIAN_POINT('Ctrl Pts',(36.7456966945039,32.1897381268672,-61.057655954971));
#168183=CARTESIAN_POINT('Ctrl Pts',(36.7381722170941,32.16533252777,-61.089828496865));
#168184=CARTESIAN_POINT('Ctrl Pts',(36.7314349486327,32.1434956696669,-61.1227130004321));
#168185=CARTESIAN_POINT('Ctrl Pts',(36.7254206591586,32.1240104384723,-61.1560745996167));
#168186=CARTESIAN_POINT('Ctrl Pts',(36.721175758641,32.1102577136761,-61.1796212995642));
#168187=CARTESIAN_POINT('Ctrl Pts',(36.7172906773545,32.0976754369519,-61.2034046454934));
#168188=CARTESIAN_POINT('Ctrl Pts',(36.7137393100582,32.0861766206928,-61.2273317382593));
#168189=CARTESIAN_POINT('Ctrl Pts',(37.5,30.3198029183591,-64.9254179945063));
#168190=CARTESIAN_POINT('Ctrl Pts',(37.5,29.4819543139165,-64.4114488783587));
#168191=CARTESIAN_POINT('Ctrl Pts',(36.7055659807482,29.9753365781776,-64.714108863636));
#168192=CARTESIAN_POINT('Ctrl Pts',(37.5,31.0308541172825,-63.7662953234662));
#168193=CARTESIAN_POINT('Ctrl Pts',(37.5000000000047,30.1937476367692,-63.2670920970213));
#168194=CARTESIAN_POINT('Ctrl Pts',(36.7083606505135,30.6839990376866,-63.5549861665061));
#168195=CARTESIAN_POINT('Ctrl Pts',(37.5,31.7365266751429,-62.6039057229559));
#168196=CARTESIAN_POINT('Ctrl Pts',(37.5,30.9051975556495,-62.1106946535587));
#168197=CARTESIAN_POINT('Ctrl Pts',(36.7110836457466,31.3874027455588,-62.3925965705953));
#168198=CARTESIAN_POINT('Ctrl Pts',(37.5,32.4374646344434,-61.4386408691296));
#168199=CARTESIAN_POINT('Ctrl Pts',(37.5,31.6156971887288,-60.9443257831195));
#168200=CARTESIAN_POINT('Ctrl Pts',(36.7137393100582,32.0861766206928,-61.2273317382593));
#168201=CARTESIAN_POINT('',(37.5,30.3198029183596,-64.9254179945056));
#168202=CARTESIAN_POINT('Ctrl Pts',(37.5,30.3198029183591,-64.9254179945063));
#168203=CARTESIAN_POINT('Ctrl Pts',(37.5,31.0308541172825,-63.7662953234662));
#168204=CARTESIAN_POINT('Ctrl Pts',(37.5,31.7365266751429,-62.6039057229559));
#168205=CARTESIAN_POINT('Ctrl Pts',(37.5,32.4374646344434,-61.4386408691296));
#168206=CARTESIAN_POINT('Origin',(37.,30.3198029183592,-64.9254179945062));
#168207=CARTESIAN_POINT('Ctrl Pts',(36.7055659807485,29.9753365781889,-64.7141088636423));
#168208=CARTESIAN_POINT('Ctrl Pts',(37.5,29.4819543139285,-64.4114488783659));
#168209=CARTESIAN_POINT('Ctrl Pts',(37.5,30.3198029183707,-64.9254179945125));
#168210=CARTESIAN_POINT('Ctrl Pts',(36.7276066422259,29.6936558584646,-65.1425806750807));
#168211=CARTESIAN_POINT('Ctrl Pts',(37.5,29.2617307842025,-64.8907595368038));
#168212=CARTESIAN_POINT('Ctrl Pts',(37.5,30.066275812609,-65.3387061138468));
#168213=CARTESIAN_POINT('Ctrl Pts',(36.7506399492972,29.4626112609503,-65.5904100084171));
#168214=CARTESIAN_POINT('Ctrl Pts',(37.4999999999999,29.0782932545581,-65.3939122854256));
#168215=CARTESIAN_POINT('Ctrl Pts',(37.5,29.8583501338385,-65.770493027413));
#168216=CARTESIAN_POINT('Ctrl Pts',(36.7981064172734,29.0734767074675,-66.5135522731121));
#168217=CARTESIAN_POINT('Ctrl Pts',(37.5,28.7875108426025,-66.3978618624443));
#168218=CARTESIAN_POINT('Ctrl Pts',(37.5,29.5081290337376,-66.6603034853058));
#168219=CARTESIAN_POINT('Ctrl Pts',(36.8225713421442,28.9158110192433,-66.9894827414662));
#168220=CARTESIAN_POINT('Ctrl Pts',(37.5,28.6734901542511,-66.902255679337));
#168221=CARTESIAN_POINT('Ctrl Pts',(37.5,29.3662299161008,-67.1188991703195));
#168222=CARTESIAN_POINT('Ctrl Pts',(36.8977082013987,28.5389562140588,-68.4518423383231));
#168223=CARTESIAN_POINT('Ctrl Pts',(37.5,28.43212483966,-68.3736721849867));
#168224=CARTESIAN_POINT('Ctrl Pts',(37.5,29.0270605890893,-68.5274557979285));
#168225=CARTESIAN_POINT('Ctrl Pts',(36.9485508209842,28.41999998,-69.4422434553462));
#168226=CARTESIAN_POINT('Ctrl Pts',(37.5,28.3657190858733,-69.3869874906105));
#168227=CARTESIAN_POINT('Ctrl Pts',(37.5,28.9199999811121,-69.4807175010263));
#168228=CARTESIAN_POINT('Ctrl Pts',(37.,28.41999998,-70.4461836365688));
#168229=CARTESIAN_POINT('Ctrl Pts',(37.5,28.41999998,-70.4461836365687));
#168230=CARTESIAN_POINT('Ctrl Pts',(37.5,28.91999998,-70.4461836365688));
#168231=CARTESIAN_POINT('',(37.5,28.91999998,-70.4461836365688));
#168232=CARTESIAN_POINT('Ctrl Pts',(37.5,28.91999998,-70.4461836365688));
#168233=CARTESIAN_POINT('Ctrl Pts',(37.5,28.91999998,-69.912174657427));
#168234=CARTESIAN_POINT('Ctrl Pts',(37.5,28.9527491161422,-69.3820227305296));
#168235=CARTESIAN_POINT('Ctrl Pts',(37.5,29.0202545273658,-68.8559643077838));
#168236=CARTESIAN_POINT('Ctrl Pts',(37.5,29.074821691239,-68.4307314910276));
#168237=CARTESIAN_POINT('Ctrl Pts',(37.5,29.1520996751838,-68.0081734812178));
#168238=CARTESIAN_POINT('Ctrl Pts',(37.5,29.2531734731887,-67.5884180460506));
#168239=CARTESIAN_POINT('Ctrl Pts',(37.5,29.3662299152087,-67.1188991701865));
#168240=CARTESIAN_POINT('Ctrl Pts',(37.5,29.5081290337322,-66.6603034853492));
#168241=CARTESIAN_POINT('Ctrl Pts',(37.5,29.6832395831696,-66.2153982561153));
#168242=CARTESIAN_POINT('Ctrl Pts',(37.5,29.8137242360819,-65.8838745152443));
#168243=CARTESIAN_POINT('Ctrl Pts',(37.5,29.9624113407221,-65.5596714884955));
#168244=CARTESIAN_POINT('Ctrl Pts',(37.5,30.1346313217786,-65.24493295738));
#168245=CARTESIAN_POINT('Ctrl Pts',(37.5,30.1935307469803,-65.1372920294355));
#168246=CARTESIAN_POINT('Ctrl Pts',(37.5,30.255183072144,-65.0307582682231));
#168247=CARTESIAN_POINT('Ctrl Pts',(37.5,30.3198029183595,-64.9254179945056));
#168248=CARTESIAN_POINT('Origin',(37.,28.91999998,-70.4461836365688));
#168249=CARTESIAN_POINT('Origin',(37.,28.91999998,-55.24995));
#168250=CARTESIAN_POINT('',(37.5,28.91999998,-91.34995));
#168251=CARTESIAN_POINT('',(37.5,28.91999998,-69.7748183683767));
#168252=CARTESIAN_POINT('',(37.,28.41999998,-91.34995));
#168253=CARTESIAN_POINT('Origin',(37.,28.91999998,-91.34995));
#168254=CARTESIAN_POINT('',(37.,28.41999998,-91.34995));
#168255=CARTESIAN_POINT('Origin',(38.,43.91999998,-58.24995));
#168256=CARTESIAN_POINT('',(38.,46.91999998,-58.24995));
#168257=CARTESIAN_POINT('',(37.5,46.41999998,-58.24995));
#168258=CARTESIAN_POINT('Origin',(38.,46.41999998,-58.24995));
#168259=CARTESIAN_POINT('',(37.5,43.91999998,-55.74995));
#168260=CARTESIAN_POINT('Origin',(37.5,43.91999998,-58.24995));
#168261=CARTESIAN_POINT('',(38.,43.91999998,-55.24995));
#168262=CARTESIAN_POINT('Origin',(38.,43.91999998,-55.74995));
#168263=CARTESIAN_POINT('Origin',(38.,43.91999998,-58.24995));
#168264=CARTESIAN_POINT('Origin',(0.,43.91999998,-58.24995));
#168265=CARTESIAN_POINT('',(38.5,43.91999998,-55.24995));
#168266=CARTESIAN_POINT('',(0.,43.91999998,-55.24995));
#168267=CARTESIAN_POINT('',(38.5,46.91999998,-58.24995));
#168268=CARTESIAN_POINT('Origin',(38.5,43.91999998,-58.24995));
#168269=CARTESIAN_POINT('',(-39.,46.91999998,-58.24995));
#168270=CARTESIAN_POINT('Origin',(38.5,43.91999998,-58.24995));
#168271=CARTESIAN_POINT('',(39.,43.91999998,-55.74995));
#168272=CARTESIAN_POINT('Origin',(38.5,43.91999998,-55.74995));
#168273=CARTESIAN_POINT('',(39.,46.41999998,-58.24995));
#168274=CARTESIAN_POINT('Origin',(39.,43.91999998,-58.24995));
#168275=CARTESIAN_POINT('Origin',(38.5,46.41999998,-58.24995));
#168276=CARTESIAN_POINT('Origin',(38.5,46.41999998,-129.34995));
#168277=CARTESIAN_POINT('',(39.,46.41999998,-91.9958480337503));
#168278=CARTESIAN_POINT('',(39.,46.41999998,-129.34995));
#168279=CARTESIAN_POINT('',(38.5,46.91999998,-91.84995));
#168280=CARTESIAN_POINT('Ctrl Pts',(39.,46.41999998,-91.9958480337503));
#168281=CARTESIAN_POINT('Ctrl Pts',(39.,46.4383593062444,-91.9958480337503));
#168282=CARTESIAN_POINT('Ctrl Pts',(38.9989710148889,46.4572833490541,-91.9952104626986));
#168283=CARTESIAN_POINT('Ctrl Pts',(38.9967508671932,46.4766440820793,-91.9938816236437));
#168284=CARTESIAN_POINT('Ctrl Pts',(38.9953313980197,46.4890225214778,-91.9930320197733));
#168285=CARTESIAN_POINT('Ctrl Pts',(38.9934248666238,46.5015785833831,-91.9919000447932));
#168286=CARTESIAN_POINT('Ctrl Pts',(38.9909875853142,46.5142679203736,-91.9904744337629));
#168287=CARTESIAN_POINT('Ctrl Pts',(38.9879236812039,46.5302196743252,-91.9886822994377));
#168288=CARTESIAN_POINT('Ctrl Pts',(38.9840210150448,46.5463837492805,-91.9864258165825));
#168289=CARTESIAN_POINT('Ctrl Pts',(38.9791896661436,46.5626525596803,-91.9836879413693));
#168290=CARTESIAN_POINT('Ctrl Pts',(38.9767739916931,46.5707869648802,-91.9823190037628));
#168291=CARTESIAN_POINT('Ctrl Pts',(38.9741260943782,46.5789471626428,-91.9808298188763));
#168292=CARTESIAN_POINT('Ctrl Pts',(38.9712345064629,46.5871170280941,-91.9792189642192));
#168293=CARTESIAN_POINT('Ctrl Pts',(38.9697887125053,46.5912019608197,-91.9784135368906));
#168294=CARTESIAN_POINT('Ctrl Pts',(38.9682819877514,46.5952892977622,-91.9775776967405));
#168295=CARTESIAN_POINT('Ctrl Pts',(38.9667128998072,46.5993768111374,-91.9767113231393));
#168296=CARTESIAN_POINT('Ctrl Pts',(38.9665488507948,46.5998041629213,-91.9766207433001));
#168297=CARTESIAN_POINT('Ctrl Pts',(38.9663841201167,46.6002315164782,-91.9765298297484));
#168298=CARTESIAN_POINT('Ctrl Pts',(38.9662187061398,46.6006588691706,-91.976438582373));
#168299=CARTESIAN_POINT('Ctrl Pts',(38.9660815493286,46.6010132185049,-91.9763629225087));
#168300=CARTESIAN_POINT('Ctrl Pts',(38.9659442495352,46.6013667545193,-91.9762872126274));
#168301=CARTESIAN_POINT('Ctrl Pts',(38.9658014814792,46.6017330596689,-91.9762085198219));
#168302=CARTESIAN_POINT('Ctrl Pts',(38.964878272724,46.6041017696637,-91.9756996532795));
#168303=CARTESIAN_POINT('Ctrl Pts',(38.9637824718195,46.6068475079059,-91.9750972858545));
#168304=CARTESIAN_POINT('Ctrl Pts',(38.9628075054374,46.6092327396235,-91.9745628844117));
#168305=CARTESIAN_POINT('Ctrl Pts',(38.9623758791192,46.6102887029911,-91.9743263001239));
#168306=CARTESIAN_POINT('Ctrl Pts',(38.9619686005258,46.611274297802,-91.9741033520448));
#168307=CARTESIAN_POINT('Ctrl Pts',(38.9616138110508,46.6121267335955,-91.9739093074448));
#168308=CARTESIAN_POINT('Ctrl Pts',(38.9614200658218,46.6125922360406,-91.9738033425893));
#168309=CARTESIAN_POINT('Ctrl Pts',(38.9612419963564,46.6130180505684,-91.973706020483));
#168310=CARTESIAN_POINT('Ctrl Pts',(38.9610842933711,46.6133939988585,-91.9736198702739));
#168311=CARTESIAN_POINT('Ctrl Pts',(38.9610119987885,46.6135663419795,-91.9735803770874));
#168312=CARTESIAN_POINT('Ctrl Pts',(38.9609443960246,46.6137272414247,-91.9735434559988));
#168313=CARTESIAN_POINT('Ctrl Pts',(38.9608751120365,46.6138919016539,-91.973505625203));
#168314=CARTESIAN_POINT('Ctrl Pts',(38.9567213876535,46.6237636372138,-91.9712375874808));
#168315=CARTESIAN_POINT('Ctrl Pts',(38.9518680842499,46.6344001787413,-91.9686174080448));
#168316=CARTESIAN_POINT('Ctrl Pts',(38.946177595039,46.6456366502153,-91.9656152575245));
#168317=CARTESIAN_POINT('Ctrl Pts',(38.9401988073236,46.657442397511,-91.9624610083931));
#168318=CARTESIAN_POINT('Ctrl Pts',(38.9333015040993,46.6699024228789,-91.9588870343257));
#168319=CARTESIAN_POINT('Ctrl Pts',(38.9252978398083,46.6828446406519,-91.9548765239483));
#168320=CARTESIAN_POINT('Ctrl Pts',(38.9201412478996,46.6911830382935,-91.9522926367924));
#168321=CARTESIAN_POINT('Ctrl Pts',(38.9145249398867,46.6997211758053,-91.949528013274));
#168322=CARTESIAN_POINT('Ctrl Pts',(38.9083979295449,46.7084008365676,-91.9465877544647));
#168323=CARTESIAN_POINT('Ctrl Pts',(38.9009630650995,46.7189332328916,-91.9430198764193));
#168324=CARTESIAN_POINT('Ctrl Pts',(38.892777050832,46.7296758500678,-91.9391926280371));
#168325=CARTESIAN_POINT('Ctrl Pts',(38.8837164293804,46.7405353151116,-91.9351210844034));
#168326=CARTESIAN_POINT('Ctrl Pts',(38.8751108750016,46.7508493666871,-91.9312540328625));
#168327=CARTESIAN_POINT('Ctrl Pts',(38.8657161059638,46.7612691278656,-91.9271661831289));
#168328=CARTESIAN_POINT('Ctrl Pts',(38.8554209343761,46.7716757316366,-91.9228953364302));
#168329=CARTESIAN_POINT('Ctrl Pts',(38.8548765192935,46.7722260393225,-91.922669491398));
#168330=CARTESIAN_POINT('Ctrl Pts',(38.8543295855841,46.7727763000726,-91.9224431416288));
#168331=CARTESIAN_POINT('Ctrl Pts',(38.8537801165802,46.7733264928175,-91.9222162951506));
#168332=CARTESIAN_POINT('Ctrl Pts',(38.8536544843425,46.7734522905335,-91.9221644282928));
#168333=CARTESIAN_POINT('Ctrl Pts',(38.85352882043,46.7735779836955,-91.9221125901406));
#168334=CARTESIAN_POINT('Ctrl Pts',(38.8534031249738,46.7737035723748,-91.9220607807091));
#168335=CARTESIAN_POINT('Ctrl Pts',(38.8462316750874,46.7808689301918,-91.9191048366159));
#168336=CARTESIAN_POINT('Ctrl Pts',(38.8389362233865,46.7877118845293,-91.9162395555616));
#168337=CARTESIAN_POINT('Ctrl Pts',(38.8315472950243,46.7942461691172,-91.9134652859837));
#168338=CARTESIAN_POINT('Ctrl Pts',(38.8181190696914,46.8061212126327,-91.9084234835463));
#168339=CARTESIAN_POINT('Ctrl Pts',(38.804374545969,46.8169853430965,-91.9036748558894));
#168340=CARTESIAN_POINT('Ctrl Pts',(38.7904695579344,46.8269040598907,-91.8992337321801));
#168341=CARTESIAN_POINT('Ctrl Pts',(38.7771257367623,46.8364224847054,-91.8949718399416));
#168342=CARTESIAN_POINT('Ctrl Pts',(38.7636334875039,46.8450704493382,-91.8909923724618));
#168343=CARTESIAN_POINT('Ctrl Pts',(38.7500931237289,46.8529065841947,-91.887282952442));
#168344=CARTESIAN_POINT('Ctrl Pts',(38.7362680437785,46.8609074911639,-91.8834955336402));
#168345=CARTESIAN_POINT('Ctrl Pts',(38.7223990660432,46.8680567950519,-91.8799962545976));
#168346=CARTESIAN_POINT('Ctrl Pts',(38.7086077471669,46.8743998864685,-91.8767851783845));
#168347=CARTESIAN_POINT('Ctrl Pts',(38.7029413913131,46.8770060341112,-91.8754658629034));
#168348=CARTESIAN_POINT('Ctrl Pts',(38.697284315972,46.8794776843018,-91.8741947680128));
#168349=CARTESIAN_POINT('Ctrl Pts',(38.6916560145369,46.8818135523074,-91.8729730791622));
#168350=CARTESIAN_POINT('Ctrl Pts',(38.690434966776,46.8823203137933,-91.8727080364219));
#168351=CARTESIAN_POINT('Ctrl Pts',(38.6892145306102,46.8828209021287,-91.8724452601857));
#168352=CARTESIAN_POINT('Ctrl Pts',(38.6879949385285,46.8833153304816,-91.8721847293447));
#168353=CARTESIAN_POINT('Ctrl Pts',(38.6845743466761,46.8847020544697,-91.8714540180803));
#168354=CARTESIAN_POINT('Ctrl Pts',(38.6811624576419,46.8860394931494,-91.870741323611));
#168355=CARTESIAN_POINT('Ctrl Pts',(38.6777616037319,46.8873292507991,-91.8700466429565));
#168356=CARTESIAN_POINT('Ctrl Pts',(38.6743607498219,46.8886190084487,-91.8693519623019));
#168357=CARTESIAN_POINT('Ctrl Pts',(38.6709709301683,46.8898610847578,-91.8686752954307));
#168358=CARTESIAN_POINT('Ctrl Pts',(38.6675943952643,46.8910570583194,-91.8680166390568));
#168359=CARTESIAN_POINT('Ctrl Pts',(38.6521588071316,46.8965243660297,-91.8650056384902));
#168360=CARTESIAN_POINT('Ctrl Pts',(38.6369789277987,46.9010399726731,-91.8623722770382));
#168361=CARTESIAN_POINT('Ctrl Pts',(38.6221553104875,46.9047591974349,-91.8601140144284));
#168362=CARTESIAN_POINT('Ctrl Pts',(38.6073316931762,46.9084784221968,-91.8578557518186));
#168363=CARTESIAN_POINT('Ctrl Pts',(38.5928631234692,46.9114011072647,-91.8559725211624));
#168364=CARTESIAN_POINT('Ctrl Pts',(38.5788026188502,46.9136563357898,-91.8544668874172));
#168365=CARTESIAN_POINT('Ctrl Pts',(38.5647421142311,46.915911564315,-91.8529612536721));
#168366=CARTESIAN_POINT('Ctrl Pts',(38.5510974137732,46.917496438632,-91.8518320044153));
#168367=CARTESIAN_POINT('Ctrl Pts',(38.5379391593889,46.918518762006,-91.851079193558));
#168368=CARTESIAN_POINT('Ctrl Pts',(38.5313600321968,46.919029923693,-91.8507027881294));
#168369=CARTESIAN_POINT('Ctrl Pts',(38.5249025899683,46.9194002702488,-91.8504204897178));
#168370=CARTESIAN_POINT('Ctrl Pts',(38.5185762063117,46.9196427903307,-91.8502322928751));
#168371=CARTESIAN_POINT('Ctrl Pts',(38.512249822655,46.9198853104125,-91.8500440960323));
#168372=CARTESIAN_POINT('Ctrl Pts',(38.5060545004698,46.91999998,-91.8499500002645));
#168373=CARTESIAN_POINT('Ctrl Pts',(38.5,46.91999998,-91.84995));
#168374=CARTESIAN_POINT('',(38.5,46.91999998,-129.34995));
#168375=CARTESIAN_POINT('Origin',(40.,31.080768958446,-179.64995));
#168376=CARTESIAN_POINT('',(39.,31.080768958446,-91.9958480337503));
#168377=CARTESIAN_POINT('Ctrl Pts',(39.3277310924369,30.3404619167909,-92.0491293459315));
#168378=CARTESIAN_POINT('Ctrl Pts',(39.2886346270581,30.3759652101421,-92.0422366709188));
#168379=CARTESIAN_POINT('Ctrl Pts',(39.2523153224603,30.4148006640942,-92.0360096476917));
#168380=CARTESIAN_POINT('Ctrl Pts',(39.219197064997,30.4564585863616,-92.0304533816565));
#168381=CARTESIAN_POINT('Ctrl Pts',(39.1844077477968,30.5002184572809,-92.024616761123));
#168382=CARTESIAN_POINT('Ctrl Pts',(39.1531513695584,30.5470922331216,-92.0195203571601));
#168383=CARTESIAN_POINT('Ctrl Pts',(39.125895733847,30.5964367240933,-92.0151624600667));
#168384=CARTESIAN_POINT('Ctrl Pts',(39.112241386304,30.6211569997895,-92.0129792696946));
#168385=CARTESIAN_POINT('Ctrl Pts',(39.099590693715,30.6464966177574,-92.0109813029423));
#168386=CARTESIAN_POINT('Ctrl Pts',(39.0879995509094,30.6723709176288,-92.0091676111272));
#168387=CARTESIAN_POINT('Ctrl Pts',(39.067970142895,30.7170815141512,-92.0060335652451));
#168388=CARTESIAN_POINT('Ctrl Pts',(39.0510881489839,30.7634337254292,-92.0034479181842));
#168389=CARTESIAN_POINT('Ctrl Pts',(39.0376514204517,30.8109406522508,-92.0014180562603));
#168390=CARTESIAN_POINT('Ctrl Pts',(39.0245645049345,30.857210779411,-91.9994410399468));
#168391=CARTESIAN_POINT('Ctrl Pts',(39.0147461926495,30.9045752998721,-91.9979911959902));
#168392=CARTESIAN_POINT('Ctrl Pts',(39.0084275646637,30.9525664602203,-91.9970678562248));
#168393=CARTESIAN_POINT('Ctrl Pts',(39.0028510130954,30.9949214115026,-91.9962529559286));
#168394=CARTESIAN_POINT('Ctrl Pts',(39.,31.0377638135206,-91.9958480382673));
#168395=CARTESIAN_POINT('Ctrl Pts',(39.,31.080768958446,-91.9958480337503));
#168396=CARTESIAN_POINT('',(39.,31.080768958446,-61.14995));
#168397=CARTESIAN_POINT('',(39.,31.080768958446,-129.34995));
#168398=CARTESIAN_POINT('Origin',(40.,31.080768958446,-61.14995));
#168399=CARTESIAN_POINT('Ctrl Pts',(29.,30.0207919771236,-76.4370443259982));
#168400=CARTESIAN_POINT('Ctrl Pts',(29.,29.2642096076976,-76.0137531166873));
#168401=CARTESIAN_POINT('Ctrl Pts',(28.2496025504691,29.6431021990262,-76.2257351951278));
#168402=CARTESIAN_POINT('Ctrl Pts',(29.,32.8015320477175,-71.4668042994815));
#168403=CARTESIAN_POINT('Ctrl Pts',(29.,32.0024463153694,-71.1716406391234));
#168404=CARTESIAN_POINT('Ctrl Pts',(28.2608542879989,32.4163856120597,-71.2554899486297));
#168405=CARTESIAN_POINT('Ctrl Pts',(29.,35.5206920342409,-66.4628921538691));
#168406=CARTESIAN_POINT('Ctrl Pts',(28.9999999999899,34.7556963975018,-66.1533445021367));
#168407=CARTESIAN_POINT('Ctrl Pts',(28.2706820191605,35.1297158291743,-66.2515800426151));
#168408=CARTESIAN_POINT('Ctrl Pts',(29.,38.2024209812184,-61.4386408691297));
#168409=CARTESIAN_POINT('Ctrl Pts',(29.,37.4942143736512,-61.0606306836509));
#168410=CARTESIAN_POINT('Ctrl Pts',(28.2795019009908,37.8065307949999,-61.2273317382593));
#168411=CARTESIAN_POINT('',(28.2795019009908,37.8065307949999,-61.2273317382593));
#168412=CARTESIAN_POINT('',(29.,38.2024209812184,-61.4386408691297));
#168413=CARTESIAN_POINT('Origin',(28.5,38.2024209812184,-61.4386408691297));
#168414=CARTESIAN_POINT('',(29.,30.0207919771236,-76.4370443259982));
#168415=CARTESIAN_POINT('Ctrl Pts',(29.,30.0207919771236,-76.4370443259982));
#168416=CARTESIAN_POINT('Ctrl Pts',(29.,32.8015436034469,-71.4667836449984));
#168417=CARTESIAN_POINT('Ctrl Pts',(29.,35.5206811754595,-66.4629124977081));
#168418=CARTESIAN_POINT('Ctrl Pts',(29.,38.2024209812184,-61.4386408691297));
#168419=CARTESIAN_POINT('Origin',(28.5,30.0207919771236,-76.4370443259982));
#168420=CARTESIAN_POINT('Ctrl Pts',(28.2795019009908,37.8065307949999,-61.2273317382593));
#168421=CARTESIAN_POINT('Ctrl Pts',(28.277453635604,37.1848867012263,-62.3941267255567));
#168422=CARTESIAN_POINT('Ctrl Pts',(28.275381852787,36.5706479594793,-63.5422196084077));
#168423=CARTESIAN_POINT('Ctrl Pts',(28.2732866240955,35.9637160883466,-64.6715679822654));
#168424=CARTESIAN_POINT('Ctrl Pts',(28.2711270058156,35.3381322707528,-65.8356229622629));
#168425=CARTESIAN_POINT('Ctrl Pts',(28.2689424796447,34.7203113773663,-66.9797636636303));
#168426=CARTESIAN_POINT('Ctrl Pts',(28.2667339239111,34.1101940280727,-68.1039712769445));
#168427=CARTESIAN_POINT('Ctrl Pts',(28.2644834413072,33.4884943082005,-69.2495206685244));
#168428=CARTESIAN_POINT('Ctrl Pts',(28.2622080112682,32.8747935600169,-70.3743730692533));
#168429=CARTESIAN_POINT('Ctrl Pts',(28.2599093458026,32.2690767258885,-71.4785358153589));
#168430=CARTESIAN_POINT('Ctrl Pts',(28.257539766533,31.6446735341878,-72.616761969858));
#168431=CARTESIAN_POINT('Ctrl Pts',(28.2551454983198,31.0287545675081,-73.7330022870964));
#168432=CARTESIAN_POINT('Ctrl Pts',(28.2527292012792,30.4213516569412,-74.827292366658));
#168433=CARTESIAN_POINT('Ctrl Pts',(28.2516909581113,30.1603605985564,-75.2974908478906));
#168434=CARTESIAN_POINT('Ctrl Pts',(28.2506486572428,29.900942426465,-75.76363703424));
#168435=CARTESIAN_POINT('Ctrl Pts',(28.2496025504691,29.6431021990262,-76.2257351951278));
#168436=CARTESIAN_POINT('Ctrl Pts',(28.2496025504691,29.6431021990262,-76.2257351951279));
#168437=CARTESIAN_POINT('Ctrl Pts',(29.,29.2642096076976,-76.0137531166872));
#168438=CARTESIAN_POINT('Ctrl Pts',(29.,30.0207919771236,-76.4370443259982));
#168439=CARTESIAN_POINT('Ctrl Pts',(28.2688173873502,29.4296103781281,-76.5845570406398));
#168440=CARTESIAN_POINT('Ctrl Pts',(29.,29.0941349251779,-76.4054204039549));
#168441=CARTESIAN_POINT('Ctrl Pts',(29.,29.8286446521612,-76.7804846793283));
#168442=CARTESIAN_POINT('Ctrl Pts',(28.2886273449575,29.2500516159651,-76.9550303093546));
#168443=CARTESIAN_POINT('Ctrl Pts',(29.,28.9500939111529,-76.8125874626777));
#168444=CARTESIAN_POINT('Ctrl Pts',(29.,29.6670464531659,-77.134908720041));
#168445=CARTESIAN_POINT('Ctrl Pts',(28.3291630969748,28.9452627171061,-77.7145350708491));
#168446=CARTESIAN_POINT('Ctrl Pts',(29.,28.7180119748831,-77.6282159000457));
#168447=CARTESIAN_POINT('Ctrl Pts',(29.,29.392736442598,-77.861168463682));
#168448=CARTESIAN_POINT('Ctrl Pts',(28.3498943566417,28.8202033592585,-78.1036672968219));
#168449=CARTESIAN_POINT('Ctrl Pts',(29.,28.6262186304227,-78.0380158313972));
#168450=CARTESIAN_POINT('Ctrl Pts',(29.,29.2801830215621,-78.2330925203216));
#168451=CARTESIAN_POINT('Ctrl Pts',(28.3921729695334,28.6196836802033,-78.89905271603));
#168452=CARTESIAN_POINT('Ctrl Pts',(29.,28.4907909944947,-78.8635806040775));
#168453=CARTESIAN_POINT('Ctrl Pts',(29.,29.0997153099535,-78.9928975231766));
#168454=CARTESIAN_POINT('Ctrl Pts',(28.4137198127509,28.544609722815,-79.3053090810168));
#168455=CARTESIAN_POINT('Ctrl Pts',(29.,28.4446634876444,-79.2803896999264));
#168456=CARTESIAN_POINT('Ctrl Pts',(29.,29.0321487487139,-79.3807788748604));
#168457=CARTESIAN_POINT('Ctrl Pts',(28.4567512459693,28.4450459981447,-80.1187974753391));
#168458=CARTESIAN_POINT('Ctrl Pts',(29.,28.3995314322135,-80.1063804977281));
#168459=CARTESIAN_POINT('Ctrl Pts',(29.,28.9425413961498,-80.1570353641513));
#168460=CARTESIAN_POINT('Ctrl Pts',(28.4783422408471,28.41999998,-80.5280280808492));
#168461=CARTESIAN_POINT('Ctrl Pts',(29.,28.3978619671205,-80.5188978169702));
#168462=CARTESIAN_POINT('Ctrl Pts',(29.,28.9199999806373,-80.547320361459));
#168463=CARTESIAN_POINT('Ctrl Pts',(28.5,28.41999998,-80.9397703408579));
#168464=CARTESIAN_POINT('Ctrl Pts',(29.,28.41999998,-80.9397703408578));
#168465=CARTESIAN_POINT('Ctrl Pts',(29.,28.91999998,-80.9397703408579));
#168466=CARTESIAN_POINT('',(29.,28.91999998,-80.9397703408579));
#168467=CARTESIAN_POINT('Ctrl Pts',(29.,28.91999998,-80.9397703408579));
#168468=CARTESIAN_POINT('Ctrl Pts',(29.,28.9199999800001,-80.5473141158908));
#168469=CARTESIAN_POINT('Ctrl Pts',(29.,28.9425413961516,-80.1570353641503));
#168470=CARTESIAN_POINT('Ctrl Pts',(29.,28.98734507234,-79.7689071194953));
#168471=CARTESIAN_POINT('Ctrl Pts',(29.,29.0321487485283,-79.3807788748402));
#168472=CARTESIAN_POINT('Ctrl Pts',(29.,29.0997153099481,-78.9928975232084));
#168473=CARTESIAN_POINT('Ctrl Pts',(29.,29.1899491656343,-78.6129950217198));
#168474=CARTESIAN_POINT('Ctrl Pts',(29.,29.2801830213205,-78.2330925202312));
#168475=CARTESIAN_POINT('Ctrl Pts',(29.,29.3927364426023,-77.8611684636915));
#168476=CARTESIAN_POINT('Ctrl Pts',(29.,29.5298914474149,-77.498038591685));
#168477=CARTESIAN_POINT('Ctrl Pts',(29.,29.6670464522275,-77.1349087196785));
#168478=CARTESIAN_POINT('Ctrl Pts',(29.,29.8286298518252,-76.7805111234986));
#168479=CARTESIAN_POINT('Ctrl Pts',(29.,30.0207919771236,-76.4370443259982));
#168480=CARTESIAN_POINT('Origin',(28.5,28.91999998,-80.9397703408579));
#168481=CARTESIAN_POINT('Origin',(28.5,28.91999998,-55.24995));
#168482=CARTESIAN_POINT('',(29.,28.91999998,-91.34995));
#168483=CARTESIAN_POINT('',(29.,28.91999998,-80.3749072158811));
#168484=CARTESIAN_POINT('',(28.5,28.41999998,-91.34995));
#168485=CARTESIAN_POINT('Origin',(28.5,28.91999998,-91.34995));
#168486=CARTESIAN_POINT('',(28.5,28.41999998,-91.34995));
#168487=CARTESIAN_POINT('Origin',(29.5,43.91999998,-58.24995));
#168488=CARTESIAN_POINT('',(29.5,46.91999998,-58.24995));
#168489=CARTESIAN_POINT('',(29.,46.41999998,-58.24995));
#168490=CARTESIAN_POINT('Origin',(29.5,46.41999998,-58.24995));
#168491=CARTESIAN_POINT('',(29.,43.91999998,-55.74995));
#168492=CARTESIAN_POINT('Origin',(29.,43.91999998,-58.24995));
#168493=CARTESIAN_POINT('',(29.5,43.91999998,-55.24995));
#168494=CARTESIAN_POINT('Origin',(29.5,43.91999998,-55.74995));
#168495=CARTESIAN_POINT('Origin',(29.5,43.91999998,-58.24995));
#168496=CARTESIAN_POINT('Origin',(0.,43.91999998,-58.24995));
#168497=CARTESIAN_POINT('',(30.,46.91999998,-58.24995));
#168498=CARTESIAN_POINT('',(-39.,46.91999998,-58.24995));
#168499=CARTESIAN_POINT('',(30.,43.91999998,-55.24995));
#168500=CARTESIAN_POINT('',(0.,43.91999998,-55.24995));
#168501=CARTESIAN_POINT('Origin',(30.,43.91999998,-58.24995));
#168502=CARTESIAN_POINT('Origin',(30.,43.91999998,-58.24995));
#168503=CARTESIAN_POINT('',(30.5,43.91999998,-55.74995));
#168504=CARTESIAN_POINT('Origin',(30.,43.91999998,-55.74995));
#168505=CARTESIAN_POINT('',(30.5,46.41999998,-58.24995));
#168506=CARTESIAN_POINT('Origin',(30.5,43.91999998,-58.24995));
#168507=CARTESIAN_POINT('Origin',(30.,46.41999998,-58.24995));
#168508=CARTESIAN_POINT('Origin',(31.,28.91999998,-55.24995));
#168509=CARTESIAN_POINT('',(30.5,28.91999998,-78.0460091084363));
#168510=CARTESIAN_POINT('Origin',(31.,28.91999998,-78.0460091084363));
#168511=CARTESIAN_POINT('',(31.,28.41999998,-91.34995));
#168512=CARTESIAN_POINT('',(31.,28.41999998,-78.6384479219785));
#168513=CARTESIAN_POINT('',(30.5,28.91999998,-91.34995));
#168514=CARTESIAN_POINT('Origin',(31.,28.91999998,-91.34995));
#168515=CARTESIAN_POINT('',(30.5,28.91999998,-91.34995));
#168516=CARTESIAN_POINT('Ctrl Pts',(31.,28.41999998,-78.0460091084363));
#168517=CARTESIAN_POINT('Ctrl Pts',(30.5,28.4199999800001,-78.0460091084362));
#168518=CARTESIAN_POINT('Ctrl Pts',(30.5,28.91999998,-78.0460091084363));
#168519=CARTESIAN_POINT('Ctrl Pts',(30.9540427885061,28.41999998,-77.1674732790134));
#168520=CARTESIAN_POINT('Ctrl Pts',(30.4999999999986,28.4639319715929,-77.2061881935471));
#168521=CARTESIAN_POINT('Ctrl Pts',(30.5,28.9199999815576,-77.20604216556));
#168522=CARTESIAN_POINT('Ctrl Pts',(30.9086864990993,28.524456817556,-76.3042505917732));
#168523=CARTESIAN_POINT('Ctrl Pts',(30.5,28.594723031989,-76.3445661605256));
#168524=CARTESIAN_POINT('Ctrl Pts',(30.5,29.0140111325264,-76.3798194513939));
#168525=CARTESIAN_POINT('Ctrl Pts',(30.8417479231147,28.8453484758852,-75.0340652196707));
#168526=CARTESIAN_POINT('Ctrl Pts',(30.5,28.9540243183721,-75.0718611408805));
#168527=CARTESIAN_POINT('Ctrl Pts',(30.5,29.3028136269337,-75.1629449138939));
#168528=CARTESIAN_POINT('Ctrl Pts',(30.8195011122979,28.9813539161962,-74.6125811736547));
#168529=CARTESIAN_POINT('Ctrl Pts',(30.5,29.0970986774549,-74.6573700140041));
#168530=CARTESIAN_POINT('Ctrl Pts',(30.5,29.4252185218281,-74.758955076818));
#168531=CARTESIAN_POINT('Ctrl Pts',(30.7763886958648,29.3132233924744,-73.7967725466866));
#168532=CARTESIAN_POINT('Ctrl Pts',(30.5,29.4381839095486,-73.8581557735759));
#168533=CARTESIAN_POINT('Ctrl Pts',(30.5,29.7239010519754,-73.9766691906993));
#168534=CARTESIAN_POINT('Ctrl Pts',(30.7554505056092,29.508874874601,-73.4010655029222));
#168535=CARTESIAN_POINT('Ctrl Pts',(30.5,29.6348298970151,-73.4702277561984));
#168536=CARTESIAN_POINT('Ctrl Pts',(30.5,29.8999811721136,-73.5970610003643));
#168537=CARTESIAN_POINT('Ctrl Pts',(30.7353076117354,29.7418701453453,-73.0207363867646));
#168538=CARTESIAN_POINT('Ctrl Pts',(30.5,29.8691857803932,-73.0938794170476));
#168539=CARTESIAN_POINT('Ctrl Pts',(30.5,30.1096831288108,-73.2320455176344));
#168540=CARTESIAN_POINT('',(30.5,30.1096831288108,-73.2320455176344));
#168541=CARTESIAN_POINT('Origin',(31.,30.1096831288108,-73.2320455176344));
#168542=CARTESIAN_POINT('Ctrl Pts',(30.5,30.1096831288108,-73.2320455176344));
#168543=CARTESIAN_POINT('Ctrl Pts',(30.5,29.8999686314803,-73.5970828192481));
#168544=CARTESIAN_POINT('Ctrl Pts',(30.5,29.7239010511178,-73.976669190304));
#168545=CARTESIAN_POINT('Ctrl Pts',(30.5,29.5745597864535,-74.3678121335876));
#168546=CARTESIAN_POINT('Ctrl Pts',(30.5,29.4252185217892,-74.7589550768712));
#168547=CARTESIAN_POINT('Ctrl Pts',(30.5,29.3028136262495,-75.1629449137757));
#168548=CARTESIAN_POINT('Ctrl Pts',(30.5,29.2065461283391,-75.5685697596184));
#168549=CARTESIAN_POINT('Ctrl Pts',(30.5,29.0974180990883,-76.0283826871664));
#168550=CARTESIAN_POINT('Ctrl Pts',(30.5,29.0199506911356,-76.492948109106));
#168551=CARTESIAN_POINT('Ctrl Pts',(30.5,28.9733024240056,-76.9621397516276));
#168552=CARTESIAN_POINT('Ctrl Pts',(30.5,28.9376489765477,-77.3207447031834));
#168553=CARTESIAN_POINT('Ctrl Pts',(30.5,28.91999998,-77.6820522875113));
#168554=CARTESIAN_POINT('Ctrl Pts',(30.5,28.91999998,-78.0460091084363));
#168555=CARTESIAN_POINT('Ctrl Pts',(30.5,36.7276789742547,-61.4386408691296));
#168556=CARTESIAN_POINT('Ctrl Pts',(30.5,36.4678387256643,-61.2958335593366));
#168557=CARTESIAN_POINT('Ctrl Pts',(30.7601599624812,36.3431985357226,-61.2273317382593));
#168558=CARTESIAN_POINT('Ctrl Pts',(30.5,34.5564303542403,-65.3892634389964));
#168559=CARTESIAN_POINT('Ctrl Pts',(30.5,34.3134045700868,-65.2278638132481));
#168560=CARTESIAN_POINT('Ctrl Pts',(30.7526164452201,34.1766563796975,-65.1779528603621));
#168561=CARTESIAN_POINT('Ctrl Pts',(30.5,32.3553350664733,-69.3231754387568));
#168562=CARTESIAN_POINT('Ctrl Pts',(30.5,32.1210861733241,-69.1599841087648));
#168563=CARTESIAN_POINT('Ctrl Pts',(30.7443983582191,31.9809814038522,-69.1118639196982));
#168564=CARTESIAN_POINT('Ctrl Pts',(30.5,30.1096831288108,-73.2320455176344));
#168565=CARTESIAN_POINT('Ctrl Pts',(30.5,29.8691857803939,-73.0938794170475));
#168566=CARTESIAN_POINT('Ctrl Pts',(30.7353076117347,29.741870145346,-73.0207363867641));
#168567=CARTESIAN_POINT('',(30.5,36.7276789742547,-61.4386408691296));
#168568=CARTESIAN_POINT('Origin',(31.,36.7276789742547,-61.4386408691296));
#168569=CARTESIAN_POINT('Ctrl Pts',(30.5,36.7276789742547,-61.4386408691296));
#168570=CARTESIAN_POINT('Ctrl Pts',(30.5,34.5564250420216,-65.3892731044285));
#168571=CARTESIAN_POINT('Ctrl Pts',(30.5,32.355340677558,-69.3231656718822));
#168572=CARTESIAN_POINT('Ctrl Pts',(30.5,30.1096831288108,-73.2320455176344));
#168573=CARTESIAN_POINT('Ctrl Pts',(30.7601599624812,36.3431985357226,-61.2273317382593));
#168574=CARTESIAN_POINT('Ctrl Pts',(30.5,36.4678387256643,-61.2958335593366));
#168575=CARTESIAN_POINT('Ctrl Pts',(30.5,36.7276789742547,-61.4386408691297));
#168576=CARTESIAN_POINT('Ctrl Pts',(30.7833440352389,36.4311997587239,-61.0408976853214));
#168577=CARTESIAN_POINT('Ctrl Pts',(30.5,36.536757012545,-61.1328271281761));
#168578=CARTESIAN_POINT('Ctrl Pts',(30.5,36.7789093803379,-61.3454266101228));
#168579=CARTESIAN_POINT('Ctrl Pts',(30.820204224048,36.5713423922847,-60.8940610213177));
#168580=CARTESIAN_POINT('Ctrl Pts',(30.5000000000002,36.6495790716841,-60.9942767827739));
#168581=CARTESIAN_POINT('Ctrl Pts',(30.5,36.8604662025248,-61.2720055170969));
#168582=CARTESIAN_POINT('Ctrl Pts',(30.9048607560821,36.8949030802612,-60.6989334962026));
#168583=CARTESIAN_POINT('Ctrl Pts',(30.4999999999998,36.921160791843,-60.7754981362285));
#168584=CARTESIAN_POINT('Ctrl Pts',(30.5,37.0485310665384,-61.1744417416632));
#168585=CARTESIAN_POINT('Ctrl Pts',(30.9524183405754,37.0774198714491,-60.64995));
#168586=CARTESIAN_POINT('Ctrl Pts',(30.5,37.0857740751484,-60.6953661941756));
#168587=CARTESIAN_POINT('Ctrl Pts',(30.5,37.1545174137893,-61.1499500119967));
#168588=CARTESIAN_POINT('Ctrl Pts',(31.,37.2609769076718,-60.64995));
#168589=CARTESIAN_POINT('Ctrl Pts',(30.5,37.2609769076718,-60.64995));
#168590=CARTESIAN_POINT('Ctrl Pts',(30.5,37.2609769076718,-61.14995));
#168591=CARTESIAN_POINT('',(30.5,37.2609769076718,-61.14995));
#168592=CARTESIAN_POINT('',(31.,37.2609769076718,-60.64995));
#168593=CARTESIAN_POINT('Origin',(31.,37.2609769076718,-61.14995));
#168594=CARTESIAN_POINT('Ctrl Pts',(30.7601599624812,36.3431985357226,-61.2273317382593));
#168595=CARTESIAN_POINT('Ctrl Pts',(30.763965363455,36.3576429322361,-61.1967307159962));
#168596=CARTESIAN_POINT('Ctrl Pts',(30.7682373320678,36.3739555244459,-61.1662491652629));
#168597=CARTESIAN_POINT('Ctrl Pts',(30.773014719755,36.3922097826873,-61.1361721037419));
#168598=CARTESIAN_POINT('Ctrl Pts',(30.7743832716099,36.3974389791877,-61.1275560941091));
#168599=CARTESIAN_POINT('Ctrl Pts',(30.7757932280396,36.4028272069756,-61.1189733621298));
#168600=CARTESIAN_POINT('Ctrl Pts',(30.7772453313422,36.4083754424347,-61.1104308162074));
#168601=CARTESIAN_POINT('Ctrl Pts',(30.7822566925532,36.4275229864965,-61.0809495918337));
#168602=CARTESIAN_POINT('Ctrl Pts',(30.7877692333939,36.4485775577365,-61.0519471656573));
#168603=CARTESIAN_POINT('Ctrl Pts',(30.7938075568224,36.4715887509763,-61.0236793562699));
#168604=CARTESIAN_POINT('Ctrl Pts',(30.7956267481173,36.4785214307048,-61.0151629935126));
#168605=CARTESIAN_POINT('Ctrl Pts',(30.7974936059083,36.4856314523552,-61.0067135459256));
#168606=CARTESIAN_POINT('Ctrl Pts',(30.7994086489996,36.4929194816368,-60.9983386454677));
#168607=CARTESIAN_POINT('Ctrl Pts',(30.8053381175456,36.5154851046153,-60.9724077883165));
#168608=CARTESIAN_POINT('Ctrl Pts',(30.8117244764344,36.5397508645177,-60.9472021615385));
#168609=CARTESIAN_POINT('Ctrl Pts',(30.8185588211127,36.5657140442116,-60.9229694331518));
#168610=CARTESIAN_POINT('Ctrl Pts',(30.8212582864498,36.5759691172173,-60.9133978628872));
#168611=CARTESIAN_POINT('Ctrl Pts',(30.8240275191732,36.5864885832815,-60.9039784112583));
#168612=CARTESIAN_POINT('Ctrl Pts',(30.8268654522856,36.5972705027269,-60.8947276746678));
#168613=CARTESIAN_POINT('Ctrl Pts',(30.8318768733917,36.6163099714291,-60.8783920759203));
#168614=CARTESIAN_POINT('Ctrl Pts',(30.8371024716969,36.6361694013684,-60.8625813969166));
#168615=CARTESIAN_POINT('Ctrl Pts',(30.8425326224079,36.6568361342905,-60.8473901690906));
#168616=CARTESIAN_POINT('Ctrl Pts',(30.8452476977634,36.6671695007516,-60.8397945551776));
#168617=CARTESIAN_POINT('Ctrl Pts',(30.8480139129425,36.6777046960906,-60.8323538223576));
#168618=CARTESIAN_POINT('Ctrl Pts',(30.8508295920009,36.6884393999272,-60.8250806072626));
#168619=CARTESIAN_POINT('Ctrl Pts',(30.8522374315301,36.6938067518455,-60.8214439997151));
#168620=CARTESIAN_POINT('Ctrl Pts',(30.8536576365094,36.6992239800803,-60.8178492742012));
#168621=CARTESIAN_POINT('Ctrl Pts',(30.8550899796344,36.7046907663651,-60.814298049174));
#168622=CARTESIAN_POINT('Ctrl Pts',(30.8560154879301,36.7082231295039,-60.8120034256547));
#168623=CARTESIAN_POINT('Ctrl Pts',(30.8570682094331,36.7122433277919,-60.8094291323204));
#168624=CARTESIAN_POINT('Ctrl Pts',(30.8580115255638,36.7158468637295,-60.8071553682941));
#168625=CARTESIAN_POINT('Ctrl Pts',(30.8585281124733,36.7178202631368,-60.8059101900415));
#168626=CARTESIAN_POINT('Ctrl Pts',(30.8590117680525,36.7196682301612,-60.8047541406749));
#168627=CARTESIAN_POINT('Ctrl Pts',(30.8594229432602,36.7212394976976,-60.8037765840641));
#168628=CARTESIAN_POINT('Ctrl Pts',(30.8604475203524,36.7251548230705,-60.8013406830395));
#168629=CARTESIAN_POINT('Ctrl Pts',(30.8614836657748,36.7291158819178,-60.7989137988806));
#168630=CARTESIAN_POINT('Ctrl Pts',(30.8625314764417,36.7331228697491,-60.7964975160502));
#168631=CARTESIAN_POINT('Ctrl Pts',(30.8690570966094,36.7580778367397,-60.7814492401846));
#168632=CARTESIAN_POINT('Ctrl Pts',(30.8760300291748,36.784795266773,-60.7667926107252));
#168633=CARTESIAN_POINT('Ctrl Pts',(30.8834787244378,36.8133365487953,-60.7528950405293));
#168634=CARTESIAN_POINT('Ctrl Pts',(30.8856856098912,36.8217927062689,-60.7487774945135));
#168635=CARTESIAN_POINT('Ctrl Pts',(30.8879342100648,36.8304087431804,-60.7447268360333));
#168636=CARTESIAN_POINT('Ctrl Pts',(30.8902251321549,36.8391856521961,-60.7407532768451));
#168637=CARTESIAN_POINT('Ctrl Pts',(30.8958575471384,36.8607643842102,-60.730983964128));
#168638=CARTESIAN_POINT('Ctrl Pts',(30.9017446838295,36.8833145238806,-60.7216812541265));
#168639=CARTESIAN_POINT('Ctrl Pts',(30.9078839561844,36.9068356960058,-60.7130073200878));
#168640=CARTESIAN_POINT('Ctrl Pts',(30.9109535923618,36.9185962820684,-60.7086703530685));
#168641=CARTESIAN_POINT('Ctrl Pts',(30.9140861029083,36.9305993739776,-60.7044907499071));
#168642=CARTESIAN_POINT('Ctrl Pts',(30.9172801297012,36.9428432830316,-60.7004897073433));
#168643=CARTESIAN_POINT('Ctrl Pts',(30.9188771430977,36.9489652375587,-60.6984891860615));
#168644=CARTESIAN_POINT('Ctrl Pts',(30.9204895355962,36.9551473964347,-60.6965333068457));
#168645=CARTESIAN_POINT('Ctrl Pts',(30.9221170541162,36.9613894159181,-60.6946247772135));
#168646=CARTESIAN_POINT('Ctrl Pts',(30.9229308133762,36.9645104256597,-60.6936705123975));
#168647=CARTESIAN_POINT('Ctrl Pts',(30.9237483541366,36.967646400545,-60.6927280849868));
#168648=CARTESIAN_POINT('Ctrl Pts',(30.9245696419522,36.9707972931077,-60.6917978351345));
#168649=CARTESIAN_POINT('Ctrl Pts',(30.9251964133939,36.9732019184251,-60.6910879085654));
#168650=CARTESIAN_POINT('Ctrl Pts',(30.9260411033132,36.9764431639241,-60.6901460669173));
#168651=CARTESIAN_POINT('Ctrl Pts',(30.9266098300196,36.9786257121803,-60.6895206596725));
#168652=CARTESIAN_POINT('Ctrl Pts',(30.9267863324083,36.9793030585691,-60.6893265666725));
#168653=CARTESIAN_POINT('Ctrl Pts',(30.9269362296689,36.9798783303591,-60.6891624942613));
#168654=CARTESIAN_POINT('Ctrl Pts',(30.9270447106142,36.9802946739586,-60.6890439593315));
#168655=CARTESIAN_POINT('Ctrl Pts',(30.9302404200775,36.9925596222182,-60.6855520723829));
#168656=CARTESIAN_POINT('Ctrl Pts',(30.9338876720354,37.0065603067294,-60.6818105517145));
#168657=CARTESIAN_POINT('Ctrl Pts',(30.9379937153134,37.0223289997633,-60.6780391759794));
#168658=CARTESIAN_POINT('Ctrl Pts',(30.9420570063409,37.0379335086743,-60.6743070679258));
#168659=CARTESIAN_POINT('Ctrl Pts',(30.9465697396705,37.0552699885961,-60.6705458315636));
#168660=CARTESIAN_POINT('Ctrl Pts',(30.9515368184822,37.0743626826108,-60.6670184499722));
#168661=CARTESIAN_POINT('Ctrl Pts',(30.9564323410571,37.0931803253556,-60.6635418841948));
#168662=CARTESIAN_POINT('Ctrl Pts',(30.961769379885,37.1137045804594,-60.6602926154819));
#168663=CARTESIAN_POINT('Ctrl Pts',(30.9675481761194,37.135942761274,-60.6575694262484));
#168664=CARTESIAN_POINT('Ctrl Pts',(30.9731323446384,37.1574319684012,-60.654937953019));
#168665=CARTESIAN_POINT('Ctrl Pts',(30.9791291569654,37.1805221375206,-60.6527979719705));
#168666=CARTESIAN_POINT('Ctrl Pts',(30.9855324226127,37.2051964674286,-60.6514602685091));
#168667=CARTESIAN_POINT('Ctrl Pts',(30.9901458013928,37.2229736511785,-60.6504964895403));
#168668=CARTESIAN_POINT('Ctrl Pts',(30.9949700422445,37.2415727055254,-60.64995));
#168669=CARTESIAN_POINT('Ctrl Pts',(31.,37.2609769076718,-60.64995));
#168670=CARTESIAN_POINT('Ctrl Pts',(30.5,37.2609769076718,-61.14995));
#168671=CARTESIAN_POINT('Ctrl Pts',(30.5,37.2057964810293,-61.14995));
#168672=CARTESIAN_POINT('Ctrl Pts',(30.5,37.1508139868675,-61.156525590466));
#168673=CARTESIAN_POINT('Ctrl Pts',(30.5,37.0975659565498,-61.1696247206416));
#168674=CARTESIAN_POINT('Ctrl Pts',(30.5,37.0479567714747,-61.1818286870481));
#168675=CARTESIAN_POINT('Ctrl Pts',(30.5,36.9998515275001,-61.1996955772651));
#168676=CARTESIAN_POINT('Ctrl Pts',(30.5,36.9544986327132,-61.223223625875));
#168677=CARTESIAN_POINT('Ctrl Pts',(30.5,36.9220640062062,-61.2400499711984));
#168678=CARTESIAN_POINT('Ctrl Pts',(30.5,36.8911731746046,-61.2597722334506));
#168679=CARTESIAN_POINT('Ctrl Pts',(30.5,36.8624864317525,-61.2822151380553));
#168680=CARTESIAN_POINT('Ctrl Pts',(30.5,36.8352464003273,-61.3035262164813));
#168681=CARTESIAN_POINT('Ctrl Pts',(30.5,36.8099924249355,-61.3272911886641));
#168682=CARTESIAN_POINT('Ctrl Pts',(30.5,36.7873187400317,-61.3533954059166));
#168683=CARTESIAN_POINT('Ctrl Pts',(30.5,36.7660341218412,-61.377900390428));
#168684=CARTESIAN_POINT('Ctrl Pts',(30.5,36.7470225594145,-61.4044673363617));
#168685=CARTESIAN_POINT('Ctrl Pts',(30.5,36.7308159346661,-61.4330244036173));
#168686=CARTESIAN_POINT('Ctrl Pts',(30.5,36.7297582655658,-61.4348880814713));
#168687=CARTESIAN_POINT('Ctrl Pts',(30.5,36.7287125602851,-61.4367602423503));
#168688=CARTESIAN_POINT('Ctrl Pts',(30.5,36.7276789742547,-61.4386408691296));
#168689=CARTESIAN_POINT('Origin',(37.,-12.9675000200281,-61.14995));
#168690=CARTESIAN_POINT('',(37.,37.923330431502,-60.64995));
#168691=CARTESIAN_POINT('',(37.5,37.923330431502,-61.14995));
#168692=CARTESIAN_POINT('Origin',(37.,37.923330431502,-61.14995));
#168693=CARTESIAN_POINT('',(37.5,-9.33460238845303,-61.14995));
#168694=CARTESIAN_POINT('',(37.,-12.9675000200281,-60.64995));
#168695=CARTESIAN_POINT('Origin',(31.,-9.33460238845303,-61.14995));
#168696=CARTESIAN_POINT('',(30.5,38.4482624126576,-61.14995));
#168697=CARTESIAN_POINT('',(31.,38.4482624126576,-60.64995));
#168698=CARTESIAN_POINT('Origin',(31.,38.4482624126576,-61.14995));
#168699=CARTESIAN_POINT('',(31.,-12.9675000200281,-60.64995));
#168700=CARTESIAN_POINT('',(30.5,-9.33460238845303,-61.14995));
#168701=CARTESIAN_POINT('Origin',(0.,-12.9675000200281,-61.64995));
#168702=CARTESIAN_POINT('Origin',(0.,-12.9675000200281,-60.64995));
#168703=CARTESIAN_POINT('Origin',(32.85,-70.08000002,-174.34995));
#168704=CARTESIAN_POINT('',(33.35,-70.08000002,-176.84995));
#168705=CARTESIAN_POINT('Origin',(32.85,-70.08000002,-176.84995));
#168706=CARTESIAN_POINT('',(33.35,-72.58000002,-174.34995));
#168707=CARTESIAN_POINT('Origin',(33.35,-70.08000002,-174.34995));
#168708=CARTESIAN_POINT('Origin',(32.85,-72.58000002,-174.34995));
#168709=CARTESIAN_POINT('Origin',(32.85,-72.58000002,-55.24995));
#168710=CARTESIAN_POINT('',(33.35,-72.58000002,-58.24995));
#168711=CARTESIAN_POINT('',(33.35,-72.58000002,-174.34995));
#168712=CARTESIAN_POINT('Origin',(32.85,-72.58000002,-58.24995));
#168713=CARTESIAN_POINT('Ctrl Pts',(33.8806075480013,-61.4290931059938,
-60.6557206474106));
#168714=CARTESIAN_POINT('Ctrl Pts',(33.3500000000017,-61.4317841533,-60.6232112509527));
#168715=CARTESIAN_POINT('Ctrl Pts',(33.35,-61.3857298748211,-61.15282619958));
#168716=CARTESIAN_POINT('Ctrl Pts',(33.8204813483267,-61.214817269187,-60.6326735238177));
#168717=CARTESIAN_POINT('Ctrl Pts',(33.3499999999973,-61.2202673099084,
-60.6650058644588));
#168718=CARTESIAN_POINT('Ctrl Pts',(33.35,-61.2575945542474,-61.141321528844));
#168719=CARTESIAN_POINT('Ctrl Pts',(33.7566015486364,-60.9886558736888,
-60.6786599271601));
#168720=CARTESIAN_POINT('Ctrl Pts',(33.35,-61.0126032841866,-60.7560614808116));
#168721=CARTESIAN_POINT('Ctrl Pts',(33.35,-61.1220945388604,-61.1643294714043));
#168722=CARTESIAN_POINT('Ctrl Pts',(33.6462317574322,-60.5998176841187,
-60.9087900837106));
#168723=CARTESIAN_POINT('Ctrl Pts',(33.35,-60.6865246086057,-61.01647290262));
#168724=CARTESIAN_POINT('Ctrl Pts',(33.35,-60.8888304023229,-61.2794071648862));
#168725=CARTESIAN_POINT('Ctrl Pts',(33.5982385932668,-60.4318222621551,
-61.0947839923052));
#168726=CARTESIAN_POINT('Ctrl Pts',(33.3499999999994,-60.5516411453185,
-61.1871692827256));
#168727=CARTESIAN_POINT('Ctrl Pts',(33.35,-60.7878913738886,-61.3723612907971));
#168728=CARTESIAN_POINT('Ctrl Pts',(33.5744465072952,-60.3486837713638,
-61.3484667599621));
#168729=CARTESIAN_POINT('Ctrl Pts',(33.3500000000003,-60.4870054034178,
-61.4019031189409));
#168730=CARTESIAN_POINT('Ctrl Pts',(33.35,-60.7378676393038,-61.4992508410464));
#168731=CARTESIAN_POINT('',(33.35,-60.7669593817595,-61.4386408691297));
#168732=CARTESIAN_POINT('Origin',(33.85,-60.7669593817595,-61.4386408691297));
#168733=CARTESIAN_POINT('',(33.85,-61.3211699373828,-60.64995));
#168734=CARTESIAN_POINT('Ctrl Pts',(33.85,-61.3211699373828,-60.64995));
#168735=CARTESIAN_POINT('Ctrl Pts',(33.8408946232257,-61.2887822220266,
-60.64995));
#168736=CARTESIAN_POINT('Ctrl Pts',(33.8320360329935,-61.2574987712952,
-60.6514617262184));
#168737=CARTESIAN_POINT('Ctrl Pts',(33.8234947330584,-61.2274137239541,
-60.6541908134115));
#168738=CARTESIAN_POINT('Ctrl Pts',(33.8147158384926,-61.1964917963056,
-60.6569958160353));
#168739=CARTESIAN_POINT('Ctrl Pts',(33.8062719252371,-61.1668355547361,
-60.6610862959292));
#168740=CARTESIAN_POINT('Ctrl Pts',(33.7982087688177,-61.1385034904715,
-60.6661576313229));
#168741=CARTESIAN_POINT('Ctrl Pts',(33.7897805562155,-61.1088887033258,
-60.6714585693988));
#168742=CARTESIAN_POINT('Ctrl Pts',(33.7817681532881,-61.0807203975373,
-60.6778306117877));
#168743=CARTESIAN_POINT('Ctrl Pts',(33.7741937721167,-61.0540230202112,
-60.6849510110676));
#168744=CARTESIAN_POINT('Ctrl Pts',(33.7664268947605,-61.0266471527007,
-60.6922523689849));
#168745=CARTESIAN_POINT('Ctrl Pts',(33.7591202239172,-61.0008173969275,
-60.7003402004141));
#168746=CARTESIAN_POINT('Ctrl Pts',(33.7522713515567,-60.976523346829,-60.7088999701646));
#168747=CARTESIAN_POINT('Ctrl Pts',(33.7451537939754,-60.9512762271051,
-60.7177955446293));
#168748=CARTESIAN_POINT('Ctrl Pts',(33.7385302859764,-60.9276871255218,
-60.7272004222153));
#168749=CARTESIAN_POINT('Ctrl Pts',(33.7323756813871,-60.9057134546262,
-60.7368036104378));
#168750=CARTESIAN_POINT('Ctrl Pts',(33.7289765914216,-60.8935777466109,
-60.7421072981484));
#168751=CARTESIAN_POINT('Ctrl Pts',(33.7257201687046,-60.8819342854479,
-60.7474722461951));
#168752=CARTESIAN_POINT('Ctrl Pts',(33.7226000576368,-60.8707730258723,
-60.752851779779));
#168753=CARTESIAN_POINT('Ctrl Pts',(33.7176811117149,-60.8531769752573,
-60.7613327710671));
#168754=CARTESIAN_POINT('Ctrl Pts',(33.7131011490807,-60.836779646766,-60.7698488054675));
#168755=CARTESIAN_POINT('Ctrl Pts',(33.7088302172017,-60.8215350129312,
-60.77823724668));
#168756=CARTESIAN_POINT('Ctrl Pts',(33.7066947512622,-60.8139126960137,
-60.7824314672863));
#168757=CARTESIAN_POINT('Ctrl Pts',(33.7046364618188,-60.8065784470663,
-60.7865941739577));
#168758=CARTESIAN_POINT('Ctrl Pts',(33.7026512377244,-60.7995260481909,
-60.7907073021494));
#168759=CARTESIAN_POINT('Ctrl Pts',(33.7016586256772,-60.7959998487532,
-60.7927638662452));
#168760=CARTESIAN_POINT('Ctrl Pts',(33.700684285193,-60.7925441192497,-60.7948080508209));
#168761=CARTESIAN_POINT('Ctrl Pts',(33.6997276798046,-60.7891580545039,
-60.7968377444204));
#168762=CARTESIAN_POINT('Ctrl Pts',(33.6992493771104,-60.787465022131,-60.7978525912201));
#168763=CARTESIAN_POINT('Ctrl Pts',(33.6987755085231,-60.78578940642,-60.7988638162632));
#168764=CARTESIAN_POINT('Ctrl Pts',(33.6983060077729,-60.784131107961,-60.799871162729));
#168765=CARTESIAN_POINT('Ctrl Pts',(33.6979171366822,-60.7827575972046,
-60.8007055126608));
#168766=CARTESIAN_POINT('Ctrl Pts',(33.6977636893367,-60.7822136993763,
-60.8010361890538));
#168767=CARTESIAN_POINT('Ctrl Pts',(33.6972679602333,-60.780467262921,-60.802107581507));
#168768=CARTESIAN_POINT('Ctrl Pts',(33.6971651743236,-60.7801051517227,
-60.8023297271247));
#168769=CARTESIAN_POINT('Ctrl Pts',(33.697047717804,-60.7796914074066,-60.8025838438696));
#168770=CARTESIAN_POINT('Ctrl Pts',(33.6969105433143,-60.7792080657786,
-60.8028813142771));
#168771=CARTESIAN_POINT('Ctrl Pts',(33.687366364001,-60.7455786411208,-60.8235783907874));
#168772=CARTESIAN_POINT('Ctrl Pts',(33.6782837661359,-60.7137258174839,
-60.8458827892109));
#168773=CARTESIAN_POINT('Ctrl Pts',(33.6697182991571,-60.6837179852912,
-60.869478970828));
#168774=CARTESIAN_POINT('Ctrl Pts',(33.6610001352008,-60.653175202081,-60.89349580267));
#168775=CARTESIAN_POINT('Ctrl Pts',(33.6528175632848,-60.6245435544086,
-60.9188503903528));
#168776=CARTESIAN_POINT('Ctrl Pts',(33.6451985198799,-60.5978527728285,
-60.94522326713));
#168777=CARTESIAN_POINT('Ctrl Pts',(33.6373713547231,-60.5704329059907,
-60.9723165452788));
#168778=CARTESIAN_POINT('Ctrl Pts',(33.6301387768433,-60.5450611554622,
-61.0004840158148));
#168779=CARTESIAN_POINT('Ctrl Pts',(33.6235011899514,-60.5217288367252,
-61.0294008158947));
#168780=CARTESIAN_POINT('Ctrl Pts',(33.616755885099,-60.49801786987,-61.0587868917486));
#168781=CARTESIAN_POINT('Ctrl Pts',(33.6106247947373,-60.4764127066887,
-61.0889464349294));
#168782=CARTESIAN_POINT('Ctrl Pts',(33.6050809985361,-60.4568671948489,
-61.1195670593001));
#168783=CARTESIAN_POINT('Ctrl Pts',(33.5994074183963,-60.4368641096391,
-61.1509045327563));
#168784=CARTESIAN_POINT('Ctrl Pts',(33.5943486981784,-60.4190178726719,
-61.1827245851904));
#168785=CARTESIAN_POINT('Ctrl Pts',(33.5898513690894,-60.403246067445,-61.2147276758847));
#168786=CARTESIAN_POINT('Ctrl Pts',(33.5892613820072,-60.4011770257618,
-61.2189260366736));
#168787=CARTESIAN_POINT('Ctrl Pts',(33.5886810256773,-60.3991436438934,
-61.2231276001908));
#168788=CARTESIAN_POINT('Ctrl Pts',(33.5881101525802,-60.3971457002532,
-61.2273317382593));
#168789=CARTESIAN_POINT('',(33.35,-61.3211699373828,-61.14995));
#168790=CARTESIAN_POINT('Origin',(33.85,-61.3211699373828,-61.14995));
#168791=CARTESIAN_POINT('Ctrl Pts',(33.35,-60.7669593817595,-61.4386408691297));
#168792=CARTESIAN_POINT('Ctrl Pts',(33.35,-60.7854255655574,-61.4063230635264));
#168793=CARTESIAN_POINT('Ctrl Pts',(33.35,-60.8074669942766,-61.3766005831691));
#168794=CARTESIAN_POINT('Ctrl Pts',(33.35,-60.832315928212,-61.3495741724077));
#168795=CARTESIAN_POINT('Ctrl Pts',(33.35,-60.8598479301247,-61.3196295802289));
#168796=CARTESIAN_POINT('Ctrl Pts',(33.35,-60.8908254879517,-61.2929954345219));
#168797=CARTESIAN_POINT('Ctrl Pts',(33.35,-60.924148426403,-61.269769822738));
#168798=CARTESIAN_POINT('Ctrl Pts',(33.35,-60.9500168068532,-61.2517399313257));
#168799=CARTESIAN_POINT('Ctrl Pts',(33.35,-60.9772970763437,-61.2357633244769));
#168800=CARTESIAN_POINT('Ctrl Pts',(33.35,-61.0054624679791,-61.2218683128495));
#168801=CARTESIAN_POINT('Ctrl Pts',(33.35,-61.0316582964252,-61.2089449583455));
#168802=CARTESIAN_POINT('Ctrl Pts',(33.35,-61.0586931044519,-61.1978139207404));
#168803=CARTESIAN_POINT('Ctrl Pts',(33.35,-61.0863521110361,-61.1884108897488));
#168804=CARTESIAN_POINT('Ctrl Pts',(33.35,-61.1146264284014,-61.1787986760331));
#168805=CARTESIAN_POINT('Ctrl Pts',(33.35,-61.1435543947087,-61.1709920371076));
#168806=CARTESIAN_POINT('Ctrl Pts',(33.35,-61.1729286914007,-61.1649732421567));
#168807=CARTESIAN_POINT('Ctrl Pts',(33.35,-61.2017965294043,-61.1590582206179));
#168808=CARTESIAN_POINT('Ctrl Pts',(33.35,-61.2310968493209,-61.1548700235783));
#168809=CARTESIAN_POINT('Ctrl Pts',(33.35,-61.2606330881678,-61.1524405238988));
#168810=CARTESIAN_POINT('Ctrl Pts',(33.35,-61.2807251508687,-61.1507878537622));
#168811=CARTESIAN_POINT('Ctrl Pts',(33.35,-61.3009263849489,-61.14995));
#168812=CARTESIAN_POINT('Ctrl Pts',(33.35,-61.3211699373828,-61.14995));
#168813=CARTESIAN_POINT('Ctrl Pts',(33.35,-56.3642045114132,-69.0177323827589));
#168814=CARTESIAN_POINT('Ctrl Pts',(33.35,-56.134778922778,-68.8820528924306));
#168815=CARTESIAN_POINT('Ctrl Pts',(33.5712930253538,-56.006893899348,-68.8064232518886));
#168816=CARTESIAN_POINT('Ctrl Pts',(33.35,-57.8514943778664,-66.5028176210733));
#168817=CARTESIAN_POINT('Ctrl Pts',(33.35,-57.623019767821,-66.3564728841549));
#168818=CARTESIAN_POINT('Ctrl Pts',(33.5772316679252,-57.489551829777,-66.2915080112617));
#168819=CARTESIAN_POINT('Ctrl Pts',(33.35,-59.3174222737568,-63.975486542669));
#168820=CARTESIAN_POINT('Ctrl Pts',(33.35,-59.0838703919199,-63.828995910853));
#168821=CARTESIAN_POINT('Ctrl Pts',(33.5828208370019,-58.9513545007691,
-63.7641770795492));
#168822=CARTESIAN_POINT('Ctrl Pts',(33.35,-60.7669593817595,-61.4386408691297));
#168823=CARTESIAN_POINT('Ctrl Pts',(33.35,-60.5242644024533,-61.2999665374096));
#168824=CARTESIAN_POINT('Ctrl Pts',(33.5881101525803,-60.3971457002532,
-61.2273317382593));
#168825=CARTESIAN_POINT('',(33.35,-56.3642045114132,-69.0177323827589));
#168826=CARTESIAN_POINT('Origin',(33.85,-56.3642045114132,-69.0177323827589));
#168827=CARTESIAN_POINT('Ctrl Pts',(33.35,-56.3642045114132,-69.0177323827589));
#168828=CARTESIAN_POINT('Ctrl Pts',(33.35,-57.8514954063616,-66.5028158819518));
#168829=CARTESIAN_POINT('Ctrl Pts',(33.35,-59.3174212852614,-63.975488272466));
#168830=CARTESIAN_POINT('Ctrl Pts',(33.35,-60.7669593817595,-61.4386408691297));
#168831=CARTESIAN_POINT('Ctrl Pts',(33.5694121272515,-56.0311308231553,
-68.7681930766575));
#168832=CARTESIAN_POINT('Ctrl Pts',(33.35,-56.1587194716786,-68.8446841104126));
#168833=CARTESIAN_POINT('Ctrl Pts',(33.35,-56.3860793134489,-68.980989400591));
#168834=CARTESIAN_POINT('Ctrl Pts',(33.5910952109519,-55.7655514639883,
-69.1827326666124));
#168835=CARTESIAN_POINT('Ctrl Pts',(33.35,-55.8926720909797,-69.2555053068349));
#168836=CARTESIAN_POINT('Ctrl Pts',(33.35,-56.1470456681896,-69.379827229092));
#168837=CARTESIAN_POINT('Ctrl Pts',(33.6136638920077,-55.5467927199511,
-69.6144308420505));
#168838=CARTESIAN_POINT('Ctrl Pts',(33.35,-55.6739612204769,-69.6790964973634));
#168839=CARTESIAN_POINT('Ctrl Pts',(33.35,-55.9501721297621,-69.7949917247217));
#168840=CARTESIAN_POINT('Ctrl Pts',(33.659375070679,-55.1847160495168,-70.489496195354));
#168841=CARTESIAN_POINT('Ctrl Pts',(33.35,-55.3038384109907,-70.536501599542));
#168842=CARTESIAN_POINT('Ctrl Pts',(33.35,-55.6242976847011,-70.6362303826783));
#168843=CARTESIAN_POINT('Ctrl Pts',(33.682489279096,-55.039631648896,-70.9322999995547));
#168844=CARTESIAN_POINT('Ctrl Pts',(33.35,-55.152089096076,-70.9724572353069));
#168845=CARTESIAN_POINT('Ctrl Pts',(33.35,-55.4937179039915,-71.0617579129361));
#168846=CARTESIAN_POINT('Ctrl Pts',(33.7541801885443,-54.6881003351372,
-72.3070874300299));
#168847=CARTESIAN_POINT('Ctrl Pts',(33.35,-54.7604537006047,-72.352581791756));
#168848=CARTESIAN_POINT('Ctrl Pts',(33.35,-55.1773203769037,-72.3823434918717));
#168849=CARTESIAN_POINT('Ctrl Pts',(33.8033026557133,-54.5764726761907,
-73.2509483926675));
#168850=CARTESIAN_POINT('Ctrl Pts',(33.3499999999908,-54.6214526391974,
-73.2954399089219));
#168851=CARTESIAN_POINT('Ctrl Pts',(33.35,-55.076843343761,-73.2882195565875));
#168852=CARTESIAN_POINT('Ctrl Pts',(33.8525101260014,-54.580084950057,-74.1994042577821));
#168853=CARTESIAN_POINT('Ctrl Pts',(33.3500000000004,-54.5775630671305,
-74.1994064437527));
#168854=CARTESIAN_POINT('Ctrl Pts',(33.35,-55.0800755412332,-74.1975793503824));
#168855=CARTESIAN_POINT('',(33.35,-55.08000002,-74.155095361993));
#168856=CARTESIAN_POINT('Origin',(33.85,-55.08000002,-74.155095361993));
#168857=CARTESIAN_POINT('Ctrl Pts',(33.35,-55.08000002,-74.155095361993));
#168858=CARTESIAN_POINT('Ctrl Pts',(33.35,-55.0800000199996,-73.9307666441726));
#168859=CARTESIAN_POINT('Ctrl Pts',(33.35,-55.0863156531016,-73.7071338026571));
#168860=CARTESIAN_POINT('Ctrl Pts',(33.35,-55.099013419779,-73.4842001164092));
#168861=CARTESIAN_POINT('Ctrl Pts',(33.35,-55.1117111864564,-73.2612664301613));
#168862=CARTESIAN_POINT('Ctrl Pts',(33.35,-55.1307909278358,-73.0390315071252));
#168863=CARTESIAN_POINT('Ctrl Pts',(33.35,-55.1563760274665,-72.8175000855932));
#168864=CARTESIAN_POINT('Ctrl Pts',(33.35,-55.1806216024911,-72.6075670863644));
#168865=CARTESIAN_POINT('Ctrl Pts',(33.35,-55.2107500142178,-72.3979880684073));
#168866=CARTESIAN_POINT('Ctrl Pts',(33.35,-55.2468600350683,-72.1892231805732));
#168867=CARTESIAN_POINT('Ctrl Pts',(33.35,-55.2824608236504,-71.9834023457995));
#168868=CARTESIAN_POINT('Ctrl Pts',(33.35,-55.3238757306222,-71.7783731405225));
#168869=CARTESIAN_POINT('Ctrl Pts',(33.35,-55.3711489449075,-71.5745698720748));
#168870=CARTESIAN_POINT('Ctrl Pts',(33.35,-55.3771233770104,-71.5488130284138));
#168871=CARTESIAN_POINT('Ctrl Pts',(33.35,-55.3831913115128,-71.5230757533215));
#168872=CARTESIAN_POINT('Ctrl Pts',(33.35,-55.3893527788882,-71.4973589120773));
#168873=CARTESIAN_POINT('Ctrl Pts',(33.35,-55.49371790368,-71.061757912807));
#168874=CARTESIAN_POINT('Ctrl Pts',(33.35,-55.62429768467,-70.6362303826932));
#168875=CARTESIAN_POINT('Ctrl Pts',(33.35,-55.7846973533805,-70.2221616988514));
#168876=CARTESIAN_POINT('Ctrl Pts',(33.35,-55.9170285274604,-69.8805512982628));
#168877=CARTESIAN_POINT('Ctrl Pts',(33.35,-56.0694235889258,-69.5466508244303));
#168878=CARTESIAN_POINT('Ctrl Pts',(33.35,-56.2474267878585,-69.2225907452635));
#168879=CARTESIAN_POINT('Ctrl Pts',(33.35,-56.2851826822517,-69.1538550247853));
#168880=CARTESIAN_POINT('Ctrl Pts',(33.35,-56.3240908525654,-69.0855620876847));
#168881=CARTESIAN_POINT('Ctrl Pts',(33.35,-56.3642045114132,-69.0177323827589));
#168882=CARTESIAN_POINT('Origin',(33.85,-55.08000002,-55.24995));
#168883=CARTESIAN_POINT('',(33.35,-55.08000002,-157.903547609535));
#168884=CARTESIAN_POINT('Origin',(33.85,-55.08000002,-157.903547609535));
#168885=CARTESIAN_POINT('',(33.35,-55.08000002,-74.7820934264633));
#168886=CARTESIAN_POINT('Ctrl Pts',(33.85,-54.58000002,-157.903547609535));
#168887=CARTESIAN_POINT('Ctrl Pts',(33.35,-54.58000002,-157.903547609535));
#168888=CARTESIAN_POINT('Ctrl Pts',(33.35,-55.08000002,-157.903547609535));
#168889=CARTESIAN_POINT('Ctrl Pts',(33.801455552521,-54.58000002,-158.839330848163));
#168890=CARTESIAN_POINT('Ctrl Pts',(33.35,-54.6262905574736,-158.795882575748));
#168891=CARTESIAN_POINT('Ctrl Pts',(33.35,-55.0800000214226,-158.800807467734));
#168892=CARTESIAN_POINT('Ctrl Pts',(33.7535837781314,-54.6911524904427,
-159.759384984053));
#168893=CARTESIAN_POINT('Ctrl Pts',(33.3500000000032,-54.7641489713074,
-159.715131975651));
#168894=CARTESIAN_POINT('Ctrl Pts',(33.35,-55.180037242033,-159.683846218103));
#168895=CARTESIAN_POINT('Ctrl Pts',(33.6829913348673,-55.0359328654928,
-161.113586648345));
#168896=CARTESIAN_POINT('Ctrl Pts',(33.3499999999985,-55.1482360556977,
-161.073701561693));
#168897=CARTESIAN_POINT('Ctrl Pts',(33.35,-55.4903395816263,-160.984647645179));
#168898=CARTESIAN_POINT('Ctrl Pts',(33.6595586460473,-55.182326049271,-161.562665253801));
#168899=CARTESIAN_POINT('Ctrl Pts',(33.3499999999999,-55.3013905829052,
-161.515682361465));
#168900=CARTESIAN_POINT('Ctrl Pts',(33.35,-55.6220934455112,-161.416204912461));
#168901=CARTESIAN_POINT('Ctrl Pts',(33.6142892652062,-55.5406109894237,
-162.429616508549));
#168902=CARTESIAN_POINT('Ctrl Pts',(33.35,-55.6678404697842,-162.365570451247));
#168903=CARTESIAN_POINT('Ctrl Pts',(33.35,-55.9445498933141,-162.249650631001));
#168904=CARTESIAN_POINT('Ctrl Pts',(33.5923371961949,-55.7524367209228,
-162.849704728299));
#168905=CARTESIAN_POINT('Ctrl Pts',(33.3500000000047,-55.8797778942332,
-162.777810522451));
#168906=CARTESIAN_POINT('Ctrl Pts',(33.35,-56.1351840325082,-162.653651176326));
#168907=CARTESIAN_POINT('Ctrl Pts',(33.571293025353,-56.0068938993578,-163.252219719633));
#168908=CARTESIAN_POINT('Ctrl Pts',(33.35,-56.1347789227877,-163.176590079091));
#168909=CARTESIAN_POINT('Ctrl Pts',(33.35,-56.364204511422,-163.040910588762));
#168910=CARTESIAN_POINT('',(33.35,-56.3642045114216,-163.040910588762));
#168911=CARTESIAN_POINT('Origin',(33.85,-56.3642045114216,-163.040910588762));
#168912=CARTESIAN_POINT('Ctrl Pts',(33.35,-56.3642045114216,-163.040910588762));
#168913=CARTESIAN_POINT('Ctrl Pts',(33.35,-56.1574464964891,-162.691295630997));
#168914=CARTESIAN_POINT('Ctrl Pts',(33.35,-55.982001331389,-162.328090330229));
#168915=CARTESIAN_POINT('Ctrl Pts',(33.35,-55.8312183865757,-161.95418118213));
#168916=CARTESIAN_POINT('Ctrl Pts',(33.35,-55.8149691192272,-161.91388650743));
#168917=CARTESIAN_POINT('Ctrl Pts',(33.35,-55.7990063112411,-161.873467504156));
#168918=CARTESIAN_POINT('Ctrl Pts',(33.35,-55.7833216689026,-161.832927771927));
#168919=CARTESIAN_POINT('Ctrl Pts',(33.35,-55.6220934454647,-161.4162049124));
#168920=CARTESIAN_POINT('Ctrl Pts',(33.35,-55.4903395808871,-160.984647645305));
#168921=CARTESIAN_POINT('Ctrl Pts',(33.35,-55.3869054679322,-160.551047169605));
#168922=CARTESIAN_POINT('Ctrl Pts',(33.35,-55.2731785652169,-160.074298854097));
#168923=CARTESIAN_POINT('Ctrl Pts',(33.35,-55.1917492545591,-159.592825164626));
#168924=CARTESIAN_POINT('Ctrl Pts',(33.35,-55.141467476699,-159.106794321393));
#168925=CARTESIAN_POINT('Ctrl Pts',(33.35,-55.1002871472374,-158.70873937774));
#168926=CARTESIAN_POINT('Ctrl Pts',(33.35,-55.08000002,-158.307627565795));
#168927=CARTESIAN_POINT('Ctrl Pts',(33.35,-55.08000002,-157.903547609535));
#168928=CARTESIAN_POINT('Ctrl Pts',(33.35,-60.9047458754482,-170.861259130871));
#168929=CARTESIAN_POINT('Ctrl Pts',(33.35,-60.6616577186179,-171.000024903864));
#168930=CARTESIAN_POINT('Ctrl Pts',(33.5886122085038,-60.5345771657124,
-171.07256826174));
#168931=CARTESIAN_POINT('Ctrl Pts',(33.35,-59.4103431251365,-168.243382962268));
#168932=CARTESIAN_POINT('Ctrl Pts',(33.3499999999583,-59.1768144406969,
-168.390475993822));
#168933=CARTESIAN_POINT('Ctrl Pts',(33.5831748521597,-59.0440141159766,
-168.454692464379));
#168934=CARTESIAN_POINT('Ctrl Pts',(33.35,-57.8986390322929,-165.635544032027));
#168935=CARTESIAN_POINT('Ctrl Pts',(33.3500000000315,-57.6703808898087,
-165.782543034447));
#168936=CARTESIAN_POINT('Ctrl Pts',(33.5774199132796,-57.5365496870091,
-165.846853703856));
#168937=CARTESIAN_POINT('Ctrl Pts',(33.35,-56.364204511422,-163.040910588762));
#168938=CARTESIAN_POINT('Ctrl Pts',(33.35,-56.1347789227867,-163.176590079091));
#168939=CARTESIAN_POINT('Ctrl Pts',(33.5712930253539,-56.0068938993568,
-163.252219719633));
#168940=CARTESIAN_POINT('',(33.35,-60.9047458754482,-170.861259130871));
#168941=CARTESIAN_POINT('Origin',(33.85,-60.9047458754482,-170.861259130871));
#168942=CARTESIAN_POINT('Ctrl Pts',(33.35,-60.9047458754482,-170.861259130871));
#168943=CARTESIAN_POINT('Ctrl Pts',(33.35,-59.4103419837617,-168.243380962845));
#168944=CARTESIAN_POINT('Ctrl Pts',(33.35,-57.8986402212887,-165.635546042559));
#168945=CARTESIAN_POINT('Ctrl Pts',(33.35,-56.3642045114219,-163.040910588762));
#168946=CARTESIAN_POINT('Ctrl Pts',(33.5750675957151,-60.4869407444486,
-170.953330140827));
#168947=CARTESIAN_POINT('Ctrl Pts',(33.35,-60.6250690696869,-170.899634921035));
#168948=CARTESIAN_POINT('Ctrl Pts',(33.35,-60.8761373158519,-170.801627468756));
#168949=CARTESIAN_POINT('Ctrl Pts',(33.5983572986425,-60.5684969171355,
-171.202165692941));
#168950=CARTESIAN_POINT('Ctrl Pts',(33.3499999999999,-60.6884266834228,
-171.110284935414));
#168951=CARTESIAN_POINT('Ctrl Pts',(33.35,-60.9251533634944,-170.926061957919));
#168952=CARTESIAN_POINT('Ctrl Pts',(33.645886928716,-60.7351980774689,-171.389554331221));
#168953=CARTESIAN_POINT('Ctrl Pts',(33.35,-60.8223319990726,-171.281977972795));
#168954=CARTESIAN_POINT('Ctrl Pts',(33.35,-61.0252654854184,-171.01974252204));
#168955=CARTESIAN_POINT('Ctrl Pts',(33.7566428569643,-61.1261755253357,
-171.621593660576));
#168956=CARTESIAN_POINT('Ctrl Pts',(33.35,-61.1501400117675,-171.544190338249));
#168957=CARTESIAN_POINT('Ctrl Pts',(33.35,-61.2596546585114,-171.135765475889));
#168958=CARTESIAN_POINT('Ctrl Pts',(33.8194265539495,-61.3488867187904,
-171.667078490997));
#168959=CARTESIAN_POINT('Ctrl Pts',(33.35,-61.354614484144,-171.633806784439));
#168960=CARTESIAN_POINT('Ctrl Pts',(33.35,-61.3929914759312,-171.158511634364));
#168961=CARTESIAN_POINT('Ctrl Pts',(33.8808666646521,-61.5682521131594,
-171.644230663833));
#168962=CARTESIAN_POINT('Ctrl Pts',(33.35,-61.5709679425831,-171.67697447423));
#168963=CARTESIAN_POINT('Ctrl Pts',(33.35,-61.5240790589959,-171.147092730284));
#168964=CARTESIAN_POINT('',(33.35,-61.4584329769396,-171.14995));
#168965=CARTESIAN_POINT('Origin',(33.85,-61.4584329769396,-171.14995));
#168966=CARTESIAN_POINT('Ctrl Pts',(33.35,-61.4584329769396,-171.14995));
#168967=CARTESIAN_POINT('Ctrl Pts',(33.35,-61.3933512658348,-171.14995));
#168968=CARTESIAN_POINT('Ctrl Pts',(33.35,-61.3285261814807,-171.141518537402));
#168969=CARTESIAN_POINT('Ctrl Pts',(33.35,-61.2661398376647,-171.12453960829));
#168970=CARTESIAN_POINT('Ctrl Pts',(33.35,-61.2235444953656,-171.112946954302));
#168971=CARTESIAN_POINT('Ctrl Pts',(33.35,-61.1820855819996,-171.097368683161));
#168972=CARTESIAN_POINT('Ctrl Pts',(33.35,-61.1424600695408,-171.077754003862));
#168973=CARTESIAN_POINT('Ctrl Pts',(33.35,-61.1076390364327,-171.06051754798));
#168974=CARTESIAN_POINT('Ctrl Pts',(33.35,-61.0743836755039,-171.040165282673));
#168975=CARTESIAN_POINT('Ctrl Pts',(33.35,-61.0435144499423,-171.016803427715));
#168976=CARTESIAN_POINT('Ctrl Pts',(33.35,-61.0154640589458,-170.995574869044));
#168977=CARTESIAN_POINT('Ctrl Pts',(33.35,-60.989382795281,-170.971860522155));
#168978=CARTESIAN_POINT('Ctrl Pts',(33.35,-60.9659114268316,-170.94570880678));
#168979=CARTESIAN_POINT('Ctrl Pts',(33.35,-60.9427675971707,-170.919922033959));
#168980=CARTESIAN_POINT('Ctrl Pts',(33.35,-60.9221601342061,-170.891765212973));
#168981=CARTESIAN_POINT('Ctrl Pts',(33.35,-60.9047458754482,-170.861259130871));
#168982=CARTESIAN_POINT('Origin',(33.85,-12.9675000200281,-171.14995));
#168983=CARTESIAN_POINT('',(33.35,-63.4074419114814,-171.14995));
#168984=CARTESIAN_POINT('Origin',(33.85,-63.4074419114814,-171.14995));
#168985=CARTESIAN_POINT('',(33.35,-61.8036605881122,-171.14995));
#168986=CARTESIAN_POINT('Ctrl Pts',(33.35,-64.9221832702593,-172.64995));
#168987=CARTESIAN_POINT('Ctrl Pts',(33.3499999999999,-64.4875399013512,
-172.64995));
#168988=CARTESIAN_POINT('Ctrl Pts',(33.7804134495199,-64.4270492358885,
-172.64995));
#168989=CARTESIAN_POINT('Ctrl Pts',(33.35,-64.922183270247,-172.453565067926));
#168990=CARTESIAN_POINT('Ctrl Pts',(33.35,-64.4875399013443,-172.511015867074));
#168991=CARTESIAN_POINT('Ctrl Pts',(33.7804134495211,-64.4270492358883,
-172.51902671195));
#168992=CARTESIAN_POINT('Ctrl Pts',(33.35,-64.8827586015461,-172.257328160063));
#168993=CARTESIAN_POINT('Ctrl Pts',(33.35,-64.4577842162266,-172.371853931892));
#168994=CARTESIAN_POINT('Ctrl Pts',(33.7822246014263,-64.4005115826131,
-172.38820210671));
#168995=CARTESIAN_POINT('Ctrl Pts',(33.35,-64.7310022982632,-171.894521542842));
#168996=CARTESIAN_POINT('Ctrl Pts',(33.35,-64.3449732070946,-172.118296873734));
#168997=CARTESIAN_POINT('Ctrl Pts',(33.7891962191206,-64.2983609167864,
-172.14633102856));
#168998=CARTESIAN_POINT('Ctrl Pts',(33.35,-64.6187303406215,-171.728129909852));
#168999=CARTESIAN_POINT('Ctrl Pts',(33.3500000000013,-64.2614041148292,
-172.003556970023));
#169000=CARTESIAN_POINT('Ctrl Pts',(33.7943539433762,-64.2227880741536,
-172.035403273235));
#169001=CARTESIAN_POINT('Ctrl Pts',(33.35,-64.3383212554124,-171.450449746589));
#169002=CARTESIAN_POINT('Ctrl Pts',(33.3499999999986,-64.0569588954535,
-171.817687494207));
#169003=CARTESIAN_POINT('Ctrl Pts',(33.8072358131761,-64.0340382552807,
-171.850283164391));
#169004=CARTESIAN_POINT('Ctrl Pts',(33.35,-64.1702943967697,-171.339270411997));
#169005=CARTESIAN_POINT('Ctrl Pts',(33.3499999999999,-63.9353951792977,
-171.746711574348));
#169006=CARTESIAN_POINT('Ctrl Pts',(33.8149548930127,-63.9209355035967,
-171.776163607997));
#169007=CARTESIAN_POINT('Ctrl Pts',(33.35,-63.8039222708381,-171.18899099047));
#169008=CARTESIAN_POINT('Ctrl Pts',(33.3499999999999,-63.6769599183967,
-171.658003579003));
#169009=CARTESIAN_POINT('Ctrl Pts',(33.831785867019,-63.6743219805034,-171.675977326981));
#169010=CARTESIAN_POINT('Ctrl Pts',(33.35,-63.6057568308558,-171.149950000016));
#169011=CARTESIAN_POINT('Ctrl Pts',(33.35,-63.5396903402446,-171.640924254979));
#169012=CARTESIAN_POINT('Ctrl Pts',(33.8408895000012,-63.5409322550068,
-171.64995));
#169013=CARTESIAN_POINT('Ctrl Pts',(33.35,-63.4074419114814,-171.14995));
#169014=CARTESIAN_POINT('Ctrl Pts',(33.35,-63.4074419114814,-171.64995));
#169015=CARTESIAN_POINT('Ctrl Pts',(33.85,-63.4074419114814,-171.64995));
#169016=CARTESIAN_POINT('',(33.35,-64.9221832702593,-172.64995));
#169017=CARTESIAN_POINT('Origin',(33.85,-64.9221832702593,-172.64995));
#169018=CARTESIAN_POINT('Ctrl Pts',(33.35,-64.9221832702593,-172.64995));
#169019=CARTESIAN_POINT('Ctrl Pts',(33.35,-64.922183270247,-172.453565067926));
#169020=CARTESIAN_POINT('Ctrl Pts',(33.35,-64.8827586015461,-172.257328160063));
#169021=CARTESIAN_POINT('Ctrl Pts',(33.35,-64.7310022982632,-171.894521542842));
#169022=CARTESIAN_POINT('Ctrl Pts',(33.35,-64.6187303406215,-171.728129909852));
#169023=CARTESIAN_POINT('Ctrl Pts',(33.35,-64.3383212554124,-171.450449746589));
#169024=CARTESIAN_POINT('Ctrl Pts',(33.35,-64.1702943967697,-171.339270411997));
#169025=CARTESIAN_POINT('Ctrl Pts',(33.35,-63.8039222708381,-171.18899099047));
#169026=CARTESIAN_POINT('Ctrl Pts',(33.35,-63.6057568308558,-171.149950000016));
#169027=CARTESIAN_POINT('Ctrl Pts',(33.35,-63.4074419114814,-171.14995));
#169028=CARTESIAN_POINT('Origin',(33.85,-64.9221832702593,-171.64995));
#169029=CARTESIAN_POINT('',(33.7804134495199,-64.4270492358885,-171.64995));
#169030=CARTESIAN_POINT('',(33.35,-64.9221832702593,-55.24995));
#169031=CARTESIAN_POINT('Origin',(32.85,-73.08000002,-176.84995));
#169032=CARTESIAN_POINT('',(33.35,67.7009572055632,-176.84995));
#169033=CARTESIAN_POINT('Origin',(32.85,-70.08000002,-58.24995));
#169034=CARTESIAN_POINT('',(33.35,-70.08000002,-55.74995));
#169035=CARTESIAN_POINT('Origin',(33.35,-70.08000002,-58.24995));
#169036=CARTESIAN_POINT('',(32.85,-70.08000002,-55.24995));
#169037=CARTESIAN_POINT('Origin',(32.85,-70.08000002,-55.74995));
#169038=CARTESIAN_POINT('Origin',(32.85,-70.08000002,-58.24995));
#169039=CARTESIAN_POINT('Origin',(-3.3975957231091E-14,-70.08000002,-58.24995));
#169040=CARTESIAN_POINT('',(32.35,-70.08000002,-55.24995));
#169041=CARTESIAN_POINT('',(41.5,-70.08000002,-55.24995));
#169042=CARTESIAN_POINT('Origin',(32.35,-70.08000002,-58.24995));
#169043=CARTESIAN_POINT('Origin',(32.35,-70.08000002,-58.24995));
#169044=CARTESIAN_POINT('',(31.85,-70.08000002,-55.74995));
#169045=CARTESIAN_POINT('Origin',(32.35,-70.08000002,-55.74995));
#169046=CARTESIAN_POINT('',(31.85,-72.58000002,-58.24995));
#169047=CARTESIAN_POINT('Origin',(31.85,-70.08000002,-58.24995));
#169048=CARTESIAN_POINT('Origin',(32.35,-72.58000002,-58.24995));
#169049=CARTESIAN_POINT('Origin',(32.35,-72.58000002,-55.24995));
#169050=CARTESIAN_POINT('',(31.85,-72.58000002,-174.34995));
#169051=CARTESIAN_POINT('',(31.85,-72.58000002,-58.24995));
#169052=CARTESIAN_POINT('Origin',(32.35,-72.58000002,-174.34995));
#169053=CARTESIAN_POINT('Origin',(32.35,-70.08000002,-174.34995));
#169054=CARTESIAN_POINT('',(31.85,-70.08000002,-176.84995));
#169055=CARTESIAN_POINT('Origin',(31.85,-70.08000002,-174.34995));
#169056=CARTESIAN_POINT('Origin',(32.35,-70.08000002,-176.84995));
#169057=CARTESIAN_POINT('Origin',(32.35,67.7009572055632,-176.84995));
#169058=CARTESIAN_POINT('',(31.85,67.7009572055632,-176.84995));
#169059=CARTESIAN_POINT('Origin',(31.35,-65.2735353570153,-171.64995));
#169060=CARTESIAN_POINT('',(31.85,-65.2735353570153,-172.64995));
#169061=CARTESIAN_POINT('',(31.85,-65.2735353570153,-55.24995));
#169062=CARTESIAN_POINT('Origin',(31.35,-65.2735353570153,-172.64995));
#169063=CARTESIAN_POINT('',(31.28041344952,-64.7784013226445,-171.64995));
#169064=CARTESIAN_POINT('Ctrl Pts',(31.85,-63.7585925544192,-171.149950013428));
#169065=CARTESIAN_POINT('Ctrl Pts',(31.8499999999999,-63.7586583477387,
-171.65003477338));
#169066=CARTESIAN_POINT('Ctrl Pts',(31.3499152383757,-63.7586584017713,
-171.649950001854));
#169067=CARTESIAN_POINT('Ctrl Pts',(31.85,-63.9569747212759,-171.149923566191));
#169068=CARTESIAN_POINT('Ctrl Pts',(31.85,-63.8934770903365,-171.659221103016));
#169069=CARTESIAN_POINT('Ctrl Pts',(31.3408008078195,-63.8921937709272,
-171.649930655763));
#169070=CARTESIAN_POINT('Ctrl Pts',(31.85,-64.1552123321859,-171.188965548735));
#169071=CARTESIAN_POINT('Ctrl Pts',(31.85,-64.0229027076712,-171.695281914067));
#169072=CARTESIAN_POINT('Ctrl Pts',(31.3316930631424,-64.0256328180304,
-171.675956808334));
#169073=CARTESIAN_POINT('Ctrl Pts',(31.85,-64.521646483527,-171.339270411997));
#169074=CARTESIAN_POINT('Ctrl Pts',(31.85,-64.2556937071631,-171.81002165518));
#169075=CARTESIAN_POINT('Ctrl Pts',(31.3148578735171,-64.2722905946127,
-171.776157476854));
#169076=CARTESIAN_POINT('Ctrl Pts',(31.85,-64.6896733421684,-171.450449746589));
#169077=CARTESIAN_POINT('Ctrl Pts',(31.850000000002,-64.3582551123188,-171.889069508912));
#169078=CARTESIAN_POINT('Ctrl Pts',(31.3071382160674,-64.3853952154975,
-171.850276197781));
#169079=CARTESIAN_POINT('Ctrl Pts',(31.85,-64.9700824273775,-171.728129909852));
#169080=CARTESIAN_POINT('Ctrl Pts',(31.8499999999979,-64.5258884542433,
-172.075284894373));
#169081=CARTESIAN_POINT('Ctrl Pts',(31.294255447738,-64.5741487063124,-172.035396209826));
#169082=CARTESIAN_POINT('Ctrl Pts',(31.85,-65.0823543850191,-171.894521542842));
#169083=CARTESIAN_POINT('Ctrl Pts',(31.85,-64.5901493684385,-172.182240159754));
#169084=CARTESIAN_POINT('Ctrl Pts',(31.289097389763,-64.6497234916245,-172.14632470545));
#169085=CARTESIAN_POINT('Ctrl Pts',(31.85,-65.2341363800668,-172.257389581842));
#169086=CARTESIAN_POINT('Ctrl Pts',(31.8499999999999,-64.6765834404086,
-172.409795949396));
#169087=CARTESIAN_POINT('Ctrl Pts',(31.2821241606569,-64.7518941169831,
-172.388239289312));
#169088=CARTESIAN_POINT('Ctrl Pts',(31.85,-65.2735620506093,-172.453697958274));
#169089=CARTESIAN_POINT('Ctrl Pts',(31.85,-64.6982492704848,-172.529747068593));
#169090=CARTESIAN_POINT('Ctrl Pts',(31.2803128569907,-64.7784332664479,
-172.519113452117));
#169091=CARTESIAN_POINT('Ctrl Pts',(31.85,-65.2735353434557,-172.650149483381));
#169092=CARTESIAN_POINT('Ctrl Pts',(31.8499999999999,-64.6982345639698,
-172.650072180543));
#169093=CARTESIAN_POINT('Ctrl Pts',(31.2803140827874,-64.7784152888562,
-172.650082990805));
#169094=CARTESIAN_POINT('',(31.85,-63.7587939982373,-171.14995));
#169095=CARTESIAN_POINT('Ctrl Pts',(31.85,-63.7587939982373,-171.14995));
#169096=CARTESIAN_POINT('Ctrl Pts',(31.85,-63.9571089176128,-171.149950000016));
#169097=CARTESIAN_POINT('Ctrl Pts',(31.85,-64.1552743575927,-171.18899099047));
#169098=CARTESIAN_POINT('Ctrl Pts',(31.85,-64.521646483527,-171.339270411997));
#169099=CARTESIAN_POINT('Ctrl Pts',(31.85,-64.6896733421684,-171.450449746589));
#169100=CARTESIAN_POINT('Ctrl Pts',(31.85,-64.9700824273775,-171.728129909852));
#169101=CARTESIAN_POINT('Ctrl Pts',(31.85,-65.0823543850191,-171.894521542842));
#169102=CARTESIAN_POINT('Ctrl Pts',(31.85,-65.2341106883021,-172.257328160063));
#169103=CARTESIAN_POINT('Ctrl Pts',(31.85,-65.273535357003,-172.453565067926));
#169104=CARTESIAN_POINT('Ctrl Pts',(31.85,-65.2735353570153,-172.64995));
#169105=CARTESIAN_POINT('Origin',(31.35,-63.7587939982373,-171.14995));
#169106=CARTESIAN_POINT('Origin',(31.35,-12.9675000200281,-171.14995));
#169107=CARTESIAN_POINT('',(31.85,-63.1109998882233,-171.14995));
#169108=CARTESIAN_POINT('',(31.85,-63.6885235808861,-171.14995));
#169109=CARTESIAN_POINT('Origin',(31.35,-63.1109998882233,-171.14995));
#169110=CARTESIAN_POINT('Ctrl Pts',(31.3495340997183,-63.1109998882233,
-171.649949782937));
#169111=CARTESIAN_POINT('Ctrl Pts',(31.8499999999999,-63.1109998882232,
-171.650416117547));
#169112=CARTESIAN_POINT('Ctrl Pts',(31.85,-63.1109998882233,-171.14995));
#169113=CARTESIAN_POINT('Ctrl Pts',(31.3254339042549,-63.0188799316811,
-171.649927325175));
#169114=CARTESIAN_POINT('Ctrl Pts',(31.8499999999969,-63.0165598996745,
-171.675136694187));
#169115=CARTESIAN_POINT('Ctrl Pts',(31.85,-63.0574084096236,-171.149949978884));
#169116=CARTESIAN_POINT('Ctrl Pts',(31.301798787247,-62.9287579316647,-171.63773683985));
#169117=CARTESIAN_POINT('Ctrl Pts',(31.8500000000009,-62.9205269518794,
-171.689702894937));
#169118=CARTESIAN_POINT('Ctrl Pts',(31.85,-63.0049471542817,-171.14386632127));
#169119=CARTESIAN_POINT('Ctrl Pts',(31.2554698848903,-62.7525001587558,
-171.589540674115));
#169120=CARTESIAN_POINT('Ctrl Pts',(31.8499999999991,-62.7176222625568,
-171.698243814111));
#169121=CARTESIAN_POINT('Ctrl Pts',(31.85,-62.9022833467989,-171.11979081221));
#169122=CARTESIAN_POINT('Ctrl Pts',(31.2324358840903,-62.6650789422019,
-171.552638259287));
#169123=CARTESIAN_POINT('Ctrl Pts',(31.8499999999999,-62.6082192965497,
-171.690638470313));
#169124=CARTESIAN_POINT('Ctrl Pts',(31.85,-62.8513307506207,-171.101350238814));
#169125=CARTESIAN_POINT('Ctrl Pts',(31.1898390398577,-62.5037420018705,
-171.455718071437));
#169126=CARTESIAN_POINT('Ctrl Pts',(31.85,-62.384922264433,-171.644778100208));
#169127=CARTESIAN_POINT('Ctrl Pts',(31.85,-62.7572432252394,-171.052906534958));
#169128=CARTESIAN_POINT('Ctrl Pts',(31.1701167672829,-62.4292143353616,
-171.396060292184));
#169129=CARTESIAN_POINT('Ctrl Pts',(31.8499999999993,-62.2702741424481,
-171.605345720721));
#169130=CARTESIAN_POINT('Ctrl Pts',(31.85,-62.7137529944933,-171.02308307076));
#169131=CARTESIAN_POINT('Ctrl Pts',(31.1344584332459,-62.2946837716206,
-171.25015961779));
#169132=CARTESIAN_POINT('Ctrl Pts',(31.8500000000008,-62.0379421582966,
-171.477274777814));
#169133=CARTESIAN_POINT('Ctrl Pts',(31.85,-62.6352107798375,-170.950134506763));
#169134=CARTESIAN_POINT('Ctrl Pts',(31.1192027095743,-62.2372474415666,
-171.166311520395));
#169135=CARTESIAN_POINT('Ctrl Pts',(31.8499999999999,-61.9259673058959,
-171.38837548536));
#169136=CARTESIAN_POINT('Ctrl Pts',(31.85,-62.6016585634489,-170.908207754234));
#169137=CARTESIAN_POINT('Ctrl Pts',(31.1074206615884,-62.1929294743655,
-171.072435409621));
#169138=CARTESIAN_POINT('Ctrl Pts',(31.85,-61.8321698700148,-171.271436537469));
#169139=CARTESIAN_POINT('Ctrl Pts',(31.85,-62.5757608260974,-170.861259130871));
#169140=CARTESIAN_POINT('',(31.85,-62.5757608260974,-170.861259130871));
#169141=CARTESIAN_POINT('Ctrl Pts',(31.85,-62.5757608260974,-170.861259130871));
#169142=CARTESIAN_POINT('Ctrl Pts',(31.85,-62.5934214847794,-170.893275292324));
#169143=CARTESIAN_POINT('Ctrl Pts',(31.85,-62.6145900881585,-170.922872024471));
#169144=CARTESIAN_POINT('Ctrl Pts',(31.85,-62.6386464997605,-170.949982960699));
#169145=CARTESIAN_POINT('Ctrl Pts',(31.85,-62.6499713199274,-170.962745731906));
#169146=CARTESIAN_POINT('Ctrl Pts',(31.85,-62.6619368642692,-170.974957283073));
#169147=CARTESIAN_POINT('Ctrl Pts',(31.85,-62.6744818503514,-170.986608828398));
#169148=CARTESIAN_POINT('Ctrl Pts',(31.85,-62.7038852881232,-171.013918184158));
#169149=CARTESIAN_POINT('Ctrl Pts',(31.85,-62.7356294724137,-171.037482725823));
#169150=CARTESIAN_POINT('Ctrl Pts',(31.85,-62.7694892975018,-171.057780531265));
#169151=CARTESIAN_POINT('Ctrl Pts',(31.85,-62.780852617915,-171.064592452659));
#169152=CARTESIAN_POINT('Ctrl Pts',(31.85,-62.7924544589394,-171.071036069574));
#169153=CARTESIAN_POINT('Ctrl Pts',(31.85,-62.8042869861286,-171.077128390385));
#169154=CARTESIAN_POINT('Ctrl Pts',(31.85,-62.8513324723594,-171.10135112744));
#169155=CARTESIAN_POINT('Ctrl Pts',(31.85,-62.9022833426441,-171.119790824143));
#169156=CARTESIAN_POINT('Ctrl Pts',(31.85,-62.9536152465698,-171.131828583671));
#169157=CARTESIAN_POINT('Ctrl Pts',(31.85,-63.0049433927144,-171.143865461968));
#169158=CARTESIAN_POINT('Ctrl Pts',(31.85,-63.0574025248319,-171.14995));
#169159=CARTESIAN_POINT('Ctrl Pts',(31.85,-63.1109998882233,-171.14995));
#169160=CARTESIAN_POINT('Origin',(31.35,-62.5757608260974,-170.861259130871));
#169161=CARTESIAN_POINT('Ctrl Pts',(31.85,-56.2763252281792,-159.66866755714));
#169162=CARTESIAN_POINT('Ctrl Pts',(31.8499999999999,-55.4929314270088,
-160.119633364362));
#169163=CARTESIAN_POINT('Ctrl Pts',(31.0842850915597,-55.9092502513102,
-159.879976688011));
#169164=CARTESIAN_POINT('Ctrl Pts',(31.85,-58.4122993941661,-163.37916820794));
#169165=CARTESIAN_POINT('Ctrl Pts',(31.8500000000875,-57.6056192097127,
-163.747040286917));
#169166=CARTESIAN_POINT('Ctrl Pts',(31.0928842088245,-58.0390008802754,
-163.590479273921));
#169167=CARTESIAN_POINT('Ctrl Pts',(31.85,-60.5078533703316,-167.112448841938));
#169168=CARTESIAN_POINT('Ctrl Pts',(31.8499999999999,-59.7238064590067,
-167.480553670321));
#169169=CARTESIAN_POINT('Ctrl Pts',(31.1007058108654,-60.129339000976,-167.323759171684));
#169170=CARTESIAN_POINT('Ctrl Pts',(31.85,-62.5757608260975,-170.861259130871));
#169171=CARTESIAN_POINT('Ctrl Pts',(31.8499999999999,-61.8331341426276,
-171.27090462831));
#169172=CARTESIAN_POINT('Ctrl Pts',(31.1079170675507,-62.1926886331265,
-171.07256826174));
#169173=CARTESIAN_POINT('',(31.85,-56.2763252281792,-159.66866755714));
#169174=CARTESIAN_POINT('Ctrl Pts',(31.85,-56.2763252281792,-159.66866755714));
#169175=CARTESIAN_POINT('Ctrl Pts',(31.85,-58.4123038607033,-163.37917596697));
#169176=CARTESIAN_POINT('Ctrl Pts',(31.85,-60.5078491316876,-167.112441157955));
#169177=CARTESIAN_POINT('Ctrl Pts',(31.85,-62.5757608260974,-170.861259130871));
#169178=CARTESIAN_POINT('Origin',(31.35,-56.2763252281792,-159.66866755714));
#169179=CARTESIAN_POINT('Ctrl Pts',(31.0842850915597,-55.9092502513102,
-159.879976688011));
#169180=CARTESIAN_POINT('Ctrl Pts',(31.85,-55.4929314270087,-160.119633364362));
#169181=CARTESIAN_POINT('Ctrl Pts',(31.85,-56.2763252281792,-159.66866755714));
#169182=CARTESIAN_POINT('Ctrl Pts',(31.1045100388203,-55.6745659332473,
-159.497727845842));
#169183=CARTESIAN_POINT('Ctrl Pts',(31.8499999999999,-55.3073385167954,
-159.699359913876));
#169184=CARTESIAN_POINT('Ctrl Pts',(31.85,-56.0651024669579,-159.301742606223));
#169185=CARTESIAN_POINT('Ctrl Pts',(31.1254451190221,-55.4786764778281,
-159.101707988136));
#169186=CARTESIAN_POINT('Ctrl Pts',(31.85,-55.150888528242,-159.261095570535));
#169187=CARTESIAN_POINT('Ctrl Pts',(31.85,-55.8888088329065,-158.921766047559));
#169188=CARTESIAN_POINT('Ctrl Pts',(31.1683825098781,-55.1470153257944,
-158.288497370345));
#169189=CARTESIAN_POINT('Ctrl Pts',(31.8499999999999,-54.9001304967853,
-158.384215791274));
#169190=CARTESIAN_POINT('Ctrl Pts',(31.85,-55.5903137943537,-158.141820520556));
#169191=CARTESIAN_POINT('Ctrl Pts',(31.1903926108665,-55.0114922210667,
-157.871160476353));
#169192=CARTESIAN_POINT('Ctrl Pts',(31.8499999999999,-54.8012512449405,
-157.943770771097));
#169193=CARTESIAN_POINT('Ctrl Pts',(31.85,-55.4683430012288,-157.741722853926));
#169194=CARTESIAN_POINT('Ctrl Pts',(31.235360609423,-54.7945396526329,-157.017225985171));
#169195=CARTESIAN_POINT('Ctrl Pts',(31.8499999999999,-54.6558194805957,
-157.05645039125));
#169196=CARTESIAN_POINT('Ctrl Pts',(31.85,-55.2730856891008,-156.923456306516));
#169197=CARTESIAN_POINT('Ctrl Pts',(31.2582224016427,-54.7139233464081,
-156.582445743712));
#169198=CARTESIAN_POINT('Ctrl Pts',(31.8500000000015,-54.6065272690148,
-156.610041402948));
#169199=CARTESIAN_POINT('Ctrl Pts',(31.85,-55.2005310139637,-156.507030856831));
#169200=CARTESIAN_POINT('Ctrl Pts',(31.3039546551071,-54.6068982720801,
-155.711146263543));
#169201=CARTESIAN_POINT('Ctrl Pts',(31.8499999999985,-54.5582899067328,
-155.725181694391));
#169202=CARTESIAN_POINT('Ctrl Pts',(31.85,-55.1042084466757,-155.672936697905));
#169203=CARTESIAN_POINT('Ctrl Pts',(31.3269276470654,-54.58000002,-155.272681199498));
#169204=CARTESIAN_POINT('Ctrl Pts',(31.85,-54.5563817475358,-155.28312293345));
#169205=CARTESIAN_POINT('Ctrl Pts',(31.85,-55.0800000206076,-155.253403124156));
#169206=CARTESIAN_POINT('Ctrl Pts',(31.35,-54.58000002,-154.831379798159));
#169207=CARTESIAN_POINT('Ctrl Pts',(31.8499999999999,-54.58000002,-154.831379798158));
#169208=CARTESIAN_POINT('Ctrl Pts',(31.85,-55.08000002,-154.831379798159));
#169209=CARTESIAN_POINT('',(31.85,-55.08000002,-154.831379798159));
#169210=CARTESIAN_POINT('Ctrl Pts',(31.85,-55.08000002,-154.831379798159));
#169211=CARTESIAN_POINT('Ctrl Pts',(31.85,-55.08000002,-155.253410854053));
#169212=CARTESIAN_POINT('Ctrl Pts',(31.85,-55.1042084466772,-155.6729366979));
#169213=CARTESIAN_POINT('Ctrl Pts',(31.85,-55.1523697302198,-156.089983777379));
#169214=CARTESIAN_POINT('Ctrl Pts',(31.85,-55.2005310137623,-156.507030856859));
#169215=CARTESIAN_POINT('Ctrl Pts',(31.85,-55.2730856890926,-156.92345630647));
#169216=CARTESIAN_POINT('Ctrl Pts',(31.85,-55.3707143450195,-157.332589580255));
#169217=CARTESIAN_POINT('Ctrl Pts',(31.85,-55.4683430009464,-157.74172285404));
#169218=CARTESIAN_POINT('Ctrl Pts',(31.85,-55.5903137943579,-158.141820520543));
#169219=CARTESIAN_POINT('Ctrl Pts',(31.85,-55.7395613131142,-158.531793284255));
#169220=CARTESIAN_POINT('Ctrl Pts',(31.85,-55.8729496111504,-158.880327073396));
#169221=CARTESIAN_POINT('Ctrl Pts',(31.85,-56.0279262450874,-159.220847441937));
#169222=CARTESIAN_POINT('Ctrl Pts',(31.85,-56.2101595914815,-159.551250340852));
#169223=CARTESIAN_POINT('Ctrl Pts',(31.85,-56.2318262511927,-159.590533640643));
#169224=CARTESIAN_POINT('Ctrl Pts',(31.85,-56.2538782710457,-159.629673897772));
#169225=CARTESIAN_POINT('Ctrl Pts',(31.85,-56.2763252281792,-159.66866755714));
#169226=CARTESIAN_POINT('Origin',(31.35,-55.08000002,-154.831379798159));
#169227=CARTESIAN_POINT('Origin',(31.35,-55.08000002,-55.24995));
#169228=CARTESIAN_POINT('',(31.85,-55.08000002,-77.227263173365));
#169229=CARTESIAN_POINT('',(31.85,-55.08000002,-155.433057559267));
#169230=CARTESIAN_POINT('Origin',(31.35,-55.08000002,-77.2272631733642));
#169231=CARTESIAN_POINT('Ctrl Pts',(31.3500000000009,-54.58000002,-77.2272631733658));
#169232=CARTESIAN_POINT('Ctrl Pts',(31.85,-54.5800000200009,-77.2272631733658));
#169233=CARTESIAN_POINT('Ctrl Pts',(31.85,-55.08000002,-77.227263173365));
#169234=CARTESIAN_POINT('Ctrl Pts',(31.3038531467957,-54.5800000199985,
-76.3446192991014));
#169235=CARTESIAN_POINT('Ctrl Pts',(31.85,-54.5315963664815,-76.3014537863538));
#169236=CARTESIAN_POINT('Ctrl Pts',(31.85,-55.0800000215433,-76.3831770294161));
#169237=CARTESIAN_POINT('Ctrl Pts',(31.258313471615,-54.6849196157793,-75.4773117729577));
#169238=CARTESIAN_POINT('Ctrl Pts',(31.85,-54.5888070575115,-75.4165208091089));
#169239=CARTESIAN_POINT('Ctrl Pts',(31.85,-55.1744276549191,-75.5528673220433));
#169240=CARTESIAN_POINT('Ctrl Pts',(31.1911093410829,-55.0074869144856,
-74.2010813719198));
#169241=CARTESIAN_POINT('Ctrl Pts',(31.85,-54.7984161464127,-74.129239130374));
#169242=CARTESIAN_POINT('Ctrl Pts',(31.85,-55.4647382256782,-74.3299545388963));
#169243=CARTESIAN_POINT('Ctrl Pts',(31.1687759778426,-55.1442253086702,
-73.7776011027959));
#169244=CARTESIAN_POINT('Ctrl Pts',(31.85,-54.8981200391591,-73.6821630179211));
#169245=CARTESIAN_POINT('Ctrl Pts',(31.85,-55.5878027790484,-73.9239717796963));
#169246=CARTESIAN_POINT('Ctrl Pts',(31.1255062785665,-55.4779574226737,
-72.9580899132975));
#169247=CARTESIAN_POINT('Ctrl Pts',(31.85,-55.1503671712329,-72.798619733739));
#169248=CARTESIAN_POINT('Ctrl Pts',(31.85,-55.8881616831611,-73.1379857970122));
#169249=CARTESIAN_POINT('Ctrl Pts',(31.1044941422599,-55.6747504070549,
-72.5606146570313));
#169250=CARTESIAN_POINT('Ctrl Pts',(31.8500000000028,-55.3074747056296,
-72.358974665281));
#169251=CARTESIAN_POINT('Ctrl Pts',(31.85,-56.0652689851553,-72.7566110978467));
#169252=CARTESIAN_POINT('Ctrl Pts',(31.0842850915597,-55.9092502513102,
-72.178666283495));
#169253=CARTESIAN_POINT('Ctrl Pts',(31.85,-55.4929314270087,-71.9390096071439));
#169254=CARTESIAN_POINT('Ctrl Pts',(31.85,-56.2763252281792,-72.3899754143654));
#169255=CARTESIAN_POINT('',(31.85,-56.2763252281792,-72.3899754143654));
#169256=CARTESIAN_POINT('Ctrl Pts',(31.85,-56.2763252281792,-72.3899754143654));
#169257=CARTESIAN_POINT('Ctrl Pts',(31.85,-56.0652560607924,-72.7566335394409));
#169258=CARTESIAN_POINT('Ctrl Pts',(31.85,-55.8881616822718,-73.1379857966025));
#169259=CARTESIAN_POINT('Ctrl Pts',(31.85,-55.737982230652,-73.5309787881812));
#169260=CARTESIAN_POINT('Ctrl Pts',(31.85,-55.5878027790321,-73.9239717797599));
#169261=CARTESIAN_POINT('Ctrl Pts',(31.85,-55.4647382249676,-74.3299545387688));
#169262=CARTESIAN_POINT('Ctrl Pts',(31.85,-55.367968034963,-74.7375921331689));
#169263=CARTESIAN_POINT('Ctrl Pts',(31.85,-55.2585018339704,-75.1987107776467));
#169264=CARTESIAN_POINT('Ctrl Pts',(31.85,-55.1807511519299,-75.664581041178));
#169265=CARTESIAN_POINT('Ctrl Pts',(31.85,-55.1338484059999,-76.1350729813846));
#169266=CARTESIAN_POINT('Ctrl Pts',(31.85,-55.0978253247024,-76.4964285710373));
#169267=CARTESIAN_POINT('Ctrl Pts',(31.85,-55.0800000199994,-76.8605105831137));
#169268=CARTESIAN_POINT('Ctrl Pts',(31.85,-55.08000002,-77.227263173365));
#169269=CARTESIAN_POINT('Origin',(31.35,-56.2763252281792,-72.3899754143654));
#169270=CARTESIAN_POINT('Ctrl Pts',(31.85,-62.4426282692182,-61.4386408691297));
#169271=CARTESIAN_POINT('Ctrl Pts',(31.85,-61.6992317916068,-61.0282555233051));
#169272=CARTESIAN_POINT('Ctrl Pts',(31.1074520910898,-62.0598503138784,
-61.2273317382593));
#169273=CARTESIAN_POINT('Ctrl Pts',(31.85,-60.4178950612392,-65.1063632921145));
#169274=CARTESIAN_POINT('Ctrl Pts',(31.8500000000147,-59.6343590655212,
-64.7356884621635));
#169275=CARTESIAN_POINT('Ctrl Pts',(31.1003696873064,-60.0396054978548,
-64.8950530477878));
#169276=CARTESIAN_POINT('Ctrl Pts',(31.85,-58.3664713365843,-68.7590848262753));
#169277=CARTESIAN_POINT('Ctrl Pts',(31.85,-57.56108933629,-68.3880588333245));
#169278=CARTESIAN_POINT('Ctrl Pts',(31.0926997115701,-57.9933062860146,
-68.5477739147732));
#169279=CARTESIAN_POINT('Ctrl Pts',(31.85,-56.2763252281792,-72.3899754143654));
#169280=CARTESIAN_POINT('Ctrl Pts',(31.85,-55.4929314270087,-71.9390096071439));
#169281=CARTESIAN_POINT('Ctrl Pts',(31.0842850915597,-55.9092502513102,
-72.178666283495));
#169282=CARTESIAN_POINT('',(31.85,-62.4426282692182,-61.4386408691297));
#169283=CARTESIAN_POINT('Ctrl Pts',(31.85,-62.4426282692182,-61.4386408691297));
#169284=CARTESIAN_POINT('Ctrl Pts',(31.85,-60.41789121461,-65.1063702600533));
#169285=CARTESIAN_POINT('Ctrl Pts',(31.85,-58.3664753860174,-68.7590777918155));
#169286=CARTESIAN_POINT('Ctrl Pts',(31.85,-56.2763252281792,-72.3899754143654));
#169287=CARTESIAN_POINT('',(31.1074520910898,-62.0598503138784,-61.2273317382593));
#169288=CARTESIAN_POINT('Origin',(31.35,-62.4426282692182,-61.4386408691297));
#169289=CARTESIAN_POINT('Ctrl Pts',(31.0842850915597,-55.9092502513102,
-72.178666283495));
#169290=CARTESIAN_POINT('Ctrl Pts',(31.0866188993887,-56.4872664046269,
-71.1716326888473));
#169291=CARTESIAN_POINT('Ctrl Pts',(31.0889358110602,-57.0723871813429,
-70.1454736819142));
#169292=CARTESIAN_POINT('Ctrl Pts',(31.0912335136878,-57.6645912286248,
-69.1001560516859));
#169293=CARTESIAN_POINT('Ctrl Pts',(31.0934878913511,-58.2456288094846,
-68.0745486957657));
#169294=CARTESIAN_POINT('Ctrl Pts',(31.0957237752392,-58.8334849007926,
-67.0304983146088));
#169295=CARTESIAN_POINT('Ctrl Pts',(31.0979394902314,-59.428182062844,-65.9679985255963));
#169296=CARTESIAN_POINT('Ctrl Pts',(31.1000978632644,-60.007488662236,-64.9329958739871));
#169297=CARTESIAN_POINT('Ctrl Pts',(31.1022370964783,-60.5932867432086,
-63.8804863393331));
#169298=CARTESIAN_POINT('Ctrl Pts',(31.1043561549919,-61.1856397486797,
-62.8104889207958));
#169299=CARTESIAN_POINT('Ctrl Pts',(31.1053929798596,-61.4754695587821,
-62.2869545658413));
#169300=CARTESIAN_POINT('Ctrl Pts',(31.1064249829176,-61.7668692831667,
-61.7592339914446));
#169301=CARTESIAN_POINT('Ctrl Pts',(31.1074520910898,-62.0598503138784,
-61.2273317382593));
#169302=CARTESIAN_POINT('Origin',(31.35,67.7009572055632,-61.14995));
#169303=CARTESIAN_POINT('',(31.35,-62.9782728042642,-60.64995));
#169304=CARTESIAN_POINT('',(31.85,-62.9782728042642,-61.14995));
#169305=CARTESIAN_POINT('Origin',(31.35,-62.9782728042642,-61.14995));
#169306=CARTESIAN_POINT('',(31.85,-64.3526414204797,-61.14995));
#169307=CARTESIAN_POINT('',(31.85,67.7009572055632,-61.14995));
#169308=CARTESIAN_POINT('',(31.35,-64.3526414204797,-60.64995));
#169309=CARTESIAN_POINT('Origin',(31.35,-64.3526414204797,-61.14995));
#169310=CARTESIAN_POINT('',(31.35,-12.9675000200281,-60.64995));
#169311=CARTESIAN_POINT('Ctrl Pts',(31.1074520910898,-62.0598503138784,
-61.2273317382593));
#169312=CARTESIAN_POINT('Ctrl Pts',(31.8499999999999,-61.6992317916067,
-61.028255523305));
#169313=CARTESIAN_POINT('Ctrl Pts',(31.85,-62.4426282692183,-61.4386408691297));
#169314=CARTESIAN_POINT('Ctrl Pts',(31.1192593280084,-62.1041984096607,
-61.1334442002736));
#169315=CARTESIAN_POINT('Ctrl Pts',(31.8500000000001,-61.7930681218295,
-60.9114185604269));
#169316=CARTESIAN_POINT('Ctrl Pts',(31.85,-62.4685470764636,-61.3916901534439));
#169317=CARTESIAN_POINT('Ctrl Pts',(31.1342845229578,-62.1606836378221,
-61.0509981549565));
#169318=CARTESIAN_POINT('Ctrl Pts',(31.8499999999998,-61.9033127772783,
-60.8239692453656));
#169319=CARTESIAN_POINT('Ctrl Pts',(31.85,-62.5015432853809,-61.3504740791978));
#169320=CARTESIAN_POINT('Ctrl Pts',(31.1697097530512,-62.2941363459118,
-60.9056817830676));
#169321=CARTESIAN_POINT('Ctrl Pts',(31.8500000000002,-62.1341758421231,
-60.6961222616711));
#169322=CARTESIAN_POINT('Ctrl Pts',(31.85,-62.5794711033445,-61.2778158898142));
#169323=CARTESIAN_POINT('Ctrl Pts',(31.1896892584046,-62.369523292851,-60.8449704353912));
#169324=CARTESIAN_POINT('Ctrl Pts',(31.8500000000001,-62.2503354665,-60.6558084251244));
#169325=CARTESIAN_POINT('Ctrl Pts',(31.85,-62.6234753527752,-61.2474602210686));
#169326=CARTESIAN_POINT('Ctrl Pts',(31.2539016024624,-62.6123775685824,
-60.6987791235328));
#169327=CARTESIAN_POINT('Ctrl Pts',(31.8499999999996,-62.5772240699999,
-60.5884818802849));
#169328=CARTESIAN_POINT('Ctrl Pts',(31.85,-62.765153261125,-61.1743645550205));
#169329=CARTESIAN_POINT('Ctrl Pts',(31.3019361194217,-62.7947963971694,
-60.64995));
#169330=CARTESIAN_POINT('Ctrl Pts',(31.85,-62.7861985042763,-60.599633723582));
#169331=CARTESIAN_POINT('Ctrl Pts',(31.85,-62.8714721065165,-61.1499500118284));
#169332=CARTESIAN_POINT('Ctrl Pts',(31.35,-62.9782728042642,-60.64995));
#169333=CARTESIAN_POINT('Ctrl Pts',(31.8499999999999,-62.9782728042642,
-60.64995));
#169334=CARTESIAN_POINT('Ctrl Pts',(31.85,-62.9782728042642,-61.14995));
#169335=CARTESIAN_POINT('Ctrl Pts',(31.85,-62.9782728042642,-61.14995));
#169336=CARTESIAN_POINT('Ctrl Pts',(31.85,-62.9222361461989,-61.14995));
#169337=CARTESIAN_POINT('Ctrl Pts',(31.85,-62.8664016141293,-61.1566668506652));
#169338=CARTESIAN_POINT('Ctrl Pts',(31.85,-62.8123519766769,-61.1700628877857));
#169339=CARTESIAN_POINT('Ctrl Pts',(31.85,-62.7632675286839,-61.1822283179041));
#169340=CARTESIAN_POINT('Ctrl Pts',(31.85,-62.7156536890988,-61.1999027909616));
#169341=CARTESIAN_POINT('Ctrl Pts',(31.85,-62.6707013203275,-61.2230949953743));
#169342=CARTESIAN_POINT('Ctrl Pts',(31.85,-62.6234720220053,-61.2474619324435));
#169343=CARTESIAN_POINT('Ctrl Pts',(31.85,-62.5794710795978,-61.2778158553603));
#169344=CARTESIAN_POINT('Ctrl Pts',(31.85,-62.5405071542091,-61.3141449414402));
#169345=CARTESIAN_POINT('Ctrl Pts',(31.85,-62.5015487187516,-61.350468908832));
#169346=CARTESIAN_POINT('Ctrl Pts',(31.85,-62.4685524875291,-61.3916801947947));
#169347=CARTESIAN_POINT('Ctrl Pts',(31.85,-62.4426282692182,-61.4386408691297));
#169348=CARTESIAN_POINT('Ctrl Pts',(31.1074520910898,-62.0598503138784,
-61.2273317382593));
#169349=CARTESIAN_POINT('Ctrl Pts',(31.1108987502867,-62.072795958949,-61.1999250308078));
#169350=CARTESIAN_POINT('Ctrl Pts',(31.1147345475847,-62.0872074931539,
-61.1725886690502));
#169351=CARTESIAN_POINT('Ctrl Pts',(31.1189833805676,-62.1031783133733,
-61.1455576859644));
#169352=CARTESIAN_POINT('Ctrl Pts',(31.1208390286195,-62.1101534572652,
-61.1337520933918));
#169353=CARTESIAN_POINT('Ctrl Pts',(31.1227733311916,-62.1174255501541,
-61.1220043179659));
#169354=CARTESIAN_POINT('Ctrl Pts',(31.1247876568115,-62.1250000854343,
-61.1103318592589));
#169355=CARTESIAN_POINT('Ctrl Pts',(31.1287109590604,-62.1397530086992,
-61.0875974100488));
#169356=CARTESIAN_POINT('Ctrl Pts',(31.1329376519543,-62.1556525802205,
-61.0651534254741));
#169357=CARTESIAN_POINT('Ctrl Pts',(31.1374716858149,-62.1727165590761,
-61.0431207160486));
#169358=CARTESIAN_POINT('Ctrl Pts',(31.1403005099853,-62.1833629276993,
-61.0293743121004));
#169359=CARTESIAN_POINT('Ctrl Pts',(31.1432488445812,-62.1944620910562,
-61.0157875755612));
#169360=CARTESIAN_POINT('Ctrl Pts',(31.146316387066,-62.2060136847393,-61.0023855422076));
#169361=CARTESIAN_POINT('Ctrl Pts',(31.1481654956904,-62.2129769628714,
-60.9943068226528));
#169362=CARTESIAN_POINT('Ctrl Pts',(31.1500582276936,-62.2201057956471,
-60.986293492844));
#169363=CARTESIAN_POINT('Ctrl Pts',(31.1519971380045,-62.227409991867,-60.9783399690121));
#169364=CARTESIAN_POINT('Ctrl Pts',(31.1557249806558,-62.2414533924559,
-60.9630481397807));
#169365=CARTESIAN_POINT('Ctrl Pts',(31.1596037700658,-62.2560707690401,
-60.9480773991703));
#169366=CARTESIAN_POINT('Ctrl Pts',(31.1636402857178,-62.2712889198747,
-60.9334493797663));
#169367=CARTESIAN_POINT('Ctrl Pts',(31.166544145986,-62.2822368233077,-60.9229260155553));
#169368=CARTESIAN_POINT('Ctrl Pts',(31.1695296424351,-62.2934956800733,
-60.9125801941714));
#169369=CARTESIAN_POINT('Ctrl Pts',(31.1725993165996,-62.3050756093665,
-60.9024228237426));
#169370=CARTESIAN_POINT('Ctrl Pts',(31.1753410923218,-62.3154185862757,
-60.8933504498841));
#169371=CARTESIAN_POINT('Ctrl Pts',(31.1781501655449,-62.3260182489252,
-60.8844284021417));
#169372=CARTESIAN_POINT('Ctrl Pts',(31.1810233977105,-62.3368631657002,
-60.8756799581451));
#169373=CARTESIAN_POINT('Ctrl Pts',(31.1881225361094,-62.3636586213652,
-60.8540644355817));
#169374=CARTESIAN_POINT('Ctrl Pts',(31.1956178552882,-62.3919682155818,
-60.8334957734164));
#169375=CARTESIAN_POINT('Ctrl Pts',(31.2034928509274,-62.4217365557345,
-60.8141976243507));
#169376=CARTESIAN_POINT('Ctrl Pts',(31.2044308739207,-62.4252823846867,
-60.8118989427538));
#169377=CARTESIAN_POINT('Ctrl Pts',(31.2054988244701,-62.4293197487863,
-60.8093185870448));
#169378=CARTESIAN_POINT('Ctrl Pts',(31.2064549723818,-62.4329347477781,
-60.8070416049354));
#169379=CARTESIAN_POINT('Ctrl Pts',(31.206975096698,-62.434901231055,-60.8058029746481));
#169380=CARTESIAN_POINT('Ctrl Pts',(31.2074620124814,-62.4367422457334,
-60.8046531307694));
#169381=CARTESIAN_POINT('Ctrl Pts',(31.2078761028582,-62.4383079307552,
-60.8036805117118));
#169382=CARTESIAN_POINT('Ctrl Pts',(31.2089360045458,-62.4423154428585,
-60.801191005463));
#169383=CARTESIAN_POINT('Ctrl Pts',(31.210008459837,-62.4463709054711,-60.7987103220674));
#169384=CARTESIAN_POINT('Ctrl Pts',(31.21109356135,-62.4504746931321,-60.7962399497209));
#169385=CARTESIAN_POINT('Ctrl Pts',(31.2176343274827,-62.4752114712354,
-60.7813490592517));
#169386=CARTESIAN_POINT('Ctrl Pts',(31.2246242218186,-62.5016658401879,
-60.7668461547674));
#169387=CARTESIAN_POINT('Ctrl Pts',(31.2320809775905,-62.5299093892021,
-60.7530846416116));
#169388=CARTESIAN_POINT('Ctrl Pts',(31.2343612993462,-62.5385464401189,
-60.7488762862891));
#169389=CARTESIAN_POINT('Ctrl Pts',(31.2366852199439,-62.5473505889011,
-60.7447375430121));
#169390=CARTESIAN_POINT('Ctrl Pts',(31.2390530712776,-62.5563232432806,
-60.7406792618884));
#169391=CARTESIAN_POINT('Ctrl Pts',(31.2447507611333,-62.5779138731933,
-60.7309139413801));
#169392=CARTESIAN_POINT('Ctrl Pts',(31.2507016754884,-62.6004763561987,
-60.721616180738));
#169393=CARTESIAN_POINT('Ctrl Pts',(31.2569048308005,-62.6240100284728,
-60.7129476795834));
#169394=CARTESIAN_POINT('Ctrl Pts',(31.2600064084566,-62.6357768646099,
-60.7086134290061));
#169395=CARTESIAN_POINT('Ctrl Pts',(31.2631709773321,-62.6477862416905,
-60.7044366435674));
#169396=CARTESIAN_POINT('Ctrl Pts',(31.2663979733409,-62.6600364364823,
-60.7004383808229));
#169397=CARTESIAN_POINT('Ctrl Pts',(31.2680114713453,-62.6661615338782,
-60.6984392494507));
#169398=CARTESIAN_POINT('Ctrl Pts',(31.2696405761633,-62.6723468361821,
-60.6964847512362));
#169399=CARTESIAN_POINT('Ctrl Pts',(31.2712851822209,-62.678591997083,-60.6945775736112));
#169400=CARTESIAN_POINT('Ctrl Pts',(31.2721074852497,-62.6817145775334,
-60.6936239847987));
#169401=CARTESIAN_POINT('Ctrl Pts',(31.2729336635908,-62.6848521226649,
-60.6926822262165));
#169402=CARTESIAN_POINT('Ctrl Pts',(31.2737637028789,-62.6880045848913,
-60.6917526357354));
#169403=CARTESIAN_POINT('Ctrl Pts',(31.2743969734453,-62.6904097259108,
-60.6910434135348));
#169404=CARTESIAN_POINT('Ctrl Pts',(31.2752507214592,-62.6936524636479,
-60.6901022655063));
#169405=CARTESIAN_POINT('Ctrl Pts',(31.2758255067016,-62.6958357698216,
-60.6894773904497));
#169406=CARTESIAN_POINT('Ctrl Pts',(31.2760041029658,-62.6965141628936,
-60.6892832303661));
#169407=CARTESIAN_POINT('Ctrl Pts',(31.2761557406995,-62.6970901666106,
-60.6891191468964));
#169408=CARTESIAN_POINT('Ctrl Pts',(31.276265388598,-62.6975066730064,-60.6890007076171));
#169409=CARTESIAN_POINT('Ctrl Pts',(31.2794923723847,-62.7097646314778,
-60.6855149897932));
#169410=CARTESIAN_POINT('Ctrl Pts',(31.2831760644004,-62.7237611744023,
-60.6817788945145));
#169411=CARTESIAN_POINT('Ctrl Pts',(31.287323887984,-62.7395282728487,-60.6780123031017));
#169412=CARTESIAN_POINT('Ctrl Pts',(31.2914319889272,-62.7551443738452,
-60.674281783367));
#169413=CARTESIAN_POINT('Ctrl Pts',(31.2959955302348,-62.7724978666158,
-60.6705214565164));
#169414=CARTESIAN_POINT('Ctrl Pts',(31.301019614512,-62.791612885044,-60.6669950606601));
#169415=CARTESIAN_POINT('Ctrl Pts',(31.3059736788063,-62.8104615000466,
-60.6635178117056));
#169416=CARTESIAN_POINT('Ctrl Pts',(31.3113757072995,-62.8310235174328,
-60.6602681537048));
#169417=CARTESIAN_POINT('Ctrl Pts',(31.3172261299313,-62.8533062793187,
-60.6575460641314));
#169418=CARTESIAN_POINT('Ctrl Pts',(31.3228826744743,-62.8748506092043,
-60.6549141823186));
#169419=CARTESIAN_POINT('Ctrl Pts',(31.3289585309402,-62.898004070122,-60.6527757376979));
#169420=CARTESIAN_POINT('Ctrl Pts',(31.3354476363654,-62.9227499384764,
-60.6514431409284));
#169421=CARTESIAN_POINT('Ctrl Pts',(31.3400888166132,-62.9404488396189,
-60.6504900323873));
#169422=CARTESIAN_POINT('Ctrl Pts',(31.3449412714657,-62.9589618928917,
-60.64995));
#169423=CARTESIAN_POINT('Ctrl Pts',(31.35,-62.9782728042642,-60.64995));
#169424=CARTESIAN_POINT('Origin',(0.,-12.9675000200281,-60.64995));
#169425=CARTESIAN_POINT('',(25.5011648721215,-65.1922357602732,-61.2273317382593));
#169426=CARTESIAN_POINT('Origin',(0.,-12.9675000200281,-61.2273317382593));
#169427=CARTESIAN_POINT('Ctrl Pts',(25.5011648721215,-65.1922357602732,
-61.2273317382594));
#169428=CARTESIAN_POINT('Ctrl Pts',(25.4991627264348,-64.5368797680873,
-62.4921139271883));
#169429=CARTESIAN_POINT('Ctrl Pts',(25.4971342104485,-63.8900461478545,
-63.7361686020899));
#169430=CARTESIAN_POINT('Ctrl Pts',(25.4950786388046,-63.2516311374157,
-64.9594484662041));
#169431=CARTESIAN_POINT('Ctrl Pts',(25.4929314940811,-62.5847755573274,
-66.2372238788364));
#169432=CARTESIAN_POINT('Ctrl Pts',(25.4907548287261,-61.9271053228049,
-67.4923322416149));
#169433=CARTESIAN_POINT('Ctrl Pts',(25.488548990673,-61.2785535158614,-68.7247481694799));
#169434=CARTESIAN_POINT('Ctrl Pts',(25.4863229332212,-60.6240568810712,
-69.968460805562));
#169435=CARTESIAN_POINT('Ctrl Pts',(25.4840671719797,-59.9788468670033,
-71.1890632334062));
#169436=CARTESIAN_POINT('Ctrl Pts',(25.4817831377555,-59.3429037702644,
-72.3865566306907));
#169437=CARTESIAN_POINT('Ctrl Pts',(25.4794165618636,-58.6839786169288,
-73.6273256939456));
#169438=CARTESIAN_POINT('Ctrl Pts',(25.4770196348699,-58.0350023501894,
-74.8432853373019));
#169439=CARTESIAN_POINT('Ctrl Pts',(25.4745950365093,-57.3960031446104,
-76.0344647149628));
#169440=CARTESIAN_POINT('Ctrl Pts',(25.4724033328441,-56.8183829813483,
-77.1112254066692));
#169441=CARTESIAN_POINT('Ctrl Pts',(25.4701890367985,-56.2489160726328,
-78.1677381930187));
#169442=CARTESIAN_POINT('Ctrl Pts',(25.4679548160676,-55.6876551762764,
-79.2040423737711));
#169443=CARTESIAN_POINT('Origin',(24.7,-70.08000002,-174.34995));
#169444=CARTESIAN_POINT('',(25.2,-70.08000002,-176.84995));
#169445=CARTESIAN_POINT('Origin',(24.7,-70.08000002,-176.84995));
#169446=CARTESIAN_POINT('',(25.2,-72.58000002,-174.34995));
#169447=CARTESIAN_POINT('Origin',(25.2,-70.08000002,-174.34995));
#169448=CARTESIAN_POINT('Origin',(24.7,-72.58000002,-174.34995));
#169449=CARTESIAN_POINT('Origin',(24.7,-72.58000002,-55.24995));
#169450=CARTESIAN_POINT('',(25.2,-72.58000002,-58.24995));
#169451=CARTESIAN_POINT('',(25.2,-72.58000002,-174.34995));
#169452=CARTESIAN_POINT('Origin',(24.7,-72.58000002,-58.24995));
#169453=CARTESIAN_POINT('Ctrl Pts',(25.2,-56.0768896606488,-79.4153515046414));
#169454=CARTESIAN_POINT('Ctrl Pts',(25.2,-55.8110355215084,-79.2710235754996));
#169455=CARTESIAN_POINT('Ctrl Pts',(25.4679548160676,-55.6876551762764,
-79.2040423737711));
#169456=CARTESIAN_POINT('Ctrl Pts',(25.2,-59.3123390931711,-73.4556067153995));
#169457=CARTESIAN_POINT('Ctrl Pts',(25.2000000000118,-59.0651351497249,
-73.255975182323));
#169458=CARTESIAN_POINT('Ctrl Pts',(25.4808037502955,-58.9154492031739,
-73.2442891352868));
#169459=CARTESIAN_POINT('Ctrl Pts',(25.2,-62.4759645157842,-67.4577026174502));
#169460=CARTESIAN_POINT('Ctrl Pts',(25.200000000035,-62.2130344026582,-67.2677845851136));
#169461=CARTESIAN_POINT('Ctrl Pts',(25.4916367264251,-62.0734180747052,
-67.2463887183684));
#169462=CARTESIAN_POINT('Ctrl Pts',(25.2,-65.5994372375941,-61.4386408691297));
#169463=CARTESIAN_POINT('Ctrl Pts',(25.1999999999999,-65.3080942147003,
-61.2874541854323));
#169464=CARTESIAN_POINT('Ctrl Pts',(25.5011648721215,-65.1922357602732,
-61.2273317382594));
#169465=CARTESIAN_POINT('',(25.2,-56.0768896606488,-79.4153515046414));
#169466=CARTESIAN_POINT('Origin',(25.7,-56.0768896606488,-79.4153515046414));
#169467=CARTESIAN_POINT('',(25.2,-65.5994372375942,-61.4386408691297));
#169468=CARTESIAN_POINT('Origin',(25.7,-65.5994372375942,-61.4386408691297));
#169469=CARTESIAN_POINT('Ctrl Pts',(25.2,-56.0768896606488,-79.4153515046414));
#169470=CARTESIAN_POINT('Ctrl Pts',(25.2,-59.3123551324919,-73.4555771707379));
#169471=CARTESIAN_POINT('Ctrl Pts',(25.2,-62.4759494901776,-67.4577315724186));
#169472=CARTESIAN_POINT('Ctrl Pts',(25.2,-65.5994372375941,-61.4386408691297));
#169473=CARTESIAN_POINT('Ctrl Pts',(25.4545017719006,-55.8438706635705,
-78.943998453909));
#169474=CARTESIAN_POINT('Ctrl Pts',(25.2000000000001,-55.9670041176591,
-79.0175935267739));
#169475=CARTESIAN_POINT('Ctrl Pts',(25.2,-56.2177692725606,-79.1675127966822));
#169476=CARTESIAN_POINT('Ctrl Pts',(25.4946642550745,-55.3775661721662,
-79.6840646292403));
#169477=CARTESIAN_POINT('Ctrl Pts',(25.1999999999996,-55.4896073847247,
-79.7583704081732));
#169478=CARTESIAN_POINT('Ctrl Pts',(25.2,-55.7980013963185,-79.8734371403239));
#169479=CARTESIAN_POINT('Ctrl Pts',(25.5373410788309,-55.060286146179,-80.4743302772342));
#169480=CARTESIAN_POINT('Ctrl Pts',(25.2000000000013,-55.1662734412503,
-80.5380010629174));
#169481=CARTESIAN_POINT('Ctrl Pts',(25.2,-55.5124752416472,-80.6262357014044));
#169482=CARTESIAN_POINT('Ctrl Pts',(25.6012210394754,-54.7627355327589,
-81.6666848695308));
#169483=CARTESIAN_POINT('Ctrl Pts',(25.1999999999993,-54.8412314292706,
-81.6875787444334));
#169484=CARTESIAN_POINT('Ctrl Pts',(25.2,-55.2446154752418,-81.7605756924265));
#169485=CARTESIAN_POINT('Ctrl Pts',(25.6211910848485,-54.694018420619,-82.0406920440613));
#169486=CARTESIAN_POINT('Ctrl Pts',(25.2,-54.7601766884843,-82.0569617949468));
#169487=CARTESIAN_POINT('Ctrl Pts',(25.2,-55.1827439360829,-82.1162012744658));
#169488=CARTESIAN_POINT('Ctrl Pts',(25.6662757795504,-54.5909095821962,
-82.8883828751549));
#169489=CARTESIAN_POINT('Ctrl Pts',(25.2,-54.6218448035381,-82.9004000920468));
#169490=CARTESIAN_POINT('Ctrl Pts',(25.2,-55.0898763101586,-82.9217439686801));
#169491=CARTESIAN_POINT('Ctrl Pts',(25.6914944489404,-54.5694774201419,
-83.364867732155));
#169492=CARTESIAN_POINT('Ctrl Pts',(25.2,-54.5787849570664,-83.3759856193062));
#169493=CARTESIAN_POINT('Ctrl Pts',(25.2,-55.0705472464169,-83.3741940098927));
#169494=CARTESIAN_POINT('Ctrl Pts',(25.7167531711063,-54.5847952699482,
-83.8448396592079));
#169495=CARTESIAN_POINT('Ctrl Pts',(25.1999999999999,-54.5674926027507,
-83.8453670198231));
#169496=CARTESIAN_POINT('Ctrl Pts',(25.2,-55.0842863948154,-83.8295657569677));
#169497=CARTESIAN_POINT('',(25.2,-55.08000002,-83.5456386250819));
#169498=CARTESIAN_POINT('Origin',(25.7,-55.08000002,-83.5456386250819));
#169499=CARTESIAN_POINT('Ctrl Pts',(25.2,-55.08000002,-83.5456386250819));
#169500=CARTESIAN_POINT('Ctrl Pts',(25.2,-55.08000002,-83.1859931739116));
#169501=CARTESIAN_POINT('Ctrl Pts',(25.2,-55.1006621337637,-82.8281867002424));
#169502=CARTESIAN_POINT('Ctrl Pts',(25.2,-55.1417030348396,-82.4721939873445));
#169503=CARTESIAN_POINT('Ctrl Pts',(25.2,-55.1827439359154,-82.1162012744465));
#169504=CARTESIAN_POINT('Ctrl Pts',(25.2,-55.2446154752336,-81.7605756924466));
#169505=CARTESIAN_POINT('Ctrl Pts',(25.2,-55.3267103680732,-81.4129179556859));
#169506=CARTESIAN_POINT('Ctrl Pts',(25.2,-55.4088052609128,-81.0652602189252));
#169507=CARTESIAN_POINT('Ctrl Pts',(25.2,-55.5103655940696,-80.7242806574902));
#169508=CARTESIAN_POINT('Ctrl Pts',(25.2,-55.6343884585548,-80.3910074402699));
#169509=CARTESIAN_POINT('Ctrl Pts',(25.2,-55.75841132304,-80.0577342230496));
#169510=CARTESIAN_POINT('Ctrl Pts',(25.2,-55.9048956589413,-79.7321669507792));
#169511=CARTESIAN_POINT('Ctrl Pts',(25.2,-56.0768896606488,-79.4153515046414));
#169512=CARTESIAN_POINT('Origin',(25.7,-55.08000002,-55.24995));
#169513=CARTESIAN_POINT('',(25.2,-55.08000002,-148.513004346424));
#169514=CARTESIAN_POINT('Origin',(25.7,-55.08000002,-148.513004346424));
#169515=CARTESIAN_POINT('',(25.2,-55.08000002,-84.0594740639255));
#169516=CARTESIAN_POINT('Ctrl Pts',(25.7,-54.58000002,-148.513004346424));
#169517=CARTESIAN_POINT('Ctrl Pts',(25.2,-54.58000002,-148.513004346424));
#169518=CARTESIAN_POINT('Ctrl Pts',(25.2,-55.08000002,-148.513004346424));
#169519=CARTESIAN_POINT('Ctrl Pts',(25.6600482417947,-54.58000002,-149.271156587884));
#169520=CARTESIAN_POINT('Ctrl Pts',(25.2000000000095,-54.6184124317501,
-149.241944845519));
#169521=CARTESIAN_POINT('Ctrl Pts',(25.2,-55.0800000219098,-149.232572052747));
#169522=CARTESIAN_POINT('Ctrl Pts',(25.6205133511944,-54.6700019565425,
-150.014998643991));
#169523=CARTESIAN_POINT('Ctrl Pts',(25.1999999999999,-54.7333981827002,
-149.982853405445));
#169524=CARTESIAN_POINT('Ctrl Pts',(25.2,-55.161001761834,-149.939471833849));
#169525=CARTESIAN_POINT('Ctrl Pts',(25.5425103305472,-55.0316743873447,
-151.47324255767));
#169526=CARTESIAN_POINT('Ctrl Pts',(25.2,-55.1367600846321,-151.417636910868));
#169527=CARTESIAN_POINT('Ctrl Pts',(25.2,-55.4865069516644,-151.326860933587));
#169528=CARTESIAN_POINT('Ctrl Pts',(25.5037571210995,-55.3070348279188,
-152.192808028705));
#169529=CARTESIAN_POINT('Ctrl Pts',(25.2,-55.4199215048179,-152.126493092391));
#169530=CARTESIAN_POINT('Ctrl Pts',(25.2,-55.7343229434107,-152.012278589766));
#169531=CARTESIAN_POINT('Ctrl Pts',(25.4679548160676,-55.6876551762764,
-152.854600597735));
#169532=CARTESIAN_POINT('Ctrl Pts',(25.2,-55.8110355215084,-152.787619396006));
#169533=CARTESIAN_POINT('Ctrl Pts',(25.2,-56.0768896606487,-152.643291466864));
#169534=CARTESIAN_POINT('',(25.2,-56.0768896606488,-152.643291466864));
#169535=CARTESIAN_POINT('Origin',(25.7,-56.0768896606488,-152.643291466864));
#169536=CARTESIAN_POINT('Ctrl Pts',(25.2,-56.0768896606487,-152.643291466864));
#169537=CARTESIAN_POINT('Ctrl Pts',(25.2,-56.014966929036,-152.529228896965));
#169538=CARTESIAN_POINT('Ctrl Pts',(25.2,-55.9563289964364,-152.41374598058));
#169539=CARTESIAN_POINT('Ctrl Pts',(25.2,-55.9007756544418,-152.296934067097));
#169540=CARTESIAN_POINT('Ctrl Pts',(25.2,-55.8430042328461,-152.175458201579));
#169541=CARTESIAN_POINT('Ctrl Pts',(25.2,-55.7885684933974,-152.052544547972));
#169542=CARTESIAN_POINT('Ctrl Pts',(25.2,-55.7372926676245,-151.928266900595));
#169543=CARTESIAN_POINT('Ctrl Pts',(25.2,-55.7009775154016,-151.84024956271));
#169544=CARTESIAN_POINT('Ctrl Pts',(25.2,-55.6662483997963,-151.75154742078));
#169545=CARTESIAN_POINT('Ctrl Pts',(25.2,-55.6330574644204,-151.662180878469));
#169546=CARTESIAN_POINT('Ctrl Pts',(25.2,-55.563802642011,-151.475712375941));
#169547=CARTESIAN_POINT('Ctrl Pts',(25.2,-55.5013746560331,-151.286675000308));
#169548=CARTESIAN_POINT('Ctrl Pts',(25.2,-55.4456440455194,-151.096220906466));
#169549=CARTESIAN_POINT('Ctrl Pts',(25.2,-55.400687777678,-150.94258711033));
#169550=CARTESIAN_POINT('Ctrl Pts',(25.2,-55.3600885309574,-150.78803223373));
#169551=CARTESIAN_POINT('Ctrl Pts',(25.2,-55.323754356376,-150.633166383806));
#169552=CARTESIAN_POINT('Ctrl Pts',(25.2,-55.224809284665,-150.211436351325));
#169553=CARTESIAN_POINT('Ctrl Pts',(25.2,-55.1560866851019,-149.784875950094));
#169554=CARTESIAN_POINT('Ctrl Pts',(25.2,-55.1174016248576,-149.353514705437));
#169555=CARTESIAN_POINT('Ctrl Pts',(25.2,-55.0924544716307,-149.075339228945));
#169556=CARTESIAN_POINT('Ctrl Pts',(25.2,-55.0800000200004,-148.795167064065));
#169557=CARTESIAN_POINT('Ctrl Pts',(25.2,-55.08000002,-148.513004346424));
#169558=CARTESIAN_POINT('Ctrl Pts',(25.2,-65.7246041881209,-170.861259130871));
#169559=CARTESIAN_POINT('Ctrl Pts',(25.2,-65.4329690822618,-171.012528323755));
#169560=CARTESIAN_POINT('Ctrl Pts',(25.5015460489969,-65.317216804244,-171.07256826174));
#169561=CARTESIAN_POINT('Ctrl Pts',(25.2,-62.5605386715726,-164.761189683274));
#169562=CARTESIAN_POINT('Ctrl Pts',(25.1999999998579,-62.297876586317,-164.952133926682));
#169563=CARTESIAN_POINT('Ctrl Pts',(25.4919266567716,-62.1578398412392,
-164.972503788787));
#169564=CARTESIAN_POINT('Ctrl Pts',(25.2,-59.3555677916457,-158.682664145768));
#169565=CARTESIAN_POINT('Ctrl Pts',(25.2,-59.109002613422,-158.883754709366));
#169566=CARTESIAN_POINT('Ctrl Pts',(25.4809754250192,-58.9585757861229,
-158.893982149016));
#169567=CARTESIAN_POINT('Ctrl Pts',(25.2,-56.0768896606488,-152.643291466864));
#169568=CARTESIAN_POINT('Ctrl Pts',(25.2,-55.8110355215084,-152.787619396006));
#169569=CARTESIAN_POINT('Ctrl Pts',(25.4679548160676,-55.6876551762764,
-152.854600597735));
#169570=CARTESIAN_POINT('',(25.2,-65.7246041881209,-170.861259130871));
#169571=CARTESIAN_POINT('Origin',(25.7,-65.7246041881209,-170.861259130871));
#169572=CARTESIAN_POINT('Ctrl Pts',(25.2,-65.7246041881209,-170.861259130871));
#169573=CARTESIAN_POINT('Ctrl Pts',(25.2,-62.5605227754587,-164.761159036905));
#169574=CARTESIAN_POINT('Ctrl Pts',(25.2,-59.3555847723563,-158.682695424483));
#169575=CARTESIAN_POINT('Ctrl Pts',(25.2,-56.0768896606488,-152.643291466864));
#169576=CARTESIAN_POINT('Ctrl Pts',(25.5015460489969,-65.3172168042439,
-171.07256826174));
#169577=CARTESIAN_POINT('Ctrl Pts',(25.2,-65.4329690822618,-171.012528323755));
#169578=CARTESIAN_POINT('Ctrl Pts',(25.2,-65.7246041881209,-170.861259130871));
#169579=CARTESIAN_POINT('Ctrl Pts',(25.5078751098564,-65.3460382794916,
-171.13407782586));
#169580=CARTESIAN_POINT('Ctrl Pts',(25.2,-65.4555942264487,-171.066917428723));
#169581=CARTESIAN_POINT('Ctrl Pts',(25.2,-65.7405566104338,-170.892014084856));
#169582=CARTESIAN_POINT('Ctrl Pts',(25.5154426820321,-65.380521047679,-171.191481806562));
#169583=CARTESIAN_POINT('Ctrl Pts',(25.1999999999994,-65.4828113676634,
-171.118510663779));
#169584=CARTESIAN_POINT('Ctrl Pts',(25.2,-65.7596409576893,-170.920716557309));
#169585=CARTESIAN_POINT('Ctrl Pts',(25.5241645957028,-65.4203114663335,
-171.244965273984));
#169586=CARTESIAN_POINT('Ctrl Pts',(25.2,-65.5143246899125,-171.167561256232));
#169587=CARTESIAN_POINT('Ctrl Pts',(25.2,-65.7816577220592,-170.947457636992));
#169588=CARTESIAN_POINT('',(25.2,-65.7816577220592,-170.947457636992));
#169589=CARTESIAN_POINT('Origin',(25.7,-65.7816577220592,-170.947457636992));
#169590=CARTESIAN_POINT('Ctrl Pts',(25.2,-65.7816577220592,-170.947457636992));
#169591=CARTESIAN_POINT('Ctrl Pts',(25.2,-65.759637326036,-170.920712146581));
#169592=CARTESIAN_POINT('Ctrl Pts',(25.2,-65.7405592277015,-170.892019192244));
#169593=CARTESIAN_POINT('Ctrl Pts',(25.2,-65.7246041881209,-170.861259130871));
#169594=CARTESIAN_POINT('Ctrl Pts',(25.2,-66.1031295107182,-171.854014632589));
#169595=CARTESIAN_POINT('Ctrl Pts',(25.1999999999999,-65.7373527968364,
-171.85401463259));
#169596=CARTESIAN_POINT('Ctrl Pts',(25.5486065204957,-65.6266003779639,
-171.854014632591));
#169597=CARTESIAN_POINT('Ctrl Pts',(25.2,-66.1031295051642,-171.688945996574));
#169598=CARTESIAN_POINT('Ctrl Pts',(25.2,-65.7495636563843,-171.730197187823));
#169599=CARTESIAN_POINT('Ctrl Pts',(25.5332781069629,-65.6314702205409,
-171.740892625582));
#169600=CARTESIAN_POINT('Ctrl Pts',(25.2,-66.0766766441701,-171.528325399449));
#169601=CARTESIAN_POINT('Ctrl Pts',(25.2,-65.7357529125625,-171.605967390697));
#169602=CARTESIAN_POINT('Ctrl Pts',(25.5254918386358,-65.6165368852731,
-171.632443841085));
#169603=CARTESIAN_POINT('Ctrl Pts',(25.2,-65.9668265905144,-171.216885108557));
#169604=CARTESIAN_POINT('Ctrl Pts',(25.1999999999999,-65.6576340206492,
-171.369178819378));
#169605=CARTESIAN_POINT('Ctrl Pts',(25.5190396326646,-65.5455021430107,
-171.42367336987));
#169606=CARTESIAN_POINT('Ctrl Pts',(25.2,-65.8865499901975,-171.074857506769));
#169607=CARTESIAN_POINT('Ctrl Pts',(25.2,-65.5955175213768,-171.261530708485));
#169608=CARTESIAN_POINT('Ctrl Pts',(25.5204167023824,-65.4915081760158,
-171.329224126564));
#169609=CARTESIAN_POINT('Ctrl Pts',(25.2,-65.7816577220592,-170.947457636992));
#169610=CARTESIAN_POINT('Ctrl Pts',(25.1999999999999,-65.5143246899125,
-171.167561256232));
#169611=CARTESIAN_POINT('Ctrl Pts',(25.5241645957028,-65.4203114663335,
-171.244965273984));
#169612=CARTESIAN_POINT('',(25.2,-66.1031295107175,-171.854014632589));
#169613=CARTESIAN_POINT('',(25.5486065204179,-65.6266003779886,-171.854014632026));
#169614=CARTESIAN_POINT('Origin',(25.7,-66.1031295107182,-171.854014632589));
#169615=CARTESIAN_POINT('Ctrl Pts',(25.5241645957028,-65.4203114663335,
-171.244965273985));
#169616=CARTESIAN_POINT('Ctrl Pts',(25.5231299263541,-65.4399665220691,
-171.268226355155));
#169617=CARTESIAN_POINT('Ctrl Pts',(25.522294585227,-65.4579784931356,-171.291877835995));
#169618=CARTESIAN_POINT('Ctrl Pts',(25.5216840617807,-65.474386214064,-171.315718493851));
#169619=CARTESIAN_POINT('Ctrl Pts',(25.5210735383344,-65.4907939349924,
-171.339559151708));
#169620=CARTESIAN_POINT('Ctrl Pts',(25.5206879562631,-65.5055976477405,
-171.363588766213));
#169621=CARTESIAN_POINT('Ctrl Pts',(25.5205350576004,-65.5188821404571,
-171.387584492607));
#169622=CARTESIAN_POINT('Ctrl Pts',(25.5203772443314,-65.5325936352857,
-171.412351511218));
#169623=CARTESIAN_POINT('Ctrl Pts',(25.5204670406992,-65.5446917115373,
-171.437087091981));
#169624=CARTESIAN_POINT('Ctrl Pts',(25.5207940342398,-65.555334013505,-171.46158698178));
#169625=CARTESIAN_POINT('Ctrl Pts',(25.5210214587905,-65.5627357521982,
-171.478626695825));
#169626=CARTESIAN_POINT('Ctrl Pts',(25.5213632022661,-65.5694346066928,
-171.495553194624));
#169627=CARTESIAN_POINT('Ctrl Pts',(25.5218116495206,-65.5754939001744,
-171.512310512318));
#169628=CARTESIAN_POINT('Ctrl Pts',(25.5219110299368,-65.5768367004739,
-171.516024102242));
#169629=CARTESIAN_POINT('Ctrl Pts',(25.5220026056098,-65.5779873853903,
-171.519273109632));
#169630=CARTESIAN_POINT('Ctrl Pts',(25.5221106011063,-65.5792558272748,
-171.522927038886));
#169631=CARTESIAN_POINT('Ctrl Pts',(25.5221580914876,-65.5798136170971,
-171.524533832681));
#169632=CARTESIAN_POINT('Ctrl Pts',(25.5222088848793,-65.5803936558672,
-171.526219210179));
#169633=CARTESIAN_POINT('Ctrl Pts',(25.5222657314613,-65.5810195156442,
-171.528058604948));
#169634=CARTESIAN_POINT('Ctrl Pts',(25.5222827629558,-65.5812070260796,
-171.528609695986));
#169635=CARTESIAN_POINT('Ctrl Pts',(25.5223003400726,-65.5813985772047,
-171.529174456282));
#169636=CARTESIAN_POINT('Ctrl Pts',(25.5223185463672,-65.5815947553066,
-171.529754907915));
#169637=CARTESIAN_POINT('Ctrl Pts',(25.5233919437605,-65.5931609233538,
-171.56397687794));
#169638=CARTESIAN_POINT('Ctrl Pts',(25.5249423650029,-65.602329155868,-171.598090812457));
#169639=CARTESIAN_POINT('Ctrl Pts',(25.5270085019446,-65.6093231945859,
-171.631964042931));
#169640=CARTESIAN_POINT('Ctrl Pts',(25.5290969526855,-65.6163927672979,
-171.66620309643));
#169641=CARTESIAN_POINT('Ctrl Pts',(25.5317125482548,-65.621241287655,-171.700196223063));
#169642=CARTESIAN_POINT('Ctrl Pts',(25.5348601544508,-65.6241378124208,
-171.733792453079));
#169643=CARTESIAN_POINT('Ctrl Pts',(25.5380761467274,-65.6270972681774,
-171.768118607474));
#169644=CARTESIAN_POINT('Ctrl Pts',(25.5418477161118,-65.6280193673831,
-171.802030424976));
#169645=CARTESIAN_POINT('Ctrl Pts',(25.5461401976557,-65.6272249998709,
-171.835352357183));
#169646=CARTESIAN_POINT('Ctrl Pts',(25.5469442697997,-65.6270761981156,
-171.841594256466));
#169647=CARTESIAN_POINT('Ctrl Pts',(25.5477665059252,-65.6268672508965,
-171.8478154174));
#169648=CARTESIAN_POINT('Ctrl Pts',(25.5486065204168,-65.626600377989,-171.854014632026));
#169649=CARTESIAN_POINT('Ctrl Pts',(25.2,-66.1031295107175,-171.854014632589));
#169650=CARTESIAN_POINT('Ctrl Pts',(25.2,-66.1031295063964,-171.725572055906));
#169651=CARTESIAN_POINT('Ctrl Pts',(25.2,-66.0871173562523,-171.599865253242));
#169652=CARTESIAN_POINT('Ctrl Pts',(25.2,-66.0541497294318,-171.477055409759));
#169653=CARTESIAN_POINT('Ctrl Pts',(25.2,-66.0447396524369,-171.442001322027));
#169654=CARTESIAN_POINT('Ctrl Pts',(25.2,-66.0339478541516,-171.407183310008));
#169655=CARTESIAN_POINT('Ctrl Pts',(25.2,-66.0217516132152,-171.372605255459));
#169656=CARTESIAN_POINT('Ctrl Pts',(25.2,-65.9940406295861,-171.294040728197));
#169657=CARTESIAN_POINT('Ctrl Pts',(25.2,-65.9598967243537,-171.219005811922));
#169658=CARTESIAN_POINT('Ctrl Pts',(25.2,-65.9193893860855,-171.147550497276));
#169659=CARTESIAN_POINT('Ctrl Pts',(25.2,-65.8796084720222,-171.077376601561));
#169660=CARTESIAN_POINT('Ctrl Pts',(25.2,-65.8336900811296,-171.010655009758));
#169661=CARTESIAN_POINT('Ctrl Pts',(25.2,-65.7816577220592,-170.947457636992));
#169662=CARTESIAN_POINT('Ctrl Pts',(25.567270247017,-65.4932347742778,-60.8550643728577));
#169663=CARTESIAN_POINT('Ctrl Pts',(25.2,-65.5504599379798,-60.9384440262482));
#169664=CARTESIAN_POINT('Ctrl Pts',(25.2,-65.76604051674,-61.2525142085044));
#169665=CARTESIAN_POINT('Ctrl Pts',(25.5372515674752,-65.3560756313885,
-60.9593757850282));
#169666=CARTESIAN_POINT('Ctrl Pts',(25.1999999999999,-65.4390463676049,
-61.0441607188783));
#169667=CARTESIAN_POINT('Ctrl Pts',(25.2,-65.6901622771225,-61.3046675609273));
#169668=CARTESIAN_POINT('Ctrl Pts',(25.5126788498768,-65.2443062807722,
-61.0990698192377));
#169669=CARTESIAN_POINT('Ctrl Pts',(25.2,-65.3491857740292,-61.1739405307172));
#169670=CARTESIAN_POINT('Ctrl Pts',(25.2,-65.6282820810228,-61.3745120488097));
#169671=CARTESIAN_POINT('Ctrl Pts',(25.4971432604052,-65.1737221584172,
-61.2692230181219));
#169672=CARTESIAN_POINT('Ctrl Pts',(25.2,-65.293642201641,-61.3241535201351));
#169673=CARTESIAN_POINT('Ctrl Pts',(25.2,-65.5891959094587,-61.4595920393833));
#169674=CARTESIAN_POINT('',(25.5598256884619,-65.45949290163,-60.8818893816432));
#169675=CARTESIAN_POINT('Ctrl Pts',(25.5598256882386,-65.4594929016689,
-60.8818893816956));
#169676=CARTESIAN_POINT('Ctrl Pts',(25.5531049092406,-65.4288008059568,
-60.9073497695154));
#169677=CARTESIAN_POINT('Ctrl Pts',(25.5467989300454,-65.4000883723788,
-60.934263332496));
#169678=CARTESIAN_POINT('Ctrl Pts',(25.5409376948429,-65.3734073767371,
-60.9622975884069));
#169679=CARTESIAN_POINT('Ctrl Pts',(25.5349907014394,-65.3463360002097,
-60.9907420253246));
#169680=CARTESIAN_POINT('Ctrl Pts',(25.5295014264852,-65.3213556457941,
-61.0203397151011));
#169681=CARTESIAN_POINT('Ctrl Pts',(25.5244779293711,-65.2984740811048,
-61.0507610829557));
#169682=CARTESIAN_POINT('Ctrl Pts',(25.51932958311,-65.2750238400988,-61.0819385141152));
#169683=CARTESIAN_POINT('Ctrl Pts',(25.5146703184022,-65.2537777129736,
-61.113980610906));
#169684=CARTESIAN_POINT('Ctrl Pts',(25.5104866316509,-65.2347002082,-61.1465583656441));
#169685=CARTESIAN_POINT('Ctrl Pts',(25.5070679032027,-65.2191108937587,
-61.1731795023406));
#169686=CARTESIAN_POINT('Ctrl Pts',(25.5039662672152,-65.2049687286471,
-61.2001587559061));
#169687=CARTESIAN_POINT('Ctrl Pts',(25.5011648721215,-65.1922357602732,
-61.2273317382593));
#169688=CARTESIAN_POINT('',(25.2,-65.7473676730073,-61.2659196908498));
#169689=CARTESIAN_POINT('Origin',(25.7,-65.7473676730073,-61.2659196908498));
#169690=CARTESIAN_POINT('Origin',(25.2,-66.2733246934326,-61.766045927512));
#169691=CARTESIAN_POINT('Origin',(42.,-73.08000002,-171.14995));
#169692=CARTESIAN_POINT('',(41.5,-62.2620341086569,-171.14995));
#169693=CARTESIAN_POINT('Origin',(42.,-62.2620341086569,-171.14995));
#169694=CARTESIAN_POINT('',(42.,-58.6035812240168,-171.64995));
#169695=CARTESIAN_POINT('',(42.,-62.3323045260081,-171.64995));
#169696=CARTESIAN_POINT('',(41.5,-58.6035812240168,-171.14995));
#169697=CARTESIAN_POINT('Origin',(42.,-58.6035812240168,-171.14995));
#169698=CARTESIAN_POINT('',(41.5,-55.58000002,-171.14995));
#169699=CARTESIAN_POINT('Ctrl Pts',(41.5,-63.7767754674349,-172.64995));
#169700=CARTESIAN_POINT('Ctrl Pts',(41.5,-63.3421320985268,-172.64995));
#169701=CARTESIAN_POINT('Ctrl Pts',(41.9304134495199,-63.2816414330641,
-172.64995));
#169702=CARTESIAN_POINT('Ctrl Pts',(41.5,-63.7767754674226,-172.453565067926));
#169703=CARTESIAN_POINT('Ctrl Pts',(41.5,-63.3421320985213,-172.511015867074));
#169704=CARTESIAN_POINT('Ctrl Pts',(41.9304134495211,-63.2816414330639,
-172.51902671195));
#169705=CARTESIAN_POINT('Ctrl Pts',(41.5,-63.7373507987217,-172.257328160063));
#169706=CARTESIAN_POINT('Ctrl Pts',(41.4999999999999,-63.3123764134035,
-172.371853931892));
#169707=CARTESIAN_POINT('Ctrl Pts',(41.9322246014262,-63.2551037797886,
-172.38820210671));
#169708=CARTESIAN_POINT('Ctrl Pts',(41.5,-63.5855944954388,-171.894521542842));
#169709=CARTESIAN_POINT('Ctrl Pts',(41.5,-63.1995654042688,-172.118296873734));
#169710=CARTESIAN_POINT('Ctrl Pts',(41.9391962191206,-63.152953113962,-172.14633102856));
#169711=CARTESIAN_POINT('Ctrl Pts',(41.5,-63.4733225377971,-171.728129909852));
#169712=CARTESIAN_POINT('Ctrl Pts',(41.500000000002,-63.1159963120049,-172.003556970023));
#169713=CARTESIAN_POINT('Ctrl Pts',(41.9443539433762,-63.0773802713291,
-172.035403273235));
#169714=CARTESIAN_POINT('Ctrl Pts',(41.5,-63.192913452588,-171.450449746589));
#169715=CARTESIAN_POINT('Ctrl Pts',(41.499999999998,-62.9115510926292,-171.817687494207));
#169716=CARTESIAN_POINT('Ctrl Pts',(41.9572358131761,-62.8886304524563,
-171.850283164391));
#169717=CARTESIAN_POINT('Ctrl Pts',(41.5,-63.0248865939453,-171.339270411997));
#169718=CARTESIAN_POINT('Ctrl Pts',(41.4999999999999,-62.7899873764732,
-171.746711574348));
#169719=CARTESIAN_POINT('Ctrl Pts',(41.9649548930126,-62.7755277007723,
-171.776163607997));
#169720=CARTESIAN_POINT('Ctrl Pts',(41.5,-62.6585144680136,-171.18899099047));
#169721=CARTESIAN_POINT('Ctrl Pts',(41.5,-62.5315521155723,-171.658003579003));
#169722=CARTESIAN_POINT('Ctrl Pts',(41.981785867019,-62.528914177679,-171.675977326981));
#169723=CARTESIAN_POINT('Ctrl Pts',(41.5,-62.4603490280314,-171.149950000016));
#169724=CARTESIAN_POINT('Ctrl Pts',(41.4999999999999,-62.3942825374201,
-171.640924254979));
#169725=CARTESIAN_POINT('Ctrl Pts',(41.9908895000012,-62.3955244521823,
-171.64995));
#169726=CARTESIAN_POINT('Ctrl Pts',(41.5,-62.2620341086569,-171.14995));
#169727=CARTESIAN_POINT('Ctrl Pts',(41.4999999999999,-62.2620341086569,
-171.64995));
#169728=CARTESIAN_POINT('Ctrl Pts',(42.,-62.2620341086569,-171.64995));
#169729=CARTESIAN_POINT('',(41.5,-63.7767754674349,-172.64995));
#169730=CARTESIAN_POINT('Origin',(42.,-63.7767754674349,-172.64995));
#169731=CARTESIAN_POINT('Ctrl Pts',(41.5,-63.7767754674349,-172.64995));
#169732=CARTESIAN_POINT('Ctrl Pts',(41.5,-63.7767754674226,-172.453565067926));
#169733=CARTESIAN_POINT('Ctrl Pts',(41.5,-63.7373507987217,-172.257328160063));
#169734=CARTESIAN_POINT('Ctrl Pts',(41.5,-63.5855944954388,-171.894521542842));
#169735=CARTESIAN_POINT('Ctrl Pts',(41.5,-63.4733225377971,-171.728129909852));
#169736=CARTESIAN_POINT('Ctrl Pts',(41.5,-63.192913452588,-171.450449746589));
#169737=CARTESIAN_POINT('Ctrl Pts',(41.5,-63.0248865939453,-171.339270411997));
#169738=CARTESIAN_POINT('Ctrl Pts',(41.5,-62.6585144680136,-171.18899099047));
#169739=CARTESIAN_POINT('Ctrl Pts',(41.5,-62.4603490280314,-171.149950000016));
#169740=CARTESIAN_POINT('Ctrl Pts',(41.5,-62.2620341086569,-171.14995));
#169741=CARTESIAN_POINT('Origin',(42.,-63.7767754674349,-171.64995));
#169742=CARTESIAN_POINT('',(41.9304134495199,-63.2816414330641,-171.64995));
#169743=CARTESIAN_POINT('',(41.5,-63.7767754674349,-177.34995));
#169744=CARTESIAN_POINT('Origin',(41.,-73.08000002,-176.84995));
#169745=CARTESIAN_POINT('',(41.5,-70.08000002,-176.84995));
#169746=CARTESIAN_POINT('',(41.5,-73.08000002,-176.84995));
#169747=CARTESIAN_POINT('Origin',(41.,-70.08000002,-176.84995));
#169748=CARTESIAN_POINT('Origin',(41.,-70.08000002,-174.34995));
#169749=CARTESIAN_POINT('',(41.5,-72.58000002,-174.34995));
#169750=CARTESIAN_POINT('Origin',(41.,-72.58000002,-174.34995));
#169751=CARTESIAN_POINT('Origin',(41.5,-70.08000002,-174.34995));
#169752=CARTESIAN_POINT('Origin',(41.,-72.58000002,-4.66002702801304E-15));
#169753=CARTESIAN_POINT('',(41.5,-72.58000002,-58.24995));
#169754=CARTESIAN_POINT('Origin',(41.,-72.58000002,-58.24995));
#169755=CARTESIAN_POINT('',(41.5,-72.58000002,-174.34995));
#169756=CARTESIAN_POINT('Ctrl Pts',(42.0000617764046,-58.6035812240174,
-60.6499500038163));
#169757=CARTESIAN_POINT('Ctrl Pts',(41.5,-58.6035812240175,-60.6498882197787));
#169758=CARTESIAN_POINT('Ctrl Pts',(41.5,-58.6035812240174,-61.14995));
#169759=CARTESIAN_POINT('Ctrl Pts',(41.9298643117028,-58.4475344566847,
-60.6499412757882));
#169760=CARTESIAN_POINT('Ctrl Pts',(41.4999999999957,-58.4568531764755,
-60.7159032420905));
#169761=CARTESIAN_POINT('Ctrl Pts',(41.5,-58.4156885491981,-61.1499499554112));
#169762=CARTESIAN_POINT('Ctrl Pts',(41.8681695534325,-58.2705723212611,
-60.6499357694868));
#169763=CARTESIAN_POINT('Ctrl Pts',(41.5000000000007,-58.2676804549562,
-60.7523419094271));
#169764=CARTESIAN_POINT('Ctrl Pts',(41.5,-58.2277855029442,-61.1325395579243));
#169765=CARTESIAN_POINT('Ctrl Pts',(41.7820591277972,-57.8880263314595,
-60.6499295039941));
#169766=CARTESIAN_POINT('Ctrl Pts',(41.4999999999994,-57.8827900893775,
-60.7882832533183));
#169767=CARTESIAN_POINT('Ctrl Pts',(41.5,-57.8520667952968,-61.1008454187365));
#169768=CARTESIAN_POINT('Ctrl Pts',(41.7580490411453,-57.6823964313119,
-60.6499285241464));
#169769=CARTESIAN_POINT('Ctrl Pts',(41.5000000000007,-57.6764631965609,
-60.7926167355675));
#169770=CARTESIAN_POINT('Ctrl Pts',(41.5,-57.6641810084401,-61.0874868365943));
#169771=CARTESIAN_POINT('Ctrl Pts',(41.7579337455089,-57.270046180586,-60.6499285183491));
#169772=CARTESIAN_POINT('Ctrl Pts',(41.4999999999994,-57.2759508310879,
-60.7926435723737));
#169773=CARTESIAN_POINT('Ctrl Pts',(41.5,-57.2881262594113,-61.0874286718719));
#169774=CARTESIAN_POINT('Ctrl Pts',(41.7818539242553,-57.0640562802561,
-60.6499294916166));
#169775=CARTESIAN_POINT('Ctrl Pts',(41.5,-57.0692704467339,-60.7883470172518));
#169776=CARTESIAN_POINT('Ctrl Pts',(41.5,-57.0999570266671,-61.1007545617424));
#169777=CARTESIAN_POINT('Ctrl Pts',(41.8680165447744,-56.6807474451004,
-60.6499357558287));
#169778=CARTESIAN_POINT('Ctrl Pts',(41.5,-56.6836417097814,-60.7524277281085));
#169779=CARTESIAN_POINT('Ctrl Pts',(41.5,-56.7235644715484,-61.1324985063765));
#169780=CARTESIAN_POINT('Ctrl Pts',(41.9298158029953,-56.5034783375499,
-60.6499412695179));
#169781=CARTESIAN_POINT('Ctrl Pts',(41.5000000000006,-56.4941497059427,
-60.7159472955962));
#169782=CARTESIAN_POINT('Ctrl Pts',(41.5,-56.5353526996978,-61.1499499536044));
#169783=CARTESIAN_POINT('Ctrl Pts',(42.0000617764046,-56.3473237326805,
-60.6499500038163));
#169784=CARTESIAN_POINT('Ctrl Pts',(41.5,-56.3473237326805,-60.6498882197787));
#169785=CARTESIAN_POINT('Ctrl Pts',(41.5,-56.3473237326805,-61.14995));
#169786=CARTESIAN_POINT('',(42.,-58.6035812240174,-60.64995));
#169787=CARTESIAN_POINT('',(41.5,-58.6035812240174,-61.14995));
#169788=CARTESIAN_POINT('Origin',(42.,-58.6035812240174,-61.14995));
#169789=CARTESIAN_POINT('',(41.5,-56.3473237326805,-61.14995));
#169790=CARTESIAN_POINT('Ctrl Pts',(41.5,-56.3473237326805,-61.14995));
#169791=CARTESIAN_POINT('Ctrl Pts',(41.5,-56.4247882486864,-61.1499499808859));
#169792=CARTESIAN_POINT('Ctrl Pts',(41.5,-56.5020743317104,-61.146992865599));
#169793=CARTESIAN_POINT('Ctrl Pts',(41.5,-56.5792618257267,-61.1424262748502));
#169794=CARTESIAN_POINT('Ctrl Pts',(41.5,-56.6823474618059,-61.1363274900916));
#169795=CARTESIAN_POINT('Ctrl Pts',(41.5,-56.7852572696793,-61.1273561280415));
#169796=CARTESIAN_POINT('Ctrl Pts',(41.5000000000002,-56.8881825068221,
-61.1186215077307));
#169797=CARTESIAN_POINT('Ctrl Pts',(41.5000000000002,-56.8960417889422,
-61.1179545396756));
#169798=CARTESIAN_POINT('Ctrl Pts',(41.5000000000002,-56.9039011612641,
-61.1172889307083));
#169799=CARTESIAN_POINT('Ctrl Pts',(41.5000000000002,-56.9117607090172,
-61.1166260587005));
#169800=CARTESIAN_POINT('Ctrl Pts',(41.5000000000002,-56.9118309970963,
-61.116620130624));
#169801=CARTESIAN_POINT('Ctrl Pts',(41.5000000000002,-56.9119012851879,
-61.1166142029013));
#169802=CARTESIAN_POINT('Ctrl Pts',(41.5000000000002,-56.9119715732919,
-61.1166082755328));
#169803=CARTESIAN_POINT('Ctrl Pts',(41.5000000000007,-57.0997257526663,
-61.1007750386643));
#169804=CARTESIAN_POINT('Ctrl Pts',(41.4999999999977,-57.2880101287523,
-61.0874286525006));
#169805=CARTESIAN_POINT('Ctrl Pts',(41.5000000000023,-57.4761536341596,
-61.0874562423818));
#169806=CARTESIAN_POINT('Ctrl Pts',(41.5000000000023,-57.476328431569,-61.0874562680146));
#169807=CARTESIAN_POINT('Ctrl Pts',(41.5000000000023,-57.4765032288573,
-61.087456305165));
#169808=CARTESIAN_POINT('Ctrl Pts',(41.5000000000023,-57.4766780260241,
-61.0874563538243));
#169809=CARTESIAN_POINT('Ctrl Pts',(41.500000000005,-57.5875579724867,-61.0874872201067));
#169810=CARTESIAN_POINT('Ctrl Pts',(41.5000000000027,-57.6982145368478,
-61.092146664679));
#169811=CARTESIAN_POINT('Ctrl Pts',(41.5000000000012,-57.8087551935517,
-61.0991963488612));
#169812=CARTESIAN_POINT('Ctrl Pts',(41.5000000000001,-57.8858564168504,
-61.1041134471535));
#169813=CARTESIAN_POINT('Ctrl Pts',(41.5,-57.9629012529644,-61.1101948863674));
#169814=CARTESIAN_POINT('Ctrl Pts',(41.5,-58.039926161923,-61.1166923365635));
#169815=CARTESIAN_POINT('Ctrl Pts',(41.5,-58.0400259760021,-61.1167007563983));
#169816=CARTESIAN_POINT('Ctrl Pts',(41.5,-58.0401257900677,-61.1167091766712));
#169817=CARTESIAN_POINT('Ctrl Pts',(41.5,-58.0402256041196,-61.1167175973794));
#169818=CARTESIAN_POINT('Ctrl Pts',(41.5,-58.1358345616343,-61.1247835471794));
#169819=CARTESIAN_POINT('Ctrl Pts',(41.5,-58.2314235934534,-61.1332503625509));
#169820=CARTESIAN_POINT('Ctrl Pts',(41.5,-58.3271142909743,-61.1396237955238));
#169821=CARTESIAN_POINT('Ctrl Pts',(41.5,-58.4115316341054,-61.1452463721392));
#169822=CARTESIAN_POINT('Ctrl Pts',(41.5,-58.4960281098057,-61.1492419515511));
#169823=CARTESIAN_POINT('Ctrl Pts',(41.5,-58.5806871719383,-61.1498651031255));
#169824=CARTESIAN_POINT('Ctrl Pts',(41.5,-58.5883171817128,-61.149921265484));
#169825=CARTESIAN_POINT('Ctrl Pts',(41.5,-58.5959485120592,-61.1499499981887));
#169826=CARTESIAN_POINT('Ctrl Pts',(41.5,-58.6035812240174,-61.14995));
#169827=CARTESIAN_POINT('Origin',(42.,-56.3473237326805,-61.14995));
#169828=CARTESIAN_POINT('Ctrl Pts',(42.,-58.6035812240174,-60.64995));
#169829=CARTESIAN_POINT('Ctrl Pts',(41.9586127577212,-58.5115728992453,
-60.64995));
#169830=CARTESIAN_POINT('Ctrl Pts',(41.9223200866005,-58.4173567491328,
-60.6499639595534));
#169831=CARTESIAN_POINT('Ctrl Pts',(41.8579031946498,-58.2180944893025,
-60.6499671932779));
#169832=CARTESIAN_POINT('Ctrl Pts',(41.8306620008004,-58.1129431414189,
-60.6499312309338));
#169833=CARTESIAN_POINT('Ctrl Pts',(41.7951274186657,-57.9323775711288,
-60.6499828894707));
#169834=CARTESIAN_POINT('Ctrl Pts',(41.7836058362703,-57.8577298063973,
-60.6500200799918));
#169835=CARTESIAN_POINT('Ctrl Pts',(41.763699988371,-57.6806798505208,-60.6500271654877));
#169836=CARTESIAN_POINT('Ctrl Pts',(41.7579524619679,-57.578105462568,-60.6499494618776));
#169837=CARTESIAN_POINT('Ctrl Pts',(41.7579524619679,-57.3728595819392,
-60.6499505378071));
#169838=CARTESIAN_POINT('Ctrl Pts',(41.7636932451376,-57.2703453579393,
-60.6500300767565));
#169839=CARTESIAN_POINT('Ctrl Pts',(41.7835828980495,-57.0933348984408,
-60.6500220919564));
#169840=CARTESIAN_POINT('Ctrl Pts',(41.7951032511139,-57.0186677636549,
-60.6499835586185));
#169841=CARTESIAN_POINT('Ctrl Pts',(41.8306429216694,-56.838033533205,-60.6499306306421));
#169842=CARTESIAN_POINT('Ctrl Pts',(41.857894634129,-56.7328337987607,-60.6499676698703));
#169843=CARTESIAN_POINT('Ctrl Pts',(41.9223259722372,-56.5335329279257,
-60.6499642647307));
#169844=CARTESIAN_POINT('Ctrl Pts',(41.9586161144828,-56.4393245950077,
-60.64995));
#169845=CARTESIAN_POINT('Ctrl Pts',(42.,-56.3473237326805,-60.64995));
#169846=CARTESIAN_POINT('Origin',(42.,-12.9675000200281,-61.14995));
#169847=CARTESIAN_POINT('',(41.5,-73.08000002,-61.14995));
#169848=CARTESIAN_POINT('Origin',(42.5,-55.58000002,-177.34995));
#169849=CARTESIAN_POINT('',(41.5,-55.58000002,-60.64995));
#169850=CARTESIAN_POINT('',(42.5,-54.58000002,-171.64995));
#169851=CARTESIAN_POINT('Origin',(42.,-73.08000002,-171.14995));
#169852=CARTESIAN_POINT('',(41.5,-56.3473237326807,-171.14995));
#169853=CARTESIAN_POINT('',(42.,-56.3473237326807,-171.64995));
#169854=CARTESIAN_POINT('Origin',(42.,-56.3473237326807,-171.14995));
#169855=CARTESIAN_POINT('',(42.,-62.3323045260081,-171.64995));
#169856=CARTESIAN_POINT('',(41.5,-55.58000002,-171.14995));
#169857=CARTESIAN_POINT('Origin',(41.,-70.08000002,-58.24995));
#169858=CARTESIAN_POINT('',(41.5,-70.08000002,-55.74995));
#169859=CARTESIAN_POINT('',(41.,-70.08000002,-55.24995));
#169860=CARTESIAN_POINT('Origin',(41.,-70.08000002,-55.74995));
#169861=CARTESIAN_POINT('Origin',(41.,-70.08000002,-58.24995));
#169862=CARTESIAN_POINT('Origin',(41.5,-70.08000002,-58.24995));
#169863=CARTESIAN_POINT('Origin',(-3.3975957231091E-14,-70.08000002,-58.24995));
#169864=CARTESIAN_POINT('',(40.5,-70.08000002,-55.24995));
#169865=CARTESIAN_POINT('',(41.5,-70.08000002,-55.24995));
#169866=CARTESIAN_POINT('Origin',(40.5,-70.08000002,-58.24995));
#169867=CARTESIAN_POINT('Origin',(39.5,67.7009572055632,-171.14995));
#169868=CARTESIAN_POINT('',(40.,-56.978215522411,-171.14995));
#169869=CARTESIAN_POINT('Origin',(39.5,-56.978215522411,-171.14995));
#169870=CARTESIAN_POINT('',(40.,-62.6133861954129,-171.14995));
#169871=CARTESIAN_POINT('Origin',(39.5,-62.6133861954129,-171.14995));
#169872=CARTESIAN_POINT('',(40.,-62.5431157780617,-171.14995));
#169873=CARTESIAN_POINT('Ctrl Pts',(39.5,-56.978215522411,-171.64995));
#169874=CARTESIAN_POINT('Ctrl Pts',(40.,-56.9782155224109,-171.64995));
#169875=CARTESIAN_POINT('Ctrl Pts',(40.,-56.978215522411,-171.14995));
#169876=CARTESIAN_POINT('Ctrl Pts',(39.4660557514084,-56.8721092179034,
-171.64995));
#169877=CARTESIAN_POINT('Ctrl Pts',(40.,-56.8683451300554,-171.685098426659));
#169878=CARTESIAN_POINT('Ctrl Pts',(40.,-56.9099188320733,-171.149949989769));
#169879=CARTESIAN_POINT('Ctrl Pts',(39.4324273161011,-56.7672721138937,
-171.634782634301));
#169880=CARTESIAN_POINT('Ctrl Pts',(40.0000000000047,-56.7549311731639,
-171.710009011284));
#169881=CARTESIAN_POINT('Ctrl Pts',(40.,-56.8423993478631,-171.142369716128));
#169882=CARTESIAN_POINT('Ctrl Pts',(39.399271366643,-56.6641713142698,-171.60362375617));
#169883=CARTESIAN_POINT('Ctrl Pts',(40.,-56.6359876224365,-171.723920704752));
#169884=CARTESIAN_POINT('Ctrl Pts',(40.,-56.7758867300387,-171.126786878085));
#169885=CARTESIAN_POINT('',(40.,-56.7758867300388,-171.126786878085));
#169886=CARTESIAN_POINT('Origin',(39.5,-56.7758867300388,-171.126786878085));
#169887=CARTESIAN_POINT('Ctrl Pts',(40.,-56.7758867300388,-171.126786878085));
#169888=CARTESIAN_POINT('Ctrl Pts',(40.,-56.8424288281835,-171.142376649979));
#169889=CARTESIAN_POINT('Ctrl Pts',(40.,-56.909888666977,-171.14995));
#169890=CARTESIAN_POINT('Ctrl Pts',(40.,-56.978215522411,-171.14995));
#169891=CARTESIAN_POINT('Ctrl Pts',(40.,-56.3715344108516,-170.85018387548));
#169892=CARTESIAN_POINT('Ctrl Pts',(39.9999999999999,-55.5316163075193,
-171.321942247435));
#169893=CARTESIAN_POINT('Ctrl Pts',(39.2122207971108,-56.0150382320575,
-171.05041775096));
#169894=CARTESIAN_POINT('Ctrl Pts',(40.,-56.4127345596313,-170.923536275602));
#169895=CARTESIAN_POINT('Ctrl Pts',(40.0000000000016,-55.7019737694774,
-171.520946951432));
#169896=CARTESIAN_POINT('Ctrl Pts',(39.2305303132587,-56.0826793050571,
-171.197160563313));
#169897=CARTESIAN_POINT('Ctrl Pts',(40.,-56.4743979142815,-170.984396086855));
#169898=CARTESIAN_POINT('Ctrl Pts',(40.0000000000015,-55.9148019306841,
-171.629811017638));
#169899=CARTESIAN_POINT('Ctrl Pts',(39.2581734308863,-56.1834313742016,
-171.318842218969));
#169900=CARTESIAN_POINT('Ctrl Pts',(40.,-56.6150166715838,-171.07608877299));
#169901=CARTESIAN_POINT('Ctrl Pts',(39.9999999999985,-56.2996107654989,
-171.733927689933));
#169902=CARTESIAN_POINT('Ctrl Pts',(39.3228477027581,-56.4100322256565,
-171.502227500722));
#169903=CARTESIAN_POINT('Ctrl Pts',(40.,-56.6951614830789,-171.107874245193));
#169904=CARTESIAN_POINT('Ctrl Pts',(39.9999999999952,-56.4773256662664,
-171.740119136472));
#169905=CARTESIAN_POINT('Ctrl Pts',(39.3604560080182,-56.5377771955238,
-171.565812105304));
#169906=CARTESIAN_POINT('Ctrl Pts',(40.,-56.7758867300388,-171.126786878085));
#169907=CARTESIAN_POINT('Ctrl Pts',(40.,-56.6359876224367,-171.723920704753));
#169908=CARTESIAN_POINT('Ctrl Pts',(39.399271366643,-56.6641713142699,-171.60362375617));
#169909=CARTESIAN_POINT('',(40.,-56.3715344108516,-170.85018387548));
#169910=CARTESIAN_POINT('Origin',(39.5,-56.3715344108516,-170.85018387548));
#169911=CARTESIAN_POINT('Ctrl Pts',(40.,-56.3715344108516,-170.85018387548));
#169912=CARTESIAN_POINT('Ctrl Pts',(40.,-56.3837583326097,-170.871947332768));
#169913=CARTESIAN_POINT('Ctrl Pts',(40.,-56.3977040563911,-170.892479579619));
#169914=CARTESIAN_POINT('Ctrl Pts',(39.9999999999999,-56.4130583083892,
-170.911803741317));
#169915=CARTESIAN_POINT('Ctrl Pts',(39.9999999999997,-56.4292409786972,
-170.93217051254));
#169916=CARTESIAN_POINT('Ctrl Pts',(39.9999999999994,-56.4469891868553,
-170.951195798844));
#169917=CARTESIAN_POINT('Ctrl Pts',(39.9999999999991,-56.4659895184394,
-170.968879578562));
#169918=CARTESIAN_POINT('Ctrl Pts',(39.9999999999989,-56.4862759122394,
-170.987760307967));
#169919=CARTESIAN_POINT('Ctrl Pts',(39.9999999999988,-56.5079910115911,
-171.005112575639));
#169920=CARTESIAN_POINT('Ctrl Pts',(39.9999999999991,-56.5307948409885,
-171.020896071163));
#169921=CARTESIAN_POINT('Ctrl Pts',(39.9999999999992,-56.5352406042452,
-171.023973172086));
#169922=CARTESIAN_POINT('Ctrl Pts',(39.9999999999993,-56.5397278285598,
-171.026990509393));
#169923=CARTESIAN_POINT('Ctrl Pts',(39.9999999999994,-56.5442540887154,
-171.029947579459));
#169924=CARTESIAN_POINT('Ctrl Pts',(39.9999999999994,-56.5444049748233,
-171.030046155496));
#169925=CARTESIAN_POINT('Ctrl Pts',(39.9999999999994,-56.5445558983641,
-171.030144660686));
#169926=CARTESIAN_POINT('Ctrl Pts',(39.9999999999994,-56.5447068592425,
-171.030243095025));
#169927=CARTESIAN_POINT('Ctrl Pts',(39.9999999999998,-56.5677583970533,
-171.045273895852));
#169928=CARTESIAN_POINT('Ctrl Pts',(39.9999999999999,-56.5918056322569,
-171.058759052615));
#169929=CARTESIAN_POINT('Ctrl Pts',(40.,-56.616614889125,-171.070798762234));
#169930=CARTESIAN_POINT('Ctrl Pts',(40.,-56.6425070267789,-171.083363984176));
#169931=CARTESIAN_POINT('Ctrl Pts',(40.,-56.6692310020633,-171.094354961296));
#169932=CARTESIAN_POINT('Ctrl Pts',(40.,-56.6965412231968,-171.103832593435));
#169933=CARTESIAN_POINT('Ctrl Pts',(40.,-56.7225306079875,-171.112851847704));
#169934=CARTESIAN_POINT('Ctrl Pts',(40.,-56.7490526547637,-171.120500083882));
#169935=CARTESIAN_POINT('Ctrl Pts',(40.,-56.7758867300388,-171.126786878085));
#169936=CARTESIAN_POINT('Ctrl Pts',(39.2122207971107,-56.0150382320573,
-171.05041775096));
#169937=CARTESIAN_POINT('Ctrl Pts',(40.,-55.5316163075182,-171.321942247434));
#169938=CARTESIAN_POINT('Ctrl Pts',(40.,-56.3715344108516,-170.85018387548));
#169939=CARTESIAN_POINT('Ctrl Pts',(39.2341040930243,-55.7557644506258,
-170.620257995618));
#169940=CARTESIAN_POINT('Ctrl Pts',(39.999999999956,-55.3341015490071,-170.847929211526));
#169941=CARTESIAN_POINT('Ctrl Pts',(40.,-56.1381771304993,-170.434714809241));
#169942=CARTESIAN_POINT('Ctrl Pts',(39.2567881498609,-55.5425920931993,
-170.174365095598));
#169943=CARTESIAN_POINT('Ctrl Pts',(39.9999999999967,-55.1686346470297,
-170.352236872778));
#169944=CARTESIAN_POINT('Ctrl Pts',(40.,-55.946332886798,-170.004198915545));
#169945=CARTESIAN_POINT('Ctrl Pts',(39.3033074404025,-55.1837352900438,
-169.25987708718));
#169946=CARTESIAN_POINT('Ctrl Pts',(40.0000000000031,-54.9062023418216,
-169.365343244152));
#169947=CARTESIAN_POINT('Ctrl Pts',(40.,-55.6233617621208,-169.121472747772));
#169948=CARTESIAN_POINT('Ctrl Pts',(39.3271543017018,-55.0384654852052,
-168.791053495007));
#169949=CARTESIAN_POINT('Ctrl Pts',(39.9999999999966,-54.803396468199,-168.870754981701));
#169950=CARTESIAN_POINT('Ctrl Pts',(40.,-55.4926189390281,-168.669060842998));
#169951=CARTESIAN_POINT('Ctrl Pts',(39.3758587707466,-54.8068569180214,
-167.833341194373));
#169952=CARTESIAN_POINT('Ctrl Pts',(40.0000000000032,-54.6536169628087,
-167.876849546978));
#169953=CARTESIAN_POINT('Ctrl Pts',(40.,-55.2841712278759,-167.745175405929));
#169954=CARTESIAN_POINT('Ctrl Pts',(39.4005707712209,-54.7215461590296,
-167.347314197405));
#169955=CARTESIAN_POINT('Ctrl Pts',(39.9999999999983,-54.6033362561509,
-167.378205061485));
#169956=CARTESIAN_POINT('Ctrl Pts',(40.,-55.2073915453443,-167.276463616742));
#169957=CARTESIAN_POINT('Ctrl Pts',(39.4500853482271,-54.6083104675451,
-166.373147921324));
#169958=CARTESIAN_POINT('Ctrl Pts',(40.0000000000016,-54.5553362422517,
-166.389752651669));
#169959=CARTESIAN_POINT('Ctrl Pts',(40.,-55.1054794225729,-166.337325121725));
#169960=CARTESIAN_POINT('Ctrl Pts',(39.4749775493875,-54.58000002,-165.883246469104));
#169961=CARTESIAN_POINT('Ctrl Pts',(40.,-54.5543340703016,-165.895917381598));
#169962=CARTESIAN_POINT('Ctrl Pts',(40.,-55.0800000204413,-165.865198337359));
#169963=CARTESIAN_POINT('Ctrl Pts',(39.5,-54.58000002,-165.390538702986));
#169964=CARTESIAN_POINT('Ctrl Pts',(40.,-54.58000002,-165.390538702985));
#169965=CARTESIAN_POINT('Ctrl Pts',(40.,-55.08000002,-165.390538702986));
#169966=CARTESIAN_POINT('',(40.,-55.08000002,-165.390538702986));
#169967=CARTESIAN_POINT('Origin',(39.5,-55.08000002,-165.390538702986));
#169968=CARTESIAN_POINT('Ctrl Pts',(40.,-55.08000002,-165.390538702986));
#169969=CARTESIAN_POINT('Ctrl Pts',(40.,-55.08000002,-165.865206657822));
#169970=CARTESIAN_POINT('Ctrl Pts',(40.,-55.1054794225748,-166.33732512172));
#169971=CARTESIAN_POINT('Ctrl Pts',(40.,-55.1564354838472,-166.806894369245));
#169972=CARTESIAN_POINT('Ctrl Pts',(40.,-55.2073915451197,-167.27646361677));
#169973=CARTESIAN_POINT('Ctrl Pts',(40.,-55.2841712278673,-167.745175405874));
#169974=CARTESIAN_POINT('Ctrl Pts',(40.,-55.3883950832632,-168.207118124506));
#169975=CARTESIAN_POINT('Ctrl Pts',(40.,-55.4926189386592,-168.669060843138));
#169976=CARTESIAN_POINT('Ctrl Pts',(40.,-55.6233617621227,-169.121472747749));
#169977=CARTESIAN_POINT('Ctrl Pts',(40.,-55.7848473238897,-169.562835831867));
#169978=CARTESIAN_POINT('Ctrl Pts',(40.,-55.9143897222853,-169.916893692237));
#169979=CARTESIAN_POINT('Ctrl Pts',(40.,-56.0634514912202,-170.263936360661));
#169980=CARTESIAN_POINT('Ctrl Pts',(40.,-56.2378305483017,-170.601880104207));
#169981=CARTESIAN_POINT('Ctrl Pts',(40.,-56.280829742217,-170.685211834545));
#169982=CARTESIAN_POINT('Ctrl Pts',(40.,-56.325368553705,-170.767990232551));
#169983=CARTESIAN_POINT('Ctrl Pts',(40.,-56.3715344108516,-170.85018387548));
#169984=CARTESIAN_POINT('Origin',(39.5,-55.08000002,-55.24995));
#169985=CARTESIAN_POINT('',(40.,-55.08000002,-66.6681042685293));
#169986=CARTESIAN_POINT('',(40.,-55.08000002,-166.086292363451));
#169987=CARTESIAN_POINT('Origin',(39.5,-55.08000002,-66.6681042685293));
#169988=CARTESIAN_POINT('Ctrl Pts',(39.5,-54.58000002,-66.6681042685296));
#169989=CARTESIAN_POINT('Ctrl Pts',(39.9999999999999,-54.5800000200005,
-66.6681042685296));
#169990=CARTESIAN_POINT('Ctrl Pts',(40.,-55.08000002,-66.6681042685293));
#169991=CARTESIAN_POINT('Ctrl Pts',(39.4524759569592,-54.5800000199993,
-65.7323260169345));
#169992=CARTESIAN_POINT('Ctrl Pts',(40.000000000023,-54.5300790303385,-65.6851286065597));
#169993=CARTESIAN_POINT('Ctrl Pts',(40.,-55.0800000210321,-65.7666038778627));
#169994=CARTESIAN_POINT('Ctrl Pts',(39.4055862633018,-54.6797418208431,
-64.8099001089231));
#169995=CARTESIAN_POINT('Ctrl Pts',(40.,-54.5798306201335,-64.744699921287));
#169996=CARTESIAN_POINT('Ctrl Pts',(40.,-55.1697676396346,-64.8773517277477));
#169997=CARTESIAN_POINT('Ctrl Pts',(39.336341776171,-54.9893440187367,-63.4482326198876));
#169998=CARTESIAN_POINT('Ctrl Pts',(40.,-54.7700293023446,-63.3785482937886));
#169999=CARTESIAN_POINT('Ctrl Pts',(40.,-55.4484096194251,-63.5638700072085));
#170000=CARTESIAN_POINT('Ctrl Pts',(39.3133286552319,-55.1206346051679,
-62.9957806797004));
#170001=CARTESIAN_POINT('Ctrl Pts',(40.,-54.8613740727702,-62.9031901152049));
#170002=CARTESIAN_POINT('Ctrl Pts',(40.,-55.5665711459207,-63.1272943707367));
#170003=CARTESIAN_POINT('Ctrl Pts',(39.2684369452391,-55.4440915465439,
-62.113263414855));
#170004=CARTESIAN_POINT('Ctrl Pts',(40.,-55.0944248813133,-61.958211698159));
#170005=CARTESIAN_POINT('Ctrl Pts',(40.,-55.8576823946199,-62.2755058384848));
#170006=CARTESIAN_POINT('Ctrl Pts',(39.2465526403215,-55.635643675915,-61.6830846593873));
#170007=CARTESIAN_POINT('Ctrl Pts',(39.9999999999954,-55.2406041652953,
-61.4857700511268));
#170008=CARTESIAN_POINT('Ctrl Pts',(40.,-56.0300729172808,-61.8601972461309));
#170009=CARTESIAN_POINT('Ctrl Pts',(39.2253966502057,-55.8655297208508,
-61.2672223984388));
#170010=CARTESIAN_POINT('Ctrl Pts',(39.9999999999999,-55.4129915017042,
-61.0340816633138));
#170011=CARTESIAN_POINT('Ctrl Pts',(40.,-56.2369767507657,-61.4585861992193));
#170012=CARTESIAN_POINT('',(40.,-56.2369767507657,-61.4585861992193));
#170013=CARTESIAN_POINT('Ctrl Pts',(40.,-56.2369767507657,-61.4585861992193));
#170014=CARTESIAN_POINT('Ctrl Pts',(40.,-56.0300621110256,-61.860218211459));
#170015=CARTESIAN_POINT('Ctrl Pts',(40.,-55.8576823937473,-62.2755058381188));
#170016=CARTESIAN_POINT('Ctrl Pts',(40.,-55.7121267698271,-62.7014001044593));
#170017=CARTESIAN_POINT('Ctrl Pts',(40.,-55.566571145907,-63.1272943707998));
#170018=CARTESIAN_POINT('Ctrl Pts',(40.,-55.4484096188021,-63.563870007102));
#170019=CARTESIAN_POINT('Ctrl Pts',(40.,-55.355528959088,-64.0016972473019));
#170020=CARTESIAN_POINT('Ctrl Pts',(40.,-55.2432744366405,-64.5308503337935));
#170021=CARTESIAN_POINT('Ctrl Pts',(40.,-55.1660815895368,-65.0649117752156));
#170022=CARTESIAN_POINT('Ctrl Pts',(40.,-55.1225595401114,-65.6036868919934));
#170023=CARTESIAN_POINT('Ctrl Pts',(40.,-55.0940603190417,-65.9564890086819));
#170024=CARTESIAN_POINT('Ctrl Pts',(40.,-55.0800000199998,-66.3113124768404));
#170025=CARTESIAN_POINT('Ctrl Pts',(40.,-55.08000002,-66.6681042685293));
#170026=CARTESIAN_POINT('Origin',(39.5,-56.2369767507657,-61.4585861992193));
#170027=CARTESIAN_POINT('Ctrl Pts',(39.2250415490953,-55.8657373699498,
-61.2673293760636));
#170028=CARTESIAN_POINT('Ctrl Pts',(40.,-55.4121526631459,-61.0336495065824));
#170029=CARTESIAN_POINT('Ctrl Pts',(40.,-56.2369767507698,-61.4585861992214));
#170030=CARTESIAN_POINT('Ctrl Pts',(39.2367912602697,-55.9110350177183,
-61.1625123459351));
#170031=CARTESIAN_POINT('Ctrl Pts',(39.9999999999999,-55.5203773908674,
-60.8902955679075));
#170032=CARTESIAN_POINT('Ctrl Pts',(40.,-56.2639883391117,-61.4061555156247));
#170033=CARTESIAN_POINT('Ctrl Pts',(39.2526254167108,-55.9715434068114,
-61.0715217947418));
#170034=CARTESIAN_POINT('Ctrl Pts',(40.0000000000002,-55.6518298350008,
-60.7886660066872));
#170035=CARTESIAN_POINT('Ctrl Pts',(40.,-56.3001438773882,-61.3606672793622));
#170036=CARTESIAN_POINT('Ctrl Pts',(39.2913939492583,-56.1161109922439,
-60.9128192370848));
#170037=CARTESIAN_POINT('Ctrl Pts',(39.9999999999997,-55.923525557992,-60.6494230275178));
#170038=CARTESIAN_POINT('Ctrl Pts',(40.,-56.3871674054812,-61.2813159675772));
#170039=CARTESIAN_POINT('Ctrl Pts',(39.3134274873215,-56.1967830839396,
-60.8489419701753));
#170040=CARTESIAN_POINT('Ctrl Pts',(40.0000000000002,-56.055303527311,-60.6118369663638));
#170041=CARTESIAN_POINT('Ctrl Pts',(40.,-56.4359944422203,-61.2493819347541));
#170042=CARTESIAN_POINT('Ctrl Pts',(39.3621229995535,-56.3701234141287,
-60.7467866067772));
#170043=CARTESIAN_POINT('Ctrl Pts',(39.9999999999998,-56.3052253871045,
-60.5760036964908));
#170044=CARTESIAN_POINT('Ctrl Pts',(40.,-56.5418574657904,-61.1983186977834));
#170045=CARTESIAN_POINT('Ctrl Pts',(39.3878798646771,-56.459572422833,-60.710431798962));
#170046=CARTESIAN_POINT('Ctrl Pts',(40.0000000000002,-56.4197432892716,
-60.5759049037901));
#170047=CARTESIAN_POINT('Ctrl Pts',(40.,-56.5969271200065,-61.1801504966336));
#170048=CARTESIAN_POINT('Ctrl Pts',(39.4420692078983,-56.6422525387301,
-60.6618822224814));
#170049=CARTESIAN_POINT('Ctrl Pts',(39.9999999999997,-56.6329760211049,
-60.5982183614686));
#170050=CARTESIAN_POINT('Ctrl Pts',(40.,-56.7105746147406,-61.1558957215692));
#170051=CARTESIAN_POINT('Ctrl Pts',(39.4706843681677,-56.7360270779361,
-60.6499699008789));
#170052=CARTESIAN_POINT('Ctrl Pts',(40.,-56.7332871432547,-60.6197584771857));
#170053=CARTESIAN_POINT('Ctrl Pts',(40.,-56.769502228095,-61.1499499952173));
#170054=CARTESIAN_POINT('Ctrl Pts',(39.4996584737974,-56.8280459100727,
-60.6499501166402));
#170055=CARTESIAN_POINT('Ctrl Pts',(40.,-56.8280459100727,-60.6496083570775));
#170056=CARTESIAN_POINT('Ctrl Pts',(40.,-56.8280459100727,-61.14995));
#170057=CARTESIAN_POINT('',(40.,-56.8280459100727,-61.14995));
#170058=CARTESIAN_POINT('Ctrl Pts',(40.,-56.8280459100727,-61.14995));
#170059=CARTESIAN_POINT('Ctrl Pts',(40.,-56.7775257469882,-61.1499499958728));
#170060=CARTESIAN_POINT('Ctrl Pts',(40.,-56.7268325166741,-61.15437366761));
#170061=CARTESIAN_POINT('Ctrl Pts',(40.,-56.6774814901229,-61.1633382145163));
#170062=CARTESIAN_POINT('Ctrl Pts',(40.,-56.6695344165968,-61.1647817896225));
#170063=CARTESIAN_POINT('Ctrl Pts',(40.,-56.6616221088455,-61.1663432172134));
#170064=CARTESIAN_POINT('Ctrl Pts',(40.,-56.6537508667182,-61.1680231060305));
#170065=CARTESIAN_POINT('Ctrl Pts',(40.,-56.6068413991698,-61.1780345741922));
#170066=CARTESIAN_POINT('Ctrl Pts',(40.,-56.5611509800564,-61.1921536886351));
#170067=CARTESIAN_POINT('Ctrl Pts',(40.,-56.5168370445334,-61.2111466189142));
#170068=CARTESIAN_POINT('Ctrl Pts',(40.,-56.5074712818004,-61.2151607800691));
#170069=CARTESIAN_POINT('Ctrl Pts',(40.,-56.4981670562378,-61.2193928254492));
#170070=CARTESIAN_POINT('Ctrl Pts',(40.,-56.4889259423713,-61.2238502921498));
#170071=CARTESIAN_POINT('Ctrl Pts',(40.,-56.4359851254178,-61.2493863835865));
#170072=CARTESIAN_POINT('Ctrl Pts',(40.,-56.3871673636495,-61.2813158980448));
#170073=CARTESIAN_POINT('Ctrl Pts',(40.,-56.3436555786936,-61.3209915546623));
#170074=CARTESIAN_POINT('Ctrl Pts',(40.,-56.3001590827628,-61.3606532701805));
#170075=CARTESIAN_POINT('Ctrl Pts',(40.,-56.2640024859216,-61.4061278501816));
#170076=CARTESIAN_POINT('Ctrl Pts',(40.,-56.2369767507657,-61.4585861992193));
#170077=CARTESIAN_POINT('',(39.4999994911522,-56.8280450701521,-60.6499500000002));
#170078=CARTESIAN_POINT('Origin',(39.5,-56.8280459100727,-61.14995));
#170079=CARTESIAN_POINT('Ctrl Pts',(39.2253966502054,-55.865529720851,-61.2672223984388));
#170080=CARTESIAN_POINT('Ctrl Pts',(39.234911163723,-55.9022177765805,-61.1823557659019));
#170081=CARTESIAN_POINT('Ctrl Pts',(39.2479974736944,-55.9538728824452,
-61.0971743824038));
#170082=CARTESIAN_POINT('Ctrl Pts',(39.2746238713045,-56.0536593475906,
-60.9796220178071));
#170083=CARTESIAN_POINT('Ctrl Pts',(39.2846341785973,-56.0905800623539,
-60.942170208689));
#170084=CARTESIAN_POINT('Ctrl Pts',(39.3012162205084,-56.1508612956915,
-60.8899544631596));
#170085=CARTESIAN_POINT('Ctrl Pts',(39.3070019925557,-56.1717675923896,
-60.8732084043496));
#170086=CARTESIAN_POINT('Ctrl Pts',(39.3160276366305,-56.2042376975661,
-60.8492301021309));
#170087=CARTESIAN_POINT('Ctrl Pts',(39.3206269620396,-56.220750075716,-60.8375258888386));
#170088=CARTESIAN_POINT('Ctrl Pts',(39.3253463010804,-56.2376553063615,
-60.8262748915364));
#170089=CARTESIAN_POINT('Ctrl Pts',(39.3285179752611,-56.2490100114614,
-60.8188775954966));
#170090=CARTESIAN_POINT('Ctrl Pts',(39.3303914962528,-56.2557130146439,
-60.8146171211701));
#170091=CARTESIAN_POINT('Ctrl Pts',(39.3424129108038,-56.2987074019437,
-60.7877930361237));
#170092=CARTESIAN_POINT('Ctrl Pts',(39.3542789664704,-56.340825775592,-60.7649606346162));
#170093=CARTESIAN_POINT('Ctrl Pts',(39.3739744074941,-56.4094606619384,
-60.7340965930491));
#170094=CARTESIAN_POINT('Ctrl Pts',(39.3808520215394,-56.4332428662801,
-60.7243742045393));
#170095=CARTESIAN_POINT('Ctrl Pts',(39.3916159549907,-56.4701691837868,
-60.7108731089427));
#170096=CARTESIAN_POINT('Ctrl Pts',(39.3971093785701,-56.4889450165438,
-60.704393079611));
#170097=CARTESIAN_POINT('Ctrl Pts',(39.4037042050758,-56.5113687814886,
-60.69735570514));
#170098=CARTESIAN_POINT('Ctrl Pts',(39.4065690926056,-56.5210866631315,
-60.6944567729941));
#170099=CARTESIAN_POINT('Ctrl Pts',(39.4084874292263,-56.5275887919521,
-60.692550727735));
#170100=CARTESIAN_POINT('Ctrl Pts',(39.4099873539432,-56.5326675243218,
-60.6910973649265));
#170101=CARTESIAN_POINT('Ctrl Pts',(39.4242087195643,-56.5807982407849,
-60.6774835249891));
#170102=CARTESIAN_POINT('Ctrl Pts',(39.4543205885197,-56.6829255755301,
-60.6499501150941));
#170103=CARTESIAN_POINT('Ctrl Pts',(39.4999997135809,-56.8280450001391,
-60.6499500000004));
#170104=CARTESIAN_POINT('Origin',(40.5,-70.08000002,-58.24995));
#170105=CARTESIAN_POINT('',(40.,-70.08000002,-55.74995));
#170106=CARTESIAN_POINT('Origin',(40.5,-70.08000002,-55.74995));
#170107=CARTESIAN_POINT('',(40.,-72.58000002,-58.24995));
#170108=CARTESIAN_POINT('Origin',(40.,-70.08000002,-58.24995));
#170109=CARTESIAN_POINT('Origin',(40.5,-72.58000002,-58.24995));
#170110=CARTESIAN_POINT('Origin',(40.5,-72.58000002,-55.24995));
#170111=CARTESIAN_POINT('',(40.,-72.58000002,-174.34995));
#170112=CARTESIAN_POINT('',(40.,-72.58000002,-58.24995));
#170113=CARTESIAN_POINT('Origin',(40.5,-72.58000002,-174.34995));
#170114=CARTESIAN_POINT('Origin',(40.5,-70.08000002,-174.34995));
#170115=CARTESIAN_POINT('',(40.,-70.08000002,-176.84995));
#170116=CARTESIAN_POINT('Origin',(40.,-70.08000002,-174.34995));
#170117=CARTESIAN_POINT('Origin',(40.5,-70.08000002,-176.84995));
#170118=CARTESIAN_POINT('Origin',(40.5,67.7009572055632,-176.84995));
#170119=CARTESIAN_POINT('',(40.,67.7009572055632,-176.84995));
#170120=CARTESIAN_POINT('Origin',(39.5,-64.1281275541909,-55.24995));
#170121=CARTESIAN_POINT('',(39.5,-63.6281275541908,-172.64995));
#170122=CARTESIAN_POINT('Origin',(39.5,-64.1281275541908,-172.64995));
#170123=CARTESIAN_POINT('',(39.43041344952,-63.63299351982,-171.64995));
#170124=CARTESIAN_POINT('',(40.,-64.1281275541908,-172.64995));
#170125=CARTESIAN_POINT('',(40.,-64.1281275541909,-55.24995));
#170126=CARTESIAN_POINT('Origin',(39.5,-64.1281275541908,-172.64995));
#170127=CARTESIAN_POINT('Ctrl Pts',(40.,-62.6131847515953,-171.149950013428));
#170128=CARTESIAN_POINT('Ctrl Pts',(40.,-62.6132505449146,-171.65003477338));
#170129=CARTESIAN_POINT('Ctrl Pts',(39.4999152383759,-62.6132505989472,
-171.649950001854));
#170130=CARTESIAN_POINT('Ctrl Pts',(40.,-62.8115669184518,-171.149923566191));
#170131=CARTESIAN_POINT('Ctrl Pts',(40.,-62.7480692875133,-171.659221103016));
#170132=CARTESIAN_POINT('Ctrl Pts',(39.4908008078197,-62.7467859681038,
-171.649930655763));
#170133=CARTESIAN_POINT('Ctrl Pts',(40.,-63.0098045293616,-171.188965548735));
#170134=CARTESIAN_POINT('Ctrl Pts',(40.,-62.8774949048455,-171.695281914067));
#170135=CARTESIAN_POINT('Ctrl Pts',(39.4816930631427,-62.8802250152049,
-171.675956808334));
#170136=CARTESIAN_POINT('Ctrl Pts',(40.,-63.3762386807026,-171.339270411997));
#170137=CARTESIAN_POINT('Ctrl Pts',(40.0000000000001,-63.1102859043402,
-171.81002165518));
#170138=CARTESIAN_POINT('Ctrl Pts',(39.4648578735174,-63.1268827917894,
-171.776157476855));
#170139=CARTESIAN_POINT('Ctrl Pts',(40.,-63.5442655393439,-171.450449746589));
#170140=CARTESIAN_POINT('Ctrl Pts',(40.000000000002,-63.2128473094945,-171.889069508911));
#170141=CARTESIAN_POINT('Ctrl Pts',(39.4571382160676,-63.2399874126731,
-171.850276197781));
#170142=CARTESIAN_POINT('Ctrl Pts',(40.,-63.8246746245531,-171.728129909852));
#170143=CARTESIAN_POINT('Ctrl Pts',(39.9999999999979,-63.3804806514191,
-172.075284894372));
#170144=CARTESIAN_POINT('Ctrl Pts',(39.4442554477382,-63.428740903488,-172.035396209826));
#170145=CARTESIAN_POINT('Ctrl Pts',(40.,-63.9369465821947,-171.894521542842));
#170146=CARTESIAN_POINT('Ctrl Pts',(40.,-63.4447415656143,-172.182240159753));
#170147=CARTESIAN_POINT('Ctrl Pts',(39.4390973897632,-63.5043156888,-172.14632470545));
#170148=CARTESIAN_POINT('Ctrl Pts',(40.,-64.0887285772422,-172.257389581842));
#170149=CARTESIAN_POINT('Ctrl Pts',(40.,-63.5311756375845,-172.409795949395));
#170150=CARTESIAN_POINT('Ctrl Pts',(39.4321241606571,-63.6064863141587,
-172.388239289312));
#170151=CARTESIAN_POINT('Ctrl Pts',(40.,-64.1281542477849,-172.453697958273));
#170152=CARTESIAN_POINT('Ctrl Pts',(40.,-63.5528414676591,-172.529747068593));
#170153=CARTESIAN_POINT('Ctrl Pts',(39.4303128569903,-63.6330254636236,
-172.519113452117));
#170154=CARTESIAN_POINT('Ctrl Pts',(40.,-64.1281275406312,-172.65014948338));
#170155=CARTESIAN_POINT('Ctrl Pts',(40.,-63.5528267611457,-172.650072180543));
#170156=CARTESIAN_POINT('Ctrl Pts',(39.4303140827877,-63.6330074860316,
-172.650082990804));
#170157=CARTESIAN_POINT('Ctrl Pts',(40.,-62.6133861954129,-171.14995));
#170158=CARTESIAN_POINT('Ctrl Pts',(40.,-62.8117011147884,-171.149950000016));
#170159=CARTESIAN_POINT('Ctrl Pts',(40.,-63.0098665547682,-171.18899099047));
#170160=CARTESIAN_POINT('Ctrl Pts',(40.,-63.3762386807026,-171.339270411997));
#170161=CARTESIAN_POINT('Ctrl Pts',(40.,-63.5442655393439,-171.450449746589));
#170162=CARTESIAN_POINT('Ctrl Pts',(40.,-63.8246746245531,-171.728129909852));
#170163=CARTESIAN_POINT('Ctrl Pts',(40.,-63.9369465821947,-171.894521542842));
#170164=CARTESIAN_POINT('Ctrl Pts',(40.,-64.0887028854776,-172.257328160063));
#170165=CARTESIAN_POINT('Ctrl Pts',(40.,-64.1281275541786,-172.453565067926));
#170166=CARTESIAN_POINT('Ctrl Pts',(40.,-64.1281275541908,-172.64995));
#170167=CARTESIAN_POINT('Origin',(0.,-12.9675000200281,-61.64995));
#170168=CARTESIAN_POINT('',(39.4379155619868,-56.882767417621,-60.64995));
#170169=CARTESIAN_POINT('Origin',(0.,-12.9675000200281,-60.64995));
#170170=CARTESIAN_POINT('Origin',(39.4379155619868,-56.882767417621,-61.64995));
#170171=CARTESIAN_POINT('Origin',(33.85,67.7009572055632,-61.14995));
#170172=CARTESIAN_POINT('',(33.85,-64.1339197616649,-60.64995));
#170173=CARTESIAN_POINT('',(33.85,-12.9675000200281,-60.64995));
#170174=CARTESIAN_POINT('',(33.35,-64.133919761665,-61.14995));
#170175=CARTESIAN_POINT('Origin',(33.85,-64.133919761665,-61.14995));
#170176=CARTESIAN_POINT('',(33.35,67.7009572055632,-61.14995));
#170177=CARTESIAN_POINT('Origin',(39.5,-12.9675000200281,-61.14995));
#170178=CARTESIAN_POINT('',(40.,-63.6396088127436,-61.14995));
#170179=CARTESIAN_POINT('',(40.,67.7009572055632,-61.14995));
#170180=CARTESIAN_POINT('',(39.5,-63.6396088127436,-60.64995));
#170181=CARTESIAN_POINT('Origin',(39.5,-63.6396088127436,-61.14995));
#170182=CARTESIAN_POINT('',(39.5,-12.9675000200281,-60.64995));
#170183=CARTESIAN_POINT('Ctrl Pts',(39.4379155619868,-56.882767417621,-60.64995));
#170184=CARTESIAN_POINT('Ctrl Pts',(39.0122500629964,-56.4087764892537,
-60.6499500000001));
#170185=CARTESIAN_POINT('Ctrl Pts',(38.8323560497301,-56.2084592670262,
-61.2273317382593));
#170186=CARTESIAN_POINT('Ctrl Pts',(39.5470561894999,-56.7847541538272,
-60.64995));
#170187=CARTESIAN_POINT('Ctrl Pts',(39.1308890120013,-56.2886813392436,
-60.64995));
#170188=CARTESIAN_POINT('Ctrl Pts',(38.9597499727218,-56.0859430057577,
-61.2402727589806));
#170189=CARTESIAN_POINT('Ctrl Pts',(39.6600993514669,-56.6929757051825,
-60.64995));
#170190=CARTESIAN_POINT('Ctrl Pts',(39.2535572856597,-56.1757390223779,
-60.64995));
#170191=CARTESIAN_POINT('Ctrl Pts',(39.0917129041016,-55.9712198429402,
-61.2536666704059));
#170192=CARTESIAN_POINT('Ctrl Pts',(39.7766890844069,-56.606882728875,-60.64995));
#170193=CARTESIAN_POINT('Ctrl Pts',(39.3796800351166,-56.0692409848678,
-60.64995));
#170194=CARTESIAN_POINT('Ctrl Pts',(39.2278317447683,-55.8636034060938,
-61.2674693219905));
#170195=CARTESIAN_POINT('Ctrl Pts',(39.4379155619868,-56.882767417621,-60.64995));
#170196=CARTESIAN_POINT('Ctrl Pts',(39.4584539679692,-56.8643229911399,
-60.64995));
#170197=CARTESIAN_POINT('Ctrl Pts',(39.4791489724441,-56.8460828416128,
-60.64995));
#170198=CARTESIAN_POINT('Ctrl Pts',(39.4999988314732,-56.8280445593217,
-60.64995));
#170199=CARTESIAN_POINT('Ctrl Pts',(40.4577925858907,10.61999998,-144.90822241383));
#170200=CARTESIAN_POINT('Ctrl Pts',(39.7432392475336,10.61999998,-145.291860254625));
#170201=CARTESIAN_POINT('Ctrl Pts',(40.064213984323,9.8954018152728,-145.1195315447));
#170202=CARTESIAN_POINT('Ctrl Pts',(42.7973905232547,10.61999998,-149.265893474329));
#170203=CARTESIAN_POINT('Ctrl Pts',(42.0569998298599,10.61999998,-149.560052788611));
#170204=CARTESIAN_POINT('Ctrl Pts',(42.3982233528881,9.90519935947367,-149.477207192598));
#170205=CARTESIAN_POINT('Ctrl Pts',(45.0988060523808,10.61999998,-153.643419067924));
#170206=CARTESIAN_POINT('Ctrl Pts',(44.3825306854435,10.6199999800261,-153.946076900384));
#170207=CARTESIAN_POINT('Ctrl Pts',(44.6952062210366,9.91377387366803,-153.854728198786));
#170208=CARTESIAN_POINT('Ctrl Pts',(49.6533413888222,10.61999998,-162.423562369795));
#170209=CARTESIAN_POINT('Ctrl Pts',(48.9599089008669,10.6199999799746,-162.709726895544));
#170210=CARTESIAN_POINT('Ctrl Pts',(49.2422260788803,9.92919580612355,-162.634871500674));
#170211=CARTESIAN_POINT('Ctrl Pts',(51.9061633492443,10.61999998,-166.826341244199));
#170212=CARTESIAN_POINT('Ctrl Pts',(51.2291869847762,10.6199999797401,-167.117625919029));
#170213=CARTESIAN_POINT('Ctrl Pts',(51.491975374397,9.936039246645,-167.037652347168));
#170214=CARTESIAN_POINT('Ctrl Pts',(54.1424378198232,10.61999998,-171.237717270032));
#170215=CARTESIAN_POINT('Ctrl Pts',(53.4956787755832,10.61999998,-171.565581122671));
#170216=CARTESIAN_POINT('Ctrl Pts',(53.7255998841352,9.94225131873298,-171.449026400902));
#170217=CARTESIAN_POINT('',(40.4577925858907,10.61999998,-144.90822241383));
#170218=CARTESIAN_POINT('Origin',(40.4577925858907,10.11999998,-144.90822241383));
#170219=CARTESIAN_POINT('',(54.1424378198232,10.61999998,-171.237717270032));
#170220=CARTESIAN_POINT('Origin',(54.1424378198232,10.11999998,-171.237717270032));
#170221=CARTESIAN_POINT('Ctrl Pts',(40.4577925858907,10.61999998,-144.90822241383));
#170222=CARTESIAN_POINT('Ctrl Pts',(42.7973924930771,10.61999998,-149.265897143292));
#170223=CARTESIAN_POINT('Ctrl Pts',(45.0988060523871,10.61999998,-153.643419067936));
#170224=CARTESIAN_POINT('Ctrl Pts',(47.3760737205892,10.61999998,-158.033490718866));
#170225=CARTESIAN_POINT('Ctrl Pts',(49.6533413887914,10.61999998,-162.423562369795));
#170226=CARTESIAN_POINT('Ctrl Pts',(51.9061626796858,10.61999998,-166.826339923461));
#170227=CARTESIAN_POINT('Ctrl Pts',(54.1424378198232,10.61999998,-171.237717270032));
#170228=CARTESIAN_POINT('Ctrl Pts',(40.1796955375735,9.88440567969849,-145.31549319889));
#170229=CARTESIAN_POINT('Ctrl Pts',(39.8393811074739,10.61999998,-145.511819782235));
#170230=CARTESIAN_POINT('Ctrl Pts',(40.5615971123268,10.61999998,-145.094901201173));
#170231=CARTESIAN_POINT('Ctrl Pts',(39.7529573682649,9.92251944743362,-144.614806037804));
#170232=CARTESIAN_POINT('Ctrl Pts',(39.502953749878,10.61999998,-144.775506187451));
#170233=CARTESIAN_POINT('Ctrl Pts',(40.1775148443164,10.61999998,-144.427612983545));
#170234=CARTESIAN_POINT('Ctrl Pts',(39.4582086878617,9.96279114543498,-143.870271315249));
#170235=CARTESIAN_POINT('Ctrl Pts',(39.2626189761704,10.61999998,-143.977483356653));
#170236=CARTESIAN_POINT('Ctrl Pts',(39.912296049423,10.61999998,-143.719512225762));
#170237=CARTESIAN_POINT('Ctrl Pts',(39.0709388975647,10.0461576545263,-142.315031435705));
#170238=CARTESIAN_POINT('Ctrl Pts',(38.9964277475896,10.61999998,-142.362517500096));
#170239=CARTESIAN_POINT('Ctrl Pts',(39.5638060942237,10.61999998,-142.242424394332));
#170240=CARTESIAN_POINT('Ctrl Pts',(38.9827638115546,10.0893227527421,-141.50278642521));
#170241=CARTESIAN_POINT('Ctrl Pts',(38.9510892610462,10.61999998,-141.53616355362));
#170242=CARTESIAN_POINT('Ctrl Pts',(39.4844701295021,10.61999998,-141.472057475813));
#170243=CARTESIAN_POINT('Ctrl Pts',(39.0027794749889,10.1314228667547,-140.701237361295));
#170244=CARTESIAN_POINT('Ctrl Pts',(39.0139531655019,10.61999998,-140.701380742148));
#170245=CARTESIAN_POINT('Ctrl Pts',(39.5025080143507,10.61999998,-140.713061620781));
#170246=CARTESIAN_POINT('',(39.5,10.61999998,-140.924467062102));
#170247=CARTESIAN_POINT('Origin',(39.5,10.11999998,-140.924467062102));
#170248=CARTESIAN_POINT('Ctrl Pts',(39.5,10.61999998,-140.924467062102));
#170249=CARTESIAN_POINT('Ctrl Pts',(39.5,10.61999998,-141.064641740712));
#170250=CARTESIAN_POINT('Ctrl Pts',(39.503286113677,10.619999980029,-141.204536867586));
#170251=CARTESIAN_POINT('Ctrl Pts',(39.5098002370266,10.6199999796907,-141.344151254401));
#170252=CARTESIAN_POINT('Ctrl Pts',(39.5163738758531,10.6199999793493,-141.485041210679));
#170253=CARTESIAN_POINT('Ctrl Pts',(39.5262347839853,10.6199999785395,-141.625645980312));
#170254=CARTESIAN_POINT('Ctrl Pts',(39.5393758471114,10.6199999780094,-141.765968909083));
#170255=CARTESIAN_POINT('Ctrl Pts',(39.5454296177964,10.6199999777652,-141.830612296339));
#170256=CARTESIAN_POINT('Ctrl Pts',(39.5521802385777,10.6199999776063,-141.895195868191));
#170257=CARTESIAN_POINT('Ctrl Pts',(39.5596307210412,10.6199999776383,-141.959719632822));
#170258=CARTESIAN_POINT('Ctrl Pts',(39.5766960195724,10.6199999777115,-142.107511042463));
#170259=CARTESIAN_POINT('Ctrl Pts',(39.5974615300858,10.6199999785835,-142.255205306997));
#170260=CARTESIAN_POINT('Ctrl Pts',(39.6219007996109,10.6199999791661,-142.402216894669));
#170261=CARTESIAN_POINT('Ctrl Pts',(39.6461342711754,10.6199999797438,-142.547990528609));
#170262=CARTESIAN_POINT('Ctrl Pts',(39.6739797737391,10.6199999799661,-142.693092202931));
#170263=CARTESIAN_POINT('Ctrl Pts',(39.7053613936648,10.6199999799929,-142.836960501111));
#170264=CARTESIAN_POINT('Ctrl Pts',(39.7158636782067,10.6199999800019,-142.885107977489));
#170265=CARTESIAN_POINT('Ctrl Pts',(39.7267615964733,10.61999998,-142.933117442989));
#170266=CARTESIAN_POINT('Ctrl Pts',(39.7380510717141,10.61999998,-142.980968310073));
#170267=CARTESIAN_POINT('Ctrl Pts',(39.8192390703685,10.61999998,-143.325086707917));
#170268=CARTESIAN_POINT('Ctrl Pts',(39.9201606061911,10.61999998,-143.662539288925));
#170269=CARTESIAN_POINT('Ctrl Pts',(40.0436577688824,10.61999998,-143.992366080443));
#170270=CARTESIAN_POINT('Ctrl Pts',(40.1606310196853,10.61999998,-144.304769306275));
#170271=CARTESIAN_POINT('Ctrl Pts',(40.2978572937931,10.61999998,-144.610331317757));
#170272=CARTESIAN_POINT('Ctrl Pts',(40.4577925858907,10.61999998,-144.90822241383));
#170273=CARTESIAN_POINT('Origin',(39.5,10.11999998,-55.24995));
#170274=CARTESIAN_POINT('',(39.5,10.61999998,-91.1341759094044));
#170275=CARTESIAN_POINT('Origin',(39.5,10.11999998,-91.1341759094044));
#170276=CARTESIAN_POINT('',(39.5,10.61999998,-55.24995));
#170277=CARTESIAN_POINT('Ctrl Pts',(39.,10.11999998,-91.1341759094044));
#170278=CARTESIAN_POINT('Ctrl Pts',(39.,10.61999998,-91.1341759094044));
#170279=CARTESIAN_POINT('Ctrl Pts',(39.5,10.61999998,-91.1341759094044));
#170280=CARTESIAN_POINT('Ctrl Pts',(39.,10.0814485101051,-90.4015548889157));
#170281=CARTESIAN_POINT('Ctrl Pts',(38.9598916786063,10.6199999799975,-90.3719688890003));
#170282=CARTESIAN_POINT('Ctrl Pts',(39.5000000020536,10.61999998,-90.4402448608912));
#170283=CARTESIAN_POINT('Ctrl Pts',(39.0871202471367,10.0432464379346,-89.6831085829417));
#170284=CARTESIAN_POINT('Ctrl Pts',(39.0069350308393,10.61999998,-89.6407441936901));
#170285=CARTESIAN_POINT('Ctrl Pts',(39.5784082214306,10.61999998,-89.7587725653299));
#170286=CARTESIAN_POINT('Ctrl Pts',(39.4353702758529,9.96778569102363,-88.2750332292462));
#170287=CARTESIAN_POINT('Ctrl Pts',(39.245797474144,10.61999998,-88.1799493597601));
#170288=CARTESIAN_POINT('Ctrl Pts',(39.89183324926,10.61999998,-88.4214995542899));
#170289=CARTESIAN_POINT('Ctrl Pts',(39.7001621050063,9.93023578241304,-87.580159846776));
#170290=CARTESIAN_POINT('Ctrl Pts',(39.4581171327344,10.61999998,-87.4384896017421));
#170291=CARTESIAN_POINT('Ctrl Pts',(40.1301388343916,10.61999998,-87.7606994776464));
#170292=CARTESIAN_POINT('Ctrl Pts',(40.064213984323,9.8954018152728,-86.9391114268059));
#170293=CARTESIAN_POINT('Ctrl Pts',(39.7432392475336,10.61999998,-86.7667827168808));
#170294=CARTESIAN_POINT('Ctrl Pts',(40.4577925858907,10.61999998,-87.1504205576762));
#170295=CARTESIAN_POINT('',(40.4577925858907,10.61999998,-87.1504205576762));
#170296=CARTESIAN_POINT('',(40.0642139580843,9.89540189669767,-86.9391114694666));
#170297=CARTESIAN_POINT('Origin',(40.4577925858907,10.11999998,-87.1504205576762));
#170298=CARTESIAN_POINT('Ctrl Pts',(39.,10.11999998,-91.1341759094044));
#170299=CARTESIAN_POINT('Ctrl Pts',(39.0000027915595,10.1116886332442,-90.9762294660295));
#170300=CARTESIAN_POINT('Ctrl Pts',(39.0041370161611,10.1028100622757,-90.8063031020809));
#170301=CARTESIAN_POINT('Ctrl Pts',(39.0195460817868,10.088416855121,-90.5336914216223));
#170302=CARTESIAN_POINT('Ctrl Pts',(39.0262224941828,10.0834435553843,-90.4398713106249));
#170303=CARTESIAN_POINT('Ctrl Pts',(39.0389688428197,10.0757342797035,-90.294792834635));
#170304=CARTESIAN_POINT('Ctrl Pts',(39.0460253914765,10.0718178234885,-90.2211670523011));
#170305=CARTESIAN_POINT('Ctrl Pts',(39.0555504742131,10.0671494790069,-90.1333915636446));
#170306=CARTESIAN_POINT('Ctrl Pts',(39.0606484786909,10.0647921444233,-90.0890374660041));
#170307=CARTESIAN_POINT('Ctrl Pts',(39.0632828966796,10.063607905681,-90.0667442610206));
#170308=CARTESIAN_POINT('Ctrl Pts',(39.0644304031572,10.0630992059044,-90.0571651875067));
#170309=CARTESIAN_POINT('Ctrl Pts',(39.0651995305414,10.0627598158354,-90.0507736232742));
#170310=CARTESIAN_POINT('Ctrl Pts',(39.0658473606639,10.0624757851372,-90.045423804078));
#170311=CARTESIAN_POINT('Ctrl Pts',(39.0741342857479,10.0588524738979,-89.9771728188365));
#170312=CARTESIAN_POINT('Ctrl Pts',(39.0892493568576,10.052622511364,-89.8541397133721));
#170313=CARTESIAN_POINT('Ctrl Pts',(39.1330129366525,10.0384158850763,-89.5865583530335));
#170314=CARTESIAN_POINT('Ctrl Pts',(39.1512193030171,10.0328676478481,-89.4835383246356));
#170315=CARTESIAN_POINT('Ctrl Pts',(39.1862174444622,10.0233700821188,-89.3086276329353));
#170316=CARTESIAN_POINT('Ctrl Pts',(39.1991713761146,10.0200103880156,-89.2469300451919));
#170317=CARTESIAN_POINT('Ctrl Pts',(39.220872401986,10.0147117872523,-89.1493691658317));
#170318=CARTESIAN_POINT('Ctrl Pts',(39.2322910073433,10.0119980603492,-89.0993354888038));
#170319=CARTESIAN_POINT('Ctrl Pts',(39.2466865483573,10.0087303108317,-89.0387909591602));
#170320=CARTESIAN_POINT('Ctrl Pts',(39.2530950507342,10.0073095256592,-89.0123804941478));
#170321=CARTESIAN_POINT('Ctrl Pts',(39.2574214878754,10.0063579939484,-88.9946709698606));
#170322=CARTESIAN_POINT('Ctrl Pts',(39.2601341389045,10.0057669940108,-88.9836551782209));
#170323=CARTESIAN_POINT('Ctrl Pts',(39.3160836297246,9.99365749385951,-88.7576909135574));
#170324=CARTESIAN_POINT('Ctrl Pts',(39.3736790817413,9.98295445715858,-88.5614711434704));
#170325=CARTESIAN_POINT('Ctrl Pts',(39.4583129915093,9.96894476384489,-88.3009574359105));
#170326=CARTESIAN_POINT('Ctrl Pts',(39.4862456662361,9.96460148642293,-88.2197448294764));
#170327=CARTESIAN_POINT('Ctrl Pts',(39.527022648588,9.95853825401135,-88.1062286732771));
#170328=CARTESIAN_POINT('Ctrl Pts',(39.5471321967724,9.9556187612689,-88.0515457852448));
#170329=CARTESIAN_POINT('Ctrl Pts',(39.5699677961773,9.95239356302238,-87.9913471515293));
#170330=CARTESIAN_POINT('Ctrl Pts',(39.5812132797666,9.95082387059787,-87.9621429820663));
#170331=CARTESIAN_POINT('Ctrl Pts',(39.585994170109,9.9501600872462,-87.9498182585687));
#170332=CARTESIAN_POINT('Ctrl Pts',(39.5891726689007,9.94971952318801,-87.941644245914));
#170333=CARTESIAN_POINT('Ctrl Pts',(39.5900087473004,9.94960366877689,-87.9394947831222));
#170334=CARTESIAN_POINT('Ctrl Pts',(39.7414059070582,9.92868751729576,-87.552038152988));
#170335=CARTESIAN_POINT('Ctrl Pts',(39.9039311777724,9.91073895422256,-87.2213504986795));
#170336=CARTESIAN_POINT('Ctrl Pts',(40.0642139577648,9.89540181781408,-86.9391114735717));
#170337=CARTESIAN_POINT('Ctrl Pts',(40.4577925858907,10.61999998,-87.1504205576762));
#170338=CARTESIAN_POINT('Ctrl Pts',(40.3970580365442,10.61999998,-87.2635430663923));
#170339=CARTESIAN_POINT('Ctrl Pts',(40.3395672151847,10.61999998,-87.3780682227952));
#170340=CARTESIAN_POINT('Ctrl Pts',(40.285131428432,10.61999998,-87.4939105062397));
#170341=CARTESIAN_POINT('Ctrl Pts',(40.2286629323529,10.61999998,-87.6140785045123));
#170342=CARTESIAN_POINT('Ctrl Pts',(40.1754817433896,10.61999998,-87.7356644050394));
#170343=CARTESIAN_POINT('Ctrl Pts',(40.1254267036649,10.61999998,-87.858600474452));
#170344=CARTESIAN_POINT('Ctrl Pts',(40.0931586145975,10.61999998,-87.9378514761339));
#170345=CARTESIAN_POINT('Ctrl Pts',(40.0621906903531,10.61999998,-88.0176641176421));
#170346=CARTESIAN_POINT('Ctrl Pts',(40.0324904304422,10.61999998,-88.0980242245578));
#170347=CARTESIAN_POINT('Ctrl Pts',(39.9448659684021,10.61999998,-88.3351100668741));
#170348=CARTESIAN_POINT('Ctrl Pts',(39.8685902579799,10.61999998,-88.5761404611087));
#170349=CARTESIAN_POINT('Ctrl Pts',(39.8033297324042,10.61999998,-88.818903429086));
#170350=CARTESIAN_POINT('Ctrl Pts',(39.7790792084132,10.61999998,-88.9091130792095));
#170351=CARTESIAN_POINT('Ctrl Pts',(39.7563491787903,10.61999998,-88.9995618473943));
#170352=CARTESIAN_POINT('Ctrl Pts',(39.735120734996,10.61999998,-89.090136059728));
#170353=CARTESIAN_POINT('Ctrl Pts',(39.6384824206298,10.61999998,-89.5024573438405));
#170354=CARTESIAN_POINT('Ctrl Pts',(39.5716278198238,10.61999998,-89.9196108763147));
#170355=CARTESIAN_POINT('Ctrl Pts',(39.5345653063075,10.61999998,-90.3415980464726));
#170356=CARTESIAN_POINT('Ctrl Pts',(39.5115257817295,10.61999998,-90.6039219650634));
#170357=CARTESIAN_POINT('Ctrl Pts',(39.500000000001,10.61999998,-90.8681139415084));
#170358=CARTESIAN_POINT('Ctrl Pts',(39.5,10.61999998,-91.1341759094044));
#170359=CARTESIAN_POINT('Origin',(59.5,11.11999998,-55.24995));
#170360=CARTESIAN_POINT('',(59.5,10.61999998,-58.24995));
#170361=CARTESIAN_POINT('Origin',(59.5,11.11999998,-58.24995));
#170362=CARTESIAN_POINT('',(59.5,10.61999998,-174.34995));
#170363=CARTESIAN_POINT('',(59.5,10.61999998,-58.24995));
#170364=CARTESIAN_POINT('Origin',(59.5,11.11999998,-174.34995));
#170365=CARTESIAN_POINT('Origin',(57.,11.11999998,-174.34995));
#170366=CARTESIAN_POINT('',(57.,10.61999998,-176.84995));
#170367=CARTESIAN_POINT('Origin',(57.,10.61999998,-174.34995));
#170368=CARTESIAN_POINT('Origin',(57.,11.11999998,-176.84995));
#170369=CARTESIAN_POINT('Origin',(-83.2809572255632,11.1199999800001,-176.84995));
#170370=CARTESIAN_POINT('',(-83.2809572255632,10.6199999800001,-176.84995));
#170371=CARTESIAN_POINT('Origin',(54.2951871140408,10.11999998,-179.64995));
#170372=CARTESIAN_POINT('',(54.2951871140408,10.61999998,-171.871644662643));
#170373=CARTESIAN_POINT('Origin',(54.2951871140408,10.11999998,-171.871644662643));
#170374=CARTESIAN_POINT('',(53.8350584096845,9.92434320033876,-179.64995));
#170375=CARTESIAN_POINT('',(54.2951871140408,10.61999998,-176.84995));
#170376=CARTESIAN_POINT('Ctrl Pts',(54.125256265546,10.6199999790853,-171.204806771037));
#170377=CARTESIAN_POINT('Ctrl Pts',(53.4900212150519,10.6200436404067,-171.547539040477));
#170378=CARTESIAN_POINT('Ctrl Pts',(53.7132658667077,9.94427345761011,-171.4270966421));
#170379=CARTESIAN_POINT('Ctrl Pts',(54.2414728015496,10.6199999790668,-171.420234627159));
#170380=CARTESIAN_POINT('Ctrl Pts',(53.5293152990573,10.6200454840218,-171.669460818781));
#170381=CARTESIAN_POINT('Ctrl Pts',(53.7965641368282,9.93061460392253,-171.570704923157));
#170382=CARTESIAN_POINT('Ctrl Pts',(54.3014296083361,10.6199999790573,-171.661245462922));
#170383=CARTESIAN_POINT('Ctrl Pts',(53.5404438804711,10.6200464809797,-171.777144153386));
#170384=CARTESIAN_POINT('Ctrl Pts',(53.8395077234217,9.92361807935392,-171.73138684676));
#170385=CARTESIAN_POINT('Ctrl Pts',(54.2947083191062,10.6199999790584,-171.909234173486));
#170386=CARTESIAN_POINT('Ctrl Pts',(53.5391294683119,10.6200463684923,-171.888526671109));
#170387=CARTESIAN_POINT('Ctrl Pts',(53.8346934801601,9.92440268025281,-171.896703002619));
#170388=CARTESIAN_POINT('Origin',(52.7058336008317,10.6200000150416,-171.863895229713));
#170389=CARTESIAN_POINT('Ctrl Pts',(54.0353592674108,10.61999998,-61.0321215118284));
#170390=CARTESIAN_POINT('Ctrl Pts',(53.3881607688931,10.6199999799991,-60.7039348782963));
#170391=CARTESIAN_POINT('Ctrl Pts',(53.6186572976477,9.94192748261378,-60.8208168640295));
#170392=CARTESIAN_POINT('Ctrl Pts',(51.8138491393997,10.61999998,-65.4130322530771));
#170393=CARTESIAN_POINT('Ctrl Pts',(51.1366620554546,10.6199999801381,-65.1210166348378));
#170394=CARTESIAN_POINT('Ctrl Pts',(51.3997940829438,9.93573759523097,-65.2017242497444));
#170395=CARTESIAN_POINT('Ctrl Pts',(49.5759233704096,10.61999998,-69.7854123595329));
#170396=CARTESIAN_POINT('Ctrl Pts',(48.8824081932915,10.619999979979,-69.498350907102));
#170397=CARTESIAN_POINT('Ctrl Pts',(49.1649346369347,9.92892193238703,-69.5741060667035));
#170398=CARTESIAN_POINT('Ctrl Pts',(45.0516568115529,10.61999998,-78.5050001236053));
#170399=CARTESIAN_POINT('Ctrl Pts',(44.3353985022919,10.6199999800216,-78.2014831316521));
#170400=CARTESIAN_POINT('Ctrl Pts',(44.6481582889209,9.913573864379,-78.2936943604392));
#170401=CARTESIAN_POINT('Ctrl Pts',(42.7656039747263,10.61999998,-82.8523636293437));
#170402=CARTESIAN_POINT('Ctrl Pts',(42.0255008894278,10.6199999800755,-82.557030405903));
#170403=CARTESIAN_POINT('Ctrl Pts',(42.3665201560454,9.90504529632398,-82.6410530645212));
#170404=CARTESIAN_POINT('Ctrl Pts',(40.4418478052835,10.61999998,-87.1801174602812));
#170405=CARTESIAN_POINT('Ctrl Pts',(39.7271443485661,10.6199999799995,-86.7963620990942));
#170406=CARTESIAN_POINT('Ctrl Pts',(40.0483186661866,9.89530939594053,-86.9688144589263));
#170407=CARTESIAN_POINT('',(54.0201152391274,10.61999998,-61.0621827299711));
#170408=CARTESIAN_POINT('',(53.6034226162473,9.94191093135268,-60.8508735991007));
#170409=CARTESIAN_POINT('Origin',(54.0201152391274,10.11999998,-61.0621827299711));
#170410=CARTESIAN_POINT('Ctrl Pts',(40.064213984323,9.89540181527278,-86.9391114268059));
#170411=CARTESIAN_POINT('Ctrl Pts',(41.1403040225241,9.89991895211768,-84.9300143693684));
#170412=CARTESIAN_POINT('Ctrl Pts',(42.2484592572501,9.90444570038255,-82.8416244158638));
#170413=CARTESIAN_POINT('Ctrl Pts',(43.9590882648639,9.91091969009987,-79.5901001415064));
#170414=CARTESIAN_POINT('Ctrl Pts',(44.5373616193329,9.91303143487921,-78.4864354927038));
#170415=CARTESIAN_POINT('Ctrl Pts',(45.4168857437243,9.91614729047684,-76.8012036834748));
#170416=CARTESIAN_POINT('Ctrl Pts',(45.8596761527945,9.91769289978181,-75.951154069854));
#170417=CARTESIAN_POINT('Ctrl Pts',(46.3815668865533,9.91948502097661,-74.9464205298688));
#170418=CARTESIAN_POINT('Ctrl Pts',(46.6438379037851,9.92038011477212,-74.4408015121859));
#170419=CARTESIAN_POINT('Ctrl Pts',(46.7893905868381,9.92087561089464,-74.1600050945544));
#170420=CARTESIAN_POINT('Ctrl Pts',(46.8599302771651,9.92111540880078,-74.0238636296621));
#170421=CARTESIAN_POINT('Ctrl Pts',(46.8975790657137,9.92124332089142,-73.951187093226));
#170422=CARTESIAN_POINT('Ctrl Pts',(46.902857723862,9.92126125354295,-73.9409969471016));
#170423=CARTESIAN_POINT('Ctrl Pts',(49.024122292157,9.9284670907748,-69.8459140539938));
#170424=CARTESIAN_POINT('Ctrl Pts',(51.2561074478258,9.93535987983753,-65.4852004772353));
#170425=CARTESIAN_POINT('Ctrl Pts',(53.6034226162473,9.94191093135268,-60.8508735991007));
#170426=CARTESIAN_POINT('Ctrl Pts',(54.0201152391274,10.61999998,-61.0621827299711));
#170427=CARTESIAN_POINT('Ctrl Pts',(51.8036107556176,10.61999998,-65.4330353431782));
#170428=CARTESIAN_POINT('Ctrl Pts',(49.570749196272,10.61999998,-69.7953845096745));
#170429=CARTESIAN_POINT('Ctrl Pts',(47.313790090977,10.61999998,-74.1452062415669));
#170430=CARTESIAN_POINT('Ctrl Pts',(45.056830985682,10.61999998,-78.4950279734592));
#170431=CARTESIAN_POINT('Ctrl Pts',(42.7760635123042,10.61999998,-82.8324726037656));
#170432=CARTESIAN_POINT('Ctrl Pts',(40.4577925858907,10.61999998,-87.1504205576762));
#170433=CARTESIAN_POINT('Ctrl Pts',(39.,12.1842625441365,-89.0065976851046));
#170434=CARTESIAN_POINT('Ctrl Pts',(39.,10.9256777712437,-87.8240033916746));
#170435=CARTESIAN_POINT('Ctrl Pts',(40.0658654432757,9.93538940172282,-86.8935063764011));
#170436=CARTESIAN_POINT('Ctrl Pts',(39.,10.9797897629302,-90.28846680179));
#170437=CARTESIAN_POINT('Ctrl Pts',(39.,9.77616182942057,-89.1086695731975));
#170438=CARTESIAN_POINT('Ctrl Pts',(40.0194662171323,8.81210183467955,-88.1753591901201));
#170439=CARTESIAN_POINT('Ctrl Pts',(39.,9.73513866768107,-91.5445844304498));
#170440=CARTESIAN_POINT('Ctrl Pts',(39.,8.58691729751272,-90.3710832422126));
#170441=CARTESIAN_POINT('Ctrl Pts',(39.9723426990601,7.65560021428954,-89.4314931216999));
#170442=CARTESIAN_POINT('Ctrl Pts',(39.,7.14206310577898,-93.9773376754667));
#170443=CARTESIAN_POINT('Ctrl Pts',(39.,6.11218708321155,-92.8159732515183));
#170444=CARTESIAN_POINT('Ctrl Pts',(39.8778703452952,5.25671151505436,-91.8642463668096));
#170445=CARTESIAN_POINT('Ctrl Pts',(39.,5.80730703259943,-95.141285808143));
#170446=CARTESIAN_POINT('Ctrl Pts',(38.9999999999877,4.84006269065046,-93.9862863085864));
#170447=CARTESIAN_POINT('Ctrl Pts',(39.8310091356278,4.02698776925249,-93.0281766935241));
#170448=CARTESIAN_POINT('Ctrl Pts',(39.,4.4206962941175,-96.234166137987));
#170449=CARTESIAN_POINT('Ctrl Pts',(39.,3.51696389869249,-95.0875400976674));
#170450=CARTESIAN_POINT('Ctrl Pts',(39.7856125955649,2.75522821384069,-94.1210748292835));
#170451=CARTESIAN_POINT('',(39.8417543268106,4.28989009189694,-92.7506602165387));
#170452=CARTESIAN_POINT('Ctrl Pts',(39.8417723428441,4.28998413512524,-92.7507162227756));
#170453=CARTESIAN_POINT('Ctrl Pts',(39.8597146560854,4.76916698343337,-92.3070009482122));
#170454=CARTESIAN_POINT('Ctrl Pts',(39.8780875478676,5.25018471631922,-91.8469438750031));
#170455=CARTESIAN_POINT('Ctrl Pts',(39.8968788416962,5.7343155538529,-91.369721820308));
#170456=CARTESIAN_POINT('Ctrl Pts',(39.9061864198051,5.9741120056742,-91.1333473806427));
#170457=CARTESIAN_POINT('Ctrl Pts',(39.9155964941233,6.21467253203749,-90.8927620401306));
#170458=CARTESIAN_POINT('Ctrl Pts',(39.9251065221777,6.45615586467189,-90.6478697442548));
#170459=CARTESIAN_POINT('Ctrl Pts',(39.9416791850316,6.87697711080465,-90.2211078638612));
#170460=CARTESIAN_POINT('Ctrl Pts',(39.9584956321962,7.29904284519804,-89.7828257767047));
#170461=CARTESIAN_POINT('Ctrl Pts',(39.9755525034532,7.72296859045191,-89.332496982478));
#170462=CARTESIAN_POINT('Ctrl Pts',(39.9904670259603,8.09364911993888,-88.9387296358234));
#170463=CARTESIAN_POINT('Ctrl Pts',(40.0055653344074,8.46575119682726,-88.5357514276307));
#170464=CARTESIAN_POINT('Ctrl Pts',(40.0208411411111,8.83969191810781,-88.1232475756398));
#170465=CARTESIAN_POINT('Ctrl Pts',(40.0351460298419,9.18986526826736,-87.736962136304));
#170466=CARTESIAN_POINT('Ctrl Pts',(40.0496065738335,9.54165057206099,-87.3423230586879));
#170467=CARTESIAN_POINT('Ctrl Pts',(40.0642139729082,9.89540198625494,-86.9391115876706));
#170468=CARTESIAN_POINT('Ctrl Pts',(39.8417543268106,4.28989009189694,-92.7506602165387));
#170469=CARTESIAN_POINT('Ctrl Pts',(39.8111499956431,4.29299201950353,-92.8082417354953));
#170470=CARTESIAN_POINT('Ctrl Pts',(39.7802667553935,4.29622413902246,-92.8683179012178));
#170471=CARTESIAN_POINT('Ctrl Pts',(39.7493004842404,4.29958883760676,-92.9309560235319));
#170472=CARTESIAN_POINT('Ctrl Pts',(39.7183256003837,4.30295447202061,-92.9936115674976));
#170473=CARTESIAN_POINT('Ctrl Pts',(39.6872729212866,4.30643631872874,-93.0588330079571));
#170474=CARTESIAN_POINT('Ctrl Pts',(39.6563397338845,4.31006069299538,-93.1266868986523));
#170475=CARTESIAN_POINT('Ctrl Pts',(39.6254065464824,4.31368506726203,-93.1945407893474));
#170476=CARTESIAN_POINT('Ctrl Pts',(39.5945940943932,4.31745491936417,-93.2650236904387));
#170477=CARTESIAN_POINT('Ctrl Pts',(39.5641304981276,4.32136651585282,-93.3381731100622));
#170478=CARTESIAN_POINT('Ctrl Pts',(39.5488986999947,4.32332231409715,-93.3747478198739));
#170479=CARTESIAN_POINT('Ctrl Pts',(39.5337543520915,4.32531328847347,-93.4119889205435));
#170480=CARTESIAN_POINT('Ctrl Pts',(39.5187271516468,4.32733725951214,-93.4498994832949));
#170481=CARTESIAN_POINT('Ctrl Pts',(39.5112135514244,4.32834924503147,-93.4688547646706));
#170482=CARTESIAN_POINT('Ctrl Pts',(39.5037292367631,4.32936947808469,-93.4879774096565));
#170483=CARTESIAN_POINT('Ctrl Pts',(39.4962779863463,4.33039754815179,-93.5072676685439));
#170484=CARTESIAN_POINT('Ctrl Pts',(39.4925523611378,4.33091158318535,-93.5169127979876));
#170485=CARTESIAN_POINT('Ctrl Pts',(39.4888350016951,4.33142757732785,-93.5265998307344));
#170486=CARTESIAN_POINT('Ctrl Pts',(39.4851263808663,4.3319454745947,-93.5363287933278));
#170487=CARTESIAN_POINT('Ctrl Pts',(39.4832720704519,4.33220442322813,-93.5411932746244));
#170488=CARTESIAN_POINT('Ctrl Pts',(39.4814199446683,4.33246384763303,-93.5460682383712));
#170489=CARTESIAN_POINT('Ctrl Pts',(39.4795700627628,4.33272374031367,-93.5509536873952));
#170490=CARTESIAN_POINT('Ctrl Pts',(39.47864512181,4.33285368665399,-93.5533964119072));
#170491=CARTESIAN_POINT('Ctrl Pts',(39.4777207418251,4.33298375006261,-93.5558417577377));
#170492=CARTESIAN_POINT('Ctrl Pts',(39.4767969302229,4.33311392956962,-93.5582897252076));
#170493=CARTESIAN_POINT('Ctrl Pts',(39.4758731186208,4.33324410907663,-93.5607376926775));
#170494=CARTESIAN_POINT('Ctrl Pts',(39.4745077545883,4.33343689447469,-93.5643638035833));
#170495=CARTESIAN_POINT('Ctrl Pts',(39.4740272079786,4.3335048154045,-93.5656414928445));
#170496=CARTESIAN_POINT('Ctrl Pts',(39.4619116443501,4.33521724106759,-93.5978546543312));
#170497=CARTESIAN_POINT('Ctrl Pts',(39.4483615670327,4.33714569186926,-93.6346022140469));
#170498=CARTESIAN_POINT('Ctrl Pts',(39.4335980269417,4.33930934348358,-93.67594212584));
#170499=CARTESIAN_POINT('Ctrl Pts',(39.4185623987223,4.34151287062333,-93.7180439212436));
#170500=CARTESIAN_POINT('Ctrl Pts',(39.4022682265848,4.34396031741693,-93.7649089098956));
#170501=CARTESIAN_POINT('Ctrl Pts',(39.3850008239921,4.34667323458354,-93.8166147001729));
#170502=CARTESIAN_POINT('Ctrl Pts',(39.3761835953417,4.34805852752724,-93.8430171525961));
#170503=CARTESIAN_POINT('Ctrl Pts',(39.3671134251348,4.34951306320326,-93.8706820633472));
#170504=CARTESIAN_POINT('Ctrl Pts',(39.3578332586383,4.35103987466927,-93.8996213409729));
#170505=CARTESIAN_POINT('Ctrl Pts',(39.3382571951746,4.3542606097894,-93.9606673508278));
#170506=CARTESIAN_POINT('Ctrl Pts',(39.3177461102384,4.35779976794404,-94.0273776023551));
#170507=CARTESIAN_POINT('Ctrl Pts',(39.2967677854055,4.36164894682482,-94.0998298524968));
#170508=CARTESIAN_POINT('Ctrl Pts',(39.2934740342213,4.36225329619961,-94.111205388275));
#170509=CARTESIAN_POINT('Ctrl Pts',(39.2901688648655,4.36286528720593,-94.1227225016788));
#170510=CARTESIAN_POINT('Ctrl Pts',(39.2868541959498,4.36348488625061,-94.1343815258526));
#170511=CARTESIAN_POINT('Ctrl Pts',(39.274641085215,4.36576783876756,-94.1773399500328));
#170512=CARTESIAN_POINT('Ctrl Pts',(39.2622991914327,4.36815323253446,-94.2222238784512));
#170513=CARTESIAN_POINT('Ctrl Pts',(39.2499302932482,4.37063298596967,-94.2690438315574));
#170514=CARTESIAN_POINT('Ctrl Pts',(39.2437458441559,4.37187286268728,-94.2924538081105));
#170515=CARTESIAN_POINT('Ctrl Pts',(39.2375547020892,4.37313634560285,-94.3163478101846));
#170516=CARTESIAN_POINT('Ctrl Pts',(39.2313701710456,4.37442178670003,-94.3407266202839));
#170517=CARTESIAN_POINT('Ctrl Pts',(39.2268578943689,4.37535965342608,-94.3585135689532));
#170518=CARTESIAN_POINT('Ctrl Pts',(39.2221531070756,4.37635067920456,-94.3773493160581));
#170519=CARTESIAN_POINT('Ctrl Pts',(39.2176913730843,4.37730344240409,-94.3955037967945));
#170520=CARTESIAN_POINT('Ctrl Pts',(39.2160378498885,4.37765653742357,-94.4022318659857));
#170521=CARTESIAN_POINT('Ctrl Pts',(39.2144172036271,4.37800437246001,-94.4088662101995));
#170522=CARTESIAN_POINT('Ctrl Pts',(39.2128498752563,4.37834227799597,-94.4153182336563));
#170523=CARTESIAN_POINT('Ctrl Pts',(39.2126660218777,4.37838191555729,-94.4160750797219));
#170524=CARTESIAN_POINT('Ctrl Pts',(39.2124823293284,4.37842154399935,-94.4168317672599));
#170525=CARTESIAN_POINT('Ctrl Pts',(39.2122987973978,4.37846116332228,-94.4175882962553));
#170526=CARTESIAN_POINT('Ctrl Pts',(39.1892451767618,4.38343778421844,-94.5126166240753));
#170527=CARTESIAN_POINT('Ctrl Pts',(39.1687677021364,4.38827551589204,-94.6052466993645));
#170528=CARTESIAN_POINT('Ctrl Pts',(39.1505238108285,4.39296972656187,-94.6953494792007));
#170529=CARTESIAN_POINT('Ctrl Pts',(39.1322799195205,4.3976639372317,-94.7854522590368));
#170530=CARTESIAN_POINT('Ctrl Pts',(39.1162696674874,4.40221466077713,-94.8730283767273));
#170531=CARTESIAN_POINT('Ctrl Pts',(39.1021792361851,4.40661979062833,-94.9579995734556));
#170532=CARTESIAN_POINT('Ctrl Pts',(39.0860807420172,4.41165270663333,-95.0550802295142));
#170533=CARTESIAN_POINT('Ctrl Pts',(39.0724902488796,4.41649497941412,-95.1487491592476));
#170534=CARTESIAN_POINT('Ctrl Pts',(39.0609905931823,4.42114241942972,-95.2388722612092));
#170535=CARTESIAN_POINT('Ctrl Pts',(39.0528187821168,4.42444495323986,-95.302914957899));
#170536=CARTESIAN_POINT('Ctrl Pts',(39.0457039565657,4.42764904915551,-95.3651661449135));
#170537=CARTESIAN_POINT('Ctrl Pts',(39.0395083479183,4.43075318936736,-95.4255780326426));
#170538=CARTESIAN_POINT('Ctrl Pts',(39.0350899695047,4.43296689699252,-95.4686605764032));
#170539=CARTESIAN_POINT('Ctrl Pts',(39.0311383113794,4.43513021876868,-95.5108164380876));
#170540=CARTESIAN_POINT('Ctrl Pts',(39.0276053730942,4.43724335335137,-95.5520431268892));
#170541=CARTESIAN_POINT('Ctrl Pts',(39.0205036056785,4.44149108968677,-95.6349153232202));
#170542=CARTESIAN_POINT('Ctrl Pts',(39.0150924157327,4.44553548053849,-95.7140220206559));
#170543=CARTESIAN_POINT('Ctrl Pts',(39.0110141613094,4.4493769408033,-95.7893219652571));
#170544=CARTESIAN_POINT('Ctrl Pts',(39.0067749714961,4.45336999212692,-95.8675933836059));
#170545=CARTESIAN_POINT('Ctrl Pts',(39.003975731844,4.45714380773583,-95.9417521367898));
#170546=CARTESIAN_POINT('Ctrl Pts',(39.0022556585823,4.46070073192571,-96.0117925129403));
#170547=CARTESIAN_POINT('Ctrl Pts',(39.0006677664691,4.46398431989507,-96.0764505501149));
#170548=CARTESIAN_POINT('Ctrl Pts',(39.,4.4670831113137,-96.1375996770293));
#170549=CARTESIAN_POINT('Ctrl Pts',(39.,4.46999998000002,-96.1952589849652));
#170550=CARTESIAN_POINT('Ctrl Pts',(39.8417798628559,4.28988750369336,-92.7506121713693));
#170551=CARTESIAN_POINT('Ctrl Pts',(39.9519009607655,3.96999998000001,-92.8065726369586));
#170552=CARTESIAN_POINT('Ctrl Pts',(40.2576018765703,3.96999998000001,-92.9619213022396));
#170553=CARTESIAN_POINT('Ctrl Pts',(39.558565846057,4.31859237238363,-93.2834642887004));
#170554=CARTESIAN_POINT('Ctrl Pts',(39.6570458949425,3.9699999800025,-93.3357860473751));
#170555=CARTESIAN_POINT('Ctrl Pts',(40.0026978626623,3.96999998000001,-93.4635309699092));
#170556=CARTESIAN_POINT('Ctrl Pts',(39.3523491668799,4.34822838553358,-93.8402926529419));
#170557=CARTESIAN_POINT('Ctrl Pts',(39.4410018196003,3.96999998000002,-93.8819356839734));
#170558=CARTESIAN_POINT('Ctrl Pts',(39.817114250256,3.96999998000002,-93.9870091547076));
#170559=CARTESIAN_POINT('Ctrl Pts',(39.0722484171839,4.40869400027786,-94.9948839370727));
#170560=CARTESIAN_POINT('Ctrl Pts',(39.1236627362708,3.96999998000002,-95.0167026881129));
#170561=CARTESIAN_POINT('Ctrl Pts',(39.5650235754014,3.96999998000002,-95.0708764103351));
#170562=CARTESIAN_POINT('Ctrl Pts',(39.,4.43971662334272,-95.5966316298752));
#170563=CARTESIAN_POINT('Ctrl Pts',(39.0293922558424,3.96999998000002,-95.61424653503));
#170564=CARTESIAN_POINT('Ctrl Pts',(39.500000001452,3.96999998000002,-95.6349699403799));
#170565=CARTESIAN_POINT('Ctrl Pts',(39.,4.46999998000002,-96.1952589849652));
#170566=CARTESIAN_POINT('Ctrl Pts',(39.,3.96999998000001,-96.1952589849652));
#170567=CARTESIAN_POINT('Ctrl Pts',(39.5,3.96999998000002,-96.1952589849652));
#170568=CARTESIAN_POINT('',(39.5,3.96999998000002,-96.1952589849652));
#170569=CARTESIAN_POINT('Origin',(39.5,4.46999998000001,-96.1952589849652));
#170570=CARTESIAN_POINT('',(40.2576018765703,3.96999998000001,-92.9619213022396));
#170571=CARTESIAN_POINT('Origin',(40.2576018765703,4.46999998000001,-92.9619213022396));
#170572=CARTESIAN_POINT('Ctrl Pts',(39.5,3.96999998000002,-96.1952589849652));
#170573=CARTESIAN_POINT('Ctrl Pts',(39.5,3.96999998000001,-95.9142103380175));
#170574=CARTESIAN_POINT('Ctrl Pts',(39.5161227273835,3.96999998000002,-95.6343109988079));
#170575=CARTESIAN_POINT('Ctrl Pts',(39.5801128567305,3.96999998000002,-95.0767752377766));
#170576=CARTESIAN_POINT('Ctrl Pts',(39.6280462441481,3.96999998000002,-94.7999095964395));
#170577=CARTESIAN_POINT('Ctrl Pts',(39.81711425019,3.96999998000002,-93.9870091546851));
#170578=CARTESIAN_POINT('Ctrl Pts',(40.0026450649981,3.96999998000001,-93.4636348550876));
#170579=CARTESIAN_POINT('Ctrl Pts',(40.2576018765703,3.96999998000001,-92.9619213022396));
#170580=CARTESIAN_POINT('Origin',(39.5,4.46999998000002,-55.24995));
#170581=CARTESIAN_POINT('',(39.5,3.96999998000002,-135.863383986541));
#170582=CARTESIAN_POINT('Origin',(39.5,4.46999998000001,-135.863383986541));
#170583=CARTESIAN_POINT('',(39.5,3.96999998000002,-55.24995));
#170584=CARTESIAN_POINT('Ctrl Pts',(39.,4.46999998000002,-135.863383986541));
#170585=CARTESIAN_POINT('Ctrl Pts',(39.,3.96999998000001,-135.863383986541));
#170586=CARTESIAN_POINT('Ctrl Pts',(39.5,3.96999998000002,-135.863383986541));
#170587=CARTESIAN_POINT('Ctrl Pts',(39.,4.43959418388259,-136.464431642573));
#170588=CARTESIAN_POINT('Ctrl Pts',(39.0295065227812,3.96999998000002,-136.446655166649));
#170589=CARTESIAN_POINT('Ctrl Pts',(39.50000000251,3.96999998000002,-136.425947926524));
#170590=CARTESIAN_POINT('Ctrl Pts',(39.0706358339689,4.40924336018453,-137.053149400534));
#170591=CARTESIAN_POINT('Ctrl Pts',(39.1216633961175,3.96999998000002,-137.031492360702));
#170592=CARTESIAN_POINT('Ctrl Pts',(39.5635722498606,3.96999998000002,-136.977817064522));
#170593=CARTESIAN_POINT('Ctrl Pts',(39.3484951732863,4.34886300930159,-138.206349454905));
#170594=CARTESIAN_POINT('Ctrl Pts',(39.4368658200899,3.96999998000001,-138.164990760612));
#170595=CARTESIAN_POINT('Ctrl Pts',(39.813645656669,3.96999998000002,-138.060358011877));
#170596=CARTESIAN_POINT('Ctrl Pts',(39.5585840804945,4.31859052702601,-138.775212992296));
#170597=CARTESIAN_POINT('Ctrl Pts',(39.6570895715147,3.96999997999977,-138.722935325351));
#170598=CARTESIAN_POINT('Ctrl Pts',(40.0027227918541,3.96999998000001,-138.595161064797));
#170599=CARTESIAN_POINT('Ctrl Pts',(39.8417798628559,4.28988750369336,-139.308030800137));
#170600=CARTESIAN_POINT('Ctrl Pts',(39.9519009607655,3.96999998000001,-139.252070334547));
#170601=CARTESIAN_POINT('Ctrl Pts',(40.2576018765703,3.96999998000001,-139.096721669266));
#170602=CARTESIAN_POINT('',(40.2576018765703,3.96999998000001,-139.096721669266));
#170603=CARTESIAN_POINT('Ctrl Pts',(40.2576018765703,3.96999998000001,-139.096721669266));
#170604=CARTESIAN_POINT('Ctrl Pts',(40.1422232489788,3.96999998000001,-138.869675289079));
#170605=CARTESIAN_POINT('Ctrl Pts',(40.0403932052787,3.96999998000002,-138.635953665714));
#170606=CARTESIAN_POINT('Ctrl Pts',(39.9518763029277,3.96999998000002,-138.397956901358));
#170607=CARTESIAN_POINT('Ctrl Pts',(39.858956988463,3.96999998000002,-138.148123303464));
#170608=CARTESIAN_POINT('Ctrl Pts',(39.7807077156263,3.96999998000002,-137.893577344813));
#170609=CARTESIAN_POINT('Ctrl Pts',(39.716907177833,3.96999998000002,-137.637072537694));
#170610=CARTESIAN_POINT('Ctrl Pts',(39.7071356404173,3.96999998000002,-137.597786876369));
#170611=CARTESIAN_POINT('Ctrl Pts',(39.6977031285494,3.96999998000002,-137.558455249076));
#170612=CARTESIAN_POINT('Ctrl Pts',(39.6886089528968,3.96999998000002,-137.519087538285));
#170613=CARTESIAN_POINT('Ctrl Pts',(39.6032792176002,3.96999998000002,-137.149704268227));
#170614=CARTESIAN_POINT('Ctrl Pts',(39.5465796834581,3.96999998000002,-136.775425176616));
#170615=CARTESIAN_POINT('Ctrl Pts',(39.5191682987961,3.96999998000002,-136.396137730917));
#170616=CARTESIAN_POINT('Ctrl Pts',(39.5064128043257,3.96999998000002,-136.219641761233));
#170617=CARTESIAN_POINT('Ctrl Pts',(39.5000000000002,3.96999998000002,-136.042061173853));
#170618=CARTESIAN_POINT('Ctrl Pts',(39.5,3.96999998000002,-135.863383986541));
#170619=CARTESIAN_POINT('Origin',(40.2576018765703,4.46999998000001,-139.096721669266));
#170620=CARTESIAN_POINT('Ctrl Pts',(56.2171666226051,3.96999998000001,-171.237717270032));
#170621=CARTESIAN_POINT('Ctrl Pts',(55.8759673883189,3.96999998,-171.404299214979));
#170622=CARTESIAN_POINT('Ctrl Pts',(55.7843555297028,4.33575017898885,-171.449026400902));
#170623=CARTESIAN_POINT('Ctrl Pts',(53.5931279590331,3.96999998000001,-165.863065274939));
#170624=CARTESIAN_POINT('Ctrl Pts',(53.2681640678716,3.96999998006972,-166.052285867785));
#170625=CARTESIAN_POINT('Ctrl Pts',(53.1620910906406,4.33003381235646,-166.074376691472));
#170626=CARTESIAN_POINT('Ctrl Pts',(50.9564483006955,3.96999998000001,-160.494687880121));
#170627=CARTESIAN_POINT('Ctrl Pts',(50.6399914208629,3.96999998001567,-160.688987094682));
#170628=CARTESIAN_POINT('Ctrl Pts',(50.5275177831741,4.32360860554286,-160.70599701099));
#170629=CARTESIAN_POINT('Ctrl Pts',(45.6433184787346,3.96999998000001,-149.777683344423));
#170630=CARTESIAN_POINT('Ctrl Pts',(45.3382862796144,3.96999997998453,-149.967930534599));
#170631=CARTESIAN_POINT('Ctrl Pts',(45.2197944205701,4.30863333062082,-149.988992475295));
#170632=CARTESIAN_POINT('Ctrl Pts',(42.9672472399765,3.96999998000001,-144.428863195016));
#170633=CARTESIAN_POINT('Ctrl Pts',(42.6741187750921,3.96999998000002,-144.626843683376));
#170634=CARTESIAN_POINT('Ctrl Pts',(42.547006853164,4.30009530891334,-144.640178460294));
#170635=CARTESIAN_POINT('Ctrl Pts',(40.2576018765703,3.96999998000001,-139.096721669266));
#170636=CARTESIAN_POINT('Ctrl Pts',(39.9519009607656,3.96999998000002,-139.252070334547));
#170637=CARTESIAN_POINT('Ctrl Pts',(39.8417798628559,4.28988750369336,-139.308030800137));
#170638=CARTESIAN_POINT('',(56.217166622605,3.96999998000001,-171.237717270032));
#170639=CARTESIAN_POINT('Ctrl Pts',(56.217166622605,3.96999998000001,-171.237717270032));
#170640=CARTESIAN_POINT('Ctrl Pts',(53.5931275135095,3.96999998000001,-165.863064362474));
#170641=CARTESIAN_POINT('Ctrl Pts',(50.9564483006798,3.96999998000001,-160.49468788009));
#170642=CARTESIAN_POINT('Ctrl Pts',(48.2998833897147,3.96999998000001,-155.136185612272));
#170643=CARTESIAN_POINT('Ctrl Pts',(45.6433184787496,3.96999998000001,-149.777683344454));
#170644=CARTESIAN_POINT('Ctrl Pts',(42.9672487496428,3.96999998000001,-144.428866165794));
#170645=CARTESIAN_POINT('Ctrl Pts',(40.2576018765703,3.96999998000001,-139.096721669266));
#170646=CARTESIAN_POINT('Origin',(56.2171666226051,4.46999998000001,-171.237717270032));
#170647=CARTESIAN_POINT('Ctrl Pts',(56.362878117604,3.96999998707827,-171.9375490258));
#170648=CARTESIAN_POINT('Ctrl Pts',(55.9943718457987,3.9699379192599,-171.920606124721));
#170649=CARTESIAN_POINT('Ctrl Pts',(55.8855878616368,4.32236176169507,-171.915575297858));
#170650=CARTESIAN_POINT('Ctrl Pts',(56.3748852598389,3.96999998705621,-171.673567304561));
#170651=CARTESIAN_POINT('Ctrl Pts',(56.0043522879838,3.96993816409121,-171.724641829017));
#170652=CARTESIAN_POINT('Ctrl Pts',(55.8939328694509,4.32126340276226,-171.739613349113));
#170653=CARTESIAN_POINT('Ctrl Pts',(56.3146644389369,3.96999998716678,-171.413359333373));
#170654=CARTESIAN_POINT('Ctrl Pts',(55.9538751380083,3.96993692936927,-171.529346602164));
#170655=CARTESIAN_POINT('Ctrl Pts',(55.8520802190683,4.32676800360642,-171.566123460328));
#170656=CARTESIAN_POINT('Ctrl Pts',(56.1866565229903,3.96999998740382,-171.178434208374));
#170657=CARTESIAN_POINT('Ctrl Pts',(55.8512265932963,3.96993423686634,-171.361424046831));
#170658=CARTESIAN_POINT('Ctrl Pts',(55.7630923089791,4.33856909837021,-171.409535679069));
#170659=CARTESIAN_POINT('',(56.3642936064049,3.96999998000001,-171.871644662643));
#170660=CARTESIAN_POINT('Origin',(54.8887873791231,3.96999970486964,-171.852186214504));
#170661=CARTESIAN_POINT('Origin',(56.3642936064049,4.46999998000001,-171.871644662643));
#170662=CARTESIAN_POINT('Origin',(56.3642936064049,4.46999998000001,-179.64995));
#170663=CARTESIAN_POINT('',(56.3642936064049,3.96999998000001,-171.871644662643));
#170664=CARTESIAN_POINT('',(55.8866301012659,4.32222455627096,-179.64995));
#170665=CARTESIAN_POINT('Origin',(60.,3.46999998000001,-176.84995));
#170666=CARTESIAN_POINT('',(57.,3.96999998000001,-176.84995));
#170667=CARTESIAN_POINT('',(-83.2809572255632,3.96999998000007,-176.84995));
#170668=CARTESIAN_POINT('Origin',(57.,3.46999998000001,-176.84995));
#170669=CARTESIAN_POINT('Origin',(57.,3.46999998000001,-174.34995));
#170670=CARTESIAN_POINT('',(59.5,3.96999998000001,-174.34995));
#170671=CARTESIAN_POINT('Origin',(57.,3.96999998000001,-174.34995));
#170672=CARTESIAN_POINT('Origin',(59.5,3.46999998000001,-174.34995));
#170673=CARTESIAN_POINT('Origin',(59.5,3.46999998000001,-55.24995));
#170674=CARTESIAN_POINT('',(59.5,3.96999998000001,-58.24995));
#170675=CARTESIAN_POINT('',(59.5,3.96999998000001,-174.34995));
#170676=CARTESIAN_POINT('Origin',(59.5,3.46999998000001,-58.24995));
#170677=CARTESIAN_POINT('Ctrl Pts',(40.2576018765703,3.96999998000001,-92.9619213022396));
#170678=CARTESIAN_POINT('Ctrl Pts',(39.9519009607656,3.96999998000002,-92.8065726369586));
#170679=CARTESIAN_POINT('Ctrl Pts',(39.8417798628559,4.28988750369336,-92.7506121713693));
#170680=CARTESIAN_POINT('Ctrl Pts',(42.9469739380577,3.96999998000001,-87.6696743385966));
#170681=CARTESIAN_POINT('Ctrl Pts',(42.6535990616308,3.96999998005189,-87.4723136103566));
#170682=CARTESIAN_POINT('Ctrl Pts',(42.5267665504115,4.30001893486917,-87.4583592347964));
#170683=CARTESIAN_POINT('Ctrl Pts',(45.6032617662856,3.96999998000001,-82.3609901713122));
#170684=CARTESIAN_POINT('Ctrl Pts',(45.2981339154354,3.96999997998722,-82.1711713234106));
#170685=CARTESIAN_POINT('Ctrl Pts',(45.1797873789129,4.30850505828642,-82.1496810404423));
#170686=CARTESIAN_POINT('Ctrl Pts',(50.8772452803079,3.96999998000001,-71.7244637521124));
#170687=CARTESIAN_POINT('Ctrl Pts',(50.5607523082128,3.96999998001296,-71.5306210575042));
#170688=CARTESIAN_POINT('Ctrl Pts',(50.4483866457226,4.32340039588272,-71.5131546212415));
#170689=CARTESIAN_POINT('Ctrl Pts',(53.4945734938964,3.96999998000001,-66.3964343016074));
#170690=CARTESIAN_POINT('Ctrl Pts',(53.1696590969437,3.96999998001539,-66.20755441643));
#170691=CARTESIAN_POINT('Ctrl Pts',(53.0636135580956,4.32979794413352,-66.1851229312852));
#170692=CARTESIAN_POINT('Ctrl Pts',(56.0993680931338,3.96999998000001,-61.0621827299711));
#170693=CARTESIAN_POINT('Ctrl Pts',(55.7583700098454,3.96999998000001,-60.8956682801396));
#170694=CARTESIAN_POINT('Ctrl Pts',(55.6666368275827,4.33549309160632,-60.8508735991007));
#170695=CARTESIAN_POINT('',(55.6666368275827,4.33549309160632,-60.8508735991007));
#170696=CARTESIAN_POINT('Ctrl Pts',(55.6666368275827,4.33549309160632,-60.8508735991007));
#170697=CARTESIAN_POINT('Ctrl Pts',(54.8205608505865,4.33364196429319,-62.5846960616882));
#170698=CARTESIAN_POINT('Ctrl Pts',(53.9903026692869,4.33175386550846,-64.2827945099236));
#170699=CARTESIAN_POINT('Ctrl Pts',(53.1758068650219,4.32982708116484,-65.9451406479148));
#170700=CARTESIAN_POINT('Ctrl Pts',(52.3434513083755,4.32785804750441,-67.6439376678396));
#170701=CARTESIAN_POINT('Ctrl Pts',(51.5275573839763,4.3258486252169,-69.3053969967707));
#170702=CARTESIAN_POINT('Ctrl Pts',(50.7281139966181,4.32379940522285,-70.9295151994433));
#170703=CARTESIAN_POINT('Ctrl Pts',(49.899563188546,4.32167557393118,-72.6127669099562));
#170704=CARTESIAN_POINT('Ctrl Pts',(49.0886828014879,4.31950900276859,-74.2559089319538));
#170705=CARTESIAN_POINT('Ctrl Pts',(48.2955072571905,4.31730276847417,-75.8589672795686));
#170706=CARTESIAN_POINT('Ctrl Pts',(48.1392483326796,4.31686813102153,-76.1747765290183));
#170707=CARTESIAN_POINT('Ctrl Pts',(47.9836766773074,4.31643196122799,-76.4890301985629));
#170708=CARTESIAN_POINT('Ctrl Pts',(47.8287927443473,4.31599429265464,-76.8017286210993));
#170709=CARTESIAN_POINT('Ctrl Pts',(47.824013964662,4.31598078885443,-76.8113765996899));
#170710=CARTESIAN_POINT('Ctrl Pts',(47.8200359612573,4.31596954569576,-76.8194077686504));
#170711=CARTESIAN_POINT('Ctrl Pts',(47.8144583711674,4.31595377082859,-76.8306681161508));
#170712=CARTESIAN_POINT('Ctrl Pts',(47.8143345851444,4.31595342072971,-76.8309180222235));
#170713=CARTESIAN_POINT('Ctrl Pts',(47.8142107994953,4.3159530706297,-76.8311679274349));
#170714=CARTESIAN_POINT('Ctrl Pts',(47.8140870142199,4.31595272052855,-76.8314178317851));
#170715=CARTESIAN_POINT('Ctrl Pts',(47.1001907406593,4.31393361201366,-78.272669901606));
#170716=CARTESIAN_POINT('Ctrl Pts',(46.3987484039203,4.31187755465099,-79.6852882239203));
#170717=CARTESIAN_POINT('Ctrl Pts',(45.7096807250197,4.30978236308995,-81.06923675739));
#170718=CARTESIAN_POINT('Ctrl Pts',(45.015912454009,4.30767287882411,-82.4626261306444));
#170719=CARTESIAN_POINT('Ctrl Pts',(44.3346885815387,4.30552373988916,-83.8269534017042));
#170720=CARTESIAN_POINT('Ctrl Pts',(43.6659786213913,4.30333497175895,-85.16220785781));
#170721=CARTESIAN_POINT('Ctrl Pts',(42.9695469080432,4.30105546699622,-86.5528160497628));
#170722=CARTESIAN_POINT('Ctrl Pts',(42.2866882495013,4.29873298384541,-87.911891050928));
#170723=CARTESIAN_POINT('Ctrl Pts',(41.6174198017565,4.29636985306184,-89.2394474379971));
#170724=CARTESIAN_POINT('Ctrl Pts',(41.0144946503879,4.29424097489616,-90.4354057090332));
#170725=CARTESIAN_POINT('Ctrl Pts',(40.4225998060169,4.2920791485557,-91.6057848751819));
#170726=CARTESIAN_POINT('Ctrl Pts',(39.841779862856,4.28988750369336,-92.7506121713693));
#170727=CARTESIAN_POINT('',(56.0993680931338,3.96999998000001,-61.0621827299711));
#170728=CARTESIAN_POINT('Origin',(56.0993680931338,4.46999998000001,-61.0621827299711));
#170729=CARTESIAN_POINT('Ctrl Pts',(40.2576018765703,3.96999998000001,-92.9619213022396));
#170730=CARTESIAN_POINT('Ctrl Pts',(42.9469753996782,3.96999998000001,-87.669671462365));
#170731=CARTESIAN_POINT('Ctrl Pts',(45.6032617662994,3.96999998000001,-82.3609901712845));
#170732=CARTESIAN_POINT('Ctrl Pts',(48.2402535232915,3.96999998000001,-77.0427269617097));
#170733=CARTESIAN_POINT('Ctrl Pts',(50.8772452802837,3.96999998000001,-71.724463752135));
#170734=CARTESIAN_POINT('Ctrl Pts',(53.4945730592583,3.96999998000001,-66.3964351916018));
#170735=CARTESIAN_POINT('Ctrl Pts',(56.0993680931338,3.96999998000001,-61.0621827299711));
#170736=CARTESIAN_POINT('Origin',(57.,3.46999998000001,-58.24995));
#170737=CARTESIAN_POINT('',(57.,3.96999998000001,-55.74995));
#170738=CARTESIAN_POINT('Origin',(57.,3.96999998000001,-58.24995));
#170739=CARTESIAN_POINT('',(57.,3.46999998000001,-55.24995));
#170740=CARTESIAN_POINT('Origin',(57.,3.46999998000001,-55.74995));
#170741=CARTESIAN_POINT('Origin',(57.,3.46999998000001,-58.24995));
#170742=CARTESIAN_POINT('Origin',(57.,-2.42462934179819E-14,-58.24995));
#170743=CARTESIAN_POINT('',(57.,2.96999998000001,-55.24995));
#170744=CARTESIAN_POINT('',(57.,28.41999998,-55.24995));
#170745=CARTESIAN_POINT('Origin',(57.,2.96999998000001,-58.24995));
#170746=CARTESIAN_POINT('Origin',(57.,2.96999998000001,-58.24995));
#170747=CARTESIAN_POINT('',(57.,2.46999998000001,-55.74995));
#170748=CARTESIAN_POINT('Origin',(57.,2.96999998000001,-55.74995));
#170749=CARTESIAN_POINT('',(59.5,2.46999998000001,-58.24995));
#170750=CARTESIAN_POINT('Origin',(57.,2.46999998000001,-58.24995));
#170751=CARTESIAN_POINT('Origin',(59.5,2.96999998000001,-58.24995));
#170752=CARTESIAN_POINT('Origin',(59.5,2.96999998000001,-55.24995));
#170753=CARTESIAN_POINT('',(59.5,2.46999998000001,-174.34995));
#170754=CARTESIAN_POINT('',(59.5,2.46999998000001,-58.24995));
#170755=CARTESIAN_POINT('Origin',(59.5,2.96999998000001,-174.34995));
#170756=CARTESIAN_POINT('Origin',(57.,2.96999998000001,-174.34995));
#170757=CARTESIAN_POINT('Origin',(57.,2.46999998000001,-174.34995));
#170758=CARTESIAN_POINT('Origin',(57.077763566464,1.96999998000001,-179.64995));
#170759=CARTESIAN_POINT('',(57.077763566464,2.46999998000001,-171.871644662643));
#170760=CARTESIAN_POINT('',(57.077763566464,2.46999998000001,-176.84995));
#170761=CARTESIAN_POINT('Origin',(57.077763566464,1.96999998000001,-171.871644662643));
#170762=CARTESIAN_POINT('',(56.5940537057312,1.84341099694893,-179.64995));
#170763=CARTESIAN_POINT('Ctrl Pts',(56.9026784671178,2.46999996978156,-171.178999526256));
#170764=CARTESIAN_POINT('Ctrl Pts',(56.3489175136905,2.47012711531616,-171.477038599322));
#170765=CARTESIAN_POINT('Ctrl Pts',(56.4736088945599,1.8573874935658,-171.409915902424));
#170766=CARTESIAN_POINT('Ctrl Pts',(57.0276127026275,2.4699999696149,-171.411480993498));
#170767=CARTESIAN_POINT('Ctrl Pts',(56.4096617452283,2.47013088089768,-171.619083147105));
#170768=CARTESIAN_POINT('Ctrl Pts',(56.5595092645592,1.84739527439962,-171.564880044108));
#170769=CARTESIAN_POINT('Ctrl Pts',(57.0884505381248,2.46999996953445,-171.671060999849));
#170770=CARTESIAN_POINT('Ctrl Pts',(56.4344504334064,2.4701327527474,-171.760758212924));
#170771=CARTESIAN_POINT('Ctrl Pts',(56.6013299245167,1.84257107601692,-171.737940501487));
#170772=CARTESIAN_POINT('Ctrl Pts',(57.0763566157493,2.46999996955045,-171.938278709053));
#170773=CARTESIAN_POINT('Ctrl Pts',(56.4294059961933,2.47013238231052,-171.908444781729));
#170774=CARTESIAN_POINT('Ctrl Pts',(56.5930162481435,1.8435307818068,-171.916062071863));
#170775=CARTESIAN_POINT('',(56.9324803875071,2.46999998000001,-171.237717270032));
#170776=CARTESIAN_POINT('Origin',(55.6391139723683,2.47000037313163,-171.847693896014));
#170777=CARTESIAN_POINT('Origin',(56.9324803875071,1.96999998000001,-171.237717270032));
#170778=CARTESIAN_POINT('Ctrl Pts',(40.1772697316389,2.46999998000002,-136.935824627502));
#170779=CARTESIAN_POINT('Ctrl Pts',(39.5564442323333,2.46999998000002,-137.244681069688));
#170780=CARTESIAN_POINT('Ctrl Pts',(39.7525219240432,1.81208306781681,-137.147133758372));
#170781=CARTESIAN_POINT('Ctrl Pts',(43.0113356415696,2.46999998000002,-142.632517793947));
#170782=CARTESIAN_POINT('Ctrl Pts',(42.3628976020159,2.46999998000001,-142.852500243629));
#170783=CARTESIAN_POINT('Ctrl Pts',(42.5829522730059,1.82186961480941,-142.84383290998));
#170784=CARTESIAN_POINT('Ctrl Pts',(45.8169723643538,2.46999998000002,-148.343102920422));
#170785=CARTESIAN_POINT('Ctrl Pts',(45.1914659347836,2.46999998002509,-148.581690034117));
#170786=CARTESIAN_POINT('Ctrl Pts',(45.385956606115,1.82990288117652,-148.554412051289));
#170787=CARTESIAN_POINT('Ctrl Pts',(51.3962007668006,2.46999998000001,-159.779920646508));
#170788=CARTESIAN_POINT('Ctrl Pts',(50.7878173967191,2.46999997997542,-160.008583439984));
#170789=CARTESIAN_POINT('Ctrl Pts',(50.9608945753704,1.84386393970469,-159.991229777381));
#170790=CARTESIAN_POINT('Ctrl Pts',(54.1694331140562,2.46999998000001,-165.506332215193));
#170791=CARTESIAN_POINT('Ctrl Pts',(53.5753070147928,2.46999998000001,-165.745313705806));
#170792=CARTESIAN_POINT('Ctrl Pts',(53.7324859673961,1.84977562860519,-165.717643463624));
#170793=CARTESIAN_POINT('Ctrl Pts',(56.9324803875071,2.46999998000001,-171.237717270032));
#170794=CARTESIAN_POINT('Ctrl Pts',(56.3632322083114,2.46999998,-171.512146507354));
#170795=CARTESIAN_POINT('Ctrl Pts',(56.4941621559325,1.85499746228791,-171.449026400902));
#170796=CARTESIAN_POINT('',(40.1772697316389,2.46999998000002,-136.935824627502));
#170797=CARTESIAN_POINT('Ctrl Pts',(40.1772697316389,2.46999998000002,-136.935824627502));
#170798=CARTESIAN_POINT('Ctrl Pts',(43.0113367121144,2.46999998000002,-142.632519945825));
#170799=CARTESIAN_POINT('Ctrl Pts',(45.8169723643453,2.46999998000002,-148.343102920405));
#170800=CARTESIAN_POINT('Ctrl Pts',(48.6065865655743,2.46999998000001,-154.061511783466));
#170801=CARTESIAN_POINT('Ctrl Pts',(51.3962007668033,2.46999998000001,-159.779920646528));
#170802=CARTESIAN_POINT('Ctrl Pts',(54.1694328122146,2.46999998000001,-165.506331589084));
#170803=CARTESIAN_POINT('Ctrl Pts',(56.9324803874897,2.46999998000001,-171.23771727004));
#170804=CARTESIAN_POINT('Origin',(40.1772697316389,1.96999998000002,-136.935824627502));
#170805=CARTESIAN_POINT('Ctrl Pts',(39.7525219240431,1.81208306781681,-137.147133758372));
#170806=CARTESIAN_POINT('Ctrl Pts',(39.5564442323333,2.46999998000002,-137.244681069688));
#170807=CARTESIAN_POINT('Ctrl Pts',(40.1772697316389,2.46999998000002,-136.935824627502));
#170808=CARTESIAN_POINT('Ctrl Pts',(39.5010130025154,1.83757362466031,-136.660631009723));
#170809=CARTESIAN_POINT('Ctrl Pts',(39.347413825743,2.46999998000002,-136.73953631121));
#170810=CARTESIAN_POINT('Ctrl Pts',(39.950904654581,2.46999998000002,-136.480813185142));
#170811=CARTESIAN_POINT('Ctrl Pts',(39.3161891891914,1.86369282090684,-136.153853436174));
#170812=CARTESIAN_POINT('Ctrl Pts',(39.1941245109705,2.46999998000001,-136.207552272104));
#170813=CARTESIAN_POINT('Ctrl Pts',(39.7845702702201,2.46999998000002,-136.007478819399));
#170814=CARTESIAN_POINT('Ctrl Pts',(39.0651099631573,1.91665698917066,-135.104438767164));
#170815=CARTESIAN_POINT('Ctrl Pts',(39.0102330104275,2.46999998000002,-135.126982248827));
#170816=CARTESIAN_POINT('Ctrl Pts',(39.5585989668938,2.46999998000002,-135.028737339162));
#170817=CARTESIAN_POINT('Ctrl Pts',(39.,1.94368731593243,-134.55780009522));
#170818=CARTESIAN_POINT('Ctrl Pts',(38.9729770085358,2.46999998000002,-134.572511021856));
#170819=CARTESIAN_POINT('Ctrl Pts',(39.5000000000492,2.46999998000002,-134.519624150969));
#170820=CARTESIAN_POINT('Ctrl Pts',(39.,1.96999998000002,-134.012863078852));
#170821=CARTESIAN_POINT('Ctrl Pts',(39.,2.46999998000002,-134.012863078852));
#170822=CARTESIAN_POINT('Ctrl Pts',(39.5,2.46999998000002,-134.012863078852));
#170823=CARTESIAN_POINT('',(39.5,2.46999998000002,-134.012863078852));
#170824=CARTESIAN_POINT('Ctrl Pts',(39.5,2.46999998000002,-134.012863078852));
#170825=CARTESIAN_POINT('Ctrl Pts',(39.5,2.46999998000002,-134.194202123599));
#170826=CARTESIAN_POINT('Ctrl Pts',(39.5074991738613,2.46999998000002,-134.375559257497));
#170827=CARTESIAN_POINT('Ctrl Pts',(39.5222608830473,2.46999998000002,-134.556078177936));
#170828=CARTESIAN_POINT('Ctrl Pts',(39.5372803972934,2.46999998000002,-134.739749761157));
#170829=CARTESIAN_POINT('Ctrl Pts',(39.5598184209786,2.46999998000002,-134.92255477599));
#170830=CARTESIAN_POINT('Ctrl Pts',(39.5896791401065,2.46999998000002,-135.10359544212));
#170831=CARTESIAN_POINT('Ctrl Pts',(39.6126641240196,2.46999998000002,-135.242949647919));
#170832=CARTESIAN_POINT('Ctrl Pts',(39.6399889131326,2.46999998000002,-135.381258722717));
#170833=CARTESIAN_POINT('Ctrl Pts',(39.671584618531,2.46999998000002,-135.518108079287));
#170834=CARTESIAN_POINT('Ctrl Pts',(39.7480265101501,2.46999998000002,-135.849198129379));
#170835=CARTESIAN_POINT('Ctrl Pts',(39.8488754308753,2.46999998000002,-136.172910839316));
#170836=CARTESIAN_POINT('Ctrl Pts',(39.9762245150674,2.46999998000002,-136.488613556872));
#170837=CARTESIAN_POINT('Ctrl Pts',(40.0371049338934,2.46999998000002,-136.639538188888));
#170838=CARTESIAN_POINT('Ctrl Pts',(40.1040424074826,2.46999998000002,-136.788632003769));
#170839=CARTESIAN_POINT('Ctrl Pts',(40.1772697316389,2.46999998000002,-136.935824627502));
#170840=CARTESIAN_POINT('Origin',(39.5,1.96999998000002,-134.012863078852));
#170841=CARTESIAN_POINT('Origin',(39.5,1.96999998000002,-55.24995));
#170842=CARTESIAN_POINT('',(39.5,2.46999998000002,-98.0457798926543));
#170843=CARTESIAN_POINT('',(39.5,2.46999998000002,-55.24995));
#170844=CARTESIAN_POINT('Origin',(39.5,1.96999998000002,-98.0457798926543));
#170845=CARTESIAN_POINT('Ctrl Pts',(39.,1.96999998000002,-98.0457798926543));
#170846=CARTESIAN_POINT('Ctrl Pts',(39.,2.46999998000002,-98.0457798926543));
#170847=CARTESIAN_POINT('Ctrl Pts',(39.5,2.46999998000002,-98.0457798926543));
#170848=CARTESIAN_POINT('Ctrl Pts',(39.,1.9436152588707,-97.4993505936135));
#170849=CARTESIAN_POINT('Ctrl Pts',(38.9728980858888,2.46999998000002,-97.4844974242186));
#170850=CARTESIAN_POINT('Ctrl Pts',(39.5000000026568,2.46999998000002,-97.5376233160284));
#170851=CARTESIAN_POINT('Ctrl Pts',(39.0635968999967,1.91714776114478,-96.9640681661487));
#170852=CARTESIAN_POINT('Ctrl Pts',(39.0092761144151,2.46999998000002,-96.9417291681898));
#170853=CARTESIAN_POINT('Ctrl Pts',(39.5572372093883,2.46999998000002,-97.0390962063516));
#170854=CARTESIAN_POINT('Ctrl Pts',(39.312853918045,1.86422808123875,-95.9152577284902));
#170855=CARTESIAN_POINT('Ctrl Pts',(39.1914722350304,2.46999998000002,-95.8620324116114));
#170856=CARTESIAN_POINT('Ctrl Pts',(39.7815685268491,2.46999998000002,-96.0609362825129));
#170857=CARTESIAN_POINT('Ctrl Pts',(39.5010226636067,1.83757264792979,-95.3979932721737));
#170858=CARTESIAN_POINT('Ctrl Pts',(39.3474064560569,2.46999998000002,-95.3191244694837));
#170859=CARTESIAN_POINT('Ctrl Pts',(39.9509186646822,2.46999998000002,-95.5778016189611));
#170860=CARTESIAN_POINT('Ctrl Pts',(39.7525219240431,1.81208306781681,-94.9115092131337));
#170861=CARTESIAN_POINT('Ctrl Pts',(39.5564442323333,2.46999998000002,-94.8139619018179));
#170862=CARTESIAN_POINT('Ctrl Pts',(40.1772697316389,2.46999998000002,-95.1228183440041));
#170863=CARTESIAN_POINT('',(40.177269731639,2.46999998000002,-95.1228183440042));
#170864=CARTESIAN_POINT('',(39.7525219090133,1.81208319014795,-94.9115093405122));
#170865=CARTESIAN_POINT('Origin',(40.1772697316389,1.96999998000002,-95.1228183440041));
#170866=CARTESIAN_POINT('Ctrl Pts',(39.0000000024628,1.96999998000006,-98.0457798926544));
#170867=CARTESIAN_POINT('Ctrl Pts',(39.0000023795683,1.96570120570202,-97.9567519908293));
#170868=CARTESIAN_POINT('Ctrl Pts',(39.0017233767913,1.96125307100217,-97.8646389244035));
#170869=CARTESIAN_POINT('Ctrl Pts',(39.0055233301077,1.95663173737879,-97.7695025339163));
#170870=CARTESIAN_POINT('Ctrl Pts',(39.006999653108,1.9548362992372,-97.7325410162995));
#170871=CARTESIAN_POINT('Ctrl Pts',(39.0087900561879,1.95301496883546,-97.6951235500827));
#170872=CARTESIAN_POINT('Ctrl Pts',(39.0109166836443,1.95116738479208,-97.657255353352));
#170873=CARTESIAN_POINT('Ctrl Pts',(39.0147168933816,1.94786581598601,-97.5895861950714));
#170874=CARTESIAN_POINT('Ctrl Pts',(39.0195904985651,1.94447998345472,-97.5204771269352));
#170875=CARTESIAN_POINT('Ctrl Pts',(39.025667717316,1.94101327943105,-97.4499659367276));
#170876=CARTESIAN_POINT('Ctrl Pts',(39.0287063266914,1.93927992741922,-97.4147103416238));
#170877=CARTESIAN_POINT('Ctrl Pts',(39.0320459334948,1.93752636333294,-97.3791042242764));
#170878=CARTESIAN_POINT('Ctrl Pts',(39.0357031841201,1.9357538621328,-97.3431535242875));
#170879=CARTESIAN_POINT('Ctrl Pts',(39.0375318094328,1.93486761153271,-97.3251781742931));
#170880=CARTESIAN_POINT('Ctrl Pts',(39.0394398505803,1.93397662688184,-97.3071166789648));
#170881=CARTESIAN_POINT('Ctrl Pts',(39.0414294116136,1.93308109865202,-97.2889698225087));
#170882=CARTESIAN_POINT('Ctrl Pts',(39.0424241921302,1.9326333345371,-97.2798963942806));
#170883=CARTESIAN_POINT('Ctrl Pts',(39.043439352924,1.93218443455118,-97.2708016258043));
#170884=CARTESIAN_POINT('Ctrl Pts',(39.0444751581284,1.93173442564936,-97.2616856194871));
#170885=CARTESIAN_POINT('Ctrl Pts',(39.0449930607306,1.93150942119844,-97.2571276163284));
#170886=CARTESIAN_POINT('Ctrl Pts',(39.0455161244538,1.93128413951999,-97.2525643037117));
#170887=CARTESIAN_POINT('Ctrl Pts',(39.0460443823768,1.93105858419778,-97.2479956947328));
#170888=CARTESIAN_POINT('Ctrl Pts',(39.0465726402997,1.93083302887557,-97.2434270857539));
#170889=CARTESIAN_POINT('Ctrl Pts',(39.0472468859898,1.9305481048655,-97.2376563271244));
#170890=CARTESIAN_POINT('Ctrl Pts',(39.0476447718804,1.93038110095292,-97.2342739919009));
#170891=CARTESIAN_POINT('Ctrl Pts',(39.0547397971647,1.92740311904867,-97.1739608355568));
#170892=CARTESIAN_POINT('Ctrl Pts',(39.0630811872692,1.92424565323167,-97.109804789609));
#170893=CARTESIAN_POINT('Ctrl Pts',(39.0729996746766,1.92088476300344,-97.0418531112313));
#170894=CARTESIAN_POINT('Ctrl Pts',(39.0826231429977,1.91762384031288,-96.9759226122161));
#170895=CARTESIAN_POINT('Ctrl Pts',(39.0937316247875,1.91417106351811,-96.9064185529857));
#170896=CARTESIAN_POINT('Ctrl Pts',(39.1066630521812,1.9105202065299,-96.8334125920886));
#170897=CARTESIAN_POINT('Ctrl Pts',(39.1162799426628,1.90780512406058,-96.7791192562424));
#170898=CARTESIAN_POINT('Ctrl Pts',(39.1269058081946,1.90498076441849,-96.7228896719113));
#170899=CARTESIAN_POINT('Ctrl Pts',(39.1386912625358,1.90205227654554,-96.6647659242202));
#170900=CARTESIAN_POINT('Ctrl Pts',(39.1460189431004,1.90023147074128,-96.6286271175209));
#170901=CARTESIAN_POINT('Ctrl Pts',(39.1537950911084,1.89837054965722,-96.5917562863848));
#170902=CARTESIAN_POINT('Ctrl Pts',(39.1620576208011,1.89647235503082,-96.5541660084023));
#170903=CARTESIAN_POINT('Ctrl Pts',(39.1661888856474,1.89552325771762,-96.5353708694111));
#170904=CARTESIAN_POINT('Ctrl Pts',(39.1704417732556,1.89456484623122,-96.5163958745825));
#170905=CARTESIAN_POINT('Ctrl Pts',(39.1748211237916,1.89359762560557,-96.4972428190492));
#170906=CARTESIAN_POINT('Ctrl Pts',(39.1770107990596,1.89311401529275,-96.4876662912825));
#170907=CARTESIAN_POINT('Ctrl Pts',(39.179232091689,1.89262820293435,-96.4780452486739));
#170908=CARTESIAN_POINT('Ctrl Pts',(39.18148561435,1.89214025762443,-96.4683799240122));
#170909=CARTESIAN_POINT('Ctrl Pts',(39.1826123756804,1.89189628496947,-96.4635472616813));
#170910=CARTESIAN_POINT('Ctrl Pts',(39.1837471946203,1.89165177909316,-96.4587035288602));
#170911=CARTESIAN_POINT('Ctrl Pts',(39.1848901481332,1.89140674918914,-96.4538487554583));
#170912=CARTESIAN_POINT('Ctrl Pts',(39.1854616248896,1.89128423423713,-96.4514213687574));
#170913=CARTESIAN_POINT('Ctrl Pts',(39.1860351352956,1.89116158827922,-96.4489912219127));
#170914=CARTESIAN_POINT('Ctrl Pts',(39.1866106889937,1.89103881250212,-96.4465583187171));
#170915=CARTESIAN_POINT('Ctrl Pts',(39.1871862426919,1.89091603672502,-96.4441254155214));
#170916=CARTESIAN_POINT('Ctrl Pts',(39.1874086280478,1.89086852694691,-96.4431840239398));
#170917=CARTESIAN_POINT('Ctrl Pts',(39.1883434896272,1.89067009691365,-96.4392513438899));
#170918=CARTESIAN_POINT('Ctrl Pts',(39.2039030113169,1.88736749418148,-96.373797139888));
#170919=CARTESIAN_POINT('Ctrl Pts',(39.2194686344583,1.88423223388531,-96.3125811755131));
#170920=CARTESIAN_POINT('Ctrl Pts',(39.234696896302,1.8812995042039,-96.2555688744947));
#170921=CARTESIAN_POINT('Ctrl Pts',(39.2500971432766,1.87833365282396,-96.1979126872501));
#170922=CARTESIAN_POINT('Ctrl Pts',(39.2651521559665,1.87557453440026,-96.1445550998185));
#170923=CARTESIAN_POINT('Ctrl Pts',(39.2795546795664,1.87303882497464,-96.0954463781737));
#170924=CARTESIAN_POINT('Ctrl Pts',(39.2940772709897,1.8704819763987,-96.045928257629));
#170925=CARTESIAN_POINT('Ctrl Pts',(39.3079363553328,1.86815189115088,-96.0007296292346));
#170926=CARTESIAN_POINT('Ctrl Pts',(39.3208676806068,1.86605171503959,-95.9597934618329));
#170927=CARTESIAN_POINT('Ctrl Pts',(39.3338976046489,1.86393552550563,-95.9185451643449));
#170928=CARTESIAN_POINT('Ctrl Pts',(39.3459855447184,1.86205241809051,-95.8816241304791));
#170929=CARTESIAN_POINT('Ctrl Pts',(39.3569133198007,1.86039707135961,-95.8489731675027));
#170930=CARTESIAN_POINT('Ctrl Pts',(39.3678631601099,1.85873838217327,-95.8162562761098));
#170931=CARTESIAN_POINT('Ctrl Pts',(39.3776482049348,1.85730808413837,-95.7878263605496));
#170932=CARTESIAN_POINT('Ctrl Pts',(39.3861007469163,1.85609710073972,-95.7636330869288));
#170933=CARTESIAN_POINT('Ctrl Pts',(39.3945648893821,1.85488445535656,-95.7394066098418));
#170934=CARTESIAN_POINT('Ctrl Pts',(39.401692939157,1.85389150890907,-95.7194281489415));
#170935=CARTESIAN_POINT('Ctrl Pts',(39.4073673786352,1.8531092421283,-95.7036590330933));
#170936=CARTESIAN_POINT('Ctrl Pts',(39.4107258929006,1.85264624412601,-95.6943258115951));
#170937=CARTESIAN_POINT('Ctrl Pts',(39.4135761564115,1.852257070151,-95.6864674008105));
#170938=CARTESIAN_POINT('Ctrl Pts',(39.4159020403612,1.85194027203048,-95.6800782245838));
#170939=CARTESIAN_POINT('Ctrl Pts',(39.4177341500928,1.85169072866027,-95.675045440406));
#170940=CARTESIAN_POINT('Ctrl Pts',(39.4192410137785,1.85148609903756,-95.6709243205286));
#170941=CARTESIAN_POINT('Ctrl Pts',(39.4204173925654,1.85132587896651,-95.6677130149262));
#170942=CARTESIAN_POINT('Ctrl Pts',(39.4210055819589,1.85124576893097,-95.6661073621251));
#170943=CARTESIAN_POINT('Ctrl Pts',(39.4215111848868,1.8511767702981,-95.6647291751866));
#170944=CARTESIAN_POINT('Ctrl Pts',(39.4219337654556,1.85111883252293,-95.6635782981435));
#170945=CARTESIAN_POINT('Ctrl Pts',(39.42214505574,1.85108986363535,-95.6630028596219));
#170946=CARTESIAN_POINT('Ctrl Pts',(39.4223355926106,1.85106366052513,-95.6624842493419));
#170947=CARTESIAN_POINT('Ctrl Pts',(39.4225053348427,1.85104021921531,-95.662022452596));
#170948=CARTESIAN_POINT('Ctrl Pts',(39.4225902059587,1.85102849856041,-95.6617915542231));
#170949=CARTESIAN_POINT('Ctrl Pts',(39.422669878551,1.85101746839093,-95.6615748592819));
#170950=CARTESIAN_POINT('Ctrl Pts',(39.422744348315,1.8510071282838,-95.6613723662314));
#170951=CARTESIAN_POINT('Ctrl Pts',(39.422781583197,1.85100195823023,-95.6612711197062));
#170952=CARTESIAN_POINT('Ctrl Pts',(39.4228175174062,1.85099696069703,-95.6611734236659));
#170953=CARTESIAN_POINT('Ctrl Pts',(39.4228514987551,1.85099222175874,-95.661081052689));
#170954=CARTESIAN_POINT('Ctrl Pts',(39.4228854801041,1.85098748282044,-95.6609886817121));
#170955=CARTESIAN_POINT('Ctrl Pts',(39.4229187089809,1.85098281980264,-95.6608980492788));
#170956=CARTESIAN_POINT('Ctrl Pts',(39.4233430620384,1.85092351009055,-95.6597454129));
#170957=CARTESIAN_POINT('Ctrl Pts',(39.4544661950375,1.84657358489319,-95.5752081280062));
#170958=CARTESIAN_POINT('Ctrl Pts',(39.4861260597182,1.84238472192749,-95.4944667312749));
#170959=CARTESIAN_POINT('Ctrl Pts',(39.5179232619264,1.8383884084295,-95.417491701329));
#170960=CARTESIAN_POINT('Ctrl Pts',(39.5502997984827,1.83431928344136,-95.3391142121822));
#170961=CARTESIAN_POINT('Ctrl Pts',(39.5828183403341,1.8304494528387,-95.264641080767));
#170962=CARTESIAN_POINT('Ctrl Pts',(39.6150932788069,1.82678245847445,-95.1940123862938));
#170963=CARTESIAN_POINT('Ctrl Pts',(39.6482525478298,1.82301498877866,-95.1214484716407));
#170964=CARTESIAN_POINT('Ctrl Pts',(39.6811543457219,1.8194612646841,-95.0529420298684));
#170965=CARTESIAN_POINT('Ctrl Pts',(39.7134238132575,1.8160993657089,-94.9884058941551));
#170966=CARTESIAN_POINT('Ctrl Pts',(39.7265686486177,1.81472990993844,-94.9621173637418));
#170967=CARTESIAN_POINT('Ctrl Pts',(39.7396090786083,1.81339202353714,-94.9364874232129));
#170968=CARTESIAN_POINT('Ctrl Pts',(39.7525219085452,1.81208326361859,-94.911509475135));
#170969=CARTESIAN_POINT('Ctrl Pts',(40.1772697316388,2.46999998000002,-95.1228183440041));
#170970=CARTESIAN_POINT('Ctrl Pts',(40.0557143101432,2.46999998000002,-95.367154206676));
#170971=CARTESIAN_POINT('Ctrl Pts',(39.9506490904769,2.46999998000002,-95.6194942161999));
#170972=CARTESIAN_POINT('Ctrl Pts',(39.862036785698,2.46999998000002,-95.876484568063));
#170973=CARTESIAN_POINT('Ctrl Pts',(39.785571796048,2.46999998000002,-96.0982456953059));
#170974=CARTESIAN_POINT('Ctrl Pts',(39.721358807228,2.46999998000002,-96.3234708895919));
#170975=CARTESIAN_POINT('Ctrl Pts',(39.6694028678064,2.46999998000002,-96.5500162443606));
#170976=CARTESIAN_POINT('Ctrl Pts',(39.5883957972391,2.46999998000002,-96.903234293053));
#170977=CARTESIAN_POINT('Ctrl Pts',(39.5360425809489,2.46999998000002,-97.2613436845068));
#170978=CARTESIAN_POINT('Ctrl Pts',(39.5132030141794,2.46999998000002,-97.624491207193));
#170979=CARTESIAN_POINT('Ctrl Pts',(39.5044179952615,2.46999998000002,-97.7641723968143));
#170980=CARTESIAN_POINT('Ctrl Pts',(39.5,2.46999998000002,-97.9045990595786));
#170981=CARTESIAN_POINT('Ctrl Pts',(39.5,2.46999998000002,-98.0457798926543));
#170982=CARTESIAN_POINT('Ctrl Pts',(56.8241336558648,2.46999998000001,-61.0456553781473));
#170983=CARTESIAN_POINT('Ctrl Pts',(56.2546351764993,2.46999997999971,-60.771071756775));
#170984=CARTESIAN_POINT('Ctrl Pts',(56.3858722762367,1.85477834326924,-60.8343476935333));
#170985=CARTESIAN_POINT('Ctrl Pts',(54.0775409927178,2.46999998000001,-66.7422070144501));
#170986=CARTESIAN_POINT('Ctrl Pts',(53.4833299990046,2.46999998010366,-66.5027538223377));
#170987=CARTESIAN_POINT('Ctrl Pts',(53.6406504195319,1.84956966069372,-66.5308964372918));
#170988=CARTESIAN_POINT('Ctrl Pts',(51.3208277321712,2.46999998000001,-72.433816174677));
#170989=CARTESIAN_POINT('Ctrl Pts',(50.7124694309102,2.46999998,-72.2045026335238));
#170990=CARTESIAN_POINT('Ctrl Pts',(50.8855763842636,1.84367574323028,-72.2225074476142));
#170991=CARTESIAN_POINT('Ctrl Pts',(45.7749111060821,2.46999998000002,-83.8011613014347));
#170992=CARTESIAN_POINT('Ctrl Pts',(45.1494935787875,2.46999998,-83.5619433099981));
#170993=CARTESIAN_POINT('Ctrl Pts',(45.3439391239116,1.82976876705617,-83.5898527848085));
#170994=CARTESIAN_POINT('Ctrl Pts',(42.9860576374377,2.46999998000002,-89.47707155374));
#170995=CARTESIAN_POINT('Ctrl Pts',(42.3379617991063,2.4699999799188,-89.2560712524343));
#170996=CARTESIAN_POINT('Ctrl Pts',(42.5577095805282,1.8217713755538,-89.2657567838175));
#170997=CARTESIAN_POINT('Ctrl Pts',(40.1690969821091,2.46999998000002,-95.1392460099596));
#170998=CARTESIAN_POINT('Ctrl Pts',(39.5482160849935,2.46999998000026,-94.8303544504712));
#170999=CARTESIAN_POINT('Ctrl Pts',(39.7443638707198,1.81204072079829,-94.9279389902309));
#171000=CARTESIAN_POINT('',(56.8161649572467,2.46999998000001,-61.0621827299711));
#171001=CARTESIAN_POINT('',(56.377904566775,1.85477723331148,-60.8508735991007));
#171002=CARTESIAN_POINT('Origin',(56.8161649572467,1.96999998000001,-61.0621827299711));
#171003=CARTESIAN_POINT('Ctrl Pts',(39.7525219240432,1.8120830678168,-94.9115092131337));
#171004=CARTESIAN_POINT('Ctrl Pts',(41.0321872437539,1.8165076616864,-92.3359756573271));
#171005=CARTESIAN_POINT('Ctrl Pts',(42.3688267391817,1.8209983325356,-89.6310450958057));
#171006=CARTESIAN_POINT('Ctrl Pts',(44.4594400294678,1.82716626150394,-85.3795537449517));
#171007=CARTESIAN_POINT('Ctrl Pts',(45.1705837525141,1.82914107837277,-83.9300407099051));
#171008=CARTESIAN_POINT('Ctrl Pts',(46.2587091665782,1.83202090427287,-81.7072472801921));
#171009=CARTESIAN_POINT('Ctrl Pts',(46.808124123156,1.83344150427555,-80.5837195960498));
#171010=CARTESIAN_POINT('Ctrl Pts',(47.4584728770403,1.83508731520312,-79.2517081016338));
#171011=CARTESIAN_POINT('Ctrl Pts',(47.7859880572214,1.8359111325951,-78.5803950553633));
#171012=CARTESIAN_POINT('Ctrl Pts',(47.9679389518065,1.83636798435703,-78.2073063487587));
#171013=CARTESIAN_POINT('Ctrl Pts',(48.0561756206575,1.83658937557106,-78.0263353058769));
#171014=CARTESIAN_POINT('Ctrl Pts',(48.1032839361376,1.83670755389347,-77.9297068476094));
#171015=CARTESIAN_POINT('Ctrl Pts',(48.1100653589499,1.83672456568112,-77.9157965646182));
#171016=CARTESIAN_POINT('Ctrl Pts',(50.6741769084835,1.84315675199189,-72.6561333006624));
#171017=CARTESIAN_POINT('Ctrl Pts',(53.4284137093914,1.84917961846372,-66.9712432304567));
#171018=CARTESIAN_POINT('Ctrl Pts',(56.377904566775,1.85477723331148,-60.8508735991007));
#171019=CARTESIAN_POINT('Ctrl Pts',(56.8161649572467,2.46999998000001,-61.0621827299711));
#171020=CARTESIAN_POINT('Ctrl Pts',(54.0722086604215,2.46999998000001,-66.7532163030615));
#171021=CARTESIAN_POINT('Ctrl Pts',(51.3181460106093,2.46999998000001,-72.4393128412014));
#171022=CARTESIAN_POINT('Ctrl Pts',(48.5478694191173,2.46999998000001,-78.1174887380514));
#171023=CARTESIAN_POINT('Ctrl Pts',(45.7775928276252,2.46999998000002,-83.7956646349013));
#171024=CARTESIAN_POINT('Ctrl Pts',(42.9914528488282,2.46999998000002,-89.4660911391003));
#171025=CARTESIAN_POINT('Ctrl Pts',(40.1772697316389,2.46999998000002,-95.1228183440041));
#171026=CARTESIAN_POINT('Ctrl Pts',(39.,3.43040799630139,-96.9953075914435));
#171027=CARTESIAN_POINT('Ctrl Pts',(39.,2.57465910981969,-95.8526291198646));
#171028=CARTESIAN_POINT('Ctrl Pts',(39.7537608994937,1.84791623342104,-94.8822119187994));
#171029=CARTESIAN_POINT('Ctrl Pts',(39.,2.33014533501219,-97.8192913905431));
#171030=CARTESIAN_POINT('Ctrl Pts',(38.999999999981,1.53000434811038,-96.6793434201897));
#171031=CARTESIAN_POINT('Ctrl Pts',(39.7190156956536,0.840907950229365,
-95.7061778087214));
#171032=CARTESIAN_POINT('Ctrl Pts',(39.,1.18987438490308,-98.6014496888564));
#171033=CARTESIAN_POINT('Ctrl Pts',(39.,0.446333199097853,-97.4659491905239));
#171034=CARTESIAN_POINT('Ctrl Pts',(39.6851690092259,-0.199333099759264,
-96.4883539675537));
#171035=CARTESIAN_POINT('Ctrl Pts',(39.,-0.603530653465397,-99.6882419580977));
#171036=CARTESIAN_POINT('Ctrl Pts',(39.,-1.25780446014918,-98.559487559907));
#171037=CARTESIAN_POINT('Ctrl Pts',(39.6371434881247,-1.8297111910827,-97.5751461950565));
#171038=CARTESIAN_POINT('Ctrl Pts',(39.,-1.21720470538169,-100.036841989918));
#171039=CARTESIAN_POINT('Ctrl Pts',(39.0000000000024,-1.84018826968395,
-98.9100164272499));
#171040=CARTESIAN_POINT('Ctrl Pts',(39.6215593402708,-2.38668766534493,
-97.9237462143533));
#171041=CARTESIAN_POINT('Ctrl Pts',(39.,-2.45808495944723,-100.689411149812));
#171042=CARTESIAN_POINT('Ctrl Pts',(38.9999999999976,-3.01723045502807,
-99.5661131270649));
#171043=CARTESIAN_POINT('Ctrl Pts',(39.5921043556329,-3.51112289490215,
-98.5763153513056));
#171044=CARTESIAN_POINT('Ctrl Pts',(39.,-3.08699664896505,-100.99454469153));
#171045=CARTESIAN_POINT('Ctrl Pts',(39.,-3.61357786082266,-99.8729679343378));
#171046=CARTESIAN_POINT('Ctrl Pts',(39.5781831338039,-4.08013648047372,
-98.8814488059413));
#171047=CARTESIAN_POINT('Ctrl Pts',(39.,-3.72540427022208,-101.27597320326));
#171048=CARTESIAN_POINT('Ctrl Pts',(39.,-4.21906468716858,-100.156127274739));
#171049=CARTESIAN_POINT('Ctrl Pts',(39.565238633238,-4.65691791624337,-99.1628773826332));
#171050=CARTESIAN_POINT('',(39.5857301728914,-3.7824234709496,-98.7152328423687));
#171051=CARTESIAN_POINT('Ctrl Pts',(39.5857305622805,-3.78242133832598,
-98.7152357168537));
#171052=CARTESIAN_POINT('Ctrl Pts',(39.5925013633664,-3.50507902913527,
-98.566659849342));
#171053=CARTESIAN_POINT('Ctrl Pts',(39.5995343541385,-3.22737884836422,
-98.4116495172459));
#171054=CARTESIAN_POINT('Ctrl Pts',(39.6068290975047,-2.94890292239653,
-98.2500352611615));
#171055=CARTESIAN_POINT('Ctrl Pts',(39.6124208939522,-2.73543678447178,
-98.1261496112259));
#171056=CARTESIAN_POINT('Ctrl Pts',(39.6181738810536,-2.52128731141673,
-97.9982124747704));
#171057=CARTESIAN_POINT('Ctrl Pts',(39.6240733158027,-2.30678756415044,
-97.8664764985964));
#171058=CARTESIAN_POINT('Ctrl Pts',(39.6296232126047,-2.10499679740912,
-97.7425457994774));
#171059=CARTESIAN_POINT('Ctrl Pts',(39.6353027291037,-1.90289595837455,
-97.6152528102953));
#171060=CARTESIAN_POINT('Ctrl Pts',(39.6410984012804,-1.70080336620325,
-97.484827319336));
#171061=CARTESIAN_POINT('Ctrl Pts',(39.6450625324154,-1.56257582117692,
-97.3956187282123));
#171062=CARTESIAN_POINT('Ctrl Pts',(39.6490809808139,-1.42435295854234,
-97.3049450480543));
#171063=CARTESIAN_POINT('Ctrl Pts',(39.6531490421426,-1.28624913053006,
-97.212886559647));
#171064=CARTESIAN_POINT('Ctrl Pts',(39.6682655575824,-0.773068900499357,
-96.8708062789114));
#171065=CARTESIAN_POINT('Ctrl Pts',(39.6840971342397,-0.259895270686603,
-96.5089494827552));
#171066=CARTESIAN_POINT('Ctrl Pts',(39.7006573795269,0.255684130879655,
-96.1258675663254));
#171067=CARTESIAN_POINT('Ctrl Pts',(39.7124916438098,0.624126916064151,
-95.8521099883181));
#171068=CARTESIAN_POINT('Ctrl Pts',(39.7246979184353,0.993796081660326,
-95.5675100901926));
#171069=CARTESIAN_POINT('Ctrl Pts',(39.7372758034841,1.36558709194006,-95.2715490323558));
#171070=CARTESIAN_POINT('Ctrl Pts',(39.742298747403,1.5140608128363,-95.1533577951219));
#171071=CARTESIAN_POINT('Ctrl Pts',(39.7473808898758,1.66287325720136,-95.0333550182876));
#171072=CARTESIAN_POINT('Ctrl Pts',(39.7525219085452,1.81208326361858,-94.911509475135));
#171073=CARTESIAN_POINT('Ctrl Pts',(39.5857320339139,-3.78242364196796,
-98.7152337592039));
#171074=CARTESIAN_POINT('Ctrl Pts',(39.5647695935044,-3.78057566286457,
-98.758128723926));
#171075=CARTESIAN_POINT('Ctrl Pts',(39.5426881139166,-3.7785869067278,-98.8046816267017));
#171076=CARTESIAN_POINT('Ctrl Pts',(39.519765128284,-3.77644182021921,-98.8550122588158));
#171077=CARTESIAN_POINT('Ctrl Pts',(39.501693369924,-3.7747507017207,-98.894691340601));
#171078=CARTESIAN_POINT('Ctrl Pts',(39.4830995277155,-3.77296247279516,
-98.9367185702283));
#171079=CARTESIAN_POINT('Ctrl Pts',(39.4641420358889,-3.77107389124137,
-98.9811511179016));
#171080=CARTESIAN_POINT('Ctrl Pts',(39.4426398204678,-3.76893179946144,
-99.0315479858268));
#171081=CARTESIAN_POINT('Ctrl Pts',(39.4206691128835,-3.76666025515081,
-99.0850397431287));
#171082=CARTESIAN_POINT('Ctrl Pts',(39.3984931481515,-3.76426354211129,
-99.1417019859204));
#171083=CARTESIAN_POINT('Ctrl Pts',(39.3874051657855,-3.76306518559153,
-99.1700331073162));
#171084=CARTESIAN_POINT('Ctrl Pts',(39.3762664009185,-3.76183569968917,
-99.199156695867));
#171085=CARTESIAN_POINT('Ctrl Pts',(39.3651129498974,-3.76057674596568,
-99.2290809819656));
#171086=CARTESIAN_POINT('Ctrl Pts',(39.3595362243869,-3.75994726910395,
-99.2440431250149));
#171087=CARTESIAN_POINT('Ctrl Pts',(39.3539558493515,-3.7593104214926,-99.2592054504292));
#171088=CARTESIAN_POINT('Ctrl Pts',(39.3483765482337,-3.75866651196756,
-99.2745688609028));
#171089=CARTESIAN_POINT('Ctrl Pts',(39.3455868976748,-3.75834455720504,
-99.2822505661396));
#171090=CARTESIAN_POINT('Ctrl Pts',(39.3427975168664,-3.75802083673782,
-99.2899825431161));
#171091=CARTESIAN_POINT('Ctrl Pts',(39.3400090065945,-3.75769539178263,
-99.2977649015877));
#171092=CARTESIAN_POINT('Ctrl Pts',(39.3386147514586,-3.75753266930503,
-99.3016560808235));
#171093=CARTESIAN_POINT('Ctrl Pts',(39.3372207140364,-3.75736951569224,
-99.3055598554609));
#171094=CARTESIAN_POINT('Ctrl Pts',(39.335826970206,-3.75720593647556,-99.3094762387292));
#171095=CARTESIAN_POINT('Ctrl Pts',(39.3344332263756,-3.75704235725887,
-99.3133926219975));
#171096=CARTESIAN_POINT('Ctrl Pts',(39.3335565762715,-3.75693935012291,
-99.3158593676638));
#171097=CARTESIAN_POINT('Ctrl Pts',(39.3316466957756,-3.75671392763538,
-99.3212632275588));
#171098=CARTESIAN_POINT('Ctrl Pts',(39.3120453395123,-3.75440038681578,
-99.3767237567527));
#171099=CARTESIAN_POINT('Ctrl Pts',(39.2945611211606,-3.75221686724286,
-99.4288752600496));
#171100=CARTESIAN_POINT('Ctrl Pts',(39.2788945448127,-3.75018391351401,
-99.4775817224279));
#171101=CARTESIAN_POINT('Ctrl Pts',(39.2630442479134,-3.74812711951709,
-99.5268593611707));
#171102=CARTESIAN_POINT('Ctrl Pts',(39.249054055268,-3.7462241551025,-99.5726111325386));
#171103=CARTESIAN_POINT('Ctrl Pts',(39.2366499945523,-3.74448358754834,
-99.6147331608509));
#171104=CARTESIAN_POINT('Ctrl Pts',(39.2240969536772,-3.74272211474086,
-99.657361099819));
#171105=CARTESIAN_POINT('Ctrl Pts',(39.2131680464728,-3.74112669492314,
-99.6962720163725));
#171106=CARTESIAN_POINT('Ctrl Pts',(39.2036218248227,-3.73969751603952,
-99.7313891637658));
#171107=CARTESIAN_POINT('Ctrl Pts',(39.1940360201446,-3.73826241112255,
-99.7666519230126));
#171108=CARTESIAN_POINT('Ctrl Pts',(39.1858442044626,-3.73699469031387,
-99.7980898058902));
#171109=CARTESIAN_POINT('Ctrl Pts',(39.178848316674,-3.7358896890291,-99.82564954893));
#171110=CARTESIAN_POINT('Ctrl Pts',(39.1718273274359,-3.7347807229675,-99.8533081771318));
#171111=CARTESIAN_POINT('Ctrl Pts',(39.1660107449371,-3.73383545695238,
-99.8770611283396));
#171112=CARTESIAN_POINT('Ctrl Pts',(39.1612472807937,-3.73304752251837,
-99.8968733708105));
#171113=CARTESIAN_POINT('Ctrl Pts',(39.1595812339107,-3.73277193826534,
-99.9038028078379));
#171114=CARTESIAN_POINT('Ctrl Pts',(39.1580444579001,-3.73251559828333,
-99.910250327255));
#171115=CARTESIAN_POINT('Ctrl Pts',(39.1566319198793,-3.73227824181624,
-99.9162148626195));
#171116=CARTESIAN_POINT('Ctrl Pts',(39.1551064101022,-3.73202190208881,
-99.922656428709));
#171117=CARTESIAN_POINT('Ctrl Pts',(39.1537257931825,-3.73178770267067,
-99.9285346636997));
#171118=CARTESIAN_POINT('Ctrl Pts',(39.1524847145106,-3.73157534599519,
-99.9338484768152));
#171119=CARTESIAN_POINT('Ctrl Pts',(39.1518641751747,-3.73146916765746,
-99.936505383373));
#171120=CARTESIAN_POINT('Ctrl Pts',(39.15127853624,-3.73136844832386,-99.9390211880862));
#171121=CARTESIAN_POINT('Ctrl Pts',(39.1507272247462,-3.73127315735143,
-99.9413957776894));
#171122=CARTESIAN_POINT('Ctrl Pts',(39.1504515689993,-3.73122551186521,
-99.9425830724911));
#171123=CARTESIAN_POINT('Ctrl Pts',(39.1501844960998,-3.73117922336374,
-99.9437350637426));
#171124=CARTESIAN_POINT('Ctrl Pts',(39.1499259404233,-3.73113428790966,
-99.9448517385624));
#171125=CARTESIAN_POINT('Ctrl Pts',(39.1497966625851,-3.73111182018261,
-99.9454100759722));
#171126=CARTESIAN_POINT('Ctrl Pts',(39.1496695141143,-3.7310896907109,-99.9459595842882));
#171127=CARTESIAN_POINT('Ctrl Pts',(39.1495444871842,-3.73106789902453,
-99.9465002619851));
#171128=CARTESIAN_POINT('Ctrl Pts',(39.1495132304517,-3.73106245110294,
-99.9466354314093));
#171129=CARTESIAN_POINT('Ctrl Pts',(39.1495030287109,-3.73106067541122,
-99.946679562838));
#171130=CARTESIAN_POINT('Ctrl Pts',(39.1494981838382,-3.73105983425694,
-99.9467005194));
#171131=CARTESIAN_POINT('Ctrl Pts',(39.1494945501837,-3.73105920339123,
-99.9467162368216));
#171132=CARTESIAN_POINT('Ctrl Pts',(39.1494939304581,-3.73105909813003,
-99.9467189185376));
#171133=CARTESIAN_POINT('Ctrl Pts',(39.1494897051637,-3.731058363178,-99.94673719502));
#171134=CARTESIAN_POINT('Ctrl Pts',(39.1494770292805,-3.73105615832187,
-99.9467920244674));
#171135=CARTESIAN_POINT('Ctrl Pts',(39.1494318011524,-3.73104829699593,
-99.9469871836392));
#171136=CARTESIAN_POINT('Ctrl Pts',(39.1491757634381,-3.73100353684427,
-99.9480958017481));
#171137=CARTESIAN_POINT('Ctrl Pts',(39.1280875954373,-3.72731693309337,
-100.039405494116));
#171138=CARTESIAN_POINT('Ctrl Pts',(39.109772797189,-3.72369719320944,-100.128756426151));
#171139=CARTESIAN_POINT('Ctrl Pts',(39.0939077592067,-3.72018651132105,
-100.215952276152));
#171140=CARTESIAN_POINT('Ctrl Pts',(39.077695335567,-3.71659895848302,-100.305057392788));
#171141=CARTESIAN_POINT('Ctrl Pts',(39.0640405428947,-3.71312512146226,
-100.391912157614));
#171142=CARTESIAN_POINT('Ctrl Pts',(39.0526011972676,-3.70978648587783,
-100.476356109603));
#171143=CARTESIAN_POINT('Ctrl Pts',(39.0407653272854,-3.70633212249175,
-100.563727159407));
#171144=CARTESIAN_POINT('Ctrl Pts',(39.0313005753357,-3.70302232059837,
-100.648517517554));
#171145=CARTESIAN_POINT('Ctrl Pts',(39.0238403729853,-3.69985856977579,
-100.730599277938));
#171146=CARTESIAN_POINT('Ctrl Pts',(39.0162275336137,-3.69663008806803,
-100.814360445235));
#171147=CARTESIAN_POINT('Ctrl Pts',(39.0107016304485,-3.69355343458246,
-100.89530140222));
#171148=CARTESIAN_POINT('Ctrl Pts',(39.0068940598651,-3.69061080968657,
-100.973333128231));
#171149=CARTESIAN_POINT('Ctrl Pts',(39.0029720963335,-3.68757977788401,
-101.053709204528));
#171150=CARTESIAN_POINT('Ctrl Pts',(39.0008728253103,-3.68469068702846,
-101.130998989905));
#171151=CARTESIAN_POINT('Ctrl Pts',(39.0002225969439,-3.68190774101026,
-101.205148883042));
#171152=CARTESIAN_POINT('Ctrl Pts',(39.0000727567577,-3.68126643224657,
-101.222236162488));
#171153=CARTESIAN_POINT('Ctrl Pts',(39.0000000001679,-3.68063070304705,
-101.239156866278));
#171154=CARTESIAN_POINT('Ctrl Pts',(39.,-3.68000002,-101.255910620448));
#171155=CARTESIAN_POINT('Ctrl Pts',(39.6406521140204,-3.78697803566041,
-98.6057147789936));
#171156=CARTESIAN_POINT('Ctrl Pts',(39.7174896230836,-4.18000001999998,
-98.6445257445324));
#171157=CARTESIAN_POINT('Ctrl Pts',(40.0766182115838,-4.18000001999998,
-98.8259229955145));
#171158=CARTESIAN_POINT('Ctrl Pts',(39.4187804907282,-3.76832519858073,
-99.0363833344201));
#171159=CARTESIAN_POINT('Ctrl Pts',(39.4849150761468,-4.18000001999998,
-99.0700146927968));
#171160=CARTESIAN_POINT('Ctrl Pts',(39.87692608831,-4.18000001999998,-99.2216958278296));
#171161=CARTESIAN_POINT('Ctrl Pts',(39.2562588135465,-3.74954484420426,
-99.4842872473771));
#171162=CARTESIAN_POINT('Ctrl Pts',(39.3129722860326,-4.18000001999998,
-99.5090269233591));
#171163=CARTESIAN_POINT('Ctrl Pts',(39.7306548682082,-4.18000001999998,
-99.6328320937587));
#171164=CARTESIAN_POINT('Ctrl Pts',(39.0420216354292,-3.71207776720274,
-100.41203214575));
#171165=CARTESIAN_POINT('Ctrl Pts',(39.070686775237,-4.18000001999998,-100.423129382882));
#171166=CARTESIAN_POINT('Ctrl Pts',(39.5378302081339,-4.18000001999998,
-100.48343236993));
#171167=CARTESIAN_POINT('Ctrl Pts',(38.9909689698687,-3.69325270187659,
-100.895713807542));
#171168=CARTESIAN_POINT('Ctrl Pts',(39.0043575688645,-4.18000001999998,
-100.903770629911));
#171169=CARTESIAN_POINT('Ctrl Pts',(39.4918770183597,-4.18000001999999,
-100.926406647344));
#171170=CARTESIAN_POINT('Ctrl Pts',(39.0013094879538,-3.6752109923929,-101.378179163766));
#171171=CARTESIAN_POINT('Ctrl Pts',(38.9964768548807,-4.18000001999999,
-101.378270171681));
#171172=CARTESIAN_POINT('Ctrl Pts',(39.5011768353311,-4.18000001999999,
-101.367775593403));
#171173=CARTESIAN_POINT('',(39.5,-4.18000001999998,-101.255910620448));
#171174=CARTESIAN_POINT('Origin',(39.5,-3.68000001999999,-101.255910620448));
#171175=CARTESIAN_POINT('',(40.0271577790679,-4.18000001999998,-98.926539349744));
#171176=CARTESIAN_POINT('Origin',(40.0271577790679,-3.68000001999999,-98.926539349744));
#171177=CARTESIAN_POINT('Ctrl Pts',(39.5,-4.18000001999999,-101.255910620448));
#171178=CARTESIAN_POINT('Ctrl Pts',(39.5,-4.18000001999999,-100.974485528886));
#171179=CARTESIAN_POINT('Ctrl Pts',(39.5222808837194,-4.18000001999999,
-100.693150422405));
#171180=CARTESIAN_POINT('Ctrl Pts',(39.5655905128992,-4.18000001999999,
-100.416810780349));
#171181=CARTESIAN_POINT('Ctrl Pts',(39.5844991865996,-4.18000001999999,
-100.296162873149));
#171182=CARTESIAN_POINT('Ctrl Pts',(39.6074169109172,-4.18000001999998,
-100.176467126241));
#171183=CARTESIAN_POINT('Ctrl Pts',(39.6342425380315,-4.18000001999998,
-100.058132231812));
#171184=CARTESIAN_POINT('Ctrl Pts',(39.7053092693719,-4.18000001999998,
-99.7446381943849));
#171185=CARTESIAN_POINT('Ctrl Pts',(39.8034555232797,-4.18000001999998,
-99.4388673313559));
#171186=CARTESIAN_POINT('Ctrl Pts',(39.930132764858,-4.18000001999998,-99.1412335948014));
#171187=CARTESIAN_POINT('Ctrl Pts',(39.960795555159,-4.18000001999998,-99.0691900237798));
#171188=CARTESIAN_POINT('Ctrl Pts',(39.9931302150563,-4.18000001999998,
-98.9976232754198));
#171189=CARTESIAN_POINT('Ctrl Pts',(40.0271577790679,-4.18000001999998,
-98.926539349744));
#171190=CARTESIAN_POINT('Origin',(39.5,-3.68000001999999,-55.24995));
#171191=CARTESIAN_POINT('',(39.5,-4.18000001999998,-130.802732351058));
#171192=CARTESIAN_POINT('Origin',(39.5,-3.68000001999999,-130.802732351058));
#171193=CARTESIAN_POINT('',(39.5,-4.18000001999998,-55.24995));
#171194=CARTESIAN_POINT('Ctrl Pts',(39.,-3.68000001999999,-130.802732351058));
#171195=CARTESIAN_POINT('Ctrl Pts',(39.,-4.18000001999998,-130.802732351057));
#171196=CARTESIAN_POINT('Ctrl Pts',(39.5,-4.18000001999998,-130.802732351058));
#171197=CARTESIAN_POINT('Ctrl Pts',(39.,-3.69663481492557,-131.244626684237));
#171198=CARTESIAN_POINT('Ctrl Pts',(39.0163626300028,-4.18000001999998,
-131.237396673044));
#171199=CARTESIAN_POINT('Ctrl Pts',(39.5000000028449,-4.18000001999998,
-131.207067934262));
#171200=CARTESIAN_POINT('Ctrl Pts',(39.0498728558349,-3.71353967201765,
-131.677827554702));
#171201=CARTESIAN_POINT('Ctrl Pts',(39.0799719048085,-4.18000001999998,
-131.667492297612));
#171202=CARTESIAN_POINT('Ctrl Pts',(39.5448855698238,-4.18000001999998,
-131.603841024792));
#171203=CARTESIAN_POINT('Ctrl Pts',(39.2448092923438,-3.74782444813235,
-132.527335109052));
#171204=CARTESIAN_POINT('Ctrl Pts',(39.3005991742935,-4.18000001999998,
-132.50452184294));
#171205=CARTESIAN_POINT('Ctrl Pts',(39.720328363537,-4.18000001999998,-132.382704674372));
#171206=CARTESIAN_POINT('Ctrl Pts',(39.391689897628,-3.76532817544854,-132.946345914773));
#171207=CARTESIAN_POINT('Ctrl Pts',(39.4567563186094,-4.18000001999999,
-132.915330450675));
#171208=CARTESIAN_POINT('Ctrl Pts',(39.8525202266285,-4.18000001999998,
-132.767284004423));
#171209=CARTESIAN_POINT('Ctrl Pts',(39.585730865626,-3.78242429107036,-133.343412752622));
#171210=CARTESIAN_POINT('Ctrl Pts',(39.6607823401612,-4.18000001999998,
-133.307485940342));
#171211=CARTESIAN_POINT('Ctrl Pts',(40.0271577790634,-4.18000001999998,
-133.132103621752));
#171212=CARTESIAN_POINT('',(40.0271577790634,-4.18000001999998,-133.132103621752));
#171213=CARTESIAN_POINT('Origin',(40.0271577790634,-3.68000001999999,-133.132103621752));
#171214=CARTESIAN_POINT('Ctrl Pts',(40.0271577790634,-4.18000001999998,
-133.132103621752));
#171215=CARTESIAN_POINT('Ctrl Pts',(39.903504593422,-4.18000001999998,-132.873790865225));
#171216=CARTESIAN_POINT('Ctrl Pts',(39.8011022473334,-4.18000001999999,
-132.605500495487));
#171217=CARTESIAN_POINT('Ctrl Pts',(39.7207150267675,-4.18000001999999,
-132.332596829901));
#171218=CARTESIAN_POINT('Ctrl Pts',(39.6875913562942,-4.18000001999999,
-132.220146479881));
#171219=CARTESIAN_POINT('Ctrl Pts',(39.6582049915466,-4.18000001999998,
-132.106913147221));
#171220=CARTESIAN_POINT('Ctrl Pts',(39.6326069664648,-4.18000001999998,
-131.993272849631));
#171221=CARTESIAN_POINT('Ctrl Pts',(39.5604708508297,-4.18000001999999,
-131.673030580095));
#171222=CARTESIAN_POINT('Ctrl Pts',(39.5173036683663,-4.18000001999998,
-131.347852435203));
#171223=CARTESIAN_POINT('Ctrl Pts',(39.5042396692598,-4.18000001999998,
-131.017545146527));
#171224=CARTESIAN_POINT('Ctrl Pts',(39.5014171427712,-4.18000001999998,
-130.946181005725));
#171225=CARTESIAN_POINT('Ctrl Pts',(39.5,-4.18000001999998,-130.874577408223));
#171226=CARTESIAN_POINT('Ctrl Pts',(39.5,-4.18000001999998,-130.802732351058));
#171227=CARTESIAN_POINT('Ctrl Pts',(58.1221005562789,-4.18000001999999,
-171.237717270032));
#171228=CARTESIAN_POINT('Ctrl Pts',(57.7306096110337,-4.18000001999999,
-171.422588467367));
#171229=CARTESIAN_POINT('Ctrl Pts',(57.6746235421417,-3.75150367745622,
-171.449026400902));
#171230=CARTESIAN_POINT('Ctrl Pts',(52.1178467328245,-4.18000001999999,
-158.52285936551));
#171231=CARTESIAN_POINT('Ctrl Pts',(51.7702631771107,-4.18000001999999,
-158.785894332693));
#171232=CARTESIAN_POINT('Ctrl Pts',(51.6715280616305,-3.75870638021677,
-158.734184170827));
#171233=CARTESIAN_POINT('Ctrl Pts',(46.0984623496487,-4.18000001999998,
-145.815120328436));
#171234=CARTESIAN_POINT('Ctrl Pts',(45.7948164697718,-4.18000001999998,
-146.15085325192));
#171235=CARTESIAN_POINT('Ctrl Pts',(45.6536266465224,-3.76768226491552,
-146.026454114168));
#171236=CARTESIAN_POINT('Ctrl Pts',(40.0271577790634,-4.18000001999998,
-133.132103621752));
#171237=CARTESIAN_POINT('Ctrl Pts',(39.660782340162,-4.18000001999998,-133.307485940342));
#171238=CARTESIAN_POINT('Ctrl Pts',(39.5857308656265,-3.78242429107081,
-133.343412752623));
#171239=CARTESIAN_POINT('',(58.1221005562789,-4.18000001999999,-171.237717270032));
#171240=CARTESIAN_POINT('Origin',(58.1221005562789,-3.68000001999999,-171.237717270032));
#171241=CARTESIAN_POINT('Ctrl Pts',(58.1221005562789,-4.18000001999999,
-171.237717270032));
#171242=CARTESIAN_POINT('Ctrl Pts',(52.1178384024439,-4.18000001999999,
-158.522841724749));
#171243=CARTESIAN_POINT('Ctrl Pts',(46.0984712740486,-4.18000001999998,
-145.815138971718));
#171244=CARTESIAN_POINT('Ctrl Pts',(40.0271577790634,-4.18000001999998,
-133.132103621752));
#171245=CARTESIAN_POINT('Ctrl Pts',(58.2644174754153,-4.18000001999999,
-171.871644662643));
#171246=CARTESIAN_POINT('Ctrl Pts',(57.8378063278745,-4.18000001999999,
-171.871644662643));
#171247=CARTESIAN_POINT('Ctrl Pts',(57.7706512256236,-3.75870764711888,
-171.871644662643));
#171248=CARTESIAN_POINT('Ctrl Pts',(58.2644174584531,-4.18000001999999,
-171.652701076652));
#171249=CARTESIAN_POINT('Ctrl Pts',(57.8378063150439,-4.18000001999999,
-171.715730578987));
#171250=CARTESIAN_POINT('Ctrl Pts',(57.7706512252069,-3.75870764450445,
-171.725685252419));
#171251=CARTESIAN_POINT('Ctrl Pts',(58.2165506240601,-4.18000001999999,
-171.437728673605));
#171252=CARTESIAN_POINT('Ctrl Pts',(57.801183875227,-4.18000002000114,-171.562158552623));
#171253=CARTESIAN_POINT('Ctrl Pts',(57.7383541282856,-3.7562957918519,-171.582363368286));
#171254=CARTESIAN_POINT('Ctrl Pts',(58.1221005562789,-4.18000001999999,
-171.237717270032));
#171255=CARTESIAN_POINT('Ctrl Pts',(57.7306096110337,-4.18000001999999,
-171.422588467367));
#171256=CARTESIAN_POINT('Ctrl Pts',(57.6746235421417,-3.75150367745622,
-171.449026400902));
#171257=CARTESIAN_POINT('',(58.2644174754153,-4.18000001999999,-171.871644662643));
#171258=CARTESIAN_POINT('Origin',(58.2644174754153,-3.68000001999999,-171.871644662643));
#171259=CARTESIAN_POINT('Origin',(56.1314697890424,-4.18000001999999,-172.0066931789));
#171260=CARTESIAN_POINT('Origin',(58.2644174754153,-3.68000001999999,-179.64995));
#171261=CARTESIAN_POINT('',(57.7706512256236,-3.75870764711888,-179.64995));
#171262=CARTESIAN_POINT('',(58.2644174754153,-4.18000001999999,-171.871644662643));
#171263=CARTESIAN_POINT('Ctrl Pts',(60.,-4.68000001999999,-174.488343624884));
#171264=CARTESIAN_POINT('Ctrl Pts',(60.,-4.18000002,-174.488343624884));
#171265=CARTESIAN_POINT('Ctrl Pts',(59.5,-4.18000001999999,-174.488343624884));
#171266=CARTESIAN_POINT('Ctrl Pts',(60.,-4.67777472283721,-174.78368089075));
#171267=CARTESIAN_POINT('Ctrl Pts',(59.9977796185047,-4.18000001999829,
-174.78302738694));
#171268=CARTESIAN_POINT('Ctrl Pts',(59.499999993334,-4.18000001999999,-174.734541991424));
#171269=CARTESIAN_POINT('Ctrl Pts',(59.9573556192874,-4.67559899657361,
-175.071875505894));
#171270=CARTESIAN_POINT('Ctrl Pts',(59.9531694408477,-4.18000002000085,
-175.070632089297));
#171271=CARTESIAN_POINT('Ctrl Pts',(59.4644630183961,-4.18000001999999,
-174.974786360247));
#171272=CARTESIAN_POINT('Ctrl Pts',(59.8306767385091,-4.67241126250759,
-175.493405719049));
#171273=CARTESIAN_POINT('Ctrl Pts',(59.8236519200077,-4.18000001999958,
-175.490806712526));
#171274=CARTESIAN_POINT('Ctrl Pts',(59.3588972809293,-4.18000001999999,
-175.326182058073));
#171275=CARTESIAN_POINT('Ctrl Pts',(59.7776634626824,-4.67136322522169,
-175.631868709625));
#171276=CARTESIAN_POINT('Ctrl Pts',(59.7698424718428,-4.18000001999956,
-175.628550598836));
#171277=CARTESIAN_POINT('Ctrl Pts',(59.3147195516479,-4.18000001999999,
-175.441607525732));
#171278=CARTESIAN_POINT('Ctrl Pts',(59.6537038929485,-4.66936150715186,
-175.896123076728));
#171279=CARTESIAN_POINT('Ctrl Pts',(59.6445293525488,-4.18000002000041,
-175.891155901683));
#171280=CARTESIAN_POINT('Ctrl Pts',(59.2114199113778,-4.18000001999999,
-175.661895244315));
#171281=CARTESIAN_POINT('Ctrl Pts',(59.5824462721252,-4.66839878682381,
-176.023110187492));
#171282=CARTESIAN_POINT('Ctrl Pts',(59.5727342923808,-4.18000002000089,
-176.017245435326));
#171283=CARTESIAN_POINT('Ctrl Pts',(59.1520385607459,-4.18000001999999,
-175.767754281813));
#171284=CARTESIAN_POINT('Ctrl Pts',(59.4213258837533,-4.66655021592386,
-176.266776880891));
#171285=CARTESIAN_POINT('Ctrl Pts',(59.4108028292072,-4.1800000199991,-176.25895171657));
#171286=CARTESIAN_POINT('Ctrl Pts',(59.0177715691528,-4.18000001999999,
-175.970879863896));
#171287=CARTESIAN_POINT('Ctrl Pts',(59.3305935235461,-4.66565781609966,
-176.3843179035));
#171288=CARTESIAN_POINT('Ctrl Pts',(59.3198146755637,-4.18000001999915,
-176.37546218739));
#171289=CARTESIAN_POINT('Ctrl Pts',(58.9421612688066,-4.18000001999999,
-176.06886452411));
#171290=CARTESIAN_POINT('Ctrl Pts',(59.1349023357136,-4.66400011582949,
-176.602528392516));
#171291=CARTESIAN_POINT('Ctrl Pts',(59.1239216856836,-4.18000002000084,
-176.591561815318));
#171292=CARTESIAN_POINT('Ctrl Pts',(58.7790852805764,-4.18000001999999,
-176.250769420981));
#171293=CARTESIAN_POINT('Ctrl Pts',(59.0299133821615,-4.66323171680632,
-176.703607721972));
#171294=CARTESIAN_POINT('Ctrl Pts',(59.0189867750955,-4.18000001999871,
-176.691604703902));
#171295=CARTESIAN_POINT('Ctrl Pts',(58.6915944853457,-4.18000001999999,
-176.33503132506));
#171296=CARTESIAN_POINT('Ctrl Pts',(58.6938786030259,-4.66110543474911,
-176.983174915482));
#171297=CARTESIAN_POINT('Ctrl Pts',(58.6838036746477,-4.18000002000249,
-176.967887143763));
#171298=CARTESIAN_POINT('Ctrl Pts',(58.4115655020993,-4.18000001999999,
-176.56808461344));
#171299=CARTESIAN_POINT('Ctrl Pts',(58.437917085704,-4.65991812350376,-177.139087667033));
#171300=CARTESIAN_POINT('Ctrl Pts',(58.4288067817606,-4.18000002000125,
-177.121996578829));
#171301=CARTESIAN_POINT('Ctrl Pts',(58.1982641486948,-4.18000001999999,
-176.698056997615));
#171302=CARTESIAN_POINT('Ctrl Pts',(58.1703978083756,-4.65905396057624,
-177.252515804372));
#171303=CARTESIAN_POINT('Ctrl Pts',(58.1625546348518,-4.18000002,-177.234024164027));
#171304=CARTESIAN_POINT('Ctrl Pts',(57.9753315069797,-4.18000001999999,
-176.792613205276));
#171305=CARTESIAN_POINT('',(59.5,-4.18000001999999,-174.488343624884));
#171306=CARTESIAN_POINT('Ctrl Pts',(59.5,-4.18000001999999,-174.488343624884));
#171307=CARTESIAN_POINT('Ctrl Pts',(59.5,-4.18000001999999,-174.676432184958));
#171308=CARTESIAN_POINT('Ctrl Pts',(59.4792627601818,-4.18000001935391,
-174.860994953572));
#171309=CARTESIAN_POINT('Ctrl Pts',(59.4381337746112,-4.18000002064829,
-175.042081103196));
#171310=CARTESIAN_POINT('Ctrl Pts',(59.4313812635049,-4.1800000208608,-175.071811625833));
#171311=CARTESIAN_POINT('Ctrl Pts',(59.4240789892375,-4.18000002115769,
-175.101448468711));
#171312=CARTESIAN_POINT('Ctrl Pts',(59.4162283471532,-4.18000002161129,
-175.130991885445));
#171313=CARTESIAN_POINT('Ctrl Pts',(59.4092933860371,-4.18000002201199,
-175.157089425504));
#171314=CARTESIAN_POINT('Ctrl Pts',(59.4019280344311,-4.18000002232545,
-175.183113688583));
#171315=CARTESIAN_POINT('Ctrl Pts',(59.3941336392735,-4.18000002248888,
-175.209064512545));
#171316=CARTESIAN_POINT('Ctrl Pts',(59.3589528015432,-4.18000002322649,
-175.326196337184));
#171317=CARTESIAN_POINT('Ctrl Pts',(59.3147522563139,-4.18000002089879,
-175.441619139941));
#171318=CARTESIAN_POINT('Ctrl Pts',(59.2630854722639,-4.18000002030225,
-175.551758766342));
#171319=CARTESIAN_POINT('Ctrl Pts',(59.2343127518865,-4.18000001997004,
-175.613094433564));
#171320=CARTESIAN_POINT('Ctrl Pts',(59.2031440665131,-4.18000001999999,
-175.673101168879));
#171321=CARTESIAN_POINT('Ctrl Pts',(59.1695814056726,-4.18000001999999,
-175.731779921994));
#171322=CARTESIAN_POINT('Ctrl Pts',(59.1428767576963,-4.18000001999999,
-175.778468575586));
#171323=CARTESIAN_POINT('Ctrl Pts',(59.1146521957298,-4.18000001999991,
-175.824314777934));
#171324=CARTESIAN_POINT('Ctrl Pts',(59.0849057084902,-4.18000002000059,
-175.869317498238));
#171325=CARTESIAN_POINT('Ctrl Pts',(59.0177729179323,-4.18000002000212,
-175.970881026476));
#171326=CARTESIAN_POINT('Ctrl Pts',(58.9421638152095,-4.18000002001086,
-176.068866658213));
#171327=CARTESIAN_POINT('Ctrl Pts',(58.8606254499681,-4.18000002000853,
-176.15981892266));
#171328=CARTESIAN_POINT('Ctrl Pts',(58.8332817762446,-4.18000002000775,
-176.190319522422));
#171329=CARTESIAN_POINT('Ctrl Pts',(58.8052684934466,-4.18000002000547,
-176.220067577769));
#171330=CARTESIAN_POINT('Ctrl Pts',(58.7765893403539,-4.18000002000312,
-176.2490672712));
#171331=CARTESIAN_POINT('Ctrl Pts',(58.7334919025219,-4.18000001999957,
-176.292646399243));
#171332=CARTESIAN_POINT('Ctrl Pts',(58.6887854216327,-4.1800000198565,-176.334637716937));
#171333=CARTESIAN_POINT('Ctrl Pts',(58.6426104314496,-4.18000002015176,
-176.374934331061));
#171334=CARTESIAN_POINT('Ctrl Pts',(58.6279756118803,-4.18000002024535,
-176.387706043077));
#171335=CARTESIAN_POINT('Ctrl Pts',(58.6131935185633,-4.18000002040339,
-176.40030782898));
#171336=CARTESIAN_POINT('Ctrl Pts',(58.5982692931781,-4.18000002077447,
-176.412737145102));
#171337=CARTESIAN_POINT('Ctrl Pts',(58.5771929061033,-4.18000002129852,
-176.430290155116));
#171338=CARTESIAN_POINT('Ctrl Pts',(58.5557921166901,-4.18000002220248,
-176.447510765875));
#171339=CARTESIAN_POINT('Ctrl Pts',(58.5341058949341,-4.18000002446768,
-176.464377473526));
#171340=CARTESIAN_POINT('Ctrl Pts',(58.4881980669412,-4.18000002926289,
-176.500082813181));
#171341=CARTESIAN_POINT('Ctrl Pts',(58.4409815652464,-4.18000004169373,
-176.534222750276));
#171342=CARTESIAN_POINT('Ctrl Pts',(58.3925215548526,-4.18000005349381,
-176.566751049322));
#171343=CARTESIAN_POINT('Ctrl Pts',(58.3507358574757,-4.18000006366869,
-176.59479928227));
#171344=CARTESIAN_POINT('Ctrl Pts',(58.3080246526019,-4.18000007127262,
-176.621648795663));
#171345=CARTESIAN_POINT('Ctrl Pts',(58.2644174754055,-4.18000006545692,
-176.647241333307));
#171346=CARTESIAN_POINT('Origin',(59.5,-4.68000001999999,-174.488343624884));
#171347=CARTESIAN_POINT('Ctrl Pts',(40.0271577790679,-4.18000001999998,
-98.926539349744));
#171348=CARTESIAN_POINT('Ctrl Pts',(39.6607823401664,-4.18000001999998,
-98.7511570311542));
#171349=CARTESIAN_POINT('Ctrl Pts',(39.585730865631,-3.7824242910708,-98.7152302188737));
#171350=CARTESIAN_POINT('Ctrl Pts',(46.0600623067188,-4.18000001999998,
-86.3237407210712));
#171351=CARTESIAN_POINT('Ctrl Pts',(45.7555532717617,-4.18000001999998,
-85.989998533184));
#171352=CARTESIAN_POINT('Ctrl Pts',(45.6152479999264,-3.76777550625849,
-86.1124074338642));
#171353=CARTESIAN_POINT('Ctrl Pts',(52.0416537250564,-4.18000001999999,
-73.6965087765536));
#171354=CARTESIAN_POINT('Ctrl Pts',(51.6938180895878,-4.18000002,-73.4342549076826));
#171355=CARTESIAN_POINT('Ctrl Pts',(51.5953561718106,-3.75882512748543,
-73.4851842533606));
#171356=CARTESIAN_POINT('Ctrl Pts',(58.0081705490647,-4.18000001999999,
-61.0621827299711));
#171357=CARTESIAN_POINT('Ctrl Pts',(57.6167925372613,-4.18000001999999,
-60.8773558160983));
#171358=CARTESIAN_POINT('Ctrl Pts',(57.5607154366947,-3.75164060643487,
-60.8508735991007));
#171359=CARTESIAN_POINT('',(57.5607154366947,-3.75164060643487,-60.8508735991007));
#171360=CARTESIAN_POINT('Ctrl Pts',(57.5607154366947,-3.75164060643487,
-60.8508735991007));
#171361=CARTESIAN_POINT('Ctrl Pts',(55.9461395978097,-3.75358515890381,
-64.27045854236));
#171362=CARTESIAN_POINT('Ctrl Pts',(54.3918375646665,-3.7555208048552,-67.5588600426932));
#171363=CARTESIAN_POINT('Ctrl Pts',(52.1508196005947,-3.75871164726325,
-72.2946871288037));
#171364=CARTESIAN_POINT('Ctrl Pts',(51.4188856818639,-3.75981653600606,
-73.8405002967756));
#171365=CARTESIAN_POINT('Ctrl Pts',(50.3435910299283,-3.76151388746903,
-76.1100262576363));
#171366=CARTESIAN_POINT('Ctrl Pts',(49.8115952016668,-3.76237194900324,
-77.2324907902923));
#171367=CARTESIAN_POINT('Ctrl Pts',(49.2008224325657,-3.76337812834746,
-78.5205104614526));
#171368=CARTESIAN_POINT('Ctrl Pts',(48.8979081133578,-3.76388059401857,
-79.1591397261314));
#171369=CARTESIAN_POINT('Ctrl Pts',(48.7282140480925,-3.76416277298739,
-79.5168554019473));
#171370=CARTESIAN_POINT('Ctrl Pts',(48.6449347296394,-3.76430143017905,
-79.6923933180138));
#171371=CARTESIAN_POINT('Ctrl Pts',(48.6020070309088,-3.76437293568594,
-79.7828734307288));
#171372=CARTESIAN_POINT('Ctrl Pts',(48.5998549578026,-3.76437652051741,
-79.7874094159184));
#171373=CARTESIAN_POINT('Ctrl Pts',(45.3063254247015,-3.76986294272013,
-86.7292502309379));
#171374=CARTESIAN_POINT('Ctrl Pts',(42.3026944142814,-3.775823395277,-93.0362663227149));
#171375=CARTESIAN_POINT('Ctrl Pts',(39.585730865631,-3.78242429107081,-98.7152302188737));
#171376=CARTESIAN_POINT('',(58.0081705490647,-4.18000001999999,-61.0621827299711));
#171377=CARTESIAN_POINT('Origin',(58.0081705490647,-3.68000001999999,-61.0621827299711));
#171378=CARTESIAN_POINT('Ctrl Pts',(40.0271577790679,-4.18000001999998,
-98.926539349744));
#171379=CARTESIAN_POINT('Ctrl Pts',(46.0600710189762,-4.18000001999998,
-86.3237225210772));
#171380=CARTESIAN_POINT('Ctrl Pts',(52.0416455898407,-4.18000001999999,
-73.6965260027483));
#171381=CARTESIAN_POINT('Ctrl Pts',(58.0081705490647,-4.18000001999999,
-61.0621827299711));
#171382=CARTESIAN_POINT('Origin',(59.5,-4.68000001999999,-55.24995));
#171383=CARTESIAN_POINT('',(59.5,-4.18000001999999,-58.1445632485962));
#171384=CARTESIAN_POINT('',(60.,-4.68000002001403,-58.1445632485962));
#171385=CARTESIAN_POINT('Origin',(59.5,-4.68000001999999,-58.1445632485962));
#171386=CARTESIAN_POINT('',(60.,-4.68000001999999,-58.1637190207452));
#171387=CARTESIAN_POINT('',(59.5,-4.18000001999999,-174.466077711105));
#171388=CARTESIAN_POINT('Origin',(60.,-2.55003103885676E-14,0.));
#171389=CARTESIAN_POINT('',(60.,-5.18000001999999,-58.1246434856214));
#171390=CARTESIAN_POINT('Ctrl Pts',(60.,-4.68000002001403,-58.1445632485962));
#171391=CARTESIAN_POINT('Ctrl Pts',(60.,-4.84666977904325,-58.1380335512985));
#171392=CARTESIAN_POINT('Ctrl Pts',(60.,-5.01333597711292,-58.1313769278999));
#171393=CARTESIAN_POINT('Ctrl Pts',(60.,-5.18000001999999,-58.1246434856214));
#171394=CARTESIAN_POINT('',(60.,-5.18000001999999,-174.534521368494));
#171395=CARTESIAN_POINT('Origin',(59.5,-5.18000001999999,-55.24995));
#171396=CARTESIAN_POINT('',(59.5,-5.68000001999999,-58.1246434856214));
#171397=CARTESIAN_POINT('Origin',(59.5,-5.18000001999999,-58.1246434856214));
#171398=CARTESIAN_POINT('',(59.5,-5.68000001999999,-174.511260182693));
#171399=CARTESIAN_POINT('',(59.5,-5.68000001999999,-58.1042606444049));
#171400=CARTESIAN_POINT('Origin',(59.5,-5.18000001999999,-174.511260182693));
#171401=CARTESIAN_POINT('Ctrl Pts',(59.5,-5.68000001999999,-174.511260182693));
#171402=CARTESIAN_POINT('Ctrl Pts',(60.,-5.68000001999998,-174.511260182694));
#171403=CARTESIAN_POINT('Ctrl Pts',(60.,-5.18000001999999,-174.511260182693));
#171404=CARTESIAN_POINT('Ctrl Pts',(59.4999999934949,-5.68000001999999,
-174.751455697725));
#171405=CARTESIAN_POINT('Ctrl Pts',(60.0022233258349,-5.68000002000248,
-174.800030292485));
#171406=CARTESIAN_POINT('Ctrl Pts',(60.,-5.17778160006748,-174.799392136338));
#171407=CARTESIAN_POINT('Ctrl Pts',(59.4661441339012,-5.68000001999999,
-174.985974426754));
#171408=CARTESIAN_POINT('Ctrl Pts',(59.9636195754477,-5.68000001999999,
-175.081942695907));
#171409=CARTESIAN_POINT('Ctrl Pts',(59.9593729581191,-5.1756134281897,-175.080714219829));
#171410=CARTESIAN_POINT('Ctrl Pts',(59.3657005801303,-5.68000001999999,
-175.329231362388));
#171411=CARTESIAN_POINT('Ctrl Pts',(59.8460772881358,-5.68000001999999,
-175.49508011951));
#171412=CARTESIAN_POINT('Ctrl Pts',(59.8388406974375,-5.17243729299778,
-175.492475419334));
#171413=CARTESIAN_POINT('Ctrl Pts',(59.3235784200839,-5.68000001999999,
-175.4423463311));
#171414=CARTESIAN_POINT('Ctrl Pts',(59.7963955952484,-5.68000002000071,
-175.631508024916));
#171415=CARTESIAN_POINT('Ctrl Pts',(59.7882941049042,-5.17139018325129,
-175.628164866621));
#171416=CARTESIAN_POINT('Ctrl Pts',(59.2250283845896,-5.68000001999999,
-175.658495472519));
#171417=CARTESIAN_POINT('Ctrl Pts',(59.6796421793893,-5.68000001999927,
-175.892503005072));
#171418=CARTESIAN_POINT('Ctrl Pts',(59.6700340607039,-5.16938852396119,
-175.887451075324));
#171419=CARTESIAN_POINT('Ctrl Pts',(59.1683759292615,-5.68000001999999,
-175.762481455964));
#171420=CARTESIAN_POINT('Ctrl Pts',(59.6122794132826,-5.6800000200009,-176.018182187565));
#171421=CARTESIAN_POINT('Ctrl Pts',(59.6020511144931,-5.16842516963192,
-176.012189602522));
#171422=CARTESIAN_POINT('Ctrl Pts',(59.0403562655437,-5.68000001999999,
-175.962298484052));
#171423=CARTESIAN_POINT('Ctrl Pts',(59.4596388112852,-5.68000001999906,
-176.259950074275));
#171424=CARTESIAN_POINT('Ctrl Pts',(59.4484275192731,-5.16657340194589,
-176.251884189743));
#171425=CARTESIAN_POINT('Ctrl Pts',(58.9683527741555,-5.68000001999999,
-176.058826880554));
#171426=CARTESIAN_POINT('Ctrl Pts',(59.3735776050024,-5.68000001999968,
-176.376845479805));
#171427=CARTESIAN_POINT('Ctrl Pts',(59.3620233301153,-5.16567852041965,
-176.367676771746));
#171428=CARTESIAN_POINT('Ctrl Pts',(58.8121204079676,-5.68000001999999,
-176.239514776908));
#171429=CARTESIAN_POINT('Ctrl Pts',(59.1864690073094,-5.6800000200003,-176.595885870473));
#171430=CARTESIAN_POINT('Ctrl Pts',(59.1745444884326,-5.16400295101772,
-176.584424539694));
#171431=CARTESIAN_POINT('Ctrl Pts',(58.7283002756348,-5.68000001999999,
-176.3234477233));
#171432=CARTESIAN_POINT('Ctrl Pts',(59.0859070073554,-5.68000001999999,
-176.697708952909));
#171433=CARTESIAN_POINT('Ctrl Pts',(59.0739603306682,-5.16322437006847,
-176.685107962755));
#171434=CARTESIAN_POINT('Ctrl Pts',(58.460151514568,-5.68000001999999,-176.556489535136));
#171435=CARTESIAN_POINT('Ctrl Pts',(58.7634647581383,-5.68000001999999,
-176.980908577071));
#171436=CARTESIAN_POINT('Ctrl Pts',(58.7521818176688,-5.16106213487567,
-176.9646578323));
#171437=CARTESIAN_POINT('Ctrl Pts',(58.2562917522372,-5.68000001999999,
-176.688008530437));
#171438=CARTESIAN_POINT('Ctrl Pts',(58.5179479000405,-5.68000002000953,
-177.140745767071));
#171439=CARTESIAN_POINT('Ctrl Pts',(58.5075501754184,-5.15984115636875,
-177.122423932479));
#171440=CARTESIAN_POINT('Ctrl Pts',(58.0404491789985,-5.68000001999999,
-176.786906275262));
#171441=CARTESIAN_POINT('Ctrl Pts',(58.2576969618386,-5.68000001999996,
-177.261045698521));
#171442=CARTESIAN_POINT('Ctrl Pts',(58.2485390147982,-5.15892282666644,
-177.241058641939));
#171443=CARTESIAN_POINT('Ctrl Pts',(58.6082745331212,-5.6800000199515,-176.427328712824));
#171444=CARTESIAN_POINT('Ctrl Pts',(58.6185667882716,-5.68000001995871,
-176.418676244678));
#171445=CARTESIAN_POINT('Ctrl Pts',(58.628783204882,-5.68000001996413,-176.409943629197));
#171446=CARTESIAN_POINT('Ctrl Pts',(58.6389210444463,-5.68000001996836,
-176.401132572172));
#171447=CARTESIAN_POINT('Ctrl Pts',(58.7108573560273,-5.68000001999836,
-176.338610874188));
#171448=CARTESIAN_POINT('Ctrl Pts',(58.7792948136839,-5.68000001999946,
-176.271947442152));
#171449=CARTESIAN_POINT('Ctrl Pts',(58.8440583693344,-5.68000001994282,
-176.201117847418));
#171450=CARTESIAN_POINT('Ctrl Pts',(58.8596678064668,-5.68000001992916,
-176.184046361842));
#171451=CARTESIAN_POINT('Ctrl Pts',(58.8750639774275,-5.6800000199106,-176.166733035301));
#171452=CARTESIAN_POINT('Ctrl Pts',(58.8902447330317,-5.68000001988414,
-176.149177868712));
#171453=CARTESIAN_POINT('Ctrl Pts',(58.9227212058659,-5.68000001982754,
-176.111621774291));
#171454=CARTESIAN_POINT('Ctrl Pts',(58.9541409398416,-5.68000001973543,
-176.072997877296));
#171455=CARTESIAN_POINT('Ctrl Pts',(58.9843599854969,-5.68000001956972,
-176.033520885199));
#171456=CARTESIAN_POINT('Ctrl Pts',(59.0268866354123,-5.6800000193365,-175.977965715067));
#171457=CARTESIAN_POINT('Ctrl Pts',(59.0670052242283,-5.68000001940972,
-175.920749643185));
#171458=CARTESIAN_POINT('Ctrl Pts',(59.1043833915298,-5.68000001957814,
-175.862401050087));
#171459=CARTESIAN_POINT('Ctrl Pts',(59.1540049590064,-5.68000001980172,
-175.784940092029));
#171460=CARTESIAN_POINT('Ctrl Pts',(59.1991811925137,-5.68000001997513,
-175.705064487821));
#171461=CARTESIAN_POINT('Ctrl Pts',(59.2399658936416,-5.68000001998964,
-175.622670099363));
#171462=CARTESIAN_POINT('Ctrl Pts',(59.2487993257312,-5.68000001999278,
-175.604824553978));
#171463=CARTESIAN_POINT('Ctrl Pts',(59.2574265918442,-5.6800000199934,-175.586860742585));
#171464=CARTESIAN_POINT('Ctrl Pts',(59.2658479718429,-5.68000001999155,
-175.568777423473));
#171465=CARTESIAN_POINT('Ctrl Pts',(59.2686911708562,-5.68000001999092,
-175.5626721919));
#171466=CARTESIAN_POINT('Ctrl Pts',(59.2715106588894,-5.68000001999007,
-175.556553812533));
#171467=CARTESIAN_POINT('Ctrl Pts',(59.2743064287832,-5.68000001998893,
-175.550422281673));
#171468=CARTESIAN_POINT('Ctrl Pts',(59.3235845105522,-5.68000001996885,
-175.44234826609));
#171469=CARTESIAN_POINT('Ctrl Pts',(59.3657187337311,-5.68000001965404,
-175.32923562655));
#171470=CARTESIAN_POINT('Ctrl Pts',(59.3992004790971,-5.68000001961977,
-175.214817860028));
#171471=CARTESIAN_POINT('Ctrl Pts',(59.4149912346775,-5.68000001960361,
-175.160855828914));
#171472=CARTESIAN_POINT('Ctrl Pts',(59.4289384514506,-5.68000001972945,
-175.106577823109));
#171473=CARTESIAN_POINT('Ctrl Pts',(59.4410301448459,-5.68000001987896,
-175.051984501471));
#171474=CARTESIAN_POINT('Ctrl Pts',(59.4606225263251,-5.68000002012122,
-174.963525991253));
#171475=CARTESIAN_POINT('Ctrl Pts',(59.4753677357896,-5.68000001999999,
-174.874236789973));
#171476=CARTESIAN_POINT('Ctrl Pts',(59.485211909548,-5.68000001999999,-174.784118621956));
#171477=CARTESIAN_POINT('Ctrl Pts',(59.4950560833064,-5.68000001999999,
-174.694000453939));
#171478=CARTESIAN_POINT('Ctrl Pts',(59.5,-5.68000001999999,-174.603053692373));
#171479=CARTESIAN_POINT('Ctrl Pts',(59.5,-5.68000001999999,-174.511260182694));
#171480=CARTESIAN_POINT('Origin',(58.6082745331205,-6.18000001999999,-179.64995));
#171481=CARTESIAN_POINT('',(58.6082745331205,-5.68000001999999,-171.871644662643));
#171482=CARTESIAN_POINT('',(58.6082745331205,-5.68000001999999,-176.785131631246));
#171483=CARTESIAN_POINT('Origin',(58.6082745331205,-6.18000001999999,-171.871644662643));
#171484=CARTESIAN_POINT('',(58.1115942404669,-6.2375212064409,-179.64995));
#171485=CARTESIAN_POINT('Ctrl Pts',(58.4667946194619,-5.68000001999999,
-171.237717270032));
#171486=CARTESIAN_POINT('Ctrl Pts',(57.9641288550927,-5.68000002000002,
-171.47368839131));
#171487=CARTESIAN_POINT('Ctrl Pts',(58.0166638356104,-6.23225639415715,
-171.449026400902));
#171488=CARTESIAN_POINT('Ctrl Pts',(58.559801654985,-5.68000001999999,-171.435840927268));
#171489=CARTESIAN_POINT('Ctrl Pts',(58.0192749608379,-5.68000001999239,
-171.600361788065));
#171490=CARTESIAN_POINT('Ctrl Pts',(58.0790703543615,-6.23572556787351,
-171.581106868264));
#171491=CARTESIAN_POINT('Ctrl Pts',(58.608274529079,-5.68000001999999,-171.650520905847));
#171492=CARTESIAN_POINT('Ctrl Pts',(58.0470269895722,-5.68000001999999,
-171.733866658521));
#171493=CARTESIAN_POINT('Ctrl Pts',(58.1115942404139,-6.23752120598293,
-171.724230304954));
#171494=CARTESIAN_POINT('Ctrl Pts',(58.6082745331205,-5.68000001999999,
-171.871644662643));
#171495=CARTESIAN_POINT('Ctrl Pts',(58.0470269915054,-5.68000001999999,
-171.871644662643));
#171496=CARTESIAN_POINT('Ctrl Pts',(58.1115942404669,-6.2375212064409,-171.871644662643));
#171497=CARTESIAN_POINT('',(58.4667946194619,-5.68000001999999,-171.237717270032));
#171498=CARTESIAN_POINT('Origin',(56.431269633621,-5.68000001999999,-172.018134872838));
#171499=CARTESIAN_POINT('Origin',(58.4667946194619,-6.18000001999999,-171.237717270032));
#171500=CARTESIAN_POINT('Ctrl Pts',(39.9791515366304,-5.68000001999998,
-131.975599874271));
#171501=CARTESIAN_POINT('Ctrl Pts',(39.452498014741,-5.68000001999998,-132.224696623613));
#171502=CARTESIAN_POINT('Ctrl Pts',(39.532390596256,-6.25584930059378,-132.186909005141));
#171503=CARTESIAN_POINT('Ctrl Pts',(46.164205183661,-5.68000001999998,-145.052367414711));
#171504=CARTESIAN_POINT('Ctrl Pts',(45.5680069655751,-5.68000001999999,
-145.12303284731));
#171505=CARTESIAN_POINT('Ctrl Pts',(45.7155147614494,-6.24444363034862,
-145.263691191481));
#171506=CARTESIAN_POINT('Ctrl Pts',(52.3196619691199,-5.68000001999999,
-158.143093167052));
#171507=CARTESIAN_POINT('Ctrl Pts',(51.7735675289641,-5.68000001999999,
-158.300965634462));
#171508=CARTESIAN_POINT('Ctrl Pts',(51.870165118292,-6.23767750446664,-158.354412070984));
#171509=CARTESIAN_POINT('Ctrl Pts',(58.4667946194619,-5.68000001999999,
-171.237717270032));
#171510=CARTESIAN_POINT('Ctrl Pts',(57.9641288550927,-5.68000001999999,
-171.47368839131));
#171511=CARTESIAN_POINT('Ctrl Pts',(58.0166638356104,-6.23225639415715,
-171.449026400902));
#171512=CARTESIAN_POINT('',(39.9791515366304,-5.68000001999998,-131.975599874271));
#171513=CARTESIAN_POINT('Ctrl Pts',(39.9791515366304,-5.68000001999998,
-131.975599874271));
#171514=CARTESIAN_POINT('Ctrl Pts',(46.164205183661,-5.68000001999998,-145.052367414711));
#171515=CARTESIAN_POINT('Ctrl Pts',(52.3196619691199,-5.68000001999999,
-158.143093167052));
#171516=CARTESIAN_POINT('Ctrl Pts',(58.4667946194619,-5.68000001999999,
-171.237717270032));
#171517=CARTESIAN_POINT('Origin',(39.9791515366304,-6.18000001999998,-131.975599874271));
#171518=CARTESIAN_POINT('Ctrl Pts',(39.618753076714,-6.26204052658076,-132.359337517737));
#171519=CARTESIAN_POINT('Ctrl Pts',(39.532762793516,-5.68000001999998,-132.403808231301));
#171520=CARTESIAN_POINT('Ctrl Pts',(40.0568611319685,-5.68000001999998,
-132.132760898312));
#171521=CARTESIAN_POINT('Ctrl Pts',(39.3987722978057,-6.2471624346873,-131.938591278504));
#171522=CARTESIAN_POINT('Ctrl Pts',(39.3306902060804,-5.68000001999999,
-131.97378409023));
#171523=CARTESIAN_POINT('Ctrl Pts',(39.8588799388418,-5.68000001999998,
-131.74924323321));
#171524=CARTESIAN_POINT('Ctrl Pts',(39.2388485421598,-6.2323178027174,-131.500725395993));
#171525=CARTESIAN_POINT('Ctrl Pts',(39.184800952389,-5.68000001999998,-131.524152834328));
#171526=CARTESIAN_POINT('Ctrl Pts',(39.7149524852865,-5.68000001999998,
-131.350461425493));
#171527=CARTESIAN_POINT('Ctrl Pts',(39.0323991983154,-6.20294681074234,
-130.592962730002));
#171528=CARTESIAN_POINT('Ctrl Pts',(39.0100410980795,-5.68000001999998,
-130.601991338715));
#171529=CARTESIAN_POINT('Ctrl Pts',(39.5291545030825,-5.68000001999998,
-130.524411418172));
#171530=CARTESIAN_POINT('Ctrl Pts',(38.9864634800499,-6.18831094500166,
-130.119221198789));
#171531=CARTESIAN_POINT('Ctrl Pts',(38.9779951282223,-5.68000001999999,
-130.125131443124));
#171532=CARTESIAN_POINT('Ctrl Pts',(39.4878153045286,-5.68000001999998,
-130.093651490435));
#171533=CARTESIAN_POINT('Ctrl Pts',(39.0034550536173,-6.17442081705026,
-129.647293013264));
#171534=CARTESIAN_POINT('Ctrl Pts',(39.0089685715929,-5.68000001999997,
-129.647466586728));
#171535=CARTESIAN_POINT('Ctrl Pts',(39.5031107769257,-5.68000001999998,
-129.664863321024));
#171536=CARTESIAN_POINT('',(39.5,-5.68000001999998,-129.839692850412));
#171537=CARTESIAN_POINT('Ctrl Pts',(39.5,-5.68000001999998,-129.839692850412));
#171538=CARTESIAN_POINT('Ctrl Pts',(39.5,-5.68000001999998,-130.074011953488));
#171539=CARTESIAN_POINT('Ctrl Pts',(39.5166979118863,-5.68000001999998,
-130.308218863682));
#171540=CARTESIAN_POINT('Ctrl Pts',(39.5492808611194,-5.68000001999998,
-130.539004174579));
#171541=CARTESIAN_POINT('Ctrl Pts',(39.5682253579849,-5.68000001999998,
-130.673188209537));
#171542=CARTESIAN_POINT('Ctrl Pts',(39.592538815617,-5.68000001999998,-130.806215404487));
#171543=CARTESIAN_POINT('Ctrl Pts',(39.6220534778078,-5.68000001999998,
-130.937436349817));
#171544=CARTESIAN_POINT('Ctrl Pts',(39.6907803864138,-5.68000001999998,
-131.242993291602));
#171545=CARTESIAN_POINT('Ctrl Pts',(39.7874256609062,-5.68000001999998,
-131.540730203369));
#171546=CARTESIAN_POINT('Ctrl Pts',(39.9132393368524,-5.68000001999998,
-131.830296953039));
#171547=CARTESIAN_POINT('Ctrl Pts',(39.9343840561751,-5.68000001999998,
-131.878962629492));
#171548=CARTESIAN_POINT('Ctrl Pts',(39.9563527642584,-5.68000001999998,
-131.927397503922));
#171549=CARTESIAN_POINT('Ctrl Pts',(39.9791515366304,-5.68000001999998,
-131.975599874271));
#171550=CARTESIAN_POINT('Origin',(39.5,-6.18000001999998,-129.839692850412));
#171551=CARTESIAN_POINT('Origin',(39.5,-6.18000001999998,-55.24995));
#171552=CARTESIAN_POINT('',(39.5,-5.68000001999998,-102.218950121094));
#171553=CARTESIAN_POINT('',(39.5,-5.68000001999998,-55.24995));
#171554=CARTESIAN_POINT('Origin',(39.5,-6.18000001999998,-102.218950121094));
#171555=CARTESIAN_POINT('Ctrl Pts',(39.,-6.18000001999998,-102.218950121094));
#171556=CARTESIAN_POINT('Ctrl Pts',(39.,-5.68000001999997,-102.218950121094));
#171557=CARTESIAN_POINT('Ctrl Pts',(39.5,-5.68000001999998,-102.218950121094));
#171558=CARTESIAN_POINT('Ctrl Pts',(39.,-6.19216140385576,-101.811197248376));
#171559=CARTESIAN_POINT('Ctrl Pts',(38.9876888787772,-5.68000001999998,
-101.806176686079));
#171560=CARTESIAN_POINT('Ctrl Pts',(39.5000000028438,-5.68000001999998,
-101.848394057804));
#171561=CARTESIAN_POINT('Ctrl Pts',(39.0453283089643,-6.20458878978192,
-101.411268531309));
#171562=CARTESIAN_POINT('Ctrl Pts',(39.0208449410789,-5.68000001999935,
-101.403186844504));
#171563=CARTESIAN_POINT('Ctrl Pts',(39.5407954776771,-5.68000001999998,
-101.484716832152));
#171564=CARTESIAN_POINT('Ctrl Pts',(39.2226569363477,-6.22996106887011,
-100.626634066533));
#171565=CARTESIAN_POINT('Ctrl Pts',(39.1707994584459,-5.68000002000062,
-100.606268005686));
#171566=CARTESIAN_POINT('Ctrl Pts',(39.7003912431037,-5.68000001999998,
-100.770720159946));
#171567=CARTESIAN_POINT('Ctrl Pts',(39.3562549507175,-6.24299658541821,
-100.239515789679));
#171568=CARTESIAN_POINT('Ctrl Pts',(39.2916053087195,-5.68000001999999,
-100.209430566875));
#171569=CARTESIAN_POINT('Ctrl Pts',(39.8206290570768,-5.68000001999998,
-100.418199709297));
#171570=CARTESIAN_POINT('Ctrl Pts',(39.532390596256,-6.25584930059378,-99.8717339663646));
#171571=CARTESIAN_POINT('Ctrl Pts',(39.4524980147409,-5.68000001999997,
-99.8339463478928));
#171572=CARTESIAN_POINT('Ctrl Pts',(39.9791515366304,-5.68000001999998,
-100.083043097235));
#171573=CARTESIAN_POINT('',(39.9791515366304,-5.68000001999998,-100.083043097235));
#171574=CARTESIAN_POINT('Ctrl Pts',(39.9791515366304,-5.68000001999998,
-100.083043097235));
#171575=CARTESIAN_POINT('Ctrl Pts',(39.8867451235786,-5.68000001999998,
-100.278413622974));
#171576=CARTESIAN_POINT('Ctrl Pts',(39.8073027352592,-5.68000001999998,
-100.479790373913));
#171577=CARTESIAN_POINT('Ctrl Pts',(39.7413121766283,-5.68000001999998,
-100.684533556806));
#171578=CARTESIAN_POINT('Ctrl Pts',(39.6941478985853,-5.68000001999998,
-100.830866071725));
#171579=CARTESIAN_POINT('Ctrl Pts',(39.6538540640997,-5.68000001999998,
-100.978917355183));
#171580=CARTESIAN_POINT('Ctrl Pts',(39.6205933601941,-5.68000001999998,
-101.127718496005));
#171581=CARTESIAN_POINT('Ctrl Pts',(39.551582895664,-5.68000001999998,-101.436456274974));
#171582=CARTESIAN_POINT('Ctrl Pts',(39.5117440271939,-5.68000001999998,
-101.750163184502));
#171583=CARTESIAN_POINT('Ctrl Pts',(39.5022324725657,-5.68000001999998,
-102.069036097533));
#171584=CARTESIAN_POINT('Ctrl Pts',(39.5007456673957,-5.68000001999998,
-102.118880935121));
#171585=CARTESIAN_POINT('Ctrl Pts',(39.5,-5.68000001999998,-102.168852019186));
#171586=CARTESIAN_POINT('Ctrl Pts',(39.5,-5.68000001999998,-102.218950121094));
#171587=CARTESIAN_POINT('',(39.5323905862198,-6.25584928266823,-99.8717340064415));
#171588=CARTESIAN_POINT('Origin',(39.9791515366304,-6.18000001999998,-100.083043097235));
#171589=CARTESIAN_POINT('Ctrl Pts',(39.,-6.18000001999998,-102.218950121094));
#171590=CARTESIAN_POINT('Ctrl Pts',(39.,-6.18280348526599,-102.124954155648));
#171591=CARTESIAN_POINT('Ctrl Pts',(39.002404218496,-6.1857384871018,-102.026328836378));
#171592=CARTESIAN_POINT('Ctrl Pts',(39.0079897759941,-6.18884348395754,
-101.923270891007));
#171593=CARTESIAN_POINT('Ctrl Pts',(39.0125734589699,-6.19139154137743,
-101.838698321506));
#171594=CARTESIAN_POINT('Ctrl Pts',(39.0193007259262,-6.19405410413894,
-101.751140850617));
#171595=CARTESIAN_POINT('Ctrl Pts',(39.0286266629022,-6.19685324413035,
-101.660712168677));
#171596=CARTESIAN_POINT('Ctrl Pts',(39.0389718041625,-6.1999582939171,-101.560400801459));
#171597=CARTESIAN_POINT('Ctrl Pts',(39.0525152513023,-6.2032250360155,-101.456576568294));
#171598=CARTESIAN_POINT('Ctrl Pts',(39.0698700180508,-6.20663833765055,
-101.34953622736));
#171599=CARTESIAN_POINT('Ctrl Pts',(39.078547401425,-6.20834498846808,-101.296016056893));
#171600=CARTESIAN_POINT('Ctrl Pts',(39.0881773224577,-6.21008774743007,
-101.241693476407));
#171601=CARTESIAN_POINT('Ctrl Pts',(39.0988327090458,-6.21186142692311,
-101.186615167821));
#171602=CARTESIAN_POINT('Ctrl Pts',(39.1041604023398,-6.21274826666963,
-101.159076013528));
#171603=CARTESIAN_POINT('Ctrl Pts',(39.1097444325043,-6.21364284141544,
-101.131347913177));
#171604=CARTESIAN_POINT('Ctrl Pts',(39.1155935001094,-6.21454424764705,
-101.1034374055));
#171605=CARTESIAN_POINT('Ctrl Pts',(39.1185180339119,-6.21499495076286,
-101.089482151662));
#171606=CARTESIAN_POINT('Ctrl Pts',(39.1215088240554,-6.21544736233241,
-101.075481294353));
#171607=CARTESIAN_POINT('Ctrl Pts',(39.1245669329916,-6.21590136327086,
-101.061435665813));
#171608=CARTESIAN_POINT('Ctrl Pts',(39.1260959874597,-6.21612836374009,
-101.054412851542));
#171609=CARTESIAN_POINT('Ctrl Pts',(39.1276418714215,-6.21635576159457,
-101.047378844344));
#171610=CARTESIAN_POINT('Ctrl Pts',(39.1292047157078,-6.21658354115136,
-101.040333750366));
#171611=CARTESIAN_POINT('Ctrl Pts',(39.129986137851,-6.21669743092976,-101.036811203377));
#171612=CARTESIAN_POINT('Ctrl Pts',(39.1307718000616,-6.21681141613672,
-101.033285884685));
#171613=CARTESIAN_POINT('Ctrl Pts',(39.1315617185623,-6.21692549475772,
-101.0297578077));
#171614=CARTESIAN_POINT('Ctrl Pts',(39.132351637063,-6.21703957337873,-101.026229730715));
#171615=CARTESIAN_POINT('Ctrl Pts',(39.1334695671107,-6.21720007707638,
-101.021266095499));
#171616=CARTESIAN_POINT('Ctrl Pts',(39.133944259014,-6.21726800786083,-101.019165315283));
#171617=CARTESIAN_POINT('Ctrl Pts',(39.1339603748108,-6.21727031411192,
-101.019093993765));
#171618=CARTESIAN_POINT('Ctrl Pts',(39.1339764959978,-6.21727262090659,
-101.019022654972));
#171619=CARTESIAN_POINT('Ctrl Pts',(39.1339926225771,-6.21727492824492,
-101.018951298903));
#171620=CARTESIAN_POINT('Ctrl Pts',(39.1415847113272,-6.21836117952214,
-100.985358210486));
#171621=CARTESIAN_POINT('Ctrl Pts',(39.1503796125988,-6.21956859795788,
-100.947916935796));
#171622=CARTESIAN_POINT('Ctrl Pts',(39.1606238041844,-6.22090460123468,
-100.906695960147));
#171623=CARTESIAN_POINT('Ctrl Pts',(39.17086799577,-6.22224060451149,-100.865474984498));
#171624=CARTESIAN_POINT('Ctrl Pts',(39.1825616354608,-6.22370521203984,
-100.820473748147));
#171625=CARTESIAN_POINT('Ctrl Pts',(39.1959980262754,-6.22530555624786,
-100.771786764605));
#171626=CARTESIAN_POINT('Ctrl Pts',(39.2094486874067,-6.22690760012501,
-100.723048072335));
#171627=CARTESIAN_POINT('Ctrl Pts',(39.2246457230915,-6.22864484024711,
-100.670616186616));
#171628=CARTESIAN_POINT('Ctrl Pts',(39.241924393445,-6.23051375185755,-100.614627493635));
#171629=CARTESIAN_POINT('Ctrl Pts',(39.2505637286217,-6.23144820766277,
-100.586633147144));
#171630=CARTESIAN_POINT('Ctrl Pts',(39.2597240993998,-6.23241542427668,
-100.55775027571));
#171631=CARTESIAN_POINT('Ctrl Pts',(39.2694509482011,-6.23341381238282,
-100.528000444015));
#171632=CARTESIAN_POINT('Ctrl Pts',(39.276025240513,-6.23408861420041,-100.507892792113));
#171633=CARTESIAN_POINT('Ctrl Pts',(39.2826944322007,-6.23476065600126,
-100.487877252101));
#171634=CARTESIAN_POINT('Ctrl Pts',(39.2898035531922,-6.23546318331865,
-100.466971130998));
#171635=CARTESIAN_POINT('Ctrl Pts',(39.2932125749473,-6.23580006475749,
-100.456946062956));
#171636=CARTESIAN_POINT('Ctrl Pts',(39.2967234539788,-6.23614395786301,
-100.446716396379));
#171637=CARTESIAN_POINT('Ctrl Pts',(39.3003783770287,-6.23649853510275,
-100.43617497279));
#171638=CARTESIAN_POINT('Ctrl Pts',(39.3204952758673,-6.23845014786308,
-100.378154393679));
#171639=CARTESIAN_POINT('Ctrl Pts',(39.3404185039594,-6.24028810043805,
-100.323848615045));
#171640=CARTESIAN_POINT('Ctrl Pts',(39.3598170113798,-6.24201123183849,
-100.273176028293));
#171641=CARTESIAN_POINT('Ctrl Pts',(39.3797647162903,-6.24378314737576,
-100.22106883336));
#171642=CARTESIAN_POINT('Ctrl Pts',(39.3991575025057,-6.2454336686,-100.172802869366));
#171643=CARTESIAN_POINT('Ctrl Pts',(39.4176886735397,-6.24696265708752,
-100.128275640437));
#171644=CARTESIAN_POINT('Ctrl Pts',(39.4364188261594,-6.24850806334774,
-100.083270292852));
#171645=CARTESIAN_POINT('Ctrl Pts',(39.454268839455,-6.24992933485546,-100.042083812078));
#171646=CARTESIAN_POINT('Ctrl Pts',(39.4709753783267,-6.25122713146687,
-100.004605647237));
#171647=CARTESIAN_POINT('Ctrl Pts',(39.487832770042,-6.25253664662219,-99.9667890707241));
#171648=CARTESIAN_POINT('Ctrl Pts',(39.5035260267009,-6.25372046637617,
-99.9327475642426));
#171649=CARTESIAN_POINT('Ctrl Pts',(39.5178373919463,-6.25477976690218,
-99.9023711938222));
#171650=CARTESIAN_POINT('Ctrl Pts',(39.5228608944142,-6.25515159717242,
-99.8917086351383));
#171651=CARTESIAN_POINT('Ctrl Pts',(39.5277145979465,-6.25550808835496,
-99.8814977315729));
#171652=CARTESIAN_POINT('Ctrl Pts',(39.5323905785446,-6.25584929930136,
-99.871734003347));
#171653=CARTESIAN_POINT('Ctrl Pts',(58.3535376001277,-5.68000001999999,
-61.0621827299711));
#171654=CARTESIAN_POINT('Ctrl Pts',(57.8507724536939,-5.68000001999999,
-60.826158857425));
#171655=CARTESIAN_POINT('Ctrl Pts',(57.9034184448965,-6.23235646472971,
-60.8508735991007));
#171656=CARTESIAN_POINT('Ctrl Pts',(52.2440275184664,-5.68000001999999,
-74.0763270103718));
#171657=CARTESIAN_POINT('Ctrl Pts',(51.698167660392,-5.68000001999999,-73.9177186732266));
#171658=CARTESIAN_POINT('Ctrl Pts',(51.794541964381,-6.23776491179514,-73.865008277307));
#171659=CARTESIAN_POINT('Ctrl Pts',(46.1262203434603,-5.68000001999998,
-87.0865851147193));
#171660=CARTESIAN_POINT('Ctrl Pts',(45.5309288684318,-5.68000001999999,
-87.0138122441779));
#171661=CARTESIAN_POINT('Ctrl Pts',(45.6775416788308,-6.24451367719405,
-86.8752616229197));
#171662=CARTESIAN_POINT('Ctrl Pts',(39.9791515366304,-5.68000001999998,
-100.083043097235));
#171663=CARTESIAN_POINT('Ctrl Pts',(39.4524980147409,-5.68000001999998,
-99.8339463478929));
#171664=CARTESIAN_POINT('Ctrl Pts',(39.532390596256,-6.25584930059378,-99.8717339663645));
#171665=CARTESIAN_POINT('',(58.3535376001277,-5.68000001999999,-61.0621827299711));
#171666=CARTESIAN_POINT('Ctrl Pts',(58.3535376001277,-5.68000001999999,
-61.0621827299711));
#171667=CARTESIAN_POINT('Ctrl Pts',(52.2440275184664,-5.68000001999999,
-74.0763270103718));
#171668=CARTESIAN_POINT('Ctrl Pts',(46.1262203434603,-5.68000001999998,
-87.0865851147193));
#171669=CARTESIAN_POINT('Ctrl Pts',(39.9791515366304,-5.68000001999998,
-100.083043097235));
#171670=CARTESIAN_POINT('',(57.9034184448965,-6.23235646472971,-60.8508735991007));
#171671=CARTESIAN_POINT('Origin',(58.3535376001277,-6.18000001999999,-61.0621827299711));
#171672=CARTESIAN_POINT('Ctrl Pts',(39.532390596256,-6.25584930059377,-99.8717339663646));
#171673=CARTESIAN_POINT('Ctrl Pts',(40.911961747875,-6.25330448130522,-96.9540582124415));
#171674=CARTESIAN_POINT('Ctrl Pts',(42.3682944181388,-6.25068917191027,
-93.8698701165745));
#171675=CARTESIAN_POINT('Ctrl Pts',(44.6679782761596,-6.24721138579723,
-88.9938194598585));
#171676=CARTESIAN_POINT('Ctrl Pts',(45.4537358898071,-6.24611496597599,
-87.3268411554672));
#171677=CARTESIAN_POINT('Ctrl Pts',(46.6611636792454,-6.24453107456046,
-84.7639315706514));
#171678=CARTESIAN_POINT('Ctrl Pts',(47.2720753433432,-6.24375324528844,
-83.4668662461863));
#171679=CARTESIAN_POINT('Ctrl Pts',(47.9974003487209,-6.24285185802002,
-81.9263049365434));
#171680=CARTESIAN_POINT('Ctrl Pts',(48.3632113198011,-6.24239951385331,
-81.1491946739469));
#171681=CARTESIAN_POINT('Ctrl Pts',(48.5698654666445,-6.24214413381149,
-80.7101493240497));
#171682=CARTESIAN_POINT('Ctrl Pts',(48.6718338188353,-6.24201809389911,
-80.4935007144023));
#171683=CARTESIAN_POINT('Ctrl Pts',(48.7245329191054,-6.24195292792929,
-80.3815296305629));
#171684=CARTESIAN_POINT('Ctrl Pts',(48.7283847105348,-6.24194816478105,
-80.3733456164068));
#171685=CARTESIAN_POINT('Ctrl Pts',(51.5332710940133,-6.23847954177077,
-74.4137117874514));
#171686=CARTESIAN_POINT('Ctrl Pts',(54.5907059876843,-6.23528934935773,
-67.9081592073181));
#171687=CARTESIAN_POINT('Ctrl Pts',(57.9034184448965,-6.23235646472971,
-60.8508735991007));
#171688=CARTESIAN_POINT('Ctrl Pts',(39.,-5.46102446043621,-101.971753092595));
#171689=CARTESIAN_POINT('Ctrl Pts',(39.,-5.86351617202512,-100.855722952121));
#171690=CARTESIAN_POINT('Ctrl Pts',(39.5330007135517,-6.22310220971892,
-99.8586617838914));
#171691=CARTESIAN_POINT('Ctrl Pts',(39.,-6.48207062104881,-102.33998922066));
#171692=CARTESIAN_POINT('Ctrl Pts',(38.9999999999962,-6.82975403393395,
-101.225648609944));
#171693=CARTESIAN_POINT('Ctrl Pts',(39.5158163721933,-7.1434218710037,-100.226898392254));
#171694=CARTESIAN_POINT('Ctrl Pts',(39.,-7.52739464652098,-102.644232481647));
#171695=CARTESIAN_POINT('Ctrl Pts',(39.,-7.81966925102655,-101.531783862877));
#171696=CARTESIAN_POINT('Ctrl Pts',(39.50142226749,-8.08385740698738,-100.53114117287));
#171697=CARTESIAN_POINT('Ctrl Pts',(39.,-9.13906178103241,-102.985482622022));
#171698=CARTESIAN_POINT('Ctrl Pts',(39.,-9.34536808184436,-101.875027810475));
#171699=CARTESIAN_POINT('Ctrl Pts',(39.485193560998,-9.53196095727464,-100.872391313355));
#171700=CARTESIAN_POINT('Ctrl Pts',(39.,-9.68642581410213,-103.080287874832));
#171701=CARTESIAN_POINT('Ctrl Pts',(39.,-9.86335482772211,-101.970380205613));
#171702=CARTESIAN_POINT('Ctrl Pts',(39.4806657492121,-10.0234751165263,
-100.967196566129));
#171703=CARTESIAN_POINT('Ctrl Pts',(39.,-10.7786703656218,-103.225601722724));
#171704=CARTESIAN_POINT('Ctrl Pts',(39.,-10.8967689955421,-102.116504004052));
#171705=CARTESIAN_POINT('Ctrl Pts',(39.4737139394979,-11.0038787161503,
-101.11251041402));
#171706=CARTESIAN_POINT('Ctrl Pts',(39.,-11.32407160958,-103.276476522877));
#171707=CARTESIAN_POINT('Ctrl Pts',(39.0000000000038,-11.4127969575427,
-102.167673995048));
#171708=CARTESIAN_POINT('Ctrl Pts',(39.4712727906473,-11.493239882702,-101.16338521793));
#171709=CARTESIAN_POINT('Ctrl Pts',(39.,-11.8687533077036,-103.305636003273));
#171710=CARTESIAN_POINT('Ctrl Pts',(39.,-11.9281041096302,-102.196998431102));
#171711=CARTESIAN_POINT('Ctrl Pts',(39.4698732852484,-11.9818774403001,
-101.192544694569));
#171712=CARTESIAN_POINT('',(39.470299293038,-11.8429061139822,-101.18366751689));
#171713=CARTESIAN_POINT('Ctrl Pts',(39.4702992602694,-11.8429061149159,
-101.183667501603));
#171714=CARTESIAN_POINT('Ctrl Pts',(39.4714157143871,-11.5010965926809,
-101.160397081716));
#171715=CARTESIAN_POINT('Ctrl Pts',(39.4730376963082,-11.1594525392257,
-101.126547380785));
#171716=CARTESIAN_POINT('Ctrl Pts',(39.4751582271049,-10.8177256429982,
-101.08215692154));
#171717=CARTESIAN_POINT('Ctrl Pts',(39.4757870845495,-10.7163842698549,
-101.068992637007));
#171718=CARTESIAN_POINT('Ctrl Pts',(39.4764598030603,-10.6150355967854,
-101.054900989002));
#171719=CARTESIAN_POINT('Ctrl Pts',(39.4771762399035,-10.5136731096961,
-101.039882102517));
#171720=CARTESIAN_POINT('Ctrl Pts',(39.4773994513674,-10.4820928394407,
-101.035202851763));
#171721=CARTESIAN_POINT('Ctrl Pts',(39.4776269777968,-10.4505092705441,
-101.03043207286));
#171722=CARTESIAN_POINT('Ctrl Pts',(39.4778587715597,-10.418924943814,-101.025570636239));
#171723=CARTESIAN_POINT('Ctrl Pts',(39.4790878128322,-10.2514552042292,
-100.999793815603));
#171724=CARTESIAN_POINT('Ctrl Pts',(39.4804337172402,-10.0839399037763,
-100.971475421647));
#171725=CARTESIAN_POINT('Ctrl Pts',(39.4819042200723,-9.91634393709639,
-100.940630337302));
#171726=CARTESIAN_POINT('Ctrl Pts',(39.4825182652867,-9.8463600519611,-100.927750201326));
#171727=CARTESIAN_POINT('Ctrl Pts',(39.4831540697067,-9.77636222049717,
-100.91442887348));
#171728=CARTESIAN_POINT('Ctrl Pts',(39.4838123356305,-9.70634878432406,
-100.900664901762));
#171729=CARTESIAN_POINT('Ctrl Pts',(39.4849296694305,-9.58750869878921,
-100.877302077913));
#171730=CARTESIAN_POINT('Ctrl Pts',(39.4861104003532,-9.46862238083702,
-100.852667202291));
#171731=CARTESIAN_POINT('Ctrl Pts',(39.4873506398552,-9.34967902011701,
-100.826758874769));
#171732=CARTESIAN_POINT('Ctrl Pts',(39.4879707596062,-9.29020733975701,
-100.813804711008));
#171733=CARTESIAN_POINT('Ctrl Pts',(39.4886056849366,-9.23072140625689,
-100.800532150721));
#171734=CARTESIAN_POINT('Ctrl Pts',(39.4892544851105,-9.17121992545558,
-100.786940815446));
#171735=CARTESIAN_POINT('Ctrl Pts',(39.4895788851974,-9.14146918505491,
-100.780145147809));
#171736=CARTESIAN_POINT('Ctrl Pts',(39.4899067493168,-9.11171455870462,
-100.77326978421));
#171737=CARTESIAN_POINT('Ctrl Pts',(39.4902378654102,-9.08195585995781,
-100.76631480003));
#171738=CARTESIAN_POINT('Ctrl Pts',(39.4903578915464,-9.07116864151043,
-100.76379369068));
#171739=CARTESIAN_POINT('Ctrl Pts',(39.4904803125607,-9.06020644484888,
-100.76122118129));
#171740=CARTESIAN_POINT('Ctrl Pts',(39.4906030413979,-9.04925973560232,
-100.758641447143));
#171741=CARTESIAN_POINT('Ctrl Pts',(39.4908188845949,-9.03000775884592,
-100.754104468886));
#171742=CARTESIAN_POINT('Ctrl Pts',(39.4910357318681,-9.01079978065262,
-100.749544053052));
#171743=CARTESIAN_POINT('Ctrl Pts',(39.4912417658406,-8.99266748358911,
-100.745210479822));
#171744=CARTESIAN_POINT('Ctrl Pts',(39.496412730107,-8.53758981341583,-100.636448065327));
#171745=CARTESIAN_POINT('Ctrl Pts',(39.5024412863883,-8.08236775931935,
-100.509291986928));
#171746=CARTESIAN_POINT('Ctrl Pts',(39.5093071903843,-7.62642775454604,
-100.363713049691));
#171747=CARTESIAN_POINT('Ctrl Pts',(39.5152832138175,-7.22958151925537,
-100.237002402292));
#171748=CARTESIAN_POINT('Ctrl Pts',(39.5218935920656,-6.83219144237864,
-100.096334431291));
#171749=CARTESIAN_POINT('Ctrl Pts',(39.5291209804618,-6.43385878842381,
-99.9417276591744));
#171750=CARTESIAN_POINT('Ctrl Pts',(39.5301971998785,-6.37454367859804,
-99.9187053998219));
#171751=CARTESIAN_POINT('Ctrl Pts',(39.5312870926446,-6.31520762564802,
-99.8953741493161));
#171752=CARTESIAN_POINT('Ctrl Pts',(39.5323905926521,-6.25584926600113,
-99.8717340627362));
#171753=CARTESIAN_POINT('Origin',(46.4732015204142,-11.8458781654969,-103.848204069008));
#171754=CARTESIAN_POINT('Ctrl Pts',(39.4702993039609,-11.842906113671,-101.183667521985));
#171755=CARTESIAN_POINT('Ctrl Pts',(39.4816972464314,-12.33000002,-101.188984626754));
#171756=CARTESIAN_POINT('Ctrl Pts',(39.9232693735648,-12.33000002,-101.394976652855));
#171757=CARTESIAN_POINT('Ctrl Pts',(39.1608544296035,-11.8384595965422,
-101.84673342232));
#171758=CARTESIAN_POINT('Ctrl Pts',(39.1678459389433,-12.3300000200023,
-101.851466764233));
#171759=CARTESIAN_POINT('Ctrl Pts',(39.6447687306727,-12.33000002,-101.991980946201));
#171760=CARTESIAN_POINT('Ctrl Pts',(39.,-11.834085348836,-102.564353929887));
#171761=CARTESIAN_POINT('Ctrl Pts',(39.0040688095373,-12.3300000199977,
-102.567343181294));
#171762=CARTESIAN_POINT('Ctrl Pts',(39.5000000016323,-12.33000002,-102.638067201068));
#171763=CARTESIAN_POINT('Ctrl Pts',(39.,-11.83000002,-103.303524786513));
#171764=CARTESIAN_POINT('Ctrl Pts',(39.,-12.33000002,-103.303524786513));
#171765=CARTESIAN_POINT('Ctrl Pts',(39.5,-12.33000002,-103.303524786513));
#171766=CARTESIAN_POINT('',(39.5,-12.33000002,-103.303524786513));
#171767=CARTESIAN_POINT('Origin',(39.5,-11.83000002,-103.303524786513));
#171768=CARTESIAN_POINT('',(39.9232693735648,-12.33000002,-101.394976652855));
#171769=CARTESIAN_POINT('Origin',(39.9232693735648,-11.83000002,-101.394976652855));
#171770=CARTESIAN_POINT('Origin',(46.190877869282,-12.33000002,-103.784865184748));
#171771=CARTESIAN_POINT('Origin',(39.5,-11.83000002,-55.24995));
#171772=CARTESIAN_POINT('',(39.5,-12.33000002,-128.755118184993));
#171773=CARTESIAN_POINT('Origin',(39.5,-11.83000002,-128.755118184993));
#171774=CARTESIAN_POINT('',(39.5,-12.33000002,-55.24995));
#171775=CARTESIAN_POINT('Ctrl Pts',(39.,-11.83000002,-128.755118184993));
#171776=CARTESIAN_POINT('Ctrl Pts',(39.,-12.33000002,-128.755118184993));
#171777=CARTESIAN_POINT('Ctrl Pts',(39.5,-12.33000002,-128.755118184993));
#171778=CARTESIAN_POINT('Ctrl Pts',(39.,-11.8340442872404,-129.486859645108));
#171779=CARTESIAN_POINT('Ctrl Pts',(39.0040281122736,-12.33000002,-129.483935534574));
#171780=CARTESIAN_POINT('Ctrl Pts',(39.5000000055219,-12.33000002,-129.413887248834));
#171781=CARTESIAN_POINT('Ctrl Pts',(39.1577125252496,-11.8384144493887,
-130.205177204234));
#171782=CARTESIAN_POINT('Ctrl Pts',(39.1646430478985,-12.33000002,-130.200415506093));
#171783=CARTESIAN_POINT('Ctrl Pts',(39.6419410176262,-12.33000002,-130.060600444225));
#171784=CARTESIAN_POINT('Ctrl Pts',(39.4702993039609,-11.8429061136709,
-130.874975449521));
#171785=CARTESIAN_POINT('Ctrl Pts',(39.4816972464314,-12.33000002,-130.869658344752));
#171786=CARTESIAN_POINT('Ctrl Pts',(39.9232693735648,-12.33000002,-130.663666318651));
#171787=CARTESIAN_POINT('',(39.9232693735648,-12.33000002,-130.663666318651));
#171788=CARTESIAN_POINT('Origin',(39.9232693735648,-11.83000002,-130.663666318651));
#171789=CARTESIAN_POINT('Origin',(46.1904260133955,-12.33000002,-128.271059668222));
#171790=CARTESIAN_POINT('Ctrl Pts',(58.8484691650909,-12.33000002,-171.237717270032));
#171791=CARTESIAN_POINT('Ctrl Pts',(58.4031988243933,-12.33000002,-171.445389024352));
#171792=CARTESIAN_POINT('Ctrl Pts',(58.3953999019963,-11.8387575339013,
-171.449026400902));
#171793=CARTESIAN_POINT('Ctrl Pts',(52.5405278046811,-12.33000002,-157.712819732222));
#171794=CARTESIAN_POINT('Ctrl Pts',(52.1019974789428,-12.3300000202716,
-157.93276270106));
#171795=CARTESIAN_POINT('Ctrl Pts',(52.0874768317228,-11.839695897332,-157.924129189572));
#171796=CARTESIAN_POINT('Ctrl Pts',(46.2323452217992,-12.33000002,-144.188034690057));
#171797=CARTESIAN_POINT('Ctrl Pts',(45.801395679434,-12.33000002,-144.421507685211));
#171798=CARTESIAN_POINT('Ctrl Pts',(45.7793173035632,-11.8408682174628,
-144.399344282617));
#171799=CARTESIAN_POINT('Ctrl Pts',(39.9232693735648,-12.33000002,-130.663666318651));
#171800=CARTESIAN_POINT('Ctrl Pts',(39.4816972464314,-12.33000002,-130.869658344752));
#171801=CARTESIAN_POINT('Ctrl Pts',(39.4702993039609,-11.842906113671,-130.874975449521));
#171802=CARTESIAN_POINT('',(58.8484691650909,-12.33000002,-171.237717270032));
#171803=CARTESIAN_POINT('Origin',(58.8484691650909,-11.83000002,-171.237717270032));
#171804=CARTESIAN_POINT('Ctrl Pts',(58.8484691650909,-12.33000002,-171.237717270032));
#171805=CARTESIAN_POINT('Ctrl Pts',(52.5405278046811,-12.33000002,-157.712819732223));
#171806=CARTESIAN_POINT('Ctrl Pts',(46.2323452217992,-12.33000002,-144.188034690057));
#171807=CARTESIAN_POINT('Ctrl Pts',(39.9232693735648,-12.33000002,-130.663666318651));
#171808=CARTESIAN_POINT('Ctrl Pts',(58.9890336736409,-12.33000002,-171.871644662643));
#171809=CARTESIAN_POINT('Ctrl Pts',(58.4985823439911,-12.33000002,-171.871644662643));
#171810=CARTESIAN_POINT('Ctrl Pts',(58.48912660861,-11.8396398505087,-171.871644662643));
#171811=CARTESIAN_POINT('Ctrl Pts',(58.9890336571231,-12.33000002,-171.652832645897));
#171812=CARTESIAN_POINT('Ctrl Pts',(58.4985823327705,-12.33000002,-171.724385262387));
#171813=CARTESIAN_POINT('Ctrl Pts',(58.4891266086039,-11.8396398501934,
-171.725770040011));
#171814=CARTESIAN_POINT('Ctrl Pts',(58.9418960593107,-12.33000002,-171.438034482585));
#171815=CARTESIAN_POINT('Ctrl Pts',(58.46651035226,-12.3300000200013,-171.579769437466));
#171816=CARTESIAN_POINT('Ctrl Pts',(58.4576958292209,-11.8393453695788,
-171.582571135794));
#171817=CARTESIAN_POINT('Ctrl Pts',(58.8484691650909,-12.33000002,-171.237717270032));
#171818=CARTESIAN_POINT('Ctrl Pts',(58.4031988243933,-12.33000002,-171.445389024352));
#171819=CARTESIAN_POINT('Ctrl Pts',(58.3953999019963,-11.8387575339013,
-171.449026400902));
#171820=CARTESIAN_POINT('',(58.9890336736409,-12.33000002,-171.871644662643));
#171821=CARTESIAN_POINT('Origin',(58.9890336736409,-11.83000002,-171.871644662643));
#171822=CARTESIAN_POINT('Origin',(56.7618024059963,-12.33000002,-172.033247591146));
#171823=CARTESIAN_POINT('Origin',(58.9890336736409,-11.83000002,-179.64995));
#171824=CARTESIAN_POINT('',(58.48912660861,-11.8396398505087,-179.64995));
#171825=CARTESIAN_POINT('',(58.9890336736409,-12.33000002,-171.871644662643));
#171826=CARTESIAN_POINT('Ctrl Pts',(60.,-12.83000002,-174.751778045593));
#171827=CARTESIAN_POINT('Ctrl Pts',(60.,-12.33000002,-174.751778045593));
#171828=CARTESIAN_POINT('Ctrl Pts',(59.5,-12.33000002,-174.751778045593));
#171829=CARTESIAN_POINT('Ctrl Pts',(60.,-12.8299432805227,-174.99625355239));
#171830=CARTESIAN_POINT('Ctrl Pts',(59.9999432570754,-12.33000002,-174.996239713811));
#171831=CARTESIAN_POINT('Ctrl Pts',(59.4999999944591,-12.33000002,-174.955507700223));
#171832=CARTESIAN_POINT('Ctrl Pts',(59.9705492201332,-12.8298880430416,
-175.2357685753));
#171833=CARTESIAN_POINT('Ctrl Pts',(59.970440441932,-12.33000002,-175.235742099222));
#171834=CARTESIAN_POINT('Ctrl Pts',(59.4754576845908,-12.33000002,-175.155103617038));
#171835=CARTESIAN_POINT('Ctrl Pts',(59.8547629729398,-12.8297804365705,
-175.705055936053));
#171836=CARTESIAN_POINT('Ctrl Pts',(59.8545561835904,-12.33000002,-175.704977777008));
#171837=CARTESIAN_POINT('Ctrl Pts',(59.3789691429701,-12.33000002,-175.546176541216));
#171838=CARTESIAN_POINT('Ctrl Pts',(59.7670622382429,-12.8297278961218,
-175.935624391263));
#171839=CARTESIAN_POINT('Ctrl Pts',(59.7668149966741,-12.3300000199993,
-175.935510188038));
#171840=CARTESIAN_POINT('Ctrl Pts',(59.3058851982286,-12.33000002,-175.738316981093));
#171841=CARTESIAN_POINT('Ctrl Pts',(59.5424974437338,-12.829631160742,-176.362316424594));
#171842=CARTESIAN_POINT('Ctrl Pts',(59.5421886833106,-12.3300000200007,
-176.362111673427));
#171843=CARTESIAN_POINT('Ctrl Pts',(59.1187478700854,-12.33000002,-176.093893786804));
#171844=CARTESIAN_POINT('Ctrl Pts',(59.4031198237833,-12.8295857148276,
-176.563935060575));
#171845=CARTESIAN_POINT('Ctrl Pts',(59.4027925942033,-12.3300000200005,
-176.563680085108));
#171846=CARTESIAN_POINT('Ctrl Pts',(59.0025998517383,-12.33000002,-176.261909367341));
#171847=CARTESIAN_POINT('Ctrl Pts',(59.0805964717746,-12.8295042980195,
-176.926638521725));
#171848=CARTESIAN_POINT('Ctrl Pts',(59.0802573870172,-12.3300000199995,
-176.926274585031));
#171849=CARTESIAN_POINT('Ctrl Pts',(58.73383039456,-12.33000002,-176.564162347066));
#171850=CARTESIAN_POINT('Ctrl Pts',(58.8998912349101,-12.8294686666967,
-177.086178383746));
#171851=CARTESIAN_POINT('Ctrl Pts',(58.8995591592806,-12.3300000199849,
-177.085762552869));
#171852=CARTESIAN_POINT('Ctrl Pts',(58.5832426931945,-12.33000002,-176.697112268189));
#171853=CARTESIAN_POINT('Ctrl Pts',(58.699732291115,-12.8294380172077,-177.223805132118));
#171854=CARTESIAN_POINT('Ctrl Pts',(58.699414230519,-12.33000002,-177.223342557405));
#171855=CARTESIAN_POINT('Ctrl Pts',(58.4164435759292,-12.33000002,-176.811801263203));
#171856=CARTESIAN_POINT('',(59.5,-12.33000002,-174.751778045594));
#171857=CARTESIAN_POINT('Ctrl Pts',(59.5,-12.33000002,-174.751778045594));
#171858=CARTESIAN_POINT('Ctrl Pts',(59.5,-12.33000002,-174.844927230273));
#171859=CARTESIAN_POINT('Ctrl Pts',(59.4948737621761,-12.3300000199839,
-174.937101433735));
#171860=CARTESIAN_POINT('Ctrl Pts',(59.4847164002782,-12.3300000200162,
-175.028427073489));
#171861=CARTESIAN_POINT('Ctrl Pts',(59.4744815669569,-12.3300000200487,
-175.120449264903));
#171862=CARTESIAN_POINT('Ctrl Pts',(59.4591385334095,-12.3300000199961,
-175.211609900805));
#171863=CARTESIAN_POINT('Ctrl Pts',(59.438732272217,-12.3300000210573,-175.302031274497));
#171864=CARTESIAN_POINT('Ctrl Pts',(59.4350695133288,-12.3300000212478,
-175.318261179968));
#171865=CARTESIAN_POINT('Ctrl Pts',(59.4312434964565,-12.3300000214808,
-175.334467250167));
#171866=CARTESIAN_POINT('Ctrl Pts',(59.4272543062711,-12.330000021774,-175.350650168439));
#171867=CARTESIAN_POINT('Ctrl Pts',(59.4106840236565,-12.3300000229918,
-175.417870711165));
#171868=CARTESIAN_POINT('Ctrl Pts',(59.3911649601375,-12.3300000250948,
-175.484771053152));
#171869=CARTESIAN_POINT('Ctrl Pts',(59.3688362082559,-12.3300000304207,
-175.550947464116));
#171870=CARTESIAN_POINT('Ctrl Pts',(59.3452983767326,-12.330000036035,-175.620707261724));
#171871=CARTESIAN_POINT('Ctrl Pts',(59.318757276387,-12.3300000404266,-175.689252183756));
#171872=CARTESIAN_POINT('Ctrl Pts',(59.2894219594714,-12.3300000414655,
-175.756217087947));
#171873=CARTESIAN_POINT('Ctrl Pts',(59.265578831198,-12.3300000423099,-175.810644752902));
#171874=CARTESIAN_POINT('Ctrl Pts',(59.2398885853161,-12.3300000411891,
-175.864029149378));
#171875=CARTESIAN_POINT('Ctrl Pts',(59.2124386122788,-12.330000039031,-175.916169632722));
#171876=CARTESIAN_POINT('Ctrl Pts',(59.1785809256147,-12.3300000363691,
-175.980481395257));
#171877=CARTESIAN_POINT('Ctrl Pts',(59.1417731864694,-12.3300000322739,
-176.043500821863));
#171878=CARTESIAN_POINT('Ctrl Pts',(59.1021371288072,-12.3300000288604,
-176.105011973128));
#171879=CARTESIAN_POINT('Ctrl Pts',(59.0666804433847,-12.3300000258069,
-176.16003716153));
#171880=CARTESIAN_POINT('Ctrl Pts',(59.0289595515133,-12.3300000233307,
-176.21385559589));
#171881=CARTESIAN_POINT('Ctrl Pts',(58.9890336736408,-12.3300000218957,
-176.26629097911));
#171882=CARTESIAN_POINT('Origin',(59.5,-12.83000002,-174.751778045594));
#171883=CARTESIAN_POINT('Ctrl Pts',(39.9232693735648,-12.33000002,-101.394976652855));
#171884=CARTESIAN_POINT('Ctrl Pts',(39.4816972464314,-12.33000002,-101.188984626754));
#171885=CARTESIAN_POINT('Ctrl Pts',(39.4702993039609,-11.842906113671,-101.183667521985));
#171886=CARTESIAN_POINT('Ctrl Pts',(46.1948314689912,-12.33000002,-87.9510241496856));
#171887=CARTESIAN_POINT('Ctrl Pts',(45.7637467547491,-12.3300000200387,
-87.7178689736084));
#171888=CARTESIAN_POINT('Ctrl Pts',(45.741803891981,-11.8408803347909,-87.7397145657271));
#171889=CARTESIAN_POINT('Ctrl Pts',(52.4655100689676,-12.33000002,-74.5066595330064));
#171890=CARTESIAN_POINT('Ctrl Pts',(52.0269437270063,-12.3300000197686,
-74.2868280745294));
#171891=CARTESIAN_POINT('Ctrl Pts',(52.0124594137882,-11.8397106642502,
-74.2953500811619));
#171892=CARTESIAN_POINT('Ctrl Pts',(58.7359481105893,-12.33000002,-61.0621827299711));
#171893=CARTESIAN_POINT('Ctrl Pts',(58.2906927660831,-12.33000002,-60.8545178210735));
#171894=CARTESIAN_POINT('Ctrl Pts',(58.2828791719688,-11.838774304476,-60.8508735991007));
#171895=CARTESIAN_POINT('',(58.2828791719688,-11.838774304476,-60.8508735991007));
#171896=CARTESIAN_POINT('Ctrl Pts',(58.2828791719688,-11.838774304476,-60.8508735991007));
#171897=CARTESIAN_POINT('Ctrl Pts',(55.3775064758257,-11.8392081628502,
-67.080315389494));
#171898=CARTESIAN_POINT('Ctrl Pts',(52.6531073433158,-11.8396682774539,
-72.921588901895));
#171899=CARTESIAN_POINT('Ctrl Pts',(50.1096592410629,-11.8401779861306,
-78.3746829039473));
#171900=CARTESIAN_POINT('Ctrl Pts',(47.223103444897,-11.8407564538154,-84.5633918792627));
#171901=CARTESIAN_POINT('Ctrl Pts',(44.5696120347148,-11.841398417424,-90.2521277977888));
#171902=CARTESIAN_POINT('Ctrl Pts',(42.149198203414,-11.8420910505548,-95.4408968196894));
#171903=CARTESIAN_POINT('Ctrl Pts',(41.2220298729399,-11.8423563719205,
-97.4285165601807));
#171904=CARTESIAN_POINT('Ctrl Pts',(40.329062911927,-11.8426287216759,-99.3427731426528));
#171905=CARTESIAN_POINT('Ctrl Pts',(39.4702993039609,-11.842906113671,-101.183667521985));
#171906=CARTESIAN_POINT('',(58.7359481105893,-12.33000002,-61.0621827299711));
#171907=CARTESIAN_POINT('Origin',(58.7359481105893,-11.83000002,-61.0621827299711));
#171908=CARTESIAN_POINT('Ctrl Pts',(39.9232693735648,-12.33000002,-101.394976652855));
#171909=CARTESIAN_POINT('Ctrl Pts',(46.1948314689912,-12.33000002,-87.9510241496856));
#171910=CARTESIAN_POINT('Ctrl Pts',(52.4655100689676,-12.33000002,-74.5066595330064));
#171911=CARTESIAN_POINT('Ctrl Pts',(58.7359481105893,-12.33000002,-61.0621827299711));
#171912=CARTESIAN_POINT('Origin',(59.5,-12.83000002,-55.24995));
#171913=CARTESIAN_POINT('',(59.5,-12.33000002,-57.909894348981));
#171914=CARTESIAN_POINT('',(60.,-12.83000002,-57.909894348981));
#171915=CARTESIAN_POINT('Origin',(59.5,-12.83000002,-57.909894348981));
#171916=CARTESIAN_POINT('',(60.,-12.83000002,-57.911664394164));
#171917=CARTESIAN_POINT('',(59.5,-12.33000002,-174.749818876635));
#171918=CARTESIAN_POINT('Origin',(60.,-2.55003103885676E-14,0.));
#171919=CARTESIAN_POINT('',(60.,-13.33000002,-57.9104088126279));
#171920=CARTESIAN_POINT('Origin',(60.,-12.9674754042923,-167.271246742336));
#171921=CARTESIAN_POINT('',(60.,-13.33000002,-174.748117418411));
#171922=CARTESIAN_POINT('Origin',(59.5,-13.33000002,-55.24995));
#171923=CARTESIAN_POINT('',(59.5,-13.83000002,-57.9104088126279));
#171924=CARTESIAN_POINT('Origin',(59.5,-13.33000002,-57.9104088126279));
#171925=CARTESIAN_POINT('',(59.5,-13.83000002,-174.751208632418));
#171926=CARTESIAN_POINT('',(59.5,-13.83000002,-57.9132014677655));
#171927=CARTESIAN_POINT('Origin',(59.5,-13.33000002,-174.751208632418));
#171928=CARTESIAN_POINT('Ctrl Pts',(59.5,-13.83000002,-174.751208632418));
#171929=CARTESIAN_POINT('Ctrl Pts',(60.,-13.83000002,-174.751208632417));
#171930=CARTESIAN_POINT('Ctrl Pts',(60.,-13.33000002,-174.751208632418));
#171931=CARTESIAN_POINT('Ctrl Pts',(59.499999994458,-13.83000002,-174.955005950799));
#171932=CARTESIAN_POINT('Ctrl Pts',(59.9998505155736,-13.83000002,-174.995728395116));
#171933=CARTESIAN_POINT('Ctrl Pts',(60.,-13.3301495200469,-174.995764866376));
#171934=CARTESIAN_POINT('Ctrl Pts',(59.4754418884424,-13.83000002,-175.154666905584));
#171935=CARTESIAN_POINT('Ctrl Pts',(59.9702437452671,-13.8300000199993,
-175.235287718005));
#171936=CARTESIAN_POINT('Ctrl Pts',(59.9705302647519,-13.3302950638363,
-175.235357479373));
#171937=CARTESIAN_POINT('Ctrl Pts',(59.3788903697392,-13.83000002,-175.545864512034));
#171938=CARTESIAN_POINT('Ctrl Pts',(59.8541239849711,-13.8300000200007,
-175.704587709371));
#171939=CARTESIAN_POINT('Ctrl Pts',(59.8546684450659,-13.3305785951146,
-175.704793574078));
#171940=CARTESIAN_POINT('Ctrl Pts',(59.3057599866248,-13.83000002,-175.738059080183));
#171941=CARTESIAN_POINT('Ctrl Pts',(59.7662611489698,-13.8300000199988,
-175.935125812779));
#171942=CARTESIAN_POINT('Ctrl Pts',(59.7669119843163,-13.3307170303008,
-175.935426552567));
#171943=CARTESIAN_POINT('Ctrl Pts',(59.1185058620249,-13.83000002,-176.093723731171));
#171944=CARTESIAN_POINT('Ctrl Pts',(59.5413945721013,-13.8300000200012,
-176.361684206804));
#171945=CARTESIAN_POINT('Ctrl Pts',(59.5422070340633,-13.3309719059141,
-176.362223209373));
#171946=CARTESIAN_POINT('Ctrl Pts',(59.0022803225031,-13.83000002,-176.261780328219));
#171947=CARTESIAN_POINT('Ctrl Pts',(59.4018755020326,-13.8300000199995,
-176.563219594419));
#171948=CARTESIAN_POINT('Ctrl Pts',(59.4027363887007,-13.331091646732,-176.563890694693));
#171949=CARTESIAN_POINT('Ctrl Pts',(58.7333577194631,-13.83000002,-176.564062061699));
#171950=CARTESIAN_POINT('Ctrl Pts',(59.0791375439908,-13.8300000200005,
-176.925670411677));
#171951=CARTESIAN_POINT('Ctrl Pts',(59.0800292616587,-13.3313061338651,
-176.92662799811));
#171952=CARTESIAN_POINT('Ctrl Pts',(58.5826842101506,-13.83000002,-176.697016027753));
#171953=CARTESIAN_POINT('Ctrl Pts',(58.8983479608961,-13.830000020003,-177.085078467603));
#171954=CARTESIAN_POINT('Ctrl Pts',(58.8992210551541,-13.3313999972609,
-177.086172425279));
#171955=CARTESIAN_POINT('Ctrl Pts',(58.4157868605055,-13.83000002,-176.811694866106));
#171956=CARTESIAN_POINT('Ctrl Pts',(58.698108161756,-13.83000002,-177.222569964948));
#171957=CARTESIAN_POINT('Ctrl Pts',(58.6989442326066,-13.3314807280565,
-177.223786737086));
#171958=CARTESIAN_POINT('Ctrl Pts',(58.9842656455839,-13.8300000182384,
-176.2719717603));
#171959=CARTESIAN_POINT('Ctrl Pts',(59.0284765648177,-13.8300000166394,
-176.214285352615));
#171960=CARTESIAN_POINT('Ctrl Pts',(59.0700022374974,-13.8300000137057,
-176.154919321395));
#171961=CARTESIAN_POINT('Ctrl Pts',(59.108769049557,-13.8300000102313,-176.094105263609));
#171962=CARTESIAN_POINT('Ctrl Pts',(59.1458171677547,-13.830000006911,-176.0359873457));
#171963=CARTESIAN_POINT('Ctrl Pts',(59.18034578997,-13.8300000031738,-175.976545944298));
#171964=CARTESIAN_POINT('Ctrl Pts',(59.2122555343191,-13.8300000007997,
-175.915955958697));
#171965=CARTESIAN_POINT('Ctrl Pts',(59.2455714173137,-13.829999998321,-175.852696007478));
#171966=CARTESIAN_POINT('Ctrl Pts',(59.2762989800144,-13.8299999975166,
-175.787603392926));
#171967=CARTESIAN_POINT('Ctrl Pts',(59.3042804787193,-13.8299999996639,
-175.721026919923));
#171968=CARTESIAN_POINT('Ctrl Pts',(59.3272704921691,-13.8300000014281,
-175.666326704402));
#171969=CARTESIAN_POINT('Ctrl Pts',(59.3484061154264,-13.8300000052622,
-175.610623961591));
#171970=CARTESIAN_POINT('Ctrl Pts',(59.3675737697888,-13.8300000097259,
-175.554108016098));
#171971=CARTESIAN_POINT('Ctrl Pts',(59.3904098382371,-13.8300000150439,
-175.486775729355));
#171972=CARTESIAN_POINT('Ctrl Pts',(59.4103356014117,-13.830000017107,-175.418690311177));
#171973=CARTESIAN_POINT('Ctrl Pts',(59.4272061992403,-13.8300000182966,
-175.350275598526));
#171974=CARTESIAN_POINT('Ctrl Pts',(59.449240943989,-13.8300000198503,-175.260918911488));
#171975=CARTESIAN_POINT('Ctrl Pts',(59.4663032629516,-13.8300000198819,
-175.170862100582));
#171976=CARTESIAN_POINT('Ctrl Pts',(59.4783606526567,-13.8300000199558,
-175.079983307972));
#171977=CARTESIAN_POINT('Ctrl Pts',(59.4903258960553,-13.8300000200293,
-174.989799039243));
#171978=CARTESIAN_POINT('Ctrl Pts',(59.4973624498087,-13.83000002,-174.898805302283));
#171979=CARTESIAN_POINT('Ctrl Pts',(59.4993876311079,-13.83000002,-174.806876041458));
#171980=CARTESIAN_POINT('Ctrl Pts',(59.4997955668077,-13.83000002,-174.788358574718));
#171981=CARTESIAN_POINT('Ctrl Pts',(59.5,-13.83000002,-174.769803126625));
#171982=CARTESIAN_POINT('Ctrl Pts',(59.5,-13.83000002,-174.751208632418));
#171983=CARTESIAN_POINT('Origin',(58.9842656455947,-14.33000002,-179.64995));
#171984=CARTESIAN_POINT('',(58.9842656455947,-13.83000002,-171.871644662643));
#171985=CARTESIAN_POINT('',(58.9842656455947,-13.83000002,-176.75597498356));
#171986=CARTESIAN_POINT('Origin',(58.9842656455946,-14.33000002,-171.871644662643));
#171987=CARTESIAN_POINT('',(58.4843989875811,-14.3184534098307,-179.64995));
#171988=CARTESIAN_POINT('Ctrl Pts',(58.8436897472855,-13.83000002,-171.237717270032));
#171989=CARTESIAN_POINT('Ctrl Pts',(58.3999663918639,-13.83000002,-171.444684327491));
#171990=CARTESIAN_POINT('Ctrl Pts',(58.3906572805143,-14.3195102506022,
-171.449026400902));
#171991=CARTESIAN_POINT('Ctrl Pts',(58.9361841983689,-13.83000002,-171.436019148456));
#171992=CARTESIAN_POINT('Ctrl Pts',(58.4628431558437,-13.8300000200007,
-171.577873523862));
#171993=CARTESIAN_POINT('Ctrl Pts',(58.452336355597,-14.3188132239679,-171.581227559315));
#171994=CARTESIAN_POINT('Ctrl Pts',(58.9842656416468,-13.83000002,-171.650610345097));
#171995=CARTESIAN_POINT('Ctrl Pts',(58.4956819559116,-13.83000002,-171.722618633075));
#171996=CARTESIAN_POINT('Ctrl Pts',(58.484398987579,-14.3184534099214,-171.72428852145));
#171997=CARTESIAN_POINT('Ctrl Pts',(58.9842656455947,-13.83000002,-171.871644662643));
#171998=CARTESIAN_POINT('Ctrl Pts',(58.4956819583251,-13.83000002,-171.871644662643));
#171999=CARTESIAN_POINT('Ctrl Pts',(58.4843989875811,-14.3184534098307,
-171.871644662643));
#172000=CARTESIAN_POINT('',(58.8436897472855,-13.83000002,-171.237717270032));
#172001=CARTESIAN_POINT('Origin',(56.7574781748151,-13.83000002,-172.032172120179));
#172002=CARTESIAN_POINT('Origin',(58.8436897472855,-14.33000002,-171.237717270032));
#172003=CARTESIAN_POINT('Ctrl Pts',(39.923987884714,-13.83000002,-130.68030635931));
#172004=CARTESIAN_POINT('Ctrl Pts',(39.4846775617168,-13.83000002,-130.885279386667));
#172005=CARTESIAN_POINT('Ctrl Pts',(39.4710976496822,-14.3145440753934,
-130.89161549018));
#172006=CARTESIAN_POINT('Ctrl Pts',(46.2315241188232,-13.83000002,-144.198991310165));
#172007=CARTESIAN_POINT('Ctrl Pts',(45.8048635488014,-13.83000002,-144.43668735532));
#172008=CARTESIAN_POINT('Ctrl Pts',(45.7785509549148,-14.3169830983588,
-144.410301102566));
#172009=CARTESIAN_POINT('Ctrl Pts',(52.5377799111353,-13.83000002,-157.718273616974));
#172010=CARTESIAN_POINT('Ctrl Pts',(52.1020957034304,-13.8300000200905,
-157.939875120093));
#172011=CARTESIAN_POINT('Ctrl Pts',(52.0847736772191,-14.3183867301138,
-157.929583215096));
#172012=CARTESIAN_POINT('Ctrl Pts',(58.8436897472855,-13.83000002,-171.237717270032));
#172013=CARTESIAN_POINT('Ctrl Pts',(58.3999663918639,-13.83000002,-171.444684327491));
#172014=CARTESIAN_POINT('Ctrl Pts',(58.3906572805143,-14.3195102506022,
-171.449026400902));
#172015=CARTESIAN_POINT('',(39.923987884714,-13.83000002,-130.68030635931));
#172016=CARTESIAN_POINT('Ctrl Pts',(39.923987884714,-13.83000002,-130.68030635931));
#172017=CARTESIAN_POINT('Ctrl Pts',(46.2315241188232,-13.83000002,-144.198991310165));
#172018=CARTESIAN_POINT('Ctrl Pts',(52.5377799111353,-13.83000002,-157.718273616974));
#172019=CARTESIAN_POINT('Ctrl Pts',(58.8436897472855,-13.83000002,-171.237717270032));
#172020=CARTESIAN_POINT('Origin',(39.923987884714,-14.33000002,-130.68030635931));
#172021=CARTESIAN_POINT('Ctrl Pts',(39.4710976496822,-14.3145440753934,
-130.89161549018));
#172022=CARTESIAN_POINT('Ctrl Pts',(39.4846775617168,-13.83000002,-130.885279386667));
#172023=CARTESIAN_POINT('Ctrl Pts',(39.923987884714,-13.83000002,-130.68030635931));
#172024=CARTESIAN_POINT('Ctrl Pts',(39.1611309974652,-14.3198673792142,
-130.227665983087));
#172025=CARTESIAN_POINT('Ctrl Pts',(39.1694803296317,-13.83000002,-130.222011573448));
#172026=CARTESIAN_POINT('Ctrl Pts',(39.6450175280278,-13.83000002,-130.082400567686));
#172027=CARTESIAN_POINT('Ctrl Pts',(39.,-14.325106270286,-129.50903420183));
#172028=CARTESIAN_POINT('Ctrl Pts',(39.0048700588287,-13.83000002,-129.505450476954));
#172029=CARTESIAN_POINT('Ctrl Pts',(39.5000000016417,-13.83000002,-129.435305216167));
#172030=CARTESIAN_POINT('Ctrl Pts',(39.,-14.33000002,-128.768820397718));
#172031=CARTESIAN_POINT('Ctrl Pts',(38.9999999999999,-13.83000002,-128.768820397718));
#172032=CARTESIAN_POINT('Ctrl Pts',(39.5,-13.83000002,-128.768820397718));
#172033=CARTESIAN_POINT('',(39.5,-13.83000002,-128.768820397718));
#172034=CARTESIAN_POINT('Origin',(46.1927888984987,-13.83000002,-128.288325652416));
#172035=CARTESIAN_POINT('Origin',(39.5,-14.33000002,-128.768820397718));
#172036=CARTESIAN_POINT('Origin',(39.5,-14.33000002,-55.24995));
#172037=CARTESIAN_POINT('',(39.5,-13.83000002,-103.289822573788));
#172038=CARTESIAN_POINT('',(39.5,-13.83000002,-55.24995));
#172039=CARTESIAN_POINT('Origin',(39.5,-14.33000002,-103.289822573788));
#172040=CARTESIAN_POINT('Ctrl Pts',(39.,-14.33000002,-103.289822573788));
#172041=CARTESIAN_POINT('Ctrl Pts',(39.,-13.83000002,-103.289822573788));
#172042=CARTESIAN_POINT('Ctrl Pts',(39.5,-13.83000002,-103.289822573788));
#172043=CARTESIAN_POINT('Ctrl Pts',(39.,-14.3251554673834,-102.557050168938));
#172044=CARTESIAN_POINT('Ctrl Pts',(39.0048213824044,-13.83000002,-102.560555788171));
#172045=CARTESIAN_POINT('Ctrl Pts',(39.5000000055327,-13.83000002,-102.630037977128));
#172046=CARTESIAN_POINT('Ctrl Pts',(39.1579830770898,-14.319921441001,-101.837719843386));
#172047=CARTESIAN_POINT('Ctrl Pts',(39.1662598483009,-13.830000019993,-101.843408229318));
#172048=CARTESIAN_POINT('Ctrl Pts',(39.6421844024665,-13.83000002,-101.982314517002));
#172049=CARTESIAN_POINT('Ctrl Pts',(39.4710976496822,-14.3145440753935,
-101.167027481325));
#172050=CARTESIAN_POINT('Ctrl Pts',(39.4846775617168,-13.83000002,-101.173363584839));
#172051=CARTESIAN_POINT('Ctrl Pts',(39.923987884714,-13.83000002,-101.378336612196));
#172052=CARTESIAN_POINT('',(39.923987884714,-13.83000002,-101.378336612196));
#172053=CARTESIAN_POINT('Origin',(46.1924380477474,-13.83000002,-103.773062785038));
#172054=CARTESIAN_POINT('',(39.4710972477948,-14.3145440616689,-101.167027293814));
#172055=CARTESIAN_POINT('Origin',(39.923987884714,-14.33000002,-101.378336612196));
#172056=CARTESIAN_POINT('Origin',(46.4032459150591,-14.3112053351235,-103.821907513578));
#172057=CARTESIAN_POINT('Ctrl Pts',(58.7311595360587,-13.83000002,-61.0621827299711));
#172058=CARTESIAN_POINT('Ctrl Pts',(58.2874540965012,-13.83000002,-60.8552238163692));
#172059=CARTESIAN_POINT('Ctrl Pts',(58.2781275348581,-14.3194901627709,
-60.8508735991007));
#172060=CARTESIAN_POINT('Ctrl Pts',(52.4627544636864,-13.83000002,-74.5012048985427));
#172061=CARTESIAN_POINT('Ctrl Pts',(52.0270272593534,-13.8300000198715,
-74.2797364934824));
#172062=CARTESIAN_POINT('Ctrl Pts',(52.0097486856907,-14.3183690440453,
-74.2898953083048));
#172063=CARTESIAN_POINT('Ctrl Pts',(46.194004389791,-13.83000002,-87.9400661652057));
#172064=CARTESIAN_POINT('Ctrl Pts',(45.7671827316852,-13.8300000198453,
-87.7027488289555));
#172065=CARTESIAN_POINT('Ctrl Pts',(45.7410317152176,-14.3169685900793,
-87.7287563851229));
#172066=CARTESIAN_POINT('Ctrl Pts',(39.923987884714,-13.83000002,-101.378336612196));
#172067=CARTESIAN_POINT('Ctrl Pts',(39.4846775617168,-13.83000002,-101.173363584839));
#172068=CARTESIAN_POINT('Ctrl Pts',(39.4710976496822,-14.3145440753934,
-101.167027481326));
#172069=CARTESIAN_POINT('',(58.7311595360587,-13.83000002,-61.0621827299711));
#172070=CARTESIAN_POINT('Ctrl Pts',(58.7311595360587,-13.83000002,-61.0621827299711));
#172071=CARTESIAN_POINT('Ctrl Pts',(52.4627544636864,-13.83000002,-74.5012048985427));
#172072=CARTESIAN_POINT('Ctrl Pts',(46.194004389791,-13.83000002,-87.9400661652057));
#172073=CARTESIAN_POINT('Ctrl Pts',(39.923987884714,-13.83000002,-101.378336612196));
#172074=CARTESIAN_POINT('',(58.2781275348581,-14.3194901627709,-60.8508735991007));
#172075=CARTESIAN_POINT('Origin',(58.7311595360587,-14.33000002,-61.0621827299711));
#172076=CARTESIAN_POINT('Ctrl Pts',(39.4710976496823,-14.3145440753934,
-101.167027481325));
#172077=CARTESIAN_POINT('Ctrl Pts',(41.5746782641129,-14.3153575069286,
-96.6584495163958));
#172078=CARTESIAN_POINT('Ctrl Pts',(43.8638536657975,-14.3161254468934,
-91.7517222040427));
#172079=CARTESIAN_POINT('Ctrl Pts',(46.3385980299419,-14.3168265117389,
-86.4468333272163));
#172080=CARTESIAN_POINT('Ctrl Pts',(46.751055423966,-14.3169433558798,-85.5626851810786));
#172081=CARTESIAN_POINT('Ctrl Pts',(47.1686676754888,-14.3170546060321,
-84.6674770644942));
#172082=CARTESIAN_POINT('Ctrl Pts',(47.5914346875375,-14.3171629162029,
-83.7612089442138));
#172083=CARTESIAN_POINT('Ctrl Pts',(47.8028181935619,-14.3172170712883,
-83.3080748840737));
#172084=CARTESIAN_POINT('Ctrl Pts',(48.0154903745181,-14.3172711248367,
-82.8521758187235));
#172085=CARTESIAN_POINT('Ctrl Pts',(48.2294512239489,-14.3173253426588,
-82.3935117469702));
#172086=CARTESIAN_POINT('Ctrl Pts',(48.3364316486644,-14.3173524515698,
-82.1641797110936));
#172087=CARTESIAN_POINT('Ctrl Pts',(48.4437342405363,-14.3173796015504,
-81.9341564236338));
#172088=CARTESIAN_POINT('Ctrl Pts',(48.5513589988902,-14.3174068298701,
-81.703441884523));
#172089=CARTESIAN_POINT('Ctrl Pts',(48.6556204835456,-14.3174332073049,
-81.4799371747593));
#172090=CARTESIAN_POINT('Ctrl Pts',(48.7601843138941,-14.317459658259,-81.2557837415226));
#172091=CARTESIAN_POINT('Ctrl Pts',(48.8650504894187,-14.3174862185691,
-81.0309815848041));
#172092=CARTESIAN_POINT('Ctrl Pts',(48.8684332692744,-14.3174870753533,
-81.0237299023293));
#172093=CARTESIAN_POINT('Ctrl Pts',(48.8724050841776,-14.3174880813788,
-81.0152155015906));
#172094=CARTESIAN_POINT('Ctrl Pts',(48.8751997728309,-14.317488789274,-81.0092245122283));
#172095=CARTESIAN_POINT('Ctrl Pts',(51.1015771319527,-14.3180527310343,
-76.2365271818777));
#172096=CARTESIAN_POINT('Ctrl Pts',(53.4929070387879,-14.3185834838436,
-71.1099546195311));
#172097=CARTESIAN_POINT('Ctrl Pts',(56.0492020811948,-14.3190764132052,
-65.6295126793767));
#172098=CARTESIAN_POINT('Ctrl Pts',(56.7787408124601,-14.3192170898701,
-64.065454308388));
#172099=CARTESIAN_POINT('Ctrl Pts',(57.521715671378,-14.3193548761951,-62.4725744724866));
#172100=CARTESIAN_POINT('Ctrl Pts',(58.2781275348581,-14.3194901627709,
-60.8508735991007));
#172101=CARTESIAN_POINT('Ctrl Pts',(39.,-14.2911437666779,-103.292364908221));
#172102=CARTESIAN_POINT('Ctrl Pts',(39.,-14.2196500163134,-102.183653245897));
#172103=CARTESIAN_POINT('Ctrl Pts',(39.4705101402401,-14.154883972851,-101.179273599517));
#172104=CARTESIAN_POINT('Ctrl Pts',(39.,-15.3821188871317,-103.222014874282));
#172105=CARTESIAN_POINT('Ctrl Pts',(38.9999999999962,-15.2519052464411,
-102.112898232639));
#172106=CARTESIAN_POINT('Ctrl Pts',(39.473885603051,-15.1336440339978,-101.108924169704));
#172107=CARTESIAN_POINT('Ctrl Pts',(39.,-16.4753328054123,-103.064008234267));
#172108=CARTESIAN_POINT('Ctrl Pts',(39.,-16.2866475513133,-101.953874758818));
#172109=CARTESIAN_POINT('Ctrl Pts',(39.4814699289176,-16.1148163368312,
-100.950916925651));
#172110=CARTESIAN_POINT('Ctrl Pts',(39.,-18.6473032869024,-102.580339184276));
#172111=CARTESIAN_POINT('Ctrl Pts',(39.,-18.3422738396393,-101.467519549647));
#172112=CARTESIAN_POINT('Ctrl Pts',(39.5044475737172,-18.0667048767241,
-100.467247875485));
#172113=CARTESIAN_POINT('Ctrl Pts',(39.,-19.6982839688054,-102.261854767811));
#172114=CARTESIAN_POINT('Ctrl Pts',(39.,-19.3376015901503,-101.147059506123));
#172115=CARTESIAN_POINT('Ctrl Pts',(39.5194922305763,-19.012479411179,-100.148762913439));
#172116=CARTESIAN_POINT('Ctrl Pts',(39.,-20.7209336217775,-101.88126637264));
#172117=CARTESIAN_POINT('Ctrl Pts',(39.,-20.3054076594241,-100.764738681203));
#172118=CARTESIAN_POINT('Ctrl Pts',(39.5372194307944,-19.9345274212658,
-99.7681750639369));
#172119=CARTESIAN_POINT('',(39.5365899583801,-19.9017174907778,-99.7816873754343));
#172120=CARTESIAN_POINT('Ctrl Pts',(39.5365899564018,-19.9017175093585,
-99.7816874458032));
#172121=CARTESIAN_POINT('Ctrl Pts',(39.530122557743,-19.5639073116448,-99.9204980182519));
#172122=CARTESIAN_POINT('Ctrl Pts',(39.5240916280606,-19.2268288969008,
-100.049342899962));
#172123=CARTESIAN_POINT('Ctrl Pts',(39.5185098148994,-18.8902357403587,
-100.168182990067));
#172124=CARTESIAN_POINT('Ctrl Pts',(39.5124505611178,-18.5248520742067,
-100.297188072209));
#172125=CARTESIAN_POINT('Ctrl Pts',(39.5069205643145,-18.1600421489813,
-100.414403319327));
#172126=CARTESIAN_POINT('Ctrl Pts',(39.5019314566728,-17.7955093298411,
-100.519838481297));
#172127=CARTESIAN_POINT('Ctrl Pts',(39.4994317811217,-17.6128686972832,
-100.572664300168));
#172128=CARTESIAN_POINT('Ctrl Pts',(39.4970678142959,-17.4302977870856,
-100.622533895174));
#172129=CARTESIAN_POINT('Ctrl Pts',(39.4948406453418,-17.2477595012952,
-100.669453192989));
#172130=CARTESIAN_POINT('Ctrl Pts',(39.4945248369439,-17.2218759133065,
-100.676106261785));
#172131=CARTESIAN_POINT('Ctrl Pts',(39.4942244698344,-17.1970497893428,
-100.682432750568));
#172132=CARTESIAN_POINT('Ctrl Pts',(39.4939047480909,-17.1703984768855,
-100.689162165644));
#172133=CARTESIAN_POINT('Ctrl Pts',(39.4938728326357,-17.1677380736302,
-100.689833913341));
#172134=CARTESIAN_POINT('Ctrl Pts',(39.4938407261658,-17.1650594675226,
-100.690509636197));
#172135=CARTESIAN_POINT('Ctrl Pts',(39.4938083953304,-17.1623597805275,
-100.69119003266));
#172136=CARTESIAN_POINT('Ctrl Pts',(39.4935227058336,-17.1385041575733,
-100.697202315387));
#172137=CARTESIAN_POINT('Ctrl Pts',(39.493239218094,-17.1146379939548,-100.703167010794));
#172138=CARTESIAN_POINT('Ctrl Pts',(39.4929579387798,-17.0907609744762,
-100.70908405176));
#172139=CARTESIAN_POINT('Ctrl Pts',(39.4899905322944,-16.8388660825674,
-100.771506934803));
#172140=CARTESIAN_POINT('Ctrl Pts',(39.4872919536633,-16.5874251012425,
-100.828152222157));
#172141=CARTESIAN_POINT('Ctrl Pts',(39.4848610087856,-16.3362741421625,
-100.879107025452));
#172142=CARTESIAN_POINT('Ctrl Pts',(39.4824374819515,-16.0858895718154,
-100.929906339843));
#172143=CARTESIAN_POINT('Ctrl Pts',(39.4802799507959,-15.8357930472734,
-100.975049887297));
#172144=CARTESIAN_POINT('Ctrl Pts',(39.47838954742,-15.5858173398232,-101.014572640927));
#172145=CARTESIAN_POINT('Ctrl Pts',(39.4765129834559,-15.3376716739312,
-101.053806053315));
#172146=CARTESIAN_POINT('Ctrl Pts',(39.4748996443138,-15.0896448639291,
-101.087500689895));
#172147=CARTESIAN_POINT('Ctrl Pts',(39.4735530184565,-14.8415715919254,
-101.115639683381));
#172148=CARTESIAN_POINT('Ctrl Pts',(39.4725996226103,-14.6659385266556,
-101.135561771883));
#172149=CARTESIAN_POINT('Ctrl Pts',(39.4717799652781,-14.490282131345,-101.152698050753));
#172150=CARTESIAN_POINT('Ctrl Pts',(39.4710960421325,-14.3145440204951,
-101.16702673128));
#172151=CARTESIAN_POINT('Ctrl Pts',(39.5365899564018,-19.9017175093585,
-99.7816874458032));
#172152=CARTESIAN_POINT('Ctrl Pts',(39.5215966413189,-19.9028363193258,
-99.8129429095326));
#172153=CARTESIAN_POINT('Ctrl Pts',(39.5051517179811,-19.9040793375384,
-99.8479870711594));
#172154=CARTESIAN_POINT('Ctrl Pts',(39.487486986643,-19.9054569612971,-99.8869339480742));
#172155=CARTESIAN_POINT('Ctrl Pts',(39.4698222553048,-19.9068345850559,
-99.9258808249889));
#172156=CARTESIAN_POINT('Ctrl Pts',(39.4509374704379,-19.9083470628612,
-99.9687309905404));
#172157=CARTESIAN_POINT('Ctrl Pts',(39.4311216183148,-19.9099998322464,
-100.015606617578));
#172158=CARTESIAN_POINT('Ctrl Pts',(39.4149965614371,-19.9113447655945,
-100.053751439585));
#172159=CARTESIAN_POINT('Ctrl Pts',(39.3983441841591,-19.9127752427056,
-100.094348136095));
#172160=CARTESIAN_POINT('Ctrl Pts',(39.3812363475712,-19.9142986868476,
-100.137720804013));
#172161=CARTESIAN_POINT('Ctrl Pts',(39.3649091779095,-19.9157526129972,
-100.179114284955));
#172162=CARTESIAN_POINT('Ctrl Pts',(39.3481669883162,-19.9172913357008,
-100.22303642595));
#172163=CARTESIAN_POINT('Ctrl Pts',(39.3311188505349,-19.9189170716437,
-100.269774993623));
#172164=CARTESIAN_POINT('Ctrl Pts',(39.3221264132096,-19.9197746039303,
-100.294428339687));
#172165=CARTESIAN_POINT('Ctrl Pts',(39.313049662529,-19.9206562638823,-100.319865377738));
#172166=CARTESIAN_POINT('Ctrl Pts',(39.3039104841802,-19.9215616723638,
-100.346128647387));
#172167=CARTESIAN_POINT('Ctrl Pts',(39.2834462149981,-19.9235890453047,
-100.404936846459));
#172168=CARTESIAN_POINT('Ctrl Pts',(39.2651753202424,-19.9255089595866,
-100.460671945153));
#172169=CARTESIAN_POINT('Ctrl Pts',(39.2487802898612,-19.9273067637394,
-100.513176264637));
#172170=CARTESIAN_POINT('Ctrl Pts',(39.232189706142,-19.9291260113782,-100.566306834558));
#172171=CARTESIAN_POINT('Ctrl Pts',(39.2175195190471,-19.9308204611124,
-100.616129564333));
#172172=CARTESIAN_POINT('Ctrl Pts',(39.2044721454028,-19.9323862009587,
-100.662523063451));
#172173=CARTESIAN_POINT('Ctrl Pts',(39.1912503422537,-19.933972873081,-100.709536794295));
#172174=CARTESIAN_POINT('Ctrl Pts',(39.179694640591,-19.9354276023642,-100.753029464758));
#172175=CARTESIAN_POINT('Ctrl Pts',(39.1695341254265,-19.9367542033861,
-100.792910420823));
#172176=CARTESIAN_POINT('Ctrl Pts',(39.167223353613,-19.9370559077977,-100.801980412617));
#172177=CARTESIAN_POINT('Ctrl Pts',(39.1649849144337,-19.9373510088919,
-100.810863723644));
#172178=CARTESIAN_POINT('Ctrl Pts',(39.1628159253519,-19.9376395889075,
-100.819559501765));
#172179=CARTESIAN_POINT('Ctrl Pts',(39.1577463085425,-19.9383140921173,
-100.839884298835));
#172180=CARTESIAN_POINT('Ctrl Pts',(39.1530558607523,-19.9389529548387,
-100.859184461679));
#172181=CARTESIAN_POINT('Ctrl Pts',(39.1487102691849,-19.9395574210345,
-100.877450576426));
#172182=CARTESIAN_POINT('Ctrl Pts',(39.1465374734011,-19.9398596541323,
-100.886583633799));
#172183=CARTESIAN_POINT('Ctrl Pts',(39.1444509506023,-19.9401532929735,
-100.895458192899));
#172184=CARTESIAN_POINT('Ctrl Pts',(39.1424467411147,-19.9404385093095,
-100.904073269843));
#172185=CARTESIAN_POINT('Ctrl Pts',(39.1414446363709,-19.9405811174774,
-100.908380808314));
#172186=CARTESIAN_POINT('Ctrl Pts',(39.1404631136491,-19.9407216203324,
-100.91262347713));
#172187=CARTESIAN_POINT('Ctrl Pts',(39.1395016999041,-19.9408600401499,
-100.916801159935));
#172188=CARTESIAN_POINT('Ctrl Pts',(39.1390209930316,-19.9409292500586,
-100.918890001337));
#172189=CARTESIAN_POINT('Ctrl Pts',(39.1385453136342,-19.9409979392265,
-100.920962596289));
#172190=CARTESIAN_POINT('Ctrl Pts',(39.1380746038964,-19.9410661104793,
-100.923018930895));
#172191=CARTESIAN_POINT('Ctrl Pts',(39.1376038941586,-19.941134281732,-100.925075265502));
#172192=CARTESIAN_POINT('Ctrl Pts',(39.1374930189679,-19.9411502345416,
-100.925556891227));
#172193=CARTESIAN_POINT('Ctrl Pts',(39.1366773267527,-19.9412690733654,
-100.929139140079));
#172194=CARTESIAN_POINT('Ctrl Pts',(39.1161408417601,-19.9442610495997,
-101.019328550293));
#172195=CARTESIAN_POINT('Ctrl Pts',(39.0984087631728,-19.947194301293,-101.107745690636));
#172196=CARTESIAN_POINT('Ctrl Pts',(39.0831681755561,-19.9500376502056,
-101.194177581913));
#172197=CARTESIAN_POINT('Ctrl Pts',(39.0674129017333,-19.9529770211681,
-101.28352834373));
#172198=CARTESIAN_POINT('Ctrl Pts',(39.054319620319,-19.9558204102339,-101.3707575086));
#172199=CARTESIAN_POINT('Ctrl Pts',(39.043541575639,-19.9585528417086,-101.455682826679));
#172200=CARTESIAN_POINT('Ctrl Pts',(39.0325596286468,-19.9613369661491,
-101.542214787635));
#172201=CARTESIAN_POINT('Ctrl Pts',(39.0239807695704,-19.9640060729754,
-101.62635515219));
#172202=CARTESIAN_POINT('Ctrl Pts',(39.017446398052,-19.9665620140938,-101.707963194666));
#172203=CARTESIAN_POINT('Ctrl Pts',(39.0106980132704,-19.9692016672109,
-101.792244057844));
#172204=CARTESIAN_POINT('Ctrl Pts',(39.0061296681829,-19.9717207963296,
-101.873824248984));
#172205=CARTESIAN_POINT('Ctrl Pts',(39.0033639495716,-19.9741374443006,
-101.952600153975));
#172206=CARTESIAN_POINT('Ctrl Pts',(39.0010525559368,-19.9761571091772,
-102.018435530223));
#172207=CARTESIAN_POINT('Ctrl Pts',(39.000000428941,-19.9781055542109,-102.082313347502));
#172208=CARTESIAN_POINT('Ctrl Pts',(39.000000000131,-19.9800000199999,-102.144196959718));
#172209=CARTESIAN_POINT('Ctrl Pts',(39.6286602916726,-19.8949860872698,
-99.5986214172193));
#172210=CARTESIAN_POINT('Ctrl Pts',(39.5391188861498,-20.48000002,-99.5520413536212));
#172211=CARTESIAN_POINT('Ctrl Pts',(40.0657759443213,-20.48000002,-99.8260192271647));
#172212=CARTESIAN_POINT('Ctrl Pts',(39.4043265400278,-19.9104340007096,
-100.024930299828));
#172213=CARTESIAN_POINT('Ctrl Pts',(39.333589588996,-20.48000002,-99.9880739006574));
#172214=CARTESIAN_POINT('Ctrl Pts',(39.8638772323513,-20.48000002,-100.214892381557));
#172215=CARTESIAN_POINT('Ctrl Pts',(39.2415142628292,-19.9258615536628,
-100.468806409009));
#172216=CARTESIAN_POINT('Ctrl Pts',(39.1854308339039,-20.48000002,-100.444304985299));
#172217=CARTESIAN_POINT('Ctrl Pts',(39.7173505054454,-20.48000002,-100.61942636691));
#172218=CARTESIAN_POINT('Ctrl Pts',(39.0318769517979,-19.9564049059902,
-101.38937941419));
#172219=CARTESIAN_POINT('Ctrl Pts',(39.0089042696538,-20.48000002,-101.379934587793));
#172220=CARTESIAN_POINT('Ctrl Pts',(39.5286840449944,-20.48000002,-101.45767138333));
#172221=CARTESIAN_POINT('Ctrl Pts',(38.985661982892,-19.9716359202423,-101.870016772883));
#172222=CARTESIAN_POINT('Ctrl Pts',(38.9771311417734,-20.48000002,-101.863799189494));
#172223=CARTESIAN_POINT('Ctrl Pts',(39.4870938285405,-20.48000002,-101.894962965541));
#172224=CARTESIAN_POINT('Ctrl Pts',(39.0038798675758,-19.9860848632948,
-102.348581386991));
#172225=CARTESIAN_POINT('Ctrl Pts',(39.0098865266841,-20.48000002,-102.348383053508));
#172226=CARTESIAN_POINT('Ctrl Pts',(39.5034933040112,-20.48000002,-102.330021385346));
#172227=CARTESIAN_POINT('',(39.5,-20.48000002,-102.144196959718));
#172228=CARTESIAN_POINT('Origin',(39.5,-19.98000002,-102.144196959718));
#172229=CARTESIAN_POINT('',(39.9829309662066,-20.48000002,-99.9929964369266));
#172230=CARTESIAN_POINT('Origin',(39.9829309662066,-19.98000002,-99.9929964369266));
#172231=CARTESIAN_POINT('Ctrl Pts',(39.5,-20.48000002,-102.144196959718));
#172232=CARTESIAN_POINT('Ctrl Pts',(39.5,-20.48000002,-101.901224059727));
#172233=CARTESIAN_POINT('Ctrl Pts',(39.5178405979396,-20.48000002,-101.658367298417));
#172234=CARTESIAN_POINT('Ctrl Pts',(39.5526223904373,-20.48000002,-101.419269624472));
#172235=CARTESIAN_POINT('Ctrl Pts',(39.5712680114436,-20.48000002,-101.291095534188));
#172236=CARTESIAN_POINT('Ctrl Pts',(39.5947811831661,-20.48000002,-101.164001820978));
#172237=CARTESIAN_POINT('Ctrl Pts',(39.6230172792885,-20.48000002,-101.038548856259));
#172238=CARTESIAN_POINT('Ctrl Pts',(39.6919421332749,-20.48000002,-100.732315755268));
#172239=CARTESIAN_POINT('Ctrl Pts',(39.7887207445095,-20.48000002,-100.433895586519));
#172240=CARTESIAN_POINT('Ctrl Pts',(39.9146180003271,-20.48000002,-100.143643141342));
#172241=CARTESIAN_POINT('Ctrl Pts',(39.93650642588,-20.48000002,-100.093180015704));
#172242=CARTESIAN_POINT('Ctrl Pts',(39.9592751462315,-20.48000002,-100.042963811213));
#172243=CARTESIAN_POINT('Ctrl Pts',(39.9829309662065,-20.48000002,-99.9929964369266));
#172244=CARTESIAN_POINT('Origin',(39.5,-19.98000002,-55.24995));
#172245=CARTESIAN_POINT('',(39.5,-20.48000002,-129.914446011788));
#172246=CARTESIAN_POINT('Origin',(39.5,-19.98000002,-129.914446011788));
#172247=CARTESIAN_POINT('',(39.5,-20.48000002,-55.24995));
#172248=CARTESIAN_POINT('Ctrl Pts',(39.,-19.98000002,-129.914446011788));
#172249=CARTESIAN_POINT('Ctrl Pts',(39.,-20.48000002,-129.914446011788));
#172250=CARTESIAN_POINT('Ctrl Pts',(39.5,-20.48000002,-129.914446011788));
#172251=CARTESIAN_POINT('Ctrl Pts',(39.,-19.9674346440713,-130.324899900514));
#172252=CARTESIAN_POINT('Ctrl Pts',(38.9872746975485,-20.48000002,-130.330124066848));
#172253=CARTESIAN_POINT('Ctrl Pts',(39.5000000028435,-20.48000002,-130.287671434236));
#172254=CARTESIAN_POINT('Ctrl Pts',(39.0456887600695,-19.9546004036482,
-130.727459443406));
#172255=CARTESIAN_POINT('Ctrl Pts',(39.0203709824336,-20.48000002,-130.73585622864));
#172256=CARTESIAN_POINT('Ctrl Pts',(39.5411198836701,-20.48000002,-130.653963774132));
#172257=CARTESIAN_POINT('Ctrl Pts',(39.2244077003248,-19.9284125341257,
-131.517220896748));
#172258=CARTESIAN_POINT('Ctrl Pts',(39.1707024462744,-20.48000002,-131.538360679722));
#172259=CARTESIAN_POINT('Ctrl Pts',(39.7019669306849,-20.48000002,-131.373086703203));
#172260=CARTESIAN_POINT('Ctrl Pts',(39.3590527322559,-19.9149653023259,
-131.906857743156));
#172261=CARTESIAN_POINT('Ctrl Pts',(39.2920635693995,-20.48000002,-131.938092167695));
#172262=CARTESIAN_POINT('Ctrl Pts',(39.8231470367065,-20.48000002,-131.72814043837));
#172263=CARTESIAN_POINT('Ctrl Pts',(39.5365899624517,-19.9017174575869,
-132.27695566545));
#172264=CARTESIAN_POINT('Ctrl Pts',(39.4537365768201,-20.48000002,-132.316180555747));
#172265=CARTESIAN_POINT('Ctrl Pts',(39.9829309662066,-20.48000002,-132.065646534579));
#172266=CARTESIAN_POINT('',(39.9829309662066,-20.48000002,-132.065646534579));
#172267=CARTESIAN_POINT('Origin',(39.9829309662066,-19.98000002,-132.065646534579));
#172268=CARTESIAN_POINT('Ctrl Pts',(39.9829309662066,-20.48000002,-132.065646534579));
#172269=CARTESIAN_POINT('Ctrl Pts',(39.8887941972372,-20.48000002,-131.866804677728));
#172270=CARTESIAN_POINT('Ctrl Pts',(39.8080127216862,-20.48000002,-131.661768384112));
#172271=CARTESIAN_POINT('Ctrl Pts',(39.7410867352565,-20.48000002,-131.453290684188));
#172272=CARTESIAN_POINT('Ctrl Pts',(39.6944643395902,-20.48000002,-131.308059656123));
#172273=CARTESIAN_POINT('Ctrl Pts',(39.6545649019177,-20.48000002,-131.161159371038));
#172274=CARTESIAN_POINT('Ctrl Pts',(39.6215434069806,-20.48000002,-131.013525238711));
#172275=CARTESIAN_POINT('Ctrl Pts',(39.5522800663376,-20.48000002,-130.70385927061));
#172276=CARTESIAN_POINT('Ctrl Pts',(39.5121705688344,-20.48000002,-130.389227115448));
#172277=CARTESIAN_POINT('Ctrl Pts',(39.5023709529579,-20.48000002,-130.069431842247));
#172278=CARTESIAN_POINT('Ctrl Pts',(39.5007919718951,-20.48000002,-130.017904242929));
#172279=CARTESIAN_POINT('Ctrl Pts',(39.5,-20.48000002,-129.966242581154));
#172280=CARTESIAN_POINT('Ctrl Pts',(39.5,-20.48000002,-129.914446011788));
#172281=CARTESIAN_POINT('Ctrl Pts',(58.4402350532158,-20.48000002,-171.237717270032));
#172282=CARTESIAN_POINT('Ctrl Pts',(57.9358462259716,-20.48000002,-171.474604875281));
#172283=CARTESIAN_POINT('Ctrl Pts',(57.9903087491627,-19.9260113903464,
-171.449026400902));
#172284=CARTESIAN_POINT('Ctrl Pts',(52.3041884424236,-20.48000002,-158.172646387016));
#172285=CARTESIAN_POINT('Ctrl Pts',(51.7549262849061,-20.4800000195716,
-158.328906441528));
#172286=CARTESIAN_POINT('Ctrl Pts',(51.8549375290089,-19.9204232153646,
-158.383965825354));
#172287=CARTESIAN_POINT('Ctrl Pts',(46.1592765266851,-20.48000002,-145.111728668187));
#172288=CARTESIAN_POINT('Ctrl Pts',(45.5582765746384,-20.4800000200247,
-145.178124710387));
#172289=CARTESIAN_POINT('Ctrl Pts',(45.7108852546953,-19.9134492574988,
-145.323053305542));
#172290=CARTESIAN_POINT('Ctrl Pts',(39.9829309662066,-20.48000002,-132.065646534579));
#172291=CARTESIAN_POINT('Ctrl Pts',(39.4537365768201,-20.48000002,-132.316180555747));
#172292=CARTESIAN_POINT('Ctrl Pts',(39.5365899624517,-19.9017174575869,
-132.27695566545));
#172293=CARTESIAN_POINT('',(58.4402350532158,-20.48000002,-171.237717270032));
#172294=CARTESIAN_POINT('Origin',(58.4402350532158,-19.98000002,-171.237717270032));
#172295=CARTESIAN_POINT('Ctrl Pts',(58.4402350532158,-20.48000002,-171.237717270032));
#172296=CARTESIAN_POINT('Ctrl Pts',(52.3041884424236,-20.48000002,-158.172646387016));
#172297=CARTESIAN_POINT('Ctrl Pts',(46.1592765266851,-20.48000002,-145.111728668187));
#172298=CARTESIAN_POINT('Ctrl Pts',(39.9829309662066,-20.48000002,-132.065646534579));
#172299=CARTESIAN_POINT('Ctrl Pts',(58.5817791104913,-20.48000002,-171.871644662643));
#172300=CARTESIAN_POINT('Ctrl Pts',(58.0183573349639,-20.48000002,-171.871644662643));
#172301=CARTESIAN_POINT('Ctrl Pts',(58.0853233553177,-19.9205720538986,
-171.871644662643));
#172302=CARTESIAN_POINT('Ctrl Pts',(58.5817790937258,-20.48000002,-171.652759539508));
#172303=CARTESIAN_POINT('Ctrl Pts',(58.018357325283,-20.48000002,-171.735617762033));
#172304=CARTESIAN_POINT('Ctrl Pts',(58.0853233550829,-19.9205720558596,
-171.725723025901));
#172305=CARTESIAN_POINT('Ctrl Pts',(58.5342346140381,-20.48000002,-171.437864213701));
#172306=CARTESIAN_POINT('Ctrl Pts',(57.9913238325147,-20.4800000200031,
-171.602371122267));
#172307=CARTESIAN_POINT('Ctrl Pts',(58.0534084851269,-19.9223906228206,
-171.582455328445));
#172308=CARTESIAN_POINT('Ctrl Pts',(58.4402350532158,-20.48000002,-171.237717270032));
#172309=CARTESIAN_POINT('Ctrl Pts',(57.9358462259716,-20.48000002,-171.474604875281));
#172310=CARTESIAN_POINT('Ctrl Pts',(57.9903087491627,-19.9260113903464,
-171.449026400902));
#172311=CARTESIAN_POINT('',(58.5817791104913,-20.48000002,-171.871644662643));
#172312=CARTESIAN_POINT('Origin',(58.5817791104913,-19.98000002,-171.871644662643));
#172313=CARTESIAN_POINT('Origin',(56.4084014798071,-20.48000002,-172.018072886377));
#172314=CARTESIAN_POINT('Origin',(58.5817791104913,-19.98000002,-179.64995));
#172315=CARTESIAN_POINT('',(58.0853233553177,-19.9205720538986,-179.64995));
#172316=CARTESIAN_POINT('',(58.5817791104913,-20.48000002,-171.871644662643));
#172317=CARTESIAN_POINT('Ctrl Pts',(60.,-20.98000002,-174.500886972636));
#172318=CARTESIAN_POINT('Ctrl Pts',(60.,-20.48000002,-174.500886972636));
#172319=CARTESIAN_POINT('Ctrl Pts',(59.5,-20.48000002,-174.500886972636));
#172320=CARTESIAN_POINT('Ctrl Pts',(60.,-20.9822194010082,-174.791464522024));
#172321=CARTESIAN_POINT('Ctrl Pts',(60.0022242907223,-20.48000002,-174.792108323791));
#172322=CARTESIAN_POINT('Ctrl Pts',(59.4999999934397,-20.48000002,-174.74311983516));
#172323=CARTESIAN_POINT('Ctrl Pts',(59.9586932949262,-20.9843889926879,
-175.075119998302));
#172324=CARTESIAN_POINT('Ctrl Pts',(59.9629392387446,-20.4800000199999,
-175.076359449429));
#172325=CARTESIAN_POINT('Ctrl Pts',(59.4655777479701,-20.48000002,-174.979582459221));
#172326=CARTESIAN_POINT('Ctrl Pts',(59.8360926556437,-20.9875676565265,
-175.49019987132));
#172327=CARTESIAN_POINT('Ctrl Pts',(59.8433264812564,-20.48000002,-175.492827860986));
#172328=CARTESIAN_POINT('Ctrl Pts',(59.3634105452706,-20.48000002,-175.325604118318));
#172329=CARTESIAN_POINT('Ctrl Pts',(59.7847122422101,-20.9886147234176,
-175.626841448369));
#172330=CARTESIAN_POINT('Ctrl Pts',(59.7928073162253,-20.4800000200006,
-175.630213503224));
#172331=CARTESIAN_POINT('Ctrl Pts',(59.3205935345334,-20.48000002,-175.43951222267));
#172332=CARTESIAN_POINT('Ctrl Pts',(59.6645318784846,-20.9906156905346,
-175.887821675912));
#172333=CARTESIAN_POINT('Ctrl Pts',(59.674123349008,-20.4800000199994,-175.892915048025));
#172334=CARTESIAN_POINT('Ctrl Pts',(59.2204432327122,-20.48000002,-175.657072445029));
#172335=CARTESIAN_POINT('Ctrl Pts',(59.5954458739788,-20.9915785299556,
-176.013328010605));
#172336=CARTESIAN_POINT('Ctrl Pts',(59.605650654114,-20.4800000200002,-176.019368430779));
#172337=CARTESIAN_POINT('Ctrl Pts',(59.162871562207,-20.48000002,-175.761697975082));
#172338=CARTESIAN_POINT('Ctrl Pts',(59.4392988603324,-20.9934287142977,
-176.254382360717));
#172339=CARTESIAN_POINT('Ctrl Pts',(59.4504692034509,-20.4800000199998,
-176.262509186853));
#172340=CARTESIAN_POINT('Ctrl Pts',(59.032749049719,-20.48000002,-175.962647558431));
#172341=CARTESIAN_POINT('Ctrl Pts',(59.3514188912717,-20.9943227517297,
-176.370801152158));
#172342=CARTESIAN_POINT('Ctrl Pts',(59.3629214966957,-20.48000002,-176.380037040048));
#172343=CARTESIAN_POINT('Ctrl Pts',(58.9595157418279,-20.48000002,-176.059697515632));
#172344=CARTESIAN_POINT('Ctrl Pts',(59.1611693306144,-20.9959919273243,
-176.588063887092));
#172345=CARTESIAN_POINT('Ctrl Pts',(59.1730156260874,-20.48000002,-176.599598651605));
#172346=CARTESIAN_POINT('Ctrl Pts',(58.800974443077,-20.48000002,-176.240813845549));
#172347=CARTESIAN_POINT('Ctrl Pts',(59.0590996873029,-20.9967669365736,
-176.688892319953));
#172348=CARTESIAN_POINT('Ctrl Pts',(59.0709534896778,-20.4800000200012,
-176.701568343258));
#172349=CARTESIAN_POINT('Ctrl Pts',(58.7159164062094,-20.48000002,-176.324867284949));
#172350=CARTESIAN_POINT('Ctrl Pts',(58.7325172788836,-20.9989167502369,
-176.968486930424));
#172351=CARTESIAN_POINT('Ctrl Pts',(58.7436561080181,-20.4800000199975,
-176.984811315106));
#172352=CARTESIAN_POINT('Ctrl Pts',(58.4437643988224,-20.48000002,-176.557945321316));
#172353=CARTESIAN_POINT('Ctrl Pts',(58.484009011739,-21.0001266369645,-177.125700665905));
#172354=CARTESIAN_POINT('Ctrl Pts',(58.4942266187642,-20.4800000200099,
-177.144085084891));
#172355=CARTESIAN_POINT('Ctrl Pts',(58.2366741051621,-20.48000002,-176.68900326854));
#172356=CARTESIAN_POINT('Ctrl Pts',(58.2221195094937,-21.0010265837306,
-177.24260269584));
#172357=CARTESIAN_POINT('Ctrl Pts',(58.2310611931749,-20.4800000199999,
-177.262627176116));
#172358=CARTESIAN_POINT('Ctrl Pts',(58.0184329245781,-20.48000002,-176.786456163744));
#172359=CARTESIAN_POINT('',(59.5,-20.48000002,-174.500886972636));
#172360=CARTESIAN_POINT('Ctrl Pts',(59.5,-20.48000002,-174.500886972636));
#172361=CARTESIAN_POINT('Ctrl Pts',(59.5,-20.48000002,-174.594133457896));
#172362=CARTESIAN_POINT('Ctrl Pts',(59.4948998873889,-20.48000002,-174.686506499847));
#172363=CARTESIAN_POINT('Ctrl Pts',(59.484743418878,-20.48000002,-174.778024581704));
#172364=CARTESIAN_POINT('Ctrl Pts',(59.4745869503671,-20.48000002,-174.869542663562));
#172365=CARTESIAN_POINT('Ctrl Pts',(59.4593733052792,-20.4800000198432,
-174.96020535248));
#172366=CARTESIAN_POINT('Ctrl Pts',(59.4391579117629,-20.4800000201565,
-175.050010672616));
#172367=CARTESIAN_POINT('Ctrl Pts',(59.4270641008619,-20.4800000203439,
-175.103736490952));
#172368=CARTESIAN_POINT('Ctrl Pts',(59.4131703468088,-20.4800000205099,
-175.157156500734));
#172369=CARTESIAN_POINT('Ctrl Pts',(59.3974877716946,-20.4800000205022,
-175.210269911122));
#172370=CARTESIAN_POINT('Ctrl Pts',(59.3634319732391,-20.4800000204854,
-175.325609361837));
#172371=CARTESIAN_POINT('Ctrl Pts',(59.3206017517199,-20.4800000200584,
-175.43951508737));
#172372=CARTESIAN_POINT('Ctrl Pts',(59.2705225473981,-20.480000020021,-175.548294250575));
#172373=CARTESIAN_POINT('Ctrl Pts',(59.2665668880551,-20.4800000200181,
-175.556886505965));
#172374=CARTESIAN_POINT('Ctrl Pts',(59.2625645131408,-20.4800000200159,
-175.56545285612));
#172375=CARTESIAN_POINT('Ctrl Pts',(59.2585154363462,-20.4800000200145,
-175.573993307709));
#172376=CARTESIAN_POINT('Ctrl Pts',(59.2235121463779,-20.4800000200017,
-175.647823446922));
#172377=CARTESIAN_POINT('Ctrl Pts',(59.1850753506039,-20.4800000200467,
-175.719619366777));
#172378=CARTESIAN_POINT('Ctrl Pts',(59.1431476193817,-20.4800000203096,
-175.789501989863));
#172379=CARTESIAN_POINT('Ctrl Pts',(59.1284714749913,-20.4800000204017,
-175.813963305486));
#172380=CARTESIAN_POINT('Ctrl Pts',(59.1133672159704,-20.4800000205138,
-175.838189938606));
#172381=CARTESIAN_POINT('Ctrl Pts',(59.0978311232235,-20.4800000206151,
-175.862186246726));
#172382=CARTESIAN_POINT('Ctrl Pts',(59.057684395778,-20.4800000208766,-175.924194967805));
#172383=CARTESIAN_POINT('Ctrl Pts',(59.0143956166168,-20.4800000209379,
-175.984944386851));
#172384=CARTESIAN_POINT('Ctrl Pts',(58.9683824813746,-20.4800000205207,
-176.043771514579));
#172385=CARTESIAN_POINT('Ctrl Pts',(58.939956521226,-20.4800000202629,-176.080113693386));
#172386=CARTESIAN_POINT('Ctrl Pts',(58.9105390187326,-20.480000020158,-176.115667750748));
#172387=CARTESIAN_POINT('Ctrl Pts',(58.8802525752657,-20.4800000200989,
-176.150262230718));
#172388=CARTESIAN_POINT('Ctrl Pts',(58.8008883718402,-20.4800000199439,
-176.240915441575));
#172389=CARTESIAN_POINT('Ctrl Pts',(58.7158063838685,-20.4800000199516,
-176.324965650418));
#172390=CARTESIAN_POINT('Ctrl Pts',(58.6252060810682,-20.4800000201162,
-176.402568149682));
#172391=CARTESIAN_POINT('Ctrl Pts',(58.6108845926547,-20.4800000201422,
-176.414835032459));
#172392=CARTESIAN_POINT('Ctrl Pts',(58.5964064444941,-20.4800000201761,
-176.426947791328));
#172393=CARTESIAN_POINT('Ctrl Pts',(58.5817791104913,-20.4800000202216,
-176.438901946458));
#172394=CARTESIAN_POINT('Origin',(59.5,-20.98000002,-174.500886972636));
#172395=CARTESIAN_POINT('Ctrl Pts',(39.9829309662066,-20.48000002,-99.9929964369266));
#172396=CARTESIAN_POINT('Ctrl Pts',(39.4537365768202,-20.48000002,-99.742462415759));
#172397=CARTESIAN_POINT('Ctrl Pts',(39.5365899624517,-19.9017174575869,
-99.7816873060563));
#172398=CARTESIAN_POINT('Ctrl Pts',(46.1212593572987,-20.48000002,-87.0272166609364));
#172399=CARTESIAN_POINT('Ctrl Pts',(45.5211976544485,-20.48000002,-86.9586415917399));
#172400=CARTESIAN_POINT('Ctrl Pts',(45.6728806075319,-19.9133770447829,
-86.815892326284));
#172401=CARTESIAN_POINT('Ctrl Pts',(52.2285110086243,-20.48000002,-74.0467697366574));
#172402=CARTESIAN_POINT('Ctrl Pts',(51.6794916123544,-20.4800000199249,
-73.8897477208158));
#172403=CARTESIAN_POINT('Ctrl Pts',(51.7792721521254,-19.9203329608279,
-73.8354504790526));
#172404=CARTESIAN_POINT('Ctrl Pts',(58.3269264615434,-20.48000002,-61.0621827299711));
#172405=CARTESIAN_POINT('Ctrl Pts',(57.8224346115608,-20.48000002,-60.8252402001721));
#172406=CARTESIAN_POINT('Ctrl Pts',(57.8770125754992,-19.9259080025173,
-60.8508735991007));
#172407=CARTESIAN_POINT('',(57.8770125754992,-19.9259080025173,-60.8508735991007));
#172408=CARTESIAN_POINT('Ctrl Pts',(57.8770125754992,-19.9259080025173,
-60.8508735991007));
#172409=CARTESIAN_POINT('Ctrl Pts',(56.2239580313905,-19.9243966479237,
-64.3709010723032));
#172410=CARTESIAN_POINT('Ctrl Pts',(54.6344108974312,-19.9229079589042,
-67.7535839786999));
#172411=CARTESIAN_POINT('Ctrl Pts',(52.3453693536531,-19.9204384147188,
-72.6215914880863));
#172412=CARTESIAN_POINT('Ctrl Pts',(51.5982350930194,-19.9195813611909,
-74.2099245161803));
#172413=CARTESIAN_POINT('Ctrl Pts',(50.5013522959551,-19.9182610265938,
-76.5409198457692));
#172414=CARTESIAN_POINT('Ctrl Pts',(49.9588655093536,-19.9175926897662,
-77.6935414574256));
#172415=CARTESIAN_POINT('Ctrl Pts',(49.336384233353,-19.9168076573922,-79.0157335780332));
#172416=CARTESIAN_POINT('Ctrl Pts',(48.9864133340098,-19.9163628051879,
-79.7589815597841));
#172417=CARTESIAN_POINT('Ctrl Pts',(48.8137672692214,-19.9161425058677,
-80.1255999074955));
#172418=CARTESIAN_POINT('Ctrl Pts',(48.7263143503862,-19.9160307783446,
-80.3112990142576));
#172419=CARTESIAN_POINT('Ctrl Pts',(48.7241371808068,-19.9160279967759,
-80.3159220498041));
#172420=CARTESIAN_POINT('Ctrl Pts',(45.3540283295419,-19.9117221121947,
-87.4720485631386));
#172421=CARTESIAN_POINT('Ctrl Pts',(42.2926058529678,-19.9069541729552,
-93.9583097862753));
#172422=CARTESIAN_POINT('Ctrl Pts',(39.5365899624517,-19.9017174575869,
-99.7816873060563));
#172423=CARTESIAN_POINT('',(58.3269264615434,-20.48000002,-61.0621827299711));
#172424=CARTESIAN_POINT('Origin',(58.3269264615434,-19.98000002,-61.0621827299711));
#172425=CARTESIAN_POINT('Ctrl Pts',(39.9829309662066,-20.48000002,-99.9929964369266));
#172426=CARTESIAN_POINT('Ctrl Pts',(46.1212593572987,-20.48000002,-87.0272166609364));
#172427=CARTESIAN_POINT('Ctrl Pts',(52.2285110086243,-20.48000002,-74.0467697366574));
#172428=CARTESIAN_POINT('Ctrl Pts',(58.3269264615434,-20.48000002,-61.0621827299711));
#172429=CARTESIAN_POINT('Origin',(59.5,-20.98000002,-55.24995));
#172430=CARTESIAN_POINT('',(59.5,-20.48000002,-58.1336824582564));
#172431=CARTESIAN_POINT('',(59.5,-20.48000002,-174.524030413304));
#172432=CARTESIAN_POINT('',(60.,-20.98000002,-58.1336824582564));
#172433=CARTESIAN_POINT('Origin',(59.5,-20.98000002,-58.1336824582564));
#172434=CARTESIAN_POINT('',(60.,-20.98000002,-58.1134713856835));
#172435=CARTESIAN_POINT('Origin',(60.,-2.55003103885676E-14,0.));
#172436=CARTESIAN_POINT('',(60.,-21.48000002,-58.1532962439713));
#172437=CARTESIAN_POINT('Ctrl Pts',(60.,-20.98000002,-58.1336824582564));
#172438=CARTESIAN_POINT('Ctrl Pts',(60.,-21.1466635001965,-58.1403364979909));
#172439=CARTESIAN_POINT('Ctrl Pts',(60.,-21.3133297017902,-58.1468913732678));
#172440=CARTESIAN_POINT('Ctrl Pts',(60.,-21.48000002,-58.1532962439713));
#172441=CARTESIAN_POINT('',(60.,-21.48000002,-174.45635375974));
#172442=CARTESIAN_POINT('Origin',(59.5,-21.48000002,-55.24995));
#172443=CARTESIAN_POINT('',(59.5,-21.98000002,-58.1532962439713));
#172444=CARTESIAN_POINT('Origin',(59.5,-21.48000002,-58.1532962439713));
#172445=CARTESIAN_POINT('',(59.5,-21.98000002,-174.47822483969));
#172446=CARTESIAN_POINT('',(59.5,-21.98000002,-58.1720074546108));
#172447=CARTESIAN_POINT('Origin',(59.5,-21.48000002,-174.47822483969));
#172448=CARTESIAN_POINT('Ctrl Pts',(59.5,-21.98000002,-174.47822483969));
#172449=CARTESIAN_POINT('Ctrl Pts',(60.,-21.98000002,-174.47822483969));
#172450=CARTESIAN_POINT('Ctrl Pts',(60.,-21.48000002,-174.47822483969));
#172451=CARTESIAN_POINT('Ctrl Pts',(59.4999999932692,-21.98000002,-174.72672222605));
#172452=CARTESIAN_POINT('Ctrl Pts',(59.9977907999382,-21.9800000199965,
-174.775666642734));
#172453=CARTESIAN_POINT('Ctrl Pts',(60.,-21.4822140856788,-174.77632287275));
#172454=CARTESIAN_POINT('Ctrl Pts',(59.4638082272143,-21.98000002,-174.969157756816));
#172455=CARTESIAN_POINT('Ctrl Pts',(59.9524075929633,-21.98000002,-175.065899995449));
#172456=CARTESIAN_POINT('Ctrl Pts',(59.9565698697824,-21.4843793273514,
-175.067148740399));
#172457=CARTESIAN_POINT('Ctrl Pts',(59.3562425753485,-21.98000002,-175.323664095203));
#172458=CARTESIAN_POINT('Ctrl Pts',(59.8205081565721,-21.98000002,-175.489804158754));
#172459=CARTESIAN_POINT('Ctrl Pts',(59.8274910918555,-21.4875521339025,
-175.492414399022));
#172460=CARTESIAN_POINT('Ctrl Pts',(59.3112699374162,-21.98000002,-175.439952697294));
#172461=CARTESIAN_POINT('Ctrl Pts',(59.7657533403762,-21.9800000200007,
-175.628582862653));
#172462=CARTESIAN_POINT('Ctrl Pts',(59.7735239255666,-21.4885940652802,
-175.631914079949));
#172463=CARTESIAN_POINT('Ctrl Pts',(59.2061209187896,-21.98000002,-175.661808757878));
#172464=CARTESIAN_POINT('Ctrl Pts',(59.6382394618755,-21.9800000199994,
-175.893067776338));
#172465=CARTESIAN_POINT('Ctrl Pts',(59.6473451018805,-21.4905837846614,
-175.89805223939));
#172466=CARTESIAN_POINT('Ctrl Pts',(59.1456765053938,-21.98000002,-175.768375282423));
#172467=CARTESIAN_POINT('Ctrl Pts',(59.5651790529315,-21.9800000199994,
-176.020005430174));
#172468=CARTESIAN_POINT('Ctrl Pts',(59.5748118056443,-21.4915405113197,
-176.025889197601));
#172469=CARTESIAN_POINT('Ctrl Pts',(59.0089721749525,-21.98000002,-175.972743369523));
#172470=CARTESIAN_POINT('Ctrl Pts',(59.4003458450454,-21.9800000200006,
-176.263201660659));
#172471=CARTESIAN_POINT('Ctrl Pts',(59.4107666107714,-21.493376849955,-176.271048580335));
#172472=CARTESIAN_POINT('Ctrl Pts',(58.9319928876421,-21.98000002,-176.071220734744));
#172473=CARTESIAN_POINT('Ctrl Pts',(59.3077278616495,-21.9800000199987,
-176.380304393309));
#172474=CARTESIAN_POINT('Ctrl Pts',(59.3183914660909,-21.4942625520954,
-176.389181693558));
#172475=CARTESIAN_POINT('Ctrl Pts',(58.7662605376602,-21.98000002,-176.253552125047));
#172476=CARTESIAN_POINT('Ctrl Pts',(59.1086757415209,-21.9800000200013,
-176.59692321781));
#172477=CARTESIAN_POINT('Ctrl Pts',(59.1195126442718,-21.495903657329,-176.607905725284));
#172478=CARTESIAN_POINT('Ctrl Pts',(58.6773437522104,-21.98000002,-176.337917446619));
#172479=CARTESIAN_POINT('Ctrl Pts',(59.0020443621077,-21.9800000199996,
-176.697095400112));
#172480=CARTESIAN_POINT('Ctrl Pts',(59.012812502338,-21.4966636432885,-176.7091099968));
#172481=CARTESIAN_POINT('Ctrl Pts',(58.3926916168304,-21.98000002,-176.570893328242));
#172482=CARTESIAN_POINT('Ctrl Pts',(58.6613611188049,-21.9800000200008,
-176.973308002926));
#172483=CARTESIAN_POINT('Ctrl Pts',(58.6712299408253,-21.4987636190772,
-176.988586760981));
#172484=CARTESIAN_POINT('Ctrl Pts',(58.1758692424685,-21.98000002,-176.700106570217));
#172485=CARTESIAN_POINT('Ctrl Pts',(58.4021689190212,-21.9800000199881,
-177.126531916838));
#172486=CARTESIAN_POINT('Ctrl Pts',(58.4110432062101,-21.4999301516852,
-177.143590179504));
#172487=CARTESIAN_POINT('Ctrl Pts',(57.9501667771809,-21.98000002,-176.792941619423));
#172488=CARTESIAN_POINT('Ctrl Pts',(58.132621442372,-21.98000002,-177.23652912386));
#172489=CARTESIAN_POINT('Ctrl Pts',(58.140200132617,-21.5007687140674,-177.254954590203));
#172490=CARTESIAN_POINT('Ctrl Pts',(58.2281061322556,-21.9799999688995,
-176.657965001835));
#172491=CARTESIAN_POINT('Ctrl Pts',(58.2763381470521,-21.9799999587489,
-176.630735497029));
#172492=CARTESIAN_POINT('Ctrl Pts',(58.3235842378115,-21.9799999676447,
-176.601941540627));
#172493=CARTESIAN_POINT('Ctrl Pts',(58.3697659029187,-21.9799999836463,
-176.571657891927));
#172494=CARTESIAN_POINT('Ctrl Pts',(58.4333419149384,-21.9800000056749,
-176.529967892025));
#172495=CARTESIAN_POINT('Ctrl Pts',(58.4951281469266,-21.9800000132519,
-176.485368653426));
#172496=CARTESIAN_POINT('Ctrl Pts',(58.5544579572714,-21.9800000168151,
-176.438221543427));
#172497=CARTESIAN_POINT('Ctrl Pts',(58.5638633718754,-21.98000001738,-176.430747423514));
#172498=CARTESIAN_POINT('Ctrl Pts',(58.573207108192,-21.9800000178323,-176.423209364714));
#172499=CARTESIAN_POINT('Ctrl Pts',(58.582486579001,-21.9800000181999,-176.415608906189));
#172500=CARTESIAN_POINT('Ctrl Pts',(58.6422321318881,-21.9800000205672,
-176.366673616007));
#172501=CARTESIAN_POINT('Ctrl Pts',(58.6996264562076,-21.9800000199999,
-176.315076489292));
#172502=CARTESIAN_POINT('Ctrl Pts',(58.7545482746591,-21.9800000199988,
-176.260908374673));
#172503=CARTESIAN_POINT('Ctrl Pts',(58.7869024533102,-21.9800000199981,
-176.228998199318));
#172504=CARTESIAN_POINT('Ctrl Pts',(58.8184303801206,-21.9800000199976,
-176.196159475715));
#172505=CARTESIAN_POINT('Ctrl Pts',(58.8491278703888,-21.9800000199976,
-176.162387482235));
#172506=CARTESIAN_POINT('Ctrl Pts',(58.9319941632242,-21.9800000199974,
-176.071221726439));
#172507=CARTESIAN_POINT('Ctrl Pts',(59.0089727564858,-21.9800000199996,
-175.972743969313));
#172508=CARTESIAN_POINT('Ctrl Pts',(59.0773246245197,-21.9800000199999,
-175.870559516175));
#172509=CARTESIAN_POINT('Ctrl Pts',(59.1060118933486,-21.98000002,-175.82767271642));
#172510=CARTESIAN_POINT('Ctrl Pts',(59.1333062996812,-21.98000002,-175.784013939838));
#172511=CARTESIAN_POINT('Ctrl Pts',(59.1592107352546,-21.98000002,-175.739584721266));
#172512=CARTESIAN_POINT('Ctrl Pts',(59.1950270177852,-21.98000002,-175.678155494582));
#172513=CARTESIAN_POINT('Ctrl Pts',(59.2281939400895,-21.9800000200315,
-175.615256612429));
#172514=CARTESIAN_POINT('Ctrl Pts',(59.2587125449347,-21.9800000196412,
-175.550888840134));
#172515=CARTESIAN_POINT('Ctrl Pts',(59.311304650302,-21.9800000189686,-175.439965137037));
#172516=CARTESIAN_POINT('Ctrl Pts',(59.356300154325,-21.98000001654,-175.32367896183));
#172517=CARTESIAN_POINT('Ctrl Pts',(59.3921466355886,-21.9800000173947,
-175.205510135853));
#172518=CARTESIAN_POINT('Ctrl Pts',(59.3996691193178,-21.9800000175741,
-175.180712079269));
#172519=CARTESIAN_POINT('Ctrl Pts',(59.4067991608448,-21.9800000178929,
-175.15584684927));
#172520=CARTESIAN_POINT('Ctrl Pts',(59.4135356395821,-21.9800000182925,
-175.130914599889));
#172521=CARTESIAN_POINT('Ctrl Pts',(59.4621021364647,-21.9800000211732,
-174.951166090456));
#172522=CARTESIAN_POINT('Ctrl Pts',(59.4903344201338,-21.9800000199997,
-174.767951128808));
#172523=CARTESIAN_POINT('Ctrl Pts',(59.4979153635692,-21.98000002,-174.581221680396));
#172524=CARTESIAN_POINT('Ctrl Pts',(59.499304412066,-21.98000002,-174.547007434923));
#172525=CARTESIAN_POINT('Ctrl Pts',(59.5,-21.98000002,-174.512675235736));
#172526=CARTESIAN_POINT('Ctrl Pts',(59.5,-21.98000002,-174.47822483969));
#172527=CARTESIAN_POINT('Origin',(58.2281061322669,-22.48000002,-179.64995));
#172528=CARTESIAN_POINT('',(58.2281061322669,-21.98000002,-171.871644662643));
#172529=CARTESIAN_POINT('',(58.2281061322669,-21.98000002,-176.848603273909));
#172530=CARTESIAN_POINT('Origin',(58.2281061322669,-22.48000002,-171.871644662643));
#172531=CARTESIAN_POINT('',(57.7346476057223,-22.3993856132206,-179.64995));
#172532=CARTESIAN_POINT('Ctrl Pts',(58.0564197191617,-21.9800000366742,
-171.178790026127));
#172533=CARTESIAN_POINT('Ctrl Pts',(57.6735493970763,-21.9798882430102,
-171.380807602766));
#172534=CARTESIAN_POINT('Ctrl Pts',(57.6186574596683,-22.4082912353334,
-171.40978315061));
#172535=CARTESIAN_POINT('Ctrl Pts',(58.1793335836445,-21.9800000364255,
-171.412176181737));
#172536=CARTESIAN_POINT('Ctrl Pts',(57.7654281245283,-21.9798905214978,
-171.542966774725));
#172537=CARTESIAN_POINT('Ctrl Pts',(57.7016369198821,-22.4019038408433,
-171.565352937794));
#172538=CARTESIAN_POINT('Ctrl Pts',(58.2385448347246,-21.9800000363068,
-171.671295447806));
#172539=CARTESIAN_POINT('Ctrl Pts',(57.8110872810659,-21.9798915951361,
-171.728859197825));
#172540=CARTESIAN_POINT('Ctrl Pts',(57.7416081447113,-22.3988541543228,
-171.738094620076));
#172541=CARTESIAN_POINT('Ctrl Pts',(58.2267633341816,-21.9800000363304,
-171.938197690258));
#172542=CARTESIAN_POINT('Ctrl Pts',(57.8020514502591,-21.9798913838386,
-171.91910344938));
#172543=CARTESIAN_POINT('Ctrl Pts',(57.7336548687769,-22.399461430235,-171.916008414622));
#172544=CARTESIAN_POINT('',(58.085700246061,-21.98000002,-171.237717270032));
#172545=CARTESIAN_POINT('Origin',(56.8433387828479,-21.9799994107774,-171.841912580628));
#172546=CARTESIAN_POINT('Origin',(58.085700246061,-22.48000002,-171.237717270032));
#172547=CARTESIAN_POINT('Ctrl Pts',(40.0320988180411,-21.98000002,-133.252725050377));
#172548=CARTESIAN_POINT('Ctrl Pts',(39.6675936435998,-21.98000002,-133.427429361974));
#172549=CARTESIAN_POINT('Ctrl Pts',(39.5912209089345,-22.3752378108182,
-133.464034181247));
#172550=CARTESIAN_POINT('Ctrl Pts',(46.0913014593244,-21.98000002,-145.894718230889));
#172551=CARTESIAN_POINT('Ctrl Pts',(45.790260298639,-21.98000002,-146.231563592216));
#172552=CARTESIAN_POINT('Ctrl Pts',(45.6468692907591,-22.3902470227078,
-146.106052933848));
#172553=CARTESIAN_POINT('Ctrl Pts',(52.0964117641256,-21.98000002,-158.56249372189));
#172554=CARTESIAN_POINT('Ctrl Pts',(51.7509431131532,-21.9800000203624,
-158.826102375503));
#172555=CARTESIAN_POINT('Ctrl Pts',(51.6504270099243,-22.3994099070849,
-158.773819030963));
#172556=CARTESIAN_POINT('Ctrl Pts',(58.085700246061,-21.98000002,-171.237717270032));
#172557=CARTESIAN_POINT('Ctrl Pts',(57.6956367824858,-21.98000002,-171.422029807066));
#172558=CARTESIAN_POINT('Ctrl Pts',(57.638503474757,-22.4067641070473,-171.449026400902));
#172559=CARTESIAN_POINT('',(40.032098818041,-21.98000002,-133.252725050377));
#172560=CARTESIAN_POINT('Ctrl Pts',(40.0320988180411,-21.98000002,-133.252725050377));
#172561=CARTESIAN_POINT('Ctrl Pts',(46.0913111616059,-21.98000002,-145.894738473846));
#172562=CARTESIAN_POINT('Ctrl Pts',(52.0964027110273,-21.98000002,-158.56247456275));
#172563=CARTESIAN_POINT('Ctrl Pts',(58.085700246061,-21.98000002,-171.237717270032));
#172564=CARTESIAN_POINT('Origin',(40.0320988180411,-22.48000002,-133.252725050377));
#172565=CARTESIAN_POINT('Ctrl Pts',(39.5912209089345,-22.3752378108182,
-133.464034181247));
#172566=CARTESIAN_POINT('Ctrl Pts',(39.6675936435998,-21.98000002,-133.427429361974));
#172567=CARTESIAN_POINT('Ctrl Pts',(40.0320988180411,-21.98000002,-133.252725050377));
#172568=CARTESIAN_POINT('Ctrl Pts',(39.3953798878174,-22.3926947961315,
-133.064083894138));
#172569=CARTESIAN_POINT('Ctrl Pts',(39.4616506489997,-21.98000002,-133.032398833922));
#172570=CARTESIAN_POINT('Ctrl Pts',(39.8558398148562,-21.98000002,-132.884976140755));
#172571=CARTESIAN_POINT('Ctrl Pts',(39.2495325922488,-22.4102623065174,
-132.649599803771));
#172572=CARTESIAN_POINT('Ctrl Pts',(39.306634221246,-21.98000002,-132.626108677501));
#172573=CARTESIAN_POINT('Ctrl Pts',(39.7245793327553,-21.98000002,-132.504273278823));
#172574=CARTESIAN_POINT('Ctrl Pts',(39.0515573542344,-22.4453411404847,
-131.793566113248));
#172575=CARTESIAN_POINT('Ctrl Pts',(39.0825794362701,-21.9800000199999,
-131.782866385322));
#172576=CARTESIAN_POINT('Ctrl Pts',(39.5464016190797,-21.98000002,-131.71886357396));
#172577=CARTESIAN_POINT('Ctrl Pts',(39.,-22.4629715740863,-131.348761468896));
#172578=CARTESIAN_POINT('Ctrl Pts',(39.0167438766121,-21.9800000200007,
-131.341321155374));
#172579=CARTESIAN_POINT('Ctrl Pts',(39.5000000005303,-21.98000002,-131.311180490184));
#172580=CARTESIAN_POINT('Ctrl Pts',(39.,-22.48000002,-130.903539806302));
#172581=CARTESIAN_POINT('Ctrl Pts',(39.,-21.98000002,-130.903539806302));
#172582=CARTESIAN_POINT('Ctrl Pts',(39.5,-21.98000002,-130.903539806302));
#172583=CARTESIAN_POINT('',(39.5,-21.98000002,-130.903539806302));
#172584=CARTESIAN_POINT('Ctrl Pts',(39.5,-21.98000002,-130.903539806302));
#172585=CARTESIAN_POINT('Ctrl Pts',(39.5,-21.98000002,-131.168997483208));
#172586=CARTESIAN_POINT('Ctrl Pts',(39.5196729008546,-21.98000002,-131.434381070388));
#172587=CARTESIAN_POINT('Ctrl Pts',(39.5579798343717,-21.98000002,-131.695636340096));
#172588=CARTESIAN_POINT('Ctrl Pts',(39.5785131750261,-21.98000002,-131.835674786355));
#172589=CARTESIAN_POINT('Ctrl Pts',(39.6044013642074,-21.98000002,-131.974527214016));
#172590=CARTESIAN_POINT('Ctrl Pts',(39.6354904757816,-21.98000002,-132.111568426422));
#172591=CARTESIAN_POINT('Ctrl Pts',(39.7067779603521,-21.98000002,-132.425804595304));
#172592=CARTESIAN_POINT('Ctrl Pts',(39.805057091038,-21.98000002,-132.732328205559));
#172593=CARTESIAN_POINT('Ctrl Pts',(39.9318010945635,-21.98000002,-133.030718310498));
#172594=CARTESIAN_POINT('Ctrl Pts',(39.9634506501669,-21.98000002,-133.105230034564));
#172595=CARTESIAN_POINT('Ctrl Pts',(39.9968754124341,-21.98000002,-133.179234513779));
#172596=CARTESIAN_POINT('Ctrl Pts',(40.032098818041,-21.98000002,-133.252725050377));
#172597=CARTESIAN_POINT('Origin',(39.5,-22.48000002,-130.903539806302));
#172598=CARTESIAN_POINT('Origin',(39.5,-22.48000002,-55.24995));
#172599=CARTESIAN_POINT('',(39.5,-21.98000002,-101.155103165204));
#172600=CARTESIAN_POINT('',(39.5,-21.98000002,-55.24995));
#172601=CARTESIAN_POINT('Origin',(39.5,-22.48000002,-101.155103165204));
#172602=CARTESIAN_POINT('Ctrl Pts',(39.,-22.48000002,-101.155103165204));
#172603=CARTESIAN_POINT('Ctrl Pts',(39.,-21.98000002,-101.155103165204));
#172604=CARTESIAN_POINT('Ctrl Pts',(39.5,-21.98000002,-101.155103165204));
#172605=CARTESIAN_POINT('Ctrl Pts',(39.,-22.4629652077836,-100.709715051444));
#172606=CARTESIAN_POINT('Ctrl Pts',(39.0167494918295,-21.9800000199972,
-100.717175065292));
#172607=CARTESIAN_POINT('Ctrl Pts',(39.5000000028409,-21.98000002,-100.74730649838));
#172608=CARTESIAN_POINT('Ctrl Pts',(39.0503363863868,-22.445662928874,-100.273107244626));
#172609=CARTESIAN_POINT('Ctrl Pts',(39.0810957011176,-21.9800000199993,
-100.283723962358));
#172610=CARTESIAN_POINT('Ctrl Pts',(39.5453027473158,-21.98000002,-100.347142039227));
#172611=CARTESIAN_POINT('Ctrl Pts',(39.2470786821289,-22.4105936079244,
-99.4169535019087));
#172612=CARTESIAN_POINT('Ctrl Pts',(39.3039755059085,-21.9800000200007,
-99.4402934124299));
#172613=CARTESIAN_POINT('Ctrl Pts',(39.7223708143483,-21.98000002,-99.5616325432134));
#172614=CARTESIAN_POINT('Ctrl Pts',(39.3953243387798,-22.392699749305,-98.9946725198791));
#172615=CARTESIAN_POINT('Ctrl Pts',(39.461600153608,-21.98000002,-99.0263409880856));
#172616=CARTESIAN_POINT('Ctrl Pts',(39.8557911961828,-21.98000002,-99.1737682638933));
#172617=CARTESIAN_POINT('Ctrl Pts',(39.5912209089311,-22.3752378108185,
-98.5946087902659));
#172618=CARTESIAN_POINT('Ctrl Pts',(39.6675936435963,-21.98000002,-98.6312136095388));
#172619=CARTESIAN_POINT('Ctrl Pts',(40.032098818038,-21.98000002,-98.8059179211357));
#172620=CARTESIAN_POINT('',(40.032098818038,-21.98000002,-98.8059179211358));
#172621=CARTESIAN_POINT('Ctrl Pts',(40.032098818038,-21.98000002,-98.8059179211358));
#172622=CARTESIAN_POINT('Ctrl Pts',(39.9030508971585,-21.98000002,-99.0751650535137));
#172623=CARTESIAN_POINT('Ctrl Pts',(39.7969528124074,-21.98000002,-99.3552012197209));
#172624=CARTESIAN_POINT('Ctrl Pts',(39.7146317074512,-21.98000002,-99.6400255235404));
#172625=CARTESIAN_POINT('Ctrl Pts',(39.6845025786606,-21.98000002,-99.7442698499136));
#172626=CARTESIAN_POINT('Ctrl Pts',(39.6575579700038,-21.98000002,-99.849155332173));
#172627=CARTESIAN_POINT('Ctrl Pts',(39.6338367806139,-21.98000002,-99.9543872911712));
#172628=CARTESIAN_POINT('Ctrl Pts',(39.561388548558,-21.98000002,-100.275782195106));
#172629=CARTESIAN_POINT('Ctrl Pts',(39.5178914194317,-21.98000002,-100.602110104162));
#172630=CARTESIAN_POINT('Ctrl Pts',(39.5044747449633,-21.98000002,-100.933563458967));
#172631=CARTESIAN_POINT('Ctrl Pts',(39.5014958184563,-21.98000002,-101.007156597624));
#172632=CARTESIAN_POINT('Ctrl Pts',(39.5,-21.98000002,-101.081002444677));
#172633=CARTESIAN_POINT('Ctrl Pts',(39.5,-21.98000002,-101.155103165204));
#172634=CARTESIAN_POINT('',(39.5912209089345,-22.3752378108151,-98.5946087902606));
#172635=CARTESIAN_POINT('Origin',(40.032098818038,-22.4800000199998,-98.8059179211357));
#172636=CARTESIAN_POINT('Ctrl Pts',(39.,-22.48000002,-101.155103165204));
#172637=CARTESIAN_POINT('Ctrl Pts',(39.,-22.4767350571047,-101.069738228568));
#172638=CARTESIAN_POINT('Ctrl Pts',(39.001844810516,-22.4732834802974,-100.980072408275));
#172639=CARTESIAN_POINT('Ctrl Pts',(39.0061450083956,-22.4696426076462,
-100.88622267467));
#172640=CARTESIAN_POINT('Ctrl Pts',(39.0096198368864,-22.4667005551237,
-100.810386227766));
#172641=CARTESIAN_POINT('Ctrl Pts',(39.0146989999904,-22.4636348949715,
-100.73181802585));
#172642=CARTESIAN_POINT('Ctrl Pts',(39.0217284047154,-22.4604441490632,
-100.65058434866));
#172643=CARTESIAN_POINT('Ctrl Pts',(39.026292189657,-22.458372582736,-100.597844031776));
#172644=CARTESIAN_POINT('Ctrl Pts',(39.031678928859,-22.4562481400062,-100.543976489461));
#172645=CARTESIAN_POINT('Ctrl Pts',(39.0379859380183,-22.454071013344,-100.489016010024));
#172646=CARTESIAN_POINT('Ctrl Pts',(39.0484435371741,-22.4504611378278,
-100.39788649858));
#172647=CARTESIAN_POINT('Ctrl Pts',(39.0614304565616,-22.4467066621347,
-100.303758414252));
#172648=CARTESIAN_POINT('Ctrl Pts',(39.0773930576913,-22.4428095278211,
-100.206815225869));
#172649=CARTESIAN_POINT('Ctrl Pts',(39.09274066922,-22.439062538027,-100.113606958396));
#172650=CARTESIAN_POINT('Ctrl Pts',(39.1108399400955,-22.4351837761763,
-100.017799350643));
#172651=CARTESIAN_POINT('Ctrl Pts',(39.1320731933389,-22.4311775089901,
-99.9196156578223));
#172652=CARTESIAN_POINT('Ctrl Pts',(39.1369808481102,-22.4302515380122,
-99.8969224010233));
#172653=CARTESIAN_POINT('Ctrl Pts',(39.1420558181611,-22.4293187663864,
-99.8741024539549));
#172654=CARTESIAN_POINT('Ctrl Pts',(39.1473026139867,-22.4283792645213,
-99.8511589578541));
#172655=CARTESIAN_POINT('Ctrl Pts',(39.1477530888856,-22.4282986015755,
-99.8491890948312));
#172656=CARTESIAN_POINT('Ctrl Pts',(39.1485162523428,-22.4281623691545,
-99.8458628893345));
#172657=CARTESIAN_POINT('Ctrl Pts',(39.1486578411466,-22.4281371266263,
-99.8452466389702));
#172658=CARTESIAN_POINT('Ctrl Pts',(39.1486743781443,-22.4281341784015,
-99.8451746634286));
#172659=CARTESIAN_POINT('Ctrl Pts',(39.1486909425236,-22.4281312255307,
-99.8451025748626));
#172660=CARTESIAN_POINT('Ctrl Pts',(39.148707534297,-22.428128268014,-99.845030373276));
#172661=CARTESIAN_POINT('Ctrl Pts',(39.1518270689057,-22.4275722047527,
-99.8314552513122));
#172662=CARTESIAN_POINT('Ctrl Pts',(39.1559125612838,-22.4268517977281,
-99.8138813002624));
#172663=CARTESIAN_POINT('Ctrl Pts',(39.1610759072736,-22.4259667647546,
-99.7923348463416));
#172664=CARTESIAN_POINT('Ctrl Pts',(39.1662355138054,-22.42508237275,-99.7708039970424));
#172665=CARTESIAN_POINT('Ctrl Pts',(39.1724714900693,-22.4240335791768,
-99.7453061166653));
#172666=CARTESIAN_POINT('Ctrl Pts',(39.1799461680143,-22.4228199948629,
-99.7158789022736));
#172667=CARTESIAN_POINT('Ctrl Pts',(39.1867519047032,-22.4217150194578,
-99.6890852565657));
#172668=CARTESIAN_POINT('Ctrl Pts',(39.1945851963102,-22.4204734171491,
-99.6590340292539));
#172669=CARTESIAN_POINT('Ctrl Pts',(39.2036042917547,-22.4190949885092,
-99.6257653903841));
#172670=CARTESIAN_POINT('Ctrl Pts',(39.2134357504478,-22.4175924027657,
-99.5895001960708));
#172671=CARTESIAN_POINT('Ctrl Pts',(39.2246753006762,-22.415927280686,-99.5494129467876));
#172672=CARTESIAN_POINT('Ctrl Pts',(39.2375704699864,-22.4141000585316,
-99.5055833725206));
#172673=CARTESIAN_POINT('Ctrl Pts',(39.2501483362211,-22.4123177976487,
-99.4628322841872));
#172674=CARTESIAN_POINT('Ctrl Pts',(39.2643018106626,-22.4103812720758,
-99.4165198589484));
#172675=CARTESIAN_POINT('Ctrl Pts',(39.2803005761706,-22.4082917028185,
-99.3667489313563));
#172676=CARTESIAN_POINT('Ctrl Pts',(39.2900736410679,-22.4070152608362,
-99.3363456789858));
#172677=CARTESIAN_POINT('Ctrl Pts',(39.3005360632784,-22.4056817248198,
-99.3046524019425));
#172678=CARTESIAN_POINT('Ctrl Pts',(39.3117561762374,-22.4042915876652,
-99.2716991216448));
#172679=CARTESIAN_POINT('Ctrl Pts',(39.3152146560669,-22.4038630927537,
-99.2615416254019));
#172680=CARTESIAN_POINT('Ctrl Pts',(39.3187451592901,-22.4034292213711,
-99.2512644589312));
#172681=CARTESIAN_POINT('Ctrl Pts',(39.3223498480703,-22.4029895534928,
-99.2408686341921));
#172682=CARTESIAN_POINT('Ctrl Pts',(39.3241521924604,-22.4027697195536,
-99.2356707218225));
#172683=CARTESIAN_POINT('Ctrl Pts',(39.3259731076755,-22.4025482786348,
-99.2304431532566));
#172684=CARTESIAN_POINT('Ctrl Pts',(39.3278127975991,-22.4023256545837,
-99.2251860363515));
#172685=CARTESIAN_POINT('Ctrl Pts',(39.3296524875228,-22.4021030305325,
-99.2199289194463));
#172686=CARTESIAN_POINT('Ctrl Pts',(39.3319414859164,-22.401827635554,-99.2134232135355));
#172687=CARTESIAN_POINT('Ctrl Pts',(39.3333884566463,-22.401654256214,-99.209326170086));
#172688=CARTESIAN_POINT('Ctrl Pts',(39.3571412292357,-22.398808144714,-99.1420710837627));
#172689=CARTESIAN_POINT('Ctrl Pts',(39.3809074316803,-22.3961123131947,
-99.0787019928113));
#172690=CARTESIAN_POINT('Ctrl Pts',(39.4043137429003,-22.3935678599518,
-99.0191392615585));
#172691=CARTESIAN_POINT('Ctrl Pts',(39.4281732527221,-22.3909741403959,
-98.9584232624427));
#172692=CARTESIAN_POINT('Ctrl Pts',(39.4516587935485,-22.3885376879477,
-98.9016618018122));
#172693=CARTESIAN_POINT('Ctrl Pts',(39.4744264125052,-22.3862580561699,
-98.8487497482935));
#172694=CARTESIAN_POINT('Ctrl Pts',(39.4976916026771,-22.3839286045512,
-98.794681336931));
#172695=CARTESIAN_POINT('Ctrl Pts',(39.5202071163624,-22.3817628736423,
-98.7446317833894));
#172696=CARTESIAN_POINT('Ctrl Pts',(39.541659516076,-22.3797591779471,-98.6984773338181));
#172697=CARTESIAN_POINT('Ctrl Pts',(39.5589079809675,-22.378148137909,-98.6613675739008));
#172698=CARTESIAN_POINT('Ctrl Pts',(39.5754702335143,-22.3766418202078,
-98.6267755530437));
#172699=CARTESIAN_POINT('Ctrl Pts',(39.5912077081794,-22.3752389875185,
-98.5946357492765));
#172700=CARTESIAN_POINT('Ctrl Pts',(57.9716987024741,-21.98000002,-61.0621827299711));
#172701=CARTESIAN_POINT('Ctrl Pts',(57.5817506954796,-21.98000002,-60.8779152752782));
#172702=CARTESIAN_POINT('Ctrl Pts',(57.5245249214072,-22.4066238608121,
-60.8508735991008));
#172703=CARTESIAN_POINT('Ctrl Pts',(52.0201596782203,-21.98000002,-73.6568689967289));
#172704=CARTESIAN_POINT('Ctrl Pts',(51.6744341991619,-21.980000020072,-73.3940563428121));
#172705=CARTESIAN_POINT('Ctrl Pts',(51.5741970743562,-22.3992883743679,
-73.4455439799432));
#172706=CARTESIAN_POINT('Ctrl Pts',(46.0528581107812,-21.98000002,-86.2441334050211));
#172707=CARTESIAN_POINT('Ctrl Pts',(45.7509404552383,-21.98000002,-85.9093076925101));
#172708=CARTESIAN_POINT('Ctrl Pts',(45.6084483216386,-22.3901517945239,
-86.0327992211263));
#172709=CARTESIAN_POINT('Ctrl Pts',(40.032098818038,-21.98000002,-98.8059179211357));
#172710=CARTESIAN_POINT('Ctrl Pts',(39.6675936435968,-21.98000002,-98.6312136095384));
#172711=CARTESIAN_POINT('Ctrl Pts',(39.5912209089315,-22.3752378108182,
-98.5946087902654));
#172712=CARTESIAN_POINT('',(57.9716987024741,-21.98000002,-61.0621827299711));
#172713=CARTESIAN_POINT('Ctrl Pts',(57.9716987024741,-21.98000002,-61.0621827299711));
#172714=CARTESIAN_POINT('Ctrl Pts',(52.0201508381868,-21.98000002,-73.6568877040663));
#172715=CARTESIAN_POINT('Ctrl Pts',(46.0528675815424,-21.98000002,-86.2441136451113));
#172716=CARTESIAN_POINT('Ctrl Pts',(40.032098818038,-21.98000002,-98.8059179211357));
#172717=CARTESIAN_POINT('',(57.5245249214072,-22.4066238608121,-60.8508735991007));
#172718=CARTESIAN_POINT('Origin',(57.9716987024741,-22.48000002,-61.0621827299711));
#172719=CARTESIAN_POINT('Ctrl Pts',(39.5912209089345,-22.3752378108151,
-98.5946087902606));
#172720=CARTESIAN_POINT('Ctrl Pts',(40.9473935734796,-22.3785991491226,
-95.763407376981));
#172721=CARTESIAN_POINT('Ctrl Pts',(42.3747096804507,-22.3820178133902,
-92.7761193440102));
#172722=CARTESIAN_POINT('Ctrl Pts',(44.6224781400908,-22.3866023021413,
-88.061057365017));
#172723=CARTESIAN_POINT('Ctrl Pts',(45.389531418281,-22.3880535629714,-86.4503483837631));
#172724=CARTESIAN_POINT('Ctrl Pts',(46.5668026381736,-22.3901600190474,
-83.9757524294981));
#172725=CARTESIAN_POINT('Ctrl Pts',(47.1621109494658,-22.3911969294873,
-82.7238213317696));
#172726=CARTESIAN_POINT('Ctrl Pts',(47.8683124092611,-22.3924015844907,
-81.2376270900431));
#172727=CARTESIAN_POINT('Ctrl Pts',(48.2243315716556,-22.3930065987344,
-80.4881279789192));
#172728=CARTESIAN_POINT('Ctrl Pts',(48.4254131098423,-22.3933482630478,
-80.0647341691511));
#172729=CARTESIAN_POINT('Ctrl Pts',(48.5246188153984,-22.3935169090336,
-79.8558253309021));
#172730=CARTESIAN_POINT('Ctrl Pts',(48.5758868958006,-22.3936041070006,
-79.7478585128181));
#172731=CARTESIAN_POINT('Ctrl Pts',(48.5796195095595,-22.3936104557674,
-79.7399978701883));
#172732=CARTESIAN_POINT('Ctrl Pts',(51.3232477570397,-22.3982772069777,
-73.9620770724378));
#172733=CARTESIAN_POINT('Ctrl Pts',(54.3039844455626,-22.4026536205826,
-67.667581314042));
#172734=CARTESIAN_POINT('Ctrl Pts',(57.5245249214072,-22.4066238608121,
-60.8508735991007));
#172735=CARTESIAN_POINT('Ctrl Pts',(39.7614971661825,-28.0062467616585,
-94.6983380795177));
#172736=CARTESIAN_POINT('Ctrl Pts',(39.,-28.741729147553,-95.6677964063875));
#172737=CARTESIAN_POINT('Ctrl Pts',(39.,-29.6093496431988,-96.8114293882212));
#172738=CARTESIAN_POINT('Ctrl Pts',(39.7437819827477,-27.4973039569491,
-95.1199826758911));
#172739=CARTESIAN_POINT('Ctrl Pts',(39.,-28.2134674407351,-96.0912283932403));
#172740=CARTESIAN_POINT('Ctrl Pts',(39.,-29.0535677480794,-97.2330749436175));
#172741=CARTESIAN_POINT('Ctrl Pts',(39.7262969548998,-26.9800167700376,
-95.5308471039398));
#172742=CARTESIAN_POINT('Ctrl Pts',(39.,-27.6753857963049,-96.504280291422));
#172743=CARTESIAN_POINT('Ctrl Pts',(39.,-28.4877143439141,-97.6439384126816));
#172744=CARTESIAN_POINT('Ctrl Pts',(39.6919956601185,-25.9258412309992,
-96.3274629617598));
#172745=CARTESIAN_POINT('Ctrl Pts',(39.,-26.5774575077333,-97.3050952674327));
#172746=CARTESIAN_POINT('Ctrl Pts',(39.,-27.3325353334211,-98.4405542704251));
#172747=CARTESIAN_POINT('Ctrl Pts',(39.6751334260609,-25.3873798477126,
-96.7142461865699));
#172748=CARTESIAN_POINT('Ctrl Pts',(39.,-26.0159584590169,-97.6939770973016));
#172749=CARTESIAN_POINT('Ctrl Pts',(39.,-26.741479037393,-98.8273374953048));
#172750=CARTESIAN_POINT('Ctrl Pts',(39.6263764589698,-23.7517847228855,
-97.8205111744839));
#172751=CARTESIAN_POINT('Ctrl Pts',(39.,-24.3098005849941,-98.8051808316371));
#172752=CARTESIAN_POINT('Ctrl Pts',(39.,-24.9430461321624,-99.9336024831245));
#172753=CARTESIAN_POINT('Ctrl Pts',(39.5962627317006,-22.634454054442,-98.4870223585708));
#172754=CARTESIAN_POINT('Ctrl Pts',(38.9999999999805,-23.1402109105079,
-99.4757726121153));
#172755=CARTESIAN_POINT('Ctrl Pts',(39.,-23.7104174150638,-100.600117065969));
#172756=CARTESIAN_POINT('Ctrl Pts',(39.5698473334291,-21.4814334314007,
-99.0625227403511));
#172757=CARTESIAN_POINT('Ctrl Pts',(39.,-21.9292338920902,-100.055223222194));
#172758=CARTESIAN_POINT('Ctrl Pts',(39.,-22.4346346021703,-101.175614049055));
#172759=CARTESIAN_POINT('',(39.7602371815487,-27.9700232796676,-94.7283182583424));
#172760=CARTESIAN_POINT('Ctrl Pts',(39.760237187334,-27.9700232996177,-94.7283182916262));
#172761=CARTESIAN_POINT('Ctrl Pts',(39.7447508838319,-27.5244916807806,
-95.096692988375));
#172762=CARTESIAN_POINT('Ctrl Pts',(39.7297644606222,-27.0817800144324,
-95.4491475626341));
#172763=CARTESIAN_POINT('Ctrl Pts',(39.7152783970567,-26.6405416183526,
-95.7865386233445));
#172764=CARTESIAN_POINT('Ctrl Pts',(39.7132243273442,-26.5779756616797,
-95.8343794157002));
#172765=CARTESIAN_POINT('Ctrl Pts',(39.7111803019538,-26.5154393868985,
-95.8819173924144));
#172766=CARTESIAN_POINT('Ctrl Pts',(39.7091463075091,-26.4529290005184,
-95.9291550328498));
#172767=CARTESIAN_POINT('Ctrl Pts',(39.7021598335833,-26.2382149506942,
-96.0914094303885));
#172768=CARTESIAN_POINT('Ctrl Pts',(39.6952842340061,-26.0235489205403,
-96.2502889063942));
#172769=CARTESIAN_POINT('Ctrl Pts',(39.6885330384432,-25.809181245456,-96.4055817431426));
#172770=CARTESIAN_POINT('Ctrl Pts',(39.681431379786,-25.5836854734279,-96.5689360273148));
#172771=CARTESIAN_POINT('Ctrl Pts',(39.6744673646565,-25.3585197762647,
-96.7283219086833));
#172772=CARTESIAN_POINT('Ctrl Pts',(39.6676547428316,-25.1339280420678,
-96.8835265364444));
#172773=CARTESIAN_POINT('Ctrl Pts',(39.6647014284074,-25.0365661122239,
-96.9508087190838));
#172774=CARTESIAN_POINT('Ctrl Pts',(39.6617765415299,-24.939311468461,-97.0173055150268));
#172775=CARTESIAN_POINT('Ctrl Pts',(39.6588811036972,-24.8421814727703,
-97.0830011825413));
#172776=CARTESIAN_POINT('Ctrl Pts',(39.6476505823632,-24.4654438075899,
-97.3378146643689));
#172777=CARTESIAN_POINT('Ctrl Pts',(39.6368573959785,-24.0905821641491,
-97.5807135994866));
#172778=CARTESIAN_POINT('Ctrl Pts',(39.6265067297219,-23.7166730378311,
-97.8120922005714));
#172779=CARTESIAN_POINT('Ctrl Pts',(39.617412986147,-23.3881691878632,-98.0153735753937));
#172780=CARTESIAN_POINT('Ctrl Pts',(39.6086607036092,-23.060400896105,-98.2097630572075));
#172781=CARTESIAN_POINT('Ctrl Pts',(39.6002528798929,-22.7327299685291,
-98.3954874204445));
#172782=CARTESIAN_POINT('Ctrl Pts',(39.597195434678,-22.6135747693504,-98.4630247624282));
#172783=CARTESIAN_POINT('Ctrl Pts',(39.5941835411059,-22.4944322994311,
-98.5294158133307));
#172784=CARTESIAN_POINT('Ctrl Pts',(39.5912173600348,-22.3752713037914,
-98.5946697908291));
#172785=CARTESIAN_POINT('Ctrl Pts',(39.7602371793877,-27.9700232590251,
-94.7283182583078));
#172786=CARTESIAN_POINT('Ctrl Pts',(39.721173342089,-27.9739864535911,-94.8036965512742));
#172787=CARTESIAN_POINT('Ctrl Pts',(39.6812588478966,-27.9782127469329,
-94.8842699537839));
#172788=CARTESIAN_POINT('Ctrl Pts',(39.6410880301102,-27.9827071593153,
-94.9702238054998));
#172789=CARTESIAN_POINT('Ctrl Pts',(39.6256104639824,-27.9844388284395,
-95.0033412897129));
#172790=CARTESIAN_POINT('Ctrl Pts',(39.6100953866432,-27.9862102988464,
-95.0372576699903));
#172791=CARTESIAN_POINT('Ctrl Pts',(39.5945787380208,-27.9880218495183,
-95.0719841268097));
#172792=CARTESIAN_POINT('Ctrl Pts',(39.5666842850881,-27.9912784944409,
-95.1344122669862));
#172793=CARTESIAN_POINT('Ctrl Pts',(39.5387859048961,-27.9946645037012,
-95.1994551025455));
#172794=CARTESIAN_POINT('Ctrl Pts',(39.5111086085599,-27.9981802158359,
-95.2671566087482));
#172795=CARTESIAN_POINT('Ctrl Pts',(39.4972699603918,-27.9999380719032,
-95.3010073618496));
#172796=CARTESIAN_POINT('Ctrl Pts',(39.4834868072858,-28.001728337867,-95.3355225476929));
#172797=CARTESIAN_POINT('Ctrl Pts',(39.4697884556866,-28.0035509529382,
-95.3707060919163));
#172798=CARTESIAN_POINT('Ctrl Pts',(39.462939279887,-28.0044622604738,-95.388297864028));
#172799=CARTESIAN_POINT('Ctrl Pts',(39.456111308277,-28.0053816551031,-95.406056726538));
#172800=CARTESIAN_POINT('Ctrl Pts',(39.449308271849,-28.0063091210918,-95.4239830388244));
#172801=CARTESIAN_POINT('Ctrl Pts',(39.445906753635,-28.0067728540861,-95.4329461949676));
#172802=CARTESIAN_POINT('Ctrl Pts',(39.4425114693047,-28.0072386049083,
-95.441951213587));
#172803=CARTESIAN_POINT('Ctrl Pts',(39.4391228871938,-28.0077063712997,
-95.4509981355552));
#172804=CARTESIAN_POINT('Ctrl Pts',(39.4374285961383,-28.0079402544954,
-95.4555215965394));
#172805=CARTESIAN_POINT('Ctrl Pts',(39.4357359806405,-28.0081746415827,
-95.460055533362));
#172806=CARTESIAN_POINT('Ctrl Pts',(39.4340450994288,-28.0084095322498,
-95.4645999506646));
#172807=CARTESIAN_POINT('Ctrl Pts',(39.433199658823,-28.0085269775834,-95.4668721593159));
#172808=CARTESIAN_POINT('Ctrl Pts',(39.4323546517888,-28.0086445488119,
-95.4691469880873));
#172809=CARTESIAN_POINT('Ctrl Pts',(39.431510085679,-28.0087622458945,-95.4714244375276));
#172810=CARTESIAN_POINT('Ctrl Pts',(39.4306655195692,-28.008879942977,-95.4737018869679));
#172811=CARTESIAN_POINT('Ctrl Pts',(39.4291050611265,-28.0090979116105,
-95.4779201015231));
#172812=CARTESIAN_POINT('Ctrl Pts',(39.4289777174792,-28.0091157146626,
-95.4782646483947));
#172813=CARTESIAN_POINT('Ctrl Pts',(39.426693894066,-28.0094350005327,-95.4844438668219));
#172814=CARTESIAN_POINT('Ctrl Pts',(39.4228824393387,-28.0099686170733,
-95.4947718201092));
#172815=CARTESIAN_POINT('Ctrl Pts',(39.4176054119079,-28.0107171614978,
-95.5092693092406));
#172816=CARTESIAN_POINT('Ctrl Pts',(39.412306317478,-28.0114688361181,-95.5238274226692));
#172817=CARTESIAN_POINT('Ctrl Pts',(39.4055293860221,-28.0124372416699,
-95.5425900228496));
#172818=CARTESIAN_POINT('Ctrl Pts',(39.3973879849454,-28.0136233734704,
-95.5655935175528));
#172819=CARTESIAN_POINT('Ctrl Pts',(39.3891953935039,-28.0148169632648,
-95.5887416504178));
#172820=CARTESIAN_POINT('Ctrl Pts',(39.3796211568778,-28.0162310288329,
-95.6161841886283));
#172821=CARTESIAN_POINT('Ctrl Pts',(39.3688314625449,-28.0178669439296,
-95.6479736028182));
#172822=CARTESIAN_POINT('Ctrl Pts',(39.358671911494,-28.0194073177739,-95.6779064411708));
#172823=CARTESIAN_POINT('Ctrl Pts',(39.3474346778275,-28.0211444822674,
-95.7116951824943));
#172824=CARTESIAN_POINT('Ctrl Pts',(39.3353005090293,-28.0230794904341,
-95.7493891119716));
#172825=CARTESIAN_POINT('Ctrl Pts',(39.3220949453622,-28.025185351492,-95.7904112531542));
#172826=CARTESIAN_POINT('Ctrl Pts',(39.307827638871,-28.0275253887629,-95.8360556009816));
#172827=CARTESIAN_POINT('Ctrl Pts',(39.2927843742968,-28.0301004647007,
-95.8863862017628));
#172828=CARTESIAN_POINT('Ctrl Pts',(39.2775020102043,-28.0327164692158,
-95.9375167633733));
#172829=CARTESIAN_POINT('Ctrl Pts',(39.2614179145521,-28.035575275758,-95.9934882030578));
#172830=CARTESIAN_POINT('Ctrl Pts',(39.2448872805952,-28.0386765911129,
-96.0543562552077));
#172831=CARTESIAN_POINT('Ctrl Pts',(39.2287363134251,-28.0417066771102,
-96.1138263223896));
#172832=CARTESIAN_POINT('Ctrl Pts',(39.2121593315286,-28.0449683682601,
-96.1779727979824));
#172833=CARTESIAN_POINT('Ctrl Pts',(39.1955312387891,-28.0484600623225,
-96.2468332932256));
#172834=CARTESIAN_POINT('Ctrl Pts',(39.1946291423112,-28.048649491439,-96.2505690680494));
#172835=CARTESIAN_POINT('Ctrl Pts',(39.1934506554151,-28.0488980061046,
-96.255470935905));
#172836=CARTESIAN_POINT('Ctrl Pts',(39.1928245891292,-28.0490303797397,
-96.2580822296316));
#172837=CARTESIAN_POINT('Ctrl Pts',(39.1927284851265,-28.0490506996906,
-96.2584830750132));
#172838=CARTESIAN_POINT('Ctrl Pts',(39.1926324279919,-28.0490710181889,
-96.25888387789));
#172839=CARTESIAN_POINT('Ctrl Pts',(39.1925364176938,-28.0490913352319,
-96.2592846382602));
#172840=CARTESIAN_POINT('Ctrl Pts',(39.1705544952503,-28.0537429994074,
-96.3510402473537));
#172841=CARTESIAN_POINT('Ctrl Pts',(39.1510615013283,-28.0583237172308,
-96.4406840483798));
#172842=CARTESIAN_POINT('Ctrl Pts',(39.1337484254094,-28.0627975236857,
-96.528086779579));
#172843=CARTESIAN_POINT('Ctrl Pts',(39.1196099345289,-28.0664509976298,
-96.5994630459213));
#172844=CARTESIAN_POINT('Ctrl Pts',(39.1069256168401,-28.0700332425997,
-96.6693458907162));
#172845=CARTESIAN_POINT('Ctrl Pts',(39.095537681765,-28.0735262649617,-96.7376882535311));
#172846=CARTESIAN_POINT('Ctrl Pts',(39.0802857711333,-28.078204484898,-96.8292194752271));
#172847=CARTESIAN_POINT('Ctrl Pts',(39.0673590162165,-28.0827242117545,
-96.9179853660842));
#172848=CARTESIAN_POINT('Ctrl Pts',(39.0564122238475,-28.0870466384659,
-97.0038380129319));
#172849=CARTESIAN_POINT('Ctrl Pts',(39.0491330840064,-28.0899208638486,
-97.0609262814465));
#172850=CARTESIAN_POINT('Ctrl Pts',(39.0427297849026,-28.0927079320018,
-97.1167275272839));
#172851=CARTESIAN_POINT('Ctrl Pts',(39.0371055462776,-28.0953973309735,
-97.171209960409));
#172852=CARTESIAN_POINT('Ctrl Pts',(39.028325243207,-28.0995958971482,-97.2562654331141));
#172853=CARTESIAN_POINT('Ctrl Pts',(39.0214375200278,-28.1035689840776,
-97.3381388769938));
#172854=CARTESIAN_POINT('Ctrl Pts',(39.0160961336416,-28.1073516111888,
-97.4167589491541));
#172855=CARTESIAN_POINT('Ctrl Pts',(39.0106007252515,-28.1112433125676,
-97.4976460771276));
#172856=CARTESIAN_POINT('Ctrl Pts',(39.0067420005837,-28.1149334424741,
-97.5750899904949));
#172857=CARTESIAN_POINT('Ctrl Pts',(39.0041777909439,-28.1184604696338,
-97.6490565225246));
#172858=CARTESIAN_POINT('Ctrl Pts',(39.0015182173996,-28.1221186682375,
-97.7257738972244));
#172859=CARTESIAN_POINT('Ctrl Pts',(39.0002510559389,-28.1256014236328,
-97.7987508895155));
#172860=CARTESIAN_POINT('Ctrl Pts',(39.000033928547,-28.128951635191,-97.8679882137764));
#172861=CARTESIAN_POINT('Ctrl Pts',(39.0000111867388,-28.1293025345779,
-97.8752400945046));
#172862=CARTESIAN_POINT('Ctrl Pts',(39.,-28.1296519797826,-97.8824509799334));
#172863=CARTESIAN_POINT('Ctrl Pts',(39.,-28.1300000200001,-97.8896208912436));
#172864=CARTESIAN_POINT('Ctrl Pts',(39.7602371906926,-27.9700232578782,
-94.7283182364936));
#172865=CARTESIAN_POINT('Ctrl Pts',(39.5607615517246,-28.6300000199999,
-94.628899882694));
#172866=CARTESIAN_POINT('Ctrl Pts',(40.1842134716234,-28.63000002,-94.9396273673639));
#172867=CARTESIAN_POINT('Ctrl Pts',(39.5060135610296,-27.995815206986,-95.2188728854821));
#172868=CARTESIAN_POINT('Ctrl Pts',(39.3499072921674,-28.63000002,-95.1384098881608));
#172869=CARTESIAN_POINT('Ctrl Pts',(39.9554048343097,-28.63000002,-95.3987151357952));
#172870=CARTESIAN_POINT('Ctrl Pts',(39.3193354149279,-28.0222617282467,
-95.7300059572715));
#172871=CARTESIAN_POINT('Ctrl Pts',(39.1953130903143,-28.63000002,-95.6752490593844));
#172872=CARTESIAN_POINT('Ctrl Pts',(39.7874018733942,-28.63000002,-95.8764151880824));
#172873=CARTESIAN_POINT('Ctrl Pts',(39.0657374218185,-28.0759209337118,
-96.7885633195629));
#172874=CARTESIAN_POINT('Ctrl Pts',(39.0100660589831,-28.63000002,-96.7655348922061));
#172875=CARTESIAN_POINT('Ctrl Pts',(39.5591636796777,-28.63000002,-96.8642956936284));
#172876=CARTESIAN_POINT('Ctrl Pts',(39.,-28.1033206002549,-97.3400031641594));
#172877=CARTESIAN_POINT('Ctrl Pts',(38.9725899744442,-28.63000002,-97.3249520920672));
#172878=CARTESIAN_POINT('Ctrl Pts',(39.500000000016,-28.63000002,-97.3781967454117));
#172879=CARTESIAN_POINT('Ctrl Pts',(39.,-28.13000002,-97.8896208912436));
#172880=CARTESIAN_POINT('Ctrl Pts',(39.,-28.63000002,-97.8896208912435));
#172881=CARTESIAN_POINT('Ctrl Pts',(39.5,-28.63000002,-97.8896208912436));
#172882=CARTESIAN_POINT('',(39.5,-28.63000002,-97.8896208912436));
#172883=CARTESIAN_POINT('Origin',(39.5,-28.13000002,-97.8896208912436));
#172884=CARTESIAN_POINT('',(40.1842134716234,-28.63000002,-94.9396273673639));
#172885=CARTESIAN_POINT('Origin',(40.1842134716234,-28.13000002,-94.9396273673639));
#172886=CARTESIAN_POINT('Ctrl Pts',(39.5,-28.63000002,-97.8896208912436));
#172887=CARTESIAN_POINT('Ctrl Pts',(39.5,-28.63000002,-97.7089321417025));
#172888=CARTESIAN_POINT('Ctrl Pts',(39.50738071193,-28.63000002,-97.5282244682254));
#172889=CARTESIAN_POINT('Ctrl Pts',(39.5219120167722,-28.63000002,-97.3483295034422));
#172890=CARTESIAN_POINT('Ctrl Pts',(39.5366966813149,-28.63000002,-97.1652979907098));
#172891=CARTESIAN_POINT('Ctrl Pts',(39.5588835421168,-28.63000002,-96.9831066045011));
#172892=CARTESIAN_POINT('Ctrl Pts',(39.5882836977189,-28.63000002,-96.8026267328142));
#172893=CARTESIAN_POINT('Ctrl Pts',(39.6119618388167,-28.63000002,-96.6572728127554));
#172894=CARTESIAN_POINT('Ctrl Pts',(39.6403197974462,-28.63000002,-96.5130286888779));
#172895=CARTESIAN_POINT('Ctrl Pts',(39.6732827765156,-28.63000002,-96.3703554408507));
#172896=CARTESIAN_POINT('Ctrl Pts',(39.7499154654027,-28.63000002,-96.0386671366604));
#172897=CARTESIAN_POINT('Ctrl Pts',(39.8508333618868,-28.63000002,-95.7143394136881));
#172898=CARTESIAN_POINT('Ctrl Pts',(39.9781561959403,-28.63000002,-95.3980147135159));
#172899=CARTESIAN_POINT('Ctrl Pts',(40.0404386993088,-28.63000002,-95.2432781782316));
#172900=CARTESIAN_POINT('Ctrl Pts',(40.1090402739364,-28.63000002,-95.0904568779001));
#172901=CARTESIAN_POINT('Ctrl Pts',(40.1842134716234,-28.63000002,-94.9396273673639));
#172902=CARTESIAN_POINT('Origin',(39.5,-28.13000002,-55.24995));
#172903=CARTESIAN_POINT('',(39.5,-28.63000002,-134.169022080262));
#172904=CARTESIAN_POINT('Origin',(39.5,-28.13000002,-134.169022080262));
#172905=CARTESIAN_POINT('',(39.5,-28.63000002,-55.24995));
#172906=CARTESIAN_POINT('Ctrl Pts',(39.,-28.13000002,-134.169022080262));
#172907=CARTESIAN_POINT('Ctrl Pts',(39.,-28.63000002,-134.169022080263));
#172908=CARTESIAN_POINT('Ctrl Pts',(39.5,-28.63000002,-134.169022080262));
#172909=CARTESIAN_POINT('Ctrl Pts',(39.,-28.1032444606982,-134.720208320017));
#172910=CARTESIAN_POINT('Ctrl Pts',(38.9725065924499,-28.63000002,-134.735408648257));
#172911=CARTESIAN_POINT('Ctrl Pts',(39.500000002646,-28.63000002,-134.681913680777));
#172912=CARTESIAN_POINT('Ctrl Pts',(39.0642137165569,-28.076417661445,-135.260142317137));
#172913=CARTESIAN_POINT('Ctrl Pts',(39.0091060618314,-28.6300000199999,
-135.282961361938));
#172914=CARTESIAN_POINT('Ctrl Pts',(39.5577923442835,-28.63000002,-135.185082649765));
#172915=CARTESIAN_POINT('Ctrl Pts',(39.3159560341664,-28.0228058044255,
-136.318039323049));
#172916=CARTESIAN_POINT('Ctrl Pts',(39.1926311399543,-28.63000002,-136.37231025087));
#172917=CARTESIAN_POINT('Ctrl Pts',(39.7843604313674,-28.63000002,-136.172328627912));
#172918=CARTESIAN_POINT('Ctrl Pts',(39.5060247583741,-27.995814073424,-136.839791694484));
#172919=CARTESIAN_POINT('Ctrl Pts',(39.3499007457719,-28.63000002,-136.920217264961));
#172920=CARTESIAN_POINT('Ctrl Pts',(39.9554204749436,-28.63000002,-136.659959223536));
#172921=CARTESIAN_POINT('Ctrl Pts',(39.7602371906926,-27.9700232578782,
-137.330324735012));
#172922=CARTESIAN_POINT('Ctrl Pts',(39.5607615517247,-28.63000002,-137.429743088812));
#172923=CARTESIAN_POINT('Ctrl Pts',(40.1842134716234,-28.63000002,-137.119015604142));
#172924=CARTESIAN_POINT('',(40.1842134716234,-28.63000002,-137.119015604142));
#172925=CARTESIAN_POINT('Ctrl Pts',(40.1842134716234,-28.63000002,-137.119015604142));
#172926=CARTESIAN_POINT('Ctrl Pts',(40.0632593004047,-28.63000002,-136.87632992622));
#172927=CARTESIAN_POINT('Ctrl Pts',(39.9584937855372,-28.63000002,-136.62577590122));
#172928=CARTESIAN_POINT('Ctrl Pts',(39.8698562579301,-28.63000002,-136.370603923319));
#172929=CARTESIAN_POINT('Ctrl Pts',(39.790754739042,-28.63000002,-136.142884450827));
#172930=CARTESIAN_POINT('Ctrl Pts',(39.7244982953545,-28.63000002,-135.91148583538));
#172931=CARTESIAN_POINT('Ctrl Pts',(39.6710763875084,-28.63000002,-135.678705638911));
#172932=CARTESIAN_POINT('Ctrl Pts',(39.5896852679394,-28.63000002,-135.324052621675));
#172933=CARTESIAN_POINT('Ctrl Pts',(39.5369428910349,-28.63000002,-134.964508495217));
#172934=CARTESIAN_POINT('Ctrl Pts',(39.5136924175149,-28.63000002,-134.599929291455));
#172935=CARTESIAN_POINT('Ctrl Pts',(39.5045817727589,-28.63000002,-134.457069766118));
#172936=CARTESIAN_POINT('Ctrl Pts',(39.5,-28.63000002,-134.313437038192));
#172937=CARTESIAN_POINT('Ctrl Pts',(39.5,-28.63000002,-134.169022080262));
#172938=CARTESIAN_POINT('Origin',(40.1842134716235,-28.13000002,-137.119015604142));
#172939=CARTESIAN_POINT('Ctrl Pts',(56.8814116147779,-28.63000002,-171.255207540975));
#172940=CARTESIAN_POINT('Ctrl Pts',(56.3101888392034,-28.6300000199993,
-171.530874113378));
#172941=CARTESIAN_POINT('Ctrl Pts',(56.4435504331081,-28.0132665904809,
-171.466515117848));
#172942=CARTESIAN_POINT('Ctrl Pts',(54.1272610644231,-28.63000002,-165.548193876387));
#172943=CARTESIAN_POINT('Ctrl Pts',(53.5308515392379,-28.6300000202216,
-165.788070495429));
#172944=CARTESIAN_POINT('Ctrl Pts',(53.6908080796597,-28.0079900448831,
-165.759504469858));
#172945=CARTESIAN_POINT('Ctrl Pts',(51.3626815512523,-28.63000002,-159.846279798555));
#172946=CARTESIAN_POINT('Ctrl Pts',(50.7518430064623,-28.63000002,-160.075814652758));
#172947=CARTESIAN_POINT('Ctrl Pts',(50.9279125759463,-28.0020195102152,
-160.05758849772));
#172948=CARTESIAN_POINT('Ctrl Pts',(45.8000159539871,-28.63000002,-148.458842597754));
#172949=CARTESIAN_POINT('Ctrl Pts',(45.1718093453638,-28.63000002,-148.698490742611));
#172950=CARTESIAN_POINT('Ctrl Pts',(45.3696439177297,-27.9879328369328,
-148.670151070157));
#172951=CARTESIAN_POINT('Ctrl Pts',(43.002293156202,-28.63000002,-142.773138192163));
#172952=CARTESIAN_POINT('Ctrl Pts',(42.350918422607,-28.6300000199999,-142.994193600403));
#172953=CARTESIAN_POINT('Ctrl Pts',(42.5746173757444,-27.9798324917395,
-142.984453134689));
#172954=CARTESIAN_POINT('Ctrl Pts',(40.1755504430153,-28.63000002,-137.101634098975));
#172955=CARTESIAN_POINT('Ctrl Pts',(39.552039110073,-28.63000002,-137.412399462834));
#172956=CARTESIAN_POINT('Ctrl Pts',(39.7515900663067,-27.9699781154354,
-137.31294095905));
#172957=CARTESIAN_POINT('',(56.8729709358987,-28.63000002,-171.237717270032));
#172958=CARTESIAN_POINT('Ctrl Pts',(56.8729709358987,-28.63000002,-171.237717270032));
#172959=CARTESIAN_POINT('Ctrl Pts',(54.1216123272523,-28.63000002,-165.536543461238));
#172960=CARTESIAN_POINT('Ctrl Pts',(51.3598402340142,-28.63000002,-159.840463284682));
#172961=CARTESIAN_POINT('Ctrl Pts',(48.5813487526192,-28.63000002,-154.152561198155));
#172962=CARTESIAN_POINT('Ctrl Pts',(45.8028572712242,-28.63000002,-148.464659111628));
#172963=CARTESIAN_POINT('Ctrl Pts',(43.0080103715946,-28.63000002,-142.784757083568));
#172964=CARTESIAN_POINT('Ctrl Pts',(40.1842134716234,-28.63000002,-137.119015604142));
#172965=CARTESIAN_POINT('Origin',(56.8729709358987,-28.13000002,-171.237717270032));
#172966=CARTESIAN_POINT('Ctrl Pts',(57.017028950725,-28.6300000098418,-171.937510237498));
#172967=CARTESIAN_POINT('Ctrl Pts',(56.3674234002834,-28.6301310958619,
-171.9078715334));
#172968=CARTESIAN_POINT('Ctrl Pts',(56.5341822214496,-28.0016231613287,
-171.915549358366));
#172969=CARTESIAN_POINT('Ctrl Pts',(57.0288581213358,-28.6300000098265,
-171.673675468004));
#172970=CARTESIAN_POINT('Ctrl Pts',(56.3722793953451,-28.6301314641988,
-171.762633256231));
#172971=CARTESIAN_POINT('Ctrl Pts',(56.5423215389878,-28.0006714526254,
-171.739685194435));
#172972=CARTESIAN_POINT('Ctrl Pts',(56.9695606031425,-28.6300000099035,
-171.413737441436));
#172973=CARTESIAN_POINT('Ctrl Pts',(56.3485431365402,-28.6301296243106,
-171.621528645649));
#172974=CARTESIAN_POINT('Ctrl Pts',(56.5015214234675,-28.0054385079109,
-171.56638157453));
#172975=CARTESIAN_POINT('Ctrl Pts',(56.8427717751314,-28.6300000100697,
-171.178320644756));
#172976=CARTESIAN_POINT('Ctrl Pts',(56.2873571642799,-28.6301257916421,
-171.477955081174));
#172977=CARTESIAN_POINT('Ctrl Pts',(56.4142663415167,-28.0157208016423,
-171.409463522487));
#172978=CARTESIAN_POINT('',(57.0184057454332,-28.63000002,-171.871644662643));
#172979=CARTESIAN_POINT('Origin',(55.5771425537374,-28.6300004042113,-171.848433761036));
#172980=CARTESIAN_POINT('Origin',(57.0184057454332,-28.13000002,-171.871644662643));
#172981=CARTESIAN_POINT('Origin',(57.0184057454332,-28.13000002,-179.64995));
#172982=CARTESIAN_POINT('',(57.0184057454332,-28.63000002,-171.871644662643));
#172983=CARTESIAN_POINT('',(56.5351989170821,-28.0015042572884,-179.64995));
#172984=CARTESIAN_POINT('Origin',(57.,-29.13000002,-174.34995));
#172985=CARTESIAN_POINT('',(59.5,-28.63000002,-174.34995));
#172986=CARTESIAN_POINT('Origin',(57.,-28.63000002,-174.34995));
#172987=CARTESIAN_POINT('Origin',(59.5,-29.13000002,-174.34995));
#172988=CARTESIAN_POINT('Origin',(59.5,-29.13000002,-55.24995));
#172989=CARTESIAN_POINT('',(59.5,-28.63000002,-58.24995));
#172990=CARTESIAN_POINT('',(59.5,-28.63000002,-174.34995));
#172991=CARTESIAN_POINT('Origin',(59.5,-29.13000002,-58.24995));
#172992=CARTESIAN_POINT('Ctrl Pts',(40.1842134716234,-28.63000002,-94.9396273673639));
#172993=CARTESIAN_POINT('Ctrl Pts',(39.5607615517246,-28.6300000199999,
-94.628899882694));
#172994=CARTESIAN_POINT('Ctrl Pts',(39.7602371906926,-27.9700232578782,
-94.7283182364936));
#172995=CARTESIAN_POINT('Ctrl Pts',(42.9880924510224,-28.63000002,-89.3138497353063));
#172996=CARTESIAN_POINT('Ctrl Pts',(42.3373257946448,-28.63000002,-89.0914456452771));
#172997=CARTESIAN_POINT('Ctrl Pts',(42.5604321400969,-27.9797945689722,
-89.1025347299149));
#172998=CARTESIAN_POINT('Ctrl Pts',(45.7634210292322,-28.63000002,-83.6741003095587));
#172999=CARTESIAN_POINT('Ctrl Pts',(45.1354691768678,-28.630000020022,-83.4336169877673));
#173000=CARTESIAN_POINT('Ctrl Pts',(45.3330806261701,-27.9878402480233,
-83.4627911786917));
#173001=CARTESIAN_POINT('Ctrl Pts',(51.2816902902029,-28.63000002,-72.3787631830378));
#173002=CARTESIAN_POINT('Ctrl Pts',(50.6710028559025,-28.6300000199784,
-72.148355955617));
#173003=CARTESIAN_POINT('Ctrl Pts',(50.8469740031289,-28.0018438144725,
-72.1674540521641));
#173004=CARTESIAN_POINT('Ctrl Pts',(54.0242786911866,-28.63000002,-66.7229996739341));
#173005=CARTESIAN_POINT('Ctrl Pts',(53.4278489247074,-28.6300000200659,
-66.4825194498726));
#173006=CARTESIAN_POINT('Ctrl Pts',(53.5878832423525,-28.0077864042225,
-66.5116884426403));
#173007=CARTESIAN_POINT('Ctrl Pts',(56.7565335485771,-28.63000002,-61.0621827299711));
#173008=CARTESIAN_POINT('Ctrl Pts',(56.1850547298497,-28.63000002,-60.7863522634768));
#173009=CARTESIAN_POINT('Ctrl Pts',(56.3187331343194,-28.0130417005584,
-60.8508735991007));
#173010=CARTESIAN_POINT('',(56.3187331343194,-28.0130417005584,-60.8508735991007));
#173011=CARTESIAN_POINT('Ctrl Pts',(56.3187331343194,-28.0130417005584,
-60.8508735991007));
#173012=CARTESIAN_POINT('Ctrl Pts',(55.4206729151416,-28.0113134574357,
-62.7124744999959));
#173013=CARTESIAN_POINT('Ctrl Pts',(54.5407043741536,-28.0095946269229,
-64.5337352621368));
#173014=CARTESIAN_POINT('Ctrl Pts',(53.6787898395932,-28.0078255152441,
-66.3146356201485));
#173015=CARTESIAN_POINT('Ctrl Pts',(53.1318515029365,-28.0067029039408,
-67.4447275730113));
#173016=CARTESIAN_POINT('Ctrl Pts',(52.5921839629517,-28.0055600958576,
-68.5585681337777));
#173017=CARTESIAN_POINT('Ctrl Pts',(52.0597872155532,-28.0043823157945,
-69.6561569895613));
#173018=CARTESIAN_POINT('Ctrl Pts',(51.3740895455159,-28.0028653999812,
-71.0697909472201));
#173019=CARTESIAN_POINT('Ctrl Pts',(50.7004503528809,-28.0012983267211,
-72.4564656700406));
#173020=CARTESIAN_POINT('Ctrl Pts',(50.0388732398342,-27.9996975550347,
-73.8161848482626));
#173021=CARTESIAN_POINT('Ctrl Pts',(49.7080846833108,-27.9988971691915,
-74.4960444373736));
#173022=CARTESIAN_POINT('Ctrl Pts',(49.3803117753967,-27.9980888638163,
-75.1691652377898));
#173023=CARTESIAN_POINT('Ctrl Pts',(49.055555577712,-27.9972777309138,-75.8355482397257));
#173024=CARTESIAN_POINT('Ctrl Pts',(48.8931774788696,-27.9968721644625,
-76.1687397406936));
#173025=CARTESIAN_POINT('Ctrl Pts',(48.7315535703334,-27.9964658957672,
-76.5002467983552));
#173026=CARTESIAN_POINT('Ctrl Pts',(48.5706840017103,-27.996059781108,-76.8300695637573));
#173027=CARTESIAN_POINT('Ctrl Pts',(48.4902492173988,-27.9958567237784,
-76.9949809464584));
#173028=CARTESIAN_POINT('Ctrl Pts',(48.410003018773,-27.9956537052356,-77.1594712564479));
#173029=CARTESIAN_POINT('Ctrl Pts',(48.3299454270974,-27.9954508395193,
-77.3235405144964));
#173030=CARTESIAN_POINT('Ctrl Pts',(48.2899166312597,-27.9953494066612,
-77.4055751435206));
#173031=CARTESIAN_POINT('Ctrl Pts',(48.2499349872017,-27.9952480120268,
-77.4875045095808));
#173032=CARTESIAN_POINT('Ctrl Pts',(48.210000497641,-27.9951466706255,-77.569328615371));
#173033=CARTESIAN_POINT('Ctrl Pts',(48.1750578192753,-27.9950579968994,
-77.6409247079375));
#173034=CARTESIAN_POINT('Ctrl Pts',(48.1401512435743,-27.9949693639309,
-77.7124402106111));
#173035=CARTESIAN_POINT('Ctrl Pts',(48.1052807723934,-27.994880782046,-77.7838751252387));
#173036=CARTESIAN_POINT('Ctrl Pts',(48.1002992765105,-27.9948681274911,
-77.7940801130427));
#173037=CARTESIAN_POINT('Ctrl Pts',(48.0962023871856,-27.9948577195745,
-77.8024728272216));
#173038=CARTESIAN_POINT('Ctrl Pts',(48.0903384937855,-27.9948428272692,
-77.8144851539887));
#173039=CARTESIAN_POINT('Ctrl Pts',(48.0902347666554,-27.9948425638374,
-77.8146976415112));
#173040=CARTESIAN_POINT('Ctrl Pts',(48.0901310397955,-27.9948423004048,
-77.8149101284225));
#173041=CARTESIAN_POINT('Ctrl Pts',(48.0900273132056,-27.9948420369715,
-77.8151226147225));
#173042=CARTESIAN_POINT('Ctrl Pts',(47.3394787984715,-27.9929358768115,
-79.3526384730988));
#173043=CARTESIAN_POINT('Ctrl Pts',(46.6030922990866,-27.9909910456638,
-80.8581611087631));
#173044=CARTESIAN_POINT('Ctrl Pts',(45.8807954360895,-27.9890047060169,
-82.3316567645428));
#173045=CARTESIAN_POINT('Ctrl Pts',(45.1431757263836,-27.9869762280479,
-83.8364112409215));
#173046=CARTESIAN_POINT('Ctrl Pts',(44.4202500280405,-27.9849044756312,
-85.3077656006454));
#173047=CARTESIAN_POINT('Ctrl Pts',(43.7119916769706,-27.9827892726554,
-86.7457096119736));
#173048=CARTESIAN_POINT('Ctrl Pts',(42.9722991493508,-27.9805801919813,
-88.2474729709351));
#173049=CARTESIAN_POINT('Ctrl Pts',(42.2486049085613,-27.9783237247899,
-89.7127945630624));
#173050=CARTESIAN_POINT('Ctrl Pts',(41.5409305949263,-27.9760225982136,
-91.1416892705798));
#173051=CARTESIAN_POINT('Ctrl Pts',(40.9356314794565,-27.9740543624667,
-92.3638739477615));
#173052=CARTESIAN_POINT('Ctrl Pts',(40.3420535665444,-27.972053512525,-93.5594092747014));
#173053=CARTESIAN_POINT('Ctrl Pts',(39.7602371906927,-27.9700232578782,
-94.7283182364936));
#173054=CARTESIAN_POINT('',(56.7565335485771,-28.63000002,-61.0621827299711));
#173055=CARTESIAN_POINT('Origin',(56.7565335485771,-28.13000002,-61.0621827299711));
#173056=CARTESIAN_POINT('Ctrl Pts',(40.1842134716234,-28.63000002,-94.9396273673639));
#173057=CARTESIAN_POINT('Ctrl Pts',(42.9880935290232,-28.63000002,-89.3138475723767));
#173058=CARTESIAN_POINT('Ctrl Pts',(45.7634210292107,-28.63000002,-83.6741003095903));
#173059=CARTESIAN_POINT('Ctrl Pts',(48.5225556597151,-28.63000002,-78.0264317462971));
#173060=CARTESIAN_POINT('Ctrl Pts',(51.2816902902195,-28.63000002,-72.3787631830038));
#173061=CARTESIAN_POINT('Ctrl Pts',(54.0242783838037,-28.63000002,-66.7230003106817));
#173062=CARTESIAN_POINT('Ctrl Pts',(56.7565335485771,-28.63000002,-61.0621827299711));
#173063=CARTESIAN_POINT('Origin',(57.,-29.13000002,-58.24995));
#173064=CARTESIAN_POINT('',(57.,-28.63000002,-55.74995));
#173065=CARTESIAN_POINT('Origin',(57.,-28.63000002,-58.24995));
#173066=CARTESIAN_POINT('',(57.,-29.13000002,-55.24995));
#173067=CARTESIAN_POINT('Origin',(57.,-29.13000002,-55.74995));
#173068=CARTESIAN_POINT('Origin',(57.,-29.13000002,-58.24995));
#173069=CARTESIAN_POINT('Origin',(57.,-2.42462934179819E-14,-58.24995));
#173070=CARTESIAN_POINT('',(57.,-29.63000002,-55.24995));
#173071=CARTESIAN_POINT('',(57.,28.41999998,-55.24995));
#173072=CARTESIAN_POINT('Origin',(57.,-29.63000002,-58.24995));
#173073=CARTESIAN_POINT('Origin',(57.,-29.63000002,-58.24995));
#173074=CARTESIAN_POINT('',(57.,-30.13000002,-55.74995));
#173075=CARTESIAN_POINT('Origin',(57.,-29.63000002,-55.74995));
#173076=CARTESIAN_POINT('',(59.5,-30.13000002,-58.24995));
#173077=CARTESIAN_POINT('Origin',(57.,-30.13000002,-58.24995));
#173078=CARTESIAN_POINT('Origin',(59.5,-29.63000002,-58.24995));
#173079=CARTESIAN_POINT('Origin',(59.5,-29.63000002,-55.24995));
#173080=CARTESIAN_POINT('',(59.5,-30.13000002,-174.34995));
#173081=CARTESIAN_POINT('',(59.5,-30.13000002,-58.24995));
#173082=CARTESIAN_POINT('Origin',(59.5,-29.63000002,-174.34995));
#173083=CARTESIAN_POINT('Origin',(57.,-29.63000002,-174.34995));
#173084=CARTESIAN_POINT('',(57.,-30.13000002,-176.84995));
#173085=CARTESIAN_POINT('Origin',(57.,-30.13000002,-174.34995));
#173086=CARTESIAN_POINT('Origin',(57.,-29.63000002,-176.84995));
#173087=CARTESIAN_POINT('Origin',(-83.2809572255632,-29.6300000199999,-176.84995));
#173088=CARTESIAN_POINT('',(-83.2809572255632,-30.13000002,-176.84995));
#173089=CARTESIAN_POINT('Origin',(56.294192362543,-30.63000002,-179.64995));
#173090=CARTESIAN_POINT('',(56.294192362543,-30.13000002,-171.871644662643));
#173091=CARTESIAN_POINT('',(56.294192362543,-30.13000002,-176.84995));
#173092=CARTESIAN_POINT('Origin',(56.294192362543,-30.63000002,-171.871644662643));
#173093=CARTESIAN_POINT('',(55.8171229357418,-30.4803178166104,-179.64995));
#173094=CARTESIAN_POINT('Ctrl Pts',(56.1167176003611,-30.13000002714,-171.179145966886));
#173095=CARTESIAN_POINT('Ctrl Pts',(55.7825352402592,-30.1299356988045,
-171.361452749053));
#173096=CARTESIAN_POINT('Ctrl Pts',(55.6935671754689,-30.4968373543263,
-171.410008924779));
#173097=CARTESIAN_POINT('Ctrl Pts',(56.2430624746474,-30.1300000269106,
-171.410992898787));
#173098=CARTESIAN_POINT('Ctrl Pts',(55.8840206261747,-30.1299383387469,
-171.527291609574));
#173099=CARTESIAN_POINT('Ctrl Pts',(55.7814946229066,-30.4850537049709,
-171.564548662911));
#173100=CARTESIAN_POINT('Ctrl Pts',(56.3050537145651,-30.130000026799,-171.670900042786));
#173101=CARTESIAN_POINT('Ctrl Pts',(55.9360241189749,-30.1299395985436,
-171.722483207042));
#173102=CARTESIAN_POINT('Ctrl Pts',(55.8246219322658,-30.4793202225602,
-171.737832654878));
#173103=CARTESIAN_POINT('Ctrl Pts',(56.2927384034373,-30.1300000268212,
-171.93833459815));
#173104=CARTESIAN_POINT('Ctrl Pts',(55.925777764091,-30.1299393505852,-171.921245295793));
#173105=CARTESIAN_POINT('Ctrl Pts',(55.8160539307423,-30.4804600576221,
-171.916099630748));
#173106=CARTESIAN_POINT('',(56.1468816861249,-30.13000002,-171.237717270032));
#173107=CARTESIAN_POINT('Origin',(54.8146431261402,-30.1299997583389,-171.852158294305));
#173108=CARTESIAN_POINT('Origin',(56.146881686125,-30.63000002,-171.237717270032));
#173109=CARTESIAN_POINT('Ctrl Pts',(40.2651432342477,-30.13000002,-139.30435351063));
#173110=CARTESIAN_POINT('Ctrl Pts',(39.9609182162754,-30.1300000199999,
-139.459264328773));
#173111=CARTESIAN_POINT('Ctrl Pts',(39.850159149164,-30.447965242174,-139.5156626415));
#173112=CARTESIAN_POINT('Ctrl Pts',(42.9624569131523,-30.13000002,-144.601532315192));
#173113=CARTESIAN_POINT('Ctrl Pts',(42.6706800009636,-30.13000002,-144.798763083095));
#173114=CARTESIAN_POINT('Ctrl Pts',(42.5429900246349,-30.4581917776324,
-144.812847565038));
#173115=CARTESIAN_POINT('Ctrl Pts',(45.6258101137111,-30.13000002,-149.91560863326));
#173116=CARTESIAN_POINT('Ctrl Pts',(45.3221739986871,-30.1300000200307,
-150.105257848785));
#173117=CARTESIAN_POINT('Ctrl Pts',(45.2030035072277,-30.4667604203174,
-150.126917764117));
#173118=CARTESIAN_POINT('Ctrl Pts',(50.9129382266982,-30.13000002,-160.563437524381));
#173119=CARTESIAN_POINT('Ctrl Pts',(50.5978344679358,-30.1300000199689,
-160.757133407541));
#173120=CARTESIAN_POINT('Ctrl Pts',(50.484627394531,-30.4818027714,-160.774746655264));
#173121=CARTESIAN_POINT('Ctrl Pts',(53.53633422979,-30.13000002,-165.897383514726));
#173122=CARTESIAN_POINT('Ctrl Pts',(53.2127313470812,-30.1300000198871,
-166.08608254617));
#173123=CARTESIAN_POINT('Ctrl Pts',(53.105875183067,-30.4882648083968,-166.108694936931));
#173124=CARTESIAN_POINT('Ctrl Pts',(56.1468816861249,-30.13000002,-171.237717270032));
#173125=CARTESIAN_POINT('Ctrl Pts',(55.8070372118623,-30.13000002,-171.403845487572));
#173126=CARTESIAN_POINT('Ctrl Pts',(55.7146117108563,-30.4940179634924,
-171.449026400902));
#173127=CARTESIAN_POINT('',(40.2651432342477,-30.13000002,-139.30435351063));
#173128=CARTESIAN_POINT('Ctrl Pts',(40.2651432342477,-30.13000002,-139.30435351063));
#173129=CARTESIAN_POINT('Ctrl Pts',(42.96245845912,-30.13000002,-144.601535351275));
#173130=CARTESIAN_POINT('Ctrl Pts',(45.6258101137032,-30.13000002,-149.915608633243));
#173131=CARTESIAN_POINT('Ctrl Pts',(48.2693741701893,-30.13000002,-155.239523078828));
#173132=CARTESIAN_POINT('Ctrl Pts',(50.9129382266755,-30.13000002,-160.563437524412));
#173133=CARTESIAN_POINT('Ctrl Pts',(53.5363337714711,-30.13000002,-165.897382577172));
#173134=CARTESIAN_POINT('Ctrl Pts',(56.1468816861249,-30.13000002,-171.237717270032));
#173135=CARTESIAN_POINT('Origin',(40.2651432342477,-30.63000002,-139.30435351063));
#173136=CARTESIAN_POINT('Ctrl Pts',(39.850159149164,-30.447965242174,-139.5156626415));
#173137=CARTESIAN_POINT('Ctrl Pts',(39.9609182162754,-30.13000002,-139.459264328773));
#173138=CARTESIAN_POINT('Ctrl Pts',(40.2651432342477,-30.13000002,-139.30435351063));
#173139=CARTESIAN_POINT('Ctrl Pts',(39.5639348330521,-30.4769451657213,
-138.978519823589));
#173140=CARTESIAN_POINT('Ctrl Pts',(39.6630612728547,-30.13000002,-138.925676053694));
#173141=CARTESIAN_POINT('Ctrl Pts',(40.0075294671789,-30.13000002,-138.798433034953));
#173142=CARTESIAN_POINT('Ctrl Pts',(39.3557167999464,-30.5068849023477,
-138.41703103581));
#173143=CARTESIAN_POINT('Ctrl Pts',(39.4450625268456,-30.13000002,-138.37488926852));
#173144=CARTESIAN_POINT('Ctrl Pts',(39.8201451200256,-30.13000002,-138.270288236581));
#173145=CARTESIAN_POINT('Ctrl Pts',(39.0729048436467,-30.5680016657979,
-137.252632910085));
#173146=CARTESIAN_POINT('Ctrl Pts',(39.1248051359359,-30.13000002,-137.23047141255));
#173147=CARTESIAN_POINT('Ctrl Pts',(39.5656143592083,-30.13000002,-137.176619865119));
#173148=CARTESIAN_POINT('Ctrl Pts',(39.,-30.5993710675033,-136.645762741564));
#173149=CARTESIAN_POINT('Ctrl Pts',(39.0297176446585,-30.13000002,-136.627803193949));
#173150=CARTESIAN_POINT('Ctrl Pts',(39.5000000014551,-30.13000002,-136.607413315277));
#173151=CARTESIAN_POINT('Ctrl Pts',(39.,-30.63000002,-136.04214564125));
#173152=CARTESIAN_POINT('Ctrl Pts',(39.,-30.13000002,-136.04214564125));
#173153=CARTESIAN_POINT('Ctrl Pts',(39.5,-30.13000002,-136.04214564125));
#173154=CARTESIAN_POINT('',(39.5,-30.13000002,-136.04214564125));
#173155=CARTESIAN_POINT('Ctrl Pts',(39.5,-30.13000002,-136.04214564125));
#173156=CARTESIAN_POINT('Ctrl Pts',(39.5,-30.13000002,-136.325718326755));
#173157=CARTESIAN_POINT('Ctrl Pts',(39.5162728499327,-30.13000002,-136.608122039194));
#173158=CARTESIAN_POINT('Ctrl Pts',(39.5808560770791,-30.13000002,-137.170628022919));
#173159=CARTESIAN_POINT('Ctrl Pts',(39.6292470494507,-30.13000002,-137.450036957971));
#173160=CARTESIAN_POINT('Ctrl Pts',(39.8201451199495,-30.13000002,-138.270288236609));
#173161=CARTESIAN_POINT('Ctrl Pts',(40.0074751366267,-30.13000002,-138.798326348879));
#173162=CARTESIAN_POINT('Ctrl Pts',(40.2651432342477,-30.13000002,-139.30435351063));
#173163=CARTESIAN_POINT('Origin',(39.5,-30.63000002,-136.04214564125));
#173164=CARTESIAN_POINT('Origin',(39.5,-30.63000002,-55.24995));
#173165=CARTESIAN_POINT('',(39.5,-30.13000002,-96.0164973302555));
#173166=CARTESIAN_POINT('',(39.5,-30.13000002,-55.24995));
#173167=CARTESIAN_POINT('Origin',(39.5,-30.63000002,-96.0164973302555));
#173168=CARTESIAN_POINT('Ctrl Pts',(39.,-30.63000002,-96.0164973302555));
#173169=CARTESIAN_POINT('Ctrl Pts',(39.,-30.13000002,-96.0164973302554));
#173170=CARTESIAN_POINT('Ctrl Pts',(39.5,-30.13000002,-96.0164973302555));
#173171=CARTESIAN_POINT('Ctrl Pts',(39.,-30.599243623439,-95.4103686640728));
#173172=CARTESIAN_POINT('Ctrl Pts',(39.0298365376099,-30.1300000199999,
-95.4284967516594));
#173173=CARTESIAN_POINT('Ctrl Pts',(39.5000000024932,-30.13000002,-95.4488679082906));
#173174=CARTESIAN_POINT('Ctrl Pts',(39.0712857711311,-30.5685553796042,
-94.8166771620692));
#173175=CARTESIAN_POINT('Ctrl Pts',(39.1227981005945,-30.13000002,-94.8386739331622));
#173176=CARTESIAN_POINT('Ctrl Pts',(39.5641571932953,-30.13000002,-94.8920319207365));
#173177=CARTESIAN_POINT('Ctrl Pts',(39.3518132725282,-30.5075286049387,
-93.6537603297063));
#173178=CARTESIAN_POINT('Ctrl Pts',(39.4408759042576,-30.13000002,-93.6956127800614));
#173179=CARTESIAN_POINT('Ctrl Pts',(39.8166319459981,-30.13000002,-93.7997753189033));
#173180=CARTESIAN_POINT('Ctrl Pts',(39.5639528617268,-30.4769433431446,
-93.080089311988));
#173181=CARTESIAN_POINT('Ctrl Pts',(39.6631053450898,-30.13000002,-93.1328879562182));
#173182=CARTESIAN_POINT('Ctrl Pts',(40.0075545499357,-30.13000002,-93.260160670532));
#173183=CARTESIAN_POINT('Ctrl Pts',(39.850159149164,-30.447965242174,-92.5429803300057));
#173184=CARTESIAN_POINT('Ctrl Pts',(39.9609182162754,-30.13000002,-92.5993786427328));
#173185=CARTESIAN_POINT('Ctrl Pts',(40.2651432342477,-30.13000002,-92.7542894608761));
#173186=CARTESIAN_POINT('',(40.2651432342477,-30.13000002,-92.754289460876));
#173187=CARTESIAN_POINT('',(39.8501336363284,-30.4479678253472,-92.5430282091296));
#173188=CARTESIAN_POINT('Origin',(40.2651432342477,-30.63000002,-92.754289460876));
#173189=CARTESIAN_POINT('Ctrl Pts',(39.,-30.63000002,-96.0164973302555));
#173190=CARTESIAN_POINT('Ctrl Pts',(39.,-30.6249052535773,-95.9160927210813));
#173191=CARTESIAN_POINT('Ctrl Pts',(39.0019517748916,-30.6195721960509,
-95.8112962237002));
#173192=CARTESIAN_POINT('Ctrl Pts',(39.0064236822507,-30.614000333733,-95.7021746191804));
#173193=CARTESIAN_POINT('Ctrl Pts',(39.0102527558462,-30.6092294229861,
-95.6087391740764));
#173194=CARTESIAN_POINT('Ctrl Pts',(39.0159309893287,-30.6042831282349,
-95.5121269654206));
#173195=CARTESIAN_POINT('Ctrl Pts',(39.0238420499257,-30.5991629267857,
-95.4124159301744));
#173196=CARTESIAN_POINT('Ctrl Pts',(39.0276963700442,-30.5966683313754,
-95.363836066012));
#173197=CARTESIAN_POINT('Ctrl Pts',(39.0320810493253,-30.5941324656576,
-95.3145208290036));
#173198=CARTESIAN_POINT('Ctrl Pts',(39.037041991603,-30.5915556817932,-95.2644827119115));
#173199=CARTESIAN_POINT('Ctrl Pts',(39.041382816096,-30.5893009959119,-95.220699359456));
#173200=CARTESIAN_POINT('Ctrl Pts',(39.0461648739216,-30.5870149782656,
-95.1763624788107));
#173201=CARTESIAN_POINT('Ctrl Pts',(39.0514193421249,-30.5846979430726,
-95.1314819004068));
#173202=CARTESIAN_POINT('Ctrl Pts',(39.0514662876117,-30.5846772417683,
-95.1310809196571));
#173203=CARTESIAN_POINT('Ctrl Pts',(39.0515142285028,-30.5846561156216,
-95.1306717143191));
#173204=CARTESIAN_POINT('Ctrl Pts',(39.0515634188643,-30.5846344546871,
-95.1302521554465));
#173205=CARTESIAN_POINT('Ctrl Pts',(39.0518641291921,-30.5845020371465,
-95.127687309768));
#173206=CARTESIAN_POINT('Ctrl Pts',(39.0522050961516,-30.5843525639836,
-95.1247923237199));
#173207=CARTESIAN_POINT('Ctrl Pts',(39.0525159392357,-30.5842169296647,
-95.1221655723487));
#173208=CARTESIAN_POINT('Ctrl Pts',(39.0526833331722,-30.5841438884304,
-95.1207510250266));
#173209=CARTESIAN_POINT('Ctrl Pts',(39.0528419432779,-30.5840748603693,
-95.1194142571582));
#173210=CARTESIAN_POINT('Ctrl Pts',(39.0529804943758,-30.5840146697563,
-95.1182486665959));
#173211=CARTESIAN_POINT('Ctrl Pts',(39.0530440420663,-30.5839870627975,
-95.1177140581416));
#173212=CARTESIAN_POINT('Ctrl Pts',(39.0531033676915,-30.5839613149507,
-95.117215459505));
#173213=CARTESIAN_POINT('Ctrl Pts',(39.0531573748585,-30.5839378916815,
-95.1167618808849));
#173214=CARTESIAN_POINT('Ctrl Pts',(39.0531858824795,-30.5839255277358,
-95.1165224599322));
#173215=CARTESIAN_POINT('Ctrl Pts',(39.0532129081873,-30.5839138114741,
-95.1162955826442));
#173216=CARTESIAN_POINT('Ctrl Pts',(39.0532382904984,-30.5839028113527,
-95.1160825741236));
#173217=CARTESIAN_POINT('Ctrl Pts',(39.0532602675523,-30.583893286993,-95.1158981425439));
#173218=CARTESIAN_POINT('Ctrl Pts',(39.0532810893944,-30.5838842660806,
-95.1157234607359));
#173219=CARTESIAN_POINT('Ctrl Pts',(39.0533023391604,-30.5838750624374,
-95.1155452413819));
#173220=CARTESIAN_POINT('Ctrl Pts',(39.0592332600412,-30.5813062774663,
-95.0658032871499));
#173221=CARTESIAN_POINT('Ctrl Pts',(39.0662052340743,-30.5784987766604,
-95.011508413269));
#173222=CARTESIAN_POINT('Ctrl Pts',(39.0745203401635,-30.5754521822375,
-94.9526940905704));
#173223=CARTESIAN_POINT('Ctrl Pts',(39.0825579442499,-30.5725072625311,
-94.8958425921788));
#173224=CARTESIAN_POINT('Ctrl Pts',(39.0918507976603,-30.5693389401508,
-94.8347683127649));
#173225=CARTESIAN_POINT('Ctrl Pts',(39.1027173036832,-30.5659470513343,
-94.7695096773549));
#173226=CARTESIAN_POINT('Ctrl Pts',(39.1141365869548,-30.5623826177307,
-94.7009313466487));
#173227=CARTESIAN_POINT('Ctrl Pts',(39.1272940640147,-30.5585711624585,
-94.6277296646441));
#173228=CARTESIAN_POINT('Ctrl Pts',(39.1426044136615,-30.5545146082183,
-94.5499943643404));
#173229=CARTESIAN_POINT('Ctrl Pts',(39.1579147633082,-30.5504580539782,
-94.4722590640368));
#173230=CARTESIAN_POINT('Ctrl Pts',(39.1753792515526,-30.5461561819419,
-94.389986077742));
#173231=CARTESIAN_POINT('Ctrl Pts',(39.1954540957825,-30.5416127257937,
-94.303302840083));
#173232=CARTESIAN_POINT('Ctrl Pts',(39.1991593872304,-30.5407741225639,
-94.2873033804859));
#173233=CARTESIAN_POINT('Ctrl Pts',(39.2027413140868,-30.5399744287283,
-94.2720525195795));
#173234=CARTESIAN_POINT('Ctrl Pts',(39.2066491849319,-30.5391142739385,
-94.2556556609144));
#173235=CARTESIAN_POINT('Ctrl Pts',(39.2082189913868,-30.5387687465158,
-94.2490689809567));
#173236=CARTESIAN_POINT('Ctrl Pts',(39.2098419385736,-30.5384134641158,
-94.2422974725426));
#173237=CARTESIAN_POINT('Ctrl Pts',(39.2115495219815,-30.5380419914382,
-94.2352187459229));
#173238=CARTESIAN_POINT('Ctrl Pts',(39.2116381806325,-30.5380227043765,
-94.2348512146211));
#173239=CARTESIAN_POINT('Ctrl Pts',(39.2117270689434,-30.5380033735724,
-94.2344828534231));
#173240=CARTESIAN_POINT('Ctrl Pts',(39.211816191455,-30.5379839981243,-94.2341136452022));
#173241=CARTESIAN_POINT('Ctrl Pts',(39.2303698501946,-30.533950388163,-94.1572513215619));
#173242=CARTESIAN_POINT('Ctrl Pts',(39.2491858444372,-30.5301075162906,
-94.0846500822156));
#173243=CARTESIAN_POINT('Ctrl Pts',(39.2678896114286,-30.5264770887774,
-94.0162910979177));
#173244=CARTESIAN_POINT('Ctrl Pts',(39.2871262661881,-30.5227432269981,
-93.9459845023932));
#173245=CARTESIAN_POINT('Ctrl Pts',(39.3062439542278,-30.5192340377043,
-93.8801647140279));
#173246=CARTESIAN_POINT('Ctrl Pts',(39.3248813010155,-30.5159694653193,
-93.818780919685));
#173247=CARTESIAN_POINT('Ctrl Pts',(39.3356188989651,-30.5140886361355,
-93.7834156656183));
#173248=CARTESIAN_POINT('Ctrl Pts',(39.3461979255374,-30.5122889392155,
-93.7495223469786));
#173249=CARTESIAN_POINT('Ctrl Pts',(39.3565563938204,-30.5105737630814,
-93.7170880835705));
#173250=CARTESIAN_POINT('Ctrl Pts',(39.3748703165573,-30.5075413067044,
-93.6597438336436));
#173251=CARTESIAN_POINT('Ctrl Pts',(39.3924929457479,-30.5047638464613,
-93.6069649458907));
#173252=CARTESIAN_POINT('Ctrl Pts',(39.4091261367344,-30.5022275366221,
-93.5586840765167));
#173253=CARTESIAN_POINT('Ctrl Pts',(39.4132999564277,-30.5015910923004,
-93.5465688038931));
#173254=CARTESIAN_POINT('Ctrl Pts',(39.4174117270447,-30.5009698324755,
-93.5347367182726));
#173255=CARTESIAN_POINT('Ctrl Pts',(39.4214572463548,-30.500363538649,-93.523186689646));
#173256=CARTESIAN_POINT('Ctrl Pts',(39.4315409550048,-30.4988523135543,
-93.4943975244871));
#173257=CARTESIAN_POINT('Ctrl Pts',(39.4412125697053,-30.4974336004572,
-93.4673609360235));
#173258=CARTESIAN_POINT('Ctrl Pts',(39.4504127978213,-30.4961019998094,
-93.442060190349));
#173259=CARTESIAN_POINT('Ctrl Pts',(39.4550129118793,-30.4954361994855,
-93.4294098175118));
#173260=CARTESIAN_POINT('Ctrl Pts',(39.459495280608,-30.4947922073451,-93.4171934409355));
#173261=CARTESIAN_POINT('Ctrl Pts',(39.4638532593191,-30.4941692342306,
-93.4054090017087));
#173262=CARTESIAN_POINT('Ctrl Pts',(39.4660322486747,-30.4938577476734,
-93.3995167820953));
#173263=CARTESIAN_POINT('Ctrl Pts',(39.4681801470372,-30.493551517769,-93.3937325490637));
#173264=CARTESIAN_POINT('Ctrl Pts',(39.4702961652564,-30.4932504519151,
-93.3880560566882));
#173265=CARTESIAN_POINT('Ctrl Pts',(39.471354174366,-30.4930999189882,-93.3852178105004));
#173266=CARTESIAN_POINT('Ctrl Pts',(39.4724042138444,-30.4929506771965,
-93.3824064996216));
#173267=CARTESIAN_POINT('Ctrl Pts',(39.473446187943,-30.4928027147915,-93.3796220936597));
#173268=CARTESIAN_POINT('Ctrl Pts',(39.4739671749922,-30.492728733589,-93.3782298906788));
#173269=CARTESIAN_POINT('Ctrl Pts',(39.4744861457219,-30.4926550722409,
-93.3768444139362));
#173270=CARTESIAN_POINT('Ctrl Pts',(39.4750030883437,-30.4925817292688,
-93.3754656596573));
#173271=CARTESIAN_POINT('Ctrl Pts',(39.4755200309655,-30.4925083862968,
-93.3740869053783));
#173272=CARTESIAN_POINT('Ctrl Pts',(39.4756022368881,-30.4924967046419,
-93.3738667780565));
#173273=CARTESIAN_POINT('Ctrl Pts',(39.4765478202071,-30.4923626540173,
-93.3713495604645));
#173274=CARTESIAN_POINT('Ctrl Pts',(39.5126025370099,-30.4872513568841,
-93.2753690523553));
#173275=CARTESIAN_POINT('Ctrl Pts',(39.549431291156,-30.4823498708368,-93.1835388191733));
#173276=CARTESIAN_POINT('Ctrl Pts',(39.5866068526539,-30.4776588176486,
-93.095820174658));
#173277=CARTESIAN_POINT('Ctrl Pts',(39.6248843739199,-30.4728287120379,
-93.0055013698956));
#173278=CARTESIAN_POINT('Ctrl Pts',(39.6635293745984,-30.4682216676362,
-92.9195409504136));
#173279=CARTESIAN_POINT('Ctrl Pts',(39.7021109540059,-30.4638355826243,
-92.8378531504812));
#173280=CARTESIAN_POINT('Ctrl Pts',(39.7422060023605,-30.4592774413211,
-92.7529609211173));
#173281=CARTESIAN_POINT('Ctrl Pts',(39.7822322739401,-30.4549579016675,
-92.672682491943));
#173282=CARTESIAN_POINT('Ctrl Pts',(39.8217476739595,-30.4508721484859,
-92.5968843423184));
#173283=CARTESIAN_POINT('Ctrl Pts',(39.8312408753335,-30.4498905849006,
-92.5786745532789));
#173284=CARTESIAN_POINT('Ctrl Pts',(39.8407047841214,-30.4489225049938,
-92.5607232068311));
#173285=CARTESIAN_POINT('Ctrl Pts',(39.8501336363284,-30.4479678253472,
-92.5430282091296));
#173286=CARTESIAN_POINT('Ctrl Pts',(40.2651432342476,-30.13000002,-92.7542894608761));
#173287=CARTESIAN_POINT('Ctrl Pts',(40.149768118957,-30.13000002,-92.9808714190862));
#173288=CARTESIAN_POINT('Ctrl Pts',(40.0478331438219,-30.13000002,-93.2140840893024));
#173289=CARTESIAN_POINT('Ctrl Pts',(39.9590875376241,-30.13000002,-93.45156448926));
#173290=CARTESIAN_POINT('Ctrl Pts',(39.8658509560192,-30.13000002,-93.7010625955762));
#173291=CARTESIAN_POINT('Ctrl Pts',(39.7871721235837,-30.13000002,-93.9552726783295));
#173292=CARTESIAN_POINT('Ctrl Pts',(39.7228113496721,-30.13000002,-94.2114776823655));
#173293=CARTESIAN_POINT('Ctrl Pts',(39.7115691395802,-30.13000002,-94.2562302592369));
#173294=CARTESIAN_POINT('Ctrl Pts',(39.700763918709,-30.13000002,-94.3010437266484));
#173295=CARTESIAN_POINT('Ctrl Pts',(39.6903945692724,-30.13000002,-94.3459036197334));
#173296=CARTESIAN_POINT('Ctrl Pts',(39.6046719082244,-30.13000002,-94.7167571079952));
#173297=CARTESIAN_POINT('Ctrl Pts',(39.5475807634106,-30.13000002,-95.0925075650471));
#173298=CARTESIAN_POINT('Ctrl Pts',(39.5197593574037,-30.13000002,-95.4732641712651));
#173299=CARTESIAN_POINT('Ctrl Pts',(39.5066102516738,-30.13000002,-95.6532194499914));
#173300=CARTESIAN_POINT('Ctrl Pts',(39.5000000000002,-30.13000002,-95.8342931017866));
#173301=CARTESIAN_POINT('Ctrl Pts',(39.5,-30.13000002,-96.0164973302555));
#173302=CARTESIAN_POINT('Ctrl Pts',(56.0289353856639,-30.13000002,-61.0621827299711));
#173303=CARTESIAN_POINT('Ctrl Pts',(55.6892944482707,-30.13000002,-60.8961225062558));
#173304=CARTESIAN_POINT('Ctrl Pts',(55.5967474138374,-30.4937575588533,
-60.8508735991007));
#173305=CARTESIAN_POINT('Ctrl Pts',(53.4376477846732,-30.13000002,-66.3621114555649));
#173306=CARTESIAN_POINT('Ctrl Pts',(53.1140955473737,-30.1300000200305,
-66.1737552088486));
#173307=CARTESIAN_POINT('Ctrl Pts',(53.0072677069205,-30.4880260434848,
-66.1508000801069));
#173308=CARTESIAN_POINT('Ctrl Pts',(50.8336218773704,-30.13000002,-71.655706365272));
#173309=CARTESIAN_POINT('Ctrl Pts',(50.518482898395,-30.13000002,-71.4624685012804));
#173310=CARTESIAN_POINT('Ctrl Pts',(50.405384759569,-30.4815921581836,-71.4443972343972));
#173311=CARTESIAN_POINT('Ctrl Pts',(45.5856873606873,-30.13000002,-82.223056081386));
#173312=CARTESIAN_POINT('Ctrl Pts',(45.2819556815256,-30.13000002,-82.0338364947541));
#173313=CARTESIAN_POINT('Ctrl Pts',(45.1629315870884,-30.4666308723541,
-82.01174695052));
#173314=CARTESIAN_POINT('Ctrl Pts',(42.94214612644,-30.13000002,-87.4969984415611));
#173315=CARTESIAN_POINT('Ctrl Pts',(42.650123001142,-30.13000002,-87.3003867975457));
#173316=CARTESIAN_POINT('Ctrl Pts',(42.5227129344255,-30.4581147715466,
-87.2856833539494));
#173317=CARTESIAN_POINT('Ctrl Pts',(40.2651432342477,-30.13000002,-92.7542894608761));
#173318=CARTESIAN_POINT('Ctrl Pts',(39.9609182162754,-30.13000002,-92.5993786427328));
#173319=CARTESIAN_POINT('Ctrl Pts',(39.850159149164,-30.447965242174,-92.5429803300057));
#173320=CARTESIAN_POINT('',(56.0289353856639,-30.13000002,-61.0621827299711));
#173321=CARTESIAN_POINT('',(55.5967474138374,-30.4937575588533,-60.8508735991007));
#173322=CARTESIAN_POINT('Origin',(56.0289353856639,-30.63000002,-61.0621827299711));
#173323=CARTESIAN_POINT('Ctrl Pts',(39.850159149164,-30.447965242174,-92.5429803300057));
#173324=CARTESIAN_POINT('Ctrl Pts',(40.4919890794513,-30.4504027129368,
-91.2804087139596));
#173325=CARTESIAN_POINT('Ctrl Pts',(41.1472641150672,-30.452803979004,-89.9867515631817));
#173326=CARTESIAN_POINT('Ctrl Pts',(41.8159279844008,-30.4551647590928,
-88.6619683163481));
#173327=CARTESIAN_POINT('Ctrl Pts',(42.4652749676593,-30.4574573391156,
-87.3754564465499));
#173328=CARTESIAN_POINT('Ctrl Pts',(43.1272482893852,-30.4597117299785,
-86.0595906033186));
#173329=CARTESIAN_POINT('Ctrl Pts',(43.8018380914677,-30.461925824762,-84.7143559757826));
#173330=CARTESIAN_POINT('Ctrl Pts',(44.4532739805521,-30.4640639252777,
-83.4152937710014));
#173331=CARTESIAN_POINT('Ctrl Pts',(45.1164743748462,-30.4661644409739,
-82.0888454883916));
#173332=CARTESIAN_POINT('Ctrl Pts',(45.7914697121484,-30.4682272829623,
-80.7350244407743));
#173333=CARTESIAN_POINT('Ctrl Pts',(46.4393888922545,-30.4702073779584,
-79.4355093556948));
#173334=CARTESIAN_POINT('Ctrl Pts',(47.0981756635805,-30.4721527594818,
-78.1107735479491));
#173335=CARTESIAN_POINT('Ctrl Pts',(47.7678960568131,-30.4740650926897,
-76.7608514488592));
#173336=CARTESIAN_POINT('Ctrl Pts',(47.7732963461685,-30.4740805127856,
-76.7499663541003));
#173337=CARTESIAN_POINT('Ctrl Pts',(47.7794480652732,-30.4740980732275,
-76.7375663802255));
#173338=CARTESIAN_POINT('Ctrl Pts',(47.7841581747548,-30.4741115104162,
-76.7280720931668));
#173339=CARTESIAN_POINT('Ctrl Pts',(47.7842851392984,-30.4741118726257,
-76.7278161675185));
#173340=CARTESIAN_POINT('Ctrl Pts',(47.7844110563643,-30.47411223184,-76.727562353186));
#173341=CARTESIAN_POINT('Ctrl Pts',(47.7845358830013,-30.4741125879365,
-76.7273107367533));
#173342=CARTESIAN_POINT('Ctrl Pts',(48.5628078545631,-30.4763327867105,
-75.1585268464595));
#173343=CARTESIAN_POINT('Ctrl Pts',(49.3583939950128,-30.4785153611757,
-73.5505206630954));
#173344=CARTESIAN_POINT('Ctrl Pts',(50.1712495695924,-30.4806565898269,
-71.9032649192444));
#173345=CARTESIAN_POINT('Ctrl Pts',(50.962904574651,-30.4827419718206,-70.2989722318186));
#173346=CARTESIAN_POINT('Ctrl Pts',(51.7709397108168,-30.484788125207,-68.6574505523832));
#173347=CARTESIAN_POINT('Ctrl Pts',(52.5953571041642,-30.4867937041832,
-66.9786972374972));
#173348=CARTESIAN_POINT('Ctrl Pts',(53.3928114301762,-30.4887336894912,
-65.3548485607644));
#173349=CARTESIAN_POINT('Ctrl Pts',(54.2055938276031,-30.4906357043452,
-63.6961637244116));
#173350=CARTESIAN_POINT('Ctrl Pts',(55.033749835842,-30.4925006401861,-62.0026629615056));
#173351=CARTESIAN_POINT('Ctrl Pts',(55.2206323562122,-30.4929214834896,
-61.6205058707253));
#173352=CARTESIAN_POINT('Ctrl Pts',(55.408297930604,-30.4933404476046,-61.2365759484398));
#173353=CARTESIAN_POINT('Ctrl Pts',(55.5967474138374,-30.4937575588533,
-60.8508735991007));
#173354=CARTESIAN_POINT('Ctrl Pts',(56.0289353856639,-30.13000002,-61.0621827299711));
#173355=CARTESIAN_POINT('Ctrl Pts',(53.4376473376604,-30.13000002,-66.3621123698348));
#173356=CARTESIAN_POINT('Ctrl Pts',(50.8336218773754,-30.13000002,-71.6557063652599));
#173357=CARTESIAN_POINT('Ctrl Pts',(48.2096546190284,-30.13000002,-76.9393812233288));
#173358=CARTESIAN_POINT('Ctrl Pts',(45.5856873606815,-30.13000002,-82.2230560813977));
#173359=CARTESIAN_POINT('Ctrl Pts',(42.9421476228591,-30.13000002,-87.4969955027855));
#173360=CARTESIAN_POINT('Ctrl Pts',(40.2651432342477,-30.13000002,-92.754289460876));
#173361=CARTESIAN_POINT('Ctrl Pts',(40.0751063884513,-36.0938884806558,
-86.6376094090262));
#173362=CARTESIAN_POINT('Ctrl Pts',(39.,-37.0899493132599,-87.566881951549));
#173363=CARTESIAN_POINT('Ctrl Pts',(39.,-38.3588510099497,-88.7507007177297));
#173364=CARTESIAN_POINT('Ctrl Pts',(40.0284942066422,-34.9676073874133,
-87.9314164096932));
#173365=CARTESIAN_POINT('Ctrl Pts',(38.9999999999938,-35.9377762186182,
-88.8634929468774));
#173366=CARTESIAN_POINT('Ctrl Pts',(39.,-37.1517824539261,-90.044523203833));
#173367=CARTESIAN_POINT('Ctrl Pts',(39.9811083568879,-33.8078923846355,
-89.2002134624161));
#173368=CARTESIAN_POINT('Ctrl Pts',(39.,-34.7456425298457,-90.138609363953));
#173369=CARTESIAN_POINT('Ctrl Pts',(39.,-35.9043080884012,-91.3133047711639));
#173370=CARTESIAN_POINT('Ctrl Pts',(39.8860349814824,-31.4034505542693,
-91.6586472348866));
#173371=CARTESIAN_POINT('Ctrl Pts',(39.,-32.2660375633753,-92.6092802152048));
#173372=CARTESIAN_POINT('Ctrl Pts',(39.,-33.3065376953223,-93.7717385435459));
#173373=CARTESIAN_POINT('Ctrl Pts',(39.8388209456929,-30.1709967638591,
-92.8359193626927));
#173374=CARTESIAN_POINT('Ctrl Pts',(39.,-30.9915371636578,-93.792984660173));
#173375=CARTESIAN_POINT('Ctrl Pts',(39.,-31.9694828580011,-94.9490286570666));
#173376=CARTESIAN_POINT('Ctrl Pts',(39.7930043023957,-28.8965637205256,
-93.942810661998));
#173377=CARTESIAN_POINT('Ctrl Pts',(39.,-29.6660656545474,-94.9083553778138));
#173378=CARTESIAN_POINT('Ctrl Pts',(39.,-30.5806160716777,-96.0559019707015));
#173379=CARTESIAN_POINT('',(40.0734472026555,-36.0537916247009,-86.6836434020945));
#173380=CARTESIAN_POINT('Ctrl Pts',(40.0734472049734,-36.0537916894494,
-86.683643483585));
#173381=CARTESIAN_POINT('Ctrl Pts',(40.0582294002964,-35.6859715947434,
-87.1056818970377));
#173382=CARTESIAN_POINT('Ctrl Pts',(40.0431653813165,-35.3202583628105,
-87.5185158963228));
#173383=CARTESIAN_POINT('Ctrl Pts',(40.0282656000844,-34.9562785737579,
-87.9223716670628));
#173384=CARTESIAN_POINT('Ctrl Pts',(40.0116226499473,-34.5497157265767,
-88.3734757034434));
#173385=CARTESIAN_POINT('Ctrl Pts',(39.9951846492463,-34.1453161855968,
-88.8133780401699));
#173386=CARTESIAN_POINT('Ctrl Pts',(39.9789600467457,-33.7425726182128,
-89.2424636967788));
#173387=CARTESIAN_POINT('Ctrl Pts',(39.9636394913162,-33.3622702257363,
-89.6476403774287));
#173388=CARTESIAN_POINT('Ctrl Pts',(39.9485091110465,-32.9834450563986,
-90.0431738242611));
#173389=CARTESIAN_POINT('Ctrl Pts',(39.9335716691851,-32.6056714694524,
-90.4294303486514));
#173390=CARTESIAN_POINT('Ctrl Pts',(39.9155227303514,-32.1492069404469,
-90.8961448267766));
#173391=CARTESIAN_POINT('Ctrl Pts',(39.897824098653,-31.6960435093008,-91.347532590367));
#173392=CARTESIAN_POINT('Ctrl Pts',(39.8804902707974,-31.2451213065669,
-91.7842587747131));
#173393=CARTESIAN_POINT('Ctrl Pts',(39.8702497189193,-30.9787235871182,
-92.0422697105862));
#173394=CARTESIAN_POINT('Ctrl Pts',(39.8601363016365,-30.713108867239,-92.2951643300845));
#173395=CARTESIAN_POINT('Ctrl Pts',(39.8501516349846,-30.4480624604452,
-92.5430839616816));
#173396=CARTESIAN_POINT('Ctrl Pts',(40.0734472049734,-36.0537916894494,
-86.683643483585));
#173397=CARTESIAN_POINT('Ctrl Pts',(40.0245584466381,-36.0584545847703,
-86.7694976519593));
#173398=CARTESIAN_POINT('Ctrl Pts',(39.9757226962818,-36.0633262985487,
-86.8593752483436));
#173399=CARTESIAN_POINT('Ctrl Pts',(39.927286973467,-36.0684348005888,-86.9533520768013));
#173400=CARTESIAN_POINT('Ctrl Pts',(39.8951777242464,-36.0718213540584,
-87.0156516612927));
#173401=CARTESIAN_POINT('Ctrl Pts',(39.8632450041024,-36.0753114008984,
-87.0797523342764));
#173402=CARTESIAN_POINT('Ctrl Pts',(39.8315977698661,-36.0789050638006,
-87.1456702267159));
#173403=CARTESIAN_POINT('Ctrl Pts',(39.7919047583749,-36.0834123550793,
-87.2283466351038));
#173404=CARTESIAN_POINT('Ctrl Pts',(39.7526605370814,-36.0880833296136,
-87.3138822668377));
#173405=CARTESIAN_POINT('Ctrl Pts',(39.714092383476,-36.0929016857489,-87.402296181153));
#173406=CARTESIAN_POINT('Ctrl Pts',(39.6948083066732,-36.0953108638166,
-87.4465031383107));
#173407=CARTESIAN_POINT('Ctrl Pts',(39.6756934496369,-36.0977565857494,
-87.4914294306899));
#173408=CARTESIAN_POINT('Ctrl Pts',(39.6567773264731,-36.1002348892133,
-87.5370759143626));
#173409=CARTESIAN_POINT('Ctrl Pts',(39.6473192648912,-36.1014740409452,
-87.559899156199));
#173410=CARTESIAN_POINT('Ctrl Pts',(39.6379108833219,-36.1027213366419,
-87.5829024445171));
#173411=CARTESIAN_POINT('Ctrl Pts',(39.6285559461866,-36.1039761301367,
-87.6060857648908));
#173412=CARTESIAN_POINT('Ctrl Pts',(39.6238784776189,-36.1046035268841,
-87.6176774250777));
#173413=CARTESIAN_POINT('Ctrl Pts',(39.61921436983,-36.1052327979438,-87.6293140931487));
#173414=CARTESIAN_POINT('Ctrl Pts',(39.614564094214,-36.1058638576854,-87.6409957632537));
#173415=CARTESIAN_POINT('Ctrl Pts',(39.612238956406,-36.1061793875562,-87.6468365983062));
#173416=CARTESIAN_POINT('Ctrl Pts',(39.6099172766201,-36.1064953645889,
-87.6526886838591));
#173417=CARTESIAN_POINT('Ctrl Pts',(39.6075991140024,-36.1068117775199,
-87.6585520187252));
#173418=CARTESIAN_POINT('Ctrl Pts',(39.6052809513847,-36.1071281904509,
-87.6644153535913));
#173419=CARTESIAN_POINT('Ctrl Pts',(39.6022185548814,-36.1075476937166,
-87.6721943105456));
#173420=CARTESIAN_POINT('Ctrl Pts',(39.6006552368152,-36.1077623125535,
-87.6761757699178));
#173421=CARTESIAN_POINT('Ctrl Pts',(39.5779632105313,-36.1108775687474,
-87.7339678358275));
#173422=CARTESIAN_POINT('Ctrl Pts',(39.5542205394167,-36.1141975364057,
-87.7964178534076));
#173423=CARTESIAN_POINT('Ctrl Pts',(39.5297328530949,-36.1177665535606,
-87.8636089002945));
#173424=CARTESIAN_POINT('Ctrl Pts',(39.5056031226127,-36.1212833995746,
-87.9298177626136));
#173425=CARTESIAN_POINT('Ctrl Pts',(39.4807501012066,-36.1250425564943,
-88.000630514969));
#173426=CARTESIAN_POINT('Ctrl Pts',(39.4555131835107,-36.1290706613253,
-88.0761190496449));
#173427=CARTESIAN_POINT('Ctrl Pts',(39.4308618377357,-36.1330053020847,
-88.1498560246892));
#173428=CARTESIAN_POINT('Ctrl Pts',(39.4058444701722,-36.1371969955752,
-88.2280547461139));
#173429=CARTESIAN_POINT('Ctrl Pts',(39.3808197403438,-36.141648612017,-88.3107684439465));
#173430=CARTESIAN_POINT('Ctrl Pts',(39.3714871748443,-36.1433087698811,
-88.3416151706854));
#173431=CARTESIAN_POINT('Ctrl Pts',(39.3621539945362,-36.1450048212813,
-88.3730896656766));
#173432=CARTESIAN_POINT('Ctrl Pts',(39.352840229561,-36.1467359139454,-88.4051939925927));
#173433=CARTESIAN_POINT('Ctrl Pts',(39.3385398145363,-36.1493938448261,
-88.4544871839289));
#173434=CARTESIAN_POINT('Ctrl Pts',(39.3242849868855,-36.1521345745536,
-88.5052653310622));
#173435=CARTESIAN_POINT('Ctrl Pts',(39.3101516172692,-36.1549520365536,
-88.5575337102131));
#173436=CARTESIAN_POINT('Ctrl Pts',(39.3030849324611,-36.1563607675536,
-88.5836678997886));
#173437=CARTESIAN_POINT('Ctrl Pts',(39.2960486439358,-36.1577886899918,
-88.6101746554091));
#173438=CARTESIAN_POINT('Ctrl Pts',(39.2890526314425,-36.1592345959982,
-88.6370542948565));
#173439=CARTESIAN_POINT('Ctrl Pts',(39.2855546251958,-36.1599575490013,
-88.6504941145803));
#173440=CARTESIAN_POINT('Ctrl Pts',(39.2820666894481,-36.1606849983143,
-88.6640271556613));
#173441=CARTESIAN_POINT('Ctrl Pts',(39.2785900750634,-36.1614167794284,
-88.6776534472724));
#173442=CARTESIAN_POINT('Ctrl Pts',(39.276851767871,-36.1617826699853,-88.684466593078));
#173443=CARTESIAN_POINT('Ctrl Pts',(39.2751162911093,-36.1621496435148,
-88.6913030515374));
#173444=CARTESIAN_POINT('Ctrl Pts',(39.2733838024279,-36.1625176778282,
-88.6981628250376));
#173445=CARTESIAN_POINT('Ctrl Pts',(39.2725175580872,-36.1627016949849,
-88.7015927117877));
#173446=CARTESIAN_POINT('Ctrl Pts',(39.2716520607718,-36.1628859773388,
-88.7050284272993));
#173447=CARTESIAN_POINT('Ctrl Pts',(39.2707873302702,-36.1630705220061,
-88.7084699717845));
#173448=CARTESIAN_POINT('Ctrl Pts',(39.2699225997686,-36.1632550666735,
-88.7119115162696));
#173449=CARTESIAN_POINT('Ctrl Pts',(39.2693983359119,-36.1633670415458,
-88.713999895811));
#173450=CARTESIAN_POINT('Ctrl Pts',(39.2681954590309,-36.1636249400336,
-88.7188120923488));
#173451=CARTESIAN_POINT('Ctrl Pts',(39.248398147037,-36.167869511449,-88.7980126803225));
#173452=CARTESIAN_POINT('Ctrl Pts',(39.2307677419702,-36.171950025859,-88.8731714624208));
#173453=CARTESIAN_POINT('Ctrl Pts',(39.2149695096784,-36.1758143575034,
-88.9441946157667));
#173454=CARTESIAN_POINT('Ctrl Pts',(39.1988652605947,-36.1797535424828,
-89.0165935102169));
#173455=CARTESIAN_POINT('Ctrl Pts',(39.1846644603266,-36.1834685416629,
-89.0846953678492));
#173456=CARTESIAN_POINT('Ctrl Pts',(39.1720493682215,-36.1869310591102,
-89.1484303377924));
#173457=CARTESIAN_POINT('Ctrl Pts',(39.1591222702079,-36.1904792141329,
-89.2137416487592));
#173458=CARTESIAN_POINT('Ctrl Pts',(39.1478599448633,-36.1937626900379,
-89.2744677490584));
#173459=CARTESIAN_POINT('Ctrl Pts',(39.1379644992164,-36.1967721114012,
-89.3305586607797));
#173460=CARTESIAN_POINT('Ctrl Pts',(39.127964529343,-36.1998133208668,-89.3872420530587));
#173461=CARTESIAN_POINT('Ctrl Pts',(39.1193603137208,-36.2025751137754,
-89.4391922114424));
#173462=CARTESIAN_POINT('Ctrl Pts',(39.11189245695,-36.2050620666782,-89.4863771085259));
#173463=CARTESIAN_POINT('Ctrl Pts',(39.104334359811,-36.2075790715159,-89.5341321802417));
#173464=CARTESIAN_POINT('Ctrl Pts',(39.0979401478849,-36.2098149531853,
-89.5770064754588));
#173465=CARTESIAN_POINT('Ctrl Pts',(39.0924918051001,-36.211782447031,-89.6149810792825));
#173466=CARTESIAN_POINT('Ctrl Pts',(39.089202610369,-36.2129702339684,-89.6379065580461));
#173467=CARTESIAN_POINT('Ctrl Pts',(39.0862591379092,-36.2140603258838,
-89.6590465409137));
#173468=CARTESIAN_POINT('Ctrl Pts',(39.0836224115253,-36.2150560549564,
-89.6783985960165));
#173469=CARTESIAN_POINT('Ctrl Pts',(39.0796481868764,-36.2165568747034,
-89.7075671191007));
#173470=CARTESIAN_POINT('Ctrl Pts',(39.0763692393887,-36.2178434340386,
-89.732673665977));
#173471=CARTESIAN_POINT('Ctrl Pts',(39.0736808720347,-36.2189267619753,
-89.7537135766213));
#173472=CARTESIAN_POINT('Ctrl Pts',(39.0723366883577,-36.2194684259437,
-89.7642335319435));
#173473=CARTESIAN_POINT('Ctrl Pts',(39.0711406879357,-36.2199592627485,
-89.7737368858829));
#173474=CARTESIAN_POINT('Ctrl Pts',(39.0700829940987,-36.2204004509078,
-89.782223326275));
#173475=CARTESIAN_POINT('Ctrl Pts',(39.0695541471802,-36.2206210449875,
-89.7864665464711));
#173476=CARTESIAN_POINT('Ctrl Pts',(39.0690599092086,-36.2208292307969,
-89.790455542088));
#173477=CARTESIAN_POINT('Ctrl Pts',(39.068599245928,-36.221025129606,-89.7941902836961));
#173478=CARTESIAN_POINT('Ctrl Pts',(39.0683689142878,-36.2211230790106,
-89.7960576545002));
#173479=CARTESIAN_POINT('Ctrl Pts',(39.0681469783199,-36.2212179569089,
-89.7978614620406));
#173480=CARTESIAN_POINT('Ctrl Pts',(39.0679333209832,-36.2213097782944,
-89.7996017034629));
#173481=CARTESIAN_POINT('Ctrl Pts',(39.0678264923148,-36.2213556889871,
-89.8004718241741));
#173482=CARTESIAN_POINT('Ctrl Pts',(39.067721733429,-36.2214008355664,-89.8013260533702));
#173483=CARTESIAN_POINT('Ctrl Pts',(39.0676190304694,-36.221445219821,-89.80216439073));
#173484=CARTESIAN_POINT('Ctrl Pts',(39.0675676789896,-36.2214674119482,
-89.8025835594099));
#173485=CARTESIAN_POINT('Ctrl Pts',(39.0675168415914,-36.221489413483,-89.8029987551334));
#173486=CARTESIAN_POINT('Ctrl Pts',(39.067466758021,-36.2215111314003,-89.8034079910735));
#173487=CARTESIAN_POINT('Ctrl Pts',(39.0674166744505,-36.2215328493176,
-89.8038172270136));
#173488=CARTESIAN_POINT('Ctrl Pts',(39.0673667213199,-36.2215544886427,
-89.8042244740143));
#173489=CARTESIAN_POINT('Ctrl Pts',(39.0671690648645,-36.2216404734312,
-89.805843073341));
#173490=CARTESIAN_POINT('Ctrl Pts',(39.0535618414146,-36.2275599068601,
-89.9172719799453));
#173491=CARTESIAN_POINT('Ctrl Pts',(39.0424392254192,-36.2333308081245,
-90.0254583105046));
#173492=CARTESIAN_POINT('Ctrl Pts',(39.0334327685362,-36.2389072191113,
-90.1302828991747));
#173493=CARTESIAN_POINT('Ctrl Pts',(39.0242321778508,-36.2446038294043,
-90.237366977481));
#173494=CARTESIAN_POINT('Ctrl Pts',(39.01723947308,-36.2500978354871,-90.340943088193));
#173495=CARTESIAN_POINT('Ctrl Pts',(39.0120825306864,-36.2553769973198,
-90.4409205822943));
#173496=CARTESIAN_POINT('Ctrl Pts',(39.0067454951592,-36.26084052049,-90.5443895368034));
#173497=CARTESIAN_POINT('Ctrl Pts',(39.0033742127362,-36.266074288559,-90.6440043974332));
#173498=CARTESIAN_POINT('Ctrl Pts',(39.0015855904073,-36.2710982035765,
-90.7396993298735));
#173499=CARTESIAN_POINT('Ctrl Pts',(39.0005031226411,-36.27413865878,-90.7976135569795));
#173500=CARTESIAN_POINT('Ctrl Pts',(39.0000009314936,-36.2771028717565,
-90.8540927106737));
#173501=CARTESIAN_POINT('Ctrl Pts',(39.0000000012937,-36.28000002,-90.9091273827666));
#173502=CARTESIAN_POINT('Origin',(57.,-37.28000002,-174.34995));
#173503=CARTESIAN_POINT('',(57.,-36.78000002,-176.84995));
#173504=CARTESIAN_POINT('Origin',(57.,-37.28000002,-176.84995));
#173505=CARTESIAN_POINT('',(59.5,-36.78000002,-174.34995));
#173506=CARTESIAN_POINT('Origin',(57.,-36.78000002,-174.34995));
#173507=CARTESIAN_POINT('Origin',(59.5,-37.28000002,-174.34995));
#173508=CARTESIAN_POINT('Origin',(59.5,-37.28000002,-55.24995));
#173509=CARTESIAN_POINT('',(59.5,-36.78000002,-58.24995));
#173510=CARTESIAN_POINT('',(59.5,-36.78000002,-174.34995));
#173511=CARTESIAN_POINT('Origin',(59.5,-37.28000002,-58.24995));
#173512=CARTESIAN_POINT('Ctrl Pts',(40.4661024946855,-36.78000002,-86.8949524600738));
#173513=CARTESIAN_POINT('Ctrl Pts',(39.7490326214953,-36.78000002,-86.5090582163831));
#173514=CARTESIAN_POINT('Ctrl Pts',(40.0734472163172,-36.0537915241817,
-86.6836433292035));
#173515=CARTESIAN_POINT('Ctrl Pts',(42.7671781583824,-36.78000002,-82.6190865682492));
#173516=CARTESIAN_POINT('Ctrl Pts',(42.0251435460116,-36.78000002,-82.3205925927599));
#173517=CARTESIAN_POINT('Ctrl Pts',(42.3689613408276,-36.0634493712886,
-82.407773086856));
#173518=CARTESIAN_POINT('Ctrl Pts',(45.0306161020287,-36.78000002,-78.3240684577782));
#173519=CARTESIAN_POINT('Ctrl Pts',(44.3122026972581,-36.7800000199999,
-78.0178858717772));
#173520=CARTESIAN_POINT('Ctrl Pts',(44.6279666698635,-36.0719269202766,
-78.1127593269182));
#173521=CARTESIAN_POINT('Ctrl Pts',(49.5095281828678,-36.78000002,-69.7096607994621));
#173522=CARTESIAN_POINT('Ctrl Pts',(48.8138634148613,-36.78000002,-69.420066134471));
#173523=CARTESIAN_POINT('Ctrl Pts',(49.0993449617391,-36.0872029629615,
-69.4983516685814));
#173524=CARTESIAN_POINT('Ctrl Pts',(51.7247198970815,-36.78000002,-65.3901198450985));
#173525=CARTESIAN_POINT('Ctrl Pts',(51.0452850559209,-36.7800000200001,
-65.0958859597511));
#173526=CARTESIAN_POINT('Ctrl Pts',(51.3114450013405,-36.0939978375791,
-65.1788088209436));
#173527=CARTESIAN_POINT('Ctrl Pts',(53.9233979868778,-36.78000002,-61.0621827299711));
#173528=CARTESIAN_POINT('Ctrl Pts',(53.2738374538033,-36.7800000199999,
-60.7321930665019));
#173529=CARTESIAN_POINT('Ctrl Pts',(53.5074514076768,-36.1001753985996,
-60.8508735991007));
#173530=CARTESIAN_POINT('',(53.5074514076768,-36.1001753985996,-60.8508735991007));
#173531=CARTESIAN_POINT('',(53.9233979868778,-36.78000002,-61.0621827299711));
#173532=CARTESIAN_POINT('Origin',(53.9233979868778,-36.28000002,-61.0621827299711));
#173533=CARTESIAN_POINT('',(40.4661024946855,-36.78000002,-86.8949524600738));
#173534=CARTESIAN_POINT('Ctrl Pts',(40.4661024946855,-36.78000002,-86.8949524600738));
#173535=CARTESIAN_POINT('Ctrl Pts',(42.7668758174593,-36.78000002,-82.6196483790844));
#173536=CARTESIAN_POINT('Ctrl Pts',(45.0302107640621,-36.78000002,-78.3248411901957));
#173537=CARTESIAN_POINT('Ctrl Pts',(47.2696870908413,-36.78000002,-74.0176051177503));
#173538=CARTESIAN_POINT('Ctrl Pts',(49.5091634176204,-36.78000002,-69.7103690453049));
#173539=CARTESIAN_POINT('Ctrl Pts',(51.7244980141576,-36.78000002,-65.3905566052077));
#173540=CARTESIAN_POINT('Ctrl Pts',(53.9233979868778,-36.78000002,-61.0621827299711));
#173541=CARTESIAN_POINT('Origin',(40.4661024946855,-36.28000002,-86.8949524600738));
#173542=CARTESIAN_POINT('Ctrl Pts',(53.5074514076768,-36.1001753985996,
-60.8508735991007));
#173543=CARTESIAN_POINT('Ctrl Pts',(52.7922585244569,-36.0981634975119,
-62.2603906482166));
#173544=CARTESIAN_POINT('Ctrl Pts',(52.087761822413,-36.0961532083163,-63.6445356363279));
#173545=CARTESIAN_POINT('Ctrl Pts',(51.3939147382574,-36.0941045783538,
-65.0032879478635));
#173546=CARTESIAN_POINT('Ctrl Pts',(50.9587608446394,-36.0928197573533,
-65.8554445286564));
#173547=CARTESIAN_POINT('Ctrl Pts',(50.5277967496853,-36.0915198832934,
-66.6976138903416));
#173548=CARTESIAN_POINT('Ctrl Pts',(50.101020147517,-36.0901953772584,-67.5297957986045));
#173549=CARTESIAN_POINT('Ctrl Pts',(49.547387044142,-36.0884771706303,-68.6093382339287));
#173550=CARTESIAN_POINT('Ctrl Pts',(49.0007983189538,-36.0867228439177,
-69.6720723858452));
#173551=CARTESIAN_POINT('Ctrl Pts',(48.461251821417,-36.0849437847744,-70.718001906085));
#173552=CARTESIAN_POINT('Ctrl Pts',(48.1914785726486,-36.0840542552027,
-71.240966666205));
#173553=CARTESIAN_POINT('Ctrl Pts',(47.9234660064517,-36.0831588800052,
-71.7597303678619));
#173554=CARTESIAN_POINT('Ctrl Pts',(47.6572144784549,-36.0822610994337,
-72.2742940187899));
#173555=CARTESIAN_POINT('Ctrl Pts',(47.5240887144565,-36.081812209148,-72.531575844254));
#173556=CARTESIAN_POINT('Ctrl Pts',(47.391403221895,-36.0813627242012,-72.7878076633787));
#173557=CARTESIAN_POINT('Ctrl Pts',(47.2591580668236,-36.0809132157062,
-73.0429896319059));
#173558=CARTESIAN_POINT('Ctrl Pts',(47.193035489288,-36.0806884614586,-73.1705806161696));
#173559=CARTESIAN_POINT('Ctrl Pts',(47.1270229967962,-36.0804637017278,
-73.2979091381477));
#173560=CARTESIAN_POINT('Ctrl Pts',(47.0611206002298,-36.0802390131329,
-73.4249752193029));
#173561=CARTESIAN_POINT('Ctrl Pts',(46.9993371034487,-36.0800283675751,
-73.5440996703859));
#173562=CARTESIAN_POINT('Ctrl Pts',(46.937650370691,-36.0798177845541,-73.6629934606037));
#173563=CARTESIAN_POINT('Ctrl Pts',(46.876060411837,-36.0796073308672,-73.7816566085978));
#173564=CARTESIAN_POINT('Ctrl Pts',(46.8719544145801,-36.0795933006214,
-73.7895674851308));
#173565=CARTESIAN_POINT('Ctrl Pts',(46.8684113527144,-36.0795811932909,
-73.7963936317983));
#173566=CARTESIAN_POINT('Ctrl Pts',(46.8637437084935,-36.0795652467564,
-73.8053861619924));
#173567=CARTESIAN_POINT('Ctrl Pts',(46.8637144102822,-36.079565146662,-73.8054426069651));
#173568=CARTESIAN_POINT('Ctrl Pts',(46.8636851120899,-36.0795650465676,
-73.8054990518909));
#173569=CARTESIAN_POINT('Ctrl Pts',(46.8636558139168,-36.0795649464731,
-73.80555549677));
#173570=CARTESIAN_POINT('Ctrl Pts',(46.2429826651902,-36.0774444738694,
-75.0013235981928));
#173571=CARTESIAN_POINT('Ctrl Pts',(45.6309093168581,-36.0752947306591,
-76.1761119836538));
#173572=CARTESIAN_POINT('Ctrl Pts',(45.0273544360468,-36.0731155201471,
-77.3298876420855));
#173573=CARTESIAN_POINT('Ctrl Pts',(44.4120213549676,-36.0708937829675,
-78.506178901337));
#173574=CARTESIAN_POINT('Ctrl Pts',(43.8055426292206,-36.0686414218454,
-79.6606294077665));
#173575=CARTESIAN_POINT('Ctrl Pts',(43.2078811739115,-36.066359429761,-80.7932300885606));
#173576=CARTESIAN_POINT('Ctrl Pts',(42.5897731390426,-36.0639993685084,
-81.9645781400002));
#173577=CARTESIAN_POINT('Ctrl Pts',(41.9810960802422,-36.0616076169725,
-83.1125558332997));
#173578=CARTESIAN_POINT('Ctrl Pts',(41.3818591117218,-36.0591864926988,
-84.2371795897531));
#173579=CARTESIAN_POINT('Ctrl Pts',(40.9405953429784,-36.0574036347014,
-85.0653256208907));
#173580=CARTESIAN_POINT('Ctrl Pts',(40.5044515400523,-36.0556048756295,
-85.8808085557189));
#173581=CARTESIAN_POINT('Ctrl Pts',(40.0734472163172,-36.0537915241817,
-86.6836433292035));
#173582=CARTESIAN_POINT('Ctrl Pts',(40.1309220332522,-36.0483277296961,
-86.5845687421098));
#173583=CARTESIAN_POINT('Ctrl Pts',(39.7968669198671,-36.7800000199995,
-86.3981771484168));
#173584=CARTESIAN_POINT('Ctrl Pts',(40.5178020946704,-36.78000002,-86.8005666302754));
#173585=CARTESIAN_POINT('Ctrl Pts',(39.7317438420182,-36.0850974253399,
-87.2612325210988));
#173586=CARTESIAN_POINT('Ctrl Pts',(39.4836336651727,-36.7800000200025,
-87.1082114503545));
#173587=CARTESIAN_POINT('Ctrl Pts',(40.1585088632339,-36.78000002,-87.4451185554427));
#173588=CARTESIAN_POINT('Ctrl Pts',(39.4528126178963,-36.1238332542013,
-87.9779440827562));
#173589=CARTESIAN_POINT('Ctrl Pts',(39.2579727974598,-36.7800000200001,
-87.8751206778157));
#173590=CARTESIAN_POINT('Ctrl Pts',(39.9075095278365,-36.78000002,-88.1269484527019));
#173591=CARTESIAN_POINT('Ctrl Pts',(39.0804486566366,-36.2039143776693,
-89.4721907623552));
#173592=CARTESIAN_POINT('Ctrl Pts',(39.0022563977957,-36.78000002,-89.4265019469593));
#173593=CARTESIAN_POINT('Ctrl Pts',(39.572394069454,-36.78000002,-89.5466301924888));
#173594=CARTESIAN_POINT('Ctrl Pts',(38.9910757956325,-36.2453106379154,
-90.2508802901019));
#173595=CARTESIAN_POINT('Ctrl Pts',(38.95517376435,-36.78000002,-90.2192417070188));
#173596=CARTESIAN_POINT('Ctrl Pts',(39.4919635455253,-36.78000002,-90.2855006253694));
#173597=CARTESIAN_POINT('Ctrl Pts',(39.0007023042009,-36.2858508900221,
-91.0217464384246));
#173598=CARTESIAN_POINT('Ctrl Pts',(39.0064880541292,-36.78000002,-91.0217157887641));
#173599=CARTESIAN_POINT('Ctrl Pts',(39.5006328637826,-36.78000002,-91.0158318926359));
#173600=CARTESIAN_POINT('',(39.5,-36.78000002,-90.9091273827666));
#173601=CARTESIAN_POINT('Ctrl Pts',(39.5,-36.78000002,-90.9091273827666));
#173602=CARTESIAN_POINT('Ctrl Pts',(39.5,-36.78000002,-90.7679100061199));
#173603=CARTESIAN_POINT('Ctrl Pts',(39.5033096444594,-36.7800000200224,
-90.6269761431631));
#173604=CARTESIAN_POINT('Ctrl Pts',(39.5098707684965,-36.7800000197587,
-90.486327108651));
#173605=CARTESIAN_POINT('Ctrl Pts',(39.5164908621434,-36.7800000194927,
-90.3444139586241));
#173606=CARTESIAN_POINT('Ctrl Pts',(39.5264211472599,-36.7800000188623,
-90.2027900769916));
#173607=CARTESIAN_POINT('Ctrl Pts',(39.5396544427955,-36.7800000184551,
-90.0614520511831));
#173608=CARTESIAN_POINT('Ctrl Pts',(39.5457621647723,-36.7800000182671,
-89.9962186129912));
#173609=CARTESIAN_POINT('Ctrl Pts',(39.5525742276005,-36.780000018147,-89.9310460673889));
#173610=CARTESIAN_POINT('Ctrl Pts',(39.5600936571067,-36.7800000181768,
-89.8659343821325));
#173611=CARTESIAN_POINT('Ctrl Pts',(39.5772069508045,-36.7800000182445,
-89.7177482209293));
#173612=CARTESIAN_POINT('Ctrl Pts',(39.5980137125872,-36.7800000189104,
-89.569651212335));
#173613=CARTESIAN_POINT('Ctrl Pts',(39.6224903903715,-36.7800000193564,
-89.4222267568301));
#173614=CARTESIAN_POINT('Ctrl Pts',(39.646759527969,-36.7800000197985,-89.276052327955));
#173615=CARTESIAN_POINT('Ctrl Pts',(39.6746364995121,-36.780000019972,-89.1305398192698));
#173616=CARTESIAN_POINT('Ctrl Pts',(39.7060481712977,-36.780000019994,-88.9862487847489));
#173617=CARTESIAN_POINT('Ctrl Pts',(39.7169272984727,-36.7800000200016,
-88.9362749875731));
#173618=CARTESIAN_POINT('Ctrl Pts',(39.7282299820615,-36.78000002,-88.8864475773885));
#173619=CARTESIAN_POINT('Ctrl Pts',(39.7399518035734,-36.78000002,-88.8367893012138));
#173620=CARTESIAN_POINT('Ctrl Pts',(39.8212039955519,-36.78000002,-88.4925728511548));
#173621=CARTESIAN_POINT('Ctrl Pts',(39.9220601466511,-36.78000002,-88.1550003033774));
#173622=CARTESIAN_POINT('Ctrl Pts',(40.0453748819428,-36.78000002,-87.8250390461133));
#173623=CARTESIAN_POINT('Ctrl Pts',(40.16398080735,-36.78000002,-87.5076774577049));
#173624=CARTESIAN_POINT('Ctrl Pts',(40.3033623181985,-36.78000002,-87.1973567576874));
#173625=CARTESIAN_POINT('Ctrl Pts',(40.4661024946855,-36.78000002,-86.8949524600739));
#173626=CARTESIAN_POINT('Origin',(39.5,-36.28000002,-90.9091273827666));
#173627=CARTESIAN_POINT('Origin',(39.5,-36.28000002,-55.24995));
#173628=CARTESIAN_POINT('',(39.5,-36.78000002,-141.149515588739));
#173629=CARTESIAN_POINT('',(39.5,-36.78000002,-55.24995));
#173630=CARTESIAN_POINT('Origin',(39.5,-36.28000002,-141.149515588739));
#173631=CARTESIAN_POINT('Ctrl Pts',(39.,-36.28000002,-141.149515588739));
#173632=CARTESIAN_POINT('Ctrl Pts',(38.9999999999999,-36.78000002,-141.149515588739));
#173633=CARTESIAN_POINT('Ctrl Pts',(39.5,-36.78000002,-141.149515588739));
#173634=CARTESIAN_POINT('Ctrl Pts',(39.,-36.2411525212205,-141.887468602714));
#173635=CARTESIAN_POINT('Ctrl Pts',(38.9595709612524,-36.78000002,-141.917511819575));
#173636=CARTESIAN_POINT('Ctrl Pts',(39.5000000020403,-36.78000002,-141.848776286889));
#173637=CARTESIAN_POINT('Ctrl Pts',(39.0877747262142,-36.202664552653,-142.611197003283));
#173638=CARTESIAN_POINT('Ctrl Pts',(39.0069624314851,-36.78000002,-142.654181226843));
#173639=CARTESIAN_POINT('Ctrl Pts',(39.5789972525929,-36.78000002,-142.535527260215));
#173640=CARTESIAN_POINT('Ctrl Pts',(39.4389223885666,-36.1266531472167,
-144.029685314679));
#173641=CARTESIAN_POINT('Ctrl Pts',(39.2475606867303,-36.78000002,-144.126025522057));
#173642=CARTESIAN_POINT('Ctrl Pts',(39.8950301507098,-36.78000002,-143.883204247708));
#173643=CARTESIAN_POINT('Ctrl Pts',(39.7059668714196,-36.0888399354841,
-144.729666200452));
#173644=CARTESIAN_POINT('Ctrl Pts',(39.4615987310595,-36.78000002,-144.873235586497));
#173645=CARTESIAN_POINT('Ctrl Pts',(40.1353628336737,-36.78000002,-144.549109040068));
#173646=CARTESIAN_POINT('Ctrl Pts',(40.0734472163172,-36.0537915241817,
-145.374999642303));
#173647=CARTESIAN_POINT('Ctrl Pts',(39.7490326214954,-36.78000002,-145.549584755123));
#173648=CARTESIAN_POINT('Ctrl Pts',(40.4661024946855,-36.78000002,-145.163690511432));
#173649=CARTESIAN_POINT('',(40.4661024946856,-36.78000002,-145.163690511432));
#173650=CARTESIAN_POINT('Ctrl Pts',(40.4661024946855,-36.78000002,-145.163690511432));
#173651=CARTESIAN_POINT('Ctrl Pts',(40.4051245273351,-36.78000002,-145.05038106453));
#173652=CARTESIAN_POINT('Ctrl Pts',(40.3473970436746,-36.78000002,-144.935666150371));
#173653=CARTESIAN_POINT('Ctrl Pts',(40.2927291183489,-36.78000002,-144.819632460354));
#173654=CARTESIAN_POINT('Ctrl Pts',(40.2359907375988,-36.78000002,-144.699204190123));
#173655=CARTESIAN_POINT('Ctrl Pts',(40.182547909167,-36.78000002,-144.577354792971));
#173656=CARTESIAN_POINT('Ctrl Pts',(40.1322366185222,-36.78000002,-144.454153170975));
#173657=CARTESIAN_POINT('Ctrl Pts',(40.0991220934988,-36.78000002,-144.373062760806));
#173658=CARTESIAN_POINT('Ctrl Pts',(40.0673652289501,-36.78000002,-144.291385980202));
#173659=CARTESIAN_POINT('Ctrl Pts',(40.0369306905871,-36.78000002,-144.209138150939));
#173660=CARTESIAN_POINT('Ctrl Pts',(39.9567208320406,-36.78000002,-143.99237498955));
#173661=CARTESIAN_POINT('Ctrl Pts',(39.8859370924984,-36.78000002,-143.772269498041));
#173662=CARTESIAN_POINT('Ctrl Pts',(39.8243406671238,-36.78000002,-143.550546349406));
#173663=CARTESIAN_POINT('Ctrl Pts',(39.7928424603809,-36.78000002,-143.437165069032));
#173664=CARTESIAN_POINT('Ctrl Pts',(39.7637458267515,-36.78000002,-143.323361070991));
#173665=CARTESIAN_POINT('Ctrl Pts',(39.737013701299,-36.78000002,-143.209365754044));
#173666=CARTESIAN_POINT('Ctrl Pts',(39.6399004481884,-36.78000002,-142.795240207321));
#173667=CARTESIAN_POINT('Ctrl Pts',(39.5726401857881,-36.78000002,-142.376286688206));
#173668=CARTESIAN_POINT('Ctrl Pts',(39.5352116792707,-36.78000002,-141.952508599874));
#173669=CARTESIAN_POINT('Ctrl Pts',(39.5117389237049,-36.78000002,-141.686742198618));
#173670=CARTESIAN_POINT('Ctrl Pts',(39.5000000000007,-36.78000002,-141.41907812932));
#173671=CARTESIAN_POINT('Ctrl Pts',(39.5,-36.78000002,-141.149515588739));
#173672=CARTESIAN_POINT('Origin',(40.4661024946856,-36.28000002,-145.163690511432));
#173673=CARTESIAN_POINT('Ctrl Pts',(54.061590101286,-36.78000002,-171.268536075449));
#173674=CARTESIAN_POINT('Ctrl Pts',(53.4125141483451,-36.78000002,-171.598146859086));
#173675=CARTESIAN_POINT('Ctrl Pts',(53.6454853125448,-36.1005363232099,
-171.479840562953));
#173676=CARTESIAN_POINT('Ctrl Pts',(51.8377538941353,-36.78000002,-166.889319970653));
#173677=CARTESIAN_POINT('Ctrl Pts',(51.1583704358619,-36.7800000200002,
-167.182444881139));
#173678=CARTESIAN_POINT('Ctrl Pts',(51.4243352023986,-36.0943124607371,
-167.100627882666));
#173679=CARTESIAN_POINT('Ctrl Pts',(49.5972294079553,-36.78000002,-162.518792058211));
#173680=CARTESIAN_POINT('Ctrl Pts',(48.9013482881149,-36.7800000199664,
-162.806967721366));
#173681=CARTESIAN_POINT('Ctrl Pts',(49.1869218186486,-36.0874610318388,
-162.730098242847));
#173682=CARTESIAN_POINT('Ctrl Pts',(45.066960038919,-36.78000002,-153.803374490657));
#173683=CARTESIAN_POINT('Ctrl Pts',(44.348109595875,-36.7800000200345,-154.108244930852));
#173684=CARTESIAN_POINT('Ctrl Pts',(44.6642494092406,-36.072038540157,-154.01468012643));
#173685=CARTESIAN_POINT('Ctrl Pts',(42.777508353219,-36.78000002,-149.458325760535));
#173686=CARTESIAN_POINT('Ctrl Pts',(42.0345588527891,-36.7800000199998,
-149.755027455429));
#173687=CARTESIAN_POINT('Ctrl Pts',(42.3792743432826,-36.0634712454522,
-149.669636259109));
#173688=CARTESIAN_POINT('Ctrl Pts',(40.4497212107858,-36.78000002,-145.133252264122));
#173689=CARTESIAN_POINT('Ctrl Pts',(39.7324960674638,-36.78000002,-145.519268764292));
#173690=CARTESIAN_POINT('Ctrl Pts',(40.0571172805695,-36.0536964873408,
-145.34455504538));
#173691=CARTESIAN_POINT('',(54.0459394689003,-36.78000002,-171.237717270032));
#173692=CARTESIAN_POINT('Ctrl Pts',(54.0459394689003,-36.78000002,-171.237717270032));
#173693=CARTESIAN_POINT('Ctrl Pts',(51.8272412193298,-36.78000002,-166.868813514854));
#173694=CARTESIAN_POINT('Ctrl Pts',(49.5919157423625,-36.78000002,-162.508569528244));
#173695=CARTESIAN_POINT('Ctrl Pts',(47.3320947234338,-36.78000002,-158.161083274436));
#173696=CARTESIAN_POINT('Ctrl Pts',(45.0722737045051,-36.78000002,-153.813597020627));
#173697=CARTESIAN_POINT('Ctrl Pts',(42.7882516015473,-36.78000002,-149.478715140467));
#173698=CARTESIAN_POINT('Ctrl Pts',(40.4661024946855,-36.78000002,-145.163690511432));
#173699=CARTESIAN_POINT('Origin',(54.0459394689003,-36.28000002,-171.237717270032));
#173700=CARTESIAN_POINT('Ctrl Pts',(54.1985583159464,-36.7800000191852,
-171.906167818556));
#173701=CARTESIAN_POINT('Ctrl Pts',(53.439506223589,-36.7800433691512,-171.887030357476));
#173702=CARTESIAN_POINT('Ctrl Pts',(53.7393383808297,-36.082487169742,-171.894658379215));
#173703=CARTESIAN_POINT('Ctrl Pts',(54.2046305452548,-36.7800000191843,
-171.662933242572));
#173704=CARTESIAN_POINT('Ctrl Pts',(53.4406325939144,-36.7800434674344,
-171.77861312897));
#173705=CARTESIAN_POINT('Ctrl Pts',(53.7436938429465,-36.0817727411105,
-171.732515491476));
#173706=CARTESIAN_POINT('Ctrl Pts',(54.1464425180027,-36.7800000191923,
-171.423436673455));
#173707=CARTESIAN_POINT('Ctrl Pts',(53.4304080193293,-36.7800425499783,
-171.672542976743));
#173708=CARTESIAN_POINT('Ctrl Pts',(53.7019584052344,-36.0886165914289,
-171.572834421448));
#173709=CARTESIAN_POINT('Ctrl Pts',(54.0297882222771,-36.7800000192084,
-171.206777509126));
#173710=CARTESIAN_POINT('Ctrl Pts',(53.3916114660656,-36.7800408062075,
-171.550460731129));
#173711=CARTESIAN_POINT('Ctrl Pts',(53.6182347475101,-36.1024349685033,
-171.42841039456));
#173712=CARTESIAN_POINT('',(54.1989607257493,-36.78000002,-171.871644662643));
#173713=CARTESIAN_POINT('Origin',(52.6055188870422,-36.7800000520242,-171.864725026498));
#173714=CARTESIAN_POINT('Origin',(54.1989607257493,-36.28000002,-171.871644662643));
#173715=CARTESIAN_POINT('Origin',(54.1989607257493,-36.28000002,-179.64995));
#173716=CARTESIAN_POINT('',(54.1989607257493,-36.78000002,-171.871644662643));
#173717=CARTESIAN_POINT('',(53.7396474992599,-36.0824364606782,-179.64995));
#173718=CARTESIAN_POINT('Origin',(60.,-37.28000002,-176.84995));
#173719=CARTESIAN_POINT('',(-83.2809572255632,-36.78000002,-176.84995));
#173720=CARTESIAN_POINT('Origin',(57.,-37.28000002,-58.24995));
#173721=CARTESIAN_POINT('',(57.,-36.78000002,-55.74995));
#173722=CARTESIAN_POINT('Origin',(57.,-36.78000002,-58.24995));
#173723=CARTESIAN_POINT('',(57.,-37.28000002,-55.24995));
#173724=CARTESIAN_POINT('Origin',(57.,-37.28000002,-55.74995));
#173725=CARTESIAN_POINT('Origin',(57.,-37.28000002,-58.24995));
#173726=CARTESIAN_POINT('Origin',(57.,-2.42462934179819E-14,-58.24995));
#173727=CARTESIAN_POINT('',(57.,-37.78000002,-55.24995));
#173728=CARTESIAN_POINT('',(57.,28.41999998,-55.24995));
#173729=CARTESIAN_POINT('Origin',(57.,-37.78000002,-58.24995));
#173730=CARTESIAN_POINT('Origin',(57.,-37.78000002,-58.24995));
#173731=CARTESIAN_POINT('',(57.,-38.28000002,-55.74995));
#173732=CARTESIAN_POINT('Origin',(57.,-37.78000002,-55.74995));
#173733=CARTESIAN_POINT('Origin',(57.,-38.28000002,-58.24995));
#173734=CARTESIAN_POINT('Origin',(57.,11.61999998,-58.24995));
#173735=CARTESIAN_POINT('',(57.,12.11999998,-55.74995));
#173736=CARTESIAN_POINT('Origin',(57.,12.11999998,-58.24995));
#173737=CARTESIAN_POINT('',(57.,11.61999998,-55.24995));
#173738=CARTESIAN_POINT('Origin',(57.,11.61999998,-55.74995));
#173739=CARTESIAN_POINT('Origin',(57.,11.61999998,-58.24995));
#173740=CARTESIAN_POINT('Origin',(57.,-2.42462934179819E-14,-58.24995));
#173741=CARTESIAN_POINT('',(57.,11.11999998,-55.24995));
#173742=CARTESIAN_POINT('',(57.,28.41999998,-55.24995));
#173743=CARTESIAN_POINT('Origin',(57.,11.11999998,-58.24995));
#173744=CARTESIAN_POINT('Origin',(57.,11.11999998,-58.24995));
#173745=CARTESIAN_POINT('',(57.,10.61999998,-55.74995));
#173746=CARTESIAN_POINT('Origin',(57.,11.11999998,-55.74995));
#173747=CARTESIAN_POINT('Origin',(57.,10.61999998,-58.24995));
#173748=CARTESIAN_POINT('Ctrl Pts',(5.,45.5214348882082,-61.0621827299711));
#173749=CARTESIAN_POINT('Ctrl Pts',(5.,45.1055585268383,-60.8674008824013));
#173750=CARTESIAN_POINT('Ctrl Pts',(5.45757488824865,45.0702713246265,-60.8508735991007));
#173751=CARTESIAN_POINT('Ctrl Pts',(5.,40.8246742459034,-71.0901794372786));
#173752=CARTESIAN_POINT('Ctrl Pts',(5.00000000013405,40.426315064797,-70.8653394730463));
#173753=CARTESIAN_POINT('Ctrl Pts',(5.45419794131935,40.3738290579191,-70.8788685457756));
#173754=CARTESIAN_POINT('Ctrl Pts',(5.,36.1242566254946,-81.1164625478583));
#173755=CARTESIAN_POINT('Ctrl Pts',(5.00000000003379,35.7394456595583,-80.8717315350143));
#173756=CARTESIAN_POINT('Ctrl Pts',(5.4500940393161,35.6738220550387,-80.9051511012611));
#173757=CARTESIAN_POINT('Ctrl Pts',(5.,31.4150905187971,-91.1386408691297));
#173758=CARTESIAN_POINT('Ctrl Pts',(4.99999999999999,31.0104747491644,-90.9485222334823));
#173759=CARTESIAN_POINT('Ctrl Pts',(5.44427033638569,30.9653765476951,-90.9273317382593));
#173760=CARTESIAN_POINT('',(5.,45.5214348882082,-61.062182729971));
#173761=CARTESIAN_POINT('',(5.45757488824865,45.0702713246265,-60.8508735991007));
#173762=CARTESIAN_POINT('Origin',(5.5,45.5214348882082,-61.062182729971));
#173763=CARTESIAN_POINT('',(5.44427033638568,30.9653765476951,-90.9273317382593));
#173764=CARTESIAN_POINT('Ctrl Pts',(5.44427033638568,30.9653765476951,-90.9273317382593));
#173765=CARTESIAN_POINT('Ctrl Pts',(5.44561970702987,32.0563384739202,-88.6051603388755));
#173766=CARTESIAN_POINT('Ctrl Pts',(5.44696375827399,33.1898917997868,-86.1910626080188));
#173767=CARTESIAN_POINT('Ctrl Pts',(5.44885264917258,34.9541150607098,-82.4320265145244));
#173768=CARTESIAN_POINT('Ctrl Pts',(5.44976896906513,35.8521997505521,-80.5180360934748));
#173769=CARTESIAN_POINT('Ctrl Pts',(5.45080151723396,36.927917076703,-78.2247206138878));
#173770=CARTESIAN_POINT('Ctrl Pts',(5.45131315589655,37.4727634355675,-77.062981210337));
#173771=CARTESIAN_POINT('Ctrl Pts',(5.45160037064691,37.7812047612991,-76.4052610779079));
#173772=CARTESIAN_POINT('Ctrl Pts',(5.45174164230917,37.9336020084846,-76.0802730329389));
#173773=CARTESIAN_POINT('Ctrl Pts',(5.45181457454894,38.0124146208361,-75.9122006235131));
#173774=CARTESIAN_POINT('Ctrl Pts',(5.45181971490317,38.0179701347131,-75.9003531509149));
#173775=CARTESIAN_POINT('Ctrl Pts',(5.45385962122421,40.2228504311467,-71.1983046079137));
#173776=CARTESIAN_POINT('Ctrl Pts',(5.45577865562035,42.5721856437188,-66.1848666861869));
#173777=CARTESIAN_POINT('Ctrl Pts',(5.45757488824865,45.0702713246265,-60.8508735991007));
#173778=CARTESIAN_POINT('',(5.,31.415090518797,-91.1386408691297));
#173779=CARTESIAN_POINT('Origin',(5.5,31.415090518797,-91.1386408691297));
#173780=CARTESIAN_POINT('Ctrl Pts',(5.,45.5214348882082,-61.0621827299711));
#173781=CARTESIAN_POINT('Ctrl Pts',(5.,40.8246742459034,-71.0901794372786));
#173782=CARTESIAN_POINT('Ctrl Pts',(5.,36.1242566254946,-81.1164625478583));
#173783=CARTESIAN_POINT('Ctrl Pts',(5.,31.4150905187971,-91.1386408691297));
#173784=CARTESIAN_POINT('Ctrl Pts',(12.,30.2507177004773,-91.1386408691297));
#173785=CARTESIAN_POINT('Ctrl Pts',(12.,29.679733250215,-90.8631216114043));
#173786=CARTESIAN_POINT('Ctrl Pts',(11.3834743397155,29.812801930373,-90.9273317382593));
#173787=CARTESIAN_POINT('Ctrl Pts',(12.,35.0807977947169,-81.1288119730547));
#173788=CARTESIAN_POINT('Ctrl Pts',(11.9999999998861,34.4484178829812,-81.0174669870403));
#173789=CARTESIAN_POINT('Ctrl Pts',(11.3956361798112,34.6396513996494,-80.9174913671817));
#173790=CARTESIAN_POINT('Ctrl Pts',(12.,39.8700921493796,-71.0994291820815));
#173791=CARTESIAN_POINT('Ctrl Pts',(11.9999999999222,39.2806183751482,-70.92559601425));
#173792=CARTESIAN_POINT('Ctrl Pts',(11.4042255504145,39.4271199662976,-70.8881122426161));
#173793=CARTESIAN_POINT('Ctrl Pts',(12.,44.6428767076058,-61.062182729971));
#173794=CARTESIAN_POINT('Ctrl Pts',(12.,44.102645384174,-60.8052987597771));
#173795=CARTESIAN_POINT('Ctrl Pts',(11.4112929481563,44.1984900402045,-60.8508735991007));
#173796=CARTESIAN_POINT('',(11.4112929481563,44.1984900402045,-60.8508735991007));
#173797=CARTESIAN_POINT('',(12.,44.6428767076058,-61.062182729971));
#173798=CARTESIAN_POINT('Origin',(11.5,44.6428767076058,-61.062182729971));
#173799=CARTESIAN_POINT('',(12.,30.2507177004773,-91.1386408691297));
#173800=CARTESIAN_POINT('Ctrl Pts',(12.,30.2507177004773,-91.1386408691297));
#173801=CARTESIAN_POINT('Ctrl Pts',(12.,35.0808027196733,-81.1288017666047));
#173802=CARTESIAN_POINT('Ctrl Pts',(12.,39.8700874953717,-71.0994389691951));
#173803=CARTESIAN_POINT('Ctrl Pts',(12.,44.6428767076058,-61.062182729971));
#173804=CARTESIAN_POINT('',(11.3834743397155,29.812801930373,-90.9273317382593));
#173805=CARTESIAN_POINT('Origin',(11.5,30.2507177004773,-91.1386408691297));
#173806=CARTESIAN_POINT('Ctrl Pts',(11.4112929481563,44.1984900402045,-60.8508735991007));
#173807=CARTESIAN_POINT('Ctrl Pts',(11.4094109984326,42.9279405506231,-63.5236506500919));
#173808=CARTESIAN_POINT('Ctrl Pts',(11.4075038463216,41.6949692901581,-66.1140437492198));
#173809=CARTESIAN_POINT('Ctrl Pts',(11.4044750232958,39.9018903158517,-69.876057470117));
#173810=CARTESIAN_POINT('Ctrl Pts',(11.4029232381826,39.0194448925056,-71.7261703486169));
#173811=CARTESIAN_POINT('Ctrl Pts',(11.4010679295011,38.0145870304699,-73.8305709051232));
#173812=CARTESIAN_POINT('Ctrl Pts',(11.4001352611225,37.5183227466879,-74.8692550662738));
#173813=CARTESIAN_POINT('Ctrl Pts',(11.3996102114504,37.2409077632026,-75.4497134989859));
#173814=CARTESIAN_POINT('Ctrl Pts',(11.3993518934088,37.1049529011707,-75.7341278491348));
#173815=CARTESIAN_POINT('Ctrl Pts',(11.3992186208999,37.0349202316132,-75.8806206533949));
#173816=CARTESIAN_POINT('Ctrl Pts',(11.3992115364803,37.0311977944665,-75.8884071252557));
#173817=CARTESIAN_POINT('Ctrl Pts',(11.3943001013229,34.4508453562602,-81.2858634887265));
#173818=CARTESIAN_POINT('Ctrl Pts',(11.3891021666564,32.0464009004938,-86.2953312405831));
#173819=CARTESIAN_POINT('Ctrl Pts',(11.3834743397155,29.812801930373,-90.9273317382593));
#173820=CARTESIAN_POINT('Ctrl Pts',(13.5,29.5462485400348,-91.058247935017));
#173821=CARTESIAN_POINT('Ctrl Pts',(13.5,29.2108963546553,-90.8936099040706));
#173822=CARTESIAN_POINT('Ctrl Pts',(13.8582614853459,29.115831713372,-90.8469388041467));
#173823=CARTESIAN_POINT('Ctrl Pts',(13.5,29.5320844445084,-91.0870988658315));
#173824=CARTESIAN_POINT('Ctrl Pts',(13.5,29.1946688455411,-90.923776404174));
#173825=CARTESIAN_POINT('Ctrl Pts',(13.8598257678503,29.1000938294036,-90.8779461296248));
#173826=CARTESIAN_POINT('Ctrl Pts',(13.5,29.518158585283,-91.1160643410222));
#173827=CARTESIAN_POINT('Ctrl Pts',(13.4999999999997,29.1787031940904,-90.9540383533105));
#173828=CARTESIAN_POINT('Ctrl Pts',(13.8613943096149,29.0846206527093,-90.9090791787867));
#173829=CARTESIAN_POINT('Ctrl Pts',(13.5,29.5044693674792,-91.1451435916293));
#173830=CARTESIAN_POINT('Ctrl Pts',(13.5,29.1629965026825,-90.9843933533492));
#173831=CARTESIAN_POINT('Ctrl Pts',(13.8629670146618,29.0694104105324,-90.9403371832586));
#173832=CARTESIAN_POINT('',(13.5,29.5462485400348,-91.058247935017));
#173833=CARTESIAN_POINT('',(13.8582614743845,29.1158316800856,-90.8469387878052));
#173834=CARTESIAN_POINT('Origin',(14.,29.5462485400348,-91.058247935017));
#173835=CARTESIAN_POINT('',(13.8629628324617,29.0693971421497,-90.9403366624458));
#173836=CARTESIAN_POINT('Origin',(13.9259921622961,31.8088924073546,-92.6508709683574));
#173837=CARTESIAN_POINT('',(13.5,29.5044693674792,-91.1451435916293));
#173838=CARTESIAN_POINT('Origin',(14.,29.5044693674792,-91.1451435916293));
#173839=CARTESIAN_POINT('Ctrl Pts',(13.5,29.5462485400348,-91.058247935017));
#173840=CARTESIAN_POINT('Ctrl Pts',(13.5,29.5320849211775,-91.0870978945881));
#173841=CARTESIAN_POINT('Ctrl Pts',(13.5,29.5181581265359,-91.1160653155133));
#173842=CARTESIAN_POINT('Ctrl Pts',(13.5,29.5044693674792,-91.1451435916293));
#173843=CARTESIAN_POINT('Ctrl Pts',(13.5,44.086908282047,-61.0621827299711));
#173844=CARTESIAN_POINT('Ctrl Pts',(13.5,43.724980245498,-60.8884062566336));
#173845=CARTESIAN_POINT('Ctrl Pts',(13.8920088064511,43.6468101642065,-60.8508735991007));
#173846=CARTESIAN_POINT('Ctrl Pts',(13.5,39.2774015744131,-71.0790468430123));
#173847=CARTESIAN_POINT('Ctrl Pts',(13.5,38.9561333124887,-70.8371780085667));
#173848=CARTESIAN_POINT('Ctrl Pts',(13.883422492558,38.8394158858892,-70.8677262129548));
#173849=CARTESIAN_POINT('Ctrl Pts',(13.5,34.4430593692808,-81.0839048048873));
#173850=CARTESIAN_POINT('Ctrl Pts',(13.5000000000877,34.1527775267561,-80.7999951426717));
#173851=CARTESIAN_POINT('Ctrl Pts',(13.8729900235566,34.0078012896411,-80.8725774805421));
#173852=CARTESIAN_POINT('Ctrl Pts',(13.5,29.5462485400348,-91.058247935017));
#173853=CARTESIAN_POINT('Ctrl Pts',(13.5,29.2108963546553,-90.8936099040706));
#173854=CARTESIAN_POINT('Ctrl Pts',(13.8582614853459,29.115831713372,-90.8469388041467));
#173855=CARTESIAN_POINT('',(13.5,44.086908282047,-61.0621827299711));
#173856=CARTESIAN_POINT('',(13.8920088064511,43.6468101642065,-60.8508735991007));
#173857=CARTESIAN_POINT('Origin',(14.,44.086908282047,-61.0621827299711));
#173858=CARTESIAN_POINT('Ctrl Pts',(13.8582614853459,29.115831713372,-90.8469388041467));
#173859=CARTESIAN_POINT('Ctrl Pts',(13.8606694674642,29.9156242721724,-89.2162213924719));
#173860=CARTESIAN_POINT('Ctrl Pts',(13.8630372008162,30.7386522803969,-87.534015044631));
#173861=CARTESIAN_POINT('Ctrl Pts',(13.8653554193648,31.584799169861,-85.8002497556502));
#173862=CARTESIAN_POINT('Ctrl Pts',(13.8675774780501,32.3958478287453,-84.1384011688891));
#173863=CARTESIAN_POINT('Ctrl Pts',(13.8697540270431,33.2281369500207,-82.4291821376903));
#173864=CARTESIAN_POINT('Ctrl Pts',(13.8718797439041,34.0816065397358,-80.6725529454259));
#173865=CARTESIAN_POINT('Ctrl Pts',(13.8738910205824,34.8891287045455,-79.0104937166035));
#173866=CARTESIAN_POINT('Ctrl Pts',(13.8758567874135,35.7156127493098,-77.3059903174534));
#173867=CARTESIAN_POINT('Ctrl Pts',(13.8777752709462,36.5610466523927,-75.5590348924101));
#173868=CARTESIAN_POINT('Ctrl Pts',(13.8796481768889,37.3863955043561,-73.8535820483342));
#173869=CARTESIAN_POINT('Ctrl Pts',(13.8814760018982,38.2298035907086,-72.1076716166056));
#173870=CARTESIAN_POINT('Ctrl Pts',(13.8832599520145,39.0913013121694,-70.3213206281249));
#173871=CARTESIAN_POINT('Ctrl Pts',(13.8849797115563,39.9218003901471,-68.5992466029468));
#173872=CARTESIAN_POINT('Ctrl Pts',(13.8866586900895,40.7691106156835,-66.8395898988203));
#173873=CARTESIAN_POINT('Ctrl Pts',(13.8883008096956,41.6333016406227,-65.042387541687));
#173874=CARTESIAN_POINT('Ctrl Pts',(13.8895573392646,42.2945699015106,-63.6671905738076));
#173875=CARTESIAN_POINT('Ctrl Pts',(13.8907923409499,42.965722872781,-62.2700105827591));
#173876=CARTESIAN_POINT('Ctrl Pts',(13.8920088064511,43.6468101642066,-60.8508735991007));
#173877=CARTESIAN_POINT('Ctrl Pts',(13.5,44.086908282047,-61.0621827299711));
#173878=CARTESIAN_POINT('Ctrl Pts',(13.5,39.2774232822218,-71.079001631676));
#173879=CARTESIAN_POINT('Ctrl Pts',(13.5,34.4431166252676,-81.0837881795346));
#173880=CARTESIAN_POINT('Ctrl Pts',(13.5,29.5462485400348,-91.058247935017));
#173881=CARTESIAN_POINT('Ctrl Pts',(20.5,29.726759920701,-85.9392854774869));
#173882=CARTESIAN_POINT('Ctrl Pts',(20.5,29.0600890554149,-85.5959926642051));
#173883=CARTESIAN_POINT('Ctrl Pts',(19.8077680666402,29.3163999141123,-85.7279763466165));
#173884=CARTESIAN_POINT('Ctrl Pts',(20.5,33.9784532599698,-77.6825438045949));
#173885=CARTESIAN_POINT('Ctrl Pts',(20.5000000001728,33.2278557603418,-77.5610859264982));
#173886=CARTESIAN_POINT('Ctrl Pts',(19.8234665452012,33.5607487699413,-77.4712163753771));
#173887=CARTESIAN_POINT('Ctrl Pts',(20.5,38.1440461521965,-69.3822166533219));
#173888=CARTESIAN_POINT('Ctrl Pts',(20.5000000002289,37.4529027206824,-69.1923113693162));
#173889=CARTESIAN_POINT('Ctrl Pts',(19.8355385600285,37.7216554195719,-69.1708971047811));
#173890=CARTESIAN_POINT('Ctrl Pts',(20.5,42.270218132516,-61.0621827299711));
#173891=CARTESIAN_POINT('Ctrl Pts',(20.5,41.6540022187559,-60.7565814715328));
#173892=CARTESIAN_POINT('Ctrl Pts',(19.8457268663587,41.8441333387867,-60.8508735991007));
#173893=CARTESIAN_POINT('',(19.8457268663587,41.8441333387867,-60.8508735991007));
#173894=CARTESIAN_POINT('',(20.5,42.270218132516,-61.0621827299711));
#173895=CARTESIAN_POINT('Origin',(20.,42.270218132516,-61.0621827299711));
#173896=CARTESIAN_POINT('',(20.5,29.726759920701,-85.9392854774869));
#173897=CARTESIAN_POINT('Ctrl Pts',(20.5,29.726759920701,-85.9392854774869));
#173898=CARTESIAN_POINT('Ctrl Pts',(20.5,33.9784770268254,-77.682497649623));
#173899=CARTESIAN_POINT('Ctrl Pts',(20.5,38.1440239783714,-69.3822613645965));
#173900=CARTESIAN_POINT('Ctrl Pts',(20.5,42.270218132516,-61.0621827299711));
#173901=CARTESIAN_POINT('',(19.8077681423597,29.3163998849126,-85.7279763868962));
#173902=CARTESIAN_POINT('Origin',(20.,29.726759920701,-85.9392854774869));
#173903=CARTESIAN_POINT('Ctrl Pts',(19.8457268663587,41.8441333387867,-60.8508735991007));
#173904=CARTESIAN_POINT('Ctrl Pts',(19.8438917319593,41.101585869444,-62.3494898488539));
#173905=CARTESIAN_POINT('Ctrl Pts',(19.8420266925439,40.3704767068203,-63.8218555336744));
#173906=CARTESIAN_POINT('Ctrl Pts',(19.8401287326225,39.6506919358387,-65.2679151976064));
#173907=CARTESIAN_POINT('Ctrl Pts',(19.8381885441163,38.9148923418786,-66.7461489092091));
#173908=CARTESIAN_POINT('Ctrl Pts',(19.8362139596767,38.1909268139742,-68.1968930645251));
#173909=CARTESIAN_POINT('Ctrl Pts',(19.8342035897005,37.4787222386946,-69.620114247757));
#173910=CARTESIAN_POINT('Ctrl Pts',(19.832114429525,36.73860501991,-71.0991141593137));
#173911=CARTESIAN_POINT('Ctrl Pts',(19.8299866260592,36.0111887347363,-72.5483914937309));
#173912=CARTESIAN_POINT('Ctrl Pts',(19.8278205210925,35.2964419024826,-73.9679356449112));
#173913=CARTESIAN_POINT('Ctrl Pts',(19.8256028260814,34.5646719704813,-75.4212890283832));
#173914=CARTESIAN_POINT('Ctrl Pts',(19.8233449918063,33.8461823850751,-76.8434761657068));
#173915=CARTESIAN_POINT('Ctrl Pts',(19.8210492509101,33.1409891728991,-78.2345121767389));
#173916=CARTESIAN_POINT('Ctrl Pts',(19.8186535378293,32.4050870483357,-79.6861233638405));
#173917=CARTESIAN_POINT('Ctrl Pts',(19.8162165495322,31.6836646490343,-81.1038113445808));
#173918=CARTESIAN_POINT('Ctrl Pts',(19.8137427373434,30.9767915267581,-82.4876206314048));
#173919=CARTESIAN_POINT('Ctrl Pts',(19.8117734698976,30.414088248637,-83.5891960025022));
#173920=CARTESIAN_POINT('Ctrl Pts',(19.8097809087695,29.860605784483,-84.6693034148617));
#173921=CARTESIAN_POINT('Ctrl Pts',(19.8077680666402,29.3163999141123,-85.7279763466165));
#173922=CARTESIAN_POINT('Ctrl Pts',(19.8077680666402,29.3163999141123,-85.7279763466166));
#173923=CARTESIAN_POINT('Ctrl Pts',(20.5,29.060089055415,-85.5959926642051));
#173924=CARTESIAN_POINT('Ctrl Pts',(20.5,29.7267599207011,-85.9392854774869));
#173925=CARTESIAN_POINT('Ctrl Pts',(19.8381616888784,29.0132146764574,-86.2891090855032));
#173926=CARTESIAN_POINT('Ctrl Pts',(20.5000000000088,28.8159639706074,-86.1813743808706));
#173927=CARTESIAN_POINT('Ctrl Pts',(20.5,29.4538783950287,-86.4692184100357));
#173928=CARTESIAN_POINT('Ctrl Pts',(19.8696882890952,28.7939665404343,-86.8767409776521));
#173929=CARTESIAN_POINT('Ctrl Pts',(20.5,28.6378348142226,-86.8034965148886));
#173930=CARTESIAN_POINT('Ctrl Pts',(20.5,29.2565698845367,-87.023482728964));
#173931=CARTESIAN_POINT('Ctrl Pts',(19.9342607161865,28.4963466916806,-88.096087277311));
#173932=CARTESIAN_POINT('Ctrl Pts',(20.5,28.4280256078311,-88.0643854695474));
#173933=CARTESIAN_POINT('Ctrl Pts',(20.5,28.9887120203667,-88.1720534995035));
#173934=CARTESIAN_POINT('Ctrl Pts',(19.9674881255149,28.4199999800001,-88.7314889737132));
#173935=CARTESIAN_POINT('Ctrl Pts',(20.5,28.3863947724214,-88.7102571696975));
#173936=CARTESIAN_POINT('Ctrl Pts',(20.5,28.9199999814054,-88.7697908796757));
#173937=CARTESIAN_POINT('Ctrl Pts',(20.,28.4199999800001,-89.3628471840451));
#173938=CARTESIAN_POINT('Ctrl Pts',(20.5,28.41999998,-89.3628471840451));
#173939=CARTESIAN_POINT('Ctrl Pts',(20.5,28.9199999800001,-89.3628471840451));
#173940=CARTESIAN_POINT('',(20.5,28.9199999800001,-89.3628471840452));
#173941=CARTESIAN_POINT('Ctrl Pts',(20.5,28.9199999800001,-89.3628471840452));
#173942=CARTESIAN_POINT('Ctrl Pts',(20.5,28.9199999800001,-89.0651820878934));
#173943=CARTESIAN_POINT('Ctrl Pts',(20.5,28.93706429112,-88.7687961767652));
#173944=CARTESIAN_POINT('Ctrl Pts',(20.5,29.004819730958,-88.1785451079783));
#173945=CARTESIAN_POINT('Ctrl Pts',(20.5,29.0556764864843,-87.8849108068938));
#173946=CARTESIAN_POINT('Ctrl Pts',(20.5,29.2565698843866,-87.0234827289138));
#173947=CARTESIAN_POINT('Ctrl Pts',(20.5,29.453814841029,-86.4693418183145));
#173948=CARTESIAN_POINT('Ctrl Pts',(20.5,29.726759920701,-85.9392854774869));
#173949=CARTESIAN_POINT('',(20.,28.4199999800001,-89.3628471840451));
#173950=CARTESIAN_POINT('Origin',(20.,28.9199999800001,-89.3628471840452));
#173951=CARTESIAN_POINT('Ctrl Pts',(19.8077680691566,29.3163998890102,-85.7279763930753));
#173952=CARTESIAN_POINT('Ctrl Pts',(19.8138059530845,29.2561708716977,-85.8394477061454));
#173953=CARTESIAN_POINT('Ctrl Pts',(19.8202703692203,29.1954402850721,-85.9590140875865));
#173954=CARTESIAN_POINT('Ctrl Pts',(19.8271724235496,29.1354166241997,-86.0869929818154));
#173955=CARTESIAN_POINT('Ctrl Pts',(19.8278791125124,29.1292709092249,-86.100096511245));
#173956=CARTESIAN_POINT('Ctrl Pts',(19.8285903887909,29.1231326473758,-86.1132882440816));
#173957=CARTESIAN_POINT('Ctrl Pts',(19.8293062638353,29.1170031622791,-86.1265685285763));
#173958=CARTESIAN_POINT('Ctrl Pts',(19.8344373255712,29.0730698436299,-86.2217554751544));
#173959=CARTESIAN_POINT('Ctrl Pts',(19.8398044093972,29.0295900163094,-86.3214872821633));
#173960=CARTESIAN_POINT('Ctrl Pts',(19.8454079188031,28.9870783305874,-86.4258270644159));
#173961=CARTESIAN_POINT('Ctrl Pts',(19.8477324609691,28.9694429169824,-86.4691110505534));
#173962=CARTESIAN_POINT('Ctrl Pts',(19.8500976503827,28.9519743036303,-86.5131873880211));
#173963=CARTESIAN_POINT('Ctrl Pts',(19.8525033305116,28.9347097768219,-86.5580575288924));
#173964=CARTESIAN_POINT('Ctrl Pts',(19.8526348911436,28.9337656230121,-86.5605113647213));
#173965=CARTESIAN_POINT('Ctrl Pts',(19.8527665728447,28.9328220795741,-86.5629675741412));
#173966=CARTESIAN_POINT('Ctrl Pts',(19.8528983755796,28.9318791526062,-86.5654261572288));
#173967=CARTESIAN_POINT('Ctrl Pts',(19.8529637620926,28.9314113724307,-86.5666458449325));
#173968=CARTESIAN_POINT('Ctrl Pts',(19.8530291783932,28.930943743974,-86.567866116817));
#173969=CARTESIAN_POINT('Ctrl Pts',(19.8530946244768,28.9304762679801,-86.5690869728917));
#173970=CARTESIAN_POINT('Ctrl Pts',(19.8531272591149,28.9302431614438,-86.5696957518119));
#173971=CARTESIAN_POINT('Ctrl Pts',(19.8531599011586,28.9300100928176,-86.5703046759916));
#173972=CARTESIAN_POINT('Ctrl Pts',(19.8531925506074,28.9297770621936,-86.5709137454318));
#173973=CARTESIAN_POINT('Ctrl Pts',(19.8532109379793,28.9296458250397,-86.5712567584595));
#173974=CARTESIAN_POINT('Ctrl Pts',(19.8532294228268,28.9295139204569,-86.5716015920954));
#173975=CARTESIAN_POINT('Ctrl Pts',(19.8532484967547,28.9293778437378,-86.5719574174513));
#173976=CARTESIAN_POINT('Ctrl Pts',(19.8533833936122,28.9284154660929,-86.5744739270359));
#173977=CARTESIAN_POINT('Ctrl Pts',(19.8535396018,28.927302884498,-86.5773881447066));
#173978=CARTESIAN_POINT('Ctrl Pts',(19.8536815320461,28.926293817902,-86.5800361364514));
#173979=CARTESIAN_POINT('Ctrl Pts',(19.8538223534622,28.9252926346389,-86.5826634407606));
#173980=CARTESIAN_POINT('Ctrl Pts',(19.8539491178474,28.9243932488445,-86.5850286292047));
#173981=CARTESIAN_POINT('Ctrl Pts',(19.8540270312009,28.9238408419878,-86.5864823782079));
#173982=CARTESIAN_POINT('Ctrl Pts',(19.8540350253345,28.9237841634593,-86.5866315370267));
#173983=CARTESIAN_POINT('Ctrl Pts',(19.8540429572621,28.9237279313574,-86.5867795355964));
#173984=CARTESIAN_POINT('Ctrl Pts',(19.854050924075,28.9236714573129,-86.5869281854998));
#173985=CARTESIAN_POINT('Ctrl Pts',(19.8563700093498,28.9072322454547,-86.6301991655269));
#173986=CARTESIAN_POINT('Ctrl Pts',(19.8589484826522,28.8894066613016,-86.6783454040105));
#173987=CARTESIAN_POINT('Ctrl Pts',(19.861789010759,28.8704970519722,-86.7314446547894));
#173988=CARTESIAN_POINT('Ctrl Pts',(19.8645532478657,28.8520953175712,-86.7831177640904));
#173989=CARTESIAN_POINT('Ctrl Pts',(19.8675656622532,28.8326675258354,-86.839481569511));
#173990=CARTESIAN_POINT('Ctrl Pts',(19.8708290798645,28.8125353830987,-86.9006211059241));
#173991=CARTESIAN_POINT('Ctrl Pts',(19.8742516216661,28.7914215974065,-86.9647418051478));
#173992=CARTESIAN_POINT('Ctrl Pts',(19.8779505890201,28.7695315696661,-87.0341217459319));
#173993=CARTESIAN_POINT('Ctrl Pts',(19.881927060228,28.7472934410884,-87.108826435092));
#173994=CARTESIAN_POINT('Ctrl Pts',(19.8858361123418,28.7254323489346,-87.1822645433543));
#173995=CARTESIAN_POINT('Ctrl Pts',(19.8900135681237,28.7032345847988,-87.2608526848623));
#173996=CARTESIAN_POINT('Ctrl Pts',(19.8944591271272,28.6811431666031,-87.3446366822712));
#173997=CARTESIAN_POINT('Ctrl Pts',(19.8955745229581,28.6756004045488,-87.3656581829045));
#173998=CARTESIAN_POINT('Ctrl Pts',(19.8967067865892,28.6700644898885,-87.3870066305516));
#173999=CARTESIAN_POINT('Ctrl Pts',(19.8978558878223,28.6645427205203,-87.4086823557021));
#174000=CARTESIAN_POINT('Ctrl Pts',(19.89887720476,28.6596349922718,-87.4279476602687));
#174001=CARTESIAN_POINT('Ctrl Pts',(19.8998752459103,28.6549099612437,-87.446781111282));
#174002=CARTESIAN_POINT('Ctrl Pts',(19.9009366140947,28.6499659548319,-87.4668174126734));
#174003=CARTESIAN_POINT('Ctrl Pts',(19.9012200059135,28.6486458747789,-87.4721672281063));
#174004=CARTESIAN_POINT('Ctrl Pts',(19.9015079153701,28.6473104524095,-87.4776028816474));
#174005=CARTESIAN_POINT('Ctrl Pts',(19.9018019975683,28.6459526530311,-87.4831556819491));
#174006=CARTESIAN_POINT('Ctrl Pts',(19.9018595593474,28.6456868860161,-87.4842425517656));
#174007=CARTESIAN_POINT('Ctrl Pts',(19.9019170864846,28.6454215357657,-87.4853286991829));
#174008=CARTESIAN_POINT('Ctrl Pts',(19.9019745789215,28.6451566012051,-87.4864141240178));
#174009=CARTESIAN_POINT('Ctrl Pts',(19.9059518365993,28.6268287467454,-87.5615025094597));
#174010=CARTESIAN_POINT('Ctrl Pts',(19.9097655725751,28.6105182419633,-87.6331851842344));
#174011=CARTESIAN_POINT('Ctrl Pts',(19.913394524837,28.5959092357283,-87.7013592376738));
#174012=CARTESIAN_POINT('Ctrl Pts',(19.9171523881801,28.5807812745294,-87.7719550344457));
#174013=CARTESIAN_POINT('Ctrl Pts',(19.9207121251527,28.5674776275295,-87.8387888721745));
#174014=CARTESIAN_POINT('Ctrl Pts',(19.9240526752648,28.5556847412826,-87.9017892292155));
#174015=CARTESIAN_POINT('Ctrl Pts',(19.9264836775809,28.5471027614233,-87.947636173206));
#174016=CARTESIAN_POINT('Ctrl Pts',(19.9287986577477,28.5393216422585,-87.9914538920984));
#174017=CARTESIAN_POINT('Ctrl Pts',(19.9309902059722,28.5322331361077,-88.0332265793131));
#174018=CARTESIAN_POINT('Ctrl Pts',(19.9341130131768,28.5221324968288,-88.0927498182434));
#174019=CARTESIAN_POINT('Ctrl Pts',(19.9369954702788,28.5134356307963,-88.1481148204475));
#174020=CARTESIAN_POINT('Ctrl Pts',(19.9396491505859,28.5058659354445,-88.1992828513666));
#174021=CARTESIAN_POINT('Ctrl Pts',(19.9404596972027,28.5035538291438,-88.214911740137));
#174022=CARTESIAN_POINT('Ctrl Pts',(19.9412489070806,28.5013471920599,-88.2301492763028));
#174023=CARTESIAN_POINT('Ctrl Pts',(19.9420171267609,28.4992389562131,-88.244994858652));
#174024=CARTESIAN_POINT('Ctrl Pts',(19.943658788847,28.4947337203449,-88.2767194165039));
#174025=CARTESIAN_POINT('Ctrl Pts',(19.945205054462,28.4906773451103,-88.3066533814086));
#174026=CARTESIAN_POINT('Ctrl Pts',(19.9466613325595,28.48700670808,-88.3347914894808));
#174027=CARTESIAN_POINT('Ctrl Pts',(19.9473894716083,28.4851713895648,-88.3488605435169));
#174028=CARTESIAN_POINT('Ctrl Pts',(19.9480951270559,28.4834326321617,-88.3624806487063));
#174029=CARTESIAN_POINT('Ctrl Pts',(19.948779043131,28.4817832803921,-88.3756513708551));
#174030=CARTESIAN_POINT('Ctrl Pts',(19.9491210011685,28.4809586045074,-88.3822367319295));
#174031=CARTESIAN_POINT('Ctrl Pts',(19.9494575252137,28.4801562877716,-88.388709748227));
#174032=CARTESIAN_POINT('Ctrl Pts',(19.9497887098329,28.479375482198,-88.3950703715738));
#174033=CARTESIAN_POINT('Ctrl Pts',(19.9499543021425,28.4789850794112,-88.3982506832472));
#174034=CARTESIAN_POINT('Ctrl Pts',(19.9501185596432,28.4786000548937,-88.401402896738));
#174035=CARTESIAN_POINT('Ctrl Pts',(19.9502814943068,28.478220305484,-88.4045270067001));
#174036=CARTESIAN_POINT('Ctrl Pts',(19.9503629616386,28.4780304307791,-88.4060890616811));
#174037=CARTESIAN_POINT('Ctrl Pts',(19.9504440982641,28.4778418748811,-88.4076440907833));
#174038=CARTESIAN_POINT('Ctrl Pts',(19.9505249056845,28.4776546250721,-88.4091920933774));
#174039=CARTESIAN_POINT('Ctrl Pts',(19.950605713105,28.4774673752631,-88.4107400959714));
#174040=CARTESIAN_POINT('Ctrl Pts',(19.9506232874581,28.477426349047,-88.4110771956486));
#174041=CARTESIAN_POINT('Ctrl Pts',(19.9507663418393,28.4770967813136,-88.4138150210238));
#174042=CARTESIAN_POINT('Ctrl Pts',(19.9561774440553,28.4646307199664,-88.5173746102378));
#174043=CARTESIAN_POINT('Ctrl Pts',(19.9614261063647,28.4545670612358,-88.6180628114536));
#174044=CARTESIAN_POINT('Ctrl Pts',(19.9665083066635,28.4465583754429,-88.7157667717928));
#174045=CARTESIAN_POINT('Ctrl Pts',(19.9717269590573,28.4383346642888,-88.8160939876713));
#174046=CARTESIAN_POINT('Ctrl Pts',(19.97677011187,28.4322776514497,-88.9132749359466));
#174047=CARTESIAN_POINT('Ctrl Pts',(19.9816359372707,28.4280374234223,-89.0072367202588));
#174048=CARTESIAN_POINT('Ctrl Pts',(19.9866936397869,28.4236299878492,-89.1049037579766));
#174049=CARTESIAN_POINT('Ctrl Pts',(19.9915597727704,28.4211852765213,-89.1990930646804));
#174050=CARTESIAN_POINT('Ctrl Pts',(19.9962346717654,28.4203405465593,-89.289770015951));
#174051=CARTESIAN_POINT('Ctrl Pts',(19.9975038532053,28.4201112120666,-89.314387767843));
#174052=CARTESIAN_POINT('Ctrl Pts',(19.998758951749,28.4199999800001,-89.338746881695));
#174053=CARTESIAN_POINT('Ctrl Pts',(20.,28.4199999800001,-89.3628471840451));
#174054=CARTESIAN_POINT('Origin',(20.,28.9199999800001,-55.24995));
#174055=CARTESIAN_POINT('',(20.5,28.9199999800001,-91.34995));
#174056=CARTESIAN_POINT('',(20.5,28.9199999800001,-88.9338641536579));
#174057=CARTESIAN_POINT('',(20.,28.4199999800001,-91.34995));
#174058=CARTESIAN_POINT('Origin',(20.,28.9199999800001,-91.34995));
#174059=CARTESIAN_POINT('',(20.,28.4199999800001,-91.34995));
#174060=CARTESIAN_POINT('Origin',(21.,43.91999998,-58.24995));
#174061=CARTESIAN_POINT('',(21.,46.91999998,-58.24995));
#174062=CARTESIAN_POINT('',(20.5,46.41999998,-58.24995));
#174063=CARTESIAN_POINT('Origin',(21.,46.41999998,-58.24995));
#174064=CARTESIAN_POINT('',(20.5,43.91999998,-55.74995));
#174065=CARTESIAN_POINT('Origin',(20.5,43.91999998,-58.24995));
#174066=CARTESIAN_POINT('',(21.,43.91999998,-55.24995));
#174067=CARTESIAN_POINT('Origin',(21.,43.91999998,-55.74995));
#174068=CARTESIAN_POINT('Origin',(21.,43.91999998,-58.24995));
#174069=CARTESIAN_POINT('Origin',(0.,43.91999998,-58.24995));
#174070=CARTESIAN_POINT('',(21.5,46.91999998,-58.24995));
#174071=CARTESIAN_POINT('',(-39.,46.91999998,-58.24995));
#174072=CARTESIAN_POINT('',(21.5,43.91999998,-55.24995));
#174073=CARTESIAN_POINT('',(0.,43.91999998,-55.24995));
#174074=CARTESIAN_POINT('Origin',(21.5,43.91999998,-58.24995));
#174075=CARTESIAN_POINT('Origin',(21.5,43.91999998,-58.24995));
#174076=CARTESIAN_POINT('',(22.,43.91999998,-55.74995));
#174077=CARTESIAN_POINT('Origin',(21.5,43.91999998,-55.74995));
#174078=CARTESIAN_POINT('',(22.,46.41999998,-58.24995));
#174079=CARTESIAN_POINT('Origin',(22.,43.91999998,-58.24995));
#174080=CARTESIAN_POINT('Origin',(21.5,46.41999998,-58.24995));
#174081=CARTESIAN_POINT('Origin',(22.5,28.9199999800001,-55.24995));
#174082=CARTESIAN_POINT('',(22.,28.9199999800001,-87.1305533863517));
#174083=CARTESIAN_POINT('Origin',(22.5,28.91999998,-87.1305533863517));
#174084=CARTESIAN_POINT('',(22.5,28.4199999800001,-91.34995));
#174085=CARTESIAN_POINT('',(22.5,28.4199999800001,-87.5942752792638));
#174086=CARTESIAN_POINT('',(22.,28.9199999800001,-91.34995));
#174087=CARTESIAN_POINT('Origin',(22.5,28.9199999800001,-91.34995));
#174088=CARTESIAN_POINT('',(22.,28.9199999800001,-91.34995));
#174089=CARTESIAN_POINT('Ctrl Pts',(22.5,28.41999998,-87.1305533863517));
#174090=CARTESIAN_POINT('Ctrl Pts',(22.,28.41999998,-87.1305533863516));
#174091=CARTESIAN_POINT('Ctrl Pts',(22.,28.91999998,-87.1305533863517));
#174092=CARTESIAN_POINT('Ctrl Pts',(22.4639153689348,28.41999998,-86.4410479992692));
#174093=CARTESIAN_POINT('Ctrl Pts',(22.0000000000044,28.4548243482677,-86.4651291551651));
#174094=CARTESIAN_POINT('Ctrl Pts',(22.,28.9199999821681,-86.4796041157695));
#174095=CARTESIAN_POINT('Ctrl Pts',(22.4281188150557,28.5015955861724,-85.7652097651195));
#174096=CARTESIAN_POINT('Ctrl Pts',(22.,28.5601858706255,-85.7927489918333));
#174097=CARTESIAN_POINT('Ctrl Pts',(22.,28.9934360246446,-85.840664401161));
#174098=CARTESIAN_POINT('Ctrl Pts',(22.3573227200049,28.8261151186122,-84.4410318437717));
#174099=CARTESIAN_POINT('Ctrl Pts',(22.,28.9249341693522,-84.4905989888491));
#174100=CARTESIAN_POINT('Ctrl Pts',(22.,29.2855036056616,-84.5872260208873));
#174101=CARTESIAN_POINT('Ctrl Pts',(22.3220283366802,29.072521775155,-83.7873824528849));
#174102=CARTESIAN_POINT('Ctrl Pts',(22.,29.1803706436616,-83.8479871870358));
#174103=CARTESIAN_POINT('Ctrl Pts',(22.,29.5072644006254,-83.9676830002751));
#174104=CARTESIAN_POINT('Ctrl Pts',(22.2890532034791,29.4093902975657,-83.1809305852948));
#174105=CARTESIAN_POINT('Ctrl Pts',(22.,29.5283900973743,-83.2436286443491));
#174106=CARTESIAN_POINT('Ctrl Pts',(22.,29.8104512658091,-83.3922397161652));
#174107=CARTESIAN_POINT('',(22.,29.8104512658091,-83.3922397161652));
#174108=CARTESIAN_POINT('Origin',(22.5,29.8104512658091,-83.3922397161652));
#174109=CARTESIAN_POINT('Ctrl Pts',(22.,29.8104512658091,-83.3922397161652));
#174110=CARTESIAN_POINT('Ctrl Pts',(22.,29.7130107699212,-83.5771800425296));
#174111=CARTESIAN_POINT('Ctrl Pts',(22.,29.6241027734271,-83.7664339874128));
#174112=CARTESIAN_POINT('Ctrl Pts',(22.,29.5434345930966,-83.9588738468728));
#174113=CARTESIAN_POINT('Ctrl Pts',(22.,29.4578017187799,-84.1631573478909));
#174114=CARTESIAN_POINT('Ctrl Pts',(22.,29.3814538044554,-84.3710319263881));
#174115=CARTESIAN_POINT('Ctrl Pts',(22.,29.3140928258488,-84.5811807101608));
#174116=CARTESIAN_POINT('Ctrl Pts',(22.,29.2470690502148,-84.7902775081099));
#174117=CARTESIAN_POINT('Ctrl Pts',(22.,29.188942707981,-85.0016271465759));
#174118=CARTESIAN_POINT('Ctrl Pts',(22.,29.1394698146751,-85.2139452109128));
#174119=CARTESIAN_POINT('Ctrl Pts',(22.,29.0466872110912,-85.6121313989588));
#174120=CARTESIAN_POINT('Ctrl Pts',(22.,28.9832164657711,-86.0152044949698));
#174121=CARTESIAN_POINT('Ctrl Pts',(22.,28.9492578229235,-86.4231979120729));
#174122=CARTESIAN_POINT('Ctrl Pts',(22.,28.9297677681887,-86.6573596265579));
#174123=CARTESIAN_POINT('Ctrl Pts',(22.,28.9199999800002,-86.8931422598655));
#174124=CARTESIAN_POINT('Ctrl Pts',(22.,28.91999998,-87.1305533863517));
#174125=CARTESIAN_POINT('Ctrl Pts',(22.,41.1098595241823,-61.4386408691296));
#174126=CARTESIAN_POINT('Ctrl Pts',(22.,40.7995210108967,-61.2819013639433));
#174127=CARTESIAN_POINT('Ctrl Pts',(22.3259225534138,40.6914751389564,-61.2273317382593));
#174128=CARTESIAN_POINT('Ctrl Pts',(22.,37.3993732891074,-68.7852685139811));
#174129=CARTESIAN_POINT('Ctrl Pts',(22.,37.1246521940256,-68.5757439011997));
#174130=CARTESIAN_POINT('Ctrl Pts',(22.3157409333924,36.9852292354808,-68.5739513464269));
#174131=CARTESIAN_POINT('Ctrl Pts',(22.,33.6470169072337,-76.1105064350252));
#174132=CARTESIAN_POINT('Ctrl Pts',(22.,33.3938486289533,-75.8821367178777));
#174133=CARTESIAN_POINT('Ctrl Pts',(22.3038724392466,33.2381690210168,-75.8991829107314));
#174134=CARTESIAN_POINT('Ctrl Pts',(22.,29.8104512658091,-83.3922397161652));
#174135=CARTESIAN_POINT('Ctrl Pts',(22.,29.5283900973743,-83.243628644349));
#174136=CARTESIAN_POINT('Ctrl Pts',(22.2890532034791,29.4093902975657,-83.1809305852948));
#174137=CARTESIAN_POINT('',(22.,41.1098595241823,-61.4386408691296));
#174138=CARTESIAN_POINT('',(22.3259225534138,40.6914751389564,-61.2273317382593));
#174139=CARTESIAN_POINT('Origin',(22.5,41.1098595241823,-61.4386408691296));
#174140=CARTESIAN_POINT('Ctrl Pts',(22.2890532034791,29.4093902975657,-83.1809305852948));
#174141=CARTESIAN_POINT('Ctrl Pts',(22.2915992865075,30.0672102202902,-81.9298583665631));
#174142=CARTESIAN_POINT('Ctrl Pts',(22.2941161314434,30.7375917756893,-80.6490156487439));
#174143=CARTESIAN_POINT('Ctrl Pts',(22.2965989022532,31.4204400512108,-79.3383406087535));
#174144=CARTESIAN_POINT('Ctrl Pts',(22.2990071415531,32.0827895707544,-78.067011363099));
#174145=CARTESIAN_POINT('Ctrl Pts',(22.3013833157878,32.7568683731644,-76.7676139152288));
#174146=CARTESIAN_POINT('Ctrl Pts',(22.3037242761676,33.4426330710029,-75.4401153073922));
#174147=CARTESIAN_POINT('Ctrl Pts',(22.3059739143508,34.101645697684,-74.164403175777));
#174148=CARTESIAN_POINT('Ctrl Pts',(22.308191030053,34.7714501903432,-72.8627395683749));
#174149=CARTESIAN_POINT('Ctrl Pts',(22.310374071687,35.4520502432749,-71.5351181260537));
#174150=CARTESIAN_POINT('Ctrl Pts',(22.3125129104872,36.1188693171654,-70.2343787317024));
#174151=CARTESIAN_POINT('Ctrl Pts',(22.3146190356274,36.7960510223641,-68.908721970169));
#174152=CARTESIAN_POINT('Ctrl Pts',(22.3166922686174,37.4836420872136,-67.5581653122663));
#174153=CARTESIAN_POINT('Ctrl Pts',(22.318707401592,38.1519641882275,-66.2454564809706));
#174154=CARTESIAN_POINT('Ctrl Pts',(22.320691457232,38.8301203169625,-64.9092237355817));
#174155=CARTESIAN_POINT('Ctrl Pts',(22.3226455520959,39.5181964415169,-63.5495064562538));
#174156=CARTESIAN_POINT('Ctrl Pts',(22.3237472546366,39.9061280760574,-62.782909087359));
#174157=CARTESIAN_POINT('Ctrl Pts',(22.3248394573525,40.2972136823501,-62.0088473266159));
#174158=CARTESIAN_POINT('Ctrl Pts',(22.3259225534138,40.6914751389564,-61.2273317382593));
#174159=CARTESIAN_POINT('Ctrl Pts',(22.,41.1098595241823,-61.4386408691296));
#174160=CARTESIAN_POINT('Ctrl Pts',(22.,37.3993520818416,-68.7853105030709));
#174161=CARTESIAN_POINT('Ctrl Pts',(22.,33.6470396305176,-76.1104633065809));
#174162=CARTESIAN_POINT('Ctrl Pts',(22.,29.8104512658091,-83.3922397161652));
#174163=CARTESIAN_POINT('Ctrl Pts',(28.4933647440612,38.6927858841382,-60.650327573148));
#174164=CARTESIAN_POINT('Ctrl Pts',(29.,38.6926240909195,-60.6436056187277));
#174165=CARTESIAN_POINT('Ctrl Pts',(29.,38.7048160259599,-61.150138786574));
#174166=CARTESIAN_POINT('Ctrl Pts',(28.4508217728044,38.5151017970219,-60.6551690977179));
#174167=CARTESIAN_POINT('Ctrl Pts',(29.,38.5056874437974,-60.6032547660267));
#174168=CARTESIAN_POINT('Ctrl Pts',(29.,38.6042425482601,-61.1525595652015));
#174169=CARTESIAN_POINT('Ctrl Pts',(28.4075947879363,38.335472514688,-60.707925961796));
#174170=CARTESIAN_POINT('Ctrl Pts',(29.,38.2987442898004,-60.603134659432));
#174171=CARTESIAN_POINT('Ctrl Pts',(29.,38.5024684382473,-61.1789379706814));
#174172=CARTESIAN_POINT('Ctrl Pts',(28.3514280416523,38.1029959208976,-60.8540715547449));
#174173=CARTESIAN_POINT('Ctrl Pts',(29.0000000000001,37.990375163389,-60.6863576421133));
#174174=CARTESIAN_POINT('Ctrl Pts',(29.,38.3706532052714,-61.2520107824808));
#174175=CARTESIAN_POINT('Ctrl Pts',(28.3338483525148,38.0303960306507,-60.9145171861254));
#174176=CARTESIAN_POINT('Ctrl Pts',(29.,37.8822359354345,-60.7316627868476));
#174177=CARTESIAN_POINT('Ctrl Pts',(29.,38.3294709783247,-61.2822335925436));
#174178=CARTESIAN_POINT('Ctrl Pts',(28.302912455342,37.9028346914031,-61.0569005178125));
#174179=CARTESIAN_POINT('Ctrl Pts',(29.,37.6732261500514,-60.8640556435108));
#174180=CARTESIAN_POINT('Ctrl Pts',(29.,38.2570904307121,-61.3534252594253));
#174181=CARTESIAN_POINT('Ctrl Pts',(28.28982523324,37.8489775515987,-61.1370349799883));
#174182=CARTESIAN_POINT('Ctrl Pts',(29.,37.5759010011862,-60.9505556565881));
#174183=CARTESIAN_POINT('Ctrl Pts',(29.,38.2265217687548,-61.3934878926125));
#174184=CARTESIAN_POINT('Ctrl Pts',(28.2795019009908,37.8065307949999,-61.2273317382593));
#174185=CARTESIAN_POINT('Ctrl Pts',(29.,37.4942143736512,-61.0606306836509));
#174186=CARTESIAN_POINT('Ctrl Pts',(29.,38.2024209812184,-61.4386408691297));
#174187=CARTESIAN_POINT('',(28.49336474298,38.692785884125,-60.6503274733137));
#174188=CARTESIAN_POINT('',(29.,38.7048160259599,-61.150138786574));
#174189=CARTESIAN_POINT('Origin',(28.5,38.7048160259599,-61.150138786574));
#174190=CARTESIAN_POINT('Ctrl Pts',(29.,38.2024209812184,-61.4386408691297));
#174191=CARTESIAN_POINT('Ctrl Pts',(29.,38.2265260808242,-61.3934796764616));
#174192=CARTESIAN_POINT('Ctrl Pts',(29.,38.2570947542809,-61.3534209131338));
#174193=CARTESIAN_POINT('Ctrl Pts',(29.,38.293280667393,-61.3178293882391));
#174194=CARTESIAN_POINT('Ctrl Pts',(29.,38.3294709547425,-61.2822335609581));
#174195=CARTESIAN_POINT('Ctrl Pts',(29.,38.3706505444737,-61.2520122466304));
#174196=CARTESIAN_POINT('Ctrl Pts',(29.,38.4145916132166,-61.2276531730517));
#174197=CARTESIAN_POINT('Ctrl Pts',(29.,38.4390337855644,-61.2141034645061));
#174198=CARTESIAN_POINT('Ctrl Pts',(29.,38.4644512947928,-61.2023317240159));
#174199=CARTESIAN_POINT('Ctrl Pts',(29.,38.490593259323,-61.1923093713145));
#174200=CARTESIAN_POINT('Ctrl Pts',(29.,38.5172131854938,-61.1821037768321));
#174201=CARTESIAN_POINT('Ctrl Pts',(29.,38.5445857496398,-61.1737118246007));
#174202=CARTESIAN_POINT('Ctrl Pts',(29.,38.5724697430453,-61.1671525783509));
#174203=CARTESIAN_POINT('Ctrl Pts',(29.,38.5996144829857,-61.1607672291985));
#174204=CARTESIAN_POINT('Ctrl Pts',(29.,38.6272453201521,-61.1561187181941));
#174205=CARTESIAN_POINT('Ctrl Pts',(29.,38.6551404973774,-61.1532723608215));
#174206=CARTESIAN_POINT('Ctrl Pts',(29.,38.6716230181358,-61.1515905237032));
#174207=CARTESIAN_POINT('Ctrl Pts',(29.,38.688197742811,-61.1505387782063));
#174208=CARTESIAN_POINT('Ctrl Pts',(29.,38.7048160259599,-61.150138786574));
#174209=CARTESIAN_POINT('Ctrl Pts',(28.4933647440612,38.6927858841382,-60.650327573148));
#174210=CARTESIAN_POINT('Ctrl Pts',(28.4866112948369,38.6645795682284,-60.6510961370265));
#174211=CARTESIAN_POINT('Ctrl Pts',(28.4800601957753,38.6372412590608,-60.6530442725806));
#174212=CARTESIAN_POINT('Ctrl Pts',(28.4737238128436,38.6108170677176,-60.6559437523982));
#174213=CARTESIAN_POINT('Ctrl Pts',(28.4670685534825,38.5830630874591,-60.6589891476034));
#174214=CARTESIAN_POINT('Ctrl Pts',(28.4606500721898,38.5563171621938,-60.6630840224132));
#174215=CARTESIAN_POINT('Ctrl Pts',(28.4544730160308,38.5305935477136,-60.6680036899134));
#174216=CARTESIAN_POINT('Ctrl Pts',(28.4538555252183,38.5280220807886,-60.6684954855849));
#174217=CARTESIAN_POINT('Ctrl Pts',(28.4532404400623,38.525460801933,-60.6689955548281));
#174218=CARTESIAN_POINT('Ctrl Pts',(28.4526277607726,38.522909707497,-60.6695036937783));
#174219=CARTESIAN_POINT('Ctrl Pts',(28.4435667341815,38.485181103132,-60.6770186540817));
#174220=CARTESIAN_POINT('Ctrl Pts',(28.4350378093247,38.4497043204397,-60.6862892049898));
#174221=CARTESIAN_POINT('Ctrl Pts',(28.4270696258733,38.4165855517814,-60.6966603137934));
#174222=CARTESIAN_POINT('Ctrl Pts',(28.4242404806142,38.4048265595461,-60.7003426302813));
#174223=CARTESIAN_POINT('Ctrl Pts',(28.4214820436404,38.3933649319099,-60.7041640893731));
#174224=CARTESIAN_POINT('Ctrl Pts',(28.4187957564384,38.3822061546877,-60.7080959629319));
#174225=CARTESIAN_POINT('Ctrl Pts',(28.4157769158789,38.3696659582232,-60.7125145892669));
#174226=CARTESIAN_POINT('Ctrl Pts',(28.4128472428645,38.357500126538,-60.7170753249694));
#174227=CARTESIAN_POINT('Ctrl Pts',(28.4100050480235,38.3457010004413,-60.7217450693001));
#174228=CARTESIAN_POINT('Ctrl Pts',(28.4038012283365,38.3199463795004,-60.7319379847875));
#174229=CARTESIAN_POINT('Ctrl Pts',(28.3980168462861,38.2959498502083,-60.7426442520555));
#174230=CARTESIAN_POINT('Ctrl Pts',(28.3926401637082,38.2736568809467,-60.7535341130708));
#174231=CARTESIAN_POINT('Ctrl Pts',(28.3876929931094,38.2531447676696,-60.7635540462657));
#174232=CARTESIAN_POINT('Ctrl Pts',(28.3830906731624,38.234073632809,-60.7737303004237));
#174233=CARTESIAN_POINT('Ctrl Pts',(28.3788195853896,38.2163832003577,-60.7838358975799));
#174234=CARTESIAN_POINT('Ctrl Pts',(28.3762732387338,38.2058364787947,-60.7898606750819));
#174235=CARTESIAN_POINT('Ctrl Pts',(28.3738445066921,38.1957800356412,-60.7958609581478));
#174236=CARTESIAN_POINT('Ctrl Pts',(28.3715298746371,38.1861985984285,-60.8017935811565));
#174237=CARTESIAN_POINT('Ctrl Pts',(28.3710654296699,38.1842760249112,-60.8029839979626));
#174238=CARTESIAN_POINT('Ctrl Pts',(28.3706055595698,38.1823724975692,-60.8041717490278));
#174239=CARTESIAN_POINT('Ctrl Pts',(28.3701502904136,38.1804881188278,-60.8053563570953));
#174240=CARTESIAN_POINT('Ctrl Pts',(28.3697831735728,38.1789686063346,-60.8063115932792));
#174241=CARTESIAN_POINT('Ctrl Pts',(28.3694189788947,38.1774612515492,-60.8072648797398));
#174242=CARTESIAN_POINT('Ctrl Pts',(28.3690577461341,38.1759662158436,-60.8082158932158));
#174243=CARTESIAN_POINT('Ctrl Pts',(28.3687139645852,38.1745434055486,-60.8091209630808));
#174244=CARTESIAN_POINT('Ctrl Pts',(28.3685506475493,38.1738674773002,-60.8095518784965));
#174245=CARTESIAN_POINT('Ctrl Pts',(28.3681154374745,38.1720662519997,-60.8107093564416));
#174246=CARTESIAN_POINT('Ctrl Pts',(28.3680374556281,38.1717435047037,-60.8109167557474));
#174247=CARTESIAN_POINT('Ctrl Pts',(28.3679507553739,38.1713846756153,-60.8111475922255));
#174248=CARTESIAN_POINT('Ctrl Pts',(28.3678527542032,38.1709790791434,-60.8114089693127));
#174249=CARTESIAN_POINT('Ctrl Pts',(28.3607255558591,38.1414818141342,-60.8304177865576));
#174250=CARTESIAN_POINT('Ctrl Pts',(28.3539183117575,38.113332878083,-60.850746794587));
#174251=CARTESIAN_POINT('Ctrl Pts',(28.3474565546205,38.0866307902112,-60.8721473077096));
#174252=CARTESIAN_POINT('Ctrl Pts',(28.3407512736884,38.0589223825975,-60.8943543404928));
#174253=CARTESIAN_POINT('Ctrl Pts',(28.334417972381,38.032771774352,-60.9177151428445));
#174254=CARTESIAN_POINT('Ctrl Pts',(28.3284731047364,38.008240394159,-60.9419785882647));
#174255=CARTESIAN_POINT('Ctrl Pts',(28.32497451288,37.9938035232142,-60.9562577779171));
#174256=CARTESIAN_POINT('Ctrl Pts',(28.3216102278411,37.9799265561799,-60.970850091482));
#174257=CARTESIAN_POINT('Ctrl Pts',(28.3183818526901,37.9666149649566,-60.9857084492844));
#174258=CARTESIAN_POINT('Ctrl Pts',(28.3093491455501,37.9293703141764,-61.0272808156703));
#174259=CARTESIAN_POINT('Ctrl Pts',(28.3014724081544,37.8969287820801,-61.0703254314474));
#174260=CARTESIAN_POINT('Ctrl Pts',(28.2946292360272,37.8687619975003,-61.1144056260449));
#174261=CARTESIAN_POINT('Ctrl Pts',(28.2888847384778,37.8451174037381,-61.1514087241892));
#174262=CARTESIAN_POINT('Ctrl Pts',(28.2838681852101,37.8244837283527,-61.1891405466858));
#174263=CARTESIAN_POINT('Ctrl Pts',(28.2795019009908,37.8065307949998,-61.2273317382593));
#174264=CARTESIAN_POINT('Ctrl Pts',(22.3259225534138,40.6914751389564,-61.2273317382593));
#174265=CARTESIAN_POINT('Ctrl Pts',(22.,40.7995210108967,-61.2819013639433));
#174266=CARTESIAN_POINT('Ctrl Pts',(22.,41.1098595241823,-61.4386408691297));
#174267=CARTESIAN_POINT('Ctrl Pts',(22.3307532272019,40.7164963923335,-61.1738110360374));
#174268=CARTESIAN_POINT('Ctrl Pts',(22.,40.8194184511061,-61.2339961299344));
#174269=CARTESIAN_POINT('Ctrl Pts',(22.,41.1233751604146,-61.4118804447591));
#174270=CARTESIAN_POINT('Ctrl Pts',(22.3364246839863,40.745888690896,-61.1232259520736));
#174271=CARTESIAN_POINT('Ctrl Pts',(22.,40.8429002807173,-61.1881281443964));
#174272=CARTESIAN_POINT('Ctrl Pts',(22.,41.1392509618672,-61.3865876948747));
#174273=CARTESIAN_POINT('Ctrl Pts',(22.3428990418276,40.7794755973204,-61.0754935261973));
#174274=CARTESIAN_POINT('Ctrl Pts',(22.,40.8698280768405,-61.1441646043172));
#174275=CARTESIAN_POINT('Ctrl Pts',(22.,41.1573899115079,-61.3627217630986));
#174276=CARTESIAN_POINT('',(22.,41.1573899115079,-61.3627217630986));
#174277=CARTESIAN_POINT('',(22.3428990418278,40.7794755973209,-61.0754935261978));
#174278=CARTESIAN_POINT('Origin',(22.5,41.1573899115079,-61.3627217630986));
#174279=CARTESIAN_POINT('Origin',(22.4949966047551,41.5721884749956,-61.6542986908816));
#174280=CARTESIAN_POINT('Origin',(22.,41.5483105744962,-61.6603021206194));
#174281=CARTESIAN_POINT('Origin',(0.,-12.9675000200281,-60.64995));
#174282=CARTESIAN_POINT('Origin',(0.,-12.9675000200281,-61.2273317382593));
#174283=CARTESIAN_POINT('Origin',(24.2,-70.08000002,-58.24995));
#174284=CARTESIAN_POINT('',(24.2,-70.08000002,-55.24995));
#174285=CARTESIAN_POINT('',(23.7,-70.08000002,-55.74995));
#174286=CARTESIAN_POINT('Origin',(24.2,-70.08000002,-55.74995));
#174287=CARTESIAN_POINT('',(23.7,-72.58000002,-58.24995));
#174288=CARTESIAN_POINT('Origin',(23.7,-70.08000002,-58.24995));
#174289=CARTESIAN_POINT('Origin',(24.2,-72.58000002,-58.24995));
#174290=CARTESIAN_POINT('Origin',(24.2,-70.08000002,-58.24995));
#174291=CARTESIAN_POINT('Origin',(24.2,-72.58000002,-55.24995));
#174292=CARTESIAN_POINT('',(23.7,-72.58000002,-174.34995));
#174293=CARTESIAN_POINT('',(23.7,-72.58000002,-58.24995));
#174294=CARTESIAN_POINT('Origin',(24.2,-72.58000002,-174.34995));
#174295=CARTESIAN_POINT('Origin',(24.2,-70.08000002,-174.34995));
#174296=CARTESIAN_POINT('',(23.7,-70.08000002,-176.84995));
#174297=CARTESIAN_POINT('Origin',(23.7,-70.08000002,-174.34995));
#174298=CARTESIAN_POINT('Origin',(24.2,-70.08000002,-176.84995));
#174299=CARTESIAN_POINT('Ctrl Pts',(23.7,-55.9902808012637,-149.835491960129));
#174300=CARTESIAN_POINT('Ctrl Pts',(23.6999999999999,-55.2903249255959,
-150.206318626088));
#174301=CARTESIAN_POINT('Ctrl Pts',(22.9849163103247,-55.591423110293,-150.046801090999));
#174302=CARTESIAN_POINT('Ctrl Pts',(23.7,-59.7506418899787,-156.933381838169));
#174303=CARTESIAN_POINT('Ctrl Pts',(23.7,-58.9786022357095,-157.10917403496));
#174304=CARTESIAN_POINT('Ctrl Pts',(22.9994804181366,-59.343937645489,-157.144704426787));
#174305=CARTESIAN_POINT('Ctrl Pts',(23.7,-63.4274104915032,-164.074673486974));
#174306=CARTESIAN_POINT('Ctrl Pts',(23.7000000002973,-62.707250125371,-164.298966961939));
#174307=CARTESIAN_POINT('Ctrl Pts',(23.0112491123844,-63.0152939322715,
-164.285990110815));
#174308=CARTESIAN_POINT('Ctrl Pts',(23.7,-67.0618271655313,-171.237717270032));
#174309=CARTESIAN_POINT('Ctrl Pts',(23.7,-66.413901371901,-171.56646471025));
#174310=CARTESIAN_POINT('Ctrl Pts',(23.0213852109847,-66.6453596297547,
-171.449026400902));
#174311=CARTESIAN_POINT('',(23.0213852109847,-66.6453596297547,-171.449026400902));
#174312=CARTESIAN_POINT('',(23.7,-67.0618271655313,-171.237717270032));
#174313=CARTESIAN_POINT('Origin',(23.2,-67.0618271655313,-171.237717270032));
#174314=CARTESIAN_POINT('',(23.7,-55.9902808012637,-149.835491960129));
#174315=CARTESIAN_POINT('Ctrl Pts',(23.7,-55.9902808012637,-149.835491960129));
#174316=CARTESIAN_POINT('Ctrl Pts',(23.7,-59.7506641394806,-156.933423835337));
#174317=CARTESIAN_POINT('Ctrl Pts',(23.7,-63.4273897219659,-164.074632552453));
#174318=CARTESIAN_POINT('Ctrl Pts',(23.7,-67.0618271655313,-171.237717270032));
#174319=CARTESIAN_POINT('Origin',(23.2,-55.9902808012637,-149.835491960129));
#174320=CARTESIAN_POINT('Ctrl Pts',(23.0213852109847,-66.6453596297547,
-171.449026400902));
#174321=CARTESIAN_POINT('Ctrl Pts',(23.0194522730378,-65.9531118514689,
-170.083046727027));
#174322=CARTESIAN_POINT('Ctrl Pts',(23.0174911199861,-65.2705560001936,
-168.739955519058));
#174323=CARTESIAN_POINT('Ctrl Pts',(23.0155001081443,-64.5975812226656,
-167.419805386397));
#174324=CARTESIAN_POINT('Ctrl Pts',(23.0134670373099,-63.9103902357703,
-166.071767833125));
#174325=CARTESIAN_POINT('Ctrl Pts',(23.0114028370452,-63.2331895248465,
-164.747650752542));
#174326=CARTESIAN_POINT('Ctrl Pts',(23.009307102834,-62.5659090224749,-163.447484054915));
#174327=CARTESIAN_POINT('Ctrl Pts',(23.0071368764899,-61.8749102701637,
-162.101103390916));
#174328=CARTESIAN_POINT('Ctrl Pts',(23.0049328366384,-61.1945495374443,
-160.780405954722));
#174329=CARTESIAN_POINT('Ctrl Pts',(23.0026959184795,-60.5247985662132,
-159.485397982963));
#174330=CARTESIAN_POINT('Ctrl Pts',(23.0004093438121,-59.8401800439888,
-158.16164261421));
#174331=CARTESIAN_POINT('Ctrl Pts',(22.9980884208888,-59.1666477519959,
-156.864729804607));
#174332=CARTESIAN_POINT('Ctrl Pts',(22.9957355042192,-58.5042202747206,
-155.594639653445));
#174333=CARTESIAN_POINT('Ctrl Pts',(22.9932955694915,-57.8172942024143,
-154.277577682221));
#174334=CARTESIAN_POINT('Ctrl Pts',(22.990821234914,-57.1423096389527,-152.989358956594));
#174335=CARTESIAN_POINT('Ctrl Pts',(22.9883164942772,-56.4793368434331,
-151.729934291109));
#174336=CARTESIAN_POINT('Ctrl Pts',(22.9871890935365,-56.1809282937553,
-151.163058711302));
#174337=CARTESIAN_POINT('Ctrl Pts',(22.9860555502485,-55.8849539210098,
-150.602016347596));
#174338=CARTESIAN_POINT('Ctrl Pts',(22.9849163103247,-55.591423110293,-150.046801090999));
#174339=CARTESIAN_POINT('Ctrl Pts',(22.9849163103247,-55.591423110293,-150.046801090999));
#174340=CARTESIAN_POINT('Ctrl Pts',(23.7,-55.2903249255959,-150.206318626088));
#174341=CARTESIAN_POINT('Ctrl Pts',(23.7,-55.9902808012637,-149.835491960129));
#174342=CARTESIAN_POINT('Ctrl Pts',(23.0185164903604,-55.2457834197403,
-149.428587397877));
#174343=CARTESIAN_POINT('Ctrl Pts',(23.6999999999934,-55.0174267883622,
-149.559543666635));
#174344=CARTESIAN_POINT('Ctrl Pts',(23.7,-55.679180688293,-149.248273246943));
#174345=CARTESIAN_POINT('Ctrl Pts',(23.0536516940073,-54.9992937875436,
-148.778013896122));
#174346=CARTESIAN_POINT('Ctrl Pts',(23.6999999999976,-54.8189393966138,
-148.866857423336));
#174347=CARTESIAN_POINT('Ctrl Pts',(23.7,-55.4573644110639,-148.631050162126));
#174348=CARTESIAN_POINT('Ctrl Pts',(23.1260141051261,-54.6648889616571,
-147.425793812224));
#174349=CARTESIAN_POINT('Ctrl Pts',(23.7000000000022,-54.5876251483541,
-147.465034950376));
#174350=CARTESIAN_POINT('Ctrl Pts',(23.7,-55.1564000672167,-147.34971633988));
#174351=CARTESIAN_POINT('Ctrl Pts',(23.1633521516227,-54.58000002,-146.721873935393));
#174352=CARTESIAN_POINT('Ctrl Pts',(23.7,-54.5419546351293,-146.748518174438));
#174353=CARTESIAN_POINT('Ctrl Pts',(23.7,-55.0800000213654,-146.683510743886));
#174354=CARTESIAN_POINT('Ctrl Pts',(23.2,-54.58000002,-146.023178055809));
#174355=CARTESIAN_POINT('Ctrl Pts',(23.7,-54.58000002,-146.023178055809));
#174356=CARTESIAN_POINT('Ctrl Pts',(23.7,-55.08000002,-146.023178055809));
#174357=CARTESIAN_POINT('',(23.7,-55.08000002,-146.023178055809));
#174358=CARTESIAN_POINT('Ctrl Pts',(23.7,-55.08000002,-146.023178055809));
#174359=CARTESIAN_POINT('Ctrl Pts',(23.7,-55.08000002,-146.158053606653));
#174360=CARTESIAN_POINT('Ctrl Pts',(23.7000000000707,-55.0831707493112,
-146.292669951121));
#174361=CARTESIAN_POINT('Ctrl Pts',(23.6999999992499,-55.0894565008803,
-146.427026468199));
#174362=CARTESIAN_POINT('Ctrl Pts',(23.6999999984213,-55.0958009827677,
-146.562638332538));
#174363=CARTESIAN_POINT('Ctrl Pts',(23.6999999964552,-55.1053189899911,
-146.697986218053));
#174364=CARTESIAN_POINT('Ctrl Pts',(23.6999999951529,-55.118005919724,-146.833072917224));
#174365=CARTESIAN_POINT('Ctrl Pts',(23.6999999945721,-55.1236634789143,
-146.893312944755));
#174366=CARTESIAN_POINT('Ctrl Pts',(23.6999999941814,-55.1299519000527,
-146.953501011813));
#174367=CARTESIAN_POINT('Ctrl Pts',(23.6999999942164,-55.1368740952971,
-147.013636993293));
#174368=CARTESIAN_POINT('Ctrl Pts',(23.6999999943017,-55.1537261451256,
-147.160037740544));
#174369=CARTESIAN_POINT('Ctrl Pts',(23.6999999965898,-55.1743560689037,
-147.306288458158));
#174370=CARTESIAN_POINT('Ctrl Pts',(23.6999999980531,-55.1987232126618,
-147.451788749128));
#174371=CARTESIAN_POINT('Ctrl Pts',(23.6999999995039,-55.2228814172676,
-147.596041429475));
#174372=CARTESIAN_POINT('Ctrl Pts',(23.699999999956,-55.2507128773888,-147.739555725363));
#174373=CARTESIAN_POINT('Ctrl Pts',(23.6999999999927,-55.2821282400243,
-147.881757850271));
#174374=CARTESIAN_POINT('Ctrl Pts',(23.700000000002,-55.2901469859137,-147.918054827575));
#174375=CARTESIAN_POINT('Ctrl Pts',(23.7,-55.298398982964,-147.954266404713));
#174376=CARTESIAN_POINT('Ctrl Pts',(23.7,-55.3068822390434,-147.990383251025));
#174377=CARTESIAN_POINT('Ctrl Pts',(23.7,-55.3875157587036,-148.333674601652));
#174378=CARTESIAN_POINT('Ctrl Pts',(23.7,-55.4886143891028,-148.670181748626));
#174379=CARTESIAN_POINT('Ctrl Pts',(23.7,-55.6129610034793,-148.998982220304));
#174380=CARTESIAN_POINT('Ctrl Pts',(23.7,-55.7206760510301,-149.283805081137));
#174381=CARTESIAN_POINT('Ctrl Pts',(23.7,-55.8458362712953,-149.562844907636));
#174382=CARTESIAN_POINT('Ctrl Pts',(23.7,-55.9902808012637,-149.835491960129));
#174383=CARTESIAN_POINT('Origin',(23.2,-55.08000002,-146.023178055809));
#174384=CARTESIAN_POINT('Origin',(23.2,-55.08000002,-55.24995));
#174385=CARTESIAN_POINT('',(23.7,-55.08000002,-86.035464915697));
#174386=CARTESIAN_POINT('',(23.7,-55.08000002,-146.505061715151));
#174387=CARTESIAN_POINT('Origin',(23.2,-55.08000002,-86.035464915697));
#174388=CARTESIAN_POINT('Ctrl Pts',(23.2,-54.58000002,-86.035464915697));
#174389=CARTESIAN_POINT('Ctrl Pts',(23.7,-54.58000002,-86.0354649156969));
#174390=CARTESIAN_POINT('Ctrl Pts',(23.7,-55.08000002,-86.035464915697));
#174391=CARTESIAN_POINT('Ctrl Pts',(23.163155884673,-54.58000002,-85.3330272043393));
#174392=CARTESIAN_POINT('Ctrl Pts',(23.7,-54.5417374496194,-85.3059841364058));
#174393=CARTESIAN_POINT('Ctrl Pts',(23.7,-55.0800000221098,-85.3715851430748));
#174394=CARTESIAN_POINT('Ctrl Pts',(23.1266268844869,-54.6631759768986,
-84.6443771511225));
#174395=CARTESIAN_POINT('Ctrl Pts',(23.6999999999999,-54.5866204760292,
-84.6055144627376));
#174396=CARTESIAN_POINT('Ctrl Pts',(23.7,-55.1548583802702,-84.7198400663338));
#174397=CARTESIAN_POINT('Ctrl Pts',(23.054421382878,-54.9946392637262,-83.2949364184621));
#174398=CARTESIAN_POINT('Ctrl Pts',(23.7,-54.8153941542428,-83.2070098309739));
#174399=CARTESIAN_POINT('Ctrl Pts',(23.7,-55.4531753402921,-83.4411601721359));
#174400=CARTESIAN_POINT('Ctrl Pts',(23.0184485767712,-55.2464820601011,
-82.6288059779555));
#174401=CARTESIAN_POINT('Ctrl Pts',(23.7000000000021,-55.01791265188,-82.4979478032362));
#174402=CARTESIAN_POINT('Ctrl Pts',(23.7,-55.6798282904624,-82.8091473369244));
#174403=CARTESIAN_POINT('Ctrl Pts',(22.9849163103247,-55.591423110293,-82.011841880507));
#174404=CARTESIAN_POINT('Ctrl Pts',(23.7,-55.290324925596,-81.8523243454179));
#174405=CARTESIAN_POINT('Ctrl Pts',(23.7,-55.9902808012637,-82.2231510113773));
#174406=CARTESIAN_POINT('',(23.7,-55.9902808012638,-82.2231510113773));
#174407=CARTESIAN_POINT('Ctrl Pts',(23.7,-55.9902808012637,-82.2231510113773));
#174408=CARTESIAN_POINT('Ctrl Pts',(23.7,-55.895308966207,-82.4024156114538));
#174409=CARTESIAN_POINT('Ctrl Pts',(23.7,-55.8083129339555,-82.5857246305521));
#174410=CARTESIAN_POINT('Ctrl Pts',(23.7,-55.7290034297555,-82.7720704820173));
#174411=CARTESIAN_POINT('Ctrl Pts',(23.7,-55.6467059711239,-82.9654368402717));
#174412=CARTESIAN_POINT('Ctrl Pts',(23.7,-55.5726850268913,-83.1620740930086));
#174413=CARTESIAN_POINT('Ctrl Pts',(23.7,-55.5066653875376,-83.3608873091128));
#174414=CARTESIAN_POINT('Ctrl Pts',(23.7,-55.4379479535128,-83.5678247325011));
#174415=CARTESIAN_POINT('Ctrl Pts',(23.7,-55.3778989830437,-83.77712082886));
#174416=CARTESIAN_POINT('Ctrl Pts',(23.7,-55.3262609792119,-83.9875567996252));
#174417=CARTESIAN_POINT('Ctrl Pts',(23.7,-55.3186643927325,-84.018514523233));
#174418=CARTESIAN_POINT('Ctrl Pts',(23.7,-55.3112499282573,-84.049496922863));
#174419=CARTESIAN_POINT('Ctrl Pts',(23.7,-55.304016859788,-84.0805001191198));
#174420=CARTESIAN_POINT('Ctrl Pts',(23.7,-55.21004869831,-84.4832770822505));
#174421=CARTESIAN_POINT('Ctrl Pts',(23.7,-55.1455757138287,-84.8909305418253));
#174422=CARTESIAN_POINT('Ctrl Pts',(23.7,-55.1107223807412,-85.3034811063192));
#174423=CARTESIAN_POINT('Ctrl Pts',(23.7,-55.090251973458,-85.5457844194318));
#174424=CARTESIAN_POINT('Ctrl Pts',(23.7,-55.0800000200001,-85.7897771817885));
#174425=CARTESIAN_POINT('Ctrl Pts',(23.7,-55.08000002,-86.035464915697));
#174426=CARTESIAN_POINT('',(22.9849163801915,-55.5914230811224,-82.0118419126005));
#174427=CARTESIAN_POINT('Origin',(23.2,-55.9902808012638,-82.2231510113773));
#174428=CARTESIAN_POINT('Ctrl Pts',(23.2,-54.58000002,-86.035464915697));
#174429=CARTESIAN_POINT('Ctrl Pts',(23.1920402965293,-54.5800017017972,
-85.8837121586465));
#174430=CARTESIAN_POINT('Ctrl Pts',(23.1835403629471,-54.5839598123894,
-85.7206407633663));
#174431=CARTESIAN_POINT('Ctrl Pts',(23.1697796176188,-54.5986644019983,
-85.4593001058024));
#174432=CARTESIAN_POINT('Ctrl Pts',(23.165027521493,-54.6050321375862,-85.3694015520161));
#174433=CARTESIAN_POINT('Ctrl Pts',(23.1576641956209,-54.6171785178051,
-85.2304493091738));
#174434=CARTESIAN_POINT('Ctrl Pts',(23.1539241950504,-54.6239008049671,
-85.1599475867037));
#174435=CARTESIAN_POINT('Ctrl Pts',(23.1494668404016,-54.6329698265421,
-85.0759224813336));
#174436=CARTESIAN_POINT('Ctrl Pts',(23.1472161062405,-54.6378224902552,
-85.033469831222));
#174437=CARTESIAN_POINT('Ctrl Pts',(23.1460854202932,-54.6403298113479,
-85.0121338935036));
#174438=CARTESIAN_POINT('Ctrl Pts',(23.1455997231209,-54.6414218885205,
-85.0029664772816));
#174439=CARTESIAN_POINT('Ctrl Pts',(23.1452756792326,-54.6421538486887,
-84.9968496620711));
#174440=CARTESIAN_POINT('Ctrl Pts',(23.1450102786686,-54.6427571616886,
-84.991839171787));
#174441=CARTESIAN_POINT('Ctrl Pts',(23.1411745835637,-54.651500893296,-84.9194207908848));
#174442=CARTESIAN_POINT('Ctrl Pts',(23.1350026391964,-54.6665568729644,
-84.7980543962098));
#174443=CARTESIAN_POINT('Ctrl Pts',(23.1214040625537,-54.7085737971116,
-84.5416144084218));
#174444=CARTESIAN_POINT('Ctrl Pts',(23.116147164529,-54.7259043978822,-84.4437479506998));
#174445=CARTESIAN_POINT('Ctrl Pts',(23.1072156913328,-54.7588787344353,
-84.2786960342647));
#174446=CARTESIAN_POINT('Ctrl Pts',(23.1040658786267,-54.7710385863112,
-84.2206390915918));
#174447=CARTESIAN_POINT('Ctrl Pts',(23.0991086491905,-54.791325856885,-84.1290624366227));
#174448=CARTESIAN_POINT('Ctrl Pts',(23.0965721813468,-54.8019818279521,
-84.0821516295463));
#174449=CARTESIAN_POINT('Ctrl Pts',(23.0935208041597,-54.8153795734307,
-84.0254767767619));
#174450=CARTESIAN_POINT('Ctrl Pts',(23.0921945341807,-54.8213361128053,
-84.0007729266273));
#174451=CARTESIAN_POINT('Ctrl Pts',(23.0913063774615,-54.8253557005597,
-83.9842118158473));
#174452=CARTESIAN_POINT('Ctrl Pts',(23.0907645078269,-54.8278300533453,
-83.9740948772035));
#174453=CARTESIAN_POINT('Ctrl Pts',(23.0791426045535,-54.8812408887612,
-83.7568936655029));
#174454=CARTESIAN_POINT('Ctrl Pts',(23.0688848562799,-54.9361530157815,
-83.5685045958181));
#174455=CARTESIAN_POINT('Ctrl Pts',(23.0554633667156,-55.0166580274008,
-83.3187294874312));
#174456=CARTESIAN_POINT('Ctrl Pts',(23.051304010892,-55.043196963619,-83.2409289274376));
#174457=CARTESIAN_POINT('Ctrl Pts',(23.0455019800433,-55.0818833389378,
-83.1322819992919));
#174458=CARTESIAN_POINT('Ctrl Pts',(23.0427094889204,-55.1009475486401,
-83.0799715449524));
#174459=CARTESIAN_POINT('Ctrl Pts',(23.0396275793895,-55.1225688432194,
-83.0224327427873));
#174460=CARTESIAN_POINT('Ctrl Pts',(23.0381285275456,-55.1332091208129,
-82.9945316065666));
#174461=CARTESIAN_POINT('Ctrl Pts',(23.0374948273548,-55.1377311211599,
-82.9827595784604));
#174462=CARTESIAN_POINT('Ctrl Pts',(23.0370742789371,-55.1407371415232,
-82.974952753697));
#174463=CARTESIAN_POINT('Ctrl Pts',(23.0369652251154,-55.1415168257422,
-82.9729283381724));
#174464=CARTESIAN_POINT('Ctrl Pts',(23.0169042607352,-55.2853799515071,
-82.6010865135727));
#174465=CARTESIAN_POINT('Ctrl Pts',(22.9996766784886,-55.4395892989142,
-82.2834139753259));
#174466=CARTESIAN_POINT('Ctrl Pts',(22.9849163124813,-55.5914230881085,
-82.0118419201865));
#174467=CARTESIAN_POINT('Ctrl Pts',(23.7,-66.9393955463102,-61.0621827299711));
#174468=CARTESIAN_POINT('Ctrl Pts',(23.6999999999999,-66.2910081673095,
-60.7330850354506));
#174469=CARTESIAN_POINT('Ctrl Pts',(23.0210431649761,-66.5230748737403,
-60.8508735991007));
#174470=CARTESIAN_POINT('Ctrl Pts',(23.7,-63.3447762129971,-68.1442919238122));
#174471=CARTESIAN_POINT('Ctrl Pts',(23.7000000000839,-62.6252669058498,
-67.9176543808627));
#174472=CARTESIAN_POINT('Ctrl Pts',(23.0109831737233,-62.9327835325611,
-67.9329755599233));
#174473=CARTESIAN_POINT('Ctrl Pts',(23.7,-59.7084208561779,-75.2049556739983));
#174474=CARTESIAN_POINT('Ctrl Pts',(23.7000000000403,-58.9382045046749,
-75.0250759674623));
#174475=CARTESIAN_POINT('Ctrl Pts',(22.9993168926453,-59.3018045077389,
-74.9936336228867));
#174476=CARTESIAN_POINT('Ctrl Pts',(23.7,-55.9902808012637,-82.2231510113773));
#174477=CARTESIAN_POINT('Ctrl Pts',(23.7,-55.290324925596,-81.8523243454179));
#174478=CARTESIAN_POINT('Ctrl Pts',(22.9849163103247,-55.591423110293,-82.011841880507));
#174479=CARTESIAN_POINT('',(23.7,-66.9393955463102,-61.0621827299711));
#174480=CARTESIAN_POINT('Ctrl Pts',(23.7,-66.9393955463102,-61.0621827299711));
#174481=CARTESIAN_POINT('Ctrl Pts',(23.7,-63.3447563953728,-68.1443309684329));
#174482=CARTESIAN_POINT('Ctrl Pts',(23.7,-59.7084420726901,-75.2049156266561));
#174483=CARTESIAN_POINT('Ctrl Pts',(23.7,-55.9902808012637,-82.2231510113772));
#174484=CARTESIAN_POINT('',(23.0210431649761,-66.5230748737403,-60.8508735991007));
#174485=CARTESIAN_POINT('Origin',(23.2,-66.9393955463102,-61.0621827299711));
#174486=CARTESIAN_POINT('Ctrl Pts',(22.9849163103247,-55.591423110293,-82.011841880507));
#174487=CARTESIAN_POINT('Ctrl Pts',(22.9874520115223,-56.2447590890542,
-80.7760530302538));
#174488=CARTESIAN_POINT('Ctrl Pts',(22.9899593093536,-56.9101806270537,
-79.5114224368043));
#174489=CARTESIAN_POINT('Ctrl Pts',(22.9924336508059,-57.5875975912162,
-78.2178899897237));
#174490=CARTESIAN_POINT('Ctrl Pts',(22.9948354544934,-58.2451554076757,
-76.9622787245506));
#174491=CARTESIAN_POINT('Ctrl Pts',(22.9972062002304,-58.9140154656596,
-75.679435243296));
#174492=CARTESIAN_POINT('Ctrl Pts',(22.9995429153294,-59.5941386568059,
-74.3693281841293));
#174493=CARTESIAN_POINT('Ctrl Pts',(23.0017912304752,-60.2485321994087,
-73.1087836080915));
#174494=CARTESIAN_POINT('Ctrl Pts',(23.0040080387239,-60.9133527386916,
-71.8229992084517));
#174495=CARTESIAN_POINT('Ctrl Pts',(23.0061918653351,-61.5886078011582,
-70.5119701265815));
#174496=CARTESIAN_POINT('Ctrl Pts',(23.0083322086256,-62.2504175048093,
-69.2270456345218));
#174497=CARTESIAN_POINT('Ctrl Pts',(23.010440865525,-62.9222501651157,-67.9178716804198));
#174498=CARTESIAN_POINT('Ctrl Pts',(23.0125176561367,-63.6041562644662,
-66.5844673204324));
#174499=CARTESIAN_POINT('Ctrl Pts',(23.0145386178111,-64.2677311499829,
-65.2869079550462));
#174500=CARTESIAN_POINT('Ctrl Pts',(23.0165294006075,-64.9408450698268,
-63.9664033639007));
#174501=CARTESIAN_POINT('Ctrl Pts',(23.018491050079,-65.6235878475027,-62.6229946789642));
#174502=CARTESIAN_POINT('Ctrl Pts',(23.019347233991,-65.9215785899104,-62.0366488918377));
#174503=CARTESIAN_POINT('Ctrl Pts',(23.0201978841437,-66.2214041884932,
-61.4459402241975));
#174504=CARTESIAN_POINT('Ctrl Pts',(23.0210431649761,-66.5230748737403,
-60.8508735991007));
#174505=CARTESIAN_POINT('Ctrl Pts',(25.1782904241482,-54.58000002,-84.0816077695088));
#174506=CARTESIAN_POINT('Ctrl Pts',(23.9800920467566,-54.58000002,-82.9059773201362));
#174507=CARTESIAN_POINT('Ctrl Pts',(23.0246352694011,-55.592944139339,-81.9685164608053));
#174508=CARTESIAN_POINT('Ctrl Pts',(23.9841110090257,-54.58000002,-85.2987111873827));
#174509=CARTESIAN_POINT('Ctrl Pts',(22.8383173576728,-54.5800000199764,
-84.1257656115248));
#174510=CARTESIAN_POINT('Ctrl Pts',(21.9095359072908,-55.5502317234241,
-83.1856130754768));
#174511=CARTESIAN_POINT('Ctrl Pts',(22.7486109694941,-54.58000002,-86.4914322348344));
#174512=CARTESIAN_POINT('Ctrl Pts',(21.6556870958782,-54.5800000200059,
-85.3242347169187));
#174513=CARTESIAN_POINT('Ctrl Pts',(20.7596485158525,-55.5069863868931,
-84.3783409260868));
#174514=CARTESIAN_POINT('Ctrl Pts',(20.1853568720873,-54.58000002,-88.7908549573443));
#174515=CARTESIAN_POINT('Ctrl Pts',(19.2046498564035,-54.580000019994,-87.6346041928195));
#174516=CARTESIAN_POINT('Ctrl Pts',(18.3831304802005,-55.4209867081881,
-86.677763648685));
#174517=CARTESIAN_POINT('Ctrl Pts',(18.8674767865624,-54.58000002,-89.8890267533221));
#174518=CARTESIAN_POINT('Ctrl Pts',(17.9458952665738,-54.5800000199822,
-88.738506470326));
#174519=CARTESIAN_POINT('Ctrl Pts',(17.1656615705366,-55.378552771758,-87.7759223265742));
#174520=CARTESIAN_POINT('Ctrl Pts',(17.501426021519,-54.58000002,-90.9187660074097));
#174521=CARTESIAN_POINT('Ctrl Pts',(16.6397068497462,-54.58000002,-89.7756104658071));
#174522=CARTESIAN_POINT('Ctrl Pts',(15.908562035693,-55.3376387148139,-88.8056746987062));
#174523=CARTESIAN_POINT('',(17.3782102443508,-55.3867109640818,-87.5561378285247));
#174524=CARTESIAN_POINT('Ctrl Pts',(17.3782874561047,-55.3867051039103,
-87.556225265873));
#174525=CARTESIAN_POINT('Ctrl Pts',(18.0129714837723,-55.4084038769681,
-86.9972203403477));
#174526=CARTESIAN_POINT('Ctrl Pts',(18.6500362552073,-55.4308164859441,
-86.4112422645402));
#174527=CARTESIAN_POINT('Ctrl Pts',(19.2925057736155,-55.4539248269632,
-85.7964162320036));
#174528=CARTESIAN_POINT('Ctrl Pts',(19.3853509908652,-55.4572642833587,
-85.7075658586768));
#174529=CARTESIAN_POINT('Ctrl Pts',(19.4783091534519,-55.4606182248066,
-85.6181130637534));
#174530=CARTESIAN_POINT('Ctrl Pts',(19.5713894980265,-55.4639865475406,
-85.5280522873859));
#174531=CARTESIAN_POINT('Ctrl Pts',(19.9333948730858,-55.4770865305736,
-85.1777905293742));
#174532=CARTESIAN_POINT('Ctrl Pts',(20.296400295736,-55.4903745638692,-84.8191217954611));
#174533=CARTESIAN_POINT('Ctrl Pts',(20.6606795729677,-55.5038451834361,
-84.4518497844382));
#174534=CARTESIAN_POINT('Ctrl Pts',(21.0070859618513,-55.5166548845963,
-84.1025974963494));
#174535=CARTESIAN_POINT('Ctrl Pts',(21.3546440024347,-55.5296297142268,
-83.7455647941717));
#174536=CARTESIAN_POINT('Ctrl Pts',(21.7035673985787,-55.542761750743,-83.3806236068663));
#174537=CARTESIAN_POINT('Ctrl Pts',(22.0308691120961,-55.5550800363645,
-83.0382966741983));
#174538=CARTESIAN_POINT('Ctrl Pts',(22.3593719626064,-55.5675366547334,
-82.6890106640993));
#174539=CARTESIAN_POINT('Ctrl Pts',(22.6892363727748,-55.580122001814,-82.3327033186524));
#174540=CARTESIAN_POINT('Ctrl Pts',(22.7876738992419,-55.5838776977853,
-82.2263747404044));
#174541=CARTESIAN_POINT('Ctrl Pts',(22.886232576619,-55.5876448353322,-82.1194212171195));
#174542=CARTESIAN_POINT('Ctrl Pts',(22.9849164160517,-55.5914231002813,
-82.0118419843783));
#174543=CARTESIAN_POINT('Ctrl Pts',(17.3782124086123,-55.3866898704104,
-87.5561779776695));
#174544=CARTESIAN_POINT('Ctrl Pts',(17.3842286240988,-55.3280540017891,
-87.6677848839424));
#174545=CARTESIAN_POINT('Ctrl Pts',(17.3906321444487,-55.2684282622658,
-87.7889551607595));
#174546=CARTESIAN_POINT('Ctrl Pts',(17.4010617540412,-55.1796759858784,
-87.9857741968713));
#174547=CARTESIAN_POINT('Ctrl Pts',(17.4046735378182,-55.1502087677355,
-88.053893722921));
#174548=CARTESIAN_POINT('Ctrl Pts',(17.4102842569604,-55.1064962524215,
-88.15988362143));
#174549=CARTESIAN_POINT('Ctrl Pts',(17.4131375697184,-55.0847624375805,
-88.213830936193));
#174550=CARTESIAN_POINT('Ctrl Pts',(17.4165447907984,-55.059691963569,-88.2784434090018));
#174551=CARTESIAN_POINT('Ctrl Pts',(17.4182670115253,-55.0472373150833,
-88.3111687633467));
#174552=CARTESIAN_POINT('Ctrl Pts',(17.4191326431444,-55.0410312913305,
-88.3276362900039));
#174553=CARTESIAN_POINT('Ctrl Pts',(17.4195045820392,-55.0383762555384,
-88.3347162758178));
#174554=CARTESIAN_POINT('Ctrl Pts',(17.4197527515741,-55.0366072874539,
-88.3394412613556));
#174555=CARTESIAN_POINT('Ctrl Pts',(17.4199359858737,-55.0353036730375,
-88.3429308972497));
#174556=CARTESIAN_POINT('Ctrl Pts',(17.4241772216026,-55.0051590733497,
-88.4237156579429));
#174557=CARTESIAN_POINT('Ctrl Pts',(17.4296648760824,-54.9665842581938,
-88.5311376661661));
#174558=CARTESIAN_POINT('Ctrl Pts',(17.4403028769676,-54.901358367034,-88.7357239344459));
#174559=CARTESIAN_POINT('Ctrl Pts',(17.4442474101977,-54.8784231995579,
-88.811164929113));
#174560=CARTESIAN_POINT('Ctrl Pts',(17.4507497336677,-54.8432876528706,
-88.9353776653523));
#174561=CARTESIAN_POINT('Ctrl Pts',(17.4541462110081,-54.8255399335536,
-89.0002461963404));
#174562=CARTESIAN_POINT('Ctrl Pts',(17.4577462028239,-54.8077493096576,
-89.0692833205201));
#174563=CARTESIAN_POINT('Ctrl Pts',(17.4601887667519,-54.7959065114956,
-89.1162363644095));
#174564=CARTESIAN_POINT('Ctrl Pts',(17.4615109836412,-54.7896224138083,
-89.1417160608586));
#174565=CARTESIAN_POINT('Ctrl Pts',(17.4816184041917,-54.6958051164707,
-89.5304494018354));
#174566=CARTESIAN_POINT('Ctrl Pts',(17.4976217601376,-54.6506607776598,
-89.8378333642392));
#174567=CARTESIAN_POINT('Ctrl Pts',(17.5128265027635,-54.6172691760158,
-90.1417732814389));
#174568=CARTESIAN_POINT('Ctrl Pts',(17.5156576011187,-54.611790867425,-90.198591549364));
#174569=CARTESIAN_POINT('Ctrl Pts',(17.5189723296823,-54.6060867273699,
-90.2646304500862));
#174570=CARTESIAN_POINT('Ctrl Pts',(17.5196241069914,-54.6050032951348,
-90.2775891192987));
#174571=CARTESIAN_POINT('Ctrl Pts',(17.5205858356443,-54.6034581849455,
-90.296653285516));
#174572=CARTESIAN_POINT('Ctrl Pts',(17.5209033418797,-54.6029538192376,
-90.3029333388735));
#174573=CARTESIAN_POINT('Ctrl Pts',(17.5218721007445,-54.6014589661519,
-90.3220976255049));
#174574=CARTESIAN_POINT('Ctrl Pts',(17.5242872361714,-54.5978262790508,
-90.3698821869256));
#174575=CARTESIAN_POINT('Ctrl Pts',(17.526667856459,-54.5947081383125,-90.4170335494899));
#174576=CARTESIAN_POINT('Ctrl Pts',(17.5360744592059,-54.5837858480397,
-90.6035864662938));
#174577=CARTESIAN_POINT('Ctrl Pts',(17.5432187572949,-54.5800000268131,
-90.7462467549563));
#174578=CARTESIAN_POINT('Ctrl Pts',(17.55,-54.58000002,-90.8821060618472));
#174579=CARTESIAN_POINT('Origin',(16.55,-70.08000002,-174.34995));
#174580=CARTESIAN_POINT('',(17.05,-70.08000002,-176.84995));
#174581=CARTESIAN_POINT('Origin',(16.55,-70.08000002,-176.84995));
#174582=CARTESIAN_POINT('',(17.05,-72.58000002,-174.34995));
#174583=CARTESIAN_POINT('Origin',(17.05,-70.08000002,-174.34995));
#174584=CARTESIAN_POINT('Origin',(16.55,-72.58000002,-174.34995));
#174585=CARTESIAN_POINT('Origin',(16.55,-72.58000002,-55.24995));
#174586=CARTESIAN_POINT('',(17.05,-72.58000002,-58.24995));
#174587=CARTESIAN_POINT('',(17.05,-72.58000002,-174.34995));
#174588=CARTESIAN_POINT('Origin',(16.55,-72.58000002,-58.24995));
#174589=CARTESIAN_POINT('Ctrl Pts',(17.3782102443508,-55.3867109640818,
-87.5561378285247));
#174590=CARTESIAN_POINT('Ctrl Pts',(17.0499999999999,-55.4939415516614,
-87.6101736986065));
#174591=CARTESIAN_POINT('Ctrl Pts',(17.05,-55.8060398696737,-87.7674469593951));
#174592=CARTESIAN_POINT('Ctrl Pts',(17.4056693808345,-55.1158123847072,
-88.0713943440392));
#174593=CARTESIAN_POINT('Ctrl Pts',(17.05,-55.2114257865401,-88.1214372575005));
#174594=CARTESIAN_POINT('Ctrl Pts',(17.05,-55.5622216475024,-88.2512880043934));
#174595=CARTESIAN_POINT('Ctrl Pts',(17.4339593787444,-54.9179776170691,
-88.6091505606876));
#174596=CARTESIAN_POINT('Ctrl Pts',(17.05,-55.0036171481024,-88.6486574682591));
#174597=CARTESIAN_POINT('Ctrl Pts',(17.05,-55.3841798573999,-88.7556128927223));
#174598=CARTESIAN_POINT('Ctrl Pts',(17.4916046269366,-54.6493515142325,
-89.7235249939138));
#174599=CARTESIAN_POINT('Ctrl Pts',(17.0499999999999,-54.6987064687868,
-89.7439019899564));
#174600=CARTESIAN_POINT('Ctrl Pts',(17.05,-55.1424163647715,-89.7992759203947));
#174601=CARTESIAN_POINT('Ctrl Pts',(17.5211522384036,-54.58000002,-90.3041534556916));
#174602=CARTESIAN_POINT('Ctrl Pts',(17.0500000000018,-54.6080382399387,
-90.3203722819605));
#174603=CARTESIAN_POINT('Ctrl Pts',(17.05,-55.0800000196891,-90.3423386098486));
#174604=CARTESIAN_POINT('Ctrl Pts',(17.55,-54.58000002,-90.8821060618472));
#174605=CARTESIAN_POINT('Ctrl Pts',(17.0499999999999,-54.58000002,-90.8821060618472));
#174606=CARTESIAN_POINT('Ctrl Pts',(17.05,-55.08000002,-90.8821060618472));
#174607=CARTESIAN_POINT('',(17.05,-55.08000002,-90.8821060618472));
#174608=CARTESIAN_POINT('Origin',(17.55,-55.08000002,-90.8821060618472));
#174609=CARTESIAN_POINT('',(17.05,-55.8060398696737,-87.7674469593951));
#174610=CARTESIAN_POINT('Origin',(17.55,-55.8060398696737,-87.7674469593951));
#174611=CARTESIAN_POINT('Ctrl Pts',(17.05,-55.08000002,-90.8821060618472));
#174612=CARTESIAN_POINT('Ctrl Pts',(17.05,-55.0800000198976,-90.7044011282776));
#174613=CARTESIAN_POINT('Ctrl Pts',(17.05,-55.0867609195445,-90.5266735432509));
#174614=CARTESIAN_POINT('Ctrl Pts',(17.05,-55.1000918811982,-90.3496297314756));
#174615=CARTESIAN_POINT('Ctrl Pts',(17.05,-55.1137303582782,-90.1685019155117));
#174616=CARTESIAN_POINT('Ctrl Pts',(17.05,-55.1342455055614,-89.988088644052));
#174617=CARTESIAN_POINT('Ctrl Pts',(17.05,-55.1614876321833,-89.8091398363491));
#174618=CARTESIAN_POINT('Ctrl Pts',(17.05,-55.1887297588052,-89.6301910286463));
#174619=CARTESIAN_POINT('Ctrl Pts',(17.05,-55.2226990580678,-89.4527054855482));
#174620=CARTESIAN_POINT('Ctrl Pts',(17.05,-55.2632981110657,-89.2774444065538));
#174621=CARTESIAN_POINT('Ctrl Pts',(17.05,-55.3408916382099,-88.942482768631));
#174622=CARTESIAN_POINT('Ctrl Pts',(17.05,-55.4420234811562,-88.6147745215355));
#174623=CARTESIAN_POINT('Ctrl Pts',(17.05,-55.5689958159258,-88.2950290565852));
#174624=CARTESIAN_POINT('Ctrl Pts',(17.05,-55.6398317020634,-88.1166480463494));
#174625=CARTESIAN_POINT('Ctrl Pts',(17.05,-55.7187108542584,-87.9407455779152));
#174626=CARTESIAN_POINT('Ctrl Pts',(17.05,-55.8060398696737,-87.7674469593951));
#174627=CARTESIAN_POINT('Origin',(17.55,-55.08000002,-55.24995));
#174628=CARTESIAN_POINT('',(17.05,-55.08000002,-141.176536909659));
#174629=CARTESIAN_POINT('Origin',(17.55,-55.08000002,-141.176536909659));
#174630=CARTESIAN_POINT('',(17.05,-55.08000002,-91.2551956845905));
#174631=CARTESIAN_POINT('Ctrl Pts',(17.55,-54.58000002,-141.176536909659));
#174632=CARTESIAN_POINT('Ctrl Pts',(17.0499999999999,-54.5800000199999,
-141.176536909659));
#174633=CARTESIAN_POINT('Ctrl Pts',(17.05,-55.08000002,-141.176536909659));
#174634=CARTESIAN_POINT('Ctrl Pts',(17.5210482604771,-54.58000002,-141.756572644947));
#174635=CARTESIAN_POINT('Ctrl Pts',(17.05,-54.6081354389567,-141.740217950908));
#174636=CARTESIAN_POINT('Ctrl Pts',(17.05,-55.0800000225241,-141.718258289701));
#174637=CARTESIAN_POINT('Ctrl Pts',(17.4921321192376,-54.6477817704653,
-142.324800749723));
#174638=CARTESIAN_POINT('Ctrl Pts',(17.05,-54.6967583223106,-142.304574247435));
#174639=CARTESIAN_POINT('Ctrl Pts',(17.05,-55.1410035947335,-142.249713786832));
#174640=CARTESIAN_POINT('Ctrl Pts',(17.4345568574947,-54.9143222027725,
-143.438059836182));
#174641=CARTESIAN_POINT('Ctrl Pts',(17.05,-54.9996847823657,-143.398819151438));
#174642=CARTESIAN_POINT('Ctrl Pts',(17.05,-55.3808899851806,-143.292313830226));
#174643=CARTESIAN_POINT('Ctrl Pts',(17.4056704634348,-55.1158017299176,
-143.987228363879));
#174644=CARTESIAN_POINT('Ctrl Pts',(17.05,-55.2114362483487,-143.937224655552));
#174645=CARTESIAN_POINT('Ctrl Pts',(17.05,-55.5622193543528,-143.807350422822));
#174646=CARTESIAN_POINT('Ctrl Pts',(17.3782102443502,-55.3867109640874,
-144.502505142992));
#174647=CARTESIAN_POINT('Ctrl Pts',(17.05,-55.4939415516672,-144.44846927291));
#174648=CARTESIAN_POINT('Ctrl Pts',(17.05,-55.8060398696787,-144.291196012121));
#174649=CARTESIAN_POINT('',(17.05,-55.8060398696787,-144.291196012121));
#174650=CARTESIAN_POINT('Origin',(17.55,-55.8060398696787,-144.291196012121));
#174651=CARTESIAN_POINT('Ctrl Pts',(17.05,-55.8060398696787,-144.291196012121));
#174652=CARTESIAN_POINT('Ctrl Pts',(17.05,-55.6831540655492,-144.047337313039));
#174653=CARTESIAN_POINT('Ctrl Pts',(17.05,-55.5762002500364,-143.795681932959));
#174654=CARTESIAN_POINT('Ctrl Pts',(17.05,-55.4849662480682,-143.539333784846));
#174655=CARTESIAN_POINT('Ctrl Pts',(17.05,-55.3950897214922,-143.286799853971));
#174656=CARTESIAN_POINT('Ctrl Pts',(17.05,-55.3204688827065,-143.029710172846));
#174657=CARTESIAN_POINT('Ctrl Pts',(17.05,-55.2609467896032,-142.77101380861));
#174658=CARTESIAN_POINT('Ctrl Pts',(17.05,-55.1772261529212,-142.407145147547));
#174659=CARTESIAN_POINT('Ctrl Pts',(17.05,-55.1222258452557,-142.038367265712));
#174660=CARTESIAN_POINT('Ctrl Pts',(17.05,-55.0966366319611,-141.66456206908));
#174661=CARTESIAN_POINT('Ctrl Pts',(17.05,-55.085565206749,-141.50283156839));
#174662=CARTESIAN_POINT('Ctrl Pts',(17.05,-55.0800000200001,-141.340159872026));
#174663=CARTESIAN_POINT('Ctrl Pts',(17.05,-55.08000002,-141.176536909659));
#174664=CARTESIAN_POINT('Ctrl Pts',(17.05,-69.1496478013716,-171.237717270032));
#174665=CARTESIAN_POINT('Ctrl Pts',(17.0499999999999,-68.809126121555,-171.404072041895));
#174666=CARTESIAN_POINT('Ctrl Pts',(17.4148840712406,-68.7171063154928,
-171.449026400902));
#174667=CARTESIAN_POINT('Ctrl Pts',(17.05,-64.7499600097223,-162.23172927942));
#174668=CARTESIAN_POINT('Ctrl Pts',(17.05,-64.4501495263081,-162.463595694272));
#174669=CARTESIAN_POINT('Ctrl Pts',(17.4052437025222,-64.32043537753,-162.443049517833));
#174670=CARTESIAN_POINT('Ctrl Pts',(17.05,-60.3166713897233,-153.242244037967));
#174671=CARTESIAN_POINT('Ctrl Pts',(17.0500000000351,-60.0450216003573,
-153.507379856866));
#174672=CARTESIAN_POINT('Ctrl Pts',(17.393699089013,-59.8910064308848,-153.453571789302));
#174673=CARTESIAN_POINT('Ctrl Pts',(17.05,-55.8060398696787,-144.291196012121));
#174674=CARTESIAN_POINT('Ctrl Pts',(17.05,-55.4939415516665,-144.448469272909));
#174675=CARTESIAN_POINT('Ctrl Pts',(17.3782102443508,-55.3867109640869,
-144.502505142991));
#174676=CARTESIAN_POINT('',(17.05,-69.1496478013716,-171.237717270032));
#174677=CARTESIAN_POINT('',(17.4148840712406,-68.7171063154928,-171.449026400902));
#174678=CARTESIAN_POINT('Origin',(17.55,-69.1496478013716,-171.237717270032));
#174679=CARTESIAN_POINT('Ctrl Pts',(17.3782102443508,-55.3867109640869,
-144.502505142991));
#174680=CARTESIAN_POINT('Ctrl Pts',(17.380720868236,-56.1168229918889,-145.953404949254));
#174681=CARTESIAN_POINT('Ctrl Pts',(17.3831954450421,-56.8646679860372,
-147.444471578493));
#174682=CARTESIAN_POINT('Ctrl Pts',(17.3856269123549,-57.6301346747941,
-148.975776438915));
#174683=CARTESIAN_POINT('Ctrl Pts',(17.3879710060604,-58.3680946866318,
-150.452054596438));
#174684=CARTESIAN_POINT('Ctrl Pts',(17.390275021825,-59.122432474325,-151.965731174827));
#174685=CARTESIAN_POINT('Ctrl Pts',(17.3925346451406,-59.8930912343523,
-153.516847722935));
#174686=CARTESIAN_POINT('Ctrl Pts',(17.3946832424879,-60.6258838887878,
-154.99175058732));
#174687=CARTESIAN_POINT('Ctrl Pts',(17.3967917011905,-61.3734335506627,
-156.500505714666));
#174688=CARTESIAN_POINT('Ctrl Pts',(17.3988582507656,-62.1357307859902,
-158.043123599146));
#174689=CARTESIAN_POINT('Ctrl Pts',(17.4008823945055,-62.8823855943037,
-159.554086787072));
#174690=CARTESIAN_POINT('Ctrl Pts',(17.4028663182098,-63.6431878049361,
-161.097535507723));
#174691=CARTESIAN_POINT('Ctrl Pts',(17.4048103792945,-64.4181692783863,
-162.673452998055));
#174692=CARTESIAN_POINT('Ctrl Pts',(17.406689765421,-65.1673686945184,-164.196942918881));
#174693=CARTESIAN_POINT('Ctrl Pts',(17.4085318928252,-65.9298195526288,
-165.750777247564));
#174694=CARTESIAN_POINT('Ctrl Pts',(17.4103390985595,-66.7055930840024,
-167.33491867873));
#174695=CARTESIAN_POINT('Ctrl Pts',(17.4118784989981,-67.3664066769433,
-168.684310155134));
#174696=CARTESIAN_POINT('Ctrl Pts',(17.4133925883603,-68.0368875784479,
-170.055691692052));
#174697=CARTESIAN_POINT('Ctrl Pts',(17.4148840712406,-68.7171063154928,
-171.449026400902));
#174698=CARTESIAN_POINT('Ctrl Pts',(17.05,-69.1496478013716,-171.237717270032));
#174699=CARTESIAN_POINT('Ctrl Pts',(17.05,-64.7499424271364,-162.231693289135));
#174700=CARTESIAN_POINT('Ctrl Pts',(17.05,-60.3166901832211,-153.242281332923));
#174701=CARTESIAN_POINT('Ctrl Pts',(17.05,-55.8060398696787,-144.291196012121));
#174702=CARTESIAN_POINT('Ctrl Pts',(17.05,-55.8060398696737,-87.7674469593951));
#174703=CARTESIAN_POINT('Ctrl Pts',(17.0499999999999,-55.4939415516614,
-87.6101736986065));
#174704=CARTESIAN_POINT('Ctrl Pts',(17.3782102443508,-55.3867109640818,
-87.5561378285247));
#174705=CARTESIAN_POINT('Ctrl Pts',(17.05,-60.2763921316847,-78.8963304394585));
#174706=CARTESIAN_POINT('Ctrl Pts',(17.0499999998605,-60.0039146247672,
-78.6330864204663));
#174707=CARTESIAN_POINT('Ctrl Pts',(17.3935607753682,-59.8507835488919,
-78.6850032603101));
#174708=CARTESIAN_POINT('Ctrl Pts',(17.05,-64.6707170319981,-69.9874285386638));
#174709=CARTESIAN_POINT('Ctrl Pts',(17.0499999999316,-64.3705933782976,
-69.756601957739));
#174710=CARTESIAN_POINT('Ctrl Pts',(17.4050347595683,-64.2412639062053,
-69.7761086016325));
#174711=CARTESIAN_POINT('Ctrl Pts',(17.05,-69.0317756926871,-61.0621827299711));
#174712=CARTESIAN_POINT('Ctrl Pts',(17.05,-68.6914563568371,-60.8958957033858));
#174713=CARTESIAN_POINT('Ctrl Pts',(17.4146253252297,-68.5993151180197,
-60.8508735991007));
#174714=CARTESIAN_POINT('',(17.4146253252297,-68.5993151180197,-60.8508735991007));
#174715=CARTESIAN_POINT('Ctrl Pts',(17.4146253252297,-68.5993151180197,
-60.8508735991007));
#174716=CARTESIAN_POINT('Ctrl Pts',(17.4128776238819,-67.8051417363082,
-62.4773308663589));
#174717=CARTESIAN_POINT('Ctrl Pts',(17.4110988447299,-67.0242728470718,
-64.0737822849279));
#174718=CARTESIAN_POINT('Ctrl Pts',(17.4092848745463,-66.2565999860111,
-65.6401711202791));
#174719=CARTESIAN_POINT('Ctrl Pts',(17.407428178194,-65.4708453943339,-67.2434546048986));
#174720=CARTESIAN_POINT('Ctrl Pts',(17.4055346211606,-64.6989159435754,
-68.8152427226574));
#174721=CARTESIAN_POINT('Ctrl Pts',(17.4036021153684,-63.9407442116168,
-70.3555001505591));
#174722=CARTESIAN_POINT('Ctrl Pts',(17.4015949038351,-63.1532634957471,
-71.9552999990896));
#174723=CARTESIAN_POINT('Ctrl Pts',(17.3995456779925,-62.3806248102645,
-73.521084285121));
#174724=CARTESIAN_POINT('Ctrl Pts',(17.3974544925988,-61.6228031213183,
-75.0528398018804));
#174725=CARTESIAN_POINT('Ctrl Pts',(17.3953146083248,-60.8473335146984,
-76.6202663685062));
#174726=CARTESIAN_POINT('Ctrl Pts',(17.3931308036726,-60.0873807420183,
-78.1520580110134));
#174727=CARTESIAN_POINT('Ctrl Pts',(17.3909054532109,-59.3429628661628,
-79.6482351286049));
#174728=CARTESIAN_POINT('Ctrl Pts',(17.3885629111999,-58.5593424081476,
-81.2232040219992));
#174729=CARTESIAN_POINT('Ctrl Pts',(17.3861743366006,-57.7929361965902,
-82.7587086075468));
#174730=CARTESIAN_POINT('Ctrl Pts',(17.3837449346187,-57.0438170021005,
-84.2547997688877));
#174731=CARTESIAN_POINT('Ctrl Pts',(17.3819219752636,-56.481697660022,-85.3774272298958));
#174732=CARTESIAN_POINT('Ctrl Pts',(17.380076081124,-55.9293130928866,-86.4778631342493));
#174733=CARTESIAN_POINT('Ctrl Pts',(17.3782102443508,-55.3867109640818,
-87.5561378285247));
#174734=CARTESIAN_POINT('',(17.05,-69.0317756926871,-61.0621827299711));
#174735=CARTESIAN_POINT('Origin',(17.55,-69.0317756926871,-61.0621827299711));
#174736=CARTESIAN_POINT('Ctrl Pts',(17.05,-55.8060398696737,-87.7674469593951));
#174737=CARTESIAN_POINT('Ctrl Pts',(17.05,-60.2764102501238,-78.896294484622));
#174738=CARTESIAN_POINT('Ctrl Pts',(17.05,-64.6707000732441,-69.9874632456984));
#174739=CARTESIAN_POINT('Ctrl Pts',(17.05,-69.0317756926871,-61.0621827299711));
#174740=CARTESIAN_POINT('Origin',(16.55,-70.08000002,-58.24995));
#174741=CARTESIAN_POINT('',(17.05,-70.08000002,-55.74995));
#174742=CARTESIAN_POINT('Origin',(17.05,-70.08000002,-58.24995));
#174743=CARTESIAN_POINT('',(16.55,-70.08000002,-55.24995));
#174744=CARTESIAN_POINT('Origin',(16.55,-70.08000002,-55.74995));
#174745=CARTESIAN_POINT('Origin',(16.55,-70.08000002,-58.24995));
#174746=CARTESIAN_POINT('Origin',(-3.3975957231091E-14,-70.08000002,-58.24995));
#174747=CARTESIAN_POINT('',(16.05,-70.08000002,-55.24995));
#174748=CARTESIAN_POINT('',(41.5,-70.08000002,-55.24995));
#174749=CARTESIAN_POINT('Origin',(16.05,-70.08000002,-58.24995));
#174750=CARTESIAN_POINT('Origin',(16.05,-70.08000002,-58.24995));
#174751=CARTESIAN_POINT('',(15.55,-70.08000002,-55.74995));
#174752=CARTESIAN_POINT('Origin',(16.05,-70.08000002,-55.74995));
#174753=CARTESIAN_POINT('',(15.55,-72.58000002,-58.24995));
#174754=CARTESIAN_POINT('Origin',(15.55,-70.08000002,-58.24995));
#174755=CARTESIAN_POINT('Origin',(16.05,-72.58000002,-58.24995));
#174756=CARTESIAN_POINT('Origin',(16.05,-72.58000002,-55.24995));
#174757=CARTESIAN_POINT('',(15.55,-72.58000002,-174.34995));
#174758=CARTESIAN_POINT('',(15.55,-72.58000002,-58.24995));
#174759=CARTESIAN_POINT('Origin',(16.05,-72.58000002,-174.34995));
#174760=CARTESIAN_POINT('Origin',(16.05,-70.08000002,-174.34995));
#174761=CARTESIAN_POINT('',(15.55,-70.08000002,-176.84995));
#174762=CARTESIAN_POINT('Origin',(15.55,-70.08000002,-174.34995));
#174763=CARTESIAN_POINT('Origin',(16.05,-70.08000002,-176.84995));
#174764=CARTESIAN_POINT('Ctrl Pts',(15.55,-55.7328910677637,-142.237228854888));
#174765=CARTESIAN_POINT('Ctrl Pts',(15.55,-55.1214867472491,-142.539470838321));
#174766=CARTESIAN_POINT('Ctrl Pts',(14.8995694550282,-55.3054345175152,
-142.448537985759));
#174767=CARTESIAN_POINT('Ctrl Pts',(15.55,-60.4987241912205,-151.878017105041));
#174768=CARTESIAN_POINT('Ctrl Pts',(15.5500000000182,-59.8063638088321,
-151.967058554268));
#174769=CARTESIAN_POINT('Ctrl Pts',(14.9144862578123,-60.0660270491051,
-152.089344301479));
#174770=CARTESIAN_POINT('Ctrl Pts',(15.55,-65.1981673386922,-161.551271258869));
#174771=CARTESIAN_POINT('Ctrl Pts',(15.549999999915,-64.5626692295555,-161.718722395353));
#174772=CARTESIAN_POINT('Ctrl Pts',(14.9252396269456,-64.7624344426112,
-161.762591659591));
#174773=CARTESIAN_POINT('Ctrl Pts',(15.55,-69.870344670579,-171.237717270032));
#174774=CARTESIAN_POINT('Ctrl Pts',(15.5499999999999,-69.3001099534342,
-171.51276528209));
#174775=CARTESIAN_POINT('Ctrl Pts',(14.9341313545396,-69.4322546019743,
-171.449026400902));
#174776=CARTESIAN_POINT('',(14.9341313545396,-69.4322546019744,-171.449026400902));
#174777=CARTESIAN_POINT('',(15.55,-69.870344670579,-171.237717270032));
#174778=CARTESIAN_POINT('Origin',(15.05,-69.870344670579,-171.237717270032));
#174779=CARTESIAN_POINT('',(15.55,-55.7328910677637,-142.237228854888));
#174780=CARTESIAN_POINT('Ctrl Pts',(15.55,-55.7328910677637,-142.237228854888));
#174781=CARTESIAN_POINT('Ctrl Pts',(15.55,-60.4987378575172,-151.878044750548));
#174782=CARTESIAN_POINT('Ctrl Pts',(15.55,-65.1981545194713,-161.551244681819));
#174783=CARTESIAN_POINT('Ctrl Pts',(15.55,-69.870344670579,-171.237717270032));
#174784=CARTESIAN_POINT('Origin',(15.05,-55.7328910677637,-142.237228854888));
#174785=CARTESIAN_POINT('Ctrl Pts',(14.9341313545396,-69.4322546019743,
-171.449026400902));
#174786=CARTESIAN_POINT('Ctrl Pts',(14.9325246708401,-68.5884451336383,
-169.698743719727));
#174787=CARTESIAN_POINT('Ctrl Pts',(14.9310233213259,-67.7597775482042,
-167.982185348246));
#174788=CARTESIAN_POINT('Ctrl Pts',(14.9295360070345,-66.9461670298033,
-166.299394335229));
#174789=CARTESIAN_POINT('Ctrl Pts',(14.9279426283007,-66.0745357241675,
-164.496598901032));
#174790=CARTESIAN_POINT('Ctrl Pts',(14.9263653852153,-65.2201851979954,
-162.732558509485));
#174791=CARTESIAN_POINT('Ctrl Pts',(14.9246943502029,-64.3830706161263,
-161.007300204738));
#174792=CARTESIAN_POINT('Ctrl Pts',(14.9230233151905,-63.5459560342572,
-159.282041899991));
#174793=CARTESIAN_POINT('Ctrl Pts',(14.9212584740815,-62.7260779904469,
-157.59556600155));
#174794=CARTESIAN_POINT('Ctrl Pts',(14.9192919729217,-61.923445829236,-155.947872412608));
#174795=CARTESIAN_POINT('Ctrl Pts',(14.9171604680817,-61.0534670205351,
-154.161925406137));
#174796=CARTESIAN_POINT('Ctrl Pts',(14.9147932490124,-60.2037518026807,
-152.421545017592));
#174797=CARTESIAN_POINT('Ctrl Pts',(14.9123287456633,-59.3742952696168,
-150.726717945526));
#174798=CARTESIAN_POINT('Ctrl Pts',(14.9096915492495,-58.4867169284227,
-148.91313068535));
#174799=CARTESIAN_POINT('Ctrl Pts',(14.9069430335476,-57.6223358513715,
-147.151703764968));
#174800=CARTESIAN_POINT('Ctrl Pts',(14.904257075721,-56.7812024435093,-145.4423974361));
#174801=CARTESIAN_POINT('Ctrl Pts',(14.902659968314,-56.2810529688437,-144.426020420951));
#174802=CARTESIAN_POINT('Ctrl Pts',(14.901085044351,-55.789124173773,-143.428071155623));
#174803=CARTESIAN_POINT('Ctrl Pts',(14.8995694550282,-55.3054345175152,
-142.448537985759));
#174804=CARTESIAN_POINT('Ctrl Pts',(14.8995694550282,-55.3054345175152,
-142.448537985759));
#174805=CARTESIAN_POINT('Ctrl Pts',(15.55,-55.1214867472491,-142.539470838321));
#174806=CARTESIAN_POINT('Ctrl Pts',(15.55,-55.7328910677637,-142.237228854888));
#174807=CARTESIAN_POINT('Ctrl Pts',(14.923902352475,-55.0632436795865,-141.975933471946));
#174808=CARTESIAN_POINT('Ctrl Pts',(15.55,-54.9185275760486,-142.049333574245));
#174809=CARTESIAN_POINT('Ctrl Pts',(15.55,-55.5149133573324,-141.796282446699));
#174810=CARTESIAN_POINT('Ctrl Pts',(14.9487965116602,-54.8849324628699,
-141.484081280379));
#174811=CARTESIAN_POINT('Ctrl Pts',(15.5499999999978,-54.7697596388846,
-141.534069766353));
#174812=CARTESIAN_POINT('Ctrl Pts',(15.55,-55.354439218511,-141.337957116977));
#174813=CARTESIAN_POINT('Ctrl Pts',(14.999232255606,-54.6427941514753,-140.466078071863));
#174814=CARTESIAN_POINT('Ctrl Pts',(15.550000000002,-54.5906769405451,-140.486936595447));
#174815=CARTESIAN_POINT('Ctrl Pts',(15.55,-55.1365147383997,-140.390621931638));
#174816=CARTESIAN_POINT('Ctrl Pts',(15.0249522987129,-54.58000002,-139.93601039575));
#174817=CARTESIAN_POINT('Ctrl Pts',(15.55,-54.554309680371,-139.949574386333));
#174818=CARTESIAN_POINT('Ctrl Pts',(15.55,-55.0800000201344,-139.897989788153));
#174819=CARTESIAN_POINT('Ctrl Pts',(15.05,-54.58000002,-139.407335470919));
#174820=CARTESIAN_POINT('Ctrl Pts',(15.55,-54.58000002,-139.407335470919));
#174821=CARTESIAN_POINT('Ctrl Pts',(15.55,-55.08000002,-139.407335470919));
#174822=CARTESIAN_POINT('',(15.55,-55.08000002,-139.407335470919));
#174823=CARTESIAN_POINT('Ctrl Pts',(15.55,-55.08000002,-139.407335470919));
#174824=CARTESIAN_POINT('Ctrl Pts',(15.55,-55.08000002,-139.590838222559));
#174825=CARTESIAN_POINT('Ctrl Pts',(15.55,-55.0879005396307,-139.774357162876));
#174826=CARTESIAN_POINT('Ctrl Pts',(15.55,-55.1034481519508,-139.956947178508));
#174827=CARTESIAN_POINT('Ctrl Pts',(15.55,-55.1192595423608,-140.142634984629));
#174828=CARTESIAN_POINT('Ctrl Pts',(15.55,-55.1429798052589,-140.327363292653));
#174829=CARTESIAN_POINT('Ctrl Pts',(15.55,-55.1743956555213,-140.510141133097));
#174830=CARTESIAN_POINT('Ctrl Pts',(15.55,-55.1948438531099,-140.629109022394));
#174831=CARTESIAN_POINT('Ctrl Pts',(15.55,-55.2185534084261,-140.747250607223));
#174832=CARTESIAN_POINT('Ctrl Pts',(15.55,-55.2454769784189,-140.864289524316));
#174833=CARTESIAN_POINT('Ctrl Pts',(15.55,-55.3211274089255,-141.193148010263));
#174834=CARTESIAN_POINT('Ctrl Pts',(15.55,-55.4215956233221,-141.51457580258));
#174835=CARTESIAN_POINT('Ctrl Pts',(15.55,-55.5489107707194,-141.827965375909));
#174836=CARTESIAN_POINT('Ctrl Pts',(15.55,-55.6049725527737,-141.965962922291));
#174837=CARTESIAN_POINT('Ctrl Pts',(15.55,-55.666240524004,-142.102401687741));
#174838=CARTESIAN_POINT('Ctrl Pts',(15.55,-55.7328910677637,-142.237228854888));
#174839=CARTESIAN_POINT('Origin',(15.05,-55.08000002,-139.407335470919));
#174840=CARTESIAN_POINT('Origin',(15.05,-55.08000002,-55.24995));
#174841=CARTESIAN_POINT('',(15.55,-55.08000002,-92.6513075005872));
#174842=CARTESIAN_POINT('',(15.55,-55.08000002,-139.74173251362));
#174843=CARTESIAN_POINT('Origin',(15.05,-55.08000002,-92.6513075005872));
#174844=CARTESIAN_POINT('Ctrl Pts',(15.05,-54.58000002,-92.6513075005872));
#174845=CARTESIAN_POINT('Ctrl Pts',(15.55,-54.5800000199999,-92.6513075005872));
#174846=CARTESIAN_POINT('Ctrl Pts',(15.55,-55.08000002,-92.6513075005872));
#174847=CARTESIAN_POINT('Ctrl Pts',(15.024892260188,-54.58000002,-92.1213653817264));
#174848=CARTESIAN_POINT('Ctrl Pts',(15.5499999999999,-54.5542439251598,
-92.1076806752376));
#174849=CARTESIAN_POINT('Ctrl Pts',(15.55,-55.0800000226551,-92.1594703795246));
#174850=CARTESIAN_POINT('Ctrl Pts',(14.9996997961174,-54.6413287797427,
-91.6021394176417));
#174851=CARTESIAN_POINT('Ctrl Pts',(15.5499999999983,-54.5897383680245,
-91.5814692358521));
#174852=CARTESIAN_POINT('Ctrl Pts',(15.55,-55.1351959031758,-91.676922782688));
#174853=CARTESIAN_POINT('Ctrl Pts',(14.9493011640063,-54.8817452975266,
-90.5846126995011));
#174854=CARTESIAN_POINT('Ctrl Pts',(15.5500000000017,-54.7672056222625,
-90.5350573580561));
#174855=CARTESIAN_POINT('Ctrl Pts',(15.55,-55.3515707703666,-90.7300471126767));
#174856=CARTESIAN_POINT('Ctrl Pts',(14.923904192,-55.0632253929174,-90.0827451820487));
#174857=CARTESIAN_POINT('Ctrl Pts',(15.5499999999938,-54.9184989239094,
-90.0093785901182));
#174858=CARTESIAN_POINT('Ctrl Pts',(15.55,-55.5149014993407,-90.2623845064693));
#174859=CARTESIAN_POINT('Ctrl Pts',(14.8995694550282,-55.3054345175152,
-89.6101049857472));
#174860=CARTESIAN_POINT('Ctrl Pts',(15.55,-55.121486747249,-89.5191721331851));
#174861=CARTESIAN_POINT('Ctrl Pts',(15.55,-55.7328910677637,-89.8214141166176));
#174862=CARTESIAN_POINT('',(15.55,-55.7328910677637,-89.8214141166176));
#174863=CARTESIAN_POINT('Ctrl Pts',(15.55,-55.7328910677637,-89.8214141166176));
#174864=CARTESIAN_POINT('Ctrl Pts',(15.55,-55.6023063246612,-90.0855735666696));
#174865=CARTESIAN_POINT('Ctrl Pts',(15.55,-55.4913767816605,-90.3592181628643));
#174866=CARTESIAN_POINT('Ctrl Pts',(15.55,-55.4001499318864,-90.6379301891953));
#174867=CARTESIAN_POINT('Ctrl Pts',(15.55,-55.3390449811745,-90.8246151911869));
#174868=CARTESIAN_POINT('Ctrl Pts',(15.55,-55.2867806294651,-91.0135745317669));
#174869=CARTESIAN_POINT('Ctrl Pts',(15.55,-55.2433833364682,-91.2034849476131));
#174870=CARTESIAN_POINT('Ctrl Pts',(15.55,-55.1636960311289,-91.5522036867227));
#174871=CARTESIAN_POINT('Ctrl Pts',(15.55,-55.1127619110557,-91.9058298381009));
#174872=CARTESIAN_POINT('Ctrl Pts',(15.55,-55.0914526404123,-92.2645121879628));
#174873=CARTESIAN_POINT('Ctrl Pts',(15.55,-55.0838313896102,-92.3927947647028));
#174874=CARTESIAN_POINT('Ctrl Pts',(15.55,-55.08000002,-92.5217241762766));
#174875=CARTESIAN_POINT('Ctrl Pts',(15.55,-55.08000002,-92.6513075005872));
#174876=CARTESIAN_POINT('',(14.8995695466442,-55.3054345064313,-89.6101050856063));
#174877=CARTESIAN_POINT('Origin',(15.05,-55.7328910677637,-89.8214141166176));
#174878=CARTESIAN_POINT('Ctrl Pts',(15.05,-54.5800000213444,-92.6513075005872));
#174879=CARTESIAN_POINT('Ctrl Pts',(15.0458933768937,-54.5800017521292,
-92.5646301382912));
#174880=CARTESIAN_POINT('Ctrl Pts',(15.0416395067651,-54.5816724036173,
-92.4748619271837));
#174881=CARTESIAN_POINT('Ctrl Pts',(15.0372157372707,-54.5853737320494,
-92.3820625728329));
#174882=CARTESIAN_POINT('Ctrl Pts',(15.0355328910543,-54.5867817544511,
-92.3467607691209));
#174883=CARTESIAN_POINT('Ctrl Pts',(15.0338256891318,-54.5884839168519,
-92.3110207073987));
#174884=CARTESIAN_POINT('Ctrl Pts',(15.0320938066638,-54.5905011024224,
-92.2748471742631));
#174885=CARTESIAN_POINT('Ctrl Pts',(15.0289515288417,-54.594161026002,-92.2092149543954));
#174886=CARTESIAN_POINT('Ctrl Pts',(15.0257275985235,-54.5988577289582,
-92.1421551536645));
#174887=CARTESIAN_POINT('Ctrl Pts',(15.0224251368449,-54.6047198056994,
-92.0737042390075));
#174888=CARTESIAN_POINT('Ctrl Pts',(15.0207739060056,-54.6076508440699,
-92.0394787816791));
#174889=CARTESIAN_POINT('Ctrl Pts',(15.0191030478259,-54.6108733196573,
-92.004905554086));
#174890=CARTESIAN_POINT('Ctrl Pts',(15.0174137469137,-54.614403682952,-91.9699903181173));
#174891=CARTESIAN_POINT('Ctrl Pts',(15.0165690964576,-54.6161688645993,
-91.952532700133));
#174892=CARTESIAN_POINT('Ctrl Pts',(15.0157198355364,-54.6180110230736,
-91.9349895803821));
#174893=CARTESIAN_POINT('Ctrl Pts',(15.0148661413604,-54.6199322383161,
-91.9173617205731));
#174894=CARTESIAN_POINT('Ctrl Pts',(15.0144392942724,-54.6208928459373,
-91.9085477906686));
#174895=CARTESIAN_POINT('Ctrl Pts',(15.0140113388933,-54.6218732180572,
-91.8997126757832));
#174896=CARTESIAN_POINT('Ctrl Pts',(15.0135823003155,-54.6228736158331,
-91.8908564754731));
#174897=CARTESIAN_POINT('Ctrl Pts',(15.0133677810267,-54.623373814721,-91.8864283753181));
#174898=CARTESIAN_POINT('Ctrl Pts',(15.0131529909395,-54.6238790200414,
-91.881995003809));
#174899=CARTESIAN_POINT('Ctrl Pts',(15.0129379333912,-54.6243892645035,
-91.877556373683));
#174900=CARTESIAN_POINT('Ctrl Pts',(15.0127228758429,-54.6248995089657,
-91.8731177435571));
#174901=CARTESIAN_POINT('Ctrl Pts',(15.0124491667809,-54.6255557109238,
-91.8674689771974));
#174902=CARTESIAN_POINT('Ctrl Pts',(15.0122919617645,-54.6259351480827,
-91.8642247202862));
#174903=CARTESIAN_POINT('Ctrl Pts',(15.0095085000646,-54.6326534375083,
-91.8067821203983));
#174904=CARTESIAN_POINT('Ctrl Pts',(15.0065479524336,-54.640561215979,-91.7454833205905));
#174905=CARTESIAN_POINT('Ctrl Pts',(15.0033879091281,-54.6499830230815,
-91.6803729622894));
#174906=CARTESIAN_POINT('Ctrl Pts',(15.0003178326951,-54.6591365900248,
-91.6171163049481));
#174907=CARTESIAN_POINT('Ctrl Pts',(14.9970591152687,-54.6697195336152,
-91.5502616453185));
#174908=CARTESIAN_POINT('Ctrl Pts',(14.9936054921246,-54.6820664342457,
-91.4798778723979));
#174909=CARTESIAN_POINT('Ctrl Pts',(14.9909769599697,-54.6914635873127,
-91.426309198983));
#174910=CARTESIAN_POINT('Ctrl Pts',(14.988235755913,-54.701883324779,-91.3706967310606));
#174911=CARTESIAN_POINT('Ctrl Pts',(14.9853868715498,-54.713486216082,-91.3130843738657));
#174912=CARTESIAN_POINT('Ctrl Pts',(14.9836460612115,-54.7205761609719,
-91.2778803521415));
#174913=CARTESIAN_POINT('Ctrl Pts',(14.9818651855333,-54.7281080902031,
-91.2419298484048));
#174914=CARTESIAN_POINT('Ctrl Pts',(14.9800469402429,-54.7361204910152,
-91.2052454222553));
#174915=CARTESIAN_POINT('Ctrl Pts',(14.9791378175977,-54.7401266914212,
-91.1869032091805));
#174916=CARTESIAN_POINT('Ctrl Pts',(14.978219356738,-54.7442530383326,-91.1683775216247));
#174917=CARTESIAN_POINT('Ctrl Pts',(14.9772920391227,-54.7485044521196,
-91.1496701581355));
#174918=CARTESIAN_POINT('Ctrl Pts',(14.976828380315,-54.7506301590131,-91.1403164763909));
#174919=CARTESIAN_POINT('Ctrl Pts',(14.9763625075567,-54.7527871343342,
-91.1309173760119));
#174920=CARTESIAN_POINT('Ctrl Pts',(14.9758944868423,-54.7549760012729,
-91.1214730904895));
#174921=CARTESIAN_POINT('Ctrl Pts',(14.9756604764851,-54.7560704347422,
-91.1167509477282));
#174922=CARTESIAN_POINT('Ctrl Pts',(14.9754259291553,-54.7571728412223,
-91.1120175087052));
#174923=CARTESIAN_POINT('Ctrl Pts',(14.9751908536412,-54.7582832990244,
-91.1072728034403));
#174924=CARTESIAN_POINT('Ctrl Pts',(14.9750733158841,-54.7588385279254,
-91.1049004508078));
#174925=CARTESIAN_POINT('Ctrl Pts',(14.974955646082,-54.7593957696634,-91.1025252816164));
#174926=CARTESIAN_POINT('Ctrl Pts',(14.9748378453696,-54.7599550340516,
-91.1001472996742));
#174927=CARTESIAN_POINT('Ctrl Pts',(14.9747200446573,-54.7605142984398,
-91.097769317732));
#174928=CARTESIAN_POINT('Ctrl Pts',(14.9746589234672,-54.7608045194713,
-91.0965354989367));
#174929=CARTESIAN_POINT('Ctrl Pts',(14.9744840516501,-54.761638905001,-91.0930049194237));
#174930=CARTESIAN_POINT('Ctrl Pts',(14.9712879276385,-54.7768889302514,
-91.0284766830101));
#174931=CARTESIAN_POINT('Ctrl Pts',(14.9682575247718,-54.7921574606343,
-90.9681333553976));
#174932=CARTESIAN_POINT('Ctrl Pts',(14.9654248623909,-54.8071025510312,
-90.9119403256999));
#174933=CARTESIAN_POINT('Ctrl Pts',(14.962559488986,-54.8222202243711,-90.855098390028));
#174934=CARTESIAN_POINT('Ctrl Pts',(14.9598960678549,-54.8370067435763,
-90.8025026027613));
#174935=CARTESIAN_POINT('Ctrl Pts',(14.957449120201,-54.8511563261295,-90.754103022306));
#174936=CARTESIAN_POINT('Ctrl Pts',(14.9549597206588,-54.8655513885955,
-90.7048637616166));
#174937=CARTESIAN_POINT('Ctrl Pts',(14.9526940092514,-54.8792870587007,
-90.6599670468528));
#174938=CARTESIAN_POINT('Ctrl Pts',(14.9506537885868,-54.8920937467772,
-90.619354020203));
#174939=CARTESIAN_POINT('Ctrl Pts',(14.94861546294,-54.9048885396201,-90.5787787161429));
#174940=CARTESIAN_POINT('Ctrl Pts',(14.9468018624224,-54.9167561342402,
-90.542478692155));
#174941=CARTESIAN_POINT('Ctrl Pts',(14.9452068624669,-54.9274800524862,
-90.5103964667988));
#174942=CARTESIAN_POINT('Ctrl Pts',(14.9436064679013,-54.9382402411767,
-90.4782057329156));
#174943=CARTESIAN_POINT('Ctrl Pts',(14.9422258779312,-54.9478490573687,
-90.4502610146561));
#174944=CARTESIAN_POINT('Ctrl Pts',(14.9410556150303,-54.9561397422719,
-90.4265116055838));
#174945=CARTESIAN_POINT('Ctrl Pts',(14.9398899886193,-54.9643975801323,
-90.4028562898062));
#174946=CARTESIAN_POINT('Ctrl Pts',(14.9389328214154,-54.9713478278598,
-90.3833628560987));
#174947=CARTESIAN_POINT('Ctrl Pts',(14.9381751005125,-54.9768757304564,
-90.3679930506267));
#174948=CARTESIAN_POINT('Ctrl Pts',(14.937852325165,-54.9792305165991,-90.3614457925467));
#174949=CARTESIAN_POINT('Ctrl Pts',(14.9375657634153,-54.9813278138561,
-90.3556469787911));
#174950=CARTESIAN_POINT('Ctrl Pts',(14.9373148566348,-54.9831614508253,
-90.3505944556927));
#174951=CARTESIAN_POINT('Ctrl Pts',(14.9371894032445,-54.9840782693099,
-90.3480681941436));
#174952=CARTESIAN_POINT('Ctrl Pts',(14.9370728694485,-54.9849291965647,
-90.3457285136322));
#174953=CARTESIAN_POINT('Ctrl Pts',(14.936965191492,-54.9857136121027,-90.3435751934635));
#174954=CARTESIAN_POINT('Ctrl Pts',(14.9369113525138,-54.9861058198717,
-90.3424985333791));
#174955=CARTESIAN_POINT('Ctrl Pts',(14.9368597278605,-54.9864814012052,
-90.341468463903));
#174956=CARTESIAN_POINT('Ctrl Pts',(14.9368103110741,-54.9868402876361,
-90.3404849606904));
#174957=CARTESIAN_POINT('Ctrl Pts',(14.9367856026809,-54.9870197308516,
-90.3399932090841));
#174958=CARTESIAN_POINT('Ctrl Pts',(14.9367614463196,-54.9871950008638,
-90.3395130992309));
#174959=CARTESIAN_POINT('Ctrl Pts',(14.9367381141154,-54.9873639714566,
-90.3390504377747));
#174960=CARTESIAN_POINT('Ctrl Pts',(14.9367147819112,-54.9875329420495,
-90.3385877763185));
#174961=CARTESIAN_POINT('Ctrl Pts',(14.936691690197,-54.9876994699089,-90.3381308072005));
#174962=CARTESIAN_POINT('Ctrl Pts',(14.9365793719496,-54.9885126937962,
-90.3359077490858));
#174963=CARTESIAN_POINT('Ctrl Pts',(14.932320345283,-55.0193495551381,-90.2516109940237));
#174964=CARTESIAN_POINT('Ctrl Pts',(14.9282177537613,-55.0507709943322,
-90.1710764495536));
#174965=CARTESIAN_POINT('Ctrl Pts',(14.9243031313811,-55.0823649839917,
-90.0942965928955));
#174966=CARTESIAN_POINT('Ctrl Pts',(14.9203172922909,-55.114533746843,-90.0161199198253));
#174967=CARTESIAN_POINT('Ctrl Pts',(14.9165260129442,-55.1468809599686,
-89.9418352830905));
#174968=CARTESIAN_POINT('Ctrl Pts',(14.9129329981448,-55.1790051991007,
-89.8714032691796));
#174969=CARTESIAN_POINT('Ctrl Pts',(14.9092446511795,-55.2119817790847,
-89.7991025080434));
#174970=CARTESIAN_POINT('Ctrl Pts',(14.9057648845781,-55.2447230132529,
-89.7308609781904));
#174971=CARTESIAN_POINT('Ctrl Pts',(14.9024718238562,-55.2768360660964,
-89.6666112571839));
#174972=CARTESIAN_POINT('Ctrl Pts',(14.9014882245471,-55.2864278651114,
-89.6474206055301));
#174973=CARTESIAN_POINT('Ctrl Pts',(14.9005211306358,-55.2959639152063,
-89.6285859491188));
#174974=CARTESIAN_POINT('Ctrl Pts',(14.8995696009239,-55.3054345059065,
-89.6101051906852));
#174975=CARTESIAN_POINT('Ctrl Pts',(15.55,-69.753968537624,-61.0621827299711));
#174976=CARTESIAN_POINT('Ctrl Pts',(15.55,-69.1834807533182,-60.7869757488078));
#174977=CARTESIAN_POINT('Ctrl Pts',(14.9339094669349,-69.3159372152924,
-60.8508735991008));
#174978=CARTESIAN_POINT('Ctrl Pts',(15.55,-65.1200769667078,-70.6679657074144));
#174979=CARTESIAN_POINT('Ctrl Pts',(15.5499999999812,-64.4850428243905,
-70.4989618700373));
#174980=CARTESIAN_POINT('Ctrl Pts',(14.9250579803326,-64.6843968356381,
-70.4566455899725));
#174981=CARTESIAN_POINT('Ctrl Pts',(15.55,-60.4591562379615,-80.2606677496439));
#174982=CARTESIAN_POINT('Ctrl Pts',(15.5500000001812,-59.7682625842489,
-80.1682572157014));
#174983=CARTESIAN_POINT('Ctrl Pts',(14.9143624117001,-60.0265024281888,
-80.0493410623047));
#174984=CARTESIAN_POINT('Ctrl Pts',(15.55,-55.7328910677637,-89.8214141166175));
#174985=CARTESIAN_POINT('Ctrl Pts',(15.55,-55.1214867472491,-89.519172133185));
#174986=CARTESIAN_POINT('Ctrl Pts',(14.8995694550282,-55.3054345175152,
-89.6101049857472));
#174987=CARTESIAN_POINT('',(15.55,-69.7539685376239,-61.0621827299711));
#174988=CARTESIAN_POINT('Ctrl Pts',(15.55,-69.7539685376239,-61.0621827299711));
#174989=CARTESIAN_POINT('Ctrl Pts',(15.55,-65.1200645664474,-70.6679914124205));
#174990=CARTESIAN_POINT('Ctrl Pts',(15.55,-60.459169452046,-80.2606410189155));
#174991=CARTESIAN_POINT('Ctrl Pts',(15.55,-55.7328910677637,-89.8214141166175));
#174992=CARTESIAN_POINT('',(14.9339094669349,-69.3159372152925,-60.8508735991008));
#174993=CARTESIAN_POINT('Origin',(15.05,-69.753968537624,-61.0621827299711));
#174994=CARTESIAN_POINT('Ctrl Pts',(14.8995694550282,-55.3054345175152,
-89.6101049857472));
#174995=CARTESIAN_POINT('Ctrl Pts',(14.9021428471819,-56.126714494731,-87.9469084112056));
#174996=CARTESIAN_POINT('Ctrl Pts',(14.9048838536198,-56.9717170086061,
-86.2306729016001));
#174997=CARTESIAN_POINT('Ctrl Pts',(14.9076126716805,-57.8403614223101,
-84.4613461791733));
#174998=CARTESIAN_POINT('Ctrl Pts',(14.9101550205963,-58.6496484961364,
-82.8129233916143));
#174999=CARTESIAN_POINT('Ctrl Pts',(14.9126867965068,-59.4794565058462,
-81.1184174199939));
#175000=CARTESIAN_POINT('Ctrl Pts',(14.9150655785119,-60.329761996796,-79.3778019676598));
#175001=CARTESIAN_POINT('Ctrl Pts',(14.9164835292938,-60.8366143830631,
-78.3402512226876));
#175002=CARTESIAN_POINT('Ctrl Pts',(14.917847170542,-61.3507506625969,-77.2863173579256));
#175003=CARTESIAN_POINT('Ctrl Pts',(14.9191269994737,-61.8721739455428,
-76.2159986380771));
#175004=CARTESIAN_POINT('Ctrl Pts',(14.9210339184465,-62.6490839890544,
-74.6212456026722));
#175005=CARTESIAN_POINT('Ctrl Pts',(14.9227536565489,-63.4421679559353,
-72.9901189526708));
#175006=CARTESIAN_POINT('Ctrl Pts',(14.9243835901195,-64.2514169346386,
-71.3226182784319));
#175007=CARTESIAN_POINT('Ctrl Pts',(14.9260180885611,-65.0629323353103,
-69.6504475208691));
#175008=CARTESIAN_POINT('Ctrl Pts',(14.9275622911326,-65.8907028888218,
-67.9416989707886));
#175009=CARTESIAN_POINT('Ctrl Pts',(14.9291162534416,-66.7347676310078,
-66.1963964579937));
#175010=CARTESIAN_POINT('Ctrl Pts',(14.9306702157506,-67.5788323731938,
-64.4510939451989));
#175011=CARTESIAN_POINT('Ctrl Pts',(14.9322338889336,-68.4391910232791,
-62.6692371075657));
#175012=CARTESIAN_POINT('Ctrl Pts',(14.9339094669349,-69.3159372152924,
-60.8508735991008));
#175013=CARTESIAN_POINT('Ctrl Pts',(16.4431419066885,-54.58000002,-91.6952124319348));
#175014=CARTESIAN_POINT('Ctrl Pts',(15.6303319911964,-54.58000002,-90.5558876551412));
#175015=CARTESIAN_POINT('Ctrl Pts',(14.9356335973474,-55.3065630170304,
-89.5821211232313));
#175016=CARTESIAN_POINT('Ctrl Pts',(15.339723951503,-54.58000002,-92.4824059293848));
#175017=CARTESIAN_POINT('Ctrl Pts',(14.580009345269,-54.5800000199812,-91.3456221401381));
#175018=CARTESIAN_POINT('Ctrl Pts',(13.9221964884044,-55.2748268726715,
-90.3693030445756));
#175019=CARTESIAN_POINT('Ctrl Pts',(14.2000751633255,-54.58000002,-93.2257513219804));
#175020=CARTESIAN_POINT('Ctrl Pts',(13.4941774039103,-54.58000002,-92.0929943757894));
#175021=CARTESIAN_POINT('Ctrl Pts',(12.878461314285,-55.2441424314898,-91.1126600131971));
#175022=CARTESIAN_POINT('Ctrl Pts',(11.824167023199,-54.58000002,-94.5957116711942));
#175023=CARTESIAN_POINT('Ctrl Pts',(11.232462400793,-54.58000002,-93.4698992380895));
#175024=CARTESIAN_POINT('Ctrl Pts',(10.7089431339248,-55.1865276043544,
-92.4826203625704));
#175025=CARTESIAN_POINT('Ctrl Pts',(10.607529289827,-54.58000002,-95.2106503240539));
#175026=CARTESIAN_POINT('Ctrl Pts',(10.0749231938442,-54.5800000200141,
-94.0883976981553));
#175027=CARTESIAN_POINT('Ctrl Pts',(9.60108129664725,-55.1600911541447,
-93.0975581705506));
#175028=CARTESIAN_POINT('Ctrl Pts',(9.35547542469517,-54.58000002,-95.7390202399778));
#175029=CARTESIAN_POINT('Ctrl Pts',(8.88330761013172,-54.58000002,-94.6201459052405));
#175030=CARTESIAN_POINT('Ctrl Pts',(8.4637455188182,-55.1370659786207,-93.6259289312743));
#175031=CARTESIAN_POINT('',(9.30242220787995,-55.1547652726018,-93.2181494891395));
#175032=CARTESIAN_POINT('Ctrl Pts',(9.30244148822568,-55.1547632761147,
-93.2181873809143));
#175033=CARTESIAN_POINT('Ctrl Pts',(9.61839909982102,-55.1616974672035,
-93.0577850773918));
#175034=CARTESIAN_POINT('Ctrl Pts',(9.93432541699597,-55.1689288990669,
-92.8897556011866));
#175035=CARTESIAN_POINT('Ctrl Pts',(10.2507660919963,-55.1764563648516,
-92.7139149924441));
#175036=CARTESIAN_POINT('Ctrl Pts',(10.5909200390141,-55.1845479200782,
-92.5248973286759));
#175037=CARTESIAN_POINT('Ctrl Pts',(10.9316681646333,-55.1929815934896,
-92.3268537703324));
#175038=CARTESIAN_POINT('Ctrl Pts',(11.2736708069581,-55.2017567532371,
-92.1194964152936));
#175039=CARTESIAN_POINT('Ctrl Pts',(11.4466658104287,-55.2061954873377,
-92.0146089614693));
#175040=CARTESIAN_POINT('Ctrl Pts',(11.6199815475503,-55.2107216033676,
-91.9073375579729));
#175041=CARTESIAN_POINT('Ctrl Pts',(11.7937022241049,-55.2153350179221,
-91.7976401878838));
#175042=CARTESIAN_POINT('Ctrl Pts',(12.2295670546593,-55.2269100658263,
-91.5224097053964));
#175043=CARTESIAN_POINT('Ctrl Pts',(12.6650898659555,-55.2389551468803,
-91.2337939943317));
#175044=CARTESIAN_POINT('Ctrl Pts',(13.1016107174846,-55.2514743713384,
-90.9311140181789));
#175045=CARTESIAN_POINT('Ctrl Pts',(13.5853543625944,-55.2653479245766,
-90.5956901444901));
#175046=CARTESIAN_POINT('Ctrl Pts',(14.0703195878936,-55.2798042384788,
-90.242989300559));
#175047=CARTESIAN_POINT('Ctrl Pts',(14.5583239929663,-55.294841368818,-89.8720620734263));
#175048=CARTESIAN_POINT('Ctrl Pts',(14.6718999929854,-55.2983410444314,
-89.7857341011416));
#175049=CARTESIAN_POINT('Ctrl Pts',(14.7856407595719,-55.301872131609,-89.6984190004166));
#175050=CARTESIAN_POINT('Ctrl Pts',(14.8995696009239,-55.3054345059065,
-89.6101051906852));
#175051=CARTESIAN_POINT('Ctrl Pts',(9.30244004339758,-55.1547632444057,
-93.2181881144106));
#175052=CARTESIAN_POINT('Ctrl Pts',(9.30427433941287,-55.1332939358577,
-93.2623011656816));
#175053=CARTESIAN_POINT('Ctrl Pts',(9.30624352124608,-55.1107681190608,
-93.3100497844399));
#175054=CARTESIAN_POINT('Ctrl Pts',(9.30836251838502,-55.0874709846995,
-93.3615546812591));
#175055=CARTESIAN_POINT('Ctrl Pts',(9.30992763140037,-55.0702634823677,
-93.3995967261891));
#175056=CARTESIAN_POINT('Ctrl Pts',(9.31157437985831,-55.0526361927093,
-93.439688104872));
#175057=CARTESIAN_POINT('Ctrl Pts',(9.31330526457061,-55.0347219445586,
-93.481875686768));
#175058=CARTESIAN_POINT('Ctrl Pts',(9.31534242415013,-55.0136378238366,
-93.5315282349621));
#175059=CARTESIAN_POINT('Ctrl Pts',(9.3174964869314,-54.9921554559608,-93.5840849551193));
#175060=CARTESIAN_POINT('Ctrl Pts',(9.31976404326403,-54.9705191678377,
-93.6396151789178));
#175061=CARTESIAN_POINT('Ctrl Pts',(9.32089782143035,-54.9597010237762,
-93.6673802908171));
#175062=CARTESIAN_POINT('Ctrl Pts',(9.32205983145287,-54.9488448734871,
-93.6958886290157));
#175063=CARTESIAN_POINT('Ctrl Pts',(9.3232486734891,-54.9379841011688,-93.7251477030176));
#175064=CARTESIAN_POINT('Ctrl Pts',(9.32384309450721,-54.9325537150096,
-93.7397772400185));
#175065=CARTESIAN_POINT('Ctrl Pts',(9.32444422673949,-54.9271221929293,
-93.754594468051));
#175066=CARTESIAN_POINT('Ctrl Pts',(9.32505180826187,-54.9216938962469,
-93.7696002084956));
#175067=CARTESIAN_POINT('Ctrl Pts',(9.32535559902306,-54.9189797479057,
-93.777103078718));
#175068=CARTESIAN_POINT('Ctrl Pts',(9.32566100229853,-54.9162664070469,
-93.7846530774654));
#175069=CARTESIAN_POINT('Ctrl Pts',(9.32596798310117,-54.9135544280597,
-93.7922503045262));
#175070=CARTESIAN_POINT('Ctrl Pts',(9.32612147350249,-54.9121984385661,
-93.7960489180566));
#175071=CARTESIAN_POINT('Ctrl Pts',(9.3262753582968,-54.9108427896114,-93.7998593386901));
#175072=CARTESIAN_POINT('Ctrl Pts',(9.32642963280402,-54.9094875511762,
-93.8036815784753));
#175073=CARTESIAN_POINT('Ctrl Pts',(9.32650677005764,-54.9088099319586,
-93.8055926983679));
#175074=CARTESIAN_POINT('Ctrl Pts',(9.32658400474017,-54.9081324153753,
-93.80750677305));
#175075=CARTESIAN_POINT('Ctrl Pts',(9.32666133624566,-54.9074550102173,
-93.809423803998));
#175076=CARTESIAN_POINT('Ctrl Pts',(9.32673866775115,-54.9067776050594,
-93.8113408349459));
#175077=CARTESIAN_POINT('Ctrl Pts',(9.32677113000359,-54.9064930880799,
-93.8121454682918));
#175078=CARTESIAN_POINT('Ctrl Pts',(9.32689362062015,-54.9054231378333,
-93.8151837671098));
#175079=CARTESIAN_POINT('Ctrl Pts',(9.32907568700704,-54.8863628821635,
-93.8693084822138));
#175080=CARTESIAN_POINT('Ctrl Pts',(9.33113370306065,-54.8693839288859,
-93.9201129178801));
#175081=CARTESIAN_POINT('Ctrl Pts',(9.3330474098387,-54.8541913521633,-93.9674628293226));
#175082=CARTESIAN_POINT('Ctrl Pts',(9.33498196023909,-54.8388333016414,
-94.0153284643247));
#175083=CARTESIAN_POINT('Ctrl Pts',(9.33676931245704,-54.8253003429326,
-94.0596643643792));
#175084=CARTESIAN_POINT('Ctrl Pts',(9.33840041440837,-54.8133245098168,
-94.1003684347088));
#175085=CARTESIAN_POINT('Ctrl Pts',(9.34004917218116,-54.8012190446009,
-94.1415131052091));
#175086=CARTESIAN_POINT('Ctrl Pts',(9.34153852943323,-54.7907042806318,
-94.1789473298604));
#175087=CARTESIAN_POINT('Ctrl Pts',(9.34286722215193,-54.7815462682086,
-94.2125960809697));
#175088=CARTESIAN_POINT('Ctrl Pts',(9.34420075570395,-54.7723548903496,
-94.2463674247548));
#175089=CARTESIAN_POINT('Ctrl Pts',(9.34537267165175,-54.7645299865231,
-94.2763260722162));
#175090=CARTESIAN_POINT('Ctrl Pts',(9.34638621535443,-54.7578816051877,
-94.3024201830284));
#175091=CARTESIAN_POINT('Ctrl Pts',(9.34740282266097,-54.7512131280176,
-94.3285931676167));
#175092=CARTESIAN_POINT('Ctrl Pts',(9.34826027114869,-54.745728182414,-94.3508785485639));
#175093=CARTESIAN_POINT('Ctrl Pts',(9.34896342191889,-54.7412840483787,
-94.3692425251512));
#175094=CARTESIAN_POINT('Ctrl Pts',(9.34916988110587,-54.7399791613777,
-94.3746345574672));
#175095=CARTESIAN_POINT('Ctrl Pts',(9.34936303935837,-54.738764331903,-94.3796886188088));
#175096=CARTESIAN_POINT('Ctrl Pts',(9.3495430157132,-54.7376367641466,-94.3844040976793));
#175097=CARTESIAN_POINT('Ctrl Pts',(9.35007821311692,-54.7342837051501,
-94.3984265621923));
#175098=CARTESIAN_POINT('Ctrl Pts',(9.35049691873413,-54.7317001298129,
-94.4094544485823));
#175099=CARTESIAN_POINT('Ctrl Pts',(9.35080171450003,-54.729832066066,-94.417476557166));
#175100=CARTESIAN_POINT('Ctrl Pts',(9.35095411238298,-54.7288980341925,
-94.4214876114579));
#175101=CARTESIAN_POINT('Ctrl Pts',(9.35107801732042,-54.7281433382731,
-94.4247473300645));
#175102=CARTESIAN_POINT('Ctrl Pts',(9.35117363515788,-54.7275639869044,
-94.4272549215081));
#175103=CARTESIAN_POINT('Ctrl Pts',(9.35122144407661,-54.7272743112201,
-94.4285087172299));
#175104=CARTESIAN_POINT('Ctrl Pts',(9.35126218405767,-54.727028499904,-94.429574487568));
#175105=CARTESIAN_POINT('Ctrl Pts',(9.35129586718252,-54.7268262272475,
-94.4304521681997));
#175106=CARTESIAN_POINT('Ctrl Pts',(9.35131270874495,-54.7267250909192,
-94.4308910085156));
#175107=CARTESIAN_POINT('Ctrl Pts',(9.35132778627098,-54.7266348410177,
-94.431282826806));
#175108=CARTESIAN_POINT('Ctrl Pts',(9.3513411014339,-54.7265554475381,-94.4316276172239));
#175109=CARTESIAN_POINT('Ctrl Pts',(9.35134775901537,-54.7265157507983,
-94.4318000124328));
#175110=CARTESIAN_POINT('Ctrl Pts',(9.35135397600869,-54.7264787684293,
-94.4319606507287));
#175111=CARTESIAN_POINT('Ctrl Pts',(9.35135953256314,-54.7264458494721,
-94.4321036520747));
#175112=CARTESIAN_POINT('Ctrl Pts',(9.35136508911759,-54.726412930515,-94.4322466534208));
#175113=CARTESIAN_POINT('Ctrl Pts',(9.35137044371634,-54.7263810282556,
-94.4323837104159));
#175114=CARTESIAN_POINT('Ctrl Pts',(9.35144642391555,-54.7259337110089,
-94.4343302656795));
#175115=CARTESIAN_POINT('Ctrl Pts',(9.35496709525164,-54.7052065080629,
-94.5245272037296));
#175116=CARTESIAN_POINT('Ctrl Pts',(9.35842399639266,-54.6872251950304,
-94.6127481737394));
#175117=CARTESIAN_POINT('Ctrl Pts',(9.36177567320373,-54.671666092566,-94.6987859198705));
#175118=CARTESIAN_POINT('Ctrl Pts',(9.3652001974941,-54.6557688186553,-94.7866936651941));
#175119=CARTESIAN_POINT('Ctrl Pts',(9.36851502920089,-54.6423995879464,
-94.8723223801593));
#175120=CARTESIAN_POINT('Ctrl Pts',(9.37169866947417,-54.6312146453525,
-94.955500484486));
#175121=CARTESIAN_POINT('Ctrl Pts',(9.37499207965511,-54.619644052996,-95.0415465173622));
#175122=CARTESIAN_POINT('Ctrl Pts',(9.37814525879686,-54.6104103700865,
-95.1249701790108));
#175123=CARTESIAN_POINT('Ctrl Pts',(9.38115604701931,-54.6031440314951,
-95.2056319574495));
#175124=CARTESIAN_POINT('Ctrl Pts',(9.38422794052159,-54.5957302193453,
-95.2879308023903));
#175125=CARTESIAN_POINT('Ctrl Pts',(9.38715185380867,-54.5903639102433,
-95.3673548787892));
#175126=CARTESIAN_POINT('Ctrl Pts',(9.38994437245913,-54.5866723986661,
-95.4438035593695));
#175127=CARTESIAN_POINT('Ctrl Pts',(9.39281977434526,-54.5828713213305,
-95.5225212718889));
#175128=CARTESIAN_POINT('Ctrl Pts',(9.39555612076478,-54.58084546469,-95.5980847279305));
#175129=CARTESIAN_POINT('Ctrl Pts',(9.39818746661894,-54.5802163907876,
-95.6704283316989));
#175130=CARTESIAN_POINT('Ctrl Pts',(9.39879705050409,-54.5800706580201,
-95.6871876242796));
#175131=CARTESIAN_POINT('Ctrl Pts',(9.39940105561197,-54.5800000205198,
-95.7037742834776));
#175132=CARTESIAN_POINT('Ctrl Pts',(9.4,-54.58000002,-95.7201877838351));
#175133=CARTESIAN_POINT('Ctrl Pts',(9.30242220787995,-55.1547652726018,
-93.2181494891395));
#175134=CARTESIAN_POINT('Ctrl Pts',(8.89999999999997,-55.2270244231188,
-93.2526539147005));
#175135=CARTESIAN_POINT('Ctrl Pts',(8.9,-55.5972887473416,-93.4294586200098));
#175136=CARTESIAN_POINT('Ctrl Pts',(9.31868748160984,-54.9644104418147,
-93.609279542603));
#175137=CARTESIAN_POINT('Ctrl Pts',(8.90000000000102,-55.0269773455407,
-93.6389456903403));
#175138=CARTESIAN_POINT('Ctrl Pts',(8.9,-55.4259676862915,-93.7882391070165));
#175139=CARTESIAN_POINT('Ctrl Pts',(9.33504644279423,-54.8225599750811,
-94.0144115846847));
#175140=CARTESIAN_POINT('Ctrl Pts',(8.90000000000064,-54.8762991189121,
-94.036294307786));
#175141=CARTESIAN_POINT('Ctrl Pts',(8.9,-55.2983039792949,-94.15951472994));
#175142=CARTESIAN_POINT('Ctrl Pts',(9.36771205478627,-54.6300877991462,
-94.8508246266895));
#175143=CARTESIAN_POINT('Ctrl Pts',(8.89999999999928,-54.6591463230926,
-94.8606734038326));
#175144=CARTESIAN_POINT('Ctrl Pts',(8.9,-55.1250790215096,-94.9253056568412));
#175145=CARTESIAN_POINT('Ctrl Pts',(9.38412882836456,-54.58000002,-95.28525344501));
#175146=CARTESIAN_POINT('Ctrl Pts',(8.89999999999998,-54.5956237519515,
-95.2920343273126));
#175147=CARTESIAN_POINT('Ctrl Pts',(8.9,-55.0800000205144,-95.3226944715878));
#175148=CARTESIAN_POINT('Ctrl Pts',(9.4,-54.58000002,-95.7201877838351));
#175149=CARTESIAN_POINT('Ctrl Pts',(8.89999999999996,-54.58000002,-95.720187783835));
#175150=CARTESIAN_POINT('Ctrl Pts',(8.9,-55.08000002,-95.7201877838351));
#175151=CARTESIAN_POINT('',(8.9,-55.08000002,-95.7201877838351));
#175152=CARTESIAN_POINT('Origin',(9.4,-55.08000002,-95.7201877838351));
#175153=CARTESIAN_POINT('',(8.9,-55.5972887473416,-93.4294586200098));
#175154=CARTESIAN_POINT('Origin',(9.4,-55.5972887473416,-93.4294586200098));
#175155=CARTESIAN_POINT('Ctrl Pts',(8.9,-55.08000002,-95.7201877838351));
#175156=CARTESIAN_POINT('Ctrl Pts',(8.9,-55.08000002,-95.3987883664614));
#175157=CARTESIAN_POINT('Ctrl Pts',(8.9,-55.1094672114476,-95.0775170947052));
#175158=CARTESIAN_POINT('Ctrl Pts',(8.9,-55.1665218943283,-94.7639046607854));
#175159=CARTESIAN_POINT('Ctrl Pts',(8.9,-55.1800381380326,-94.6896099338406));
#175160=CARTESIAN_POINT('Ctrl Pts',(8.9,-55.1951028648123,-94.6157450445103));
#175161=CARTESIAN_POINT('Ctrl Pts',(8.9,-55.2116915002618,-94.5424101933588));
#175162=CARTESIAN_POINT('Ctrl Pts',(8.9,-55.2822535699003,-94.2304701974735));
#175163=CARTESIAN_POINT('Ctrl Pts',(8.9,-55.3800515517671,-93.9262693258917));
#175164=CARTESIAN_POINT('Ctrl Pts',(8.9,-55.5065195348801,-93.6302150670226));
#175165=CARTESIAN_POINT('Ctrl Pts',(8.9,-55.5352865894012,-93.5628730505181));
#175166=CARTESIAN_POINT('Ctrl Pts',(8.9,-55.5655372445695,-93.4959526010179));
#175167=CARTESIAN_POINT('Ctrl Pts',(8.9,-55.5972887473416,-93.4294586200098));
#175168=CARTESIAN_POINT('Origin',(9.4,-55.08000002,-55.24995));
#175169=CARTESIAN_POINT('',(8.9,-55.08000002,-136.338455187671));
#175170=CARTESIAN_POINT('Origin',(9.4,-55.08000002,-136.338455187671));
#175171=CARTESIAN_POINT('',(8.9,-55.08000002,-95.926725859984));
#175172=CARTESIAN_POINT('Ctrl Pts',(9.4,-54.58000002,-136.338455187671));
#175173=CARTESIAN_POINT('Ctrl Pts',(8.89999999999996,-54.58000002,-136.338455187671));
#175174=CARTESIAN_POINT('Ctrl Pts',(8.9,-55.08000002,-136.338455187671));
#175175=CARTESIAN_POINT('Ctrl Pts',(9.38412562712359,-54.58000002,-136.773477252872));
#175176=CARTESIAN_POINT('Ctrl Pts',(8.90000000000676,-54.5956263749734,
-136.766680459455));
#175177=CARTESIAN_POINT('Ctrl Pts',(8.9,-55.0800000228167,-136.736031631193));
#175178=CARTESIAN_POINT('Ctrl Pts',(9.36801042327471,-54.6289055341263,
-137.200007658363));
#175179=CARTESIAN_POINT('Ctrl Pts',(8.90000000000101,-54.6577176624563,
-137.1902362241));
#175180=CARTESIAN_POINT('Ctrl Pts',(8.9,-55.1240149822832,-137.126190519306));
#175181=CARTESIAN_POINT('Ctrl Pts',(9.33535293620398,-54.8201888415935,
-138.036551263121));
#175182=CARTESIAN_POINT('Ctrl Pts',(8.89999999999897,-54.8737336732754,
-138.014810226815));
#175183=CARTESIAN_POINT('Ctrl Pts',(8.9,-55.2961699598647,-137.892092266279));
#175184=CARTESIAN_POINT('Ctrl Pts',(9.31869380983081,-54.964336399011,-138.449211290729));
#175185=CARTESIAN_POINT('Ctrl Pts',(8.89999999999893,-55.0269063853653,
-138.419560264108));
#175186=CARTESIAN_POINT('Ctrl Pts',(8.9,-55.4259022184636,-138.270266767248));
#175187=CARTESIAN_POINT('Ctrl Pts',(9.30242220788036,-55.154765272597,-138.840493482357));
#175188=CARTESIAN_POINT('Ctrl Pts',(8.89999999999998,-55.2270244231137,
-138.805989056796));
#175189=CARTESIAN_POINT('Ctrl Pts',(8.9,-55.5972887473373,-138.629184351487));
#175190=CARTESIAN_POINT('',(8.9,-55.5972887473373,-138.629184351487));
#175191=CARTESIAN_POINT('Origin',(9.4,-55.5972887473373,-138.629184351487));
#175192=CARTESIAN_POINT('Ctrl Pts',(8.9,-55.5972887473373,-138.629184351487));
#175193=CARTESIAN_POINT('Ctrl Pts',(8.9,-55.4856871847872,-138.395468415773));
#175194=CARTESIAN_POINT('Ctrl Pts',(8.9,-55.3917128230548,-138.153503053547));
#175195=CARTESIAN_POINT('Ctrl Pts',(8.9,-55.3159696737911,-137.907364658634));
#175196=CARTESIAN_POINT('Ctrl Pts',(8.9,-55.2754252840371,-137.775609759164));
#175197=CARTESIAN_POINT('Ctrl Pts',(8.9,-55.2401039344703,-137.642659649433));
#175198=CARTESIAN_POINT('Ctrl Pts',(8.9,-55.2100924708571,-137.509141392841));
#175199=CARTESIAN_POINT('Ctrl Pts',(8.9,-55.1385732376582,-137.190958865905));
#175200=CARTESIAN_POINT('Ctrl Pts',(8.9,-55.0960936141186,-136.867828326609));
#175201=CARTESIAN_POINT('Ctrl Pts',(8.9,-55.0837682332358,-136.539559845945));
#175202=CARTESIAN_POINT('Ctrl Pts',(8.9,-55.0812593131245,-136.472738430779));
#175203=CARTESIAN_POINT('Ctrl Pts',(8.9,-55.08000002,-136.40570409352));
#175204=CARTESIAN_POINT('Ctrl Pts',(8.9,-55.08000002,-136.338455187671));
#175205=CARTESIAN_POINT('Ctrl Pts',(8.9,-71.0715121820529,-171.237717270032));
#175206=CARTESIAN_POINT('Ctrl Pts',(8.89999999999996,-70.6807353060531,
-171.422308714525));
#175207=CARTESIAN_POINT('Ctrl Pts',(9.3276302147955,-70.6241744288951,-171.449026400902));
#175208=CARTESIAN_POINT('Ctrl Pts',(8.9,-65.932751045448,-160.359049360718));
#175209=CARTESIAN_POINT('Ctrl Pts',(8.89999999999997,-65.5751008964372,
-160.600947379136));
#175210=CARTESIAN_POINT('Ctrl Pts',(9.32139302491482,-65.48642588992,-160.570366012028));
#175211=CARTESIAN_POINT('Ctrl Pts',(8.9,-60.7816272203214,-149.486223352848));
#175212=CARTESIAN_POINT('Ctrl Pts',(8.89999999996837,-60.4515277778623,
-149.769759336176));
#175213=CARTESIAN_POINT('Ctrl Pts',(9.31373872503275,-60.3366136221522,
-149.697543381378));
#175214=CARTESIAN_POINT('Ctrl Pts',(8.9,-55.5972887473373,-138.629184351487));
#175215=CARTESIAN_POINT('Ctrl Pts',(8.89999999999998,-55.2270244231145,
-138.805989056796));
#175216=CARTESIAN_POINT('Ctrl Pts',(9.30242220787994,-55.1547652725975,
-138.840493482357));
#175217=CARTESIAN_POINT('',(8.9,-71.0715121820529,-171.237717270032));
#175218=CARTESIAN_POINT('',(9.3276302147955,-70.6241744288951,-171.449026400902));
#175219=CARTESIAN_POINT('Origin',(9.4,-71.0715121820529,-171.237717270032));
#175220=CARTESIAN_POINT('Ctrl Pts',(9.30242220787652,-55.1547652726017,
-138.840493482365));
#175221=CARTESIAN_POINT('Ctrl Pts',(9.30502066599635,-56.3446027211807,
-141.333450373329));
#175222=CARTESIAN_POINT('Ctrl Pts',(9.30762015406821,-57.5854232432311,
-143.937974471921));
#175223=CARTESIAN_POINT('Ctrl Pts',(9.31122614649335,-59.523163084648,-148.012111431249));
#175224=CARTESIAN_POINT('Ctrl Pts',(9.31238561873438,-60.1818270656114,
-149.398048886265));
#175225=CARTESIAN_POINT('Ctrl Pts',(9.31408147943844,-61.1889472073688,
-151.518792771649));
#175226=CARTESIAN_POINT('Ctrl Pts',(9.31491917086314,-61.6972882651846,
-152.589624140057));
#175227=CARTESIAN_POINT('Ctrl Pts',(9.31588935336845,-62.2987186132309,
-153.8572313982));
#175228=CARTESIAN_POINT('Ctrl Pts',(9.3163744849145,-62.6015250786792,-154.495611026022));
#175229=CARTESIAN_POINT('Ctrl Pts',(9.31664331763924,-62.7697289037899,
-154.850266319648));
#175230=CARTESIAN_POINT('Ctrl Pts',(9.31677352444865,-62.8512928935264,
-155.0222567554));
#175231=CARTESIAN_POINT('Ctrl Pts',(9.31684300904555,-62.8948372533087,
-155.114080321108));
#175232=CARTESIAN_POINT('Ctrl Pts',(9.31685291467516,-62.90104528335,-155.127171497753));
#175233=CARTESIAN_POINT('Ctrl Pts',(9.32068386750567,-65.3020872796149,
-160.190390144699));
#175234=CARTESIAN_POINT('Ctrl Pts',(9.32429261610782,-67.874900615077,-165.627718505107));
#175235=CARTESIAN_POINT('Ctrl Pts',(9.3276302147955,-70.6241744288951,-171.449026400902));
#175236=CARTESIAN_POINT('Ctrl Pts',(8.9,-71.0715121820529,-171.237717270032));
#175237=CARTESIAN_POINT('Ctrl Pts',(8.9,-65.932751045448,-160.359049360718));
#175238=CARTESIAN_POINT('Ctrl Pts',(8.9,-60.7816272203214,-149.486223352848));
#175239=CARTESIAN_POINT('Ctrl Pts',(8.9,-55.5972887473373,-138.629184351487));
#175240=CARTESIAN_POINT('Ctrl Pts',(8.9,-55.5972887473416,-93.4294586200098));
#175241=CARTESIAN_POINT('Ctrl Pts',(8.89999999999997,-55.2270244231188,
-93.2526539147005));
#175242=CARTESIAN_POINT('Ctrl Pts',(9.30242220787995,-55.1547652726018,
-93.2181494891395));
#175243=CARTESIAN_POINT('Ctrl Pts',(8.9,-60.7433024895534,-82.6526792495127));
#175244=CARTESIAN_POINT('Ctrl Pts',(8.89999999981176,-60.4125449242165,
-82.3706902717217));
#175245=CARTESIAN_POINT('Ctrl Pts',(9.31365506854171,-60.298307210959,-82.4413594877101));
#175246=CARTESIAN_POINT('Ctrl Pts',(8.9,-65.8565639782118,-71.8603324984455));
#175247=CARTESIAN_POINT('Ctrl Pts',(8.89999999999997,-65.4986935712713,
-71.6191417519029));
#175248=CARTESIAN_POINT('Ctrl Pts',(9.32127686740287,-65.4102595335587,
-71.6490160146723));
#175249=CARTESIAN_POINT('Ctrl Pts',(8.9,-70.9575466375288,-61.0621827299711));
#175250=CARTESIAN_POINT('Ctrl Pts',(8.89999999999996,-70.5668839574465,
-60.8776359696917));
#175251=CARTESIAN_POINT('Ctrl Pts',(9.32749162718857,-70.5102313269446,
-60.8508735991008));
#175252=CARTESIAN_POINT('',(9.32749162718857,-70.5102313269446,-60.8508735991008));
#175253=CARTESIAN_POINT('Ctrl Pts',(9.32749162718857,-70.5102313269446,
-60.8508735991008));
#175254=CARTESIAN_POINT('Ctrl Pts',(9.32582952826763,-69.1462755360622,
-63.7387697434672));
#175255=CARTESIAN_POINT('Ctrl Pts',(9.32415588545215,-67.8258212790612,
-66.5319899948945));
#175256=CARTESIAN_POINT('Ctrl Pts',(9.32147279007466,-65.91040469489,-70.579806532627));
#175257=CARTESIAN_POINT('Ctrl Pts',(9.32055305784016,-65.2828097278533,
-71.9054097386364));
#175258=CARTESIAN_POINT('Ctrl Pts',(9.31914659172631,-64.3577321272153,
-73.8583110877983));
#175259=CARTESIAN_POINT('Ctrl Pts',(9.31843696007727,-63.8992720094891,
-74.8258858974162));
#175260=CARTESIAN_POINT('Ctrl Pts',(9.31760366459636,-63.3715390091911,
-75.9391904116184));
#175261=CARTESIAN_POINT('Ctrl Pts',(9.31713451737182,-63.0766964068097,
-76.5610556110707));
#175262=CARTESIAN_POINT('Ctrl Pts',(9.31690371853256,-62.9322529809882,
-76.8656644741659));
#175263=CARTESIAN_POINT('Ctrl Pts',(9.31678465495306,-62.8578608284992,
-77.0225352384175));
#175264=CARTESIAN_POINT('Ctrl Pts',(9.31677841983388,-62.8539654033096,
-77.0307494927582));
#175265=CARTESIAN_POINT('Ctrl Pts',(9.31234247770848,-60.0829432119856,
-82.8739514734244));
#175266=CARTESIAN_POINT('Ctrl Pts',(9.30758397812651,-57.5183467731809,
-88.265954719794));
#175267=CARTESIAN_POINT('Ctrl Pts',(9.30242220787995,-55.1547652726018,
-93.2181494891395));
#175268=CARTESIAN_POINT('',(8.9,-70.9575466375288,-61.0621827299711));
#175269=CARTESIAN_POINT('Origin',(9.4,-70.9575466375288,-61.0621827299711));
#175270=CARTESIAN_POINT('Ctrl Pts',(8.9,-55.5972887473416,-93.4294586200098));
#175271=CARTESIAN_POINT('Ctrl Pts',(8.9,-60.7433024895534,-82.6526792495127));
#175272=CARTESIAN_POINT('Ctrl Pts',(8.9,-65.8565639782118,-71.8603324984455));
#175273=CARTESIAN_POINT('Ctrl Pts',(8.9,-70.9575466375288,-61.0621827299711));
#175274=CARTESIAN_POINT('Origin',(8.4,-72.58000002,-55.24995));
#175275=CARTESIAN_POINT('',(8.4,-73.08000002,-174.451268889151));
#175276=CARTESIAN_POINT('',(8.9,-72.58000002,-174.451268889151));
#175277=CARTESIAN_POINT('Origin',(8.4,-72.58000002,-174.451268889151));
#175278=CARTESIAN_POINT('',(8.9,-72.58000002,-58.1763194612681));
#175279=CARTESIAN_POINT('',(8.9,-72.58000002,-174.432329119515));
#175280=CARTESIAN_POINT('',(8.4,-73.08000002,-58.1763194612681));
#175281=CARTESIAN_POINT('Origin',(8.4,-72.58000002,-58.1763194612681));
#175282=CARTESIAN_POINT('',(8.4,-73.08000002,-58.1922197332626));
#175283=CARTESIAN_POINT('Origin',(-3.54807775957937E-14,-73.08000002,3.11172719585489E-30));
#175284=CARTESIAN_POINT('',(7.9,-73.08000002,-58.1594740865074));
#175285=CARTESIAN_POINT('Ctrl Pts',(8.4,-73.08000002,-58.1763194612681));
#175286=CARTESIAN_POINT('Ctrl Pts',(8.23332974561635,-73.08000002,-58.1708448514923));
#175287=CARTESIAN_POINT('Ctrl Pts',(8.06666350196851,-73.08000002,-58.1652131587787));
#175288=CARTESIAN_POINT('Ctrl Pts',(7.9,-73.08000002,-58.1594740865074));
#175289=CARTESIAN_POINT('',(7.9,-73.08000002,-174.471034982976));
#175290=CARTESIAN_POINT('',(7.9,-73.08000002,-174.491325336599));
#175291=CARTESIAN_POINT('Ctrl Pts',(7.9,-73.08000002,-174.471034982976));
#175292=CARTESIAN_POINT('Ctrl Pts',(8.06666381945983,-73.08000002,-174.464342510025));
#175293=CARTESIAN_POINT('Ctrl Pts',(8.23333002609749,-73.08000002,-174.457737044943));
#175294=CARTESIAN_POINT('Ctrl Pts',(8.4,-73.08000002,-174.451268889151));
#175295=CARTESIAN_POINT('Origin',(7.9,-72.58000002,-55.24995));
#175296=CARTESIAN_POINT('',(7.4,-72.58000002,-58.1594740865074));
#175297=CARTESIAN_POINT('Origin',(7.9,-72.58000002,-58.1594740865074));
#175298=CARTESIAN_POINT('',(7.4,-72.58000002,-174.471034982976));
#175299=CARTESIAN_POINT('',(7.4,-72.58000002,-58.1419820049528));
#175300=CARTESIAN_POINT('Origin',(7.9,-72.58000002,-174.471034982976));
#175301=CARTESIAN_POINT('Ctrl Pts',(7.4,-55.5541151520872,-137.531452880088));
#175302=CARTESIAN_POINT('Ctrl Pts',(7.39999999999997,-55.0309624818203,
-137.77858424555));
#175303=CARTESIAN_POINT('Ctrl Pts',(6.82752390105444,-55.106794611208,-137.742762010959));
#175304=CARTESIAN_POINT('Ctrl Pts',(7.4,-60.858236996045,-148.759754479668));
#175305=CARTESIAN_POINT('Ctrl Pts',(7.39999999999996,-60.2903951615484,
-148.888188464867));
#175306=CARTESIAN_POINT('Ctrl Pts',(6.83631982946675,-60.4094944461354,
-148.971070239217));
#175307=CARTESIAN_POINT('Ctrl Pts',(7.4,-66.1431501582269,-159.997106821727));
#175308=CARTESIAN_POINT('Ctrl Pts',(7.40000000024359,-65.6065688428949,
-160.175729571892));
#175309=CARTESIAN_POINT('Ctrl Pts',(6.84214680798085,-65.6936814170396,
-160.208420694715));
#175310=CARTESIAN_POINT('Ctrl Pts',(7.4,-71.4211246238516,-171.237717270032));
#175311=CARTESIAN_POINT('Ctrl Pts',(7.39999999999995,-70.9175980522951,
-171.474145745141));
#175312=CARTESIAN_POINT('Ctrl Pts',(6.84687749809456,-70.9710952348089,
-171.449026400902));
#175313=CARTESIAN_POINT('',(6.84687749809456,-70.9710952348089,-171.449026400902));
#175314=CARTESIAN_POINT('',(7.4,-71.4211246238516,-171.237717270032));
#175315=CARTESIAN_POINT('Origin',(6.9,-71.4211246238516,-171.237717270032));
#175316=CARTESIAN_POINT('',(7.4,-55.5541151520872,-137.531452880088));
#175317=CARTESIAN_POINT('Ctrl Pts',(7.4,-55.5541151520872,-137.531452880088));
#175318=CARTESIAN_POINT('Ctrl Pts',(7.4,-60.858236996045,-148.759754479668));
#175319=CARTESIAN_POINT('Ctrl Pts',(7.4,-66.1431501582269,-159.997106821727));
#175320=CARTESIAN_POINT('Ctrl Pts',(7.4,-71.4211246238516,-171.237717270032));
#175321=CARTESIAN_POINT('Origin',(6.9,-55.5541151520872,-137.531452880088));
#175322=CARTESIAN_POINT('Ctrl Pts',(6.84687749809456,-70.9710952348089,
-171.449026400902));
#175323=CARTESIAN_POINT('Ctrl Pts',(6.84560962234199,-69.5566916474712,
-168.436423337422));
#175324=CARTESIAN_POINT('Ctrl Pts',(6.84434141864909,-68.1892497014956,
-165.525328844702));
#175325=CARTESIAN_POINT('Ctrl Pts',(6.84229651062739,-66.2085386323005,
-161.310949961766));
#175326=CARTESIAN_POINT('Ctrl Pts',(6.84124275267032,-65.2357958436729,
-159.241826234334));
#175327=CARTESIAN_POINT('Ctrl Pts',(6.83997337454142,-64.1317508737894,
-156.894463551891));
#175328=CARTESIAN_POINT('Ctrl Pts',(6.83933395326739,-63.5874334599924,
-155.73743596056));
#175329=CARTESIAN_POINT('Ctrl Pts',(6.83897379504999,-63.2834219089447,
-155.091291807594));
#175330=CARTESIAN_POINT('Ctrl Pts',(6.83879657177648,-63.134517564385,-154.774836350161));
#175331=CARTESIAN_POINT('Ctrl Pts',(6.83870513850053,-63.0578356875946,
-154.611876236652));
#175332=CARTESIAN_POINT('Ctrl Pts',(6.83870038730762,-63.0538514139574,
-154.603409094398));
#175333=CARTESIAN_POINT('Ctrl Pts',(6.83527484268849,-60.1816612512713,
-148.499619545533));
#175334=CARTESIAN_POINT('Ctrl Pts',(6.83155090300906,-57.5345067998195,
-142.883369926133));
#175335=CARTESIAN_POINT('Ctrl Pts',(6.82752390105444,-55.106794611208,-137.742762010959));
#175336=CARTESIAN_POINT('Ctrl Pts',(6.82155174273623,-55.1933079511192,
-137.915802602945));
#175337=CARTESIAN_POINT('Ctrl Pts',(7.40000000000079,-55.1116820355855,
-137.95800482368));
#175338=CARTESIAN_POINT('Ctrl Pts',(7.4,-55.6319612289116,-137.689008690545));
#175339=CARTESIAN_POINT('Ctrl Pts',(6.83574484367583,-54.9750692399274,
-137.49783139603));
#175340=CARTESIAN_POINT('Ctrl Pts',(7.39999999999827,-54.9102656072896,
-137.531225757498));
#175341=CARTESIAN_POINT('Ctrl Pts',(7.4,-55.4355479201386,-137.308418641867));
#175342=CARTESIAN_POINT('Ctrl Pts',(6.84992613641256,-54.8164562186196,
-137.062923068212));
#175343=CARTESIAN_POINT('Ctrl Pts',(7.39999999999997,-54.7649351562061,
-137.085189013788));
#175344=CARTESIAN_POINT('Ctrl Pts',(7.4,-55.2927998688587,-136.91270337825));
#175345=CARTESIAN_POINT('Ctrl Pts',(6.87803385475026,-54.6118666660822,
-136.161406076667));
#175346=CARTESIAN_POINT('Ctrl Pts',(7.39999999999997,-54.5904817529938,
-136.169973106407));
#175347=CARTESIAN_POINT('Ctrl Pts',(7.4,-55.1086754192619,-136.09302879305));
#175348=CARTESIAN_POINT('Ctrl Pts',(6.89206539026919,-54.566470030062,-135.690989882161));
#175349=CARTESIAN_POINT('Ctrl Pts',(7.40000000000168,-54.5583847259971,
-135.696616305969));
#175350=CARTESIAN_POINT('Ctrl Pts',(7.4,-55.0678212801175,-135.665613736665));
#175351=CARTESIAN_POINT('Ctrl Pts',(6.90540919710522,-54.5834976982804,
-135.222393609581));
#175352=CARTESIAN_POINT('Ctrl Pts',(7.39999999999918,-54.5888446965326,
-135.222564106606));
#175353=CARTESIAN_POINT('Ctrl Pts',(7.4,-55.0831491250257,-135.24013604883));
#175354=CARTESIAN_POINT('',(7.4,-55.08000002,-135.415380765739));
#175355=CARTESIAN_POINT('Ctrl Pts',(7.4,-55.08000002,-135.415380765739));
#175356=CARTESIAN_POINT('Ctrl Pts',(7.4,-55.08000002,-135.642528198471));
#175357=CARTESIAN_POINT('Ctrl Pts',(7.4,-55.0958102967117,-135.869567477776));
#175358=CARTESIAN_POINT('Ctrl Pts',(7.4,-55.1266901212397,-136.093433076221));
#175359=CARTESIAN_POINT('Ctrl Pts',(7.4,-55.1457148268955,-136.231354103363));
#175360=CARTESIAN_POINT('Ctrl Pts',(7.4,-55.1704583130128,-136.368070310451));
#175361=CARTESIAN_POINT('Ctrl Pts',(7.4,-55.2007376448274,-136.502866089854));
#175362=CARTESIAN_POINT('Ctrl Pts',(7.4,-55.2691608068209,-136.807468367956));
#175363=CARTESIAN_POINT('Ctrl Pts',(7.4,-55.3655723350795,-137.104245532169));
#175364=CARTESIAN_POINT('Ctrl Pts',(7.4,-55.4912205286075,-137.392848584246));
#175365=CARTESIAN_POINT('Ctrl Pts',(7.4,-55.5114273685592,-137.439261950958));
#175366=CARTESIAN_POINT('Ctrl Pts',(7.4,-55.5323904712439,-137.485463878358));
#175367=CARTESIAN_POINT('Ctrl Pts',(7.4,-55.5541151520872,-137.531452880088));
#175368=CARTESIAN_POINT('Origin',(6.9,-55.08000002,-135.415380765739));
#175369=CARTESIAN_POINT('Origin',(6.9,-55.08000002,-55.24995));
#175370=CARTESIAN_POINT('',(7.4,-55.08000002,-96.6432622057672));
#175371=CARTESIAN_POINT('',(7.4,-55.08000002,-135.57795249279));
#175372=CARTESIAN_POINT('Origin',(6.9,-55.08000002,-96.6432622057672));
#175373=CARTESIAN_POINT('Ctrl Pts',(6.9,-54.58000002,-96.6432622057672));
#175374=CARTESIAN_POINT('Ctrl Pts',(7.39999999999996,-54.58000002,-96.6432622057672));
#175375=CARTESIAN_POINT('Ctrl Pts',(7.4,-55.08000002,-96.6432622057672));
#175376=CARTESIAN_POINT('Ctrl Pts',(6.8883412776675,-54.58000002,-96.2390470799649));
#175377=CARTESIAN_POINT('Ctrl Pts',(7.39999999999997,-54.5682037738145,
-96.2342789461818));
#175378=CARTESIAN_POINT('Ctrl Pts',(7.4,-55.0800000228223,-96.276173584436));
#175379=CARTESIAN_POINT('Ctrl Pts',(6.87644795534686,-54.6248256750472,
-95.842546745885));
#175380=CARTESIAN_POINT('Ctrl Pts',(7.39999999999997,-54.6014014206736,
-95.8348803330818));
#175381=CARTESIAN_POINT('Ctrl Pts',(7.4,-55.1203431091477,-95.9158883524807));
#175382=CARTESIAN_POINT('Ctrl Pts',(6.85220551019199,-54.8002766424245,
-95.064563743706));
#175383=CARTESIAN_POINT('Ctrl Pts',(7.39999999999995,-54.7508604913788,
-95.0452270964761));
#175384=CARTESIAN_POINT('Ctrl Pts',(7.4,-55.2782489805768,-95.2085406483778));
#175385=CARTESIAN_POINT('Ctrl Pts',(6.83977061757738,-54.9324757245047,
-94.6806963574476));
#175386=CARTESIAN_POINT('Ctrl Pts',(7.39999999999369,-54.8709621105524,
-94.6521767160421));
#175387=CARTESIAN_POINT('Ctrl Pts',(7.4,-55.3972278356279,-94.8593050327909));
#175388=CARTESIAN_POINT('Ctrl Pts',(6.82752390105444,-55.106794611208,-94.3158809605474));
#175389=CARTESIAN_POINT('Ctrl Pts',(7.39999999999997,-55.0309624818203,
-94.2800587259558));
#175390=CARTESIAN_POINT('Ctrl Pts',(7.4,-55.5541151520872,-94.5271900914177));
#175391=CARTESIAN_POINT('',(7.4,-55.5541151520872,-94.5271900914178));
#175392=CARTESIAN_POINT('Ctrl Pts',(7.4,-55.5541151520872,-94.5271900914178));
#175393=CARTESIAN_POINT('Ctrl Pts',(7.4,-55.4646684466496,-94.7165399244866));
#175394=CARTESIAN_POINT('Ctrl Pts',(7.4,-55.3874966670403,-94.9115657139011));
#175395=CARTESIAN_POINT('Ctrl Pts',(7.4,-55.3230550301972,-95.1098279144973));
#175396=CARTESIAN_POINT('Ctrl Pts',(7.4,-55.2745243397298,-95.2591382355855));
#175397=CARTESIAN_POINT('Ctrl Pts',(7.4,-55.2332126733291,-95.4102831677243));
#175398=CARTESIAN_POINT('Ctrl Pts',(7.4,-55.199296044664,-95.5622145003849));
#175399=CARTESIAN_POINT('Ctrl Pts',(7.4,-55.1306219000107,-95.8698439649617));
#175400=CARTESIAN_POINT('Ctrl Pts',(7.4,-55.0911602505336,-96.1824496092641));
#175401=CARTESIAN_POINT('Ctrl Pts',(7.4,-55.0820478268106,-96.5002250748419));
#175402=CARTESIAN_POINT('Ctrl Pts',(7.4,-55.0806839263479,-96.5477880633181));
#175403=CARTESIAN_POINT('Ctrl Pts',(7.4,-55.08000002,-96.5954668848809));
#175404=CARTESIAN_POINT('Ctrl Pts',(7.4,-55.08000002,-96.6432622057672));
#175405=CARTESIAN_POINT('',(6.82752390124981,-55.1067946109655,-94.3158809609937));
#175406=CARTESIAN_POINT('Origin',(6.9,-55.5541151520872,-94.5271900914178));
#175407=CARTESIAN_POINT('Ctrl Pts',(6.9,-54.58000002,-96.6432622057672));
#175408=CARTESIAN_POINT('Ctrl Pts',(6.89747516029584,-54.58000002,-96.5557244490382));
#175409=CARTESIAN_POINT('Ctrl Pts',(6.89483138514496,-54.5820978077061,
-96.4637717709372));
#175410=CARTESIAN_POINT('Ctrl Pts',(6.89203565904072,-54.5869879127523,
-96.3675661682017));
#175411=CARTESIAN_POINT('Ctrl Pts',(6.88947633569459,-54.5914645172348,
-96.2794955790493));
#175412=CARTESIAN_POINT('Ctrl Pts',(6.88678966447231,-54.5982820020438,
-96.1878610154668));
#175413=CARTESIAN_POINT('Ctrl Pts',(6.88394936679525,-54.6080107494815,
-96.0927938740058));
#175414=CARTESIAN_POINT('Ctrl Pts',(6.88097789104612,-54.6181888154334,
-95.9933360926358));
#175415=CARTESIAN_POINT('Ctrl Pts',(6.87784445989682,-54.6315541980301,
-95.890142050635));
#175416=CARTESIAN_POINT('Ctrl Pts',(6.87456401227554,-54.6487592943821,
-95.7835116338186));
#175417=CARTESIAN_POINT('Ctrl Pts',(6.8729237884649,-54.6573618425582,-95.7301964254104));
#175418=CARTESIAN_POINT('Ctrl Pts',(6.87124734708462,-54.6669241215913,
-95.6760238582546));
#175419=CARTESIAN_POINT('Ctrl Pts',(6.86953990780671,-54.6775244017527,
-95.6210418063674));
#175420=CARTESIAN_POINT('Ctrl Pts',(6.86868618816775,-54.6828245418335,
-95.5935507804238));
#175421=CARTESIAN_POINT('Ctrl Pts',(6.86782471473417,-54.6883841572439,
-95.5658573703005));
#175422=CARTESIAN_POINT('Ctrl Pts',(6.86695640095496,-54.6942126277729,
-95.5379683292162));
#175423=CARTESIAN_POINT('Ctrl Pts',(6.86652224406536,-54.6971268630374,
-95.524023808674));
#175424=CARTESIAN_POINT('Ctrl Pts',(6.86608637653929,-54.7001083092455,
-95.510030378775));
#175425=CARTESIAN_POINT('Ctrl Pts',(6.86564891907798,-54.7031581143021,
-95.4959889008478));
#175426=CARTESIAN_POINT('Ctrl Pts',(6.86543019034733,-54.7046830168303,
-95.4889681618842));
#175427=CARTESIAN_POINT('Ctrl Pts',(6.86521106409204,-54.7062250088754,
-95.4819354107944));
#175428=CARTESIAN_POINT('Ctrl Pts',(6.86499155622248,-54.7077842319553,
-95.4748907575898));
#175429=CARTESIAN_POINT('Ctrl Pts',(6.86488180228771,-54.7085638434952,
-95.4713684309875));
#175430=CARTESIAN_POINT('Ctrl Pts',(6.86477195294651,-54.7093477627807,
-95.4678431288482));
#175431=CARTESIAN_POINT('Ctrl Pts',(6.8646620102436,-54.7101360073698,-95.4643148650801));
#175432=CARTESIAN_POINT('Ctrl Pts',(6.86455206754068,-54.7109242519588,
-95.460786601312));
#175433=CARTESIAN_POINT('Ctrl Pts',(6.86438870235264,-54.7121027263867,
-95.4555439545126));
#175434=CARTESIAN_POINT('Ctrl Pts',(6.86433190484278,-54.7125137344833,
-95.453721202814));
#175435=CARTESIAN_POINT('Ctrl Pts',(6.86433018162012,-54.7125262043691,
-95.4536659009699));
#175436=CARTESIAN_POINT('Ctrl Pts',(6.86432845787219,-54.7125386791002,
-95.453610581626));
#175437=CARTESIAN_POINT('Ctrl Pts',(6.86432673359892,-54.712551158678,-95.4535552447826));
#175438=CARTESIAN_POINT('Ctrl Pts',(6.86351930135692,-54.7183950198008,
-95.4276424428322));
#175439=CARTESIAN_POINT('Ctrl Pts',(6.86259629795188,-54.7253045249752,
-95.3978804668901));
#175440=CARTESIAN_POINT('Ctrl Pts',(6.86155176392851,-54.7334765966147,
-95.3643212878303));
#175441=CARTESIAN_POINT('Ctrl Pts',(6.86051181961651,-54.7416127599454,
-95.3309095687308));
#175442=CARTESIAN_POINT('Ctrl Pts',(6.85935139548513,-54.7510005850816,
-95.2937335050213));
#175443=CARTESIAN_POINT('Ctrl Pts',(6.85806469255273,-54.7618822044733,
-95.2528636616271));
#175444=CARTESIAN_POINT('Ctrl Pts',(6.8577356277149,-54.7646650988231,-95.2424114989327));
#175445=CARTESIAN_POINT('Ctrl Pts',(6.85739830478949,-54.7675459309099,
-95.2317178653169));
#175446=CARTESIAN_POINT('Ctrl Pts',(6.85705262961774,-54.7705292349977,
-95.2207842021938));
#175447=CARTESIAN_POINT('Ctrl Pts',(6.85571293772219,-54.7820912696329,
-95.1784099124803));
#175448=CARTESIAN_POINT('Ctrl Pts',(6.85424828974271,-54.7951888263501,
-95.1324292778536));
#175449=CARTESIAN_POINT('Ctrl Pts',(6.85266114233615,-54.8101095220533,
-95.0829520905385));
#175450=CARTESIAN_POINT('Ctrl Pts',(6.85243695912735,-54.8122170575137,
-95.0759634803005));
#175451=CARTESIAN_POINT('Ctrl Pts',(6.8522103329922,-54.8143610336592,-95.0689051620074));
#175452=CARTESIAN_POINT('Ctrl Pts',(6.85198127202152,-54.8165423261462,
-95.0617774993062));
#175453=CARTESIAN_POINT('Ctrl Pts',(6.85105590131421,-54.8253544086477,
-95.0329828501979));
#175454=CARTESIAN_POINT('Ctrl Pts',(6.85009096050149,-54.8347751397566,
-95.0030562681139));
#175455=CARTESIAN_POINT('Ctrl Pts',(6.84908838500605,-54.8448644132515,
-94.9720250304464));
#175456=CARTESIAN_POINT('Ctrl Pts',(6.84858709725833,-54.8499090499989,
-94.9565094116127));
#175457=CARTESIAN_POINT('Ctrl Pts',(6.84807640877095,-54.8551208983739,
-94.940717653009));
#175458=CARTESIAN_POINT('Ctrl Pts',(6.84755689936396,-54.8605077376624,
-94.9246536948557));
#175459=CARTESIAN_POINT('Ctrl Pts',(6.847151051795,-54.8647160072338,-94.9121043198558));
#175460=CARTESIAN_POINT('Ctrl Pts',(6.84671716909453,-54.8692741665164,
-94.8986776066087));
#175461=CARTESIAN_POINT('Ctrl Pts',(6.84630851886264,-54.8736171201975,
-94.8860425593514));
#175462=CARTESIAN_POINT('Ctrl Pts',(6.84619407210966,-54.8748334096018,
-94.88250398279));
#175463=CARTESIAN_POINT('Ctrl Pts',(6.84608160495438,-54.8760325092529,
-94.8790274153598));
#175464=CARTESIAN_POINT('Ctrl Pts',(6.84597228850087,-54.8772013065748,
-94.8756493244326));
#175465=CARTESIAN_POINT('Ctrl Pts',(6.84397369594434,-54.8985699985937,
-94.8138889291219));
#175466=CARTESIAN_POINT('Ctrl Pts',(6.84208965831291,-54.9198341771577,
-94.7560365588245));
#175467=CARTESIAN_POINT('Ctrl Pts',(6.84032134685682,-54.9406229360708,
-94.7020029951088));
#175468=CARTESIAN_POINT('Ctrl Pts',(6.83855714785133,-54.9613633478765,
-94.6480950938497));
#175469=CARTESIAN_POINT('Ctrl Pts',(6.8369081109529,-54.9816307635276,-94.5979875534939));
#175470=CARTESIAN_POINT('Ctrl Pts',(6.83537425787087,-55.001110405453,-94.551575598675));
#175471=CARTESIAN_POINT('Ctrl Pts',(6.83381061644668,-55.0209683536487,
-94.5042622959978));
#175472=CARTESIAN_POINT('Ctrl Pts',(6.83236665529882,-55.0400076472729,
-94.4607889078687));
#175473=CARTESIAN_POINT('Ctrl Pts',(6.83104156414129,-55.0579490545743,
-94.4210374968657));
#175474=CARTESIAN_POINT('Ctrl Pts',(6.82975787054648,-55.0753299490915,
-94.3825279713894));
#175475=CARTESIAN_POINT('Ctrl Pts',(6.82858571520043,-55.0916808891523,
-94.347511028551));
#175476=CARTESIAN_POINT('Ctrl Pts',(6.82752390106997,-55.106794610987,-94.31588096101));
#175477=CARTESIAN_POINT('Ctrl Pts',(7.4,-71.3078420373655,-61.0621827299711));
#175478=CARTESIAN_POINT('Ctrl Pts',(7.39999999999997,-70.8042142666047,
-60.8257004209668));
#175479=CARTESIAN_POINT('Ctrl Pts',(6.84677576889373,-70.8578246683297,
-60.8508735991007));
#175480=CARTESIAN_POINT('Ctrl Pts',(7.4,-66.0675133276181,-72.2223201517098));
#175481=CARTESIAN_POINT('Ctrl Pts',(7.39999999999996,-65.5311408351844,
-72.0430210271706));
#175482=CARTESIAN_POINT('Ctrl Pts',(6.84206094040904,-65.61805576689,-72.0110063808198));
#175483=CARTESIAN_POINT('Ctrl Pts',(7.4,-60.8202894597531,-83.3792196747323));
#175484=CARTESIAN_POINT('Ctrl Pts',(7.39999999995234,-60.2531402990131,
-83.2491486934777));
#175485=CARTESIAN_POINT('Ctrl Pts',(6.83625690025051,-60.3715570323219,
-83.1679040708394));
#175486=CARTESIAN_POINT('Ctrl Pts',(7.4,-55.5541151520872,-94.5271900914177));
#175487=CARTESIAN_POINT('Ctrl Pts',(7.39999999999997,-55.0309624818203,
-94.2800587259558));
#175488=CARTESIAN_POINT('Ctrl Pts',(6.82752390105444,-55.106794611208,-94.3158809605474));
#175489=CARTESIAN_POINT('',(7.4,-71.3078420373655,-61.0621827299711));
#175490=CARTESIAN_POINT('Ctrl Pts',(7.4,-71.3078420373655,-61.0621827299711));
#175491=CARTESIAN_POINT('Ctrl Pts',(7.4,-66.0675133276181,-72.2223201517098));
#175492=CARTESIAN_POINT('Ctrl Pts',(7.4,-60.8202894597531,-83.3792196747323));
#175493=CARTESIAN_POINT('Ctrl Pts',(7.4,-55.5541151520872,-94.5271900914177));
#175494=CARTESIAN_POINT('',(6.84677576889373,-70.8578246683297,-60.8508735991007));
#175495=CARTESIAN_POINT('Origin',(6.9,-71.3078420373655,-61.0621827299711));
#175496=CARTESIAN_POINT('Ctrl Pts',(6.82752390105444,-55.106794611208,-94.3158809605474));
#175497=CARTESIAN_POINT('Ctrl Pts',(6.82952415560735,-56.3126649847602,
-91.7624865276987));
#175498=CARTESIAN_POINT('Ctrl Pts',(6.8315454834894,-57.5727256222142,-89.0918089072798));
#175499=CARTESIAN_POINT('Ctrl Pts',(6.83340376219997,-58.8869041773412,
-86.3038079768894));
#175500=CARTESIAN_POINT('Ctrl Pts',(6.83433290155526,-59.5439934549047,
-84.9098075116943));
#175501=CARTESIAN_POINT('Ctrl Pts',(6.83522669847064,-60.2146122398928,
-83.4864764706228));
#175502=CARTESIAN_POINT('Ctrl Pts',(6.83609469396308,-60.8987533307654,
-82.0338119093995));
#175503=CARTESIAN_POINT('Ctrl Pts',(6.83652869170931,-61.2408238762017,
-81.3074796287878));
#175504=CARTESIAN_POINT('Ctrl Pts',(6.83695657838775,-61.5862750307562,
-80.5738139942268));
#175505=CARTESIAN_POINT('Ctrl Pts',(6.83738159482193,-61.9351061371133,
-79.8328148104165));
#175506=CARTESIAN_POINT('Ctrl Pts',(6.83759410303902,-62.1095216902918,
-79.4623152185113));
#175507=CARTESIAN_POINT('Ctrl Pts',(6.83780589456058,-62.284782236783,-79.0899822418052));
#175508=CARTESIAN_POINT('Ctrl Pts',(6.83801780376435,-62.4608876783509,
-78.7158158549579));
#175509=CARTESIAN_POINT('Ctrl Pts',(6.83812375836623,-62.5489403991348,
-78.5287326615342));
#175510=CARTESIAN_POINT('Ctrl Pts',(6.83823079828926,-62.6372042208913,
-78.3411910683908));
#175511=CARTESIAN_POINT('Ctrl Pts',(6.83833751782365,-62.7256793104055,
-78.1531911415523));
#175512=CARTESIAN_POINT('Ctrl Pts',(6.83839254508357,-62.7712992784363,
-78.0562536792761));
#175513=CARTESIAN_POINT('Ctrl Pts',(6.83844748719141,-62.8169754159942,
-77.9591943601788));
#175514=CARTESIAN_POINT('Ctrl Pts',(6.83850234420444,-62.8627077234333,
-77.8620131846426));
#175515=CARTESIAN_POINT('Ctrl Pts',(6.83852934414054,-62.885216593501,-77.8141818248084));
#175516=CARTESIAN_POINT('Ctrl Pts',(6.83855632346278,-62.9077390706416,
-77.7663209454311));
#175517=CARTESIAN_POINT('Ctrl Pts',(6.83858328217936,-62.9302751549059,
-77.7184305465605));
#175518=CARTESIAN_POINT('Ctrl Pts',(6.83859665623016,-62.941455165459,-77.6946724189958));
#175519=CARTESIAN_POINT('Ctrl Pts',(6.83861002520974,-62.9526385248478,
-77.6709070264179));
#175520=CARTESIAN_POINT('Ctrl Pts',(6.83862338911918,-62.9638252330791,
-77.6471343688332));
#175521=CARTESIAN_POINT('Ctrl Pts',(6.83862671704584,-62.9666109856172,
-77.6412144199229));
#175522=CARTESIAN_POINT('Ctrl Pts',(6.83863004465809,-62.969396945826,-77.6352940204902));
#175523=CARTESIAN_POINT('Ctrl Pts',(6.83863337195595,-62.9721831137055,
-77.629373170535));
#175524=CARTESIAN_POINT('Ctrl Pts',(6.83863417442051,-62.9728550706734,
-77.6279452033216));
#175525=CARTESIAN_POINT('Ctrl Pts',(6.83863497686678,-62.9735270397206,
-77.6265172099031));
#175526=CARTESIAN_POINT('Ctrl Pts',(6.83863577929477,-62.9741990208472,
-77.6250891902796));
#175527=CARTESIAN_POINT('Ctrl Pts',(6.83863645562837,-62.9747654061459,
-77.6238855711764));
#175528=CARTESIAN_POINT('Ctrl Pts',(6.83863712970764,-62.9753299227988,
-77.6226859227363));
#175529=CARTESIAN_POINT('Ctrl Pts',(6.83863781492277,-62.9759037853613,
-77.6214664130097));
#175530=CARTESIAN_POINT('Ctrl Pts',(6.83864118100574,-62.9787228547662,
-77.6154756361513));
#175531=CARTESIAN_POINT('Ctrl Pts',(6.83864475015493,-62.9817125075398,
-77.609122344141));
#175532=CARTESIAN_POINT('Ctrl Pts',(6.83864816330869,-62.984572000546,-77.6030456438992));
#175533=CARTESIAN_POINT('Ctrl Pts',(6.83864986821899,-62.9860003508123,
-77.6000102609171));
#175534=CARTESIAN_POINT('Ctrl Pts',(6.83865153421473,-62.987396224711,-77.5970438909131));
#175535=CARTESIAN_POINT('Ctrl Pts',(6.83865311659043,-62.9887221396635,
-77.5942261885717));
#175536=CARTESIAN_POINT('Ctrl Pts',(6.83865381739304,-62.9893093609242,
-77.5929782844598));
#175537=CARTESIAN_POINT('Ctrl Pts',(6.83865450179456,-62.9898828602488,
-77.5917595404295));
#175538=CARTESIAN_POINT('Ctrl Pts',(6.83865516591314,-62.990439381622,-77.5905768759047));
#175539=CARTESIAN_POINT('Ctrl Pts',(6.83865566961575,-62.9908614768272,
-77.5896798806604));
#175540=CARTESIAN_POINT('Ctrl Pts',(6.83865616165061,-62.9912738054544,
-77.5888036401762));
#175541=CARTESIAN_POINT('Ctrl Pts',(6.83865664032437,-62.9916749469045,
-77.5879511734013));
#175542=CARTESIAN_POINT('Ctrl Pts',(6.83865696846394,-62.9919499366577,
-77.5873667919368));
#175543=CARTESIAN_POINT('Ctrl Pts',(6.83865729477323,-62.992223397155,-77.5867856602091));
#175544=CARTESIAN_POINT('Ctrl Pts',(6.83865762193763,-62.9924975788079,
-77.5862029958628));
#175545=CARTESIAN_POINT('Ctrl Pts',(6.84001201799662,-64.1275555370883,
-75.1740875375366));
#175546=CARTESIAN_POINT('Ctrl Pts',(6.84132064847969,-65.3028889469105,
-72.6748470242097));
#175547=CARTESIAN_POINT('Ctrl Pts',(6.84258533113874,-66.5185108777293,
-70.0884870713488));
#175548=CARTESIAN_POINT('Ctrl Pts',(6.84378902860916,-67.6755134132239,
-67.6268458757626));
#175549=CARTESIAN_POINT('Ctrl Pts',(6.84495288483861,-68.8690124037817,
-65.08628466818));
#175550=CARTESIAN_POINT('Ctrl Pts',(6.84608524591606,-70.0990616765064,
-62.4668293203369));
#175551=CARTESIAN_POINT('Ctrl Pts',(6.84631667458969,-70.3504555802412,
-61.9314726316618));
#175552=CARTESIAN_POINT('Ctrl Pts',(6.84654681219227,-70.6033763429088,
-61.3928206107334));
#175553=CARTESIAN_POINT('Ctrl Pts',(6.84677576889373,-70.8578246683297,
-60.8508735991007));
#175554=CARTESIAN_POINT('Ctrl Pts',(7.58857520038279,-54.58000002,-96.4164960598359));
#175555=CARTESIAN_POINT('Ctrl Pts',(7.2042299691157,-54.58000002,-95.3011321772634));
#175556=CARTESIAN_POINT('Ctrl Pts',(6.8604212943599,-55.1073456615429,-94.3034047511324));
#175557=CARTESIAN_POINT('Ctrl Pts',(6.56867789944001,-54.58000002,-96.7679442920248));
#175558=CARTESIAN_POINT('Ctrl Pts',(6.23607825680947,-54.580000019985,-95.6541184528592));
#175559=CARTESIAN_POINT('Ctrl Pts',(5.93585888223459,-55.0918247516195,
-94.6548535475511));
#175560=CARTESIAN_POINT('Ctrl Pts',(5.52653095835546,-54.58000002,-97.0582339217052));
#175561=CARTESIAN_POINT('Ctrl Pts',(5.24614565799262,-54.58000002,-95.9461039187036));
#175562=CARTESIAN_POINT('Ctrl Pts',(4.99263467931988,-55.0788453329258,
-94.9451426129372));
#175563=CARTESIAN_POINT('Ctrl Pts',(3.38973164031852,-54.58000002,-97.4945129415963));
#175564=CARTESIAN_POINT('Ctrl Pts',(3.21753929952213,-54.58000002,-96.3846721597723));
#175565=CARTESIAN_POINT('Ctrl Pts',(3.06075099962147,-55.0592467101081,
-95.3814216329573));
#175566=CARTESIAN_POINT('Ctrl Pts',(2.28937244057036,-54.58000002,-97.638711952094));
#175567=CARTESIAN_POINT('Ctrl Pts',(2.17279343333145,-54.5800000200112,
-96.5297363078781));
#175568=CARTESIAN_POINT('Ctrl Pts',(2.0669285329079,-55.052711592208,-95.5256220795631));
#175569=CARTESIAN_POINT('Ctrl Pts',(1.21149627184771,-54.58000002,-97.6987697451473));
#175570=CARTESIAN_POINT('Ctrl Pts',(1.14972373305894,-54.5800000199999,
-96.5901184946094));
#175571=CARTESIAN_POINT('Ctrl Pts',(1.09375770007614,-55.0499908864773,
-95.5856784364438));
#175572=CARTESIAN_POINT('',(1.23668893160606,-55.0504165218159,-95.5762821576559));
#175573=CARTESIAN_POINT('Ctrl Pts',(1.23668893165476,-55.0504165218147,
-95.5762821576554));
#175574=CARTESIAN_POINT('Ctrl Pts',(1.71088764457684,-55.0519150062272,
-95.543198672456));
#175575=CARTESIAN_POINT('Ctrl Pts',(2.18480270652532,-55.0542599488238,
-95.4911648085245));
#175576=CARTESIAN_POINT('Ctrl Pts',(2.8961822350534,-55.0590678993593,-95.3846884445288));
#175577=CARTESIAN_POINT('Ctrl Pts',(3.25199862731268,-55.0617933172342,
-95.3243438705064));
#175578=CARTESIAN_POINT('Ctrl Pts',(3.6675418607141,-55.0655275836122,-95.2415056814372));
#175579=CARTESIAN_POINT('Ctrl Pts',(3.8754446803529,-55.0675314608682,-95.1969775403918));
#175580=CARTESIAN_POINT('Ctrl Pts',(3.96457669660492,-55.0684193417625,
-95.1772278271201));
#175581=CARTESIAN_POINT('Ctrl Pts',(4.0240051857539,-55.0690176961945,-95.1639133017718));
#175582=CARTESIAN_POINT('Ctrl Pts',(4.0549182561813,-55.069332380045,-95.1569083381592));
#175583=CARTESIAN_POINT('Ctrl Pts',(4.996285678452,-55.0790115168945,-94.941364334101));
#175584=CARTESIAN_POINT('Ctrl Pts',(5.90958570151961,-55.0914523430888,
-94.6631990870593));
#175585=CARTESIAN_POINT('Ctrl Pts',(6.82752390105444,-55.106794611208,-94.3158809605474));
#175586=CARTESIAN_POINT('Origin',(1.23481659430174,-62.0604750000681,-98.242868717055));
#175587=CARTESIAN_POINT('Ctrl Pts',(1.23668893165476,-55.0504165218147,
-95.5762821576554));
#175588=CARTESIAN_POINT('Ctrl Pts',(0.749999999999967,-55.0621625368995,
-95.5817617789931));
#175589=CARTESIAN_POINT('Ctrl Pts',(0.749999999999973,-55.5033748716332,
-95.7875912885257));
#175590=CARTESIAN_POINT('Ctrl Pts',(1.24124884403065,-54.7408920390033,
-96.2394858776278));
#175591=CARTESIAN_POINT('Ctrl Pts',(0.750000000004129,-54.7481304442385,
-96.2443585547261));
#175592=CARTESIAN_POINT('Ctrl Pts',(0.749999999999973,-55.2248025687359,
-96.3847337445855));
#175593=CARTESIAN_POINT('Ctrl Pts',(1.24576233955167,-54.58000002,-96.9572624945429));
#175594=CARTESIAN_POINT('Ctrl Pts',(0.750000000006829,-54.5842199033567,
-96.9603643458105));
#175595=CARTESIAN_POINT('Ctrl Pts',(0.749999999999973,-55.0800000216326,
-97.0309759697293));
#175596=CARTESIAN_POINT('Ctrl Pts',(1.25,-54.58000002,-97.6965903014517));
#175597=CARTESIAN_POINT('Ctrl Pts',(0.749999999999965,-54.5800000199999,
-97.6965903014516));
#175598=CARTESIAN_POINT('Ctrl Pts',(0.749999999999973,-55.08000002,-97.6965903014517));
#175599=CARTESIAN_POINT('',(0.749999999999973,-55.08000002,-97.6965903014517));
#175600=CARTESIAN_POINT('Origin',(1.24999999999997,-55.08000002,-97.6965903014517));
#175601=CARTESIAN_POINT('',(0.749999999999973,-55.5033748716332,-95.7875912885257));
#175602=CARTESIAN_POINT('Origin',(1.24999999999997,-55.5033748716332,-95.7875912885257));
#175603=CARTESIAN_POINT('Origin',(0.749999999999973,-61.7707294447932,-98.1780034241954));
#175604=CARTESIAN_POINT('Origin',(1.24999999999997,-55.08000002,-55.24995));
#175605=CARTESIAN_POINT('',(0.749999999999973,-55.08000002,-134.362052670054));
#175606=CARTESIAN_POINT('Origin',(1.24999999999997,-55.08000002,-134.362052670054));
#175607=CARTESIAN_POINT('',(0.749999999999973,-55.08000002,-97.7195882395211));
#175608=CARTESIAN_POINT('Ctrl Pts',(1.24999999999997,-54.58000002,-134.362052670054));
#175609=CARTESIAN_POINT('Ctrl Pts',(0.749999999999966,-54.5800000199999,
-134.362052670054));
#175610=CARTESIAN_POINT('Ctrl Pts',(0.749999999999973,-55.08000002,-134.362052670054));
#175611=CARTESIAN_POINT('Ctrl Pts',(1.24580493030994,-54.58000002,-135.093949837831));
#175612=CARTESIAN_POINT('Ctrl Pts',(0.750000000006796,-54.5841777042435,
-135.09091556402));
#175613=CARTESIAN_POINT('Ctrl Pts',(0.749999999999973,-55.0800000255278,
-135.020977206459));
#175614=CARTESIAN_POINT('Ctrl Pts',(1.24129514745974,-54.7377489917927,
-135.812422632741));
#175615=CARTESIAN_POINT('Ctrl Pts',(0.749999999993926,-54.7449249516581,
-135.807520949259));
#175616=CARTESIAN_POINT('Ctrl Pts',(0.749999999999973,-55.2219738253108,
-135.667845593964));
#175617=CARTESIAN_POINT('Ctrl Pts',(1.23668893165479,-55.0504165218146,
-136.482360813851));
#175618=CARTESIAN_POINT('Ctrl Pts',(0.74999999999998,-55.0621625368994,
-136.476881192513));
#175619=CARTESIAN_POINT('Ctrl Pts',(0.749999999999973,-55.5033748716332,
-136.27105168298));
#175620=CARTESIAN_POINT('',(0.749999999999973,-55.5033748716332,-136.27105168298));
#175621=CARTESIAN_POINT('Origin',(1.24999999999997,-55.5033748716332,-136.27105168298));
#175622=CARTESIAN_POINT('Origin',(0.749999999999973,-61.7710312681108,-133.877753475455));
#175623=CARTESIAN_POINT('Ctrl Pts',(0.749999999999965,-71.813687061541,
-171.237717270032));
#175624=CARTESIAN_POINT('Ctrl Pts',(0.749999999999976,-71.3691907154172,
-171.445036077089));
#175625=CARTESIAN_POINT('Ctrl Pts',(1.24037635835043,-71.360635368318,-171.449026400902));
#175626=CARTESIAN_POINT('Ctrl Pts',(0.749999999999967,-66.3773023734559,
-159.58198200727));
#175627=CARTESIAN_POINT('Ctrl Pts',(0.749999999778459,-65.9383759687714,
-159.799181671811));
#175628=CARTESIAN_POINT('Ctrl Pts',(1.23948769887611,-65.9242696435089,
-159.793291324051));
#175629=CARTESIAN_POINT('Ctrl Pts',(0.74999999999997,-60.9406796476674,
-147.926357767621));
#175630=CARTESIAN_POINT('Ctrl Pts',(0.749999999843541,-60.5069208340151,
-148.152089356292));
#175631=CARTESIAN_POINT('Ctrl Pts',(1.23838899982829,-60.4876714538986,
-148.137667147083));
#175632=CARTESIAN_POINT('Ctrl Pts',(0.749999999999973,-55.5033748716332,
-136.27105168298));
#175633=CARTESIAN_POINT('Ctrl Pts',(0.749999999999973,-55.0621625368995,
-136.476881192513));
#175634=CARTESIAN_POINT('Ctrl Pts',(1.23668893165476,-55.0504165218146,
-136.482360813851));
#175635=CARTESIAN_POINT('',(0.749999999999965,-71.813687061541,-171.237717270032));
#175636=CARTESIAN_POINT('',(1.24037635835043,-71.360635368318,-171.449026400902));
#175637=CARTESIAN_POINT('Origin',(1.24999999999996,-71.813687061541,-171.237717270032));
#175638=CARTESIAN_POINT('Ctrl Pts',(1.23668893165476,-55.0504165218146,
-136.482360813851));
#175639=CARTESIAN_POINT('Ctrl Pts',(1.23673299366641,-55.1913381585796,
-136.784440607054));
#175640=CARTESIAN_POINT('Ctrl Pts',(1.23677661819369,-55.3322593149882,
-137.08652062441));
#175641=CARTESIAN_POINT('Ctrl Pts',(1.23699261729668,-56.0368627647092,
-138.596921799561));
#175642=CARTESIAN_POINT('Ctrl Pts',(1.23715863033152,-56.6005380707885,
-139.805246217854));
#175643=CARTESIAN_POINT('Ctrl Pts',(1.23731859936897,-57.1642067307399,
-141.01357373723));
#175644=CARTESIAN_POINT('Ctrl Pts',(1.23795847551899,-59.4188813711729,
-145.84688381608));
#175645=CARTESIAN_POINT('Ctrl Pts',(1.23850317159002,-61.6734513223852,
-150.68024274455));
#175646=CARTESIAN_POINT('Ctrl Pts',(1.23898586311735,-63.927952799307,-155.513633616344));
#175647=CARTESIAN_POINT('Ctrl Pts',(1.23951632777425,-66.4055876545563,
-160.825396689281));
#175648=CARTESIAN_POINT('Ctrl Pts',(1.23997137264739,-68.8831392394364,
-166.137198611174));
#175649=CARTESIAN_POINT('Ctrl Pts',(1.24037635835043,-71.360635368318,-171.449026400902));
#175650=CARTESIAN_POINT('Ctrl Pts',(0.749999999999965,-71.813687061541,
-171.237717270032));
#175651=CARTESIAN_POINT('Ctrl Pts',(0.749999999999967,-66.3773023734559,
-159.58198200727));
#175652=CARTESIAN_POINT('Ctrl Pts',(0.74999999999997,-60.9406796476674,
-147.926357767621));
#175653=CARTESIAN_POINT('Ctrl Pts',(0.749999999999973,-55.5033748716332,
-136.27105168298));
#175654=CARTESIAN_POINT('Ctrl Pts',(0.749999999999971,-55.5033748716332,
-95.7875912885257));
#175655=CARTESIAN_POINT('Ctrl Pts',(0.749999999999964,-55.0621625368994,
-95.581761778993));
#175656=CARTESIAN_POINT('Ctrl Pts',(1.23668893165476,-55.0504165218147,
-95.5762821576554));
#175657=CARTESIAN_POINT('Ctrl Pts',(0.749999999999969,-60.9031648374056,
-84.2127012585751));
#175658=CARTESIAN_POINT('Ctrl Pts',(0.750000000106769,-60.4692939396047,
-83.9872370540609));
#175659=CARTESIAN_POINT('Ctrl Pts',(1.23837727019305,-60.4501569855996,
-84.0013918846235));
#175660=CARTESIAN_POINT('Ctrl Pts',(0.749999999999967,-66.3022815738571,
-72.6374971882577));
#175661=CARTESIAN_POINT('Ctrl Pts',(0.749999999981978,-65.8633206076967,
-72.4204079747872));
#175662=CARTESIAN_POINT('Ctrl Pts',(1.23947201783252,-65.8492492116834,
-72.4261878753526));
#175663=CARTESIAN_POINT('Ctrl Pts',(0.749999999999965,-71.701161634982,
-61.062182729971));
#175664=CARTESIAN_POINT('Ctrl Pts',(0.749999999999965,-71.2566817467536,
-60.8548714197835));
#175665=CARTESIAN_POINT('Ctrl Pts',(1.24035792914739,-71.2481103336038,
-60.8508735991007));
#175666=CARTESIAN_POINT('',(1.24035792914739,-71.2481103336038,-60.8508735991007));
#175667=CARTESIAN_POINT('Ctrl Pts',(1.24035792914739,-71.2481103336038,
-60.8508735991007));
#175668=CARTESIAN_POINT('Ctrl Pts',(1.24033480878609,-71.1072117831156,
-61.1529641634137));
#175669=CARTESIAN_POINT('Ctrl Pts',(1.24031152212174,-70.9663130484708,
-61.4550546418214));
#175670=CARTESIAN_POINT('Ctrl Pts',(1.24019423907957,-70.2618184344542,
-62.9655065950025));
#175671=CARTESIAN_POINT('Ctrl Pts',(1.2400976958218,-69.6982197351968,-64.1738667543558));
#175672=CARTESIAN_POINT('Ctrl Pts',(1.23999818500278,-69.1346177525067,
-65.3822253820002));
#175673=CARTESIAN_POINT('Ctrl Pts',(1.23960014172664,-66.8802098214716,
-70.2156598931668));
#175674=CARTESIAN_POINT('Ctrl Pts',(1.23915545083688,-64.6257502610154,
-75.0490703206921));
#175675=CARTESIAN_POINT('Ctrl Pts',(1.23864216610312,-62.3712150282457,
-79.8824454429464));
#175676=CARTESIAN_POINT('Ctrl Pts',(1.23808662039688,-59.9310540692955,
-85.1137734354556));
#175677=CARTESIAN_POINT('Ctrl Pts',(1.23745196892516,-57.4908058054248,
-90.3450606997508));
#175678=CARTESIAN_POINT('Ctrl Pts',(1.23668893165476,-55.0504165218147,
-95.5762821576554));
#175679=CARTESIAN_POINT('',(0.749999999999965,-71.701161634982,-61.0621827299711));
#175680=CARTESIAN_POINT('Origin',(1.24999999999996,-71.701161634982,-61.0621827299711));
#175681=CARTESIAN_POINT('Ctrl Pts',(0.749999999999971,-55.5033748716332,
-95.7875912885257));
#175682=CARTESIAN_POINT('Ctrl Pts',(0.749999999999969,-60.9031648374056,
-84.2127012585751));
#175683=CARTESIAN_POINT('Ctrl Pts',(0.749999999999967,-66.3022815738571,
-72.6374971882577));
#175684=CARTESIAN_POINT('Ctrl Pts',(0.749999999999965,-71.701161634982,
-61.062182729971));
#175685=CARTESIAN_POINT('Origin',(41.5,-73.08000002,-177.34995));
#175686=CARTESIAN_POINT('',(24.2,-66.7760495265873,-177.34995));
#175687=CARTESIAN_POINT('',(24.2,-73.08000002,-177.34995));
#175688=CARTESIAN_POINT('',(24.7,-66.5483734731532,-177.34995));
#175689=CARTESIAN_POINT('Origin',(0.,-12.9675000200281,-177.34995));
#175690=CARTESIAN_POINT('',(24.7,-73.08000002,-177.34995));
#175691=CARTESIAN_POINT('Origin',(24.7,-73.08000002,-176.84995));
#175692=CARTESIAN_POINT('',(25.0407404589729,-66.228934721057,-177.2158679411));
#175693=CARTESIAN_POINT('Ctrl Pts',(24.7,-66.5483734731532,-177.34995));
#175694=CARTESIAN_POINT('Ctrl Pts',(24.7151484196587,-66.5344070727695,
-177.34995));
#175695=CARTESIAN_POINT('Ctrl Pts',(24.7294276217104,-66.5212071123009,
-177.349259041047));
#175696=CARTESIAN_POINT('Ctrl Pts',(24.7428260025297,-66.5087976049832,
-177.348101171356));
#175697=CARTESIAN_POINT('Ctrl Pts',(24.7495926258282,-66.5025303953502,
-177.347516409053));
#175698=CARTESIAN_POINT('Ctrl Pts',(24.7561350473995,-66.4964643177492,
-177.346811961198));
#175699=CARTESIAN_POINT('Ctrl Pts',(24.7624541748984,-66.4905999359657,
-177.346013195118));
#175700=CARTESIAN_POINT('Ctrl Pts',(24.7782079605574,-66.4759798458257,
-177.3440218459));
#175701=CARTESIAN_POINT('Ctrl Pts',(24.7925691181153,-66.4626181429203,
-177.341448439213));
#175702=CARTESIAN_POINT('Ctrl Pts',(24.805519745065,-66.4505491735357,-177.338647136582));
#175703=CARTESIAN_POINT('Ctrl Pts',(24.8080497717743,-66.4481913869192,
-177.338099875781));
#175704=CARTESIAN_POINT('Ctrl Pts',(24.8105259039867,-66.4458829797902,
-177.337543769072));
#175705=CARTESIAN_POINT('Ctrl Pts',(24.812948010595,-66.4436241853332,-177.336981231575));
#175706=CARTESIAN_POINT('Ctrl Pts',(24.8245684958003,-66.4327872190828,
-177.334282358356));
#175707=CARTESIAN_POINT('Ctrl Pts',(24.8349638344589,-66.4230751742553,
-177.3314348709));
#175708=CARTESIAN_POINT('Ctrl Pts',(24.8441561790726,-66.4144557330666,
-177.3286658351));
#175709=CARTESIAN_POINT('Ctrl Pts',(24.8466873935909,-66.4120822738902,
-177.327903350238));
#175710=CARTESIAN_POINT('Ctrl Pts',(24.8491274673187,-66.4097915816494,
-177.327146526476));
#175711=CARTESIAN_POINT('Ctrl Pts',(24.8514769953736,-66.407582837082,-177.326399450407));
#175712=CARTESIAN_POINT('Ctrl Pts',(24.8569180259311,-66.4024678325347,
-177.324669373718));
#175713=CARTESIAN_POINT('Ctrl Pts',(24.8618700924437,-66.3977843689127,
-177.322993320373));
#175714=CARTESIAN_POINT('Ctrl Pts',(24.8663521453577,-66.3935491356442,
-177.321412257989));
#175715=CARTESIAN_POINT('Ctrl Pts',(24.8685931718147,-66.39143151901,-177.320621726797));
#175716=CARTESIAN_POINT('Ctrl Pts',(24.8707166368713,-66.3894259510714,
-177.319854809349));
#175717=CARTESIAN_POINT('Ctrl Pts',(24.8727240319675,-66.3875324318892,
-177.319116074401));
#175718=CARTESIAN_POINT('Ctrl Pts',(24.8737277295157,-66.3865856722982,
-177.318746706927));
#175719=CARTESIAN_POINT('Ctrl Pts',(24.8747024069947,-66.3856669248983,
-177.318384377616));
#175720=CARTESIAN_POINT('Ctrl Pts',(24.8756482370288,-66.3847761897005,
-177.318029612383));
#175721=CARTESIAN_POINT('Ctrl Pts',(24.8761211520459,-66.3843308221016,
-177.317852229766));
#175722=CARTESIAN_POINT('Ctrl Pts',(24.8762952359649,-66.3841660105406,
-177.317786544152));
#175723=CARTESIAN_POINT('Ctrl Pts',(24.8766081401647,-66.3838714254534,
-177.317668448636));
#175724=CARTESIAN_POINT('Ctrl Pts',(24.8769210443645,-66.3835768403661,
-177.31755035312));
#175725=CARTESIAN_POINT('Ctrl Pts',(24.8773729678627,-66.3831524816923,
-177.31738036387));
#175726=CARTESIAN_POINT('Ctrl Pts',(24.8783993497236,-66.3821880207246,
-177.316988504263));
#175727=CARTESIAN_POINT('Ctrl Pts',(24.8948214594981,-66.3667566452422,
-177.310718750545));
#175728=CARTESIAN_POINT('Ctrl Pts',(24.9105266151752,-66.351990337037,-177.303734637161));
#175729=CARTESIAN_POINT('Ctrl Pts',(24.9255112984692,-66.3378890967839,
-177.296168963569));
#175730=CARTESIAN_POINT('Ctrl Pts',(24.9431116330293,-66.3213264146572,
-177.287282663888));
#175731=CARTESIAN_POINT('Ctrl Pts',(24.959731749144,-66.3056662947302,-177.277584719044));
#175732=CARTESIAN_POINT('Ctrl Pts',(24.9753358287529,-66.2909341784927,
-177.267297394451));
#175733=CARTESIAN_POINT('Ctrl Pts',(24.9914404771145,-66.2757294655218,
-177.256680059157));
#175734=CARTESIAN_POINT('Ctrl Pts',(25.0064629606483,-66.2615131607872,
-177.245435170344));
#175735=CARTESIAN_POINT('Ctrl Pts',(25.0204053672138,-66.2482764016167,
-177.233798655926));
#175736=CARTESIAN_POINT('Ctrl Pts',(25.0274581624319,-66.241580559594,-177.227912301023));
#175737=CARTESIAN_POINT('Ctrl Pts',(25.0342352192367,-66.2351348025665,
-177.221925578959));
#175738=CARTESIAN_POINT('Ctrl Pts',(25.0407404589728,-66.228934721057,-177.2158679411));
#175739=CARTESIAN_POINT('',(25.2,-66.1031295107182,-176.84995));
#175740=CARTESIAN_POINT('Ctrl Pts',(25.0407404589729,-66.228934721057,-177.2158679411));
#175741=CARTESIAN_POINT('Ctrl Pts',(25.0847395070529,-66.1869996509441,
-177.174896307427));
#175742=CARTESIAN_POINT('Ctrl Pts',(25.1244954390544,-66.1555483483594,
-177.12286866857));
#175743=CARTESIAN_POINT('Ctrl Pts',(25.1822082377855,-66.1136132782465,
-176.998799564474));
#175744=CARTESIAN_POINT('Ctrl Pts',(25.2,-66.1031295107183,-176.926663869319));
#175745=CARTESIAN_POINT('Ctrl Pts',(25.2,-66.1031295107182,-176.84995));
#175746=CARTESIAN_POINT('',(25.2,67.7009572055632,-176.84995));
#175747=CARTESIAN_POINT('Ctrl Pts',(26.2379083085631,-65.1635541261514,
-171.346593949865));
#175748=CARTESIAN_POINT('Ctrl Pts',(26.188244627337,-65.494631983645,-171.628250848894));
#175749=CARTESIAN_POINT('Ctrl Pts',(26.0510006858591,-65.5133697788369,
-172.043246117731));
#175750=CARTESIAN_POINT('Ctrl Pts',(25.9971706168399,-65.2375572433357,
-171.303343061545));
#175751=CARTESIAN_POINT('Ctrl Pts',(25.9737737091347,-65.5150103099346,
-171.582081143282));
#175752=CARTESIAN_POINT('Ctrl Pts',(25.8585042848855,-65.5396766827938,
-171.956814849412));
#175753=CARTESIAN_POINT('Ctrl Pts',(25.7542731404381,-65.3249121430513,
-171.265064732433));
#175754=CARTESIAN_POINT('Ctrl Pts',(25.7517856586292,-65.5594176286463,
-171.534269559735));
#175755=CARTESIAN_POINT('Ctrl Pts',(25.6686777183217,-65.5842439051372,
-171.880177321686));
#175756=CARTESIAN_POINT('Ctrl Pts',(25.5048932192108,-65.4282717079069,
-171.24324485235));
#175757=CARTESIAN_POINT('Ctrl Pts',(25.5297574101185,-65.6321545000982,
-171.506780891573));
#175758=CARTESIAN_POINT('Ctrl Pts',(25.4789337502923,-65.6496774707413,
-171.836549850108));
#175759=CARTESIAN_POINT('Ctrl Pts',(26.0394480946395,-65.5149709682656,
-172.038055421481));
#175760=CARTESIAN_POINT('Ctrl Pts',(25.9934781597493,-65.5214316212864,
-172.017499691038));
#175761=CARTESIAN_POINT('Ctrl Pts',(25.9500895256781,-65.5286146559866,
-171.9986631729));
#175762=CARTESIAN_POINT('Ctrl Pts',(25.8888633443777,-65.5399834876779,
-171.97298721415));
#175763=CARTESIAN_POINT('Ctrl Pts',(25.8592138997392,-65.5458173722782,
-171.960793939389));
#175764=CARTESIAN_POINT('Ctrl Pts',(25.8310028817436,-65.5517918933206,
-171.94956772155));
#175765=CARTESIAN_POINT('Ctrl Pts',(25.8125141728673,-65.5557974424197,
-171.942298477862));
#175766=CARTESIAN_POINT('Ctrl Pts',(25.8054251757784,-65.557359537272,-171.93953600361));
#175767=CARTESIAN_POINT('Ctrl Pts',(25.7071248585263,-65.5796157721532,
-171.901876249447));
#175768=CARTESIAN_POINT('Ctrl Pts',(25.6251638390528,-65.6022780898996,
-171.874763931484));
#175769=CARTESIAN_POINT('Ctrl Pts',(25.5486065204936,-65.6266003779646,
-171.854014632593));
#175770=CARTESIAN_POINT('Ctrl Pts',(25.54864668864,-65.6265809455192,-176.826359947228));
#175771=CARTESIAN_POINT('Ctrl Pts',(25.1997818129229,-65.7371542671639,
-176.835443989308));
#175772=CARTESIAN_POINT('Ctrl Pts',(25.1998556150807,-66.1032295031672,
-176.838160112216));
#175773=CARTESIAN_POINT('Ctrl Pts',(25.5529523483652,-65.6253023760353,
-176.972546990942));
#175774=CARTESIAN_POINT('Ctrl Pts',(25.2023635504854,-65.7357920520888,
-176.925322463907));
#175775=CARTESIAN_POINT('Ctrl Pts',(25.2016488868717,-66.1021639228633,
-176.911221791747));
#175776=CARTESIAN_POINT('Ctrl Pts',(25.5170441055793,-65.6358444287873,
-177.121198634883));
#175777=CARTESIAN_POINT('Ctrl Pts',(25.1809363031095,-65.747065159673,-177.017221417402));
#175778=CARTESIAN_POINT('Ctrl Pts',(25.1866937732675,-66.1109497354307,
-176.985515400943));
#175779=CARTESIAN_POINT('Ctrl Pts',(25.3765977400936,-65.6860676120866,
-177.38644456451));
#175780=CARTESIAN_POINT('Ctrl Pts',(25.0919963386827,-65.7962596108139,
-177.18144271446));
#175781=CARTESIAN_POINT('Ctrl Pts',(25.1281992647199,-66.1528013266155,
-177.118080932736));
#175782=CARTESIAN_POINT('Ctrl Pts',(25.2719907766206,-65.7262135374441,
-177.504397480335));
#175783=CARTESIAN_POINT('Ctrl Pts',(25.0235400714211,-65.8346526306424,
-177.25498331877));
#175784=CARTESIAN_POINT('Ctrl Pts',(25.0846190279164,-66.1862656195983,
-177.177043188278));
#175785=CARTESIAN_POINT('Ctrl Pts',(25.1465824121021,-65.7870908289106,
-177.597292784559));
#175786=CARTESIAN_POINT('Ctrl Pts',(24.9378206840703,-65.8881436940036,
-177.307601476654));
#175787=CARTESIAN_POINT('Ctrl Pts',(25.0323995999485,-66.2369758560726,
-177.223456543475));
#175788=CARTESIAN_POINT('',(25.166383622031,-65.7775666303703,-177.581785882201));
#175789=CARTESIAN_POINT('Origin',(25.3814809179458,-66.228934721057,-177.581785882201));
#175790=CARTESIAN_POINT('',(25.548606520496,-65.6266003779638,-176.84995));
#175791=CARTESIAN_POINT('Ctrl Pts',(25.548606520496,-65.6266003779638,-176.84995));
#175792=CARTESIAN_POINT('Ctrl Pts',(25.5483880050666,-65.6266698003955,
-176.923301524269));
#175793=CARTESIAN_POINT('Ctrl Pts',(25.5391662663674,-65.6295529063921,
-176.994603239542));
#175794=CARTESIAN_POINT('Ctrl Pts',(25.5119555175164,-65.6384880995831,
-177.098481098957));
#175795=CARTESIAN_POINT('Ctrl Pts',(25.5006581261773,-65.6422428632939,
-177.132594599846));
#175796=CARTESIAN_POINT('Ctrl Pts',(25.4804126501714,-65.6491589363909,
-177.182996172806));
#175797=CARTESIAN_POINT('Ctrl Pts',(25.4731144514682,-65.6516787676171,
-177.199668584064));
#175798=CARTESIAN_POINT('Ctrl Pts',(25.4574280034951,-65.6571730351468,
-177.232757180455));
#175799=CARTESIAN_POINT('Ctrl Pts',(25.4484827026432,-65.6603481655915,
-177.250189665967));
#175800=CARTESIAN_POINT('Ctrl Pts',(25.3731469612502,-65.6874900466836,
-177.387635611196));
#175801=CARTESIAN_POINT('Ctrl Pts',(25.2806998533548,-65.7230897793383,
-177.49307709271));
#175802=CARTESIAN_POINT('Ctrl Pts',(25.166383622031,-65.7775666303703,-177.581785882201));
#175803=CARTESIAN_POINT('Origin',(25.7,-66.1031295107182,-176.84995));
#175804=CARTESIAN_POINT('Origin',(25.7,-66.1031295107182,-179.64995));
#175805=CARTESIAN_POINT('',(25.548606520496,-65.6266003779638,-179.64995));
#175806=CARTESIAN_POINT('',(25.2,-66.1031295107182,-171.799329694116));
#175807=CARTESIAN_POINT('Ctrl Pts',(0.749999999999965,-71.9542570083556,
-171.871644662643));
#175808=CARTESIAN_POINT('Ctrl Pts',(0.749999999999965,-71.4647403528508,
-171.871644662643));
#175809=CARTESIAN_POINT('Ctrl Pts',(1.23940677966098,-71.4543692372681,
-171.871644662643));
#175810=CARTESIAN_POINT('Ctrl Pts',(0.749999999999965,-71.9542569918424,
-171.652832243085));
#175811=CARTESIAN_POINT('Ctrl Pts',(0.75,-71.4647403416089,-171.724250912112));
#175812=CARTESIAN_POINT('Ctrl Pts',(1.23940678000784,-71.4543692372607,
-171.725769781663));
#175813=CARTESIAN_POINT('Ctrl Pts',(0.749999999999965,-71.9071171402653,
-171.43803354201));
#175814=CARTESIAN_POINT('Ctrl Pts',(0.749999999994888,-71.4326041940841,
-171.579497326419));
#175815=CARTESIAN_POINT('Ctrl Pts',(1.23973038817724,-71.4229357713421,
-171.582570495172));
#175816=CARTESIAN_POINT('Ctrl Pts',(0.749999999999965,-71.813687061541,
-171.237717270032));
#175817=CARTESIAN_POINT('Ctrl Pts',(0.749999999999965,-71.3691907154173,
-171.445036077089));
#175818=CARTESIAN_POINT('Ctrl Pts',(1.24037635835043,-71.360635368318,-171.449026400902));
#175819=CARTESIAN_POINT('',(0.749999999999965,-71.9542570083556,-171.871644662643));
#175820=CARTESIAN_POINT('',(1.23940677966098,-71.4543692372681,-171.871644662643));
#175821=CARTESIAN_POINT('Origin',(1.24999999999996,-71.9542570083556,-171.871644662643));
#175822=CARTESIAN_POINT('Origin',(1.25479963396822,-69.9697011186647,-171.979266830671));
#175823=CARTESIAN_POINT('Origin',(0.749999999999965,-69.7273331732481,-172.033160909053));
#175824=CARTESIAN_POINT('Origin',(0.,-12.9675000200281,-171.64995));
#175825=CARTESIAN_POINT('Origin',(0.,-12.9675000200281,-171.449026400902));
#175826=CARTESIAN_POINT('Ctrl Pts',(7.4,-71.4211246238516,-171.237717270032));
#175827=CARTESIAN_POINT('Ctrl Pts',(7.39999999999995,-70.9175980522952,
-171.474145745141));
#175828=CARTESIAN_POINT('Ctrl Pts',(6.84687749809456,-70.9710952348089,
-171.449026400902));
#175829=CARTESIAN_POINT('Ctrl Pts',(7.4,-71.5141496698322,-171.435834655863));
#175830=CARTESIAN_POINT('Ctrl Pts',(7.40000000000424,-70.9726288200743,
-171.600718024433));
#175831=CARTESIAN_POINT('Ctrl Pts',(6.84335093752903,-71.0335272731666,
-171.581102626116));
#175832=CARTESIAN_POINT('Ctrl Pts',(7.4,-71.5626363329153,-171.650517772678));
#175833=CARTESIAN_POINT('Ctrl Pts',(7.39999999999997,-71.0003029730699,
-171.734045906264));
#175834=CARTESIAN_POINT('Ctrl Pts',(6.84152542419482,-71.0660673850682,
-171.724228262147));
#175835=CARTESIAN_POINT('Ctrl Pts',(7.4,-71.5626363369615,-171.871644662643));
#175836=CARTESIAN_POINT('Ctrl Pts',(7.39999999999996,-71.0003029749948,
-171.871644662643));
#175837=CARTESIAN_POINT('Ctrl Pts',(6.84152542372878,-71.066067385123,-171.871644662643));
#175838=CARTESIAN_POINT('',(6.84152542372877,-71.066067385123,-171.871644662643));
#175839=CARTESIAN_POINT('',(7.4,-71.5626363369615,-171.871644662643));
#175840=CARTESIAN_POINT('Origin',(6.9,-71.5626363369615,-171.871644662643));
#175841=CARTESIAN_POINT('Origin',(7.4,-69.3873379576789,-172.017654079519));
#175842=CARTESIAN_POINT('Origin',(6.92387916107346,-69.6079656440742,-171.968783295101));
#175843=CARTESIAN_POINT('Ctrl Pts',(7.4,-72.58000002,-174.471034982976));
#175844=CARTESIAN_POINT('Ctrl Pts',(7.39999999999995,-73.0800000199999,
-174.471034982977));
#175845=CARTESIAN_POINT('Ctrl Pts',(7.9,-73.08000002,-174.471034982976));
#175846=CARTESIAN_POINT('Ctrl Pts',(7.4,-72.5800000132661,-174.719615315523));
#175847=CARTESIAN_POINT('Ctrl Pts',(7.39999999999984,-73.081997137201,-174.769844466954));
#175848=CARTESIAN_POINT('Ctrl Pts',(7.90199316078775,-73.08000002,-174.769251346187));
#175849=CARTESIAN_POINT('Ctrl Pts',(7.4,-72.5437711321103,-174.962127460747));
#175850=CARTESIAN_POINT('Ctrl Pts',(7.39999999999996,-73.040326257465,-175.061328113453));
#175851=CARTESIAN_POINT('Ctrl Pts',(7.90394076068631,-73.0365253516511,
-175.060187649793));
#175852=CARTESIAN_POINT('Ctrl Pts',(7.4,-72.4360935067573,-175.316738645421));
#175853=CARTESIAN_POINT('Ctrl Pts',(7.39999999999996,-72.9137734508192,
-175.488022550208));
#175854=CARTESIAN_POINT('Ctrl Pts',(7.90679252703161,-72.9073122055494,
-175.485606387024));
#175855=CARTESIAN_POINT('Ctrl Pts',(7.4,-72.3910774582401,-175.433049854657));
#175856=CARTESIAN_POINT('Ctrl Pts',(7.39999999999998,-72.8605108035235,
-175.628237972001));
#175857=CARTESIAN_POINT('Ctrl Pts',(7.90772857701081,-72.8532929465542,
-175.625142180141));
#175858=CARTESIAN_POINT('Ctrl Pts',(7.4,-72.2858284501893,-175.654944429739));
#175859=CARTESIAN_POINT('Ctrl Pts',(7.39999999999997,-72.7355139213092,
-175.896009980972));
#175860=CARTESIAN_POINT('Ctrl Pts',(7.90951546143904,-72.7269941355612,
-175.891343758978));
#175861=CARTESIAN_POINT('Ctrl Pts',(7.4,-72.2253270246874,-175.761526340889));
#175862=CARTESIAN_POINT('Ctrl Pts',(7.39999999999901,-72.6634371311262,
-176.024735407069));
#175863=CARTESIAN_POINT('Ctrl Pts',(7.9103743244834,-72.6543924247951,-176.019207476496));
#175864=CARTESIAN_POINT('Ctrl Pts',(7.4,-72.0884932351423,-175.96591668417));
#175865=CARTESIAN_POINT('Ctrl Pts',(7.40000000000093,-72.5000420015558,
-176.271831635453));
#175866=CARTESIAN_POINT('Ctrl Pts',(7.9120222658245,-72.4901918790006,-176.264409528534));
#175867=CARTESIAN_POINT('Ctrl Pts',(7.4,-72.0114432535103,-176.064396375895));
#175868=CARTESIAN_POINT('Ctrl Pts',(7.39999999999755,-72.4078441030974,
-176.390977561524));
#175869=CARTESIAN_POINT('Ctrl Pts',(7.91281676658892,-72.3977319011293,
-176.382553154925));
#175870=CARTESIAN_POINT('Ctrl Pts',(7.4,-71.8455797798041,-176.246702589259));
#175871=CARTESIAN_POINT('Ctrl Pts',(7.40000000000237,-72.2090331198025,
-176.611745838634));
#175872=CARTESIAN_POINT('Ctrl Pts',(7.91428825612723,-72.198695730848,-176.6012613201));
#175873=CARTESIAN_POINT('Ctrl Pts',(7.4,-71.7565932593015,-176.331051292497));
#175874=CARTESIAN_POINT('Ctrl Pts',(7.40000000000137,-72.1022117673413,
-176.713954380549));
#175875=CARTESIAN_POINT('Ctrl Pts',(7.91496944868021,-72.0919119068452,
-176.702452310058));
#175876=CARTESIAN_POINT('Ctrl Pts',(7.4,-71.4717169212771,-176.56396241752));
#175877=CARTESIAN_POINT('Ctrl Pts',(7.39999999999722,-71.7595719221786,
-176.996603847265));
#175878=CARTESIAN_POINT('Ctrl Pts',(7.91685114292327,-71.7500603021656,
-176.981869807169));
#175879=CARTESIAN_POINT('Ctrl Pts',(7.4,-71.2547332556153,-176.693097313134));
#175880=CARTESIAN_POINT('Ctrl Pts',(7.39999999999668,-71.4982684775377,
-177.153312936568));
#175881=CARTESIAN_POINT('Ctrl Pts',(7.91789548135802,-71.4896799957509,
-177.136789521634));
#175882=CARTESIAN_POINT('Ctrl Pts',(7.4,-71.028920068719,-176.785817298486));
#175883=CARTESIAN_POINT('Ctrl Pts',(7.39999999999996,-71.2260554869631,
-177.265927135801));
#175884=CARTESIAN_POINT('Ctrl Pts',(7.91864558019502,-71.2187040784628,
-177.248023282853));
#175885=CARTESIAN_POINT('',(7.40000000143918,-71.5626363369614,-176.485569595296));
#175886=CARTESIAN_POINT('Ctrl Pts',(7.40000000575672,-71.5626363369612,
-176.485569595296));
#175887=CARTESIAN_POINT('Ctrl Pts',(7.39999999964314,-71.5963334703268,
-176.460729295267));
#175888=CARTESIAN_POINT('Ctrl Pts',(7.40000000050213,-71.6293602055438,
-176.435105116127));
#175889=CARTESIAN_POINT('Ctrl Pts',(7.40000000080687,-71.6616524595397,
-176.408710325206));
#175890=CARTESIAN_POINT('Ctrl Pts',(7.40000000085713,-71.6669782225453,
-176.404357194544));
#175891=CARTESIAN_POINT('Ctrl Pts',(7.40000000093686,-71.6722864874059,
-176.399982537289));
#175892=CARTESIAN_POINT('Ctrl Pts',(7.40000000105475,-71.6775773354997,
-176.395586157876));
#175893=CARTESIAN_POINT('Ctrl Pts',(7.40000000288459,-71.759704119665,-176.327343695265));
#175894=CARTESIAN_POINT('Ctrl Pts',(7.40000000086288,-71.8372393620171,
-176.253983607117));
#175895=CARTESIAN_POINT('Ctrl Pts',(7.40000000055521,-71.9102228395816,
-176.175469994321));
#175896=CARTESIAN_POINT('Ctrl Pts',(7.40000000052935,-71.9163567428985,
-176.168871310263));
#175897=CARTESIAN_POINT('Ctrl Pts',(7.40000000051231,-71.9224585008204,
-176.162236193809));
#175898=CARTESIAN_POINT('Ctrl Pts',(7.40000000050508,-71.9285281400417,
-176.15556460665));
#175899=CARTESIAN_POINT('Ctrl Pts',(7.40000000048088,-71.9488281698803,
-176.133251349886));
#175900=CARTESIAN_POINT('Ctrl Pts',(7.4000000005302,-71.9687792955913,-176.110498872159));
#175901=CARTESIAN_POINT('Ctrl Pts',(7.40000000090086,-71.9883433756989,
-176.087359845977));
#175902=CARTESIAN_POINT('Ctrl Pts',(7.40000000204431,-72.0486965657351,
-176.01597831223));
#175903=CARTESIAN_POINT('Ctrl Pts',(7.40000000174205,-72.1052822109679,
-175.940916275219));
#175904=CARTESIAN_POINT('Ctrl Pts',(7.40000000104438,-72.1569369843104,
-175.863739490819));
#175905=CARTESIAN_POINT('Ctrl Pts',(7.40000000027758,-72.2137093550038,
-175.778916564894));
#175906=CARTESIAN_POINT('Ctrl Pts',(7.39999999999849,-72.2650200455803,
-175.691076839899));
#175907=CARTESIAN_POINT('Ctrl Pts',(7.40000000003311,-72.3109220293856,
-175.600232860702));
#175908=CARTESIAN_POINT('Ctrl Pts',(7.4000000000402,-72.3203292671906,-175.5816151269));
#175909=CARTESIAN_POINT('Ctrl Pts',(7.40000000005342,-72.3295088745487,
-175.562871130851));
#175910=CARTESIAN_POINT('Ctrl Pts',(7.40000000007737,-72.3384609015072,
-175.544000911756));
#175911=CARTESIAN_POINT('Ctrl Pts',(7.40000000021819,-72.3910932309574,
-175.433055804823));
#175912=CARTESIAN_POINT('Ctrl Pts',(7.4000000012263,-72.436127459958,-175.316747505601));
#175913=CARTESIAN_POINT('Ctrl Pts',(7.40000000110901,-72.4720179137164,
-175.198544593051));
#175914=CARTESIAN_POINT('Ctrl Pts',(7.40000000106034,-72.4869106518372,
-175.14949631315));
#175915=CARTESIAN_POINT('Ctrl Pts',(7.40000000071105,-72.5002693294562,
-175.100185099317));
#175916=CARTESIAN_POINT('Ctrl Pts',(7.4000000003472,-72.5120857612517,-175.050611983827));
#175917=CARTESIAN_POINT('Ctrl Pts',(7.39999999965227,-72.534654114155,-174.955931662031));
#175918=CARTESIAN_POINT('Ctrl Pts',(7.4,-72.5516373021817,-174.860293425931));
#175919=CARTESIAN_POINT('Ctrl Pts',(7.4,-72.5629735391251,-174.763699740561));
#175920=CARTESIAN_POINT('Ctrl Pts',(7.4,-72.5743097760684,-174.667106055192));
#175921=CARTESIAN_POINT('Ctrl Pts',(7.4,-72.58000002,-174.569557605373));
#175922=CARTESIAN_POINT('Ctrl Pts',(7.4,-72.58000002,-174.471034982976));
#175923=CARTESIAN_POINT('',(7.91859121655489,-71.2381488508947,-177.239961484012));
#175924=CARTESIAN_POINT('Ctrl Pts',(7.4,-71.5626363369615,-176.485569595297));
#175925=CARTESIAN_POINT('Ctrl Pts',(7.4,-71.5506036695784,-176.519632609605));
#175926=CARTESIAN_POINT('Ctrl Pts',(7.40124182377961,-71.5387437345536,
-176.553192135052));
#175927=CARTESIAN_POINT('Ctrl Pts',(7.40377535877835,-71.5271166640425,
-176.586019648744));
#175928=CARTESIAN_POINT('Ctrl Pts',(7.40622177366248,-71.5158894110653,
-176.617718329893));
#175929=CARTESIAN_POINT('Ctrl Pts',(7.40987259906279,-71.5048792758311,
-176.648734213767));
#175930=CARTESIAN_POINT('Ctrl Pts',(7.41473087025355,-71.494133681817,-176.678884073483));
#175931=CARTESIAN_POINT('Ctrl Pts',(7.41866902349833,-71.4854232178944,
-176.703323789425));
#175932=CARTESIAN_POINT('Ctrl Pts',(7.42339982845854,-71.4768864593179,
-176.727194803422));
#175933=CARTESIAN_POINT('Ctrl Pts',(7.42890359949814,-71.4685453034926,
-176.75041264347));
#175934=CARTESIAN_POINT('Ctrl Pts',(7.43039440453314,-71.4662859367761,
-176.756701653787));
#175935=CARTESIAN_POINT('Ctrl Pts',(7.43194146136298,-71.4640414204283,
-176.762941376912));
#175936=CARTESIAN_POINT('Ctrl Pts',(7.43354440994792,-71.4618116713854,
-176.769131638689));
#175937=CARTESIAN_POINT('Ctrl Pts',(7.4377989840509,-71.4558934325703,-176.785561939508));
#175938=CARTESIAN_POINT('Ctrl Pts',(7.44244689889008,-71.4500853619215,
-176.801621162751));
#175939=CARTESIAN_POINT('Ctrl Pts',(7.44746558592961,-71.4443873125637,
-176.817288504605));
#175940=CARTESIAN_POINT('Ctrl Pts',(7.45592268298431,-71.4347854075113,
-176.843689878032));
#175941=CARTESIAN_POINT('Ctrl Pts',(7.46543034530173,-71.4255017180002,
-176.868960780972));
#175942=CARTESIAN_POINT('Ctrl Pts',(7.47583467172322,-71.4165597639218,
-176.892953826141));
#175943=CARTESIAN_POINT('Ctrl Pts',(7.48331456949562,-71.4101311976041,
-176.91020295096));
#175944=CARTESIAN_POINT('Ctrl Pts',(7.49125715404826,-71.4038792424485,
-176.926792127842));
#175945=CARTESIAN_POINT('Ctrl Pts',(7.49959455240465,-71.3978116293706,
-176.942679207561));
#175946=CARTESIAN_POINT('Ctrl Pts',(7.50169522409967,-71.3962828475487,
-176.946682079591));
#175947=CARTESIAN_POINT('Ctrl Pts',(7.50382092027666,-71.3947657561162,
-176.950640434758));
#175948=CARTESIAN_POINT('Ctrl Pts',(7.50596959979478,-71.3932574848628,
-176.954554085486));
#175949=CARTESIAN_POINT('Ctrl Pts',(7.50734971529259,-71.39228870915,-176.957067857306));
#175950=CARTESIAN_POINT('Ctrl Pts',(7.50849831293203,-71.391492060449,-176.95913101286));
#175951=CARTESIAN_POINT('Ctrl Pts',(7.50987883023994,-71.3905463578264,
-176.96157741569));
#175952=CARTESIAN_POINT('Ctrl Pts',(7.5106476180218,-71.3900197113169,-176.962939777896));
#175953=CARTESIAN_POINT('Ctrl Pts',(7.51148881635629,-71.3894469329875,
-176.964420536038));
#175954=CARTESIAN_POINT('Ctrl Pts',(7.51248752482203,-71.3887735212086,
-176.966158828872));
#175955=CARTESIAN_POINT('Ctrl Pts',(7.52040526868911,-71.3834347239867,
-176.979939985129));
#175956=CARTESIAN_POINT('Ctrl Pts',(7.528724573393,-71.3781777648363,-176.993315121));
#175957=CARTESIAN_POINT('Ctrl Pts',(7.53742401159906,-71.3730105085842,
-177.006241431523));
#175958=CARTESIAN_POINT('Ctrl Pts',(7.55157063114754,-71.3646077581333,
-177.027261593147));
#175959=CARTESIAN_POINT('Ctrl Pts',(7.56677045080576,-71.3564218411025,
-177.047118964408));
#175960=CARTESIAN_POINT('Ctrl Pts',(7.58280101197635,-71.3485013029008,
-177.065623012365));
#175961=CARTESIAN_POINT('Ctrl Pts',(7.58472281489058,-71.3475517595108,
-177.067841346016));
#175962=CARTESIAN_POINT('Ctrl Pts',(7.58665653135238,-71.3466060208685,
-177.070040284832));
#175963=CARTESIAN_POINT('Ctrl Pts',(7.5886017583046,-71.3456641628206,-177.072219547107));
#175964=CARTESIAN_POINT('Ctrl Pts',(7.60267640683548,-71.338849368806,-177.087987553275));
#175965=CARTESIAN_POINT('Ctrl Pts',(7.61736717206938,-71.3322314016754,
-177.102738989088));
#175966=CARTESIAN_POINT('Ctrl Pts',(7.63254357701316,-71.3258225700846,
-177.11639818297));
#175967=CARTESIAN_POINT('Ctrl Pts',(7.64013177948506,-71.3226181542892,
-177.12322777991));
#175968=CARTESIAN_POINT('Ctrl Pts',(7.64784173532136,-71.3194674390364,
-177.129784166108));
#175969=CARTESIAN_POINT('Ctrl Pts',(7.6556568499062,-71.3163736401622,-177.13605865242));
#175970=CARTESIAN_POINT('Ctrl Pts',(7.65935939288764,-71.3149079005133,
-177.139031296646));
#175971=CARTESIAN_POINT('Ctrl Pts',(7.6628170835859,-71.3135596068012,-177.141730715413));
#175972=CARTESIAN_POINT('Ctrl Pts',(7.66640603380969,-71.3121789599471,
-177.144461325117));
#175973=CARTESIAN_POINT('Ctrl Pts',(7.66983434317808,-71.3108601106321,
-177.147069713154));
#175974=CARTESIAN_POINT('Ctrl Pts',(7.67338251641711,-71.309511712934,-177.149706742547));
#175975=CARTESIAN_POINT('Ctrl Pts',(7.67739913373759,-71.308009866984,-177.152597143897));
#175976=CARTESIAN_POINT('Ctrl Pts',(7.67805299354838,-71.307765383472,-177.153067668503));
#175977=CARTESIAN_POINT('Ctrl Pts',(7.67871931450839,-71.3075168498756,
-177.153544807822));
#175978=CARTESIAN_POINT('Ctrl Pts',(7.67939965845519,-71.3072637521496,
-177.154029406282));
#175979=CARTESIAN_POINT('Ctrl Pts',(7.68837037659409,-71.3039265160767,
-177.160419109932));
#175980=CARTESIAN_POINT('Ctrl Pts',(7.69748767629138,-71.3006476354715,
-177.166472905463));
#175981=CARTESIAN_POINT('Ctrl Pts',(7.70673174046216,-71.297430665461,-177.172175429854));
#175982=CARTESIAN_POINT('Ctrl Pts',(7.72768672414405,-71.2901382502603,
-177.185102244658));
#175983=CARTESIAN_POINT('Ctrl Pts',(7.74939099709486,-71.2831283244239,
-177.196256748911));
#175984=CARTESIAN_POINT('Ctrl Pts',(7.77148013541325,-71.2764641353456,
-177.205563508786));
#175985=CARTESIAN_POINT('Ctrl Pts',(7.79294215838971,-71.2699891440147,
-177.214606047767));
#175986=CARTESIAN_POINT('Ctrl Pts',(7.81476661214664,-71.2638406432925,
-177.221904234036));
#175987=CARTESIAN_POINT('Ctrl Pts',(7.83662991855142,-71.2580661408856,
-177.227435014853));
#175988=CARTESIAN_POINT('Ctrl Pts',(7.85770145362575,-71.2525007598884,
-177.232765500545));
#175989=CARTESIAN_POINT('Ctrl Pts',(7.8788084897248,-71.247282821352,-177.236454389783));
#175990=CARTESIAN_POINT('Ctrl Pts',(7.89968194537098,-71.2424439309288,
-177.238523807616));
#175991=CARTESIAN_POINT('Ctrl Pts',(7.90600864332505,-71.24097727401,-177.239151043555));
#175992=CARTESIAN_POINT('Ctrl Pts',(7.91231406191567,-71.2395453591647,
-177.239629801061));
#175993=CARTESIAN_POINT('Ctrl Pts',(7.91859121655422,-71.2381488509314,
-177.239961484007));
#175994=CARTESIAN_POINT('Ctrl Pts',(7.9,-73.08000002,-174.471034982976));
#175995=CARTESIAN_POINT('Ctrl Pts',(7.90029399716905,-73.080000019775,-174.515022787248));
#175996=CARTESIAN_POINT('Ctrl Pts',(7.90085674855018,-73.0803883548312,
-174.607717845982));
#175997=CARTESIAN_POINT('Ctrl Pts',(7.90228899981587,-73.0600424381335,
-174.824207987439));
#175998=CARTESIAN_POINT('Ctrl Pts',(7.90286592665474,-73.0495149637409,
-174.909313799419));
#175999=CARTESIAN_POINT('Ctrl Pts',(7.9038762253622,-73.0228545180863,-175.056228893897));
#176000=CARTESIAN_POINT('Ctrl Pts',(7.9042367222111,-73.0121368256507,-175.108399370711));
#176001=CARTESIAN_POINT('Ctrl Pts',(7.90480656268785,-72.9924911650618,
-175.191284311026));
#176002=CARTESIAN_POINT('Ctrl Pts',(7.90509867676605,-72.9817743855232,
-175.233882088622));
#176003=CARTESIAN_POINT('Ctrl Pts',(7.90544965740232,-72.967510881305,-175.285539712882));
#176004=CARTESIAN_POINT('Ctrl Pts',(7.90562730551323,-72.959913400428,-175.311848730422));
#176005=CARTESIAN_POINT('Ctrl Pts',(7.90570385869998,-72.9565547804075,
-175.323225805126));
#176006=CARTESIAN_POINT('Ctrl Pts',(7.90575498195503,-72.9542926010636,
-175.330833008964));
#176007=CARTESIAN_POINT('Ctrl Pts',(7.90578862396314,-72.9527882461173,
-175.335846745901));
#176008=CARTESIAN_POINT('Ctrl Pts',(7.90693329510708,-72.9012674128257,
-175.506610298774));
#176009=CARTESIAN_POINT('Ctrl Pts',(7.90796841236697,-72.839623599414,-175.657481499327));
#176010=CARTESIAN_POINT('Ctrl Pts',(7.90929927756806,-72.7426206144854,
-175.855928107122));
#176011=CARTESIAN_POINT('Ctrl Pts',(7.9097081812878,-72.7095177001685,-175.917489253729));
#176012=CARTESIAN_POINT('Ctrl Pts',(7.91027517352814,-72.6599954134491,
-176.003103640448));
#176013=CARTESIAN_POINT('Ctrl Pts',(7.91054721380992,-72.6352646259782,
-176.044232319737));
#176014=CARTESIAN_POINT('Ctrl Pts',(7.91084698606837,-72.6067161650734,
-176.089341310574));
#176015=CARTESIAN_POINT('Ctrl Pts',(7.91099284326656,-72.5925469657504,
-176.111186720346));
#176016=CARTESIAN_POINT('Ctrl Pts',(7.91105453093491,-72.5865000065411,
-176.120398132595));
#176017=CARTESIAN_POINT('Ctrl Pts',(7.91109547794238,-72.5824747114477,
-176.126505658783));
#176018=CARTESIAN_POINT('Ctrl Pts',(7.91110782189276,-72.5812598872988,
-176.128346248943));
#176019=CARTESIAN_POINT('Ctrl Pts',(7.91294980900864,-72.3991760858112,
-176.402443010638));
#176020=CARTESIAN_POINT('Ctrl Pts',(7.91462251977688,-72.1818766937441,
-176.633078403434));
#176021=CARTESIAN_POINT('Ctrl Pts',(7.91709744842058,-71.7199235074033,
-177.001812138227));
#176022=CARTESIAN_POINT('Ctrl Pts',(7.9179199571433,-71.4758859239583,-177.140416596742));
#176023=CARTESIAN_POINT('Ctrl Pts',(7.91859121655449,-71.2381488509313,
-177.239961484006));
#176024=CARTESIAN_POINT('Ctrl Pts',(8.40355780430818,-73.08000002,-174.451130838212));
#176025=CARTESIAN_POINT('Ctrl Pts',(8.48384574056985,-73.0800000199999,
-176.520599502442));
#176026=CARTESIAN_POINT('Ctrl Pts',(8.51230691249381,-71.1434663357064,
-177.254202907715));
#176027=CARTESIAN_POINT('Ctrl Pts',(8.20353011255175,-73.08000002,-174.458891192924));
#176028=CARTESIAN_POINT('Ctrl Pts',(8.28507376820399,-73.0800000200062,
-176.507651386999));
#176029=CARTESIAN_POINT('Ctrl Pts',(8.31384446654333,-71.1696907801609,
-177.251953160255));
#176030=CARTESIAN_POINT('Ctrl Pts',(8.00350691066062,-73.08000002,-174.46684979476));
#176031=CARTESIAN_POINT('Ctrl Pts',(8.08524840860192,-73.0800000200062,
-176.495676023668));
#176032=CARTESIAN_POINT('Ctrl Pts',(8.11484675268685,-71.1950080123696,
-177.249844108498));
#176033=CARTESIAN_POINT('Ctrl Pts',(7.80348623696872,-73.08000002,-174.474919939778));
#176034=CARTESIAN_POINT('Ctrl Pts',(7.88456937757999,-73.0800000199999,
-176.484587012089));
#176035=CARTESIAN_POINT('Ctrl Pts',(7.91536503462485,-71.2194103886423,
-177.247865511993));
#176036=CARTESIAN_POINT('',(8.41817820009134,-71.1781942230057,-177.244433726518));
#176037=CARTESIAN_POINT('Origin',(0.060185797981942,-4.47315859110275,-188.387285563199));
#176038=CARTESIAN_POINT('Ctrl Pts',(8.4181782717274,-71.1781985203566,-177.244444626904));
#176039=CARTESIAN_POINT('Ctrl Pts',(8.41754848274224,-71.4223190079251,
-177.148366085912));
#176040=CARTESIAN_POINT('Ctrl Pts',(8.41677076479328,-71.673624968976,-177.012030245796));
#176041=CARTESIAN_POINT('Ctrl Pts',(8.41497352559848,-72.0310711490723,
-176.73626320784));
#176042=CARTESIAN_POINT('Ctrl Pts',(8.41427511117919,-72.1468008645235,
-176.632607910667));
#176043=CARTESIAN_POINT('Ctrl Pts',(8.4131024423523,-72.3104942873253,-176.460057862085));
#176044=CARTESIAN_POINT('Ctrl Pts',(8.41269135999703,-72.3634047131022,
-176.399713077921));
#176045=CARTESIAN_POINT('Ctrl Pts',(8.4120536281718,-72.4396864660478,-176.305177352398));
#176046=CARTESIAN_POINT('Ctrl Pts',(8.41172955234536,-72.4770565412457,
-176.256906560854));
#176047=CARTESIAN_POINT('Ctrl Pts',(8.41134506529128,-72.5191777814738,
-176.198902525325));
#176048=CARTESIAN_POINT('Ctrl Pts',(8.41115161467346,-72.5398534996524,
-176.169488201525));
#176049=CARTESIAN_POINT('Ctrl Pts',(8.41106849187588,-72.548630387431,-176.156794784155));
#176050=CARTESIAN_POINT('Ctrl Pts',(8.41101303376165,-72.5544627669252,
-176.148313233444));
#176051=CARTESIAN_POINT('Ctrl Pts',(8.41097732083378,-72.5582002437319,
-176.142841345939));
#176052=CARTESIAN_POINT('Ctrl Pts',(8.41032368769178,-72.6263945170234,
-176.042570516628));
#176053=CARTESIAN_POINT('Ctrl Pts',(8.40959647252647,-72.6963293373607,
-175.927578445735));
#176054=CARTESIAN_POINT('Ctrl Pts',(8.40828842764586,-72.7968914105421,
-175.726319312506));
#176055=CARTESIAN_POINT('Ctrl Pts',(8.40781726081728,-72.8296531002271,
-175.654464109059));
#176056=CARTESIAN_POINT('Ctrl Pts',(8.40706213181642,-72.8761394871332,
-175.539615438644));
#176057=CARTESIAN_POINT('Ctrl Pts',(8.40680248104364,-72.8911907824282,
-175.500158002453));
#176058=CARTESIAN_POINT('Ctrl Pts',(8.4064028588357,-72.9129021099126,-175.439252056873));
#176059=CARTESIAN_POINT('Ctrl Pts',(8.40620052494692,-72.9235412990844,
-175.408369486283));
#176060=CARTESIAN_POINT('Ctrl Pts',(8.40596059062688,-72.9355307482792,
-175.371601060581));
#176061=CARTESIAN_POINT('Ctrl Pts',(8.40583973271934,-72.9414142108593,
-175.353034085953));
#176062=CARTESIAN_POINT('Ctrl Pts',(8.40578775433374,-72.9439112614011,
-175.345037862003));
#176063=CARTESIAN_POINT('Ctrl Pts',(8.40575306260396,-72.9455704663852,
-175.339698415293));
#176064=CARTESIAN_POINT('Ctrl Pts',(8.40574305179098,-72.9460486900454,
-175.338157470166));
#176065=CARTESIAN_POINT('Ctrl Pts',(8.40413497651592,-73.0222745409279,
-175.090414177992));
#176066=CARTESIAN_POINT('Ctrl Pts',(8.40277568211103,-73.0511183020758,
-174.892229744757));
#176067=CARTESIAN_POINT('Ctrl Pts',(8.40089353347954,-73.0800350040009,
-174.598255016089));
#176068=CARTESIAN_POINT('Ctrl Pts',(8.40032278615858,-73.08000002,-174.501236406862));
#176069=CARTESIAN_POINT('Ctrl Pts',(8.4,-73.08000002,-174.451268889151));
#176070=CARTESIAN_POINT('Ctrl Pts',(8.4,-73.08000002,-174.451268889151));
#176071=CARTESIAN_POINT('Ctrl Pts',(8.89999999999996,-73.0800000199999,
-174.45126888915));
#176072=CARTESIAN_POINT('Ctrl Pts',(8.9,-72.58000002,-174.451268889151));
#176073=CARTESIAN_POINT('Ctrl Pts',(8.40197484549326,-73.08000002,-174.75697631869));
#176074=CARTESIAN_POINT('Ctrl Pts',(8.89999999999997,-73.0780290434905,
-174.756376067791));
#176075=CARTESIAN_POINT('Ctrl Pts',(8.9,-72.58000001309,-174.70608894667));
#176076=CARTESIAN_POINT('Ctrl Pts',(8.40390532350201,-73.0343597586633,
-175.055047332367));
#176077=CARTESIAN_POINT('Ctrl Pts',(8.89999999999997,-73.0306532835766,
-175.053905133681));
#176078=CARTESIAN_POINT('Ctrl Pts',(8.9,-72.5419664714886,-174.954543971783));
#176079=CARTESIAN_POINT('Ctrl Pts',(8.40673247093662,-72.8985137923177,
-175.490582060873));
#176080=CARTESIAN_POINT('Ctrl Pts',(8.89999999999997,-72.892300013639,-175.488192872161));
#176081=CARTESIAN_POINT('Ctrl Pts',(8.9,-72.4287614956301,-175.317581230789));
#176082=CARTESIAN_POINT('Ctrl Pts',(8.40765712457444,-72.8418854248583,
-175.632858253021));
#176083=CARTESIAN_POINT('Ctrl Pts',(8.89999999999996,-72.8349801887897,
-175.629812439872));
#176084=CARTESIAN_POINT('Ctrl Pts',(8.9,-72.3815711902508,-175.436174718935));
#176085=CARTESIAN_POINT('Ctrl Pts',(8.40942187655549,-72.7094695330285,
-175.904119271778));
#176086=CARTESIAN_POINT('Ctrl Pts',(8.89999999999995,-72.7014018648635,
-175.899567338683));
#176087=CARTESIAN_POINT('Ctrl Pts',(8.9,-72.2712246146549,-175.662282844729));
#176088=CARTESIAN_POINT('Ctrl Pts',(8.41026946333178,-72.6333495611344,
-176.034257895752));
#176089=CARTESIAN_POINT('Ctrl Pts',(8.90000000000094,-72.6248303464193,
-176.028888062411));
#176090=CARTESIAN_POINT('Ctrl Pts',(8.9,-72.2077913051056,-175.770759223));
#176091=CARTESIAN_POINT('Ctrl Pts',(8.41189381664575,-72.4610685811814,
-176.283431179031));
#176092=CARTESIAN_POINT('Ctrl Pts',(8.89999999999898,-72.4518932717193,
-176.276278393733));
#176093=CARTESIAN_POINT('Ctrl Pts',(8.9,-72.0642238201576,-175.978456398961));
#176094=CARTESIAN_POINT('Ctrl Pts',(8.41267385193151,-72.3642066660697,
-176.402964676645));
#176095=CARTESIAN_POINT('Ctrl Pts',(8.89999999999997,-72.354843766023,-176.394881486481));
#176096=CARTESIAN_POINT('Ctrl Pts',(8.9,-71.9835055577593,-176.078093003191));
#176097=CARTESIAN_POINT('Ctrl Pts',(8.41411048564612,-72.15640796091,-176.622941542856));
#176098=CARTESIAN_POINT('Ctrl Pts',(8.89999999999996,-72.1469580486365,
-176.612968031678));
#176099=CARTESIAN_POINT('Ctrl Pts',(8.9,-71.8103399713904,-176.261453778625));
#176100=CARTESIAN_POINT('Ctrl Pts',(8.41477368991416,-72.0449155064423,
-176.724399172119));
#176101=CARTESIAN_POINT('Ctrl Pts',(8.89999999999996,-72.0355638390553,
-176.713502881279));
#176102=CARTESIAN_POINT('Ctrl Pts',(8.9,-71.7174295924368,-176.34602338026));
#176103=CARTESIAN_POINT('Ctrl Pts',(8.4165979801388,-71.6877682388606,-177.003302608065));
#176104=CARTESIAN_POINT('Ctrl Pts',(8.89999999999996,-71.6793465425378,
-176.989505620533));
#176105=CARTESIAN_POINT('Ctrl Pts',(8.9,-71.4198068682475,-176.578502281526));
#176106=CARTESIAN_POINT('Ctrl Pts',(8.41759316850175,-71.4163525958445,
-177.155190995531));
#176107=CARTESIAN_POINT('Ctrl Pts',(8.90000000001297,-71.4089014982389,
-177.139847092069));
#176108=CARTESIAN_POINT('Ctrl Pts',(8.9,-71.1936270830052,-176.705108386635));
#176109=CARTESIAN_POINT('Ctrl Pts',(8.41828452049191,-71.1360889256296,
-177.260652939026));
#176110=CARTESIAN_POINT('Ctrl Pts',(8.89999999999996,-71.1298793121603,
-177.244155204947));
#176111=CARTESIAN_POINT('Ctrl Pts',(8.9,-70.9600741080247,-176.793015835821));
#176112=CARTESIAN_POINT('',(8.89999997275898,-71.2138732976769,-176.681036188727));
#176113=CARTESIAN_POINT('Ctrl Pts',(8.41817820009134,-71.1781942230057,
-177.244433726518));
#176114=CARTESIAN_POINT('Ctrl Pts',(8.4375676815764,-71.1735772869606,-177.245495661848));
#176115=CARTESIAN_POINT('Ctrl Pts',(8.45706991645918,-71.1692642601874,
-177.245202134556));
#176116=CARTESIAN_POINT('Ctrl Pts',(8.47646911593593,-71.1652585866833,
-177.243540741873));
#176117=CARTESIAN_POINT('Ctrl Pts',(8.49577878075638,-71.1612714008803,
-177.241887017147));
#176118=CARTESIAN_POINT('Ctrl Pts',(8.51498522998455,-71.1575887387568,
-177.23887793747));
#176119=CARTESIAN_POINT('Ctrl Pts',(8.53387350322163,-71.1542229400008,
-177.234551943534));
#176120=CARTESIAN_POINT('Ctrl Pts',(8.55275572222947,-71.1508582200793,
-177.230227336202));
#176121=CARTESIAN_POINT('Ctrl Pts',(8.57131886615291,-71.1478102320468,
-177.224586951484));
#176122=CARTESIAN_POINT('Ctrl Pts',(8.58936291095303,-71.1450997228584,
-177.217718454791));
#176123=CARTESIAN_POINT('Ctrl Pts',(8.60132827930681,-71.1433023298002,
-177.213163816743));
#176124=CARTESIAN_POINT('Ctrl Pts',(8.61306573561802,-71.1416535136919,
-177.208070186524));
#176125=CARTESIAN_POINT('Ctrl Pts',(8.62452390663931,-71.1401610362592,
-177.202473579344));
#176126=CARTESIAN_POINT('Ctrl Pts',(8.64195785660902,-71.1378901871993,
-177.193958174102));
#176127=CARTESIAN_POINT('Ctrl Pts',(8.65874305599649,-71.1359810973278,
-177.184277184033));
#176128=CARTESIAN_POINT('Ctrl Pts',(8.6747322821397,-71.1344654177415,-177.173585916584));
#176129=CARTESIAN_POINT('Ctrl Pts',(8.68781013665856,-71.1332257181495,
-177.164841350771));
#176130=CARTESIAN_POINT('Ctrl Pts',(8.70035618379775,-71.1322493563043,
-177.155421846894));
#176131=CARTESIAN_POINT('Ctrl Pts',(8.71231337647849,-71.1315550709588,
-177.145423344239));
#176132=CARTESIAN_POINT('Ctrl Pts',(8.72071844212296,-71.1310670371819,
-177.13839509995));
#176133=CARTESIAN_POINT('Ctrl Pts',(8.72898238026593,-71.1307390133705,
-177.130939053363));
#176134=CARTESIAN_POINT('Ctrl Pts',(8.73693891047363,-71.1305519295886,
-177.123212241614));
#176135=CARTESIAN_POINT('Ctrl Pts',(8.74495542280103,-71.1303634354328,
-177.11542717953));
#176136=CARTESIAN_POINT('Ctrl Pts',(8.75265932972759,-71.1303181328619,
-177.107367856751));
#176137=CARTESIAN_POINT('Ctrl Pts',(8.75991760607799,-71.1304134424502,
-177.099229163266));
#176138=CARTESIAN_POINT('Ctrl Pts',(8.7674395027199,-71.1305122136788,-177.090794872777));
#176139=CARTESIAN_POINT('Ctrl Pts',(8.77448249260797,-71.1307621917784,
-177.082276150992));
#176140=CARTESIAN_POINT('Ctrl Pts',(8.78094542604629,-71.1311763041073,
-177.073915789783));
#176141=CARTESIAN_POINT('Ctrl Pts',(8.78162793702423,-71.1312200359843,
-177.073032903032));
#176142=CARTESIAN_POINT('Ctrl Pts',(8.78230402224777,-71.1312656104982,
-177.072151798275));
#176143=CARTESIAN_POINT('Ctrl Pts',(8.78297359262185,-71.1313130510302,
-177.071272771358));
#176144=CARTESIAN_POINT('Ctrl Pts',(8.79600518416733,-71.1322363679208,
-177.054164607398));
#176145=CARTESIAN_POINT('Ctrl Pts',(8.80812287853332,-71.1338142536925,
-177.035862021369));
#176146=CARTESIAN_POINT('Ctrl Pts',(8.81918777435556,-71.1360315585211,
-177.016532094964));
#176147=CARTESIAN_POINT('Ctrl Pts',(8.83018794089226,-71.1382358921875,
-176.997315248008));
#176148=CARTESIAN_POINT('Ctrl Pts',(8.84014710779646,-71.1410722089947,
-176.977084017575));
#176149=CARTESIAN_POINT('Ctrl Pts',(8.84897550413698,-71.1445316150493,
-176.956023186274));
#176150=CARTESIAN_POINT('Ctrl Pts',(8.85781148218762,-71.1479939919961,
-176.93494426821));
#176151=CARTESIAN_POINT('Ctrl Pts',(8.86551459101941,-71.152080615517,-176.913035370358));
#176152=CARTESIAN_POINT('Ctrl Pts',(8.8720466382876,-71.1567877685274,-176.890487227023));
#176153=CARTESIAN_POINT('Ctrl Pts',(8.87859517279702,-71.161506802647,-176.867882170952));
#176154=CARTESIAN_POINT('Ctrl Pts',(8.8839669332145,-71.1668496494419,-176.844635638253));
#176155=CARTESIAN_POINT('Ctrl Pts',(8.88817509862186,-71.1728160217048,
-176.820929774949));
#176156=CARTESIAN_POINT('Ctrl Pts',(8.89243798486614,-71.1788599776299,
-176.796915652689));
#176157=CARTESIAN_POINT('Ctrl Pts',(8.89550727603177,-71.1855439770296,
-176.772431064185));
#176158=CARTESIAN_POINT('Ctrl Pts',(8.89744466027399,-71.1928686565381,
-176.747640578285));
#176159=CARTESIAN_POINT('Ctrl Pts',(8.89916327906971,-71.1993662482918,
-176.725649383098));
#176160=CARTESIAN_POINT('Ctrl Pts',(8.89999223003091,-71.2063681174939,
-176.703417350348));
#176161=CARTESIAN_POINT('Ctrl Pts',(8.89999994551797,-71.2138732976722,
-176.681036188718));
#176162=CARTESIAN_POINT('Ctrl Pts',(8.9,-72.58000002,-174.451268889151));
#176163=CARTESIAN_POINT('Ctrl Pts',(8.9,-72.58000002,-174.643662890546));
#176164=CARTESIAN_POINT('Ctrl Pts',(8.90000000018189,-72.5583230934325,
-174.832372832558));
#176165=CARTESIAN_POINT('Ctrl Pts',(8.89999999981754,-72.5152520259331,
-175.017431778835));
#176166=CARTESIAN_POINT('Ctrl Pts',(8.89999999974366,-72.5065182586995,
-175.0549572421));
#176167=CARTESIAN_POINT('Ctrl Pts',(8.89999999963417,-72.4969046367659,
-175.092332595982));
#176168=CARTESIAN_POINT('Ctrl Pts',(8.89999999944856,-72.4864132528963,
-175.129558133433));
#176169=CARTESIAN_POINT('Ctrl Pts',(8.89999999933697,-72.4801056624026,
-175.151938731556));
#176170=CARTESIAN_POINT('Ctrl Pts',(8.89999999923514,-72.4734752856604,
-175.174281489137));
#176171=CARTESIAN_POINT('Ctrl Pts',(8.8999999991621,-72.4665241218154,-175.196577428232));
#176172=CARTESIAN_POINT('Ctrl Pts',(8.89999999896656,-72.4479148757583,
-175.256266801975));
#176173=CARTESIAN_POINT('Ctrl Pts',(8.89999999902277,-72.4269795805928,
-175.315421893865));
#176174=CARTESIAN_POINT('Ctrl Pts',(8.89999999928889,-72.403958991798,-175.373505006317));
#176175=CARTESIAN_POINT('Ctrl Pts',(8.89999999941373,-72.3931602367393,
-175.400751281815));
#176176=CARTESIAN_POINT('Ctrl Pts',(8.8999999995758,-72.3819033245034,-175.427761928545));
#176177=CARTESIAN_POINT('Ctrl Pts',(8.89999999971899,-72.3702165277834,
-175.454483443826));
#176178=CARTESIAN_POINT('Ctrl Pts',(8.89999999989012,-72.356250141463,-175.486417173351));
#176179=CARTESIAN_POINT('Ctrl Pts',(8.89999999994017,-72.3416346359546,
-175.518026103028));
#176180=CARTESIAN_POINT('Ctrl Pts',(8.89999999996783,-72.3264029998066,
-175.549231269472));
#176181=CARTESIAN_POINT('Ctrl Pts',(8.90000000003108,-72.2915692635033,
-175.620595404528));
#176182=CARTESIAN_POINT('Ctrl Pts',(8.90000000000045,-72.2533993434511,
-175.690229109067));
#176183=CARTESIAN_POINT('Ctrl Pts',(8.89999999999886,-72.2119321367876,
-175.757979856507));
#176184=CARTESIAN_POINT('Ctrl Pts',(8.89999999999793,-72.1877543610133,
-175.797482454149));
#176185=CARTESIAN_POINT('Ctrl Pts',(8.89999999999706,-72.1624481423419,
-175.836359594911));
#176186=CARTESIAN_POINT('Ctrl Pts',(8.89999999999683,-72.1360090283531,
-175.874608824138));
#176187=CARTESIAN_POINT('Ctrl Pts',(8.8999999999962,-72.0642253375692,-175.978457646179));
#176188=CARTESIAN_POINT('Ctrl Pts',(8.89999999999926,-71.983506448042,-176.078093573446));
#176189=CARTESIAN_POINT('Ctrl Pts',(8.8999999999998,-71.8969230956059,-176.169773703533));
#176190=CARTESIAN_POINT('Ctrl Pts',(8.90000000000003,-71.8581752387953,
-176.210802474689));
#176191=CARTESIAN_POINT('Ctrl Pts',(8.9,-71.8181601276395,-176.250407223135));
#176192=CARTESIAN_POINT('Ctrl Pts',(8.9,-71.7768804944358,-176.288591148433));
#176193=CARTESIAN_POINT('Ctrl Pts',(8.9,-71.7350069729775,-176.327324424174));
#176194=CARTESIAN_POINT('Ctrl Pts',(8.9,-71.691683332544,-176.364727207912));
#176195=CARTESIAN_POINT('Ctrl Pts',(8.9,-71.6470438920772,-176.40066126947));
#176196=CARTESIAN_POINT('Ctrl Pts',(8.9,-71.6374948625339,-176.408348091075));
#176197=CARTESIAN_POINT('Ctrl Pts',(8.9,-71.6278871345229,-176.415966736531));
#176198=CARTESIAN_POINT('Ctrl Pts',(8.9,-71.6182220181434,-176.423516347907));
#176199=CARTESIAN_POINT('Ctrl Pts',(8.9,-71.5940005454252,-176.442436213824));
#176200=CARTESIAN_POINT('Ctrl Pts',(8.9,-71.5693801206575,-176.460921216669));
#176201=CARTESIAN_POINT('Ctrl Pts',(8.9,-71.5444197215458,-176.478940580039));
#176202=CARTESIAN_POINT('Ctrl Pts',(8.9,-71.4920391665984,-176.516755049627));
#176203=CARTESIAN_POINT('Ctrl Pts',(8.89999999451621,-71.4381757456861,
-176.552638667358));
#176204=CARTESIAN_POINT('Ctrl Pts',(8.89999997064356,-71.3830164241513,
-176.586384312661));
#176205=CARTESIAN_POINT('Ctrl Pts',(8.89999995870723,-71.355436763384,-176.603257135313));
#176206=CARTESIAN_POINT('Ctrl Pts',(8.89999994562374,-71.3275333910231,
-176.61959527903));
#176207=CARTESIAN_POINT('Ctrl Pts',(8.89999993949196,-71.2993337292249,
-176.635377629733));
#176208=CARTESIAN_POINT('Ctrl Pts',(8.89999993336017,-71.2711340674268,
-176.651159980436));
#176209=CARTESIAN_POINT('Ctrl Pts',(8.89999993496575,-71.242638116192,-176.666386538126));
#176210=CARTESIAN_POINT('Ctrl Pts',(8.89999994551797,-71.2138732976722,
-176.681036188718));
#176211=CARTESIAN_POINT('Ctrl Pts',(8.9,-71.2138732976838,-171.871644662643));
#176212=CARTESIAN_POINT('Ctrl Pts',(8.89999999999996,-70.7880957152448,
-171.871644662643));
#176213=CARTESIAN_POINT('Ctrl Pts',(9.32033898305081,-70.7202599648223,
-171.871644662643));
#176214=CARTESIAN_POINT('Ctrl Pts',(8.9,-71.2138732807092,-171.652697712588));
#176215=CARTESIAN_POINT('Ctrl Pts',(8.89999999999997,-70.7880957023883,
-171.715624308049));
#176216=CARTESIAN_POINT('Ctrl Pts',(9.32033898569755,-70.7202599643952,
-171.725683074261));
#176217=CARTESIAN_POINT('Ctrl Pts',(8.9,-71.16598797688,-171.437720890984));
#176218=CARTESIAN_POINT('Ctrl Pts',(8.90000000000455,-70.7514100828351,
-171.561941332422));
#176219=CARTESIAN_POINT('Ctrl Pts',(9.32278024510803,-70.6879410017649,
-171.582358093922));
#176220=CARTESIAN_POINT('Ctrl Pts',(8.9,-71.0715121820529,-171.237717270032));
#176221=CARTESIAN_POINT('Ctrl Pts',(8.89999999999997,-70.680735306053,-171.422308714525));
#176222=CARTESIAN_POINT('Ctrl Pts',(9.3276302147955,-70.6241744288951,-171.449026400902));
#176223=CARTESIAN_POINT('',(8.9,-71.2138732976838,-171.871644662643));
#176224=CARTESIAN_POINT('',(9.32033898305081,-70.7202599648223,-171.871644662643));
#176225=CARTESIAN_POINT('Origin',(9.4,-71.2138732976838,-171.871644662643));
#176226=CARTESIAN_POINT('Origin',(9.42941145485511,-69.2860804967121,-171.96074458416));
#176227=CARTESIAN_POINT('Origin',(8.9,-69.0831852719725,-172.006057477089));
#176228=CARTESIAN_POINT('Origin',(0.,-12.9675000200281,-171.64995));
#176229=CARTESIAN_POINT('Origin',(0.,-12.9675000200281,-171.449026400902));
#176230=CARTESIAN_POINT('Ctrl Pts',(15.5499999899231,-69.8405291599117,
-171.179005018994));
#176231=CARTESIAN_POINT('Ctrl Pts',(15.5501264775731,-69.2858420378445,
-171.477695372047));
#176232=CARTESIAN_POINT('Ctrl Pts',(14.9365391746094,-69.4116829512028,
-171.409919376296));
#176233=CARTESIAN_POINT('Ctrl Pts',(15.5499999897578,-69.9655161046422,
-171.411462758814));
#176234=CARTESIAN_POINT('Ctrl Pts',(15.5501302527646,-69.3463988305637,
-171.619616090566));
#176235=CARTESIAN_POINT('Ctrl Pts',(14.9264726997877,-69.4976592258842,
-171.564867666237));
#176236=CARTESIAN_POINT('Ctrl Pts',(15.5499999896779,-70.0263968022397,
-171.67105498688));
#176237=CARTESIAN_POINT('Ctrl Pts',(15.5501321305782,-69.3710444733645,
-171.760987815194));
#176238=CARTESIAN_POINT('Ctrl Pts',(14.9216112388798,-69.5395284795157,
-171.737936502975));
#176239=CARTESIAN_POINT('Ctrl Pts',(15.5499999896938,-70.014294651194,-171.938280796929));
#176240=CARTESIAN_POINT('Ctrl Pts',(15.5501317589361,-69.3660274114058,
-171.908368448016));
#176241=CARTESIAN_POINT('Ctrl Pts',(14.9225783333433,-69.5312053406244,
-171.916063466645));
#176242=CARTESIAN_POINT('',(14.9224576271186,-69.5322439721301,-171.871644662643));
#176243=CARTESIAN_POINT('',(15.55,-70.015703322148,-171.871644662643));
#176244=CARTESIAN_POINT('Origin',(15.05,-70.015703322148,-171.871644662643));
#176245=CARTESIAN_POINT('Origin',(15.5500003878737,-68.575584871424,-171.847853238404));
#176246=CARTESIAN_POINT('Origin',(15.0818693592772,-68.1696517950468,-171.933679697753));
#176247=CARTESIAN_POINT('Origin',(16.05,67.7009572055632,-176.84995));
#176248=CARTESIAN_POINT('',(15.55,-70.015703322148,-176.84995));
#176249=CARTESIAN_POINT('',(15.55,67.7009572055632,-176.84995));
#176250=CARTESIAN_POINT('',(16.05,-69.7424724991055,-177.34995));
#176251=CARTESIAN_POINT('Ctrl Pts',(15.55,-70.015703322148,-176.84995));
#176252=CARTESIAN_POINT('Ctrl Pts',(15.55,-70.015703322148,-176.91494123845));
#176253=CARTESIAN_POINT('Ctrl Pts',(15.5628555543669,-70.0086459123549,
-176.981685962264));
#176254=CARTESIAN_POINT('Ctrl Pts',(15.6027343713053,-69.9874736829755,
-177.076046165501));
#176255=CARTESIAN_POINT('Ctrl Pts',(15.6194250432354,-69.9786519207341,
-177.106520258027));
#176256=CARTESIAN_POINT('Ctrl Pts',(15.6493572717207,-69.9627727486995,
-177.149601759466));
#176257=CARTESIAN_POINT('Ctrl Pts',(15.665543236393,-69.9541715305142,-177.170484481011));
#176258=CARTESIAN_POINT('Ctrl Pts',(15.6864714438853,-69.9429789196704,
-177.193440465358));
#176259=CARTESIAN_POINT('Ctrl Pts',(15.695866056015,-69.9379339743885,-177.202950082533));
#176260=CARTESIAN_POINT('Ctrl Pts',(15.7022221563807,-69.93451554152,-177.20921380285));
#176261=CARTESIAN_POINT('Ctrl Pts',(15.7065958386429,-69.9321588011156,
-177.213380882268));
#176262=CARTESIAN_POINT('Ctrl Pts',(15.742655916585,-69.9127040608674,-177.24705982817));
#176263=CARTESIAN_POINT('Ctrl Pts',(15.7871759484761,-69.8878370635255,
-177.279883700671));
#176264=CARTESIAN_POINT('Ctrl Pts',(15.9012930184395,-69.8249897616838,
-177.331412046965));
#176265=CARTESIAN_POINT('Ctrl Pts',(15.9712278950399,-69.7870094571841,
-177.34995));
#176266=CARTESIAN_POINT('Ctrl Pts',(16.05,-69.7424724991055,-177.34995));
#176267=CARTESIAN_POINT('',(16.05,-73.08000002,-177.34995));
#176268=CARTESIAN_POINT('Origin',(41.5,-73.08000002,-177.34995));
#176269=CARTESIAN_POINT('',(16.55,-69.5987413979107,-177.34995));
#176270=CARTESIAN_POINT('Origin',(0.,-12.9675000200281,-177.34995));
#176271=CARTESIAN_POINT('',(16.55,-73.08000002,-177.34995));
#176272=CARTESIAN_POINT('Origin',(16.55,-73.08000002,-176.84995));
#176273=CARTESIAN_POINT('',(17.05,-69.2968662511513,-176.84995));
#176274=CARTESIAN_POINT('Ctrl Pts',(16.55,-69.5987413979107,-177.34995));
#176275=CARTESIAN_POINT('Ctrl Pts',(16.6373149037964,-69.5477073176868,
-177.34995));
#176276=CARTESIAN_POINT('Ctrl Pts',(16.7108961971465,-69.505235927113,-177.327452298007));
#176277=CARTESIAN_POINT('Ctrl Pts',(16.7952352006602,-69.4543728757275,
-177.286795171739));
#176278=CARTESIAN_POINT('Ctrl Pts',(16.8192471597269,-69.4395591976782,
-177.272004751375));
#176279=CARTESIAN_POINT('Ctrl Pts',(16.849797428493,-69.420549689223,-177.250296803926));
#176280=CARTESIAN_POINT('Ctrl Pts',(16.85907485883,-69.4147483545077,-177.243132320069));
#176281=CARTESIAN_POINT('Ctrl Pts',(16.8717470097012,-69.4068491045895,
-177.232714631389));
#176282=CARTESIAN_POINT('Ctrl Pts',(16.8777722497188,-69.4031001676691,
-177.227587343521));
#176283=CARTESIAN_POINT('Ctrl Pts',(16.8842838194923,-69.3990776119963,
-177.221789622403));
#176284=CARTESIAN_POINT('Ctrl Pts',(16.8869663155695,-69.3974289175796,
-177.219348341421));
#176285=CARTESIAN_POINT('Ctrl Pts',(16.8887309156035,-69.3963465119717,
-177.217730912076));
#176286=CARTESIAN_POINT('Ctrl Pts',(16.8887814612853,-69.3963144313396,
-177.217689547856));
#176287=CARTESIAN_POINT('Ctrl Pts',(16.9978912643005,-69.3296738982238,
-177.116243128376));
#176288=CARTESIAN_POINT('Ctrl Pts',(17.05,-69.2968662511514,-176.977183756916));
#176289=CARTESIAN_POINT('Ctrl Pts',(17.05,-69.2968662511513,-176.84995));
#176290=CARTESIAN_POINT('',(17.05,67.7009572055632,-176.84995));
#176291=CARTESIAN_POINT('Ctrl Pts',(17.0500000069342,-69.2954487057977,
-171.937551171933));
#176292=CARTESIAN_POINT('Ctrl Pts',(17.0499387022882,-68.9277121722468,
-171.920632758432));
#176293=CARTESIAN_POINT('Ctrl Pts',(17.4014093021639,-68.8184551193695,
-171.915576738158));
#176294=CARTESIAN_POINT('Ctrl Pts',(17.0500000069124,-69.3074655181351,
-171.673561286109));
#176295=CARTESIAN_POINT('Ctrl Pts',(17.0499389461697,-68.9377102872281,
-171.724562885898));
#176296=CARTESIAN_POINT('Ctrl Pts',(17.4003036470898,-68.8268112548536,
-171.739609324912));
#176297=CARTESIAN_POINT('Ctrl Pts',(17.0500000070217,-69.2471945003534,
-171.413338787174));
#176298=CARTESIAN_POINT('Ctrl Pts',(17.0499377162343,-68.887140708855,-171.529148195035));
#176299=CARTESIAN_POINT('Ctrl Pts',(17.4058449755969,-68.7849016359872,
-171.566109516219));
#176300=CARTESIAN_POINT('Ctrl Pts',(17.050000007256,-69.1191208280442,-171.178440426026));
#176301=CARTESIAN_POINT('Ctrl Pts',(17.049935034885,-68.784349448281,-171.361182926232));
#176302=CARTESIAN_POINT('Ctrl Pts',(17.4177209010562,-68.6958205805999,
-171.409539580699));
#176303=CARTESIAN_POINT('',(17.05,-69.2968662511513,-171.871644662643));
#176304=CARTESIAN_POINT('',(17.4012711864406,-68.8194987407181,-171.871644662643));
#176305=CARTESIAN_POINT('Origin',(17.55,-69.2968662511513,-171.871644662643));
#176306=CARTESIAN_POINT('Origin',(17.5775564056945,-67.4962149130001,-171.919974670304));
#176307=CARTESIAN_POINT('Origin',(17.0499997303006,-67.819556247646,-171.852380931002));
#176308=CARTESIAN_POINT('Origin',(0.,-12.9675000200281,-171.64995));
#176309=CARTESIAN_POINT('Origin',(0.,-12.9675000200281,-171.449026400902));
#176310=CARTESIAN_POINT('Ctrl Pts',(23.6999999991623,-67.0454033354271,
-171.20624326692));
#176311=CARTESIAN_POINT('Ctrl Pts',(23.7000418723672,-66.4085345904086,
-171.54923960952));
#176312=CARTESIAN_POINT('Ctrl Pts',(23.0233258551592,-66.6335614679979,
-171.428053802022));
#176313=CARTESIAN_POINT('Ctrl Pts',(23.6999999991454,-67.1609416565798,
-171.420795636131));
#176314=CARTESIAN_POINT('Ctrl Pts',(23.7000436385783,-66.4472919682882,
-171.670421709918));
#176315=CARTESIAN_POINT('Ctrl Pts',(23.0096928629965,-66.7164302706426,
-171.571078901793));
#176316=CARTESIAN_POINT('Ctrl Pts',(23.6999999991368,-67.2206799332608,
-171.660715193498));
#176317=CARTESIAN_POINT('Ctrl Pts',(23.7000445959749,-66.4581897882971,
-171.777275420467));
#176318=CARTESIAN_POINT('Ctrl Pts',(23.0026938228069,-66.7592463230828,
-171.731032985114));
#176319=CARTESIAN_POINT('Ctrl Pts',(23.6999999991377,-67.2142749444978,
-171.907589194386));
#176320=CARTESIAN_POINT('Ctrl Pts',(23.7000444926391,-66.4569597257247,
-171.887725483324));
#176321=CARTESIAN_POINT('Ctrl Pts',(23.0034444927494,-66.7546555329274,
-171.895606459213));
#176322=CARTESIAN_POINT('',(23.0033898305084,-66.7549897951204,-171.871644662643));
#176323=CARTESIAN_POINT('',(23.7,-67.2147119299503,-171.871644662643));
#176324=CARTESIAN_POINT('Origin',(23.2,-67.2147119299503,-171.871644662643));
#176325=CARTESIAN_POINT('Origin',(23.7000000319861,-65.6225360749325,-171.86419456266));
#176326=CARTESIAN_POINT('Origin',(23.2065639509939,-65.5194270282055,-171.885488297765));
#176327=CARTESIAN_POINT('Origin',(24.2,67.7009572055632,-176.84995));
#176328=CARTESIAN_POINT('',(23.7,-67.2147119299503,-176.84995));
#176329=CARTESIAN_POINT('',(23.7,67.7009572055632,-176.84995));
#176330=CARTESIAN_POINT('Ctrl Pts',(23.7,-67.2147119299503,-176.84995));
#176331=CARTESIAN_POINT('Ctrl Pts',(23.7,-67.2147119285726,-176.870692031375));
#176332=CARTESIAN_POINT('Ctrl Pts',(23.7012797601937,-67.2135616384388,
-176.891634364146));
#176333=CARTESIAN_POINT('Ctrl Pts',(23.7039194454134,-67.2112230997102,
-176.912596783915));
#176334=CARTESIAN_POINT('Ctrl Pts',(23.7066095392776,-67.2088399031692,
-176.933959511703));
#176335=CARTESIAN_POINT('Ctrl Pts',(23.7107117632145,-67.2052226460133,
-176.955342815323));
#176336=CARTESIAN_POINT('Ctrl Pts',(23.7162692188089,-67.2003662942674,
-176.976554114755));
#176337=CARTESIAN_POINT('Ctrl Pts',(23.7220047923845,-67.1953542951115,
-176.998445242172));
#176338=CARTESIAN_POINT('Ctrl Pts',(23.7292901618176,-67.1890225112425,
-177.020152969052));
#176339=CARTESIAN_POINT('Ctrl Pts',(23.7381319919838,-67.1814025218832,
-177.041467487942));
#176340=CARTESIAN_POINT('Ctrl Pts',(23.7391976331291,-67.1804841402771,
-177.044036371069));
#176341=CARTESIAN_POINT('Ctrl Pts',(23.7402858382315,-67.1795470891622,
-177.046599546418));
#176342=CARTESIAN_POINT('Ctrl Pts',(23.7413965830518,-67.1785914583024,
-177.04915664994));
#176343=CARTESIAN_POINT('Ctrl Pts',(23.741870080286,-67.1781840842947,-177.050246712593));
#176344=CARTESIAN_POINT('Ctrl Pts',(23.7423474960057,-67.1777734819474,
-177.051335172668));
#176345=CARTESIAN_POINT('Ctrl Pts',(23.7428288211218,-67.1773596636845,
-177.05242200224));
#176346=CARTESIAN_POINT('Ctrl Pts',(23.7517852561296,-67.169659387399,-177.072645585206));
#176347=CARTESIAN_POINT('Ctrl Pts',(23.7621641594692,-67.1607728029265,
-177.09245347496));
#176348=CARTESIAN_POINT('Ctrl Pts',(23.7739445340405,-67.1506901238837,
-177.111633175902));
#176349=CARTESIAN_POINT('Ctrl Pts',(23.7812121202196,-67.1444698854341,
-177.123465578059));
#176350=CARTESIAN_POINT('Ctrl Pts',(23.789012306361,-67.1377950491387,-177.135058645404));
#176351=CARTESIAN_POINT('Ctrl Pts',(23.7973324888522,-67.1306693301689,
-177.146360830239));
#176352=CARTESIAN_POINT('Ctrl Pts',(23.8082358689858,-67.121331263037,-177.161172045945));
#176353=CARTESIAN_POINT('Ctrl Pts',(23.8200331807256,-67.1112150240728,
-177.175484411367));
#176354=CARTESIAN_POINT('Ctrl Pts',(23.8326843101586,-67.1003206129902,
-177.189182955555));
#176355=CARTESIAN_POINT('Ctrl Pts',(23.839009874875,-67.0948734074488,-177.196032227649));
#176356=CARTESIAN_POINT('Ctrl Pts',(23.8455486735696,-67.089231658847,-177.202728037883));
#176357=CARTESIAN_POINT('Ctrl Pts',(23.8522943595325,-67.0833953671697,
-177.209255974639));
#176358=CARTESIAN_POINT('Ctrl Pts',(23.8531068061667,-67.0826924474732,
-177.210042195681));
#176359=CARTESIAN_POINT('Ctrl Pts',(23.853922355455,-67.0819866047119,-177.210826081485));
#176360=CARTESIAN_POINT('Ctrl Pts',(23.8547411191067,-67.0812777232316,
-177.211607719321));
#176361=CARTESIAN_POINT('Ctrl Pts',(23.8573214233073,-67.0790437087423,
-177.214071022849));
#176362=CARTESIAN_POINT('Ctrl Pts',(23.8599283666054,-67.0767840894236,
-177.21650808797));
#176363=CARTESIAN_POINT('Ctrl Pts',(23.8625657042021,-67.0744950225944,
-177.218921760132));
#176364=CARTESIAN_POINT('Ctrl Pts',(23.8643028035408,-67.0729873140326,
-177.220511540796));
#176365=CARTESIAN_POINT('Ctrl Pts',(23.8660524525317,-67.0714674465852,
-177.222090569041));
#176366=CARTESIAN_POINT('Ctrl Pts',(23.8678145807482,-67.0699354202555,
-177.223658583861));
#176367=CARTESIAN_POINT('Ctrl Pts',(23.8691222662937,-67.0687984946517,
-177.224822216732));
#176368=CARTESIAN_POINT('Ctrl Pts',(23.8708574224727,-67.0672886464112,
-177.226347875915));
#176369=CARTESIAN_POINT('Ctrl Pts',(23.8720842239918,-67.0662206684884,
-177.227414994998));
#176370=CARTESIAN_POINT('Ctrl Pts',(23.8725105581066,-67.0658495282385,
-177.227785836786));
#176371=CARTESIAN_POINT('Ctrl Pts',(23.8728752241867,-67.0655320043267,
-177.228101752667));
#176372=CARTESIAN_POINT('Ctrl Pts',(23.8731383243725,-67.0653028646134,
-177.228329329561));
#176373=CARTESIAN_POINT('Ctrl Pts',(23.887766197763,-67.0525631293517,-177.240982175007));
#176374=CARTESIAN_POINT('Ctrl Pts',(23.9043961020168,-67.0378486429253,
-177.25389505309));
#176375=CARTESIAN_POINT('Ctrl Pts',(23.9232187485375,-67.0211404256529,
-177.266409258693));
#176376=CARTESIAN_POINT('Ctrl Pts',(23.9397950230927,-67.0064262356728,
-177.277429967587));
#176377=CARTESIAN_POINT('Ctrl Pts',(23.9580728621069,-66.990165285662,-177.288140814983));
#176378=CARTESIAN_POINT('Ctrl Pts',(23.9781590017411,-66.9723643726518,
-177.298066162563));
#176379=CARTESIAN_POINT('Ctrl Pts',(23.9861671400254,-66.9652673308325,
-177.302023297055));
#176380=CARTESIAN_POINT('Ctrl Pts',(23.9944623545837,-66.9579257812752,
-177.305855307432));
#176381=CARTESIAN_POINT('Ctrl Pts',(24.0030496089252,-66.9503413947625,
-177.30953097987));
#176382=CARTESIAN_POINT('Ctrl Pts',(24.0072023560129,-66.9466736288213,
-177.311308514039));
#176383=CARTESIAN_POINT('Ctrl Pts',(24.0114211643624,-66.942952280217,-177.313048623161));
#176384=CARTESIAN_POINT('Ctrl Pts',(24.0157157303611,-66.9391675502872,
-177.314751315045));
#176385=CARTESIAN_POINT('Ctrl Pts',(24.0184771087475,-66.9367339932224,
-177.315846135003));
#176386=CARTESIAN_POINT('Ctrl Pts',(24.021264601256,-66.9342788232166,-177.316923432121));
#176387=CARTESIAN_POINT('Ctrl Pts',(24.0240806672581,-66.9317995439269,
-177.317982914177));
#176388=CARTESIAN_POINT('Ctrl Pts',(24.0418552938833,-66.9161506693476,
-177.324670221204));
#176389=CARTESIAN_POINT('Ctrl Pts',(24.0607501496559,-66.8995614641303,
-177.330637276664));
#176390=CARTESIAN_POINT('Ctrl Pts',(24.0806754375043,-66.8820258797966,
-177.335543884029));
#176391=CARTESIAN_POINT('Ctrl Pts',(24.08898231696,-66.8747152709686,-177.337589455276));
#176392=CARTESIAN_POINT('Ctrl Pts',(24.0974678845696,-66.8672405112961,
-177.339451006893));
#176393=CARTESIAN_POINT('Ctrl Pts',(24.1061239179331,-66.8596026636562,
-177.341105388679));
#176394=CARTESIAN_POINT('Ctrl Pts',(24.1276333471999,-66.8406233302057,
-177.34521637191));
#176395=CARTESIAN_POINT('Ctrl Pts',(24.1501943609476,-66.8206347276726,
-177.348045999505));
#176396=CARTESIAN_POINT('Ctrl Pts',(24.17369751107,-66.7996305028337,-177.349268224205));
#176397=CARTESIAN_POINT('Ctrl Pts',(24.1823400263588,-66.7919068856439,
-177.349717657391));
#176398=CARTESIAN_POINT('Ctrl Pts',(24.1911096430966,-66.7840462719998,
-177.34995));
#176399=CARTESIAN_POINT('Ctrl Pts',(24.2,-66.7760495265873,-177.34995));
#176400=CARTESIAN_POINT('Origin',(0.,-12.9675000200281,-171.64995));
#176401=CARTESIAN_POINT('',(42.,30.4123236926243,-171.64995));
#176402=CARTESIAN_POINT('Origin',(44.5079524583208,31.5404524382925,-171.64995));
#176403=CARTESIAN_POINT('',(42.,28.91999998,-171.64995));
#176404=CARTESIAN_POINT('Origin',(0.,-12.9675000200281,-171.64995));
#176405=CARTESIAN_POINT('',(42.,32.6685811839606,-171.64995));
#176406=CARTESIAN_POINT('',(42.,28.91999998,-171.64995));
#176407=CARTESIAN_POINT('Origin',(44.5079524583208,31.5404524382925,-171.64995));
#176408=CARTESIAN_POINT('Ctrl Pts',(45.342056117244,28.41999998,-171.14995));
#176409=CARTESIAN_POINT('Ctrl Pts',(45.342056117244,28.41999998,-171.649955087908));
#176410=CARTESIAN_POINT('Ctrl Pts',(45.342056117244,28.9200050678815,-171.649949999974));
#176411=CARTESIAN_POINT('Ctrl Pts',(45.2032855852167,28.41999998,-171.149950027441));
#176412=CARTESIAN_POINT('Ctrl Pts',(45.2207546457863,28.4199999799926,-171.611343620546));
#176413=CARTESIAN_POINT('Ctrl Pts',(45.2161093325492,28.8799153348106,-171.649950408626));
#176414=CARTESIAN_POINT('Ctrl Pts',(45.0642313709306,28.41999998,-171.155055788632));
#176415=CARTESIAN_POINT('Ctrl Pts',(45.0814092233328,28.4199999800032,-171.586474354512));
#176416=CARTESIAN_POINT('Ctrl Pts',(45.0809055449373,28.8470468727513,-171.649950690988));
#176417=CARTESIAN_POINT('Ctrl Pts',(44.7862672310248,28.41999998,-171.163656910012));
#176418=CARTESIAN_POINT('Ctrl Pts',(44.7998786663722,28.4199999799969,-171.556875075933));
#176419=CARTESIAN_POINT('Ctrl Pts',(44.7999542633241,28.8023061531436,-171.649951053492));
#176420=CARTESIAN_POINT('Ctrl Pts',(44.6472721153249,28.41999998,-171.16702013224));
#176421=CARTESIAN_POINT('Ctrl Pts',(44.652744176702,28.4199999799986,-171.550586180072));
#176422=CARTESIAN_POINT('Ctrl Pts',(44.6541596767004,28.7904721518725,-171.64995113455));
#176423=CARTESIAN_POINT('Ctrl Pts',(44.3691883762669,28.41999998,-171.167028040093));
#176424=CARTESIAN_POINT('Ctrl Pts',(44.3637416796286,28.4199999800014,-171.550568959217));
#176425=CARTESIAN_POINT('Ctrl Pts',(44.36232828092,28.7904412154044,-171.649951134795));
#176426=CARTESIAN_POINT('Ctrl Pts',(44.2300913879779,28.41999998,-171.163669856825));
#176427=CARTESIAN_POINT('Ctrl Pts',(44.2164931090597,28.4199999799986,-171.556843793952));
#176428=CARTESIAN_POINT('Ctrl Pts',(44.2164190292983,28.802252604719,-171.649951053893));
#176429=CARTESIAN_POINT('Ctrl Pts',(43.9520032655911,28.41999998,-171.15506708045));
#176430=CARTESIAN_POINT('Ctrl Pts',(43.9348222136901,28.4199999800015,-171.586421593668));
#176431=CARTESIAN_POINT('Ctrl Pts',(43.9353228646307,28.846974377406,-171.649950691605));
#176432=CARTESIAN_POINT('Ctrl Pts',(43.8129594627921,28.41999998,-171.149950027533));
#176433=CARTESIAN_POINT('Ctrl Pts',(43.7954409326623,28.41999998,-171.611251100138));
#176434=CARTESIAN_POINT('Ctrl Pts',(43.8001087095933,28.8798156647999,-171.649950409642));
#176435=CARTESIAN_POINT('Ctrl Pts',(43.6738487993976,28.41999998,-171.14995));
#176436=CARTESIAN_POINT('Ctrl Pts',(43.6738487993976,28.41999998,-171.649955087908));
#176437=CARTESIAN_POINT('Ctrl Pts',(43.6738487993977,28.9200050678815,-171.649949999974));
#176438=CARTESIAN_POINT('',(44.5079524583208,28.7904524382925,-171.649949999924));
#176439=CARTESIAN_POINT('Ctrl Pts',(45.342056117244,28.91999998,-171.64995));
#176440=CARTESIAN_POINT('Ctrl Pts',(45.2444206001237,28.8889220866335,-171.64995));
#176441=CARTESIAN_POINT('Ctrl Pts',(45.1451244228621,28.8633251672671,-171.649944548206));
#176442=CARTESIAN_POINT('Ctrl Pts',(44.9394280113021,28.8223952301246,-171.649950242377));
#176443=CARTESIAN_POINT('Ctrl Pts',(44.8330889161033,28.8076347675278,-171.649941035199));
#176444=CARTESIAN_POINT('Ctrl Pts',(44.6535686799005,28.7933450738466,-171.649939911887));
#176445=CARTESIAN_POINT('Ctrl Pts',(44.5807764535826,28.7904525215287,-171.649950037471));
#176446=CARTESIAN_POINT('Ctrl Pts',(44.5079556015787,28.7904524382943,-171.649949999926));
#176447=CARTESIAN_POINT('Ctrl Pts',(44.5079524583208,28.7904524382925,-171.649949999924));
#176448=CARTESIAN_POINT('Ctrl Pts',(44.4351590053695,28.7904524382925,-171.649949961984));
#176449=CARTESIAN_POINT('Ctrl Pts',(44.3623973025111,28.7933425641162,-171.649939477443));
#176450=CARTESIAN_POINT('Ctrl Pts',(44.1829231968703,28.8076227744787,-171.649940712955));
#176451=CARTESIAN_POINT('Ctrl Pts',(44.0766026663103,28.8223760301809,-171.649950205467));
#176452=CARTESIAN_POINT('Ctrl Pts',(43.8708751019518,28.8633007826367,-171.649945186571));
#176453=CARTESIAN_POINT('Ctrl Pts',(43.771530849245,28.8889072750242,-171.64995));
#176454=CARTESIAN_POINT('Ctrl Pts',(43.6738487993977,28.91999998,-171.64995));
#176455=CARTESIAN_POINT('Ctrl Pts',(45.342056117244,28.41999998,-171.14995));
#176456=CARTESIAN_POINT('Ctrl Pts',(45.222494788141,28.41999998,-171.149950023642));
#176457=CARTESIAN_POINT('Ctrl Pts',(45.102890712293,28.41999998,-171.153734801587));
#176458=CARTESIAN_POINT('Ctrl Pts',(44.9833706553288,28.41999998,-171.157527071728));
#176459=CARTESIAN_POINT('Ctrl Pts',(44.9639944908896,28.41999998,-171.158141861008));
#176460=CARTESIAN_POINT('Ctrl Pts',(44.9446205282342,28.41999998,-171.158756957286));
#176461=CARTESIAN_POINT('Ctrl Pts',(44.9252493015934,28.41999998,-171.15935636922));
#176462=CARTESIAN_POINT('Ctrl Pts',(44.7862513546676,28.41999998,-171.163657440581));
#176463=CARTESIAN_POINT('Ctrl Pts',(44.6473090850418,28.41999998,-171.167020207454));
#176464=CARTESIAN_POINT('Ctrl Pts',(44.5082302458003,28.41999998,-171.167024238765));
#176465=CARTESIAN_POINT('Ctrl Pts',(44.5082032664897,28.41999998,-171.167024239547));
#176466=CARTESIAN_POINT('Ctrl Pts',(44.5081762871737,28.41999998,-171.167024240203));
#176467=CARTESIAN_POINT('Ctrl Pts',(44.5081493078523,28.41999998,-171.167024240732));
#176468=CARTESIAN_POINT('Ctrl Pts',(44.3691292618367,28.41999998,-171.16702696589));
#176469=CARTESIAN_POINT('Ctrl Pts',(44.2300667116137,28.41999998,-171.163669289098));
#176470=CARTESIAN_POINT('Ctrl Pts',(44.0910473224682,28.41999998,-171.159368608161));
#176471=CARTESIAN_POINT('Ctrl Pts',(43.9520204566156,28.41999998,-171.155067695926));
#176472=CARTESIAN_POINT('Ctrl Pts',(43.8129841111527,28.41999998,-171.149950027538));
#176473=CARTESIAN_POINT('Ctrl Pts',(43.6738487993976,28.41999998,-171.14995));
#176474=CARTESIAN_POINT('Origin',(0.,-12.9675000200281,-171.64995));
#176475=CARTESIAN_POINT('Origin',(44.5079524583208,-57.4754524783487,-171.64995));
#176476=CARTESIAN_POINT('Ctrl Pts',(43.1572831724514,-54.58000002,-171.14995));
#176477=CARTESIAN_POINT('Ctrl Pts',(43.1572831724515,-54.58000002,-171.650098123446));
#176478=CARTESIAN_POINT('Ctrl Pts',(43.1572831724514,-55.0801481215052,
-171.649949978066));
#176479=CARTESIAN_POINT('Ctrl Pts',(43.3817682803707,-54.58000002,-171.149950056136));
#176480=CARTESIAN_POINT('Ctrl Pts',(43.3143913613983,-54.5800000199971,
-171.561466059479));
#176481=CARTESIAN_POINT('Ctrl Pts',(43.3271185292342,-54.98437233152,-171.649978738968));
#176482=CARTESIAN_POINT('Ctrl Pts',(43.6059648750607,-54.58000002,-171.185915645006));
#176483=CARTESIAN_POINT('Ctrl Pts',(43.5407821982003,-54.5800000200016,
-171.520211742113));
#176484=CARTESIAN_POINT('Ctrl Pts',(43.529947173783,-54.8943395876962,-171.649995064611));
#176485=CARTESIAN_POINT('Ctrl Pts',(44.0540062919344,-54.58000002,-171.260373422648));
#176486=CARTESIAN_POINT('Ctrl Pts',(44.0046317151096,-54.5800000199985,
-171.495876387334));
#176487=CARTESIAN_POINT('Ctrl Pts',(43.9881565230544,-54.764616113508,-171.65000835312));
#176488=CARTESIAN_POINT('Ctrl Pts',(44.2780419706102,-54.58000002,-171.296906912307));
#176489=CARTESIAN_POINT('Ctrl Pts',(44.2580491347888,-54.58000002,-171.503655116484));
#176490=CARTESIAN_POINT('Ctrl Pts',(44.2440095987557,-54.7260645641698,
-171.650006647718));
#176491=CARTESIAN_POINT('Ctrl Pts',(44.7276655629966,-54.58000002,-171.297869301671));
#176492=CARTESIAN_POINT('Ctrl Pts',(44.7466180387422,-54.58000002,-171.503788967852));
#176493=CARTESIAN_POINT('Ctrl Pts',(44.7601884828714,-54.724965517749,-171.65000663285));
#176494=CARTESIAN_POINT('Ctrl Pts',(44.9532637149971,-54.58000002,-171.261822611311));
#176495=CARTESIAN_POINT('Ctrl Pts',(45.0021140860299,-54.58000002,-171.495868847089));
#176496=CARTESIAN_POINT('Ctrl Pts',(45.0183788445838,-54.7626525929473,
-171.650008425802));
#176497=CARTESIAN_POINT('Ctrl Pts',(45.4045230317323,-54.58000002,-171.186802156157));
#176498=CARTESIAN_POINT('Ctrl Pts',(45.4698465063651,-54.58000002,-171.51943524171));
#176499=CARTESIAN_POINT('Ctrl Pts',(45.4809398893321,-54.8922510295818,
-171.649995402787));
#176500=CARTESIAN_POINT('Ctrl Pts',(45.6299507757146,-54.58000002,-171.149950055386));
#176501=CARTESIAN_POINT('Ctrl Pts',(45.6987517183233,-54.5800000199883,
-171.559908009068));
#176502=CARTESIAN_POINT('Ctrl Pts',(45.6855420836464,-54.9825427397822,
-171.649979290157));
#176503=CARTESIAN_POINT('Ctrl Pts',(45.8586217441902,-54.58000002,-171.14995));
#176504=CARTESIAN_POINT('Ctrl Pts',(45.8586217441902,-54.58000002,-171.650098123446));
#176505=CARTESIAN_POINT('Ctrl Pts',(45.8586217441902,-55.0801481215052,
-171.649949978066));
#176506=CARTESIAN_POINT('Ctrl Pts',(43.1572831724514,-55.08000002,-171.64995));
#176507=CARTESIAN_POINT('Ctrl Pts',(43.2591939625018,-55.0225379010838,
-171.64995));
#176508=CARTESIAN_POINT('Ctrl Pts',(43.3646678477779,-54.9716377963967,
-171.649923799797));
#176509=CARTESIAN_POINT('Ctrl Pts',(43.5936897926191,-54.8786129298122,
-171.649916554972));
#176510=CARTESIAN_POINT('Ctrl Pts',(43.7176454367752,-54.838244085283,-171.650015979223));
#176511=CARTESIAN_POINT('Ctrl Pts',(43.9338902925313,-54.7844427443934,
-171.649835982333));
#176512=CARTESIAN_POINT('Ctrl Pts',(44.0248533307643,-54.7666339585907,
-171.649693211769));
#176513=CARTESIAN_POINT('Ctrl Pts',(44.1415243890184,-54.7498576856655,
-171.649668212268));
#176514=CARTESIAN_POINT('Ctrl Pts',(44.1665445877735,-54.7466107515317,
-171.649670743825));
#176515=CARTESIAN_POINT('Ctrl Pts',(44.2185163631217,-54.7405922226087,
-171.6496923846));
#176516=CARTESIAN_POINT('Ctrl Pts',(44.2454709099305,-54.7378737484813,
-171.649712753147));
#176517=CARTESIAN_POINT('Ctrl Pts',(44.3345799964015,-54.7302149256914,
-171.649800202596));
#176518=CARTESIAN_POINT('Ctrl Pts',(44.3968571027421,-54.7269903094681,
-171.649898655));
#176519=CARTESIAN_POINT('Ctrl Pts',(44.4753229318754,-54.7255987179305,
-171.649945978707));
#176520=CARTESIAN_POINT('Ctrl Pts',(44.4914595253056,-54.7254545924529,
-171.649951370195));
#176521=CARTESIAN_POINT('Ctrl Pts',(44.5716245853701,-54.7254442044783,
-171.649943153781));
#176522=CARTESIAN_POINT('Ctrl Pts',(44.63563633795,-54.7276720035778,-171.649830605824));
#176523=CARTESIAN_POINT('Ctrl Pts',(44.8100535271275,-54.7398514986523,
-171.649607168589));
#176524=CARTESIAN_POINT('Ctrl Pts',(44.9200103914804,-54.754242207499,-171.649613940458));
#176525=CARTESIAN_POINT('Ctrl Pts',(45.1075048885201,-54.7904085846999,
-171.649838422852));
#176526=CARTESIAN_POINT('Ctrl Pts',(45.1854986877315,-54.809021075728,-171.649951780061));
#176527=CARTESIAN_POINT('Ctrl Pts',(45.3711482014372,-54.8619988092884,
-171.649947090133));
#176528=CARTESIAN_POINT('Ctrl Pts',(45.4777060174367,-54.8996370242685,
-171.649926384802));
#176529=CARTESIAN_POINT('Ctrl Pts',(45.6764516340787,-54.9839240727134,
-171.649937563492));
#176530=CARTESIAN_POINT('Ctrl Pts',(45.7689217186597,-55.0294229071028,
-171.64995));
#176531=CARTESIAN_POINT('Ctrl Pts',(45.8586217441902,-55.08000002,-171.64995));
#176532=CARTESIAN_POINT('Ctrl Pts',(43.1572831724514,-54.58000002,-171.14995));
#176533=CARTESIAN_POINT('Ctrl Pts',(43.2795244112609,-54.58000002,-171.149950030568));
#176534=CARTESIAN_POINT('Ctrl Pts',(43.4015975649155,-54.58000002,-171.160610139865));
#176535=CARTESIAN_POINT('Ctrl Pts',(43.5235528170182,-54.58000002,-171.176313109178));
#176536=CARTESIAN_POINT('Ctrl Pts',(43.6257700730182,-54.5800000200001,
-171.189474612324));
#176537=CARTESIAN_POINT('Ctrl Pts',(43.7279044984682,-54.5800000200001,
-171.20618048842));
#176538=CARTESIAN_POINT('Ctrl Pts',(43.829985527596,-54.5800000200001,-171.223144870208));
#176539=CARTESIAN_POINT('Ctrl Pts',(43.9984923413722,-54.5800000200002,
-171.251148250928));
#176540=CARTESIAN_POINT('Ctrl Pts',(44.1669616089357,-54.5800000200002,
-171.278751491315));
#176541=CARTESIAN_POINT('Ctrl Pts',(44.3358012503099,-54.5800000200001,
-171.290923113046));
#176542=CARTESIAN_POINT('Ctrl Pts',(44.3914319971457,-54.5800000200001,
-171.294933524354));
#176543=CARTESIAN_POINT('Ctrl Pts',(44.4471029574805,-54.5800000200001,
-171.297268373358));
#176544=CARTESIAN_POINT('Ctrl Pts',(44.5028287572163,-54.58000002,-171.297388261734));
#176545=CARTESIAN_POINT('Ctrl Pts',(44.5028370935956,-54.58000002,-171.297388279669));
#176546=CARTESIAN_POINT('Ctrl Pts',(44.5028454299759,-54.58000002,-171.297388297554));
#176547=CARTESIAN_POINT('Ctrl Pts',(44.5028537663573,-54.58000002,-171.29738831539));
#176548=CARTESIAN_POINT('Ctrl Pts',(44.7276220562719,-54.58000002,-171.297869208197));
#176549=CARTESIAN_POINT('Ctrl Pts',(44.9531763212381,-54.5800000200004,
-171.261837296445));
#176550=CARTESIAN_POINT('Ctrl Pts',(45.1787623634369,-54.5800000200001,
-171.22433455003));
#176551=CARTESIAN_POINT('Ctrl Pts',(45.1788060542272,-54.5800000200001,
-171.224327286617));
#176552=CARTESIAN_POINT('Ctrl Pts',(45.178849745033,-54.5800000200001,-171.224320023146));
#176553=CARTESIAN_POINT('Ctrl Pts',(45.1788934358544,-54.5800000200001,
-171.224312759618));
#176554=CARTESIAN_POINT('Ctrl Pts',(45.294603484892,-54.58000002,-171.205076152327));
#176555=CARTESIAN_POINT('Ctrl Pts',(45.4103612459223,-54.58000002,-171.185995253716));
#176556=CARTESIAN_POINT('Ctrl Pts',(45.526508841826,-54.58000002,-171.171982248345));
#176557=CARTESIAN_POINT('Ctrl Pts',(45.6241378685054,-54.58000002,-171.160203476132));
#176558=CARTESIAN_POINT('Ctrl Pts',(45.722042620539,-54.58000002,-171.152008348194));
#176559=CARTESIAN_POINT('Ctrl Pts',(45.8204240164971,-54.58000002,-171.150287040904));
#176560=CARTESIAN_POINT('Ctrl Pts',(45.8331484827202,-54.58000002,-171.150064410231));
#176561=CARTESIAN_POINT('Ctrl Pts',(45.8458809158954,-54.58000002,-171.149950003086));
#176562=CARTESIAN_POINT('Ctrl Pts',(45.8586217441902,-54.58000002,-171.14995));
#176563=CARTESIAN_POINT('Origin',(0.,-12.9675000200281,-171.64995));
#176564=CARTESIAN_POINT('',(44.5079524583208,-60.2254524783487,-171.64995));
#176565=CARTESIAN_POINT('Origin',(44.5079524583208,-57.4754524783487,-171.64995));
#176566=CARTESIAN_POINT('Origin',(44.5079524583208,-57.4754524783487,-171.64995));
#176567=CARTESIAN_POINT('Ctrl Pts',(41.5,-58.6035812240168,-171.14995));
#176568=CARTESIAN_POINT('Ctrl Pts',(41.5,-58.6035812240167,-171.650011780221));
#176569=CARTESIAN_POINT('Ctrl Pts',(42.0000617764046,-58.6035812240168,
-171.649949996184));
#176570=CARTESIAN_POINT('Ctrl Pts',(41.5,-58.415688549198,-171.149950044589));
#176571=CARTESIAN_POINT('Ctrl Pts',(41.5,-58.4568531764745,-171.58399675791));
#176572=CARTESIAN_POINT('Ctrl Pts',(41.9298643117037,-58.4475344566842,
-171.649958724212));
#176573=CARTESIAN_POINT('Ctrl Pts',(41.5,-58.227785502943,-171.167360442076));
#176574=CARTESIAN_POINT('Ctrl Pts',(41.5,-58.2676804549564,-171.547558090573));
#176575=CARTESIAN_POINT('Ctrl Pts',(41.8681695534326,-58.2705723212599,
-171.649964230513));
#176576=CARTESIAN_POINT('Ctrl Pts',(41.5,-57.8520667952971,-171.199054581264));
#176577=CARTESIAN_POINT('Ctrl Pts',(41.5,-57.8827900893765,-171.511616746682));
#176578=CARTESIAN_POINT('Ctrl Pts',(41.7820591277973,-57.8880263314597,
-171.649970496006));
#176579=CARTESIAN_POINT('Ctrl Pts',(41.5,-57.6641810084405,-171.212413163406));
#176580=CARTESIAN_POINT('Ctrl Pts',(41.4999999999974,-57.6764631965623,
-171.507283264427));
#176581=CARTESIAN_POINT('Ctrl Pts',(41.7580490411455,-57.6823964313123,
-171.649971475853));
#176582=CARTESIAN_POINT('Ctrl Pts',(41.5,-57.2881262594105,-171.212471328128));
#176583=CARTESIAN_POINT('Ctrl Pts',(41.5000000000026,-57.275950831087,-171.507256427632));
#176584=CARTESIAN_POINT('Ctrl Pts',(41.7579337455091,-57.2700461805852,
-171.649971481651));
#176585=CARTESIAN_POINT('Ctrl Pts',(41.5,-57.0999570266663,-171.199145438258));
#176586=CARTESIAN_POINT('Ctrl Pts',(41.5,-57.0692704467351,-171.511552982749));
#176587=CARTESIAN_POINT('Ctrl Pts',(41.7818539242554,-57.0640562802561,
-171.649970508384));
#176588=CARTESIAN_POINT('Ctrl Pts',(41.5,-56.7235644715492,-171.167401493624));
#176589=CARTESIAN_POINT('Ctrl Pts',(41.5,-56.6836417097802,-171.547472271891));
#176590=CARTESIAN_POINT('Ctrl Pts',(41.8680165447745,-56.6807474451005,
-171.649964244171));
#176591=CARTESIAN_POINT('Ctrl Pts',(41.5,-56.5353526996975,-171.149950046396));
#176592=CARTESIAN_POINT('Ctrl Pts',(41.4999999999999,-56.494149705945,-171.583952704407));
#176593=CARTESIAN_POINT('Ctrl Pts',(41.929815802996,-56.5034783375505,-171.649958730482));
#176594=CARTESIAN_POINT('Ctrl Pts',(41.5,-56.3473237326807,-171.14995));
#176595=CARTESIAN_POINT('Ctrl Pts',(41.5,-56.3473237326807,-171.650011780221));
#176596=CARTESIAN_POINT('Ctrl Pts',(42.0000617764046,-56.3473237326807,
-171.649949996184));
#176597=CARTESIAN_POINT('Ctrl Pts',(42.,-58.6035812240168,-171.64995));
#176598=CARTESIAN_POINT('Ctrl Pts',(41.9586127577212,-58.5115728992447,
-171.64995));
#176599=CARTESIAN_POINT('Ctrl Pts',(41.9223200866005,-58.4173567491321,
-171.649936040447));
#176600=CARTESIAN_POINT('Ctrl Pts',(41.8579031946499,-58.2180944893019,
-171.649932806722));
#176601=CARTESIAN_POINT('Ctrl Pts',(41.8306620008006,-58.1129431414185,
-171.649968769067));
#176602=CARTESIAN_POINT('Ctrl Pts',(41.7951274186659,-57.9323775711288,
-171.649917110529));
#176603=CARTESIAN_POINT('Ctrl Pts',(41.7836058362706,-57.8577298063977,
-171.649879920008));
#176604=CARTESIAN_POINT('Ctrl Pts',(41.7636999883713,-57.6806798505214,
-171.649872834512));
#176605=CARTESIAN_POINT('Ctrl Pts',(41.7579524619681,-57.5781054625682,
-171.649950538122));
#176606=CARTESIAN_POINT('Ctrl Pts',(41.7579524619681,-57.3728595819387,
-171.649949462193));
#176607=CARTESIAN_POINT('Ctrl Pts',(41.7636932451378,-57.2703453579385,
-171.649869923244));
#176608=CARTESIAN_POINT('Ctrl Pts',(41.7835828980498,-57.0933348984401,
-171.649877908044));
#176609=CARTESIAN_POINT('Ctrl Pts',(41.7951032511141,-57.0186677636545,
-171.649916441382));
#176610=CARTESIAN_POINT('Ctrl Pts',(41.8306429216695,-56.8380335332052,
-171.649969369358));
#176611=CARTESIAN_POINT('Ctrl Pts',(41.857894634129,-56.7328337987611,-171.64993233013));
#176612=CARTESIAN_POINT('Ctrl Pts',(41.9223259722371,-56.5335329279263,
-171.649935735269));
#176613=CARTESIAN_POINT('Ctrl Pts',(41.9586161144825,-56.4393245950086,
-171.64995));
#176614=CARTESIAN_POINT('Ctrl Pts',(42.,-56.3473237326807,-171.64995));
#176615=CARTESIAN_POINT('Ctrl Pts',(41.5,-58.6035812240168,-171.14995));
#176616=CARTESIAN_POINT('Ctrl Pts',(41.5,-58.4156574039305,-171.149950044596));
#176617=CARTESIAN_POINT('Ctrl Pts',(41.4999999999992,-58.2278101348557,
-171.167358426711));
#176618=CARTESIAN_POINT('Ctrl Pts',(41.5000000000009,-58.0399262281501,
-171.183208448531));
#176619=CARTESIAN_POINT('Ctrl Pts',(41.5000000000009,-58.0397839854562,
-171.183220448228));
#176620=CARTESIAN_POINT('Ctrl Pts',(41.5000000000009,-58.039641742701,-171.183232446501));
#176621=CARTESIAN_POINT('Ctrl Pts',(41.5000000000009,-58.0394994998845,
-171.183244443348));
#176622=CARTESIAN_POINT('Ctrl Pts',(41.5000000000023,-57.8789705149695,
-171.196783556844));
#176623=CARTESIAN_POINT('Ctrl Pts',(41.4999999999993,-57.7184422672226,
-171.208492413787));
#176624=CARTESIAN_POINT('Ctrl Pts',(41.500000000002,-57.5579169091166,-171.211623701819));
#176625=CARTESIAN_POINT('Ctrl Pts',(41.5000000000025,-57.5306624002125,
-171.21215534192));
#176626=CARTESIAN_POINT('Ctrl Pts',(41.5000000000032,-57.5034079726048,
-171.212439843791));
#176627=CARTESIAN_POINT('Ctrl Pts',(41.5000000000045,-57.4761536342535,
-171.212444366368));
#176628=CARTESIAN_POINT('Ctrl Pts',(41.5000000000045,-57.4759114394356,
-171.212444406558));
#176629=CARTESIAN_POINT('Ctrl Pts',(41.5000000000045,-57.4756692446243,
-171.212444424596));
#176630=CARTESIAN_POINT('Ctrl Pts',(41.5000000000045,-57.4754270498201,
-171.212444420506));
#176631=CARTESIAN_POINT('Ctrl Pts',(41.5000000000123,-57.3141767266989,
-171.21244169735));
#176632=CARTESIAN_POINT('Ctrl Pts',(41.5000000000007,-57.1529297994966,
-171.202628065339));
#176633=CARTESIAN_POINT('Ctrl Pts',(41.5000000000001,-56.991684015905,-171.189830777414));
#176634=CARTESIAN_POINT('Ctrl Pts',(41.5,-56.9650429029001,-171.187716402786));
#176635=CARTESIAN_POINT('Ctrl Pts',(41.5,-56.9384018139027,-171.185520466728));
#176636=CARTESIAN_POINT('Ctrl Pts',(41.5,-56.9117607329797,-171.183273657174));
#176637=CARTESIAN_POINT('Ctrl Pts',(41.5,-56.9116320467988,-171.18326280426));
#176638=CARTESIAN_POINT('Ctrl Pts',(41.5,-56.9115033606235,-171.183251950612));
#176639=CARTESIAN_POINT('Ctrl Pts',(41.5,-56.9113746744539,-171.183241096235));
#176640=CARTESIAN_POINT('Ctrl Pts',(41.5000000000001,-56.7724125203339,
-171.171519963662));
#176641=CARTESIAN_POINT('Ctrl Pts',(41.5,-56.6334506983205,-171.158942972401));
#176642=CARTESIAN_POINT('Ctrl Pts',(41.5,-56.494486471781,-171.153174108112));
#176643=CARTESIAN_POINT('Ctrl Pts',(41.5,-56.4454325541955,-171.151137717881));
#176644=CARTESIAN_POINT('Ctrl Pts',(41.5,-56.3963783401914,-171.149950012104));
#176645=CARTESIAN_POINT('Ctrl Pts',(41.5,-56.3473237326807,-171.14995));
#176646=CARTESIAN_POINT('Origin',(45.5612236321975,-62.7713643393447,-171.64995));
#176647=CARTESIAN_POINT('',(26.0394480946395,-65.5149709682656,-179.39995));
#176648=CARTESIAN_POINT('',(26.0394480946395,-65.5149709682656,-171.64995));
#176649=CARTESIAN_POINT('',(44.628608857647,-62.9024347982158,-179.39995));
#176650=CARTESIAN_POINT('',(44.628608857647,-62.9024347982158,-179.39995));
#176651=CARTESIAN_POINT('',(44.628608857647,-62.9024347982158,-171.64995));
#176652=CARTESIAN_POINT('Origin',(44.2110895547669,-59.9316305919911,-171.64995));
#176653=CARTESIAN_POINT('',(46.2674193015002,-62.1160087581289,-179.39995));
#176654=CARTESIAN_POINT('Origin',(44.2110895547669,-59.9316305919911,-179.39995));
#176655=CARTESIAN_POINT('',(46.2674193015002,-62.1160087581289,-171.64995));
#176656=CARTESIAN_POINT('Origin',(0.,-12.9675000200281,-171.64995));
#176657=CARTESIAN_POINT('',(49.148508738101,-59.2349193215281,-179.39995));
#176658=CARTESIAN_POINT('Origin',(0.,-12.9675000200281,-179.39995));
#176659=CARTESIAN_POINT('',(49.148508738101,-59.2349193215281,-171.64995));
#176660=CARTESIAN_POINT('Origin',(46.9641305719631,-57.1785895747948,-171.64995));
#176661=CARTESIAN_POINT('',(49.9349347781878,-57.596108877675,-179.39995));
#176662=CARTESIAN_POINT('Origin',(46.9641305719631,-57.1785895747948,-179.39995));
#176663=CARTESIAN_POINT('',(49.9349347781878,-57.596108877675,-171.64995));
#176664=CARTESIAN_POINT('Origin',(52.6124803109501,-38.5443824635529,-171.64995));
#176665=CARTESIAN_POINT('',(52.5050296388285,-39.3089337226171,-179.39995));
#176666=CARTESIAN_POINT('',(52.5050296388285,-39.3089337226171,-179.39995));
#176667=CARTESIAN_POINT('',(52.5050296388285,-39.3089337226171,-171.64995));
#176668=CARTESIAN_POINT('Origin',(57.4563699825363,-40.0047992274175,-179.64995));
#176669=CARTESIAN_POINT('',(52.9322463618642,-37.8758780299853,-179.39995));
#176670=CARTESIAN_POINT('',(52.9322463618642,-37.8758780299853,-179.64995));
#176671=CARTESIAN_POINT('Origin',(57.4563699825363,-40.0047992274175,-179.39995));
#176672=CARTESIAN_POINT('Origin',(0.,-12.9675000200281,-179.64995));
#176673=CARTESIAN_POINT('',(52.9322463618642,11.9408779899289,-179.39995));
#176674=CARTESIAN_POINT('',(52.9322463618642,11.9408779899289,-179.64995));
#176675=CARTESIAN_POINT('Origin',(0.,-12.9675000200281,-179.39995));
#176676=CARTESIAN_POINT('Origin',(57.4563699825364,14.0697991873612,-179.64995));
#176677=CARTESIAN_POINT('',(52.5050296388285,13.3739336825608,-179.39995));
#176678=CARTESIAN_POINT('Origin',(57.4563699825364,14.0697991873612,-179.39995));
#176679=CARTESIAN_POINT('',(52.5050296388285,13.3739336825608,-171.64995));
#176680=CARTESIAN_POINT('Origin',(52.6124803109502,12.6093824234965,-171.64995));
#176681=CARTESIAN_POINT('',(49.9349347781878,31.6611088376188,-179.39995));
#176682=CARTESIAN_POINT('',(49.9349347781878,31.6611088376188,-179.39995));
#176683=CARTESIAN_POINT('',(49.9349347781878,31.6611088376188,-171.64995));
#176684=CARTESIAN_POINT('Origin',(46.9641305719631,31.2435895347386,-171.64995));
#176685=CARTESIAN_POINT('',(49.1485087381009,33.2999192814719,-179.39995));
#176686=CARTESIAN_POINT('Origin',(46.9641305719631,31.2435895347386,-179.39995));
#176687=CARTESIAN_POINT('',(49.1485087381009,33.2999192814719,-171.64995));
#176688=CARTESIAN_POINT('Origin',(0.,-12.9675000200281,-171.64995));
#176689=CARTESIAN_POINT('',(46.2674193015002,36.1810087180727,-179.39995));
#176690=CARTESIAN_POINT('Origin',(0.,-12.9675000200281,-179.39995));
#176691=CARTESIAN_POINT('',(46.2674193015002,36.1810087180727,-171.64995));
#176692=CARTESIAN_POINT('Origin',(44.2110895547669,33.9966305519348,-171.64995));
#176693=CARTESIAN_POINT('',(44.628608857647,36.9674347581595,-179.39995));
#176694=CARTESIAN_POINT('Origin',(44.2110895547669,33.9966305519348,-179.39995));
#176695=CARTESIAN_POINT('',(44.628608857647,36.9674347581595,-171.64995));
#176696=CARTESIAN_POINT('Origin',(45.5612236321975,36.8363642992885,-171.64995));
#176697=CARTESIAN_POINT('',(26.3414337025898,39.5375296188,-179.39995));
#176698=CARTESIAN_POINT('',(26.3414337025898,39.5375296188,-177.84995));
#176699=CARTESIAN_POINT('',(26.3414337025898,39.5375296188,-171.64995));
#176700=CARTESIAN_POINT('',(38.43041344952,37.8385343144662,-177.84995));
#176701=CARTESIAN_POINT('',(45.5612236321975,36.8363642992885,-177.84995));
#176702=CARTESIAN_POINT('',(41.93041344952,37.3466413930079,-174.34995));
#176703=CARTESIAN_POINT('Ctrl Pts',(38.43041344952,37.8385343144662,-177.84995));
#176704=CARTESIAN_POINT('Ctrl Pts',(38.8886449769195,37.7741340731185,-177.849949999987));
#176705=CARTESIAN_POINT('Ctrl Pts',(39.3465310504406,37.7097823821472,-177.758854365991));
#176706=CARTESIAN_POINT('Ctrl Pts',(39.7698054627978,37.6502950429264,-177.58352836379));
#176707=CARTESIAN_POINT('Ctrl Pts',(40.193079875155,37.5908077037056,-177.408202361589));
#176708=CARTESIAN_POINT('Ctrl Pts',(40.5813269737971,37.5362431323916,-177.148783944032));
#176709=CARTESIAN_POINT('Ctrl Pts',(40.9052871836729,37.4907134940853,-176.824823734153));
#176710=CARTESIAN_POINT('Ctrl Pts',(41.2292473935486,37.445183855779,-176.500863524274));
#176711=CARTESIAN_POINT('Ctrl Pts',(41.4886658111382,37.4087249748338,-176.112616425556));
#176712=CARTESIAN_POINT('Ctrl Pts',(41.6639918133095,37.3840845121436,-175.689342013278));
#176713=CARTESIAN_POINT('Ctrl Pts',(41.8393178154807,37.3594440494534,-175.266067601));
#176714=CARTESIAN_POINT('Ctrl Pts',(41.9304134495165,37.3466413930083,-174.808181527339));
#176715=CARTESIAN_POINT('Ctrl Pts',(41.93041344952,37.3466413930079,-174.34995));
#176716=CARTESIAN_POINT('',(41.93041344952,37.3466413930079,-171.64995));
#176717=CARTESIAN_POINT('',(26.3414337025898,39.5375296188,-179.39995));
#176718=CARTESIAN_POINT('Ctrl Pts',(41.5,37.8417754273786,-174.34995));
#176719=CARTESIAN_POINT('Ctrl Pts',(41.5,37.4071320584705,-174.34995));
#176720=CARTESIAN_POINT('Ctrl Pts',(41.93041344952,37.3466413930079,-174.34995));
#176721=CARTESIAN_POINT('Ctrl Pts',(41.5,37.8417754273818,-174.742719880575));
#176722=CARTESIAN_POINT('Ctrl Pts',(41.4999999999921,37.4071320584705,-174.750729116851));
#176723=CARTESIAN_POINT('Ctrl Pts',(41.9304134495165,37.3466413930083,-174.808181527339));
#176724=CARTESIAN_POINT('Ctrl Pts',(41.4219180279654,37.8545780838243,-175.135193658002));
#176725=CARTESIAN_POINT('Ctrl Pts',(41.418170761701,37.4186324079233,-175.152286591264));
#176726=CARTESIAN_POINT('Ctrl Pts',(41.8393178154807,37.3594440494534,-175.266067601));
#176727=CARTESIAN_POINT('Ctrl Pts',(41.1213591671024,37.9038590092046,-175.860806936189));
#176728=CARTESIAN_POINT('Ctrl Pts',(41.1060831277358,37.4624934645027,-175.889590467068));
#176729=CARTESIAN_POINT('Ctrl Pts',(41.4886658111382,37.4087249748338,-176.112616425556));
#176730=CARTESIAN_POINT('Ctrl Pts',(40.8990005234543,37.9403178901501,-176.193590163665));
#176731=CARTESIAN_POINT('Ctrl Pts',(40.8743194488686,37.4950657253844,-176.226515658809));
#176732=CARTESIAN_POINT('Ctrl Pts',(41.2292473935486,37.445183855779,-176.500863524274));
#176733=CARTESIAN_POINT('Ctrl Pts',(40.343640163665,38.0313771667621,-176.748950523454));
#176734=CARTESIAN_POINT('Ctrl Pts',(40.3016108905592,37.5755546642088,-176.782638117262));
#176735=CARTESIAN_POINT('Ctrl Pts',(40.5813269737971,37.5362431323916,-177.148783944032));
#176736=CARTESIAN_POINT('Ctrl Pts',(40.0108569362568,38.0859417380754,-176.971309167074));
#176737=CARTESIAN_POINT('Ctrl Pts',(39.9585494594759,37.6237688040866,-177.001555340038));
#176738=CARTESIAN_POINT('Ctrl Pts',(40.193079875155,37.5908077037056,-177.408202361589));
#176739=CARTESIAN_POINT('Ctrl Pts',(39.2852436579338,38.204916416519,-177.271868027993));
#176740=CARTESIAN_POINT('Ctrl Pts',(39.218856185771,37.7277259142,-177.290648705564));
#176741=CARTESIAN_POINT('Ctrl Pts',(39.3465310504406,37.7097823821472,-177.758854365991));
#176742=CARTESIAN_POINT('Ctrl Pts',(38.8927698806272,38.2692681074913,-177.34995));
#176743=CARTESIAN_POINT('Ctrl Pts',(38.8208550398785,37.7836613274466,-177.358977353131));
#176744=CARTESIAN_POINT('Ctrl Pts',(38.8886449769195,37.7741340731185,-177.849949999987));
#176745=CARTESIAN_POINT('Ctrl Pts',(38.5,38.333668348837,-177.34995));
#176746=CARTESIAN_POINT('Ctrl Pts',(38.43041344952,37.8385343144661,-177.34995));
#176747=CARTESIAN_POINT('Ctrl Pts',(38.43041344952,37.8385343144662,-177.84995));
#176748=CARTESIAN_POINT('',(41.5,37.8417754273786,-174.34995));
#176749=CARTESIAN_POINT('Origin',(42.,37.8417754273786,-174.34995));
#176750=CARTESIAN_POINT('',(38.5,38.333668348837,-177.34995));
#176751=CARTESIAN_POINT('Origin',(38.5,38.333668348837,-177.84995));
#176752=CARTESIAN_POINT('Ctrl Pts',(41.5,37.8417754273786,-174.34995));
#176753=CARTESIAN_POINT('Ctrl Pts',(41.5,37.8417754273786,-174.476353976316));
#176754=CARTESIAN_POINT('Ctrl Pts',(41.4919114500808,37.8431014152902,-174.603274421342));
#176755=CARTESIAN_POINT('Ctrl Pts',(41.4757304211612,37.8457540208828,-174.729690050826));
#176756=CARTESIAN_POINT('Ctrl Pts',(41.4680748448541,37.8470090229366,-174.789499875202));
#176757=CARTESIAN_POINT('Ctrl Pts',(41.4586080657167,37.8485609393631,-174.849195979142));
#176758=CARTESIAN_POINT('Ctrl Pts',(41.4473309666377,37.8504096236584,-174.908666369613));
#176759=CARTESIAN_POINT('Ctrl Pts',(41.4297746293963,37.85328767986,-175.001250661341));
#176760=CARTESIAN_POINT('Ctrl Pts',(41.4078298483949,37.8568852355436,-175.093293139518));
#176761=CARTESIAN_POINT('Ctrl Pts',(41.3814995882027,37.8612023039407,-175.184367198324));
#176762=CARTESIAN_POINT('Ctrl Pts',(41.371452626058,37.862849588185,-175.219118758487));
#176763=CARTESIAN_POINT('Ctrl Pts',(41.360858123554,37.8645866920548,-175.253429957384));
#176764=CARTESIAN_POINT('Ctrl Pts',(41.3496247022485,37.8664286294454,-175.28762251975));
#176765=CARTESIAN_POINT('Ctrl Pts',(41.3385105141439,37.8682510162392,-175.321452157185));
#176766=CARTESIAN_POINT('Ctrl Pts',(41.3267707930063,37.8701760402071,-175.355165937406));
#176767=CARTESIAN_POINT('Ctrl Pts',(41.3142698257931,37.8722259837527,-175.389059282268));
#176768=CARTESIAN_POINT('Ctrl Pts',(41.306292887867,37.8735340643305,-175.410686817439));
#176769=CARTESIAN_POINT('Ctrl Pts',(41.2980050551031,37.8748931622609,-175.432387137017));
#176770=CARTESIAN_POINT('Ctrl Pts',(41.2893609525011,37.8763107253537,-175.454232639964));
#176771=CARTESIAN_POINT('Ctrl Pts',(41.2835806796571,37.8772586434694,-175.468840630321));
#176772=CARTESIAN_POINT('Ctrl Pts',(41.2776735291647,37.8782273521849,-175.48343068445));
#176773=CARTESIAN_POINT('Ctrl Pts',(41.2716385658268,37.8792170058608,-175.498000373649));
#176774=CARTESIAN_POINT('Ctrl Pts',(41.236613156753,37.8849607068411,-175.582559184651));
#176775=CARTESIAN_POINT('Ctrl Pts',(41.1972870501281,37.8914091716528,-175.666416279207));
#176776=CARTESIAN_POINT('Ctrl Pts',(41.153627526666,37.8985679655939,-175.749123315229));
#176777=CARTESIAN_POINT('Ctrl Pts',(41.1114124456556,37.905489916229,-175.829094051255));
#176778=CARTESIAN_POINT('Ctrl Pts',(41.06514597395,37.9130759664727,-175.907989464207));
#176779=CARTESIAN_POINT('Ctrl Pts',(41.0148201132632,37.9213276113521,-175.985363378084));
#176780=CARTESIAN_POINT('Ctrl Pts',(40.9626287142217,37.9298851379354,-176.06560547945));
#176781=CARTESIAN_POINT('Ctrl Pts',(40.9060697862906,37.9391587833669,-176.144214115591));
#176782=CARTESIAN_POINT('Ctrl Pts',(40.8451545165363,37.9491467133671,-176.220648295229));
#176783=CARTESIAN_POINT('Ctrl Pts',(40.7909989817862,37.9580262881009,-176.288600614708));
#176784=CARTESIAN_POINT('Ctrl Pts',(40.7333998072024,37.9674704968541,-176.354834221104));
#176785=CARTESIAN_POINT('Ctrl Pts',(40.6723886669702,37.9774741461908,-176.418927468631));
#176786=CARTESIAN_POINT('Ctrl Pts',(40.6647732100798,37.9787228093034,-176.426927636496));
#176787=CARTESIAN_POINT('Ctrl Pts',(40.6571046345291,37.9799801819804,-176.434894399285));
#176788=CARTESIAN_POINT('Ctrl Pts',(40.6493830370906,37.9812462483545,-176.442826888852));
#176789=CARTESIAN_POINT('Ctrl Pts',(40.6433862987247,37.9822294994059,-176.448987410026));
#176790=CARTESIAN_POINT('Ctrl Pts',(40.6368004697369,37.9833093402939,-176.455693039846));
#176791=CARTESIAN_POINT('Ctrl Pts',(40.6307040241344,37.9843089345486,-176.461844450969));
#176792=CARTESIAN_POINT('Ctrl Pts',(40.6273684653236,37.9848558442795,-176.46521008316));
#176793=CARTESIAN_POINT('Ctrl Pts',(40.624180151531,37.9853786095184,-176.468410535592));
#176794=CARTESIAN_POINT('Ctrl Pts',(40.6213203422155,37.9858475093267,-176.471270344904));
#176795=CARTESIAN_POINT('Ctrl Pts',(40.5709024849344,37.9941141176937,-176.521688202121));
#176796=CARTESIAN_POINT('Ctrl Pts',(40.5175232725426,38.0028663790502,-176.571427643008));
#176797=CARTESIAN_POINT('Ctrl Pts',(40.4611036304162,38.012117202431,-176.620119132926));
#176798=CARTESIAN_POINT('Ctrl Pts',(40.4062711116874,38.0211077937777,-176.667440897692));
#176799=CARTESIAN_POINT('Ctrl Pts',(40.348566681604,38.0305693139387,-176.713772847727));
#176800=CARTESIAN_POINT('Ctrl Pts',(40.2879492542279,38.0405084467926,-176.758738723489));
#176801=CARTESIAN_POINT('Ctrl Pts',(40.2508731893274,38.0465876215562,-176.786241667778));
#176802=CARTESIAN_POINT('Ctrl Pts',(40.2127079839217,38.0528453708976,-176.813232834678));
#176803=CARTESIAN_POINT('Ctrl Pts',(40.1734506493455,38.059282172562,-176.839618952926));
#176804=CARTESIAN_POINT('Ctrl Pts',(40.1114897149355,38.0694415542431,-176.881264891444));
#176805=CARTESIAN_POINT('Ctrl Pts',(40.0468039828495,38.0800477054872,-176.921407207624));
#176806=CARTESIAN_POINT('Ctrl Pts',(39.9794042488894,38.0910988561683,-176.959651363111));
#176807=CARTESIAN_POINT('Ctrl Pts',(39.9127899593656,38.1020212219966,-176.997449839404));
#176808=CARTESIAN_POINT('Ctrl Pts',(39.8435235796991,38.1133784359477,-177.033394563102));
#176809=CARTESIAN_POINT('Ctrl Pts',(39.7716539135189,38.1251624959684,-177.067065073469));
#176810=CARTESIAN_POINT('Ctrl Pts',(39.7312690241559,38.1317841763723,-177.085985153501));
#176811=CARTESIAN_POINT('Ctrl Pts',(39.6900628025815,38.1385405259433,-177.104186447972));
#176812=CARTESIAN_POINT('Ctrl Pts',(39.6480502970953,38.1454290772972,-177.121588597534));
#176813=CARTESIAN_POINT('Ctrl Pts',(39.6400227671394,38.1467453056846,-177.124913709314));
#176814=CARTESIAN_POINT('Ctrl Pts',(39.6319659013663,38.1480663440989,-177.128209611011));
#176815=CARTESIAN_POINT('Ctrl Pts',(39.6238797774804,38.1493921797995,-177.131475878803));
#176816=CARTESIAN_POINT('Ctrl Pts',(39.6206230494417,38.1499261669559,-177.132791384978));
#176817=CARTESIAN_POINT('Ctrl Pts',(39.6173615800294,38.1504609315351,-177.134102082276));
#176818=CARTESIAN_POINT('Ctrl Pts',(39.6140953721306,38.1509963995422,-177.135407943764));
#176819=CARTESIAN_POINT('Ctrl Pts',(39.6108291642318,38.1515318675494,-177.136713805253));
#176820=CARTESIAN_POINT('Ctrl Pts',(39.6061167246918,38.1523044534494,-177.138585218931));
#176821=CARTESIAN_POINT('Ctrl Pts',(39.6042825755168,38.152605166686,-177.139310978034));
#176822=CARTESIAN_POINT('Ctrl Pts',(39.5690593443383,38.1583801014609,-177.153248547029));
#176823=CARTESIAN_POINT('Ctrl Pts',(39.530961535174,38.1646266368639,-177.167548422363));
#176824=CARTESIAN_POINT('Ctrl Pts',(39.4899041451713,38.1713585854016,-177.181880372341));
#176825=CARTESIAN_POINT('Ctrl Pts',(39.4495809627956,38.177970150058,-177.195956031625));
#176826=CARTESIAN_POINT('Ctrl Pts',(39.4064025243435,38.1850500171143,-177.210062601644));
#176827=CARTESIAN_POINT('Ctrl Pts',(39.3603028130147,38.1926088913928,-177.223839844921));
#176828=CARTESIAN_POINT('Ctrl Pts',(39.3156809756124,38.1999254417415,-177.237175414528));
#176829=CARTESIAN_POINT('Ctrl Pts',(39.26832167597,38.2076908595149,-177.250202308661));
#176830=CARTESIAN_POINT('Ctrl Pts',(39.2181864360695,38.2159113437581,-177.262550300708));
#176831=CARTESIAN_POINT('Ctrl Pts',(39.1970979178763,38.2193691477272,-177.267744269171));
#176832=CARTESIAN_POINT('Ctrl Pts',(39.1755185545334,38.2229074170752,-177.272817588752));
#176833=CARTESIAN_POINT('Ctrl Pts',(39.1534469930419,38.2265263653629,-177.277740366434));
#176834=CARTESIAN_POINT('Ctrl Pts',(39.1037587962994,38.2346734561155,-177.288822679123));
#176835=CARTESIAN_POINT('Ctrl Pts',(39.0515724039289,38.2432301617833,-177.299144914683));
#176836=CARTESIAN_POINT('Ctrl Pts',(38.9968918500243,38.2521958209189,-177.308339389731));
#176837=CARTESIAN_POINT('Ctrl Pts',(38.9435492322889,38.2609421062775,-177.317308892283));
#176838=CARTESIAN_POINT('Ctrl Pts',(38.8878326440064,38.2700776380719,-177.325205101624));
#176839=CARTESIAN_POINT('Ctrl Pts',(38.8297783760627,38.2795964658924,-177.331651494106));
#176840=CARTESIAN_POINT('Ctrl Pts',(38.7739147618162,38.2887561046972,-177.337854634644));
#176841=CARTESIAN_POINT('Ctrl Pts',(38.7158863278997,38.2982706966594,-177.342715195092));
#176842=CARTESIAN_POINT('Ctrl Pts',(38.6557601433083,38.3081292448576,-177.345865997974));
#176843=CARTESIAN_POINT('Ctrl Pts',(38.6052967544591,38.3164034394467,-177.348510439695));
#176844=CARTESIAN_POINT('Ctrl Pts',(38.5533561382533,38.3249198465959,-177.34995));
#176845=CARTESIAN_POINT('Ctrl Pts',(38.5,38.333668348837,-177.34995));
#176846=CARTESIAN_POINT('Origin',(42.,37.8417754273786,-171.64995));
#176847=CARTESIAN_POINT('',(41.5,37.8417754273786,-172.64995));
#176848=CARTESIAN_POINT('Origin',(42.,37.8417754273786,-172.64995));
#176849=CARTESIAN_POINT('',(41.5,37.8417754273786,-92.34995));
#176850=CARTESIAN_POINT('Ctrl Pts',(41.5,36.3270340686007,-171.14995));
#176851=CARTESIAN_POINT('Ctrl Pts',(41.5,36.3270340686007,-171.64995));
#176852=CARTESIAN_POINT('Ctrl Pts',(42.,36.3270340686007,-171.64995));
#176853=CARTESIAN_POINT('Ctrl Pts',(41.5,36.5253489879757,-171.149950000016));
#176854=CARTESIAN_POINT('Ctrl Pts',(41.5,36.4592824973649,-171.640924254979));
#176855=CARTESIAN_POINT('Ctrl Pts',(41.9908895000013,36.460524412126,-171.64995));
#176856=CARTESIAN_POINT('Ctrl Pts',(41.5,36.7235144279567,-171.18899099047));
#176857=CARTESIAN_POINT('Ctrl Pts',(41.5,36.5965520755147,-171.658003579003));
#176858=CARTESIAN_POINT('Ctrl Pts',(41.9817858670191,36.5939141376228,-171.675977326981));
#176859=CARTESIAN_POINT('Ctrl Pts',(41.5,37.0898865538897,-171.339270411997));
#176860=CARTESIAN_POINT('Ctrl Pts',(41.5,36.8549873364184,-171.746711574348));
#176861=CARTESIAN_POINT('Ctrl Pts',(41.9649548930127,36.840527660716,-171.776163607997));
#176862=CARTESIAN_POINT('Ctrl Pts',(41.5,37.2579134125323,-171.450449746589));
#176863=CARTESIAN_POINT('Ctrl Pts',(41.4999999999986,36.9765510525756,-171.817687494207));
#176864=CARTESIAN_POINT('Ctrl Pts',(41.9572358131754,36.9536304124011,-171.850283164392));
#176865=CARTESIAN_POINT('Ctrl Pts',(41.5,37.5383224977403,-171.728129909852));
#176866=CARTESIAN_POINT('Ctrl Pts',(41.5000000000014,37.1809962719461,-172.003556970024));
#176867=CARTESIAN_POINT('Ctrl Pts',(41.9443539433771,37.1423802312719,-172.035403273234));
#176868=CARTESIAN_POINT('Ctrl Pts',(41.5,37.6505944553831,-171.894521542842));
#176869=CARTESIAN_POINT('Ctrl Pts',(41.5,37.2645653642152,-172.118296873734));
#176870=CARTESIAN_POINT('Ctrl Pts',(41.9391962191204,37.2179530739059,-172.146331028561));
#176871=CARTESIAN_POINT('Ctrl Pts',(41.5,37.8023507586648,-172.257328160063));
#176872=CARTESIAN_POINT('Ctrl Pts',(41.5,37.3773763733446,-172.371853931892));
#176873=CARTESIAN_POINT('Ctrl Pts',(41.9322246014265,37.3201037397322,-172.388202106709));
#176874=CARTESIAN_POINT('Ctrl Pts',(41.5,37.8417754273637,-172.453565067926));
#176875=CARTESIAN_POINT('Ctrl Pts',(41.5,37.4071320584576,-172.511015867074));
#176876=CARTESIAN_POINT('Ctrl Pts',(41.9304134495219,37.3466413930076,-172.51902671195));
#176877=CARTESIAN_POINT('Ctrl Pts',(41.5,37.8417754273786,-172.64995));
#176878=CARTESIAN_POINT('Ctrl Pts',(41.5,37.4071320584705,-172.64995));
#176879=CARTESIAN_POINT('Ctrl Pts',(41.93041344952,37.3466413930079,-172.64995));
#176880=CARTESIAN_POINT('',(41.5,36.3270340686007,-171.14995));
#176881=CARTESIAN_POINT('Origin',(42.,36.3270340686007,-171.14995));
#176882=CARTESIAN_POINT('Ctrl Pts',(41.5,36.3270340686007,-171.14995));
#176883=CARTESIAN_POINT('Ctrl Pts',(41.5,36.5253489879757,-171.149950000016));
#176884=CARTESIAN_POINT('Ctrl Pts',(41.5,36.7235144279567,-171.18899099047));
#176885=CARTESIAN_POINT('Ctrl Pts',(41.5,37.0898865538897,-171.339270411997));
#176886=CARTESIAN_POINT('Ctrl Pts',(41.5,37.2579134125323,-171.450449746589));
#176887=CARTESIAN_POINT('Ctrl Pts',(41.5,37.5383224977403,-171.728129909852));
#176888=CARTESIAN_POINT('Ctrl Pts',(41.5,37.6505944553831,-171.894521542842));
#176889=CARTESIAN_POINT('Ctrl Pts',(41.5,37.8023507586648,-172.257328160063));
#176890=CARTESIAN_POINT('Ctrl Pts',(41.5,37.8417754273637,-172.453565067926));
#176891=CARTESIAN_POINT('Ctrl Pts',(41.5,37.8417754273786,-172.64995));
#176892=CARTESIAN_POINT('Origin',(42.,58.91999998,-171.14995));
#176893=CARTESIAN_POINT('',(41.5,32.6685811839606,-171.14995));
#176894=CARTESIAN_POINT('Origin',(42.,32.6685811839606,-171.14995));
#176895=CARTESIAN_POINT('',(41.5,36.3973044859519,-171.14995));
#176896=CARTESIAN_POINT('Ctrl Pts',(41.5,30.4123236926243,-171.14995));
#176897=CARTESIAN_POINT('Ctrl Pts',(41.5,30.4123236926244,-171.650011780222));
#176898=CARTESIAN_POINT('Ctrl Pts',(42.0000617764046,30.4123236926243,-171.649949996184));
#176899=CARTESIAN_POINT('Ctrl Pts',(41.5,30.6002163674433,-171.149950044589));
#176900=CARTESIAN_POINT('Ctrl Pts',(41.5,30.5590517401679,-171.583996757915));
#176901=CARTESIAN_POINT('Ctrl Pts',(41.929864311704,30.5683704599569,-171.649958724212));
#176902=CARTESIAN_POINT('Ctrl Pts',(41.5,30.7881194136978,-171.167360442076));
#176903=CARTESIAN_POINT('Ctrl Pts',(41.5,30.7482244616852,-171.547558090571));
#176904=CARTESIAN_POINT('Ctrl Pts',(41.8681695534321,30.7453325953812,-171.649964230513));
#176905=CARTESIAN_POINT('Ctrl Pts',(41.5,31.1638381213445,-171.199054581264));
#176906=CARTESIAN_POINT('Ctrl Pts',(41.5,31.1331148272644,-171.511616746684));
#176907=CARTESIAN_POINT('Ctrl Pts',(41.782059127798,31.1278785851814,-171.649970496006));
#176908=CARTESIAN_POINT('Ctrl Pts',(41.5,31.3517239082014,-171.212413163406));
#176909=CARTESIAN_POINT('Ctrl Pts',(41.5000000000007,31.3394417200798,-171.507283264433));
#176910=CARTESIAN_POINT('Ctrl Pts',(41.7580490411456,31.3335084853296,-171.649971475853));
#176911=CARTESIAN_POINT('Ctrl Pts',(41.5,31.72777865723,-171.212471328128));
#176912=CARTESIAN_POINT('Ctrl Pts',(41.4999999999994,31.739954085554,-171.507256427626));
#176913=CARTESIAN_POINT('Ctrl Pts',(41.7579337455091,31.7458587360553,-171.649971481651));
#176914=CARTESIAN_POINT('Ctrl Pts',(41.5,31.9159478899749,-171.199145438258));
#176915=CARTESIAN_POINT('Ctrl Pts',(41.5000000000001,31.9466344699074,-171.511552982749));
#176916=CARTESIAN_POINT('Ctrl Pts',(41.7818539242555,31.9518486363857,-171.649970508384));
#176917=CARTESIAN_POINT('Ctrl Pts',(41.5,32.2923404450921,-171.167401493624));
#176918=CARTESIAN_POINT('Ctrl Pts',(41.5,32.3322632068598,-171.547472271891));
#176919=CARTESIAN_POINT('Ctrl Pts',(41.8680165447745,32.3351574715402,-171.649964244171));
#176920=CARTESIAN_POINT('Ctrl Pts',(41.5,32.4805522169437,-171.149950046396));
#176921=CARTESIAN_POINT('Ctrl Pts',(41.5,32.5217552106974,-171.583952704406));
#176922=CARTESIAN_POINT('Ctrl Pts',(41.9298158029953,32.5124265790917,-171.649958730482));
#176923=CARTESIAN_POINT('Ctrl Pts',(41.5,32.6685811839606,-171.14995));
#176924=CARTESIAN_POINT('Ctrl Pts',(41.5,32.6685811839606,-171.650011780222));
#176925=CARTESIAN_POINT('Ctrl Pts',(42.0000617764046,32.6685811839606,-171.649949996184));
#176926=CARTESIAN_POINT('',(41.5,30.4123236926243,-171.14995));
#176927=CARTESIAN_POINT('Origin',(42.,30.4123236926243,-171.14995));
#176928=CARTESIAN_POINT('Ctrl Pts',(42.,30.4123236926244,-171.64995));
#176929=CARTESIAN_POINT('Ctrl Pts',(41.9586127577213,30.5043320173964,-171.64995));
#176930=CARTESIAN_POINT('Ctrl Pts',(41.9223200866006,30.5985481675088,-171.649936040447));
#176931=CARTESIAN_POINT('Ctrl Pts',(41.8579031946499,30.7978104273391,-171.649932806722));
#176932=CARTESIAN_POINT('Ctrl Pts',(41.8306620008007,30.9029617752221,-171.649968769066));
#176933=CARTESIAN_POINT('Ctrl Pts',(41.7951274186661,31.0835273455115,-171.649917110529));
#176934=CARTESIAN_POINT('Ctrl Pts',(41.7836058362707,31.1581751102427,-171.649879920008));
#176935=CARTESIAN_POINT('Ctrl Pts',(41.7636999883716,31.3352250661168,-171.649872834512));
#176936=CARTESIAN_POINT('Ctrl Pts',(41.7579524619681,31.4377994540704,-171.649950538122));
#176937=CARTESIAN_POINT('Ctrl Pts',(41.7579524619681,31.6430453346997,-171.649949462193));
#176938=CARTESIAN_POINT('Ctrl Pts',(41.7636932451375,31.7455595586994,-171.649869923244));
#176939=CARTESIAN_POINT('Ctrl Pts',(41.7835828980497,31.9225700182006,-171.649877908044));
#176940=CARTESIAN_POINT('Ctrl Pts',(41.795103251114,31.9972371529861,-171.649916441382));
#176941=CARTESIAN_POINT('Ctrl Pts',(41.8306429216694,32.1778713834354,-171.649969369358));
#176942=CARTESIAN_POINT('Ctrl Pts',(41.8578946341289,32.2830711178797,-171.64993233013));
#176943=CARTESIAN_POINT('Ctrl Pts',(41.922325972237,32.4823719887145,-171.649935735269));
#176944=CARTESIAN_POINT('Ctrl Pts',(41.9586161144823,32.5765803216321,-171.64995));
#176945=CARTESIAN_POINT('Ctrl Pts',(42.,32.6685811839606,-171.64995));
#176946=CARTESIAN_POINT('Ctrl Pts',(41.5,30.4123236926243,-171.14995));
#176947=CARTESIAN_POINT('Ctrl Pts',(41.5,30.6002475127106,-171.149950044596));
#176948=CARTESIAN_POINT('Ctrl Pts',(41.4999999999992,30.7880947817855,-171.167358426711));
#176949=CARTESIAN_POINT('Ctrl Pts',(41.5000000000009,30.9759786884911,-171.183208448531));
#176950=CARTESIAN_POINT('Ctrl Pts',(41.5000000000009,30.976120931185,-171.183220448228));
#176951=CARTESIAN_POINT('Ctrl Pts',(41.5000000000009,30.9762631739402,-171.183232446501));
#176952=CARTESIAN_POINT('Ctrl Pts',(41.5000000000009,30.9764054167567,-171.183244443348));
#176953=CARTESIAN_POINT('Ctrl Pts',(41.5000000000023,31.1369344018913,-171.196783556862));
#176954=CARTESIAN_POINT('Ctrl Pts',(41.4999999999993,31.2974626498578,-171.208492413819));
#176955=CARTESIAN_POINT('Ctrl Pts',(41.500000000002,31.4579880081833,-171.211623701832));
#176956=CARTESIAN_POINT('Ctrl Pts',(41.5000000000025,31.4852425168678,-171.212155341924));
#176957=CARTESIAN_POINT('Ctrl Pts',(41.5000000000032,31.512496944256,-171.212439843791));
#176958=CARTESIAN_POINT('Ctrl Pts',(41.5000000000045,31.5397512823877,-171.212444366369));
#176959=CARTESIAN_POINT('Ctrl Pts',(41.5000000000045,31.5399934772056,-171.212444406558));
#176960=CARTESIAN_POINT('Ctrl Pts',(41.5000000000045,31.5402356720169,-171.212444424596));
#176961=CARTESIAN_POINT('Ctrl Pts',(41.5000000000045,31.5404778668211,-171.212444420506));
#176962=CARTESIAN_POINT('Ctrl Pts',(41.5000000000123,31.7017281895742,-171.21244169735));
#176963=CARTESIAN_POINT('Ctrl Pts',(41.5000000000007,31.8629751164084,-171.202628065384));
#176964=CARTESIAN_POINT('Ctrl Pts',(41.5000000000001,32.0242208996319,-171.189830777502));
#176965=CARTESIAN_POINT('Ctrl Pts',(41.5,32.0508620130049,-171.187716402846));
#176966=CARTESIAN_POINT('Ctrl Pts',(41.5,32.0775031023704,-171.185520466759));
#176967=CARTESIAN_POINT('Ctrl Pts',(41.5,32.1041441836616,-171.183273657174));
#176968=CARTESIAN_POINT('Ctrl Pts',(41.5,32.1042728698425,-171.18326280426));
#176969=CARTESIAN_POINT('Ctrl Pts',(41.5,32.1044015560177,-171.183251950612));
#176970=CARTESIAN_POINT('Ctrl Pts',(41.5,32.1045302421874,-171.183241096235));
#176971=CARTESIAN_POINT('Ctrl Pts',(41.5000000000001,32.2434923963672,-171.171519963657));
#176972=CARTESIAN_POINT('Ctrl Pts',(41.5,32.3824542184406,-171.15894297239));
#176973=CARTESIAN_POINT('Ctrl Pts',(41.5,32.5214184450399,-171.153174108105));
#176974=CARTESIAN_POINT('Ctrl Pts',(41.5,32.5704723625655,-171.151137717878));
#176975=CARTESIAN_POINT('Ctrl Pts',(41.5,32.6195265765098,-171.149950012104));
#176976=CARTESIAN_POINT('Ctrl Pts',(41.5,32.6685811839606,-171.14995));
#176977=CARTESIAN_POINT('Origin',(42.,58.91999998,-171.14995));
#176978=CARTESIAN_POINT('',(41.5,36.3973044859519,-171.14995));
#176979=CARTESIAN_POINT('Origin',(42.,28.91999998,-92.34995));
#176980=CARTESIAN_POINT('',(42.,28.41999998,-95.34995));
#176981=CARTESIAN_POINT('',(42.,28.41999998,-95.34995));
#176982=CARTESIAN_POINT('',(41.5,28.91999998,-95.34995));
#176983=CARTESIAN_POINT('',(41.5,28.91999998,-171.64995));
#176984=CARTESIAN_POINT('Origin',(42.,28.91999998,-95.34995));
#176985=CARTESIAN_POINT('Ctrl Pts',(37.,28.41999998,-91.34995));
#176986=CARTESIAN_POINT('Ctrl Pts',(37.,28.41999998,-92.34995));
#176987=CARTESIAN_POINT('Ctrl Pts',(37.,29.41999998,-92.34995));
#176988=CARTESIAN_POINT('Ctrl Pts',(37.5,28.41999998,-91.34995));
#176989=CARTESIAN_POINT('Ctrl Pts',(37.5,28.41999998,-92.34995));
#176990=CARTESIAN_POINT('Ctrl Pts',(37.5,29.41999998,-92.34995));
#176991=CARTESIAN_POINT('Ctrl Pts',(37.5,28.91999998,-91.34995));
#176992=CARTESIAN_POINT('Ctrl Pts',(37.5,28.91999998,-91.84995));
#176993=CARTESIAN_POINT('Ctrl Pts',(37.5,29.41999998,-91.84995));
#176994=CARTESIAN_POINT('',(37.5,29.41999998,-91.84995));
#176995=CARTESIAN_POINT('Origin',(37.5,29.41999998,-91.34995));
#176996=CARTESIAN_POINT('',(37.,29.41999998,-92.34995));
#176997=CARTESIAN_POINT('Origin',(37.,29.41999998,-91.84995));
#176998=CARTESIAN_POINT('Origin',(37.,29.41999998,-91.34995));
#176999=CARTESIAN_POINT('Origin',(60.,28.41999998,-55.24995));
#177000=CARTESIAN_POINT('',(30.5,28.41999998,-91.34995));
#177001=CARTESIAN_POINT('Ctrl Pts',(31.,29.41999998,-92.34995));
#177002=CARTESIAN_POINT('Ctrl Pts',(31.,28.41999998,-92.34995));
#177003=CARTESIAN_POINT('Ctrl Pts',(31.,28.41999998,-91.34995));
#177004=CARTESIAN_POINT('Ctrl Pts',(30.5,29.41999998,-92.34995));
#177005=CARTESIAN_POINT('Ctrl Pts',(30.5,28.41999998,-92.34995));
#177006=CARTESIAN_POINT('Ctrl Pts',(30.5,28.41999998,-91.34995));
#177007=CARTESIAN_POINT('Ctrl Pts',(30.5,29.41999998,-91.84995));
#177008=CARTESIAN_POINT('Ctrl Pts',(30.5,28.91999998,-91.84995));
#177009=CARTESIAN_POINT('Ctrl Pts',(30.5,28.91999998,-91.34995));
#177010=CARTESIAN_POINT('',(31.,29.41999998,-92.34995));
#177011=CARTESIAN_POINT('Origin',(31.,29.41999998,-91.34995));
#177012=CARTESIAN_POINT('',(30.5,29.41999998,-91.84995));
#177013=CARTESIAN_POINT('Origin',(31.,29.41999998,-91.84995));
#177014=CARTESIAN_POINT('Origin',(30.5,29.41999998,-91.34995));
#177015=CARTESIAN_POINT('Origin',(30.,46.41999998,-92.34995));
#177016=CARTESIAN_POINT('',(30.5,46.41999998,-91.84995));
#177017=CARTESIAN_POINT('',(30.5,46.41999998,-58.24995));
#177018=CARTESIAN_POINT('',(30.,46.91999998,-91.84995));
#177019=CARTESIAN_POINT('Origin',(30.,46.41999998,-91.84995));
#177020=CARTESIAN_POINT('',(30.,46.91999998,-92.34995));
#177021=CARTESIAN_POINT('Origin',(-39.,46.91999998,-129.34995));
#177022=CARTESIAN_POINT('',(29.5,46.91999998,-91.84995));
#177023=CARTESIAN_POINT('',(-39.,46.91999998,-91.84995));
#177024=CARTESIAN_POINT('',(29.5,46.91999998,-58.24995));
#177025=CARTESIAN_POINT('Origin',(29.5,46.41999998,-92.34995));
#177026=CARTESIAN_POINT('',(29.,46.41999998,-91.84995));
#177027=CARTESIAN_POINT('Origin',(29.5,46.41999998,-91.84995));
#177028=CARTESIAN_POINT('',(29.,46.41999998,-92.34995));
#177029=CARTESIAN_POINT('Ctrl Pts',(28.5,28.41999998,-91.34995));
#177030=CARTESIAN_POINT('Ctrl Pts',(28.5,28.41999998,-92.34995));
#177031=CARTESIAN_POINT('Ctrl Pts',(28.5,29.41999998,-92.34995));
#177032=CARTESIAN_POINT('Ctrl Pts',(29.,28.41999998,-91.34995));
#177033=CARTESIAN_POINT('Ctrl Pts',(29.,28.41999998,-92.34995));
#177034=CARTESIAN_POINT('Ctrl Pts',(29.,29.41999998,-92.34995));
#177035=CARTESIAN_POINT('Ctrl Pts',(29.,28.91999998,-91.34995));
#177036=CARTESIAN_POINT('Ctrl Pts',(29.,28.91999998,-91.84995));
#177037=CARTESIAN_POINT('Ctrl Pts',(29.,29.41999998,-91.84995));
#177038=CARTESIAN_POINT('',(29.,29.41999998,-91.84995));
#177039=CARTESIAN_POINT('Origin',(29.,29.41999998,-91.34995));
#177040=CARTESIAN_POINT('',(28.5,29.41999998,-92.34995));
#177041=CARTESIAN_POINT('Origin',(28.5,29.41999998,-91.84995));
#177042=CARTESIAN_POINT('Origin',(28.5,29.41999998,-91.34995));
#177043=CARTESIAN_POINT('Origin',(60.,28.41999998,-55.24995));
#177044=CARTESIAN_POINT('',(22.,28.4199999800001,-91.34995));
#177045=CARTESIAN_POINT('Ctrl Pts',(22.5,29.41999998,-92.34995));
#177046=CARTESIAN_POINT('Ctrl Pts',(22.5,28.41999998,-92.34995));
#177047=CARTESIAN_POINT('Ctrl Pts',(22.5,28.41999998,-91.34995));
#177048=CARTESIAN_POINT('Ctrl Pts',(22.,29.41999998,-92.34995));
#177049=CARTESIAN_POINT('Ctrl Pts',(22.,28.41999998,-92.34995));
#177050=CARTESIAN_POINT('Ctrl Pts',(22.,28.41999998,-91.34995));
#177051=CARTESIAN_POINT('Ctrl Pts',(22.,29.41999998,-91.84995));
#177052=CARTESIAN_POINT('Ctrl Pts',(22.,28.91999998,-91.84995));
#177053=CARTESIAN_POINT('Ctrl Pts',(22.,28.91999998,-91.34995));
#177054=CARTESIAN_POINT('',(22.5,29.41999998,-92.34995));
#177055=CARTESIAN_POINT('Origin',(22.5,29.41999998,-91.34995));
#177056=CARTESIAN_POINT('',(22.,29.41999998,-91.84995));
#177057=CARTESIAN_POINT('Origin',(22.5,29.41999998,-91.84995));
#177058=CARTESIAN_POINT('Origin',(22.,29.41999998,-91.34995));
#177059=CARTESIAN_POINT('Origin',(21.5,46.41999998,-92.34995));
#177060=CARTESIAN_POINT('',(22.,46.41999998,-91.84995));
#177061=CARTESIAN_POINT('',(22.,46.41999998,-58.24995));
#177062=CARTESIAN_POINT('',(21.5,46.91999998,-91.84995));
#177063=CARTESIAN_POINT('Origin',(21.5,46.41999998,-91.84995));
#177064=CARTESIAN_POINT('',(21.5,46.91999998,-92.34995));
#177065=CARTESIAN_POINT('Origin',(-39.,46.91999998,-129.34995));
#177066=CARTESIAN_POINT('',(21.,46.91999998,-91.84995));
#177067=CARTESIAN_POINT('',(-39.,46.91999998,-91.84995));
#177068=CARTESIAN_POINT('',(21.,46.91999998,-58.24995));
#177069=CARTESIAN_POINT('Origin',(21.,46.41999998,-92.34995));
#177070=CARTESIAN_POINT('',(20.5,46.41999998,-91.84995));
#177071=CARTESIAN_POINT('Origin',(21.,46.41999998,-91.84995));
#177072=CARTESIAN_POINT('',(20.5,46.41999998,-92.34995));
#177073=CARTESIAN_POINT('Ctrl Pts',(20.,28.41999998,-91.34995));
#177074=CARTESIAN_POINT('Ctrl Pts',(20.,28.41999998,-92.34995));
#177075=CARTESIAN_POINT('Ctrl Pts',(20.,29.41999998,-92.34995));
#177076=CARTESIAN_POINT('Ctrl Pts',(20.5,28.41999998,-91.34995));
#177077=CARTESIAN_POINT('Ctrl Pts',(20.5,28.41999998,-92.34995));
#177078=CARTESIAN_POINT('Ctrl Pts',(20.5,29.41999998,-92.34995));
#177079=CARTESIAN_POINT('Ctrl Pts',(20.5,28.91999998,-91.34995));
#177080=CARTESIAN_POINT('Ctrl Pts',(20.5,28.91999998,-91.84995));
#177081=CARTESIAN_POINT('Ctrl Pts',(20.5,29.41999998,-91.84995));
#177082=CARTESIAN_POINT('',(20.5,29.41999998,-91.84995));
#177083=CARTESIAN_POINT('Origin',(20.5,29.41999998,-91.34995));
#177084=CARTESIAN_POINT('',(20.,29.41999998,-92.34995));
#177085=CARTESIAN_POINT('Origin',(20.,29.41999998,-91.84995));
#177086=CARTESIAN_POINT('Origin',(20.,29.41999998,-91.34995));
#177087=CARTESIAN_POINT('Origin',(60.,28.41999998,-55.24995));
#177088=CARTESIAN_POINT('',(17.5283474636331,28.4199999800081,-91.3499485560103));
#177089=CARTESIAN_POINT('Origin',(20.088871062793,28.4200000295341,-83.1773333825974));
#177090=CARTESIAN_POINT('',(16.1621051845127,28.4199999800001,-91.34995));
#177091=CARTESIAN_POINT('Ctrl Pts',(19.8416434885933,29.3176415862829,-85.6947270505041));
#177092=CARTESIAN_POINT('Ctrl Pts',(20.7092106783515,28.41999998,-86.6470800003654));
#177093=CARTESIAN_POINT('Ctrl Pts',(21.7666112105514,28.41999998,-87.8078183592076));
#177094=CARTESIAN_POINT('Ctrl Pts',(18.8896716409139,29.2827357288726,-86.6297133466452));
#177095=CARTESIAN_POINT('Ctrl Pts',(19.7296405475881,28.4199999799976,-87.5847244149314));
#177096=CARTESIAN_POINT('Ctrl Pts',(20.7402388551495,28.41999998,-88.7428151801658));
#177097=CARTESIAN_POINT('Ctrl Pts',(17.9119477871191,29.2478866829953,-87.5391531932496));
#177098=CARTESIAN_POINT('Ctrl Pts',(18.7197222668567,28.4199999800025,-88.4987039616193));
#177099=CARTESIAN_POINT('Ctrl Pts',(19.6830654074503,28.4199999800001,-89.6522445020127));
#177100=CARTESIAN_POINT('Ctrl Pts',(15.8876250911483,29.1791411788287,-89.290529750932));
#177101=CARTESIAN_POINT('Ctrl Pts',(16.6238286994528,28.4199999799976,-90.2586559409325));
#177102=CARTESIAN_POINT('Ctrl Pts',(17.4871574021565,28.4199999800001,-91.4036210595759));
#177103=CARTESIAN_POINT('Ctrl Pts',(14.8453850851454,29.1454134093176,-90.1279271408305));
#177104=CARTESIAN_POINT('Ctrl Pts',(15.5423832476573,28.4199999800097,-91.1005048403699));
#177105=CARTESIAN_POINT('Ctrl Pts',(16.353131902533,28.4199999800001,-92.2410073071712));
#177106=CARTESIAN_POINT('Ctrl Pts',(13.781556827362,29.1135284095041,-90.9029551205337));
#177107=CARTESIAN_POINT('Ctrl Pts',(14.4341913591531,28.41999998,-91.8807658383619));
#177108=CARTESIAN_POINT('Ctrl Pts',(15.1919283151595,28.4199999800001,-93.0160464292372));
#177109=CARTESIAN_POINT('Ctrl Pts',(17.5283474636331,28.4199999800081,-91.3499485560103));
#177110=CARTESIAN_POINT('Ctrl Pts',(17.4449670690501,28.4200000828332,-91.3407525162259));
#177111=CARTESIAN_POINT('Ctrl Pts',(17.3556350906279,28.4209780981964,-91.3309072709742));
#177112=CARTESIAN_POINT('Ctrl Pts',(17.2604628566404,28.4233820658963,-91.3204025719688));
#177113=CARTESIAN_POINT('Ctrl Pts',(17.209353748992,28.4246730374203,-91.3147613700153));
#177114=CARTESIAN_POINT('Ctrl Pts',(17.1565605798997,28.4263761331184,-91.3089299869687));
#177115=CARTESIAN_POINT('Ctrl Pts',(17.1021019331091,28.4285667561178,-91.3029068081637));
#177116=CARTESIAN_POINT('Ctrl Pts',(17.0241651859755,28.4317017960211,-91.29428692884));
#177117=CARTESIAN_POINT('Ctrl Pts',(16.9428200887949,28.435834974118,-91.2852725602857));
#177118=CARTESIAN_POINT('Ctrl Pts',(16.8581470738689,28.4411979043932,-91.2758758511481));
#177119=CARTESIAN_POINT('Ctrl Pts',(16.8158105664059,28.4438793695307,-91.2711774965793));
#177120=CARTESIAN_POINT('Ctrl Pts',(16.7726423863633,28.4468684484924,-91.2663838155556));
#177121=CARTESIAN_POINT('Ctrl Pts',(16.72865452465,28.4501948590961,-91.2614980219493));
#177122=CARTESIAN_POINT('Ctrl Pts',(16.7066605937934,28.451858064398,-91.2590551251462));
#177123=CARTESIAN_POINT('Ctrl Pts',(16.6844617436482,28.4536056114285,-91.256589201598));
#177124=CARTESIAN_POINT('Ctrl Pts',(16.662059622183,28.4554412241898,-91.2541008944022));
#177125=CARTESIAN_POINT('Ctrl Pts',(16.6508585614504,28.4563590305704,-91.2528567408044));
#177126=CARTESIAN_POINT('Ctrl Pts',(16.63960667785,28.4572987847638,-91.2516076963612));
#177127=CARTESIAN_POINT('Ctrl Pts',(16.6283041889963,28.4582610451365,-91.2503528794858));
#177128=CARTESIAN_POINT('Ctrl Pts',(16.6170017001427,28.4592233055093,-91.2490980626103));
#177129=CARTESIAN_POINT('Ctrl Pts',(16.6040146503638,28.4603524696449,-91.247656024132));
#177130=CARTESIAN_POINT('Ctrl Pts',(16.5942451218782,28.4612158251874,-91.2465711301194));
#177131=CARTESIAN_POINT('Ctrl Pts',(16.4255035637327,28.4761279020287,-91.2278325895262));
#177132=CARTESIAN_POINT('Ctrl Pts',(16.2577107764323,28.495018036401,-91.2091649348818));
#177133=CARTESIAN_POINT('Ctrl Pts',(16.0911292123908,28.517718159937,-91.190598973341));
#177134=CARTESIAN_POINT('Ctrl Pts',(15.9587321256393,28.5357599537114,-91.1758429633655));
#177135=CARTESIAN_POINT('Ctrl Pts',(15.8270995738065,28.5562073684433,-91.1611511371293));
#177136=CARTESIAN_POINT('Ctrl Pts',(15.6963501489323,28.5789561723598,-91.1465376691438));
#177137=CARTESIAN_POINT('Ctrl Pts',(15.6873039166932,28.5805301063453,-91.1455265991116));
#177138=CARTESIAN_POINT('Ctrl Pts',(15.6799762942362,28.5818126045997,-91.1447075451513));
#177139=CARTESIAN_POINT('Ctrl Pts',(15.669481806099,28.5836615901236,-91.1435525932031));
#177140=CARTESIAN_POINT('Ctrl Pts',(15.6689270297337,28.5837593341446,-91.1434915382916));
#177141=CARTESIAN_POINT('Ctrl Pts',(15.6683634058881,28.5838586733159,-91.1434295448885));
#177142=CARTESIAN_POINT('Ctrl Pts',(15.6677902137525,28.583959738813,-91.1433665350773));
#177143=CARTESIAN_POINT('Ctrl Pts',(15.6460612240955,28.5877910041168,-91.1409779127442));
#177144=CARTESIAN_POINT('Ctrl Pts',(15.6244513449189,28.5916691515427,-91.1385998012044));
#177145=CARTESIAN_POINT('Ctrl Pts',(15.602960062943,28.5955921284231,-91.1362322410147));
#177146=CARTESIAN_POINT('Ctrl Pts',(15.3794960512604,28.6363828151961,-91.1116146077591));
#177147=CARTESIAN_POINT('Ctrl Pts',(15.1688312125338,28.6819952998695,-91.0881339378895));
#177148=CARTESIAN_POINT('Ctrl Pts',(14.9704909007038,28.7307074200043,-91.0658565029333));
#177149=CARTESIAN_POINT('Ctrl Pts',(14.8672115437093,28.7560726944608,-91.0542562430741));
#177150=CARTESIAN_POINT('Ctrl Pts',(14.7672740628269,28.7822789906839,-91.0429824470375));
#177151=CARTESIAN_POINT('Ctrl Pts',(14.6706121874534,28.8090890708133,-91.0320453163648));
#177152=CARTESIAN_POINT('Ctrl Pts',(14.5146056345302,28.85235895533,-91.0143934339808));
#177153=CARTESIAN_POINT('Ctrl Pts',(14.367125110666,28.8972010263637,-90.9976177986137));
#177154=CARTESIAN_POINT('Ctrl Pts',(14.2279053139402,28.9426415327345,-90.9817809628304));
#177155=CARTESIAN_POINT('Ctrl Pts',(14.0992751073288,28.9846256604266,-90.9671487373368));
#177156=CARTESIAN_POINT('Ctrl Pts',(13.9776966559743,29.027120305016,-90.9533180092168));
#177157=CARTESIAN_POINT('Ctrl Pts',(13.8629628324617,29.0693971421497,-90.9403366624458));
#177158=CARTESIAN_POINT('Ctrl Pts',(19.8077681778583,29.3163999071086,-85.7279764688716));
#177159=CARTESIAN_POINT('Ctrl Pts',(19.4082493848523,29.3017607914722,-86.1198602027121));
#177160=CARTESIAN_POINT('Ctrl Pts',(19.0112633927749,29.2873923085991,-86.5002814539897));
#177161=CARTESIAN_POINT('Ctrl Pts',(18.6159839225994,29.273296094587,-86.8698151354957));
#177162=CARTESIAN_POINT('Ctrl Pts',(18.0851775960533,29.2543668049513,-87.3660483851714));
#177163=CARTESIAN_POINT('Ctrl Pts',(17.5574499676151,29.2359287990193,-87.842649941049));
#177164=CARTESIAN_POINT('Ctrl Pts',(17.0308778298195,29.2179724993612,-88.3010753210071));
#177165=CARTESIAN_POINT('Ctrl Pts',(16.9871738817249,29.2164821789817,-88.3391232874164));
#177166=CARTESIAN_POINT('Ctrl Pts',(16.9434779139457,29.2149951697386,-88.37704606025));
#177167=CARTESIAN_POINT('Ctrl Pts',(16.8997888344922,29.2135114625125,-88.4148444754352));
#177168=CARTESIAN_POINT('Ctrl Pts',(16.6124645154597,29.2037537570695,-88.6634284245469));
#177169=CARTESIAN_POINT('Ctrl Pts',(16.3257931544452,29.1941526893015,-88.9062649282737));
#177170=CARTESIAN_POINT('Ctrl Pts',(16.0398114822454,29.1847211178926,-89.1432707978858));
#177171=CARTESIAN_POINT('Ctrl Pts',(15.7410191195434,29.174867054576,-89.3908934626912));
#177172=CARTESIAN_POINT('Ctrl Pts',(15.4429795241797,29.1651979819656,-89.6321521383054));
#177173=CARTESIAN_POINT('Ctrl Pts',(15.1456858692503,29.1557258311974,-89.8669852373506));
#177174=CARTESIAN_POINT('Ctrl Pts',(14.8277972288318,29.1455974982188,-90.118086373695));
#177175=CARTESIAN_POINT('Ctrl Pts',(14.510761504061,29.1356942810336,-90.3618417424226));
#177176=CARTESIAN_POINT('Ctrl Pts',(14.1945159768074,29.1260282160452,-90.5982005175673));
#177177=CARTESIAN_POINT('Ctrl Pts',(14.082333602721,29.1225993545277,-90.682044512966));
#177178=CARTESIAN_POINT('Ctrl Pts',(13.9702501885868,29.119200315509,-90.7649579036228));
#177179=CARTESIAN_POINT('Ctrl Pts',(13.8582614415001,29.1158315802267,-90.8469387387806));
#177180=CARTESIAN_POINT('Ctrl Pts',(13.9704776589254,29.793296457161,-92.3317099697086));
#177181=CARTESIAN_POINT('Ctrl Pts',(13.5,29.798334383687,-92.3043420473087));
#177182=CARTESIAN_POINT('Ctrl Pts',(13.5,29.8836583509376,-91.8408299848543));
#177183=CARTESIAN_POINT('Ctrl Pts',(13.9485824763266,29.6507732526529,-92.3041572803908));
#177184=CARTESIAN_POINT('Ctrl Pts',(13.5,29.6658016093476,-92.2593052595342));
#177185=CARTESIAN_POINT('Ctrl Pts',(13.5,29.8088158028921,-91.8270528245268));
#177186=CARTESIAN_POINT('Ctrl Pts',(13.9277414892694,29.5120300570818,-92.2444171371624));
#177187=CARTESIAN_POINT('Ctrl Pts',(13.5,29.5406281722262,-92.1878683704653));
#177188=CARTESIAN_POINT('Ctrl Pts',(13.5,29.7360856593875,-91.7971835648529));
#177189=CARTESIAN_POINT('Ctrl Pts',(13.8924131672203,29.2732201982241,-92.0703719609639));
#177190=CARTESIAN_POINT('Ctrl Pts',(13.5,29.3333704157687,-92.0065554596633));
#177191=CARTESIAN_POINT('Ctrl Pts',(13.5,29.6110266364568,-91.7101609842055));
#177192=CARTESIAN_POINT('Ctrl Pts',(13.8776710606793,29.1715523493698,-91.9547463954628));
#177193=CARTESIAN_POINT('Ctrl Pts',(13.4999999999999,29.2476129207544,-91.895386283959));
#177194=CARTESIAN_POINT('Ctrl Pts',(13.5,29.5578590401594,-91.6523482016898));
#177195=CARTESIAN_POINT('Ctrl Pts',(13.8571693529918,29.0291974882966,-91.6899374203782));
#177196=CARTESIAN_POINT('Ctrl Pts',(13.5000000000001,29.1302566914018,-91.6522607622863));
#177197=CARTESIAN_POINT('Ctrl Pts',(13.5,29.4834479217461,-91.5199437062307));
#177198=CARTESIAN_POINT('Ctrl Pts',(13.851254772454,28.9875557647693,-91.5391474846049));
#177199=CARTESIAN_POINT('Ctrl Pts',(13.5000000000001,29.0962692564556,-91.5174684103174));
#177200=CARTESIAN_POINT('Ctrl Pts',(13.5,29.4617011701904,-91.4445487431295));
#177201=CARTESIAN_POINT('Ctrl Pts',(13.8496827900737,28.9765232161018,-91.2324126084916));
#177202=CARTESIAN_POINT('Ctrl Pts',(13.4999999999999,29.0873381907095,-91.2460073456115));
#177203=CARTESIAN_POINT('Ctrl Pts',(13.5,29.4559384360516,-91.2911813034188));
#177204=CARTESIAN_POINT('Ctrl Pts',(13.8539744318671,29.0067940350096,-91.0793665022882));
#177205=CARTESIAN_POINT('Ctrl Pts',(13.4999999999996,29.1119956223332,-91.1098405101534));
#177206=CARTESIAN_POINT('Ctrl Pts',(13.5,29.4717444256829,-91.2146593048585));
#177207=CARTESIAN_POINT('Ctrl Pts',(13.8629670146647,29.0694104105324,-90.9403371832566));
#177208=CARTESIAN_POINT('Ctrl Pts',(13.5,29.162996502681,-90.984393353347));
#177209=CARTESIAN_POINT('Ctrl Pts',(13.5,29.5044693674792,-91.1451435916293));
#177210=CARTESIAN_POINT('',(13.9704776589253,29.7932964571609,-92.3317099697081));
#177211=CARTESIAN_POINT('Ctrl Pts',(13.9704776589253,29.7932964571608,-92.3317099697086));
#177212=CARTESIAN_POINT('Ctrl Pts',(13.9660719436602,29.7646181560608,-92.3261658597216));
#177213=CARTESIAN_POINT('Ctrl Pts',(13.9618386370306,29.7371021221773,-92.3195123058631));
#177214=CARTESIAN_POINT('Ctrl Pts',(13.9578073956371,29.7108795338756,-92.3120680988498));
#177215=CARTESIAN_POINT('Ctrl Pts',(13.9545099890295,29.6894304249052,-92.3059790123879));
#177216=CARTESIAN_POINT('Ctrl Pts',(13.951347604472,29.6688456216843,-92.2993607697152));
#177217=CARTESIAN_POINT('Ctrl Pts',(13.9483326909375,29.6491723257345,-92.2923807044248));
#177218=CARTESIAN_POINT('Ctrl Pts',(13.9449822942959,29.6273098928904,-92.2846239356023));
#177219=CARTESIAN_POINT('Ctrl Pts',(13.9418154271827,29.6065821601135,-92.2764227184054));
#177220=CARTESIAN_POINT('Ctrl Pts',(13.9388506916509,29.5870682923812,-92.2680191239684));
#177221=CARTESIAN_POINT('Ctrl Pts',(13.937368323885,29.577311358515,-92.2638173267498));
#177222=CARTESIAN_POINT('Ctrl Pts',(13.9359364614834,29.5678578067295,-92.2595650702609));
#177223=CARTESIAN_POINT('Ctrl Pts',(13.9345572256012,29.5587169031431,-92.2552934382594));
#177224=CARTESIAN_POINT('Ctrl Pts',(13.9331779897191,29.5495759995568,-92.251021806258));
#177225=CARTESIAN_POINT('Ctrl Pts',(13.9318513808664,29.5407477463153,-92.2467308038121));
#177226=CARTESIAN_POINT('Ctrl Pts',(13.9305793585068,29.5322409034925,-92.2424520252128));
#177227=CARTESIAN_POINT('Ctrl Pts',(13.9274618297608,29.5113919562722,-92.2319654050833));
#177228=CARTESIAN_POINT('Ctrl Pts',(13.9246529340422,29.4924097351835,-92.2215211793986));
#177229=CARTESIAN_POINT('Ctrl Pts',(13.9221331430184,29.4752674918061,-92.2114767008387));
#177230=CARTESIAN_POINT('Ctrl Pts',(13.9205404067363,29.4644320404825,-92.2051276801119));
#177231=CARTESIAN_POINT('Ctrl Pts',(13.9190630962149,29.4543309529263,-92.1989375124784));
#177232=CARTESIAN_POINT('Ctrl Pts',(13.9176958195654,29.4449523900882,-92.1929871167551));
#177233=CARTESIAN_POINT('Ctrl Pts',(13.9159306301178,29.4328444233788,-92.1853050022808));
#177234=CARTESIAN_POINT('Ctrl Pts',(13.9143475548871,29.4219382408964,-92.1780218851911));
#177235=CARTESIAN_POINT('Ctrl Pts',(13.9129299430038,29.4121931549255,-92.1712831761532));
#177236=CARTESIAN_POINT('Ctrl Pts',(13.9122211370622,29.40732061194,-92.1679138216343));
#177237=CARTESIAN_POINT('Ctrl Pts',(13.9115536689625,29.4027382131008,-92.1646801183343));
#177238=CARTESIAN_POINT('Ctrl Pts',(13.9109253948871,29.3984404244484,-92.1615974984745));
#177239=CARTESIAN_POINT('Ctrl Pts',(13.9106330619778,29.3964406840335,-92.1601631702616));
#177240=CARTESIAN_POINT('Ctrl Pts',(13.9103492096096,29.3945025216351,-92.1587614975373));
#177241=CARTESIAN_POINT('Ctrl Pts',(13.9100736461926,29.3926255121625,-92.1573939964895));
#177242=CARTESIAN_POINT('Ctrl Pts',(13.9100530928442,29.3924855123394,-92.157291999186));
#177243=CARTESIAN_POINT('Ctrl Pts',(13.9100325852604,29.3923458505292,-92.1571901901387));
#177244=CARTESIAN_POINT('Ctrl Pts',(13.9100121233666,29.3922065265855,-92.1570885699965));
#177245=CARTESIAN_POINT('Ctrl Pts',(13.9098647237869,29.3912028907114,-92.1563565377456));
#177246=CARTESIAN_POINT('Ctrl Pts',(13.9097197094941,29.3902168737225,-92.1556343722458));
#177247=CARTESIAN_POINT('Ctrl Pts',(13.9095770470687,29.3892483865609,-92.1549222874115));
#177248=CARTESIAN_POINT('Ctrl Pts',(13.909505715856,29.3887641429801,-92.1545662449943));
#177249=CARTESIAN_POINT('Ctrl Pts',(13.9094751716244,29.3885555991234,-92.1544125945762));
#177250=CARTESIAN_POINT('Ctrl Pts',(13.9094250101062,29.3882155492447,-92.1541618662424));
#177251=CARTESIAN_POINT('Ctrl Pts',(13.9093748485881,29.3878754993659,-92.1539111379085));
#177252=CARTESIAN_POINT('Ctrl Pts',(13.9093050857272,29.3874037424048,-92.1535636138701));
#177253=CARTESIAN_POINT('Ctrl Pts',(13.9091560094093,29.3863954359885,-92.152816470617));
#177254=CARTESIAN_POINT('Ctrl Pts',(13.9048390217758,29.3571966578547,-92.1311805177665));
#177255=CARTESIAN_POINT('Ctrl Pts',(13.9007550483884,29.329522680952,-92.1081500266596));
#177256=CARTESIAN_POINT('Ctrl Pts',(13.8969256320677,29.303496130266,-92.0840897594474));
#177257=CARTESIAN_POINT('Ctrl Pts',(13.8931589395588,29.2778958807006,-92.0604235866737));
#177258=CARTESIAN_POINT('Ctrl Pts',(13.8896385152793,29.2538895184042,-92.0357614245562));
#177259=CARTESIAN_POINT('Ctrl Pts',(13.8863779446049,29.2315457150798,-92.0104355370998));
#177260=CARTESIAN_POINT('Ctrl Pts',(13.8856272645384,29.2264015089148,-92.0046047667294));
#177261=CARTESIAN_POINT('Ctrl Pts',(13.8848903295692,29.221345225095,-91.9987387408664));
#177262=CARTESIAN_POINT('Ctrl Pts',(13.8841672543394,29.2163773369429,-91.9928413741767));
#177263=CARTESIAN_POINT('Ctrl Pts',(13.8809865167897,29.1945240805472,-91.9668994321714));
#177264=CARTESIAN_POINT('Ctrl Pts',(13.8780714941699,29.1743821555997,-91.9403489716015));
#177265=CARTESIAN_POINT('Ctrl Pts',(13.8754145679604,29.1559578661073,-91.9134942881761));
#177266=CARTESIAN_POINT('Ctrl Pts',(13.8751241956756,29.1539442975643,-91.9105593719722));
#177267=CARTESIAN_POINT('Ctrl Pts',(13.874836900671,29.1519512003806,-91.9076207966203));
#177268=CARTESIAN_POINT('Ctrl Pts',(13.8745526690139,29.1499785504107,-91.9046789404017));
#177269=CARTESIAN_POINT('Ctrl Pts',(13.8731101836618,29.1399672845464,-91.8897489197756));
#177270=CARTESIAN_POINT('Ctrl Pts',(13.8717464644608,29.1304829683556,-91.8747345104047));
#177271=CARTESIAN_POINT('Ctrl Pts',(13.8704584257147,29.1215200363874,-91.8596831904024));
#177272=CARTESIAN_POINT('Ctrl Pts',(13.8698849070136,29.1175291555882,-91.8529813628963));
#177273=CARTESIAN_POINT('Ctrl Pts',(13.869356255753,29.1138487597176,-91.8466285500808));
#177274=CARTESIAN_POINT('Ctrl Pts',(13.868831041355,29.1101938494189,-91.840157299871));
#177275=CARTESIAN_POINT('Ctrl Pts',(13.8683658756017,29.1069568111566,-91.8344259185726));
#177276=CARTESIAN_POINT('Ctrl Pts',(13.8679034723206,29.103740197726,-91.8286012287684));
#177277=CARTESIAN_POINT('Ctrl Pts',(13.8674193485158,29.1003751246054,-91.8223417922768));
#177278=CARTESIAN_POINT('Ctrl Pts',(13.8672224644036,29.099006612198,-91.8197961963281));
#177279=CARTESIAN_POINT('Ctrl Pts',(13.867021980309,29.0976135305897,-91.8171779274437));
#177280=CARTESIAN_POINT('Ctrl Pts',(13.8668164546783,29.0961859184677,-91.8144631545686));
#177281=CARTESIAN_POINT('Ctrl Pts',(13.8642275697956,29.0782031324296,-91.7802667653671));
#177282=CARTESIAN_POINT('Ctrl Pts',(13.8619343749943,29.0622384906243,-91.7449845405102));
#177283=CARTESIAN_POINT('Ctrl Pts',(13.8599486096495,29.0483917564659,-91.709006233217));
#177284=CARTESIAN_POINT('Ctrl Pts',(13.8579976218432,29.0347875259502,-91.673658029057));
#177285=CARTESIAN_POINT('Ctrl Pts',(13.8563434001964,29.0232278025212,-91.6376388186669));
#177286=CARTESIAN_POINT('Ctrl Pts',(13.8549901949726,29.0137586069535,-91.6013194042953));
#177287=CARTESIAN_POINT('Ctrl Pts',(13.853656462459,29.0044256737189,-91.5655226286316));
#177288=CARTESIAN_POINT('Ctrl Pts',(13.8526151487513,28.9971236073399,-91.5294349801731));
#177289=CARTESIAN_POINT('Ctrl Pts',(13.8518634700335,28.9918473079284,-91.4934004105108));
#177290=CARTESIAN_POINT('Ctrl Pts',(13.8511117913156,28.9865710085169,-91.4573658408485));
#177291=CARTESIAN_POINT('Ctrl Pts',(13.8506497573169,28.9833205884546,-91.4213850311442));
#177292=CARTESIAN_POINT('Ctrl Pts',(13.8504675584972,28.9820398733893,-91.3857800321588));
#177293=CARTESIAN_POINT('Ctrl Pts',(13.850459871782,28.9819858417989,-91.3842779066858));
#177294=CARTESIAN_POINT('Ctrl Pts',(13.8504526772006,28.9819352758935,-91.3827767240698));
#177295=CARTESIAN_POINT('Ctrl Pts',(13.8504459726624,28.981888160148,-91.3812765043687));
#177296=CARTESIAN_POINT('Ctrl Pts',(13.8503108157195,28.9809383527283,-91.3510335402089));
#177297=CARTESIAN_POINT('Ctrl Pts',(13.8503713034644,28.9813677928989,-91.3203201309666));
#177298=CARTESIAN_POINT('Ctrl Pts',(13.8506407953683,28.9832638958992,-91.2893816972864));
#177299=CARTESIAN_POINT('Ctrl Pts',(13.8509127119446,28.9851770585159,-91.258164904357));
#177300=CARTESIAN_POINT('Ctrl Pts',(13.8513974319433,28.9885835117664,-91.2267196122043));
#177301=CARTESIAN_POINT('Ctrl Pts',(13.8521014903619,28.9935216895577,-91.1953097078188));
#177302=CARTESIAN_POINT('Ctrl Pts',(13.85280750844,28.9984736121552,-91.163812377855));
#177303=CARTESIAN_POINT('Ctrl Pts',(13.8537340898665,29.0049657742317,-91.1323513226142));
#177304=CARTESIAN_POINT('Ctrl Pts',(13.8548804607771,29.0129848879013,-91.1011947079472));
#177305=CARTESIAN_POINT('Ctrl Pts',(13.8560254849809,29.020994581064,-91.0700746947195));
#177306=CARTESIAN_POINT('Ctrl Pts',(13.8573897688233,29.0305275024821,-91.0392591235628));
#177307=CARTESIAN_POINT('Ctrl Pts',(13.858965299919,29.0415198349271,-91.009006688265));
#177308=CARTESIAN_POINT('Ctrl Pts',(13.8601766023979,29.04997097853,-90.9857479598451));
#177309=CARTESIAN_POINT('Ctrl Pts',(13.8615126204926,29.0592837088275,-90.9628220098879));
#177310=CARTESIAN_POINT('Ctrl Pts',(13.8629668992758,29.0694096071188,-90.9403389671137));
#177311=CARTESIAN_POINT('',(13.5,29.8836583509375,-91.8408299848543));
#177312=CARTESIAN_POINT('Origin',(14.,29.8836583509375,-91.8408299848543));
#177313=CARTESIAN_POINT('Ctrl Pts',(13.5,29.5044693674792,-91.1451435916293));
#177314=CARTESIAN_POINT('Ctrl Pts',(13.5,29.4871798972865,-91.1818706195726));
#177315=CARTESIAN_POINT('Ctrl Pts',(13.5,29.4746493543107,-91.2204653406996));
#177316=CARTESIAN_POINT('Ctrl Pts',(13.5,29.4670724885977,-91.259957519387));
#177317=CARTESIAN_POINT('Ctrl Pts',(13.5,29.4602667842095,-91.2954302470261));
#177318=CARTESIAN_POINT('Ctrl Pts',(13.5,29.4574580326191,-91.3316285116295));
#177319=CARTESIAN_POINT('Ctrl Pts',(13.5000000000001,29.4588194335385,-91.3678650371612));
#177320=CARTESIAN_POINT('Ctrl Pts',(13.5000000000001,29.4588222728777,-91.367940612098));
#177321=CARTESIAN_POINT('Ctrl Pts',(13.5000000000001,29.4588251305407,-91.3680161857943));
#177322=CARTESIAN_POINT('Ctrl Pts',(13.5000000000001,29.4588280065244,-91.3680917582431));
#177323=CARTESIAN_POINT('Ctrl Pts',(13.5000000000004,29.4617431600592,-91.4446934778138));
#177324=CARTESIAN_POINT('Ctrl Pts',(13.4999999999999,29.483485076552,-91.5200098118263));
#177325=CARTESIAN_POINT('Ctrl Pts',(13.5000000000001,29.5206532241076,-91.5861460983069));
#177326=CARTESIAN_POINT('Ctrl Pts',(13.5000000000001,29.5206776694618,-91.5861895958997));
#177327=CARTESIAN_POINT('Ctrl Pts',(13.5000000000001,29.5207021217052,-91.5862330898687));
#177328=CARTESIAN_POINT('Ctrl Pts',(13.5000000000001,29.5207265808359,-91.5862765802124));
#177329=CARTESIAN_POINT('Ctrl Pts',(13.5000000000003,29.5579279046594,-91.6524235901087));
#177330=CARTESIAN_POINT('Ctrl Pts',(13.5,29.6110672833213,-91.710189265371));
#177331=CARTESIAN_POINT('Ctrl Pts',(13.5,29.6735560708361,-91.7536723853085));
#177332=CARTESIAN_POINT('Ctrl Pts',(13.5,29.6735766131945,-91.7536866798063));
#177333=CARTESIAN_POINT('Ctrl Pts',(13.5,29.6735971566538,-91.7537009728318));
#177334=CARTESIAN_POINT('Ctrl Pts',(13.5,29.6736177012137,-91.753715264385));
#177335=CARTESIAN_POINT('Ctrl Pts',(13.5,29.6935761704139,-91.7675991112376));
#177336=CARTESIAN_POINT('Ctrl Pts',(13.5,29.7144903240443,-91.7800410703758));
#177337=CARTESIAN_POINT('Ctrl Pts',(13.5,29.7361680987988,-91.7910278638482));
#177338=CARTESIAN_POINT('Ctrl Pts',(13.5,29.7580697930565,-91.8021281448608));
#177339=CARTESIAN_POINT('Ctrl Pts',(13.5,29.78075231092,-91.8117435399085));
#177340=CARTESIAN_POINT('Ctrl Pts',(13.5,29.8040427282678,-91.8198138783841));
#177341=CARTESIAN_POINT('Ctrl Pts',(13.5,29.8266838607853,-91.8276592338434));
#177342=CARTESIAN_POINT('Ctrl Pts',(13.5,29.8499007708166,-91.8340446948146));
#177343=CARTESIAN_POINT('Ctrl Pts',(13.5,29.8735386060567,-91.8388665069538));
#177344=CARTESIAN_POINT('Ctrl Pts',(13.5,29.8769034909812,-91.8395528998832));
#177345=CARTESIAN_POINT('Ctrl Pts',(13.5,29.8802768936902,-91.8402075213397));
#177346=CARTESIAN_POINT('Ctrl Pts',(13.5,29.8836583509375,-91.8408299848543));
#177347=CARTESIAN_POINT('Ctrl Pts',(14.,29.9836543272765,-92.34995));
#177348=CARTESIAN_POINT('Ctrl Pts',(13.5,29.9836543272765,-92.34995));
#177349=CARTESIAN_POINT('Ctrl Pts',(13.5,29.9836543272765,-91.84995));
#177350=CARTESIAN_POINT('Ctrl Pts',(13.9900288285115,29.9192223045234,-92.34995));
#177351=CARTESIAN_POINT('Ctrl Pts',(13.5,29.9198591164476,-92.340077310875));
#177352=CARTESIAN_POINT('Ctrl Pts',(13.5,29.9498130224307,-91.8499499813658));
#177353=CARTESIAN_POINT('Ctrl Pts',(13.9801870069313,29.8557668849998,-92.3437935523175));
#177354=CARTESIAN_POINT('Ctrl Pts',(13.4999999999992,29.8581345500688,-92.3247747757233));
#177355=CARTESIAN_POINT('Ctrl Pts',(13.5,29.9164799575816,-91.8468718299503));
#177356=CARTESIAN_POINT('Ctrl Pts',(13.9704776589253,29.7932964571608,-92.3317099697086));
#177357=CARTESIAN_POINT('Ctrl Pts',(13.5,29.7983343836869,-92.3043420473086));
#177358=CARTESIAN_POINT('Ctrl Pts',(13.5,29.8836583509375,-91.8408299848543));
#177359=CARTESIAN_POINT('',(14.,29.9836543272765,-92.34995));
#177360=CARTESIAN_POINT('',(13.5,29.9836543272765,-91.84995));
#177361=CARTESIAN_POINT('Origin',(14.,29.9836543272765,-91.84995));
#177362=CARTESIAN_POINT('Origin',(13.5,29.9835150560362,-91.2987164399481));
#177363=CARTESIAN_POINT('Origin',(14.0082677506659,29.9821486511294,-91.3259572338972));
#177364=CARTESIAN_POINT('Origin',(13.,46.41999998,-92.34995));
#177365=CARTESIAN_POINT('',(13.5,46.41999998,-91.84995));
#177366=CARTESIAN_POINT('',(13.5,46.41999998,-58.2497627936531));
#177367=CARTESIAN_POINT('',(13.5,46.41999998,-58.24995));
#177368=CARTESIAN_POINT('',(13.,46.91999998,-91.84995));
#177369=CARTESIAN_POINT('Origin',(13.,46.41999998,-91.84995));
#177370=CARTESIAN_POINT('',(13.,46.91999998,-58.2497627936531));
#177371=CARTESIAN_POINT('',(13.,46.91999998,-92.34995));
#177372=CARTESIAN_POINT('Origin',(13.,46.41999998,-58.2497627936531));
#177373=CARTESIAN_POINT('Origin',(-39.,46.91999998,-129.34995));
#177374=CARTESIAN_POINT('',(12.5,46.91999998,-91.84995));
#177375=CARTESIAN_POINT('',(-39.,46.91999998,-91.84995));
#177376=CARTESIAN_POINT('',(12.5,46.91999998,-58.2465463958495));
#177377=CARTESIAN_POINT('',(12.5,46.91999998,-58.2396719107252));
#177378=CARTESIAN_POINT('Origin',(13.1654225534,46.91999998,6.33069708304167));
#177379=CARTESIAN_POINT('Origin',(12.5,46.41999998,-92.34995));
#177380=CARTESIAN_POINT('',(12.,46.41999998,-91.84995));
#177381=CARTESIAN_POINT('Origin',(12.5,46.41999998,-91.84995));
#177382=CARTESIAN_POINT('',(12.,46.41999998,-58.2465463958495));
#177383=CARTESIAN_POINT('',(12.,46.41999998,-92.34995));
#177384=CARTESIAN_POINT('Origin',(12.5,46.41999998,-58.2465463958495));
#177385=CARTESIAN_POINT('Ctrl Pts',(11.3828490268763,29.8129372786953,-90.9273970483904));
#177386=CARTESIAN_POINT('Ctrl Pts',(12.,29.6789774176902,-90.8627568967152));
#177387=CARTESIAN_POINT('Ctrl Pts',(12.,30.2507177004773,-91.1386408691297));
#177388=CARTESIAN_POINT('Ctrl Pts',(11.3736122815127,29.7418362505901,-91.0798688801893));
#177389=CARTESIAN_POINT('Ctrl Pts',(11.9999999999987,29.5823965713538,-91.0340021334692));
#177390=CARTESIAN_POINT('Ctrl Pts',(12.,30.2139234693476,-91.2148931255634));
#177391=CARTESIAN_POINT('Ctrl Pts',(11.3694271586094,29.7097409287485,-91.2531177376593));
#177392=CARTESIAN_POINT('Ctrl Pts',(11.9999999999999,29.5374187137922,-91.2360706889224));
#177393=CARTESIAN_POINT('Ctrl Pts',(12.,30.1973151560885,-91.3015254072135));
#177394=CARTESIAN_POINT('Ctrl Pts',(11.3717857023911,29.7278584436048,-91.5056751034728));
#177395=CARTESIAN_POINT('Ctrl Pts',(12.0000000000001,29.5627300607015,-91.5325373605759));
#177396=CARTESIAN_POINT('Ctrl Pts',(12.,30.2066913195442,-91.427825927492));
#177397=CARTESIAN_POINT('Ctrl Pts',(11.3740091557864,29.7449360486904,-91.59034805389));
#177398=CARTESIAN_POINT('Ctrl Pts',(11.9999999999998,29.5864519111761,-91.6308853388652));
#177399=CARTESIAN_POINT('Ctrl Pts',(12.,30.2155293203062,-91.4701692696895));
#177400=CARTESIAN_POINT('Ctrl Pts',(11.3810283772274,29.7989166519369,-91.7500080967778));
#177401=CARTESIAN_POINT('Ctrl Pts',(12.0000000000001,29.6601524162645,-91.8125032590501));
#177402=CARTESIAN_POINT('Ctrl Pts',(12.,30.2434629903521,-91.5500105484349));
#177403=CARTESIAN_POINT('Ctrl Pts',(11.3858517899463,29.8360332465147,-91.8263697865188));
#177404=CARTESIAN_POINT('Ctrl Pts',(11.9999999999999,29.7099192942087,-91.8968680856685));
#177405=CARTESIAN_POINT('Ctrl Pts',(12.,30.2626690028682,-91.5881956385046));
#177406=CARTESIAN_POINT('Ctrl Pts',(11.4037918623192,29.9743449793193,-92.038010246663));
#177407=CARTESIAN_POINT('Ctrl Pts',(12.0000000000002,29.8889381806538,-92.1200651023362));
#177408=CARTESIAN_POINT('Ctrl Pts',(12.,30.3342288077533,-91.6940226905849));
#177409=CARTESIAN_POINT('Ctrl Pts',(11.4201987017183,30.1011425197784,-92.1530192095865));
#177410=CARTESIAN_POINT('Ctrl Pts',(11.9999999999989,30.044850112339,-92.2289441977774));
#177411=CARTESIAN_POINT('Ctrl Pts',(12.,30.3998197343385,-91.7515247512526));
#177412=CARTESIAN_POINT('Ctrl Pts',(11.4619399583253,30.4256124104741,-92.3272312824867));
#177413=CARTESIAN_POINT('Ctrl Pts',(12.0000000000013,30.4142697832356,-92.3669482747856));
#177414=CARTESIAN_POINT('Ctrl Pts',(12.,30.5676008328764,-91.8386125685596));
#177415=CARTESIAN_POINT('Ctrl Pts',(11.4887517849116,30.6352262411195,-92.3673064106212));
#177416=CARTESIAN_POINT('Ctrl Pts',(11.9999999999994,30.6346409292876,-92.3781417391106));
#177417=CARTESIAN_POINT('Ctrl Pts',(12.,30.675950734103,-91.8586341550587));
#177418=CARTESIAN_POINT('Ctrl Pts',(11.5140711352129,30.8347410688585,-92.3430217069376));
#177419=CARTESIAN_POINT('Ctrl Pts',(12.0000000000002,30.8328497940556,-92.3295276769414));
#177420=CARTESIAN_POINT('Ctrl Pts',(12.,30.7790312201287,-91.8464778288845));
#177421=CARTESIAN_POINT('',(12.,30.7194735506599,-91.84995));
#177422=CARTESIAN_POINT('Ctrl Pts',(12.,30.7194735506598,-91.84995));
#177423=CARTESIAN_POINT('Ctrl Pts',(12.,30.6947425199752,-91.84995));
#177424=CARTESIAN_POINT('Ctrl Pts',(12.,30.6701386971986,-91.8481899526742));
#177425=CARTESIAN_POINT('Ctrl Pts',(12.,30.6458464406133,-91.8447815200538));
#177426=CARTESIAN_POINT('Ctrl Pts',(12.,30.6209700785576,-91.841291131929));
#177427=CARTESIAN_POINT('Ctrl Pts',(12.,30.5964191072392,-91.8360720015142));
#177428=CARTESIAN_POINT('Ctrl Pts',(12.,30.5723817191876,-91.8291895987897));
#177429=CARTESIAN_POINT('Ctrl Pts',(12.,30.548553583565,-91.8223671093755));
#177430=CARTESIAN_POINT('Ctrl Pts',(12.,30.5252287940054,-91.8139098291041));
#177431=CARTESIAN_POINT('Ctrl Pts',(12.,30.5026013041075,-91.8038327530222));
#177432=CARTESIAN_POINT('Ctrl Pts',(12.,30.4932234054494,-91.7996563375783));
#177433=CARTESIAN_POINT('Ctrl Pts',(12.,30.4839655197029,-91.7952011432061));
#177434=CARTESIAN_POINT('Ctrl Pts',(12.,30.4748428234451,-91.7904659511164));
#177435=CARTESIAN_POINT('Ctrl Pts',(12.,30.3998197342529,-91.7515247512294));
#177436=CARTESIAN_POINT('Ctrl Pts',(12.,30.3342288071963,-91.6940226895201));
#177437=CARTESIAN_POINT('Ctrl Pts',(12.,30.2865222597932,-91.6234713302197));
#177438=CARTESIAN_POINT('Ctrl Pts',(12.,30.2626689858469,-91.5881956502074));
#177439=CARTESIAN_POINT('Ctrl Pts',(12.,30.2434629741256,-91.5500105562497));
#177440=CARTESIAN_POINT('Ctrl Pts',(12.,30.2294961429083,-91.5100899134078));
#177441=CARTESIAN_POINT('Ctrl Pts',(12.,30.2155293119778,-91.4701692713854));
#177442=CARTESIAN_POINT('Ctrl Pts',(12.,30.2066913177853,-91.427825927269));
#177443=CARTESIAN_POINT('Ctrl Pts',(12.,30.20356593057,-91.3857257541517));
#177444=CARTESIAN_POINT('Ctrl Pts',(12.,30.2016706004035,-91.3601949246491));
#177445=CARTESIAN_POINT('Ctrl Pts',(12.,30.2018789661756,-91.3345298932578));
#177446=CARTESIAN_POINT('Ctrl Pts',(12.,30.2040942316499,-91.3090051705625));
#177447=CARTESIAN_POINT('Ctrl Pts',(12.,30.2063233672373,-91.2833206337077));
#177448=CARTESIAN_POINT('Ctrl Pts',(12.,30.2105848815976,-91.2577766407644));
#177449=CARTESIAN_POINT('Ctrl Pts',(12.,30.2168325161081,-91.2326549802759));
#177450=CARTESIAN_POINT('Ctrl Pts',(12.,30.2228393598883,-91.2085015363124));
#177451=CARTESIAN_POINT('Ctrl Pts',(12.,30.2306827015454,-91.1847372739709));
#177452=CARTESIAN_POINT('Ctrl Pts',(12.,30.2403633283688,-91.1616344702769));
#177453=CARTESIAN_POINT('Ctrl Pts',(12.,30.2436077578597,-91.1538916433923));
#177454=CARTESIAN_POINT('Ctrl Pts',(12.,30.2470588833974,-91.1462233796091));
#177455=CARTESIAN_POINT('Ctrl Pts',(12.,30.2507177004773,-91.1386408691297));
#177456=CARTESIAN_POINT('',(11.5,30.7194735506599,-92.34995));
#177457=CARTESIAN_POINT('Origin',(11.5,30.7194735506599,-91.84995));
#177458=CARTESIAN_POINT('',(11.3712933400037,29.7190889970661,-91.34995));
#177459=CARTESIAN_POINT('Ctrl Pts',(11.3712933400037,29.7190889970661,-91.34995));
#177460=CARTESIAN_POINT('Ctrl Pts',(11.3712933400037,29.7190889970661,-91.4733567786907));
#177461=CARTESIAN_POINT('Ctrl Pts',(11.3741527847607,29.7422826479407,-91.6008386596925));
#177462=CARTESIAN_POINT('Ctrl Pts',(11.3836657034065,29.8155581996794,-91.783323087588));
#177463=CARTESIAN_POINT('Ctrl Pts',(11.3876915067885,29.8463423612377,-91.842649921852));
#177464=CARTESIAN_POINT('Ctrl Pts',(11.394957471004,29.9019098608904,-91.9272311993885));
#177465=CARTESIAN_POINT('Ctrl Pts',(11.3975826489861,29.9219927335249,-91.9546886186485));
#177466=CARTESIAN_POINT('Ctrl Pts',(11.4018054333812,29.9543927938362,-91.9944916815559));
#177467=CARTESIAN_POINT('Ctrl Pts',(11.4039879398925,29.9711612553143,-92.0140473917535));
#177468=CARTESIAN_POINT('Ctrl Pts',(11.4066528137211,29.9916995580463,-92.0361959839154));
#177469=CARTESIAN_POINT('Ctrl Pts',(11.4078195966584,30.0007081718305,-92.0455388832796));
#177470=CARTESIAN_POINT('Ctrl Pts',(11.4086028563942,30.0067595156802,-92.0517335659694));
#177471=CARTESIAN_POINT('Ctrl Pts',(11.4091488014936,30.0109808652905,-92.05598374434));
#177472=CARTESIAN_POINT('Ctrl Pts',(11.4172463075705,30.0736231630541,-92.1184615112787));
#177473=CARTESIAN_POINT('Ctrl Pts',(11.427711960877,30.1586873759409,-92.1882507670382));
#177474=CARTESIAN_POINT('Ctrl Pts',(11.4577433109396,30.3931008233118,-92.3041894616728));
#177475=CARTESIAN_POINT('Ctrl Pts',(11.4776449981906,30.5437415320498,-92.34995));
#177476=CARTESIAN_POINT('Ctrl Pts',(11.5,30.7194735506599,-92.34995));
#177477=CARTESIAN_POINT('Origin',(11.4700666481164,30.4797619500454,-91.297907126496));
#177478=CARTESIAN_POINT('Ctrl Pts',(5.5,31.8716754827171,-92.34995));
#177479=CARTESIAN_POINT('Ctrl Pts',(4.99900616154848,31.8716754827171,-92.34995));
#177480=CARTESIAN_POINT('Ctrl Pts',(5.00000098575356,31.8716754827171,-91.8489571492614));
#177481=CARTESIAN_POINT('Ctrl Pts',(5.48989377680063,31.7056523166615,-92.34995));
#177482=CARTESIAN_POINT('Ctrl Pts',(4.99903601393591,31.7072113826353,-92.3399186475543));
#177483=CARTESIAN_POINT('Ctrl Pts',(5.00000096584847,31.7882063435843,-91.84896712888));
#177484=CARTESIAN_POINT('Ctrl Pts',(5.47963373781052,31.538103809625,-92.3071746231476));
#177485=CARTESIAN_POINT('Ctrl Pts',(4.99906555653679,31.5446619586649,-92.2883582792096));
#177486=CARTESIAN_POINT('Ctrl Pts',(5.0000009456393,31.7039607739187,-91.827630757647));
#177487=CARTESIAN_POINT('Ctrl Pts',(5.46619042199875,31.3196047327668,-92.1878686007335));
#177488=CARTESIAN_POINT('Ctrl Pts',(4.99910325428495,31.3370094182925,-92.161272810455));
#177489=CARTESIAN_POINT('Ctrl Pts',(5.00000091915851,31.5940866659351,-91.7681041344854));
#177490=CARTESIAN_POINT('Ctrl Pts',(5.46194839019336,31.2508398250121,-92.1383294170381));
#177491=CARTESIAN_POINT('Ctrl Pts',(4.99911492812254,31.2726858878275,-92.1103972204605));
#177492=CARTESIAN_POINT('Ctrl Pts',(5.00000091080218,31.5595055375377,-91.7433851154792));
#177493=CARTESIAN_POINT('Ctrl Pts',(5.45439667136824,31.1286541135227,-92.0244078521253));
#177494=CARTESIAN_POINT('Ctrl Pts',(4.99913545432273,31.1595480268539,-91.9961676804233));
#177495=CARTESIAN_POINT('Ctrl Pts',(5.00000089592572,31.4980571027827,-91.6865378587347));
#177496=CARTESIAN_POINT('Ctrl Pts',(5.45108997919633,31.0752759499814,-91.9605552262364));
#177497=CARTESIAN_POINT('Ctrl Pts',(4.99914433728197,31.1105664451878,-91.9333048742067));
#177498=CARTESIAN_POINT('Ctrl Pts',(5.00000088941156,31.4712115049494,-91.6546739801719));
#177499=CARTESIAN_POINT('Ctrl Pts',(5.44262999595016,30.938884482232,-91.7477840212027));
#177500=CARTESIAN_POINT('Ctrl Pts',(4.99916680129804,30.9866628751626,-91.7272955383522));
#177501=CARTESIAN_POINT('Ctrl Pts',(5.00000087274503,31.4026135113348,-91.548492809174));
#177502=CARTESIAN_POINT('Ctrl Pts',(5.43928039898085,30.8851161679224,-91.5835323055617));
#177503=CARTESIAN_POINT('Ctrl Pts',(4.99917557416918,30.9382275273278,-91.5708670061702));
#177504=CARTESIAN_POINT('Ctrl Pts',(5.00000086614598,31.3755689941209,-91.4665221319675));
#177505=CARTESIAN_POINT('Ctrl Pts',(5.43788833142316,30.8627516985332,-91.2503023235849));
#177506=CARTESIAN_POINT('Ctrl Pts',(4.99917920690125,30.918174361902,-91.2558237036598));
#177507=CARTESIAN_POINT('Ctrl Pts',(5.00000086340344,31.3643200540035,-91.3002194649784));
#177508=CARTESIAN_POINT('Ctrl Pts',(5.4398728408893,30.894582824155,-91.0791566847487));
#177509=CARTESIAN_POINT('Ctrl Pts',(4.99917405374089,30.9467642298381,-91.0936720204705));
#177510=CARTESIAN_POINT('Ctrl Pts',(5.00000086731322,31.3803302826741,-91.2148086838993));
#177511=CARTESIAN_POINT('Ctrl Pts',(5.44427033638568,30.9653765476951,-90.9273317382594));
#177512=CARTESIAN_POINT('Ctrl Pts',(4.99916246706145,31.0105597677356,-90.9485621815415));
#177513=CARTESIAN_POINT('Ctrl Pts',(5.0000008759766,31.4159376038041,-91.1390388927805));
#177514=CARTESIAN_POINT('',(5.43844464087133,30.8716892291687,-91.3499500006361));
#177515=CARTESIAN_POINT('Origin',(5.48568341414045,31.6321344502636,-91.297904512692));
#177516=CARTESIAN_POINT('',(5.5,31.8716754827171,-92.34995));
#177517=CARTESIAN_POINT('Ctrl Pts',(5.49999999999999,31.8716754827171,-92.34995));
#177518=CARTESIAN_POINT('Ctrl Pts',(5.4978815673594,31.8368742625198,-92.34995));
#177519=CARTESIAN_POINT('Ctrl Pts',(5.49579787553642,31.8029594634244,-92.348133240981));
#177520=CARTESIAN_POINT('Ctrl Pts',(5.493769479706,31.7700915140547,-92.3447767183816));
#177521=CARTESIAN_POINT('Ctrl Pts',(5.49169197795832,31.7364278566788,-92.3413389369279));
#177522=CARTESIAN_POINT('Ctrl Pts',(5.48967245804065,31.7038621275029,-92.3362865275642));
#177523=CARTESIAN_POINT('Ctrl Pts',(5.48772616666163,31.6725108730827,-92.3299137899354));
#177524=CARTESIAN_POINT('Ctrl Pts',(5.48573075716194,31.6403684140593,-92.3233802249508));
#177525=CARTESIAN_POINT('Ctrl Pts',(5.48381228263233,31.609502182019,-92.3154593937791));
#177526=CARTESIAN_POINT('Ctrl Pts',(5.48198053529549,31.5799839743614,-92.3064561998247));
#177527=CARTESIAN_POINT('Ctrl Pts',(5.48001777371976,31.548354500902,-92.2968090597431));
#177528=CARTESIAN_POINT('Ctrl Pts',(5.47815458294883,31.5182727007077,-92.2859199157918));
#177529=CARTESIAN_POINT('Ctrl Pts',(5.47639575095647,31.4897685177843,-92.2741396830177));
#177530=CARTESIAN_POINT('Ctrl Pts',(5.47464127727594,31.4613349670296,-92.2623886411658));
#177531=CARTESIAN_POINT('Ctrl Pts',(5.47299054949597,31.4344704273083,-92.2497512170054));
#177532=CARTESIAN_POINT('Ctrl Pts',(5.47144226944925,31.4091563595002,-92.2365449915221));
#177533=CARTESIAN_POINT('Ctrl Pts',(5.46982926682253,31.3827840905079,-92.2227867076515));
#177534=CARTESIAN_POINT('Ctrl Pts',(5.46832739057934,31.3580940820943,-92.2084115017261));
#177535=CARTESIAN_POINT('Ctrl Pts',(5.46692979196242,31.3350228801632,-92.1937391327595));
#177536=CARTESIAN_POINT('Ctrl Pts',(5.46563435464848,31.3136381309962,-92.1801392808328));
#177537=CARTESIAN_POINT('Ctrl Pts',(5.46442839146343,31.2936432479195,-92.1662837176707));
#177538=CARTESIAN_POINT('Ctrl Pts',(5.46330338345437,31.2749638086464,-92.1523952289126));
#177539=CARTESIAN_POINT('Ctrl Pts',(5.46199291939706,31.2532050890809,-92.1362172415728));
#177540=CARTESIAN_POINT('Ctrl Pts',(5.46079227751257,31.2332310339142,-92.1199956745703));
#177541=CARTESIAN_POINT('Ctrl Pts',(5.45968468767403,31.2148987829739,-92.1040310703102));
#177542=CARTESIAN_POINT('Ctrl Pts',(5.45913089275476,31.2057326575037,-92.0960487681802));
#177543=CARTESIAN_POINT('Ctrl Pts',(5.45860031611243,31.1969766464014,-92.0881298511603));
#177544=CARTESIAN_POINT('Ctrl Pts',(5.4580906611324,31.1886114184243,-92.080306896806));
#177545=CARTESIAN_POINT('Ctrl Pts',(5.45783583364236,31.1844288044357,-92.0763954196288));
#177546=CARTESIAN_POINT('Ctrl Pts',(5.4575862390359,31.1803439061936,-92.072507911857));
#177547=CARTESIAN_POINT('Ctrl Pts',(5.4573415784771,31.1763542226034,-92.0686481149132));
#177548=CARTESIAN_POINT('Ctrl Pts',(5.45721924819772,31.1743593808083,-92.0667182164412));
#177549=CARTESIAN_POINT('Ctrl Pts',(5.45709815159589,31.1723883440164,-92.0647952442053));
#177550=CARTESIAN_POINT('Ctrl Pts',(5.45697825169214,31.1704408029121,-92.0628796526239));
#177551=CARTESIAN_POINT('Ctrl Pts',(5.45689074900465,31.1690194916743,-92.061481658078));
#177552=CARTESIAN_POINT('Ctrl Pts',(5.45684243353217,31.1682316144817,-92.0607031835794));
#177553=CARTESIAN_POINT('Ctrl Pts',(5.45674878977622,31.1667167878402,-92.0591974721066));
#177554=CARTESIAN_POINT('Ctrl Pts',(5.45671411887524,31.1661559345943,-92.0586399936838));
#177555=CARTESIAN_POINT('Ctrl Pts',(5.45667326412361,31.1654956759037,-92.057982576319));
#177556=CARTESIAN_POINT('Ctrl Pts',(5.45662210535926,31.164668359648,-92.0571554655836));
#177557=CARTESIAN_POINT('Ctrl Pts',(5.45476221172077,31.1345910061276,-92.0270855838199));
#177558=CARTESIAN_POINT('Ctrl Pts',(5.45302521158081,31.1066918096424,-91.9953506844654));
#177559=CARTESIAN_POINT('Ctrl Pts',(5.45142749767532,31.0810905033727,-91.9622939859181));
#177560=CARTESIAN_POINT('Ctrl Pts',(5.44981011830393,31.0551740833559,-91.9288304089078));
#177561=CARTESIAN_POINT('Ctrl Pts',(5.44833546364656,31.0316123470578,-91.8940128061608));
#177562=CARTESIAN_POINT('Ctrl Pts',(5.44701370805013,31.0104761931718,-91.8581941654681));
#177563=CARTESIAN_POINT('Ctrl Pts',(5.44567535131068,30.9890745709085,-91.8219256455554));
#177564=CARTESIAN_POINT('Ctrl Pts',(5.44449373720189,30.9701596493975,-91.7846312698169));
#177565=CARTESIAN_POINT('Ctrl Pts',(5.44347271632439,30.9537531147354,-91.7466667565915));
#177566=CARTESIAN_POINT('Ctrl Pts',(5.44243190076202,30.9370285041252,-91.7079662196546));
#177567=CARTESIAN_POINT('Ctrl Pts',(5.44155794121925,30.9229102693208,-91.6685697880071));
#177568=CARTESIAN_POINT('Ctrl Pts',(5.44084832463001,30.911370814837,-91.6288357624295));
#177569=CARTESIAN_POINT('Ctrl Pts',(5.44013077807845,30.8997024069992,-91.5886577092878));
#177570=CARTESIAN_POINT('Ctrl Pts',(5.43958122565515,30.8906703898251,-91.5481348790471));
#177571=CARTESIAN_POINT('Ctrl Pts',(5.43919091728486,30.8841994180308,-91.5076122570601));
#177572=CARTESIAN_POINT('Ctrl Pts',(5.4387941168249,30.8776208130615,-91.4664156129009));
#177573=CARTESIAN_POINT('Ctrl Pts',(5.43856185618865,30.8736887906221,-91.4252195592088));
#177574=CARTESIAN_POINT('Ctrl Pts',(5.43847928442791,30.8722814764636,-91.3843544127705));
#177575=CARTESIAN_POINT('Ctrl Pts',(5.43845605490473,30.8718855634231,-91.3728580142727));
#177576=CARTESIAN_POINT('Ctrl Pts',(5.43844464087176,30.871689229176,-91.3613875941317));
#177577=CARTESIAN_POINT('Ctrl Pts',(5.43844464087133,30.8716892291687,-91.3499500006361));
#177578=CARTESIAN_POINT('',(5.,31.8716754827171,-91.84995));
#177579=CARTESIAN_POINT('Origin',(5.5,31.8716754827171,-91.84995));
#177580=CARTESIAN_POINT('Ctrl Pts',(5.,31.415090518797,-91.1386408691297));
#177581=CARTESIAN_POINT('Ctrl Pts',(5.,31.3430615709327,-91.2919348798756));
#177582=CARTESIAN_POINT('Ctrl Pts',(5.,31.355929990322,-91.4779432828738));
#177583=CARTESIAN_POINT('Ctrl Pts',(5.,31.5391820921123,-91.7616382083514));
#177584=CARTESIAN_POINT('Ctrl Pts',(5.,31.7023337675853,-91.84995));
#177585=CARTESIAN_POINT('Ctrl Pts',(5.,31.8716754827171,-91.84995));
#177586=CARTESIAN_POINT('Origin',(4.5,46.41999998,-92.34995));
#177587=CARTESIAN_POINT('',(5.,46.41999998,-91.84995));
#177588=CARTESIAN_POINT('',(5.,46.41999998,-57.9428177527387));
#177589=CARTESIAN_POINT('',(5.,46.41999998,-57.9628508566217));
#177590=CARTESIAN_POINT('',(4.5,46.91999998,-91.84995));
#177591=CARTESIAN_POINT('Origin',(4.5,46.41999998,-91.84995));
#177592=CARTESIAN_POINT('',(4.5,46.91999998,-57.9428177527387));
#177593=CARTESIAN_POINT('',(4.5,46.91999998,-92.34995));
#177594=CARTESIAN_POINT('Origin',(4.5,46.41999998,-57.9428177527387));
#177595=CARTESIAN_POINT('Origin',(-39.,46.91999998,-129.34995));
#177596=CARTESIAN_POINT('',(4.,46.91999998,-91.84995));
#177597=CARTESIAN_POINT('',(-39.,46.91999998,-91.84995));
#177598=CARTESIAN_POINT('',(4.,46.91999998,-57.9242045702762));
#177599=CARTESIAN_POINT('',(4.,46.91999998,-57.9072287192657));
#177600=CARTESIAN_POINT('Ctrl Pts',(4.,46.91999998,-57.9242045702762));
#177601=CARTESIAN_POINT('Ctrl Pts',(4.16667353124555,46.91999998,-57.9301478976981));
#177602=CARTESIAN_POINT('Ctrl Pts',(4.33333987978916,46.91999998,-57.9363643903873));
#177603=CARTESIAN_POINT('Ctrl Pts',(4.5,46.91999998,-57.9428177527387));
#177604=CARTESIAN_POINT('Origin',(4.,46.41999998,-92.34995));
#177605=CARTESIAN_POINT('',(3.5,46.41999998,-91.84995));
#177606=CARTESIAN_POINT('Origin',(4.,46.41999998,-91.84995));
#177607=CARTESIAN_POINT('',(3.5,46.41999998,-57.9242045702762));
#177608=CARTESIAN_POINT('',(3.5,46.41999998,-92.34995));
#177609=CARTESIAN_POINT('Origin',(4.,46.41999998,-57.9242045702762));
#177610=CARTESIAN_POINT('Ctrl Pts',(41.0540572871253,28.7076050220164,-93.3976987687948));
#177611=CARTESIAN_POINT('Ctrl Pts',(40.9209666515892,28.8387123238495,-93.5739383154377));
#177612=CARTESIAN_POINT('Ctrl Pts',(40.9899542848408,29.0638025010082,-93.6765918018241));
#177613=CARTESIAN_POINT('Ctrl Pts',(40.8263518506557,28.931917162897,-93.0559775318146));
#177614=CARTESIAN_POINT('Ctrl Pts',(40.6946394065552,29.0602110175707,-93.2636650794047));
#177615=CARTESIAN_POINT('Ctrl Pts',(40.7930602005308,29.2900891143653,-93.3836137237161));
#177616=CARTESIAN_POINT('Ctrl Pts',(40.5620537232219,29.1885351995273,-92.7839978150636));
#177617=CARTESIAN_POINT('Ctrl Pts',(40.4345448959912,29.3109818121476,-93.0268336432776));
#177618=CARTESIAN_POINT('Ctrl Pts',(40.5646325235533,29.548843193136,-93.1505624120075));
#177619=CARTESIAN_POINT('Ctrl Pts',(39.979050150362,29.7418321774292,-92.3381410201203));
#177620=CARTESIAN_POINT('Ctrl Pts',(39.8699190705461,29.8439046252157,-92.6499647524336));
#177621=CARTESIAN_POINT('Ctrl Pts',(40.0606440851126,30.1068692044787,-92.7683994467215));
#177622=CARTESIAN_POINT('Ctrl Pts',(39.6579655806366,30.0405777253273,-92.1665648604216));
#177623=CARTESIAN_POINT('Ctrl Pts',(39.5589873293178,30.1314683688792,-92.5153277294035));
#177624=CARTESIAN_POINT('Ctrl Pts',(39.7830757934441,30.4081688522969,-92.6213339269874));
#177625=CARTESIAN_POINT('Ctrl Pts',(39.3277310924369,30.3404619167909,-92.0491293459315));
#177626=CARTESIAN_POINT('Ctrl Pts',(39.2532568247562,30.4080916052286,-92.4345203712043));
#177627=CARTESIAN_POINT('Ctrl Pts',(39.4975990396159,30.7106154376184,-92.5206751536556));
#177628=CARTESIAN_POINT('',(39.4975990396159,30.7106154376184,-92.5206751536556));
#177629=CARTESIAN_POINT('Origin',(39.6638655462185,30.7106154376184,-92.0491293459315));
#177630=CARTESIAN_POINT('',(40.9899542848408,29.0638025010082,-93.6765918018241));
#177631=CARTESIAN_POINT('Origin',(41.4049466656476,29.0638025010082,-93.3976987687947));
#177632=CARTESIAN_POINT('Ctrl Pts',(39.4975990396159,30.7106154376184,-92.5206751536556));
#177633=CARTESIAN_POINT('Ctrl Pts',(39.5502437311338,30.6548413440315,-92.5392376110171));
#177634=CARTESIAN_POINT('Ctrl Pts',(39.6012366148037,30.6005720208656,-92.5588889597982));
#177635=CARTESIAN_POINT('Ctrl Pts',(39.6505780614367,30.5478567214463,-92.5794001703044));
#177636=CARTESIAN_POINT('Ctrl Pts',(39.7019051901957,30.4930199635987,-92.6007368277089));
#177637=CARTESIAN_POINT('Ctrl Pts',(39.7514455416351,30.4398645312726,-92.6230039260027));
#177638=CARTESIAN_POINT('Ctrl Pts',(39.799227420812,30.3884074698674,-92.6459761157129));
#177639=CARTESIAN_POINT('Ctrl Pts',(39.8509326004218,30.332725344175,-92.6708345184267));
#177640=CARTESIAN_POINT('Ctrl Pts',(39.900578831291,30.2790318107528,-92.6965182934803));
#177641=CARTESIAN_POINT('Ctrl Pts',(39.9482309785535,30.2273074761566,-92.7227817257198));
#177642=CARTESIAN_POINT('Ctrl Pts',(39.9787063007134,30.194227838598,-92.7395781683673));
#177643=CARTESIAN_POINT('Ctrl Pts',(40.0083613832834,30.161958444705,-92.7566098271306));
#177644=CARTESIAN_POINT('Ctrl Pts',(40.0372057906019,30.1305006022898,-92.7738119274539));
#177645=CARTESIAN_POINT('Ctrl Pts',(40.0970075868769,30.0652804900306,-92.8094762587635));
#177646=CARTESIAN_POINT('Ctrl Pts',(40.1533265445702,30.0035479209865,-92.8458721381057));
#177647=CARTESIAN_POINT('Ctrl Pts',(40.2062866145755,29.945258258757,-92.8824715547153));
#177648=CARTESIAN_POINT('Ctrl Pts',(40.2376516594108,29.9107368189424,-92.9041471745321));
#177649=CARTESIAN_POINT('Ctrl Pts',(40.2678386038127,29.877422603041,-92.925894814687));
#177650=CARTESIAN_POINT('Ctrl Pts',(40.2968760309461,29.8453006562658,-92.9476110057979));
#177651=CARTESIAN_POINT('Ctrl Pts',(40.2997081664554,29.8421676753142,-92.9497290721021));
#177652=CARTESIAN_POINT('Ctrl Pts',(40.3015941680139,29.8400809906412,-92.9511431029648));
#177653=CARTESIAN_POINT('Ctrl Pts',(40.3049675683909,29.8363475009641,-92.953683917945));
#177654=CARTESIAN_POINT('Ctrl Pts',(40.3054835593242,29.8357764312398,-92.9540725576991));
#177655=CARTESIAN_POINT('Ctrl Pts',(40.306034306853,29.8351668697406,-92.95448763497));
#177656=CARTESIAN_POINT('Ctrl Pts',(40.3066284628192,29.8345092283034,-92.9549358002383));
#177657=CARTESIAN_POINT('Ctrl Pts',(40.3086347740026,29.8322885430872,-92.9564491385554));
#177658=CARTESIAN_POINT('Ctrl Pts',(40.3106380437744,29.8300708433843,-92.9579641773452));
#177659=CARTESIAN_POINT('Ctrl Pts',(40.3126382671633,29.8278561371225,-92.9594809011795));
#177660=CARTESIAN_POINT('Ctrl Pts',(40.3644584567136,29.7704792966522,-92.9987749705472));
#177661=CARTESIAN_POINT('Ctrl Pts',(40.4143172745278,29.7150280799745,-93.0391169254633));
#177662=CARTESIAN_POINT('Ctrl Pts',(40.4622134803595,29.6615579422969,-93.0804043143038));
#177663=CARTESIAN_POINT('Ctrl Pts',(40.5106606856377,29.6074726824868,-93.122166674554));
#177664=CARTESIAN_POINT('Ctrl Pts',(40.5570999020178,29.5554143181597,-93.164896282026));
#177665=CARTESIAN_POINT('Ctrl Pts',(40.6015490772091,29.5054130210184,-93.2084453489337));
#177666=CARTESIAN_POINT('Ctrl Pts',(40.6471301804922,29.4541384072719,-93.2531034220713));
#177667=CARTESIAN_POINT('Ctrl Pts',(40.690618621974,29.4050269608719,-93.2986231900119));
#177668=CARTESIAN_POINT('Ctrl Pts',(40.7320534431439,29.3580828825712,-93.3448022074815));
#177669=CARTESIAN_POINT('Ctrl Pts',(40.774314355202,29.310202874677,-93.3919019014374));
#177670=CARTESIAN_POINT('Ctrl Pts',(40.8144390257268,29.264577440295,-93.4396872428883));
#177671=CARTESIAN_POINT('Ctrl Pts',(40.8524882640605,29.2211825760875,-93.4879006275346));
#177672=CARTESIAN_POINT('Ctrl Pts',(40.8920154539822,29.1761021194406,-93.5379867710458));
#177673=CARTESIAN_POINT('Ctrl Pts',(40.929302926327,29.1334288224211,-93.588534721447));
#177674=CARTESIAN_POINT('Ctrl Pts',(40.964438429471,29.0931062913192,-93.6392119293362));
#177675=CARTESIAN_POINT('Ctrl Pts',(40.9730731090496,29.0831968804752,-93.6516660402185));
#177676=CARTESIAN_POINT('Ctrl Pts',(40.9815779064276,29.0734293123152,-93.664127764331));
#177677=CARTESIAN_POINT('Ctrl Pts',(40.9899542848408,29.0638025010082,-93.6765918018241));
#177678=CARTESIAN_POINT('Ctrl Pts',(39.3571428571429,31.080768958446,-92.4750054575003));
#177679=CARTESIAN_POINT('Ctrl Pts',(39.,31.080768958446,-92.3685260300003));
#177680=CARTESIAN_POINT('Ctrl Pts',(39.,31.080768958446,-91.9958480337503));
#177681=CARTESIAN_POINT('Ctrl Pts',(39.3571429430277,30.9391538899445,-92.4750054831062));
#177682=CARTESIAN_POINT('Ctrl Pts',(39.0000001561187,30.8288322275033,-92.3685260646169));
#177683=CARTESIAN_POINT('Ctrl Pts',(39.,30.7973529986378,-91.9958480635187));
#177684=CARTESIAN_POINT('Ctrl Pts',(39.410274588038,30.8031308123719,-92.4898846529936));
#177685=CARTESIAN_POINT('Ctrl Pts',(39.0995023767794,30.5843250255347,-92.3886066067861));
#177686=CARTESIAN_POINT('Ctrl Pts',(39.1237015311635,30.5257400818631,-92.0131591004063));
#177687=CARTESIAN_POINT('Ctrl Pts',(39.4975990396159,30.7106154376184,-92.5206751536556));
#177688=CARTESIAN_POINT('Ctrl Pts',(39.2532568247562,30.4080916052285,-92.4345203712043));
#177689=CARTESIAN_POINT('Ctrl Pts',(39.3277310924369,30.3404619167909,-92.0491293459315));
#177690=CARTESIAN_POINT('',(39.3571428571429,31.080768958446,-92.4750054575003));
#177691=CARTESIAN_POINT('Origin',(39.5,31.080768958446,-91.9958480337503));
#177692=CARTESIAN_POINT('Ctrl Pts',(39.3571428571429,31.080768958446,-92.4750054575003));
#177693=CARTESIAN_POINT('Ctrl Pts',(39.3571428624528,31.0720133575057,-92.4750054590834));
#177694=CARTESIAN_POINT('Ctrl Pts',(39.3573458482566,31.0633092009137,-92.4750623091666));
#177695=CARTESIAN_POINT('Ctrl Pts',(39.3577390766937,31.0546580420142,-92.475173820379));
#177696=CARTESIAN_POINT('Ctrl Pts',(39.3586243755247,31.0351811676592,-92.4754248722785));
#177697=CARTESIAN_POINT('Ctrl Pts',(39.3604436448217,31.0159715870608,-92.4759439815933));
#177698=CARTESIAN_POINT('Ctrl Pts',(39.3631916882095,30.9970230542622,-92.476746763375));
#177699=CARTESIAN_POINT('Ctrl Pts',(39.3641054890546,30.9907221401785,-92.4770137106414));
#177700=CARTESIAN_POINT('Ctrl Pts',(39.3651223182342,30.9844503546779,-92.4773121194727));
#177701=CARTESIAN_POINT('Ctrl Pts',(39.3662428843127,30.9782083090249,-92.4776428409703));
#177702=CARTESIAN_POINT('Ctrl Pts',(39.3683883585622,30.9662570743143,-92.4782760516934));
#177703=CARTESIAN_POINT('Ctrl Pts',(39.3708845217043,30.9545679259021,-92.4790189420789));
#177704=CARTESIAN_POINT('Ctrl Pts',(39.3737461808994,30.9429694337232,-92.4798801534962));
#177705=CARTESIAN_POINT('Ctrl Pts',(39.3765700228016,30.9315242175094,-92.4807299838641));
#177706=CARTESIAN_POINT('Ctrl Pts',(39.3797500540198,30.9201667541774,-92.481695025529));
#177707=CARTESIAN_POINT('Ctrl Pts',(39.3833449200573,30.9087492309475,-92.482798172154));
#177708=CARTESIAN_POINT('Ctrl Pts',(39.3862733107318,30.8994484758694,-92.4836967993228));
#177709=CARTESIAN_POINT('Ctrl Pts',(39.3894777725275,30.8901079961926,-92.4846873039166));
#177710=CARTESIAN_POINT('Ctrl Pts',(39.3930110105606,30.8806604192302,-92.4857896691593));
#177711=CARTESIAN_POINT('Ctrl Pts',(39.3991440441352,30.8642612108655,-92.4877031669144));
#177712=CARTESIAN_POINT('Ctrl Pts',(39.4059290901326,30.8484191983756,-92.4898483081196));
#177713=CARTESIAN_POINT('Ctrl Pts',(39.4133615041905,30.833134388963,-92.492236979355));
#177714=CARTESIAN_POINT('Ctrl Pts',(39.418935814734,30.8216707819036,-92.4940284827816));
#177715=CARTESIAN_POINT('Ctrl Pts',(39.4248742687166,30.8105206008932,-92.495956985567));
#177716=CARTESIAN_POINT('Ctrl Pts',(39.4311748370853,30.7996838446308,-92.4980279306107));
#177717=CARTESIAN_POINT('Ctrl Pts',(39.4406256896384,30.7834287102371,-92.5011343481761));
#177718=CARTESIAN_POINT('Ctrl Pts',(39.4508913265187,30.7678787816064,-92.5045611481668));
#177719=CARTESIAN_POINT('Ctrl Pts',(39.4619645235623,30.753034049853,-92.5083285582182));
#177720=CARTESIAN_POINT('Ctrl Pts',(39.4675011220841,30.7456116839763,-92.5102122632439));
#177721=CARTESIAN_POINT('Ctrl Pts',(39.4732396026272,30.7383656171964,-92.5121811573189));
#177722=CARTESIAN_POINT('Ctrl Pts',(39.4791790118521,30.7312958485624,-92.5142379855905));
#177723=CARTESIAN_POINT('Ctrl Pts',(39.485118421077,30.7242260799284,-92.516294813862));
#177724=CARTESIAN_POINT('Ctrl Pts',(39.4912587585353,30.7173326092718,-92.5184395778772));
#177725=CARTESIAN_POINT('Ctrl Pts',(39.4975990396159,30.7106154376184,-92.5206751536556));
#177726=CARTESIAN_POINT('Origin',(39.5,58.91999998,-91.9958480337503));
#177727=CARTESIAN_POINT('',(39.3571428571429,46.41999998,-92.4750054575003));
#177728=CARTESIAN_POINT('Origin',(39.5,46.41999998,-91.9958480337503));
#177729=CARTESIAN_POINT('',(39.,46.41999998,-91.9958480337503));
#177730=CARTESIAN_POINT('',(39.3571428571429,58.91999998,-92.4750054575003));
#177731=CARTESIAN_POINT('Origin',(38.5,28.91999998,-95.34995));
#177732=CARTESIAN_POINT('',(41.2907166092886,28.91999998,-94.2490863360338));
#177733=CARTESIAN_POINT('Origin',(41.75583604417,28.91999998,-94.0656090587062));
#177734=CARTESIAN_POINT('Origin',(38.5,28.41999998,-95.34995));
#177735=CARTESIAN_POINT('Origin',(38.5,28.91999998,-95.34995));
#177736=CARTESIAN_POINT('Ctrl Pts',(40.9899542848408,29.0638025010082,-93.6765918018241));
#177737=CARTESIAN_POINT('Ctrl Pts',(40.9209666515892,28.8387123238495,-93.5739383154377));
#177738=CARTESIAN_POINT('Ctrl Pts',(41.0540572871253,28.7076050220164,-93.3976987687948));
#177739=CARTESIAN_POINT('Ctrl Pts',(41.0445777715999,29.0010249744694,-93.7578714615268));
#177740=CARTESIAN_POINT('Ctrl Pts',(40.9927653037546,28.7197223139655,-93.6733291751567));
#177741=CARTESIAN_POINT('Ctrl Pts',(41.181465342889,28.5820956174237,-93.4924903917862));
#177742=CARTESIAN_POINT('Ctrl Pts',(41.1012013116007,28.9670983124193,-93.8513385014916));
#177743=CARTESIAN_POINT('Ctrl Pts',(41.064373682842,28.640994986895,-93.7860557549848));
#177744=CARTESIAN_POINT('Ctrl Pts',(41.3136336664734,28.5141965951637,-93.601569918277));
#177745=CARTESIAN_POINT('Ctrl Pts',(41.203906529354,28.9262911739198,-94.0457359962981));
#177746=CARTESIAN_POINT('Ctrl Pts',(41.1909352247283,28.5106646509549,-94.0164009875504));
#177747=CARTESIAN_POINT('Ctrl Pts',(41.5532792074141,28.4325824175145,-93.828366995811));
#177748=CARTESIAN_POINT('Ctrl Pts',(41.2500626594833,28.9199999557335,-94.1460275680244));
#177749=CARTESIAN_POINT('Ctrl Pts',(41.245616944193,28.4623003387481,-94.1347575623882));
#177750=CARTESIAN_POINT('Ctrl Pts',(41.6609761593771,28.4199999800001,-93.9453729847263));
#177751=CARTESIAN_POINT('Ctrl Pts',(41.2907166092886,28.91999998,-94.2490863360339));
#177752=CARTESIAN_POINT('Ctrl Pts',(41.2907166092886,28.4199999800001,-94.2490863360339));
#177753=CARTESIAN_POINT('Ctrl Pts',(41.7558360441699,28.41999998,-94.0656090587062));
#177754=CARTESIAN_POINT('Ctrl Pts',(40.9899542848408,29.0638025010082,-93.6765918018241));
#177755=CARTESIAN_POINT('Ctrl Pts',(41.0017693811953,29.0502236370209,-93.6941726460364));
#177756=CARTESIAN_POINT('Ctrl Pts',(41.0140708376759,29.0375478614379,-93.7129059904779));
#177757=CARTESIAN_POINT('Ctrl Pts',(41.0268202538681,29.0258419966797,-93.7328567862257));
#177758=CARTESIAN_POINT('Ctrl Pts',(41.0391013343248,29.0145661339467,-93.7520747115062));
#177759=CARTESIAN_POINT('Ctrl Pts',(41.0517974761858,29.0041919373727,-93.7724211552444));
#177760=CARTESIAN_POINT('Ctrl Pts',(41.0648448407171,28.9947506178104,-93.7939356517422));
#177761=CARTESIAN_POINT('Ctrl Pts',(41.0769698659622,28.9859767203872,-93.8139292537102));
#177762=CARTESIAN_POINT('Ctrl Pts',(41.0893969827306,28.978009516043,-93.8349292598603));
#177763=CARTESIAN_POINT('Ctrl Pts',(41.1020540344261,28.970836888857,-93.8569624977988));
#177764=CARTESIAN_POINT('Ctrl Pts',(41.114660062725,28.9636931761299,-93.8789069148439));
#177765=CARTESIAN_POINT('Ctrl Pts',(41.1274932261777,28.9573390332433,-93.9018734002197));
#177766=CARTESIAN_POINT('Ctrl Pts',(41.1404601253197,28.9517165675485,-93.9258935221142));
#177767=CARTESIAN_POINT('Ctrl Pts',(41.1426479037218,28.9507679437581,-93.9299462029689));
#177768=CARTESIAN_POINT('Ctrl Pts',(41.1451435660091,28.949712012454,-93.9345963342413));
#177769=CARTESIAN_POINT('Ctrl Pts',(41.1473963625423,28.9487825885311,-93.938820756772));
#177770=CARTESIAN_POINT('Ctrl Pts',(41.1488876270705,28.9481673456952,-93.9416171617641));
#177771=CARTESIAN_POINT('Ctrl Pts',(41.1502729027338,28.9476061534381,-93.9442266086178));
#177772=CARTESIAN_POINT('Ctrl Pts',(41.1513966516507,28.9471554910944,-93.9463491184234));
#177773=CARTESIAN_POINT('Ctrl Pts',(41.151782175637,28.9470008825865,-93.947077286815));
#177774=CARTESIAN_POINT('Ctrl Pts',(41.1521678999204,28.9468468449385,-93.9478066003647));
#177775=CARTESIAN_POINT('Ctrl Pts',(41.152553818993,28.9466933775795,-93.9485370568041));
#177776=CARTESIAN_POINT('Ctrl Pts',(41.1650174545953,28.9417369984439,-93.972127865167));
#177777=CARTESIAN_POINT('Ctrl Pts',(41.177689249371,28.937413983186,-93.996873043816));
#177778=CARTESIAN_POINT('Ctrl Pts',(41.1904798430551,28.9337971267814,-94.0228026361174));
#177779=CARTESIAN_POINT('Ctrl Pts',(41.2027935565744,28.9303151200265,-94.0477654782778));
#177780=CARTESIAN_POINT('Ctrl Pts',(41.2152173467937,28.9274879657075,-94.0738260971387));
#177781=CARTESIAN_POINT('Ctrl Pts',(41.2276649958569,28.9253345395707,-94.1010116186227));
#177782=CARTESIAN_POINT('Ctrl Pts',(41.239510966971,28.92328520289,-94.1268830824301));
#177783=CARTESIAN_POINT('Ctrl Pts',(41.2513785111291,28.9218461913099,-94.153773355429));
#177784=CARTESIAN_POINT('Ctrl Pts',(41.2631878035387,28.9209877361867,-94.181705677918));
#177785=CARTESIAN_POINT('Ctrl Pts',(41.2724131953157,28.9203171130402,-94.2035263433116));
#177786=CARTESIAN_POINT('Ctrl Pts',(41.2816029331176,28.91999997456,-94.2259829415861));
#177787=CARTESIAN_POINT('Ctrl Pts',(41.2907166092885,28.91999998,-94.2490863360338));
#177788=CARTESIAN_POINT('Ctrl Pts',(38.9935757799223,46.3414635373644,-91.9917603781375));
#177789=CARTESIAN_POINT('Ctrl Pts',(38.9900733339343,46.3237628848257,-92.3673479459613));
#177790=CARTESIAN_POINT('Ctrl Pts',(39.3465508854728,46.2628551564744,-92.471625094235));
#177791=CARTESIAN_POINT('Ctrl Pts',(39.0086597700523,46.4322161067703,-92.0014907415683));
#177792=CARTESIAN_POINT('Ctrl Pts',(39.0135957341955,46.4340914316513,-92.3710345401694));
#177793=CARTESIAN_POINT('Ctrl Pts',(39.372415088039,46.4444445610447,-92.4799718784786));
#177794=CARTESIAN_POINT('Ctrl Pts',(38.9968525252245,46.5274603514191,-91.9931823769061));
#177795=CARTESIAN_POINT('Ctrl Pts',(38.9935526885049,46.5545728778829,-92.3674784092348));
#177796=CARTESIAN_POINT('Ctrl Pts',(39.352171245683,46.6350158585226,-92.472845419099));
#177797=CARTESIAN_POINT('Ctrl Pts',(38.9364433009268,46.6726027208644,-91.9601428292582));
#177798=CARTESIAN_POINT('Ctrl Pts',(38.911047638376,46.7195613858442,-92.3581836088519));
#177799=CARTESIAN_POINT('Ctrl Pts',(39.248577561246,46.9254427981845,-92.4445007012883));
#177800=CARTESIAN_POINT('Ctrl Pts',(38.8992979918264,46.7278476911263,-91.9409870962964));
#177801=CARTESIAN_POINT('Ctrl Pts',(38.8613543660254,46.7770521061531,-92.3536048202297));
#177802=CARTESIAN_POINT('Ctrl Pts',(39.1848780116966,47.0359893155312,-92.4280665419693));
#177803=CARTESIAN_POINT('Ctrl Pts',(38.8075082704007,46.819559441354,-91.903134346114));
#177804=CARTESIAN_POINT('Ctrl Pts',(38.7552065584773,46.8601509227914,-92.3483332716903));
#177805=CARTESIAN_POINT('Ctrl Pts',(39.0274561372425,47.2195137681446,-92.3955887391387));
#177806=CARTESIAN_POINT('Ctrl Pts',(38.7519713842669,46.8567503512399,-91.884306817494));
#177807=CARTESIAN_POINT('Ctrl Pts',(38.698339541767,46.8858041857146,-92.3478246517919));
#177808=CARTESIAN_POINT('Ctrl Pts',(38.9322034872781,47.2939415269622,-92.3794330966327));
#177809=CARTESIAN_POINT('Ctrl Pts',(38.6076467465342,46.9167126634347,-91.8524730691734));
#177810=CARTESIAN_POINT('Ctrl Pts',(38.5727409105641,46.9214414682097,-92.3493758984604));
#177811=CARTESIAN_POINT('Ctrl Pts',(38.6846545006084,47.4139412866979,-92.3521157644398));
#177812=CARTESIAN_POINT('Ctrl Pts',(38.5109178162184,46.9287522863742,-91.8445567093303));
#177813=CARTESIAN_POINT('Ctrl Pts',(38.5081212350499,46.9220589191625,-92.3516898082073));
#177814=CARTESIAN_POINT('Ctrl Pts',(38.5187272696553,47.4380404247362,-92.345320843866));
#177815=CARTESIAN_POINT('Ctrl Pts',(38.4229506706146,46.9135241055511,-91.8538609392359));
#177816=CARTESIAN_POINT('Ctrl Pts',(38.4459457313602,46.9181397812628,-92.3496852111588));
#177817=CARTESIAN_POINT('Ctrl Pts',(38.3678334725473,47.4075618803718,-92.353306306564));
#177818=CARTESIAN_POINT('',(38.5,47.41999998,-92.34995));
#177819=CARTESIAN_POINT('Origin',(38.5,47.41999998,-91.84995));
#177820=CARTESIAN_POINT('Ctrl Pts',(38.5,47.41999998,-92.34995));
#177821=CARTESIAN_POINT('Ctrl Pts',(38.6219812275058,47.41999998,-92.34995));
#177822=CARTESIAN_POINT('Ctrl Pts',(38.7465335263591,47.3872258650965,-92.3582058121698));
#177823=CARTESIAN_POINT('Ctrl Pts',(38.904967841915,47.3039420525654,-92.3769331713773));
#177824=CARTESIAN_POINT('Ctrl Pts',(38.9543966496893,47.2707466454047,-92.3841945628516));
#177825=CARTESIAN_POINT('Ctrl Pts',(39.0234767926682,47.2128023301881,-92.395882049767));
#177826=CARTESIAN_POINT('Ctrl Pts',(39.0456603010004,47.19212902437,-92.3999114754588));
#177827=CARTESIAN_POINT('Ctrl Pts',(39.0883490971152,47.1480653445753,-92.408127809539));
#177828=CARTESIAN_POINT('Ctrl Pts',(39.1098053189841,47.1234786494394,-92.4125184625557));
#177829=CARTESIAN_POINT('Ctrl Pts',(39.1659681949264,47.0528208887496,-92.4245521432492));
#177830=CARTESIAN_POINT('Ctrl Pts',(39.1988865967866,47.0026358634964,-92.4323449540457));
#177831=CARTESIAN_POINT('Ctrl Pts',(39.2558436333345,46.8961061100704,-92.446579186395));
#177832=CARTESIAN_POINT('Ctrl Pts',(39.280342254491,46.8383758180937,-92.4531476926319));
#177833=CARTESIAN_POINT('Ctrl Pts',(39.3380013103976,46.6642587706065,-92.4690917299284));
#177834=CARTESIAN_POINT('Ctrl Pts',(39.3570864259713,46.5441464965183,-92.4749886329755));
#177835=CARTESIAN_POINT('Ctrl Pts',(39.3571428571429,46.41999998,-92.4750054575003));
#177836=CARTESIAN_POINT('Origin',(-39.,46.91999998,-129.34995));
#177837=CARTESIAN_POINT('',(38.,46.91999998,-91.84995));
#177838=CARTESIAN_POINT('',(-39.,46.91999998,-91.84995));
#177839=CARTESIAN_POINT('',(38.,46.91999998,-58.24995));
#177840=CARTESIAN_POINT('Origin',(38.,46.41999998,-92.34995));
#177841=CARTESIAN_POINT('',(37.5,46.41999998,-91.84995));
#177842=CARTESIAN_POINT('Origin',(38.,46.41999998,-91.84995));
#177843=CARTESIAN_POINT('',(37.5,46.41999998,-92.34995));
#177844=CARTESIAN_POINT('Origin',(24.7,-70.08000002,-58.24995));
#177845=CARTESIAN_POINT('',(25.2,-70.08000002,-55.74995));
#177846=CARTESIAN_POINT('Origin',(25.2,-70.08000002,-58.24995));
#177847=CARTESIAN_POINT('',(24.7,-70.08000002,-55.24995));
#177848=CARTESIAN_POINT('Origin',(24.7,-70.08000002,-55.74995));
#177849=CARTESIAN_POINT('Origin',(24.7,-70.08000002,-58.24995));
#177850=CARTESIAN_POINT('Origin',(-3.3975957231091E-14,-70.08000002,-58.24995));
#177851=CARTESIAN_POINT('',(41.5,-70.08000002,-55.24995));
#177852=CARTESIAN_POINT('Origin',(-1.8445455022812E-14,-55.08000002,-61.14995));
#177853=CARTESIAN_POINT('',(50.4435446592566,-54.58000002,-61.14995));
#177854=CARTESIAN_POINT('',(60.,-54.58000002,-61.14995));
#177855=CARTESIAN_POINT('',(50.4435446592566,-55.08000002,-60.64995));
#177856=CARTESIAN_POINT('Origin',(50.4435446592566,-55.08000002,-61.14995));
#177857=CARTESIAN_POINT('',(-1.8445455022812E-14,-55.08000002,-60.64995));
#177858=CARTESIAN_POINT('Origin',(44.5079524583206,-57.4754524783489,-52.64995));
#177859=CARTESIAN_POINT('',(44.5079524583206,-60.2254524783489,-55.24995));
#177860=CARTESIAN_POINT('Origin',(44.5079524583206,-57.4754524783489,-55.24995));
#177861=CARTESIAN_POINT('',(44.5079524583206,-60.2254524783489,-60.64995));
#177862=CARTESIAN_POINT('',(44.5079524583206,-60.2254524783489,-52.64995));
#177863=CARTESIAN_POINT('Origin',(44.5079524583206,-57.4754524783489,-60.64995));
#177864=CARTESIAN_POINT('Origin',(44.5079524583206,-57.4754524783489,-60.64995));
#177865=CARTESIAN_POINT('Origin',(0.,45.41999998,-55.24995));
#177866=CARTESIAN_POINT('',(44.5079524583206,-59.475452478349,-55.24995));
#177867=CARTESIAN_POINT('Origin',(44.5079524583206,-57.4754524783489,-55.24995));
#177868=CARTESIAN_POINT('Origin',(44.5079524583206,-57.475452478349,235.35105));
#177869=CARTESIAN_POINT('',(44.5079524583206,-59.475452478349,-52.64995));
#177870=CARTESIAN_POINT('Origin',(44.5079524583206,-57.4754524783489,-52.64995));
#177871=CARTESIAN_POINT('',(44.5079524583206,-59.475452478349,235.35105));
#177872=CARTESIAN_POINT('Origin',(42.,-12.9675000200281,-61.14995));
#177873=CARTESIAN_POINT('',(42.,-63.4208871539288,-60.64995));
#177874=CARTESIAN_POINT('',(41.5,-63.4208871539288,-61.14995));
#177875=CARTESIAN_POINT('Origin',(42.,-63.4208871539288,-61.14995));
#177876=CARTESIAN_POINT('',(41.5,-73.08000002,-61.14995));
#177877=CARTESIAN_POINT('',(42.,-12.9675000200281,-60.64995));
#177878=CARTESIAN_POINT('Origin',(39.5,46.91999998,-61.14995));
#177879=CARTESIAN_POINT('',(39.5,31.080768958446,-60.64995));
#177880=CARTESIAN_POINT('Origin',(39.5,31.080768958446,-61.14995));
#177881=CARTESIAN_POINT('',(39.,37.7046087726872,-61.14995));
#177882=CARTESIAN_POINT('',(39.,31.080768958446,-61.14995));
#177883=CARTESIAN_POINT('',(39.5,37.7046087726872,-60.64995));
#177884=CARTESIAN_POINT('Origin',(39.5,37.7046087726872,-61.14995));
#177885=CARTESIAN_POINT('',(39.5,37.7483531044501,-60.64995));
#177886=CARTESIAN_POINT('Ctrl Pts',(39.6638655462185,30.7106154376184,-60.64995));
#177887=CARTESIAN_POINT('Ctrl Pts',(39.5,30.859420873127,-60.64995));
#177888=CARTESIAN_POINT('Ctrl Pts',(39.5,31.080768958446,-60.64995));
#177889=CARTESIAN_POINT('Ctrl Pts',(39.327731092437,30.3404619167909,-60.64995));
#177890=CARTESIAN_POINT('Ctrl Pts',(39.,30.638072787808,-60.64995));
#177891=CARTESIAN_POINT('Ctrl Pts',(39.,31.080768958446,-60.64995));
#177892=CARTESIAN_POINT('Ctrl Pts',(39.327731092437,30.3404619167909,-61.14995));
#177893=CARTESIAN_POINT('Ctrl Pts',(39.,30.638072787808,-61.14995));
#177894=CARTESIAN_POINT('Ctrl Pts',(39.,31.080768958446,-61.14995));
#177895=CARTESIAN_POINT('',(39.6638655462185,30.7106154376184,-60.64995));
#177896=CARTESIAN_POINT('Origin',(39.6638655462185,30.7106154376184,-61.14995));
#177897=CARTESIAN_POINT('Origin',(40.,31.080768958446,-60.64995));
#177898=CARTESIAN_POINT('Origin',(0.,-12.9675000200281,-61.14995));
#177899=CARTESIAN_POINT('',(41.4049466656476,29.0638025010082,-60.64995));
#177900=CARTESIAN_POINT('Origin',(41.4049466656476,29.0638025010082,-61.14995));
#177901=CARTESIAN_POINT('Origin',(0.,-12.9675000200281,-60.64995));
#177902=CARTESIAN_POINT('Ctrl Pts',(41.7558360441701,28.91999998,-60.64995));
#177903=CARTESIAN_POINT('Ctrl Pts',(41.5509245680609,28.91999998,-60.64995));
#177904=CARTESIAN_POINT('Ctrl Pts',(41.4049466656477,29.0638025010082,-60.64995));
#177905=CARTESIAN_POINT('Ctrl Pts',(41.7558360441701,28.41999998,-60.64995));
#177906=CARTESIAN_POINT('Ctrl Pts',(41.3460130919516,28.41999998,-60.64995));
#177907=CARTESIAN_POINT('Ctrl Pts',(41.0540572871252,28.7076050220163,-60.64995));
#177908=CARTESIAN_POINT('Ctrl Pts',(41.7558360441701,28.41999998,-61.14995));
#177909=CARTESIAN_POINT('Ctrl Pts',(41.3460130919516,28.41999998,-61.14995));
#177910=CARTESIAN_POINT('Ctrl Pts',(41.0540572871252,28.7076050220163,-61.14995));
#177911=CARTESIAN_POINT('',(41.7558360441701,28.91999998,-60.64995));
#177912=CARTESIAN_POINT('Origin',(41.7558360441701,28.91999998,-61.14995));
#177913=CARTESIAN_POINT('Origin',(41.7558360441701,29.41999998,-60.64995));
#177914=CARTESIAN_POINT('Origin',(1.8346904061005E-14,28.9199999800001,
-61.14995));
#177915=CARTESIAN_POINT('',(60.,28.41999998,-61.14995));
#177916=CARTESIAN_POINT('',(1.8346904061005E-14,28.9199999800001,-60.64995));
#177917=CARTESIAN_POINT('Origin',(44.5079524583208,31.5404524382925,-52.64995));
#177918=CARTESIAN_POINT('',(44.5079524583208,28.7904524382925,-55.24995));
#177919=CARTESIAN_POINT('Origin',(44.5079524583208,31.5404524382925,-55.24995));
#177920=CARTESIAN_POINT('',(44.5079524583208,28.7904524382925,-52.64995));
#177921=CARTESIAN_POINT('Origin',(44.5079524583208,31.5404524382925,-60.64995));
#177922=CARTESIAN_POINT('Origin',(0.,45.41999998,-55.24995));
#177923=CARTESIAN_POINT('',(44.5079524583208,29.5404524382925,-55.24995));
#177924=CARTESIAN_POINT('Origin',(44.5079524583208,31.5404524382925,-55.24995));
#177925=CARTESIAN_POINT('Origin',(44.5079524583208,31.5404524382925,235.35105));
#177926=CARTESIAN_POINT('',(44.5079524583208,29.5404524382925,-52.64995));
#177927=CARTESIAN_POINT('Origin',(44.5079524583208,31.5404524382925,-52.64995));
#177928=CARTESIAN_POINT('',(44.5079524583208,29.5404524382925,235.35105));
#177929=CARTESIAN_POINT('Origin',(1.8346904061005E-14,28.9199999800001,
-61.14995));
#177930=CARTESIAN_POINT('',(50.4632296085449,28.91999998,-60.64995));
#177931=CARTESIAN_POINT('',(1.8346904061005E-14,28.9199999800001,-60.64995));
#177932=CARTESIAN_POINT('',(50.4632296085449,28.41999998,-61.14995));
#177933=CARTESIAN_POINT('Origin',(50.4632296085449,28.91999998,-61.14995));
#177934=CARTESIAN_POINT('',(60.,28.41999998,-61.14995));
#177935=CARTESIAN_POINT('Origin',(0.,-12.9675000200281,-60.64995));
#177936=CARTESIAN_POINT('',(51.6244217512083,-41.5825130958571,-60.64995));
#177937=CARTESIAN_POINT('',(53.7167487055513,-17.6671065732338,-60.64995));
#177938=CARTESIAN_POINT('Origin',(0.,-12.9675000200281,-60.64995));
#177939=CARTESIAN_POINT('Origin',(-83.2809572255632,-44.93000002,-55.2499500000007));
#177940=CARTESIAN_POINT('',(52.8810286821225,-44.93000002,-59.64995));
#177941=CARTESIAN_POINT('Ctrl Pts',(51.3752989258075,-44.93000002,-61.14995));
#177942=CARTESIAN_POINT('Ctrl Pts',(51.5724340164545,-44.93000002,-61.149949999985));
#177943=CARTESIAN_POINT('Ctrl Pts',(51.7694205173407,-44.93000002,-61.1109090094727));
#177944=CARTESIAN_POINT('Ctrl Pts',(52.1336129969961,-44.93000002,-60.9606295880612));
#177945=CARTESIAN_POINT('Ctrl Pts',(52.3006402190038,-44.93000002,-60.8494502533521));
#177946=CARTESIAN_POINT('Ctrl Pts',(52.5793810752606,-44.93000002,-60.5717700902076));
#177947=CARTESIAN_POINT('Ctrl Pts',(52.6909850969965,-44.93000002,-60.4053784571342));
#177948=CARTESIAN_POINT('Ctrl Pts',(52.8418385613238,-44.93000002,-60.0425718399611));
#177949=CARTESIAN_POINT('Ctrl Pts',(52.8810286821055,-44.93000002,-59.8463349320562));
#177950=CARTESIAN_POINT('Ctrl Pts',(52.8810286821225,-44.93000002,-59.64995));
#177951=CARTESIAN_POINT('',(52.8810286821225,-44.93000002,-55.74995));
#177952=CARTESIAN_POINT('',(52.8810286821225,-44.93000002,-55.2499500000007));
#177953=CARTESIAN_POINT('',(-83.2809572255632,-44.93000002,-55.74995));
#177954=CARTESIAN_POINT('Ctrl Pts',(51.375172246442,-44.93000002,-61.1499499946262));
#177955=CARTESIAN_POINT('Ctrl Pts',(51.3752141318477,-44.93000002,-60.6498941830801));
#177956=CARTESIAN_POINT('Ctrl Pts',(51.3752141521426,-44.4299442087041,
-60.6499499995188));
#177957=CARTESIAN_POINT('Ctrl Pts',(51.5723496265306,-44.93000002,-61.1499667235334));
#177958=CARTESIAN_POINT('Ctrl Pts',(51.5079545643181,-44.9300000200007,
-60.6441634129642));
#177959=CARTESIAN_POINT('Ctrl Pts',(51.5071649062657,-44.424237291042,-60.6499618311935));
#177960=CARTESIAN_POINT('Ctrl Pts',(51.7693815122227,-44.93000002,-61.1109251044414));
#177961=CARTESIAN_POINT('Ctrl Pts',(51.637293275499,-44.9300000200007,-60.6119868070537));
#177962=CARTESIAN_POINT('Ctrl Pts',(51.6390186853523,-44.4185345954033,
-60.6239348042612));
#177963=CARTESIAN_POINT('Ctrl Pts',(52.1336129969961,-44.93000002,-60.9606295880612));
#177964=CARTESIAN_POINT('Ctrl Pts',(51.8725693108456,-44.9300000199993,
-60.5030970594193));
#177965=CARTESIAN_POINT('Ctrl Pts',(51.8827629060799,-44.4079926660298,
-60.5237387895065));
#177966=CARTESIAN_POINT('Ctrl Pts',(52.3006402190038,-44.93000002,-60.8494502533521));
#177967=CARTESIAN_POINT('Ctrl Pts',(51.977992200991,-44.93000002,-60.4261477374103));
#177968=CARTESIAN_POINT('Ctrl Pts',(51.9945380358051,-44.4031584192941,
-60.4496195485704));
#177969=CARTESIAN_POINT('Ctrl Pts',(52.5793810752606,-44.93000002,-60.5717700902076));
#177970=CARTESIAN_POINT('Ctrl Pts',(52.1520057930301,-44.93000002,-60.2406358789575));
#177971=CARTESIAN_POINT('Ctrl Pts',(52.1810724759249,-44.3950908753576,
-60.2644994621534));
#177972=CARTESIAN_POINT('Ctrl Pts',(52.6909850969965,-44.93000002,-60.4053784571342));
#177973=CARTESIAN_POINT('Ctrl Pts',(52.2200668721359,-44.9300000199999,
-60.1321953438309));
#177974=CARTESIAN_POINT('Ctrl Pts',(52.2557584885118,-44.3918607474242,
-60.153571413262));
#177975=CARTESIAN_POINT('Ctrl Pts',(52.8418547177727,-44.93000002,-60.0425329832694));
#177976=CARTESIAN_POINT('Ctrl Pts',(52.3118976785816,-44.93000002,-59.8989282761455));
#177977=CARTESIAN_POINT('Ctrl Pts',(52.3567212630826,-44.387494169614,-59.9116734379891));
#177978=CARTESIAN_POINT('Ctrl Pts',(52.8810454695352,-44.93000002,-59.8462508632613));
#177979=CARTESIAN_POINT('Ctrl Pts',(52.3353165341951,-44.9300000200007,
-59.7745406636052));
#177980=CARTESIAN_POINT('Ctrl Pts',(52.3829479761289,-44.3863598840851,
-59.7808179550118));
#177981=CARTESIAN_POINT('Ctrl Pts',(52.8810286767281,-44.93000002,-59.6498238026878));
#177982=CARTESIAN_POINT('Ctrl Pts',(52.3353064873126,-44.93000002,-59.6498699040777));
#177983=CARTESIAN_POINT('Ctrl Pts',(52.3829367382961,-44.3863603697065,
-59.6498658680002));
#177984=CARTESIAN_POINT('',(52.3829313330767,-44.3864221486262,-59.64995));
#177985=CARTESIAN_POINT('Ctrl Pts',(52.3829313330767,-44.3864221486262,
-59.64995));
#177986=CARTESIAN_POINT('Ctrl Pts',(52.3829313330767,-44.3864221486262,
-59.6909167350341));
#177987=CARTESIAN_POINT('Ctrl Pts',(52.3803897263674,-44.3865523180115,
-59.7322798285798));
#177988=CARTESIAN_POINT('Ctrl Pts',(52.3751806262637,-44.3868016431244,
-59.7737125482639));
#177989=CARTESIAN_POINT('Ctrl Pts',(52.3700397112217,-44.3870477046701,
-59.8146029300225));
#177990=CARTESIAN_POINT('Ctrl Pts',(52.3623003085474,-44.38740979058,-59.8555607844284));
#177991=CARTESIAN_POINT('Ctrl Pts',(52.3518818373882,-44.3878808509431,
-59.8962415307623));
#177992=CARTESIAN_POINT('Ctrl Pts',(52.3416571248465,-44.3883431507112,
-59.9361657126203));
#177993=CARTESIAN_POINT('Ctrl Pts',(52.3288517987115,-44.3889103859351,
-59.975822586086));
#177994=CARTESIAN_POINT('Ctrl Pts',(52.3134335070198,-44.3895797261845,
-60.0148624568469));
#177995=CARTESIAN_POINT('Ctrl Pts',(52.2981820855851,-44.3902418222476,
-60.0534798039331));
#177996=CARTESIAN_POINT('Ctrl Pts',(52.2803736880321,-44.3910038020508,
-60.0914930062));
#177997=CARTESIAN_POINT('Ctrl Pts',(52.2600242856205,-44.3918670628984,
-60.1285460469148));
#177998=CARTESIAN_POINT('Ctrl Pts',(52.2399875641714,-44.3927170592173,
-60.1650297450909));
#177999=CARTESIAN_POINT('Ctrl Pts',(52.2174871679696,-44.3936652341685,
-60.2005820954543));
#178000=CARTESIAN_POINT('Ctrl Pts',(52.192587492136,-44.3947172215951,-60.2348527378331));
#178001=CARTESIAN_POINT('Ctrl Pts',(52.1812851570981,-44.3951947344121,
-60.2504086946543));
#178002=CARTESIAN_POINT('Ctrl Pts',(52.1694891682159,-44.3956936970622,
-60.2657004677395));
#178003=CARTESIAN_POINT('Ctrl Pts',(52.1572090867896,-44.3962149460507,
-60.2806949718618));
#178004=CARTESIAN_POINT('Ctrl Pts',(52.146382848985,-44.3966744841684,-60.2939142708023));
#178005=CARTESIAN_POINT('Ctrl Pts',(52.1351803878862,-44.3971513466985,
-60.3069025151132));
#178006=CARTESIAN_POINT('Ctrl Pts',(52.1236097339139,-44.3976462362116,
-60.319637030479));
#178007=CARTESIAN_POINT('Ctrl Pts',(52.1184044198055,-44.3978688731837,
-60.3253659333271));
#178008=CARTESIAN_POINT('Ctrl Pts',(52.1128462456499,-44.3981087671614,
-60.3313432771974));
#178009=CARTESIAN_POINT('Ctrl Pts',(52.1073053941287,-44.3983470728172,
-60.3371563979184));
#178010=CARTESIAN_POINT('Ctrl Pts',(52.1015839317946,-44.3985931463364,
-60.3431590043988));
#178011=CARTESIAN_POINT('Ctrl Pts',(52.0958811206976,-44.3988375421255,
-60.3489863692236));
#178012=CARTESIAN_POINT('Ctrl Pts',(52.090645706994,-44.3990631132714,-60.3542239167039));
#178013=CARTESIAN_POINT('Ctrl Pts',(52.0896810715817,-44.3991046752047,
-60.3551889452689));
#178014=CARTESIAN_POINT('Ctrl Pts',(52.0887324034389,-44.3991456067858,
-60.3561340538162));
#178015=CARTESIAN_POINT('Ctrl Pts',(52.0878026339309,-44.3991858116419,
-60.3570567811866));
#178016=CARTESIAN_POINT('Ctrl Pts',(52.0656716302681,-44.400142794861,-60.3790201631155));
#178017=CARTESIAN_POINT('Ctrl Pts',(52.0418506706569,-44.4011805791872,
-60.4006133594539));
#178018=CARTESIAN_POINT('Ctrl Pts',(52.0162710562994,-44.4022931542543,
-60.4215416038383));
#178019=CARTESIAN_POINT('Ctrl Pts',(51.9913941546727,-44.4033751651131,
-60.4418949160304));
#178020=CARTESIAN_POINT('Ctrl Pts',(51.9648534607165,-44.4045278757317,
-60.4616189818122));
#178021=CARTESIAN_POINT('Ctrl Pts',(51.9366235653637,-44.4057490631047,
-60.4804121740066));
#178022=CARTESIAN_POINT('Ctrl Pts',(51.9083936700108,-44.4069702504778,
-60.499205366201));
#178023=CARTESIAN_POINT('Ctrl Pts',(51.8784739585051,-44.4082598608211,
-60.5170673748192));
#178024=CARTESIAN_POINT('Ctrl Pts',(51.8468854021593,-44.4096197288869,
-60.5336701569294));
#178025=CARTESIAN_POINT('Ctrl Pts',(51.8309424071766,-44.4103060650876,
-60.5420497127719));
#178026=CARTESIAN_POINT('Ctrl Pts',(51.8145750983105,-44.4110103672594,
-60.5501081144062));
#178027=CARTESIAN_POINT('Ctrl Pts',(51.7977914535884,-44.4117333333892,
-60.5578010744768));
#178028=CARTESIAN_POINT('Ctrl Pts',(51.7893996312274,-44.4120948164541,
-60.561647554512));
#178029=CARTESIAN_POINT('Ctrl Pts',(51.78090372741,-44.4124609657279,-60.5654026797756));
#178030=CARTESIAN_POINT('Ctrl Pts',(51.7723051681535,-44.4128319059709,
-60.5690607764376));
#178031=CARTESIAN_POINT('Ctrl Pts',(51.7680058885252,-44.4130173760924,
-60.5708898247687));
#178032=CARTESIAN_POINT('Ctrl Pts',(51.7636809453568,-44.4132040439841,
-60.572694616651));
#178033=CARTESIAN_POINT('Ctrl Pts',(51.7593305321249,-44.4133919265732,
-60.5744744411433));
#178034=CARTESIAN_POINT('Ctrl Pts',(51.7566892401513,-44.4135059968346,
-60.5755550364558));
#178035=CARTESIAN_POINT('Ctrl Pts',(51.7533267700704,-44.4136516104333,
-60.5769130552734));
#178036=CARTESIAN_POINT('Ctrl Pts',(51.7505384799174,-44.4137720333314,
-60.5780234113453));
#178037=CARTESIAN_POINT('Ctrl Pts',(51.7487342394082,-44.413849956309,-60.5787418980503));
#178038=CARTESIAN_POINT('Ctrl Pts',(51.747170962424,-44.4139173797181,-60.5793580291754));
#178039=CARTESIAN_POINT('Ctrl Pts',(51.7462030841064,-44.4139592360934,
-60.5797383010624));
#178040=CARTESIAN_POINT('Ctrl Pts',(51.730823640736,-44.4146243277082,-60.5857807651258));
#178041=CARTESIAN_POINT('Ctrl Pts',(51.7138127700712,-44.4153695794285,
-60.59203299983));
#178042=CARTESIAN_POINT('Ctrl Pts',(51.6951076439614,-44.4161894945035,
-60.5982457370374));
#178043=CARTESIAN_POINT('Ctrl Pts',(51.6768144165372,-44.4169913545309,
-60.6043216658492));
#178044=CARTESIAN_POINT('Ctrl Pts',(51.6568999668665,-44.4178645591487,
-60.6103597074779));
#178045=CARTESIAN_POINT('Ctrl Pts',(51.6353215996103,-44.4188053729988,
-60.6160795516463));
#178046=CARTESIAN_POINT('Ctrl Pts',(51.6145837107182,-44.4197095421076,
-60.62157660763));
#178047=CARTESIAN_POINT('Ctrl Pts',(51.5923083534765,-44.4206760997577,
-60.6267794477222));
#178048=CARTESIAN_POINT('Ctrl Pts',(51.5684827119301,-44.4217039246985,
-60.6313985671859));
#178049=CARTESIAN_POINT('Ctrl Pts',(51.5452580328485,-44.4227058244523,
-60.6359011769886));
#178050=CARTESIAN_POINT('Ctrl Pts',(51.5205596402882,-44.4237658829128,
-60.6398488190514));
#178051=CARTESIAN_POINT('Ctrl Pts',(51.4944094354873,-44.4248860161899,
-60.6429384344745));
#178052=CARTESIAN_POINT('Ctrl Pts',(51.4692420222068,-44.4259640519961,
-60.6459119342548));
#178053=CARTESIAN_POINT('Ctrl Pts',(51.4427294002456,-44.4270976906941,
-60.6480902258672));
#178054=CARTESIAN_POINT('Ctrl Pts',(51.4149307233305,-44.4282921075643,
-60.6491761922995));
#178055=CARTESIAN_POINT('Ctrl Pts',(51.4019948308487,-44.4288479199239,
-60.6496815381132));
#178056=CARTESIAN_POINT('Ctrl Pts',(51.3887810672911,-44.4294169472215,
-60.64995));
#178057=CARTESIAN_POINT('Ctrl Pts',(51.3752989258075,-44.43000002,-60.64995));
#178058=CARTESIAN_POINT('',(52.3810286821225,-44.43000002,-59.64995));
#178059=CARTESIAN_POINT('Origin',(52.8810286821225,-44.43000002,-59.64995));
#178060=CARTESIAN_POINT('Origin',(52.8810286821225,-44.43000002,-59.64995));
#178061=CARTESIAN_POINT('Origin',(-83.2809572255632,-45.4300000199999,-55.74995));
#178062=CARTESIAN_POINT('',(52.7935400185966,-45.43000002,-55.24995));
#178063=CARTESIAN_POINT('Ctrl Pts',(52.8810286821225,-44.93000002,-55.74995));
#178064=CARTESIAN_POINT('Ctrl Pts',(52.8810286821214,-44.93000002,-55.7240274876136));
#178065=CARTESIAN_POINT('Ctrl Pts',(52.8806555354494,-44.9321038000435,
-55.6978059976788));
#178066=CARTESIAN_POINT('Ctrl Pts',(52.8799059022337,-44.9363531599825,
-55.6716073783532));
#178067=CARTESIAN_POINT('Ctrl Pts',(52.8791497351538,-44.9406395576885,
-55.6451804097294));
#178068=CARTESIAN_POINT('Ctrl Pts',(52.8780104850152,-44.9471091347783,
-55.6187767695886));
#178069=CARTESIAN_POINT('Ctrl Pts',(52.8764897360373,-44.9557761309555,
-55.5927712416137));
#178070=CARTESIAN_POINT('Ctrl Pts',(52.8759205170078,-44.9590202029387,
-55.5830373265427));
#178071=CARTESIAN_POINT('Ctrl Pts',(52.8752978996289,-44.9625718489931,
-55.5733596261139));
#178072=CARTESIAN_POINT('Ctrl Pts',(52.8746221467745,-44.9664307842404,
-55.5637593428073));
#178073=CARTESIAN_POINT('Ctrl Pts',(52.8728440766865,-44.9765845812825,
-55.5384986628543));
#178074=CARTESIAN_POINT('Ctrl Pts',(52.8706960694052,-44.9888727751743,
-55.5137551369759));
#178075=CARTESIAN_POINT('Ctrl Pts',(52.8681778191489,-45.0032950405858,
-55.489926848577));
#178076=CARTESIAN_POINT('Ctrl Pts',(52.867671674228,-45.0061937820303,-55.485137583842));
#178077=CARTESIAN_POINT('Ctrl Pts',(52.8671505801727,-45.0091786900675,
-55.4803854542241));
#178078=CARTESIAN_POINT('Ctrl Pts',(52.8666145463196,-45.0122496941479,
-55.4756739401742));
#178079=CARTESIAN_POINT('Ctrl Pts',(52.8650130502525,-45.0214248627082,
-55.4615974575482));
#178080=CARTESIAN_POINT('Ctrl Pts',(52.8632780871792,-45.0313686933034,
-55.4478834520303));
#178081=CARTESIAN_POINT('Ctrl Pts',(52.8614096369564,-45.0420727511099,
-55.4346345056539));
#178082=CARTESIAN_POINT('Ctrl Pts',(52.8604754118449,-45.0474247800131,
-55.4280100324658));
#178083=CARTESIAN_POINT('Ctrl Pts',(52.8595078154648,-45.052966812139,-55.4215019155655));
#178084=CARTESIAN_POINT('Ctrl Pts',(52.8585068493069,-45.0586966555504,
-55.4151241748974));
#178085=CARTESIAN_POINT('Ctrl Pts',(52.858006366228,-45.0615615772561,-55.4119353045634));
#178086=CARTESIAN_POINT('Ctrl Pts',(52.8574975407611,-45.0644734423857,
-55.4087790343541));
#178087=CARTESIAN_POINT('Ctrl Pts',(52.8569803733541,-45.0674318984956,
-55.4056571673493));
#178088=CARTESIAN_POINT('Ctrl Pts',(52.8566794288446,-45.069153451538,-55.4038405239921));
#178089=CARTESIAN_POINT('Ctrl Pts',(52.8563126508256,-45.071250909713,-55.4016627141456));
#178090=CARTESIAN_POINT('Ctrl Pts',(52.8559894746429,-45.0730986811608,
-55.399777933153));
#178091=CARTESIAN_POINT('Ctrl Pts',(52.8557572787116,-45.0744262697484,
-55.3984237539124));
#178092=CARTESIAN_POINT('Ctrl Pts',(52.855547825501,-45.0756236244489,-55.3972196143699));
#178093=CARTESIAN_POINT('Ctrl Pts',(52.8554038192003,-45.0764466282408,
-55.3963966105726));
#178094=CARTESIAN_POINT('Ctrl Pts',(52.8536925773759,-45.0862264677528,
-55.3866167709961));
#178095=CARTESIAN_POINT('Ctrl Pts',(52.851754330019,-45.0971430353417,-55.3765446164713));
#178096=CARTESIAN_POINT('Ctrl Pts',(52.8495832355115,-45.109325146193,-55.3664154208622));
#178097=CARTESIAN_POINT('Ctrl Pts',(52.8475054116275,-45.1209839112987,
-55.3567213773785));
#178098=CARTESIAN_POINT('Ctrl Pts',(52.8452141961207,-45.1338025296426,
-55.3469750519385));
#178099=CARTESIAN_POINT('Ctrl Pts',(52.8427082950591,-45.1478716582866,
-55.3374234994891));
#178100=CARTESIAN_POINT('Ctrl Pts',(52.8403472166539,-45.1611276947396,
-55.3284239565424));
#178101=CARTESIAN_POINT('Ctrl Pts',(52.8377954759301,-45.1754943248228,
-55.3195974072008));
#178102=CARTESIAN_POINT('Ctrl Pts',(52.8350568009413,-45.1910192354886,
-55.3111870421648));
#178103=CARTESIAN_POINT('Ctrl Pts',(52.8339582620473,-45.1972465966259,
-55.3078134716817));
#178104=CARTESIAN_POINT('Ctrl Pts',(52.8328297081496,-45.2036599569019,
-55.3045072862908));
#178105=CARTESIAN_POINT('Ctrl Pts',(52.8316716567513,-45.2102607648964,
-55.3012859403148));
#178106=CARTESIAN_POINT('Ctrl Pts',(52.828999083875,-45.2254942341827,-55.2938516572656));
#178107=CARTESIAN_POINT('Ctrl Pts',(52.826174751091,-45.2417391406544,-55.2868619638522));
#178108=CARTESIAN_POINT('Ctrl Pts',(52.8231873524218,-45.2589873547265,
-55.2805581078704));
#178109=CARTESIAN_POINT('Ctrl Pts',(52.8202817251599,-45.275763448773,-55.2744268017326));
#178110=CARTESIAN_POINT('Ctrl Pts',(52.8172217775644,-45.2934889899389,
-55.2689442786239));
#178111=CARTESIAN_POINT('Ctrl Pts',(52.8140036335369,-45.3121198505846,
-55.264362018836));
#178112=CARTESIAN_POINT('Ctrl Pts',(52.8108844970282,-45.3301775251725,
-55.259920734147));
#178113=CARTESIAN_POINT('Ctrl Pts',(52.8076167059087,-45.3490858911464,
-55.256325174742));
#178114=CARTESIAN_POINT('Ctrl Pts',(52.8042036732994,-45.3687660560856,
-55.2538325278146));
#178115=CARTESIAN_POINT('Ctrl Pts',(52.8007906406901,-45.3884462210248,
-55.2513398808872));
#178116=CARTESIAN_POINT('Ctrl Pts',(52.7972322905145,-45.4088985894293,
-55.24995));
#178117=CARTESIAN_POINT('Ctrl Pts',(52.7935400185966,-45.43000002,-55.24995));
#178118=CARTESIAN_POINT('',(60.,-45.43000002,-55.24995));
#178119=CARTESIAN_POINT('Origin',(60.,28.41999998,-55.24995));
#178120=CARTESIAN_POINT('',(52.7497956868337,-45.93000002,-55.24995));
#178121=CARTESIAN_POINT('',(59.2602401389193,28.4847205815761,-55.24995));
#178122=CARTESIAN_POINT('',(60.,-45.93000002,-55.24995));
#178123=CARTESIAN_POINT('Origin',(60.,-45.93000002,-55.74995));
#178124=CARTESIAN_POINT('',(52.6623070233078,-46.43000002,-55.74995));
#178125=CARTESIAN_POINT('Ctrl Pts',(52.7497956868337,-45.93000002,-55.24995));
#178126=CARTESIAN_POINT('Ctrl Pts',(52.7460187925163,-45.9515850697951,
-55.24995));
#178127=CARTESIAN_POINT('Ctrl Pts',(52.7423610411603,-45.9724892144497,
-55.2514041468224));
#178128=CARTESIAN_POINT('Ctrl Pts',(52.7388452120446,-45.9925822697903,
-55.2540052053732));
#178129=CARTESIAN_POINT('Ctrl Pts',(52.7353551265784,-46.0125281995008,
-55.2565872184194));
#178130=CARTESIAN_POINT('Ctrl Pts',(52.7320048008033,-46.0316753989214,
-55.260299617229));
#178131=CARTESIAN_POINT('Ctrl Pts',(52.7288082793926,-46.0499436023777,
-55.2648742466987));
#178132=CARTESIAN_POINT('Ctrl Pts',(52.7254663302596,-46.0690429290696,
-55.2696570017705));
#178133=CARTESIAN_POINT('Ctrl Pts',(52.7222924665376,-46.0871816432422,
-55.2753821626626));
#178134=CARTESIAN_POINT('Ctrl Pts',(52.7192945613869,-46.1043147495782,
-55.2817780783569));
#178135=CARTESIAN_POINT('Ctrl Pts',(52.716494116128,-46.1203193674686,-55.2877527209429));
#178136=CARTESIAN_POINT('Ctrl Pts',(52.7138470746185,-46.1354472789192,
-55.2943131224857));
#178137=CARTESIAN_POINT('Ctrl Pts',(52.7113543626339,-46.1496931930989,
-55.3012636512206));
#178138=CARTESIAN_POINT('Ctrl Pts',(52.7084584871895,-46.166243196994,-55.3093383367891));
#178139=CARTESIAN_POINT('Ctrl Pts',(52.7057691575151,-46.1816127864123,
-55.3179437621966));
#178140=CARTESIAN_POINT('Ctrl Pts',(52.7032802093755,-46.1958371901192,
-55.3268178701236));
#178141=CARTESIAN_POINT('Ctrl Pts',(52.7006035647027,-46.2111342844216,
-55.3363611921922));
#178142=CARTESIAN_POINT('Ctrl Pts',(52.6981585023978,-46.2251078794353,
-55.3462154234316));
#178143=CARTESIAN_POINT('Ctrl Pts',(52.695930445538,-46.237841282656,-55.3561026478091));
#178144=CARTESIAN_POINT('Ctrl Pts',(52.6936636080107,-46.2507963184048,
-55.3661619652632));
#178145=CARTESIAN_POINT('Ctrl Pts',(52.6916213571538,-46.2624678354595,
-55.3762552362856));
#178146=CARTESIAN_POINT('Ctrl Pts',(52.6897832999643,-46.272972380365,-55.3861352293988));
#178147=CARTESIAN_POINT('Ctrl Pts',(52.6895145215425,-46.2745084560746,
-55.3875799771312));
#178148=CARTESIAN_POINT('Ctrl Pts',(52.6892501028258,-46.2760196159558,
-55.3890202396049));
#178149=CARTESIAN_POINT('Ctrl Pts',(52.6889899717987,-46.2775062715784,
-55.3904553319095));
#178150=CARTESIAN_POINT('Ctrl Pts',(52.6887686497785,-46.2787711327118,
-55.3916763224679));
#178151=CARTESIAN_POINT('Ctrl Pts',(52.6886223994534,-46.2796069571358,
-55.3924916493942));
#178152=CARTESIAN_POINT('Ctrl Pts',(52.6884184363187,-46.2807725552524,
-55.3936383710037));
#178153=CARTESIAN_POINT('Ctrl Pts',(52.6882898108671,-46.2815076174213,
-55.3943615290642));
#178154=CARTESIAN_POINT('Ctrl Pts',(52.6881382781733,-46.2823735725975,
-55.3952167714233));
#178155=CARTESIAN_POINT('Ctrl Pts',(52.687931817023,-46.2835534087318,-55.3963966075452));
#178156=CARTESIAN_POINT('Ctrl Pts',(52.6843315421343,-46.3041274218082,
-55.416970620405));
#178157=CARTESIAN_POINT('Ctrl Pts',(52.6811035150388,-46.3225747482756,
-55.439163047915));
#178158=CARTESIAN_POINT('Ctrl Pts',(52.6782552198821,-46.338852377289,-55.4624843710585));
#178159=CARTESIAN_POINT('Ctrl Pts',(52.6754034087636,-46.3551500995569,
-55.4858344822573));
#178160=CARTESIAN_POINT('Ctrl Pts',(52.6729322643169,-46.3692727837042,
-55.5103162635779));
#178161=CARTESIAN_POINT('Ctrl Pts',(52.670845226173,-46.3812005423344,-55.5354850657357));
#178162=CARTESIAN_POINT('Ctrl Pts',(52.6687546255404,-46.3931486611603,
-55.5606968300082));
#178163=CARTESIAN_POINT('Ctrl Pts',(52.6670494390977,-46.402894380944,-55.5865979625005));
#178164=CARTESIAN_POINT('Ctrl Pts',(52.6657290991159,-46.4104407221667,
-55.6127884619271));
#178165=CARTESIAN_POINT('Ctrl Pts',(52.6644028119805,-46.4180210540667,
-55.6390969301531));
#178166=CARTESIAN_POINT('Ctrl Pts',(52.6634648417048,-46.4233821745086,
-55.6656973742807));
#178167=CARTESIAN_POINT('Ctrl Pts',(52.6629106187229,-46.4265499748194,
-55.6922317372147));
#178168=CARTESIAN_POINT('Ctrl Pts',(52.6625072019682,-46.4288558043545,
-55.7115459968728));
#178169=CARTESIAN_POINT('Ctrl Pts',(52.6623070233078,-46.43000002,-55.7308262353414));
#178170=CARTESIAN_POINT('Ctrl Pts',(52.6623070233078,-46.43000002,-55.74995));
#178171=CARTESIAN_POINT('',(-83.2809572255632,-46.4300000199999,-55.74995));
#178172=CARTESIAN_POINT('Origin',(-83.2809572255632,-46.4300000199999,-55.2499500000008));
#178173=CARTESIAN_POINT('',(52.6623070233077,-46.43000002,-59.64995));
#178174=CARTESIAN_POINT('',(52.6623070233078,-46.43000002,-55.2499500000008));
#178175=CARTESIAN_POINT('Ctrl Pts',(52.6623070233077,-46.43000002,-59.64995));
#178176=CARTESIAN_POINT('Ctrl Pts',(52.6623070232906,-46.43000002,-59.8463349320562));
#178177=CARTESIAN_POINT('Ctrl Pts',(52.623116902509,-46.43000002,-60.0425718399611));
#178178=CARTESIAN_POINT('Ctrl Pts',(52.5476901703453,-46.43000002,-60.2239751485476));
#178179=CARTESIAN_POINT('Ctrl Pts',(52.4722634381816,-46.43000002,-60.4053784571342));
#178180=CARTESIAN_POINT('Ctrl Pts',(52.3606594164458,-46.43000002,-60.5717700902076));
#178181=CARTESIAN_POINT('Ctrl Pts',(52.2212889883174,-46.43000002,-60.7106101717798));
#178182=CARTESIAN_POINT('Ctrl Pts',(52.0819185601891,-46.43000002,-60.8494502533521));
#178183=CARTESIAN_POINT('Ctrl Pts',(51.9148913381812,-46.43000002,-60.9606295880612));
#178184=CARTESIAN_POINT('Ctrl Pts',(51.7327950983536,-46.43000002,-61.0357692987669));
#178185=CARTESIAN_POINT('Ctrl Pts',(51.550698858526,-46.43000002,-61.1109090094727));
#178186=CARTESIAN_POINT('Ctrl Pts',(51.3537123576397,-46.43000002,-61.149949999985));
#178187=CARTESIAN_POINT('Ctrl Pts',(51.1565772669927,-46.43000002,-61.14995));
#178188=CARTESIAN_POINT('Ctrl Pts',(52.6623070233078,-46.43000002,-59.64995));
#178189=CARTESIAN_POINT('Ctrl Pts',(52.2041414362991,-46.43000002,-59.64995));
#178190=CARTESIAN_POINT('Ctrl Pts',(52.1642096742619,-46.8864221486262,
-59.64995));
#178191=CARTESIAN_POINT('Ctrl Pts',(52.6623070232907,-46.43000002,-59.8463349320562));
#178192=CARTESIAN_POINT('Ctrl Pts',(52.2041414362827,-46.4300000200027,
-59.7861314645));
#178193=CARTESIAN_POINT('Ctrl Pts',(52.1642096742618,-46.8864221486274,
-59.7808732880376));
#178194=CARTESIAN_POINT('Ctrl Pts',(52.6231169025091,-46.43000002,-60.0425718399611));
#178195=CARTESIAN_POINT('Ctrl Pts',(52.175748088412,-46.43000002,-59.9224177216061));
#178196=CARTESIAN_POINT('Ctrl Pts',(52.1379836960638,-46.8875563641358,
-59.9116978933072));
#178197=CARTESIAN_POINT('Ctrl Pts',(52.4722634381817,-46.43000002,-60.4053784571342));
#178198=CARTESIAN_POINT('Ctrl Pts',(52.0676362723124,-46.43000002,-60.1718710142644));
#178199=CARTESIAN_POINT('Ctrl Pts',(52.0370327526638,-46.8919222689988,
-60.153568971423));
#178200=CARTESIAN_POINT('Ctrl Pts',(52.3606594164458,-46.43000002,-60.5717700902076));
#178201=CARTESIAN_POINT('Ctrl Pts',(51.9876181407653,-46.43000002,-60.2852157712123));
#178202=CARTESIAN_POINT('Ctrl Pts',(51.9623474855296,-46.8951522414972,
-60.264496726805));
#178203=CARTESIAN_POINT('Ctrl Pts',(52.0819185601891,-46.43000002,-60.8494502533521));
#178204=CARTESIAN_POINT('Ctrl Pts',(51.7906875266988,-46.43000002,-60.4706504746462));
#178205=CARTESIAN_POINT('Ctrl Pts',(51.7758144647026,-46.9032193817865,
-60.4496168355682));
#178206=CARTESIAN_POINT('Ctrl Pts',(51.9148913381812,-46.43000002,-60.9606295880612));
#178207=CARTESIAN_POINT('Ctrl Pts',(51.6733804433437,-46.4300000200007,
-60.5426326522478));
#178208=CARTESIAN_POINT('Ctrl Pts',(51.6640400635624,-46.9080533772402,
-60.5237363920407));
#178209=CARTESIAN_POINT('Ctrl Pts',(51.550698858526,-46.43000002,-61.1109090094727));
#178210=CARTESIAN_POINT('Ctrl Pts',(51.4220052245013,-46.4300000199993,
-60.6353187454025));
#178211=CARTESIAN_POINT('Ctrl Pts',(51.4203229267752,-46.9185936039748,
-60.6239226729819));
#178212=CARTESIAN_POINT('Ctrl Pts',(51.3537123576397,-46.43000002,-61.149949999985));
#178213=CARTESIAN_POINT('Ctrl Pts',(51.2877237368248,-46.4300000199999,
-60.6556217969811));
#178214=CARTESIAN_POINT('Ctrl Pts',(51.288499814922,-46.9242946617933,-60.64995));
#178215=CARTESIAN_POINT('Ctrl Pts',(51.1565772669927,-46.43000002,-61.14995));
#178216=CARTESIAN_POINT('Ctrl Pts',(51.1565772669928,-46.43000002,-60.64995));
#178217=CARTESIAN_POINT('Ctrl Pts',(51.1565772669927,-46.93000002,-60.64995));
#178218=CARTESIAN_POINT('',(52.1642096742619,-46.8864221486262,-59.64995));
#178219=CARTESIAN_POINT('Origin',(52.6623070233077,-46.93000002,-59.64995));
#178220=CARTESIAN_POINT('Ctrl Pts',(51.1565772669927,-46.93000002,-60.64995));
#178221=CARTESIAN_POINT('Ctrl Pts',(51.1847702648877,-46.928780735242,-60.64995));
#178222=CARTESIAN_POINT('Ctrl Pts',(51.2117854385287,-46.927612388776,-60.6487640562879));
#178223=CARTESIAN_POINT('Ctrl Pts',(51.2375495222804,-46.9264981491786,
-60.6466905423627));
#178224=CARTESIAN_POINT('Ctrl Pts',(51.264653008408,-46.9253259833931,-60.6445092322705));
#178225=CARTESIAN_POINT('Ctrl Pts',(51.2903722894732,-46.9242136814127,
-60.6413458429197));
#178226=CARTESIAN_POINT('Ctrl Pts',(51.314667764435,-46.923162955895,-60.6375094924141));
#178227=CARTESIAN_POINT('Ctrl Pts',(51.3362491645544,-46.922229608107,-60.6341017049398));
#178228=CARTESIAN_POINT('Ctrl Pts',(51.3567080746573,-46.9213448055277,
-60.6301623057541));
#178229=CARTESIAN_POINT('Ctrl Pts',(51.3760406982618,-46.9205087123465,
-60.6258833728634));
#178230=CARTESIAN_POINT('Ctrl Pts',(51.3993088743585,-46.9195024152309,
-60.6207333753234));
#178231=CARTESIAN_POINT('Ctrl Pts',(51.4209463563881,-46.9185666420243,
-60.6150923634367));
#178232=CARTESIAN_POINT('Ctrl Pts',(51.4409781638996,-46.9177003106867,
-60.6092528148882));
#178233=CARTESIAN_POINT('Ctrl Pts',(51.461841288257,-46.9167980267356,-60.6031709259978));
#178234=CARTESIAN_POINT('Ctrl Pts',(51.4809635757311,-46.9159710301266,
-60.59687378199));
#178235=CARTESIAN_POINT('Ctrl Pts',(51.4983982409252,-46.9152170194459,
-60.590641719777));
#178236=CARTESIAN_POINT('Ctrl Pts',(51.5058957306206,-46.9148927696111,
-60.587961724394));
#178237=CARTESIAN_POINT('Ctrl Pts',(51.5130813113975,-46.9145820091467,
-60.5852931620018));
#178238=CARTESIAN_POINT('Ctrl Pts',(51.5199602052477,-46.9142845122131,
-60.5826554871348));
#178239=CARTESIAN_POINT('Ctrl Pts',(51.5217040730788,-46.9142090937892,
-60.5819868103897));
#178240=CARTESIAN_POINT('Ctrl Pts',(51.5225209356732,-46.9141737217426,
-60.5816714634958));
#178241=CARTESIAN_POINT('Ctrl Pts',(51.5242736665976,-46.9140978936724,
-60.5809901111742));
#178242=CARTESIAN_POINT('Ctrl Pts',(51.5250828151279,-46.9140628876308,
-60.5806755647587));
#178243=CARTESIAN_POINT('Ctrl Pts',(51.5260912919896,-46.9140192649611,
-60.5802826897577));
#178244=CARTESIAN_POINT('Ctrl Pts',(51.5274809097942,-46.9139591688407,
-60.5797369933149));
#178245=CARTESIAN_POINT('Ctrl Pts',(51.5324129413637,-46.9137458756876,
-60.5778002074776));
#178246=CARTESIAN_POINT('Ctrl Pts',(51.5373132446684,-46.9135339542674,
-60.5758307565194));
#178247=CARTESIAN_POINT('Ctrl Pts',(51.5421814960853,-46.9133234186079,
-60.5738295347324));
#178248=CARTESIAN_POINT('Ctrl Pts',(51.575230464493,-46.9118941607979,-60.5602438938215));
#178249=CARTESIAN_POINT('Ctrl Pts',(51.6067903400481,-46.9105292839638,
-60.5452002162122));
#178250=CARTESIAN_POINT('Ctrl Pts',(51.6368130930596,-46.9092308751016,
-60.5290286703019));
#178251=CARTESIAN_POINT('Ctrl Pts',(51.665490560407,-46.9079906464745,-60.5135817531047));
#178252=CARTESIAN_POINT('Ctrl Pts',(51.6927660898016,-46.9068110401859,
-60.4971053444812));
#178253=CARTESIAN_POINT('Ctrl Pts',(51.7186284446323,-46.9056925505819,
-60.479855118547));
#178254=CARTESIAN_POINT('Ctrl Pts',(51.7476702048669,-46.9044365587312,
-60.4604842248734));
#178255=CARTESIAN_POINT('Ctrl Pts',(51.7749307436447,-46.9032576007661,
-60.4401373907221));
#178256=CARTESIAN_POINT('Ctrl Pts',(51.8004335247133,-46.9021546619314,
-60.4191325964794));
#178257=CARTESIAN_POINT('Ctrl Pts',(51.8124227509342,-46.9016361544336,
-60.4092579389186));
#178258=CARTESIAN_POINT('Ctrl Pts',(51.8240239907144,-46.9011344264906,
-60.3992372748785));
#178259=CARTESIAN_POINT('Ctrl Pts',(51.8352421085066,-46.9006492677257,
-60.3891007236107));
#178260=CARTESIAN_POINT('Ctrl Pts',(51.8406826553793,-46.9004139761152,
-60.3841847133385));
#178261=CARTESIAN_POINT('Ctrl Pts',(51.8457127685635,-46.9001964348515,
-60.3795368119428));
#178262=CARTESIAN_POINT('Ctrl Pts',(51.8507857721989,-46.8999770320173,
-60.3747537947662));
#178263=CARTESIAN_POINT('Ctrl Pts',(51.855707981935,-46.8997641508833,-60.3701129517062));
#178264=CARTESIAN_POINT('Ctrl Pts',(51.8606707216413,-46.8995495106536,
-60.3653448266592));
#178265=CARTESIAN_POINT('Ctrl Pts',(51.8660550406273,-46.899316625737,-60.3600469434816));
#178266=CARTESIAN_POINT('Ctrl Pts',(51.8670486809789,-46.8992736483705,
-60.3590692542852));
#178267=CARTESIAN_POINT('Ctrl Pts',(51.8680565774982,-46.899230054037,-60.3580734246752));
#178268=CARTESIAN_POINT('Ctrl Pts',(51.8690809779991,-46.8991857454855,
-60.3570567840805));
#178269=CARTESIAN_POINT('Ctrl Pts',(51.9031359181947,-46.8977127619508,
-60.3232598124644));
#178270=CARTESIAN_POINT('Ctrl Pts',(51.9344045600307,-46.8963604150637,
-60.2873222677668));
#178271=CARTESIAN_POINT('Ctrl Pts',(51.9627607287964,-46.8951340888708,
-60.2497596517395));
#178272=CARTESIAN_POINT('Ctrl Pts',(51.9915444077599,-46.8938892740394,
-60.2116307250254));
#178273=CARTESIAN_POINT('Ctrl Pts',(52.0173271644005,-46.8927743070765,
-60.1718273241926));
#178274=CARTESIAN_POINT('Ctrl Pts',(52.0400037418449,-46.8917936658769,
-60.1308415624652));
#178275=CARTESIAN_POINT('Ctrl Pts',(52.0577545058505,-46.8910260398738,
-60.0987587410695));
#178276=CARTESIAN_POINT('Ctrl Pts',(52.0736025244311,-46.8903406975554,
-60.0659504745663));
#178277=CARTESIAN_POINT('Ctrl Pts',(52.0875082244596,-46.8897393152827,
-60.032633432405));
#178278=CARTESIAN_POINT('Ctrl Pts',(52.0888900686388,-46.8896795544227,
-60.0293226346255));
#178279=CARTESIAN_POINT('Ctrl Pts',(52.0902527105013,-46.8896206236163,
-60.0260068882407));
#178280=CARTESIAN_POINT('Ctrl Pts',(52.0915961909269,-46.8895625210615,
-60.0226864258008));
#178281=CARTESIAN_POINT('Ctrl Pts',(52.1091485881571,-46.8888034187308,
-59.979305015382));
#178282=CARTESIAN_POINT('Ctrl Pts',(52.123429659647,-46.8881857939979,-59.9351228136313));
#178283=CARTESIAN_POINT('Ctrl Pts',(52.1345334358967,-46.8877055802516,
-59.8906338459064));
#178284=CARTESIAN_POINT('Ctrl Pts',(52.1457717122319,-46.8872195496743,
-59.8456059831406));
#178285=CARTESIAN_POINT('Ctrl Pts',(52.1537552706727,-46.8868742784422,
-59.800263845221));
#178286=CARTESIAN_POINT('Ctrl Pts',(52.158589917584,-46.886665190664,-59.7550665496285));
#178287=CARTESIAN_POINT('Ctrl Pts',(52.1623541733489,-46.8865023949338,
-59.7198759382737));
#178288=CARTESIAN_POINT('Ctrl Pts',(52.1642096742619,-46.8864221486262,
-59.6847720495211));
#178289=CARTESIAN_POINT('Ctrl Pts',(52.1642096742619,-46.8864221486262,
-59.64995));
#178290=CARTESIAN_POINT('Origin',(0.,-12.9675000200281,-60.64995));
#178291=CARTESIAN_POINT('',(53.7167487055513,-17.6671065732338,-60.64995));
#178292=CARTESIAN_POINT('Ctrl Pts',(50.6621396387151,-53.08000002,-61.1499499946262));
#178293=CARTESIAN_POINT('Ctrl Pts',(50.6621815241177,-53.0800000199999,
-60.6498941830841));
#178294=CARTESIAN_POINT('Ctrl Pts',(50.6621815444126,-52.5799442087081,
-60.6499499995188));
#178295=CARTESIAN_POINT('Ctrl Pts',(50.8593170188006,-53.08000002,-61.1499667235322));
#178296=CARTESIAN_POINT('Ctrl Pts',(50.7949219565861,-53.08000002,-60.6441634129678));
#178297=CARTESIAN_POINT('Ctrl Pts',(50.7941322985337,-52.5742372910461,
-60.6499618311926));
#178298=CARTESIAN_POINT('Ctrl Pts',(51.0563489044894,-53.08000002,-61.1109251044403));
#178299=CARTESIAN_POINT('Ctrl Pts',(50.9242606677665,-53.08000002,-60.6119868070572));
#178300=CARTESIAN_POINT('Ctrl Pts',(50.925986077618,-52.5685345954075,-60.6239348042603));
#178301=CARTESIAN_POINT('Ctrl Pts',(51.4205803892599,-53.08000002,-60.9606295880612));
#178302=CARTESIAN_POINT('Ctrl Pts',(51.1595367031111,-53.08000002,-60.5030970594232));
#178303=CARTESIAN_POINT('Ctrl Pts',(51.1697302983437,-52.5579926660341,
-60.5237387895063));
#178304=CARTESIAN_POINT('Ctrl Pts',(51.5876076112677,-53.08000002,-60.8494502533514));
#178305=CARTESIAN_POINT('Ctrl Pts',(51.2649595932576,-53.0800000200007,
-60.4261477374134));
#178306=CARTESIAN_POINT('Ctrl Pts',(51.2815054280689,-52.5531584192985,
-60.4496195485702));
#178307=CARTESIAN_POINT('Ctrl Pts',(51.8663484675245,-53.08000002,-60.5717700902082));
#178308=CARTESIAN_POINT('Ctrl Pts',(51.4389731852977,-53.0800000199992,
-60.2406358789611));
#178309=CARTESIAN_POINT('Ctrl Pts',(51.4680398681885,-52.545090875362,-60.2644994621532));
#178310=CARTESIAN_POINT('Ctrl Pts',(51.9779524892604,-53.08000002,-60.4053784571342));
#178311=CARTESIAN_POINT('Ctrl Pts',(51.507034264404,-53.08000002,-60.1321953438333));
#178312=CARTESIAN_POINT('Ctrl Pts',(51.5427258807753,-52.5418607474287,
-60.1535714132618));
#178313=CARTESIAN_POINT('Ctrl Pts',(52.1288221100354,-53.08000002,-60.0425329832722));
#178314=CARTESIAN_POINT('Ctrl Pts',(51.5988650708495,-53.08000002,-59.8989282761487));
#178315=CARTESIAN_POINT('Ctrl Pts',(51.6436886553452,-52.5374941696185,
-59.9116734379909));
#178316=CARTESIAN_POINT('Ctrl Pts',(52.1680128617978,-53.08000002,-59.8462508632673));
#178317=CARTESIAN_POINT('Ctrl Pts',(51.6222839264631,-53.0800000200021,
-59.7745406636097));
#178318=CARTESIAN_POINT('Ctrl Pts',(51.6699153683916,-52.5363598840896,
-59.7808179550158));
#178319=CARTESIAN_POINT('Ctrl Pts',(52.167996068992,-53.08000002,-59.6498238026969));
#178320=CARTESIAN_POINT('Ctrl Pts',(51.6222738795813,-53.08000002,-59.6498699040835));
#178321=CARTESIAN_POINT('Ctrl Pts',(51.6699041305595,-52.536360369711,-59.6498658680063));
#178322=CARTESIAN_POINT('',(51.6698987253405,-52.5364221486262,-59.64995));
#178323=CARTESIAN_POINT('',(52.1679960743864,-53.08000002,-59.64995));
#178324=CARTESIAN_POINT('Origin',(52.1679960743864,-52.58000002,-59.64995));
#178325=CARTESIAN_POINT('Ctrl Pts',(50.6622663180714,-53.08000002,-61.14995));
#178326=CARTESIAN_POINT('Ctrl Pts',(50.8594014087184,-53.08000002,-61.149949999985));
#178327=CARTESIAN_POINT('Ctrl Pts',(51.0563879096046,-53.08000002,-61.1109090094727));
#178328=CARTESIAN_POINT('Ctrl Pts',(51.4205803892599,-53.08000002,-60.9606295880612));
#178329=CARTESIAN_POINT('Ctrl Pts',(51.5876076112677,-53.08000002,-60.8494502533514));
#178330=CARTESIAN_POINT('Ctrl Pts',(51.8663484675245,-53.08000002,-60.5717700902082));
#178331=CARTESIAN_POINT('Ctrl Pts',(51.9779524892604,-53.08000002,-60.4053784571342));
#178332=CARTESIAN_POINT('Ctrl Pts',(52.1288059535877,-53.08000002,-60.0425718399611));
#178333=CARTESIAN_POINT('Ctrl Pts',(52.1679960743694,-53.08000002,-59.8463349320561));
#178334=CARTESIAN_POINT('Ctrl Pts',(52.1679960743864,-53.08000002,-59.64995));
#178335=CARTESIAN_POINT('Ctrl Pts',(51.6698987253405,-52.5364221486262,
-59.64995));
#178336=CARTESIAN_POINT('Ctrl Pts',(51.6698987253405,-52.5364221486262,
-59.6909727319776));
#178337=CARTESIAN_POINT('Ctrl Pts',(51.6673501566751,-52.5365526733191,
-59.7323929144446));
#178338=CARTESIAN_POINT('Ctrl Pts',(51.6621266428239,-52.5368026661919,
-59.7738824503071));
#178339=CARTESIAN_POINT('Ctrl Pts',(51.6570039945927,-52.537047831723,-59.8145708266674));
#178340=CARTESIAN_POINT('Ctrl Pts',(51.6493083876707,-52.5374078679653,
-59.855325534387));
#178341=CARTESIAN_POINT('Ctrl Pts',(51.638960382346,-52.5378758248444,-59.8958071079189));
#178342=CARTESIAN_POINT('Ctrl Pts',(51.6287267706847,-52.53833860862,-59.935841171486));
#178343=CARTESIAN_POINT('Ctrl Pts',(51.6158987551754,-52.5389069118211,
-59.9756077249091));
#178344=CARTESIAN_POINT('Ctrl Pts',(51.6004436152177,-52.5395778717659,
-60.014754279517));
#178345=CARTESIAN_POINT('Ctrl Pts',(51.5852405811232,-52.5402378869418,
-60.0532622714225));
#178346=CARTESIAN_POINT('Ctrl Pts',(51.5674952125664,-52.5409972179362,
-60.0911698875945));
#178347=CARTESIAN_POINT('Ctrl Pts',(51.5472232272244,-52.5418572398676,
-60.1281241911634));
#178348=CARTESIAN_POINT('Ctrl Pts',(51.5340632031642,-52.5424155428221,
-60.1521139245758));
#178349=CARTESIAN_POINT('Ctrl Pts',(51.5198393596716,-52.5430163636053,
-60.1757015641967));
#178350=CARTESIAN_POINT('Ctrl Pts',(51.5045674653046,-52.5436610817872,
-60.1987879161313));
#178351=CARTESIAN_POINT('Ctrl Pts',(51.4859751882522,-52.5444459732205,
-60.2268936534408));
#178352=CARTESIAN_POINT('Ctrl Pts',(51.465828954641,-52.5452958698133,-60.2542563740088));
#178353=CARTESIAN_POINT('Ctrl Pts',(51.4441764790361,-52.5462149460492,
-60.2806949718832));
#178354=CARTESIAN_POINT('Ctrl Pts',(51.4333502412336,-52.5466744841671,
-60.2939142708204));
#178355=CARTESIAN_POINT('Ctrl Pts',(51.4221477801373,-52.5471513466974,
-60.3069025151278));
#178356=CARTESIAN_POINT('Ctrl Pts',(51.4105771261679,-52.5476462362108,
-60.31963703049));
#178357=CARTESIAN_POINT('Ctrl Pts',(51.4053718121764,-52.547868873178,-60.3253659332093));
#178358=CARTESIAN_POINT('Ctrl Pts',(51.3998136381294,-52.5481087671514,
-60.3313432769659));
#178359=CARTESIAN_POINT('Ctrl Pts',(51.3942727867154,-52.5483470728028,
-60.3371563975798));
#178360=CARTESIAN_POINT('Ctrl Pts',(51.3885513244787,-52.5485931463181,
-60.3431590039636));
#178361=CARTESIAN_POINT('Ctrl Pts',(51.3828485134777,-52.5488375421032,
-60.348986368698));
#178362=CARTESIAN_POINT('Ctrl Pts',(51.3776130998802,-52.5490631132445,
-60.3542239160814));
#178363=CARTESIAN_POINT('Ctrl Pts',(51.3766484642515,-52.5491046751872,
-60.3551889448644));
#178364=CARTESIAN_POINT('Ctrl Pts',(51.3756997959006,-52.5491456067773,
-60.35613405362));
#178365=CARTESIAN_POINT('Ctrl Pts',(51.3747700261947,-52.5491858116419,
-60.3570567811866));
#178366=CARTESIAN_POINT('Ctrl Pts',(51.3526390232836,-52.5501427948295,
-60.3790201623695));
#178367=CARTESIAN_POINT('Ctrl Pts',(51.3288180644561,-52.5511805791252,
-60.4006133580694));
#178368=CARTESIAN_POINT('Ctrl Pts',(51.303238450899,-52.5522931541618,-60.4215416019267));
#178369=CARTESIAN_POINT('Ctrl Pts',(51.2783615492186,-52.5533751650271,
-60.441894914287));
#178370=CARTESIAN_POINT('Ctrl Pts',(51.251820855113,-52.5545278756568,-60.4616189803006));
#178371=CARTESIAN_POINT('Ctrl Pts',(51.2235909594968,-52.5557490630439,
-60.480412172761));
#178372=CARTESIAN_POINT('Ctrl Pts',(51.1953610638806,-52.5569702504311,
-60.4992053652214));
#178373=CARTESIAN_POINT('Ctrl Pts',(51.1654413519975,-52.5582598607915,
-60.5170673741396));
#178374=CARTESIAN_POINT('Ctrl Pts',(51.1338527951471,-52.5596197288762,
-60.533670156548));
#178375=CARTESIAN_POINT('Ctrl Pts',(51.1179098000908,-52.5603060650788,
-60.5420497124458));
#178376=CARTESIAN_POINT('Ctrl Pts',(51.1015424911284,-52.5610103672524,
-60.550108114142));
#178377=CARTESIAN_POINT('Ctrl Pts',(51.084758846286,-52.561733333384,-60.5578010742774));
#178378=CARTESIAN_POINT('Ctrl Pts',(51.0763670238648,-52.5620948164497,
-60.5616475543451));
#178379=CARTESIAN_POINT('Ctrl Pts',(51.0678711199813,-52.5624609657244,
-60.5654026796418));
#178380=CARTESIAN_POINT('Ctrl Pts',(51.0592725606525,-52.5628319059683,
-60.5690607763373));
#178381=CARTESIAN_POINT('Ctrl Pts',(51.0549732809881,-52.5630173760902,
-60.570889824685));
#178382=CARTESIAN_POINT('Ctrl Pts',(51.050648337782,-52.5632040439824,-60.5726946165842));
#178383=CARTESIAN_POINT('Ctrl Pts',(51.0462979245109,-52.5633919265719,
-60.5744744410932));
#178384=CARTESIAN_POINT('Ctrl Pts',(51.0436566325577,-52.5635059968317,
-60.5755550363978));
#178385=CARTESIAN_POINT('Ctrl Pts',(51.0402941624751,-52.5636516104294,
-60.5769130552168));
#178386=CARTESIAN_POINT('Ctrl Pts',(51.0375058723162,-52.5637720333269,
-60.5780234112916));
#178387=CARTESIAN_POINT('Ctrl Pts',(51.0357016317266,-52.5638499563074,
-60.5787418980289));
#178388=CARTESIAN_POINT('Ctrl Pts',(51.0341383546808,-52.5639173797187,
-60.5793580291782));
#178389=CARTESIAN_POINT('Ctrl Pts',(51.0331704763702,-52.5639592360933,
-60.5797383010625));
#178390=CARTESIAN_POINT('Ctrl Pts',(51.0177910339138,-52.5646243276637,
-60.5857807647669));
#178391=CARTESIAN_POINT('Ctrl Pts',(51.0007801641594,-52.5653695793414,
-60.5920329991653));
#178392=CARTESIAN_POINT('Ctrl Pts',(50.9820750389557,-52.5661894943757,
-60.5982457361307));
#178393=CARTESIAN_POINT('Ctrl Pts',(50.9637818123841,-52.5669913543647,
-60.6043216647171));
#178394=CARTESIAN_POINT('Ctrl Pts',(50.9438673635558,-52.5678645589462,
-60.6103597061813));
#178395=CARTESIAN_POINT('Ctrl Pts',(50.922288997128,-52.5688053727616,-60.6160795502538));
#178396=CARTESIAN_POINT('Ctrl Pts',(50.9015511090088,-52.5697095418381,
-60.6215766061516));
#178397=CARTESIAN_POINT('Ctrl Pts',(50.8792757525235,-52.5706760994577,
-60.6267794462207));
#178398=CARTESIAN_POINT('Ctrl Pts',(50.8554501117109,-52.571703924369,-60.6313985657287));
#178399=CARTESIAN_POINT('Ctrl Pts',(50.8322254333362,-52.5727058240945,
-60.6359011755762));
#178400=CARTESIAN_POINT('Ctrl Pts',(50.8075270414602,-52.5737658825278,
-60.6398488177474));
#178401=CARTESIAN_POINT('Ctrl Pts',(50.7813768373136,-52.5748860157782,
-60.6429384333447));
#178402=CARTESIAN_POINT('Ctrl Pts',(50.7562094246909,-52.5759640515575,
-60.6459119332894));
#178403=CARTESIAN_POINT('Ctrl Pts',(50.7296968033627,-52.5770976902288,
-60.6480902251289));
#178404=CARTESIAN_POINT('Ctrl Pts',(50.701898127047,-52.5782921070719,-60.6491761918521));
#178405=CARTESIAN_POINT('Ctrl Pts',(50.6889622309209,-52.5788479195876,
-60.6496815379545));
#178406=CARTESIAN_POINT('Ctrl Pts',(50.6757484635432,-52.579416947049,-60.64995));
#178407=CARTESIAN_POINT('Ctrl Pts',(50.6622663180714,-52.58000002,-60.64995));
#178408=CARTESIAN_POINT('Origin',(-83.2809572255632,-53.0800000199999,-55.2499500000008));
#178409=CARTESIAN_POINT('',(52.1679960743864,-53.08000002,-55.74995));
#178410=CARTESIAN_POINT('',(52.1679960743864,-53.08000002,-55.2499500000008));
#178411=CARTESIAN_POINT('',(-83.2809572255632,-53.0800000199999,-55.74995));
#178412=CARTESIAN_POINT('Origin',(-83.2809572255632,-53.5800000199999,-55.74995));
#178413=CARTESIAN_POINT('',(52.0805074108605,-53.58000002,-55.24995));
#178414=CARTESIAN_POINT('Ctrl Pts',(52.1679960743864,-53.08000002,-55.74995));
#178415=CARTESIAN_POINT('Ctrl Pts',(52.1679960743853,-53.08000002,-55.7240274879025));
#178416=CARTESIAN_POINT('Ctrl Pts',(52.1676229277195,-53.0821037999966,
-55.6978059982456));
#178417=CARTESIAN_POINT('Ctrl Pts',(52.1668732945162,-53.0863531598489,
-55.6716073791772));
#178418=CARTESIAN_POINT('Ctrl Pts',(52.1661171274503,-53.0906395574591,
-55.6451804108644));
#178419=CARTESIAN_POINT('Ctrl Pts',(52.1649778773335,-53.097109134404,-55.6187767710135));
#178420=CARTESIAN_POINT('Ctrl Pts',(52.1634571283852,-53.1057761303949,
-55.5927712432962));
#178421=CARTESIAN_POINT('Ctrl Pts',(52.162887909333,-53.1090202025008,-55.5830373277441));
#178422=CARTESIAN_POINT('Ctrl Pts',(52.1622652919261,-53.1125718487088,
-55.5733596268362));
#178423=CARTESIAN_POINT('Ctrl Pts',(52.1615895390385,-53.1164307841406,
-55.5637593430561));
#178424=CARTESIAN_POINT('Ctrl Pts',(52.1598114689721,-53.1265845810459,
-55.5384986634051));
#178425=CARTESIAN_POINT('Ctrl Pts',(52.1576634617214,-53.138872774755,-55.5137551378007));
#178426=CARTESIAN_POINT('Ctrl Pts',(52.1551452115047,-53.1532950399446,
-55.4899268496365));
#178427=CARTESIAN_POINT('Ctrl Pts',(52.154639066555,-53.1561937815553,-55.4851375846006));
#178428=CARTESIAN_POINT('Ctrl Pts',(52.1541179724691,-53.1591786897697,
-55.4803854546854));
#178429=CARTESIAN_POINT('Ctrl Pts',(52.1535819385834,-53.1622496940383,
-55.4756739403427));
#178430=CARTESIAN_POINT('Ctrl Pts',(52.1519804425163,-53.171424862605,-55.4615974576943));
#178431=CARTESIAN_POINT('Ctrl Pts',(52.1502454794431,-53.1813686932119,
-55.4478834521503));
#178432=CARTESIAN_POINT('Ctrl Pts',(52.1483770292202,-53.1920727510362,
-55.4346345057453));
#178433=CARTESIAN_POINT('Ctrl Pts',(52.1474428041087,-53.1974247799484,
-55.4280100325428));
#178434=CARTESIAN_POINT('Ctrl Pts',(52.1464752077285,-53.2029668120848,
-55.4215019156276));
#178435=CARTESIAN_POINT('Ctrl Pts',(52.1454742415707,-53.2086966555084,
-55.4151241749442));
#178436=CARTESIAN_POINT('Ctrl Pts',(52.1449737584918,-53.2115615772202,
-55.4119353046026));
#178437=CARTESIAN_POINT('Ctrl Pts',(52.1444649330249,-53.2144734423564,
-55.4087790343855));
#178438=CARTESIAN_POINT('Ctrl Pts',(52.1439477656179,-53.2174318984733,
-55.4056571673729));
#178439=CARTESIAN_POINT('Ctrl Pts',(52.1436468211098,-53.2191534515113,
-55.4038405240201));
#178440=CARTESIAN_POINT('Ctrl Pts',(52.143280043092,-53.221250909685,-55.4016627141745));
#178441=CARTESIAN_POINT('Ctrl Pts',(52.14295686691,-53.2230986811324,-55.399777933182));
#178442=CARTESIAN_POINT('Ctrl Pts',(52.1427246709765,-53.2244262697353,
-55.3984237539257));
#178443=CARTESIAN_POINT('Ctrl Pts',(52.142515217764,-53.2256236244485,-55.3972196143704));
#178444=CARTESIAN_POINT('Ctrl Pts',(52.1423712114632,-53.2264466282408,
-55.3963966105727));
#178445=CARTESIAN_POINT('Ctrl Pts',(52.1406599696547,-53.2362264676637,
-55.3866167710853));
#178446=CARTESIAN_POINT('Ctrl Pts',(52.1387217223152,-53.2471430351613,
-55.3765446166362));
#178447=CARTESIAN_POINT('Ctrl Pts',(52.1365506278256,-53.2593251459205,
-55.3664154210889));
#178448=CARTESIAN_POINT('Ctrl Pts',(52.1344728039586,-53.2709839109385,
-55.3567213776639));
#178449=CARTESIAN_POINT('Ctrl Pts',(52.1321815884692,-53.2838025291941,
-55.3469750522698));
#178450=CARTESIAN_POINT('Ctrl Pts',(52.1296756874241,-53.2978716577507,
-55.3374234998531));
#178451=CARTESIAN_POINT('Ctrl Pts',(52.1273146090356,-53.3111276941156,
-55.3284239569412));
#178452=CARTESIAN_POINT('Ctrl Pts',(52.1247628683279,-53.3254943241106,
-55.3195974076226));
#178453=CARTESIAN_POINT('Ctrl Pts',(52.1220241933538,-53.34101923469,-55.3111870425976));
#178454=CARTESIAN_POINT('Ctrl Pts',(52.1209256544364,-53.3472465959582,
-55.3078134720292));
#178455=CARTESIAN_POINT('Ctrl Pts',(52.1197971005136,-53.3536599563752,
-55.3045072865547));
#178456=CARTESIAN_POINT('Ctrl Pts',(52.1186390490883,-53.3602607645211,
-55.3012859404982));
#178457=CARTESIAN_POINT('Ctrl Pts',(52.115966476223,-53.3754942337384,-55.2938516574671));
#178458=CARTESIAN_POINT('Ctrl Pts',(52.1131421434498,-53.3917391401417,
-55.2868619640634));
#178459=CARTESIAN_POINT('Ctrl Pts',(52.1101547447912,-53.4089873541471,
-55.2805581080823));
#178460=CARTESIAN_POINT('Ctrl Pts',(52.1072491175401,-53.4257634481247,
-55.2744268019467));
#178461=CARTESIAN_POINT('Ctrl Pts',(52.1041891699554,-53.443488989223,-55.2689442788315));
#178462=CARTESIAN_POINT('Ctrl Pts',(52.1009710259383,-53.4621198498038,
-55.2643620190281));
#178463=CARTESIAN_POINT('Ctrl Pts',(52.0978518894124,-53.480177524488,-55.259920734285));
#178464=CARTESIAN_POINT('Ctrl Pts',(52.0945840982727,-53.4990858905757,
-55.2563251748323));
#178465=CARTESIAN_POINT('Ctrl Pts',(52.0911710656404,-53.5187660556456,
-55.2538325278704));
#178466=CARTESIAN_POINT('Ctrl Pts',(52.0877580330082,-53.5384462207154,
-55.2513398809084));
#178467=CARTESIAN_POINT('Ctrl Pts',(52.0841996828067,-53.5588985892674,
-55.24995));
#178468=CARTESIAN_POINT('Ctrl Pts',(52.0805074108605,-53.58000002,-55.24995));
#178469=CARTESIAN_POINT('',(60.,-53.58000002,-55.24995));
#178470=CARTESIAN_POINT('Origin',(60.,28.41999998,-55.24995));
#178471=CARTESIAN_POINT('',(52.0367630790975,-54.08000002,-55.24995));
#178472=CARTESIAN_POINT('',(59.2602401389193,28.4847205815761,-55.24995));
#178473=CARTESIAN_POINT('',(60.,-54.08000002,-55.24995));
#178474=CARTESIAN_POINT('Origin',(60.,-54.08000002,-55.74995));
#178475=CARTESIAN_POINT('',(51.9492744155716,-54.58000002,-55.74995));
#178476=CARTESIAN_POINT('Ctrl Pts',(52.0367630790975,-54.08000002,-55.24995));
#178477=CARTESIAN_POINT('Ctrl Pts',(52.0329861847726,-54.1015850698379,
-55.24995));
#178478=CARTESIAN_POINT('Ctrl Pts',(52.0293284334102,-54.1224892145297,
-55.2514041468282));
#178479=CARTESIAN_POINT('Ctrl Pts',(52.025812604289,-54.1425822699015,-55.2540052053876));
#178480=CARTESIAN_POINT('Ctrl Pts',(52.0223225188274,-54.1625281995854,
-55.256587218435));
#178481=CARTESIAN_POINT('Ctrl Pts',(52.0189721930573,-54.181675398978,-55.2602996172422));
#178482=CARTESIAN_POINT('Ctrl Pts',(52.0157756716516,-54.1999436024055,
-55.2648742467057));
#178483=CARTESIAN_POINT('Ctrl Pts',(52.012433722523,-54.2190429290726,-55.2696570017726));
#178484=CARTESIAN_POINT('Ctrl Pts',(52.0092598588055,-54.2371816432191,
-55.2753821626562));
#178485=CARTESIAN_POINT('Ctrl Pts',(52.0062619536595,-54.2543147495282,
-55.2817780783384));
#178486=CARTESIAN_POINT('Ctrl Pts',(52.0034615083816,-54.2703193675273,
-55.2877527209631));
#178487=CARTESIAN_POINT('Ctrl Pts',(52.0008144668557,-54.2854472790713,
-55.2943131225512));
#178488=CARTESIAN_POINT('Ctrl Pts',(51.9983217548574,-54.2996931933296,
-55.3012636513334));
#178489=CARTESIAN_POINT('Ctrl Pts',(51.9954258794196,-54.3162431971871,
-55.3093383368938));
#178490=CARTESIAN_POINT('Ctrl Pts',(51.9927365497521,-54.3316127865661,
-55.3179437622875));
#178491=CARTESIAN_POINT('Ctrl Pts',(51.9902476016194,-54.3458371902331,
-55.3268178701949));
#178492=CARTESIAN_POINT('Ctrl Pts',(51.9875709569559,-54.3611342844827,
-55.3363611922362));
#178493=CARTESIAN_POINT('Ctrl Pts',(51.9851258946601,-54.3751078794446,
-55.3462154234411));
#178494=CARTESIAN_POINT('Ctrl Pts',(51.982897837809,-54.3878412826151,-55.3561026477775));
#178495=CARTESIAN_POINT('Ctrl Pts',(51.9806310002184,-54.4007963187263,
-55.3661619655108));
#178496=CARTESIAN_POINT('Ctrl Pts',(51.9785887493121,-54.412467836063,-55.3762552368074));
#178497=CARTESIAN_POINT('Ctrl Pts',(51.9767506920852,-54.4229723811826,
-55.3861352301679));
#178498=CARTESIAN_POINT('Ctrl Pts',(51.9764819137112,-54.4245084566188,
-55.3875799776498));
#178499=CARTESIAN_POINT('Ctrl Pts',(51.9762174950408,-54.426019616235,-55.3890202398743));
#178500=CARTESIAN_POINT('Ctrl Pts',(51.9759573640587,-54.4275062716008,
-55.3904553319312));
#178501=CARTESIAN_POINT('Ctrl Pts',(51.9757360420398,-54.4287711327266,
-55.3916763224825));
#178502=CARTESIAN_POINT('Ctrl Pts',(51.9755897917165,-54.4296069571404,
-55.3924916493989));
#178503=CARTESIAN_POINT('Ctrl Pts',(51.9753858285837,-54.4307725552473,
-55.3936383709987));
#178504=CARTESIAN_POINT('Ctrl Pts',(51.9752572031324,-54.4315076174146,
-55.3943615290577));
#178505=CARTESIAN_POINT('Ctrl Pts',(51.9751056704388,-54.4323735725912,
-55.3952167714171));
#178506=CARTESIAN_POINT('Ctrl Pts',(51.9748992092877,-54.4335534087318,
-55.3963966075453));
#178507=CARTESIAN_POINT('Ctrl Pts',(51.9712989344309,-54.4541274216573,
-55.4169706202541));
#178508=CARTESIAN_POINT('Ctrl Pts',(51.9680709073607,-54.4725747479987,
-55.4391630475832));
#178509=CARTESIAN_POINT('Ctrl Pts',(51.9652226122223,-54.4888523769156,
-55.4624843705238));
#178510=CARTESIAN_POINT('Ctrl Pts',(51.9623708011184,-54.505150099109,-55.485834481551));
#178511=CARTESIAN_POINT('Ctrl Pts',(51.9598996566805,-54.5192727832056,
-55.510316262681));
#178512=CARTESIAN_POINT('Ctrl Pts',(51.9578126185396,-54.5312005418129,
-55.5354850646356));
#178513=CARTESIAN_POINT('Ctrl Pts',(51.9557220179087,-54.5431486606235,
-55.5606968287208));
#178514=CARTESIAN_POINT('Ctrl Pts',(51.9540168314626,-54.5528943804173,
-55.586597961014));
#178515=CARTESIAN_POINT('Ctrl Pts',(51.952696491472,-54.5604407216792,-55.6127884602357));
#178516=CARTESIAN_POINT('Ctrl Pts',(51.9513702043265,-54.5680210536256,
-55.63909692828));
#178517=CARTESIAN_POINT('Ctrl Pts',(51.9504322340363,-54.5733821741393,
-55.6656973722207));
#178518=CARTESIAN_POINT('Ctrl Pts',(51.9498780110353,-54.5765499745511,
-55.6922317349674));
#178519=CARTESIAN_POINT('Ctrl Pts',(51.9494745942481,-54.5788558042664,
-55.7115459953829));
#178520=CARTESIAN_POINT('Ctrl Pts',(51.9492744155716,-54.58000002,-55.7308262346054));
#178521=CARTESIAN_POINT('Ctrl Pts',(51.9492744155716,-54.58000002,-55.74995));
#178522=CARTESIAN_POINT('',(60.,-54.58000002,-55.74995));
#178523=CARTESIAN_POINT('Origin',(60.,-54.58000002,-55.24995));
#178524=CARTESIAN_POINT('',(51.9492744155716,-54.58000002,-59.64995));
#178525=CARTESIAN_POINT('',(51.9492744155716,-54.58000002,-55.24995));
#178526=CARTESIAN_POINT('Ctrl Pts',(51.9492744155716,-54.58000002,-59.64995));
#178527=CARTESIAN_POINT('Ctrl Pts',(51.9492744155546,-54.58000002,-59.8463349320562));
#178528=CARTESIAN_POINT('Ctrl Pts',(51.9100842947729,-54.58000002,-60.0425718399611));
#178529=CARTESIAN_POINT('Ctrl Pts',(51.7592308304456,-54.58000002,-60.4053784571342));
#178530=CARTESIAN_POINT('Ctrl Pts',(51.6476268087097,-54.58000002,-60.5717700902076));
#178531=CARTESIAN_POINT('Ctrl Pts',(51.3688859524529,-54.58000002,-60.8494502533521));
#178532=CARTESIAN_POINT('Ctrl Pts',(51.2018587304451,-54.58000002,-60.9606295880612));
#178533=CARTESIAN_POINT('Ctrl Pts',(50.8376662507899,-54.58000002,-61.1109090094727));
#178534=CARTESIAN_POINT('Ctrl Pts',(50.6406797499036,-54.58000002,-61.149949999985));
#178535=CARTESIAN_POINT('Ctrl Pts',(50.4435446592566,-54.58000002,-61.14995));
#178536=CARTESIAN_POINT('Ctrl Pts',(51.9492744155716,-54.58000002,-59.64995));
#178537=CARTESIAN_POINT('Ctrl Pts',(51.491108828563,-54.58000002,-59.64995));
#178538=CARTESIAN_POINT('Ctrl Pts',(51.4511770665258,-55.0364221486262,
-59.64995));
#178539=CARTESIAN_POINT('Ctrl Pts',(51.9492744155546,-54.58000002,-59.8463349320562));
#178540=CARTESIAN_POINT('Ctrl Pts',(51.4911088285445,-54.58000002,-59.7861314644994));
#178541=CARTESIAN_POINT('Ctrl Pts',(51.4511770665255,-55.0364221486294,
-59.7808732880376));
#178542=CARTESIAN_POINT('Ctrl Pts',(51.9100842947729,-54.58000002,-60.0425718399611));
#178543=CARTESIAN_POINT('Ctrl Pts',(51.4627154806765,-54.58000002,-59.9224177216068));
#178544=CARTESIAN_POINT('Ctrl Pts',(51.4249510883276,-55.0375563641359,
-59.9116978933072));
#178545=CARTESIAN_POINT('Ctrl Pts',(51.7592308304456,-54.58000002,-60.4053784571342));
#178546=CARTESIAN_POINT('Ctrl Pts',(51.3546036645756,-54.58000002,-60.1718710142638));
#178547=CARTESIAN_POINT('Ctrl Pts',(51.3240001449277,-55.0419222689988,
-60.153568971423));
#178548=CARTESIAN_POINT('Ctrl Pts',(51.6476268087097,-54.58000002,-60.5717700902076));
#178549=CARTESIAN_POINT('Ctrl Pts',(51.2745855330292,-54.58000002,-60.2852157712116));
#178550=CARTESIAN_POINT('Ctrl Pts',(51.2493148777934,-55.0451522414979,
-60.2644967268049));
#178551=CARTESIAN_POINT('Ctrl Pts',(51.3688859524529,-54.58000002,-60.8494502533521));
#178552=CARTESIAN_POINT('Ctrl Pts',(51.0776549189628,-54.58000002,-60.4706504746468));
#178553=CARTESIAN_POINT('Ctrl Pts',(51.0627818569665,-55.0532193817859,
-60.4496168355682));
#178554=CARTESIAN_POINT('Ctrl Pts',(51.2018587304451,-54.58000002,-60.9606295880612));
#178555=CARTESIAN_POINT('Ctrl Pts',(50.9603478356083,-54.5800000199993,
-60.5426326522464));
#178556=CARTESIAN_POINT('Ctrl Pts',(50.9510074558263,-55.0580533772402,
-60.5237363920407));
#178557=CARTESIAN_POINT('Ctrl Pts',(50.8376662507899,-54.58000002,-61.1109090094727));
#178558=CARTESIAN_POINT('Ctrl Pts',(50.7089726167645,-54.5800000200007,
-60.6353187454038));
#178559=CARTESIAN_POINT('Ctrl Pts',(50.707290319039,-55.0685936039748,-60.6239226729819));
#178560=CARTESIAN_POINT('Ctrl Pts',(50.6406797499036,-54.58000002,-61.149949999985));
#178561=CARTESIAN_POINT('Ctrl Pts',(50.5746911290892,-54.58000002,-60.6556217969812));
#178562=CARTESIAN_POINT('Ctrl Pts',(50.5754672071858,-55.0742946617933,
-60.64995));
#178563=CARTESIAN_POINT('Ctrl Pts',(50.4435446592566,-54.58000002,-61.14995));
#178564=CARTESIAN_POINT('Ctrl Pts',(50.4435446592566,-54.58000002,-60.64995));
#178565=CARTESIAN_POINT('Ctrl Pts',(50.4435446592566,-55.08000002,-60.64995));
#178566=CARTESIAN_POINT('',(51.4511770665258,-55.0364221486262,-59.64995));
#178567=CARTESIAN_POINT('Origin',(51.9492744155716,-55.08000002,-59.64995));
#178568=CARTESIAN_POINT('Ctrl Pts',(50.4435446592566,-55.08000002,-60.64995));
#178569=CARTESIAN_POINT('Ctrl Pts',(50.4717376569834,-55.0787807352492,
-60.64995));
#178570=CARTESIAN_POINT('Ctrl Pts',(50.4987528304453,-55.077612388791,-60.6487640563021));
#178571=CARTESIAN_POINT('Ctrl Pts',(50.5245169140085,-55.0764981492017,
-60.6466905424058));
#178572=CARTESIAN_POINT('Ctrl Pts',(50.5516203999557,-55.075325983424,-60.6445092323426));
#178573=CARTESIAN_POINT('Ctrl Pts',(50.5773396808283,-55.074213681452,-60.6413458430357));
#178574=CARTESIAN_POINT('Ctrl Pts',(50.6016351555871,-55.073162955943,-60.6375094925897));
#178575=CARTESIAN_POINT('Ctrl Pts',(50.6232165566326,-55.072229608115,-60.6341017049935));
#178576=CARTESIAN_POINT('Ctrl Pts',(50.6436754675382,-55.071344805501,-60.6301623056439));
#178577=CARTESIAN_POINT('Ctrl Pts',(50.6630080918224,-55.0705087122905,
-60.6258833725764));
#178578=CARTESIAN_POINT('Ctrl Pts',(50.6862762675633,-55.0695024151902,
-60.6207333750833));
#178579=CARTESIAN_POINT('Ctrl Pts',(50.707913749224,-55.0685666419995,-60.6150923632743));
#178580=CARTESIAN_POINT('Ctrl Pts',(50.7279455563559,-55.0677003106784,
-60.6092528148321));
#178581=CARTESIAN_POINT('Ctrl Pts',(50.748808680122,-55.0667980267528,-60.6031709261096));
#178582=CARTESIAN_POINT('Ctrl Pts',(50.7679309670258,-55.0659710301685,
-60.596873782305));
#178583=CARTESIAN_POINT('Ctrl Pts',(50.7853656316707,-55.0652170195116,
-60.5906417203197));
#178584=CARTESIAN_POINT('Ctrl Pts',(50.7928631219894,-55.0648927696499,
-60.5879617247275));
#178585=CARTESIAN_POINT('Ctrl Pts',(50.8000487033219,-55.0645820091614,
-60.5852931621332));
#178586=CARTESIAN_POINT('Ctrl Pts',(50.8069275976617,-55.0642845122066,
-60.5826554870772));
#178587=CARTESIAN_POINT('Ctrl Pts',(50.808671465437,-55.0642090937851,-60.5819868103532));
#178588=CARTESIAN_POINT('Ctrl Pts',(50.8094883279451,-55.0641737217418,
-60.5816714634925));
#178589=CARTESIAN_POINT('Ctrl Pts',(50.8112410587908,-55.0640978936747,
-60.5809901112017));
#178590=CARTESIAN_POINT('Ctrl Pts',(50.8120502073179,-55.0640628876332,
-60.5806755647874));
#178591=CARTESIAN_POINT('Ctrl Pts',(50.8130586841946,-55.0640192649628,
-60.5802826897809));
#178592=CARTESIAN_POINT('Ctrl Pts',(50.814448302058,-55.0639591688398,-60.579736993315));
#178593=CARTESIAN_POINT('Ctrl Pts',(50.8193803336296,-55.0637458756867,
-60.5778002074769));
#178594=CARTESIAN_POINT('Ctrl Pts',(50.8242806369343,-55.0635339542666,
-60.5758307565185));
#178595=CARTESIAN_POINT('Ctrl Pts',(50.8291488883492,-55.0633234186072,
-60.5738295347324));
#178596=CARTESIAN_POINT('Ctrl Pts',(50.8621978557542,-55.0618941608409,
-60.5602438942337));
#178597=CARTESIAN_POINT('Ctrl Pts',(50.8937577303036,-55.0605292840505,
-60.5452002171636));
#178598=CARTESIAN_POINT('Ctrl Pts',(50.9237804823248,-55.0592308752312,
-60.5290286719171));
#178599=CARTESIAN_POINT('Ctrl Pts',(50.9524579513628,-55.057990646531,-60.5135817539338));
#178600=CARTESIAN_POINT('Ctrl Pts',(50.9797334822037,-55.0568110401798,
-60.4971053444489));
#178601=CARTESIAN_POINT('Ctrl Pts',(51.00559583825,-55.0556925505231,-60.479855117644));
#178602=CARTESIAN_POINT('Ctrl Pts',(51.034637597282,-55.0544365587244,-60.4604842247053));
#178603=CARTESIAN_POINT('Ctrl Pts',(51.0618981348816,-55.0532576008103,
-60.4401373914491));
#178604=CARTESIAN_POINT('Ctrl Pts',(51.08740091482,-55.0521546620244,-60.4191325982561));
#178605=CARTESIAN_POINT('Ctrl Pts',(51.0993901420219,-55.0516361544843,
-60.4092579399431));
#178606=CARTESIAN_POINT('Ctrl Pts',(51.1109913826958,-55.0511344265027,
-60.3992372751482));
#178607=CARTESIAN_POINT('Ctrl Pts',(51.1222095012985,-55.0506492677027,
-60.3891007231335));
#178608=CARTESIAN_POINT('Ctrl Pts',(51.1276500479029,-55.0504139761039,
-60.3841847130967));
#178609=CARTESIAN_POINT('Ctrl Pts',(51.1326801607925,-55.0501964348529,
-60.3795368119712));
#178610=CARTESIAN_POINT('Ctrl Pts',(51.1377531641319,-55.049977032032,-60.3747537950781));
#178611=CARTESIAN_POINT('Ctrl Pts',(51.1426753735635,-55.0497641509116,
-60.3701129523094));
#178612=CARTESIAN_POINT('Ctrl Pts',(51.1476381129635,-55.0495495106959,
-60.3653448275671));
#178613=CARTESIAN_POINT('Ctrl Pts',(51.1530224316603,-55.0493166257935,
-60.3600469446924));
#178614=CARTESIAN_POINT('Ctrl Pts',(51.1540160724075,-55.0492736484102,
-60.35906925511));
#178615=CARTESIAN_POINT('Ctrl Pts',(51.155023969336,-55.0492300540593,-60.3580734250976));
#178616=CARTESIAN_POINT('Ctrl Pts',(51.1560483702627,-55.0491857454898,
-60.3570567840803));
#178617=CARTESIAN_POINT('Ctrl Pts',(51.1901033100392,-55.047712761985,-60.3232598128792));
#178618=CARTESIAN_POINT('Ctrl Pts',(51.2213719515089,-55.0463604151168,
-60.2873222686653));
#178619=CARTESIAN_POINT('Ctrl Pts',(51.2497281199733,-55.0451340889359,
-60.2497596531771));
#178620=CARTESIAN_POINT('Ctrl Pts',(51.2785117986632,-55.0438892741154,
-60.2116307269678));
#178621=CARTESIAN_POINT('Ctrl Pts',(51.3042945550902,-55.0427743071565,
-60.1718273266932));
#178622=CARTESIAN_POINT('Ctrl Pts',(51.3269711323931,-55.0417936659585,
-60.1308415655649));
#178623=CARTESIAN_POINT('Ctrl Pts',(51.3447218971007,-55.0410260399215,
-60.0987587431693));
#178624=CARTESIAN_POINT('Ctrl Pts',(51.360569916253,-55.0403406975752,-60.0659504756251));
#178625=CARTESIAN_POINT('Ctrl Pts',(51.3744756167235,-55.0397393152828,
-60.0326334324049));
#178626=CARTESIAN_POINT('Ctrl Pts',(51.375857460983,-55.0396795544193,-60.0293226344328));
#178627=CARTESIAN_POINT('Ctrl Pts',(51.3772201029237,-55.0396206236095,
-60.0260068878549));
#178628=CARTESIAN_POINT('Ctrl Pts',(51.3785635834251,-55.0395625210514,
-60.0226864252214));
#178629=CARTESIAN_POINT('Ctrl Pts',(51.3961159803762,-55.0388034187329,
-59.9793050154134));
#178630=CARTESIAN_POINT('Ctrl Pts',(51.4103970516706,-55.0381857940084,
-59.9351228143234));
#178631=CARTESIAN_POINT('Ctrl Pts',(51.4215008278151,-55.0377055802667,
-59.8906338472908));
#178632=CARTESIAN_POINT('Ctrl Pts',(51.4327391040554,-55.0372195496935,
-59.8456059851787));
#178633=CARTESIAN_POINT('Ctrl Pts',(51.440722662487,-55.0368742784617,-59.8002638479446));
#178634=CARTESIAN_POINT('Ctrl Pts',(51.4455573094817,-55.0366651906799,
-59.7550665530516));
#178635=CARTESIAN_POINT('Ctrl Pts',(51.4493215654944,-55.0365023949389,
-59.7198759405322));
#178636=CARTESIAN_POINT('Ctrl Pts',(51.4511770665258,-55.0364221486262,
-59.684772050632));
#178637=CARTESIAN_POINT('Ctrl Pts',(51.4511770665258,-55.0364221486262,
-59.64995));
#178638=CARTESIAN_POINT('Origin',(-83.2809572255632,-38.28000002,-55.2499500000007));
#178639=CARTESIAN_POINT('',(53.3753396310439,-38.28000002,-55.74995));
#178640=CARTESIAN_POINT('',(-83.2809572255632,-38.28000002,-55.74995));
#178641=CARTESIAN_POINT('',(53.3753396310439,-38.28000002,-60.0032396521563));
#178642=CARTESIAN_POINT('',(53.3753396310439,-38.28000002,-55.2499500000007));
#178643=CARTESIAN_POINT('Ctrl Pts',(53.3753396310439,-38.28000002,-60.0032396521563));
#178644=CARTESIAN_POINT('Ctrl Pts',(53.3753396310439,-38.28000002,-60.0589758767835));
#178645=CARTESIAN_POINT('Ctrl Pts',(53.3722852139107,-38.28000002,-60.1146939077158));
#178646=CARTESIAN_POINT('Ctrl Pts',(53.3663204826485,-38.28000002,-60.1700562792009));
#178647=CARTESIAN_POINT('Ctrl Pts',(53.3600346473474,-38.28000002,-60.2283990164902));
#178648=CARTESIAN_POINT('Ctrl Pts',(53.3505169273234,-38.28000002,-60.2863478004803));
#178649=CARTESIAN_POINT('Ctrl Pts',(53.3378827651207,-38.28000002,-60.3435292248106));
#178650=CARTESIAN_POINT('Ctrl Pts',(53.3251015247972,-38.28000002,-60.4013763154743));
#178651=CARTESIAN_POINT('Ctrl Pts',(53.3091307297629,-38.28000002,-60.4584393902281));
#178652=CARTESIAN_POINT('Ctrl Pts',(53.2900367865637,-38.2800000200001,
-60.5143350099522));
#178653=CARTESIAN_POINT('Ctrl Pts',(53.2713085336432,-38.2800000200001,
-60.5691601077554));
#178654=CARTESIAN_POINT('Ctrl Pts',(53.2495752764747,-38.2800000200002,
-60.622863235497));
#178655=CARTESIAN_POINT('Ctrl Pts',(53.2248527900283,-38.2800000200003,
-60.6750669890669));
#178656=CARTESIAN_POINT('Ctrl Pts',(53.2194501346315,-38.2800000200003,
-60.6864751818298));
#178657=CARTESIAN_POINT('Ctrl Pts',(53.2139045547126,-38.2800000200004,
-60.6978116715984));
#178658=CARTESIAN_POINT('Ctrl Pts',(53.2082159323664,-38.2800000200004,
-60.7090723322489));
#178659=CARTESIAN_POINT('Ctrl Pts',(53.2081854825349,-38.2800000200004,
-60.7091326078656));
#178660=CARTESIAN_POINT('Ctrl Pts',(53.2081550286956,-38.2800000200004,
-60.7091928811299));
#178661=CARTESIAN_POINT('Ctrl Pts',(53.2081245708486,-38.2800000200004,
-60.709253152041));
#178662=CARTESIAN_POINT('Ctrl Pts',(53.1761754390121,-38.2800000200006,
-60.7724750628697));
#178663=CARTESIAN_POINT('Ctrl Pts',(53.1397892479682,-38.2800000200007,
-60.8333871332408));
#178664=CARTESIAN_POINT('Ctrl Pts',(53.0993211720577,-38.2800000200006,
-60.8914909948819));
#178665=CARTESIAN_POINT('Ctrl Pts',(53.0593989894052,-38.2800000200005,
-60.9488110657047));
#178666=CARTESIAN_POINT('Ctrl Pts',(53.0155035526426,-38.2800000200003,
-61.0033990731716));
#178667=CARTESIAN_POINT('Ctrl Pts',(52.9679386190623,-38.2800000200002,
-61.0547432417683));
#178668=CARTESIAN_POINT('Ctrl Pts',(52.9223553337127,-38.2800000200001,
-61.1039483118066));
#178669=CARTESIAN_POINT('Ctrl Pts',(52.8734012103226,-38.28000002,-61.1501747492908));
#178670=CARTESIAN_POINT('Ctrl Pts',(52.8213200539949,-38.28000002,-61.192931263928));
#178671=CARTESIAN_POINT('Ctrl Pts',(52.7942271507165,-38.28000002,-61.215173437437));
#178672=CARTESIAN_POINT('Ctrl Pts',(52.7662877001539,-38.28000002,-61.2364758695291));
#178673=CARTESIAN_POINT('Ctrl Pts',(52.7375342894721,-38.28000002,-61.2567639997892));
#178674=CARTESIAN_POINT('Ctrl Pts',(53.3753396310439,-38.28000002,-60.0032396521563));
#178675=CARTESIAN_POINT('Ctrl Pts',(52.9171740440352,-38.28000002,-60.0032396521562));
#178676=CARTESIAN_POINT('Ctrl Pts',(52.877242281998,-38.7364221486262,-60.0032396521562));
#178677=CARTESIAN_POINT('Ctrl Pts',(53.3753396328414,-38.28000002,-60.244893556147));
#178678=CARTESIAN_POINT('Ctrl Pts',(52.9343465054118,-38.28000002,-60.1721379135101));
#178679=CARTESIAN_POINT('Ctrl Pts',(52.8788986395818,-38.7174898948119,
-60.1690974501184));
#178680=CARTESIAN_POINT('Ctrl Pts',(53.317850201657,-38.28000002,-60.4921247747839));
#178681=CARTESIAN_POINT('Ctrl Pts',(52.9111776732915,-38.28000002,-60.3567456822519));
#178682=CARTESIAN_POINT('Ctrl Pts',(52.8422535332614,-38.6982739394415,
-60.3389622441799));
#178683=CARTESIAN_POINT('Ctrl Pts',(53.0984000724383,-38.28000002,-60.9263821015509));
#178684=CARTESIAN_POINT('Ctrl Pts',(52.7751833670329,-38.28000002,-60.6874729542071));
#178685=CARTESIAN_POINT('Ctrl Pts',(52.6988044737759,-38.6656865171052,
-60.6372698562504));
#178686=CARTESIAN_POINT('Ctrl Pts',(52.9360725977236,-38.28000002,-61.1166772774171));
#178687=CARTESIAN_POINT('Ctrl Pts',(52.6635868839933,-38.28000002,-60.8378349680257));
#178688=CARTESIAN_POINT('Ctrl Pts',(52.5917711956707,-38.6521075044106,
-60.7679496692827));
#178689=CARTESIAN_POINT('Ctrl Pts',(52.7375342894721,-38.28000002,-61.2567639997892));
#178690=CARTESIAN_POINT('Ctrl Pts',(52.5193575501106,-38.28000002,-60.9475523661896));
#178691=CARTESIAN_POINT('Ctrl Pts',(52.4601060488526,-38.6442121687577,
-60.8635779995784));
#178692=CARTESIAN_POINT('',(52.8772422786263,-38.736422148331,-60.0032396521556));
#178693=CARTESIAN_POINT('Origin',(53.3753396310439,-38.78000002,-60.0032396521563));
#178694=CARTESIAN_POINT('Ctrl Pts',(52.4601061816814,-38.6442121767227,
-60.8635779031049));
#178695=CARTESIAN_POINT('Ctrl Pts',(52.4857623597633,-38.6457506363329,
-60.8449438340698));
#178696=CARTESIAN_POINT('Ctrl Pts',(52.5112243232531,-38.6475495400589,
-60.8244412198977));
#178697=CARTESIAN_POINT('Ctrl Pts',(52.536247504591,-38.6496228467422,-60.8019625565231));
#178698=CARTESIAN_POINT('Ctrl Pts',(52.5601660855939,-38.6516046312794,
-60.7804761706195));
#178699=CARTESIAN_POINT('Ctrl Pts',(52.5836838164615,-38.6538371698229,
-60.7571840989168));
#178700=CARTESIAN_POINT('Ctrl Pts',(52.6065464778335,-38.6563279032125,
-60.732017239825));
#178701=CARTESIAN_POINT('Ctrl Pts',(52.6142960302199,-38.6571721648918,
-60.7234866540913));
#178702=CARTESIAN_POINT('Ctrl Pts',(52.6219699584021,-38.6580460472365,
-60.714740899271));
#178703=CARTESIAN_POINT('Ctrl Pts',(52.6295572148155,-38.6589496944378,
-60.7057780511307));
#178704=CARTESIAN_POINT('Ctrl Pts',(52.6511165291618,-38.6615174228776,
-60.6803099701844));
#178705=CARTESIAN_POINT('Ctrl Pts',(52.6719774600956,-38.6643258339855,
-60.6530877674629));
#178706=CARTESIAN_POINT('Ctrl Pts',(52.6918501867659,-38.6673726516042,
-60.6241039054663));
#178707=CARTESIAN_POINT('Ctrl Pts',(52.7094328672616,-38.6700683672755,
-60.5984600170623));
#178708=CARTESIAN_POINT('Ctrl Pts',(52.7262421963706,-38.6729508212541,
-60.5714358630291));
#178709=CARTESIAN_POINT('Ctrl Pts',(52.7420475179718,-38.6760127168085,
-60.5430616037942));
#178710=CARTESIAN_POINT('Ctrl Pts',(52.7498509593379,-38.6775244432403,
-60.5290525963326));
#178711=CARTESIAN_POINT('Ctrl Pts',(52.7574093262473,-38.6790798381767,
-60.5147148820475));
#178712=CARTESIAN_POINT('Ctrl Pts',(52.7646922891108,-38.6806773954924,
-60.500056191524));
#178713=CARTESIAN_POINT('Ctrl Pts',(52.7663755524841,-38.6810466284222,
-60.4966682246594));
#178714=CARTESIAN_POINT('Ctrl Pts',(52.7683001317608,-38.6814754219272,
-60.4927379935618));
#178715=CARTESIAN_POINT('Ctrl Pts',(52.7699624760655,-38.6818517038284,
-60.4892922803886));
#178716=CARTESIAN_POINT('Ctrl Pts',(52.7701550375918,-38.6818952913193,
-60.4888931381737));
#178717=CARTESIAN_POINT('Ctrl Pts',(52.770344131837,-38.6819381701835,-60.4885005245996));
#178718=CARTESIAN_POINT('Ctrl Pts',(52.7705290151266,-38.6819801632172,
-60.4881160560812));
#178719=CARTESIAN_POINT('Ctrl Pts',(52.7711948210125,-38.6821313894804,
-60.4867314993527));
#178720=CARTESIAN_POINT('Ctrl Pts',(52.7718059718363,-38.6822711505817,
-60.4854523452323));
#178721=CARTESIAN_POINT('Ctrl Pts',(52.772328349338,-38.6823911134328,-60.4843545222568));
#178722=CARTESIAN_POINT('Ctrl Pts',(52.7827597911478,-38.6847866712374,
-60.462431915619));
#178723=CARTESIAN_POINT('Ctrl Pts',(52.7929574618894,-38.6873654107239,
-60.4389746467284));
#178724=CARTESIAN_POINT('Ctrl Pts',(52.802672590598,-38.6901321259938,-60.4139448759755));
#178725=CARTESIAN_POINT('Ctrl Pts',(52.8072602409309,-38.6914386163769,
-60.4021253891141));
#178726=CARTESIAN_POINT('Ctrl Pts',(52.8117398566731,-38.6927869530701,
-60.3899557998885));
#178727=CARTESIAN_POINT('Ctrl Pts',(52.816082856994,-38.6941772106881,-60.3774354714578));
#178728=CARTESIAN_POINT('Ctrl Pts',(52.8228528775337,-38.696344392805,-60.3579183463419));
#178729=CARTESIAN_POINT('Ctrl Pts',(52.8292924909856,-38.6986064410768,
-60.3375485860623));
#178730=CARTESIAN_POINT('Ctrl Pts',(52.8352842226712,-38.7009701754622,
-60.3163362365538));
#178731=CARTESIAN_POINT('Ctrl Pts',(52.838280088514,-38.7021520426549,-60.3057300617996));
#178732=CARTESIAN_POINT('Ctrl Pts',(52.8411638244454,-38.7033593973482,
-60.2949134970024));
#178733=CARTESIAN_POINT('Ctrl Pts',(52.8439198470878,-38.704593041393,-60.2838895088064));
#178734=CARTESIAN_POINT('Ctrl Pts',(52.845297858409,-38.7052098634154,-60.2783775147083));
#178735=CARTESIAN_POINT('Ctrl Pts',(52.8466439377268,-38.7058332566417,
-60.2728136617708));
#178736=CARTESIAN_POINT('Ctrl Pts',(52.8479560679907,-38.7064633552259,
-60.2671984626355));
#178737=CARTESIAN_POINT('Ctrl Pts',(52.8486121331227,-38.706778404518,-60.2643908630679));
#178738=CARTESIAN_POINT('Ctrl Pts',(52.8492597107986,-38.7070951300932,
-60.2615704268027));
#178739=CARTESIAN_POINT('Ctrl Pts',(52.8498985461022,-38.7074135496482,
-60.2587372223283));
#178740=CARTESIAN_POINT('Ctrl Pts',(52.8503738360279,-38.7076504520326,
-60.2566293338998));
#178741=CARTESIAN_POINT('Ctrl Pts',(52.8510433499346,-38.7079898874832,
-60.2536116819445));
#178742=CARTESIAN_POINT('Ctrl Pts',(52.8514616955767,-38.7082051395534,
-60.2516988745454));
#178743=CARTESIAN_POINT('Ctrl Pts',(52.8516056466525,-38.7082792069368,
-60.2510406851077));
#178744=CARTESIAN_POINT('Ctrl Pts',(52.8517203364549,-38.7083385534396,
-60.2505134212631));
#178745=CARTESIAN_POINT('Ctrl Pts',(52.8517885682409,-38.7083739084269,
-60.2501993750543));
#178746=CARTESIAN_POINT('Ctrl Pts',(52.8535288336456,-38.7092756444794,
-60.2421895634358));
#178747=CARTESIAN_POINT('Ctrl Pts',(52.8555656110489,-38.7103785356354,
-60.2324101905088));
#178748=CARTESIAN_POINT('Ctrl Pts',(52.8577577286042,-38.7116860742924,
-60.2208374968453));
#178749=CARTESIAN_POINT('Ctrl Pts',(52.8598955118563,-38.7129612040115,
-60.2095516464875));
#178750=CARTESIAN_POINT('Ctrl Pts',(52.8621809224268,-38.7144310546655,
-60.1965595734014));
#178751=CARTESIAN_POINT('Ctrl Pts',(52.8644347882344,-38.716098386014,-60.181845184474));
#178752=CARTESIAN_POINT('Ctrl Pts',(52.8666240780138,-38.7177179462679,
-60.1675523808925));
#178753=CARTESIAN_POINT('Ctrl Pts',(52.8687834948402,-38.7195239308079,
-60.151633801452));
#178754=CARTESIAN_POINT('Ctrl Pts',(52.8707043558886,-38.7215170266781,
-60.1340908447902));
#178755=CARTESIAN_POINT('Ctrl Pts',(52.8725619015244,-38.7234444261319,
-60.1171261389815));
#178756=CARTESIAN_POINT('Ctrl Pts',(52.8741962415673,-38.7255468982893,
-60.0986416700889));
#178757=CARTESIAN_POINT('Ctrl Pts',(52.8753781352092,-38.7278219393132,
-60.0786644558131));
#178758=CARTESIAN_POINT('Ctrl Pts',(52.8765007676189,-38.7299829076919,
-60.0596889173987));
#178759=CARTESIAN_POINT('Ctrl Pts',(52.8772149880542,-38.7322996416788,
-60.0393660615517));
#178760=CARTESIAN_POINT('Ctrl Pts',(52.877289594721,-38.7347659988467,-60.017751191729));
#178761=CARTESIAN_POINT('Ctrl Pts',(52.877306074807,-38.7353107997344,-60.0129766195702));
#178762=CARTESIAN_POINT('Ctrl Pts',(52.8772912114132,-38.7358628828515,
-60.0081391524345));
#178763=CARTESIAN_POINT('Ctrl Pts',(52.877242281998,-38.7364221486262,-60.0032396521562));
#178764=CARTESIAN_POINT('Origin',(0.,-12.9675000200281,-61.64995));
#178765=CARTESIAN_POINT('Ctrl Pts',(52.4601060654288,-38.6442120952127,
-60.8635774537264));
#178766=CARTESIAN_POINT('Ctrl Pts',(52.4334660241228,-38.7417025272771,
-60.8486996970615));
#178767=CARTESIAN_POINT('Ctrl Pts',(52.4037146585348,-38.8501763362785,
-60.8330778025515));
#178768=CARTESIAN_POINT('Ctrl Pts',(52.3707417991334,-38.9697354911175,
-60.8172970455499));
#178769=CARTESIAN_POINT('Ctrl Pts',(52.3399184262437,-39.0815006361153,
-60.8025450293045));
#178770=CARTESIAN_POINT('Ctrl Pts',(52.3062790584938,-39.2029553301362,
-60.7876567855608));
#178771=CARTESIAN_POINT('Ctrl Pts',(52.2697265354297,-39.3341621392828,
-60.7731334311792));
#178772=CARTESIAN_POINT('Ctrl Pts',(52.2381281819637,-39.447585749612,-60.7605785089251));
#178773=CARTESIAN_POINT('Ctrl Pts',(52.2043536425209,-39.5682934199092,
-60.7482981832768));
#178774=CARTESIAN_POINT('Ctrl Pts',(52.1683406202579,-39.696297737098,-60.7366073261809));
#178775=CARTESIAN_POINT('Ctrl Pts',(52.1503341091263,-39.7602998956925,
-60.7307618976329));
#178776=CARTESIAN_POINT('Ctrl Pts',(52.1317679882644,-39.8261258047343,
-60.725063559064));
#178777=CARTESIAN_POINT('Ctrl Pts',(52.1126344252469,-39.8937749956445,
-60.7195489815034));
#178778=CARTESIAN_POINT('Ctrl Pts',(52.1030676437381,-39.9275995910996,
-60.7167916927231));
#178779=CARTESIAN_POINT('Ctrl Pts',(52.0933589949976,-39.9618800079525,
-60.7140803064361));
#178780=CARTESIAN_POINT('Ctrl Pts',(52.0835075034003,-39.9966160398341,
-60.71141916003));
#178781=CARTESIAN_POINT('Ctrl Pts',(52.0785817576016,-40.0139840557749,
-60.7100885868269));
#178782=CARTESIAN_POINT('Ctrl Pts',(52.0736203003513,-40.0314659766725,
-60.7087705705402));
#178783=CARTESIAN_POINT('Ctrl Pts',(52.0686230077915,-40.0490617750148,
-60.7074656347461));
#178784=CARTESIAN_POINT('Ctrl Pts',(52.0661243615116,-40.057859674186,-60.7068131668491));
#178785=CARTESIAN_POINT('Ctrl Pts',(52.063616756388,-40.066686042688,-60.7061639688745));
#178786=CARTESIAN_POINT('Ctrl Pts',(52.0611001768525,-40.0755408768569,
-60.7055181050371));
#178787=CARTESIAN_POINT('Ctrl Pts',(52.0598418870847,-40.0799682939413,
-60.7051951731184));
#178788=CARTESIAN_POINT('Ctrl Pts',(52.0585813537179,-40.0844028274231,
-60.7048730747222));
#178789=CARTESIAN_POINT('Ctrl Pts',(52.0573185748043,-40.0888444768176,
-60.7045518177966));
#178790=CARTESIAN_POINT('Ctrl Pts',(52.0566871853474,-40.0910653015148,
-60.7043911893338));
#178791=CARTESIAN_POINT('Ctrl Pts',(52.056055234504,-40.0932879051895,-60.7042307712378));
#178792=CARTESIAN_POINT('Ctrl Pts',(52.055422722031,-40.0955122877773,-60.7040705644974));
#178793=CARTESIAN_POINT('Ctrl Pts',(52.0552260978451,-40.0962037641259,
-60.704020762286));
#178794=CARTESIAN_POINT('Ctrl Pts',(52.0550308665119,-40.096890323743,-60.7039713460818));
#178795=CARTESIAN_POINT('Ctrl Pts',(52.0548288548571,-40.0976007072079,
-60.7039202499623));
#178796=CARTESIAN_POINT('Ctrl Pts',(52.0543810233055,-40.0991755278765,
-60.7038069770203));
#178797=CARTESIAN_POINT('Ctrl Pts',(52.0539081791715,-40.1008382038806,
-60.7036875622797));
#178798=CARTESIAN_POINT('Ctrl Pts',(52.0534391812185,-40.1024872442081,
-60.7035693190069));
#178799=CARTESIAN_POINT('Ctrl Pts',(52.0526842447014,-40.1051416710633,
-60.7033789852027));
#178800=CARTESIAN_POINT('Ctrl Pts',(52.0519392685549,-40.1077607713129,
-60.7031917274615));
#178801=CARTESIAN_POINT('Ctrl Pts',(52.051324697943,-40.1099212352922,-60.7030375666888));
#178802=CARTESIAN_POINT('Ctrl Pts',(52.0511862974551,-40.1104077689191,
-60.703002849887));
#178803=CARTESIAN_POINT('Ctrl Pts',(52.0510545107586,-40.1108710430068,
-60.7029698095072));
#178804=CARTESIAN_POINT('Ctrl Pts',(52.0509307139482,-40.111306222927,-60.702938785362));
#178805=CARTESIAN_POINT('Ctrl Pts',(52.0508514050645,-40.111585015519,-60.7029189101301));
#178806=CARTESIAN_POINT('Ctrl Pts',(52.0507732062307,-40.1118599029495,
-60.702899318697));
#178807=CARTESIAN_POINT('Ctrl Pts',(52.0506944905704,-40.1121366041439,
-60.7028796033477));
#178808=CARTESIAN_POINT('Ctrl Pts',(52.0057005426572,-40.2702992757785,
-60.6916102905366));
#178809=CARTESIAN_POINT('Ctrl Pts',(51.9602026002465,-40.4292425721673,
-60.6820510418657));
#178810=CARTESIAN_POINT('Ctrl Pts',(51.9143651206563,-40.588388068656,-60.6743068341458));
#178811=CARTESIAN_POINT('Ctrl Pts',(51.8690090901036,-40.7458619975366,
-60.666643966879));
#178812=CARTESIAN_POINT('Ctrl Pts',(51.8233206500267,-40.9035338860859,
-60.6607583289389));
#178813=CARTESIAN_POINT('Ctrl Pts',(51.7774673696501,-41.0608420505297,
-60.6567013858634));
#178814=CARTESIAN_POINT('Ctrl Pts',(51.7320461923718,-41.2166678053247,
-60.6526826738078));
#178815=CARTESIAN_POINT('Ctrl Pts',(51.6864633051644,-41.3721366436965,
-60.6504584078783));
#178816=CARTESIAN_POINT('Ctrl Pts',(51.6408891881858,-41.5267015602231,
-60.6500277777421));
#178817=CARTESIAN_POINT('Ctrl Pts',(51.6353998048932,-41.5453188396495,
-60.6499759085227));
#178818=CARTESIAN_POINT('Ctrl Pts',(51.6299105575627,-41.5639230037829,
-60.64995));
#178819=CARTESIAN_POINT('Ctrl Pts',(51.6244217512083,-41.5825130958571,
-60.64995));
#178820=CARTESIAN_POINT('Origin',(-83.2809572255632,20.2699999800001,-55.24995));
#178821=CARTESIAN_POINT('',(52.6819919725962,20.26999998,-59.64995));
#178822=CARTESIAN_POINT('Ctrl Pts',(51.1762622162812,20.26999998,-61.14995));
#178823=CARTESIAN_POINT('Ctrl Pts',(51.3733973069281,20.26999998,-61.149949999985));
#178824=CARTESIAN_POINT('Ctrl Pts',(51.5703838078145,20.26999998,-61.1109090094727));
#178825=CARTESIAN_POINT('Ctrl Pts',(51.9345762874696,20.26999998,-60.9606295880612));
#178826=CARTESIAN_POINT('Ctrl Pts',(52.1016035094776,20.26999998,-60.849450253352));
#178827=CARTESIAN_POINT('Ctrl Pts',(52.3803443657342,20.26999998,-60.5717700902076));
#178828=CARTESIAN_POINT('Ctrl Pts',(52.4919483874702,20.26999998,-60.4053784571342));
#178829=CARTESIAN_POINT('Ctrl Pts',(52.6428018517975,20.26999998,-60.0425718399611));
#178830=CARTESIAN_POINT('Ctrl Pts',(52.6819919725819,20.26999998,-59.8463349320562));
#178831=CARTESIAN_POINT('Ctrl Pts',(52.6819919725962,20.26999998,-59.64995));
#178832=CARTESIAN_POINT('',(52.6819919725962,20.26999998,-55.74995));
#178833=CARTESIAN_POINT('',(52.6819919725962,20.26999998,-55.24995));
#178834=CARTESIAN_POINT('',(-83.2809572255632,20.2699999800001,-55.74995));
#178835=CARTESIAN_POINT('Origin',(-83.2809572255632,19.7699999800001,-55.74995));
#178836=CARTESIAN_POINT('',(52.7694806361221,19.76999998,-55.24995));
#178837=CARTESIAN_POINT('Ctrl Pts',(52.6819919725962,20.26999998,-55.74995));
#178838=CARTESIAN_POINT('Ctrl Pts',(52.6819919725961,20.26999998,-55.7240510278288));
#178839=CARTESIAN_POINT('Ctrl Pts',(52.6823594164764,20.2679000286179,-55.6978536074428));
#178840=CARTESIAN_POINT('Ctrl Pts',(52.6831016080547,20.2636583843413,-55.6716786004096));
#178841=CARTESIAN_POINT('Ctrl Pts',(52.68385006805,20.2593809158985,-55.645282523965));
#178842=CARTESIAN_POINT('Ctrl Pts',(52.6849796405233,20.2529253796767,-55.6189093033866));
#178843=CARTESIAN_POINT('Ctrl Pts',(52.68649281381,20.2442775547729,-55.5929324719567));
#178844=CARTESIAN_POINT('Ctrl Pts',(52.6870630090585,20.2410188740165,-55.5831438601805));
#178845=CARTESIAN_POINT('Ctrl Pts',(52.6876876222624,20.2374491932217,-55.5734119766137));
#178846=CARTESIAN_POINT('Ctrl Pts',(52.6883666017139,20.2335688078992,-55.5637583894405));
#178847=CARTESIAN_POINT('Ctrl Pts',(52.6901453360981,20.223403294376,-55.5384687177195));
#178848=CARTESIAN_POINT('Ctrl Pts',(52.692298393295,20.2110985161876,-55.513697484835));
#178849=CARTESIAN_POINT('Ctrl Pts',(52.6948256939525,20.1966549268352,-55.4898442374517));
#178850=CARTESIAN_POINT('Ctrl Pts',(52.6968758230015,20.1849383857046,-55.4704946459309));
#178851=CARTESIAN_POINT('Ctrl Pts',(52.6991724966386,20.1718128358059,-55.4517483678047));
#178852=CARTESIAN_POINT('Ctrl Pts',(52.7017125466146,20.1572963837663,-55.4338552809257));
#178853=CARTESIAN_POINT('Ctrl Pts',(52.7030843359257,20.1494565719781,-55.4241918705375));
#178854=CARTESIAN_POINT('Ctrl Pts',(52.704527066812,20.1412113272328,-55.4147778017497));
#178855=CARTESIAN_POINT('Ctrl Pts',(52.7060394414411,20.132568066677,-55.4056571306897));
#178856=CARTESIAN_POINT('Ctrl Pts',(52.7063406725299,20.1308465231268,-55.40384049768));
#178857=CARTESIAN_POINT('Ctrl Pts',(52.7067076790132,20.1287490714839,-55.4016626948181));
#178858=CARTESIAN_POINT('Ctrl Pts',(52.7070309911037,20.1269013041925,-55.3997779182201));
#178859=CARTESIAN_POINT('Ctrl Pts',(52.7072632840316,20.1255737223088,-55.398423745929));
#178860=CARTESIAN_POINT('Ctrl Pts',(52.7074727865942,20.1243763723405,-55.3972196111485));
#178861=CARTESIAN_POINT('Ctrl Pts',(52.7076167822125,20.1235533694274,-55.3963966082408));
#178862=CARTESIAN_POINT('Ctrl Pts',(52.7093254930192,20.1137872807912,-55.386630519669));
#178863=CARTESIAN_POINT('Ctrl Pts',(52.7112328483416,20.1028864179031,-55.3765717208586));
#178864=CARTESIAN_POINT('Ctrl Pts',(52.7133612017114,20.0907228045942,-55.3664552895126));
#178865=CARTESIAN_POINT('Ctrl Pts',(52.7153992958998,20.0790750256366,-55.3567678756524));
#178866=CARTESIAN_POINT('Ctrl Pts',(52.7176401664676,20.0662686121309,-55.3470275906972));
#178867=CARTESIAN_POINT('Ctrl Pts',(52.7200994879389,20.0522137836287,-55.3374815440121));
#178868=CARTESIAN_POINT('Ctrl Pts',(52.7224186275942,20.0389600831638,-55.3284796238985));
#178869=CARTESIAN_POINT('Ctrl Pts',(52.7249321027178,20.0245957839257,-55.3196505221431));
#178870=CARTESIAN_POINT('Ctrl Pts',(52.7276480673089,20.0090741146608,-55.3112377697569));
#178871=CARTESIAN_POINT('Ctrl Pts',(52.7287440891335,20.0028103775254,-55.3078428211445));
#178872=CARTESIAN_POINT('Ctrl Pts',(52.729873021253,19.9963585347733,-55.3045160977521));
#178873=CARTESIAN_POINT('Ctrl Pts',(52.7310351059163,19.9897171905324,-55.3012753797748));
#178874=CARTESIAN_POINT('Ctrl Pts',(52.7337031803283,19.9744690754941,-55.2938348920163));
#178875=CARTESIAN_POINT('Ctrl Pts',(52.7365482385913,19.9582094931193,-55.2868407235455));
#178876=CARTESIAN_POINT('Ctrl Pts',(52.7395689469865,19.9409460656444,-55.2805340045048));
#178877=CARTESIAN_POINT('Ctrl Pts',(52.7425051677173,19.9241654873818,-55.2744036811611));
#178878=CARTESIAN_POINT('Ctrl Pts',(52.7456074052925,19.9064361185113,-55.2689228588975));
#178879=CARTESIAN_POINT('Ctrl Pts',(52.7488680753396,19.8878013039202,-55.2643427579722));
#178880=CARTESIAN_POINT('Ctrl Pts',(52.7520256709167,19.8697555626212,-55.2599074406248));
#178881=CARTESIAN_POINT('Ctrl Pts',(52.7553318801676,19.8508604902903,-55.2563167977791));
#178882=CARTESIAN_POINT('Ctrl Pts',(52.7587730939723,19.8311938634032,-55.2538274761936));
#178883=CARTESIAN_POINT('Ctrl Pts',(52.7622143077771,19.8115272365161,-55.2513381546082));
#178884=CARTESIAN_POINT('Ctrl Pts',(52.7657906008408,19.7910886281323,-55.24995));
#178885=CARTESIAN_POINT('Ctrl Pts',(52.7694806361221,19.76999998,-55.24995));
#178886=CARTESIAN_POINT('',(60.,19.76999998,-55.24995));
#178887=CARTESIAN_POINT('Origin',(60.,28.41999998,-55.24995));
#178888=CARTESIAN_POINT('',(52.8132249678851,19.26999998,-55.24995));
#178889=CARTESIAN_POINT('',(52.0733761857257,27.7265102562164,-55.24995));
#178890=CARTESIAN_POINT('',(60.,19.26999998,-55.24995));
#178891=CARTESIAN_POINT('Origin',(60.,19.26999998,-55.74995));
#178892=CARTESIAN_POINT('',(52.900713631411,18.76999998,-55.74995));
#178893=CARTESIAN_POINT('Ctrl Pts',(52.8132249678851,19.26999998,-55.24995));
#178894=CARTESIAN_POINT('Ctrl Pts',(52.8170018622036,19.2484149301986,-55.24995));
#178895=CARTESIAN_POINT('Ctrl Pts',(52.820628852166,19.2274879325962,-55.2513479743294));
#178896=CARTESIAN_POINT('Ctrl Pts',(52.8241059377721,19.2073682602054,-55.2538882420751));
#178897=CARTESIAN_POINT('Ctrl Pts',(52.8275775058576,19.1872805141808,-55.2564244788646));
#178898=CARTESIAN_POINT('Ctrl Pts',(52.8308996449529,19.167996955483,-55.2600986723954));
#178899=CARTESIAN_POINT('Ctrl Pts',(52.834072355058,19.1496086400557,-55.2646604727419));
#178900=CARTESIAN_POINT('Ctrl Pts',(52.8373840007711,19.1304150850388,-55.2694220381106));
#178901=CARTESIAN_POINT('Ctrl Pts',(52.8405328437045,19.1121965820858,-55.2751499570336));
#178902=CARTESIAN_POINT('Ctrl Pts',(52.8435188838583,19.0950003125834,-55.2815750258563));
#178903=CARTESIAN_POINT('Ctrl Pts',(52.8462680137064,19.0791683828935,-55.2874903342807));
#178904=CARTESIAN_POINT('Ctrl Pts',(52.8488791492904,19.0642018444273,-55.2939965088991));
#178905=CARTESIAN_POINT('Ctrl Pts',(52.8513522906103,19.050102597673,-55.3009008476283));
#178906=CARTESIAN_POINT('Ctrl Pts',(52.854233915202,19.0336746095732,-55.3089455606869));
#178907=CARTESIAN_POINT('Ctrl Pts',(52.8569281965776,19.0184242891668,-55.3175297931872));
#178908=CARTESIAN_POINT('Ctrl Pts',(52.8594351347371,19.0043108258162,-55.3263826814435));
#178909=CARTESIAN_POINT('Ctrl Pts',(52.8614131894553,18.9931748499785,-55.3333678945884));
#178910=CARTESIAN_POINT('Ctrl Pts',(52.8632746095929,18.9827455690346,-55.3405210924567));
#178911=CARTESIAN_POINT('Ctrl Pts',(52.8650193951501,18.972987953445,-55.347726360613));
#178912=CARTESIAN_POINT('Ctrl Pts',(52.8669974371943,18.9619258640044,-55.3558948849884));
#178913=CARTESIAN_POINT('Ctrl Pts',(52.8688255748824,18.9517269109974,-55.36412990652));
#178914=CARTESIAN_POINT('Ctrl Pts',(52.8705038082142,18.9423264617821,-55.3722860416207));
#178915=CARTESIAN_POINT('Ctrl Pts',(52.8713429248801,18.9376262371744,-55.3763641091711));
#178916=CARTESIAN_POINT('Ctrl Pts',(52.872144565457,18.9331254533317,-55.3804228422457));
#178917=CARTESIAN_POINT('Ctrl Pts',(52.8729087299449,18.9288151725488,-55.3844463376867));
#178918=CARTESIAN_POINT('Ctrl Pts',(52.8732908121888,18.9266600321573,-55.3864580854071));
#178919=CARTESIAN_POINT('Ctrl Pts',(52.8736635254104,18.9245525258353,-55.3884610324748));
#178920=CARTESIAN_POINT('Ctrl Pts',(52.8740268696098,18.922491480226,-55.3904533482982));
#178921=CARTESIAN_POINT('Ctrl Pts',(52.8742524174911,18.921212074992,-55.3916900891451));
#178922=CARTESIAN_POINT('Ctrl Pts',(52.8744014321368,18.920371830749,-55.3925105847798));
#178923=CARTESIAN_POINT('Ctrl Pts',(52.8746097155931,18.9191841523716,-55.3936800811387));
#178924=CARTESIAN_POINT('Ctrl Pts',(52.874736964376,18.918458551641,-55.3943945737394));
#178925=CARTESIAN_POINT('Ctrl Pts',(52.8748863351359,18.9176035577891,-55.3952396410243));
#178926=CARTESIAN_POINT('Ctrl Pts',(52.8750887951412,18.9164465894067,-55.3963966094067));
#178927=CARTESIAN_POINT('Ctrl Pts',(52.8782312711263,18.8984887445873,-55.4143544542262));
#178928=CARTESIAN_POINT('Ctrl Pts',(52.8810847163286,18.8820748238315,-55.4335093827848));
#178929=CARTESIAN_POINT('Ctrl Pts',(52.883649130748,18.8673083263412,-55.4535728212673));
#178930=CARTESIAN_POINT('Ctrl Pts',(52.8862497990868,18.8523330703113,-55.4739199027816));
#178931=CARTESIAN_POINT('Ctrl Pts',(52.8885532066409,18.8390520083641,-55.4952007603898));
#178932=CARTESIAN_POINT('Ctrl Pts',(52.8905593534104,18.8275195753317,-55.5171172456793));
#178933=CARTESIAN_POINT('Ctrl Pts',(52.8926095204872,18.8157340894056,-55.539514638164));
#178934=CARTESIAN_POINT('Ctrl Pts',(52.8943492382359,18.8057746306867,-55.5625752640842));
#178935=CARTESIAN_POINT('Ctrl Pts',(52.8957785066566,18.7976461596386,-55.5859930898376));
#178936=CARTESIAN_POINT('Ctrl Pts',(52.8972258449116,18.7894149226424,-55.6097069805032));
#178937=CARTESIAN_POINT('Ctrl Pts',(52.8983548343716,18.783060901236,-55.6337866416403));
#178938=CARTESIAN_POINT('Ctrl Pts',(52.8991654750368,18.778539638464,-55.6579351495829));
#178939=CARTESIAN_POINT('Ctrl Pts',(52.8999913688049,18.7739333031199,-55.682538038477));
#178940=CARTESIAN_POINT('Ctrl Pts',(52.9004868208969,18.7712289400598,-55.7072119145565));
#178941=CARTESIAN_POINT('Ctrl Pts',(52.9006518313128,18.7703341785775,-55.7316719560988));
#178942=CARTESIAN_POINT('Ctrl Pts',(52.9006930313783,18.7701107730947,-55.7377791785246));
#178943=CARTESIAN_POINT('Ctrl Pts',(52.900713631411,18.76999998,-55.7438732289921));
#178944=CARTESIAN_POINT('Ctrl Pts',(52.900713631411,18.76999998,-55.74995));
#178945=CARTESIAN_POINT('',(-83.2809572255632,18.7699999800001,-55.74995));
#178946=CARTESIAN_POINT('Origin',(-83.2809572255632,18.7699999800001,-55.24995));
#178947=CARTESIAN_POINT('',(52.900713631411,18.76999998,-59.64995));
#178948=CARTESIAN_POINT('',(52.900713631411,18.76999998,-55.24995));
#178949=CARTESIAN_POINT('Ctrl Pts',(52.900713631411,18.76999998,-59.64995));
#178950=CARTESIAN_POINT('Ctrl Pts',(52.9007136313967,18.76999998,-59.8463349320561));
#178951=CARTESIAN_POINT('Ctrl Pts',(52.8615235106123,18.76999998,-60.0425718399612));
#178952=CARTESIAN_POINT('Ctrl Pts',(52.710670046285,18.76999998,-60.4053784571341));
#178953=CARTESIAN_POINT('Ctrl Pts',(52.5990660245491,18.76999998,-60.5717700902076));
#178954=CARTESIAN_POINT('Ctrl Pts',(52.3203251682923,18.76999998,-60.8494502533521));
#178955=CARTESIAN_POINT('Ctrl Pts',(52.1532979462845,18.76999998,-60.9606295880612));
#178956=CARTESIAN_POINT('Ctrl Pts',(51.7891054666292,18.76999998,-61.1109090094727));
#178957=CARTESIAN_POINT('Ctrl Pts',(51.592118965743,18.76999998,-61.149949999985));
#178958=CARTESIAN_POINT('Ctrl Pts',(51.394983875096,18.76999998,-61.14995));
#178959=CARTESIAN_POINT('Ctrl Pts',(52.900713631411,18.76999998,-59.64995));
#178960=CARTESIAN_POINT('Ctrl Pts',(52.3550593808763,18.76999998,-59.64995));
#178961=CARTESIAN_POINT('Ctrl Pts',(52.4026162823651,18.2264221086262,-59.64995));
#178962=CARTESIAN_POINT('Ctrl Pts',(52.9007136313967,18.76999998,-59.8463349320561));
#178963=CARTESIAN_POINT('Ctrl Pts',(52.3550593808723,18.76999998,-59.7746029379313));
#178964=CARTESIAN_POINT('Ctrl Pts',(52.402616282365,18.2264221086281,-59.7808732880371));
#178965=CARTESIAN_POINT('Ctrl Pts',(52.8615235106123,18.76999998,-60.0425718399612));
#178966=CARTESIAN_POINT('Ctrl Pts',(52.3316386425403,18.76999998,-59.8989712332646));
#178967=CARTESIAN_POINT('Ctrl Pts',(52.3763903041667,18.2275563241362,-59.9116978933078));
#178968=CARTESIAN_POINT('Ctrl Pts',(52.710670046285,18.76999998,-60.4053784571341));
#178969=CARTESIAN_POINT('Ctrl Pts',(52.239810099313,18.76999998,-60.1322291512602));
#178970=CARTESIAN_POINT('Ctrl Pts',(52.2754393607673,18.2319222289985,-60.1535689714224));
#178971=CARTESIAN_POINT('Ctrl Pts',(52.5990660245491,18.76999998,-60.5717700902076));
#178972=CARTESIAN_POINT('Ctrl Pts',(52.1717434473124,18.7699999799997,-60.2406767152624));
#178973=CARTESIAN_POINT('Ctrl Pts',(52.2007540936325,18.2351522014976,-60.2644967268053));
#178974=CARTESIAN_POINT('Ctrl Pts',(52.3203251682923,18.76999998,-60.8494502533521));
#178975=CARTESIAN_POINT('Ctrl Pts',(51.9977165994394,18.7699999800003,-60.4261994932772));
#178976=CARTESIAN_POINT('Ctrl Pts',(52.0142210728062,18.2432193417862,-60.4496168355678));
#178977=CARTESIAN_POINT('Ctrl Pts',(52.1532979462845,18.76999998,-60.9606295880612));
#178978=CARTESIAN_POINT('Ctrl Pts',(51.8922860151588,18.7699999800003,-60.5031527166051));
#178979=CARTESIAN_POINT('Ctrl Pts',(51.9024466716657,18.2480533372399,-60.5237363920407));
#178980=CARTESIAN_POINT('Ctrl Pts',(51.7891054666292,18.76999998,-61.1109090094727));
#178981=CARTESIAN_POINT('Ctrl Pts',(51.657019042446,18.7699999799997,-60.6120353079393));
#178982=CARTESIAN_POINT('Ctrl Pts',(51.6587295348784,18.2585935639752,-60.6239226729819));
#178983=CARTESIAN_POINT('Ctrl Pts',(51.592118965743,18.76999998,-61.149949999985));
#178984=CARTESIAN_POINT('Ctrl Pts',(51.5277022966008,18.7699999800007,-60.6442102195358));
#178985=CARTESIAN_POINT('Ctrl Pts',(51.5269064230252,18.264294621793,-60.64995));
#178986=CARTESIAN_POINT('Ctrl Pts',(51.394983875096,18.76999998,-61.14995));
#178987=CARTESIAN_POINT('Ctrl Pts',(51.394983875096,18.76999998,-60.64995));
#178988=CARTESIAN_POINT('Ctrl Pts',(51.394983875096,18.26999998,-60.64995));
#178989=CARTESIAN_POINT('',(52.4026162823651,18.2264221086262,-59.64995));
#178990=CARTESIAN_POINT('Origin',(52.900713631411,18.26999998,-59.64995));
#178991=CARTESIAN_POINT('Ctrl Pts',(51.394983875096,18.26999998,-60.64995));
#178992=CARTESIAN_POINT('Ctrl Pts',(51.4237727051561,18.2687549268196,-60.64995));
#178993=CARTESIAN_POINT('Ctrl Pts',(51.451335267364,18.2675736205104,-60.6487272519605));
#178994=CARTESIAN_POINT('Ctrl Pts',(51.4775920461836,18.2664491043645,-60.6465836174979));
#178995=CARTESIAN_POINT('Ctrl Pts',(51.5050161835672,18.265274592994,-60.6443446785022));
#178996=CARTESIAN_POINT('Ctrl Pts',(51.5310162920264,18.2641620725893,-60.6411017332696));
#178997=CARTESIAN_POINT('Ctrl Pts',(51.5555514746609,18.2631079651353,-60.6371711976494));
#178998=CARTESIAN_POINT('Ctrl Pts',(51.5807005119033,18.2620274845857,-60.633142322537));
#178999=CARTESIAN_POINT('Ctrl Pts',(51.6043110984276,18.2610084372763,-60.6283914211907));
#179000=CARTESIAN_POINT('Ctrl Pts',(51.6263811670969,18.2600506423559,-60.6232233711577));
#179001=CARTESIAN_POINT('Ctrl Pts',(51.6491770892134,18.2590613469108,-60.6178853512442));
#179002=CARTESIAN_POINT('Ctrl Pts',(51.6703302230382,18.2581374627052,-60.612102639129));
#179003=CARTESIAN_POINT('Ctrl Pts',(51.6898715157798,18.2572816972691,-60.6061674758653));
#179004=CARTESIAN_POINT('Ctrl Pts',(51.6928070816617,18.2571531409934,-60.6052758735025));
#179005=CARTESIAN_POINT('Ctrl Pts',(51.6957063201809,18.2570261261061,-60.6043807476975));
#179006=CARTESIAN_POINT('Ctrl Pts',(51.6985693825471,18.2569006658364,-60.6034830010222));
#179007=CARTESIAN_POINT('Ctrl Pts',(51.7111710647439,18.256348456263,-60.5995315962508));
#179008=CARTESIAN_POINT('Ctrl Pts',(51.7230716758463,18.2558263438253,-60.5955300976952));
#179009=CARTESIAN_POINT('Ctrl Pts',(51.7342861383916,18.2553356340763,-60.5915501614051));
#179010=CARTESIAN_POINT('Ctrl Pts',(51.7398933696642,18.2550902792017,-60.58956019326));
#179011=CARTESIAN_POINT('Ctrl Pts',(51.7453290261346,18.2548527717042,-60.5875755119223));
#179012=CARTESIAN_POINT('Ctrl Pts',(51.7505952924679,18.2546233027172,-60.5856042390434));
#179013=CARTESIAN_POINT('Ctrl Pts',(51.7532284256346,18.2545085682237,-60.584618602604));
#179014=CARTESIAN_POINT('Ctrl Pts',(51.7558192089008,18.2543958431508,-60.5836363114118));
#179015=CARTESIAN_POINT('Ctrl Pts',(51.7583679101829,18.2542851509382,-60.5826583363884));
#179016=CARTESIAN_POINT('Ctrl Pts',(51.7601161348254,18.2542092240906,-60.5819875162935));
#179017=CARTESIAN_POINT('Ctrl Pts',(51.7609326573293,18.2541734759912,-60.5816721106887));
#179018=CARTESIAN_POINT('Ctrl Pts',(51.7626946418676,18.2540972539743,-60.5809867219959));
#179019=CARTESIAN_POINT('Ctrl Pts',(51.7635014188846,18.2540623534573,-60.5806728964015));
#179020=CARTESIAN_POINT('Ctrl Pts',(51.7645062913134,18.2540189565485,-60.5802811765949));
#179021=CARTESIAN_POINT('Ctrl Pts',(51.7658880333948,18.2539591960934,-60.5797383010624));
#179022=CARTESIAN_POINT('Ctrl Pts',(51.7994271157594,18.2525086281088,-60.5665610609375));
#179023=CARTESIAN_POINT('Ctrl Pts',(51.8314973303886,18.2511292826187,-60.5518925917424));
#179024=CARTESIAN_POINT('Ctrl Pts',(51.8620286680791,18.2498150346114,-60.5360425708523));
#179025=CARTESIAN_POINT('Ctrl Pts',(51.8931419883397,18.2484757346577,-60.5198904198693));
#179026=CARTESIAN_POINT('Ctrl Pts',(51.9226575828774,18.2472040706567,-60.5025117129383));
#179027=CARTESIAN_POINT('Ctrl Pts',(51.9505524288216,18.2459980283681,-60.4842157548927));
#179028=CARTESIAN_POINT('Ctrl Pts',(51.9792094540704,18.2447590330217,-60.4654198908571));
#179029=CARTESIAN_POINT('Ctrl Pts',(52.0061563497031,18.243589329148,-60.4456563996028));
#179030=CARTESIAN_POINT('Ctrl Pts',(52.0314156457665,18.2424908878707,-60.4252343356306));
#179031=CARTESIAN_POINT('Ctrl Pts',(52.0333988373379,18.2424046455829,-60.4236309312824));
#179032=CARTESIAN_POINT('Ctrl Pts',(52.0353716476986,18.2423188444835,-60.4220234523116));
#179033=CARTESIAN_POINT('Ctrl Pts',(52.0373340985572,18.242233486472,-60.4204120405363));
#179034=CARTESIAN_POINT('Ctrl Pts',(52.0498612917415,18.2416886084713,-60.4101256853292));
#179035=CARTESIAN_POINT('Ctrl Pts',(52.0619661663755,18.2411617692931,-60.3996792357689));
#179036=CARTESIAN_POINT('Ctrl Pts',(52.0736557186227,18.2406535810223,-60.3891084430411));
#179037=CARTESIAN_POINT('Ctrl Pts',(52.0791075857478,18.240416568101,-60.3841783519528));
#179038=CARTESIAN_POINT('Ctrl Pts',(52.084147474518,18.2401960942946,-60.3795181564341));
#179039=CARTESIAN_POINT('Ctrl Pts',(52.0892317682909,18.2399752512423,-60.3747215662672));
#179040=CARTESIAN_POINT('Ctrl Pts',(52.0941767052513,18.2397604613383,-60.370056447165));
#179041=CARTESIAN_POINT('Ctrl Pts',(52.0991637980934,18.2395453354279,-60.3652622208462));
#179042=CARTESIAN_POINT('Ctrl Pts',(52.1045799184888,18.2393114302983,-60.359930701158));
#179043=CARTESIAN_POINT('Ctrl Pts',(52.1055352201106,18.2392701738392,-60.3589903215075));
#179044=CARTESIAN_POINT('Ctrl Pts',(52.1065037763543,18.2392283250547,-60.358033135595));
#179045=CARTESIAN_POINT('Ctrl Pts',(52.1074875832193,18.2391857716419,-60.3570567811866));
#179046=CARTESIAN_POINT('Ctrl Pts',(52.1379181186866,18.2378695345012,-60.3268567607196));
#179047=CARTESIAN_POINT('Ctrl Pts',(52.1661486617633,18.236668507618,-60.2949641541397));
#179048=CARTESIAN_POINT('Ctrl Pts',(52.1920517229949,18.2355715371104,-60.2617220237118));
#179049=CARTESIAN_POINT('Ctrl Pts',(52.2182622702554,18.2344615448559,-60.2280852877741));
#179050=CARTESIAN_POINT('Ctrl Pts',(52.2420898530018,18.2334581030591,-60.193067311089));
#179051=CARTESIAN_POINT('Ctrl Pts',(52.2634559174668,18.2325543391559,-60.1570220983486));
#179052=CARTESIAN_POINT('Ctrl Pts',(52.2850807034988,18.2316396315802,-60.1205404143085));
#179053=CARTESIAN_POINT('Ctrl Pts',(52.3041841730781,18.2308270458906,-60.0830069552407));
#179054=CARTESIAN_POINT('Ctrl Pts',(52.3207372784833,18.2301140407409,-60.0447796547096));
#179055=CARTESIAN_POINT('Ctrl Pts',(52.3375983740247,18.2293877692857,-60.0058410899653));
#179056=CARTESIAN_POINT('Ctrl Pts',(52.351813515365,18.2287648357927,-59.9661831062492));
#179057=CARTESIAN_POINT('Ctrl Pts',(52.3634032636446,18.2282470391287,-59.9261671553576));
#179058=CARTESIAN_POINT('Ctrl Pts',(52.3751177180226,18.2277236709544,-59.8857206314297));
#179059=CARTESIAN_POINT('Ctrl Pts',(52.3841503063993,18.2273077431756,-59.8449088095266));
#179060=CARTESIAN_POINT('Ctrl Pts',(52.3905700243695,18.2270052921247,-59.8040810753798));
#179061=CARTESIAN_POINT('Ctrl Pts',(52.3970915619048,18.2266980440664,-59.7626057953194));
#179062=CARTESIAN_POINT('Ctrl Pts',(52.4009170425841,18.2265079317809,-59.7211144793536));
#179063=CARTESIAN_POINT('Ctrl Pts',(52.4021626662287,18.2264451214354,-59.679942768914));
#179064=CARTESIAN_POINT('Ctrl Pts',(52.4024657503462,18.226429838474,-59.669924902299));
#179065=CARTESIAN_POINT('Ctrl Pts',(52.4026162823651,18.2264221086262,-59.6599258027971));
#179066=CARTESIAN_POINT('Ctrl Pts',(52.4026162823651,18.2264221086262,-59.64995));
#179067=CARTESIAN_POINT('Origin',(0.,-12.9675000200281,-60.64995));
#179068=CARTESIAN_POINT('',(51.6244217512084,15.6475130558006,-60.64995));
#179069=CARTESIAN_POINT('Origin',(0.,-12.9675000200281,-60.64995));
#179070=CARTESIAN_POINT('',(53.7167487055517,-8.26789346682159,-60.64995));
#179071=CARTESIAN_POINT('Origin',(0.,-12.9675000200281,-61.64995));
#179072=CARTESIAN_POINT('',(52.4885489491165,12.6049688303995,-60.8798615124595));
#179073=CARTESIAN_POINT('Ctrl Pts',(51.6244217512084,15.6475130558006,-60.64995));
#179074=CARTESIAN_POINT('Ctrl Pts',(51.6551646996741,15.5433894621099,-60.64995));
#179075=CARTESIAN_POINT('Ctrl Pts',(51.6891856571931,15.42785477597,-60.6507769894556));
#179076=CARTESIAN_POINT('Ctrl Pts',(51.7449269585569,15.2374765632288,-60.6540853355037));
#179077=CARTESIAN_POINT('Ctrl Pts',(51.7739758200045,15.1380192813913,-60.6562586768657));
#179078=CARTESIAN_POINT('Ctrl Pts',(51.809894806679,15.0145363819814,-60.6599052372727));
#179079=CARTESIAN_POINT('Ctrl Pts',(51.8283585992563,14.950936056674,-60.6620329872155));
#179080=CARTESIAN_POINT('Ctrl Pts',(51.8363794579957,14.9232808461768,-60.6630130104025));
#179081=CARTESIAN_POINT('Ctrl Pts',(51.8417506290901,14.9047556582866,-60.6636818234472));
#179082=CARTESIAN_POINT('Ctrl Pts',(51.8448598242051,14.8940282232909,-60.6640771410432));
#179083=CARTESIAN_POINT('Ctrl Pts',(51.883923482042,14.7592131237825,-60.6691236656757));
#179084=CARTESIAN_POINT('Ctrl Pts',(51.9387151074887,14.5688372951455,-60.6779958996905));
#179085=CARTESIAN_POINT('Ctrl Pts',(52.0022407624029,14.3467628952478,-60.6913501116407));
#179086=CARTESIAN_POINT('Ctrl Pts',(52.0339323134534,14.2357469132923,-60.6987687241444));
#179087=CARTESIAN_POINT('Ctrl Pts',(52.0497637801078,14.1802458880588,-60.7026621789418));
#179088=CARTESIAN_POINT('Ctrl Pts',(52.0565460034622,14.1564614021569,-60.7043701243749));
#179089=CARTESIAN_POINT('Ctrl Pts',(52.0610669293512,14.1406054681221,-60.7055174770928));
#179090=CARTESIAN_POINT('Ctrl Pts',(52.062782551509,14.134587959597,-60.7059551790868));
#179091=CARTESIAN_POINT('Ctrl Pts',(52.2450744027298,13.4951289417155,-60.752932396218));
#179092=CARTESIAN_POINT('Ctrl Pts',(52.3839308970543,12.9889668299485,-60.818448001159));
#179093=CARTESIAN_POINT('Ctrl Pts',(52.4885489491165,12.6049688303995,-60.8798615124595));
#179094=CARTESIAN_POINT('Ctrl Pts',(52.4885489491165,12.6049688303995,-60.8798615124595));
#179095=CARTESIAN_POINT('Ctrl Pts',(52.5003074888079,12.5618093982546,-60.8867640803813));
#179096=CARTESIAN_POINT('Ctrl Pts',(52.5123202735365,12.518720787882,-60.8936385283445));
#179097=CARTESIAN_POINT('Ctrl Pts',(52.5245819708709,12.4756972986243,-60.9004583201737));
#179098=CARTESIAN_POINT('Ctrl Pts',(52.813519414917,12.5211707144541,-60.5028360925953));
#179099=CARTESIAN_POINT('Ctrl Pts',(52.7011006011713,12.5792267001133,-60.7309116189004));
#179100=CARTESIAN_POINT('Ctrl Pts',(52.4885489491165,12.6049688303995,-60.8798615124595));
#179101=CARTESIAN_POINT('Ctrl Pts',(52.8184252363688,12.4804454574502,-60.5118893693287));
#179102=CARTESIAN_POINT('Ctrl Pts',(52.7083699494147,12.5371106789483,-60.7374192211269));
#179103=CARTESIAN_POINT('Ctrl Pts',(52.5003487858574,12.5616578171005,-60.8867883233088));
#179104=CARTESIAN_POINT('Ctrl Pts',(52.823766550455,12.4396518133592,-60.5210243207318));
#179105=CARTESIAN_POINT('Ctrl Pts',(52.7160214096145,12.4948853110753,-60.7440415583411));
#179106=CARTESIAN_POINT('Ctrl Pts',(52.5124335500125,12.5183120391401,-60.8937038544239));
#179107=CARTESIAN_POINT('Ctrl Pts',(52.8295491865184,12.3987982841401,-60.5301925771521));
#179108=CARTESIAN_POINT('Ctrl Pts',(52.7240626356492,12.4525613978151,-60.750736804912));
#179109=CARTESIAN_POINT('Ctrl Pts',(52.5248032674767,12.4749209213966,-60.9005813814078));
#179110=CARTESIAN_POINT('Origin',(51.9150548124647,12.3255619647296,-60.1097730249189));
#179111=CARTESIAN_POINT('Ctrl Pts',(53.2607580814926,12.11999998,-60.7033966151602));
#179112=CARTESIAN_POINT('Ctrl Pts',(52.8857929788877,12.11999998,-60.5379900686009));
#179113=CARTESIAN_POINT('Ctrl Pts',(52.81219032515,12.5218539749099,-60.5055220850798));
#179114=CARTESIAN_POINT('Ctrl Pts',(53.3498368505456,12.11999998,-60.5014612122216));
#179115=CARTESIAN_POINT('Ctrl Pts',(52.9388615253298,12.1199999799981,-60.3810288628603));
#179116=CARTESIAN_POINT('Ctrl Pts',(52.8700875991767,12.5389561241882,-60.3657903170377));
#179117=CARTESIAN_POINT('Ctrl Pts',(53.3950245780495,12.11999998,-60.2853240337268));
#179118=CARTESIAN_POINT('Ctrl Pts',(52.9540808994585,12.1199999800015,-60.2191862528169));
#179119=CARTESIAN_POINT('Ctrl Pts',(52.8985874779024,12.5574454029709,-60.2163866339305));
#179120=CARTESIAN_POINT('Ctrl Pts',(53.3950245803325,12.11999998,-60.0627241236311));
#179121=CARTESIAN_POINT('Ctrl Pts',(52.9368589933238,12.11999998,-60.0627241236309));
#179122=CARTESIAN_POINT('Ctrl Pts',(52.8969272312866,12.5764221086261,-60.0627241236309));
#179123=CARTESIAN_POINT('',(52.8969272306107,12.5764221085651,-60.0627241236309));
#179124=CARTESIAN_POINT('',(53.3950245803324,12.11999998,-60.0627241236309));
#179125=CARTESIAN_POINT('Origin',(53.3950245803325,12.61999998,-60.0627241236309));
#179126=CARTESIAN_POINT('Origin',(50.5588767643988,12.11999998,-59.7245163412853));
#179127=CARTESIAN_POINT('Ctrl Pts',(52.8969272312868,12.5764221086243,-60.0627241236309));
#179128=CARTESIAN_POINT('Ctrl Pts',(52.8972093867344,12.5731970571004,-60.0888387457683));
#179129=CARTESIAN_POINT('Ctrl Pts',(52.8966025741109,12.5702371653934,-60.1127979091318));
#179130=CARTESIAN_POINT('Ctrl Pts',(52.895492143609,12.5675483472939,-60.1345630157725));
#179131=CARTESIAN_POINT('Ctrl Pts',(52.8952383309491,12.5669337603633,-60.139537896776));
#179132=CARTESIAN_POINT('Ctrl Pts',(52.8949580002003,12.566333324942,-60.1443982053448));
#179133=CARTESIAN_POINT('Ctrl Pts',(52.8946553754963,12.5657470947143,-60.1491435666974));
#179134=CARTESIAN_POINT('Ctrl Pts',(52.8935370825506,12.5635807906436,-60.1666791612968));
#179135=CARTESIAN_POINT('Ctrl Pts',(52.8921164516363,12.5616084482314,-60.1826454242178));
#179136=CARTESIAN_POINT('Ctrl Pts',(52.8905899490122,12.559833631543,-60.1970148166353));
#179137=CARTESIAN_POINT('Ctrl Pts',(52.8896508802967,12.5587418058223,-60.2058545308072));
#179138=CARTESIAN_POINT('Ctrl Pts',(52.8886715980987,12.5577250679358,-60.2140871499417));
#179139=CARTESIAN_POINT('Ctrl Pts',(52.8876909467741,12.5567829255677,-60.2217165962902));
#179140=CARTESIAN_POINT('Ctrl Pts',(52.8859652650759,12.5551250092409,-60.2351423630245));
#179141=CARTESIAN_POINT('Ctrl Pts',(52.8842371940579,12.5536970103207,-60.2467090858731));
#179142=CARTESIAN_POINT('Ctrl Pts',(52.8826767053327,12.5524961277858,-60.2564379859943));
#179143=CARTESIAN_POINT('Ctrl Pts',(52.8811308498546,12.5513065063453,-60.2660756548253));
#179144=CARTESIAN_POINT('Ctrl Pts',(52.879749595859,12.5503398173612,-60.2739092846511));
#179145=CARTESIAN_POINT('Ctrl Pts',(52.878645753002,12.5495929425003,-60.2799623795994));
#179146=CARTESIAN_POINT('Ctrl Pts',(52.8784091261802,12.5494328376235,-60.2812599597849));
#179147=CARTESIAN_POINT('Ctrl Pts',(52.8781850597772,12.5492828377151,-60.2824756887368));
#179148=CARTESIAN_POINT('Ctrl Pts',(52.8779743558538,12.54914291719,-60.2836097586939));
#179149=CARTESIAN_POINT('Ctrl Pts',(52.8778077082517,12.5490322528056,-60.2845067046824));
#179150=CARTESIAN_POINT('Ctrl Pts',(52.8776494172265,12.5489278934755,-60.2853525696634));
#179151=CARTESIAN_POINT('Ctrl Pts',(52.8774998415707,12.5488297619182,-60.2861474384989));
#179152=CARTESIAN_POINT('Ctrl Pts',(52.8774624476567,12.5488052290289,-60.2863461557077));
#179153=CARTESIAN_POINT('Ctrl Pts',(52.8774483929893,12.54879592331,-60.2864207378837));
#179154=CARTESIAN_POINT('Ctrl Pts',(52.8774406506828,12.5487907192805,-60.286461911159));
#179155=CARTESIAN_POINT('Ctrl Pts',(52.8774329083763,12.5487855152511,-60.2865030844342));
#179156=CARTESIAN_POINT('Ctrl Pts',(52.8774314674585,12.5487844132509,-60.2865108462554));
#179157=CARTESIAN_POINT('Ctrl Pts',(52.8774192125423,12.548776290571,-60.2865759021724));
#179158=CARTESIAN_POINT('Ctrl Pts',(52.8773947027099,12.5487600452112,-60.2867060140063));
#179159=CARTESIAN_POINT('Ctrl Pts',(52.8773276045743,12.5487158014682,-60.2870654427123));
#179160=CARTESIAN_POINT('Ctrl Pts',(52.8770776120991,12.5485537277925,-60.2883791407993));
#179161=CARTESIAN_POINT('Ctrl Pts',(52.870030916608,12.5439852549261,-60.3254091769202));
#179162=CARTESIAN_POINT('Ctrl Pts',(52.8614724626347,12.5397015659191,-60.3601737018512));
#179163=CARTESIAN_POINT('Ctrl Pts',(52.8519633454955,12.5357049347099,-60.3926622296679));
#179164=CARTESIAN_POINT('Ctrl Pts',(52.8423230082821,12.5316531524035,-60.4255990795497));
#179165=CARTESIAN_POINT('Ctrl Pts',(52.8317061291368,12.5278962903145,-60.4561974030475));
#179166=CARTESIAN_POINT('Ctrl Pts',(52.8206579435906,12.5244306778137,-60.4844812536859));
#179167=CARTESIAN_POINT('Ctrl Pts',(52.8178604768424,12.5235531639729,-60.4916428940603));
#179168=CARTESIAN_POINT('Ctrl Pts',(52.8150351397417,12.5226942982607,-60.4986562874559));
#179169=CARTESIAN_POINT('Ctrl Pts',(52.81219032515,12.5218539749099,-60.5055220850798));
#179170=CARTESIAN_POINT('Origin',(-83.2809572255632,12.1199999800001,-55.24995));
#179171=CARTESIAN_POINT('',(53.3950245803324,12.11999998,-55.74995));
#179172=CARTESIAN_POINT('',(53.3950245803324,12.11999998,-55.24995));
#179173=CARTESIAN_POINT('',(-83.2809572255632,12.1199999800001,-55.74995));
#179174=CARTESIAN_POINT('Origin',(60.,28.41999998,-55.24995));
#179175=CARTESIAN_POINT('',(51.9689593648599,28.41999998,-59.64995));
#179176=CARTESIAN_POINT('Ctrl Pts',(50.4632296085449,28.41999998,-61.14995));
#179177=CARTESIAN_POINT('Ctrl Pts',(50.6603646991919,28.41999998,-61.149949999985));
#179178=CARTESIAN_POINT('Ctrl Pts',(50.8573512000782,28.41999998,-61.1109090094727));
#179179=CARTESIAN_POINT('Ctrl Pts',(51.2215436797334,28.41999998,-60.9606295880612));
#179180=CARTESIAN_POINT('Ctrl Pts',(51.3885709017413,28.41999998,-60.849450253352));
#179181=CARTESIAN_POINT('Ctrl Pts',(51.6673117579979,28.41999998,-60.5717700902076));
#179182=CARTESIAN_POINT('Ctrl Pts',(51.7789157797339,28.41999998,-60.4053784571342));
#179183=CARTESIAN_POINT('Ctrl Pts',(51.9297692440612,28.41999998,-60.0425718399611));
#179184=CARTESIAN_POINT('Ctrl Pts',(51.9689593648456,28.41999998,-59.8463349320562));
#179185=CARTESIAN_POINT('Ctrl Pts',(51.9689593648599,28.41999998,-59.64995));
#179186=CARTESIAN_POINT('',(51.9689593648599,28.41999998,-55.74995));
#179187=CARTESIAN_POINT('',(51.9689593648599,28.41999998,-55.24995));
#179188=CARTESIAN_POINT('',(60.,28.41999998,-55.74995));
#179189=CARTESIAN_POINT('Ctrl Pts',(50.4632296085449,28.41999998,-61.14995));
#179190=CARTESIAN_POINT('Ctrl Pts',(50.4632296085449,28.41999998,-60.64995));
#179191=CARTESIAN_POINT('Ctrl Pts',(50.4632296085449,28.91999998,-60.64995));
#179192=CARTESIAN_POINT('Ctrl Pts',(50.6603646991919,28.41999998,-61.149949999985));
#179193=CARTESIAN_POINT('Ctrl Pts',(50.5943760783778,28.4199999799973,-60.6556217969837));
#179194=CARTESIAN_POINT('Ctrl Pts',(50.5951521564739,28.9142946217921,-60.64995));
#179195=CARTESIAN_POINT('Ctrl Pts',(50.8573512000782,28.41999998,-61.1109090094727));
#179196=CARTESIAN_POINT('Ctrl Pts',(50.728657566052,28.4199999799997,-60.6353187454025));
#179197=CARTESIAN_POINT('Ctrl Pts',(50.7269752683276,28.9085935639752,-60.6239226729817));
#179198=CARTESIAN_POINT('Ctrl Pts',(51.2215436797334,28.41999998,-60.9606295880612));
#179199=CARTESIAN_POINT('Ctrl Pts',(50.9800327848971,28.4199999800004,-60.5426326522478));
#179200=CARTESIAN_POINT('Ctrl Pts',(50.9706924051143,28.8980533372399,-60.5237363920408));
#179201=CARTESIAN_POINT('Ctrl Pts',(51.3885709017413,28.41999998,-60.849450253352));
#179202=CARTESIAN_POINT('Ctrl Pts',(51.0973398682523,28.4199999799993,-60.4706504746461));
#179203=CARTESIAN_POINT('Ctrl Pts',(51.0824668062551,28.8932193417862,-60.4496168355678));
#179204=CARTESIAN_POINT('Ctrl Pts',(51.6673117579979,28.41999998,-60.5717700902076));
#179205=CARTESIAN_POINT('Ctrl Pts',(51.294270482316,28.4199999800007,-60.2852157712125));
#179206=CARTESIAN_POINT('Ctrl Pts',(51.2689998270813,28.8851522014976,-60.2644967268053));
#179207=CARTESIAN_POINT('Ctrl Pts',(51.7789157797339,28.41999998,-60.4053784571342));
#179208=CARTESIAN_POINT('Ctrl Pts',(51.3742886138646,28.4199999800003,-60.1718710142637));
#179209=CARTESIAN_POINT('Ctrl Pts',(51.343685094216,28.8819222289984,-60.153568971423));
#179210=CARTESIAN_POINT('Ctrl Pts',(51.9297692440612,28.41999998,-60.0425718399611));
#179211=CARTESIAN_POINT('Ctrl Pts',(51.4824004299641,28.4199999799996,-59.9224177216067));
#179212=CARTESIAN_POINT('Ctrl Pts',(51.4446360376159,28.8775563241362,-59.9116978933072));
#179213=CARTESIAN_POINT('Ctrl Pts',(51.9689593648456,28.41999998,-59.8463349320562));
#179214=CARTESIAN_POINT('Ctrl Pts',(51.5107937778383,28.4199999799973,-59.7861314644994));
#179215=CARTESIAN_POINT('Ctrl Pts',(51.4708620158139,28.8764221086278,-59.7808732880376));
#179216=CARTESIAN_POINT('Ctrl Pts',(51.9689593648599,28.41999998,-59.64995));
#179217=CARTESIAN_POINT('Ctrl Pts',(51.5107937778512,28.41999998,-59.6499499999999));
#179218=CARTESIAN_POINT('Ctrl Pts',(51.4708620158141,28.8764221086262,-59.64995));
#179219=CARTESIAN_POINT('',(51.4708620158141,28.8764221086262,-59.64995));
#179220=CARTESIAN_POINT('Ctrl Pts',(51.4708620158141,28.8764221086262,-59.64995));
#179221=CARTESIAN_POINT('Ctrl Pts',(51.4708620158141,28.8764221086262,-59.6947437542449));
#179222=CARTESIAN_POINT('Ctrl Pts',(51.4677914119307,28.8765549054479,-59.7400065139138));
#179223=CARTESIAN_POINT('Ctrl Pts',(51.4615373286702,28.8768253807065,-59.7853172193946));
#179224=CARTESIAN_POINT('Ctrl Pts',(51.4553593802397,28.8770925633022,-59.8300763295867));
#179225=CARTESIAN_POINT('Ctrl Pts',(51.4460749723573,28.8774940933935,-59.8748822598591));
#179226=CARTESIAN_POINT('Ctrl Pts',(51.433582992122,28.8780343438896,-59.9192791434306));
#179227=CARTESIAN_POINT('Ctrl Pts',(51.4237924546126,28.878457762967,-59.9540750161202));
#179228=CARTESIAN_POINT('Ctrl Pts',(51.4120317874587,28.8789663857909,-59.9886186686624));
#179229=CARTESIAN_POINT('Ctrl Pts',(51.3982557900138,28.8795621671893,-60.022668488024));
#179230=CARTESIAN_POINT('Ctrl Pts',(51.3969099642094,28.8796203711765,-60.0259949350354));
#179231=CARTESIAN_POINT('Ctrl Pts',(51.395544903161,28.8796794070455,-60.0293166615587));
#179232=CARTESIAN_POINT('Ctrl Pts',(51.394160565916,28.8797392765673,-60.0326334323651));
#179233=CARTESIAN_POINT('Ctrl Pts',(51.3763389976224,28.8805100199507,-60.0753326067533));
#179234=CARTESIAN_POINT('Ctrl Pts',(51.3553254607148,28.8814188089116,-60.1171993192663));
#179235=CARTESIAN_POINT('Ctrl Pts',(51.3312072018932,28.8824618702235,-60.1577697852322));
#179236=CARTESIAN_POINT('Ctrl Pts',(51.3081659897204,28.8834583516518,-60.1965284999963));
#179237=CARTESIAN_POINT('Ctrl Pts',(51.2822921557851,28.8845773377017,-60.2341031988361));
#179238=CARTESIAN_POINT('Ctrl Pts',(51.2536794880379,28.885814772252,-60.2700569697484));
#179239=CARTESIAN_POINT('Ctrl Pts',(51.2402309219474,28.8863963929691,-60.2869560114103));
#179240=CARTESIAN_POINT('Ctrl Pts',(51.2261775125214,28.8870041718217,-60.3034964088543));
#179241=CARTESIAN_POINT('Ctrl Pts',(51.2115313248591,28.887637587021,-60.31962880781));
#179242=CARTESIAN_POINT('Ctrl Pts',(51.2063396801368,28.8878621141644,-60.3253472709232));
#179243=CARTESIAN_POINT('Ctrl Pts',(51.2007966899397,28.8881018362233,-60.331313045859));
#179244=CARTESIAN_POINT('Ctrl Pts',(51.1952694028553,28.8883408744107,-60.3371156972533));
#179245=CARTESIAN_POINT('Ctrl Pts',(51.1895768899865,28.8885870581058,-60.3430918058271));
#179246=CARTESIAN_POINT('Ctrl Pts',(51.1839011962162,28.8888325093769,-60.3488947477628));
#179247=CARTESIAN_POINT('Ctrl Pts',(51.1786846053927,28.8890580952226,-60.3541155165136));
#179248=CARTESIAN_POINT('Ctrl Pts',(51.1776827065602,28.8891014212574,-60.3551182177591));
#179249=CARTESIAN_POINT('Ctrl Pts',(51.1766978520225,28.8891440097864,-60.3560995559722));
#179250=CARTESIAN_POINT('Ctrl Pts',(51.1757333189604,28.889185719042,-60.3570567834875));
#179251=CARTESIAN_POINT('Ctrl Pts',(51.1538095834162,28.8901337660555,-60.3788144647157));
#179252=CARTESIAN_POINT('Ctrl Pts',(51.1302168006257,28.8911541156617,-60.4001952306223));
#179253=CARTESIAN_POINT('Ctrl Pts',(51.1049004315856,28.8922490328123,-60.4209274438526));
#179254=CARTESIAN_POINT('Ctrl Pts',(51.0800414498951,28.8933241682456,-60.4412850910443));
#179255=CARTESIAN_POINT('Ctrl Pts',(51.0535203284385,28.8944712128831,-60.4610175331667));
#179256=CARTESIAN_POINT('Ctrl Pts',(51.0253174707832,28.895690924054,-60.4798306487176));
#179257=CARTESIAN_POINT('Ctrl Pts',(50.9984842726526,28.8968514004819,-60.4977301134883));
#179258=CARTESIAN_POINT('Ctrl Pts',(50.9701273672128,28.8980777738785,-60.5147982857245));
#179259=CARTESIAN_POINT('Ctrl Pts',(50.9402580440922,28.8993695559923,-60.5307488754987));
#179260=CARTESIAN_POINT('Ctrl Pts',(50.9111997131181,28.9006262644907,-60.5462663853875));
#179261=CARTESIAN_POINT('Ctrl Pts',(50.8807093109566,28.9019449068983,-60.5607262880739));
#179262=CARTESIAN_POINT('Ctrl Pts',(50.848833836721,28.9033234506075,-60.5738295325112));
#179263=CARTESIAN_POINT('Ctrl Pts',(50.8483100004268,28.9033461053678,-60.5740448690724));
#179264=CARTESIAN_POINT('Ctrl Pts',(50.8477857926334,28.9033687761946,-60.5742598379419));
#179265=CARTESIAN_POINT('Ctrl Pts',(50.8472612136072,28.9033914630764,-60.5744744380591));
#179266=CARTESIAN_POINT('Ctrl Pts',(50.8446281185304,28.9035053386106,-60.5755516113424));
#179267=CARTESIAN_POINT('Ctrl Pts',(50.8412782753391,28.9036501970354,-60.5769043222802));
#179268=CARTESIAN_POINT('Ctrl Pts',(50.838494961749,28.9037705514899,-60.5780123790327));
#179269=CARTESIAN_POINT('Ctrl Pts',(50.8366796282304,28.9038490491037,-60.5787350760979));
#179270=CARTESIAN_POINT('Ctrl Pts',(50.8351058488345,28.9039170988377,-60.5793550577221));
#179271=CARTESIAN_POINT('Ctrl Pts',(50.8341332510858,28.9039591509512,-60.5797369926547));
#179272=CARTESIAN_POINT('Ctrl Pts',(50.8185784237332,28.9046316934953,-60.5858453061323));
#179273=CARTESIAN_POINT('Ctrl Pts',(50.8013542666607,28.9053764998681,-60.5921640965717));
#179274=CARTESIAN_POINT('Ctrl Pts',(50.7823963801911,28.9061963347677,-60.5984375212453));
#179275=CARTESIAN_POINT('Ctrl Pts',(50.763113162345,28.9070302386416,-60.6048186025338));
#179276=CARTESIAN_POINT('Ctrl Pts',(50.742035176342,28.907941812522,-60.6111530887002));
#179277=CARTESIAN_POINT('Ctrl Pts',(50.7191146374363,28.9089331013732,-60.6171173698768));
#179278=CARTESIAN_POINT('Ctrl Pts',(50.6984237561229,28.9098279599125,-60.6225014594243));
#179279=CARTESIAN_POINT('Ctrl Pts',(50.6762310064599,28.9107877942718,-60.6275832962447));
#179280=CARTESIAN_POINT('Ctrl Pts',(50.6525261952328,28.9118130292334,-60.6320843347403));
#179281=CARTESIAN_POINT('Ctrl Pts',(50.6295865055205,28.9128051726289,-60.6364400929653));
#179282=CARTESIAN_POINT('Ctrl Pts',(50.6052302671986,28.9138585854426,-60.6402518751851));
#179283=CARTESIAN_POINT('Ctrl Pts',(50.5794793889038,28.9149723054461,-60.6432310344106));
#179284=CARTESIAN_POINT('Ctrl Pts',(50.5549130980113,28.9160347922967,-60.6460731468742));
#179285=CARTESIAN_POINT('Ctrl Pts',(50.5290771857652,28.9171521802695,-60.648157343778));
#179286=CARTESIAN_POINT('Ctrl Pts',(50.5020254916425,28.9183221279484,-60.649201067293));
#179287=CARTESIAN_POINT('Ctrl Pts',(50.489356743992,28.9188700334453,-60.6496898599641));
#179288=CARTESIAN_POINT('Ctrl Pts',(50.4764218916548,28.9194294429546,-60.64995));
#179289=CARTESIAN_POINT('Ctrl Pts',(50.4632296085449,28.91999998,-60.64995));
#179290=CARTESIAN_POINT('Origin',(51.9689593648599,28.91999998,-59.64995));
#179291=CARTESIAN_POINT('Origin',(60.,27.91999998,-55.74995));
#179292=CARTESIAN_POINT('',(52.0564480283858,27.91999998,-55.24995));
#179293=CARTESIAN_POINT('Ctrl Pts',(51.9689593648599,28.41999998,-55.74995));
#179294=CARTESIAN_POINT('Ctrl Pts',(51.9689593648599,28.41999998,-55.7240510277418));
#179295=CARTESIAN_POINT('Ctrl Pts',(51.9693268087427,28.4179000286038,-55.697853607272));
#179296=CARTESIAN_POINT('Ctrl Pts',(51.9700690003256,28.413658384301,-55.6716786001611));
#179297=CARTESIAN_POINT('Ctrl Pts',(51.9708174603259,28.4093809158292,-55.6452825236222));
#179298=CARTESIAN_POINT('Ctrl Pts',(51.9719470328068,28.4029253795636,-55.6189093029559));
#179299=CARTESIAN_POINT('Ctrl Pts',(51.9734602061033,28.3942775546035,-55.5929324714478));
#179300=CARTESIAN_POINT('Ctrl Pts',(51.9740304013453,28.3910188738844,-55.5831438598178));
#179301=CARTESIAN_POINT('Ctrl Pts',(51.974655014541,28.3874491931361,-55.5734119763965));
#179302=CARTESIAN_POINT('Ctrl Pts',(51.9753339939828,28.3835688078698,-55.5637583893672));
#179303=CARTESIAN_POINT('Ctrl Pts',(51.977112728374,28.3734032943058,-55.5384687175561));
#179304=CARTESIAN_POINT('Ctrl Pts',(51.9792657855805,28.361098516063,-55.5136974845899));
#179305=CARTESIAN_POINT('Ctrl Pts',(51.9817930862496,28.3466549266444,-55.4898442371366));
#179306=CARTESIAN_POINT('Ctrl Pts',(51.9838432153151,28.3349383854197,-55.4704946454921));
#179307=CARTESIAN_POINT('Ctrl Pts',(51.9861398889717,28.3218128354093,-55.451748367254));
#179308=CARTESIAN_POINT('Ctrl Pts',(51.98867993897,28.3072963832421,-55.4338552802796));
#179309=CARTESIAN_POINT('Ctrl Pts',(51.9900517282542,28.2994565716081,-55.4241918701149));
#179310=CARTESIAN_POINT('Ctrl Pts',(51.9914944591103,28.2912113270354,-55.4147778015411));
#179311=CARTESIAN_POINT('Ctrl Pts',(51.993006833706,28.2825680666705,-55.4056571306828));
#179312=CARTESIAN_POINT('Ctrl Pts',(51.993308064795,28.2808465231189,-55.4038404976718));
#179313=CARTESIAN_POINT('Ctrl Pts',(51.9936750712784,28.2787490714756,-55.4016626948096));
#179314=CARTESIAN_POINT('Ctrl Pts',(51.993998383369,28.2769013041842,-55.3997779182116));
#179315=CARTESIAN_POINT('Ctrl Pts',(51.9942306762961,28.2755737223049,-55.3984237459251));
#179316=CARTESIAN_POINT('Ctrl Pts',(51.9944401788581,28.2743763723404,-55.3972196111484));
#179317=CARTESIAN_POINT('Ctrl Pts',(51.9945841744765,28.2735533694274,-55.3963966082408));
#179318=CARTESIAN_POINT('Ctrl Pts',(51.996292885289,28.2637872807656,-55.3866305196434));
#179319=CARTESIAN_POINT('Ctrl Pts',(51.9982002406164,28.2528864178514,-55.3765717208114));
#179320=CARTESIAN_POINT('Ctrl Pts',(52.0003285939908,28.2407228045164,-55.3664552894479));
#179321=CARTESIAN_POINT('Ctrl Pts',(52.0023666881836,28.2290750255335,-55.3567678755708));
#179322=CARTESIAN_POINT('Ctrl Pts',(52.0046075587555,28.2162686120025,-55.3470275906024));
#179323=CARTESIAN_POINT('Ctrl Pts',(52.0070668802308,28.2022137834753,-55.337481543908));
#179324=CARTESIAN_POINT('Ctrl Pts',(52.0093860198903,28.1889600829847,-55.328479623784));
#179325=CARTESIAN_POINT('Ctrl Pts',(52.0118994950179,28.1745957837208,-55.3196505220217));
#179326=CARTESIAN_POINT('Ctrl Pts',(52.0146154596132,28.1590741144307,-55.3112377696321));
#179327=CARTESIAN_POINT('Ctrl Pts',(52.0157114814312,28.152810377332,-55.3078428210439));
#179328=CARTESIAN_POINT('Ctrl Pts',(52.0168404135437,28.1463585346195,-55.3045160976751));
#179329=CARTESIAN_POINT('Ctrl Pts',(52.0180024981996,28.1397171904213,-55.3012753797206));
#179330=CARTESIAN_POINT('Ctrl Pts',(52.0206705726152,28.1244690753626,-55.2938348919567));
#179331=CARTESIAN_POINT('Ctrl Pts',(52.0235156308817,28.1082094929675,-55.286840723483));
#179332=CARTESIAN_POINT('Ctrl Pts',(52.0265363392804,28.0909460654729,-55.2805340044421));
#179333=CARTESIAN_POINT('Ctrl Pts',(52.0294725600147,28.07416548719,-55.2744036810978));
#179334=CARTESIAN_POINT('Ctrl Pts',(52.0325747975933,28.0564361182996,-55.2689228588362));
#179335=CARTESIAN_POINT('Ctrl Pts',(52.0358354676438,28.0378013036895,-55.2643427579155));
#179336=CARTESIAN_POINT('Ctrl Pts',(52.0389930632159,28.0197555624189,-55.259907440584));
#179337=CARTESIAN_POINT('Ctrl Pts',(52.0422992724608,28.0008604901217,-55.2563167977524));
#179338=CARTESIAN_POINT('Ctrl Pts',(52.0457404862589,27.9811938632732,-55.2538274761772));
#179339=CARTESIAN_POINT('Ctrl Pts',(52.0491817000569,27.9615272364247,-55.2513381546019));
#179340=CARTESIAN_POINT('Ctrl Pts',(52.0527579931129,27.9410886280845,-55.24995));
#179341=CARTESIAN_POINT('Ctrl Pts',(52.0564480283858,27.91999998,-55.24995));
#179342=CARTESIAN_POINT('',(60.,27.91999998,-55.24995));
#179343=CARTESIAN_POINT('Origin',(60.,28.41999998,-55.24995));
#179344=CARTESIAN_POINT('',(52.1001923601488,27.41999998,-55.24995));
#179345=CARTESIAN_POINT('',(52.0733761857257,27.7265102562164,-55.24995));
#179346=CARTESIAN_POINT('',(60.,27.41999998,-55.24995));
#179347=CARTESIAN_POINT('Origin',(60.,27.41999998,-55.74995));
#179348=CARTESIAN_POINT('',(52.1876810236747,26.91999998,-55.74995));
#179349=CARTESIAN_POINT('Ctrl Pts',(52.1001923601488,27.41999998,-55.24995));
#179350=CARTESIAN_POINT('Ctrl Pts',(52.1039692544698,27.3984149301844,-55.24995));
#179351=CARTESIAN_POINT('Ctrl Pts',(52.1075962444343,27.3774879325696,-55.2513479743312));
#179352=CARTESIAN_POINT('Ctrl Pts',(52.1110733300424,27.3573682601684,-55.2538882420798));
#179353=CARTESIAN_POINT('Ctrl Pts',(52.1145448981266,27.3372805141512,-55.2564244788698));
#179354=CARTESIAN_POINT('Ctrl Pts',(52.1178670372207,27.3179969554615,-55.2600986724002));
#179355=CARTESIAN_POINT('Ctrl Pts',(52.1210397473245,27.2996086400427,-55.2646604727451));
#179356=CARTESIAN_POINT('Ctrl Pts',(52.1243513930363,27.2804150850335,-55.2694220381124));
#179357=CARTESIAN_POINT('Ctrl Pts',(52.1275002359685,27.2621965820888,-55.275149957033));
#179358=CARTESIAN_POINT('Ctrl Pts',(52.130486276121,27.2450003125949,-55.281575025852));
#179359=CARTESIAN_POINT('Ctrl Pts',(52.1332354059753,27.2291683828708,-55.2874903342887));
#179360=CARTESIAN_POINT('Ctrl Pts',(52.1358465415646,27.2142018443753,-55.2939965089216));
#179361=CARTESIAN_POINT('Ctrl Pts',(52.138319682889,27.2001025975964,-55.3009008476658));
#179362=CARTESIAN_POINT('Ctrl Pts',(52.1412013074786,27.1836746095095,-55.3089455607216));
#179363=CARTESIAN_POINT('Ctrl Pts',(52.1438955888521,27.1684242891165,-55.3175297932171));
#179364=CARTESIAN_POINT('Ctrl Pts',(52.1464025270093,27.1543108257794,-55.3263826814667));
#179365=CARTESIAN_POINT('Ctrl Pts',(52.1483805817288,27.1431748499345,-55.3333678946174));
#179366=CARTESIAN_POINT('Ctrl Pts',(52.1502420018674,27.1327455689858,-55.3405210924908));
#179367=CARTESIAN_POINT('Ctrl Pts',(52.151986787425,27.1229879533935,-55.3477263606511));
#179368=CARTESIAN_POINT('Ctrl Pts',(52.153964829468,27.1119258639597,-55.3558948850236));
#179369=CARTESIAN_POINT('Ctrl Pts',(52.1557929671545,27.1017269109606,-55.3641299065508));
#179370=CARTESIAN_POINT('Ctrl Pts',(52.1574712004845,27.0923264617539,-55.3722860416452));
#179371=CARTESIAN_POINT('Ctrl Pts',(52.1583103171494,27.0876262371506,-55.3763641091924));
#179372=CARTESIAN_POINT('Ctrl Pts',(52.1591119577253,27.0831254533124,-55.3804228422634));
#179373=CARTESIAN_POINT('Ctrl Pts',(52.1598761222121,27.0788151725342,-55.3844463377003));
#179374=CARTESIAN_POINT('Ctrl Pts',(52.1602582044554,27.0766600321451,-55.3864580854188));
#179375=CARTESIAN_POINT('Ctrl Pts',(52.1606309176765,27.0745525258254,-55.3884610324842));
#179376=CARTESIAN_POINT('Ctrl Pts',(52.1609942618754,27.0724914802186,-55.3904533483054));
#179377=CARTESIAN_POINT('Ctrl Pts',(52.1612198097561,27.0712120749871,-55.3916900891499));
#179378=CARTESIAN_POINT('Ctrl Pts',(52.1613688244011,27.0703718307476,-55.3925105847812));
#179379=CARTESIAN_POINT('Ctrl Pts',(52.1615771078567,27.0691841523735,-55.3936800811369));
#179380=CARTESIAN_POINT('Ctrl Pts',(52.1617043566395,27.0684585516433,-55.3943945737371));
#179381=CARTESIAN_POINT('Ctrl Pts',(52.1618537273994,27.0676035577912,-55.3952396410222));
#179382=CARTESIAN_POINT('Ctrl Pts',(52.1620561874049,27.0664465894067,-55.3963966094067));
#179383=CARTESIAN_POINT('Ctrl Pts',(52.1651986633863,27.0484887445991,-55.4143544542144));
#179384=CARTESIAN_POINT('Ctrl Pts',(52.1680521085855,27.0320748238547,-55.433509382758));
#179385=CARTESIAN_POINT('Ctrl Pts',(52.1706165230026,27.0173083263743,-55.4535728212224));
#179386=CARTESIAN_POINT('Ctrl Pts',(52.1732171913392,27.0023330703531,-55.4739199027201));
#179387=CARTESIAN_POINT('Ctrl Pts',(52.1755205988918,26.9890520084134,-55.4952007603085));
#179388=CARTESIAN_POINT('Ctrl Pts',(52.1775267456605,26.9775195753864,-55.5171172455752));
#179389=CARTESIAN_POINT('Ctrl Pts',(52.1795769127367,26.9657340894641,-55.53951463804));
#179390=CARTESIAN_POINT('Ctrl Pts',(52.1813166304854,26.9557746307472,-55.5625752639374));
#179391=CARTESIAN_POINT('Ctrl Pts',(52.1827458989067,26.9476461596984,-55.5859930896654));
#179392=CARTESIAN_POINT('Ctrl Pts',(52.1841932371623,26.9394149227008,-55.6097069803071));
#179393=CARTESIAN_POINT('Ctrl Pts',(52.1853222266237,26.9330609012905,-55.6337866414178));
#179394=CARTESIAN_POINT('Ctrl Pts',(52.1861328672907,26.928539638511,-55.6579351493319));
#179395=CARTESIAN_POINT('Ctrl Pts',(52.1869587610608,26.9239333031587,-55.6825380382005));
#179396=CARTESIAN_POINT('Ctrl Pts',(52.1874542131553,26.9212289400873,-55.7072119142524));
#179397=CARTESIAN_POINT('Ctrl Pts',(52.1876192235742,26.9203341785897,-55.7316719557658));
#179398=CARTESIAN_POINT('Ctrl Pts',(52.1876604236412,26.9201107730988,-55.7377791783033));
#179399=CARTESIAN_POINT('Ctrl Pts',(52.1876810236747,26.91999998,-55.7438732288818));
#179400=CARTESIAN_POINT('Ctrl Pts',(52.1876810236747,26.91999998,-55.74995));
#179401=CARTESIAN_POINT('',(-83.2809572255632,26.9199999800001,-55.74995));
#179402=CARTESIAN_POINT('Origin',(-83.2809572255632,26.9199999800001,-55.24995));
#179403=CARTESIAN_POINT('',(52.1876810236747,26.91999998,-59.64995));
#179404=CARTESIAN_POINT('',(52.1876810236747,26.91999998,-55.24995));
#179405=CARTESIAN_POINT('Ctrl Pts',(52.1876810236747,26.91999998,-59.64995));
#179406=CARTESIAN_POINT('Ctrl Pts',(52.1876810236604,26.91999998,-59.8463349320561));
#179407=CARTESIAN_POINT('Ctrl Pts',(52.148490902876,26.91999998,-60.0425718399612));
#179408=CARTESIAN_POINT('Ctrl Pts',(51.9976374385487,26.91999998,-60.4053784571341));
#179409=CARTESIAN_POINT('Ctrl Pts',(51.8860334168128,26.91999998,-60.5717700902076));
#179410=CARTESIAN_POINT('Ctrl Pts',(51.6072925605561,26.91999998,-60.8494502533521));
#179411=CARTESIAN_POINT('Ctrl Pts',(51.4402653385482,26.91999998,-60.9606295880611));
#179412=CARTESIAN_POINT('Ctrl Pts',(51.0760728588929,26.91999998,-61.1109090094727));
#179413=CARTESIAN_POINT('Ctrl Pts',(50.8790863580067,26.91999998,-61.149949999985));
#179414=CARTESIAN_POINT('Ctrl Pts',(50.6819512673597,26.91999998,-61.14995));
#179415=CARTESIAN_POINT('Ctrl Pts',(51.1762622162812,20.26999998,-61.14995));
#179416=CARTESIAN_POINT('Ctrl Pts',(51.1762622162812,20.26999998,-60.64995));
#179417=CARTESIAN_POINT('Ctrl Pts',(51.1762622162812,20.76999998,-60.64995));
#179418=CARTESIAN_POINT('Ctrl Pts',(51.3733973069281,20.26999998,-61.149949999985));
#179419=CARTESIAN_POINT('Ctrl Pts',(51.3074086861135,20.2699999799973,-60.6556217969837));
#179420=CARTESIAN_POINT('Ctrl Pts',(51.3081847642104,20.764294621792,-60.64995));
#179421=CARTESIAN_POINT('Ctrl Pts',(51.5703838078145,20.26999998,-61.1109090094727));
#179422=CARTESIAN_POINT('Ctrl Pts',(51.4416901737888,20.2699999799993,-60.6353187454032));
#179423=CARTESIAN_POINT('Ctrl Pts',(51.4400078760636,20.7585935639752,-60.6239226729818));
#179424=CARTESIAN_POINT('Ctrl Pts',(51.9345762874696,20.26999998,-60.9606295880612));
#179425=CARTESIAN_POINT('Ctrl Pts',(51.6930653926326,20.2699999800007,-60.5426326522471));
#179426=CARTESIAN_POINT('Ctrl Pts',(51.6837250128509,20.7480533372398,-60.5237363920407));
#179427=CARTESIAN_POINT('Ctrl Pts',(52.1016035094776,20.26999998,-60.849450253352));
#179428=CARTESIAN_POINT('Ctrl Pts',(51.810372475988,20.2699999799993,-60.4706504746462));
#179429=CARTESIAN_POINT('Ctrl Pts',(51.7954994139911,20.7432193417859,-60.4496168355681));
#179430=CARTESIAN_POINT('Ctrl Pts',(52.3803443657342,20.26999998,-60.5717700902076));
#179431=CARTESIAN_POINT('Ctrl Pts',(52.007303090053,20.2699999800007,-60.2852157712124));
#179432=CARTESIAN_POINT('Ctrl Pts',(51.9820324348179,20.7351522014979,-60.264496726805));
#179433=CARTESIAN_POINT('Ctrl Pts',(52.4919483874702,20.26999998,-60.4053784571342));
#179434=CARTESIAN_POINT('Ctrl Pts',(52.0873212216015,20.2699999800003,-60.1718710142637));
#179435=CARTESIAN_POINT('Ctrl Pts',(52.0567177019522,20.7319222289985,-60.153568971423));
#179436=CARTESIAN_POINT('Ctrl Pts',(52.6428018517975,20.26999998,-60.0425718399611));
#179437=CARTESIAN_POINT('Ctrl Pts',(52.1954330376997,20.2699999799997,-59.9224177216067));
#179438=CARTESIAN_POINT('Ctrl Pts',(52.1576686453522,20.7275563241362,-59.9116978933072));
#179439=CARTESIAN_POINT('Ctrl Pts',(52.6819919725819,20.26999998,-59.8463349320562));
#179440=CARTESIAN_POINT('Ctrl Pts',(52.2238263855712,20.2699999800007,-59.7861314644994));
#179441=CARTESIAN_POINT('Ctrl Pts',(52.1838946235501,20.7264221086281,-59.7808732880376));
#179442=CARTESIAN_POINT('Ctrl Pts',(52.6819919725962,20.26999998,-59.64995));
#179443=CARTESIAN_POINT('Ctrl Pts',(52.2238263855875,20.26999998,-59.6499499999999));
#179444=CARTESIAN_POINT('Ctrl Pts',(52.1838946235503,20.7264221086262,-59.64995));
#179445=CARTESIAN_POINT('',(52.1838946235503,20.7264221086262,-59.64995));
#179446=CARTESIAN_POINT('Ctrl Pts',(52.1838946235503,20.7264221086262,-59.64995));
#179447=CARTESIAN_POINT('Ctrl Pts',(52.1838946235503,20.7264221086262,-59.6947437539778));
#179448=CARTESIAN_POINT('Ctrl Pts',(52.1808240197036,20.7265549054463,-59.7400065133852));
#179449=CARTESIAN_POINT('Ctrl Pts',(52.1745699365138,20.7268253807018,-59.785317218617));
#179450=CARTESIAN_POINT('Ctrl Pts',(52.1683919881554,20.7270925632944,-59.8300763285467));
#179451=CARTESIAN_POINT('Ctrl Pts',(52.1591075803806,20.7274940933811,-59.874882258569));
#179452=CARTESIAN_POINT('Ctrl Pts',(52.1466156002861,20.7280343438711,-59.91927914191));
#179453=CARTESIAN_POINT('Ctrl Pts',(52.1368250627133,20.7284577629512,-59.9540750150364));
#179454=CARTESIAN_POINT('Ctrl Pts',(52.1250643954463,20.72896638578,-59.9886186680186));
#179455=CARTESIAN_POINT('Ctrl Pts',(52.1112883978351,20.7295621671856,-60.0226684878138));
#179456=CARTESIAN_POINT('Ctrl Pts',(52.1099425720032,20.729620371174,-60.0259949348954));
#179457=CARTESIAN_POINT('Ctrl Pts',(52.1085775109265,20.7296794070442,-60.0293166614888));
#179458=CARTESIAN_POINT('Ctrl Pts',(52.1071931736522,20.7297392765673,-60.0326334323651));
#179459=CARTESIAN_POINT('Ctrl Pts',(52.0893716054534,20.7305100199466,-60.0753326065261));
#179460=CARTESIAN_POINT('Ctrl Pts',(52.068358068671,20.7314188089021,-60.1171993188295));
#179461=CARTESIAN_POINT('Ctrl Pts',(52.0442398100001,20.7324618702076,-60.1577697846088));
#179462=CARTESIAN_POINT('Ctrl Pts',(52.021198598004,20.7334583516282,-60.1965284991394));
#179463=CARTESIAN_POINT('Ctrl Pts',(51.9953247642768,20.7345773376692,-60.23410319777));
#179464=CARTESIAN_POINT('Ctrl Pts',(51.9667120967645,20.7358147722093,-60.270056968504));
#179465=CARTESIAN_POINT('Ctrl Pts',(51.9532635303856,20.7363963929389,-60.2869560105833));
#179466=CARTESIAN_POINT('Ctrl Pts',(51.9392101206412,20.7370041718053,-60.3034964084302));
#179467=CARTESIAN_POINT('Ctrl Pts',(51.9245639326311,20.7376375870196,-60.3196288077707));
#179468=CARTESIAN_POINT('Ctrl Pts',(51.9193722879604,20.7378621141607,-60.3253472708277));
#179469=CARTESIAN_POINT('Ctrl Pts',(51.9138292978107,20.7381018362176,-60.3313130457146));
#179470=CARTESIAN_POINT('Ctrl Pts',(51.9083020107728,20.7383408744029,-60.3371156970632));
#179471=CARTESIAN_POINT('Ctrl Pts',(51.9026094979459,20.738587058096,-60.3430918055961));
#179472=CARTESIAN_POINT('Ctrl Pts',(51.8969338042165,20.7388325093651,-60.348894747494));
#179473=CARTESIAN_POINT('Ctrl Pts',(51.8917172134375,20.7390580952084,-60.3541155162049));
#179474=CARTESIAN_POINT('Ctrl Pts',(51.8907153144978,20.7391014212477,-60.3551182175586));
#179475=CARTESIAN_POINT('Ctrl Pts',(51.8897304598568,20.7391440097811,-60.3560995558751));
#179476=CARTESIAN_POINT('Ctrl Pts',(51.8887659266967,20.7391857190408,-60.3570567834876));
#179477=CARTESIAN_POINT('Ctrl Pts',(51.8668421914293,20.7401337660398,-60.3788144644414));
#179478=CARTESIAN_POINT('Ctrl Pts',(51.8432494089284,20.7411541156338,-60.4001952301119));
#179479=CARTESIAN_POINT('Ctrl Pts',(51.8179330401853,20.7422490327724,-60.4209274431457));
#179480=CARTESIAN_POINT('Ctrl Pts',(51.7930740583666,20.7433241682122,-60.4412850904884));
#179481=CARTESIAN_POINT('Ctrl Pts',(51.7665529367326,20.7444712128588,-60.4610175327789));
#179482=CARTESIAN_POINT('Ctrl Pts',(51.7383500788444,20.7456909240398,-60.479830648501));
#179483=CARTESIAN_POINT('Ctrl Pts',(51.7115168807664,20.7468514004655,-60.4977301132515));
#179484=CARTESIAN_POINT('Ctrl Pts',(51.68315997536,20.7480777738606,-60.514798285487));
#179485=CARTESIAN_POINT('Ctrl Pts',(51.6532906522493,20.749369555974,-60.5307488752741));
#179486=CARTESIAN_POINT('Ctrl Pts',(51.6242323211694,20.750626264477,-60.5462663852369));
#179487=CARTESIAN_POINT('Ctrl Pts',(51.5937419188686,20.7519449068907,-60.5607262880017));
#179488=CARTESIAN_POINT('Ctrl Pts',(51.5618664444573,20.7533234506075,-60.5738295325113));
#179489=CARTESIAN_POINT('Ctrl Pts',(51.5613426081777,20.7533461053672,-60.5740448690664));
#179490=CARTESIAN_POINT('Ctrl Pts',(51.5608184003988,20.7533687761933,-60.5742598379299));
#179491=CARTESIAN_POINT('Ctrl Pts',(51.5602938213872,20.7533914630745,-60.5744744380412));
#179492=CARTESIAN_POINT('Ctrl Pts',(51.5576607263164,20.7535053386084,-60.5755516113222));
#179493=CARTESIAN_POINT('Ctrl Pts',(51.5543108831315,20.753650197033,-60.5769043222577));
#179494=CARTESIAN_POINT('Ctrl Pts',(51.5515275695402,20.7537705514875,-60.5780123790108));
#179495=CARTESIAN_POINT('Ctrl Pts',(51.5497122359956,20.7538490491025,-60.5787350760865));
#179496=CARTESIAN_POINT('Ctrl Pts',(51.5481384565771,20.7539170988375,-60.5793550577197));
#179497=CARTESIAN_POINT('Ctrl Pts',(51.5471658588221,20.7539591509512,-60.5797369926547));
#179498=CARTESIAN_POINT('Ctrl Pts',(51.5316110315242,20.7546316934927,-60.5858453061108));
#179499=CARTESIAN_POINT('Ctrl Pts',(51.5143868745062,20.7553764998629,-60.592164096532));
#179500=CARTESIAN_POINT('Ctrl Pts',(51.4954289880907,20.7561963347601,-60.5984375211913));
#179501=CARTESIAN_POINT('Ctrl Pts',(51.4761457702625,20.7570302386331,-60.6048186024775));
#179502=CARTESIAN_POINT('Ctrl Pts',(51.45506778427,20.757941812513,-60.6111530886455));
#179503=CARTESIAN_POINT('Ctrl Pts',(51.4321472453672,20.7589331013641,-60.6171173698262));
#179504=CARTESIAN_POINT('Ctrl Pts',(51.411456364092,20.7598279599018,-60.6225014593681));
#179505=CARTESIAN_POINT('Ctrl Pts',(51.3892636144662,20.7607877942596,-60.627583296186));
#179506=CARTESIAN_POINT('Ctrl Pts',(51.3655588032748,20.7618130292197,-60.6320843346823));
#179507=CARTESIAN_POINT('Ctrl Pts',(51.342619113597,20.7628051726138,-60.636440092908));
#179508=CARTESIAN_POINT('Ctrl Pts',(51.3182628753082,20.7638585854262,-60.6402518751315));
#179509=CARTESIAN_POINT('Ctrl Pts',(51.2925119970447,20.7649723054284,-60.6432310343638));
#179510=CARTESIAN_POINT('Ctrl Pts',(51.2679457061843,20.7660347922777,-60.6460731468337));
#179511=CARTESIAN_POINT('Ctrl Pts',(51.2421097939689,20.7671521802492,-60.6481573437467));
#179512=CARTESIAN_POINT('Ctrl Pts',(51.2150580998752,20.7683221279269,-60.6492010672739));
#179513=CARTESIAN_POINT('Ctrl Pts',(51.2023893520667,20.7688700334307,-60.6496898599573));
#179514=CARTESIAN_POINT('Ctrl Pts',(51.1894544995639,20.7694294429471,-60.64995));
#179515=CARTESIAN_POINT('Ctrl Pts',(51.1762622162812,20.76999998,-60.64995));
#179516=CARTESIAN_POINT('Origin',(52.6819919725962,20.76999998,-59.64995));
#179517=CARTESIAN_POINT('Ctrl Pts',(52.1876810236747,26.91999998,-59.64995));
#179518=CARTESIAN_POINT('Ctrl Pts',(51.6420267731401,26.91999998,-59.64995));
#179519=CARTESIAN_POINT('Ctrl Pts',(51.6895836746289,26.3764221086262,-59.64995));
#179520=CARTESIAN_POINT('Ctrl Pts',(52.1876810236604,26.91999998,-59.8463349320561));
#179521=CARTESIAN_POINT('Ctrl Pts',(51.6420267731333,26.919999980002,-59.7746029379318));
#179522=CARTESIAN_POINT('Ctrl Pts',(51.6895836746287,26.3764221086278,-59.7808732880375));
#179523=CARTESIAN_POINT('Ctrl Pts',(52.148490902876,26.91999998,-60.0425718399612));
#179524=CARTESIAN_POINT('Ctrl Pts',(51.6186060348034,26.9199999800004,-59.8989712332639));
#179525=CARTESIAN_POINT('Ctrl Pts',(51.6633576964307,26.3775563241358,-59.9116978933072));
#179526=CARTESIAN_POINT('Ctrl Pts',(51.9976374385487,26.91999998,-60.4053784571341));
#179527=CARTESIAN_POINT('Ctrl Pts',(51.5267774915774,26.9199999799997,-60.1322291512607));
#179528=CARTESIAN_POINT('Ctrl Pts',(51.5624067530308,26.3819222289988,-60.1535689714229));
#179529=CARTESIAN_POINT('Ctrl Pts',(51.8860334168128,26.91999998,-60.5717700902076));
#179530=CARTESIAN_POINT('Ctrl Pts',(51.4587108395762,26.9199999799996,-60.2406767152617));
#179531=CARTESIAN_POINT('Ctrl Pts',(51.4877214858962,26.3851522014976,-60.2644967268053));
#179532=CARTESIAN_POINT('Ctrl Pts',(51.6072925605561,26.91999998,-60.8494502533521));
#179533=CARTESIAN_POINT('Ctrl Pts',(51.2846839917031,26.9199999800004,-60.4261994932779));
#179534=CARTESIAN_POINT('Ctrl Pts',(51.3011884650699,26.3932193417862,-60.4496168355678));
#179535=CARTESIAN_POINT('Ctrl Pts',(51.4402653385482,26.91999998,-60.9606295880611));
#179536=CARTESIAN_POINT('Ctrl Pts',(51.1792534074218,26.9199999799993,-60.5031527166058));
#179537=CARTESIAN_POINT('Ctrl Pts',(51.1894140639292,26.3980533372399,-60.5237363920408));
#179538=CARTESIAN_POINT('Ctrl Pts',(51.0760728588929,26.91999998,-61.1109090094727));
#179539=CARTESIAN_POINT('Ctrl Pts',(50.9439864347103,26.9199999800007,-60.6120353079387));
#179540=CARTESIAN_POINT('Ctrl Pts',(50.9456969271423,26.4085935639752,-60.6239226729817));
#179541=CARTESIAN_POINT('Ctrl Pts',(50.8790863580067,26.91999998,-61.149949999985));
#179542=CARTESIAN_POINT('Ctrl Pts',(50.8146696888639,26.9199999800028,-60.6442102195338));
#179543=CARTESIAN_POINT('Ctrl Pts',(50.8138738152888,26.4142946217921,-60.64995));
#179544=CARTESIAN_POINT('Ctrl Pts',(50.6819512673597,26.91999998,-61.14995));
#179545=CARTESIAN_POINT('Ctrl Pts',(50.6819512673597,26.91999998,-60.64995));
#179546=CARTESIAN_POINT('Ctrl Pts',(50.6819512673597,26.41999998,-60.64995));
#179547=CARTESIAN_POINT('',(51.6895836746288,26.3764221086262,-59.64995));
#179548=CARTESIAN_POINT('Origin',(52.1876810236747,26.41999998,-59.64995));
#179549=CARTESIAN_POINT('Ctrl Pts',(50.6819512673597,26.41999998,-60.64995));
#179550=CARTESIAN_POINT('Ctrl Pts',(50.7109216498289,26.4187470750797,-60.64995));
#179551=CARTESIAN_POINT('Ctrl Pts',(50.7386501990522,26.4175587192038,-60.6487118041208));
#179552=CARTESIAN_POINT('Ctrl Pts',(50.765056036357,26.4164278364053,-60.6465429519636));
#179553=CARTESIAN_POINT('Ctrl Pts',(50.7925707013286,26.415249465844,-60.6442830258803));
#179554=CARTESIAN_POINT('Ctrl Pts',(50.8186497119696,26.4141335381347,-60.6410132281087));
#179555=CARTESIAN_POINT('Ctrl Pts',(50.8432520459097,26.4130764642849,-60.6370534672329));
#179556=CARTESIAN_POINT('Ctrl Pts',(50.8636595387387,26.4121996276782,-60.6337688686304));
#179557=CARTESIAN_POINT('Ctrl Pts',(50.8830521268965,26.4113633856883,-60.6300090683738));
#179558=CARTESIAN_POINT('Ctrl Pts',(50.9014271157008,26.4105675025612,-60.6259392752378));
#179559=CARTESIAN_POINT('Ctrl Pts',(50.9247296256716,26.4095581917691,-60.6207781077323));
#179560=CARTESIAN_POINT('Ctrl Pts',(50.9463951635552,26.4086137504418,-60.6151198746454));
#179561=CARTESIAN_POINT('Ctrl Pts',(50.9664496076967,26.4077364426411,-60.6092623723524));
#179562=CARTESIAN_POINT('Ctrl Pts',(50.9729822346157,26.407450664361,-60.6073543226011));
#179563=CARTESIAN_POINT('Ctrl Pts',(50.9793441339268,26.4071720292579,-60.6054247759641));
#179564=CARTESIAN_POINT('Ctrl Pts',(50.9855367745778,26.4069006658479,-60.6034830010953));
#179565=CARTESIAN_POINT('Ctrl Pts',(50.9981384568014,26.4063484562733,-60.5995315963188));
#179566=CARTESIAN_POINT('Ctrl Pts',(51.0100390679368,26.4058263438341,-60.5955300977548));
#179567=CARTESIAN_POINT('Ctrl Pts',(51.021253530521,26.4053356340831,-60.5915501614527));
#179568=CARTESIAN_POINT('Ctrl Pts',(51.0268607618131,26.4050902792076,-60.5895601933016));
#179569=CARTESIAN_POINT('Ctrl Pts',(51.0322964183045,26.4048527717091,-60.5875755119569));
#179570=CARTESIAN_POINT('Ctrl Pts',(51.0375626846602,26.4046233027209,-60.5856042390701));
#179571=CARTESIAN_POINT('Ctrl Pts',(51.040195817838,26.4045085682269,-60.5846186026267));
#179572=CARTESIAN_POINT('Ctrl Pts',(51.0427866011158,26.4043958431534,-60.5836363114303));
#179573=CARTESIAN_POINT('Ctrl Pts',(51.0453353024098,26.4042851509401,-60.5826583364025));
#179574=CARTESIAN_POINT('Ctrl Pts',(51.0470835270635,26.404209224092,-60.5819875163034));
#179575=CARTESIAN_POINT('Ctrl Pts',(51.0479000495842,26.4041734759918,-60.5816721106921));
#179576=CARTESIAN_POINT('Ctrl Pts',(51.0496620341368,26.4040972539742,-60.5809867219938));
#179577=CARTESIAN_POINT('Ctrl Pts',(51.0504688111559,26.404062353457,-60.5806728963985));
#179578=CARTESIAN_POINT('Ctrl Pts',(51.0514736835841,26.4040189565482,-60.5802811765921));
#179579=CARTESIAN_POINT('Ctrl Pts',(51.0528554256585,26.4039591960934,-60.5797383010624));
#179580=CARTESIAN_POINT('Ctrl Pts',(51.0861692753423,26.4025183694385,-60.566649553076));
#179581=CARTESIAN_POINT('Ctrl Pts',(51.1180339754858,26.4011478167948,-60.5520895212465));
#179582=CARTESIAN_POINT('Ctrl Pts',(51.148380750499,26.3998415210777,-60.5363617345489));
#179583=CARTESIAN_POINT('Ctrl Pts',(51.1795224235809,26.3985010084812,-60.5202219769825));
#179584=CARTESIAN_POINT('Ctrl Pts',(51.2090659248564,26.3972281907555,-60.502852974953));
#179585=CARTESIAN_POINT('Ctrl Pts',(51.2369879076331,26.3960210253296,-60.4845643919205));
#179586=CARTESIAN_POINT('Ctrl Pts',(51.2393489032447,26.3959189511934,-60.4830179664884));
#179587=CARTESIAN_POINT('Ctrl Pts',(51.2416983328603,26.3958173488807,-60.481464953118));
#179588=CARTESIAN_POINT('Ctrl Pts',(51.244036197333,26.3957162184661,-60.4799055315775));
#179589=CARTESIAN_POINT('Ctrl Pts',(51.2725006891055,26.3944849127654,-60.4609189127518));
#179590=CARTESIAN_POINT('Ctrl Pts',(51.2992471043443,26.3933232424756,-60.4409847510347));
#179591=CARTESIAN_POINT('Ctrl Pts',(51.3243014907345,26.3922334864741,-60.4204120406075));
#179592=CARTESIAN_POINT('Ctrl Pts',(51.3368286839295,26.3916886084733,-60.4101256853938));
#179593=CARTESIAN_POINT('Ctrl Pts',(51.3489335585763,26.3911617692948,-60.3996792358246));
#179594=CARTESIAN_POINT('Ctrl Pts',(51.360623110838,26.3906535810237,-60.389108443085));
#179595=CARTESIAN_POINT('Ctrl Pts',(51.3660749779834,26.3904165681016,-60.384178351979));
#179596=CARTESIAN_POINT('Ctrl Pts',(51.3711148667758,26.3901960942943,-60.37951815644));
#179597=CARTESIAN_POINT('Ctrl Pts',(51.376199160571,26.3899752512413,-60.3747215662517));
#179598=CARTESIAN_POINT('Ctrl Pts',(51.3811440975544,26.3897604613364,-60.3700564471277));
#179599=CARTESIAN_POINT('Ctrl Pts',(51.3861311904196,26.3895453354251,-60.3652622207859));
#179600=CARTESIAN_POINT('Ctrl Pts',(51.3915473108369,26.3893114302946,-60.359930701075));
#179601=CARTESIAN_POINT('Ctrl Pts',(51.3925026124315,26.3892701738367,-60.3589903214509));
#179602=CARTESIAN_POINT('Ctrl Pts',(51.3934711686472,26.3892283250534,-60.3580331355661));
#179603=CARTESIAN_POINT('Ctrl Pts',(51.394454975483,26.3891857716419,-60.3570567811865));
#179604=CARTESIAN_POINT('Ctrl Pts',(51.4248855109459,26.3878695345018,-60.3268567607239));
#179605=CARTESIAN_POINT('Ctrl Pts',(51.4531160540184,26.3866685076191,-60.2949641541493));
#179606=CARTESIAN_POINT('Ctrl Pts',(51.4790191152461,26.3855715371119,-60.2617220237277));
#179607=CARTESIAN_POINT('Ctrl Pts',(51.5052296625032,26.3844615448578,-60.2280852877958));
#179608=CARTESIAN_POINT('Ctrl Pts',(51.5290572452464,26.3834581030612,-60.1930673111176));
#179609=CARTESIAN_POINT('Ctrl Pts',(51.5504233097089,26.3825543391582,-60.1570220983849));
#179610=CARTESIAN_POINT('Ctrl Pts',(51.5720480957387,26.3816396315826,-60.120540414352));
#179611=CARTESIAN_POINT('Ctrl Pts',(51.5911515653163,26.380827045893,-60.0830069552923));
#179612=CARTESIAN_POINT('Ctrl Pts',(51.6077046707207,26.3801140407432,-60.0447796547702));
#179613=CARTESIAN_POINT('Ctrl Pts',(51.624565766262,26.3793877692879,-60.0058410900331));
#179614=CARTESIAN_POINT('Ctrl Pts',(51.6387809076029,26.3787648357948,-59.9661831063249));
#179615=CARTESIAN_POINT('Ctrl Pts',(51.6503706558839,26.3782470391306,-59.9261671554418));
#179616=CARTESIAN_POINT('Ctrl Pts',(51.662085110263,26.3777236709561,-59.8857206315231));
#179617=CARTESIAN_POINT('Ctrl Pts',(51.6711176986419,26.377307743177,-59.8449088096299));
#179618=CARTESIAN_POINT('Ctrl Pts',(51.6775374166152,26.3770052921258,-59.8040810754937));
#179619=CARTESIAN_POINT('Ctrl Pts',(51.684058954154,26.3766980440672,-59.7626057954429));
#179620=CARTESIAN_POINT('Ctrl Pts',(51.6878844348378,26.3765079317815,-59.7211144794873));
#179621=CARTESIAN_POINT('Ctrl Pts',(51.6891300584881,26.3764451214357,-59.6799427690583));
#179622=CARTESIAN_POINT('Ctrl Pts',(51.6894331426085,26.3764298384741,-59.669924902395));
#179623=CARTESIAN_POINT('Ctrl Pts',(51.6895836746288,26.3764221086262,-59.6599258028449));
#179624=CARTESIAN_POINT('Ctrl Pts',(51.6895836746288,26.3764221086262,-59.64995));
#179625=CARTESIAN_POINT('Origin',(0.,-12.9675000200281,-60.64995));
#179626=CARTESIAN_POINT('',(53.7167487055517,-8.26789346682159,-60.64995));
#179627=CARTESIAN_POINT('Origin',(37.5,-9.33460238845303,-92.34995));
#179628=CARTESIAN_POINT('',(37.5,29.41999998,-91.84995));
#179629=CARTESIAN_POINT('',(37.5,39.429060187817,-59.64995));
#179630=CARTESIAN_POINT('Ctrl Pts',(37.5,37.923330431502,-61.14995));
#179631=CARTESIAN_POINT('Ctrl Pts',(37.5,38.1204655221491,-61.149949999985));
#179632=CARTESIAN_POINT('Ctrl Pts',(37.5,38.3174520230353,-61.1109090094727));
#179633=CARTESIAN_POINT('Ctrl Pts',(37.5,38.6816445026906,-60.9606295880611));
#179634=CARTESIAN_POINT('Ctrl Pts',(37.5,38.8486717246983,-60.8494502533514));
#179635=CARTESIAN_POINT('Ctrl Pts',(37.5,39.1274125809551,-60.5717700902082));
#179636=CARTESIAN_POINT('Ctrl Pts',(37.5,39.239016602691,-60.4053784571342));
#179637=CARTESIAN_POINT('Ctrl Pts',(37.5,39.3898700670183,-60.0425718399611));
#179638=CARTESIAN_POINT('Ctrl Pts',(37.5,39.4290601878028,-59.8463349320561));
#179639=CARTESIAN_POINT('Ctrl Pts',(37.5,39.4290601878171,-59.64995));
#179640=CARTESIAN_POINT('',(37.5,39.4290601878171,-55.74995));
#179641=CARTESIAN_POINT('',(37.5,39.4290601878171,-92.34995));
#179642=CARTESIAN_POINT('',(37.5,43.91999998,-55.74995));
#179643=CARTESIAN_POINT('Origin',(38.,-9.33460238845303,-55.74995));
#179644=CARTESIAN_POINT('',(38.,39.3415715242911,-55.24995));
#179645=CARTESIAN_POINT('Ctrl Pts',(37.5,39.4290601878171,-55.74995));
#179646=CARTESIAN_POINT('Ctrl Pts',(37.5,39.429060187816,-55.7240274876821));
#179647=CARTESIAN_POINT('Ctrl Pts',(37.5021037800324,39.4286870411454,-55.6978059978133));
#179648=CARTESIAN_POINT('Ctrl Pts',(37.5063531399508,39.4279374079327,-55.6716073785487));
#179649=CARTESIAN_POINT('Ctrl Pts',(37.5106395376341,39.4271812408562,-55.6451804099992));
#179650=CARTESIAN_POINT('Ctrl Pts',(37.5171091146894,39.4260419907227,-55.6187767699276));
#179651=CARTESIAN_POINT('Ctrl Pts',(37.5257761108222,39.4245212417519,-55.5927712420142));
#179652=CARTESIAN_POINT('Ctrl Pts',(37.5290201828345,39.423952022717,-55.5830373268288));
#179653=CARTESIAN_POINT('Ctrl Pts',(37.5325718289255,39.4233294053315,-55.573359626286));
#179654=CARTESIAN_POINT('Ctrl Pts',(37.5364307642167,39.4226536524692,-55.5637593428668));
#179655=CARTESIAN_POINT('Ctrl Pts',(37.5465845612258,39.4208755823864,-55.5384986629866));
#179656=CARTESIAN_POINT('Ctrl Pts',(37.5588727550735,39.4187275751124,-55.5137551371743));
#179657=CARTESIAN_POINT('Ctrl Pts',(37.5732950204316,39.4162093248656,-55.489926848832));
#179658=CARTESIAN_POINT('Ctrl Pts',(37.5761937619161,39.4157031799378,-55.4851375840245));
#179659=CARTESIAN_POINT('Ctrl Pts',(37.5791786699961,39.4151820858751,-55.480385454335));
#179660=CARTESIAN_POINT('Ctrl Pts',(37.5822496741218,39.4146460520141,-55.4756739402145));
#179661=CARTESIAN_POINT('Ctrl Pts',(37.5914248426836,39.413044555947,-55.4615974575831));
#179662=CARTESIAN_POINT('Ctrl Pts',(37.6013686732816,39.4113095928738,-55.447883452059));
#179663=CARTESIAN_POINT('Ctrl Pts',(37.6120727310924,39.4094411426509,-55.4346345056758));
#179664=CARTESIAN_POINT('Ctrl Pts',(37.6174247599977,39.4085069175394,-55.4280100324842));
#179665=CARTESIAN_POINT('Ctrl Pts',(37.6229667921261,39.4075393211592,-55.4215019155803));
#179666=CARTESIAN_POINT('Ctrl Pts',(37.6286966355404,39.4065383550014,-55.4151241749086));
#179667=CARTESIAN_POINT('Ctrl Pts',(37.6315615572476,39.4060378719225,-55.4119353045727));
#179668=CARTESIAN_POINT('Ctrl Pts',(37.6344734223788,39.4055290464556,-55.4087790343616));
#179669=CARTESIAN_POINT('Ctrl Pts',(37.6374318784904,39.4050118790486,-55.405657167355));
#179670=CARTESIAN_POINT('Ctrl Pts',(37.6391534315316,39.4047109345394,-55.4038405239988));
#179671=CARTESIAN_POINT('Ctrl Pts',(37.6412508897064,39.4043441565208,-55.4016627141526));
#179672=CARTESIAN_POINT('Ctrl Pts',(37.6430986611541,39.4040209803381,-55.39977793316));
#179673=CARTESIAN_POINT('Ctrl Pts',(37.6444262497453,39.4037887844064,-55.3984237539156));
#179674=CARTESIAN_POINT('Ctrl Pts',(37.6456236044489,39.4035793311953,-55.39721961437));
#179675=CARTESIAN_POINT('Ctrl Pts',(37.6464466082408,39.4034353248945,-55.3963966105727));
#179676=CARTESIAN_POINT('Ctrl Pts',(37.6562264477315,39.401724083074,-55.3866167710176));
#179677=CARTESIAN_POINT('Ctrl Pts',(37.6671430152984,39.3997858357212,-55.3765446165109));
#179678=CARTESIAN_POINT('Ctrl Pts',(37.6793251261276,39.3976147412181,-55.3664154209167));
#179679=CARTESIAN_POINT('Ctrl Pts',(37.6909838912123,39.3955369173381,-55.3567213774471));
#179680=CARTESIAN_POINT('Ctrl Pts',(37.7038025095349,39.3932457018356,-55.3469750520182));
#179681=CARTESIAN_POINT('Ctrl Pts',(37.7178716381578,39.3907398007779,-55.3374234995767));
#179682=CARTESIAN_POINT('Ctrl Pts',(37.7311276745897,39.3883787223767,-55.3284239566384));
#179683=CARTESIAN_POINT('Ctrl Pts',(37.7454943046515,39.3858269816568,-55.3195974073024));
#179684=CARTESIAN_POINT('Ctrl Pts',(37.7610192152964,39.3830883066716,-55.3111870422691));
#179685=CARTESIAN_POINT('Ctrl Pts',(37.7672465764655,39.3819897677719,-55.3078134717654));
#179686=CARTESIAN_POINT('Ctrl Pts',(37.7736599367756,39.3808612138681,-55.3045072863542));
#179687=CARTESIAN_POINT('Ctrl Pts',(37.7802607448068,39.3797031624633,-55.3012859403588));
#179688=CARTESIAN_POINT('Ctrl Pts',(37.7954942140763,39.3770305895897,-55.293851657314));
#179689=CARTESIAN_POINT('Ctrl Pts',(37.8117391205314,39.3742062568083,-55.286861963903));
#179690=CARTESIAN_POINT('Ctrl Pts',(37.8289873345872,39.3712188581417,-55.2805581079215));
#179691=CARTESIAN_POINT('Ctrl Pts',(37.8457634286169,39.3683132308824,-55.2744268017843));
#179692=CARTESIAN_POINT('Ctrl Pts',(37.8634889697662,39.3652532832896,-55.268944278674));
#179693=CARTESIAN_POINT('Ctrl Pts',(37.882119830396,39.3620351392646,-55.2643620188825));
#179694=CARTESIAN_POINT('Ctrl Pts',(37.9001775050072,39.3589160027518,-55.2599207341804));
#179695=CARTESIAN_POINT('Ctrl Pts',(37.9190858710086,39.3556482116274,-55.2563251747639));
#179696=CARTESIAN_POINT('Ctrl Pts',(37.9387660359793,39.3522351790126,-55.2538325278281));
#179697=CARTESIAN_POINT('Ctrl Pts',(37.9584462009501,39.3488221463977,-55.2513398808923));
#179698=CARTESIAN_POINT('Ctrl Pts',(37.9788985693902,39.3452637962159,-55.24995));
#179699=CARTESIAN_POINT('Ctrl Pts',(38.,39.3415715242911,-55.24995));
#179700=CARTESIAN_POINT('',(38.,38.8834059372824,-55.24995));
#179701=CARTESIAN_POINT('Origin',(0.,0.,-55.24995));
#179702=CARTESIAN_POINT('',(38.5,39.2978271925282,-55.24995));
#179703=CARTESIAN_POINT('',(38.5435778713738,39.2940146228024,-55.24995));
#179704=CARTESIAN_POINT('',(38.5,-1.68631645800828E-14,-55.24995));
#179705=CARTESIAN_POINT('Origin',(38.5,-1.68631645800828E-14,-55.74995));
#179706=CARTESIAN_POINT('',(39.,39.2103385290022,-55.74995));
#179707=CARTESIAN_POINT('Ctrl Pts',(38.5,39.2978271925282,-55.24995));
#179708=CARTESIAN_POINT('Ctrl Pts',(38.5215850497934,39.294050298211,-55.24995));
#179709=CARTESIAN_POINT('Ctrl Pts',(38.5424891944466,39.2903925468554,-55.2514041468222));
#179710=CARTESIAN_POINT('Ctrl Pts',(38.562582249786,39.2868767177398,-55.2540052053726));
#179711=CARTESIAN_POINT('Ctrl Pts',(38.5825281794975,39.2833866322734,-55.2565872184188));
#179712=CARTESIAN_POINT('Ctrl Pts',(38.6016753789192,39.2800363064982,-55.2602996172285));
#179713=CARTESIAN_POINT('Ctrl Pts',(38.6199435823765,39.2768397850872,-55.2648742466984));
#179714=CARTESIAN_POINT('Ctrl Pts',(38.6390429090693,39.2734978359541,-55.2696570017704));
#179715=CARTESIAN_POINT('Ctrl Pts',(38.657181623243,39.2703239722319,-55.2753821626628));
#179716=CARTESIAN_POINT('Ctrl Pts',(38.67431472958,39.267326067081,-55.2817780783575));
#179717=CARTESIAN_POINT('Ctrl Pts',(38.6903193474662,39.2645256218228,-55.2877527209421));
#179718=CARTESIAN_POINT('Ctrl Pts',(38.7054472589132,39.261878580314,-55.2943131224831));
#179719=CARTESIAN_POINT('Ctrl Pts',(38.7196931730899,39.2593858683299,-55.3012636512163));
#179720=CARTESIAN_POINT('Ctrl Pts',(38.7362431769865,39.2564899928853,-55.309338336785));
#179721=CARTESIAN_POINT('Ctrl Pts',(38.7516127664062,39.2538006632106,-55.317943762193));
#179722=CARTESIAN_POINT('Ctrl Pts',(38.7658371701146,39.2513117150707,-55.3268178701208));
#179723=CARTESIAN_POINT('Ctrl Pts',(38.7811342644143,39.2486350703984,-55.3363611921875));
#179724=CARTESIAN_POINT('Ctrl Pts',(38.795107859426,39.2461900080939,-55.346215423425));
#179725=CARTESIAN_POINT('Ctrl Pts',(38.8078412626453,39.2439619512343,-55.3561026478009));
#179726=CARTESIAN_POINT('Ctrl Pts',(38.820796298757,39.2416951136435,-55.3661619655362));
#179727=CARTESIAN_POINT('Ctrl Pts',(38.8324678161029,39.2396528627357,-55.3762552368417));
#179728=CARTESIAN_POINT('Ctrl Pts',(38.8429723612382,39.237814805506,-55.3861352302201));
#179729=CARTESIAN_POINT('Ctrl Pts',(38.844508436647,39.2375460271368,-55.3875799776767));
#179730=CARTESIAN_POINT('Ctrl Pts',(38.8460195962369,39.2372816084711,-55.3890202398763));
#179731=CARTESIAN_POINT('Ctrl Pts',(38.8475062515775,39.2370214774933,-55.3904553319087));
#179732=CARTESIAN_POINT('Ctrl Pts',(38.8487711127112,39.236800155473,-55.3916763224674));
#179733=CARTESIAN_POINT('Ctrl Pts',(38.8496069371356,39.2366539051479,-55.3924916493941));
#179734=CARTESIAN_POINT('Ctrl Pts',(38.8507725352525,39.2364499420131,-55.3936383710039));
#179735=CARTESIAN_POINT('Ctrl Pts',(38.8515075974215,39.2363213165615,-55.3943615290645));
#179736=CARTESIAN_POINT('Ctrl Pts',(38.8523735525978,39.2361697838677,-55.3952167714236));
#179737=CARTESIAN_POINT('Ctrl Pts',(38.8535533887318,39.2359633227174,-55.3963966075452));
#179738=CARTESIAN_POINT('Ctrl Pts',(38.8741274018139,39.2323630478275,-55.4169706204106));
#179739=CARTESIAN_POINT('Ctrl Pts',(38.8925747282859,39.2291350207311,-55.4391630479274));
#179740=CARTESIAN_POINT('Ctrl Pts',(38.9088523573029,39.2262867255737,-55.4624843710786));
#179741=CARTESIAN_POINT('Ctrl Pts',(38.9251500795738,39.2234349144546,-55.4858344822839));
#179742=CARTESIAN_POINT('Ctrl Pts',(38.9392727637231,39.2209637700076,-55.5103162636118));
#179743=CARTESIAN_POINT('Ctrl Pts',(38.9512005223542,39.2188767318635,-55.5354850657774));
#179744=CARTESIAN_POINT('Ctrl Pts',(38.9631486411807,39.2167861312309,-55.5606968300573));
#179745=CARTESIAN_POINT('Ctrl Pts',(38.9728943609641,39.2150809447883,-55.5865979625573));
#179746=CARTESIAN_POINT('Ctrl Pts',(38.9804407021853,39.2137606048068,-55.6127884619919));
#179747=CARTESIAN_POINT('Ctrl Pts',(38.9880210340836,39.2124343176718,-55.6390969302251));
#179748=CARTESIAN_POINT('Ctrl Pts',(38.9933821545229,39.2114963473967,-55.6656973743602));
#179749=CARTESIAN_POINT('Ctrl Pts',(38.9965499548298,39.2109421244155,-55.6922317373016));
#179750=CARTESIAN_POINT('Ctrl Pts',(38.9988557843579,39.2105387076621,-55.7115459969304));
#179751=CARTESIAN_POINT('Ctrl Pts',(39.,39.2103385290022,-55.7308262353698));
#179752=CARTESIAN_POINT('Ctrl Pts',(39.,39.2103385290022,-55.74995));
#179753=CARTESIAN_POINT('',(39.,46.91999998,-55.74995));
#179754=CARTESIAN_POINT('Origin',(39.,46.91999998,-129.34995));
#179755=CARTESIAN_POINT('',(39.,39.2103385290022,-59.64995));
#179756=CARTESIAN_POINT('',(39.,39.2103385290022,-59.64995));
#179757=CARTESIAN_POINT('Ctrl Pts',(39.,39.2103385290022,-59.64995));
#179758=CARTESIAN_POINT('Ctrl Pts',(39.,39.2103385289879,-59.8463349320561));
#179759=CARTESIAN_POINT('Ctrl Pts',(39.,39.1711484082035,-60.0425718399611));
#179760=CARTESIAN_POINT('Ctrl Pts',(39.,39.0957216760398,-60.2239751485477));
#179761=CARTESIAN_POINT('Ctrl Pts',(39.,39.0202949438762,-60.4053784571342));
#179762=CARTESIAN_POINT('Ctrl Pts',(39.,38.9086909221403,-60.5717700902082));
#179763=CARTESIAN_POINT('Ctrl Pts',(39.,38.7693204940119,-60.7106101717798));
#179764=CARTESIAN_POINT('Ctrl Pts',(39.,38.6299500658835,-60.8494502533514));
#179765=CARTESIAN_POINT('Ctrl Pts',(39.,38.4629228438757,-60.9606295880618));
#179766=CARTESIAN_POINT('Ctrl Pts',(39.,38.2808266040481,-61.0357692987669));
#179767=CARTESIAN_POINT('Ctrl Pts',(39.,38.0987303642205,-61.110909009472));
#179768=CARTESIAN_POINT('Ctrl Pts',(39.,37.9017438633342,-61.149949999985));
#179769=CARTESIAN_POINT('Ctrl Pts',(39.,37.7046087726872,-61.14995));
#179770=CARTESIAN_POINT('Ctrl Pts',(39.5,37.7046087726872,-60.64995));
#179771=CARTESIAN_POINT('Ctrl Pts',(39.,37.7046087726872,-60.64995));
#179772=CARTESIAN_POINT('Ctrl Pts',(39.,37.7046087726872,-61.14995));
#179773=CARTESIAN_POINT('Ctrl Pts',(39.4942946417934,37.8365313206165,-60.64995));
#179774=CARTESIAN_POINT('Ctrl Pts',(38.9999999999973,37.8357552425198,-60.655621796981));
#179775=CARTESIAN_POINT('Ctrl Pts',(39.,37.9017438633342,-61.149949999985));
#179776=CARTESIAN_POINT('Ctrl Pts',(39.4885935839755,37.9683544324696,-60.6239226729818));
#179777=CARTESIAN_POINT('Ctrl Pts',(39.,37.9700367301949,-60.6353187454024));
#179778=CARTESIAN_POINT('Ctrl Pts',(39.,38.0987303642205,-61.110909009472));
#179779=CARTESIAN_POINT('Ctrl Pts',(39.4780533572395,38.2120715692569,-60.5237363920407));
#179780=CARTESIAN_POINT('Ctrl Pts',(39.,38.2214119490388,-60.5426326522478));
#179781=CARTESIAN_POINT('Ctrl Pts',(39.,38.4629228438758,-60.9606295880618));
#179782=CARTESIAN_POINT('Ctrl Pts',(39.4732193617859,38.3238459703974,-60.4496168355678));
#179783=CARTESIAN_POINT('Ctrl Pts',(39.,38.3387190323947,-60.4706504746467));
#179784=CARTESIAN_POINT('Ctrl Pts',(39.,38.6299500658835,-60.8494502533514));
#179785=CARTESIAN_POINT('Ctrl Pts',(39.4651522214979,38.5103789912237,-60.2644967268053));
#179786=CARTESIAN_POINT('Ctrl Pts',(39.,38.5356496464585,-60.2852157712116));
#179787=CARTESIAN_POINT('Ctrl Pts',(39.,38.9086909221403,-60.5717700902082));
#179788=CARTESIAN_POINT('Ctrl Pts',(39.4619222489988,38.5850642583582,-60.153568971423));
#179789=CARTESIAN_POINT('Ctrl Pts',(39.,38.6156677780068,-60.1718710142637));
#179790=CARTESIAN_POINT('Ctrl Pts',(39.,39.0202949438762,-60.4053784571342));
#179791=CARTESIAN_POINT('Ctrl Pts',(39.4575563441359,38.6860152017583,-59.9116978933072));
#179792=CARTESIAN_POINT('Ctrl Pts',(39.,38.7237795941064,-59.9224177216067));
#179793=CARTESIAN_POINT('Ctrl Pts',(39.,39.1711484082035,-60.0425718399611));
#179794=CARTESIAN_POINT('Ctrl Pts',(39.4564221286291,38.7122411799561,-59.7808732880376));
#179795=CARTESIAN_POINT('Ctrl Pts',(39.,38.7521729419779,-59.7861314644994));
#179796=CARTESIAN_POINT('Ctrl Pts',(39.,39.2103385289879,-59.8463349320561));
#179797=CARTESIAN_POINT('Ctrl Pts',(39.4564221286262,38.7122411799564,-59.64995));
#179798=CARTESIAN_POINT('Ctrl Pts',(39.,38.7521729419935,-59.64995));
#179799=CARTESIAN_POINT('Ctrl Pts',(39.,39.2103385290023,-59.64995));
#179800=CARTESIAN_POINT('',(39.4564221286262,38.7122411799564,-59.64995));
#179801=CARTESIAN_POINT('Origin',(39.5,39.2103385290022,-59.64995));
#179802=CARTESIAN_POINT('Ctrl Pts',(39.5,37.7046087726872,-60.64995));
#179803=CARTESIAN_POINT('Ctrl Pts',(39.4987807152437,37.7328017705422,-60.64995));
#179804=CARTESIAN_POINT('Ctrl Pts',(39.4976123687796,37.7598169441407,-60.6487640562912));
#179805=CARTESIAN_POINT('Ctrl Pts',(39.4964981291842,37.7855810278475,-60.646690542373));
#179806=CARTESIAN_POINT('Ctrl Pts',(39.4953259634005,37.8126845139321,-60.6445092322876));
#179807=CARTESIAN_POINT('Ctrl Pts',(39.4942136614223,37.8384037949514,-60.6413458429473));
#179808=CARTESIAN_POINT('Ctrl Pts',(39.4931629359066,37.8626992698647,-60.6375094924559));
#179809=CARTESIAN_POINT('Ctrl Pts',(39.4922295881091,37.8842806702054,-60.6341017049524));
#179810=CARTESIAN_POINT('Ctrl Pts',(39.4913447855216,37.9047395805,-60.6301623057276));
#179811=CARTESIAN_POINT('Ctrl Pts',(39.4905086923334,37.9240722042669,-60.6258833727946));
#179812=CARTESIAN_POINT('Ctrl Pts',(39.4895023952214,37.9473403802787,-60.6207333752658));
#179813=CARTESIAN_POINT('Ctrl Pts',(39.4885666220187,37.9689778622202,-60.6150923633976));
#179814=CARTESIAN_POINT('Ctrl Pts',(39.487700290685,37.9890096696409,-60.6092528148745));
#179815=CARTESIAN_POINT('Ctrl Pts',(39.4867980067401,38.0098727938541,-60.603170926025));
#179816=CARTESIAN_POINT('Ctrl Pts',(39.485971010137,38.0289950811894,-60.5968737820667));
#179817=CARTESIAN_POINT('Ctrl Pts',(39.4852169994621,38.0464297462502,-60.590641719909));
#179818=CARTESIAN_POINT('Ctrl Pts',(39.4848927496207,38.053927236097,-60.5879617244752));
#179819=CARTESIAN_POINT('Ctrl Pts',(39.4845819891505,38.0611128170089,-60.5852931620339));
#179820=CARTESIAN_POINT('Ctrl Pts',(39.4842844922117,38.0679917109782,-60.5826554871209));
#179821=CARTESIAN_POINT('Ctrl Pts',(39.4842090737884,38.0697355787937,-60.5819868103817));
#179822=CARTESIAN_POINT('Ctrl Pts',(39.4841737017427,38.0705524413637,-60.5816714634972));
#179823=CARTESIAN_POINT('Ctrl Pts',(39.4840978736734,38.0723051722649,-60.5809901111847));
#179824=CARTESIAN_POINT('Ctrl Pts',(39.4840628676318,38.0731143207956,-60.580675564769));
#179825=CARTESIAN_POINT('Ctrl Pts',(39.4840192449618,38.0741227976636,-60.5802826897657));
#179826=CARTESIAN_POINT('Ctrl Pts',(39.4839591488405,38.0755124154886,-60.5797369933149));
#179827=CARTESIAN_POINT('Ctrl Pts',(39.4837458556873,38.0804444470589,-60.5778002074773));
#179828=CARTESIAN_POINT('Ctrl Pts',(39.4835339342671,38.0853447503636,-60.575830756519));
#179829=CARTESIAN_POINT('Ctrl Pts',(39.4833233986077,38.0902130017798,-60.5738295347324));
#179830=CARTESIAN_POINT('Ctrl Pts',(39.4818941408137,38.1232619698137,-60.5602438939751));
#179831=CARTESIAN_POINT('Ctrl Pts',(39.4805292639958,38.154821844994,-60.5452002165668));
#179832=CARTESIAN_POINT('Ctrl Pts',(39.4792308551495,38.1848445976366,-60.5290286709037));
#179833=CARTESIAN_POINT('Ctrl Pts',(39.4779906264952,38.2135220656132,-60.5135817534141));
#179834=CARTESIAN_POINT('Ctrl Pts',(39.4768110201833,38.2407975955461,-60.49710534447));
#179835=CARTESIAN_POINT('Ctrl Pts',(39.4756925305597,38.2666599508293,-60.4798551182117));
#179836=CARTESIAN_POINT('Ctrl Pts',(39.4744365387292,38.2957017105978,-60.4604842248241));
#179837=CARTESIAN_POINT('Ctrl Pts',(39.4732575807838,38.322962248921,-60.4401373910195));
#179838=CARTESIAN_POINT('Ctrl Pts',(39.4721546419679,38.3484650295551,-60.4191325971816));
#179839=CARTESIAN_POINT('Ctrl Pts',(39.4716361344536,38.3604542561586,-60.4092579393278));
#179840=CARTESIAN_POINT('Ctrl Pts',(39.4711344064957,38.3720554962878,-60.3992372749932));
#179841=CARTESIAN_POINT('Ctrl Pts',(39.470649247717,38.383273614397,-60.3891007234335));
#179842=CARTESIAN_POINT('Ctrl Pts',(39.4704139561111,38.3887141611663,-60.3841847132522));
#179843=CARTESIAN_POINT('Ctrl Pts',(39.4701964148523,38.393744274237,-60.3795368119607));
#179844=CARTESIAN_POINT('Ctrl Pts',(39.4699770120232,38.3988172777583,-60.3747537948934));
#179845=CARTESIAN_POINT('Ctrl Pts',(39.4697641308945,38.403739487377,-60.3701129519459));
#179846=CARTESIAN_POINT('Ctrl Pts',(39.4695494906704,38.4087022269652,-60.3653448270166));
#179847=CARTESIAN_POINT('Ctrl Pts',(39.4693166057594,38.4140865458396,-60.3600469439559));
#179848=CARTESIAN_POINT('Ctrl Pts',(39.4692736283864,38.4150801863462,-60.3590692546082));
#179849=CARTESIAN_POINT('Ctrl Pts',(39.4692300340461,38.4160880830258,-60.3580734248406));
#179850=CARTESIAN_POINT('Ctrl Pts',(39.4691857254875,38.4171124836934,-60.3570567840804));
#179851=CARTESIAN_POINT('Ctrl Pts',(39.4677127419675,38.4511674236831,-60.3232598126683));
#179852=CARTESIAN_POINT('Ctrl Pts',(39.4663603950896,38.4824360653392,-60.2873222682081));
#179853=CARTESIAN_POINT('Ctrl Pts',(39.4651340689026,38.5107922339571,-60.2497596524454));
#179854=CARTESIAN_POINT('Ctrl Pts',(39.4638892540765,38.5395759127878,-60.2116307259771));
#179855=CARTESIAN_POINT('Ctrl Pts',(39.4627742871156,38.5653586693248,-60.1718273254161));
#179856=CARTESIAN_POINT('Ctrl Pts',(39.4617936459168,38.5880352467008,-60.1308415639801));
#179857=CARTESIAN_POINT('Ctrl Pts',(39.4610260198971,38.6057860110494,-60.0987587420958));
#179858=CARTESIAN_POINT('Ctrl Pts',(39.4603406775651,38.6216340299095,-60.0659504750838));
#179859=CARTESIAN_POINT('Ctrl Pts',(39.4597392952827,38.6355397301541,-60.0326334324049));
#179860=CARTESIAN_POINT('Ctrl Pts',(39.459679534421,38.636921574372,-60.0293226345325));
#179861=CARTESIAN_POINT('Ctrl Pts',(39.4596206036131,38.6382842162723,-60.0260068880544));
#179862=CARTESIAN_POINT('Ctrl Pts',(39.4595625010567,38.6396276967345,-60.0226864255211));
#179863=CARTESIAN_POINT('Ctrl Pts',(39.4588033987318,38.6571800938303,-59.9793050153962));
#179864=CARTESIAN_POINT('Ctrl Pts',(39.4581857740029,38.6714611652261,-59.9351228139635));
#179865=CARTESIAN_POINT('Ctrl Pts',(39.4577055602589,38.6825649414251,-59.8906338465719));
#179866=CARTESIAN_POINT('Ctrl Pts',(39.4572195296836,38.6938032177146,-59.8456059841206));
#179867=CARTESIAN_POINT('Ctrl Pts',(39.4568742584516,38.701786776151,-59.8002638465307));
#179868=CARTESIAN_POINT('Ctrl Pts',(39.4566651706717,38.7066214231023,-59.7550665512749));
#179869=CARTESIAN_POINT('Ctrl Pts',(39.4565023749363,38.7103856789864,-59.7198759393599));
#179870=CARTESIAN_POINT('Ctrl Pts',(39.4564221286262,38.7122411799564,-59.6847720500554));
#179871=CARTESIAN_POINT('Ctrl Pts',(39.4564221286262,38.7122411799564,-59.64995));
#179872=CARTESIAN_POINT('Ctrl Pts',(29.,38.7048160259599,-61.150138786574));
#179873=CARTESIAN_POINT('Ctrl Pts',(29.,38.6926240909195,-60.6436056187277));
#179874=CARTESIAN_POINT('Ctrl Pts',(28.4933647440612,38.6927858841383,-60.650327573148));
#179875=CARTESIAN_POINT('Ctrl Pts',(29.,38.8968977730653,-61.1455154974199));
#179876=CARTESIAN_POINT('Ctrl Pts',(29.0000000000007,38.8211017330502,-60.6340675708554));
#179877=CARTESIAN_POINT('Ctrl Pts',(28.4870505338491,38.8213938162437,-60.647315885492));
#179878=CARTESIAN_POINT('Ctrl Pts',(29.,39.0908916037092,-61.103090199825));
#179879=CARTESIAN_POINT('Ctrl Pts',(28.9999999999993,38.9470356871939,-60.5993042062512));
#179880=CARTESIAN_POINT('Ctrl Pts',(28.4808526630789,38.9512642676271,-60.6191174333591));
#179881=CARTESIAN_POINT('Ctrl Pts',(29.,39.4441857876827,-60.9504725910835));
#179882=CARTESIAN_POINT('Ctrl Pts',(29.0000000000007,39.1728401027082,-60.4895768580073));
#179883=CARTESIAN_POINT('Ctrl Pts',(28.4702284641343,39.1877232210837,-60.5175376561534));
#179884=CARTESIAN_POINT('Ctrl Pts',(29.,39.6084483440092,-60.8383643971029));
#179885=CARTESIAN_POINT('Ctrl Pts',(29.0000000000007,39.2753871003781,-60.4130391624567));
#179886=CARTESIAN_POINT('Ctrl Pts',(28.465656656414,39.2976315760154,-60.4428805969007));
#179887=CARTESIAN_POINT('Ctrl Pts',(29.,39.8127532432739,-60.6300880930806));
#179888=CARTESIAN_POINT('Ctrl Pts',(28.9999999999996,39.4020840949312,-60.2760820218603));
#179889=CARTESIAN_POINT('Ctrl Pts',(28.4606134496588,39.434276061177,-60.3041245704241));
#179890=CARTESIAN_POINT('Ctrl Pts',(29.,39.8731969861748,-60.5550848424531));
#179891=CARTESIAN_POINT('Ctrl Pts',(29.,39.439411822071,-60.2273142826608));
#179892=CARTESIAN_POINT('Ctrl Pts',(28.4592438293891,39.4746917169037,-60.2541491598715));
#179893=CARTESIAN_POINT('Ctrl Pts',(29.,39.9791737873547,-60.3942177709194));
#179894=CARTESIAN_POINT('Ctrl Pts',(29.,39.5049075987374,-60.1236050817051));
#179895=CARTESIAN_POINT('Ctrl Pts',(28.4570887248156,39.5455314661108,-60.1469471546371));
#179896=CARTESIAN_POINT('Ctrl Pts',(29.,40.025042572592,-60.3073218018945));
#179897=CARTESIAN_POINT('Ctrl Pts',(29.0000000000002,39.5332188379146,-60.0680634823705));
#179898=CARTESIAN_POINT('Ctrl Pts',(28.4563005932054,39.5761796095201,-60.0890325252997));
#179899=CARTESIAN_POINT('Ctrl Pts',(29.,40.1347632142717,-60.0389178342029));
#179900=CARTESIAN_POINT('Ctrl Pts',(28.9999999999997,39.6014080499751,-59.8970923098554));
#179901=CARTESIAN_POINT('Ctrl Pts',(28.4548707416055,39.6494517959669,-59.9101257001469));
#179902=CARTESIAN_POINT('Ctrl Pts',(29.,40.1727138319509,-59.8469756744913));
#179903=CARTESIAN_POINT('Ctrl Pts',(29.,39.6256255569264,-59.7761492712348));
#179904=CARTESIAN_POINT('Ctrl Pts',(28.4551199545093,39.6747304042147,-59.7821590925224));
#179905=CARTESIAN_POINT('Ctrl Pts',(29.,40.1727138277874,-59.6524466674074));
#179906=CARTESIAN_POINT('Ctrl Pts',(29.,39.6270595772528,-59.6524466674074));
#179907=CARTESIAN_POINT('Ctrl Pts',(28.4564221286262,39.6746164787415,-59.6524466674074));
#179908=CARTESIAN_POINT('',(28.4564221286262,39.6746164787415,-59.6524466674074));
#179909=CARTESIAN_POINT('',(29.,40.1727138277873,-59.6524466674074));
#179910=CARTESIAN_POINT('Origin',(28.5,40.1727138277873,-59.6524466674074));
#179911=CARTESIAN_POINT('Ctrl Pts',(29.,38.7048160259599,-61.150138786574));
#179912=CARTESIAN_POINT('Ctrl Pts',(29.,38.7587438294331,-61.1488407776135));
#179913=CARTESIAN_POINT('Ctrl Pts',(29.0000000000001,38.8125135208639,-61.1445744929232));
#179914=CARTESIAN_POINT('Ctrl Pts',(28.9999999999995,38.8658121354595,-61.1374999313474));
#179915=CARTESIAN_POINT('Ctrl Pts',(28.999999999999,38.9206199981761,-61.1302250405726));
#179916=CARTESIAN_POINT('Ctrl Pts',(28.9999999999976,38.9749308760973,-61.1199805166189));
#179917=CARTESIAN_POINT('Ctrl Pts',(28.9999999999961,39.0284204191816,-61.1068862346652));
#179918=CARTESIAN_POINT('Ctrl Pts',(28.9999999999946,39.0824266406294,-61.0936654694443));
#179919=CARTESIAN_POINT('Ctrl Pts',(28.9999999999932,39.1355968678683,-61.0775394193002));
#179920=CARTESIAN_POINT('Ctrl Pts',(28.9999999999937,39.1875946577396,-61.0585793760252));
#179921=CARTESIAN_POINT('Ctrl Pts',(28.999999999994,39.2145745592176,-61.0487416482901));
#179922=CARTESIAN_POINT('Ctrl Pts',(28.9999999999949,39.2412386526435,-61.038140115953));
#179923=CARTESIAN_POINT('Ctrl Pts',(28.999999999996,39.2675379042626,-61.0267795633668));
#179924=CARTESIAN_POINT('Ctrl Pts',(28.999999999996,39.2679181300168,-61.02661531631));
#179925=CARTESIAN_POINT('Ctrl Pts',(28.9999999999961,39.268298302465,-61.0264509016639));
#179926=CARTESIAN_POINT('Ctrl Pts',(28.9999999999961,39.268678421493,-61.0262863194886));
#179927=CARTESIAN_POINT('Ctrl Pts',(29.0000000000039,39.4448840602191,-60.9499936185261));
#179928=CARTESIAN_POINT('Ctrl Pts',(29.,39.6087415856579,-60.8380654560188));
#179929=CARTESIAN_POINT('Ctrl Pts',(29.,39.7446514854509,-60.6995134053984));
#179930=CARTESIAN_POINT('Ctrl Pts',(29.,39.744751813756,-60.6994111266649));
#179931=CARTESIAN_POINT('Ctrl Pts',(29.,39.7448521254371,-60.6993088358292));
#179932=CARTESIAN_POINT('Ctrl Pts',(29.,39.7449524204946,-60.6992065328918));
#179933=CARTESIAN_POINT('Ctrl Pts',(28.9999999999999,39.812931097784,-60.6298669408688));
#179934=CARTESIAN_POINT('Ctrl Pts',(29.,39.8732750955302,-60.554966232983));
#179935=CARTESIAN_POINT('Ctrl Pts',(29.,39.9261853767363,-60.4746513000797));
#179936=CARTESIAN_POINT('Ctrl Pts',(29.,39.9261884127568,-60.4746466915656));
#179937=CARTESIAN_POINT('Ctrl Pts',(29.,39.9261914487538,-60.4746420830304));
#179938=CARTESIAN_POINT('Ctrl Pts',(29.,39.9261944847274,-60.4746374744739));
#179939=CARTESIAN_POINT('Ctrl Pts',(29.,39.9791069872139,-60.3943171935884));
#179940=CARTESIAN_POINT('Ctrl Pts',(29.0000000000001,40.0249202649622,-60.3075521828599));
#179941=CARTESIAN_POINT('Ctrl Pts',(28.9999999999999,40.0614666645048,-60.2182183202257));
#179942=CARTESIAN_POINT('Ctrl Pts',(28.9999999999999,40.0615163877946,-60.218096776829));
#179943=CARTESIAN_POINT('Ctrl Pts',(28.9999999999999,40.0615660940304,-60.2179752284374));
#179944=CARTESIAN_POINT('Ctrl Pts',(28.9999999999999,40.0616157832065,-60.2178536750606));
#179945=CARTESIAN_POINT('Ctrl Pts',(28.9999999999996,40.0995205469998,-60.1251282086845));
#179946=CARTESIAN_POINT('Ctrl Pts',(28.9999999999997,40.128027334411,-60.0287688634757));
#179947=CARTESIAN_POINT('Ctrl Pts',(28.9999999999998,40.1466650082863,-59.9302710126543));
#179948=CARTESIAN_POINT('Ctrl Pts',(29.,40.1639177847725,-59.8390921769278));
#179949=CARTESIAN_POINT('Ctrl Pts',(29.,40.1727138277874,-59.7460820250092));
#179950=CARTESIAN_POINT('Ctrl Pts',(29.,40.1727138277873,-59.6524466674074));
#179951=CARTESIAN_POINT('Ctrl Pts',(28.4564221286157,39.6746164786217,-59.6524466674074));
#179952=CARTESIAN_POINT('Ctrl Pts',(28.4560930610391,39.6746447582207,-59.6852214163602));
#179953=CARTESIAN_POINT('Ctrl Pts',(28.4558631142718,39.6730442805713,-59.7182876085465));
#179954=CARTESIAN_POINT('Ctrl Pts',(28.4557164536146,39.6697525629344,-59.7513995669006));
#179955=CARTESIAN_POINT('Ctrl Pts',(28.4555706011372,39.6664789844466,-59.7843290604097));
#179956=CARTESIAN_POINT('Ctrl Pts',(28.4555070608883,39.6615324787802,-59.8173029960901));
#179957=CARTESIAN_POINT('Ctrl Pts',(28.455514149446,39.6549009331809,-59.8500663155775));
#179958=CARTESIAN_POINT('Ctrl Pts',(28.4555212161303,39.6482898508114,-59.8827285359583));
#179959=CARTESIAN_POINT('Ctrl Pts',(28.4555984368539,39.6400040729076,-59.9151805618179));
#179960=CARTESIAN_POINT('Ctrl Pts',(28.4557388532419,39.6300831646837,-59.9471690591856));
#179961=CARTESIAN_POINT('Ctrl Pts',(28.4558640822193,39.6212353000596,-59.9756976865905));
#179962=CARTESIAN_POINT('Ctrl Pts',(28.4560396318297,39.6110877023737,-60.0038572147082));
#179963=CARTESIAN_POINT('Ctrl Pts',(28.4562639562526,39.5997023822614,-60.0314760384073));
#179964=CARTESIAN_POINT('Ctrl Pts',(28.4565164554916,39.5868870827672,-60.0625637455503));
#179965=CARTESIAN_POINT('Ctrl Pts',(28.4568306655563,39.5725031725775,-60.0929653078116));
#179966=CARTESIAN_POINT('Ctrl Pts',(28.4572093049085,39.5566832670391,-60.1224589103904));
#179967=CARTESIAN_POINT('Ctrl Pts',(28.4575668544929,39.5417445116846,-60.1503097538976));
#179968=CARTESIAN_POINT('Ctrl Pts',(28.4579819214458,39.525526105916,-60.1773507351382));
#179969=CARTESIAN_POINT('Ctrl Pts',(28.4584608345725,39.5081717079878,-60.2034231684565));
#179970=CARTESIAN_POINT('Ctrl Pts',(28.4589538718475,39.4903054926235,-60.2302645322804));
#179971=CARTESIAN_POINT('Ctrl Pts',(28.4595146018092,39.4712358021277,-60.2560788724074));
#179972=CARTESIAN_POINT('Ctrl Pts',(28.4601537361126,39.4511448059234,-60.280729779171));
#179973=CARTESIAN_POINT('Ctrl Pts',(28.4604733032643,39.4410993078213,-60.2930552325527));
#179974=CARTESIAN_POINT('Ctrl Pts',(28.4608125277711,39.4307988255083,-60.3050904439814));
#179975=CARTESIAN_POINT('Ctrl Pts',(28.4611730509995,39.4202677347106,-60.3168221741449));
#179976=CARTESIAN_POINT('Ctrl Pts',(28.4613533126137,39.4150021893117,-60.3226880392267));
#179977=CARTESIAN_POINT('Ctrl Pts',(28.4615389017733,39.4096790191687,-60.3284780588577));
#179978=CARTESIAN_POINT('Ctrl Pts',(28.4617300396149,39.4043013196553,-60.3341908410452));
#179979=CARTESIAN_POINT('Ctrl Pts',(28.4618256085357,39.4016124698986,-60.337047232139));
#179980=CARTESIAN_POINT('Ctrl Pts',(28.461922564793,39.3989099893976,-60.3398843152446));
#179981=CARTESIAN_POINT('Ctrl Pts',(28.4620209369187,39.3961942701274,-60.3427019292839));
#179982=CARTESIAN_POINT('Ctrl Pts',(28.4620916599414,39.3942418484026,-60.3447276065778));
#179983=CARTESIAN_POINT('Ctrl Pts',(28.4621842200406,39.3917236897839,-60.347315551478));
#179984=CARTESIAN_POINT('Ctrl Pts',(28.4622529756521,39.3898442388991,-60.3492302412195));
#179985=CARTESIAN_POINT('Ctrl Pts',(28.4622798555975,39.3891094692389,-60.3499787874795));
#179986=CARTESIAN_POINT('Ctrl Pts',(28.4623031592114,39.3884728476581,-60.3506249265858));
#179987=CARTESIAN_POINT('Ctrl Pts',(28.4623203300338,39.3880077918452,-60.3510962110302));
#179988=CARTESIAN_POINT('Ctrl Pts',(28.4627572830568,39.376173324127,-60.3630891813141));
#179989=CARTESIAN_POINT('Ctrl Pts',(28.4633159972543,39.3629930253315,-60.3758362809693));
#179990=CARTESIAN_POINT('Ctrl Pts',(28.4639775759014,39.348327220407,-60.389138830442));
#179991=CARTESIAN_POINT('Ctrl Pts',(28.4646091527633,39.3343264918589,-60.4018381255111));
#179992=CARTESIAN_POINT('Ctrl Pts',(28.4653343723215,39.3189710193108,-60.4150435155025));
#179993=CARTESIAN_POINT('Ctrl Pts',(28.4661368014099,39.3021490027413,-60.4285362299288));
#179994=CARTESIAN_POINT('Ctrl Pts',(28.466917321566,39.2857862821131,-60.4416605492256));
#179995=CARTESIAN_POINT('Ctrl Pts',(28.4677707873882,39.2680350960101,-60.455056495446));
#179996=CARTESIAN_POINT('Ctrl Pts',(28.4686835930123,39.2488152070403,-60.4684805223839));
#179997=CARTESIAN_POINT('Ctrl Pts',(28.4695604420901,39.2303524133495,-60.4813757602411));
#179998=CARTESIAN_POINT('Ctrl Pts',(28.4704919580951,39.2105336346547,-60.4942963815287));
#179999=CARTESIAN_POINT('Ctrl Pts',(28.4714689033925,39.1893205542289,-60.5069926037893));
#180000=CARTESIAN_POINT('Ctrl Pts',(28.4722342090465,39.1727029499133,-60.516938391652));
#180001=CARTESIAN_POINT('Ctrl Pts',(28.4730274301954,39.1552302186206,-60.5267456851722));
#180002=CARTESIAN_POINT('Ctrl Pts',(28.4738459588635,39.1369030987336,-60.5362827351625));
#180003=CARTESIAN_POINT('Ctrl Pts',(28.4748434548321,39.1145688434842,-60.5479050146109));
#180004=CARTESIAN_POINT('Ctrl Pts',(28.4758783442967,39.0909640246873,-60.5591258135412));
#180005=CARTESIAN_POINT('Ctrl Pts',(28.4769502258775,39.0661321619779,-60.5696935979207));
#180006=CARTESIAN_POINT('Ctrl Pts',(28.4779986229512,39.0418443556902,-60.5800298462685));
#180007=CARTESIAN_POINT('Ctrl Pts',(28.4790823682872,39.0163824910683,-60.5897405006454));
#180008=CARTESIAN_POINT('Ctrl Pts',(28.4802064426117,38.9898368116951,-60.598587708987));
#180009=CARTESIAN_POINT('Ctrl Pts',(28.4813019955003,38.9639646828817,-60.6072104347661));
#180010=CARTESIAN_POINT('Ctrl Pts',(28.4824358508781,38.9370631630029,-60.6150121023343));
#180011=CARTESIAN_POINT('Ctrl Pts',(28.483618096623,38.9092638074563,-60.6217829758405));
#180012=CARTESIAN_POINT('Ctrl Pts',(28.4847852969212,38.8818182309136,-60.6284676821375));
#180013=CARTESIAN_POINT('Ctrl Pts',(28.4859996780555,38.8534978249802,-60.6341468182533));
#180014=CARTESIAN_POINT('Ctrl Pts',(28.487276309583,38.8244736151779,-60.6386416291119));
#180015=CARTESIAN_POINT('Ctrl Pts',(28.488536054244,38.7958333281812,-60.6430769840745));
#180016=CARTESIAN_POINT('Ctrl Pts',(28.4898564588711,38.7665082903692,-60.6463584329082));
#180017=CARTESIAN_POINT('Ctrl Pts',(28.4912568106162,38.7366999833481,-60.6483483554661));
#180018=CARTESIAN_POINT('Ctrl Pts',(28.4919395182101,38.7221676648519,-60.6493184940377));
#180019=CARTESIAN_POINT('Ctrl Pts',(28.4926412967995,38.7075209967316,-60.6499822472411));
#180020=CARTESIAN_POINT('Ctrl Pts',(28.493364741833,38.6927858841118,-60.6503273734803));
#180021=CARTESIAN_POINT('Origin',(29.,-9.33460238845303,-92.34995));
#180022=CARTESIAN_POINT('',(29.,40.1727138277873,-55.74995));
#180023=CARTESIAN_POINT('',(29.,40.1727138277874,-92.34995));
#180024=CARTESIAN_POINT('',(29.,43.91999998,-55.74995));
#180025=CARTESIAN_POINT('',(29.,29.41999998,-91.84995));
#180026=CARTESIAN_POINT('Origin',(29.5,-9.33460238845303,-55.74995));
#180027=CARTESIAN_POINT('',(29.5,40.0852251642615,-55.24995));
#180028=CARTESIAN_POINT('Ctrl Pts',(29.,40.1727138277873,-55.74995));
#180029=CARTESIAN_POINT('Ctrl Pts',(29.,40.1727138277863,-55.724027487683));
#180030=CARTESIAN_POINT('Ctrl Pts',(29.0021037800322,40.1723406811158,-55.6978059978151));
#180031=CARTESIAN_POINT('Ctrl Pts',(29.0063531399503,40.171591047903,-55.6716073785514));
#180032=CARTESIAN_POINT('Ctrl Pts',(29.0106395376334,40.1708348808266,-55.6451804100022));
#180033=CARTESIAN_POINT('Ctrl Pts',(29.0171091146883,40.1696956306932,-55.6187767699309));
#180034=CARTESIAN_POINT('Ctrl Pts',(29.0257761108208,40.1681748817224,-55.5927712420178));
#180035=CARTESIAN_POINT('Ctrl Pts',(29.0290201828335,40.1676056626875,-55.5830373268311));
#180036=CARTESIAN_POINT('Ctrl Pts',(29.0325718289249,40.1669830453019,-55.5733596262871));
#180037=CARTESIAN_POINT('Ctrl Pts',(29.0364307642165,40.1663072924394,-55.5637593428667));
#180038=CARTESIAN_POINT('Ctrl Pts',(29.0465845612265,40.1645292223565,-55.5384986629846));
#180039=CARTESIAN_POINT('Ctrl Pts',(29.0588727550753,40.1623812150824,-55.5137551371703));
#180040=CARTESIAN_POINT('Ctrl Pts',(29.0732950204348,40.1598629648353,-55.4899268488264));
#180041=CARTESIAN_POINT('Ctrl Pts',(29.0761937619183,40.1593568199077,-55.4851375840208));
#180042=CARTESIAN_POINT('Ctrl Pts',(29.0791786699972,40.1588357258452,-55.4803854543331));
#180043=CARTESIAN_POINT('Ctrl Pts',(29.0822496741217,40.1582996919844,-55.4756739402144));
#180044=CARTESIAN_POINT('Ctrl Pts',(29.0914248426835,40.1566981959173,-55.461597457583));
#180045=CARTESIAN_POINT('Ctrl Pts',(29.1013686732816,40.1549632328441,-55.4478834520589));
#180046=CARTESIAN_POINT('Ctrl Pts',(29.1120727310923,40.1530947826212,-55.4346345056757));
#180047=CARTESIAN_POINT('Ctrl Pts',(29.1174247599977,40.1521605575097,-55.4280100324841));
#180048=CARTESIAN_POINT('Ctrl Pts',(29.1229667921261,40.1511929611295,-55.4215019155803));
#180049=CARTESIAN_POINT('Ctrl Pts',(29.1286966355404,40.1501919949717,-55.4151241749086));
#180050=CARTESIAN_POINT('Ctrl Pts',(29.1315615572475,40.1496915118928,-55.4119353045727));
#180051=CARTESIAN_POINT('Ctrl Pts',(29.1344734223787,40.1491826864259,-55.4087790343615));
#180052=CARTESIAN_POINT('Ctrl Pts',(29.1374318784903,40.1486655190189,-55.4056571673549));
#180053=CARTESIAN_POINT('Ctrl Pts',(29.1391534315316,40.1483645745097,-55.4038405239987));
#180054=CARTESIAN_POINT('Ctrl Pts',(29.1412508897063,40.1479977964911,-55.4016627141525));
#180055=CARTESIAN_POINT('Ctrl Pts',(29.143098661154,40.1476746203084,-55.3997779331599));
#180056=CARTESIAN_POINT('Ctrl Pts',(29.1444262497453,40.1474424243767,-55.3984237539156));
#180057=CARTESIAN_POINT('Ctrl Pts',(29.1456236044489,40.1472329711656,-55.39721961437));
#180058=CARTESIAN_POINT('Ctrl Pts',(29.1464466082408,40.1470889648648,-55.3963966105726));
#180059=CARTESIAN_POINT('Ctrl Pts',(29.1562264477315,40.1453777230443,-55.3866167710174));
#180060=CARTESIAN_POINT('Ctrl Pts',(29.1671430152986,40.1434394756915,-55.3765446165107));
#180061=CARTESIAN_POINT('Ctrl Pts',(29.1793251261279,40.1412683811884,-55.3664154209164));
#180062=CARTESIAN_POINT('Ctrl Pts',(29.1909838912127,40.1391905573084,-55.3567213774467));
#180063=CARTESIAN_POINT('Ctrl Pts',(29.2038025095355,40.1368993418058,-55.3469750520176));
#180064=CARTESIAN_POINT('Ctrl Pts',(29.2178716381586,40.1343934407481,-55.337423499576));
#180065=CARTESIAN_POINT('Ctrl Pts',(29.2311276745907,40.1320323623469,-55.3284239566376));
#180066=CARTESIAN_POINT('Ctrl Pts',(29.2454943046528,40.1294806216269,-55.3195974073015));
#180067=CARTESIAN_POINT('Ctrl Pts',(29.2610192152979,40.1267419466417,-55.3111870422682));
#180068=CARTESIAN_POINT('Ctrl Pts',(29.2672465764664,40.1256434077421,-55.3078134717647));
#180069=CARTESIAN_POINT('Ctrl Pts',(29.2736599367761,40.1245148538384,-55.3045072863538));
#180070=CARTESIAN_POINT('Ctrl Pts',(29.2802607448067,40.1233568024336,-55.3012859403587));
#180071=CARTESIAN_POINT('Ctrl Pts',(29.2954942140765,40.12068422956,-55.2938516573137));
#180072=CARTESIAN_POINT('Ctrl Pts',(29.3117391205319,40.1178598967785,-55.2868619639026));
#180073=CARTESIAN_POINT('Ctrl Pts',(29.3289873345881,40.1148724981119,-55.280558107921));
#180074=CARTESIAN_POINT('Ctrl Pts',(29.3457634286183,40.1119668708526,-55.2744268017837));
#180075=CARTESIAN_POINT('Ctrl Pts',(29.3634889697681,40.1089069232597,-55.2689442786734));
#180076=CARTESIAN_POINT('Ctrl Pts',(29.3821198303984,40.1056887792346,-55.2643620188818));
#180077=CARTESIAN_POINT('Ctrl Pts',(29.4001775050092,40.1025696427219,-55.2599207341799));
#180078=CARTESIAN_POINT('Ctrl Pts',(29.4190858710103,40.0993018515975,-55.2563251747636));
#180079=CARTESIAN_POINT('Ctrl Pts',(29.4387660359806,40.0958888189828,-55.2538325278279));
#180080=CARTESIAN_POINT('Ctrl Pts',(29.458446200951,40.092475786368,-55.2513398808922));
#180081=CARTESIAN_POINT('Ctrl Pts',(29.4788985693907,40.0889174361862,-55.24995));
#180082=CARTESIAN_POINT('Ctrl Pts',(29.5,40.0852251642615,-55.24995));
#180083=CARTESIAN_POINT('',(29.5,39.6270595772528,-55.24995));
#180084=CARTESIAN_POINT('Origin',(0.,0.,-55.24995));
#180085=CARTESIAN_POINT('',(30.,40.0414808324985,-55.24995));
#180086=CARTESIAN_POINT('',(30.0435778713739,40.0376682627727,-55.24995));
#180087=CARTESIAN_POINT('',(30.,43.91999998,-55.24995));
#180088=CARTESIAN_POINT('Origin',(30.,0.,-55.74995));
#180089=CARTESIAN_POINT('',(30.5,39.9539921689726,-55.74995));
#180090=CARTESIAN_POINT('Ctrl Pts',(30.,40.0414808324985,-55.24995));
#180091=CARTESIAN_POINT('Ctrl Pts',(30.0215850498355,40.037703938174,-55.24995));
#180092=CARTESIAN_POINT('Ctrl Pts',(30.0424891945252,40.0340461868119,-55.2514041468278));
#180093=CARTESIAN_POINT('Ctrl Pts',(30.0625822498953,40.030530357691,-55.2540052053868));
#180094=CARTESIAN_POINT('Ctrl Pts',(30.0825281795813,40.0270402722291,-55.2565872184341));
#180095=CARTESIAN_POINT('Ctrl Pts',(30.101675378976,40.0236899464585,-55.2602996172416));
#180096=CARTESIAN_POINT('Ctrl Pts',(30.1199435824056,40.0204934250524,-55.2648742467056));
#180097=CARTESIAN_POINT('Ctrl Pts',(30.1390429090745,40.0171514759235,-55.2696570017729));
#180098=CARTESIAN_POINT('Ctrl Pts',(30.1571816232228,40.0139776122057,-55.2753821626572));
#180099=CARTESIAN_POINT('Ctrl Pts',(30.1743147295337,40.0109797070594,-55.2817780783403));
#180100=CARTESIAN_POINT('Ctrl Pts',(30.1903193475258,40.0081792617827,-55.2877527209626));
#180101=CARTESIAN_POINT('Ctrl Pts',(30.2054472590637,40.0055322202579,-55.2943131225478));
#180102=CARTESIAN_POINT('Ctrl Pts',(30.2196931733167,40.0030395082604,-55.3012636513269));
#180103=CARTESIAN_POINT('Ctrl Pts',(30.2362431771765,40.0001436328223,-55.3093383368879));
#180104=CARTESIAN_POINT('Ctrl Pts',(30.2516127665579,39.9974543031544,-55.3179437622824));
#180105=CARTESIAN_POINT('Ctrl Pts',(30.2658371702272,39.9949653550214,-55.326817870191));
#180106=CARTESIAN_POINT('Ctrl Pts',(30.2811342644793,39.9922887103574,-55.3363611922337));
#180107=CARTESIAN_POINT('Ctrl Pts',(30.2951078594437,39.9898436480612,-55.3462154234402));
#180108=CARTESIAN_POINT('Ctrl Pts',(30.3078412626167,39.9876155912096,-55.3561026477787));
#180109=CARTESIAN_POINT('Ctrl Pts',(30.3207962986518,39.9853487536323,-55.3661619654529));
#180110=CARTESIAN_POINT('Ctrl Pts',(30.3324678159279,39.9833065027367,-55.3762552366905));
#180111=CARTESIAN_POINT('Ctrl Pts',(30.3429723610003,39.981468445518,-55.3861352299963));
#180112=CARTESIAN_POINT('Ctrl Pts',(30.3445084364987,39.9811996671331,-55.3875799775354));
#180113=CARTESIAN_POINT('Ctrl Pts',(30.3460195961753,39.9809352484522,-55.3890202398166));
#180114=CARTESIAN_POINT('Ctrl Pts',(30.3475062515996,39.9806751174598,-55.39045533193));
#180115=CARTESIAN_POINT('Ctrl Pts',(30.3487711127258,39.9804537954408,-55.3916763224817));
#180116=CARTESIAN_POINT('Ctrl Pts',(30.3496069371401,39.9803075451175,-55.3924916493986));
#180117=CARTESIAN_POINT('Ctrl Pts',(30.3507725352476,39.9801035819845,-55.393638370999));
#180118=CARTESIAN_POINT('Ctrl Pts',(30.351507597415,39.9799749565333,-55.3943615290581));
#180119=CARTESIAN_POINT('Ctrl Pts',(30.3523735525915,39.9798234238397,-55.3952167714174));
#180120=CARTESIAN_POINT('Ctrl Pts',(30.3535533887318,39.9796169626886,-55.3963966075452));
#180121=CARTESIAN_POINT('Ctrl Pts',(30.3741274016675,39.9760166878297,-55.4169706202642));
#180122=CARTESIAN_POINT('Ctrl Pts',(30.3925747280172,39.9727886607578,-55.4391630476053));
#180123=CARTESIAN_POINT('Ctrl Pts',(30.4088523569405,39.9699403656182,-55.4624843705594));
#180124=CARTESIAN_POINT('Ctrl Pts',(30.4251500791383,39.9670885545135,-55.485834481597));
#180125=CARTESIAN_POINT('Ctrl Pts',(30.4392727632377,39.9646174100751,-55.5103162627385));
#180126=CARTESIAN_POINT('Ctrl Pts',(30.4512005218462,39.9625303719341,-55.5354850647054));
#180127=CARTESIAN_POINT('Ctrl Pts',(30.4631486406572,39.9604397713032,-55.5606968288014));
#180128=CARTESIAN_POINT('Ctrl Pts',(30.47289436045,39.9587345848572,-55.5865979611061));
#180129=CARTESIAN_POINT('Ctrl Pts',(30.4804407017092,39.9574142448672,-55.6127884603395));
#180130=CARTESIAN_POINT('Ctrl Pts',(30.4880210336523,39.9560879577225,-55.6390969283934));
#180131=CARTESIAN_POINT('Ctrl Pts',(30.4933821541613,39.9551499874332,-55.6656973723438));
#180132=CARTESIAN_POINT('Ctrl Pts',(30.496549954567,39.9545957644334,-55.6922317351003));
#180133=CARTESIAN_POINT('Ctrl Pts',(30.4988557842716,39.9541923476481,-55.711545995471));
#180134=CARTESIAN_POINT('Ctrl Pts',(30.5,39.9539921689726,-55.730826234649));
#180135=CARTESIAN_POINT('Ctrl Pts',(30.5,39.9539921689726,-55.74995));
#180136=CARTESIAN_POINT('',(30.5,39.4958265819638,-55.74995));
#180137=CARTESIAN_POINT('Origin',(30.5,-9.33460238845303,-92.34995));
#180138=CARTESIAN_POINT('',(30.5,39.9539921689726,-59.64995));
#180139=CARTESIAN_POINT('',(30.5,39.9539921689726,-92.34995));
#180140=CARTESIAN_POINT('Ctrl Pts',(30.5,39.9539921689726,-59.64995));
#180141=CARTESIAN_POINT('Ctrl Pts',(30.5,39.9539921689583,-59.8463349320561));
#180142=CARTESIAN_POINT('Ctrl Pts',(30.5,39.9148020481738,-60.0425718399611));
#180143=CARTESIAN_POINT('Ctrl Pts',(30.5,39.7639485838465,-60.4053784571342));
#180144=CARTESIAN_POINT('Ctrl Pts',(30.5,39.65234456211,-60.5717700902076));
#180145=CARTESIAN_POINT('Ctrl Pts',(30.5,39.3736037058546,-60.8494502533521));
#180146=CARTESIAN_POINT('Ctrl Pts',(30.5,39.206576483846,-60.9606295880612));
#180147=CARTESIAN_POINT('Ctrl Pts',(30.5,38.8423840041908,-61.1109090094727));
#180148=CARTESIAN_POINT('Ctrl Pts',(30.5,38.6453975033045,-61.149949999985));
#180149=CARTESIAN_POINT('Ctrl Pts',(30.5,38.4482624126576,-61.14995));
#180150=CARTESIAN_POINT('',(30.5,46.41999998,-91.84995));
#180151=CARTESIAN_POINT('Ctrl Pts',(37.5,37.9232037521398,-61.1499499946262));
#180152=CARTESIAN_POINT('Ctrl Pts',(37.5,37.9232456375444,-60.6498941830815));
#180153=CARTESIAN_POINT('Ctrl Pts',(36.9999441887055,37.9232456578392,-60.6499499995188));
#180154=CARTESIAN_POINT('Ctrl Pts',(37.5,38.1203811322273,-61.149966723533));
#180155=CARTESIAN_POINT('Ctrl Pts',(37.5000000000028,38.0559860700137,-60.6441634129654));
#180156=CARTESIAN_POINT('Ctrl Pts',(36.9942372710435,38.0551964119617,-60.6499618311932));
#180157=CARTESIAN_POINT('Ctrl Pts',(37.5,38.3174130179182,-61.110925104441));
#180158=CARTESIAN_POINT('Ctrl Pts',(37.5,38.1853247811951,-60.6119868070542));
#180159=CARTESIAN_POINT('Ctrl Pts',(36.9885345754041,38.1870501910475,-60.6239348042609));
#180160=CARTESIAN_POINT('Ctrl Pts',(37.5,38.6816445026906,-60.9606295880611));
#180161=CARTESIAN_POINT('Ctrl Pts',(37.5,38.4206008165402,-60.5030970594214));
#180162=CARTESIAN_POINT('Ctrl Pts',(36.977992646032,38.4307944117744,-60.5237387895065));
#180163=CARTESIAN_POINT('Ctrl Pts',(37.5,38.8486717246983,-60.8494502533514));
#180164=CARTESIAN_POINT('Ctrl Pts',(37.4999999999993,38.5260237066865,-60.4261477374108));
#180165=CARTESIAN_POINT('Ctrl Pts',(36.9731583992956,38.5425695414996,-60.4496195485703));
#180166=CARTESIAN_POINT('Ctrl Pts',(37.5,39.1274125809551,-60.5717700902082));
#180167=CARTESIAN_POINT('Ctrl Pts',(37.5000000000008,38.7000372987261,-60.2406358789592));
#180168=CARTESIAN_POINT('Ctrl Pts',(36.9650908553591,38.7291039816193,-60.2644994621534));
#180169=CARTESIAN_POINT('Ctrl Pts',(37.5,39.239016602691,-60.4053784571342));
#180170=CARTESIAN_POINT('Ctrl Pts',(37.4999999999994,38.7680983778313,-60.1321953438305));
#180171=CARTESIAN_POINT('Ctrl Pts',(36.9618607274251,38.8037899942061,-60.1535714132619));
#180172=CARTESIAN_POINT('Ctrl Pts',(37.5,39.3898862234668,-60.0425329832704));
#180173=CARTESIAN_POINT('Ctrl Pts',(37.5000000000007,38.8599291842782,-59.8989282761481));
#180174=CARTESIAN_POINT('Ctrl Pts',(36.9574941496163,38.9047527687766,-59.9116734379898));
#180175=CARTESIAN_POINT('Ctrl Pts',(37.5,39.429076975232,-59.8462508632634));
#180176=CARTESIAN_POINT('Ctrl Pts',(37.5,38.8833480398924,-59.7745406636058));
#180177=CARTESIAN_POINT('Ctrl Pts',(36.9563598640845,38.9309794818232,-59.7808179550133));
#180178=CARTESIAN_POINT('Ctrl Pts',(37.5,39.4290601824227,-59.649823802691));
#180179=CARTESIAN_POINT('Ctrl Pts',(37.5,38.8833379930089,-59.6498699040797));
#180180=CARTESIAN_POINT('Ctrl Pts',(36.9563603497081,38.9309682439904,-59.6498658680024));
#180181=CARTESIAN_POINT('',(36.9564221286262,38.9309628387712,-59.64995));
#180182=CARTESIAN_POINT('Origin',(37.,39.4290601878171,-59.64995));
#180183=CARTESIAN_POINT('Ctrl Pts',(36.9564221286262,38.9309628387712,-59.64995));
#180184=CARTESIAN_POINT('Ctrl Pts',(36.9564221286262,38.9309628387712,-59.6909727320563));
#180185=CARTESIAN_POINT('Ctrl Pts',(36.9565526533189,38.928414270096,-59.7323929145967));
#180186=CARTESIAN_POINT('Ctrl Pts',(36.9568026461917,38.9231907562272,-59.7738824505257));
#180187=CARTESIAN_POINT('Ctrl Pts',(36.9570478117228,38.9180681079776,-59.8145708269595));
#180188=CARTESIAN_POINT('Ctrl Pts',(36.9574078479651,38.9103725010286,-59.8553255347459));
#180189=CARTESIAN_POINT('Ctrl Pts',(36.9578758048445,38.9000244956702,-59.8958071083368));
#180190=CARTESIAN_POINT('Ctrl Pts',(36.9583385886206,38.889790883973,-59.9358411719725));
#180191=CARTESIAN_POINT('Ctrl Pts',(36.9589068918223,38.8769628684199,-59.9756077254562));
#180192=CARTESIAN_POINT('Ctrl Pts',(36.9595778517683,38.8615077284126,-60.0147542801158));
#180193=CARTESIAN_POINT('Ctrl Pts',(36.9602378669453,38.8463046942708,-60.0532622720685));
#180194=CARTESIAN_POINT('Ctrl Pts',(36.9609971979412,38.8285593256615,-60.0911698882792));
#180195=CARTESIAN_POINT('Ctrl Pts',(36.9618572198749,38.8082873402642,-60.1281241918774));
#180196=CARTESIAN_POINT('Ctrl Pts',(36.9624155228255,38.7951273162926,-60.1521139250818));
#180197=CARTESIAN_POINT('Ctrl Pts',(36.9630163436043,38.7809034729076,-60.1757015644984));
#180198=CARTESIAN_POINT('Ctrl Pts',(36.9636610617812,38.7656315786673,-60.1987879162352));
#180199=CARTESIAN_POINT('Ctrl Pts',(36.9644459532149,38.747039301619,-60.2268936535308));
#180200=CARTESIAN_POINT('Ctrl Pts',(36.9652958498083,38.7268930680149,-60.2542563740827));
#180201=CARTESIAN_POINT('Ctrl Pts',(36.9662149260452,38.7052405924212,-60.2806949719394));
#180202=CARTESIAN_POINT('Ctrl Pts',(36.9666744641636,38.6944143546243,-60.2939142708678));
#180203=CARTESIAN_POINT('Ctrl Pts',(36.9671513266945,38.6832118935344,-60.3069025151661));
#180204=CARTESIAN_POINT('Ctrl Pts',(36.9676462162085,38.6716412395726,-60.3196370305188));
#180205=CARTESIAN_POINT('Ctrl Pts',(36.9678688531808,38.6664359254737,-60.3253659333559));
#180206=CARTESIAN_POINT('Ctrl Pts',(36.9681087471589,38.6608777513272,-60.331343277216));
#180207=CARTESIAN_POINT('Ctrl Pts',(36.9683470528149,38.6553368998154,-60.3371563979268));
#180208=CARTESIAN_POINT('Ctrl Pts',(36.9685931263345,38.6496154374899,-60.343159004398));
#180209=CARTESIAN_POINT('Ctrl Pts',(36.9688375221239,38.6439126264018,-60.3489863692137));
#180210=CARTESIAN_POINT('Ctrl Pts',(36.9690630932701,38.6386772127086,-60.3542239166839));
#180211=CARTESIAN_POINT('Ctrl Pts',(36.9691046552039,38.6377125772892,-60.3551889452559));
#180212=CARTESIAN_POINT('Ctrl Pts',(36.9691455867854,38.6367639091397,-60.35613405381));
#180213=CARTESIAN_POINT('Ctrl Pts',(36.9691857916419,38.6358341396253,-60.3570567811866));
#180214=CARTESIAN_POINT('Ctrl Pts',(36.9701363384957,38.6138519821401,-60.3788724443089));
#180215=CARTESIAN_POINT('Ctrl Pts',(36.9711666068585,38.5902025659925,-60.4003228463237));
#180216=CARTESIAN_POINT('Ctrl Pts',(36.9722706959613,38.5648184450851,-60.4211192429472));
#180217=CARTESIAN_POINT('Ctrl Pts',(36.9733490218504,38.5400266464176,-60.4414303689452));
#180218=CARTESIAN_POINT('Ctrl Pts',(36.9744977238215,38.5135797007575,-60.4611173555234));
#180219=CARTESIAN_POINT('Ctrl Pts',(36.9757145657962,38.485452049613,-60.479881063412));
#180220=CARTESIAN_POINT('Ctrl Pts',(36.9769459440814,38.4569883874845,-60.4988689212632));
#180221=CARTESIAN_POINT('Ctrl Pts',(36.9782470364914,38.4268028979539,-60.516911045168));
#180222=CARTESIAN_POINT('Ctrl Pts',(36.9796197088919,38.3949169079658,-60.5336701568701));
#180223=CARTESIAN_POINT('Ctrl Pts',(36.9803060450922,38.3789739129717,-60.5420497127212));
#180224=CARTESIAN_POINT('Ctrl Pts',(36.9810103472633,38.3626066040907,-60.5501081143651));
#180225=CARTESIAN_POINT('Ctrl Pts',(36.9817333133923,38.34582295935,-60.5578010744457));
#180226=CARTESIAN_POINT('Ctrl Pts',(36.9820947964567,38.3374311369797,-60.5616475544861));
#180227=CARTESIAN_POINT('Ctrl Pts',(36.98246094573,38.3289352331521,-60.5654026797547));
#180228=CARTESIAN_POINT('Ctrl Pts',(36.9828318859725,38.3203366738844,-60.569060776422));
#180229=CARTESIAN_POINT('Ctrl Pts',(36.9830173560938,38.3160373942505,-60.5708898247557));
#180230=CARTESIAN_POINT('Ctrl Pts',(36.9832040239853,38.3117124510762,-60.5726946166406));
#180231=CARTESIAN_POINT('Ctrl Pts',(36.9833919065741,38.3073620378383,-60.5744744411355));
#180232=CARTESIAN_POINT('Ctrl Pts',(36.9835059768349,38.3047207458701,-60.5755550364458));
#180233=CARTESIAN_POINT('Ctrl Pts',(36.9836515904334,38.3013582757846,-60.5769130552655));
#180234=CARTESIAN_POINT('Ctrl Pts',(36.9837720133312,38.2985699856306,-60.5780234113379));
#180235=CARTESIAN_POINT('Ctrl Pts',(36.9838499363092,38.2967657451051,-60.5787418980494));
#180236=CARTESIAN_POINT('Ctrl Pts',(36.9839173597185,38.2952024681103,-60.5793580291786));
#180237=CARTESIAN_POINT('Ctrl Pts',(36.9839592160933,38.2942345898009,-60.5797383010624));
#180238=CARTESIAN_POINT('Ctrl Pts',(36.9846243076896,38.2788551468116,-60.5857807649761));
#180239=CARTESIAN_POINT('Ctrl Pts',(36.9853695593922,38.2618442765263,-60.5920329995529));
#180240=CARTESIAN_POINT('Ctrl Pts',(36.9861894744502,38.2431391507943,-60.5982457366593));
#180241=CARTESIAN_POINT('Ctrl Pts',(36.9869913344616,38.2248459237255,-60.6043216653772));
#180242=CARTESIAN_POINT('Ctrl Pts',(36.9878645390643,38.204931474406,-60.6103597069373));
#180243=CARTESIAN_POINT('Ctrl Pts',(36.9888053528999,38.1833531074951,-60.6160795510658));
#180244=CARTESIAN_POINT('Ctrl Pts',(36.9897095219953,38.1626152189253,-60.6215766070136));
#180245=CARTESIAN_POINT('Ctrl Pts',(36.9906760796327,38.140339861999,-60.6267794470962));
#180246=CARTESIAN_POINT('Ctrl Pts',(36.9917039045611,38.1165142207585,-60.6313985665783));
#180247=CARTESIAN_POINT('Ctrl Pts',(36.9927058043032,38.0932895419716,-60.6359011763997));
#180248=CARTESIAN_POINT('Ctrl Pts',(36.9937658627523,38.0685911496967,-60.6398488185077));
#180249=CARTESIAN_POINT('Ctrl Pts',(36.9948859960183,38.0424409451686,-60.6429384340034));
#180250=CARTESIAN_POINT('Ctrl Pts',(36.9959640318133,38.0172735321624,-60.6459119338523));
#180251=CARTESIAN_POINT('Ctrl Pts',(36.9970976705001,37.9907609104651,-60.6480902255593));
#180252=CARTESIAN_POINT('Ctrl Pts',(36.998292087359,37.9629622338,-60.6491761921129));
#180253=CARTESIAN_POINT('Ctrl Pts',(36.9988478997837,37.9500263397988,-60.649681538047));
#180254=CARTESIAN_POINT('Ctrl Pts',(36.9994169271496,37.9368125746484,-60.64995));
#180255=CARTESIAN_POINT('Ctrl Pts',(37.,37.923330431502,-60.64995));
#180256=CARTESIAN_POINT('Ctrl Pts',(30.5,39.9539921689726,-59.64995));
#180257=CARTESIAN_POINT('Ctrl Pts',(30.5,39.4958265819639,-59.64995));
#180258=CARTESIAN_POINT('Ctrl Pts',(30.9564221286262,39.4558948199267,-59.64995));
#180259=CARTESIAN_POINT('Ctrl Pts',(30.5,39.9539921689583,-59.8463349320561));
#180260=CARTESIAN_POINT('Ctrl Pts',(30.5,39.4958265819509,-59.7861314644993));
#180261=CARTESIAN_POINT('Ctrl Pts',(30.9564221286278,39.4558948199266,-59.7808732880376));
#180262=CARTESIAN_POINT('Ctrl Pts',(30.5,39.9148020481738,-60.0425718399611));
#180263=CARTESIAN_POINT('Ctrl Pts',(30.4999999999997,39.4674332340768,-59.9224177216067));
#180264=CARTESIAN_POINT('Ctrl Pts',(30.9575563441362,39.4296688417285,-59.9116978933072));
#180265=CARTESIAN_POINT('Ctrl Pts',(30.5,39.7639485838465,-60.4053784571342));
#180266=CARTESIAN_POINT('Ctrl Pts',(30.5000000000003,39.3593214179772,-60.1718710142636));
#180267=CARTESIAN_POINT('Ctrl Pts',(30.9619222489984,39.3287178983286,-60.153568971423));
#180268=CARTESIAN_POINT('Ctrl Pts',(30.5,39.65234456211,-60.5717700902076));
#180269=CARTESIAN_POINT('Ctrl Pts',(30.5000000000001,39.2793032864295,-60.2852157712117));
#180270=CARTESIAN_POINT('Ctrl Pts',(30.9651522214976,39.2540326311941,-60.2644967268053));
#180271=CARTESIAN_POINT('Ctrl Pts',(30.5,39.3736037058546,-60.8494502533521));
#180272=CARTESIAN_POINT('Ctrl Pts',(30.5,39.0823726723643,-60.4706504746469));
#180273=CARTESIAN_POINT('Ctrl Pts',(30.9732193617862,39.0674996103677,-60.4496168355678));
#180274=CARTESIAN_POINT('Ctrl Pts',(30.5,39.206576483846,-60.9606295880612));
#180275=CARTESIAN_POINT('Ctrl Pts',(30.5,38.9650655890091,-60.5426326522477));
#180276=CARTESIAN_POINT('Ctrl Pts',(30.9780533572398,38.9557252092273,-60.5237363920407));
#180277=CARTESIAN_POINT('Ctrl Pts',(30.5,38.8423840041908,-61.1109090094727));
#180278=CARTESIAN_POINT('Ctrl Pts',(30.5,38.7136903701654,-60.6353187454024));
#180279=CARTESIAN_POINT('Ctrl Pts',(30.9885935839752,38.71200807244,-60.6239226729818));
#180280=CARTESIAN_POINT('Ctrl Pts',(30.5,38.6453975033045,-61.149949999985));
#180281=CARTESIAN_POINT('Ctrl Pts',(30.4999999999973,38.5794088824901,-60.655621796981));
#180282=CARTESIAN_POINT('Ctrl Pts',(30.994294641792,38.5801849605867,-60.64995));
#180283=CARTESIAN_POINT('Ctrl Pts',(30.5,38.4482624126576,-61.14995));
#180284=CARTESIAN_POINT('Ctrl Pts',(30.5,38.4482624126575,-60.64995));
#180285=CARTESIAN_POINT('Ctrl Pts',(31.,38.4482624126576,-60.64995));
#180286=CARTESIAN_POINT('',(30.9564221286262,39.4558948199267,-59.64995));
#180287=CARTESIAN_POINT('Origin',(31.,39.9539921689726,-59.64995));
#180288=CARTESIAN_POINT('Ctrl Pts',(31.,38.4482624126576,-60.64995));
#180289=CARTESIAN_POINT('Ctrl Pts',(30.9987818467218,38.476429247827,-60.64995));
#180290=CARTESIAN_POINT('Ctrl Pts',(30.9976145369588,38.5034204502283,-60.6487662512907));
#180291=CARTESIAN_POINT('Ctrl Pts',(30.9965012313162,38.5291629385428,-60.6466963126423));
#180292=CARTESIAN_POINT('Ctrl Pts',(30.9953475221318,38.5558396606057,-60.6445512527966));
#180293=CARTESIAN_POINT('Ctrl Pts',(30.9942517893313,38.5811758196397,-60.6414545916582));
#180294=CARTESIAN_POINT('Ctrl Pts',(30.9932156801214,38.6051333279912,-60.6377013130332));
#180295=CARTESIAN_POINT('Ctrl Pts',(30.9921218554365,38.6304253664877,-60.6337389616033));
#180296=CARTESIAN_POINT('Ctrl Pts',(30.9910944719623,38.654181113399,-60.6290450673587));
#180297=CARTESIAN_POINT('Ctrl Pts',(30.990133679575,38.6763971032037,-60.6239244744924));
#180298=CARTESIAN_POINT('Ctrl Pts',(30.989141234533,38.6993449837517,-60.618635187161));
#180299=CARTESIAN_POINT('Ctrl Pts',(30.9882197863802,38.720651233716,-60.6128905529596));
#180300=CARTESIAN_POINT('Ctrl Pts',(30.9873680866258,38.7403447214142,-60.6069806688732));
#180301=CARTESIAN_POINT('Ctrl Pts',(30.9864834145568,38.7608006137855,-60.600841992238));
#180302=CARTESIAN_POINT('Ctrl Pts',(30.9856739565944,38.7795173626662,-60.594525091633));
#180303=CARTESIAN_POINT('Ctrl Pts',(30.9849373158678,38.7965503898717,-60.588305157651));
#180304=CARTESIAN_POINT('Ctrl Pts',(30.9847129878412,38.8017374305014,-60.586411011068));
#180305=CARTESIAN_POINT('Ctrl Pts',(30.9844954066137,38.8067684677967,-60.5845255017482));
#180306=CARTESIAN_POINT('Ctrl Pts',(30.9842844922129,38.8116453509173,-60.5826554871329));
#180307=CARTESIAN_POINT('Ctrl Pts',(30.9842090737892,38.8133892187453,-60.5819868103889));
#180308=CARTESIAN_POINT('Ctrl Pts',(30.9841737017427,38.8142060813347,-60.581671463497));
#180309=CARTESIAN_POINT('Ctrl Pts',(30.9840978736727,38.8159588122539,-60.5809901111774));
#180310=CARTESIAN_POINT('Ctrl Pts',(30.9840628676311,38.8167679607848,-60.5806755647617));
#180311=CARTESIAN_POINT('Ctrl Pts',(30.9840192449614,38.8177764376487,-60.5802826897599));
#180312=CARTESIAN_POINT('Ctrl Pts',(30.9839591488407,38.819166055459,-60.5797369933149));
#180313=CARTESIAN_POINT('Ctrl Pts',(30.9837458556875,38.8240980870287,-60.5778002074775));
#180314=CARTESIAN_POINT('Ctrl Pts',(30.9835339342674,38.8289983903335,-60.5758307565192));
#180315=CARTESIAN_POINT('Ctrl Pts',(30.9833233986079,38.8338666417501,-60.5738295347323));
#180316=CARTESIAN_POINT('Ctrl Pts',(30.9818941408027,38.8669156100438,-60.5602438938683));
#180317=CARTESIAN_POINT('Ctrl Pts',(30.9805292639735,38.8984754854848,-60.5452002163202));
#180318=CARTESIAN_POINT('Ctrl Pts',(30.9792308551162,38.928498238384,-60.5290286704852));
#180319=CARTESIAN_POINT('Ctrl Pts',(30.9779906264808,38.9571757059225,-60.5135817531992));
#180320=CARTESIAN_POINT('Ctrl Pts',(30.9768110201851,38.9844512354806,-60.4971053444783));
#180321=CARTESIAN_POINT('Ctrl Pts',(30.9756925305751,39.0103135904489,-60.4798551184457));
#180322=CARTESIAN_POINT('Ctrl Pts',(30.9744365387299,39.0393553505584,-60.460484224848));
#180323=CARTESIAN_POINT('Ctrl Pts',(30.9732575807701,39.0666158892126,-60.4401373907899));
#180324=CARTESIAN_POINT('Ctrl Pts',(30.9721546419406,39.0921186701619,-60.4191325966574));
#180325=CARTESIAN_POINT('Ctrl Pts',(30.9716361344385,39.1041078964837,-60.4092579390191));
#180326=CARTESIAN_POINT('Ctrl Pts',(30.9711344064916,39.1157091363555,-60.3992372749015));
#180327=CARTESIAN_POINT('Ctrl Pts',(30.9706492477231,39.1269272542305,-60.3891007235571));
#180328=CARTESIAN_POINT('Ctrl Pts',(30.970413956114,39.1323678010709,-60.3841847133134));
#180329=CARTESIAN_POINT('Ctrl Pts',(30.9701964148518,39.1373979142195,-60.3795368119505));
#180330=CARTESIAN_POINT('Ctrl Pts',(30.9699770120193,39.1424709178192,-60.3747537948081));
#180331=CARTESIAN_POINT('Ctrl Pts',(30.9697641308869,39.1473931275184,-60.3701129517834));
#180332=CARTESIAN_POINT('Ctrl Pts',(30.969549490659,39.1523558671877,-60.3653448267733));
#180333=CARTESIAN_POINT('Ctrl Pts',(30.9693166057443,39.1577401861387,-60.3600469436324));
#180334=CARTESIAN_POINT('Ctrl Pts',(30.9692736283757,39.1587338265396,-60.3590692543879));
#180335=CARTESIAN_POINT('Ctrl Pts',(30.96923003404,39.1597417231099,-60.3580734247277));
#180336=CARTESIAN_POINT('Ctrl Pts',(30.9691857254863,39.1607661236638,-60.3570567840805));
#180337=CARTESIAN_POINT('Ctrl Pts',(30.9677127419572,39.1948210637802,-60.3232598125428));
#180338=CARTESIAN_POINT('Ctrl Pts',(30.9663603950735,39.2260897055471,-60.2873222679365));
#180339=CARTESIAN_POINT('Ctrl Pts',(30.9651340688828,39.254445874256,-60.2497596520108));
#180340=CARTESIAN_POINT('Ctrl Pts',(30.9638892540534,39.2832295531698,-60.2116307253895));
#180341=CARTESIAN_POINT('Ctrl Pts',(30.9627742870912,39.3090123097717,-60.1718273246592));
#180342=CARTESIAN_POINT('Ctrl Pts',(30.9617936458919,39.3316888871906,-60.1308415630416));
#180343=CARTESIAN_POINT('Ctrl Pts',(30.9610260198825,39.3494396513267,-60.0987587414601));
#180344=CARTESIAN_POINT('Ctrl Pts',(30.960340677559,39.3652876700136,-60.0659504747633));
#180345=CARTESIAN_POINT('Ctrl Pts',(30.9597392952827,39.3791933701244,-60.032633432405));
#180346=CARTESIAN_POINT('Ctrl Pts',(30.9596795344221,39.380575214318,-60.0293226345908));
#180347=CARTESIAN_POINT('Ctrl Pts',(30.9596206036152,39.3819378561946,-60.0260068881712));
#180348=CARTESIAN_POINT('Ctrl Pts',(30.9595625010598,39.3832813366339,-60.0226864256965));
#180349=CARTESIAN_POINT('Ctrl Pts',(30.9588033987314,39.4008337338138,-59.9793050153876));
#180350=CARTESIAN_POINT('Ctrl Pts',(30.9581857739999,39.4151148052685,-59.9351228137558));
#180351=CARTESIAN_POINT('Ctrl Pts',(30.9577055602545,39.4262185814993,-59.8906338461556));
#180352=CARTESIAN_POINT('Ctrl Pts',(30.9572195296779,39.4374568578174,-59.8456059835076));
#180353=CARTESIAN_POINT('Ctrl Pts',(30.9568742584458,39.4454404162565,-59.8002638457115));
#180354=CARTESIAN_POINT('Ctrl Pts',(30.956665170667,39.4502750631828,-59.7550665502451));
#180355=CARTESIAN_POINT('Ctrl Pts',(30.9565023749348,39.4540393189924,-59.7198759386805));
#180356=CARTESIAN_POINT('Ctrl Pts',(30.9564221286262,39.4558948199267,-59.6847720497212));
#180357=CARTESIAN_POINT('Ctrl Pts',(30.9564221286262,39.4558948199267,-59.64995));
#180358=CARTESIAN_POINT('Origin',(0.,-12.9675000200281,-60.64995));
#180359=CARTESIAN_POINT('',(4.69960655320655,40.7492486855235,-60.64995));
#180360=CARTESIAN_POINT('Origin',(33.35,67.7009572055632,-55.24995));
#180361=CARTESIAN_POINT('',(33.35,-65.63964951798,-59.64995));
#180362=CARTESIAN_POINT('Ctrl Pts',(33.35,-64.133919761665,-61.14995));
#180363=CARTESIAN_POINT('Ctrl Pts',(33.35,-64.3310548523114,-61.149949999985));
#180364=CARTESIAN_POINT('Ctrl Pts',(33.35,-64.5280413531989,-61.1109090094727));
#180365=CARTESIAN_POINT('Ctrl Pts',(33.35,-64.8922338328527,-60.9606295880612));
#180366=CARTESIAN_POINT('Ctrl Pts',(33.35,-65.0592610548614,-60.849450253352));
#180367=CARTESIAN_POINT('Ctrl Pts',(33.35,-65.338001911118,-60.5717700902076));
#180368=CARTESIAN_POINT('Ctrl Pts',(33.35,-65.4496059328539,-60.4053784571335));
#180369=CARTESIAN_POINT('Ctrl Pts',(33.35,-65.6004593971813,-60.0425718399618));
#180370=CARTESIAN_POINT('Ctrl Pts',(33.35,-65.6396495179636,-59.8463349320557));
#180371=CARTESIAN_POINT('Ctrl Pts',(33.35,-65.63964951798,-59.64995));
#180372=CARTESIAN_POINT('',(33.35,-65.63964951798,-55.74995));
#180373=CARTESIAN_POINT('',(33.35,-65.63964951798,-55.24995));
#180374=CARTESIAN_POINT('',(33.35,67.7009572055632,-55.74995));
#180375=CARTESIAN_POINT('Origin',(32.85,67.7009572055632,-55.74995));
#180376=CARTESIAN_POINT('',(32.85,-65.7271381815059,-55.24995));
#180377=CARTESIAN_POINT('Ctrl Pts',(33.35,-65.63964951798,-55.74995));
#180378=CARTESIAN_POINT('Ctrl Pts',(33.35,-65.63964951798,-55.7240510278047));
#180379=CARTESIAN_POINT('Ctrl Pts',(33.347900048614,-65.640016961861,-55.6978536073956));
#180380=CARTESIAN_POINT('Ctrl Pts',(33.3436584043302,-65.6407591534406,
-55.6716786003409));
#180381=CARTESIAN_POINT('Ctrl Pts',(33.3393809358794,-65.6415076134371,
-55.6452825238705));
#180382=CARTESIAN_POINT('Ctrl Pts',(33.3329253996456,-65.6426371859126,
-55.6189093032682));
#180383=CARTESIAN_POINT('Ctrl Pts',(33.3242775747263,-65.6441503592019,
-55.5929324718169));
#180384=CARTESIAN_POINT('Ctrl Pts',(33.3210188939802,-65.6447205544486,
-55.583143860081));
#180385=CARTESIAN_POINT('Ctrl Pts',(33.3174492131982,-65.6453451676502,
-55.5734119765541));
#180386=CARTESIAN_POINT('Ctrl Pts',(33.3135688278912,-65.6460241470991,
-55.5637583894205));
#180387=CARTESIAN_POINT('Ctrl Pts',(33.3034033143569,-65.6478028814851,
-55.5384687176752));
#180388=CARTESIAN_POINT('Ctrl Pts',(33.2910985361539,-65.6499559386847,
-55.5136974847687));
#180389=CARTESIAN_POINT('Ctrl Pts',(33.2766549467837,-65.6524832393453,
-55.4898442373666));
#180390=CARTESIAN_POINT('Ctrl Pts',(33.2649384053914,-65.6545333684401,
-55.4704946454223));
#180391=CARTESIAN_POINT('Ctrl Pts',(33.2518128551695,-65.6568300421337,
-55.4517483669));
#180392=CARTESIAN_POINT('Ctrl Pts',(33.2372964027467,-65.6593700921767,
-55.4338552796691));
#180393=CARTESIAN_POINT('Ctrl Pts',(33.2294565912626,-65.6607418814347,
-55.4241918697206));
#180394=CARTESIAN_POINT('Ctrl Pts',(33.2212113468568,-65.6621846122616,
-55.414777801353));
#180395=CARTESIAN_POINT('Ctrl Pts',(33.2125680866752,-65.6636969868252,
-55.4056571306878));
#180396=CARTESIAN_POINT('Ctrl Pts',(33.2108465431246,-65.6639982179141,
-55.4038404976778));
#180397=CARTESIAN_POINT('Ctrl Pts',(33.2087490914815,-65.6643652243974,
-55.4016626948158));
#180398=CARTESIAN_POINT('Ctrl Pts',(33.2069013241902,-65.6646885364879,
-55.3997779182178));
#180399=CARTESIAN_POINT('Ctrl Pts',(33.2055737423077,-65.6649208294156,
-55.3984237459279));
#180400=CARTESIAN_POINT('Ctrl Pts',(33.2043763923404,-65.6651303319781,
-55.3972196111485));
#180401=CARTESIAN_POINT('Ctrl Pts',(33.2035533894273,-65.6652743275964,
-55.3963966082408));
#180402=CARTESIAN_POINT('Ctrl Pts',(33.1937873007841,-65.6669830384047,
-55.3866305196621));
#180403=CARTESIAN_POINT('Ctrl Pts',(33.182886437889,-65.6688903937285,-55.3765717208458));
#180404=CARTESIAN_POINT('Ctrl Pts',(33.170722824573,-65.6710187470995,-55.3664552894951));
#180405=CARTESIAN_POINT('Ctrl Pts',(33.1590750456085,-65.6730568412891,
-55.3567678756303));
#180406=CARTESIAN_POINT('Ctrl Pts',(33.1462686320959,-65.675297711858,-55.3470275906715));
#180407=CARTESIAN_POINT('Ctrl Pts',(33.132213803587,-65.6777570333304,-55.3374815439839));
#180408=CARTESIAN_POINT('Ctrl Pts',(33.1189601031151,-65.6800761729868,
-55.3284796238675));
#180409=CARTESIAN_POINT('Ctrl Pts',(33.10459580387,-65.6825896481115,-55.3196505221102));
#180410=CARTESIAN_POINT('Ctrl Pts',(33.0890741345983,-65.6853056127038,
-55.311237769723));
#180411=CARTESIAN_POINT('Ctrl Pts',(33.0828103974728,-65.6864016345265,
-55.3078428211172));
#180412=CARTESIAN_POINT('Ctrl Pts',(33.0763585547313,-65.6875305666442,
-55.3045160977312));
#180413=CARTESIAN_POINT('Ctrl Pts',(33.069717210502,-65.6886926513055,-55.3012753797601));
#180414=CARTESIAN_POINT('Ctrl Pts',(33.0544690954581,-65.6913607257185,
-55.293834892));
#180415=CARTESIAN_POINT('Ctrl Pts',(33.0382095130778,-65.6942057839824,
-55.2868407235284));
#180416=CARTESIAN_POINT('Ctrl Pts',(33.0209460855975,-65.6972264923786,
-55.2805340044877));
#180417=CARTESIAN_POINT('Ctrl Pts',(33.0041655073293,-65.7001627131103,
-55.2744036811438));
#180418=CARTESIAN_POINT('Ctrl Pts',(32.9864361384534,-65.7032649506864,
-55.2689228588808));
#180419=CARTESIAN_POINT('Ctrl Pts',(32.9678013238571,-65.7065256207345,
-55.2643427579567));
#180420=CARTESIAN_POINT('Ctrl Pts',(32.9497555825658,-65.7096832163102,
-55.2599074406136));
#180421=CARTESIAN_POINT('Ctrl Pts',(32.9308605102442,-65.7129894255594,
-55.2563167977718));
#180422=CARTESIAN_POINT('Ctrl Pts',(32.9111938833676,-65.7164306393623,
-55.2538274761891));
#180423=CARTESIAN_POINT('Ctrl Pts',(32.8915272564911,-65.7198718531653,
-55.2513381546065));
#180424=CARTESIAN_POINT('Ctrl Pts',(32.8710886481192,-65.7234481462268,
-55.24995));
#180425=CARTESIAN_POINT('Ctrl Pts',(32.85,-65.7271381815059,-55.24995));
#180426=CARTESIAN_POINT('',(32.85,-73.08000002,-55.24995));
#180427=CARTESIAN_POINT('Origin',(41.5,-73.08000002,-55.24995));
#180428=CARTESIAN_POINT('',(32.35,-65.7708825132688,-55.24995));
#180429=CARTESIAN_POINT('',(40.7958880023324,-65.0319630596553,-55.24995));
#180430=CARTESIAN_POINT('',(32.35,-73.08000002,-55.24995));
#180431=CARTESIAN_POINT('Origin',(32.35,-73.08000002,-55.74995));
#180432=CARTESIAN_POINT('',(31.85,-65.8583711767947,-55.74995));
#180433=CARTESIAN_POINT('Ctrl Pts',(32.35,-65.7708825132688,-55.24995));
#180434=CARTESIAN_POINT('Ctrl Pts',(32.3291548218245,-65.7745299468279,
-55.24995));
#180435=CARTESIAN_POINT('Ctrl Pts',(32.3089230360357,-65.7780375764609,
-55.2512537778699));
#180436=CARTESIAN_POINT('Ctrl Pts',(32.2894400315174,-65.7814054021679,
-55.2536310599852));
#180437=CARTESIAN_POINT('Ctrl Pts',(32.2694040627665,-65.784868813089,-55.2560758138285));
#180438=CARTESIAN_POINT('Ctrl Pts',(32.2501597157281,-65.7881843716721,
-55.2596551840712));
#180439=CARTESIAN_POINT('Ctrl Pts',(32.2317985474285,-65.7913520779171,
-55.2641224414877));
#180440=CARTESIAN_POINT('Ctrl Pts',(32.2125512297628,-65.7946726644602,
-55.2688052983293));
#180441=CARTESIAN_POINT('Ctrl Pts',(32.1942741291894,-65.7978307829405,
-55.2744631104736));
#180442=CARTESIAN_POINT('Ctrl Pts',(32.1770162849582,-65.8008264333581,
-55.2808267386599));
#180443=CARTESIAN_POINT('Ctrl Pts',(32.1592871390005,-65.8039038932528,
-55.2873641538449));
#180444=CARTESIAN_POINT('Ctrl Pts',(32.1426330780179,-65.8068098900981,
-55.294645913793));
#180445=CARTESIAN_POINT('Ctrl Pts',(32.127056183543,-65.809544423894,-55.3024055276807));
#180446=CARTESIAN_POINT('Ctrl Pts',(32.1107544016718,-65.8124062121363,
-55.3105262434758));
#180447=CARTESIAN_POINT('Ctrl Pts',(32.0956317582546,-65.8150802075761,
-55.3191697908562));
#180448=CARTESIAN_POINT('Ctrl Pts',(32.0816447916951,-65.8175664102134,
-55.3280667434282));
#180449=CARTESIAN_POINT('Ctrl Pts',(32.0715059985561,-65.8193685947067,
-55.3345159160427));
#180450=CARTESIAN_POINT('Ctrl Pts',(32.0619629273805,-65.8210721048226,
-55.3410990294536));
#180451=CARTESIAN_POINT('Ctrl Pts',(32.052987973319,-65.8226769405612,-55.3477263607061));
#180452=CARTESIAN_POINT('Ctrl Pts',(32.0419258838949,-65.8246549826024,
-55.3558948850746));
#180453=CARTESIAN_POINT('Ctrl Pts',(32.0317269309072,-65.8264831202867,
-55.3641299065953));
#180454=CARTESIAN_POINT('Ctrl Pts',(32.0223264817131,-65.8281613536139,
-55.3722860416806));
#180455=CARTESIAN_POINT('Ctrl Pts',(32.017626257116,-65.8290004702776,-55.3763641092233));
#180456=CARTESIAN_POINT('Ctrl Pts',(32.0131254732844,-65.829802110852,-55.380422842289));
#180457=CARTESIAN_POINT('Ctrl Pts',(32.008815192513,-65.8305662753372,-55.38444633772));
#180458=CARTESIAN_POINT('Ctrl Pts',(32.0066600521273,-65.8309483575797,
-55.3864580854356));
#180459=CARTESIAN_POINT('Ctrl Pts',(32.0045525458112,-65.8313210708,-55.3884610324979));
#180460=CARTESIAN_POINT('Ctrl Pts',(32.0024915002078,-65.831684414998,-55.3904533483158));
#180461=CARTESIAN_POINT('Ctrl Pts',(32.00121209498,-65.831909962878,-55.3916900891568));
#180462=CARTESIAN_POINT('Ctrl Pts',(32.0003718507455,-65.832058977522,-55.3925105847833));
#180463=CARTESIAN_POINT('Ctrl Pts',(31.9991841723761,-65.8322672609766,
-55.3936800811344));
#180464=CARTESIAN_POINT('Ctrl Pts',(31.9984585716465,-65.8323945097593,
-55.3943945737339));
#180465=CARTESIAN_POINT('Ctrl Pts',(31.9976035777943,-65.832543880519,-55.3952396410192));
#180466=CARTESIAN_POINT('Ctrl Pts',(31.9964466094067,-65.832746340525,-55.3963966094067));
#180467=CARTESIAN_POINT('Ctrl Pts',(31.9784887646162,-65.835888816501,-55.4143544541973));
#180468=CARTESIAN_POINT('Ctrl Pts',(31.9620748438882,-65.8387422616958,
-55.4335093827193));
#180469=CARTESIAN_POINT('Ctrl Pts',(31.9473083464221,-65.8413066761094,
-55.4535728211574));
#180470=CARTESIAN_POINT('Ctrl Pts',(31.9323330904136,-65.8439073444429,
-55.473919902631));
#180471=CARTESIAN_POINT('Ctrl Pts',(31.9190520284849,-65.8462107519933,
-55.4952007601908));
#180472=CARTESIAN_POINT('Ctrl Pts',(31.9075195954657,-65.8482168987607,
-55.5171172454247));
#180473=CARTESIAN_POINT('Ctrl Pts',(31.8957341095488,-65.8502670658361,
-55.5395146378605));
#180474=CARTESIAN_POINT('Ctrl Pts',(31.8857746508348,-65.8520067835848,
-55.5625752637249));
#180475=CARTESIAN_POINT('Ctrl Pts',(31.8776461797849,-65.853436052007,-55.5859930894161));
#180476=CARTESIAN_POINT('Ctrl Pts',(31.8694149427853,-65.8548833902637,
-55.6097069800233));
#180477=CARTESIAN_POINT('Ctrl Pts',(31.8630609213692,-65.8560123797269,
-55.6337866410958));
#180478=CARTESIAN_POINT('Ctrl Pts',(31.8585396585789,-65.8568230203966,
-55.6579351489687));
#180479=CARTESIAN_POINT('Ctrl Pts',(31.8539333232147,-65.8576489141696,
-55.6825380378005));
#180480=CARTESIAN_POINT('Ctrl Pts',(31.851228960127,-65.8581443662676,-55.7072119138125));
#180481=CARTESIAN_POINT('Ctrl Pts',(31.8503341986073,-65.8583093766908,
-55.7316719552839));
#180482=CARTESIAN_POINT('Ctrl Pts',(31.8501107931046,-65.8583505767601,
-55.737779177983));
#180483=CARTESIAN_POINT('Ctrl Pts',(31.85,-65.8583711767947,-55.7438732287223));
#180484=CARTESIAN_POINT('Ctrl Pts',(31.85,-65.8583711767947,-55.74995));
#180485=CARTESIAN_POINT('',(31.85,67.7009572055632,-55.74995));
#180486=CARTESIAN_POINT('Origin',(31.85,67.7009572055632,-55.24995));
#180487=CARTESIAN_POINT('',(31.85,-65.8583711767947,-59.64995));
#180488=CARTESIAN_POINT('',(31.85,-65.8583711767947,-55.24995));
#180489=CARTESIAN_POINT('Ctrl Pts',(31.85,-65.8583711767947,-59.64995));
#180490=CARTESIAN_POINT('Ctrl Pts',(31.85,-65.8583711767784,-59.8463349320561));
#180491=CARTESIAN_POINT('Ctrl Pts',(31.85,-65.819181055996,-60.0425718399612));
#180492=CARTESIAN_POINT('Ctrl Pts',(31.85,-65.6683275916687,-60.4053784571341));
#180493=CARTESIAN_POINT('Ctrl Pts',(31.85,-65.5567235699328,-60.5717700902076));
#180494=CARTESIAN_POINT('Ctrl Pts',(31.85,-65.2779827136761,-60.8494502533521));
#180495=CARTESIAN_POINT('Ctrl Pts',(31.85,-65.1109554916676,-60.9606295880612));
#180496=CARTESIAN_POINT('Ctrl Pts',(31.85,-64.7467630120136,-61.1109090094727));
#180497=CARTESIAN_POINT('Ctrl Pts',(31.85,-64.5497765111262,-61.149949999985));
#180498=CARTESIAN_POINT('Ctrl Pts',(31.85,-64.3526414204797,-61.14995));
#180499=CARTESIAN_POINT('Ctrl Pts',(31.85,-65.8583711767947,-59.64995));
#180500=CARTESIAN_POINT('Ctrl Pts',(31.8499999999999,-65.3127169262601,
-59.64995));
#180501=CARTESIAN_POINT('Ctrl Pts',(31.3064221286262,-65.3602738277489,
-59.64995));
#180502=CARTESIAN_POINT('Ctrl Pts',(31.85,-65.8583711767784,-59.8463349320561));
#180503=CARTESIAN_POINT('Ctrl Pts',(31.8499999999999,-65.3127169262533,
-59.7746029379323));
#180504=CARTESIAN_POINT('Ctrl Pts',(31.3064221286269,-65.3602738277488,
-59.7808732880376));
#180505=CARTESIAN_POINT('Ctrl Pts',(31.85,-65.819181055996,-60.0425718399612));
#180506=CARTESIAN_POINT('Ctrl Pts',(31.8499999999999,-65.2892961879233,
-59.8989712332632));
#180507=CARTESIAN_POINT('Ctrl Pts',(31.3075563441358,-65.3340478495507,
-59.9116978933073));
#180508=CARTESIAN_POINT('Ctrl Pts',(31.85,-65.6683275916687,-60.4053784571341));
#180509=CARTESIAN_POINT('Ctrl Pts',(31.8499999999999,-65.1974676446973,
-60.1322291512615));
#180510=CARTESIAN_POINT('Ctrl Pts',(31.3119222489988,-65.2330969061508,
-60.1535689714229));
#180511=CARTESIAN_POINT('Ctrl Pts',(31.85,-65.5567235699328,-60.5717700902076));
#180512=CARTESIAN_POINT('Ctrl Pts',(31.8499999999999,-65.1294009926956,
-60.2406767152616));
#180513=CARTESIAN_POINT('Ctrl Pts',(31.3151522214972,-65.1584116390162,
-60.2644967268053));
#180514=CARTESIAN_POINT('Ctrl Pts',(31.85,-65.2779827136761,-60.8494502533521));
#180515=CARTESIAN_POINT('Ctrl Pts',(31.8499999999999,-64.9553741448238,
-60.4261994932778));
#180516=CARTESIAN_POINT('Ctrl Pts',(31.3232193617865,-64.9718786181899,
-60.4496168355678));
#180517=CARTESIAN_POINT('Ctrl Pts',(31.85,-65.1109554916676,-60.9606295880612));
#180518=CARTESIAN_POINT('Ctrl Pts',(31.8499999999993,-64.8499435605403,
-60.5031527166052));
#180519=CARTESIAN_POINT('Ctrl Pts',(31.3280533572402,-64.8601042170482,
-60.5237363920412));
#180520=CARTESIAN_POINT('Ctrl Pts',(31.85,-64.7467630120136,-61.1109090094727));
#180521=CARTESIAN_POINT('Ctrl Pts',(31.8500000000006,-64.6146765878316,
-60.6120353079394));
#180522=CARTESIAN_POINT('Ctrl Pts',(31.3385935839747,-64.6163870802633,
-60.6239226729814));
#180523=CARTESIAN_POINT('Ctrl Pts',(31.85,-64.5497765111262,-61.149949999985));
#180524=CARTESIAN_POINT('Ctrl Pts',(31.85,-64.4853598419829,-60.6442102195366));
#180525=CARTESIAN_POINT('Ctrl Pts',(31.3442946417934,-64.4845639684081,
-60.64995));
#180526=CARTESIAN_POINT('Ctrl Pts',(31.85,-64.3526414204797,-61.14995));
#180527=CARTESIAN_POINT('Ctrl Pts',(31.8499999999999,-64.3526414204797,
-60.64995));
#180528=CARTESIAN_POINT('Ctrl Pts',(31.35,-64.3526414204797,-60.64995));
#180529=CARTESIAN_POINT('',(31.3064221286262,-65.3602738277489,-59.64995));
#180530=CARTESIAN_POINT('Origin',(31.35,-65.8583711767947,-59.64995));
#180531=CARTESIAN_POINT('Ctrl Pts',(31.35,-64.3526414204797,-60.64995));
#180532=CARTESIAN_POINT('Ctrl Pts',(31.3487470950754,-64.3816118030486,
-60.64995));
#180533=CARTESIAN_POINT('Ctrl Pts',(31.3475587391951,-64.4093403523785,
-60.6487118041122));
#180534=CARTESIAN_POINT('Ctrl Pts',(31.346427856392,-64.4357461897957,-60.6465429519375));
#180535=CARTESIAN_POINT('Ctrl Pts',(31.3452494858262,-64.4632608548783,
-60.6442830258363));
#180536=CARTESIAN_POINT('Ctrl Pts',(31.3441335581122,-64.4893398656373,
-60.6410132280374));
#180537=CARTESIAN_POINT('Ctrl Pts',(31.3430764842574,-64.5139421997014,
-60.6370534671247));
#180538=CARTESIAN_POINT('Ctrl Pts',(31.3421996476743,-64.5343496919854,
-60.6337688685959));
#180539=CARTESIAN_POINT('Ctrl Pts',(31.3413634057054,-64.5537422796669,
-60.6300090684365));
#180540=CARTESIAN_POINT('Ctrl Pts',(31.3405675225963,-64.5721172680631,
-60.6259392754056));
#180541=CARTESIAN_POINT('Ctrl Pts',(31.3395582117953,-64.5954197782508,
-60.6207781078708));
#180542=CARTESIAN_POINT('Ctrl Pts',(31.3386137704587,-64.6170853163577,
-60.6151198747361));
#180543=CARTESIAN_POINT('Ctrl Pts',(31.3377364626481,-64.6371397607276,
-60.6092623723784));
#180544=CARTESIAN_POINT('Ctrl Pts',(31.3374506843755,-64.643672387478,-60.6073543226769));
#180545=CARTESIAN_POINT('Ctrl Pts',(31.3371720492791,-64.6500342866337,
-60.6054247760897));
#180546=CARTESIAN_POINT('Ctrl Pts',(31.3369006858754,-64.6562269271424,
-60.6034830012694));
#180547=CARTESIAN_POINT('Ctrl Pts',(31.3363484762979,-64.66882860943,-60.5995315964807));
#180548=CARTESIAN_POINT('Ctrl Pts',(31.335826363855,-64.6807292206441,-60.595530097897));
#180549=CARTESIAN_POINT('Ctrl Pts',(31.3353356540994,-64.6919436833211,
-60.5915501615662));
#180550=CARTESIAN_POINT('Ctrl Pts',(31.3350902992217,-64.6975509146595,
-60.5895601934008));
#180551=CARTESIAN_POINT('Ctrl Pts',(31.3348527917206,-64.7029865712008,
-60.5875755120395));
#180552=CARTESIAN_POINT('Ctrl Pts',(31.3346233227297,-64.7082528376098,
-60.5856042391339));
#180553=CARTESIAN_POINT('Ctrl Pts',(31.3345085882343,-64.7108859708144,
-60.584618602681));
#180554=CARTESIAN_POINT('Ctrl Pts',(31.3343958631594,-64.7134767541197,
-60.5836363114746));
#180555=CARTESIAN_POINT('Ctrl Pts',(31.3342851709446,-64.7160254554421,
-60.5826583364361));
#180556=CARTESIAN_POINT('Ctrl Pts',(31.3342092440951,-64.7177736801244,
-60.5819875163263));
#180557=CARTESIAN_POINT('Ctrl Pts',(31.3341734959929,-64.7185902026884,
-60.5816721106983));
#180558=CARTESIAN_POINT('Ctrl Pts',(31.3340972739735,-64.7203521872788,
-60.5809867219852));
#180559=CARTESIAN_POINT('Ctrl Pts',(31.3340623734561,-64.7211589643018,
-60.5806728963884));
#180560=CARTESIAN_POINT('Ctrl Pts',(31.3340189765473,-64.7221638367264,
-60.5802811765834));
#180561=CARTESIAN_POINT('Ctrl Pts',(31.3339592160933,-64.7235455787786,
-60.5797383010624));
#180562=CARTESIAN_POINT('Ctrl Pts',(31.3325183894219,-64.7568594287527,
-60.5666495529621));
#180563=CARTESIAN_POINT('Ctrl Pts',(31.3311478367635,-64.7887241291916,
-60.5520895209809));
#180564=CARTESIAN_POINT('Ctrl Pts',(31.3298415410329,-64.8190709044992,
-60.5363617340931));
#180565=CARTESIAN_POINT('Ctrl Pts',(31.3285010284235,-64.8502125778615,
-60.5202219763426));
#180566=CARTESIAN_POINT('Ctrl Pts',(31.3272282106861,-64.8797560794186,
-60.5028529740901));
#180567=CARTESIAN_POINT('Ctrl Pts',(31.3260210452493,-64.9076780624719,
-60.4845643907951));
#180568=CARTESIAN_POINT('Ctrl Pts',(31.3259189711447,-64.9100390573538,
-60.4830179658341));
#180569=CARTESIAN_POINT('Ctrl Pts',(31.3258173688633,-64.912388486247,-60.4814649529386));
#180570=CARTESIAN_POINT('Ctrl Pts',(31.3257162384798,-64.9147263500048,
-60.4799055318768));
#180571=CARTESIAN_POINT('Ctrl Pts',(31.3244849327799,-64.9431908417874,
-60.4609189130664));
#180572=CARTESIAN_POINT('Ctrl Pts',(31.32332326249,-64.9699372570743,-60.4409847513383));
#180573=CARTESIAN_POINT('Ctrl Pts',(31.3222335064864,-64.9949916435422,
-60.420412040864));
#180574=CARTESIAN_POINT('Ctrl Pts',(31.3216886284846,-65.0075188367761,
-60.4101256856269));
#180575=CARTESIAN_POINT('Ctrl Pts',(31.3211617893047,-65.019623711469,-60.3996792360251));
#180576=CARTESIAN_POINT('Ctrl Pts',(31.3206536010315,-65.0313132637831,
-60.3891084432431));
#180577=CARTESIAN_POINT('Ctrl Pts',(31.320416588106,-65.0367651310102,-60.3841783520656));
#180578=CARTESIAN_POINT('Ctrl Pts',(31.3201961142949,-65.0418050198924,
-60.3795181564444));
#180579=CARTESIAN_POINT('Ctrl Pts',(31.319975271238,-65.0468893137778,-60.3747215661699));
#180580=CARTESIAN_POINT('Ctrl Pts',(31.3197604813291,-65.0518342508541,
-60.370056446957));
#180581=CARTESIAN_POINT('Ctrl Pts',(31.3195453554136,-65.0568213438128,
-60.3652622205224));
#180582=CARTESIAN_POINT('Ctrl Pts',(31.3193114502791,-65.0622374643184,
-60.3599307007192));
#180583=CARTESIAN_POINT('Ctrl Pts',(31.3192701938261,-65.0631927657966,
-60.3589903212088));
#180584=CARTESIAN_POINT('Ctrl Pts',(31.319228345048,-65.0641613218921,-60.3580331354422));
#180585=CARTESIAN_POINT('Ctrl Pts',(31.3191857916419,-65.065145128603,-60.3570567811865));
#180586=CARTESIAN_POINT('Ctrl Pts',(31.3178695544998,-65.0955756640795,
-60.3268567607105));
#180587=CARTESIAN_POINT('Ctrl Pts',(31.3166685276156,-65.1238062071651,
-60.2949641541196));
#180588=CARTESIAN_POINT('Ctrl Pts',(31.3155715571072,-65.1497092684046,
-60.2617220236787));
#180589=CARTESIAN_POINT('Ctrl Pts',(31.3144615648519,-65.1759198156724,
-60.2280852877289));
#180590=CARTESIAN_POINT('Ctrl Pts',(31.3134581230547,-65.1997473984253,
-60.1930673110297));
#180591=CARTESIAN_POINT('Ctrl Pts',(31.3125543591512,-65.2211134628954,
-60.1570220982733));
#180592=CARTESIAN_POINT('Ctrl Pts',(31.3116396515752,-65.2427382489321,
-60.1205404142181));
#180593=CARTESIAN_POINT('Ctrl Pts',(31.3108270658856,-65.2618417185149,
-60.0830069551332));
#180594=CARTESIAN_POINT('Ctrl Pts',(31.3101140607359,-65.278394823922,-60.0447796545834));
#180595=CARTESIAN_POINT('Ctrl Pts',(31.3093877892809,-65.2952559194645,
-60.0058410898217));
#180596=CARTESIAN_POINT('Ctrl Pts',(31.3087648557882,-65.3094710608044,
-59.9661831060864));
#180597=CARTESIAN_POINT('Ctrl Pts',(31.3082470591246,-65.3210608090817,
-59.9261671551741));
#180598=CARTESIAN_POINT('Ctrl Pts',(31.3077236909507,-65.3327752634566,
-59.8857206312273));
#180599=CARTESIAN_POINT('Ctrl Pts',(31.3073077631725,-65.3418078518286,
-59.8449088093039));
#180600=CARTESIAN_POINT('Ctrl Pts',(31.3070053121221,-65.3482275697917,
-59.8040810751356));
#180601=CARTESIAN_POINT('Ctrl Pts',(31.3066980640645,-65.3547491073195,
-59.7626057950556));
#180602=CARTESIAN_POINT('Ctrl Pts',(31.3065079517797,-65.3585745879892,
-59.721114479069));
#180603=CARTESIAN_POINT('Ctrl Pts',(31.3064451414349,-65.3598202116218,
-59.6799427686078));
#180604=CARTESIAN_POINT('Ctrl Pts',(31.3064298584737,-65.3601232957331,
-59.6699249020953));
#180605=CARTESIAN_POINT('Ctrl Pts',(31.3064221286262,-65.3602738277488,
-59.6599258026955));
#180606=CARTESIAN_POINT('Ctrl Pts',(31.3064221286262,-65.3602738277488,
-59.64995));
#180607=CARTESIAN_POINT('Origin',(0.,-12.9675000200281,-60.64995));
#180608=CARTESIAN_POINT('',(28.6150130758292,-64.5919217712362,-60.64995));
#180609=CARTESIAN_POINT('Origin',(0.,-12.9675000200281,-60.64995));
#180610=CARTESIAN_POINT('',(4.6996065532056,-66.6842487255793,-60.64995));
#180611=CARTESIAN_POINT('Origin',(0.,-12.9675000200281,-61.64995));
#180612=CARTESIAN_POINT('Ctrl Pts',(28.6150130758292,-64.5919217712362,
-60.64995));
#180613=CARTESIAN_POINT('Ctrl Pts',(28.5105903987178,-64.6227530253959,
-60.64995));
#180614=CARTESIAN_POINT('Ctrl Pts',(28.3946324532739,-64.6568987835949,
-60.6507816129708));
#180615=CARTESIAN_POINT('Ctrl Pts',(28.2034335369725,-64.7128787401875,
-60.6541161203403));
#180616=CARTESIAN_POINT('Ctrl Pts',(28.1035194656054,-64.7420598028733,
-60.6563073997376));
#180617=CARTESIAN_POINT('Ctrl Pts',(27.9794226958293,-64.7781550526993,
-60.6599865693629));
#180618=CARTESIAN_POINT('Ctrl Pts',(27.9154952583806,-64.7967124481223,
-60.6621339738737));
#180619=CARTESIAN_POINT('Ctrl Pts',(27.8876955404672,-64.8047745920356,
-60.6631231848173));
#180620=CARTESIAN_POINT('Ctrl Pts',(27.8690730559331,-64.8101735462903,
-60.6637982981373));
#180621=CARTESIAN_POINT('Ctrl Pts',(27.8582817452337,-64.8133010022486,
-60.6641976300943));
#180622=CARTESIAN_POINT('Ctrl Pts',(27.7228740588381,-64.8525331605392,
-60.6692875251728));
#180623=CARTESIAN_POINT('Ctrl Pts',(27.5316692268163,-64.9075566246321,
-60.6782360197703));
#180624=CARTESIAN_POINT('Ctrl Pts',(27.3086424509084,-64.9713454327537,
-60.6917045527587));
#180625=CARTESIAN_POINT('Ctrl Pts',(27.1971541509212,-65.0031671303415,
-60.6991865024269));
#180626=CARTESIAN_POINT('Ctrl Pts',(27.1414179550069,-65.019063362529,-60.7031131487649));
#180627=CARTESIAN_POINT('Ctrl Pts',(27.1175328956354,-65.0258732819076,
-60.7048356431027));
#180628=CARTESIAN_POINT('Ctrl Pts',(27.1016099604076,-65.0304126589274,
-60.7059927668089));
#180629=CARTESIAN_POINT('Ctrl Pts',(27.0955676348509,-65.0321351095429,
-60.7064341515018));
#180630=CARTESIAN_POINT('Ctrl Pts',(26.4533713134215,-65.2151811972912,
-60.7538140910806));
#180631=CARTESIAN_POINT('Ctrl Pts',(25.9451849881814,-65.3545420411632,
-60.8199026865955));
#180632=CARTESIAN_POINT('Ctrl Pts',(25.5598256882386,-65.4594929016689,
-60.8818893816956));
#180633=CARTESIAN_POINT('Origin',(25.2,67.7009572055632,-55.24995));
#180634=CARTESIAN_POINT('',(25.2,-66.3526821257161,-60.0322609860583));
#180635=CARTESIAN_POINT('Ctrl Pts',(25.2,-65.7473676730038,-61.2659196908451));
#180636=CARTESIAN_POINT('Ctrl Pts',(25.2,-65.7793674058564,-61.2419322158013));
#180637=CARTESIAN_POINT('Ctrl Pts',(25.2,-65.8101247224077,-61.2167624788248));
#180638=CARTESIAN_POINT('Ctrl Pts',(25.2,-65.8397093268158,-61.190493472528));
#180639=CARTESIAN_POINT('Ctrl Pts',(25.2,-65.8701731473596,-61.1634437853781));
#180640=CARTESIAN_POINT('Ctrl Pts',(25.2,-65.8993940496694,-61.1352280130909));
#180641=CARTESIAN_POINT('Ctrl Pts',(25.2,-65.9274189899594,-61.1058889488372));
#180642=CARTESIAN_POINT('Ctrl Pts',(25.2,-65.9536751279189,-61.0784016282335));
#180643=CARTESIAN_POINT('Ctrl Pts',(25.2,-65.9788815373658,-61.0499274395305));
#180644=CARTESIAN_POINT('Ctrl Pts',(25.2,-66.003048363658,-61.0204714365432));
#180645=CARTESIAN_POINT('Ctrl Pts',(25.2,-66.0310884832234,-60.9862944272951));
#180646=CARTESIAN_POINT('Ctrl Pts',(25.2,-66.0577887607455,-60.9507091443266));
#180647=CARTESIAN_POINT('Ctrl Pts',(25.2,-66.0829136816561,-60.9139799086626));
#180648=CARTESIAN_POINT('Ctrl Pts',(25.2,-66.1080535088058,-60.8772288820934));
#180649=CARTESIAN_POINT('Ctrl Pts',(25.2,-66.1316155749522,-60.8393332860652));
#180650=CARTESIAN_POINT('Ctrl Pts',(25.2,-66.1534043153338,-60.8005903813967));
#180651=CARTESIAN_POINT('Ctrl Pts',(25.2,-66.1680937996896,-60.7744707764053));
#180652=CARTESIAN_POINT('Ctrl Pts',(25.2,-66.181978126642,-60.7479667212963));
#180653=CARTESIAN_POINT('Ctrl Pts',(25.2,-66.195009507084,-60.7211749919405));
#180654=CARTESIAN_POINT('Ctrl Pts',(25.2,-66.2246788862433,-60.6601765443753));
#180655=CARTESIAN_POINT('Ctrl Pts',(25.2,-66.2502610540202,-60.5971407842143));
#180656=CARTESIAN_POINT('Ctrl Pts',(25.2,-66.271692317881,-60.5326135007579));
#180657=CARTESIAN_POINT('Ctrl Pts',(25.2,-66.2932651285273,-60.4676600348046));
#180658=CARTESIAN_POINT('Ctrl Pts',(25.2,-66.310632319108,-60.4011940592067));
#180659=CARTESIAN_POINT('Ctrl Pts',(25.2,-66.3236799285615,-60.3337525436261));
#180660=CARTESIAN_POINT('Ctrl Pts',(25.2,-66.3364083911875,-60.2679606594062));
#180661=CARTESIAN_POINT('Ctrl Pts',(25.2,-66.3450260486911,-60.2012392211527));
#180662=CARTESIAN_POINT('Ctrl Pts',(25.2,-66.3493785138873,-60.1340856777927));
#180663=CARTESIAN_POINT('Ctrl Pts',(25.2,-66.3515726828268,-60.1002321689489));
#180664=CARTESIAN_POINT('Ctrl Pts',(25.2,-66.3526821241379,-60.0662689342669));
#180665=CARTESIAN_POINT('Ctrl Pts',(25.2,-66.3526821257161,-60.0322609860583));
#180666=CARTESIAN_POINT('',(25.2,-66.3526821257161,-55.74995));
#180667=CARTESIAN_POINT('',(25.2,-66.3526821257161,-55.24995));
#180668=CARTESIAN_POINT('',(25.2,67.7009572055632,-55.74995));
#180669=CARTESIAN_POINT('Ctrl Pts',(25.2,-65.6297999215446,-61.3450435291692));
#180670=CARTESIAN_POINT('Ctrl Pts',(25.2,-65.4367639336817,-61.0276731545924));
#180671=CARTESIAN_POINT('Ctrl Pts',(25.5556761922697,-65.381444422022,-60.9359047563459));
#180672=CARTESIAN_POINT('Ctrl Pts',(25.2,-65.8726226849417,-61.1992598451423));
#180673=CARTESIAN_POINT('Ctrl Pts',(25.2,-65.616119634334,-60.9126182039811));
#180674=CARTESIAN_POINT('Ctrl Pts',(25.5637941426607,-65.5425594624733,
-60.8363160388081));
#180675=CARTESIAN_POINT('Ctrl Pts',(25.2,-66.0709810864818,-60.9761699132095));
#180676=CARTESIAN_POINT('Ctrl Pts',(25.2,-65.7526726487211,-60.7337823944688));
#180677=CARTESIAN_POINT('Ctrl Pts',(25.5808970595347,-65.6733118931737,
-60.6825252684264));
#180678=CARTESIAN_POINT('Ctrl Pts',(25.2,-66.3190379296928,-60.466180071647));
#180679=CARTESIAN_POINT('Ctrl Pts',(25.2,-65.9037505527713,-60.3438811720847));
#180680=CARTESIAN_POINT('Ctrl Pts',(25.6216004744624,-65.8351484356237,
-60.3310508170863));
#180681=CARTESIAN_POINT('Ctrl Pts',(25.2,-66.3724466929311,-60.1737447607176));
#180682=CARTESIAN_POINT('Ctrl Pts',(25.1999999999999,-65.9181936015569,
-60.1252597984462));
#180683=CARTESIAN_POINT('Ctrl Pts',(25.645585200326,-65.8686915591478,-60.1295475465719));
#180684=CARTESIAN_POINT('Ctrl Pts',(25.2,-66.3461220698509,-59.8897891189412));
#180685=CARTESIAN_POINT('Ctrl Pts',(25.2,-65.8782260298731,-59.9318867276305));
#180686=CARTESIAN_POINT('Ctrl Pts',(25.6688194082641,-65.8491452831382,
-59.9342430075604));
#180687=CARTESIAN_POINT('',(25.6564221281367,-65.8545847710806,-60.0322609860566));
#180688=CARTESIAN_POINT('Ctrl Pts',(25.6564221286262,-65.8545847766702,
-60.0322609860583));
#180689=CARTESIAN_POINT('Ctrl Pts',(25.6426414728709,-65.855767307974,-60.1482566280702));
#180690=CARTESIAN_POINT('Ctrl Pts',(25.631577400267,-65.8390726440188,-60.2474362362412));
#180691=CARTESIAN_POINT('Ctrl Pts',(25.6175941734372,-65.8084997917476,
-60.365156334888));
#180692=CARTESIAN_POINT('Ctrl Pts',(25.6134196234492,-65.7973422361654,
-60.3994162323209));
#180693=CARTESIAN_POINT('Ctrl Pts',(25.6079980779481,-65.781066673351,-60.44373294877));
#180694=CARTESIAN_POINT('Ctrl Pts',(25.6063320607753,-65.775711534389,-60.4573306677679));
#180695=CARTESIAN_POINT('Ctrl Pts',(25.6040646535256,-65.7679639572994,
-60.4760386697017));
#180696=CARTESIAN_POINT('Ctrl Pts',(25.6029888858038,-65.7641608584646,
-60.4849706489919));
#180697=CARTESIAN_POINT('Ctrl Pts',(25.6018397215795,-65.7598809973385,
-60.4946694093824));
#180698=CARTESIAN_POINT('Ctrl Pts',(25.6013703968771,-65.7580836463387,
-60.4986731111241));
#180699=CARTESIAN_POINT('Ctrl Pts',(25.6010627166154,-65.7568939550516,
-60.5013084614098));
#180700=CARTESIAN_POINT('Ctrl Pts',(25.6010641599103,-65.7569055709527,
-60.501290081512));
#180701=CARTESIAN_POINT('Ctrl Pts',(25.5814801284086,-65.6796646649316,
-60.6704949285918));
#180702=CARTESIAN_POINT('Ctrl Pts',(25.5679173424065,-65.5708000415401,
-60.7954955609311));
#180703=CARTESIAN_POINT('Ctrl Pts',(25.5598256882386,-65.4594929016689,
-60.8818893816956));
#180704=CARTESIAN_POINT('Origin',(25.7,-66.3526821257161,-60.0322609860583));
#180705=CARTESIAN_POINT('Ctrl Pts',(41.5,-63.4208871539288,-61.14995));
#180706=CARTESIAN_POINT('Ctrl Pts',(41.4999999999999,-63.4208871539288,
-60.64995));
#180707=CARTESIAN_POINT('Ctrl Pts',(42.,-63.4208871539288,-60.64995));
#180708=CARTESIAN_POINT('Ctrl Pts',(41.5,-63.6180222445752,-61.149949999985));
#180709=CARTESIAN_POINT('Ctrl Pts',(41.5,-63.5520336237608,-60.6556217969809));
#180710=CARTESIAN_POINT('Ctrl Pts',(41.9942946417934,-63.5528097018572,
-60.64995));
#180711=CARTESIAN_POINT('Ctrl Pts',(41.5,-63.8150087454628,-61.1109090094727));
#180712=CARTESIAN_POINT('Ctrl Pts',(41.4999999999993,-63.6863151114373,
-60.6353187454032));
#180713=CARTESIAN_POINT('Ctrl Pts',(41.9885935839755,-63.6846328137124,
-60.6239226729814));
#180714=CARTESIAN_POINT('Ctrl Pts',(41.5,-64.1792012251166,-60.9606295880612));
#180715=CARTESIAN_POINT('Ctrl Pts',(41.5000000000007,-63.9376903302796,
-60.5426326522472));
#180716=CARTESIAN_POINT('Ctrl Pts',(41.9780533572395,-63.9283499504973,
-60.5237363920413));
#180717=CARTESIAN_POINT('Ctrl Pts',(41.5,-64.3462284471252,-60.849450253352));
#180718=CARTESIAN_POINT('Ctrl Pts',(41.5,-64.0549974136357,-60.4706504746468));
#180719=CARTESIAN_POINT('Ctrl Pts',(41.9732193617859,-64.0401243516391,
-60.4496168355678));
#180720=CARTESIAN_POINT('Ctrl Pts',(41.5,-64.6249693033818,-60.5717700902076));
#180721=CARTESIAN_POINT('Ctrl Pts',(41.4999999999999,-64.2519280277007,
-60.2852157712117));
#180722=CARTESIAN_POINT('Ctrl Pts',(41.9651522214979,-64.2266573724653,
-60.2644967268053));
#180723=CARTESIAN_POINT('Ctrl Pts',(41.5,-64.7365733251178,-60.4053784571342));
#180724=CARTESIAN_POINT('Ctrl Pts',(41.5,-64.3319461592471,-60.1718710142637));
#180725=CARTESIAN_POINT('Ctrl Pts',(41.9619222489988,-64.3013426395998,
-60.153568971423));
#180726=CARTESIAN_POINT('Ctrl Pts',(41.5,-64.8874267894451,-60.0425718399611));
#180727=CARTESIAN_POINT('Ctrl Pts',(41.5,-64.4400579753494,-59.9224177216068));
#180728=CARTESIAN_POINT('Ctrl Pts',(41.9575563441358,-64.4022935829999,
-59.9116978933072));
#180729=CARTESIAN_POINT('Ctrl Pts',(41.5,-64.9266169102275,-59.8463349320562));
#180730=CARTESIAN_POINT('Ctrl Pts',(41.5,-64.4684513232201,-59.7861314644994));
#180731=CARTESIAN_POINT('Ctrl Pts',(41.9564221286289,-64.4285195611977,
-59.7808732880376));
#180732=CARTESIAN_POINT('Ctrl Pts',(41.5,-64.9266169102438,-59.64995));
#180733=CARTESIAN_POINT('Ctrl Pts',(41.5,-64.4684513232351,-59.64995));
#180734=CARTESIAN_POINT('Ctrl Pts',(41.9564221286262,-64.428519561198,-59.64995));
#180735=CARTESIAN_POINT('',(41.9564221286262,-64.428519561198,-59.64995));
#180736=CARTESIAN_POINT('',(41.5,-64.9266169102438,-59.64995));
#180737=CARTESIAN_POINT('Origin',(42.,-64.9266169102438,-59.64995));
#180738=CARTESIAN_POINT('Ctrl Pts',(41.5,-63.4208871539288,-61.14995));
#180739=CARTESIAN_POINT('Ctrl Pts',(41.5,-63.6180222445752,-61.149949999985));
#180740=CARTESIAN_POINT('Ctrl Pts',(41.5,-63.8150087454628,-61.1109090094727));
#180741=CARTESIAN_POINT('Ctrl Pts',(41.5,-64.1792012251166,-60.9606295880612));
#180742=CARTESIAN_POINT('Ctrl Pts',(41.5,-64.3462284471252,-60.849450253352));
#180743=CARTESIAN_POINT('Ctrl Pts',(41.5,-64.6249693033818,-60.5717700902076));
#180744=CARTESIAN_POINT('Ctrl Pts',(41.5,-64.7365733251178,-60.4053784571342));
#180745=CARTESIAN_POINT('Ctrl Pts',(41.5,-64.8874267894451,-60.0425718399611));
#180746=CARTESIAN_POINT('Ctrl Pts',(41.5,-64.9266169102275,-59.8463349320562));
#180747=CARTESIAN_POINT('Ctrl Pts',(41.5,-64.9266169102438,-59.64995));
#180748=CARTESIAN_POINT('Ctrl Pts',(41.9564221286262,-64.428519561198,-59.64995));
#180749=CARTESIAN_POINT('Ctrl Pts',(41.9564221286262,-64.428519561198,-59.6947437536983));
#180750=CARTESIAN_POINT('Ctrl Pts',(41.9565549254446,-64.4254489573896,
-59.740006512832));
#180751=CARTESIAN_POINT('Ctrl Pts',(41.9568254006969,-64.4191948742738,
-59.7853172178034));
#180752=CARTESIAN_POINT('Ctrl Pts',(41.9570925832862,-64.413016925991,-59.8300763274576));
#180753=CARTESIAN_POINT('Ctrl Pts',(41.9574941133679,-64.4037325183291,
-59.8748822572172));
#180754=CARTESIAN_POINT('Ctrl Pts',(41.9580343638515,-64.3912405383823,
-59.9192791403161));
#180755=CARTESIAN_POINT('Ctrl Pts',(41.9584577829345,-64.381450000743,-59.9540750139001));
#180756=CARTESIAN_POINT('Ctrl Pts',(41.9589664057685,-64.3696893333576,
-59.9886186673433));
#180757=CARTESIAN_POINT('Ctrl Pts',(41.9595621871816,-64.3559133355721,
-60.0226684875927));
#180758=CARTESIAN_POINT('Ctrl Pts',(41.9596203911713,-64.3545675097113,
-60.0259949347482));
#180759=CARTESIAN_POINT('Ctrl Pts',(41.9596794270429,-64.3532024486048,
-60.0293166614153));
#180760=CARTESIAN_POINT('Ctrl Pts',(41.9597392965673,-64.3518181112998,
-60.0326334323651));
#180761=CARTESIAN_POINT('Ctrl Pts',(41.9605100399423,-64.3339965432011,
-60.0753326062864));
#180762=CARTESIAN_POINT('Ctrl Pts',(41.9614188288922,-64.3129830065508,
-60.1171993183685));
#180763=CARTESIAN_POINT('Ctrl Pts',(41.9624618901908,-64.2888647480389,
-60.1577697839508));
#180764=CARTESIAN_POINT('Ctrl Pts',(41.9634583716055,-64.2658235361815,
-60.1965284983154));
#180765=CARTESIAN_POINT('Ctrl Pts',(41.9645773576394,-64.2399497026142,
-60.2341031968009));
#180766=CARTESIAN_POINT('Ctrl Pts',(41.9658147921719,-64.211337035279,-60.2700569674147));
#180767=CARTESIAN_POINT('Ctrl Pts',(41.9663964129123,-64.1978884686497,
-60.2869560098567));
#180768=CARTESIAN_POINT('Ctrl Pts',(41.9670041917906,-64.1838350586287,
-60.303496408054));
#180769=CARTESIAN_POINT('Ctrl Pts',(41.967637607018,-64.1691888703163,-60.3196288077294));
#180770=CARTESIAN_POINT('Ctrl Pts',(41.9678621341568,-64.1639972256964,
-60.3253472707311));
#180771=CARTESIAN_POINT('Ctrl Pts',(41.9681018562117,-64.1584542355935,
-60.3313130455697));
#180772=CARTESIAN_POINT('Ctrl Pts',(41.9683408943949,-64.1529269486012,
-60.3371156968734));
#180773=CARTESIAN_POINT('Ctrl Pts',(41.9685870780861,-64.1472344358157,
-60.3430918053661));
#180774=CARTESIAN_POINT('Ctrl Pts',(41.9688325293532,-64.1415587421265,
-60.348894747227));
#180775=CARTESIAN_POINT('Ctrl Pts',(41.9690581151941,-64.1363421513913,
-60.3541155158986));
#180776=CARTESIAN_POINT('Ctrl Pts',(41.969101441238,-64.1353402523451,-60.3551182173598));
#180777=CARTESIAN_POINT('Ctrl Pts',(41.9691440297757,-64.1343553976018,
-60.3560995557786));
#180778=CARTESIAN_POINT('Ctrl Pts',(41.9691857390395,-64.1333908643444,
-60.3570567834876));
#180779=CARTESIAN_POINT('Ctrl Pts',(41.9701337860241,-64.1114671293489,
-60.3788144641718));
#180780=CARTESIAN_POINT('Ctrl Pts',(41.9711541356061,-64.087874347133,-60.40019522961));
#180781=CARTESIAN_POINT('Ctrl Pts',(41.972249052733,-64.0625579786825,-60.4209274424502));
#180782=CARTESIAN_POINT('Ctrl Pts',(41.9733241881793,-64.0376989967361,
-60.4412850899425));
#180783=CARTESIAN_POINT('Ctrl Pts',(41.9744712328351,-64.0111778749262,
-60.4610175323995));
#180784=CARTESIAN_POINT('Ctrl Pts',(41.975690944026,-63.9829750168074,-60.4798306482905));
#180785=CARTESIAN_POINT('Ctrl Pts',(41.9768514204353,-63.9561418191073,
-60.4977301128035));
#180786=CARTESIAN_POINT('Ctrl Pts',(41.9780777938133,-63.9277849140972,
-60.5147982848406));
#180787=CARTESIAN_POINT('Ctrl Pts',(41.979369575909,-63.8979155913966,-60.5307488744733));
#180788=CARTESIAN_POINT('Ctrl Pts',(41.9806262844306,-63.8688572598861,
-60.5462663847288));
#180789=CARTESIAN_POINT('Ctrl Pts',(41.981944926866,-63.8383668570856,-60.5607262877677));
#180790=CARTESIAN_POINT('Ctrl Pts',(41.9833234706075,-63.8064913821049,
-60.5738295325114));
#180791=CARTESIAN_POINT('Ctrl Pts',(41.9833461253665,-63.8059675458395,
-60.5740448690607));
#180792=CARTESIAN_POINT('Ctrl Pts',(41.9833687961921,-63.8054433380748,
-60.5742598379184));
#180793=CARTESIAN_POINT('Ctrl Pts',(41.9833914830727,-63.8049187590774,
-60.5744744380238));
#180794=CARTESIAN_POINT('Ctrl Pts',(41.9835053586064,-63.8022856640096,
-60.5755516113038));
#180795=CARTESIAN_POINT('Ctrl Pts',(41.9836502170309,-63.7989358208272,
-60.5769043222385));
#180796=CARTESIAN_POINT('Ctrl Pts',(41.9837705714856,-63.796152507233,-60.5780123789929));
#180797=CARTESIAN_POINT('Ctrl Pts',(41.9838490691014,-63.794337173667,-60.5787350760773));
#180798=CARTESIAN_POINT('Ctrl Pts',(41.9839171188373,-63.79276339423,-60.5793550577177));
#180799=CARTESIAN_POINT('Ctrl Pts',(41.9839591709512,-63.7917907964698,
-60.5797369926548));
#180800=CARTESIAN_POINT('Ctrl Pts',(41.984631713491,-63.7762359692054,-60.5858453060977));
#180801=CARTESIAN_POINT('Ctrl Pts',(41.9853765198597,-63.7590118122209,
-60.5921640965077));
#180802=CARTESIAN_POINT('Ctrl Pts',(41.9861963547554,-63.7400539258389,
-60.598437521158));
#180803=CARTESIAN_POINT('Ctrl Pts',(41.9870302586278,-63.7207707080213,
-60.604818602443));
#180804=CARTESIAN_POINT('Ctrl Pts',(41.9879418325075,-63.6996927220351,
-60.6111530886119));
#180805=CARTESIAN_POINT('Ctrl Pts',(41.9889331213585,-63.6767721831338,
-60.6171173697952));
#180806=CARTESIAN_POINT('Ctrl Pts',(41.9898279798952,-63.6560813018846,
-60.622501459333));
#180807=CARTESIAN_POINT('Ctrl Pts',(41.9907878142519,-63.6338885522843,
-60.6275832961487));
#180808=CARTESIAN_POINT('Ctrl Pts',(41.991813049211,-63.6101837411181,-60.6320843346451));
#180809=CARTESIAN_POINT('Ctrl Pts',(41.9928051926042,-63.5872440514646,
-60.6364400928708));
#180810=CARTESIAN_POINT('Ctrl Pts',(41.9938586054156,-63.5628878131996,
-60.6402518750963));
#180811=CARTESIAN_POINT('Ctrl Pts',(41.9949723254169,-63.5371369349592,
-60.6432310343329));
#180812=CARTESIAN_POINT('Ctrl Pts',(41.9960348122651,-63.5125706441231,
-60.6460731468065));
#180813=CARTESIAN_POINT('Ctrl Pts',(41.9971522002356,-63.4867347319315,
-60.6481573437254));
#180814=CARTESIAN_POINT('Ctrl Pts',(41.9983221479124,-63.4596830378611,
-60.6492010672608));
#180815=CARTESIAN_POINT('Ctrl Pts',(41.9988700534207,-63.4470142899449,
-60.6496898599526));
#180816=CARTESIAN_POINT('Ctrl Pts',(41.999429462942,-63.4340794373293,-60.64995));
#180817=CARTESIAN_POINT('Ctrl Pts',(42.,-63.4208871539288,-60.64995));
#180818=CARTESIAN_POINT('Origin',(41.5,-73.08000002,-177.34995));
#180819=CARTESIAN_POINT('',(41.5,-64.9266169102438,-55.74995));
#180820=CARTESIAN_POINT('',(41.5,-64.9266169102438,-177.34995));
#180821=CARTESIAN_POINT('',(41.5,-73.08000002,-55.74995));
#180822=CARTESIAN_POINT('Origin',(41.,-73.08000002,-55.74995));
#180823=CARTESIAN_POINT('',(41.,-65.0141055737697,-55.24995));
#180824=CARTESIAN_POINT('Ctrl Pts',(41.5,-64.9266169102438,-55.74995));
#180825=CARTESIAN_POINT('Ctrl Pts',(41.5,-64.9266169102438,-55.7240510278259));
#180826=CARTESIAN_POINT('Ctrl Pts',(41.4979000486174,-64.9269843541242,
-55.697853607437));
#180827=CARTESIAN_POINT('Ctrl Pts',(41.49365840434,-64.9277265457027,-55.6716786004013));
#180828=CARTESIAN_POINT('Ctrl Pts',(41.4893809358961,-64.9284750056981,
-55.6452825239533));
#180829=CARTESIAN_POINT('Ctrl Pts',(41.4829253996728,-64.9296045781717,
-55.6189093033718));
#180830=CARTESIAN_POINT('Ctrl Pts',(41.474277574767,-64.9311177514586,-55.5929324719393));
#180831=CARTESIAN_POINT('Ctrl Pts',(41.4710188940119,-64.9316879467069,
-55.583143860168));
#180832=CARTESIAN_POINT('Ctrl Pts',(41.4674492132186,-64.9323125599105,
-55.573411976606));
#180833=CARTESIAN_POINT('Ctrl Pts',(41.463568827898,-64.9329915393618,-55.5637583894376));
#180834=CARTESIAN_POINT('Ctrl Pts',(41.453403314373,-64.9347702737462,-55.5384687177127));
#180835=CARTESIAN_POINT('Ctrl Pts',(41.4410985361824,-64.9369233309436,
-55.5136974848248));
#180836=CARTESIAN_POINT('Ctrl Pts',(41.4266549468271,-64.9394506316016,
-55.4898442374385));
#180837=CARTESIAN_POINT('Ctrl Pts',(41.414938405636,-64.9415007606612,-55.470494645819));
#180838=CARTESIAN_POINT('Ctrl Pts',(41.4018128556624,-64.9437974343114,
-55.4517483676005));
#180839=CARTESIAN_POINT('Ctrl Pts',(41.3872964035339,-64.9463374843029,
-55.4338552806394));
#180840=CARTESIAN_POINT('Ctrl Pts',(41.3794565918151,-64.9477092736019,
-55.4241918703515));
#180841=CARTESIAN_POINT('Ctrl Pts',(41.3712113471472,-64.9491520044747,
-55.4147778016595));
#180842=CARTESIAN_POINT('Ctrl Pts',(41.3625680866767,-64.9506643790888,
-55.4056571306895));
#180843=CARTESIAN_POINT('Ctrl Pts',(41.3608465431265,-64.9509656101776,
-55.4038404976798));
#180844=CARTESIAN_POINT('Ctrl Pts',(41.3587490914835,-64.9513326166609,
-55.4016626948178));
#180845=CARTESIAN_POINT('Ctrl Pts',(41.3569013241922,-64.9516559287514,
-55.3997779182198));
#180846=CARTESIAN_POINT('Ctrl Pts',(41.3555737423086,-64.9518882216793,
-55.3984237459289));
#180847=CARTESIAN_POINT('Ctrl Pts',(41.3543763923405,-64.9520977242419,
-55.3972196111486));
#180848=CARTESIAN_POINT('Ctrl Pts',(41.3535533894273,-64.9522417198603,
-55.3963966082408));
#180849=CARTESIAN_POINT('Ctrl Pts',(41.3437873007902,-64.9539504306672,
-55.3866305196681));
#180850=CARTESIAN_POINT('Ctrl Pts',(41.3328864379011,-64.9558577859898,
-55.3765717208569));
#180851=CARTESIAN_POINT('Ctrl Pts',(41.3207228245913,-64.9579861393597,
-55.3664552895103));
#180852=CARTESIAN_POINT('Ctrl Pts',(41.3090750456328,-64.9600242335483,
-55.3567678756495));
#180853=CARTESIAN_POINT('Ctrl Pts',(41.2962686321262,-64.9622651041163,
-55.3470275906937));
#180854=CARTESIAN_POINT('Ctrl Pts',(41.2822138036231,-64.9647244255877,
-55.3374815440083));
#180855=CARTESIAN_POINT('Ctrl Pts',(41.2689601031572,-64.9670435652432,
-55.3284796238943));
#180856=CARTESIAN_POINT('Ctrl Pts',(41.2545958039182,-64.969557040367,-55.3196505221386));
#180857=CARTESIAN_POINT('Ctrl Pts',(41.2390741346523,-64.9722730049582,
-55.3112377697523));
#180858=CARTESIAN_POINT('Ctrl Pts',(41.2328103975183,-64.9733690267825,
-55.3078428211408));
#180859=CARTESIAN_POINT('Ctrl Pts',(41.2263585547675,-64.9744979589017,
-55.3045160977493));
#180860=CARTESIAN_POINT('Ctrl Pts',(41.2197172105282,-64.9756600435648,
-55.3012753797728));
#180861=CARTESIAN_POINT('Ctrl Pts',(41.204469095489,-64.978328117977,-55.293834892014));
#180862=CARTESIAN_POINT('Ctrl Pts',(41.1882095131135,-64.9811731762401,
-55.2868407235431));
#180863=CARTESIAN_POINT('Ctrl Pts',(41.1709460856378,-64.9841938846355,
-55.2805340045024));
#180864=CARTESIAN_POINT('Ctrl Pts',(41.1541655073744,-64.9871301053663,
-55.2744036811586));
#180865=CARTESIAN_POINT('Ctrl Pts',(41.1364361385031,-64.9902323429417,
-55.2689228588952));
#180866=CARTESIAN_POINT('Ctrl Pts',(41.1178013239113,-64.9934930129889,
-55.26434275797));
#180867=CARTESIAN_POINT('Ctrl Pts',(41.0997555826134,-64.9966506085658,
-55.2599074406232));
#180868=CARTESIAN_POINT('Ctrl Pts',(41.0808605102839,-64.9999568178164,
-55.2563167977781));
#180869=CARTESIAN_POINT('Ctrl Pts',(41.0611938833982,-65.0033980316209,
-55.253827476193));
#180870=CARTESIAN_POINT('Ctrl Pts',(41.0415272565126,-65.0068392454254,
-55.2513381546079));
#180871=CARTESIAN_POINT('Ctrl Pts',(41.0210886481305,-65.0104155384887,
-55.24995));
#180872=CARTESIAN_POINT('Ctrl Pts',(41.,-65.0141055737697,-55.24995));
#180873=CARTESIAN_POINT('',(41.,-73.08000002,-55.24995));
#180874=CARTESIAN_POINT('Origin',(41.5,-73.08000002,-55.24995));
#180875=CARTESIAN_POINT('',(40.5,-65.0578499055327,-55.24995));
#180876=CARTESIAN_POINT('',(40.7958880023324,-65.0319630596553,-55.24995));
#180877=CARTESIAN_POINT('',(40.5,-73.08000002,-55.24995));
#180878=CARTESIAN_POINT('Origin',(40.5,-73.08000002,-55.74995));
#180879=CARTESIAN_POINT('',(40.,-65.1453385690586,-55.74995));
#180880=CARTESIAN_POINT('Ctrl Pts',(40.5,-65.0578499055327,-55.24995));
#180881=CARTESIAN_POINT('Ctrl Pts',(40.478414950197,-65.0616267998515,-55.24995));
#180882=CARTESIAN_POINT('Ctrl Pts',(40.4574879525933,-65.0652537898141,
-55.2513479743296));
#180883=CARTESIAN_POINT('Ctrl Pts',(40.4373682802013,-65.0687308754204,
-55.2538882420756));
#180884=CARTESIAN_POINT('Ctrl Pts',(40.4172805341775,-65.0722024435058,
-55.2564244788652));
#180885=CARTESIAN_POINT('Ctrl Pts',(40.3979969754806,-65.0755245826009,
-55.2600986723959));
#180886=CARTESIAN_POINT('Ctrl Pts',(40.3796086600543,-65.0786972927059,
-55.2646604727422));
#180887=CARTESIAN_POINT('Ctrl Pts',(40.3604151050382,-65.0820089384189,
-55.2694220381108));
#180888=CARTESIAN_POINT('Ctrl Pts',(40.3421966020862,-65.0851577813522,
-55.2751499570335));
#180889=CARTESIAN_POINT('Ctrl Pts',(40.3250003325847,-65.0881438215058,
-55.2815750258559));
#180890=CARTESIAN_POINT('Ctrl Pts',(40.309168402891,-65.0908929513546,-55.2874903342815));
#180891=CARTESIAN_POINT('Ctrl Pts',(40.2942018644216,-65.0935040869392,
-55.2939965089016));
#180892=CARTESIAN_POINT('Ctrl Pts',(40.2801026176646,-65.0959772282596,
-55.3009008476324));
#180893=CARTESIAN_POINT('Ctrl Pts',(40.2636746295662,-65.0988588528511,
-55.3089455606908));
#180894=CARTESIAN_POINT('Ctrl Pts',(40.2484243091612,-65.1015531342264,
-55.3175297931905));
#180895=CARTESIAN_POINT('Ctrl Pts',(40.2343108458121,-65.1040600723857,
-55.3263826814461));
#180896=CARTESIAN_POINT('Ctrl Pts',(40.2231748699736,-65.106038127104,-55.3333678945917));
#180897=CARTESIAN_POINT('Ctrl Pts',(40.2127455890291,-65.1078995472417,
-55.3405210924605));
#180898=CARTESIAN_POINT('Ctrl Pts',(40.2029879734393,-65.1096443327989,
-55.3477263606172));
#180899=CARTESIAN_POINT('Ctrl Pts',(40.1919258839995,-65.111622374843,-55.3558948849923));
#180900=CARTESIAN_POINT('Ctrl Pts',(40.1817269309934,-65.1134505125309,
-55.3641299065234));
#180901=CARTESIAN_POINT('Ctrl Pts',(40.172326481779,-65.1151287458626,-55.3722860416234));
#180902=CARTESIAN_POINT('Ctrl Pts',(40.1676262571718,-65.1159678625284,
-55.3763641091735));
#180903=CARTESIAN_POINT('Ctrl Pts',(40.1631254733296,-65.1167695031052,
-55.3804228422476));
#180904=CARTESIAN_POINT('Ctrl Pts',(40.1588151925472,-65.1175336675929,
-55.3844463376882));
#180905=CARTESIAN_POINT('Ctrl Pts',(40.156660052156,-65.1179157498367,-55.3864580854084));
#180906=CARTESIAN_POINT('Ctrl Pts',(40.1545525458342,-65.1182884630583,
-55.3884610324758));
#180907=CARTESIAN_POINT('Ctrl Pts',(40.1524915002252,-65.1186518072577,
-55.390453348299));
#180908=CARTESIAN_POINT('Ctrl Pts',(40.1512120949914,-65.1188773551389,
-55.3916900891456));
#180909=CARTESIAN_POINT('Ctrl Pts',(40.1503718507489,-65.1190263697845,
-55.3925105847799));
#180910=CARTESIAN_POINT('Ctrl Pts',(40.1491841723718,-65.1192346532407,
-55.3936800811385));
#180911=CARTESIAN_POINT('Ctrl Pts',(40.1484585716412,-65.1193619020236,
-55.3943945737391));
#180912=CARTESIAN_POINT('Ctrl Pts',(40.1476035777893,-65.1195112727835,
-55.3952396410241));
#180913=CARTESIAN_POINT('Ctrl Pts',(40.1464466094067,-65.1197137327888,
-55.3963966094067));
#180914=CARTESIAN_POINT('Ctrl Pts',(40.1284887645886,-65.1228562087736,
-55.4143544542249));
#180915=CARTESIAN_POINT('Ctrl Pts',(40.1120748438341,-65.1257096539755,
-55.4335093827818));
#180916=CARTESIAN_POINT('Ctrl Pts',(40.0973083463449,-65.1282740683946,
-55.4535728212623));
#180917=CARTESIAN_POINT('Ctrl Pts',(40.0823330903159,-65.1308747367331,
-55.4739199027748));
#180918=CARTESIAN_POINT('Ctrl Pts',(40.0690520283695,-65.1331781442871,
-55.4952007603808));
#180919=CARTESIAN_POINT('Ctrl Pts',(40.0575195953378,-65.1351842910565,
-55.5171172456677));
#180920=CARTESIAN_POINT('Ctrl Pts',(40.045734109412,-65.1372344581332,-55.5395146381502));
#180921=CARTESIAN_POINT('Ctrl Pts',(40.0357746506934,-65.138974175882,-55.562575264068));
#180922=CARTESIAN_POINT('Ctrl Pts',(40.0276461796452,-65.1404034443027,
-55.5859930898185));
#180923=CARTESIAN_POINT('Ctrl Pts',(40.0194149426489,-65.1418507825577,
-55.6097069804814));
#180924=CARTESIAN_POINT('Ctrl Pts',(40.0130609212421,-65.1429797720179,
-55.6337866416156));
#180925=CARTESIAN_POINT('Ctrl Pts',(40.0085396584692,-65.1437904126833,
-55.657935149555));
#180926=CARTESIAN_POINT('Ctrl Pts',(40.0039333231242,-65.1446163064516,
-55.6825380384463));
#180927=CARTESIAN_POINT('Ctrl Pts',(40.0012289600629,-65.1451117585439,
-55.7072119145227));
#180928=CARTESIAN_POINT('Ctrl Pts',(40.0003341985789,-65.1452767689602,
-55.7316719560618));
#180929=CARTESIAN_POINT('Ctrl Pts',(40.0001107930952,-65.1453179690258,
-55.7377791785));
#180930=CARTESIAN_POINT('Ctrl Pts',(40.,-65.1453385690586,-55.7438732289798));
#180931=CARTESIAN_POINT('Ctrl Pts',(40.,-65.1453385690586,-55.74995));
#180932=CARTESIAN_POINT('',(40.,67.7009572055632,-55.74995));
#180933=CARTESIAN_POINT('Origin',(40.,67.7009572055632,-55.24995));
#180934=CARTESIAN_POINT('',(40.,-65.1453385690586,-59.64995));
#180935=CARTESIAN_POINT('',(40.,-65.1453385690586,-55.24995));
#180936=CARTESIAN_POINT('Ctrl Pts',(40.,-65.1453385690586,-59.64995));
#180937=CARTESIAN_POINT('Ctrl Pts',(40.,-65.1453385690423,-59.8463349320561));
#180938=CARTESIAN_POINT('Ctrl Pts',(40.,-65.1061484482599,-60.0425718399612));
#180939=CARTESIAN_POINT('Ctrl Pts',(40.,-64.9552949839326,-60.4053784571341));
#180940=CARTESIAN_POINT('Ctrl Pts',(40.,-64.8436909621967,-60.5717700902076));
#180941=CARTESIAN_POINT('Ctrl Pts',(40.,-64.5649501059399,-60.8494502533521));
#180942=CARTESIAN_POINT('Ctrl Pts',(40.,-64.3979228839314,-60.9606295880612));
#180943=CARTESIAN_POINT('Ctrl Pts',(40.,-64.0337304042775,-61.1109090094727));
#180944=CARTESIAN_POINT('Ctrl Pts',(40.,-63.8367439033901,-61.149949999985));
#180945=CARTESIAN_POINT('Ctrl Pts',(40.,-63.6396088127436,-61.14995));
#180946=CARTESIAN_POINT('Ctrl Pts',(33.35,-64.133919761665,-61.14995));
#180947=CARTESIAN_POINT('Ctrl Pts',(33.35,-64.1339197616649,-60.64995));
#180948=CARTESIAN_POINT('Ctrl Pts',(33.85,-64.133919761665,-60.64995));
#180949=CARTESIAN_POINT('Ctrl Pts',(33.35,-64.3310548523114,-61.149949999985));
#180950=CARTESIAN_POINT('Ctrl Pts',(33.35,-64.265066231498,-60.6556217969808));
#180951=CARTESIAN_POINT('Ctrl Pts',(33.8442946417933,-64.2658423095942,
-60.64995));
#180952=CARTESIAN_POINT('Ctrl Pts',(33.35,-64.5280413531989,-61.1109090094727));
#180953=CARTESIAN_POINT('Ctrl Pts',(33.3499999999993,-64.399347719172,-60.6353187454038));
#180954=CARTESIAN_POINT('Ctrl Pts',(33.8385935839748,-64.3976654214474,
-60.6239226729819));
#180955=CARTESIAN_POINT('Ctrl Pts',(33.35,-64.8922338328527,-60.9606295880612));
#180956=CARTESIAN_POINT('Ctrl Pts',(33.3500000000007,-64.6507229380173,
-60.5426326522465));
#180957=CARTESIAN_POINT('Ctrl Pts',(33.8280533572402,-64.6413825582346,
-60.5237363920407));
#180958=CARTESIAN_POINT('Ctrl Pts',(33.35,-65.0592610548614,-60.849450253352));
#180959=CARTESIAN_POINT('Ctrl Pts',(33.35,-64.7680300213717,-60.4706504746468));
#180960=CARTESIAN_POINT('Ctrl Pts',(33.8232193617858,-64.7531569593752,
-60.4496168355678));
#180961=CARTESIAN_POINT('Ctrl Pts',(33.35,-65.338001911118,-60.5717700902076));
#180962=CARTESIAN_POINT('Ctrl Pts',(33.35,-64.9649606354368,-60.2852157712117));
#180963=CARTESIAN_POINT('Ctrl Pts',(33.8151522214979,-64.9396899802014,
-60.2644967268053));
#180964=CARTESIAN_POINT('Ctrl Pts',(33.35,-65.4496059328539,-60.4053784571335));
#180965=CARTESIAN_POINT('Ctrl Pts',(33.35,-65.0449787669832,-60.1718710142623));
#180966=CARTESIAN_POINT('Ctrl Pts',(33.8119222489988,-65.0143752473362,
-60.1535689714224));
#180967=CARTESIAN_POINT('Ctrl Pts',(33.35,-65.6004593971813,-60.0425718399618));
#180968=CARTESIAN_POINT('Ctrl Pts',(33.35,-65.1530905830856,-59.9224177216081));
#180969=CARTESIAN_POINT('Ctrl Pts',(33.8075563441358,-65.1153261907357,
-59.9116978933078));
#180970=CARTESIAN_POINT('Ctrl Pts',(33.35,-65.6396495179636,-59.8463349320557));
#180971=CARTESIAN_POINT('Ctrl Pts',(33.35,-65.1814839309564,-59.7861314644984));
#180972=CARTESIAN_POINT('Ctrl Pts',(33.8064221286289,-65.1415521689339,
-59.7808732880372));
#180973=CARTESIAN_POINT('Ctrl Pts',(33.35,-65.63964951798,-59.64995));
#180974=CARTESIAN_POINT('Ctrl Pts',(33.3499999999999,-65.1814839309712,
-59.64995));
#180975=CARTESIAN_POINT('Ctrl Pts',(33.8064221286261,-65.1415521689341,
-59.64995));
#180976=CARTESIAN_POINT('',(33.8064221286261,-65.1415521689341,-59.64995));
#180977=CARTESIAN_POINT('Ctrl Pts',(33.8064221286261,-65.1415521689341,
-59.64995));
#180978=CARTESIAN_POINT('Ctrl Pts',(33.8064221286261,-65.1415521689341,
-59.6947437540757));
#180979=CARTESIAN_POINT('Ctrl Pts',(33.8065549254468,-65.1384815650739,
-59.740006513579));
#180980=CARTESIAN_POINT('Ctrl Pts',(33.8068254007034,-65.1322274818581,
-59.7853172189021));
#180981=CARTESIAN_POINT('Ctrl Pts',(33.8070925832971,-65.1260495334742,
-59.8300763289218));
#180982=CARTESIAN_POINT('Ctrl Pts',(33.8074941133853,-65.1167651256616,
-59.8748822590296));
#180983=CARTESIAN_POINT('Ctrl Pts',(33.8080343638775,-65.1042731455181,
-59.9192791424491));
#180984=CARTESIAN_POINT('Ctrl Pts',(33.8084577829567,-65.0944826079675,
-59.9540750154215));
#180985=CARTESIAN_POINT('Ctrl Pts',(33.8089664057838,-65.0827219407404,
-59.9886186682484));
#180986=CARTESIAN_POINT('Ctrl Pts',(33.8095621871869,-65.0689459431877,
-60.0226684878905));
#180987=CARTESIAN_POINT('Ctrl Pts',(33.8096203911749,-65.0676001173659,
-60.0259949349465));
#180988=CARTESIAN_POINT('Ctrl Pts',(33.8096794270447,-65.0662350562995,
-60.0293166615144));
#180989=CARTESIAN_POINT('Ctrl Pts',(33.8097392965673,-65.0648507190359,
-60.0326334323651));
#180990=CARTESIAN_POINT('Ctrl Pts',(33.8105100399482,-65.0470291508023,
-60.0753326066097));
#180991=CARTESIAN_POINT('Ctrl Pts',(33.8114188289058,-65.0260156139738,
-60.1171993189902));
#180992=CARTESIAN_POINT('Ctrl Pts',(33.8124618902136,-65.0018973552474,
-60.1577697848382));
#180993=CARTESIAN_POINT('Ctrl Pts',(33.8134583716327,-64.9788561432871,
-60.1965284992851));
#180994=CARTESIAN_POINT('Ctrl Pts',(33.8145773576715,-64.9529823096089,
-60.2341031978335));
#180995=CARTESIAN_POINT('Ctrl Pts',(33.8158147922089,-64.9243696421593,
-60.2700569684901));
#180996=CARTESIAN_POINT('Ctrl Pts',(33.8163964129388,-64.9109210757727,
-60.2869560105797));
#180997=CARTESIAN_POINT('Ctrl Pts',(33.8170041918055,-64.8968676660202,
-60.3034964084361));
#180998=CARTESIAN_POINT('Ctrl Pts',(33.8176376070201,-64.8822214780019,
-60.319628807785));
#180999=CARTESIAN_POINT('Ctrl Pts',(33.8178621341635,-64.8770298332783,
-60.3253472709001));
#181000=CARTESIAN_POINT('Ctrl Pts',(33.8181018562225,-64.8714868430797,
-60.3313130458379));
#181001=CARTESIAN_POINT('Ctrl Pts',(33.8183408944099,-64.8659595559936,
-60.3371156972342));
#181002=CARTESIAN_POINT('Ctrl Pts',(33.8185870781049,-64.8602670431233,
-60.34309180581));
#181003=CARTESIAN_POINT('Ctrl Pts',(33.8188325293759,-64.8545913493511,
-60.3488947477477));
#181004=CARTESIAN_POINT('Ctrl Pts',(33.8190581152215,-64.8493747585253,
-60.3541155165011));
#181005=CARTESIAN_POINT('Ctrl Pts',(33.8191014412564,-64.8483728596886,
-60.3551182177509));
#181006=CARTESIAN_POINT('Ctrl Pts',(33.8191440297855,-64.8473880051467,
-60.3560995559683));
#181007=CARTESIAN_POINT('Ctrl Pts',(33.8191857390412,-64.8464234720805,
-60.3570567834875));
#181008=CARTESIAN_POINT('Ctrl Pts',(33.8201337860552,-64.8244997364875,
-60.3788144647644));
#181009=CARTESIAN_POINT('Ctrl Pts',(33.8211541356638,-64.8009069536454,
-60.400195230713));
#181010=CARTESIAN_POINT('Ctrl Pts',(33.8222490528173,-64.775590584552,-60.4209274439786));
#181011=CARTESIAN_POINT('Ctrl Pts',(33.8233241882501,-64.7507316028861,
-60.4412850911419));
#181012=CARTESIAN_POINT('Ctrl Pts',(33.8244712328871,-64.7242104814626,
-60.4610175332332));
#181013=CARTESIAN_POINT('Ctrl Pts',(33.8256909440562,-64.6960076238503,
-60.479830648753));
#181014=CARTESIAN_POINT('Ctrl Pts',(33.8268514204858,-64.6691744256828,
-60.4977301135459));
#181015=CARTESIAN_POINT('Ctrl Pts',(33.828077793884,-64.640817520206,-60.5147982857993));
#181016=CARTESIAN_POINT('Ctrl Pts',(33.8293695759994,-64.6109481970491,
-60.5307488755859));
#181017=CARTESIAN_POINT('Ctrl Pts',(33.8306262844959,-64.5818898661206,
-60.5462663854435));
#181018=CARTESIAN_POINT('Ctrl Pts',(33.8319449269011,-64.5513994640134,
-60.5607262880999));
#181019=CARTESIAN_POINT('Ctrl Pts',(33.8333234706075,-64.519523989841,-60.5738295325113));
#181020=CARTESIAN_POINT('Ctrl Pts',(33.8333461253679,-64.5190001535445,
-60.5740448690734));
#181021=CARTESIAN_POINT('Ctrl Pts',(33.8333687961948,-64.5184759457487,
-60.5742598379439));
#181022=CARTESIAN_POINT('Ctrl Pts',(33.8333914830767,-64.5179513667201,
-60.574474438062));
#181023=CARTESIAN_POINT('Ctrl Pts',(33.8335053586103,-64.5153182716555,
-60.5755516113404));
#181024=CARTESIAN_POINT('Ctrl Pts',(33.833650217034,-64.5119684284898,-60.5769043222679));
#181025=CARTESIAN_POINT('Ctrl Pts',(33.833770571488,-64.5091851149092,-60.5780123790167));
#181026=CARTESIAN_POINT('Ctrl Pts',(33.8338490691023,-64.5073697813782,
-60.578735076087));
#181027=CARTESIAN_POINT('Ctrl Pts',(33.833917118837,-64.505796001968,-60.5793550577169));
#181028=CARTESIAN_POINT('Ctrl Pts',(33.8339591709511,-64.504823404206,-60.5797369926547));
#181029=CARTESIAN_POINT('Ctrl Pts',(33.8346317135054,-64.4892685766439,
-60.5858453062145));
#181030=CARTESIAN_POINT('Ctrl Pts',(33.8353765198879,-64.4720444193626,
-60.5921640967238));
#181031=CARTESIAN_POINT('Ctrl Pts',(33.8361963547969,-64.4530865326853,
-60.5984375214524));
#181032=CARTESIAN_POINT('Ctrl Pts',(33.837030258674,-64.4338033147713,-60.6048186027495));
#181033=CARTESIAN_POINT('Ctrl Pts',(33.8379418325563,-64.4127253287281,
-60.6111530889097));
#181034=CARTESIAN_POINT('Ctrl Pts',(33.8389331214077,-64.389804789812,-60.6171173700705));
#181035=CARTESIAN_POINT('Ctrl Pts',(33.8398279799534,-64.3691139083493,
-60.6225014596402));
#181036=CARTESIAN_POINT('Ctrl Pts',(33.8407878143187,-64.3469211585411,
-60.6275832964709));
#181037=CARTESIAN_POINT('Ctrl Pts',(33.8418130492861,-64.3232163471738,
-60.6320843349643));
#181038=CARTESIAN_POINT('Ctrl Pts',(33.8428051926872,-64.3002766573262,
-60.636440093187));
#181039=CARTESIAN_POINT('Ctrl Pts',(33.8438586055063,-64.2759204188738,
-60.6402518753928));
#181040=CARTESIAN_POINT('Ctrl Pts',(33.8449723255149,-64.2501695404544,
-60.6432310345922));
#181041=CARTESIAN_POINT('Ctrl Pts',(33.8460348123706,-64.2256032494346,
-60.6460731470319));
#181042=CARTESIAN_POINT('Ctrl Pts',(33.8471522003485,-64.1997673370657,
-60.6481573439003));
#181043=CARTESIAN_POINT('Ctrl Pts',(33.8483221480323,-64.1727156428264,
-60.6492010673677));
#181044=CARTESIAN_POINT('Ctrl Pts',(33.8488700535025,-64.1600468957922,
-60.6496898599907));
#181045=CARTESIAN_POINT('Ctrl Pts',(33.8494294629838,-64.1471120441008,
-60.64995));
#181046=CARTESIAN_POINT('Ctrl Pts',(33.85,-64.133919761665,-60.64995));
#181047=CARTESIAN_POINT('Origin',(33.85,-65.63964951798,-59.64995));
#181048=CARTESIAN_POINT('Ctrl Pts',(40.,-65.1453385690586,-59.64995));
#181049=CARTESIAN_POINT('Ctrl Pts',(39.9999999999999,-64.599684318524,-59.64995));
#181050=CARTESIAN_POINT('Ctrl Pts',(39.4564221286262,-64.6472412200127,
-59.64995));
#181051=CARTESIAN_POINT('Ctrl Pts',(40.,-65.1453385690423,-59.8463349320561));
#181052=CARTESIAN_POINT('Ctrl Pts',(39.9999999999999,-64.5996843185171,
-59.7746029379318));
#181053=CARTESIAN_POINT('Ctrl Pts',(39.4564221286269,-64.6472412200127,
-59.7808732880376));
#181054=CARTESIAN_POINT('Ctrl Pts',(40.,-65.1061484482599,-60.0425718399612));
#181055=CARTESIAN_POINT('Ctrl Pts',(40.,-64.5762635801886,-59.898971233264));
#181056=CARTESIAN_POINT('Ctrl Pts',(39.4575563441365,-64.6210152418146,
-59.9116978933072));
#181057=CARTESIAN_POINT('Ctrl Pts',(40.,-64.9552949839326,-60.4053784571341));
#181058=CARTESIAN_POINT('Ctrl Pts',(39.9999999999999,-64.4844350369598,
-60.1322291512609));
#181059=CARTESIAN_POINT('Ctrl Pts',(39.4619222489981,-64.5200642984147,
-60.153568971423));
#181060=CARTESIAN_POINT('Ctrl Pts',(40.,-64.8436909621967,-60.5717700902076));
#181061=CARTESIAN_POINT('Ctrl Pts',(39.9999999999999,-64.4163683849594,
-60.2406767152616));
#181062=CARTESIAN_POINT('Ctrl Pts',(39.4651522214972,-64.4453790312801,
-60.2644967268053));
#181063=CARTESIAN_POINT('Ctrl Pts',(40.,-64.5649501059399,-60.8494502533521));
#181064=CARTESIAN_POINT('Ctrl Pts',(39.9999999999999,-64.2423415370877,
-60.4261994932778));
#181065=CARTESIAN_POINT('Ctrl Pts',(39.4732193617865,-64.2588460104538,
-60.4496168355678));
#181066=CARTESIAN_POINT('Ctrl Pts',(40.,-64.3979228839314,-60.9606295880612));
#181067=CARTESIAN_POINT('Ctrl Pts',(39.9999999999993,-64.1369109528056,
-60.5031527166045));
#181068=CARTESIAN_POINT('Ctrl Pts',(39.4780533572402,-64.1470716093135,
-60.5237363920406));
#181069=CARTESIAN_POINT('Ctrl Pts',(40.,-64.0337304042775,-61.1109090094727));
#181070=CARTESIAN_POINT('Ctrl Pts',(40.0000000000006,-63.9016439800941,
-60.6120353079401));
#181071=CARTESIAN_POINT('Ctrl Pts',(39.4885935839748,-63.9033544725257,
-60.623922672982));
#181072=CARTESIAN_POINT('Ctrl Pts',(40.,-63.8367439033901,-61.149949999985));
#181073=CARTESIAN_POINT('Ctrl Pts',(39.9999999999999,-63.7723272342478,
-60.6442102195365));
#181074=CARTESIAN_POINT('Ctrl Pts',(39.4942946417933,-63.771531360673,-60.64995));
#181075=CARTESIAN_POINT('Ctrl Pts',(40.,-63.6396088127436,-61.14995));
#181076=CARTESIAN_POINT('Ctrl Pts',(39.9999999999999,-63.6396088127435,
-60.64995));
#181077=CARTESIAN_POINT('Ctrl Pts',(39.5,-63.6396088127436,-60.64995));
#181078=CARTESIAN_POINT('',(39.4564221286262,-64.6472412200127,-59.64995));
#181079=CARTESIAN_POINT('Origin',(39.5,-65.1453385690586,-59.64995));
#181080=CARTESIAN_POINT('Ctrl Pts',(39.5,-63.6396088127436,-60.64995));
#181081=CARTESIAN_POINT('Ctrl Pts',(39.4987470950733,-63.668579195362,-60.64995));
#181082=CARTESIAN_POINT('Ctrl Pts',(39.4975587391908,-63.6963077447446,
-60.648711804108));
#181083=CARTESIAN_POINT('Ctrl Pts',(39.4964278563854,-63.7227135822176,
-60.6465429519245));
#181084=CARTESIAN_POINT('Ctrl Pts',(39.4952494858174,-63.7502282473553,
-60.6442830258145));
#181085=CARTESIAN_POINT('Ctrl Pts',(39.494133558101,-63.7763072581729,-60.6410132280021));
#181086=CARTESIAN_POINT('Ctrl Pts',(39.4930764842437,-63.8009095922985,
-60.6370534670711));
#181087=CARTESIAN_POINT('Ctrl Pts',(39.4921996476724,-63.8213170843124,
-60.6337688685788));
#181088=CARTESIAN_POINT('Ctrl Pts',(39.4913634057138,-63.8407096717578,
-60.6300090684675));
#181089=CARTESIAN_POINT('Ctrl Pts',(39.4905675226138,-63.8590846599517,
-60.6259392754887));
#181090=CARTESIAN_POINT('Ctrl Pts',(39.4895582118083,-63.8823871702473,
-60.6207781079392));
#181091=CARTESIAN_POINT('Ctrl Pts',(39.4886137704671,-63.9040527084652,
-60.6151198747808));
#181092=CARTESIAN_POINT('Ctrl Pts',(39.4877364626516,-63.9241071529484,
-60.6092623723909));
#181093=CARTESIAN_POINT('Ctrl Pts',(39.4874506843826,-63.930639779615,-60.6073543227143));
#181094=CARTESIAN_POINT('Ctrl Pts',(39.4871720492897,-63.9370016786934,
-60.6054247761517));
#181095=CARTESIAN_POINT('Ctrl Pts',(39.486900685889,-63.9431943191312,-60.6034830013555));
#181096=CARTESIAN_POINT('Ctrl Pts',(39.4863484763101,-63.9557960014505,
-60.5995315965609));
#181097=CARTESIAN_POINT('Ctrl Pts',(39.4858263638654,-63.9676966127036,
-60.5955300979674));
#181098=CARTESIAN_POINT('Ctrl Pts',(39.4853356541076,-63.9789110754265,
-60.5915501616224));
#181099=CARTESIAN_POINT('Ctrl Pts',(39.4850902992287,-63.984518306788,-60.5895601934499));
#181100=CARTESIAN_POINT('Ctrl Pts',(39.4848527917264,-63.9899539633539,
-60.5875755120804));
#181101=CARTESIAN_POINT('Ctrl Pts',(39.4846233227342,-63.9952202297894,
-60.5856042391654));
#181102=CARTESIAN_POINT('Ctrl Pts',(39.4845085882381,-63.9978533630071,
-60.5846186027079));
#181103=CARTESIAN_POINT('Ctrl Pts',(39.4843958631624,-64.0004441463261,
-60.5836363114965));
#181104=CARTESIAN_POINT('Ctrl Pts',(39.484285170947,-64.0029928476625,-60.5826583364528));
#181105=CARTESIAN_POINT('Ctrl Pts',(39.4842092440968,-64.0047410723553,
-60.581987516339));
#181106=CARTESIAN_POINT('Ctrl Pts',(39.484173495994,-64.0055575949344,-60.5816721107052));
#181107=CARTESIAN_POINT('Ctrl Pts',(39.484097273974,-64.0073195795363,-60.5809867219877));
#181108=CARTESIAN_POINT('Ctrl Pts',(39.4840623734564,-64.0081263565634,
-60.5806728963894));
#181109=CARTESIAN_POINT('Ctrl Pts',(39.4840189765475,-64.0091312289906,
-60.5802811765833));
#181110=CARTESIAN_POINT('Ctrl Pts',(39.4839592160933,-64.0105129710424,
-60.5797383010624));
#181111=CARTESIAN_POINT('Ctrl Pts',(39.4825183894221,-64.0438268209682,
-60.5666495529811));
#181112=CARTESIAN_POINT('Ctrl Pts',(39.4811478367641,-64.0756915213578,
-60.5520895210254));
#181113=CARTESIAN_POINT('Ctrl Pts',(39.4798415410344,-64.1060382966163,
-60.5363617341694));
#181114=CARTESIAN_POINT('Ctrl Pts',(39.4785010284258,-64.1371799699317,
-60.5202219764498));
#181115=CARTESIAN_POINT('Ctrl Pts',(39.4772282106895,-64.1667234714416,
-60.5028529742347));
#181116=CARTESIAN_POINT('Ctrl Pts',(39.4760210452544,-64.1946454544485,
-60.4845643909836));
#181117=CARTESIAN_POINT('Ctrl Pts',(39.4759189711445,-64.1970064494526,
-60.4830179659437));
#181118=CARTESIAN_POINT('Ctrl Pts',(39.4758173688579,-64.1993558784669,
-60.4814649529687));
#181119=CARTESIAN_POINT('Ctrl Pts',(39.4757162384692,-64.2016937423444,
-60.4799055318267));
#181120=CARTESIAN_POINT('Ctrl Pts',(39.4744780032632,-64.2303184257544,
-60.4608120606792));
#181121=CARTESIAN_POINT('Ctrl Pts',(39.4733101859453,-64.2572056002202,
-60.440760379908));
#181122=CARTESIAN_POINT('Ctrl Pts',(39.4722151146508,-64.2823818764487,
-60.4200646444817));
#181123=CARTESIAN_POINT('Ctrl Pts',(39.4716767714853,-64.2947586744769,
-60.4098905053401));
#181124=CARTESIAN_POINT('Ctrl Pts',(39.4711560693644,-64.3067226760081,
-60.3995602559987));
#181125=CARTESIAN_POINT('Ctrl Pts',(39.4706536010265,-64.3182806560766,
-60.3891084432166));
#181126=CARTESIAN_POINT('Ctrl Pts',(39.4704165881026,-64.3237325232786,
-60.3841783520614));
#181127=CARTESIAN_POINT('Ctrl Pts',(39.4701961142932,-64.3287724121334,
-60.3795181564655));
#181128=CARTESIAN_POINT('Ctrl Pts',(39.4699752712379,-64.3338567059913,
-60.3747215662175));
#181129=CARTESIAN_POINT('Ctrl Pts',(39.4697604813308,-64.3388016430389,
-60.3700564470324));
#181130=CARTESIAN_POINT('Ctrl Pts',(39.4695453554172,-64.3437887359688,
-60.3652622206266));
#181131=CARTESIAN_POINT('Ctrl Pts',(39.4693114502845,-64.3492048564472,
-60.3599307008521));
#181132=CARTESIAN_POINT('Ctrl Pts',(39.4692701938298,-64.350160157969,-60.3589903212992));
#181133=CARTESIAN_POINT('Ctrl Pts',(39.4692283450499,-64.3511287141094,
-60.3580331354884));
#181134=CARTESIAN_POINT('Ctrl Pts',(39.4691857916419,-64.3521125208669,
-60.3570567811865));
#181135=CARTESIAN_POINT('Ctrl Pts',(39.4678695545057,-64.3825430563033,
-60.3268567607499));
#181136=CARTESIAN_POINT('Ctrl Pts',(39.466668527626,-64.4107735993503,-60.2949641542072));
#181137=CARTESIAN_POINT('Ctrl Pts',(39.465571557121,-64.436676660555,-60.2617220238234));
#181138=CARTESIAN_POINT('Ctrl Pts',(39.464461564869,-64.4628872077912,-60.2280852879266));
#181139=CARTESIAN_POINT('Ctrl Pts',(39.4634581230739,-64.4867147905155,
-60.1930673112892));
#181140=CARTESIAN_POINT('Ctrl Pts',(39.4625543591717,-64.5080808549628,
-60.157022098603));
#181141=CARTESIAN_POINT('Ctrl Pts',(39.4616396515968,-64.5297056409793,
-60.1205404146136));
#181142=CARTESIAN_POINT('Ctrl Pts',(39.4608270659075,-64.5488091105469,
-60.0830069556029));
#181143=CARTESIAN_POINT('Ctrl Pts',(39.4601140607574,-64.5653622159461,
-60.0447796551349));
#181144=CARTESIAN_POINT('Ctrl Pts',(39.4593877893017,-64.582223311484,-60.0058410904482));
#181145=CARTESIAN_POINT('Ctrl Pts',(39.4587648558077,-64.5964384528258,
-59.9661831067956));
#181146=CARTESIAN_POINT('Ctrl Pts',(39.4582470591423,-64.6080282011136,
-59.9261671559726));
#181147=CARTESIAN_POINT('Ctrl Pts',(39.4577236909665,-64.6197426555013,
-59.8857206321091));
#181148=CARTESIAN_POINT('Ctrl Pts',(39.4573077631859,-64.6287752438938,
-59.8449088102755));
#181149=CARTESIAN_POINT('Ctrl Pts',(39.457005312133,-64.6351949618876,-59.8040810762024));
#181150=CARTESIAN_POINT('Ctrl Pts',(39.4566980640726,-64.6417164994481,
-59.762605796209));
#181151=CARTESIAN_POINT('Ctrl Pts',(39.4565079517849,-64.6455419801596,
-59.7211144803144));
#181152=CARTESIAN_POINT('Ctrl Pts',(39.4564451414371,-64.646787603845,-59.679942769949));
#181153=CARTESIAN_POINT('Ctrl Pts',(39.4564298584745,-64.6470906879835,
-59.6699249029873));
#181154=CARTESIAN_POINT('Ctrl Pts',(39.4564221286262,-64.6472412200127,
-59.6599258031402));
#181155=CARTESIAN_POINT('Ctrl Pts',(39.4564221286262,-64.6472412200127,
-59.64995));
#181156=CARTESIAN_POINT('Origin',(0.,-12.9675000200281,-60.64995));
#181157=CARTESIAN_POINT('',(4.6996065532056,-66.6842487255793,-60.64995));
#181158=CARTESIAN_POINT('Origin',(-83.2809572255632,10.6199999800001,-55.24995));
#181159=CARTESIAN_POINT('',(54.1729175880533,10.61999998,-55.74995));
#181160=CARTESIAN_POINT('',(-83.2809572255632,10.6199999800001,-55.74995));
#181161=CARTESIAN_POINT('',(54.1729175880533,10.61999998,-60.42825533736));
#181162=CARTESIAN_POINT('',(54.1729175880533,10.61999998,-55.24995));
#181163=CARTESIAN_POINT('Origin',(52.5839997448578,10.6200000169308,-60.4356500018632));
#181164=CARTESIAN_POINT('Ctrl Pts',(54.1724511599876,10.6199999790607,-60.3911473089588));
#181165=CARTESIAN_POINT('Ctrl Pts',(53.416196631659,10.6200463510678,-60.4116134442483));
#181166=CARTESIAN_POINT('Ctrl Pts',(53.7125918503827,9.92402752715887,-60.4035185821655));
#181167=CARTESIAN_POINT('Ctrl Pts',(54.1790134480683,10.6199999790597,-60.6361119980572));
#181168=CARTESIAN_POINT('Ctrl Pts',(53.4174513698511,10.620046463598,-60.5214955398529));
#181169=CARTESIAN_POINT('Ctrl Pts',(53.7172936685715,9.92326040045893,-60.566814107113));
#181170=CARTESIAN_POINT('Ctrl Pts',(54.1205022571197,10.6199999790689,-60.8773492053644));
#181171=CARTESIAN_POINT('Ctrl Pts',(53.4068684094037,10.6200454844905,-60.6288932216045));
#181172=CARTESIAN_POINT('Ctrl Pts',(53.6753724344268,9.93009784663694,-60.727656118488));
#181173=CARTESIAN_POINT('Ctrl Pts',(54.002743499603,10.6199999790876,-61.0954353510634));
#181174=CARTESIAN_POINT('Ctrl Pts',(53.3671997002943,10.6200436156875,-60.7521773893818));
#181175=CARTESIAN_POINT('Ctrl Pts',(53.5909494181196,9.94395845212251,-60.8730306626286));
#181176=CARTESIAN_POINT('',(53.7129480054761,9.92396941324122,-60.42825533736));
#181177=CARTESIAN_POINT('Origin',(54.1729175880533,10.11999998,-60.42825533736));
#181178=CARTESIAN_POINT('Origin',(52.476085995332,10.1269498711132,-60.4132651018033));
#181179=CARTESIAN_POINT('Origin',(0.,-12.9675000200281,-60.64995));
#181180=CARTESIAN_POINT('Origin',(0.,-12.9675000200281,-60.8508735991007));
#181181=CARTESIAN_POINT('Origin',(-83.2809572255632,3.96999998000007,-55.24995));
#181182=CARTESIAN_POINT('',(56.2465221147258,3.96999998000001,-60.42825533736));
#181183=CARTESIAN_POINT('Origin',(54.7700863540663,3.96999970901095,-60.4480774066699));
#181184=CARTESIAN_POINT('',(56.2465221147258,3.96999998000001,-55.74995));
#181185=CARTESIAN_POINT('',(56.2465221147258,3.96999998000001,-55.24995));
#181186=CARTESIAN_POINT('',(-83.2809572255632,3.96999998000007,-55.74995));
#181187=CARTESIAN_POINT('Ctrl Pts',(56.0692321081993,3.96999998739438,-61.1207654305588));
#181188=CARTESIAN_POINT('Ctrl Pts',(55.7339281824781,3.96993431898627,-60.9380383069125));
#181189=CARTESIAN_POINT('Ctrl Pts',(55.6456300835169,4.33828227850038,-60.8898982295148));
#181190=CARTESIAN_POINT('Ctrl Pts',(56.1954681966718,3.96999998716033,-60.8888693966731));
#181191=CARTESIAN_POINT('Ctrl Pts',(55.8351750163154,3.96993697857448,-60.7722679906112));
#181192=CARTESIAN_POINT('Ctrl Pts',(55.7334016533014,4.32662458144452,-60.7353258635364));
#181193=CARTESIAN_POINT('Ctrl Pts',(56.2573698974904,3.96999998704652,-60.6289874486284));
#181194=CARTESIAN_POINT('Ctrl Pts',(55.8870156345094,3.96993824711687,-60.5772788420628));
#181195=CARTESIAN_POINT('Ctrl Pts',(55.7764277962604,4.32095586851412,-60.5620589091497));
#181196=CARTESIAN_POINT('Ctrl Pts',(56.2450717652166,3.96999998706915,-60.3615697395426));
#181197=CARTESIAN_POINT('Ctrl Pts',(55.8768003135833,3.96993799744088,-60.3787010736661));
#181198=CARTESIAN_POINT('Ctrl Pts',(55.7678794768585,4.32208288640323,-60.3838032961762));
#181199=CARTESIAN_POINT('',(55.7689460407313,4.32194224278905,-60.42825533736));
#181200=CARTESIAN_POINT('Origin',(54.4436711570071,4.49782642787904,-60.3799664581841));
#181201=CARTESIAN_POINT('Origin',(56.2465221147258,4.46999998000001,-60.42825533736));
#181202=CARTESIAN_POINT('Origin',(-83.2809572255632,3.46999998000007,-55.74995));
#181203=CARTESIAN_POINT('',(56.5468500449175,3.46999998000001,-55.24995));
#181204=CARTESIAN_POINT('Ctrl Pts',(56.2465221147258,3.96999998000001,-55.74995));
#181205=CARTESIAN_POINT('Ctrl Pts',(56.2465221147258,3.96999998000007,-55.686368912174));
#181206=CARTESIAN_POINT('Ctrl Pts',(56.2546769398593,3.95769679945019,-55.6201894474605));
#181207=CARTESIAN_POINT('Ctrl Pts',(56.2791414152599,3.91807934032033,-55.5254586103449));
#181208=CARTESIAN_POINT('Ctrl Pts',(56.2893349466768,3.90137943739412,-55.4946694819177));
#181209=CARTESIAN_POINT('Ctrl Pts',(56.3076833032272,3.87113398900435,-55.4509423050929));
#181210=CARTESIAN_POINT('Ctrl Pts',(56.3143090986482,3.86018937895708,-55.4367771782512));
#181211=CARTESIAN_POINT('Ctrl Pts',(56.3250123066359,3.84251454883922,-55.4163122595723));
#181212=CARTESIAN_POINT('Ctrl Pts',(56.3305550393438,3.83336299245163,-55.4062755461285));
#181213=CARTESIAN_POINT('Ctrl Pts',(56.3373560360861,3.82214803813549,-55.3949454630808));
#181214=CARTESIAN_POINT('Ctrl Pts',(56.3403424222434,3.81722780003639,-55.3901749729312));
#181215=CARTESIAN_POINT('Ctrl Pts',(56.3423492737411,3.8139225179561,-55.3870140318245));
#181216=CARTESIAN_POINT('Ctrl Pts',(56.3438588567501,3.81143737568338,-55.3846804045353));
#181217=CARTESIAN_POINT('Ctrl Pts',(56.361057122823,3.78313205655798,-55.3583458815392));
#181218=CARTESIAN_POINT('Ctrl Pts',(56.3862681784529,3.74351664372742,-55.3267620226715));
#181219=CARTESIAN_POINT('Ctrl Pts',(56.4537581879826,3.63103405333309,-55.272490622966));
#181220=CARTESIAN_POINT('Ctrl Pts',(56.4960371418825,3.55740103272273,-55.24995));
#181221=CARTESIAN_POINT('Ctrl Pts',(56.5468500449175,3.46999998000001,-55.24995));
#181222=CARTESIAN_POINT('',(60.,3.46999998000001,-55.24995));
#181223=CARTESIAN_POINT('Origin',(60.,28.41999998,-55.24995));
#181224=CARTESIAN_POINT('',(56.6898028749653,2.96999998000001,-55.24995));
#181225=CARTESIAN_POINT('Origin',(0.,-12.9675000200281,-55.24995));
#181226=CARTESIAN_POINT('',(60.,2.96999998000001,-55.24995));
#181227=CARTESIAN_POINT('Origin',(60.,2.96999998000001,-55.74995));
#181228=CARTESIAN_POINT('',(56.9614672388491,2.46999998000001,-55.74995));
#181229=CARTESIAN_POINT('Ctrl Pts',(56.6898028749653,2.96999998000001,-55.24995));
#181230=CARTESIAN_POINT('Ctrl Pts',(56.7016858677395,2.94886603433927,-55.24995));
#181231=CARTESIAN_POINT('Ctrl Pts',(56.7130997678492,2.92831734088818,-55.251290341342));
#181232=CARTESIAN_POINT('Ctrl Pts',(56.7240445752942,2.90849659442475,-55.2537470842863));
#181233=CARTESIAN_POINT('Ctrl Pts',(56.7352878404614,2.8881353492022,-55.2562708209998));
#181234=CARTESIAN_POINT('Ctrl Pts',(56.7460360804399,2.86854206979626,-55.2599719929299));
#181235=CARTESIAN_POINT('Ctrl Pts',(56.7562892952297,2.84981633432805,-55.264608994816));
#181236=CARTESIAN_POINT('Ctrl Pts',(56.7669895691989,2.83027412206672,-55.2694481785837));
#181237=CARTESIAN_POINT('Ctrl Pts',(56.7771507088437,2.81167651123943,-55.2753058962585));
#181238=CARTESIAN_POINT('Ctrl Pts',(56.7867727141642,2.79408090808442,-55.281919573493));
#181239=CARTESIAN_POINT('Ctrl Pts',(56.7966458647433,2.77602603971819,-55.288705875209));
#181240=CARTESIAN_POINT('Ctrl Pts',(56.805951369667,2.75902562801291,-55.2962875599196));
#181241=CARTESIAN_POINT('Ctrl Pts',(56.8146892289353,2.74309056699916,-55.3044030122517));
#181242=CARTESIAN_POINT('Ctrl Pts',(56.8237709347523,2.72652843983979,-55.3128378185799));
#181243=CARTESIAN_POINT('Ctrl Pts',(56.8322394406538,2.71111658244293,-55.3218487259178));
#181244=CARTESIAN_POINT('Ctrl Pts',(56.8400947466399,2.69682129663479,-55.3311739178811));
#181245=CARTESIAN_POINT('Ctrl Pts',(56.8417981058405,2.69372148019865,-55.3331960098984));
#181246=CARTESIAN_POINT('Ctrl Pts',(56.8434726321392,2.69067401918578,-55.3352330097888));
#181247=CARTESIAN_POINT('Ctrl Pts',(56.845118325536,2.68767834227143,-55.3372824669056));
#181248=CARTESIAN_POINT('Ctrl Pts',(56.8513033738781,2.67641961900722,-55.3449849899678));
#181249=CARTESIAN_POINT('Ctrl Pts',(56.8570811575868,2.66589325897712,-55.3528622338493));
#181250=CARTESIAN_POINT('Ctrl Pts',(56.8624516766619,2.6560608759135,-55.3607941971069));
#181251=CARTESIAN_POINT('Ctrl Pts',(56.8651369361995,2.65114468438169,-55.3647601787357));
#181252=CARTESIAN_POINT('Ctrl Pts',(56.8677203795787,2.64640180079946,-55.3687400904442));
#181253=CARTESIAN_POINT('Ctrl Pts',(56.8702020067996,2.64182647258519,-55.3727204292728));
#181254=CARTESIAN_POINT('Ctrl Pts',(56.87144282041,2.63953880847806,-55.3747105986871));
#181255=CARTESIAN_POINT('Ctrl Pts',(56.8726581799808,2.63729303714207,-55.3767008793231));
#181256=CARTESIAN_POINT('Ctrl Pts',(56.8738480855121,2.63508837452534,-55.3786896917009));
#181257=CARTESIAN_POINT('Ctrl Pts',(56.8745753673205,2.63374086333822,-55.3799052731271));
#181258=CARTESIAN_POINT('Ctrl Pts',(56.8750639043184,2.6328406229317,-55.3807258982356));
#181259=CARTESIAN_POINT('Ctrl Pts',(56.8757340298677,2.63159363101243,-55.3818723682905));
#181260=CARTESIAN_POINT('Ctrl Pts',(56.8761602965125,2.63080041985652,-55.382601637521));
#181261=CARTESIAN_POINT('Ctrl Pts',(56.876660038025,2.62986715642403,-55.3834630493362));
#181262=CARTESIAN_POINT('Ctrl Pts',(56.877341439987,2.6285969462065,-55.384650166279));
#181263=CARTESIAN_POINT('Ctrl Pts',(56.8874008790818,2.60984501557851,-55.4021754028516));
#181264=CARTESIAN_POINT('Ctrl Pts',(56.8965581664324,2.59260115861937,-55.4210010720015));
#181265=CARTESIAN_POINT('Ctrl Pts',(56.9048133020388,2.57699487761218,-55.4408432393215));
#181266=CARTESIAN_POINT('Ctrl Pts',(56.9131728876986,2.56119113444783,-55.4609364643509));
#181267=CARTESIAN_POINT('Ctrl Pts',(56.920607347811,2.54706661269637,-55.4820714680664));
#181268=CARTESIAN_POINT('Ctrl Pts',(56.927116682376,2.53470241338362,-55.5039499420776));
#181269=CARTESIAN_POINT('Ctrl Pts',(56.9337559148161,2.5220914786786,-55.5262650148309));
#181270=CARTESIAN_POINT('Ctrl Pts',(56.9394327303715,2.51131172280586,-55.549352923377));
#181271=CARTESIAN_POINT('Ctrl Pts',(56.9441471290424,2.50239512141821,-55.5729028417887));
#181272=CARTESIAN_POINT('Ctrl Pts',(56.9489146230984,2.49337809780968,-55.5967179885095));
#181273=CARTESIAN_POINT('Ctrl Pts',(56.9526978999716,2.48626615248355,-55.6210050571164));
#181274=CARTESIAN_POINT('Ctrl Pts',(56.9554969596619,2.48104061804632,-55.6454572138478));
#181275=CARTESIAN_POINT('Ctrl Pts',(56.9583447950378,2.4757240248062,-55.6703354674975));
#181276=CARTESIAN_POINT('Ctrl Pts',(56.9601738129421,2.47235983313047,-55.6953840925332));
#181277=CARTESIAN_POINT('Ctrl Pts',(56.9609840133748,2.47087968510979,-55.7203032256611));
#181278=CARTESIAN_POINT('Ctrl Pts',(56.961306163691,2.47029115154007,-55.7302115227836));
#181279=CARTESIAN_POINT('Ctrl Pts',(56.9614672388491,2.46999998000001,-55.7400996449202));
#181280=CARTESIAN_POINT('Ctrl Pts',(56.9614672388491,2.46999998000001,-55.74995));
#181281=CARTESIAN_POINT('',(-83.2809572255632,2.46999998000007,-55.74995));
#181282=CARTESIAN_POINT('Origin',(-83.2809572255632,2.46999998000007,-55.24995));
#181283=CARTESIAN_POINT('',(56.9614672388491,2.46999998000001,-60.42825533736));
#181284=CARTESIAN_POINT('',(56.9614672388491,2.46999998000001,-55.24995));
#181285=CARTESIAN_POINT('Origin',(55.5227769329619,2.47000037335106,-60.4517448637211));
#181286=CARTESIAN_POINT('Ctrl Pts',(56.9600934028813,2.46999996959074,-60.3623927486908));
#181287=CARTESIAN_POINT('Ctrl Pts',(56.3127916612335,2.47013219497061,-60.3918959659146));
#181288=CARTESIAN_POINT('Ctrl Pts',(56.4768060379592,1.84328648456651,-60.3843526253219));
#181289=CARTESIAN_POINT('Ctrl Pts',(56.9719086646405,2.46999996957515,-60.6262162467223));
#181290=CARTESIAN_POINT('Ctrl Pts',(56.3176950849992,2.47013256123684,-60.5376645429823));
#181291=CARTESIAN_POINT('Ctrl Pts',(56.4849292473983,1.84234741764349,-60.5602093497011));
#181292=CARTESIAN_POINT('Ctrl Pts',(56.9126832861355,2.46999996965326,-60.8861329835762));
#181293=CARTESIAN_POINT('Ctrl Pts',(56.2937114156122,2.47013073129461,-60.6793039133547));
#181294=CARTESIAN_POINT('Ctrl Pts',(56.4442115172646,1.84705094373349,-60.7334982606779));
#181295=CARTESIAN_POINT('Ctrl Pts',(56.7859903733788,2.46999996982182,-61.1215882796171));
#181296=CARTESIAN_POINT('Ctrl Pts',(56.232192761867,2.47012691510116,-60.8230951160809));
#181297=CARTESIAN_POINT('Ctrl Pts',(56.3570930423877,1.85720121361396,-60.8904421107847));
#181298=CARTESIAN_POINT('',(56.4778207328943,1.84316915851819,-60.42825533736));
#181299=CARTESIAN_POINT('Origin',(56.9614672388491,1.96999998000001,-60.42825533736));
#181300=CARTESIAN_POINT('Origin',(55.1149251185314,2.00184215512154,-60.3653056244591));
#181301=CARTESIAN_POINT('Origin',(0.,-12.9675000200281,-60.64995));
#181302=CARTESIAN_POINT('Origin',(0.,-12.9675000200281,-60.8508735991007));
#181303=CARTESIAN_POINT('Origin',(-83.2809572255632,-4.18000001999993,-55.24995));
#181304=CARTESIAN_POINT('',(58.1504944089282,-4.18000001999999,-60.42825533736));
#181305=CARTESIAN_POINT('Origin',(56.7672600194274,-4.18000063577663,-60.4581517878592));
#181306=CARTESIAN_POINT('',(58.1504944089236,-4.18000003396406,-55.9233081330193));
#181307=CARTESIAN_POINT('',(58.1504944089282,-4.18000001999999,-55.24995));
#181308=CARTESIAN_POINT('Ctrl Pts',(58.150494408916,-4.18000007585629,-55.9233081330339));
#181309=CARTESIAN_POINT('Ctrl Pts',(58.2011234110627,-4.1800000934009,-55.949571966873));
#181310=CARTESIAN_POINT('Ctrl Pts',(58.2508802238442,-4.18000007907268,
-55.9776159745793));
#181311=CARTESIAN_POINT('Ctrl Pts',(58.2996228616342,-4.18000005788133,
-56.007327702339));
#181312=CARTESIAN_POINT('Ctrl Pts',(58.3611066386641,-4.18000003115063,
-56.0448059621868));
#181313=CARTESIAN_POINT('Ctrl Pts',(58.4211714230486,-4.18000002563093,
-56.0849815311994));
#181314=CARTESIAN_POINT('Ctrl Pts',(58.4791990630188,-4.18000002261545,
-56.1275622952347));
#181315=CARTESIAN_POINT('Ctrl Pts',(58.5015978396009,-4.18000002145147,
-56.1439985490754));
#181316=CARTESIAN_POINT('Ctrl Pts',(58.5236932870566,-4.18000002089499,
-56.1607926562338));
#181317=CARTESIAN_POINT('Ctrl Pts',(58.5454508633043,-4.18000002055973,
-56.177925994858));
#181318=CARTESIAN_POINT('Ctrl Pts',(58.601384203271,-4.18000001969785,-56.2219715651514));
#181319=CARTESIAN_POINT('Ctrl Pts',(58.6553029072665,-4.18000001999999,
-56.2682684120419));
#181320=CARTESIAN_POINT('Ctrl Pts',(58.7070968429494,-4.18000001999999,
-56.3167184080419));
#181321=CARTESIAN_POINT('Ctrl Pts',(58.7466278917693,-4.18000001999999,
-56.3536972383227));
#181322=CARTESIAN_POINT('Ctrl Pts',(58.7849870908598,-4.18000001999997,
-56.3919927767765));
#181323=CARTESIAN_POINT('Ctrl Pts',(58.8221712586797,-4.18000002000008,
-56.4316087082659));
#181324=CARTESIAN_POINT('Ctrl Pts',(58.9081478861484,-4.18000002000031,
-56.5232080201017));
#181325=CARTESIAN_POINT('Ctrl Pts',(58.9882663096845,-4.18000002000183,
-56.6226714971191));
#181326=CARTESIAN_POINT('Ctrl Pts',(59.059488987448,-4.18000002000189,-56.7262515801497));
#181327=CARTESIAN_POINT('Ctrl Pts',(59.0864350865984,-4.18000002000191,
-56.7654396488238));
#181328=CARTESIAN_POINT('Ctrl Pts',(59.1121963184049,-4.18000002000164,
-56.8052844356691));
#181329=CARTESIAN_POINT('Ctrl Pts',(59.1367770480425,-4.18000002000115,
-56.845783548759));
#181330=CARTESIAN_POINT('Ctrl Pts',(59.1771662439534,-4.18000002000036,
-56.9123286284587));
#181331=CARTESIAN_POINT('Ctrl Pts',(59.2143783070055,-4.1800000199807,-56.9806361125577));
#181332=CARTESIAN_POINT('Ctrl Pts',(59.2484246951019,-4.18000002050115,
-57.0506994175354));
#181333=CARTESIAN_POINT('Ctrl Pts',(59.3031923634924,-4.18000002133835,
-57.1634045844535));
#181334=CARTESIAN_POINT('Ctrl Pts',(59.3500454603234,-4.18000002397293,
-57.2816264448194));
#181335=CARTESIAN_POINT('Ctrl Pts',(59.3874625053509,-4.18000002286791,
-57.4021771888577));
#181336=CARTESIAN_POINT('Ctrl Pts',(59.3945407287637,-4.18000002265887,
-57.4249819052179));
#181337=CARTESIAN_POINT('Ctrl Pts',(59.4012856253719,-4.18000002232778,
-57.4478436795316));
#181338=CARTESIAN_POINT('Ctrl Pts',(59.4076964194498,-4.18000002192605,
-57.4707623700245));
#181339=CARTESIAN_POINT('Ctrl Pts',(59.4578200392972,-4.18000001878511,
-57.6499551058582));
#181340=CARTESIAN_POINT('Ctrl Pts',(59.4876405140726,-4.18000002000073,
-57.8326096057543));
#181341=CARTESIAN_POINT('Ctrl Pts',(59.4968871656957,-4.18000002000007,
-58.0187658449578));
#181342=CARTESIAN_POINT('Ctrl Pts',(59.4989612576688,-4.18000001999992,
-58.0605220586904));
#181343=CARTESIAN_POINT('Ctrl Pts',(59.5,-4.18000001999999,-58.1024544069542));
#181344=CARTESIAN_POINT('Ctrl Pts',(59.5,-4.18000001999999,-58.1445632485962));
#181345=CARTESIAN_POINT('Ctrl Pts',(57.9789048525842,-4.18000000314622,
-61.1211158812059));
#181346=CARTESIAN_POINT('Ctrl Pts',(57.5947641336392,-4.18011275636211,
-60.9185429056887));
#181347=CARTESIAN_POINT('Ctrl Pts',(57.5408897718184,-3.75014666797429,
-60.8901206419018));
#181348=CARTESIAN_POINT('Ctrl Pts',(58.1017608867775,-4.18000000339119,
-60.8877040749259));
#181349=CARTESIAN_POINT('Ctrl Pts',(57.6864075516799,-4.18011051227318,
-60.7564968901202));
#181350=CARTESIAN_POINT('Ctrl Pts',(57.6237851397972,-3.75639532415342,
-60.7345335560658));
#181351=CARTESIAN_POINT('Ctrl Pts',(58.1609260730227,-4.18000000350811,
-60.6285977191473));
#181352=CARTESIAN_POINT('Ctrl Pts',(57.7319155584137,-4.18010945496987,
-60.5708624589658));
#181353=CARTESIAN_POINT('Ctrl Pts',(57.6637036934156,-3.75937776709444,
-60.5618009361651));
#181354=CARTESIAN_POINT('Ctrl Pts',(58.14915342597,-4.18000000348483,-60.3617046583731));
#181355=CARTESIAN_POINT('Ctrl Pts',(57.7229085994607,-4.18010966305884,
-60.3808564105654));
#181356=CARTESIAN_POINT('Ctrl Pts',(57.6557606890352,-3.75878386386294,
-60.3838931293299));
#181357=CARTESIAN_POINT('',(57.6567521511579,-3.75885801193397,-60.42825533736));
#181358=CARTESIAN_POINT('Origin',(56.2207276362741,-3.65069918556939,-60.3392403554045));
#181359=CARTESIAN_POINT('Origin',(58.1504944089282,-3.68000001999999,-60.42825533736));
#181360=CARTESIAN_POINT('Ctrl Pts',(59.5,-4.18000001999999,-58.1445632485962));
#181361=CARTESIAN_POINT('Ctrl Pts',(59.9999999999999,-4.18000001999999,
-58.144563248596));
#181362=CARTESIAN_POINT('Ctrl Pts',(60.,-4.68000001999999,-58.1445632485961));
#181363=CARTESIAN_POINT('Ctrl Pts',(59.4999999931196,-4.18000001999999,
-57.8907708245007));
#181364=CARTESIAN_POINT('Ctrl Pts',(59.9980183704624,-4.18000001999736,
-57.8406912127677));
#181365=CARTESIAN_POINT('Ctrl Pts',(60.,-4.67801447919764,-57.8400901274889));
#181366=CARTESIAN_POINT('Ctrl Pts',(59.4622668978632,-4.18000001999999,
-57.6432940448109));
#181367=CARTESIAN_POINT('Ctrl Pts',(59.9509926566885,-4.18000002000109,
-57.5443378186833));
#181368=CARTESIAN_POINT('Ctrl Pts',(59.9547202743521,-4.67607375656258,
-57.5431941162335));
#181369=CARTESIAN_POINT('Ctrl Pts',(59.3499835921793,-4.18000001999999,
-57.2816425794726));
#181370=CARTESIAN_POINT('Ctrl Pts',(59.8137304682065,-4.18000001999945,
-57.1117161950833));
#181371=CARTESIAN_POINT('Ctrl Pts',(59.819980312157,-4.67323178879642,-57.1093239470213));
#181372=CARTESIAN_POINT('Ctrl Pts',(59.3031535768727,-4.18000001999999,
-57.163418767372));
#181373=CARTESIAN_POINT('Ctrl Pts',(59.756837410337,-4.18000002,-56.9705421764153));
#181374=CARTESIAN_POINT('Ctrl Pts',(59.7637842928231,-4.67230172637259,
-56.9674919122442));
#181375=CARTESIAN_POINT('Ctrl Pts',(59.1936555403131,-4.18000001999999,
-56.9379996304409));
#181376=CARTESIAN_POINT('Ctrl Pts',(59.6242664035215,-4.18000001999999,
-56.7016181941089));
#181377=CARTESIAN_POINT('Ctrl Pts',(59.6323866477998,-4.67052667748359,
-56.6970587190125));
#181378=CARTESIAN_POINT('Ctrl Pts',(59.130710421318,-4.18000001999999,-56.8298323231333));
#181379=CARTESIAN_POINT('Ctrl Pts',(59.5482752170826,-4.18000001999972,
-56.5726707527956));
#181380=CARTESIAN_POINT('Ctrl Pts',(59.5568525046157,-4.66967405412828,
-56.567291481448));
#181381=CARTESIAN_POINT('Ctrl Pts',(58.9882652846901,-4.18000001999999,
-56.622672397275));
#181382=CARTESIAN_POINT('Ctrl Pts',(59.3766737402574,-4.18000002000027,
-56.3259306460082));
#181383=CARTESIAN_POINT('Ctrl Pts',(59.385918342594,-4.66803974391678,-56.318763868979));
#181384=CARTESIAN_POINT('Ctrl Pts',(58.9081472639374,-4.18000001999999,
-56.5232083679403));
#181385=CARTESIAN_POINT('Ctrl Pts',(59.280338735327,-4.18000002000033,-56.2075385111788));
#181386=CARTESIAN_POINT('Ctrl Pts',(59.289776717509,-4.6672543224009,-56.1994379500303));
#181387=CARTESIAN_POINT('Ctrl Pts',(58.7361948243045,-4.18000001999999,
-56.3400094513659));
#181388=CARTESIAN_POINT('Ctrl Pts',(59.0738973083079,-4.18000001999967,
-55.9896554831564));
#181389=CARTESIAN_POINT('Ctrl Pts',(59.0834337883813,-4.66580663221926,
-55.9796562580523));
#181390=CARTESIAN_POINT('Ctrl Pts',(58.6439367094154,-4.18000001999999,
-56.2554694851693));
#181391=CARTESIAN_POINT('Ctrl Pts',(58.9632803249174,-4.18000001999956,
-55.889161374227));
#181392=CARTESIAN_POINT('Ctrl Pts',(58.9727240508436,-4.66513801841297,
-55.8782346380825));
#181393=CARTESIAN_POINT('Ctrl Pts',(58.3484352743845,-4.18000001999999,
-56.0228947878735));
#181394=CARTESIAN_POINT('Ctrl Pts',(58.6095926714098,-4.18000002000086,
-55.6130627249839));
#181395=CARTESIAN_POINT('Ctrl Pts',(58.6181223301711,-4.66329754200289,
-55.5992175260631));
#181396=CARTESIAN_POINT('Ctrl Pts',(58.1237304207495,-4.18000001999999,
-55.8958235878219));
#181397=CARTESIAN_POINT('Ctrl Pts',(58.3409094947055,-4.18000001999966,
-55.4621795466313));
#181398=CARTESIAN_POINT('Ctrl Pts',(58.3484766058291,-4.66229039631671,
-55.4467718445047));
#181399=CARTESIAN_POINT('Ctrl Pts',(57.8914800739755,-4.18000001999999,
-55.8071084335971));
#181400=CARTESIAN_POINT('Ctrl Pts',(58.0634433345606,-4.18000001999999,
-55.3569201007255));
#181401=CARTESIAN_POINT('Ctrl Pts',(58.0697760887706,-4.66158691772347,
-55.3403413730918));
#181402=CARTESIAN_POINT('',(58.1110275344003,-4.66169335124394,-55.3564444851427));
#181403=CARTESIAN_POINT('Ctrl Pts',(58.1504944089282,-4.18000001999999,
-55.9233081330105));
#181404=CARTESIAN_POINT('Ctrl Pts',(58.1255832655986,-4.18002563226572,
-55.8494414008824));
#181405=CARTESIAN_POINT('Ctrl Pts',(58.106061751409,-4.18906412849159,-55.7771234176855));
#181406=CARTESIAN_POINT('Ctrl Pts',(58.0848889116252,-4.21822496899639,
-55.6769666313789));
#181407=CARTESIAN_POINT('Ctrl Pts',(58.0791815576356,-4.23049738117328,
-55.6450063090449));
#181408=CARTESIAN_POINT('Ctrl Pts',(58.0726729084789,-4.2524838218079,-55.60011339569));
#181409=CARTESIAN_POINT('Ctrl Pts',(58.070845779328,-4.26040501329147,-55.5856570568498));
#181410=CARTESIAN_POINT('Ctrl Pts',(58.0678857794548,-4.27734550201828,
-55.5579032741482));
#181411=CARTESIAN_POINT('Ctrl Pts',(58.0668113719992,-4.2856510384432,-55.5455553613248));
#181412=CARTESIAN_POINT('Ctrl Pts',(58.0626229210173,-4.33677697787841,
-55.4775428495961));
#181413=CARTESIAN_POINT('Ctrl Pts',(58.0657423370089,-4.39105200316426,
-55.4304066092172));
#181414=CARTESIAN_POINT('Ctrl Pts',(58.0816469319102,-4.51822213561182,
-55.3676734969558));
#181415=CARTESIAN_POINT('Ctrl Pts',(58.0943306756589,-4.59067482665232,
-55.3525872058048));
#181416=CARTESIAN_POINT('Ctrl Pts',(58.1110275345658,-4.6616933513699,-55.3564444847807));
#181417=CARTESIAN_POINT('Ctrl Pts',(60.,-4.68000002001403,-58.1445632485962));
#181418=CARTESIAN_POINT('Ctrl Pts',(60.,-4.67968193473502,-58.0957864029195));
#181419=CARTESIAN_POINT('Ctrl Pts',(60.0001069700172,-4.67911123269946,
-57.9996463919644));
#181420=CARTESIAN_POINT('Ctrl Pts',(59.9786990588644,-4.67769206152654,
-57.7800155067677));
#181421=CARTESIAN_POINT('Ctrl Pts',(59.9677216248097,-4.67712392184851,
-57.6942072801069));
#181422=CARTESIAN_POINT('Ctrl Pts',(59.9403282083143,-4.67613383465996,
-57.5467897991993));
#181423=CARTESIAN_POINT('Ctrl Pts',(59.9293574169479,-4.67578123721416,
-57.4945438081253));
#181424=CARTESIAN_POINT('Ctrl Pts',(59.909338151382,-4.67522481561811,-57.4116862694014));
#181425=CARTESIAN_POINT('Ctrl Pts',(59.8984361717243,-4.67493979997739,
-57.3691373259717));
#181426=CARTESIAN_POINT('Ctrl Pts',(59.8839645568739,-4.6745976975898,-57.3175982234888));
#181427=CARTESIAN_POINT('Ctrl Pts',(59.8762657221293,-4.67442462296945,
-57.2913638064885));
#181428=CARTESIAN_POINT('Ctrl Pts',(59.8728643213804,-4.67435005691444,
-57.2800219834145));
#181429=CARTESIAN_POINT('Ctrl Pts',(59.8705737762876,-4.67430026422302,
-57.2724390085803));
#181430=CARTESIAN_POINT('Ctrl Pts',(59.8690658802887,-4.67426782042607,
-57.2674905949537));
#181431=CARTESIAN_POINT('Ctrl Pts',(59.8159468167407,-4.67313231177498,
-57.0941268506631));
#181432=CARTESIAN_POINT('Ctrl Pts',(59.7524064365091,-4.67210570835516,
-56.9412163113079));
#181433=CARTESIAN_POINT('Ctrl Pts',(59.6526118787519,-4.67078986804054,
-56.7405532202682));
#181434=CARTESIAN_POINT('Ctrl Pts',(59.6185865942576,-4.67038626128515,
-56.6783902434988));
#181435=CARTESIAN_POINT('Ctrl Pts',(59.5677476238807,-4.66982743481146,
-56.5920631572585));
#181436=CARTESIAN_POINT('Ctrl Pts',(59.5423750359475,-4.66955952799355,
-56.5506254635554));
#181437=CARTESIAN_POINT('Ctrl Pts',(59.5131167474978,-4.66926458425048,
-56.5052339948439));
#181438=CARTESIAN_POINT('Ctrl Pts',(59.4986034670532,-4.66912113088379,
-56.4832661884672));
#181439=CARTESIAN_POINT('Ctrl Pts',(59.4924114798316,-4.66906046991237,
-56.4740062865164));
#181440=CARTESIAN_POINT('Ctrl Pts',(59.4882900528469,-4.66902020644244,
-56.4678673070977));
#181441=CARTESIAN_POINT('Ctrl Pts',(59.4870552619242,-4.66900815629358,
-56.4660306178073));
#181442=CARTESIAN_POINT('Ctrl Pts',(59.3000750839401,-4.66719140687508,
-56.1897207163246));
#181443=CARTESIAN_POINT('Ctrl Pts',(59.0770215284036,-4.66554103026006,
-55.958077091566));
#181444=CARTESIAN_POINT('Ctrl Pts',(58.6035557387933,-4.66312250108001,
-55.5901274066993));
#181445=CARTESIAN_POINT('Ctrl Pts',(58.3537971827932,-4.66233339403273,
-55.4532846740592));
#181446=CARTESIAN_POINT('Ctrl Pts',(58.1110275345658,-4.6616933513699,-55.3564444847807));
#181447=CARTESIAN_POINT('Ctrl Pts',(60.,-5.2768578914742,-58.1207219873789));
#181448=CARTESIAN_POINT('Ctrl Pts',(60.,-5.19571559048276,-56.120630739736));
#181449=CARTESIAN_POINT('Ctrl Pts',(58.1516269266116,-5.16456703757977,
-55.3528444275806));
#181450=CARTESIAN_POINT('Ctrl Pts',(60.,-5.07672217607537,-58.12884135333));
#181451=CARTESIAN_POINT('Ctrl Pts',(60.0000000000006,-4.99483472640268,
-56.1098379052426));
#181452=CARTESIAN_POINT('Ctrl Pts',(58.1275061007745,-4.96483231244511,
-55.3509116092302));
#181453=CARTESIAN_POINT('Ctrl Pts',(60.,-4.87658373874773,-58.1368637570314));
#181454=CARTESIAN_POINT('Ctrl Pts',(60.,-4.79479350162989,-56.0981738677457));
#181455=CARTESIAN_POINT('Ctrl Pts',(58.1024667524305,-4.76557632116263,
-55.3488500157625));
#181456=CARTESIAN_POINT('Ctrl Pts',(60.,-4.67644015442612,-58.1447026957153));
#181457=CARTESIAN_POINT('Ctrl Pts',(60.,-4.59579029342123,-56.0855524411385));
#181458=CARTESIAN_POINT('Ctrl Pts',(58.076516464363,-4.56684999234778,-55.3466493905885));
#181459=CARTESIAN_POINT('',(58.1702687711893,-5.16134041355483,-55.3608060965004));
#181460=CARTESIAN_POINT('Origin',(-8.53841912444452,-12.9124206793298,-44.4755403801697));
#181461=CARTESIAN_POINT('Ctrl Pts',(58.1702680635503,-5.1613404812212,-55.3608077644985));
#181462=CARTESIAN_POINT('Ctrl Pts',(58.2293679865849,-5.16151080175455,
-55.3858749805777));
#181463=CARTESIAN_POINT('Ctrl Pts',(58.2887638153911,-5.16169733448923,
-55.4133706067893));
#181464=CARTESIAN_POINT('Ctrl Pts',(58.3482572799606,-5.16190080218818,
-55.4433902018123));
#181465=CARTESIAN_POINT('Ctrl Pts',(58.403616216128,-5.1620901297965,-55.4713235699003));
#181466=CARTESIAN_POINT('Ctrl Pts',(58.4590597681318,-5.16229412242843,
-55.5014425932498));
#181467=CARTESIAN_POINT('Ctrl Pts',(58.5143821205383,-5.16251339670694,
-55.533829596536));
#181468=CARTESIAN_POINT('Ctrl Pts',(58.5678568240666,-5.16272534769104,
-55.5651349428123));
#181469=CARTESIAN_POINT('Ctrl Pts',(58.6212186041567,-5.16295157818672,
-55.5985595365485));
#181470=CARTESIAN_POINT('Ctrl Pts',(58.674233727342,-5.16319265297962,-55.6341791820485));
#181471=CARTESIAN_POINT('Ctrl Pts',(58.724850775648,-5.16342282304629,-55.6681876160309));
#181472=CARTESIAN_POINT('Ctrl Pts',(58.7751519844302,-5.16366652617554,
-55.7041972055608));
#181473=CARTESIAN_POINT('Ctrl Pts',(58.8248862984456,-5.16392424073454,
-55.7422722725144));
#181474=CARTESIAN_POINT('Ctrl Pts',(58.8429167479943,-5.16401767138591,
-55.756075832237));
#181475=CARTESIAN_POINT('Ctrl Pts',(58.8608722079922,-5.16411294336124,
-55.7701508313742));
#181476=CARTESIAN_POINT('Ctrl Pts',(58.8787389942346,-5.16421007847508,
-55.7845002009921));
#181477=CARTESIAN_POINT('Ctrl Pts',(58.8877315595404,-5.1642589677293,-55.7917224088159));
#181478=CARTESIAN_POINT('Ctrl Pts',(58.8967002296909,-5.16430831845212,
-55.7990129909257));
#181479=CARTESIAN_POINT('Ctrl Pts',(58.9056418555102,-5.1643581249773,-55.8063711221161));
#181480=CARTESIAN_POINT('Ctrl Pts',(58.9547410211116,-5.16463161649632,
-55.8467751950593));
#181481=CARTESIAN_POINT('Ctrl Pts',(59.0032025284632,-5.16491917470784,
-55.8892637408267));
#181482=CARTESIAN_POINT('Ctrl Pts',(59.0507464151713,-5.16522063109444,
-55.9338141127236));
#181483=CARTESIAN_POINT('Ctrl Pts',(59.0851940552815,-5.16543904952494,
-55.9660928194963));
#181484=CARTESIAN_POINT('Ctrl Pts',(59.1191606577678,-5.1656647588043,-55.9994531466577));
#181485=CARTESIAN_POINT('Ctrl Pts',(59.1525514248973,-5.16589760591263,
-56.0338733480834));
#181486=CARTESIAN_POINT('Ctrl Pts',(59.1688316709293,-5.16601113454756,
-56.0506555126113));
#181487=CARTESIAN_POINT('Ctrl Pts',(59.1849751809062,-5.16612635884093,
-56.0676894609806));
#181488=CARTESIAN_POINT('Ctrl Pts',(59.2009718553721,-5.16624325431463,
-56.084971674898));
#181489=CARTESIAN_POINT('Ctrl Pts',(59.2086173598447,-5.16629912373104,
-56.0932315944259));
#181490=CARTESIAN_POINT('Ctrl Pts',(59.2162292961149,-5.16635537467518,
-56.1015481927566));
#181491=CARTESIAN_POINT('Ctrl Pts',(59.223804757728,-5.16641198994052,-56.1099189366056));
#181492=CARTESIAN_POINT('Ctrl Pts',(59.2616457504517,-5.16669479486428,
-56.1517325280744));
#181493=CARTESIAN_POINT('Ctrl Pts',(59.2986201578731,-5.16698737347321,
-56.1949983504194));
#181494=CARTESIAN_POINT('Ctrl Pts',(59.334592750423,-5.16728901377668,-56.2396124277012));
#181495=CARTESIAN_POINT('Ctrl Pts',(59.3627978021414,-5.16752552106615,
-56.2745930134168));
#181496=CARTESIAN_POINT('Ctrl Pts',(59.3903847865505,-5.16776758215009,
-56.3103999425124));
#181497=CARTESIAN_POINT('Ctrl Pts',(59.4172896232573,-5.16801502688971,
-56.347008807102));
#181498=CARTESIAN_POINT('Ctrl Pts',(59.4307420416106,-5.16813874925952,
-56.3653132393969));
#181499=CARTESIAN_POINT('Ctrl Pts',(59.4440233093318,-5.16826381502988,
-56.3838177857316));
#181500=CARTESIAN_POINT('Ctrl Pts',(59.4571231780776,-5.16839020075939,
-56.4025190864527));
#181501=CARTESIAN_POINT('Ctrl Pts',(59.4636731124505,-5.16845339362415,
-56.4118697368133));
#181502=CARTESIAN_POINT('Ctrl Pts',(59.4701776705325,-5.16851691642642,
-56.4212695681817));
#181503=CARTESIAN_POINT('Ctrl Pts',(59.4766354471753,-5.1685807662935,-56.4307181700234));
#181504=CARTESIAN_POINT('Ctrl Pts',(59.4798643354967,-5.16861269122705,
-56.4354424709443));
#181505=CARTESIAN_POINT('Ctrl Pts',(59.4830815277213,-5.16864469793323,
-56.4401789654471));
#181506=CARTESIAN_POINT('Ctrl Pts',(59.4862868401399,-5.1686767860573,-56.444927602916));
#181507=CARTESIAN_POINT('Ctrl Pts',(59.4881839064004,-5.1686957774346,-56.4477380871213));
#181508=CARTESIAN_POINT('Ctrl Pts',(59.4900768113164,-5.16871479733262,
-56.4505528250125));
#181509=CARTESIAN_POINT('Ctrl Pts',(59.4919655159692,-5.16873384567906,
-56.453371806289));
#181510=CARTESIAN_POINT('Ctrl Pts',(59.4923738111192,-5.16873796349995,
-56.453981206166));
#181511=CARTESIAN_POINT('Ctrl Pts',(59.4927819099767,-5.1687420826503,-56.4545908043469));
#181512=CARTESIAN_POINT('Ctrl Pts',(59.4931898121432,-5.16874620312938,
-56.4552006007266));
#181513=CARTESIAN_POINT('Ctrl Pts',(59.4935348212275,-5.16874968828546,
-56.4557163746249));
#181514=CARTESIAN_POINT('Ctrl Pts',(59.4938768919222,-5.16875314605702,
-56.4562280969254));
#181515=CARTESIAN_POINT('Ctrl Pts',(59.4942319876593,-5.16875673802937,
-56.4567596810523));
#181516=CARTESIAN_POINT('Ctrl Pts',(59.4947963331228,-5.16876244666815,
-56.4576045154423));
#181517=CARTESIAN_POINT('Ctrl Pts',(59.4953854025968,-5.16876841190205,
-56.4584873269797));
#181518=CARTESIAN_POINT('Ctrl Pts',(59.4959812520547,-5.16877445315147,
-56.459381391727));
#181519=CARTESIAN_POINT('Ctrl Pts',(59.4976582299457,-5.16879145583827,
-56.4618976763262));
#181520=CARTESIAN_POINT('Ctrl Pts',(59.4993887673974,-5.16880906498809,
-56.4645037433353));
#181521=CARTESIAN_POINT('Ctrl Pts',(59.5007780026249,-5.16882323807628,
-56.4666013076562));
#181522=CARTESIAN_POINT('Ctrl Pts',(59.5012057242936,-5.16882760172673,
-56.4672471116884));
#181523=CARTESIAN_POINT('Ctrl Pts',(59.5016011421813,-5.16883163948576,
-56.4678446867341));
#181524=CARTESIAN_POINT('Ctrl Pts',(59.5019528364327,-5.1688352329881,-56.4683765142999));
#181525=CARTESIAN_POINT('Ctrl Pts',(59.5020914168666,-5.16883664895982,
-56.4685860738663));
#181526=CARTESIAN_POINT('Ctrl Pts',(59.5022224204933,-5.16883798787953,
-56.4687842301391));
#181527=CARTESIAN_POINT('Ctrl Pts',(59.5023556731693,-5.16883935012867,
-56.4689858392624));
#181528=CARTESIAN_POINT('Ctrl Pts',(59.5367190266159,-5.1691906485059,-56.5209770320496));
#181529=CARTESIAN_POINT('Ctrl Pts',(59.5720464018835,-5.16957535427328,
-56.5779234018272));
#181530=CARTESIAN_POINT('Ctrl Pts',(59.6073637659921,-5.16999470741441,
-56.6400158796074));
#181531=CARTESIAN_POINT('Ctrl Pts',(59.6250224480463,-5.17020438398497,
-56.6710621184975));
#181532=CARTESIAN_POINT('Ctrl Pts',(59.6426779759392,-5.17042272465395,
-56.7033952452903));
#181533=CARTESIAN_POINT('Ctrl Pts',(59.6602057424287,-5.17064989395518,
-56.737040707197));
#181534=CARTESIAN_POINT('Ctrl Pts',(59.6692056644245,-5.17076653779524,
-56.7543165268432));
#181535=CARTESIAN_POINT('Ctrl Pts',(59.678171880244,-5.17088550935595,-56.7719383531722));
#181536=CARTESIAN_POINT('Ctrl Pts',(59.6870874171233,-5.17100683121914,
-56.7899096887854));
#181537=CARTESIAN_POINT('Ctrl Pts',(59.6949339875807,-5.17111360667871,
-56.8057262742597));
#181538=CARTESIAN_POINT('Ctrl Pts',(59.7027422687428,-5.17122221778135,
-56.8218158271959));
#181539=CARTESIAN_POINT('Ctrl Pts',(59.7104915013929,-5.1713325453633,-56.8381608041646));
#181540=CARTESIAN_POINT('Ctrl Pts',(59.7110853572087,-5.17134100022317,
-56.8394133874938));
#181541=CARTESIAN_POINT('Ctrl Pts',(59.7116788790019,-5.17134946533307,
-56.8406674959841));
#181542=CARTESIAN_POINT('Ctrl Pts',(59.7122720621043,-5.17135794070217,
-56.8419231310425));
#181543=CARTESIAN_POINT('Ctrl Pts',(59.7310456793957,-5.17162617716265,
-56.8816626515144));
#181544=CARTESIAN_POINT('Ctrl Pts',(59.7495101056959,-5.17190543441427,
-56.9230417182683));
#181545=CARTESIAN_POINT('Ctrl Pts',(59.7674630265172,-5.17219523865143,
-56.9659917048944));
#181546=CARTESIAN_POINT('Ctrl Pts',(59.7767445993801,-5.17234506603439,
-56.9881966393615));
#181547=CARTESIAN_POINT('Ctrl Pts',(59.7858882493597,-5.1724976925733,-57.0108185107494));
#181548=CARTESIAN_POINT('Ctrl Pts',(59.7948671257502,-5.17265307882307,
-57.0338517122053));
#181549=CARTESIAN_POINT('Ctrl Pts',(59.81336526154,-5.17297320305947,-57.0813043409843));
#181550=CARTESIAN_POINT('Ctrl Pts',(59.831174391683,-5.17330518579884,-57.1305243118636));
#181551=CARTESIAN_POINT('Ctrl Pts',(59.8480354461201,-5.1736486439555,-57.1814572501127));
#181552=CARTESIAN_POINT('Ctrl Pts',(59.8557610573697,-5.17380601395919,
-57.204794348168));
#181553=CARTESIAN_POINT('Ctrl Pts',(59.8632871078165,-5.1739657909383,-57.2284907502416));
#181554=CARTESIAN_POINT('Ctrl Pts',(59.8705856169753,-5.17412792478141,
-57.2525392933092));
#181555=CARTESIAN_POINT('Ctrl Pts',(59.8708716782384,-5.1741342795329,-57.2534818634225));
#181556=CARTESIAN_POINT('Ctrl Pts',(59.8711094072179,-5.17413957064867,
-57.2542666695859));
#181557=CARTESIAN_POINT('Ctrl Pts',(59.8713509930359,-5.17414495466206,
-57.255065256389));
#181558=CARTESIAN_POINT('Ctrl Pts',(59.8717781024019,-5.17415447327771,
-57.2564771103876));
#181559=CARTESIAN_POINT('Ctrl Pts',(59.8722177914959,-5.17416428149958,
-57.2579319209848));
#181560=CARTESIAN_POINT('Ctrl Pts',(59.8729531199112,-5.17418077643834,
-57.260378593094));
#181561=CARTESIAN_POINT('Ctrl Pts',(59.8901771646284,-5.1745671474214,-57.3176884820356));
#181562=CARTESIAN_POINT('Ctrl Pts',(59.9047902755263,-5.17494006942135,
-57.3723845060344));
#181563=CARTESIAN_POINT('Ctrl Pts',(59.9172918928915,-5.17529687618782,
-57.4243847420007));
#181564=CARTESIAN_POINT('Ctrl Pts',(59.9297460126649,-5.17565232733272,
-57.4761874126511));
#181565=CARTESIAN_POINT('Ctrl Pts',(59.940104664728,-5.17599178574173,-57.5253147523025));
#181566=CARTESIAN_POINT('Ctrl Pts',(59.9488107393967,-5.17631268775669,
-57.5716951741607));
#181567=CARTESIAN_POINT('Ctrl Pts',(59.957500830105,-5.17663300061002,-57.6179904436559));
#181568=CARTESIAN_POINT('Ctrl Pts',(59.9645444268708,-5.17693482538332,
-57.6615488807856));
#181569=CARTESIAN_POINT('Ctrl Pts',(59.9703309265957,-5.17721568088245,
-57.7023085376325));
#181570=CARTESIAN_POINT('Ctrl Pts',(59.9761053124188,-5.17749594841716,
-57.7429828650907));
#181571=CARTESIAN_POINT('Ctrl Pts',(59.9806278704376,-5.17775533461081,
-57.780870126715));
#181572=CARTESIAN_POINT('Ctrl Pts',(59.9842344277409,-5.17799143846795,
-57.8159178531054));
#181573=CARTESIAN_POINT('Ctrl Pts',(59.9853062159365,-5.17806160325551,
-57.8263332537956));
#181574=CARTESIAN_POINT('Ctrl Pts',(59.9862967636936,-5.17812971229608,
-57.8364979428509));
#181575=CARTESIAN_POINT('Ctrl Pts',(59.9872140100181,-5.17819570363422,
-57.8464106967552));
#181576=CARTESIAN_POINT('Ctrl Pts',(59.9902384336499,-5.1784132959616,-57.8790958832314));
#181577=CARTESIAN_POINT('Ctrl Pts',(59.9924757817619,-5.17861044222754,
-57.9091051245478));
#181578=CARTESIAN_POINT('Ctrl Pts',(59.9941764596193,-5.17878851414488,
-57.9364589604608));
#181579=CARTESIAN_POINT('Ctrl Pts',(59.9959106434735,-5.17897009435573,
-57.9643517094501));
#181580=CARTESIAN_POINT('Ctrl Pts',(59.9970867643637,-5.17913184124641,
-57.989483403455));
#181581=CARTESIAN_POINT('Ctrl Pts',(59.9979167550151,-5.17927526458926,
-58.0118850205988));
#181582=CARTESIAN_POINT('Ctrl Pts',(59.9987570399822,-5.17942046680174,
-58.0345644834223));
#181583=CARTESIAN_POINT('Ctrl Pts',(59.9992424352802,-5.17954688819776,
-58.0544457527));
#181584=CARTESIAN_POINT('Ctrl Pts',(59.9995397872028,-5.17965615075566,
-58.0715700091907));
#181585=CARTESIAN_POINT('Ctrl Pts',(59.999842885112,-5.17976752468784,-58.0890251724035));
#181586=CARTESIAN_POINT('Ctrl Pts',(59.9999505202322,-5.17986107023935,
-58.1036157585654));
#181587=CARTESIAN_POINT('Ctrl Pts',(59.9999860523665,-5.17993856173551,
-58.1153944010507));
#181588=CARTESIAN_POINT('Ctrl Pts',(59.9999960187236,-5.17996029721361,
-58.11869817551));
#181589=CARTESIAN_POINT('Ctrl Pts',(60.,-5.17998076999238,-58.121780776237));
#181590=CARTESIAN_POINT('Ctrl Pts',(60.,-5.18000001999999,-58.1246434856214));
#181591=CARTESIAN_POINT('Ctrl Pts',(60.,-5.18000001999999,-58.1246434856214));
#181592=CARTESIAN_POINT('Ctrl Pts',(60.,-5.68000001999998,-58.1246434856214));
#181593=CARTESIAN_POINT('Ctrl Pts',(59.5,-5.68000001999999,-58.1246434856214));
#181594=CARTESIAN_POINT('Ctrl Pts',(60.,-5.17800220042073,-57.8275435066813));
#181595=CARTESIAN_POINT('Ctrl Pts',(60.0020017947382,-5.68000001999912,
-57.8269512006129));
#181596=CARTESIAN_POINT('Ctrl Pts',(59.4999999932887,-5.68000001999999,
-57.8769929082306));
#181597=CARTESIAN_POINT('Ctrl Pts',(59.9568439660775,-5.17605025203681,
-57.5376710843709));
#181598=CARTESIAN_POINT('Ctrl Pts',(59.9606548869199,-5.68000002000021,
-57.5365322236183));
#181599=CARTESIAN_POINT('Ctrl Pts',(59.4640366407682,-5.68000001999999,
-57.6353667913546));
#181600=CARTESIAN_POINT('Ctrl Pts',(59.8286045065143,-5.17319230589712,
-57.1137623423983));
#181601=CARTESIAN_POINT('Ctrl Pts',(59.8350835786331,-5.68000001999988,
-57.1113495469635));
#181602=CARTESIAN_POINT('Ctrl Pts',(59.3571704209101,-5.68000001999999,
-57.2820131603569));
#181603=CARTESIAN_POINT('Ctrl Pts',(59.7749715022372,-5.17225378701852,
-56.9746437275083));
#181604=CARTESIAN_POINT('Ctrl Pts',(59.7822107642191,-5.68000001999999,
-56.971551755675));
#181605=CARTESIAN_POINT('Ctrl Pts',(59.3124762512969,-5.68000001999999,
-57.1660493315578));
#181606=CARTESIAN_POINT('Ctrl Pts',(59.6495726219715,-5.17046209438582,
-56.7092025345767));
#181607=CARTESIAN_POINT('Ctrl Pts',(59.6581215271118,-5.68000001999999,
-56.7045411154571));
#181608=CARTESIAN_POINT('Ctrl Pts',(59.2079771855437,-5.68000001999999,
-56.9447878986704));
#181609=CARTESIAN_POINT('Ctrl Pts',(59.5774882635866,-5.16960084340769,
-56.5816816551612));
#181610=CARTESIAN_POINT('Ctrl Pts',(59.5865663613646,-5.68000001999988,
-56.5761588403972));
#181611=CARTESIAN_POINT('Ctrl Pts',(59.1479068869942,-5.68000001999999,
-56.8384914380986));
#181612=CARTESIAN_POINT('Ctrl Pts',(59.4144742405229,-5.16794806289525,
-56.3370811282929));
#181613=CARTESIAN_POINT('Ctrl Pts',(59.4243672282747,-5.6800000200001,-56.3296643856923));
#181614=CARTESIAN_POINT('Ctrl Pts',(59.0120618664304,-5.68000001999999,
-56.6346018834074));
#181615=CARTESIAN_POINT('Ctrl Pts',(59.3226768695123,-5.16715091135939,
-56.219170776799));
#181616=CARTESIAN_POINT('Ctrl Pts',(59.332837232209,-5.68000001999999,-56.210751177698));
#181617=CARTESIAN_POINT('Ctrl Pts',(58.9355640571429,-5.68000001999999,
-56.5363163451986));
#181618=CARTESIAN_POINT('Ctrl Pts',(59.1249326459437,-5.16567306852165,
-56.0006670964121));
#181619=CARTESIAN_POINT('Ctrl Pts',(59.1353297626326,-5.68000001999999,
-55.9901841613723));
#181620=CARTESIAN_POINT('Ctrl Pts',(58.770777205737,-5.68000001999999,-56.3541800398345));
#181621=CARTESIAN_POINT('Ctrl Pts',(59.0188424909195,-5.16498867365063,
-55.8995247770565));
#181622=CARTESIAN_POINT('Ctrl Pts',(59.0292080232237,-5.68000001999941,
-55.8880220414995));
#181623=CARTESIAN_POINT('Ctrl Pts',(58.6823687426766,-5.68000001999999,
-56.2698716578318));
#181624=CARTESIAN_POINT('Ctrl Pts',(58.6792405846915,-5.16309702763064,
-55.6200638122352));
#181625=CARTESIAN_POINT('Ctrl Pts',(58.6888368836822,-5.68000002000116,
-55.6053191370788));
#181626=CARTESIAN_POINT('Ctrl Pts',(58.3993671534221,-5.68000001999999,
-56.0369236173554));
#181627=CARTESIAN_POINT('Ctrl Pts',(58.4205568275121,-5.16204487752377,
-55.4647607356853));
#181628=CARTESIAN_POINT('Ctrl Pts',(58.4292417891598,-5.68000002000209,
-55.4482158581579));
#181629=CARTESIAN_POINT('Ctrl Pts',(58.1837972805939,-5.68000001999999,
-55.907468794294));
#181630=CARTESIAN_POINT('Ctrl Pts',(58.1509320687249,-5.16128538415681,
-55.3526885469843));
#181631=CARTESIAN_POINT('Ctrl Pts',(58.1583910096328,-5.68000001999999,
-55.3347486595489));
#181632=CARTESIAN_POINT('Ctrl Pts',(57.9591100572707,-5.68000001999999,
-55.8140496618682));
#181633=CARTESIAN_POINT('',(58.4950211556755,-5.6800000188644,-56.1192785199307));
#181634=CARTESIAN_POINT('Ctrl Pts',(58.1702690071152,-5.1613403910001,-55.3608055405081));
#181635=CARTESIAN_POINT('Ctrl Pts',(58.1743010560335,-5.17971624712748,
-55.3617697445889));
#181636=CARTESIAN_POINT('Ctrl Pts',(58.1786605683368,-5.19843216096695,
-55.3640065173544));
#181637=CARTESIAN_POINT('Ctrl Pts',(58.1833338005993,-5.21729373711926,
-55.3675776810761));
#181638=CARTESIAN_POINT('Ctrl Pts',(58.1886003610624,-5.238550038038,-55.3716022509258));
#181639=CARTESIAN_POINT('Ctrl Pts',(58.1942644441856,-5.25998821833413,
-55.3773204200167));
#181640=CARTESIAN_POINT('Ctrl Pts',(58.2003004346904,-5.28132166139531,
-55.3847821412548));
#181641=CARTESIAN_POINT('Ctrl Pts',(58.2049489607054,-5.29775128715139,
-55.3905286720463));
#181642=CARTESIAN_POINT('Ctrl Pts',(58.2098170367296,-5.31411560706899,
-55.397307215209));
#181643=CARTESIAN_POINT('Ctrl Pts',(58.2148923285532,-5.33028191493914,
-55.4051322059263));
#181644=CARTESIAN_POINT('Ctrl Pts',(58.2179849955258,-5.3401329753622,-55.4099004224533));
#181645=CARTESIAN_POINT('Ctrl Pts',(58.2211548043489,-5.34991112945887,
-55.4150574115756));
#181646=CARTESIAN_POINT('Ctrl Pts',(58.2243993450601,-5.35958637151734,
-55.4206069630805));
#181647=CARTESIAN_POINT('Ctrl Pts',(58.225967677309,-5.36426314875238,-55.4232894816145));
#181648=CARTESIAN_POINT('Ctrl Pts',(58.2275531794575,-5.36891497012945,
-55.4260632460597));
#181649=CARTESIAN_POINT('Ctrl Pts',(58.2291548526485,-5.3735363894443,-55.4289272873457));
#181650=CARTESIAN_POINT('Ctrl Pts',(58.2322364375269,-5.38242790111934,
-55.4344376413728));
#181651=CARTESIAN_POINT('Ctrl Pts',(58.2353848093176,-5.39122539639531,
-55.4402896686793));
#181652=CARTESIAN_POINT('Ctrl Pts',(58.238590591582,-5.39989093914508,-55.446460107076));
#181653=CARTESIAN_POINT('Ctrl Pts',(58.246168886576,-5.42037581111278,-55.4610466879965));
#181654=CARTESIAN_POINT('Ctrl Pts',(58.2540760482587,-5.44014466797659,
-55.4774287888053));
#181655=CARTESIAN_POINT('Ctrl Pts',(58.2622671943584,-5.45895665222149,
-55.4954084723211));
#181656=CARTESIAN_POINT('Ctrl Pts',(58.2685149026784,-5.47330529025757,
-55.5091222819551));
#181657=CARTESIAN_POINT('Ctrl Pts',(58.2749265025766,-5.48709521200839,
-55.5237615867766));
#181658=CARTESIAN_POINT('Ctrl Pts',(58.2814834890395,-5.50023570165083,
-55.5392311468777));
#181659=CARTESIAN_POINT('Ctrl Pts',(58.2874403289831,-5.51217347123809,
-55.5532848122378));
#181660=CARTESIAN_POINT('Ctrl Pts',(58.2935173976588,-5.52357605097868,
-55.5680240251301));
#181661=CARTESIAN_POINT('Ctrl Pts',(58.2997030672209,-5.53438410012245,
-55.5833799347695));
#181662=CARTESIAN_POINT('Ctrl Pts',(58.3013528163782,-5.53726666114311,
-55.5874754330388));
#181663=CARTESIAN_POINT('Ctrl Pts',(58.3030102474301,-5.54010686303733,
-55.5916146862691));
#181664=CARTESIAN_POINT('Ctrl Pts',(58.3046747425696,-5.54290298011746,
-55.595795358714));
#181665=CARTESIAN_POINT('Ctrl Pts',(58.3078403074174,-5.54822068260218,
-55.6037462318752));
#181666=CARTESIAN_POINT('Ctrl Pts',(58.3110339379717,-5.55338494923171,
-55.6118495944318));
#181667=CARTESIAN_POINT('Ctrl Pts',(58.3142526856721,-5.5583911824196,-55.6200917359245));
#181668=CARTESIAN_POINT('Ctrl Pts',(58.3154017686965,-5.56017839226279,
-55.6230341550751));
#181669=CARTESIAN_POINT('Ctrl Pts',(58.3167208420302,-5.56220365178525,
-55.6264272301895));
#181670=CARTESIAN_POINT('Ctrl Pts',(58.3179172203805,-5.56401232361543,
-55.629515338728));
#181671=CARTESIAN_POINT('Ctrl Pts',(58.3187709907203,-5.5653030443667,-55.6317191026759));
#181672=CARTESIAN_POINT('Ctrl Pts',(58.3195620560738,-5.56648459869974,
-55.6337664233606));
#181673=CARTESIAN_POINT('Ctrl Pts',(58.3201818027189,-5.56740338582579,
-55.6353714169426));
#181674=CARTESIAN_POINT('Ctrl Pts',(58.3283265601308,-5.57947815591762,
-55.6564643643198));
#181675=CARTESIAN_POINT('Ctrl Pts',(58.3368294939587,-5.59085195679983,
-55.6789219744901));
#181676=CARTESIAN_POINT('Ctrl Pts',(58.3456769886582,-5.60135110653471,
-55.7026578450694));
#181677=CARTESIAN_POINT('Ctrl Pts',(58.354632662861,-5.6119786307803,-55.726683937319));
#181678=CARTESIAN_POINT('Ctrl Pts',(58.3639414182481,-5.62170967284456,
-55.7520195442927));
#181679=CARTESIAN_POINT('Ctrl Pts',(58.3735831197023,-5.63039022337626,
-55.7785283749466));
#181680=CARTESIAN_POINT('Ctrl Pts',(58.3801401585359,-5.63629361161166,
-55.7965562544508));
#181681=CARTESIAN_POINT('Ctrl Pts',(58.3868510568775,-5.64171170086708,
-55.8151257580514));
#181682=CARTESIAN_POINT('Ctrl Pts',(58.3937077869254,-5.64660389354624,
-55.8341828715336));
#181683=CARTESIAN_POINT('Ctrl Pts',(58.4041124185868,-5.65402747045364,
-55.8631007733512));
#181684=CARTESIAN_POINT('Ctrl Pts',(58.4148250996874,-5.66023123059033,
-55.8930476615929));
#181685=CARTESIAN_POINT('Ctrl Pts',(58.4258082587751,-5.66518292561411,
-55.9238779014503));
#181686=CARTESIAN_POINT('Ctrl Pts',(58.4371557904385,-5.6702988959484,-55.9557309521233));
#181687=CARTESIAN_POINT('Ctrl Pts',(58.4487920759403,-5.67407831455118,
-55.9885267929902));
#181688=CARTESIAN_POINT('Ctrl Pts',(58.4606680081683,-5.67653409743918,
-56.0220755701741));
#181689=CARTESIAN_POINT('Ctrl Pts',(58.4719200139395,-5.67886086073644,
-56.0538617935414));
#181690=CARTESIAN_POINT('Ctrl Pts',(58.4833870699745,-5.68000001999999,
-56.0863234260588));
#181691=CARTESIAN_POINT('Ctrl Pts',(58.4950211556756,-5.68000001999999,
-56.1192785199305));
#181692=CARTESIAN_POINT('Ctrl Pts',(59.5,-5.68000001999999,-58.1246434856214));
#181693=CARTESIAN_POINT('Ctrl Pts',(59.5,-5.68000001999999,-58.0267693974302));
#181694=CARTESIAN_POINT('Ctrl Pts',(59.4943836373774,-5.68000001999999,
-57.9298568609375));
#181695=CARTESIAN_POINT('Ctrl Pts',(59.4831953566826,-5.68000001999999,
-57.8338865707097));
#181696=CARTESIAN_POINT('Ctrl Pts',(59.4720070759879,-5.68000001999999,
-57.7379162804819));
#181697=CARTESIAN_POINT('Ctrl Pts',(59.455245939737,-5.68000002032169,-57.6428888905768));
#181698=CARTESIAN_POINT('Ctrl Pts',(59.4329732446822,-5.68000001967878,
-57.548806713199));
#181699=CARTESIAN_POINT('Ctrl Pts',(59.4211509304572,-5.68000001933753,
-57.4988680299284));
#181700=CARTESIAN_POINT('Ctrl Pts',(59.4077647649327,-5.68000001901105,
-57.4491949286452));
#181701=CARTESIAN_POINT('Ctrl Pts',(59.3928232159439,-5.68000001896984,
-57.3997884127162));
#181702=CARTESIAN_POINT('Ctrl Pts',(59.3572029910943,-5.68000001887159,
-57.2820046937892));
#181703=CARTESIAN_POINT('Ctrl Pts',(59.3124912608683,-5.68000001980192,
-57.1660436798562));
#181704=CARTESIAN_POINT('Ctrl Pts',(59.2602343180242,-5.68000001992935,
-57.0554150259142));
#181705=CARTESIAN_POINT('Ctrl Pts',(59.2518183841936,-5.68000001994988,
-57.0375983803036));
#181706=CARTESIAN_POINT('Ctrl Pts',(59.2431998624486,-5.68000001996158,
-57.0198940947568));
#181707=CARTESIAN_POINT('Ctrl Pts',(59.2343787360437,-5.68000001996808,
-57.002302188435));
#181708=CARTESIAN_POINT('Ctrl Pts',(59.1884199680699,-5.68000002000192,
-56.9106469616823));
#181709=CARTESIAN_POINT('Ctrl Pts',(59.136987353068,-5.68000001969244,-56.8220653476532));
#181710=CARTESIAN_POINT('Ctrl Pts',(59.0800102832678,-5.68000001903091,
-56.7365294000527));
#181711=CARTESIAN_POINT('Ctrl Pts',(59.0296633903433,-5.68000001844636,
-56.6609469032671));
#181712=CARTESIAN_POINT('Ctrl Pts',(58.974589118716,-5.68000001849974,-56.587361786818));
#181713=CARTESIAN_POINT('Ctrl Pts',(58.9158341632416,-5.68000001947823,
-56.5172160817437));
#181714=CARTESIAN_POINT('Ctrl Pts',(58.8953629897436,-5.68000001981915,
-56.4927761874893));
#181715=CARTESIAN_POINT('Ctrl Pts',(58.8744667885101,-5.68000001977524,
-56.468763578303));
#181716=CARTESIAN_POINT('Ctrl Pts',(58.8531845723455,-5.68000001964656,
-56.4452355795564));
#181717=CARTESIAN_POINT('Ctrl Pts',(58.8093620434502,-5.68000001938158,
-56.396788726233));
#181718=CARTESIAN_POINT('Ctrl Pts',(58.7638692855098,-5.6800000177515,-56.3502656276834));
#181719=CARTESIAN_POINT('Ctrl Pts',(58.7166522079594,-5.68000001767937,
-56.3056325667689));
#181720=CARTESIAN_POINT('Ctrl Pts',(58.6815782873768,-5.68000001762579,
-56.2724781125951));
#181721=CARTESIAN_POINT('Ctrl Pts',(58.6455688559318,-5.680000018255,-56.2403749966795));
#181722=CARTESIAN_POINT('Ctrl Pts',(58.6086287388195,-5.68000001901365,
-56.2093177964104));
#181723=CARTESIAN_POINT('Ctrl Pts',(58.6017994579946,-5.68000001915391,
-56.203576116122));
#181724=CARTESIAN_POINT('Ctrl Pts',(58.5949404401232,-5.68000001924633,
-56.1978709269311));
#181725=CARTESIAN_POINT('Ctrl Pts',(58.5880516973688,-5.68000001929971,
-56.1922018795935));
#181726=CARTESIAN_POINT('Ctrl Pts',(58.5576786887571,-5.68000001953509,
-56.1672066040053));
#181727=CARTESIAN_POINT('Ctrl Pts',(58.5266453103076,-5.68000002035884,
-56.1428933547174));
#181728=CARTESIAN_POINT('Ctrl Pts',(58.4950211556752,-5.68000001545765,
-56.119278519931));
#181729=CARTESIAN_POINT('Origin',(-83.2809572255632,-5.68000001999993,-55.24995));
#181730=CARTESIAN_POINT('',(58.4950211556756,-5.68000001999999,-60.42825533736));
#181731=CARTESIAN_POINT('',(58.4950211556756,-5.68000001999999,-55.24995));
#181732=CARTESIAN_POINT('Origin',(56.3184043809282,-5.68000001999999,-60.2809146158445));
#181733=CARTESIAN_POINT('Ctrl Pts',(58.4950211556756,-5.68000001999999,
-60.42825533736));
#181734=CARTESIAN_POINT('Ctrl Pts',(57.9336485918015,-5.68000002,-60.4282553373601));
#181735=CARTESIAN_POINT('Ctrl Pts',(57.9983536018174,-6.23763109620483,
-60.42825533736));
#181736=CARTESIAN_POINT('Ctrl Pts',(58.4950211389271,-5.68000001999999,
-60.6471359124214));
#181737=CARTESIAN_POINT('Ctrl Pts',(57.9336485820782,-5.68000001999705,
-60.5646181976572));
#181738=CARTESIAN_POINT('Ctrl Pts',(57.9983536015968,-6.23763109430342,
-60.5741740417057));
#181739=CARTESIAN_POINT('Ctrl Pts',(58.4475018470026,-5.68000001999999,
-60.8620252214211));
#181740=CARTESIAN_POINT('Ctrl Pts',(57.9064697980399,-5.68000002000461,
-60.6982006050192));
#181741=CARTESIAN_POINT('Ctrl Pts',(57.9664686566087,-6.23586779901857,
-60.7174374956191));
#181742=CARTESIAN_POINT('Ctrl Pts',(58.3535376001277,-5.68000001999999,
-61.0621827299711));
#181743=CARTESIAN_POINT('Ctrl Pts',(57.8507724536939,-5.68000001999999,
-60.826158857425));
#181744=CARTESIAN_POINT('Ctrl Pts',(57.9034184448965,-6.23235646472971,
-60.8508735991007));
#181745=CARTESIAN_POINT('',(57.9983536018174,-6.23763109620483,-60.42825533736));
#181746=CARTESIAN_POINT('Origin',(58.4950211556756,-6.18000001999999,-60.42825533736));
#181747=CARTESIAN_POINT('Origin',(56.5401910842268,-6.15643070639488,-60.3303564555173));
#181748=CARTESIAN_POINT('Origin',(0.,-12.9675000200281,-60.64995));
#181749=CARTESIAN_POINT('Origin',(0.,-12.9675000200281,-60.8508735991007));
#181750=CARTESIAN_POINT('Origin',(-83.2809572255632,-12.3300000199999,-55.24995));
#181751=CARTESIAN_POINT('',(58.8765127194474,-12.33000002,-60.42825533736));
#181752=CARTESIAN_POINT('Origin',(56.649087690066,-12.33000002,-60.2675479548571));
#181753=CARTESIAN_POINT('',(58.8765127194368,-12.33000002,-56.2580153373943));
#181754=CARTESIAN_POINT('',(58.8765127194474,-12.33000002,-55.24995));
#181755=CARTESIAN_POINT('Ctrl Pts',(58.8765127194368,-12.330000020523,-56.2580153373943));
#181756=CARTESIAN_POINT('Ctrl Pts',(58.9314422324003,-12.3300000222489,
-56.3204146345377));
#181757=CARTESIAN_POINT('Ctrl Pts',(58.983370298854,-12.3300000263278,-56.3857545682243));
#181758=CARTESIAN_POINT('Ctrl Pts',(59.0318187534811,-12.3300000260899,
-56.4533283814552));
#181759=CARTESIAN_POINT('Ctrl Pts',(59.0712668703448,-12.3300000258962,
-56.5083489120742));
#181760=CARTESIAN_POINT('Ctrl Pts',(59.1084086074745,-12.3300000229817,
-56.5648494607724));
#181761=CARTESIAN_POINT('Ctrl Pts',(59.1430095719442,-12.3300000210667,
-56.6224388634736));
#181762=CARTESIAN_POINT('Ctrl Pts',(59.159023041084,-12.3300000201805,-56.6490914766904));
#181763=CARTESIAN_POINT('Ctrl Pts',(59.1745444070377,-12.3300000202428,
-56.6760375771056));
#181764=CARTESIAN_POINT('Ctrl Pts',(59.1895265613474,-12.3300000204054,
-56.7032144429067));
#181765=CARTESIAN_POINT('Ctrl Pts',(59.2106099692481,-12.3300000206344,
-56.7414586723615));
#181766=CARTESIAN_POINT('Ctrl Pts',(59.2307479204425,-12.3300000215029,
-56.7803865151708));
#181767=CARTESIAN_POINT('Ctrl Pts',(59.2498439227782,-12.3300000247794,
-56.8197986433709));
#181768=CARTESIAN_POINT('Ctrl Pts',(59.2732105276415,-12.3300000287887,
-56.8680248432995));
#181769=CARTESIAN_POINT('Ctrl Pts',(59.2950576358123,-12.3300000325183,
-56.9170923843789));
#181770=CARTESIAN_POINT('Ctrl Pts',(59.3153788043352,-12.330000032611,-56.9670066834531));
#181771=CARTESIAN_POINT('Ctrl Pts',(59.3234660778811,-12.3300000326479,
-56.9868712197865));
#181772=CARTESIAN_POINT('Ctrl Pts',(59.3313111418658,-12.3300000321978,
-57.0068701006064));
#181773=CARTESIAN_POINT('Ctrl Pts',(59.3389114029545,-12.3300000313575,
-57.0270043936979));
#181774=CARTESIAN_POINT('Ctrl Pts',(59.3711805702217,-12.3300000277898,
-57.1124905189758));
#181775=CARTESIAN_POINT('Ctrl Pts',(59.398787967634,-12.3300000251841,-57.1996595335916));
#181776=CARTESIAN_POINT('Ctrl Pts',(59.4213798740153,-12.3300000234584,
-57.2876290029532));
#181777=CARTESIAN_POINT('Ctrl Pts',(59.4552355589985,-12.3300000208724,
-57.4194579240095));
#181778=CARTESIAN_POINT('Ctrl Pts',(59.4782525129323,-12.3300000202447,
-57.553036259047));
#181779=CARTESIAN_POINT('Ctrl Pts',(59.4902475546029,-12.3300000200727,
-57.6884558476612));
#181780=CARTESIAN_POINT('Ctrl Pts',(59.4967374324385,-12.3300000199797,
-57.7617241705877));
#181781=CARTESIAN_POINT('Ctrl Pts',(59.5,-12.33000002,-57.8355316833217));
#181782=CARTESIAN_POINT('Ctrl Pts',(59.5,-12.33000002,-57.909894348981));
#181783=CARTESIAN_POINT('Ctrl Pts',(58.7359481105893,-12.33000002,-61.0621827299711));
#181784=CARTESIAN_POINT('Ctrl Pts',(58.2906927660831,-12.33000002,-60.8545178210735));
#181785=CARTESIAN_POINT('Ctrl Pts',(58.2828791719688,-11.838774304476,-60.8508735991007));
#181786=CARTESIAN_POINT('Ctrl Pts',(58.8284361535292,-12.33000002,-60.863878626764));
#181787=CARTESIAN_POINT('Ctrl Pts',(58.3533698277338,-12.3300000200013,
-60.7214865958624));
#181788=CARTESIAN_POINT('Ctrl Pts',(58.3445491382077,-11.8393573204241,
-60.7186709323925));
#181789=CARTESIAN_POINT('Ctrl Pts',(58.8765127155019,-12.33000002,-60.64928853347));
#181790=CARTESIAN_POINT('Ctrl Pts',(58.3860794582448,-12.330000020003,-60.5770127531963));
#181791=CARTESIAN_POINT('Ctrl Pts',(58.3766060098775,-11.8396582665817,
-60.575610749785));
#181792=CARTESIAN_POINT('Ctrl Pts',(58.8765127194474,-12.33000002,-60.42825533736));
#181793=CARTESIAN_POINT('Ctrl Pts',(58.3860794606436,-12.33000002,-60.42825533736));
#181794=CARTESIAN_POINT('Ctrl Pts',(58.376606009879,-11.839658266657,-60.42825533736));
#181795=CARTESIAN_POINT('',(58.376606009879,-11.839658266657,-60.42825533736));
#181796=CARTESIAN_POINT('Origin',(56.8912646065068,-11.8256176540576,-60.3210832102212));
#181797=CARTESIAN_POINT('Origin',(58.8765127194474,-11.83000002,-60.42825533736));
#181798=CARTESIAN_POINT('Ctrl Pts',(59.5,-12.33000002,-57.909894348981));
#181799=CARTESIAN_POINT('Ctrl Pts',(60.,-12.33000002,-57.909894348981));
#181800=CARTESIAN_POINT('Ctrl Pts',(60.,-12.83000002,-57.909894348981));
#181801=CARTESIAN_POINT('Ctrl Pts',(59.4999999942389,-12.33000002,-57.6980379098391));
#181802=CARTESIAN_POINT('Ctrl Pts',(59.9999466862306,-12.33000002,-57.6556802065741));
#181803=CARTESIAN_POINT('Ctrl Pts',(60.,-12.8299467103192,-57.6556666887753));
#181804=CARTESIAN_POINT('Ctrl Pts',(59.4734910794084,-12.33000002,-57.4906424667705));
#181805=CARTESIAN_POINT('Ctrl Pts',(59.9680873501793,-12.33000002,-57.4068180594886));
#181806=CARTESIAN_POINT('Ctrl Pts',(59.9681892936719,-12.8298948327809,
-57.4067922228916));
#181807=CARTESIAN_POINT('Ctrl Pts',(59.3691547532245,-12.33000002,-57.0846448139696));
#181808=CARTESIAN_POINT('Ctrl Pts',(59.8427924853442,-12.33000002,-56.9196714028451));
#181809=CARTESIAN_POINT('Ctrl Pts',(59.8429857054876,-12.8297938242694,
-56.9195951650643));
#181810=CARTESIAN_POINT('Ctrl Pts',(59.290326767749,-12.33000002,-56.8861589103251));
#181811=CARTESIAN_POINT('Ctrl Pts',(59.748161991806,-12.3300000200003,-56.6815232165248));
#181812=CARTESIAN_POINT('Ctrl Pts',(59.74839212134,-12.8297447315641,-56.6814121423199));
#181813=CARTESIAN_POINT('Ctrl Pts',(59.0886910851255,-12.33000002,-56.5202894131685));
#181814=CARTESIAN_POINT('Ctrl Pts',(59.5061445952809,-12.3300000199996,
-56.2425672751971));
#181815=CARTESIAN_POINT('Ctrl Pts',(59.5064293021094,-12.8296546666343,
-56.2423688578572));
#181816=CARTESIAN_POINT('Ctrl Pts',(58.9630665125599,-12.33000002,-56.3477358485963));
#181817=CARTESIAN_POINT('Ctrl Pts',(59.3553799746847,-12.3300000199993,
-56.035551183714));
#181818=CARTESIAN_POINT('Ctrl Pts',(59.3556798163584,-12.8296124190124,
-56.0353046315662));
#181819=CARTESIAN_POINT('Ctrl Pts',(58.6754296377554,-12.33000002,-56.0425683262376));
#181820=CARTESIAN_POINT('Ctrl Pts',(59.010210485167,-12.3300000200007,-55.6694530297022));
#181821=CARTESIAN_POINT('Ctrl Pts',(59.0105155640199,-12.8295379828168,
-55.6691036993668));
#181822=CARTESIAN_POINT('Ctrl Pts',(58.5142608782156,-12.33000002,-55.909436466106));
#181823=CARTESIAN_POINT('Ctrl Pts',(58.8168178148591,-12.330000020004,-55.5097431582292));
#181824=CARTESIAN_POINT('Ctrl Pts',(58.8171130576816,-12.8295056604635,
-55.509345500426));
#181825=CARTESIAN_POINT('Ctrl Pts',(58.3352984336861,-12.33000002,-55.7963700340195));
#181826=CARTESIAN_POINT('Ctrl Pts',(58.6020797386365,-12.33000002,-55.3741064461589));
#181827=CARTESIAN_POINT('Ctrl Pts',(58.6023581204233,-12.8294782784431,
-55.3736658212353));
#181828=CARTESIAN_POINT('',(58.6177174583857,-12.8294802501407,-55.3834349955086));
#181829=CARTESIAN_POINT('Ctrl Pts',(58.8765127194368,-12.33000002,-56.2580153373943));
#181830=CARTESIAN_POINT('Ctrl Pts',(58.8585209852578,-12.33000002,-56.2013005886069));
#181831=CARTESIAN_POINT('Ctrl Pts',(58.8410467971147,-12.3317761042405,
-56.1466276693133));
#181832=CARTESIAN_POINT('Ctrl Pts',(58.8243297325639,-12.3355548376282,
-56.0941100560183));
#181833=CARTESIAN_POINT('Ctrl Pts',(58.8101222933883,-12.3387662940775,
-56.0494765742092));
#181834=CARTESIAN_POINT('Ctrl Pts',(58.7964612333196,-12.3434255254537,
-56.0063987737953));
#181835=CARTESIAN_POINT('Ctrl Pts',(58.7834723352659,-12.3496919826154,
-55.964950401463));
#181836=CARTESIAN_POINT('Ctrl Pts',(58.7721737244199,-12.3551429654902,
-55.9288958395407));
#181837=CARTESIAN_POINT('Ctrl Pts',(58.7613678456248,-12.3618082266203,
-55.8940914777598));
#181838=CARTESIAN_POINT('Ctrl Pts',(58.7511110095659,-12.3697427827767,
-55.8606865226652));
#181839=CARTESIAN_POINT('Ctrl Pts',(58.7485351583987,-12.3717354280347,
-55.8522973671719));
#181840=CARTESIAN_POINT('Ctrl Pts',(58.7459938818405,-12.3738079285447,
-55.8439963184254));
#181841=CARTESIAN_POINT('Ctrl Pts',(58.7434879609094,-12.3759607512694,
-55.8357854220371));
#181842=CARTESIAN_POINT('Ctrl Pts',(58.7372458107547,-12.3813233477253,
-55.8153324031393));
#181843=CARTESIAN_POINT('Ctrl Pts',(58.7312234476295,-12.3871841683652,
-55.7954422699836));
#181844=CARTESIAN_POINT('Ctrl Pts',(58.7254354390637,-12.3935385577579,
-55.776158418215));
#181845=CARTESIAN_POINT('Ctrl Pts',(58.7225414347808,-12.3967157524543,
-55.7665164923307));
#181846=CARTESIAN_POINT('Ctrl Pts',(58.7197060675874,-12.400016186663,-55.7570260800124));
#181847=CARTESIAN_POINT('Ctrl Pts',(58.716931377285,-12.4034379210099,-55.7476928448876));
#181848=CARTESIAN_POINT('Ctrl Pts',(58.7155440321339,-12.4051487881833,
-55.7430262273252));
#181849=CARTESIAN_POINT('Ctrl Pts',(58.7141718606559,-12.4068899689845,
-55.7383988984847));
#181850=CARTESIAN_POINT('Ctrl Pts',(58.7128151416172,-12.4086611457118,
-55.7338115415017));
#181851=CARTESIAN_POINT('Ctrl Pts',(58.7119862494055,-12.4097432522886,
-55.7310088798105));
#181852=CARTESIAN_POINT('Ctrl Pts',(58.711318655935,-12.4106293729785,-55.728748087835));
#181853=CARTESIAN_POINT('Ctrl Pts',(58.7105263555936,-12.411696929288,-55.7260616020732));
#181854=CARTESIAN_POINT('Ctrl Pts',(58.7100218299517,-12.412376734034,-55.7243508859686));
#181855=CARTESIAN_POINT('Ctrl Pts',(58.7094668993149,-12.4131305686249,
-55.7224679456879));
#181856=CARTESIAN_POINT('Ctrl Pts',(58.708790617811,-12.4140639728075,-55.720169869264));
#181857=CARTESIAN_POINT('Ctrl Pts',(58.7018689859341,-12.4236172137396,
-55.6966494285302));
#181858=CARTESIAN_POINT('Ctrl Pts',(58.6953220673045,-12.4340096898909,
-55.6741234338963));
#181859=CARTESIAN_POINT('Ctrl Pts',(58.689142117507,-12.445322354964,-55.6524879771236));
#181860=CARTESIAN_POINT('Ctrl Pts',(58.688816090098,-12.4459191622203,-55.6513465840468));
#181861=CARTESIAN_POINT('Ctrl Pts',(58.6884910866061,-12.446518539468,-55.6502076772876));
#181862=CARTESIAN_POINT('Ctrl Pts',(58.6881671067845,-12.4471205016216,
-55.6490712442391));
#181863=CARTESIAN_POINT('Ctrl Pts',(58.6822938973485,-12.4580330633458,
-55.6284696238332));
#181864=CARTESIAN_POINT('Ctrl Pts',(58.6768067549597,-12.4696378308611,
-55.6089711514779));
#181865=CARTESIAN_POINT('Ctrl Pts',(58.6716658155591,-12.4820239191974,
-55.5904692077895));
#181866=CARTESIAN_POINT('Ctrl Pts',(58.6673122851234,-12.492512899586,-55.5748011034429));
#181867=CARTESIAN_POINT('Ctrl Pts',(58.6632208372979,-12.5035377526021,
-55.559896507031));
#181868=CARTESIAN_POINT('Ctrl Pts',(58.6594008505869,-12.5150268717868,
-55.5458324782439));
#181869=CARTESIAN_POINT('Ctrl Pts',(58.6588054148674,-12.5168177240764,
-55.5436402650942));
#181870=CARTESIAN_POINT('Ctrl Pts',(58.6582165495055,-12.5186197948547,
-55.541468396291));
#181871=CARTESIAN_POINT('Ctrl Pts',(58.6576342627611,-12.5204327441162,
-55.5393170772352));
#181872=CARTESIAN_POINT('Ctrl Pts',(58.6573186116315,-12.5214155236278,
-55.5381508712437));
#181873=CARTESIAN_POINT('Ctrl Pts',(58.6570048287531,-12.5224020674201,
-55.5369904365143));
#181874=CARTESIAN_POINT('Ctrl Pts',(58.6566929376964,-12.5233922269756,
-55.5358358934946));
#181875=CARTESIAN_POINT('Ctrl Pts',(58.6544037514851,-12.5306596992319,
-55.5273618962297));
#181876=CARTESIAN_POINT('Ctrl Pts',(58.6522201109272,-12.5381094452888,
-55.5192190766978));
#181877=CARTESIAN_POINT('Ctrl Pts',(58.6501344233983,-12.5457163433171,
-55.5114100449473));
#181878=CARTESIAN_POINT('Ctrl Pts',(58.6492541007718,-12.5489270469142,
-55.5081140251719));
#181879=CARTESIAN_POINT('Ctrl Pts',(58.6484620869347,-12.5519030887435,
-55.505141591748));
#181880=CARTESIAN_POINT('Ctrl Pts',(58.6476675535267,-12.5549708718073,
-55.502151001651));
#181881=CARTESIAN_POINT('Ctrl Pts',(58.6469162785288,-12.5578716292723,
-55.4993232343778));
#181882=CARTESIAN_POINT('Ctrl Pts',(58.6461627427164,-12.5608547253247,
-55.4964791002201));
#181883=CARTESIAN_POINT('Ctrl Pts',(58.6453413104498,-12.5642180477029,
-55.4933660627625));
#181884=CARTESIAN_POINT('Ctrl Pts',(58.6449732503413,-12.5657250554621,
-55.4919712004579));
#181885=CARTESIAN_POINT('Ctrl Pts',(58.6445917142175,-12.5673086803814,
-55.4905228663659));
#181886=CARTESIAN_POINT('Ctrl Pts',(58.6441917094418,-12.5689972084979,
-55.4890014166344));
#181887=CARTESIAN_POINT('Ctrl Pts',(58.6409514218902,-12.5826753367812,
-55.4766767272197));
#181888=CARTESIAN_POINT('Ctrl Pts',(58.6379842407909,-12.5969255263037,
-55.4652509528636));
#181889=CARTESIAN_POINT('Ctrl Pts',(58.6353347443317,-12.6115648322177,
-55.4549431359274));
#181890=CARTESIAN_POINT('Ctrl Pts',(58.632214720523,-12.6288039505554,-55.4428047410464));
#181891=CARTESIAN_POINT('Ctrl Pts',(58.6294915613887,-12.6467684309172,
-55.4320739374645));
#181892=CARTESIAN_POINT('Ctrl Pts',(58.6271856679341,-12.6652382398481,
-55.4228838761748));
#181893=CARTESIAN_POINT('Ctrl Pts',(58.6249108991176,-12.6834587457953,
-55.4138178610899));
#181894=CARTESIAN_POINT('Ctrl Pts',(58.6230422205788,-12.7021702479696,
-55.4062515812779));
#181895=CARTESIAN_POINT('Ctrl Pts',(58.6215869171453,-12.7211486377003,
-55.4002663143306));
#181896=CARTESIAN_POINT('Ctrl Pts',(58.6201684206881,-12.7396470332751,
-55.39443242446));
#181897=CARTESIAN_POINT('Ctrl Pts',(58.6191426248752,-12.7583983182253,
-55.3901006812464));
#181898=CARTESIAN_POINT('Ctrl Pts',(58.6185046694614,-12.777193300316,-55.3872990548521));
#181899=CARTESIAN_POINT('Ctrl Pts',(58.6179125173504,-12.7946388585472,
-55.3846985769072));
#181900=CARTESIAN_POINT('Ctrl Pts',(58.6176544005564,-12.8121216806621,
-55.383416046038));
#181901=CARTESIAN_POINT('Ctrl Pts',(58.6177174583935,-12.8294802501407,
-55.3834349955049));
#181902=CARTESIAN_POINT('Ctrl Pts',(60.,-12.83000002,-57.909894348981));
#181903=CARTESIAN_POINT('Ctrl Pts',(59.9999999999989,-12.8299744710484,
-57.8359337179673));
#181904=CARTESIAN_POINT('Ctrl Pts',(59.9972617701648,-12.8299480939923,
-57.7612058529128));
#181905=CARTESIAN_POINT('Ctrl Pts',(59.9916341638385,-12.8299212660683,
-57.6860080728811));
#181906=CARTESIAN_POINT('Ctrl Pts',(59.9860637906075,-12.829894710986,-57.6115750588015));
#181907=CARTESIAN_POINT('Ctrl Pts',(59.9776620832511,-12.8298677147732,
-57.5366821156517));
#181908=CARTESIAN_POINT('Ctrl Pts',(59.9663234619368,-12.8298406785937,
-57.4616474786362));
#181909=CARTESIAN_POINT('Ctrl Pts',(59.955082109238,-12.8298138743447,-57.3872565279253));
#181910=CARTESIAN_POINT('Ctrl Pts',(59.9409536887295,-12.829787031524,-57.3127268637753));
#181911=CARTESIAN_POINT('Ctrl Pts',(59.9238814614563,-12.8297605661022,
-57.2383904352127));
#181912=CARTESIAN_POINT('Ctrl Pts',(59.906928323879,-12.8297342852936,-57.1645725507473));
#181913=CARTESIAN_POINT('Ctrl Pts',(59.8870720994784,-12.8297083774193,
-57.0909458358442));
#181914=CARTESIAN_POINT('Ctrl Pts',(59.8643069244052,-12.8296832634698,
-57.0178481696535));
#181915=CARTESIAN_POINT('Ctrl Pts',(59.8416638492725,-12.8296582842178,
-56.94514255934));
#181916=CARTESIAN_POINT('Ctrl Pts',(59.816142868814,-12.8296340912156,-56.8729609924185));
#181917=CARTESIAN_POINT('Ctrl Pts',(59.7877896743797,-12.8296111003244,
-56.8016391523904));
#181918=CARTESIAN_POINT('Ctrl Pts',(59.7588375756144,-12.8295876237967,
-56.7288107816261));
#181919=CARTESIAN_POINT('Ctrl Pts',(59.7269321908296,-12.8295654016406,
-56.6568795902393));
#181920=CARTESIAN_POINT('Ctrl Pts',(59.6921781196006,-12.8295448649116,
-56.5861956626463));
#181921=CARTESIAN_POINT('Ctrl Pts',(59.6583339412711,-12.8295248658526,
-56.5173623039665));
#181922=CARTESIAN_POINT('Ctrl Pts',(59.6217887002356,-12.8295064658391,
-56.4497123447422));
#181923=CARTESIAN_POINT('Ctrl Pts',(59.58268887405,-12.8294900397982,-56.383552355395));
#181924=CARTESIAN_POINT('Ctrl Pts',(59.5435861500292,-12.82947361254,-56.3173874626821));
#181925=CARTESIAN_POINT('Ctrl Pts',(59.5019287886767,-12.829459160258,-56.252713343921));
#181926=CARTESIAN_POINT('Ctrl Pts',(59.4579086639815,-12.8294470237429,
-56.1898108483834));
#181927=CARTESIAN_POINT('Ctrl Pts',(59.4138217494082,-12.8294348688135,
-56.126812913543));
#181928=CARTESIAN_POINT('Ctrl Pts',(59.3673653387337,-12.8294250372887,
-56.0655924845596));
#181929=CARTESIAN_POINT('Ctrl Pts',(59.3187719001662,-12.8294178272532,
-56.006397628351));
#181930=CARTESIAN_POINT('Ctrl Pts',(59.2679932684043,-12.8294102929903,
-55.9445408449204));
#181931=CARTESIAN_POINT('Ctrl Pts',(59.2148814599025,-12.8294056222363,
-55.8848966808624));
#181932=CARTESIAN_POINT('Ctrl Pts',(59.1597391818534,-12.8294040942622,
-55.8277007148089));
#181933=CARTESIAN_POINT('Ctrl Pts',(59.106411665564,-12.8294026165744,-55.772387098482));
#181934=CARTESIAN_POINT('Ctrl Pts',(59.0511859407705,-12.8294040781501,
-55.7193631715755));
#181935=CARTESIAN_POINT('Ctrl Pts',(58.9943604122752,-12.8294086705796,
-55.6687939358799));
#181936=CARTESIAN_POINT('Ctrl Pts',(58.9346341825115,-12.829413497433,-55.6156433560243));
#181937=CARTESIAN_POINT('Ctrl Pts',(58.8731413017213,-12.8294217836238,
-55.5652050465767));
#181938=CARTESIAN_POINT('Ctrl Pts',(58.8102451196153,-12.8294336770107,
-55.5176113120292));
#181939=CARTESIAN_POINT('Ctrl Pts',(58.7473489375092,-12.8294455703977,
-55.4700175774817));
#181940=CARTESIAN_POINT('Ctrl Pts',(58.6830502669702,-12.8294610708343,
-55.4252683304837));
#181941=CARTESIAN_POINT('Ctrl Pts',(58.6177174583777,-12.8294802501408,
-55.3834349955295));
#181942=CARTESIAN_POINT('Ctrl Pts',(60.,-13.3330000856764,-57.9104187956072));
#181943=CARTESIAN_POINT('Ctrl Pts',(59.9999999999999,-13.3385258667613,
-56.2566220904403));
#181944=CARTESIAN_POINT('Ctrl Pts',(58.6015900410175,-13.3414758787461,
-55.3737206461528));
#181945=CARTESIAN_POINT('Ctrl Pts',(60.,-13.1643269532066,-57.9098552131434));
#181946=CARTESIAN_POINT('Ctrl Pts',(59.999999999998,-13.1673253991122,-56.2568074836808));
#181947=CARTESIAN_POINT('Ctrl Pts',(58.6025724987196,-13.1689005967759,
-55.3737643179335));
#181948=CARTESIAN_POINT('Ctrl Pts',(60.,-12.9956563413871,-57.9096813403539));
#181949=CARTESIAN_POINT('Ctrl Pts',(60.0000000000016,-12.9960742306928,
-56.2568641234304));
#181950=CARTESIAN_POINT('Ctrl Pts',(58.6028748593257,-12.996307708263,-55.3737777024909));
#181951=CARTESIAN_POINT('Ctrl Pts',(60.,-12.827000187199,-57.9098981644024));
#181952=CARTESIAN_POINT('Ctrl Pts',(60.,-12.8248749582876,-56.2567930570856));
#181953=CARTESIAN_POINT('Ctrl Pts',(58.6024972248876,-12.82373973381,-55.3737609414448));
#181954=CARTESIAN_POINT('',(58.6168863951182,-13.3313694067286,-55.3834094543327));
#181955=CARTESIAN_POINT('Origin',(-9.50671311766895,-12.9674995491444,-53.303688922601));
#181956=CARTESIAN_POINT('Ctrl Pts',(58.6168867413708,-13.3313694084883,
-55.383408913088));
#181957=CARTESIAN_POINT('Ctrl Pts',(58.6518309768615,-13.3313575313466,
-55.4057635202508));
#181958=CARTESIAN_POINT('Ctrl Pts',(58.6887187014103,-13.33134768207,-55.4303640415874));
#181959=CARTESIAN_POINT('Ctrl Pts',(58.727302437496,-13.3313387189539,-55.457512498856));
#181960=CARTESIAN_POINT('Ctrl Pts',(58.7659617189431,-13.3313297382884,
-55.4847141116824));
#181961=CARTESIAN_POINT('Ctrl Pts',(58.8063236557285,-13.3313216472882,
-55.5144736674302));
#181962=CARTESIAN_POINT('Ctrl Pts',(58.8481041920362,-13.3313132749985,
-55.5471338395576));
#181963=CARTESIAN_POINT('Ctrl Pts',(58.8900448541703,-13.3313048706217,
-55.5799191832962));
#181964=CARTESIAN_POINT('Ctrl Pts',(58.9334150085969,-13.3312961828305,
-55.6156274393693));
#181965=CARTESIAN_POINT('Ctrl Pts',(58.9778919914789,-13.3312860039637,
-55.6546440918516));
#181966=CARTESIAN_POINT('Ctrl Pts',(58.9877571607387,-13.3312837462511,
-55.6632981384112));
#181967=CARTESIAN_POINT('Ctrl Pts',(58.9976766455109,-13.3312814150908,
-55.6721150982506));
#181968=CARTESIAN_POINT('Ctrl Pts',(59.0076466909832,-13.3312789971485,
-55.6810994335804));
#181969=CARTESIAN_POINT('Ctrl Pts',(59.0556433273577,-13.3312673569707,
-55.7243507785303));
#181970=CARTESIAN_POINT('Ctrl Pts',(59.1046913605823,-13.331253607827,-55.7713670635205));
#181971=CARTESIAN_POINT('Ctrl Pts',(59.1543509096943,-13.3312365517527,
-55.8226288107561));
#181972=CARTESIAN_POINT('Ctrl Pts',(59.1636794475872,-13.3312333477721,
-55.8322583212952));
#181973=CARTESIAN_POINT('Ctrl Pts',(59.1730294636469,-13.3312300270276,
-55.8420377522441));
#181974=CARTESIAN_POINT('Ctrl Pts',(59.1823979034467,-13.331226581481,-55.8519704376614));
#181975=CARTESIAN_POINT('Ctrl Pts',(59.2181174888655,-13.3312134444486,
-55.889841354568));
#181976=CARTESIAN_POINT('Ctrl Pts',(59.254065600552,-13.3311984763158,-55.9299702151753));
#181977=CARTESIAN_POINT('Ctrl Pts',(59.2899681543462,-13.3311812861886,
-55.9724384503647));
#181978=CARTESIAN_POINT('Ctrl Pts',(59.324473058904,-13.3311647652552,-56.0132534411409));
#181979=CARTESIAN_POINT('Ctrl Pts',(59.3589358950507,-13.3311461918562,
-56.0562294085373));
#181980=CARTESIAN_POINT('Ctrl Pts',(59.3930756919653,-13.3311252335256,
-56.1014093033857));
#181981=CARTESIAN_POINT('Ctrl Pts',(59.413702619857,-13.3311125707094,-56.1287065493398));
#181982=CARTESIAN_POINT('Ctrl Pts',(59.4342108937052,-13.331099037572,-56.1568077491432));
#181983=CARTESIAN_POINT('Ctrl Pts',(59.4545314055103,-13.3310845637658,
-56.1857163908717));
#181984=CARTESIAN_POINT('Ctrl Pts',(59.4867505663134,-13.3310616148414,
-56.231552449795));
#181985=CARTESIAN_POINT('Ctrl Pts',(59.5185638745705,-13.3310360998369,
-56.2795149251563));
#181986=CARTESIAN_POINT('Ctrl Pts',(59.5495967522417,-13.3310081949687,
-56.329505884133));
#181987=CARTESIAN_POINT('Ctrl Pts',(59.5760753065559,-13.3309843853634,
-56.3721602694758));
#181988=CARTESIAN_POINT('Ctrl Pts',(59.6019852850859,-13.3309588362789,
-56.4162906742891));
#181989=CARTESIAN_POINT('Ctrl Pts',(59.6270838367082,-13.3309316719345,
-56.4618080042972));
#181990=CARTESIAN_POINT('Ctrl Pts',(59.655560094013,-13.3309008518747,-56.5134509524899));
#181991=CARTESIAN_POINT('Ctrl Pts',(59.6831787738492,-13.3308677658063,
-56.5672241087531));
#181992=CARTESIAN_POINT('Ctrl Pts',(59.7096306137844,-13.3308326091658,
-56.622973427477));
#181993=CARTESIAN_POINT('Ctrl Pts',(59.7363440874793,-13.3307971047927,
-56.6792741597847));
#181994=CARTESIAN_POINT('Ctrl Pts',(59.7618673284164,-13.3307594886723,
-56.7375903532155));
#181995=CARTESIAN_POINT('Ctrl Pts',(59.7858777491114,-13.3307199907229,
-56.7977099174592));
#181996=CARTESIAN_POINT('Ctrl Pts',(59.8046199401192,-13.3306891591885,
-56.8446383895037));
#181997=CARTESIAN_POINT('Ctrl Pts',(59.8224402294923,-13.3306571816186,
-56.8926645786094));
#181998=CARTESIAN_POINT('Ctrl Pts',(59.8391847459088,-13.3306241792105,
-56.9416655717737));
#181999=CARTESIAN_POINT('Ctrl Pts',(59.8585155095614,-13.3305860794687,
-56.9982349341872));
#182000=CARTESIAN_POINT('Ctrl Pts',(59.8765034568221,-13.3305464398981,
-57.0563771337676));
#182001=CARTESIAN_POINT('Ctrl Pts',(59.8928364815615,-13.3305059511937,
-57.1157678786086));
#182002=CARTESIAN_POINT('Ctrl Pts',(59.8971772508625,-13.3304951906562,
-57.1315519434763));
#182003=CARTESIAN_POINT('Ctrl Pts',(59.9014012664531,-13.3304843702828,
-57.1474239430367));
#182004=CARTESIAN_POINT('Ctrl Pts',(59.9055029853774,-13.3304735033315,
-57.1633772637068));
#182005=CARTESIAN_POINT('Ctrl Pts',(59.9215992705231,-13.3304308583944,
-57.2259825282955));
#182006=CARTESIAN_POINT('Ctrl Pts',(59.9358873636991,-13.3303875029055,
-57.2898305753006));
#182007=CARTESIAN_POINT('Ctrl Pts',(59.9481455905804,-13.330344124173,-57.3547362848755));
#182008=CARTESIAN_POINT('Ctrl Pts',(59.960235295645,-13.330301341796,-57.418749693452));
#182009=CARTESIAN_POINT('Ctrl Pts',(59.9703504144349,-13.3302585367883,
-57.4837919018522));
#182010=CARTESIAN_POINT('Ctrl Pts',(59.9783274566335,-13.3302163744338,
-57.549676722112));
#182011=CARTESIAN_POINT('Ctrl Pts',(59.9861782130125,-13.3301748795582,
-57.614518509338));
#182012=CARTESIAN_POINT('Ctrl Pts',(59.9919579901404,-13.3301340071369,
-57.6801764442022));
#182013=CARTESIAN_POINT('Ctrl Pts',(59.9955604092132,-13.3300943973881,
-57.7464645030732));
#182014=CARTESIAN_POINT('Ctrl Pts',(59.9985092463069,-13.330061973982,-57.8007260098339));
#182015=CARTESIAN_POINT('Ctrl Pts',(60.,-13.3300303967464,-57.8554095840285));
#182016=CARTESIAN_POINT('Ctrl Pts',(60.,-13.33000002,-57.9104088126279));
#182017=CARTESIAN_POINT('Ctrl Pts',(60.,-13.33000002,-57.9104088126279));
#182018=CARTESIAN_POINT('Ctrl Pts',(60.,-13.83000002,-57.9104088126279));
#182019=CARTESIAN_POINT('Ctrl Pts',(59.5,-13.83000002,-57.9104088126279));
#182020=CARTESIAN_POINT('Ctrl Pts',(60.,-13.3301404965737,-57.6560661294349));
#182021=CARTESIAN_POINT('Ctrl Pts',(59.9998595361682,-13.830000019997,-57.6561017631169));
#182022=CARTESIAN_POINT('Ctrl Pts',(59.4999999942362,-13.83000002,-57.6984561889535));
#182023=CARTESIAN_POINT('Ctrl Pts',(59.9681611381428,-13.3302771999651,
-57.4070813040103));
#182024=CARTESIAN_POINT('Ctrl Pts',(59.9678925924923,-13.8300000200007,
-57.4071493963694));
#182025=CARTESIAN_POINT('Ctrl Pts',(59.4734676164696,-13.83000002,-57.4909684574329));
#182026=CARTESIAN_POINT('Ctrl Pts',(59.8428449408308,-13.3305433698035,
-56.9196731955795));
#182027=CARTESIAN_POINT('Ctrl Pts',(59.8423361500656,-13.8300000199993,
-56.9198740502323));
#182028=CARTESIAN_POINT('Ctrl Pts',(59.3690374493417,-13.83000002,-57.084794303535));
#182029=CARTESIAN_POINT('Ctrl Pts',(59.7481694456677,-13.3306727288355,
-56.6814017112205));
#182030=CARTESIAN_POINT('Ctrl Pts',(59.7475635896442,-13.8300000199991,
-56.6816942845782));
#182031=CARTESIAN_POINT('Ctrl Pts',(59.2901412046916,-13.83000002,-56.8862343787282));
#182032=CARTESIAN_POINT('Ctrl Pts',(59.5059986510887,-13.3309100420639,
-56.2422140639419));
#182033=CARTESIAN_POINT('Ctrl Pts',(59.5052494150047,-13.8300000200009,
-56.2427365274425));
#182034=CARTESIAN_POINT('Ctrl Pts',(59.0883322092721,-13.83000002,-56.5202440244056));
#182035=CARTESIAN_POINT('Ctrl Pts',(59.3551153361278,-13.3310213578394,
-56.0350898960933));
#182036=CARTESIAN_POINT('Ctrl Pts',(59.3543264440767,-13.8300000199994,
-56.0357389914811));
#182037=CARTESIAN_POINT('Ctrl Pts',(58.9625961123716,-13.83000002,-56.3476402489859));
#182038=CARTESIAN_POINT('Ctrl Pts',(59.0096808365833,-13.3312174510841,
-55.6688506341933));
#182039=CARTESIAN_POINT('Ctrl Pts',(59.0088785326184,-13.8300000200005,
-55.6697700183809));
#182040=CARTESIAN_POINT('Ctrl Pts',(58.6747340315543,-13.83000002,-56.0424403288692));
#182041=CARTESIAN_POINT('Ctrl Pts',(58.8161264695431,-13.3313025928017,
-55.509091871258));
#182042=CARTESIAN_POINT('Ctrl Pts',(58.8153502371001,-13.83000002,-55.510138275251));
#182043=CARTESIAN_POINT('Ctrl Pts',(58.5134387215907,-13.83000002,-55.9093078011895));
#182044=CARTESIAN_POINT('Ctrl Pts',(58.6011960412544,-13.3313747072047,
-55.3734386342923));
#182045=CARTESIAN_POINT('Ctrl Pts',(58.6004643384094,-13.83000002,-55.3745979500414));
#182046=CARTESIAN_POINT('Ctrl Pts',(58.3343300343787,-13.83000002,-55.796263236946));
#182047=CARTESIAN_POINT('',(58.871735578318,-13.83000002,-56.2531111209796));
#182048=CARTESIAN_POINT('Ctrl Pts',(58.6168862797061,-13.3313694061423,
-55.3834096347511));
#182049=CARTESIAN_POINT('Ctrl Pts',(58.6166586051978,-13.3551390166932,
-55.3833412426932));
#182050=CARTESIAN_POINT('Ctrl Pts',(58.6170436760351,-13.3791016137262,
-55.3857576231866));
#182051=CARTESIAN_POINT('Ctrl Pts',(58.6180546690853,-13.4028729528674,
-55.3906118450551));
#182052=CARTESIAN_POINT('Ctrl Pts',(58.6189770783085,-13.4245614327907,
-55.395040737046));
#182053=CARTESIAN_POINT('Ctrl Pts',(58.6204203983464,-13.446089860864,-55.4014982059527));
#182054=CARTESIAN_POINT('Ctrl Pts',(58.6223869358216,-13.4671538689141,
-55.4099138186837));
#182055=CARTESIAN_POINT('Ctrl Pts',(58.6239470623716,-13.4838647216817,
-55.4165902339681));
#182056=CARTESIAN_POINT('Ctrl Pts',(58.6258366760205,-13.5002878550557,
-55.4244998730337));
#182057=CARTESIAN_POINT('Ctrl Pts',(58.6280557462051,-13.5162767774032,
-55.4336019959238));
#182058=CARTESIAN_POINT('Ctrl Pts',(58.6294397837303,-13.5262490931366,
-55.4392790041255));
#182059=CARTESIAN_POINT('Ctrl Pts',(58.6309521702184,-13.536053772359,-55.4454206393065));
#182060=CARTESIAN_POINT('Ctrl Pts',(58.6325920811364,-13.5456516620568,
-55.4520136060124));
#182061=CARTESIAN_POINT('Ctrl Pts',(58.632764313496,-13.5466596846097,-55.4527060352171));
#182062=CARTESIAN_POINT('Ctrl Pts',(58.6329379451287,-13.5476653862635,
-55.4534034132351));
#182063=CARTESIAN_POINT('Ctrl Pts',(58.6331129708765,-13.5486687027769,
-55.4541057080602));
#182064=CARTESIAN_POINT('Ctrl Pts',(58.6338940693833,-13.553146267024,-55.4572398837245));
#182065=CARTESIAN_POINT('Ctrl Pts',(58.6347033046008,-13.5575800115132,
-55.460471484084));
#182066=CARTESIAN_POINT('Ctrl Pts',(58.6355400649534,-13.5619665751822,
-55.4637967328783));
#182067=CARTESIAN_POINT('Ctrl Pts',(58.6362806787559,-13.5658491080835,
-55.4667398995169));
#182068=CARTESIAN_POINT('Ctrl Pts',(58.6370885831823,-13.5699392454374,
-55.4699453141178));
#182069=CARTESIAN_POINT('Ctrl Pts',(58.6379115394895,-13.5739434469271,
-55.4731988144793));
#182070=CARTESIAN_POINT('Ctrl Pts',(58.6387771554018,-13.5781552143021,
-55.4766209666143));
#182071=CARTESIAN_POINT('Ctrl Pts',(58.639659469486,-13.5822717024859,-55.4800963524606));
#182072=CARTESIAN_POINT('Ctrl Pts',(58.6404820528253,-13.5859780462294,
-55.4833231160771));
#182073=CARTESIAN_POINT('Ctrl Pts',(58.6408738203898,-13.5877432476288,
-55.4848599102995));
#182074=CARTESIAN_POINT('Ctrl Pts',(58.6412518113189,-13.5894158200307,
-55.4863395554386));
#182075=CARTESIAN_POINT('Ctrl Pts',(58.6416067387722,-13.5909636222847,
-55.4877260831397));
#182076=CARTESIAN_POINT('Ctrl Pts',(58.6452240649327,-13.6067384109956,
-55.501857204523));
#182077=CARTESIAN_POINT('Ctrl Pts',(58.6492790136846,-13.6219316887321,
-55.5173867126378));
#182078=CARTESIAN_POINT('Ctrl Pts',(58.6537511347767,-13.6364297661259,
-55.5342058470857));
#182079=CARTESIAN_POINT('Ctrl Pts',(58.6582232558689,-13.6509278435197,
-55.5510249815336));
#182080=CARTESIAN_POINT('Ctrl Pts',(58.6631086854053,-13.664731889532,-55.5691315342369));
#182081=CARTESIAN_POINT('Ctrl Pts',(58.6683895962004,-13.677740540402,-55.5884071874342));
#182082=CARTESIAN_POINT('Ctrl Pts',(58.6734857856715,-13.6902941608225,
-55.6070085962979));
#182083=CARTESIAN_POINT('Ctrl Pts',(58.6789585654752,-13.7021035078633,
-55.6266987231872));
#182084=CARTESIAN_POINT('Ctrl Pts',(58.6848066915835,-13.7130962049731,
-55.6473929364424));
#182085=CARTESIAN_POINT('Ctrl Pts',(58.6850186683171,-13.7134946567136,
-55.6481430385517));
#182086=CARTESIAN_POINT('Ctrl Pts',(58.6852311114247,-13.7138920091911,
-55.6488943444074));
#182087=CARTESIAN_POINT('Ctrl Pts',(58.6854440202128,-13.714288263411,-55.6496468513027));
#182088=CARTESIAN_POINT('Ctrl Pts',(58.6884873946672,-13.7199524258969,
-55.660403383631));
#182089=CARTESIAN_POINT('Ctrl Pts',(58.6916307191757,-13.7254008529457,
-55.6714221893279));
#182090=CARTESIAN_POINT('Ctrl Pts',(58.6948685872551,-13.7306305586263,
-55.6826868898889));
#182091=CARTESIAN_POINT('Ctrl Pts',(58.6964875212948,-13.7332454114665,
-55.6883192401695));
#182092=CARTESIAN_POINT('Ctrl Pts',(58.6981269348003,-13.7358066437677,
-55.6940124136505));
#182093=CARTESIAN_POINT('Ctrl Pts',(58.6997902120213,-13.7383127952728,
-55.6997653245961));
#182094=CARTESIAN_POINT('Ctrl Pts',(58.700772181751,-13.7397923832122,-55.7031617424241));
#182095=CARTESIAN_POINT('Ctrl Pts',(58.7019008874974,-13.741455747517,-55.707056057204));
#182096=CARTESIAN_POINT('Ctrl Pts',(58.7029322179606,-13.7429404982508,
-55.7106055006442));
#182097=CARTESIAN_POINT('Ctrl Pts',(58.703647772778,-13.743970643852,-55.7130681655639));
#182098=CARTESIAN_POINT('Ctrl Pts',(58.7043160412341,-13.7449159120308,
-55.715363796439));
#182099=CARTESIAN_POINT('Ctrl Pts',(58.7048515824868,-13.745665830996,-55.7172013174975));
#182100=CARTESIAN_POINT('Ctrl Pts',(58.712506737924,-13.7563853530031,-55.7434672853407));
#182101=CARTESIAN_POINT('Ctrl Pts',(58.7207003301415,-13.766106376615,-55.7711504373378));
#182102=CARTESIAN_POINT('Ctrl Pts',(58.7294033729206,-13.7747791161279,
-55.8001204503051));
#182103=CARTESIAN_POINT('Ctrl Pts',(58.7383662274934,-13.7837107627916,
-55.8299553045956));
#182104=CARTESIAN_POINT('Ctrl Pts',(58.7478693856264,-13.7915305679036,
-55.8611548223526));
#182105=CARTESIAN_POINT('Ctrl Pts',(58.757866232067,-13.7982186853384,-55.8935359318098));
#182106=CARTESIAN_POINT('Ctrl Pts',(58.7609230306435,-13.8002637530481,
-55.9034373071967));
#182107=CARTESIAN_POINT('Ctrl Pts',(58.7640258871556,-13.8022032479972,
-55.9134488916051));
#182108=CARTESIAN_POINT('Ctrl Pts',(58.7671732088176,-13.8040372220194,
-55.9235647720032));
#182109=CARTESIAN_POINT('Ctrl Pts',(58.7785673284148,-13.8106766829931,
-55.9601868791367));
#182110=CARTESIAN_POINT('Ctrl Pts',(58.7905137904197,-13.8159523307797,
-55.9980782289915));
#182111=CARTESIAN_POINT('Ctrl Pts',(58.8029474500823,-13.8199543646308,
-56.0372588901943));
#182112=CARTESIAN_POINT('Ctrl Pts',(58.8158027247144,-13.8240921040927,
-56.0777681347526));
#182113=CARTESIAN_POINT('Ctrl Pts',(58.8291786964963,-13.8268688821086,
-56.1196563252059));
#182114=CARTESIAN_POINT('Ctrl Pts',(58.842987608089,-13.8284327204152,-56.1629215142385));
#182115=CARTESIAN_POINT('Ctrl Pts',(58.8523806495261,-13.8294964681201,
-56.1923511843931));
#182116=CARTESIAN_POINT('Ctrl Pts',(58.8619736743151,-13.83000002,-56.2224174707967));
#182117=CARTESIAN_POINT('Ctrl Pts',(58.871735578318,-13.83000002,-56.2531111209796));
#182118=CARTESIAN_POINT('Ctrl Pts',(59.5,-13.83000002,-57.9104088126279));
#182119=CARTESIAN_POINT('Ctrl Pts',(59.5,-13.83000002,-57.7635265772541));
#182120=CARTESIAN_POINT('Ctrl Pts',(59.4872752713113,-13.8300000201995,
-57.6187932998347));
#182121=CARTESIAN_POINT('Ctrl Pts',(59.4620787130121,-13.8300000189704,
-57.4761129700929));
#182122=CARTESIAN_POINT('Ctrl Pts',(59.4509269987812,-13.8300000184264,
-57.4129642557027));
#182123=CARTESIAN_POINT('Ctrl Pts',(59.4373315644232,-13.8300000175808,
-57.3502178600952));
#182124=CARTESIAN_POINT('Ctrl Pts',(59.4213112185568,-13.8300000163283,
-57.287866292));
#182125=CARTESIAN_POINT('Ctrl Pts',(59.3984317821363,-13.8300000145396,
-57.1988189799231));
#182126=CARTESIAN_POINT('Ctrl Pts',(59.370414675224,-13.8300000118888,-57.1106006512125));
#182127=CARTESIAN_POINT('Ctrl Pts',(59.3376309673359,-13.8300000085315,
-57.0241300655719));
#182128=CARTESIAN_POINT('Ctrl Pts',(59.3184526052594,-13.8300000065676,
-56.9735450552968));
#182129=CARTESIAN_POINT('Ctrl Pts',(59.2977312649333,-13.8300000075911,
-56.9238144825167));
#182130=CARTESIAN_POINT('Ctrl Pts',(59.2754924251816,-13.8300000109221,
-56.874925908888));
#182131=CARTESIAN_POINT('Ctrl Pts',(59.2665370422075,-13.8300000122635,
-56.8552389151062));
#182132=CARTESIAN_POINT('Ctrl Pts',(59.2573350139601,-13.8300000139055,
-56.8356886347883));
#182133=CARTESIAN_POINT('Ctrl Pts',(59.2478858052507,-13.8300000154741,
-56.8162751713274));
#182134=CARTESIAN_POINT('Ctrl Pts',(59.2292919233252,-13.8300000185606,
-56.778073914645));
#182135=CARTESIAN_POINT('Ctrl Pts',(59.209718687562,-13.8300000193634,-56.7403307398674));
#182136=CARTESIAN_POINT('Ctrl Pts',(59.1892544368186,-13.8300000195901,
-56.7032294252422));
#182137=CARTESIAN_POINT('Ctrl Pts',(59.1734934512784,-13.8300000197646,
-56.6746550449402));
#182138=CARTESIAN_POINT('Ctrl Pts',(59.1571354382929,-13.8300000198488,
-56.6463349492494));
#182139=CARTESIAN_POINT('Ctrl Pts',(59.140235511425,-13.8300000188361,-56.6183428976771));
#182140=CARTESIAN_POINT('Ctrl Pts',(59.0995076542862,-13.8300000163955,
-56.5508836544291));
#182141=CARTESIAN_POINT('Ctrl Pts',(59.0552769615229,-13.8300000132201,
-56.4849168102432));
#182142=CARTESIAN_POINT('Ctrl Pts',(59.0079404245019,-13.8300000140848,
-56.4210933496137));
#182143=CARTESIAN_POINT('Ctrl Pts',(58.9649853093638,-13.8300000148695,
-56.3631773238039));
#182144=CARTESIAN_POINT('Ctrl Pts',(58.9194738360314,-13.8300000183267,
-56.3070268147755));
#182145=CARTESIAN_POINT('Ctrl Pts',(58.871735578318,-13.8300000195957,-56.2531111209796));
#182146=CARTESIAN_POINT('Origin',(-83.2809572255632,-13.8300000199999,-55.24995));
#182147=CARTESIAN_POINT('',(58.871735578318,-13.83000002,-60.42825533736));
#182148=CARTESIAN_POINT('',(58.871735578318,-13.83000002,-55.24995));
#182149=CARTESIAN_POINT('Origin',(56.6451562406488,-13.83000002,-60.2668362080947));
#182150=CARTESIAN_POINT('Ctrl Pts',(58.871735578318,-13.83000002,-60.42825533736));
#182151=CARTESIAN_POINT('Ctrl Pts',(58.383173457336,-13.83000002,-60.42825533736));
#182152=CARTESIAN_POINT('Ctrl Pts',(58.3718694303385,-14.3184313509278,
-60.42825533736));
#182153=CARTESIAN_POINT('Ctrl Pts',(58.871735561804,-13.83000002,-60.6470682084222));
#182154=CARTESIAN_POINT('Ctrl Pts',(58.3831734460811,-13.83000002,-60.57578605024));
#182155=CARTESIAN_POINT('Ctrl Pts',(58.3718694303297,-14.3184313513064,
-60.574130507918));
#182156=CARTESIAN_POINT('Ctrl Pts',(58.8245931841484,-13.83000002,-60.8618675123431));
#182157=CARTESIAN_POINT('Ctrl Pts',(58.3509717578384,-13.8300000200006,
-60.7206801175402));
#182158=CARTESIAN_POINT('Ctrl Pts',(58.3404329537672,-14.3187847426543,
-60.7173302229433));
#182159=CARTESIAN_POINT('Ctrl Pts',(58.7311595360587,-13.83000002,-61.0621827299711));
#182160=CARTESIAN_POINT('Ctrl Pts',(58.2874540965012,-13.83000002,-60.8552238163692));
#182161=CARTESIAN_POINT('Ctrl Pts',(58.2781275348581,-14.3194901627709,
-60.8508735991007));
#182162=CARTESIAN_POINT('',(58.3718694303385,-14.3184313509278,-60.42825533736));
#182163=CARTESIAN_POINT('Origin',(58.871735578318,-14.33000002,-60.42825533736));
#182164=CARTESIAN_POINT('Origin',(56.8873836197281,-14.3352374210018,-60.3207000331269));
#182165=CARTESIAN_POINT('Origin',(0.,-12.9675000200281,-60.64995));
#182166=CARTESIAN_POINT('Origin',(0.,-12.9675000200281,-60.8508735991007));
#182167=CARTESIAN_POINT('Origin',(-83.2809572255632,-20.4800000199999,-55.24995));
#182168=CARTESIAN_POINT('',(58.4684744114614,-20.48000002,-60.42825533736));
#182169=CARTESIAN_POINT('Origin',(56.2951177527026,-20.48000002,-60.2827926082911));
#182170=CARTESIAN_POINT('',(58.468474411447,-20.4800000218326,-56.1088024963487));
#182171=CARTESIAN_POINT('',(58.4684744114614,-20.48000002,-55.24995));
#182172=CARTESIAN_POINT('Ctrl Pts',(58.4684744114466,-20.4800000273303,
-56.1088024963493));
#182173=CARTESIAN_POINT('Ctrl Pts',(58.5045026577905,-20.4800000196856,
-56.1349726812018));
#182174=CARTESIAN_POINT('Ctrl Pts',(58.5397642385222,-20.48000002049,-56.1620276028471));
#182175=CARTESIAN_POINT('Ctrl Pts',(58.5742078503022,-20.4800000209351,
-56.1899586284693));
#182176=CARTESIAN_POINT('Ctrl Pts',(58.5777936723552,-20.4800000209814,
-56.1928664445334));
#182177=CARTESIAN_POINT('Ctrl Pts',(58.5813717160946,-20.4800000210458,
-56.1957839761558));
#182178=CARTESIAN_POINT('Ctrl Pts',(58.5849420358152,-20.4800000211331,
-56.1987112930781));
#182179=CARTESIAN_POINT('Ctrl Pts',(58.671257587695,-20.4800000232427,-56.2694816989377));
#182180=CARTESIAN_POINT('Ctrl Pts',(58.7525761504989,-20.4800000208245,
-56.3458655479472));
#182181=CARTESIAN_POINT('Ctrl Pts',(58.828900482798,-20.4800000205608,-56.4278416205054));
#182182=CARTESIAN_POINT('Ctrl Pts',(58.8336560351529,-20.4800000205444,
-56.4329493167426));
#182183=CARTESIAN_POINT('Ctrl Pts',(58.8383922119725,-20.4800000205339,
-56.4380787336291));
#182184=CARTESIAN_POINT('Ctrl Pts',(58.8431090189103,-20.4800000205297,
-56.4432298704634));
#182185=CARTESIAN_POINT('Ctrl Pts',(58.8623175352579,-20.480000020513,-56.4642071327073));
#182186=CARTESIAN_POINT('Ctrl Pts',(58.8812170617046,-20.4800000205714,
-56.4855758533909));
#182187=CARTESIAN_POINT('Ctrl Pts',(58.8997746305286,-20.4800000209296,
-56.5072905946435));
#182188=CARTESIAN_POINT('Ctrl Pts',(58.9619336923861,-20.4800000221292,
-56.580024688077));
#182189=CARTESIAN_POINT('Ctrl Pts',(59.0202267572588,-20.4800000217717,
-56.6567158251598));
#182190=CARTESIAN_POINT('Ctrl Pts',(59.0733581645971,-20.4800000210417,
-56.73565959907));
#182191=CARTESIAN_POINT('Ctrl Pts',(59.1299234282924,-20.4800000202645,
-56.8197054697148));
#182192=CARTESIAN_POINT('Ctrl Pts',(59.1811132500065,-20.480000019999,-56.9067351897848));
#182193=CARTESIAN_POINT('Ctrl Pts',(59.2269658512281,-20.4800000200342,
-56.9966989899188));
#182194=CARTESIAN_POINT('Ctrl Pts',(59.2370332340863,-20.4800000200419,
-57.016451413886));
#182195=CARTESIAN_POINT('Ctrl Pts',(59.2468434784441,-20.4800000200569,
-57.0363464697384));
#182196=CARTESIAN_POINT('Ctrl Pts',(59.2563966865596,-20.480000020085,-57.0563840875552));
#182197=CARTESIAN_POINT('Ctrl Pts',(59.3094659573342,-20.4800000202415,
-57.1676955708539));
#182198=CARTESIAN_POINT('Ctrl Pts',(59.354874917347,-20.4800000213417,-57.2844044844238));
#182199=CARTESIAN_POINT('Ctrl Pts',(59.3910801060422,-20.4800000212014,
-57.4030935519939));
#182200=CARTESIAN_POINT('Ctrl Pts',(59.4059237316432,-20.4800000211439,
-57.4517544247976));
#182201=CARTESIAN_POINT('Ctrl Pts',(59.4192561241221,-20.4800000207682,
-57.5006743231195));
#182202=CARTESIAN_POINT('Ctrl Pts',(59.4310694056707,-20.480000020378,-57.5498521826326));
#182203=CARTESIAN_POINT('Ctrl Pts',(59.453976422087,-20.4800000196214,-57.6452124794769));
#182204=CARTESIAN_POINT('Ctrl Pts',(59.4712138943901,-20.48000002,-57.7415452546604));
#182205=CARTESIAN_POINT('Ctrl Pts',(59.4827195432934,-20.48000002,-57.8388478504797));
#182206=CARTESIAN_POINT('Ctrl Pts',(59.4942251921967,-20.48000002,-57.936150446299));
#182207=CARTESIAN_POINT('Ctrl Pts',(59.5,-20.48000002,-58.0344221425213));
#182208=CARTESIAN_POINT('Ctrl Pts',(59.5,-20.48000002,-58.1336824582564));
#182209=CARTESIAN_POINT('Ctrl Pts',(58.3269264615434,-20.48000002,-61.0621827299711));
#182210=CARTESIAN_POINT('Ctrl Pts',(57.8224346115608,-20.48000002,-60.8252402001721));
#182211=CARTESIAN_POINT('Ctrl Pts',(57.8770125754992,-19.9259080025173,
-60.8508735991007));
#182212=CARTESIAN_POINT('Ctrl Pts',(58.4199720320461,-20.48000002,-60.8640724920291));
#182213=CARTESIAN_POINT('Ctrl Pts',(57.8773360553627,-20.480000020003,-60.6987815996246));
#182214=CARTESIAN_POINT('Ctrl Pts',(57.9394736727847,-19.9223173742648,
-60.7188022088811));
#182215=CARTESIAN_POINT('Ctrl Pts',(58.4684744074159,-20.48000002,-60.6493857962184));
#182216=CARTESIAN_POINT('Ctrl Pts',(57.9049228489562,-20.4800000199977,
-60.5656525957412));
#182217=CARTESIAN_POINT('Ctrl Pts',(57.9720322597472,-19.9204585218543,
-60.5756740647443));
#182218=CARTESIAN_POINT('Ctrl Pts',(58.4684744114614,-20.48000002,-60.42825533736));
#182219=CARTESIAN_POINT('Ctrl Pts',(57.9049228508695,-20.48000002,-60.42825533736));
#182220=CARTESIAN_POINT('Ctrl Pts',(57.9720322598041,-19.92045852138,-60.42825533736));
#182221=CARTESIAN_POINT('',(57.9720322598041,-19.92045852138,-60.42825533736));
#182222=CARTESIAN_POINT('Origin',(56.5149409813996,-20.0042112779349,-60.3314878981508));
#182223=CARTESIAN_POINT('Origin',(58.4684744114614,-19.98000002,-60.42825533736));
#182224=CARTESIAN_POINT('Ctrl Pts',(59.5,-20.48000002,-58.1336824582564));
#182225=CARTESIAN_POINT('Ctrl Pts',(60.,-20.48000002,-58.1336824582564));
#182226=CARTESIAN_POINT('Ctrl Pts',(60.,-20.98000002,-58.1336824582564));
#182227=CARTESIAN_POINT('Ctrl Pts',(59.4999999932334,-20.48000002,-57.8840234061944));
#182228=CARTESIAN_POINT('Ctrl Pts',(60.0019943000202,-20.4800000199965,
-57.8335762296713));
#182229=CARTESIAN_POINT('Ctrl Pts',(60.,-20.9819903749844,-57.8341710601268));
#182230=CARTESIAN_POINT('Ctrl Pts',(59.4634620545497,-20.48000002,-57.6404834185301));
#182231=CARTESIAN_POINT('Ctrl Pts',(59.9599487537765,-20.4800000200004,
-57.5408569976555));
#182232=CARTESIAN_POINT('Ctrl Pts',(59.9561544625383,-20.9839354847036,
-57.5420008057396));
#182233=CARTESIAN_POINT('Ctrl Pts',(59.3548394021004,-20.48000002,-57.2844137892711));
#182234=CARTESIAN_POINT('Ctrl Pts',(59.8322564407851,-20.4800000199998,
-57.1124079291466));
#182235=CARTESIAN_POINT('Ctrl Pts',(59.8258072839812,-20.986783840298,-57.1148311652303));
#182236=CARTESIAN_POINT('Ctrl Pts',(59.3094493357903,-20.48000002,-57.1677018516063));
#182237=CARTESIAN_POINT('Ctrl Pts',(59.7785418471728,-20.4800000199998,
-56.971709946724));
#182238=CARTESIAN_POINT('Ctrl Pts',(59.7713392035954,-20.9877182523804,
-56.9748142265907));
#182239=CARTESIAN_POINT('Ctrl Pts',(59.2033273904236,-20.48000002,-56.945074258738));
#182240=CARTESIAN_POINT('Ctrl Pts',(59.6524902953505,-20.4800000200002,
-56.7030545690594));
#182241=CARTESIAN_POINT('Ctrl Pts',(59.6439928678614,-20.9895019296767,
-56.7077325083257));
#182242=CARTESIAN_POINT('Ctrl Pts',(59.1423240613999,-20.48000002,-56.8381621017045));
#182243=CARTESIAN_POINT('Ctrl Pts',(59.5798070038494,-20.4800000200006,
-56.5739310816022));
#182244=CARTESIAN_POINT('Ctrl Pts',(59.5707888728218,-20.9903591646404,
-56.5794722449985));
#182245=CARTESIAN_POINT('Ctrl Pts',(59.0043387205048,-20.48000002,-56.6331931445326));
#182246=CARTESIAN_POINT('Ctrl Pts',(59.4150201769345,-20.4800000199993,
-56.3261371955428));
#182247=CARTESIAN_POINT('Ctrl Pts',(59.4052064654638,-20.9920036864946,
-56.333575365965));
#182248=CARTESIAN_POINT('Ctrl Pts',(58.9266500387652,-20.48000002,-56.5344951934464));
#182249=CARTESIAN_POINT('Ctrl Pts',(59.322050076116,-20.4800000199998,-56.2067284595684));
#182250=CARTESIAN_POINT('Ctrl Pts',(59.3119800474081,-20.9927961294943,
-56.2151695770875));
#182251=CARTESIAN_POINT('Ctrl Pts',(58.7595340502496,-20.48000002,-56.3519956346149));
#182252=CARTESIAN_POINT('Ctrl Pts',(59.1217230649246,-20.4800000200002,
-55.9857285998647));
#182253=CARTESIAN_POINT('Ctrl Pts',(59.1114408594098,-20.9942622260151,
-55.9962288706011));
#182254=CARTESIAN_POINT('Ctrl Pts',(58.6698748748721,-20.48000002,-56.2676023678844));
#182255=CARTESIAN_POINT('Ctrl Pts',(59.0140876322601,-20.4800000199996,
-55.8834675579712));
#182256=CARTESIAN_POINT('Ctrl Pts',(59.0038498495005,-20.9949406197357,
-55.8949841496734));
#182257=CARTESIAN_POINT('Ctrl Pts',(58.3828160087866,-20.48000002,-56.0347423933717));
#182258=CARTESIAN_POINT('Ctrl Pts',(58.6688057859238,-20.4800000200008,
-55.6008859078189));
#182259=CARTESIAN_POINT('Ctrl Pts',(58.6593792112359,-20.9968132967355,
-55.6156272797255));
#182260=CARTESIAN_POINT('Ctrl Pts',(58.1642057412792,-20.48000002,-55.9059968521648));
#182261=CARTESIAN_POINT('Ctrl Pts',(58.4055356761976,-20.48000002,-55.4446537909846));
#182262=CARTESIAN_POINT('Ctrl Pts',(58.3970469849622,-20.9978498953169,
-55.4611742661273));
#182263=CARTESIAN_POINT('Ctrl Pts',(57.9370780887383,-20.48000002,-55.8140933660895));
#182264=CARTESIAN_POINT('Ctrl Pts',(58.1317309492636,-20.48000002,-55.333033840343));
#182265=CARTESIAN_POINT('Ctrl Pts',(58.124493706486,-20.9985901469525,-55.3509197556537));
#182266=CARTESIAN_POINT('',(58.1440639001758,-20.9985364556102,-55.3589167601746));
#182267=CARTESIAN_POINT('Ctrl Pts',(58.4684744114473,-20.48000002,-56.1088024963483));
#182268=CARTESIAN_POINT('Ctrl Pts',(58.4586150911592,-20.48000002,-56.0809060452476));
#182269=CARTESIAN_POINT('Ctrl Pts',(58.4488675441718,-20.4808273659407,
-56.0533341538256));
#182270=CARTESIAN_POINT('Ctrl Pts',(58.439271777189,-20.4825381006774,-56.0262356118932));
#182271=CARTESIAN_POINT('Ctrl Pts',(58.4296891837088,-20.48424648684,-55.9991742720642));
#182272=CARTESIAN_POINT('Ctrl Pts',(58.4202577260069,-20.4868361379938,
-55.9725846325975));
#182273=CARTESIAN_POINT('Ctrl Pts',(58.4110077262225,-20.4903202028564,
-55.9465867869018));
#182274=CARTESIAN_POINT('Ctrl Pts',(58.4017480313994,-20.4938079194103,
-55.9205616925438));
#182275=CARTESIAN_POINT('Ctrl Pts',(58.3926699352244,-20.498192148329,-55.8951292415358));
#182276=CARTESIAN_POINT('Ctrl Pts',(58.3837978306082,-20.5034393255163,
-55.8703873223567));
#182277=CARTESIAN_POINT('Ctrl Pts',(58.3807115576895,-20.5052646219429,
-55.8617805353066));
#182278=CARTESIAN_POINT('Ctrl Pts',(58.3776501749549,-20.5071939136685,
-55.8532571361302));
#182279=CARTESIAN_POINT('Ctrl Pts',(58.3746146206988,-20.5092244012644,
-55.8448207432431));
#182280=CARTESIAN_POINT('Ctrl Pts',(58.372584139124,-20.5105825939711,-55.8391776418951));
#182281=CARTESIAN_POINT('Ctrl Pts',(58.3705639943634,-20.5119868533931,
-55.8335700753922));
#182282=CARTESIAN_POINT('Ctrl Pts',(58.3685538250691,-20.513436845991,-55.8279973372639));
#182283=CARTESIAN_POINT('Ctrl Pts',(58.356908165411,-20.5218371933395,-55.7957123890315));
#182284=CARTESIAN_POINT('Ctrl Pts',(58.345722168638,-20.5317310834707,-55.7649671511734));
#182285=CARTESIAN_POINT('Ctrl Pts',(58.3349661329889,-20.5429610115905,
-55.7358347356634));
#182286=CARTESIAN_POINT('Ctrl Pts',(58.331203594624,-20.5468893209383,-55.7256440079089));
#182287=CARTESIAN_POINT('Ctrl Pts',(58.3274943627873,-20.5509806039353,
-55.7156522861301));
#182288=CARTESIAN_POINT('Ctrl Pts',(58.3238427942605,-20.5552206711044,
-55.7058765663973));
#182289=CARTESIAN_POINT('Ctrl Pts',(58.3170555585969,-20.5631017597089,
-55.6877062614668));
#182290=CARTESIAN_POINT('Ctrl Pts',(58.3104649056126,-20.5715004822433,
-55.6702758635727));
#182291=CARTESIAN_POINT('Ctrl Pts',(58.3040799989639,-20.5803327986885,
-55.6536339393015));
#182292=CARTESIAN_POINT('Ctrl Pts',(58.3025560644027,-20.5824408752864,
-55.6496618838029));
#182293=CARTESIAN_POINT('Ctrl Pts',(58.3010438398826,-20.5845735942753,
-55.6457346626762));
#182294=CARTESIAN_POINT('Ctrl Pts',(58.2995426903113,-20.5867294931232,
-55.6418526824923));
#182295=CARTESIAN_POINT('Ctrl Pts',(58.2985759382629,-20.5881179088196,
-55.6393526569341));
#182296=CARTESIAN_POINT('Ctrl Pts',(58.2977808636943,-20.5892719552472,
-55.6373028066408));
#182297=CARTESIAN_POINT('Ctrl Pts',(58.2968349661429,-20.590661088457,-55.6348682143808));
#182298=CARTESIAN_POINT('Ctrl Pts',(58.2963120964897,-20.5914289682328,
-55.6335224297249));
#182299=CARTESIAN_POINT('Ctrl Pts',(58.2957432270931,-20.5922691774031,
-55.6320595294283));
#182300=CARTESIAN_POINT('Ctrl Pts',(58.2950747550774,-20.5932660660372,
-55.6303431344072));
#182301=CARTESIAN_POINT('Ctrl Pts',(58.2900178290309,-20.6008074319887,
-55.6173587723347));
#182302=CARTESIAN_POINT('Ctrl Pts',(58.2850433892305,-20.6086930001856,
-55.6047650614861));
#182303=CARTESIAN_POINT('Ctrl Pts',(58.2801491749767,-20.6169112684622,
-55.592573393822));
#182304=CARTESIAN_POINT('Ctrl Pts',(58.2713709378619,-20.6316515115047,
-55.5707064823976));
#182305=CARTESIAN_POINT('Ctrl Pts',(58.2627681449031,-20.6476358689355,
-55.5499597889634));
#182306=CARTESIAN_POINT('Ctrl Pts',(58.254476934651,-20.6644577685415,-55.5307492203234));
#182307=CARTESIAN_POINT('Ctrl Pts',(58.2536586343129,-20.6661180045886,
-55.5288532347755));
#182308=CARTESIAN_POINT('Ctrl Pts',(58.2528433587981,-20.6677864207776,
-55.5269721777696));
#182309=CARTESIAN_POINT('Ctrl Pts',(58.2520312322312,-20.6694626407703,
-55.5251064264037));
#182310=CARTESIAN_POINT('Ctrl Pts',(58.2480809834245,-20.6776159093564,
-55.5160312620064));
#182311=CARTESIAN_POINT('Ctrl Pts',(58.2441869744578,-20.6859920750144,
-55.5072765956881));
#182312=CARTESIAN_POINT('Ctrl Pts',(58.2403741015214,-20.6945317630243,
-55.4989136304009));
#182313=CARTESIAN_POINT('Ctrl Pts',(58.23462630594,-20.7074050955028,-55.4863067023113));
#182314=CARTESIAN_POINT('Ctrl Pts',(58.2290253841356,-20.7207049709202,
-55.4744915876949));
#182315=CARTESIAN_POINT('Ctrl Pts',(58.2235931329491,-20.7343275732196,
-55.4635422532062));
#182316=CARTESIAN_POINT('Ctrl Pts',(58.2233045901595,-20.7350511597281,
-55.4629606616323));
#182317=CARTESIAN_POINT('Ctrl Pts',(58.2230165181509,-20.7357756590578,
-55.4623814942482));
#182318=CARTESIAN_POINT('Ctrl Pts',(58.2227289185889,-20.7365010563778,
-55.4618047562331));
#182319=CARTESIAN_POINT('Ctrl Pts',(58.2211799409448,-20.7404079616034,
-55.4586985126577));
#182320=CARTESIAN_POINT('Ctrl Pts',(58.2197601559258,-20.7440451813824,
-55.455891187346));
#182321=CARTESIAN_POINT('Ctrl Pts',(58.2182954339984,-20.7478497743153,
-55.4530339549268));
#182322=CARTESIAN_POINT('Ctrl Pts',(58.2169581009907,-20.7513234764663,
-55.4504252200174));
#182323=CARTESIAN_POINT('Ctrl Pts',(58.215583381558,-20.7549368044839,-55.4477750853123));
#182324=CARTESIAN_POINT('Ctrl Pts',(58.214044479382,-20.7590469742192,-55.4448585269748));
#182325=CARTESIAN_POINT('Ctrl Pts',(58.2138978898006,-20.7594384923225,
-55.4445807074535));
#182326=CARTESIAN_POINT('Ctrl Pts',(58.2137498149301,-20.7598345391474,
-55.4443005040552));
#182327=CARTESIAN_POINT('Ctrl Pts',(58.213600148105,-20.7602354371672,-55.4440177446864));
#182328=CARTESIAN_POINT('Ctrl Pts',(58.2104546875774,-20.7686608774503,
-55.4380751556515));
#182329=CARTESIAN_POINT('Ctrl Pts',(58.2073520730329,-20.7772343205362,
-55.4324114748485));
#182330=CARTESIAN_POINT('Ctrl Pts',(58.2042901618585,-20.7859515214014,
-55.4270285632346));
#182331=CARTESIAN_POINT('Ctrl Pts',(58.1971740881793,-20.806210843145,-55.4145183389103));
#182332=CARTESIAN_POINT('Ctrl Pts',(58.19034522719,-20.8270685485376,-55.4036834413138));
#182333=CARTESIAN_POINT('Ctrl Pts',(58.1838456279207,-20.8482481887169,
-55.3945762010636));
#182334=CARTESIAN_POINT('Ctrl Pts',(58.1774578070436,-20.8690635870367,
-55.3856255847266));
#182335=CARTESIAN_POINT('Ctrl Pts',(58.1713880933815,-20.8901892328584,
-55.3783437776686));
#182336=CARTESIAN_POINT('Ctrl Pts',(58.1656668372239,-20.9113682799489,
-55.3727319242401));
#182337=CARTESIAN_POINT('Ctrl Pts',(58.1600697310871,-20.9320877462992,
-55.3672418468169));
#182338=CARTESIAN_POINT('Ctrl Pts',(58.1548061566892,-20.9528577928021,
-55.3633499650214));
#182339=CARTESIAN_POINT('Ctrl Pts',(58.1498945349745,-20.973452350577,-55.3610106076793));
#182340=CARTESIAN_POINT('Ctrl Pts',(58.1478923796479,-20.9818474400081,
-55.3600570006967));
#182341=CARTESIAN_POINT('Ctrl Pts',(58.1459485875571,-20.9902135813046,
-55.3593608307665));
#182342=CARTESIAN_POINT('Ctrl Pts',(58.1440639002148,-20.9985364556096,
-55.3589167601806));
#182343=CARTESIAN_POINT('Ctrl Pts',(60.,-20.98000002,-58.1336824582564));
#182344=CARTESIAN_POINT('Ctrl Pts',(59.9999999997674,-20.9803021616334,
-58.0882157632118));
#182345=CARTESIAN_POINT('Ctrl Pts',(60.0003031804244,-20.9808684474578,
-57.9944661926472));
#182346=CARTESIAN_POINT('Ctrl Pts',(59.9796366043166,-20.9822991402003,
-57.777034661397));
#182347=CARTESIAN_POINT('Ctrl Pts',(59.9689735227541,-20.9828743238743,
-57.6917239003171));
#182348=CARTESIAN_POINT('Ctrl Pts',(59.942094721024,-20.9838800398805,-57.544675306863));
#182349=CARTESIAN_POINT('Ctrl Pts',(59.9313020397326,-20.9842386835097,
-57.4924893380618));
#182350=CARTESIAN_POINT('Ctrl Pts',(59.9115468165673,-20.9848053002678,
-57.4096254596961));
#182351=CARTESIAN_POINT('Ctrl Pts',(59.9007760151545,-20.9850956924844,
-57.3670492763596));
#182352=CARTESIAN_POINT('Ctrl Pts',(59.8864524794301,-20.9854444946362,
-57.3154362005822));
#182353=CARTESIAN_POINT('Ctrl Pts',(59.878825961181,-20.9856210151906,-57.2891542770501));
#182354=CARTESIAN_POINT('Ctrl Pts',(59.8754551313071,-20.9856970774085,
-57.2777898441744));
#182355=CARTESIAN_POINT('Ctrl Pts',(59.8731848670668,-20.9857478716902,
-57.2701912967782));
#182356=CARTESIAN_POINT('Ctrl Pts',(59.8716798328276,-20.9857811954749,
-57.2651985555473));
#182357=CARTESIAN_POINT('Ctrl Pts',(59.8196830912949,-20.9869250078408,
-57.0936552223813));
#182358=CARTESIAN_POINT('Ctrl Pts',(59.757474576671,-20.9879592746227,-56.9421719733048));
#182359=CARTESIAN_POINT('Ctrl Pts',(59.6596400021207,-20.9892878172319,
-56.743058949969));
#182360=CARTESIAN_POINT('Ctrl Pts',(59.6262622512368,-20.9896958019818,
-56.6813165976652));
#182361=CARTESIAN_POINT('Ctrl Pts',(59.5763474792179,-20.9902612715535,
-56.595487236136));
#182362=CARTESIAN_POINT('Ctrl Pts',(59.5514253393024,-20.9905325160149,
-56.5542652258299));
#182363=CARTESIAN_POINT('Ctrl Pts',(59.5226651625736,-20.9908313281143,
-56.5090707039936));
#182364=CARTESIAN_POINT('Ctrl Pts',(59.5083933141467,-20.9909767015006,
-56.4871881701081));
#182365=CARTESIAN_POINT('Ctrl Pts',(59.5023030840063,-20.9910381814721,
-56.4779620351937));
#182366=CARTESIAN_POINT('Ctrl Pts',(59.4982491056196,-20.9910789899889,
-56.4718449554271));
#182367=CARTESIAN_POINT('Ctrl Pts',(59.4970283633816,-20.9910912648199,
-56.470005589356));
#182368=CARTESIAN_POINT('Ctrl Pts',(59.313480930561,-20.9929287419126,-56.1952337005415));
#182369=CARTESIAN_POINT('Ctrl Pts',(59.0944609290821,-20.9945975243808,
-55.9642839660056));
#182370=CARTESIAN_POINT('Ctrl Pts',(58.629062442157,-20.9970596244464,-55.5957578652104));
#182371=CARTESIAN_POINT('Ctrl Pts',(58.3833111942037,-20.997873466999,-55.4576663025591));
#182372=CARTESIAN_POINT('Ctrl Pts',(58.1440639002148,-20.9985364556097,
-55.3589167601806));
#182373=CARTESIAN_POINT('Ctrl Pts',(60.,-21.4835561881163,-58.1534328789326));
#182374=CARTESIAN_POINT('Ctrl Pts',(60.,-21.563522065113,-56.0718305306274));
#182375=CARTESIAN_POINT('Ctrl Pts',(58.0481390063499,-21.5914605167321,
-55.3445609916381));
#182376=CARTESIAN_POINT('Ctrl Pts',(60.,-21.2836204844253,-58.1457522408661));
#182377=CARTESIAN_POINT('Ctrl Pts',(60.,-21.3649831049967,-56.0851953591943));
#182378=CARTESIAN_POINT('Ctrl Pts',(58.0747408021896,-21.3932704964989,
-55.3468739572293));
#182379=CARTESIAN_POINT('Ctrl Pts',(60.,-21.0836896865644,-58.1378552621726));
#182380=CARTESIAN_POINT('Ctrl Pts',(59.9999999999994,-21.1653697703472,
-56.0975649789357));
#182381=CARTESIAN_POINT('Ctrl Pts',(58.1004355836544,-21.1945366814225,
-55.3490436413214));
#182382=CARTESIAN_POINT('Ctrl Pts',(60.,-20.883761812232,-58.1298294552074));
#182383=CARTESIAN_POINT('Ctrl Pts',(60.,-20.9648839320844,-56.1090266406885));
#182384=CARTESIAN_POINT('Ctrl Pts',(58.125215629935,-20.9953105578148,-55.3510803367175));
#182385=CARTESIAN_POINT('',(58.0831736435082,-21.4980516422208,-55.3542805423663));
#182386=CARTESIAN_POINT('Origin',(-8.40711756300142,-13.0336338896511,-43.9501499496686));
#182387=CARTESIAN_POINT('Ctrl Pts',(58.0831736437664,-21.4980516416407,
-55.3542805420642));
#182388=CARTESIAN_POINT('Ctrl Pts',(58.328880105512,-21.4974329387565,-55.4494594480312));
#182389=CARTESIAN_POINT('Ctrl Pts',(58.5819986525787,-21.496667325676,-55.5851943042097));
#182390=CARTESIAN_POINT('Ctrl Pts',(58.9421891742166,-21.4948870882606,
-55.8607175379279));
#182391=CARTESIAN_POINT('Ctrl Pts',(59.0588349730988,-21.4941941804047,
-55.9643994055085));
#182392=CARTESIAN_POINT('Ctrl Pts',(59.2238479950859,-21.4930296920426,
-56.1371500164854));
#182393=CARTESIAN_POINT('Ctrl Pts',(59.277189135564,-21.4926213279021,-56.1975881869849));
#182394=CARTESIAN_POINT('Ctrl Pts',(59.3540961478811,-21.4919877224573,
-56.2923012574398));
#182395=CARTESIAN_POINT('Ctrl Pts',(59.3917736538965,-21.4916657225195,
-56.3406700118079));
#182396=CARTESIAN_POINT('Ctrl Pts',(59.4342429947178,-21.4912836974144,
-56.3988037705104));
#182397=CARTESIAN_POINT('Ctrl Pts',(59.4550899460893,-21.4910914903132,
-56.4282866914381));
#182398=CARTESIAN_POINT('Ctrl Pts',(59.4639395974477,-21.4910089034144,
-56.4410102944696));
#182399=CARTESIAN_POINT('Ctrl Pts',(59.4698203457393,-21.4909538032558,
-56.4495121422603));
#182400=CARTESIAN_POINT('Ctrl Pts',(59.4735908274035,-21.4909183023144,
-56.4550001430341));
#182401=CARTESIAN_POINT('Ctrl Pts',(59.542285134935,-21.4902695208188,-56.555417590677));
#182402=CARTESIAN_POINT('Ctrl Pts',(59.6128041666099,-21.4895473392752,
-56.6706953615194));
#182403=CARTESIAN_POINT('Ctrl Pts',(59.7142648109625,-21.4882466783812,
-56.8726506836425));
#182404=CARTESIAN_POINT('Ctrl Pts',(59.7473290208614,-21.4877779516545,
-56.9447822044543));
#182405=CARTESIAN_POINT('Ctrl Pts',(59.7942525909409,-21.4870264865754,
-57.060112388415));
#182406=CARTESIAN_POINT('Ctrl Pts',(59.809446818066,-21.4867680588891,-57.0997414460801));
#182407=CARTESIAN_POINT('Ctrl Pts',(59.8313655304725,-21.486370290246,-57.1609210038875));
#182408=CARTESIAN_POINT('Ctrl Pts',(59.8421066577016,-21.4861688880082,
-57.1919444189843));
#182409=CARTESIAN_POINT('Ctrl Pts',(59.8542113411722,-21.4859300541667,
-57.2288840491873));
#182410=CARTESIAN_POINT('Ctrl Pts',(59.8601514196854,-21.4858097506293,
-57.2475383191946));
#182411=CARTESIAN_POINT('Ctrl Pts',(59.8626725113407,-21.4857580107985,
-57.2555723150833));
#182412=CARTESIAN_POINT('Ctrl Pts',(59.8643476932872,-21.4857234783297,
-57.2609370226343));
#182413=CARTESIAN_POINT('Ctrl Pts',(59.8648369543695,-21.4857133796908,
-57.2625060652884));
#182414=CARTESIAN_POINT('Ctrl Pts',(59.9413789268569,-21.4841213872645,
-57.5100727167539));
#182415=CARTESIAN_POINT('Ctrl Pts',(59.9705840598595,-21.4827732241292,
-57.7085238060111));
#182416=CARTESIAN_POINT('Ctrl Pts',(59.9999460396104,-21.4809004491039,
-58.003826414933));
#182417=CARTESIAN_POINT('Ctrl Pts',(60.,-21.4803288263114,-58.1018950252691));
#182418=CARTESIAN_POINT('Ctrl Pts',(60.,-21.48000002,-58.1532962439713));
#182419=CARTESIAN_POINT('Ctrl Pts',(60.,-21.48000002,-58.1532962439713));
#182420=CARTESIAN_POINT('Ctrl Pts',(60.,-21.98000002,-58.1532962439712));
#182421=CARTESIAN_POINT('Ctrl Pts',(59.5,-21.98000002,-58.1532962439713));
#182422=CARTESIAN_POINT('Ctrl Pts',(60.,-21.4819649551771,-57.8461243349599));
#182423=CARTESIAN_POINT('Ctrl Pts',(59.9980388947882,-21.98000002,-57.846724408982));
#182424=CARTESIAN_POINT('Ctrl Pts',(59.4999999930587,-21.98000002,-57.8972567292831));
#182425=CARTESIAN_POINT('Ctrl Pts',(59.9539303867693,-21.4838860106857,
-57.5466594347187));
#182426=CARTESIAN_POINT('Ctrl Pts',(59.9502437945621,-21.9800000199991,
-57.5478013960511));
#182427=CARTESIAN_POINT('Ctrl Pts',(59.4616086582853,-21.98000002,-57.6476410381502));
#182428=CARTESIAN_POINT('Ctrl Pts',(59.8167663234865,-21.4866995950233,
-57.1091506902012));
#182429=CARTESIAN_POINT('Ctrl Pts',(59.8105866338858,-21.9800000200004,
-57.1115394631459));
#182430=CARTESIAN_POINT('Ctrl Pts',(59.34730526825,-21.98000002,-57.282960076491));
#182431=CARTESIAN_POINT('Ctrl Pts',(59.7596240701279,-21.4876191423699,
-56.9663510387935));
#182432=CARTESIAN_POINT('Ctrl Pts',(59.7527585815745,-21.9800000200004,
-56.9693956543515));
#182433=CARTESIAN_POINT('Ctrl Pts',(59.29968672466,-21.98000002,-57.1639308209523));
#182434=CARTESIAN_POINT('Ctrl Pts',(59.6259954411174,-21.4893742131836,
-56.694110313108));
#182435=CARTESIAN_POINT('Ctrl Pts',(59.6179788443353,-21.9800000199995,
-56.6986593938776));
#182436=CARTESIAN_POINT('Ctrl Pts',(59.1883295347111,-21.98000002,-56.9370071244832));
#182437=CARTESIAN_POINT('Ctrl Pts',(59.5491776307125,-21.4902170457339,
-56.5635325439996));
#182438=CARTESIAN_POINT('Ctrl Pts',(59.5407153644089,-21.9800000200004,
-56.5688983662156));
#182439=CARTESIAN_POINT('Ctrl Pts',(59.1243146931145,-21.98000002,-56.8281652030541));
#182440=CARTESIAN_POINT('Ctrl Pts',(59.3752915646391,-21.4918319317587,
-56.3135970508604));
#182441=CARTESIAN_POINT('Ctrl Pts',(59.3661855631985,-21.9800000199995,
-56.3207427939796));
#182442=CARTESIAN_POINT('Ctrl Pts',(58.9794096363452,-21.98000002,-56.6198336495764));
#182443=CARTESIAN_POINT('Ctrl Pts',(59.2775781171727,-21.4926066631124,
-56.1938276864606));
#182444=CARTESIAN_POINT('Ctrl Pts',(59.268291108539,-21.98000002,-56.2019010018047));
#182445=CARTESIAN_POINT('Ctrl Pts',(58.897981763705,-21.98000002,-56.5200008958119));
#182446=CARTESIAN_POINT('Ctrl Pts',(59.0680465560033,-21.4940322909708,
-55.9736253396869));
#182447=CARTESIAN_POINT('Ctrl Pts',(59.058685939558,-21.98000002,-55.9835815924875));
#182448=CARTESIAN_POINT('Ctrl Pts',(58.7233721306083,-21.98000002,-56.3364530063454));
#182449=CARTESIAN_POINT('Ctrl Pts',(58.9556221515304,-21.4946900550471,
-55.8721285607086));
#182450=CARTESIAN_POINT('Ctrl Pts',(58.9463663728276,-21.98000002,-55.8830032045419));
#182451=CARTESIAN_POINT('Ctrl Pts',(58.6296851267041,-21.98000002,-56.251851153689));
#182452=CARTESIAN_POINT('Ctrl Pts',(58.5954423658223,-21.4964978360334,
-55.5933734977247));
#182453=CARTESIAN_POINT('Ctrl Pts',(58.587136508474,-21.98000002,-55.607131606824));
#182454=CARTESIAN_POINT('Ctrl Pts',(58.3295353039945,-21.98000002,-56.0194969731979));
#182455=CARTESIAN_POINT('Ctrl Pts',(58.3219561351612,-21.4974802329133,
-55.4421752934307));
#182456=CARTESIAN_POINT('Ctrl Pts',(58.3146314565664,-21.9800000200043,
-55.4574637281066));
#182457=CARTESIAN_POINT('Ctrl Pts',(58.1016300300823,-21.98000002,-55.8934667289665));
#182458=CARTESIAN_POINT('Ctrl Pts',(58.0398165251616,-21.4981583243581,
-55.3378696135325));
#182459=CARTESIAN_POINT('Ctrl Pts',(58.0337433152366,-21.98000002,-55.3542930871701));
#182460=CARTESIAN_POINT('Ctrl Pts',(57.866513770968,-21.98000002,-55.8065234638013));
#182461=CARTESIAN_POINT('',(58.1141118834537,-21.9800000069849,-55.913606468422));
#182462=CARTESIAN_POINT('Ctrl Pts',(58.0831736436236,-21.4980516422303,
-55.3542805420318));
#182463=CARTESIAN_POINT('Ctrl Pts',(58.077688301736,-21.5206990055623,-55.3530326053872));
#182464=CARTESIAN_POINT('Ctrl Pts',(58.0725563121906,-21.543329300244,-55.3536411745602));
#182465=CARTESIAN_POINT('Ctrl Pts',(58.0678467194416,-21.5655936151685,
-55.3560017266602));
#182466=CARTESIAN_POINT('Ctrl Pts',(58.0651885351446,-21.5781600206881,
-55.3573340674503));
#182467=CARTESIAN_POINT('Ctrl Pts',(58.0626646730493,-21.5906101815618,
-55.3592237425858));
#182468=CARTESIAN_POINT('Ctrl Pts',(58.0602853929275,-21.6028853626772,
-55.3616460932885));
#182469=CARTESIAN_POINT('Ctrl Pts',(58.0581274670246,-21.6140185331889,
-55.363843082739));
#182470=CARTESIAN_POINT('Ctrl Pts',(58.0561201685456,-21.6248395435586,
-55.3664403549057));
#182471=CARTESIAN_POINT('Ctrl Pts',(58.0542338762529,-21.6354769720973,
-55.3694355679586));
#182472=CARTESIAN_POINT('Ctrl Pts',(58.0523609362085,-21.646039102874,-55.3724095791921));
#182473=CARTESIAN_POINT('Ctrl Pts',(58.0506071882539,-21.6564208249666,
-55.3757761530634));
#182474=CARTESIAN_POINT('Ctrl Pts',(58.0489554951375,-21.6667374214667,
-55.3795809979916));
#182475=CARTESIAN_POINT('Ctrl Pts',(58.0477878397693,-21.6740306826454,
-55.3822708121959));
#182476=CARTESIAN_POINT('Ctrl Pts',(58.0466714218907,-21.6812912032906,
-55.3851806278496));
#182477=CARTESIAN_POINT('Ctrl Pts',(58.0456043472203,-21.6885540001523,
-55.3883406910768));
#182478=CARTESIAN_POINT('Ctrl Pts',(58.0450552768195,-21.6922911208005,
-55.3899667227229));
#182479=CARTESIAN_POINT('Ctrl Pts',(58.0445190796661,-21.6960309511488,
-55.3916600870712));
#182480=CARTESIAN_POINT('Ctrl Pts',(58.0439958538933,-21.6997781149038,
-55.3934253930027));
#182481=CARTESIAN_POINT('Ctrl Pts',(58.041921572838,-21.7146334052805,-55.400423788037));
#182482=CARTESIAN_POINT('Ctrl Pts',(58.0401111928462,-21.7292088227908,
-55.4083741119359));
#182483=CARTESIAN_POINT('Ctrl Pts',(58.0386022975759,-21.7433237632393,
-55.4171742771625));
#182484=CARTESIAN_POINT('Ctrl Pts',(58.0370898725513,-21.757471722728,-55.4259950285905));
#182485=CARTESIAN_POINT('Ctrl Pts',(58.0358805473388,-21.7711563450861,
-55.4356690560707));
#182486=CARTESIAN_POINT('Ctrl Pts',(58.0349963567716,-21.7842200732956,
-55.4460497826742));
#182487=CARTESIAN_POINT('Ctrl Pts',(58.0341155424912,-21.7972339175853,
-55.4563908704147));
#182488=CARTESIAN_POINT('Ctrl Pts',(58.0335575229446,-21.8096310261443,
-55.4674326276423));
#182489=CARTESIAN_POINT('Ctrl Pts',(58.0333258610528,-21.8212893245516,
-55.4789957790404));
#182490=CARTESIAN_POINT('Ctrl Pts',(58.0331490294813,-21.830188307514,-55.4878221346276));
#182491=CARTESIAN_POINT('Ctrl Pts',(58.0331619852258,-21.838657468733,-55.4969515115536));
#182492=CARTESIAN_POINT('Ctrl Pts',(58.0333585110965,-21.8466585948979,
-55.5062941612126));
#182493=CARTESIAN_POINT('Ctrl Pts',(58.0334888523122,-21.8519651558504,
-55.5124904564405));
#182494=CARTESIAN_POINT('Ctrl Pts',(58.0337006581951,-21.8570756893028,
-55.5187903954443));
#182495=CARTESIAN_POINT('Ctrl Pts',(58.0339893274825,-21.861986887608,-55.5251637203642));
#182496=CARTESIAN_POINT('Ctrl Pts',(58.0350033551333,-21.8792387779142,
-55.5475517192948));
#182497=CARTESIAN_POINT('Ctrl Pts',(58.0370308035539,-21.8947384255673,
-55.5717746381603));
#182498=CARTESIAN_POINT('Ctrl Pts',(58.0400916132891,-21.9083235411587,
-55.5973841240798));
#182499=CARTESIAN_POINT('Ctrl Pts',(58.0407096798096,-21.9110667711702,
-55.6025554242342));
#182500=CARTESIAN_POINT('Ctrl Pts',(58.041369802248,-21.9137320745735,-55.6077832055866));
#182501=CARTESIAN_POINT('Ctrl Pts',(58.0420720205664,-21.9163183295388,
-55.6130637074408));
#182502=CARTESIAN_POINT('Ctrl Pts',(58.0441619042696,-21.9240153262748,
-55.6287790974864));
#182503=CARTESIAN_POINT('Ctrl Pts',(58.0466233370326,-21.9310133400415,
-55.6449634250592));
#182504=CARTESIAN_POINT('Ctrl Pts',(58.0494650175479,-21.9372880694643,
-55.6615286492183));
#182505=CARTESIAN_POINT('Ctrl Pts',(58.0505762686844,-21.9397418288384,
-55.6680065499095));
#182506=CARTESIAN_POINT('Ctrl Pts',(58.0517907300022,-21.9421772063289,
-55.6747968723622));
#182507=CARTESIAN_POINT('Ctrl Pts',(58.0530602395296,-21.9444746087411,
-55.6815997527206));
#182508=CARTESIAN_POINT('Ctrl Pts',(58.0535478411702,-21.9453570102994,
-55.6842126481357));
#182509=CARTESIAN_POINT('Ctrl Pts',(58.0540433298046,-21.9462194821836,
-55.6868271396655));
#182510=CARTESIAN_POINT('Ctrl Pts',(58.05454309135,-21.9470568630598,-55.6894253280722));
#182511=CARTESIAN_POINT('Ctrl Pts',(58.0559071998638,-21.9493425098708,
-55.6965171320703));
#182512=CARTESIAN_POINT('Ctrl Pts',(58.0573071807538,-21.9514417852041,
-55.7034977235522));
#182513=CARTESIAN_POINT('Ctrl Pts',(58.0586499612016,-21.9532837016386,
-55.709985247384));
#182514=CARTESIAN_POINT('Ctrl Pts',(58.0588097209061,-21.9535028469396,
-55.7107571121312));
#182515=CARTESIAN_POINT('Ctrl Pts',(58.0589686435043,-21.95371839633,-55.7115219721044));
#182516=CARTESIAN_POINT('Ctrl Pts',(58.0591265512438,-21.9539302663629,
-55.7122791654125));
#182517=CARTESIAN_POINT('Ctrl Pts',(58.0650058136374,-21.9618186670249,
-55.7404711853563));
#182518=CARTESIAN_POINT('Ctrl Pts',(58.0720079755593,-21.9679281060019,
-55.7699383340652));
#182519=CARTESIAN_POINT('Ctrl Pts',(58.0801172540501,-21.9722379734285,
-55.8003568758901));
#182520=CARTESIAN_POINT('Ctrl Pts',(58.0886478415444,-21.9767717554675,
-55.8323557809448));
#182521=CARTESIAN_POINT('Ctrl Pts',(58.098403737083,-21.9793141024895,-55.8654069450485));
#182522=CARTESIAN_POINT('Ctrl Pts',(58.1093418112629,-21.9798788055287,
-55.8990986009792));
#182523=CARTESIAN_POINT('Ctrl Pts',(58.1109077045422,-21.9799596483424,
-55.9039218940676));
#182524=CARTESIAN_POINT('Ctrl Pts',(58.112497784602,-21.98000002,-55.9087582670901));
#182525=CARTESIAN_POINT('Ctrl Pts',(58.1141118834575,-21.98000002,-55.9136064684135));
#182526=CARTESIAN_POINT('Ctrl Pts',(59.5,-21.98000002,-58.1532962439713));
#182527=CARTESIAN_POINT('Ctrl Pts',(59.5,-21.98000002,-57.9611810443397));
#182528=CARTESIAN_POINT('Ctrl Pts',(59.4783898617073,-21.9800000201789,
-57.7727385086976));
#182529=CARTESIAN_POINT('Ctrl Pts',(59.4354406742177,-21.9800000198205,
-57.5879375289838));
#182530=CARTESIAN_POINT('Ctrl Pts',(59.4262406555719,-21.9800000197437,
-57.5483518567391));
#182531=CARTESIAN_POINT('Ctrl Pts',(59.4160613127747,-21.9800000196281,
-57.5089332628385));
#182532=CARTESIAN_POINT('Ctrl Pts',(59.4049049949538,-21.9800000194259,
-57.469681421663));
#182533=CARTESIAN_POINT('Ctrl Pts',(59.3987196130206,-21.9800000193138,
-57.4479190773891));
#182534=CARTESIAN_POINT('Ctrl Pts',(59.3922287663824,-21.9800000192153,
-57.4261931844644));
#182535=CARTESIAN_POINT('Ctrl Pts',(59.3854342581924,-21.9800000191476,
-57.4045116647966));
#182536=CARTESIAN_POINT('Ctrl Pts',(59.3665370601269,-21.9800000189591,
-57.3442100270521));
#182537=CARTESIAN_POINT('Ctrl Pts',(59.3452714576316,-21.9800000190536,
-57.284476265955));
#182538=CARTESIAN_POINT('Ctrl Pts',(59.3218795388586,-21.9800000193212,
-57.2258422130816));
#182539=CARTESIAN_POINT('Ctrl Pts',(59.3106878533866,-21.9800000194493,
-57.1977891968211));
#182540=CARTESIAN_POINT('Ctrl Pts',(59.2990101624397,-21.9800000196077,
-57.1699876439614));
#182541=CARTESIAN_POINT('Ctrl Pts',(59.2868766202345,-21.9800000197421,
-57.1424936459686));
#182542=CARTESIAN_POINT('Ctrl Pts',(59.2731919149499,-21.9800000198936,
-57.1114847902475));
#182543=CARTESIAN_POINT('Ctrl Pts',(59.2588942022727,-21.9800000199412,
-57.0807856309711));
#182544=CARTESIAN_POINT('Ctrl Pts',(59.2440132425671,-21.9800000199676,
-57.0504664636976));
#182545=CARTESIAN_POINT('Ctrl Pts',(59.2100364625766,-21.9800000200278,
-56.9812405739477));
#182546=CARTESIAN_POINT('Ctrl Pts',(59.1729132668609,-21.9800000200007,
-56.9136446874669));
#182547=CARTESIAN_POINT('Ctrl Pts',(59.1326772603373,-21.9800000199982,
-56.8478208127119));
#182548=CARTESIAN_POINT('Ctrl Pts',(59.1305108981501,-21.9800000199981,
-56.8442767643431));
#182549=CARTESIAN_POINT('Ctrl Pts',(59.1283355234418,-21.9800000199979,
-56.840737847095));
#182550=CARTESIAN_POINT('Ctrl Pts',(59.1261511452891,-21.9800000199978,
-56.8372040811614));
#182551=CARTESIAN_POINT('Ctrl Pts',(59.1024586951324,-21.980000019996,-56.7988757481558));
#182552=CARTESIAN_POINT('Ctrl Pts',(59.0776978833329,-21.9800000199944,
-56.7611395583364));
#182553=CARTESIAN_POINT('Ctrl Pts',(59.051864196737,-21.9800000199939,-56.7239980129522));
#182554=CARTESIAN_POINT('Ctrl Pts',(58.9794118018617,-21.9800000199925,
-56.6198319311016));
#182555=CARTESIAN_POINT('Ctrl Pts',(58.897983005211,-21.9800000199984,-56.5200000236488));
#182556=CARTESIAN_POINT('Ctrl Pts',(58.8106774361301,-21.9800000199995,
-56.4282264859168));
#182557=CARTESIAN_POINT('Ctrl Pts',(58.7700668687888,-21.9800000200001,
-56.385537623414));
#182558=CARTESIAN_POINT('Ctrl Pts',(58.7280754192644,-21.98000002,-56.3444004714051));
#182559=CARTESIAN_POINT('Ctrl Pts',(58.6847050658881,-21.98000002,-56.3048126520436));
#182560=CARTESIAN_POINT('Ctrl Pts',(58.6494885520049,-21.98000002,-56.2726675371986));
#182561=CARTESIAN_POINT('Ctrl Pts',(58.6132573779996,-21.98000002,-56.2414509676764));
#182562=CARTESIAN_POINT('Ctrl Pts',(58.5760924793011,-21.98000002,-56.2112492084261));
#182563=CARTESIAN_POINT('Ctrl Pts',(58.5607621926364,-21.98000002,-56.1987911729328));
#182564=CARTESIAN_POINT('Ctrl Pts',(58.5452724940628,-21.98000002,-56.1865050278662));
#182565=CARTESIAN_POINT('Ctrl Pts',(58.5296351858009,-21.98000002,-56.174399760192));
#182566=CARTESIAN_POINT('Ctrl Pts',(58.50318856599,-21.98000002,-56.1539267090422));
#182567=CARTESIAN_POINT('Ctrl Pts',(58.4762743935287,-21.98000002,-56.1339724230775));
#182568=CARTESIAN_POINT('Ctrl Pts',(58.4489601509993,-21.98000002,-56.1145700874369));
#182569=CARTESIAN_POINT('Ctrl Pts',(58.3958489442448,-21.98000002,-56.0768431961047));
#182570=CARTESIAN_POINT('Ctrl Pts',(58.3412467373532,-21.9800000154289,
-56.0410944834472));
#182571=CARTESIAN_POINT('Ctrl Pts',(58.2853645640813,-21.9799999916842,
-56.0075334770553));
#182572=CARTESIAN_POINT('Ctrl Pts',(58.2574234774454,-21.9799999798118,
-55.9907529738594));
#182573=CARTESIAN_POINT('Ctrl Pts',(58.2291619777336,-21.9799999666902,
-55.9745206253323));
#182574=CARTESIAN_POINT('Ctrl Pts',(58.2006099144576,-21.9799999607144,
-55.95885870079));
#182575=CARTESIAN_POINT('Ctrl Pts',(58.1720578511817,-21.9799999547386,
-55.9431967762476));
#182576=CARTESIAN_POINT('Ctrl Pts',(58.1432152243425,-21.9799999567774,
-55.9281052756887));
#182577=CARTESIAN_POINT('Ctrl Pts',(58.1141118834472,-21.9799999679397,
-55.9136064684357));
#182578=CARTESIAN_POINT('Origin',(-83.2809572255632,-21.9800000199999,-55.24995));
#182579=CARTESIAN_POINT('',(58.1141118834647,-21.98000002,-60.42825533736));
#182580=CARTESIAN_POINT('',(58.1141118834647,-21.98000002,-55.24995));
#182581=CARTESIAN_POINT('Origin',(55.9860799622262,-21.98000002,-60.2945890942193));
#182582=CARTESIAN_POINT('Ctrl Pts',(58.1141118834647,-21.98000002,-60.42825533736));
#182583=CARTESIAN_POINT('Ctrl Pts',(57.6893011240826,-21.98000002,-60.42825533736));
#182584=CARTESIAN_POINT('Ctrl Pts',(57.6206785412152,-22.3992316056509,
-60.42825533736));
#182585=CARTESIAN_POINT('Ctrl Pts',(58.1141118664761,-21.98000002,-60.6472062522327));
#182586=CARTESIAN_POINT('Ctrl Pts',(57.6893011111963,-21.9800000199989,
-60.5843987403017));
#182587=CARTESIAN_POINT('Ctrl Pts',(57.6206785407758,-22.3992316083349,
-60.574219492927));
#182588=CARTESIAN_POINT('Ctrl Pts',(58.0662048046675,-21.98000002,-60.8621882839625));
#182589=CARTESIAN_POINT('Ctrl Pts',(57.6525421683829,-21.98000002,-60.7382102053579));
#182590=CARTESIAN_POINT('Ctrl Pts',(57.5883338458808,-22.4017068994087,
-60.7175481239357));
#182591=CARTESIAN_POINT('Ctrl Pts',(57.9716987024741,-21.98000002,-61.0621827299711));
#182592=CARTESIAN_POINT('Ctrl Pts',(57.5817506954797,-21.98000002,-60.8779152752782));
#182593=CARTESIAN_POINT('Ctrl Pts',(57.5245249214072,-22.4066238608121,
-60.8508735991007));
#182594=CARTESIAN_POINT('',(57.6206785412152,-22.3992316056509,-60.42825533736));
#182595=CARTESIAN_POINT('Origin',(58.1141118834647,-22.48000002,-60.42825533736));
#182596=CARTESIAN_POINT('Origin',(56.1878807306156,-22.5096307883003,-60.3396608599486));
#182597=CARTESIAN_POINT('Origin',(0.,-12.9675000200281,-60.64995));
#182598=CARTESIAN_POINT('Origin',(0.,-12.9675000200281,-60.8508735991007));
#182599=CARTESIAN_POINT('Origin',(-83.2809572255632,-28.6300000199999,-55.24995));
#182600=CARTESIAN_POINT('',(56.9019881023868,-28.63000002,-60.42825533736));
#182601=CARTESIAN_POINT('Origin',(55.4600042524515,-28.6300004012302,-60.4518437845562));
#182602=CARTESIAN_POINT('',(56.9019881023868,-28.63000002,-55.74995));
#182603=CARTESIAN_POINT('',(56.9019881023868,-28.63000002,-55.24995));
#182604=CARTESIAN_POINT('',(-83.2809572255632,-28.6300000199999,-55.74995));
#182605=CARTESIAN_POINT('Ctrl Pts',(56.7267007677588,-28.6300000101017,
-61.1208879979441));
#182606=CARTESIAN_POINT('Ctrl Pts',(56.1708458184293,-28.6301256542592,
-60.8213741500007));
#182607=CARTESIAN_POINT('Ctrl Pts',(56.2981381510249,-28.0154717851087,
-60.8899762078857));
#182608=CARTESIAN_POINT('Ctrl Pts',(56.8517546922174,-28.6300000099381,
-60.8884604222472));
#182609=CARTESIAN_POINT('Ctrl Pts',(56.231166166104,-28.630129440528,-60.6796100628425));
#182610=CARTESIAN_POINT('Ctrl Pts',(56.3842107337159,-28.0053123694987,
-60.7350480688662));
#182611=CARTESIAN_POINT('Ctrl Pts',(56.9126898510831,-28.630000009859,-60.6288526395369));
#182612=CARTESIAN_POINT('Ctrl Pts',(56.2556311178187,-28.6301313253205,
-60.5386217481864));
#182613=CARTESIAN_POINT('Ctrl Pts',(56.4261416440025,-28.000404297649,-60.56196856935));
#182614=CARTESIAN_POINT('Ctrl Pts',(56.900577244494,-28.6300000098748,-60.3616165536491));
#182615=CARTESIAN_POINT('Ctrl Pts',(56.25064863923,-28.6301309522558,-60.3916281028846));
#182616=CARTESIAN_POINT('Ctrl Pts',(56.4178064988839,-28.0013806349218,
-60.3838347631882));
#182617=CARTESIAN_POINT('',(56.418846619879,-28.001258776103,-60.42825533736));
#182618=CARTESIAN_POINT('Origin',(55.0583726900799,-28.1617123603415,-60.3669939749617));
#182619=CARTESIAN_POINT('Origin',(56.9019881023868,-28.13000002,-60.42825533736));
#182620=CARTESIAN_POINT('Origin',(-83.2809572255632,-29.13000002,-55.74995));
#182621=CARTESIAN_POINT('',(56.6260651114328,-29.13000002,-55.24995));
#182622=CARTESIAN_POINT('Ctrl Pts',(56.9019881023868,-28.63000002,-55.74995));
#182623=CARTESIAN_POINT('Ctrl Pts',(56.9019881023868,-28.63000002,-55.7252977300075));
#182624=CARTESIAN_POINT('Ctrl Pts',(56.9009624215127,-28.6318266319377,
-55.7004051558798));
#182625=CARTESIAN_POINT('Ctrl Pts',(56.8989110597644,-28.6355653333565,
-55.6755568508274));
#182626=CARTESIAN_POINT('Ctrl Pts',(56.8968844354924,-28.6392589495835,
-55.6510081927576));
#182627=CARTESIAN_POINT('Ctrl Pts',(56.8938567186674,-28.6448191959989,
-55.6265031833395));
#182628=CARTESIAN_POINT('Ctrl Pts',(56.8898279092893,-28.6522850499302,
-55.6023410322127));
#182629=CARTESIAN_POINT('Ctrl Pts',(56.8858213427979,-28.6597096851966,
-55.5783122793039));
#182630=CARTESIAN_POINT('Ctrl Pts',(56.8808247072189,-28.6690193040358,
-55.5546231087945));
#182631=CARTESIAN_POINT('Ctrl Pts',(56.8748380025521,-28.6802034444929,
-55.5315855325101));
#182632=CARTESIAN_POINT('Ctrl Pts',(56.8688512978853,-28.6913875849501,
-55.5085479562256));
#182633=CARTESIAN_POINT('Ctrl Pts',(56.8618745241307,-28.7044465800051,
-55.4861625569417));
#182634=CARTESIAN_POINT('Ctrl Pts',(56.8539076812883,-28.71931576493,-55.4647510472712));
#182635=CARTESIAN_POINT('Ctrl Pts',(56.8485654122774,-28.7292864882659,
-55.4503932838693));
#182636=CARTESIAN_POINT('Ctrl Pts',(56.8427779541822,-28.7400700413755,
-55.436473634921));
#182637=CARTESIAN_POINT('Ctrl Pts',(56.8365453070028,-28.7516322157917,
-55.4230894720395));
#182638=CARTESIAN_POINT('Ctrl Pts',(56.8334289834131,-28.7574133029998,
-55.4163973905988));
#182639=CARTESIAN_POINT('Ctrl Pts',(56.8302013625523,-28.7633889371214,
-55.4098390835444));
#182640=CARTESIAN_POINT('Ctrl Pts',(56.8268624444205,-28.7695536079699,
-55.4034267193179));
#182641=CARTESIAN_POINT('Ctrl Pts',(56.8251929853546,-28.7726359433942,
-55.4002205372046));
#182642=CARTESIAN_POINT('Ctrl Pts',(56.8234957019709,-28.77576552988,-55.3970508341267));
#182643=CARTESIAN_POINT('Ctrl Pts',(56.8217705942694,-28.7789416179907,
-55.3939191047413));
#182644=CARTESIAN_POINT('Ctrl Pts',(56.8207703368452,-28.7807831874823,
-55.3921032554666));
#182645=CARTESIAN_POINT('Ctrl Pts',(56.8195504803749,-28.783019971304,-55.3899329326252));
#182646=CARTESIAN_POINT('Ctrl Pts',(56.8184767390232,-28.7849946292223,
-55.3880504554654));
#182647=CARTESIAN_POINT('Ctrl Pts',(56.8176986376089,-28.7864255921973,
-55.3866862925428));
#182648=CARTESIAN_POINT('Ctrl Pts',(56.8169972667262,-28.787717598042,-55.3854719748343));
#182649=CARTESIAN_POINT('Ctrl Pts',(56.8165117982118,-28.7886085997452,
-55.3846393128084));
#182650=CARTESIAN_POINT('Ctrl Pts',(56.8105283129488,-28.7995903532519,
-55.3743766061371));
#182651=CARTESIAN_POINT('Ctrl Pts',(56.8038505141232,-28.8116563698921,
-55.3640262829591));
#182652=CARTESIAN_POINT('Ctrl Pts',(56.7964784017351,-28.8249085696917,
-55.3538197096297));
#182653=CARTESIAN_POINT('Ctrl Pts',(56.789362571463,-28.8377000736109,-55.343967954848));
#182654=CARTESIAN_POINT('Ctrl Pts',(56.7815998623955,-28.8515974361167,
-55.3342503317759));
#182655=CARTESIAN_POINT('Ctrl Pts',(56.7731902745328,-28.8666658348978,
-55.3249145815269));
#182656=CARTESIAN_POINT('Ctrl Pts',(56.765061435188,-28.8812311851711,-55.3158904991135));
#182657=CARTESIAN_POINT('Ctrl Pts',(56.7563281873323,-28.8968913261992,
-55.3072235542836));
#182658=CARTESIAN_POINT('Ctrl Pts',(56.7469905309656,-28.9136701987031,
-55.2991713310086));
#182659=CARTESIAN_POINT('Ctrl Pts',(56.7380901202547,-28.929663382719,-55.2914961616225));
#182660=CARTESIAN_POINT('Ctrl Pts',(56.7286405798967,-28.9466733880094,
-55.2843799874074));
#182661=CARTESIAN_POINT('Ctrl Pts',(56.7186419098915,-28.96468138259,-55.2780710450498));
#182662=CARTESIAN_POINT('Ctrl Pts',(56.7088984654859,-28.9822297059132,
-55.2719231444702));
#182663=CARTESIAN_POINT('Ctrl Pts',(56.6986335677516,-29.0007261634318,
-55.266542291755));
#182664=CARTESIAN_POINT('Ctrl Pts',(56.6878472166885,-29.0201084881562,
-55.2621756144189));
#182665=CARTESIAN_POINT('Ctrl Pts',(56.67746927325,-29.0387569327062,-55.2579742742118));
#182666=CARTESIAN_POINT('Ctrl Pts',(56.6666086168719,-29.0582256425946,
-55.2547123448343));
#182667=CARTESIAN_POINT('Ctrl Pts',(56.6552652475542,-29.0784125612096,
-55.2526183861893));
#182668=CARTESIAN_POINT('Ctrl Pts',(56.6458634762107,-29.0951441678102,
-55.2508828418522));
#182669=CARTESIAN_POINT('Ctrl Pts',(56.6361300975035,-29.1123684482571,
-55.24995));
#182670=CARTESIAN_POINT('Ctrl Pts',(56.6260651114328,-29.13000002,-55.24995));
#182671=CARTESIAN_POINT('',(60.,-29.13000002,-55.24995));
#182672=CARTESIAN_POINT('Origin',(60.,28.41999998,-55.24995));
#182673=CARTESIAN_POINT('',(56.4809591809864,-29.63000002,-55.24995));
#182674=CARTESIAN_POINT('Origin',(0.,-12.9675000200281,-55.24995));
#182675=CARTESIAN_POINT('',(60.,-29.63000002,-55.24995));
#182676=CARTESIAN_POINT('Origin',(60.,-29.63000002,-55.74995));
#182677=CARTESIAN_POINT('',(56.1762739063771,-30.13000002,-55.74995));
#182678=CARTESIAN_POINT('Ctrl Pts',(56.4809591809864,-29.63000002,-55.24995));
#182679=CARTESIAN_POINT('Ctrl Pts',(56.4715391886809,-29.6459655172457,
-55.24995));
#182680=CARTESIAN_POINT('Ctrl Pts',(56.462662754235,-29.660958555519,-55.2507099202142));
#182681=CARTESIAN_POINT('Ctrl Pts',(56.454349949937,-29.6749641824274,-55.2519734860076));
#182682=CARTESIAN_POINT('Ctrl Pts',(56.4445637737142,-29.6914521843244,
-55.253461007797));
#182683=CARTESIAN_POINT('Ctrl Pts',(56.435554593509,-29.7065787354348,-55.2556468104043));
#182684=CARTESIAN_POINT('Ctrl Pts',(56.4273466888451,-29.7203275029284,
-55.2581719078906));
#182685=CARTESIAN_POINT('Ctrl Pts',(56.422431254882,-29.7285611705276,-55.2596841025922));
#182686=CARTESIAN_POINT('Ctrl Pts',(56.4178030918222,-29.7363007600898,
-55.2613190749055));
#182687=CARTESIAN_POINT('Ctrl Pts',(56.4134686415036,-29.7435398696061,
-55.2630072596282));
#182688=CARTESIAN_POINT('Ctrl Pts',(56.4084051403986,-29.7519965910681,
-55.2649793955578));
#182689=CARTESIAN_POINT('Ctrl Pts',(56.4037382707669,-29.7597773623134,
-55.267025073771));
#182690=CARTESIAN_POINT('Ctrl Pts',(56.3994596075599,-29.7669020737305,
-55.2690538840585));
#182691=CARTESIAN_POINT('Ctrl Pts',(56.395622622375,-29.7732913151433,-55.2708732642339));
#182692=CARTESIAN_POINT('Ctrl Pts',(56.3920987368373,-29.7791514240126,
-55.2726789076247));
#182693=CARTESIAN_POINT('Ctrl Pts',(56.3888834537717,-29.7844933511438,
-55.2744148706152));
#182694=CARTESIAN_POINT('Ctrl Pts',(56.3856587578915,-29.7898509168888,
-55.2761559156769));
#182695=CARTESIAN_POINT('Ctrl Pts',(56.3827332174854,-29.7946845005768,
-55.2778259230685));
#182696=CARTESIAN_POINT('Ctrl Pts',(56.3801058680076,-29.7990071903381,
-55.2793787374307));
#182697=CARTESIAN_POINT('Ctrl Pts',(56.3787921932687,-29.8011685352187,
-55.2801551446118));
#182698=CARTESIAN_POINT('Ctrl Pts',(56.3775562038427,-29.8032029432388,
-55.2809026966681));
#182699=CARTESIAN_POINT('Ctrl Pts',(56.3763978997437,-29.8051120362293,
-55.2816166210347));
#182700=CARTESIAN_POINT('Ctrl Pts',(56.3758187476942,-29.8060665827245,
-55.2819735832181));
#182701=CARTESIAN_POINT('Ctrl Pts',(56.3752590169764,-29.8069897973416,
-55.2823221473967));
#182702=CARTESIAN_POINT('Ctrl Pts',(56.3747187075913,-29.807881865021,-55.282661770634));
#182703=CARTESIAN_POINT('Ctrl Pts',(56.3744485528987,-29.8083278988607,
-55.2828315822527));
#182704=CARTESIAN_POINT('Ctrl Pts',(56.3743666403179,-29.8084621276635,
-55.2828830019629));
#182705=CARTESIAN_POINT('Ctrl Pts',(56.3741978897377,-29.8087407981391,
-55.2829896821112));
#182706=CARTESIAN_POINT('Ctrl Pts',(56.3740291391576,-29.8090194686147,
-55.2830963622595));
#182707=CARTESIAN_POINT('Ctrl Pts',(56.37377355065,-29.8094427998715,-55.2832577411222));
#182708=CARTESIAN_POINT('Ctrl Pts',(56.3731560434326,-29.8104648021674,
-55.2836533109053));
#182709=CARTESIAN_POINT('Ctrl Pts',(56.3716295461241,-29.8129912240618,
-55.2846311718795));
#182710=CARTESIAN_POINT('Ctrl Pts',(56.3701127933845,-29.8155010721099,
-55.285626187063));
#182711=CARTESIAN_POINT('Ctrl Pts',(56.3686057879999,-29.817994256596,-55.2866378253316));
#182712=CARTESIAN_POINT('Ctrl Pts',(56.3569538600269,-29.8372711658571,
-55.2944596528853));
#182713=CARTESIAN_POINT('Ctrl Pts',(56.3459518915256,-29.8554415567586,
-55.3032348643387));
#182714=CARTESIAN_POINT('Ctrl Pts',(56.3355845836553,-29.8725024376886,
-55.3126982643438));
#182715=CARTESIAN_POINT('Ctrl Pts',(56.3299355776219,-29.8817986812761,
-55.3178547431901));
#182716=CARTESIAN_POINT('Ctrl Pts',(56.3244746239002,-29.890766138149,-55.3232161626166));
#182717=CARTESIAN_POINT('Ctrl Pts',(56.3191967850647,-29.8994084321092,
-55.3287439230168));
#182718=CARTESIAN_POINT('Ctrl Pts',(56.311088424142,-29.9126856163533,-55.3372362392501));
#182719=CARTESIAN_POINT('Ctrl Pts',(56.3034308285875,-29.9251885096071,
-55.3461168072432));
#182720=CARTESIAN_POINT('Ctrl Pts',(56.2962223827156,-29.9369337314948,
-55.3552490742658));
#182721=CARTESIAN_POINT('Ctrl Pts',(56.2908160483117,-29.9457426479105,
-55.3620982745327));
#182722=CARTESIAN_POINT('Ctrl Pts',(56.2856621173763,-29.9541257111972,
-55.3690893077384));
#182723=CARTESIAN_POINT('Ctrl Pts',(56.2807554399466,-29.9620950592301,
-55.3761691040139));
#182724=CARTESIAN_POINT('Ctrl Pts',(56.2797154356931,-29.963784217723,-55.3776697158528));
#182725=CARTESIAN_POINT('Ctrl Pts',(56.2788888440829,-29.9651263359666,
-55.3788776896832));
#182726=CARTESIAN_POINT('Ctrl Pts',(56.2778887710329,-29.96674961639,-55.3803565877314));
#182727=CARTESIAN_POINT('Ctrl Pts',(56.2773160826108,-29.9676791823895,
-55.3812034736561));
#182728=CARTESIAN_POINT('Ctrl Pts',(56.276686724301,-29.9687005704798,-55.3821396856299));
#182729=CARTESIAN_POINT('Ctrl Pts',(56.2759307274251,-29.9699271388893,
-55.3832767047358));
#182730=CARTESIAN_POINT('Ctrl Pts',(56.273906754129,-29.9732109377857,-55.3863207600499));
#182731=CARTESIAN_POINT('Ctrl Pts',(56.2719114898357,-29.9764461032282,
-55.3894018338609));
#182732=CARTESIAN_POINT('Ctrl Pts',(56.2699450791873,-29.9796325533428,
-55.3925187595796));
#182733=CARTESIAN_POINT('Ctrl Pts',(56.2599035103954,-29.995904311256,-55.4084354878831));
#182734=CARTESIAN_POINT('Ctrl Pts',(56.2506758252138,-30.010814772085,-55.4252755403774));
#182735=CARTESIAN_POINT('Ctrl Pts',(56.2422529089667,-30.0243957048183,
-55.4428177801253));
#182736=CARTESIAN_POINT('Ctrl Pts',(56.2333441945075,-30.0387599283557,
-55.4613717821245));
#182737=CARTESIAN_POINT('Ctrl Pts',(56.2253354486514,-30.0516372998195,
-55.4807116725759));
#182738=CARTESIAN_POINT('Ctrl Pts',(56.2182201680098,-30.0630550384973,
-55.5006334806367));
#182739=CARTESIAN_POINT('Ctrl Pts',(56.2149590325741,-30.068288112788,-55.5097642117323));
#182740=CARTESIAN_POINT('Ctrl Pts',(56.2118856697234,-30.0732143865641,
-55.5190179172689));
#182741=CARTESIAN_POINT('Ctrl Pts',(56.2090000040314,-30.0778354020999,
-55.5283783295249));
#182742=CARTESIAN_POINT('Ctrl Pts',(56.2022281272477,-30.0886796755407,
-55.5503446850238));
#182743=CARTESIAN_POINT('Ctrl Pts',(56.1964989578389,-30.097829016622,-55.5728762690722));
#182744=CARTESIAN_POINT('Ctrl Pts',(56.1918296761308,-30.1052731127711,
-55.5956766399725));
#182745=CARTESIAN_POINT('Ctrl Pts',(56.1889265498164,-30.1099014802093,
-55.6098527725933));
#182746=CARTESIAN_POINT('Ctrl Pts',(56.1864326699304,-30.1138713642342,
-55.624133303115));
#182747=CARTESIAN_POINT('Ctrl Pts',(56.1843473599668,-30.117187484339,-55.6384523996636));
#182748=CARTESIAN_POINT('Ctrl Pts',(56.1813648251625,-30.1219303972874,
-55.6589324264064));
#182749=CARTESIAN_POINT('Ctrl Pts',(56.1792205673271,-30.1253320589938,
-55.6794841526094));
#182750=CARTESIAN_POINT('Ctrl Pts',(56.1778972989043,-30.1274293092601,
-55.6998970462423));
#182751=CARTESIAN_POINT('Ctrl Pts',(56.1768073239574,-30.1291568123186,
-55.7167111273986));
#182752=CARTESIAN_POINT('Ctrl Pts',(56.1762739063772,-30.1300000200003,
-55.7334312082419));
#182753=CARTESIAN_POINT('Ctrl Pts',(56.1762739063772,-30.1300000200003,
-55.74995));
#182754=CARTESIAN_POINT('',(-83.2809572255632,-30.13000002,-55.74995));
#182755=CARTESIAN_POINT('Origin',(-83.2809572255632,-30.13000002,-55.24995));
#182756=CARTESIAN_POINT('',(56.1762739063772,-30.13000002,-60.42825533736));
#182757=CARTESIAN_POINT('',(56.1762739063772,-30.13000002,-55.24995));
#182758=CARTESIAN_POINT('Origin',(54.6965997032562,-30.1299997573523,-60.4472632078221));
#182759=CARTESIAN_POINT('Ctrl Pts',(56.174853661752,-30.1300000267474,-60.3623460050376));
#182760=CARTESIAN_POINT('Ctrl Pts',(55.8081167820838,-30.1299397177969,
-60.3792327034747));
#182761=CARTESIAN_POINT('Ctrl Pts',(55.6982488612463,-30.4801711525811,
-60.3843213671005));
#182762=CARTESIAN_POINT('Ctrl Pts',(56.1868831687146,-30.1300000267259,
-60.6263466339185));
#182763=CARTESIAN_POINT('Ctrl Pts',(55.8181378939596,-30.1299399603517,
-60.5754394884542));
#182764=CARTESIAN_POINT('Ctrl Pts',(55.7066195808876,-30.47905606799,-60.5602959714918));
#182765=CARTESIAN_POINT('Ctrl Pts',(56.1265462537083,-30.1300000268336,
-60.886588202509));
#182766=CARTESIAN_POINT('Ctrl Pts',(55.7674480546492,-30.1299387371113,
-60.7710090719053));
#182767=CARTESIAN_POINT('Ctrl Pts',(55.6646352974887,-30.4846448609915,
-60.733808800051));
#182768=CARTESIAN_POINT('Ctrl Pts',(55.9983862620518,-30.1300000270643,
-61.1214514057001));
#182769=CARTESIAN_POINT('Ctrl Pts',(55.6644710959106,-30.1299360711904,
-60.9390296786082));
#182770=CARTESIAN_POINT('Ctrl Pts',(55.5754321736229,-30.4966175475299,
-60.8903552940655));
#182771=CARTESIAN_POINT('',(55.6992942935022,-30.4800318603739,-60.42825533736));
#182772=CARTESIAN_POINT('Origin',(56.1762739063772,-30.63000002,-60.42825533736));
#182773=CARTESIAN_POINT('Origin',(54.3783008183434,-30.6572029381318,-60.3807755792598));
#182774=CARTESIAN_POINT('Origin',(0.,-12.9675000200281,-60.64995));
#182775=CARTESIAN_POINT('Origin',(0.,-12.9675000200281,-60.8508735991007));
#182776=CARTESIAN_POINT('Ctrl Pts',(53.903079465118,-36.78000002,-61.1007217352389));
#182777=CARTESIAN_POINT('Ctrl Pts',(53.2672382848488,-36.7800000200009,
-60.7532634257798));
#182778=CARTESIAN_POINT('Ctrl Pts',(53.4928740664966,-36.1025529613072,
-60.8765730017782));
#182779=CARTESIAN_POINT('Ctrl Pts',(54.0233453777872,-36.78000002,-60.8807385305411));
#182780=CARTESIAN_POINT('Ctrl Pts',(53.3073297453563,-36.7800000199946,
-60.6286940607591));
#182781=CARTESIAN_POINT('Ctrl Pts',(53.5792270344601,-36.0882821494794,
-60.7299113961242));
#182782=CARTESIAN_POINT('Ctrl Pts',(54.0836727915734,-36.78000002,-60.6340939082454));
#182783=CARTESIAN_POINT('Ctrl Pts',(53.3177002646766,-36.7800000200061,
-60.5197710189114));
#182784=CARTESIAN_POINT('Ctrl Pts',(53.6225015011258,-36.0811780755465,
-60.565486568279));
#182785=CARTESIAN_POINT('Ctrl Pts',(54.0757885469763,-36.78000002,-60.3849343801088));
#182786=CARTESIAN_POINT('Ctrl Pts',(53.3162520055491,-36.7800000199989,
-60.4089987140158));
#182787=CARTESIAN_POINT('Ctrl Pts',(53.6168456207784,-36.0821069256242,
-60.3993736717233));
#182788=CARTESIAN_POINT('',(53.6173229282256,-36.0820590308261,-60.42825533736));
#182789=CARTESIAN_POINT('',(54.076473627675,-36.78000002,-60.42825533736));
#182790=CARTESIAN_POINT('Origin',(54.076473627675,-36.28000002,-60.42825533736));
#182791=CARTESIAN_POINT('Origin',(52.6143300188006,-36.78000002,-60.4624709867154));
#182792=CARTESIAN_POINT('Ctrl Pts',(53.6173229282257,-36.0820590308261,
-60.42825533736));
#182793=CARTESIAN_POINT('Ctrl Pts',(53.6173229282257,-36.0820590308261,
-60.4718732914667));
#182794=CARTESIAN_POINT('Ctrl Pts',(53.6139639100269,-36.0826317730148,
-60.5156743630418));
#182795=CARTESIAN_POINT('Ctrl Pts',(53.6072032158688,-36.0837570727629,
-60.5592767125907));
#182796=CARTESIAN_POINT('Ctrl Pts',(53.6004830965447,-36.0848756189367,
-60.6026173792329));
#182797=CARTESIAN_POINT('Ctrl Pts',(53.5904018582716,-36.0865400407211,
-60.6457612486292));
#182798=CARTESIAN_POINT('Ctrl Pts',(53.5769646226219,-36.0887472436547,
-60.6883213233074));
#182799=CARTESIAN_POINT('Ctrl Pts',(53.5636388975191,-36.0909361298442,
-60.7305282079898));
#182800=CARTESIAN_POINT('Ctrl Pts',(53.5470125747611,-36.0936587800579,
-60.7721604735197));
#182801=CARTESIAN_POINT('Ctrl Pts',(53.5271386403121,-36.0969295254175,
-60.8128357523528));
#182802=CARTESIAN_POINT('Ctrl Pts',(53.5208954705939,-36.0979569927486,
-60.8256134270373));
#182803=CARTESIAN_POINT('Ctrl Pts',(53.5143321784749,-36.0990386798933,
-60.8382966552944));
#182804=CARTESIAN_POINT('Ctrl Pts',(53.5074514076768,-36.1001753985996,
-60.8508735991007));
#182805=CARTESIAN_POINT('Origin',(-83.2809572255632,-36.78000002,-55.24995));
#182806=CARTESIAN_POINT('',(54.076473627675,-36.78000002,-55.74995));
#182807=CARTESIAN_POINT('',(54.076473627675,-36.78000002,-55.24995));
#182808=CARTESIAN_POINT('',(-83.2809572255632,-36.78000002,-55.74995));
#182809=CARTESIAN_POINT('Origin',(-83.2809572255632,-37.28000002,-55.74995));
#182810=CARTESIAN_POINT('',(53.7823432375799,-37.1153847305994,-55.2778252214768));
#182811=CARTESIAN_POINT('Ctrl Pts',(54.076473627675,-36.78000002,-55.74995));
#182812=CARTESIAN_POINT('Ctrl Pts',(54.0764736237006,-36.78000002,-55.7254348582675));
#182813=CARTESIAN_POINT('Ctrl Pts',(54.0748711940854,-36.7818350468828,
-55.7007325233529));
#182814=CARTESIAN_POINT('Ctrl Pts',(54.0716496717766,-36.7855406125626,
-55.6761136367726));
#182815=CARTESIAN_POINT('Ctrl Pts',(54.068323113487,-36.7893669961938,-55.6506920647993));
#182816=CARTESIAN_POINT('Ctrl Pts',(54.0632701595081,-36.7951876895575,
-55.6253595447221));
#182817=CARTESIAN_POINT('Ctrl Pts',(54.0565037344636,-36.8030047692021,
-55.6004402933233));
#182818=CARTESIAN_POINT('Ctrl Pts',(54.0554730514243,-36.8041954912383,
-55.5966445149615));
#182819=CARTESIAN_POINT('Ctrl Pts',(54.0544026690462,-36.8054324694357,
-55.592858372319));
#182820=CARTESIAN_POINT('Ctrl Pts',(54.0532926938187,-36.806715643047,-55.5890830610468));
#182821=CARTESIAN_POINT('Ctrl Pts',(54.045565771698,-36.815648259124,-55.5628018112867));
#182822=CARTESIAN_POINT('Ctrl Pts',(54.0359072128158,-36.8268241578973,
-55.5370354066851));
#182823=CARTESIAN_POINT('Ctrl Pts',(54.0243169062867,-36.8402147976036,
-55.5121923007281));
#182824=CARTESIAN_POINT('Ctrl Pts',(54.0185217530221,-36.8469101174568,
-55.4997707477495));
#182825=CARTESIAN_POINT('Ctrl Pts',(54.0122436577221,-36.8541587109129,
-55.4875806630813));
#182826=CARTESIAN_POINT('Ctrl Pts',(54.0054826167242,-36.861953334192,-55.4756781686146));
#182827=CARTESIAN_POINT('Ctrl Pts',(54.0021020962253,-36.8658506458316,
-55.4697269213813));
#182828=CARTESIAN_POINT('Ctrl Pts',(53.9986008398608,-36.8698844412374,
-55.4638475980883));
#182829=CARTESIAN_POINT('Ctrl Pts',(53.9949788498558,-36.8740534181339,
-55.4580476645523));
#182830=CARTESIAN_POINT('Ctrl Pts',(53.9942871097817,-36.8748496236407,
-55.4569399733525));
#182831=CARTESIAN_POINT('Ctrl Pts',(53.9935547350079,-36.8756923521775,
-55.4557774965243));
#182832=CARTESIAN_POINT('Ctrl Pts',(53.9928014458625,-36.8765589029471,
-55.4545938334076));
#182833=CARTESIAN_POINT('Ctrl Pts',(53.9909351836162,-36.8787057691218,
-55.4516613262808));
#182834=CARTESIAN_POINT('Ctrl Pts',(53.9889418285035,-36.880997110987,-55.4486056977901));
#182835=CARTESIAN_POINT('Ctrl Pts',(53.9871466296489,-36.8830591828349,
-55.4459130461622));
#182836=CARTESIAN_POINT('Ctrl Pts',(53.9858723589523,-36.8845228857128,
-55.4440017442156));
#182837=CARTESIAN_POINT('Ctrl Pts',(53.9846988573795,-36.8858700336466,
-55.4422722514467));
#182838=CARTESIAN_POINT('Ctrl Pts',(53.9837506400808,-36.8869578372551,
-55.4408885206699));
#182839=CARTESIAN_POINT('Ctrl Pts',(53.9735107226483,-36.8987051647392,
-55.4259454386124));
#182840=CARTESIAN_POINT('Ctrl Pts',(53.9621990035396,-36.9116599662525,
-55.4112184958409));
#182841=CARTESIAN_POINT('Ctrl Pts',(53.9497544034244,-36.9258791059603,
-55.3969517565364));
#182842=CARTESIAN_POINT('Ctrl Pts',(53.9378712005585,-36.9394567958953,
-55.3833286143042));
#182843=CARTESIAN_POINT('Ctrl Pts',(53.9249549238256,-36.9541874350935,
-55.3701252127202));
#182844=CARTESIAN_POINT('Ctrl Pts',(53.9109800116058,-36.9700858487164,
-55.3575709377622));
#182845=CARTESIAN_POINT('Ctrl Pts',(53.8972917642908,-36.98565814099,-55.3452741864279));
#182846=CARTESIAN_POINT('Ctrl Pts',(53.8825877148145,-37.0023509706149,
-55.3336002534511));
#182847=CARTESIAN_POINT('Ctrl Pts',(53.8668729413441,-37.0201419084753,
-55.322780146583));
#182848=CARTESIAN_POINT('Ctrl Pts',(53.8515575866294,-37.0374806581908,
-55.3122350518637));
#182849=CARTESIAN_POINT('Ctrl Pts',(53.8352821576126,-37.0558624917925,
-55.3025009940998));
#182850=CARTESIAN_POINT('Ctrl Pts',(53.818080891982,-37.0752298715344,-55.2938058043885));
#182851=CARTESIAN_POINT('Ctrl Pts',(53.8065758593464,-37.0881837053268,
-55.2879900438771));
#182852=CARTESIAN_POINT('Ctrl Pts',(53.7946572537875,-37.1015776749406,
-55.2826393142049));
#182853=CARTESIAN_POINT('Ctrl Pts',(53.7823432375799,-37.1153847305994,
-55.2778252214768));
#182854=CARTESIAN_POINT('',(53.65082011387,-37.28000002,-55.24995));
#182855=CARTESIAN_POINT('Ctrl Pts',(53.7823432375799,-37.1153847305994,
-55.2778252214768));
#182856=CARTESIAN_POINT('Ctrl Pts',(53.7292323645857,-37.1749351436578,
-55.2570618366145));
#182857=CARTESIAN_POINT('Ctrl Pts',(53.6853913233491,-37.2312368757479,
-55.24995));
#182858=CARTESIAN_POINT('Ctrl Pts',(53.65082011387,-37.28000002,-55.24995));
#182859=CARTESIAN_POINT('',(60.,-37.28000002,-55.24995));
#182860=CARTESIAN_POINT('Origin',(60.,28.41999998,-55.24995));
#182861=CARTESIAN_POINT('',(53.5055391860638,-37.78000002,-55.24995));
#182862=CARTESIAN_POINT('Origin',(57.8922230010149,-38.7834964612722,-55.24995));
#182863=CARTESIAN_POINT('',(60.,-37.78000002,-55.24995));
#182864=CARTESIAN_POINT('Origin',(60.,-37.78000002,-55.74995));
#182865=CARTESIAN_POINT('',(53.4093468596018,-38.0856478194539,-55.3542488214713));
#182866=CARTESIAN_POINT('Ctrl Pts',(53.5055391860638,-37.78000002,-55.24995));
#182867=CARTESIAN_POINT('Ctrl Pts',(53.4934324707211,-37.806461664537,-55.24995));
#182868=CARTESIAN_POINT('Ctrl Pts',(53.4823161171381,-37.8331687413443,
-55.2520788136903));
#182869=CARTESIAN_POINT('Ctrl Pts',(53.4722294340858,-37.8597633672056,
-55.2563959926891));
#182870=CARTESIAN_POINT('Ctrl Pts',(53.4622707511287,-37.8860205070348,
-55.2606583866491));
#182871=CARTESIAN_POINT('Ctrl Pts',(53.4533156112428,-37.9121671500672,
-55.2670537868195));
#182872=CARTESIAN_POINT('Ctrl Pts',(53.44537582615,-37.9378357595513,-55.2755941342185));
#182873=CARTESIAN_POINT('Ctrl Pts',(53.4372230919462,-37.9641928143152,
-55.2843635381178));
#182874=CARTESIAN_POINT('Ctrl Pts',(53.4301408735503,-37.9900449202448,
-55.2953945620593));
#182875=CARTESIAN_POINT('Ctrl Pts',(53.4241155832649,-38.0149832204437,
-55.3086523082856));
#182876=CARTESIAN_POINT('Ctrl Pts',(53.4181787909317,-38.0395552331459,
-55.3217153280615));
#182877=CARTESIAN_POINT('Ctrl Pts',(53.41326787339,-38.063239083628,-55.336939849031));
#182878=CARTESIAN_POINT('Ctrl Pts',(53.4093468596018,-38.0856478194539,
-55.3542488214713));
#182879=CARTESIAN_POINT('Origin',(53.4522739634651,-37.8403182980825,-55.7203377623201));
#182880=CARTESIAN_POINT('Origin',(-83.2809572255632,11.6199999800001,-55.74995));
#182881=CARTESIAN_POINT('',(53.4093468596018,12.0381477794281,-55.475810586866));
#182882=CARTESIAN_POINT('Origin',(53.4672824165089,11.7070445566108,-55.7239619428824));
#182883=CARTESIAN_POINT('',(53.5631588418786,11.61999998,-55.24995));
#182884=CARTESIAN_POINT('Ctrl Pts',(53.4093468596018,12.0381477794281,-55.475810586866));
#182885=CARTESIAN_POINT('Ctrl Pts',(53.411271555201,12.0271480752568,-55.4590326196229));
#182886=CARTESIAN_POINT('Ctrl Pts',(53.4135176755445,12.0153190624728,-55.4432762206355));
#182887=CARTESIAN_POINT('Ctrl Pts',(53.416096779611,12.0028976523553,-55.4285379015408));
#182888=CARTESIAN_POINT('Ctrl Pts',(53.4188144250206,11.9898090032297,-55.413007886389));
#182889=CARTESIAN_POINT('Ctrl Pts',(53.4219016576878,11.976062431537,-55.3986080182298));
#182890=CARTESIAN_POINT('Ctrl Pts',(53.4253639809393,11.9618801590715,-55.3853184129368));
#182891=CARTESIAN_POINT('Ctrl Pts',(53.4263179288633,11.9579726240456,-55.3816568277932));
#182892=CARTESIAN_POINT('Ctrl Pts',(53.4273003127235,11.954031716205,-55.3780794498407));
#182893=CARTESIAN_POINT('Ctrl Pts',(53.428311168957,11.950061432097,-55.3745857064195));
#182894=CARTESIAN_POINT('Ctrl Pts',(53.431076440011,11.9392004299527,-55.3650283161277));
#182895=CARTESIAN_POINT('Ctrl Pts',(53.434029674615,11.928216282372,-55.3561764344811));
#182896=CARTESIAN_POINT('Ctrl Pts',(53.4371890974518,11.9170932442165,-55.3479256972112));
#182897=CARTESIAN_POINT('Ctrl Pts',(53.4403923945095,11.905815742838,-55.3395603837388));
#182898=CARTESIAN_POINT('Ctrl Pts',(53.4438074174171,11.8943947184568,-55.3318125871665));
#182899=CARTESIAN_POINT('Ctrl Pts',(53.4474716139716,11.8827770512412,-55.3246073283533));
#182900=CARTESIAN_POINT('Ctrl Pts',(53.450288870995,11.8738446825559,-55.3190674874371));
#182901=CARTESIAN_POINT('Ctrl Pts',(53.4532537656305,11.8647952569811,-55.3138489850583));
#182902=CARTESIAN_POINT('Ctrl Pts',(53.4563919355982,11.8555940534045,-55.3089336366617));
#182903=CARTESIAN_POINT('Ctrl Pts',(53.4570281012091,11.8537287977445,-55.307937203821));
#182904=CARTESIAN_POINT('Ctrl Pts',(53.4576720413956,11.8518563454007,-55.3069526932524));
#182905=CARTESIAN_POINT('Ctrl Pts',(53.4583239030131,11.8499764038232,-55.3059799159839));
#182906=CARTESIAN_POINT('Ctrl Pts',(53.4661611528671,11.8273741037968,-55.2942843378106));
#182907=CARTESIAN_POINT('Ctrl Pts',(53.4751104310767,11.8038199874285,-55.2843487566791));
#182908=CARTESIAN_POINT('Ctrl Pts',(53.4851501145903,11.7795869692876,-55.2762231679919));
#182909=CARTESIAN_POINT('Ctrl Pts',(53.4949709984344,11.75588207301,-55.2682746641818));
#182910=CARTESIAN_POINT('Ctrl Pts',(53.5058355767072,11.7315262142338,-55.2620580158118));
#182911=CARTESIAN_POINT('Ctrl Pts',(53.5177437847908,11.7067803310973,-55.2576643682367));
#182912=CARTESIAN_POINT('Ctrl Pts',(53.5289856773389,11.6834190867124,-55.2535165641685));
#182913=CARTESIAN_POINT('Ctrl Pts',(53.5411579876986,11.6597092930614,-55.2509935902076));
#182914=CARTESIAN_POINT('Ctrl Pts',(53.5542743627635,11.6358913899761,-55.2502114786518));
#182915=CARTESIAN_POINT('Ctrl Pts',(53.5571891134863,11.6305985213373,-55.2500376760416));
#182916=CARTESIAN_POINT('Ctrl Pts',(53.5601505311349,11.6253004309346,-55.24995));
#182917=CARTESIAN_POINT('Ctrl Pts',(53.5631588418786,11.61999998,-55.24995));
#182918=CARTESIAN_POINT('',(60.,11.61999998,-55.24995));
#182919=CARTESIAN_POINT('Origin',(60.,28.41999998,-55.24995));
#182920=CARTESIAN_POINT('',(53.7374305810854,11.11999998,-55.24995));
#182921=CARTESIAN_POINT('Origin',(57.8922230010151,12.8484964212155,-55.24995));
#182922=CARTESIAN_POINT('',(60.,11.11999998,-55.24995));
#182923=CARTESIAN_POINT('Origin',(60.,11.11999998,-55.74995));
#182924=CARTESIAN_POINT('',(53.7823432375846,11.067884690566,-55.2526734204115));
#182925=CARTESIAN_POINT('Ctrl Pts',(53.7374305810854,11.11999998,-55.24995));
#182926=CARTESIAN_POINT('Ctrl Pts',(53.7521098206901,11.1023577124241,-55.24995));
#182927=CARTESIAN_POINT('Ctrl Pts',(53.7671137595184,11.084960698582,-55.2508838306004));
#182928=CARTESIAN_POINT('Ctrl Pts',(53.7823432375846,11.067884690566,-55.2526734204115));
#182929=CARTESIAN_POINT('Ctrl Pts',(53.7823432375846,11.067884690566,-55.2526734204115));
#182930=CARTESIAN_POINT('Ctrl Pts',(53.8011235246843,11.0468273478585,-55.2548802597339));
#182931=CARTESIAN_POINT('Ctrl Pts',(53.8191049193374,11.02648059754,-55.2583653100953));
#182932=CARTESIAN_POINT('Ctrl Pts',(53.8362874215441,11.0069647460792,-55.2628945248306));
#182933=CARTESIAN_POINT('Ctrl Pts',(53.8541929651849,10.9866276656112,-55.267614329381));
#182934=CARTESIAN_POINT('Ctrl Pts',(53.8712309668023,10.9671927270046,-55.27346732726));
#182935=CARTESIAN_POINT('Ctrl Pts',(53.8874014263962,10.9487392110445,-55.280195011717));
#182936=CARTESIAN_POINT('Ctrl Pts',(53.9039667551484,10.9298350755907,-55.2870869806263));
#182937=CARTESIAN_POINT('Ctrl Pts',(53.9196216552579,10.9119604190137,-55.2948962748775));
#182938=CARTESIAN_POINT('Ctrl Pts',(53.9343661267246,10.8951470539327,-55.3033616418457));
#182939=CARTESIAN_POINT('Ctrl Pts',(53.9496905615744,10.877672346998,-55.3121599880513));
#182940=CARTESIAN_POINT('Ctrl Pts',(53.9640315370416,10.8613435812081,-55.3216664686702));
#182941=CARTESIAN_POINT('Ctrl Pts',(53.9773890531262,10.8461466461998,-55.3316147856485));
#182942=CARTESIAN_POINT('Ctrl Pts',(53.9837559739738,10.8389029579489,-55.3363566962228));
#182943=CARTESIAN_POINT('Ctrl Pts',(53.9898994532802,10.8319157554432,-55.3411994334459));
#182944=CARTESIAN_POINT('Ctrl Pts',(53.9958194910456,10.825180276009,-55.3461166901571));
#182945=CARTESIAN_POINT('Ctrl Pts',(54.00467766823,10.8151019500565,-55.3534744018704));
#182946=CARTESIAN_POINT('Ctrl Pts',(54.0130355763021,10.8055875154472,-55.3609985450547));
#182947=CARTESIAN_POINT('Ctrl Pts',(54.0208932152617,10.7966139956126,-55.3686082830298));
#182948=CARTESIAN_POINT('Ctrl Pts',(54.0248220347416,10.7921272356953,-55.3724131520174));
#182949=CARTESIAN_POINT('Ctrl Pts',(54.0286257869433,10.787775720653,-55.3762394382259));
#182950=CARTESIAN_POINT('Ctrl Pts',(54.0323044718669,10.7835557757841,-55.3800779985596));
#182951=CARTESIAN_POINT('Ctrl Pts',(54.0341438143287,10.7814458033496,-55.3819972787265));
#182952=CARTESIAN_POINT('Ctrl Pts',(54.035951889971,10.7793687254093,-55.3839196297065));
#182953=CARTESIAN_POINT('Ctrl Pts',(54.0377286987937,10.7773240721282,-55.3858439410498));
#182954=CARTESIAN_POINT('Ctrl Pts',(54.0388203296637,10.7760678837239,-55.3870261941086));
#182955=CARTESIAN_POINT('Ctrl Pts',(54.039525317404,10.7752615357712,-55.3877925642775));
#182956=CARTESIAN_POINT('Ctrl Pts',(54.040534543656,10.7740965012651,-55.3889087511113));
#182957=CARTESIAN_POINT('Ctrl Pts',(54.0411679991548,10.7733652504551,-55.3896093419712));
#182958=CARTESIAN_POINT('Ctrl Pts',(54.0419213132897,10.7724929242244,-55.3904480137501));
#182959=CARTESIAN_POINT('Ctrl Pts',(54.0429653248035,10.7712869097631,-55.3916216664204));
#182960=CARTESIAN_POINT('Ctrl Pts',(54.0588511417924,10.752936034543,-55.4094801203573));
#182961=CARTESIAN_POINT('Ctrl Pts',(54.0732805056091,10.7361175475333,-55.4285968746425));
#182962=CARTESIAN_POINT('Ctrl Pts',(54.0862534162535,10.7209515952271,-55.44868535453));
#182963=CARTESIAN_POINT('Ctrl Pts',(54.0993947773437,10.7055887163023,-55.4690346789947));
#182964=CARTESIAN_POINT('Ctrl Pts',(54.1110416162365,10.6919214842835,-55.4903805240241));
#182965=CARTESIAN_POINT('Ctrl Pts',(54.1211939329318,10.6800213281955,-55.5124236099793));
#182966=CARTESIAN_POINT('Ctrl Pts',(54.131551448063,10.6678806463743,-55.5349122303772));
#182967=CARTESIAN_POINT('Ctrl Pts',(54.1403534159387,10.6575790662613,-55.5581259619573));
#182968=CARTESIAN_POINT('Ctrl Pts',(54.1475998365589,10.6491386635634,-55.5817548137324));
#182969=CARTESIAN_POINT('Ctrl Pts',(54.1549301223136,10.640600577396,-55.6056571297372));
#182970=CARTESIAN_POINT('Ctrl Pts',(54.1606686467721,10.6339666934735,-55.6299836882972));
#182971=CARTESIAN_POINT('Ctrl Pts',(54.1648154099345,10.6292088063485,-55.654430243584));
#182972=CARTESIAN_POINT('Ctrl Pts',(54.1690341997196,10.6243682777686,-55.6793014198929));
#182973=CARTESIAN_POINT('Ctrl Pts',(54.1716054522323,10.621469129154,-55.7042962935649));
#182974=CARTESIAN_POINT('Ctrl Pts',(54.1725291674727,10.6204340720944,-55.7291196457432));
#182975=CARTESIAN_POINT('Ctrl Pts',(54.1727881145264,10.6201439123522,-55.7360784287428));
#182976=CARTESIAN_POINT('Ctrl Pts',(54.1729175880533,10.61999998,-55.7430239067242));
#182977=CARTESIAN_POINT('Ctrl Pts',(54.1729175880533,10.61999998,-55.74995));
#182978=CARTESIAN_POINT('Origin',(3.5,-9.33460238845303,-92.34995));
#182979=CARTESIAN_POINT('',(3.5,45.7028119503364,-61.0621827299711));
#182980=CARTESIAN_POINT('',(3.5,45.8435334367418,-60.42825533736));
#182981=CARTESIAN_POINT('Origin',(3.5,43.6249324139852,-60.2700376788023));
#182982=CARTESIAN_POINT('',(3.50000000126666,45.8435334367292,-56.3263223051815));
#182983=CARTESIAN_POINT('',(3.5,45.8435334367418,-92.34995));
#182984=CARTESIAN_POINT('Ctrl Pts',(3.50000000506663,45.8435334367288,-56.3263223051817));
#182985=CARTESIAN_POINT('Ctrl Pts',(3.50000001032463,45.8894626566105,-56.3816811876747));
#182986=CARTESIAN_POINT('Ctrl Pts',(3.50000001775255,45.9328922004513,-56.438876382961));
#182987=CARTESIAN_POINT('Ctrl Pts',(3.50000002291889,45.9736813029624,-56.4976009415836));
#182988=CARTESIAN_POINT('Ctrl Pts',(3.50000002818049,46.0152224330363,-56.5574082032809));
#182989=CARTESIAN_POINT('Ctrl Pts',(3.50000003120722,46.0540257195003,-56.6188027368888));
#182990=CARTESIAN_POINT('Ctrl Pts',(3.50000003122783,46.0899059446862,-56.6814984159273));
#182991=CARTESIAN_POINT('Ctrl Pts',(3.50000003123068,46.0948520295369,-56.6901410079592));
#182992=CARTESIAN_POINT('Ctrl Pts',(3.50000003118087,46.0997425008543,-56.6988083694207));
#182993=CARTESIAN_POINT('Ctrl Pts',(3.5000000310803,46.1045768057904,-56.7074997895477));
#182994=CARTESIAN_POINT('Ctrl Pts',(3.50000003035461,46.1394632249473,-56.7702208072802));
#182995=CARTESIAN_POINT('Ctrl Pts',(3.50000002687238,46.1717681199834,-56.8347988963916));
#182996=CARTESIAN_POINT('Ctrl Pts',(3.50000002225516,46.2013495572016,-56.9009409523228));
#182997=CARTESIAN_POINT('Ctrl Pts',(3.5000000182853,46.2267835376253,-56.9578095805551));
#182998=CARTESIAN_POINT('Ctrl Pts',(3.50000001353393,46.2502037235481,-57.0158352648145));
#182999=CARTESIAN_POINT('Ctrl Pts',(3.50000000945277,46.2714898142467,-57.0748386052854));
#183000=CARTESIAN_POINT('Ctrl Pts',(3.50000000440193,46.2978334233143,-57.1478609820601));
#183001=CARTESIAN_POINT('Ctrl Pts',(3.5000000025334,46.3207458812431,-57.221900953307));
#183002=CARTESIAN_POINT('Ctrl Pts',(3.50000000146594,46.3400500971326,-57.2964727656199));
#183003=CARTESIAN_POINT('Ctrl Pts',(3.50000000013692,46.3640841940101,-57.3893160166336));
#183004=CARTESIAN_POINT('Ctrl Pts',(3.5000000001043,46.3827251371296,-57.4829234266614));
#183005=CARTESIAN_POINT('Ctrl Pts',(3.50000000003929,46.3959468792823,-57.577409970123));
#183006=CARTESIAN_POINT('Ctrl Pts',(3.49999999997471,46.4090811642661,-57.6712715183694));
#183007=CARTESIAN_POINT('Ctrl Pts',(3.50000000000001,46.4168677320184,-57.7660006115251));
#183008=CARTESIAN_POINT('Ctrl Pts',(3.5,46.4192300563852,-57.8617170363515));
#183009=CARTESIAN_POINT('Ctrl Pts',(3.5,46.4197429699982,-57.8824992193464));
#183010=CARTESIAN_POINT('Ctrl Pts',(3.5,46.41999998,-57.90332797385));
#183011=CARTESIAN_POINT('Ctrl Pts',(3.5,46.41999998,-57.9242045702762));
#183012=CARTESIAN_POINT('',(3.5,32.1080106234021,-91.84995));
#183013=CARTESIAN_POINT('',(3.5,32.0719455778696,-91.84995));
#183014=CARTESIAN_POINT('',(3.5,31.6538440087773,-91.1386408691296));
#183015=CARTESIAN_POINT('Ctrl Pts',(3.5,32.1080106234021,-91.84995));
#183016=CARTESIAN_POINT('Ctrl Pts',(3.5,31.9390236361236,-91.84995));
#183017=CARTESIAN_POINT('Ctrl Pts',(3.5,31.7764555346939,-91.7610777969008));
#183018=CARTESIAN_POINT('Ctrl Pts',(3.5,31.5945841314222,-91.476580999558));
#183019=CARTESIAN_POINT('Ctrl Pts',(3.5,31.5822909477801,-91.2917412718895));
#183020=CARTESIAN_POINT('Ctrl Pts',(3.5,31.6538440087773,-91.1386408691296));
#183021=CARTESIAN_POINT('Ctrl Pts',(3.5,31.6538440087773,-91.1386408691296));
#183022=CARTESIAN_POINT('Ctrl Pts',(3.5,36.3389063125119,-81.1141231801469));
#183023=CARTESIAN_POINT('Ctrl Pts',(3.5,41.0213995348935,-71.0884053145847));
#183024=CARTESIAN_POINT('Ctrl Pts',(3.5,45.7028119503364,-61.0621827299711));
#183025=CARTESIAN_POINT('Ctrl Pts',(3.5,46.41999998,-57.9242045702762));
#183026=CARTESIAN_POINT('Ctrl Pts',(3.5,46.91999998,-57.9242045702762));
#183027=CARTESIAN_POINT('Ctrl Pts',(4.,46.91999998,-57.9242045702762));
#183028=CARTESIAN_POINT('Ctrl Pts',(3.5,46.4199999742014,-57.7104514486517));
#183029=CARTESIAN_POINT('Ctrl Pts',(3.49999999999703,46.9215247752432,-57.6673651906402));
#183030=CARTESIAN_POINT('Ctrl Pts',(4.00152248707584,46.91999998,-57.6677551135179));
#183031=CARTESIAN_POINT('Ctrl Pts',(3.5,46.3930553625334,-57.5012311233074));
#183032=CARTESIAN_POINT('Ctrl Pts',(3.50000000000037,46.8905945241102,-57.4159945765447));
#183033=CARTESIAN_POINT('Ctrl Pts',(4.00300631304518,46.8876664373662,-57.4167435210981));
#183034=CARTESIAN_POINT('Ctrl Pts',(3.5,46.2869707037134,-57.0917336115785));
#183035=CARTESIAN_POINT('Ctrl Pts',(3.49999999999963,46.7659528393486,-56.9232257271801));
#183036=CARTESIAN_POINT('Ctrl Pts',(4.00589913432669,46.76036485013,-56.9254492364038));
#183037=CARTESIAN_POINT('Ctrl Pts',(3.5,46.2068681522152,-56.8917559154199));
#183038=CARTESIAN_POINT('Ctrl Pts',(3.50000000000004,46.6709152176612,-56.6822760272594));
#183039=CARTESIAN_POINT('Ctrl Pts',(4.00730581971222,46.6642417866207,-56.6855258491379));
#183040=CARTESIAN_POINT('Ctrl Pts',(3.5,46.0019773297039,-56.5234150618225));
#183041=CARTESIAN_POINT('Ctrl Pts',(3.49999999999995,46.4266646204127,-56.237771148346));
#183042=CARTESIAN_POINT('Ctrl Pts',(4.00988782131373,46.4183727996822,-56.2436081635303));
#183043=CARTESIAN_POINT('Ctrl Pts',(3.5,45.8742601250717,-56.3498268696058));
#183044=CARTESIAN_POINT('Ctrl Pts',(3.50000000000055,46.2738584100651,-56.0280733151404));
#183045=CARTESIAN_POINT('Ctrl Pts',(4.01109981373647,46.2651121552776,-56.0353451211632));
#183046=CARTESIAN_POINT('Ctrl Pts',(3.5,45.5823366328578,-56.0438443443254));
#183047=CARTESIAN_POINT('Ctrl Pts',(3.49999999999944,45.923712698628,-55.6579003398743));
#183048=CARTESIAN_POINT('Ctrl Pts',(4.01323028458345,45.9148039622378,-55.6682412064214));
#183049=CARTESIAN_POINT('Ctrl Pts',(3.5,45.4187493558633,-55.9106117044594));
#183050=CARTESIAN_POINT('Ctrl Pts',(3.50000000000323,45.7271164793515,-55.4966052387911));
#183051=CARTESIAN_POINT('Ctrl Pts',(4.01415476126711,45.7184991995766,-55.5083945642206));
#183052=CARTESIAN_POINT('Ctrl Pts',(3.5,45.2369942737712,-55.7978959562326));
#183053=CARTESIAN_POINT('Ctrl Pts',(3.49999999999999,45.5085033459109,-55.3600853439128));
#183054=CARTESIAN_POINT('Ctrl Pts',(4.01493543718735,45.5003931325255,-55.3731631297134));
#183055=CARTESIAN_POINT('',(4.01487932081911,45.5159632631672,-55.3828828377617));
#183056=CARTESIAN_POINT('Ctrl Pts',(3.5,45.8435334367294,-56.3263223051813));
#183057=CARTESIAN_POINT('Ctrl Pts',(3.5,45.829358462004,-56.2803914253743));
#183058=CARTESIAN_POINT('Ctrl Pts',(3.50100911575913,45.81531891597,-56.2356741862333));
#183059=CARTESIAN_POINT('Ctrl Pts',(3.50319349738481,45.801532809318,-56.1922448897079));
#183060=CARTESIAN_POINT('Ctrl Pts',(3.50366373776018,45.7985650202235,-56.1828956951989));
#183061=CARTESIAN_POINT('Ctrl Pts',(3.50418834634078,45.7956089381192,-56.173606026137));
#183062=CARTESIAN_POINT('Ctrl Pts',(3.50476880342442,45.792665672551,-56.1643763716752));
#183063=CARTESIAN_POINT('Ctrl Pts',(3.50726608643662,45.7800029498262,-56.1246679075265));
#183064=CARTESIAN_POINT('Ctrl Pts',(3.51079967824771,45.7675756095608,-56.0860750894433));
#183065=CARTESIAN_POINT('Ctrl Pts',(3.5154626655906,45.7554812444811,-56.0486556359451));
#183066=CARTESIAN_POINT('Ctrl Pts',(3.5169182402212,45.7517059284254,-56.0369749679103));
#183067=CARTESIAN_POINT('Ctrl Pts',(3.51848356681841,45.7479629575273,-56.0254084224728));
#183068=CARTESIAN_POINT('Ctrl Pts',(3.5201606028619,45.7442550148173,-56.0139572347226));
#183069=CARTESIAN_POINT('Ctrl Pts',(3.5221138261158,45.7399364195471,-56.0006201771886));
#183070=CARTESIAN_POINT('Ctrl Pts',(3.52421598894358,45.7356632838244,-55.9874497786217));
#183071=CARTESIAN_POINT('Ctrl Pts',(3.52646915533919,45.7314373927165,-55.9744418027717));
#183072=CARTESIAN_POINT('Ctrl Pts',(3.532348013131,45.7204113926327,-55.9405019924094));
#183073=CARTESIAN_POINT('Ctrl Pts',(3.53931414435956,45.7096879193575,-55.9076222761818));
#183074=CARTESIAN_POINT('Ctrl Pts',(3.54733023764625,45.699331249749,-55.8759996527637));
#183075=CARTESIAN_POINT('Ctrl Pts',(3.55287443235247,45.6921682352026,-55.8541284026321));
#183076=CARTESIAN_POINT('Ctrl Pts',(3.55892529436838,45.6851783107518,-55.8328413711166));
#183077=CARTESIAN_POINT('Ctrl Pts',(3.56547679288292,45.6783782894728,-55.8121802779607));
#183078=CARTESIAN_POINT('Ctrl Pts',(3.56875254214019,45.6749782788333,-55.8018497313828));
#183079=CARTESIAN_POINT('Ctrl Pts',(3.5721534672821,45.6716257509134,-55.791675655454));
#183080=CARTESIAN_POINT('Ctrl Pts',(3.57567833916439,45.6683227328112,-55.7816639721859));
#183081=CARTESIAN_POINT('Ctrl Pts',(3.57744077510554,45.6666712237602,-55.7766581305518));
#183082=CARTESIAN_POINT('Ctrl Pts',(3.5792341947625,45.6650320925117,-55.7716928867672));
#183083=CARTESIAN_POINT('Ctrl Pts',(3.58105841475146,45.6634055913715,-55.7667689928578));
#183084=CARTESIAN_POINT('Ctrl Pts',(3.58217199249725,45.6624127092169,-55.763763248642));
#183085=CARTESIAN_POINT('Ctrl Pts',(3.58309000391777,45.6616058713521,-55.7613218019833));
#183086=CARTESIAN_POINT('Ctrl Pts',(3.58418948277663,45.6606524681087,-55.7584376140889));
#183087=CARTESIAN_POINT('Ctrl Pts',(3.58489112765552,45.6600440430373,-55.7565970369377));
#183088=CARTESIAN_POINT('Ctrl Pts',(3.58566712536705,45.6593760501822,-55.7545765750859));
#183089=CARTESIAN_POINT('Ctrl Pts',(3.58662326907452,45.6585642310943,-55.7521221209547));
#183090=CARTESIAN_POINT('Ctrl Pts',(3.59663011570348,45.6500678627766,-55.7264341978348));
#183091=CARTESIAN_POINT('Ctrl Pts',(3.60756604207596,45.6418597808983,-55.7017516640631));
#183092=CARTESIAN_POINT('Ctrl Pts',(3.61939706851692,45.6340025528844,-55.6782726631486));
#183093=CARTESIAN_POINT('Ctrl Pts',(3.63078081980458,45.6264423694999,-55.6556812922116));
#183094=CARTESIAN_POINT('Ctrl Pts',(3.64309699882947,45.6191369624624,-55.6340209971509));
#183095=CARTESIAN_POINT('Ctrl Pts',(3.65611874522813,45.6121805085348,-55.613620522482));
#183096=CARTESIAN_POINT('Ctrl Pts',(3.66837924235669,45.6056307278222,-55.5944126563908));
#183097=CARTESIAN_POINT('Ctrl Pts',(3.6813233321023,45.5993584819171,-55.576222352987));
#183098=CARTESIAN_POINT('Ctrl Pts',(3.6948712464061,45.5934033229125,-55.5592148304515));
#183099=CARTESIAN_POINT('Ctrl Pts',(3.69890468364327,45.5916303739889,-55.5541514108602));
#183100=CARTESIAN_POINT('Ctrl Pts',(3.70299535045606,45.5898820494173,-55.54918217229));
#183101=CARTESIAN_POINT('Ctrl Pts',(3.70713510324855,45.5881616196546,-55.5443179945211));
#183102=CARTESIAN_POINT('Ctrl Pts',(3.71544271509736,45.5847090795157,-55.5345566143387));
#183103=CARTESIAN_POINT('Ctrl Pts',(3.72395514919793,45.5813659716028,-55.5252102230316));
#183104=CARTESIAN_POINT('Ctrl Pts',(3.73265162864498,45.5781355148738,-55.5162981662384));
#183105=CARTESIAN_POINT('Ctrl Pts',(3.73484642489412,45.5773202200922,-55.514048963105));
#183106=CARTESIAN_POINT('Ctrl Pts',(3.73677184059151,45.5766149280199,-55.5121100079521));
#183107=CARTESIAN_POINT('Ctrl Pts',(3.73889480346159,45.5758469968331,-55.5100058353679));
#183108=CARTESIAN_POINT('Ctrl Pts',(3.74058370382036,45.5752360774076,-55.5083318834197));
#183109=CARTESIAN_POINT('Ctrl Pts',(3.74239786108271,45.5745856139785,-55.506553746141));
#183110=CARTESIAN_POINT('Ctrl Pts',(3.74458472597647,45.5738132672584,-55.5044511731915));
#183111=CARTESIAN_POINT('Ctrl Pts',(3.75851748247104,45.568892561452,-55.4910554499346));
#183112=CARTESIAN_POINT('Ctrl Pts',(3.77302864720422,45.5641994060292,-55.478603396186));
#183113=CARTESIAN_POINT('Ctrl Pts',(3.78811621274905,45.5597292245555,-55.4671280662862));
#183114=CARTESIAN_POINT('Ctrl Pts',(3.80697700690182,45.554141101518,-55.4527828868446));
#183115=CARTESIAN_POINT('Ctrl Pts',(3.82647622225123,45.5489811037732,-55.4401969432647));
#183116=CARTESIAN_POINT('Ctrl Pts',(3.84639858082278,45.5442730215576,-55.4294510255291));
#183117=CARTESIAN_POINT('Ctrl Pts',(3.86604041389509,45.5396312335565,-55.4188564203967));
#183118=CARTESIAN_POINT('Ctrl Pts',(3.88609303497988,45.5354287546197,-55.4100505420465));
#183119=CARTESIAN_POINT('Ctrl Pts',(3.90634809031781,45.5316770625223,-55.4030622934231));
#183120=CARTESIAN_POINT('Ctrl Pts',(3.92624802272963,45.527991147183,-55.3961965666717));
#183121=CARTESIAN_POINT('Ctrl Pts',(3.94634292913325,45.5247403526288,-55.3910853208616));
#183122=CARTESIAN_POINT('Ctrl Pts',(3.96644019345904,45.5219243282022,-55.387707510953));
#183123=CARTESIAN_POINT('Ctrl Pts',(3.98261682616291,45.5196576618492,-55.3849886538314));
#183124=CARTESIAN_POINT('Ctrl Pts',(3.99879500906382,45.5176724685726,-55.3833919689501));
#183125=CARTESIAN_POINT('Ctrl Pts',(4.01487931457847,45.5159631508241,-55.382883017845));
#183126=CARTESIAN_POINT('Ctrl Pts',(4.,46.91999998,-57.9242045702762));
#183127=CARTESIAN_POINT('Ctrl Pts',(4.00007924273952,46.91999998,-57.9108568329946));
#183128=CARTESIAN_POINT('Ctrl Pts',(4.00017352383104,46.9199165136016,-57.8947589318435));
#183129=CARTESIAN_POINT('Ctrl Pts',(4.00028378860392,46.9196162946768,-57.8758666509881));
#183130=CARTESIAN_POINT('Ctrl Pts',(4.00039284318993,46.9193193707392,-57.8571817182253));
#183131=CARTESIAN_POINT('Ctrl Pts',(4.00051753261627,46.9188105351354,-57.8357633855592));
#183132=CARTESIAN_POINT('Ctrl Pts',(4.00065871293216,46.9179113977889,-57.8115772708384));
#183133=CARTESIAN_POINT('Ctrl Pts',(4.00080188348403,46.9169995851945,-57.7870502015335));
#183134=CARTESIAN_POINT('Ctrl Pts',(4.00096201348742,46.9156867135283,-57.7596767045056));
#183135=CARTESIAN_POINT('Ctrl Pts',(4.00113993168569,46.9137320375537,-57.7294302718212));
#183136=CARTESIAN_POINT('Ctrl Pts',(4.00131784988395,46.9117773615791,-57.6991838391367));
#183137=CARTESIAN_POINT('Ctrl Pts',(4.00151355645692,46.9091810715407,-57.6660644317711));
#183138=CARTESIAN_POINT('Ctrl Pts',(4.00172781289727,46.9056444043791,-57.6300555409693));
#183139=CARTESIAN_POINT('Ctrl Pts',(4.00194116627368,46.9021226438248,-57.5941984231133));
#183140=CARTESIAN_POINT('Ctrl Pts',(4.00217295382255,46.8976670534823,-57.5554657535219));
#183141=CARTESIAN_POINT('Ctrl Pts',(4.00242156630219,46.8919278848425,-57.5138872726071));
#183142=CARTESIAN_POINT('Ctrl Pts',(4.00267017878182,46.8861887162028,-57.4723087916922));
#183143=CARTESIAN_POINT('Ctrl Pts',(4.00293561629726,46.8791659866484,-57.4278844868078));
#183144=CARTESIAN_POINT('Ctrl Pts',(4.00321619974068,46.8704546297142,-57.3806538858939));
#183145=CARTESIAN_POINT('Ctrl Pts',(4.00328167929394,46.8684216667091,-57.3696317150546));
#183146=CARTESIAN_POINT('Ctrl Pts',(4.00335108852505,46.8661920116224,-57.3579141065444));
#183147=CARTESIAN_POINT('Ctrl Pts',(4.00341791351284,46.8639726084551,-57.3466154543736));
#183148=CARTESIAN_POINT('Ctrl Pts',(4.00348900771395,46.8616114154297,-57.3345949710762));
#183149=CARTESIAN_POINT('Ctrl Pts',(4.00355717719454,46.8592620513759,-57.3230486483617));
#183150=CARTESIAN_POINT('Ctrl Pts',(4.00361465014622,46.8572339429933,-57.3133081235097));
#183151=CARTESIAN_POINT('Ctrl Pts',(4.0036188984494,46.8570840286589,-57.3125881204212));
#183152=CARTESIAN_POINT('Ctrl Pts',(4.00362308833456,46.8569358921357,-57.3118779802164));
#183153=CARTESIAN_POINT('Ctrl Pts',(4.00362721667444,46.8567896681397,-57.3111782390562));
#183154=CARTESIAN_POINT('Ctrl Pts',(4.00373969128349,46.852805866605,-57.2921141320444));
#183155=CARTESIAN_POINT('Ctrl Pts',(4.00385082294783,46.8486732798078,-57.2732633244349));
#183156=CARTESIAN_POINT('Ctrl Pts',(4.003960635391,46.8444045670847,-57.2546306622253));
#183157=CARTESIAN_POINT('Ctrl Pts',(4.00412774291756,46.8379086363488,-57.2262763336519));
#183158=CARTESIAN_POINT('Ctrl Pts',(4.0042917882471,46.8310977738947,-57.1984284029624));
#183159=CARTESIAN_POINT('Ctrl Pts',(4.00445272368593,46.8240156437481,-57.171096378751));
#183160=CARTESIAN_POINT('Ctrl Pts',(4.0047257259229,46.8120018984446,-57.1247318004805));
#183161=CARTESIAN_POINT('Ctrl Pts',(4.00498965630254,46.799169649036,-57.0798715656276));
#183162=CARTESIAN_POINT('Ctrl Pts',(4.00524431666679,46.7857397829609,-57.0365571992696));
#183163=CARTESIAN_POINT('Ctrl Pts',(4.00553764088511,46.7702709251338,-56.9866666217082));
#183164=CARTESIAN_POINT('Ctrl Pts',(4.00581865521741,46.7540101778699,-56.9388289010681));
#183165=CARTESIAN_POINT('Ctrl Pts',(4.0060872420386,46.737261956176,-56.8930744281488));
#183166=CARTESIAN_POINT('Ctrl Pts',(4.00638137976372,46.71892046121,-56.8429672914));
#183167=CARTESIAN_POINT('Ctrl Pts',(4.00666061547987,46.6999945698815,-56.7953582140595));
#183168=CARTESIAN_POINT('Ctrl Pts',(4.00692505591205,46.6808375688148,-56.7502406324356));
#183169=CARTESIAN_POINT('Ctrl Pts',(4.00719094249502,46.6615758034652,-56.7048763153719));
#183170=CARTESIAN_POINT('Ctrl Pts',(4.00744186332538,46.6420808938963,-56.662032202587));
#183171=CARTESIAN_POINT('Ctrl Pts',(4.00767810377334,46.6226709619017,-56.6216696645318));
#183172=CARTESIAN_POINT('Ctrl Pts',(4.0079264310232,46.6022679569391,-56.5792420524993));
#183173=CARTESIAN_POINT('Ctrl Pts',(4.00815854179178,46.5819587512262,-56.5395556683638));
#183174=CARTESIAN_POINT('Ctrl Pts',(4.00837493639319,46.5620675828846,-56.50253498429));
#183175=CARTESIAN_POINT('Ctrl Pts',(4.00841906033974,46.5580116737128,-56.4949862807898));
#183176=CARTESIAN_POINT('Ctrl Pts',(4.00846253140605,46.5539729912662,-56.4875483092653));
#183177=CARTESIAN_POINT('Ctrl Pts',(4.00850535448981,46.5499540635142,-56.4802203087462));
#183178=CARTESIAN_POINT('Ctrl Pts',(4.00852061045761,46.5485222975845,-56.4776096667733));
#183179=CARTESIAN_POINT('Ctrl Pts',(4.00852856980572,46.5477743781799,-56.4762464665642));
#183180=CARTESIAN_POINT('Ctrl Pts',(4.00855086918121,46.5456663975,-56.4724302181349));
#183181=CARTESIAN_POINT('Ctrl Pts',(4.00856620879158,46.5442163298814,-56.4698050430919));
#183182=CARTESIAN_POINT('Ctrl Pts',(4.00858152375101,46.5427632883518,-56.467183969051));
#183183=CARTESIAN_POINT('Ctrl Pts',(4.00859681400415,46.5413072932493,-56.4645670062797));
#183184=CARTESIAN_POINT('Ctrl Pts',(4.00896054749668,46.5066712294084,-56.4023131639001));
#183185=CARTESIAN_POINT('Ctrl Pts',(4.00931319598185,46.470088502395,-56.3418910107853));
#183186=CARTESIAN_POINT('Ctrl Pts',(4.00965406429937,46.431893439433,-56.2834331861898));
#183187=CARTESIAN_POINT('Ctrl Pts',(4.01000373713251,46.3927118106592,-56.2234654153681));
#183188=CARTESIAN_POINT('Ctrl Pts',(4.01034101480063,46.351833327529,-56.1655645089445));
#183189=CARTESIAN_POINT('Ctrl Pts',(4.01066532568298,46.3095728022947,-56.1098411585262));
#183190=CARTESIAN_POINT('Ctrl Pts',(4.01100339145799,46.2655198950584,-56.0517544316515));
#183191=CARTESIAN_POINT('Ctrl Pts',(4.01132736838532,46.2199651772572,-55.9960336844979));
#183192=CARTESIAN_POINT('Ctrl Pts',(4.01163678119951,46.1732171831732,-55.9427728835428));
#183193=CARTESIAN_POINT('Ctrl Pts',(4.01181788083476,46.1458555346277,-55.911599282503));
#183194=CARTESIAN_POINT('Ctrl Pts',(4.0119939942426,46.1180842067542,-55.8812678356419));
#183195=CARTESIAN_POINT('Ctrl Pts',(4.0121650491596,46.0899580587577,-55.8517931637923));
#183196=CARTESIAN_POINT('Ctrl Pts',(4.01220547809655,46.0833104260319,-55.8448268066077));
#183197=CARTESIAN_POINT('Ctrl Pts',(4.01224563317101,46.0766440200839,-55.8379068481933));
#183198=CARTESIAN_POINT('Ctrl Pts',(4.0122855169593,46.0699590233885,-55.8310328738311));
#183199=CARTESIAN_POINT('Ctrl Pts',(4.01259435546335,46.0181940214239,-55.7778045309336));
#183200=CARTESIAN_POINT('Ctrl Pts',(4.01288644492606,45.9653889456504,-55.7274166744311));
#183201=CARTESIAN_POINT('Ctrl Pts',(4.01316209893909,45.9118461763452,-55.67982860949));
#183202=CARTESIAN_POINT('Ctrl Pts',(4.01344237678578,45.857405278057,-55.6314423000628));
#183203=CARTESIAN_POINT('Ctrl Pts',(4.01370566398607,45.8022018384633,-55.5859503887996));
#183204=CARTESIAN_POINT('Ctrl Pts',(4.01395252112905,45.7465895304821,-55.5432689102761));
#183205=CARTESIAN_POINT('Ctrl Pts',(4.01420785359687,45.6890678899609,-55.4991220522573));
#183206=CARTESIAN_POINT('Ctrl Pts',(4.01444560917555,45.6311089169403,-55.4579818299398));
#183207=CARTESIAN_POINT('Ctrl Pts',(4.01466664258002,45.5731406032728,-55.4197129653607));
#183208=CARTESIAN_POINT('Ctrl Pts',(4.01473933218221,45.5540769976138,-55.4071277701532));
#183209=CARTESIAN_POINT('Ctrl Pts',(4.01481021504988,45.5350126608396,-55.3948527899582));
#183210=CARTESIAN_POINT('Ctrl Pts',(4.0148793265843,45.515963602184,-55.3828822983059));
#183211=CARTESIAN_POINT('Ctrl Pts',(4.0117049092053,45.5008851266717,-55.3733547413106));
#183212=CARTESIAN_POINT('Ctrl Pts',(3.98080144737803,46.91999998,-56.2527140593899));
#183213=CARTESIAN_POINT('Ctrl Pts',(3.92215684205867,46.91999998,-57.921448793088));
#183214=CARTESIAN_POINT('Ctrl Pts',(4.20907605864183,45.4888071699417,-55.3727975967646));
#183215=CARTESIAN_POINT('Ctrl Pts',(4.17733814927366,46.9199999800018,-56.2502970131543));
#183216=CARTESIAN_POINT('Ctrl Pts',(4.11592937444032,46.91999998,-57.928258571556));
#183217=CARTESIAN_POINT('Ctrl Pts',(4.4062116365889,45.4758414047913,-55.3721833857794));
#183218=CARTESIAN_POINT('Ctrl Pts',(4.37353389556208,46.91999998,-56.2475777730215));
#183219=CARTESIAN_POINT('Ctrl Pts',(4.30969200192382,46.91999998,-57.9354449440051));
#183220=CARTESIAN_POINT('Ctrl Pts',(4.60306732532638,45.461992503193,-55.3715051982969));
#183221=CARTESIAN_POINT('Ctrl Pts',(4.5692462665161,46.9199999800001,-56.2445032348437));
#183222=CARTESIAN_POINT('Ctrl Pts',(4.50344622215482,46.91999998,-57.9429512300502));
#183223=CARTESIAN_POINT('',(4.51630724700544,45.4845441378501,-55.3818234152652));
#183224=CARTESIAN_POINT('Origin',(-0.00205740951117972,-22.4761263385902,
-51.448280968311));
#183225=CARTESIAN_POINT('Ctrl Pts',(4.51630724691536,45.4845441364184,-55.3818234176142));
#183226=CARTESIAN_POINT('Ctrl Pts',(4.51609516365136,45.539686183746,-55.4155436161894));
#183227=CARTESIAN_POINT('Ctrl Pts',(4.51587384346763,45.5949145728422,-55.4517660043098));
#183228=CARTESIAN_POINT('Ctrl Pts',(4.51563780342165,45.6499431393258,-55.4906255200563));
#183229=CARTESIAN_POINT('Ctrl Pts',(4.51540569412177,45.7040553218034,-55.5288379130265));
#183230=CARTESIAN_POINT('Ctrl Pts',(4.51515932999363,45.7579739851358,-55.5696008805653));
#183231=CARTESIAN_POINT('Ctrl Pts',(4.51489474095432,45.8113906483242,-55.6130088438551));
#183232=CARTESIAN_POINT('Ctrl Pts',(4.51463612804323,45.8636008184923,-55.6554363751671));
#183233=CARTESIAN_POINT('Ctrl Pts',(4.51436008730205,45.9153309682504,-55.7003912001386));
#183234=CARTESIAN_POINT('Ctrl Pts',(4.51406438647219,45.9662634802363,-55.7479217231849));
#183235=CARTESIAN_POINT('Ctrl Pts',(4.513901763993,45.9942741265869,-55.7740614249196));
#183236=CARTESIAN_POINT('Ctrl Pts',(4.51373322290916,46.0220430358204,-55.800979408275));
#183237=CARTESIAN_POINT('Ctrl Pts',(4.51355861607773,46.0495142484638,-55.8286777245581));
#183238=CARTESIAN_POINT('Ctrl Pts',(4.51324936416135,46.0981694189724,-55.8777351258112));
#183239=CARTESIAN_POINT('Ctrl Pts',(4.51292097533616,46.1458914126912,-55.9292432583753));
#183240=CARTESIAN_POINT('Ctrl Pts',(4.51257402801332,46.1923566835266,-55.9831763724683));
#183241=CARTESIAN_POINT('Ctrl Pts',(4.51223332955441,46.2379850689438,-56.0361380979107));
#183242=CARTESIAN_POINT('Ctrl Pts',(4.51187472815627,46.2824009821158,-56.0914384019429));
#183243=CARTESIAN_POINT('Ctrl Pts',(4.51150062802555,46.325289847004,-56.1490037731485));
#183244=CARTESIAN_POINT('Ctrl Pts',(4.5111957254623,46.3602455280244,-56.1959212366655));
#183245=CARTESIAN_POINT('Ctrl Pts',(4.51088056044139,46.394186514714,-56.2443424456773));
#183246=CARTESIAN_POINT('Ctrl Pts',(4.51055741037206,46.4269428333146,-56.2942019278305));
#183247=CARTESIAN_POINT('Ctrl Pts',(4.5103701770366,46.4459218630936,-56.3230905403786));
#183248=CARTESIAN_POINT('Ctrl Pts',(4.5101802797067,46.464503221912,-56.3524615517062));
#183249=CARTESIAN_POINT('Ctrl Pts',(4.50998830130491,46.4826544281561,-56.3822985621361));
#183250=CARTESIAN_POINT('Ctrl Pts',(4.50989231210402,46.4917300312782,-56.397217067351));
#183251=CARTESIAN_POINT('Ctrl Pts',(4.50979580322036,46.5006981216228,-56.4122520571168));
#183252=CARTESIAN_POINT('Ctrl Pts',(4.50969885839879,46.5095546859655,-56.4274011973728));
#183253=CARTESIAN_POINT('Ctrl Pts',(4.509650385988,46.5139829681369,-56.4349757675007));
#183254=CARTESIAN_POINT('Ctrl Pts',(4.50960180463459,46.5183833705597,-56.4425788741622));
#183255=CARTESIAN_POINT('Ctrl Pts',(4.50955312522921,46.5227553995485,-56.450210214626));
#183256=CARTESIAN_POINT('Ctrl Pts',(4.50952878552652,46.5249414140428,-56.4540258848579));
#183257=CARTESIAN_POINT('Ctrl Pts',(4.50950442131329,46.5271203352908,-56.4578486134765));
#183258=CARTESIAN_POINT('Ctrl Pts',(4.509480033991,46.5292921018848,-56.4616783615944));
#183259=CARTESIAN_POINT('Ctrl Pts',(4.50945700999974,46.531342459627,-56.4652940142739));
#183260=CARTESIAN_POINT('Ctrl Pts',(4.50942733452829,46.5339732395003,-56.4699603792029));
#183261=CARTESIAN_POINT('Ctrl Pts',(4.50940978857118,46.5355223682823,-56.472719241285));
#183262=CARTESIAN_POINT('Ctrl Pts',(4.50940874961371,46.5356140976146,-56.4728826031562));
#183263=CARTESIAN_POINT('Ctrl Pts',(4.50940775346655,46.5357020474182,-56.4730392698743));
#183264=CARTESIAN_POINT('Ctrl Pts',(4.50940680411579,46.5357858766478,-56.4731886251067));
#183265=CARTESIAN_POINT('Ctrl Pts',(4.50917570372938,46.5561924199199,-56.5095461584502));
#183266=CARTESIAN_POINT('Ctrl Pts',(4.50893178738087,46.577039509979,-56.5484586717076));
#183267=CARTESIAN_POINT('Ctrl Pts',(4.5086714158295,46.5980094018699,-56.5900119371826));
#183268=CARTESIAN_POINT('Ctrl Pts',(4.5084201314999,46.6182474240276,-56.6301149530582));
#183269=CARTESIAN_POINT('Ctrl Pts',(4.50815349630828,46.6385994455066,-56.6726782274364));
#183270=CARTESIAN_POINT('Ctrl Pts',(4.50786926894805,46.658740870374,-56.7177508957582));
#183271=CARTESIAN_POINT('Ctrl Pts',(4.50759076325134,46.6784768365417,-56.7619162248224));
#183272=CARTESIAN_POINT('Ctrl Pts',(4.50729534264338,46.6980101846824,-56.8084915435727));
#183273=CARTESIAN_POINT('Ctrl Pts',(4.50698225975394,46.7170030890835,-56.8574866815265));
#183274=CARTESIAN_POINT('Ctrl Pts',(4.50667871612507,46.7354173024404,-56.9049889963217));
#183275=CARTESIAN_POINT('Ctrl Pts',(4.50635855369438,46.7533229382722,-56.9547663298399));
#183276=CARTESIAN_POINT('Ctrl Pts',(4.50602267297348,46.7703885525615,-57.0067857649177));
#183277=CARTESIAN_POINT('Ctrl Pts',(4.50570201438208,46.7866807524379,-57.0564476768403));
#183278=CARTESIAN_POINT('Ctrl Pts',(4.50536702439257,46.8022067287499,-57.108153197194));
#183279=CARTESIAN_POINT('Ctrl Pts',(4.50502009884594,46.816664840301,-57.1618313115726));
#183280=CARTESIAN_POINT('Ctrl Pts',(4.50478709911119,46.8263750971247,-57.1978822352764));
#183281=CARTESIAN_POINT('Ctrl Pts',(4.50454874890674,46.8356034052046,-57.2348220520186));
#183282=CARTESIAN_POINT('Ctrl Pts',(4.50430622795092,46.8442569719706,-57.2726173865685));
#183283=CARTESIAN_POINT('Ctrl Pts',(4.50427591283144,46.8453386678164,-57.2773418033873));
#183284=CARTESIAN_POINT('Ctrl Pts',(4.50424553256607,46.8464113858651,-57.282079587099));
#183285=CARTESIAN_POINT('Ctrl Pts',(4.50421509076819,46.8474749396687,-57.2868306384043));
#183286=CARTESIAN_POINT('Ctrl Pts',(4.50418933320097,46.8483748391652,-57.2908506218439));
#183287=CARTESIAN_POINT('Ctrl Pts',(4.50415006884132,46.8497337805172,-57.2969770600281));
#183288=CARTESIAN_POINT('Ctrl Pts',(4.50411307286254,46.850990933455,-57.3027394373521));
#183289=CARTESIAN_POINT('Ctrl Pts',(4.50410634483202,46.8512195573111,-57.3037873742293));
#183290=CARTESIAN_POINT('Ctrl Pts',(4.50409969227911,46.8514449591298,-57.3048232627625));
#183291=CARTESIAN_POINT('Ctrl Pts',(4.50409321069445,46.8516639680635,-57.3058322336321));
#183292=CARTESIAN_POINT('Ctrl Pts',(4.50400896587206,46.8545105510662,-57.3189463987905));
#183293=CARTESIAN_POINT('Ctrl Pts',(4.50392566897696,46.8572242490104,-57.3318723306552));
#183294=CARTESIAN_POINT('Ctrl Pts',(4.50384341100556,46.8598131773404,-57.3446078874438));
#183295=CARTESIAN_POINT('Ctrl Pts',(4.50367889506276,46.8649910340005,-57.3700790010209));
#183296=CARTESIAN_POINT('Ctrl Pts',(4.50351853721598,46.8696701094606,-57.3947885521014));
#183297=CARTESIAN_POINT('Ctrl Pts',(4.50336288846785,46.8739125904307,-57.4187239095837));
#183298=CARTESIAN_POINT('Ctrl Pts',(4.50308835635982,46.8813954469139,-57.4609409156648));
#183299=CARTESIAN_POINT('Ctrl Pts',(4.50282854915127,46.8875224206904,-57.5007475455008));
#183300=CARTESIAN_POINT('Ctrl Pts',(4.50258522254136,46.8926036856479,-57.5381066004158));
#183301=CARTESIAN_POINT('Ctrl Pts',(4.50233588603805,46.8978104521307,-57.5763883819389));
#183302=CARTESIAN_POINT('Ctrl Pts',(4.50210382724618,46.9019194749012,-57.6121009010535));
#183303=CARTESIAN_POINT('Ctrl Pts',(4.50188963153007,46.9052193199389,-57.6452367975947));
#183304=CARTESIAN_POINT('Ctrl Pts',(4.50167067848076,46.9085924552491,-57.6791086495693));
#183305=CARTESIAN_POINT('Ctrl Pts',(4.50147036401527,46.9111201960475,-57.7102888532685));
#183306=CARTESIAN_POINT('Ctrl Pts',(4.50128838525139,46.9130612164935,-57.7387923258709));
#183307=CARTESIAN_POINT('Ctrl Pts',(4.50110143803939,46.9150552313614,-57.7680740102931));
#183308=CARTESIAN_POINT('Ctrl Pts',(4.50093381660528,46.9164301379209,-57.794531453623));
#183309=CARTESIAN_POINT('Ctrl Pts',(4.50078462327284,46.9174129714368,-57.818194171919));
#183310=CARTESIAN_POINT('Ctrl Pts',(4.50063367521126,46.9184073644949,-57.8421351979676));
#183311=CARTESIAN_POINT('Ctrl Pts',(4.50050156910709,46.9190003132005,-57.8632159463878));
#183312=CARTESIAN_POINT('Ctrl Pts',(4.50038716315524,46.9193733106124,-57.8814710357105));
#183313=CARTESIAN_POINT('Ctrl Pts',(4.50027133005522,46.9197509609516,-57.8999538467285));
#183314=CARTESIAN_POINT('Ctrl Pts',(4.50017362402679,46.919903046673,-57.9155405128008));
#183315=CARTESIAN_POINT('Ctrl Pts',(4.50009294576135,46.9199647097641,-57.9282632801726));
#183316=CARTESIAN_POINT('Ctrl Pts',(4.50005896270807,46.9199906833036,-57.9336223255003));
#183317=CARTESIAN_POINT('Ctrl Pts',(4.50002800331669,46.9199999799999,-57.9384731640903));
#183318=CARTESIAN_POINT('Ctrl Pts',(4.5,46.91999998,-57.9428177527387));
#183319=CARTESIAN_POINT('Ctrl Pts',(4.5,46.91999998,-57.9428177527387));
#183320=CARTESIAN_POINT('Ctrl Pts',(4.99999999999999,46.91999998,-57.9428177527387));
#183321=CARTESIAN_POINT('Ctrl Pts',(5.,46.41999998,-57.9428177527387));
#183322=CARTESIAN_POINT('Ctrl Pts',(4.50167566539267,46.91999998,-57.6828458026853));
#183323=CARTESIAN_POINT('Ctrl Pts',(4.99999999999699,46.9183271035242,-57.6832796231231));
#183324=CARTESIAN_POINT('Ctrl Pts',(5.,46.4199999741246,-57.7261203908743));
#183325=CARTESIAN_POINT('Ctrl Pts',(4.50330917749558,46.8867913077729,-57.4284566847483));
#183326=CARTESIAN_POINT('Ctrl Pts',(4.99999999999981,46.8836068729329,-57.4292829235226));
#183327=CARTESIAN_POINT('Ctrl Pts',(5.,46.3923260879484,-57.5140768479069));
#183328=CARTESIAN_POINT('Ctrl Pts',(4.50569802055499,46.7886864007714,-57.055145939945));
#183329=CARTESIAN_POINT('Ctrl Pts',(5.00000000000009,46.7833158134961,-57.0568766116336));
#183330=CARTESIAN_POINT('Ctrl Pts',(5.,46.310571996574,-57.2029077562381));
#183331=CARTESIAN_POINT('Ctrl Pts',(4.50648947498932,46.7474324008918,-56.931237732302));
#183332=CARTESIAN_POINT('Ctrl Pts',(4.99999999999935,46.7414185265942,-56.9334556299756));
#183333=CARTESIAN_POINT('Ctrl Pts',(5.,46.2761936631225,-57.0996254934279));
#183334=CARTESIAN_POINT('Ctrl Pts',(4.50801451396916,46.6501749278894,-56.6920779475246));
#183335=CARTESIAN_POINT('Ctrl Pts',(5.00000000000065,46.6430202500091,-56.6954228782697));
#183336=CARTESIAN_POINT('Ctrl Pts',(5.,46.1951457708619,-56.9002767254212));
#183337=CARTESIAN_POINT('Ctrl Pts',(4.50874992208284,46.5942418273256,-56.5765450470161));
#183338=CARTESIAN_POINT('Ctrl Pts',(4.99999999999985,46.5866051720245,-56.5805088850576));
#183339=CARTESIAN_POINT('Ctrl Pts',(5.,46.1485348528389,-56.8039757263989));
#183340=CARTESIAN_POINT('Ctrl Pts',(4.51087720078722,46.404990940203,-56.2418316606537));
#183341=CARTESIAN_POINT('Ctrl Pts',(5.00000000000027,46.3962887395937,-56.2480691534848));
#183342=CARTESIAN_POINT('Ctrl Pts',(5.,45.9908257800341,-56.5249797415912));
#183343=CARTESIAN_POINT('Ctrl Pts',(4.51220710564129,46.2476195396021,-56.0318427103247));
#183344=CARTESIAN_POINT('Ctrl Pts',(4.99999999999943,46.2385095854938,-56.0395648256266));
#183345=CARTESIAN_POINT('Ctrl Pts',(5.,45.859682945468,-56.349946411749));
#183346=CARTESIAN_POINT('Ctrl Pts',(4.51453310829638,45.888934282536,-55.6636820506581));
#183347=CARTESIAN_POINT('Ctrl Pts',(5.00000000000056,45.8798007876186,-55.6745387763548));
#183348=CARTESIAN_POINT('Ctrl Pts',(5.,45.5607785663138,-56.0430715492057));
#183349=CARTESIAN_POINT('Ctrl Pts',(4.51553991135993,45.6878102784858,-55.5038410313454));
#183350=CARTESIAN_POINT('Ctrl Pts',(5.,45.6790509243108,-55.5161529972778));
#183351=CARTESIAN_POINT('Ctrl Pts',(5.,45.3931752587345,-55.909838595577));
#183352=CARTESIAN_POINT('Ctrl Pts',(4.51638378732469,45.4644662248635,-55.3696531657294));
#183353=CARTESIAN_POINT('Ctrl Pts',(5.00000000000001,45.4562991060438,-55.383243356978));
#183354=CARTESIAN_POINT('Ctrl Pts',(5.,45.207055184053,-55.7979884638099));
#183355=CARTESIAN_POINT('',(4.9999999999955,45.6625902180235,-56.1488949301451));
#183356=CARTESIAN_POINT('Ctrl Pts',(4.51630724703539,45.4845441383311,-55.3818234144752));
#183357=CARTESIAN_POINT('Ctrl Pts',(4.54554286097715,45.4810304530569,-55.3807925506137));
#183358=CARTESIAN_POINT('Ctrl Pts',(4.57492336620464,45.4783968837311,-55.3834494769118));
#183359=CARTESIAN_POINT('Ctrl Pts',(4.60372984498934,45.4767192880502,-55.3896124857592));
#183360=CARTESIAN_POINT('Ctrl Pts',(4.61692192850124,45.4759510239911,-55.3924348691545));
#183361=CARTESIAN_POINT('Ctrl Pts',(4.62999357791384,45.4753830811306,-55.3959918367187));
#183362=CARTESIAN_POINT('Ctrl Pts',(4.64287614689165,45.4750218250454,-55.4002624573002));
#183363=CARTESIAN_POINT('Ctrl Pts',(4.65907655647388,45.4745675292792,-55.4056329546529));
#183364=CARTESIAN_POINT('Ctrl Pts',(4.67498108665864,45.4744400229746,-55.4121331306033));
#183365=CARTESIAN_POINT('Ctrl Pts',(4.69045701352468,45.4746510551925,-55.4197196712408));
#183366=CARTESIAN_POINT('Ctrl Pts',(4.69992582232718,45.4747801733861,-55.4243614289457));
#183367=CARTESIAN_POINT('Ctrl Pts',(4.70923612563516,45.4750360700629,-55.4294108958238));
#183368=CARTESIAN_POINT('Ctrl Pts',(4.71835329427959,45.4754210331403,-55.4348548259434));
#183369=CARTESIAN_POINT('Ctrl Pts',(4.71971079370954,45.4754783521588,-55.4356653990854));
#183370=CARTESIAN_POINT('Ctrl Pts',(4.72106393555446,45.475538528032,-55.4364846672862));
#183371=CARTESIAN_POINT('Ctrl Pts',(4.7224125609678,45.4756015634809,-55.4373125493747));
#183372=CARTESIAN_POINT('Ctrl Pts',(4.72531069163288,45.4757370236061,-55.4390916278676));
#183373=CARTESIAN_POINT('Ctrl Pts',(4.72818974066629,45.4758856810229,-55.4409104977034));
#183374=CARTESIAN_POINT('Ctrl Pts',(4.73104870708458,45.476047465006,-55.4427680187092));
#183375=CARTESIAN_POINT('Ctrl Pts',(4.73524115531564,45.4762847084271,-55.4454919264141));
#183376=CARTESIAN_POINT('Ctrl Pts',(4.7395886482537,45.476560471502,-55.4484311931122));
#183377=CARTESIAN_POINT('Ctrl Pts',(4.7438160849823,45.4768612403157,-55.451409022755));
#183378=CARTESIAN_POINT('Ctrl Pts',(4.74821455107906,45.4771741773306,-55.4545073264238));
#183379=CARTESIAN_POINT('Ctrl Pts',(4.75248292729602,45.4775141874115,-55.4576472006047));
#183380=CARTESIAN_POINT('Ctrl Pts',(4.75633522119668,45.4778490772923,-55.4605795883408));
#183381=CARTESIAN_POINT('Ctrl Pts',(4.75694303796767,45.4779019163776,-55.461042261878));
#183382=CARTESIAN_POINT('Ctrl Pts',(4.75754054294109,45.4779545964434,-55.4614996805176));
#183383=CARTESIAN_POINT('Ctrl Pts',(4.75812666234957,45.4780069577562,-55.4619507724367));
#183384=CARTESIAN_POINT('Ctrl Pts',(4.77386912235803,45.4794133194305,-55.4740665570259));
#183385=CARTESIAN_POINT('Ctrl Pts',(4.78904026416503,45.4812848835081,-55.4875078892351));
#183386=CARTESIAN_POINT('Ctrl Pts',(4.80352937623848,45.483614772575,-55.502161797825));
#183387=CARTESIAN_POINT('Ctrl Pts',(4.81801848831193,45.485944661642,-55.516815706415));
#183388=CARTESIAN_POINT('Ctrl Pts',(4.83182669596583,45.4887279060849,-55.5326796339206));
#183389=CARTESIAN_POINT('Ctrl Pts',(4.84485334429627,45.4919602456486,-55.5496336015971));
#183390=CARTESIAN_POINT('Ctrl Pts',(4.85787999262672,45.4951925852123,-55.5665875692735));
#183391=CARTESIAN_POINT('Ctrl Pts',(4.87012510664492,45.498883128266,-55.584636804503));
#183392=CARTESIAN_POINT('Ctrl Pts',(4.88150057758231,45.5030354799701,-55.6036686664228));
#183393=CARTESIAN_POINT('Ctrl Pts',(4.88174544212233,45.5031248620885,-55.6040783398456));
#183394=CARTESIAN_POINT('Ctrl Pts',(4.88198991600439,45.5032144625561,-55.6044884887332));
#183395=CARTESIAN_POINT('Ctrl Pts',(4.88223399810205,45.5033042813681,-55.6048991117999));
#183396=CARTESIAN_POINT('Ctrl Pts',(4.88765947683183,45.5053007819683,-55.6140264781068));
#183397=CARTESIAN_POINT('Ctrl Pts',(4.8928884876451,45.5074026169808,-55.6233733771008));
#183398=CARTESIAN_POINT('Ctrl Pts',(4.89792023215919,45.5096069594328,-55.6329271738964));
#183399=CARTESIAN_POINT('Ctrl Pts',(4.90054928878365,45.5107587152721,-55.6379189759809));
#183400=CARTESIAN_POINT('Ctrl Pts',(4.90312551250806,45.5119342888916,-55.6429660247168));
#183401=CARTESIAN_POINT('Ctrl Pts',(4.90564745040342,45.5131379411177,-55.6480674173699));
#183402=CARTESIAN_POINT('Ctrl Pts',(4.90715323516841,45.5138566111484,-55.6511133287506));
#183403=CARTESIAN_POINT('Ctrl Pts',(4.90884019027815,45.5146843292354,-55.6545940823321));
#183404=CARTESIAN_POINT('Ctrl Pts',(4.91034649665343,45.5154450020354,-55.6577675133901));
#183405=CARTESIAN_POINT('Ctrl Pts',(4.91136300178359,45.5159583290824,-55.6599090491384));
#183406=CARTESIAN_POINT('Ctrl Pts',(4.91229825558978,45.5164406191502,-55.6619096504392));
#183407=CARTESIAN_POINT('Ctrl Pts',(4.91305024972244,45.5168332118384,-55.6635325496486));
#183408=CARTESIAN_POINT('Ctrl Pts',(4.92411677602688,45.5226107001487,-55.6874155242751));
#183409=CARTESIAN_POINT('Ctrl Pts',(4.93418172838201,45.5290383944735,-55.7127029485112));
#183410=CARTESIAN_POINT('Ctrl Pts',(4.9431758910437,45.5361068199836,-55.7392571266968));
#183411=CARTESIAN_POINT('Ctrl Pts',(4.95243919302711,45.5433867594854,-55.7666059062005));
#183412=CARTESIAN_POINT('Ctrl Pts',(4.96056657366829,45.5513463741598,-55.7952981524042));
#183413=CARTESIAN_POINT('Ctrl Pts',(4.96751435343842,45.5599579987963,-55.8251415997744));
#183414=CARTESIAN_POINT('Ctrl Pts',(4.96956337324642,45.5624977150859,-55.8339429459345));
#183415=CARTESIAN_POINT('Ctrl Pts',(4.97151000621998,45.5650940280755,-55.8428441635502));
#183416=CARTESIAN_POINT('Ctrl Pts',(4.97335365356651,45.5677459505796,-55.8518397101609));
#183417=CARTESIAN_POINT('Ctrl Pts',(4.98019532371398,45.5775870837354,-55.8852216705573));
#183418=CARTESIAN_POINT('Ctrl Pts',(4.98563127466986,45.5881340252677,-55.919722555685));
#183419=CARTESIAN_POINT('Ctrl Pts',(4.98975026681294,45.5993409247369,-55.9553543305821));
#183420=CARTESIAN_POINT('Ctrl Pts',(4.99400798721088,45.6109252742114,-55.9921861888437));
#183421=CARTESIAN_POINT('Ctrl Pts',(4.99685902938038,45.6232147674421,-56.0302270542062));
#183422=CARTESIAN_POINT('Ctrl Pts',(4.99844839489109,45.6361384783249,-56.0694667702205));
#183423=CARTESIAN_POINT('Ctrl Pts',(4.99949969638536,45.6446869943655,-56.0954222674317));
#183424=CARTESIAN_POINT('Ctrl Pts',(4.99999994524809,45.6535125756061,-56.121901794988));
#183425=CARTESIAN_POINT('Ctrl Pts',(4.9999999999955,45.6625902180235,-56.1488949301451));
#183426=CARTESIAN_POINT('Ctrl Pts',(5.,46.41999998,-57.9428177527387));
#183427=CARTESIAN_POINT('Ctrl Pts',(5.,46.41999998,-57.7745740624592));
#183428=CARTESIAN_POINT('Ctrl Pts',(5.00000000017611,46.4033211412152,-57.6091706164621));
#183429=CARTESIAN_POINT('Ctrl Pts',(4.99999999982344,46.3703757696924,-57.4465347800693));
#183430=CARTESIAN_POINT('Ctrl Pts',(4.99999999972182,46.3608819639002,-57.3996683167638));
#183431=CARTESIAN_POINT('Ctrl Pts',(4.99999999967221,46.3500332431698,-57.3530322594102));
#183432=CARTESIAN_POINT('Ctrl Pts',(4.99999999969245,46.3378403217705,-57.3066263304899));
#183433=CARTESIAN_POINT('Ctrl Pts',(4.99999999973771,46.3105877995303,-57.202903968263));
#183434=CARTESIAN_POINT('Ctrl Pts',(4.99999999996081,46.2762003337233,-57.0996231221188));
#183435=CARTESIAN_POINT('Ctrl Pts',(4.9999999999857,46.2356732197596,-56.9999496853278));
#183436=CARTESIAN_POINT('Ctrl Pts',(4.99999999998832,46.2314106238701,-56.9894661462744));
#183437=CARTESIAN_POINT('Ctrl Pts',(4.99999999999009,46.2270807552915,-56.9790199139327));
#183438=CARTESIAN_POINT('Ctrl Pts',(4.99999999999128,46.2226837784916,-56.9686108996226));
#183439=CARTESIAN_POINT('Ctrl Pts',(5.00000000000135,46.1852595852368,-56.8800161717308));
#183440=CARTESIAN_POINT('Ctrl Pts',(5.00000000035917,46.1429808775709,-56.7941365878385));
#183441=CARTESIAN_POINT('Ctrl Pts',(4.99999999927331,46.0959886291946,-56.7109637993559));
#183442=CARTESIAN_POINT('Ctrl Pts',(4.99999999847595,46.061481441272,-56.6498886403374));
#183443=CARTESIAN_POINT('Ctrl Pts',(4.9999999969677,46.0241995329013,-56.5900309298165));
#183444=CARTESIAN_POINT('Ctrl Pts',(4.9999999904409,45.9844424230139,-56.5317775549116));
#183445=CARTESIAN_POINT('Ctrl Pts',(4.99999998658713,45.9609677338277,-56.4973816978229));
#183446=CARTESIAN_POINT('Ctrl Pts',(4.99999998917526,45.9365437147868,-56.4634809785609));
#183447=CARTESIAN_POINT('Ctrl Pts',(4.99999999269503,45.9112549501108,-56.4301707952614));
#183448=CARTESIAN_POINT('Ctrl Pts',(4.99999999800588,45.8730976568612,-56.379910276464));
#183449=CARTESIAN_POINT('Ctrl Pts',(4.99999999856442,45.8329742633927,-56.3309419284987));
#183450=CARTESIAN_POINT('Ctrl Pts',(4.99999999917036,45.7911678591845,-56.2836825816833));
#183451=CARTESIAN_POINT('Ctrl Pts',(4.99999999955207,45.7648322159121,-56.2539118964834));
#183452=CARTESIAN_POINT('Ctrl Pts',(4.99999999973279,45.7378296447702,-56.224818928837));
#183453=CARTESIAN_POINT('Ctrl Pts',(4.99999999986749,45.7102390019053,-56.1965009486372));
#183454=CARTESIAN_POINT('Ctrl Pts',(4.99999999994411,45.6945455669802,-56.1803938074714));
#183455=CARTESIAN_POINT('Ctrl Pts',(5.,45.6786637148754,-56.1645219339327));
#183456=CARTESIAN_POINT('Ctrl Pts',(5.,45.6625994185597,-56.1488914421297));
#183457=CARTESIAN_POINT('Origin',(5.,-9.33460238845303,-92.34995));
#183458=CARTESIAN_POINT('',(5.,45.6625917098448,-60.42825533736));
#183459=CARTESIAN_POINT('',(5.,45.6625917098448,-92.34995));
#183460=CARTESIAN_POINT('Origin',(5.,43.4682849810557,-60.2759318175826));
#183461=CARTESIAN_POINT('',(5.,46.41999998,-91.84995));
#183462=CARTESIAN_POINT('Ctrl Pts',(5.,45.6625917098448,-60.42825533736));
#183463=CARTESIAN_POINT('Ctrl Pts',(5.,45.2073007626125,-60.42825533736));
#183464=CARTESIAN_POINT('Ctrl Pts',(5.4533007853959,45.1647773033082,-60.42825533736));
#183465=CARTESIAN_POINT('Ctrl Pts',(5.,45.6625916931772,-60.6471114271654));
#183466=CARTESIAN_POINT('Ctrl Pts',(5.00000000000228,45.2073007505585,-60.5804098497461));
#183467=CARTESIAN_POINT('Ctrl Pts',(5.45330078693253,45.1647773031641,-60.574158272758));
#183468=CARTESIAN_POINT('Ctrl Pts',(5.,45.6152082879987,-60.8619682722934));
#183469=CARTESIAN_POINT('Ctrl Pts',(4.99999999999914,45.1727790578482,-60.730071400192));
#183470=CARTESIAN_POINT('Ctrl Pts',(5.45472878287372,45.1330538591303,-60.717398791161));
#183471=CARTESIAN_POINT('Ctrl Pts',(5.,45.5214348882082,-61.0621827299711));
#183472=CARTESIAN_POINT('Ctrl Pts',(4.99999999999999,45.1055585268382,-60.8674008824012));
#183473=CARTESIAN_POINT('Ctrl Pts',(5.45757488824865,45.0702713246265,-60.8508735991007));
#183474=CARTESIAN_POINT('',(5.4533007853959,45.1647773033082,-60.42825533736));
#183475=CARTESIAN_POINT('Origin',(5.5,45.6625917098448,-60.42825533736));
#183476=CARTESIAN_POINT('Origin',(5.51981953730066,43.6973226909656,-60.3269478376544));
#183477=CARTESIAN_POINT('Origin',(0.,-12.9675000200281,-60.64995));
#183478=CARTESIAN_POINT('Origin',(1.1373643128445E-15,-12.9675000200281,
-90.9273317382593));
#183479=CARTESIAN_POINT('Origin',(0.,-12.9675000200281,-60.8508735991007));
#183480=CARTESIAN_POINT('Origin',(12.,-9.33460238845303,-92.34995));
#183481=CARTESIAN_POINT('',(12.,44.7861808691872,-60.42825533736));
#183482=CARTESIAN_POINT('Origin',(12.0000005388087,43.3853963400085,-60.456295971705));
#183483=CARTESIAN_POINT('',(12.,44.7862606093016,-55.9010529569358));
#183484=CARTESIAN_POINT('',(12.,44.7861808691872,-92.34995));
#183485=CARTESIAN_POINT('Ctrl Pts',(12.,44.7862606093016,-55.9010529569358));
#183486=CARTESIAN_POINT('Ctrl Pts',(12.,44.8788753121608,-55.9352619713498));
#183487=CARTESIAN_POINT('Ctrl Pts',(11.9999999998966,44.9692347958784,-55.9749445041685));
#183488=CARTESIAN_POINT('Ctrl Pts',(12.0000000001034,45.0573639465224,-56.0200426809281));
#183489=CARTESIAN_POINT('Ctrl Pts',(12.0000000001611,45.0819593060274,-56.0326288214085));
#183490=CARTESIAN_POINT('Ctrl Pts',(12.0000000002553,45.1063808622814,-56.0456370713455));
#183491=CARTESIAN_POINT('Ctrl Pts',(12.0000000004528,45.1306289434624,-56.0590668658914));
#183492=CARTESIAN_POINT('Ctrl Pts',(12.0000000005851,45.1468544406639,-56.0680533540261));
#183493=CARTESIAN_POINT('Ctrl Pts',(12.0000000007159,45.1630095639554,-56.0772339702067));
#183494=CARTESIAN_POINT('Ctrl Pts',(12.0000000008214,45.179090134652,-56.0866066905108));
#183495=CARTESIAN_POINT('Ctrl Pts',(12.0000000011901,45.2352779195468,-56.1193562988592));
#183496=CARTESIAN_POINT('Ctrl Pts',(12.0000000011541,45.2902554021732,-56.1543787808435));
#183497=CARTESIAN_POINT('Ctrl Pts',(12.0000000008796,45.3436294771401,-56.1913642361008));
#183498=CARTESIAN_POINT('Ctrl Pts',(12.0000000006945,45.3796048513583,-56.2162932975287));
#183499=CARTESIAN_POINT('Ctrl Pts',(12.0000000004393,45.4148522843584,-56.242113151159));
#183500=CARTESIAN_POINT('Ctrl Pts',(12.0000000002603,45.4492603972454,-56.268719019813));
#183501=CARTESIAN_POINT('Ctrl Pts',(12.0000000001101,45.478118138608,-56.2910330966957));
#183502=CARTESIAN_POINT('Ctrl Pts',(12.0000000000612,45.5064639161954,-56.3139578240496));
#183503=CARTESIAN_POINT('Ctrl Pts',(12.0000000000338,45.5342394837982,-56.3374491395215));
#183504=CARTESIAN_POINT('Ctrl Pts',(11.9999999999739,45.5949303219844,-56.3887786981636));
#183505=CARTESIAN_POINT('Ctrl Pts',(12.,45.653197014409,-56.4429844895137));
#183506=CARTESIAN_POINT('Ctrl Pts',(12.,45.7088856859501,-56.5000343749657));
#183507=CARTESIAN_POINT('Ctrl Pts',(12.,45.7160867166447,-56.5074114224853));
#183508=CARTESIAN_POINT('Ctrl Pts',(12.,45.7232446868781,-56.5148359705657));
#183509=CARTESIAN_POINT('Ctrl Pts',(12.,45.7303593052335,-56.522307900516));
#183510=CARTESIAN_POINT('Ctrl Pts',(12.,45.7679171901077,-56.5617520239876));
#183511=CARTESIAN_POINT('Ctrl Pts',(12.,45.8043465692001,-56.6026021164951));
#183512=CARTESIAN_POINT('Ctrl Pts',(12.,45.8395823893984,-56.6448353261774));
#183513=CARTESIAN_POINT('Ctrl Pts',(12.,45.8717319797964,-56.6833694197455));
#183514=CARTESIAN_POINT('Ctrl Pts',(12.,45.9026476453863,-56.7227444562638));
#183515=CARTESIAN_POINT('Ctrl Pts',(12.,45.9322838293524,-56.7628973708158));
#183516=CARTESIAN_POINT('Ctrl Pts',(12.,45.9443118404631,-56.7791936558878));
#183517=CARTESIAN_POINT('Ctrl Pts',(12.,45.956129209429,-56.7956179995257));
#183518=CARTESIAN_POINT('Ctrl Pts',(12.,45.9677333562169,-56.8121658960379));
#183519=CARTESIAN_POINT('Ctrl Pts',(12.,45.9798251442283,-56.8294091850376));
#183520=CARTESIAN_POINT('Ctrl Pts',(12.,45.9916897000825,-56.8467926205779));
#183521=CARTESIAN_POINT('Ctrl Pts',(12.,46.0033285107085,-56.8643184852531));
#183522=CARTESIAN_POINT('Ctrl Pts',(12.,46.0482762655458,-56.9320013691878));
#183523=CARTESIAN_POINT('Ctrl Pts',(12.,46.0898342762704,-57.0017828740038));
#183524=CARTESIAN_POINT('Ctrl Pts',(12.,46.1278764894322,-57.0734367367491));
#183525=CARTESIAN_POINT('Ctrl Pts',(12.,46.1404078986321,-57.0970400920794));
#183526=CARTESIAN_POINT('Ctrl Pts',(12.,46.1525581757048,-57.1208464092098));
#183527=CARTESIAN_POINT('Ctrl Pts',(12.,46.164323905515,-57.144847012895));
#183528=CARTESIAN_POINT('Ctrl Pts',(12.,46.1884069401605,-57.1939733636938));
#183529=CARTESIAN_POINT('Ctrl Pts',(12.0000000000007,46.2108248057517,-57.2437789527949));
#183530=CARTESIAN_POINT('Ctrl Pts',(12.0000000001545,46.231652580328,-57.2944049984518));
#183531=CARTESIAN_POINT('Ctrl Pts',(12.000000000255,46.245256447615,-57.3274719016804));
#183532=CARTESIAN_POINT('Ctrl Pts',(12.0000000004148,46.2581810194019,-57.360889338337));
#183533=CARTESIAN_POINT('Ctrl Pts',(12.0000000005167,46.2704364630794,-57.3947019825787));
#183534=CARTESIAN_POINT('Ctrl Pts',(12.0000000006197,46.2828321131732,-57.4289014548942));
#183535=CARTESIAN_POINT('Ctrl Pts',(12.0000000006374,46.2944781423922,-57.4633231278189));
#183536=CARTESIAN_POINT('Ctrl Pts',(12.0000000004958,46.3053795309571,-57.4980138584003));
#183537=CARTESIAN_POINT('Ctrl Pts',(12.0000000001659,46.3307739116041,-57.5788246296216));
#183538=CARTESIAN_POINT('Ctrl Pts',(12.0000000000875,46.351920054225,-57.6603617613545));
#183539=CARTESIAN_POINT('Ctrl Pts',(12.0000000000438,46.3688636122321,-57.7426155626079));
#183540=CARTESIAN_POINT('Ctrl Pts',(12.,46.3858667849633,-57.82515876811));
#183541=CARTESIAN_POINT('Ctrl Pts',(12.0000000000021,46.3986378015382,-57.9084239530163));
#183542=CARTESIAN_POINT('Ctrl Pts',(12.0000000000007,46.4071710877912,-57.9924112496634));
#183543=CARTESIAN_POINT('Ctrl Pts',(11.9999999999993,46.4157043740442,-58.0763985463105));
#183544=CARTESIAN_POINT('Ctrl Pts',(12.,46.41999998,-58.1611082160512));
#183545=CARTESIAN_POINT('Ctrl Pts',(12.,46.41999998,-58.2465463958495));
#183546=CARTESIAN_POINT('',(12.,30.5847864844252,-91.84995));
#183547=CARTESIAN_POINT('Ctrl Pts',(11.9999999857978,44.6134318801692,-61.1210441133876));
#183548=CARTESIAN_POINT('Ctrl Pts',(12.0001420550745,44.0869928457662,-60.8415158913112));
#183549=CARTESIAN_POINT('Ctrl Pts',(11.4131406659365,44.1784219329663,-60.890075338912));
#183550=CARTESIAN_POINT('Ctrl Pts',(11.9999999856108,44.7369792722067,-60.8879413106956));
#183551=CARTESIAN_POINT('Ctrl Pts',(12.000145286376,44.1531002254807,-60.6958383983959));
#183552=CARTESIAN_POINT('Ctrl Pts',(11.4054134166098,44.2623189763507,-60.7346949078221));
#183553=CARTESIAN_POINT('Ctrl Pts',(11.9999999855212,44.7966973993881,-60.6286788556915));
#183554=CARTESIAN_POINT('Ctrl Pts',(12.0001468655555,44.1818517612737,-60.5455762622013));
#183555=CARTESIAN_POINT('Ctrl Pts',(11.4017112009619,44.3028668820625,-60.5618538448931));
#183556=CARTESIAN_POINT('Ctrl Pts',(11.9999999855391,44.7848185198866,-60.36167670255));
#183557=CARTESIAN_POINT('Ctrl Pts',(12.0001465537004,44.1760490867645,-60.3893137401235));
#183558=CARTESIAN_POINT('Ctrl Pts',(11.4024481915019,44.294801171802,-60.3838747332568));
#183559=CARTESIAN_POINT('',(11.402356187646,44.2958078622741,-60.42825533736));
#183560=CARTESIAN_POINT('Origin',(11.5321932041777,42.8849831558857,-60.3485062043524));
#183561=CARTESIAN_POINT('Origin',(11.5,44.7861808691872,-60.42825533736));
#183562=CARTESIAN_POINT('Ctrl Pts',(12.,46.41999998,-58.2465463958495));
#183563=CARTESIAN_POINT('Ctrl Pts',(12.,46.91999998,-58.2465463958495));
#183564=CARTESIAN_POINT('Ctrl Pts',(12.5,46.91999998,-58.2465463958495));
#183565=CARTESIAN_POINT('Ctrl Pts',(12.,46.4199999720693,-57.9548688319462));
#183566=CARTESIAN_POINT('Ctrl Pts',(12.0000000000051,46.9205971329195,-57.8963321594437));
#183567=CARTESIAN_POINT('Ctrl Pts',(12.5005968089278,46.91999998,-57.8965394261518));
#183568=CARTESIAN_POINT('Ctrl Pts',(12.,46.3698845360764,-57.6691983000707));
#183569=CARTESIAN_POINT('Ctrl Pts',(12.,46.8609831927853,-57.553339017633));
#183570=CARTESIAN_POINT('Ctrl Pts',(12.5011890520215,46.8598614514991,-57.5537408849781));
#183571=CARTESIAN_POINT('Ctrl Pts',(12.,46.170945649571,-57.1202211534365));
#183572=CARTESIAN_POINT('Ctrl Pts',(12.,46.6232060214067,-56.8937940810153));
#183573=CARTESIAN_POINT('Ctrl Pts',(12.5023407943396,46.6211347792778,-56.8949802448316));
#183574=CARTESIAN_POINT('Ctrl Pts',(12.,46.0263211387953,-56.8686580359845));
#183575=CARTESIAN_POINT('Ctrl Pts',(11.9999999999992,46.4499499105921,-56.5914299423666));
#183576=CARTESIAN_POINT('Ctrl Pts',(12.5028756040753,46.4475853737583,-56.5931100772464));
#183577=CARTESIAN_POINT('Ctrl Pts',(12.,45.7462130147,-56.5329239712738));
#183578=CARTESIAN_POINT('Ctrl Pts',(12.0000000000004,46.1140832559457,-56.187732860667));
#183579=CARTESIAN_POINT('Ctrl Pts',(12.503595797933,46.111455620038,-56.190236748787));
#183580=CARTESIAN_POINT('Ctrl Pts',(12.,45.64434144227,-56.430563765138));
#183581=CARTESIAN_POINT('Ctrl Pts',(12.0000000000004,45.9918445187629,-56.0645984007596));
#183582=CARTESIAN_POINT('Ctrl Pts',(12.5038165641686,45.9892097344963,-56.0674068194903));
#183583=CARTESIAN_POINT('Ctrl Pts',(12.,45.4241300187908,-56.2443433906185));
#183584=CARTESIAN_POINT('Ctrl Pts',(11.9999999999996,45.7274985396918,-55.840523660562));
#183585=CARTESIAN_POINT('Ctrl Pts',(12.5042197091625,45.7249560267766,-55.8439466125607));
#183586=CARTESIAN_POINT('Ctrl Pts',(12.,45.3048009887765,-56.159928342783));
#183587=CARTESIAN_POINT('Ctrl Pts',(12.,45.584205738319,-55.7389336239012));
#183588=CARTESIAN_POINT('Ctrl Pts',(12.5044033037043,45.5817611915078,-55.7426504905235));
#183589=CARTESIAN_POINT('Ctrl Pts',(12.,44.9276251211566,-55.9400376669437));
#183590=CARTESIAN_POINT('Ctrl Pts',(12.,45.1310727951979,-55.4742001436884));
#183591=CARTESIAN_POINT('Ctrl Pts',(12.5048829251119,45.1291501474361,-55.4787867514921));
#183592=CARTESIAN_POINT('Ctrl Pts',(12.,44.6565552133068,-55.8394367317102));
#183593=CARTESIAN_POINT('Ctrl Pts',(12.0000000000043,44.8053592277238,-55.3530984350278));
#183594=CARTESIAN_POINT('Ctrl Pts',(12.5051042651495,44.8038662560613,-55.3580679820572));
#183595=CARTESIAN_POINT('Ctrl Pts',(12.,44.367939553595,-55.7868701958087));
#183596=CARTESIAN_POINT('Ctrl Pts',(12.,44.4584726259965,-55.289799987766));
#183597=CARTESIAN_POINT('Ctrl Pts',(12.5052199580625,44.4575274683141,-55.2949893590463));
#183598=CARTESIAN_POINT('',(12.5052115665125,44.4820819006474,-55.29956472357));
#183599=CARTESIAN_POINT('Ctrl Pts',(12.,44.7862606093016,-55.9010529569358));
#183600=CARTESIAN_POINT('Ctrl Pts',(12.,44.7810881048319,-55.8832279833769));
#183601=CARTESIAN_POINT('Ctrl Pts',(12.0006703786237,44.7761284457092,-55.8662789181114));
#183602=CARTESIAN_POINT('Ctrl Pts',(12.0018185320163,44.7713976894101,-55.8503503808216));
#183603=CARTESIAN_POINT('Ctrl Pts',(12.0029958851643,44.7665466208536,-55.8340167501054));
#183604=CARTESIAN_POINT('Ctrl Pts',(12.0046741004194,44.7619366243899,-55.8187562997276));
#183605=CARTESIAN_POINT('Ctrl Pts',(12.0066350018515,44.7576008702921,-55.8046721293254));
#183606=CARTESIAN_POINT('Ctrl Pts',(12.0086618529174,44.7531192947929,-55.7901142758176));
#183607=CARTESIAN_POINT('Ctrl Pts',(12.0109892097238,44.7489312326591,-55.776812707229));
#183608=CARTESIAN_POINT('Ctrl Pts',(12.01338895859,44.7450830701278,-55.7648282080662));
#183609=CARTESIAN_POINT('Ctrl Pts',(12.0145579946409,44.7432084403313,-55.7589899673359));
#183610=CARTESIAN_POINT('Ctrl Pts',(12.0157445499893,44.7414145675279,-55.753463543691));
#183611=CARTESIAN_POINT('Ctrl Pts',(12.0169247969219,44.7397070404721,-55.7482523157339));
#183612=CARTESIAN_POINT('Ctrl Pts',(12.0193743177247,44.7361631862757,-55.7374367728701));
#183613=CARTESIAN_POINT('Ctrl Pts',(12.0217934301679,44.7329917135447,-55.727981421325));
#183614=CARTESIAN_POINT('Ctrl Pts',(12.0239997929904,44.7302399365573,-55.719894641493));
#183615=CARTESIAN_POINT('Ctrl Pts',(12.0255011769565,44.728367409607,-55.7143917561773));
#183616=CARTESIAN_POINT('Ctrl Pts',(12.0269049293583,44.7266891531487,-55.7095219207423));
#183617=CARTESIAN_POINT('Ctrl Pts',(12.028166402091,44.7252178005542,-55.7052830189335));
#183618=CARTESIAN_POINT('Ctrl Pts',(12.0297240387712,44.7234010091868,-55.7000489232846));
#183619=CARTESIAN_POINT('Ctrl Pts',(12.0310639389098,44.7218999447325,-55.6957766099129));
#183620=CARTESIAN_POINT('Ctrl Pts',(12.032125593107,44.7207326580353,-55.6924594693962));
#183621=CARTESIAN_POINT('Ctrl Pts',(12.0326564202055,44.7201490146867,-55.6908008991379));
#183622=CARTESIAN_POINT('Ctrl Pts',(12.0331180993725,44.7196487070603,-55.689381107546));
#183623=CARTESIAN_POINT('Ctrl Pts',(12.0335055719087,44.7192332875689,-55.688199347834));
#183624=CARTESIAN_POINT('Ctrl Pts',(12.0336993081768,44.7190255778231,-55.687608467978));
#183625=CARTESIAN_POINT('Ctrl Pts',(12.0338745398092,44.7188390802319,-55.6870771089147));
#183626=CARTESIAN_POINT('Ctrl Pts',(12.0340209511352,44.7186847214685,-55.6866348437614));
#183627=CARTESIAN_POINT('Ctrl Pts',(12.0341565853872,44.7185417247758,-55.6862251329499));
#183628=CARTESIAN_POINT('Ctrl Pts',(12.0342815026087,44.7184086826423,-55.6858404822045));
#183629=CARTESIAN_POINT('Ctrl Pts',(12.0348997710397,44.7177699474642,-55.6840011548822));
#183630=CARTESIAN_POINT('Ctrl Pts',(12.0349488967186,44.7177191955615,-55.6838550076768));
#183631=CARTESIAN_POINT('Ctrl Pts',(12.0350011653746,44.7176652423143,-55.683699681487));
#183632=CARTESIAN_POINT('Ctrl Pts',(12.0350568496592,44.7176078229384,-55.6835344375599));
#183633=CARTESIAN_POINT('Ctrl Pts',(12.0400192739913,44.7124907722303,-55.6688083709579));
#183634=CARTESIAN_POINT('Ctrl Pts',(12.0455323832357,44.7073153008005,-55.6542232562084));
#183635=CARTESIAN_POINT('Ctrl Pts',(12.0515296105903,44.7021205803995,-55.6399679408847));
#183636=CARTESIAN_POINT('Ctrl Pts',(12.0575194673347,44.6969322443252,-55.6257301453858));
#183637=CARTESIAN_POINT('Ctrl Pts',(12.0639919255376,44.6917245922883,-55.6118222192763));
#183638=CARTESIAN_POINT('Ctrl Pts',(12.0708341936134,44.6865526882755,-55.5984147538958));
#183639=CARTESIAN_POINT('Ctrl Pts',(12.0738508627112,44.6842724614794,-55.5925035726843));
#183640=CARTESIAN_POINT('Ctrl Pts',(12.0769388402072,44.6819994029677,-55.5866893624224));
#183641=CARTESIAN_POINT('Ctrl Pts',(12.0800859445827,44.6797392728956,-55.5809850306869));
#183642=CARTESIAN_POINT('Ctrl Pts',(12.0888020038362,44.67347973229,-55.5651866053801));
#183643=CARTESIAN_POINT('Ctrl Pts',(12.0979705023152,44.6673192139475,-55.550233182973));
#183644=CARTESIAN_POINT('Ctrl Pts',(12.107436545151,44.6612968646264,-55.536152291111));
#183645=CARTESIAN_POINT('Ctrl Pts',(12.1121695665689,44.6582856899659,-55.5291118451801));
#183646=CARTESIAN_POINT('Ctrl Pts',(12.1169770158129,44.6553091603234,-55.5222889725919));
#183647=CARTESIAN_POINT('Ctrl Pts',(12.1218401517797,44.6523726449418,-55.5156839551032));
#183648=CARTESIAN_POINT('Ctrl Pts',(12.124271719763,44.650904387251,-55.5123814463588));
#183649=CARTESIAN_POINT('Ctrl Pts',(12.1264248812969,44.6496156231053,-55.5095206617904));
#183650=CARTESIAN_POINT('Ctrl Pts',(12.1287304945814,44.6482552261011,-55.5065159503596));
#183651=CARTESIAN_POINT('Ctrl Pts',(12.1308308081185,44.6470159635314,-55.5037787887829));
#183652=CARTESIAN_POINT('Ctrl Pts',(12.1330577988297,44.6457172533762,-55.5009220320754));
#183653=CARTESIAN_POINT('Ctrl Pts',(12.1357691629899,44.6441547189305,-55.4975308599801));
#183654=CARTESIAN_POINT('Ctrl Pts',(12.136034191219,44.6440019855783,-55.4971993824353));
#183655=CARTESIAN_POINT('Ctrl Pts',(12.1363038761111,44.6438467179213,-55.4968628261204));
#183656=CARTESIAN_POINT('Ctrl Pts',(12.1365785717202,44.6436887155227,-55.496520823035));
#183657=CARTESIAN_POINT('Ctrl Pts',(12.1503224351533,44.635783371146,-55.4794093602218));
#183658=CARTESIAN_POINT('Ctrl Pts',(12.1649684649224,44.6278663758516,-55.4632013862314));
#183659=CARTESIAN_POINT('Ctrl Pts',(12.180359028425,44.6199535701122,-55.4480419954723));
#183660=CARTESIAN_POINT('Ctrl Pts',(12.1957795617725,44.6120253558688,-55.4328530850279));
#183661=CARTESIAN_POINT('Ctrl Pts',(12.2119466676888,44.6041014451226,-55.4187174594865));
#183662=CARTESIAN_POINT('Ctrl Pts',(12.2286720669685,44.5962094010195,-55.4057393699402));
#183663=CARTESIAN_POINT('Ctrl Pts',(12.2455602690405,44.588240536818,-55.3926349534117));
#183664=CARTESIAN_POINT('Ctrl Pts',(12.2630166775616,44.5803043277691,-55.3807110574856));
#183665=CARTESIAN_POINT('Ctrl Pts',(12.2808314202136,44.5724390158208,-55.3700251504023));
#183666=CARTESIAN_POINT('Ctrl Pts',(12.2910044870969,44.5679475479355,-55.3639229883004));
#183667=CARTESIAN_POINT('Ctrl Pts',(12.3012941967153,44.5634793675054,-55.3582235755147));
#183668=CARTESIAN_POINT('Ctrl Pts',(12.3116611113438,44.5590426551015,-55.35293008267));
#183669=CARTESIAN_POINT('Ctrl Pts',(12.330242046542,44.551090601031,-55.3434423950556));
#183670=CARTESIAN_POINT('Ctrl Pts',(12.3490698679653,44.5432394914724,-55.3352615934425));
#183671=CARTESIAN_POINT('Ctrl Pts',(12.367925946783,44.5355401121287,-55.3283642382583));
#183672=CARTESIAN_POINT('Ctrl Pts',(12.3870281440011,44.5277402368681,-55.3213768555534));
#183673=CARTESIAN_POINT('Ctrl Pts',(12.4061584607799,44.5200963409835,-55.315706063824));
#183674=CARTESIAN_POINT('Ctrl Pts',(12.4251133117475,44.5126625795231,-55.3112789150626));
#183675=CARTESIAN_POINT('Ctrl Pts',(12.4445420037074,44.5050429859021,-55.3067410946549));
#183676=CARTESIAN_POINT('Ctrl Pts',(12.4637856538272,44.4976444151584,-55.3035090922607));
#183677=CARTESIAN_POINT('Ctrl Pts',(12.4826620933969,44.4905226144073,-55.3014640358961));
#183678=CARTESIAN_POINT('Ctrl Pts',(12.4902405930691,44.4876633588544,-55.3006429881063));
#183679=CARTESIAN_POINT('Ctrl Pts',(12.4977603698057,44.4848486652911,-55.3000128805774));
#183680=CARTESIAN_POINT('Ctrl Pts',(12.5052115665125,44.4820819006474,-55.29956472357));
#183681=CARTESIAN_POINT('Ctrl Pts',(12.5,46.91999998,-58.2465463958495));
#183682=CARTESIAN_POINT('Ctrl Pts',(12.5001183587732,46.91999998,-58.1771332324744));
#183683=CARTESIAN_POINT('Ctrl Pts',(12.5002387653141,46.9176304364579,-58.1066977317926));
#183684=CARTESIAN_POINT('Ctrl Pts',(12.5003607390257,46.9126568864611,-58.0355338419799));
#183685=CARTESIAN_POINT('Ctrl Pts',(12.5004799036527,46.9077978785483,-57.9660088741151));
#183686=CARTESIAN_POINT('Ctrl Pts',(12.5006005637387,46.9004533625675,-57.8957888763114));
#183687=CARTESIAN_POINT('Ctrl Pts',(12.5007222595679,46.8904542319157,-57.8251501703648));
#183688=CARTESIAN_POINT('Ctrl Pts',(12.5008427738672,46.8805521815852,-57.7551972868673));
#183689=CARTESIAN_POINT('Ctrl Pts',(12.5009643035452,46.8680467092278,-57.6848339807686));
#183690=CARTESIAN_POINT('Ctrl Pts',(12.5010863958673,46.8528241024531,-57.6143279303507));
#183691=CARTESIAN_POINT('Ctrl Pts',(12.5011989872684,46.8387860811076,-57.5493084855601));
#183692=CARTESIAN_POINT('Ctrl Pts',(12.5013120568632,46.8224378094746,-57.4841677663372));
#183693=CARTESIAN_POINT('Ctrl Pts',(12.5014252487982,46.803729758825,-57.4191129723427));
#183694=CARTESIAN_POINT('Ctrl Pts',(12.5014818447657,46.7943757335003,-57.3865855753455));
#183695=CARTESIAN_POINT('Ctrl Pts',(12.5015384713309,46.7844323670111,-57.3540796050202));
#183696=CARTESIAN_POINT('Ctrl Pts',(12.5015950842516,46.7738971294599,-57.3216205428715));
#183697=CARTESIAN_POINT('Ctrl Pts',(12.5016240374496,46.7685091576696,-57.305020204213));
#183698=CARTESIAN_POINT('Ctrl Pts',(12.5016529870829,46.7629664190283,-57.2884321293601));
#183699=CARTESIAN_POINT('Ctrl Pts',(12.5016819272638,46.7572688248593,-57.2718596907753));
#183700=CARTESIAN_POINT('Ctrl Pts',(12.5017002181372,46.7536678116307,-57.2613855206603));
#183701=CARTESIAN_POINT('Ctrl Pts',(12.5017185112997,46.7500037826327,-57.2509141211986));
#183702=CARTESIAN_POINT('Ctrl Pts',(12.5017368193113,46.7462736677078,-57.2404383183051));
#183703=CARTESIAN_POINT('Ctrl Pts',(12.5017461844914,46.7443655851079,-57.2350795833535));
#183704=CARTESIAN_POINT('Ctrl Pts',(12.5017555524955,46.7424404182948,-57.2297203041163));
#183705=CARTESIAN_POINT('Ctrl Pts',(12.5017649231805,46.7404981153884,-57.2243605649049));
#183706=CARTESIAN_POINT('Ctrl Pts',(12.5018983791374,46.7128361149721,-57.1480279250182));
#183707=CARTESIAN_POINT('Ctrl Pts',(12.5020310524357,46.6819657867095,-57.0723595244106));
#183708=CARTESIAN_POINT('Ctrl Pts',(12.5021624247027,46.6478092902251,-56.9976379018118));
#183709=CARTESIAN_POINT('Ctrl Pts',(12.5022609539029,46.6221919178619,-56.9415966848627));
#183710=CARTESIAN_POINT('Ctrl Pts',(12.5023587512966,46.5947268663747,-56.8860878972876));
#183711=CARTESIAN_POINT('Ctrl Pts',(12.5024556013402,46.5653957155416,-56.8312270386029));
#183712=CARTESIAN_POINT('Ctrl Pts',(12.5024879138153,46.5556098440363,-56.8129235865218));
#183713=CARTESIAN_POINT('Ctrl Pts',(12.5025201230294,46.5456156675934,-56.7946910048095));
#183714=CARTESIAN_POINT('Ctrl Pts',(12.502552214228,46.5354149923617,-56.7765373631373));
#183715=CARTESIAN_POINT('Ctrl Pts',(12.5026571797921,46.5020500923837,-56.7171594861959));
#183716=CARTESIAN_POINT('Ctrl Pts',(12.5027607887523,46.46650156848,-56.6586795783787));
#183717=CARTESIAN_POINT('Ctrl Pts',(12.5028626133423,46.4288572096057,-56.6013268548767));
#183718=CARTESIAN_POINT('Ctrl Pts',(12.5029644347431,46.3912140298327,-56.5439759277839));
#183719=CARTESIAN_POINT('Ctrl Pts',(12.5030644713976,46.3514752242191,-56.487752338115));
#183720=CARTESIAN_POINT('Ctrl Pts',(12.5031623352766,46.3097745333203,-56.4328599106678));
#183721=CARTESIAN_POINT('Ctrl Pts',(12.5032057291689,46.2912840002589,-56.4085200203049));
#183722=CARTESIAN_POINT('Ctrl Pts',(12.503248696564,46.2724082816963,-56.3844414254211));
#183723=CARTESIAN_POINT('Ctrl Pts',(12.5032912070703,46.253161566843,-56.3606398144933));
#183724=CARTESIAN_POINT('Ctrl Pts',(12.5033026087216,46.2479994469195,-56.3542560357072));
#183725=CARTESIAN_POINT('Ctrl Pts',(12.5033150347087,46.242326326167,-56.3473004870475));
#183726=CARTESIAN_POINT('Ctrl Pts',(12.5033226268458,46.2371892796758,-56.34105451554));
#183727=CARTESIAN_POINT('Ctrl Pts',(12.5033255608336,46.2352040636999,-56.3386407545504));
#183728=CARTESIAN_POINT('Ctrl Pts',(12.5033277734457,46.2332994091198,-56.3363326367253));
#183729=CARTESIAN_POINT('Ctrl Pts',(12.5033289283955,46.2315374506266,-56.3342029953547));
#183730=CARTESIAN_POINT('Ctrl Pts',(12.5033306780701,46.2288681968597,-56.3309767256823));
#183731=CARTESIAN_POINT('Ctrl Pts',(12.5033324843988,46.2261887108314,-56.3277516232274));
#183732=CARTESIAN_POINT('Ctrl Pts',(12.5033343465982,46.2234989811437,-56.3245277666109));
#183733=CARTESIAN_POINT('Ctrl Pts',(12.5033641174473,46.1804984645187,-56.2729882008824));
#183734=CARTESIAN_POINT('Ctrl Pts',(12.5034073345385,46.1352351800247,-56.2222326288015));
#183735=CARTESIAN_POINT('Ctrl Pts',(12.5034608380734,46.087711103095,-56.1725503029996));
#183736=CARTESIAN_POINT('Ctrl Pts',(12.5035136995659,46.0407573150335,-56.1234641650498));
#183737=CARTESIAN_POINT('Ctrl Pts',(12.503576601829,45.9915966301208,-56.0754257125406));
#183738=CARTESIAN_POINT('Ctrl Pts',(12.5036465507219,45.9402647963719,-56.0286758909813));
#183739=CARTESIAN_POINT('Ctrl Pts',(12.50368351247,45.9131405028007,-56.0039727819793));
#183740=CARTESIAN_POINT('Ctrl Pts',(12.5037224426879,45.8854105601039,-55.9796288363907));
#183741=CARTESIAN_POINT('Ctrl Pts',(12.5037629060975,45.8570841630398,-55.9556751995434));
#183742=CARTESIAN_POINT('Ctrl Pts',(12.5038367165705,45.8054131647529,-55.911980679351));
#183743=CARTESIAN_POINT('Ctrl Pts',(12.5039158143411,45.7515724745622,-55.8694834215562));
#183744=CARTESIAN_POINT('Ctrl Pts',(12.5039972401431,45.6958258044151,-55.8285461839375));
#183745=CARTESIAN_POINT('Ctrl Pts',(12.5040803823153,45.6389040530895,-55.7867460324031));
#183746=CARTESIAN_POINT('Ctrl Pts',(12.5041659501983,45.5799955860921,-55.7465731230012));
#183747=CARTESIAN_POINT('Ctrl Pts',(12.504250825276,45.5194303742208,-55.7083917193762));
#183748=CARTESIAN_POINT('Ctrl Pts',(12.5042720272466,45.5043010585236,-55.6988539254619));
#183749=CARTESIAN_POINT('Ctrl Pts',(12.5042931862015,45.4890685752725,-55.6894402665091));
#183750=CARTESIAN_POINT('Ctrl Pts',(12.5043142540053,45.4737384761356,-55.6801561248251));
#183751=CARTESIAN_POINT('Ctrl Pts',(12.5043337369422,45.4595616137896,-55.6715704009183));
#183752=CARTESIAN_POINT('Ctrl Pts',(12.5043531362203,45.445277774059,-55.6630812139221));
#183753=CARTESIAN_POINT('Ctrl Pts',(12.5043724239116,45.4308917019908,-55.6546944382596));
#183754=CARTESIAN_POINT('Ctrl Pts',(12.5044489649122,45.3738022176376,-55.6214124766727));
#183755=CARTESIAN_POINT('Ctrl Pts',(12.504523615977,45.3153574552296,-55.5898123426925));
#183756=CARTESIAN_POINT('Ctrl Pts',(12.5045949328901,45.2557176044418,-55.5600969950934));
#183757=CARTESIAN_POINT('Ctrl Pts',(12.504667418844,45.1951001255114,-55.5298945476827));
#183758=CARTESIAN_POINT('Ctrl Pts',(12.5047364597886,45.133248026582,-55.5016394962639));
#183759=CARTESIAN_POINT('Ctrl Pts',(12.5048006288673,45.0703524782732,-55.4754938425311));
#183760=CARTESIAN_POINT('Ctrl Pts',(12.504862813151,45.0094023337473,-55.450156892356));
#183761=CARTESIAN_POINT('Ctrl Pts',(12.5049204224477,44.9474724509303,-55.4268007245137));
#183762=CARTESIAN_POINT('Ctrl Pts',(12.5049722441512,44.8847569474852,-55.4055245870557));
#183763=CARTESIAN_POINT('Ctrl Pts',(12.5050265469188,44.8190388184043,-55.383229813499));
#183764=CARTESIAN_POINT('Ctrl Pts',(12.5050744936202,44.7524579555756,-55.3632195169086));
#183765=CARTESIAN_POINT('Ctrl Pts',(12.5051147929775,44.6852599725649,-55.3455504977554));
#183766=CARTESIAN_POINT('Ctrl Pts',(12.5051550923347,44.6180619895543,-55.3278814786021));
#183767=CARTESIAN_POINT('Ctrl Pts',(12.5051877442253,44.550246997649,-55.3125537481411));
#183768=CARTESIAN_POINT('Ctrl Pts',(12.5052115665125,44.4820819006474,-55.29956472357));
#183769=CARTESIAN_POINT('Ctrl Pts',(12.5022360800201,44.4589702388883,-55.2952207669972));
#183770=CARTESIAN_POINT('Ctrl Pts',(12.4974463012635,46.91999998,-55.7446487532608));
#183771=CARTESIAN_POINT('Ctrl Pts',(12.4707855792057,46.91999998,-58.2462412559184));
#183772=CARTESIAN_POINT('Ctrl Pts',(12.6722965314195,44.4249835190402,-55.2908259090661));
#183773=CARTESIAN_POINT('Ctrl Pts',(12.6696732210372,46.9199999799984,-55.7170654011496));
#183774=CARTESIAN_POINT('Ctrl Pts',(12.6482571751841,46.91999998,-58.2481326596478));
#183775=CARTESIAN_POINT('Ctrl Pts',(12.8416972953071,44.3903034748093,-55.2862462023727));
#183776=CARTESIAN_POINT('Ctrl Pts',(12.8404286525071,46.9199999800016,-55.6879841619147));
#183777=CARTESIAN_POINT('Ctrl Pts',(12.8257146119078,46.91999998,-58.2493381002745));
#183778=CARTESIAN_POINT('Ctrl Pts',(13.0103905133279,44.3549359954419,-55.2814750420179));
#183779=CARTESIAN_POINT('Ctrl Pts',(13.0094744794619,46.91999998,-55.6573244385171));
#183780=CARTESIAN_POINT('Ctrl Pts',(13.0031560751435,46.91999998,-58.2497705672942));
#183781=CARTESIAN_POINT('',(13.0012809027682,44.3884783289294,-55.2865616735083));
#183782=CARTESIAN_POINT('Origin',(1.07162825033821,-13.9448070428209,-29.8942234462249));
#183783=CARTESIAN_POINT('Ctrl Pts',(13.0012808995197,44.3884779737753,-55.2865639194009));
#183784=CARTESIAN_POINT('Ctrl Pts',(13.0012784804915,44.4224225696128,-55.291931744549));
#183785=CARTESIAN_POINT('Ctrl Pts',(13.0012795549047,44.4587969009803,-55.2982778660883));
#183786=CARTESIAN_POINT('Ctrl Pts',(13.0012832293302,44.4975897490736,-55.3058907712396));
#183787=CARTESIAN_POINT('Ctrl Pts',(13.001286788091,44.5351614641449,-55.3132640350567));
#183788=CARTESIAN_POINT('Ctrl Pts',(13.0012927856775,44.5750021428636,-55.3218257397261));
#183789=CARTESIAN_POINT('Ctrl Pts',(13.0013003931539,44.6170743841883,-55.3318782262809));
#183790=CARTESIAN_POINT('Ctrl Pts',(13.001307851158,44.6583199869194,-55.3417332008163));
#183791=CARTESIAN_POINT('Ctrl Pts',(13.0013168563583,44.7017107050852,-55.3530210451754));
#183792=CARTESIAN_POINT('Ctrl Pts',(13.0013266117605,44.7471795754749,-55.3660642415441));
#183793=CARTESIAN_POINT('Ctrl Pts',(13.0013360521284,44.7911801048528,-55.3786862297325));
#183794=CARTESIAN_POINT('Ctrl Pts',(13.0013461949353,44.8371270376683,-55.392952211358));
#183795=CARTESIAN_POINT('Ctrl Pts',(13.0013563039396,44.8849248079065,-55.4091878548454));
#183796=CARTESIAN_POINT('Ctrl Pts',(13.0013625568311,44.9144899625084,-55.4192303590746));
#183797=CARTESIAN_POINT('Ctrl Pts',(13.0013687965186,44.9447625482416,-55.4300271052118));
#183798=CARTESIAN_POINT('Ctrl Pts',(13.0013748461807,44.9757120742321,-55.4416614421933));
#183799=CARTESIAN_POINT('Ctrl Pts',(13.0013842994568,45.0240741828949,-55.4598413997633));
#183800=CARTESIAN_POINT('Ctrl Pts',(13.0013931365079,45.0739799904631,-55.480023475315));
#183801=CARTESIAN_POINT('Ctrl Pts',(13.0014006105319,45.1252883103609,-55.5025313874079));
#183802=CARTESIAN_POINT('Ctrl Pts',(13.0014080845559,45.1765966302588,-55.5250392995008));
#183803=CARTESIAN_POINT('Ctrl Pts',(13.0014141955141,45.2293080017412,-55.5498730913657));
#183804=CARTESIAN_POINT('Ctrl Pts',(13.0014181864254,45.2832346253654,-55.5773823016361));
#183805=CARTESIAN_POINT('Ctrl Pts',(13.0014212224514,45.324258496423,-55.5983095212391));
#183806=CARTESIAN_POINT('Ctrl Pts',(13.0014229932898,45.3661059324401,-55.620873256131));
#183807=CARTESIAN_POINT('Ctrl Pts',(13.001423187548,45.4086013945452,-55.6451824135397));
#183808=CARTESIAN_POINT('Ctrl Pts',(13.0014233761988,45.4498701797213,-55.6687898611403));
#183809=CARTESIAN_POINT('Ctrl Pts',(13.0014220778889,45.491750347972,-55.6940436013212));
#183810=CARTESIAN_POINT('Ctrl Pts',(13.0014190141657,45.5340352237576,-55.7210302653281));
#183811=CARTESIAN_POINT('Ctrl Pts',(13.0014160783273,45.5745550598512,-55.7468904619577));
#183812=CARTESIAN_POINT('Ctrl Pts',(13.0014115213251,45.6154466101278,-55.7743420547962));
#183813=CARTESIAN_POINT('Ctrl Pts',(13.0014051054231,45.6564831493748,-55.803446918885));
#183814=CARTESIAN_POINT('Ctrl Pts',(13.0014003177448,45.6871054606683,-55.8251655682798));
#183815=CARTESIAN_POINT('Ctrl Pts',(13.0013944950829,45.7178076447179,-55.8478045670992));
#183816=CARTESIAN_POINT('Ctrl Pts',(13.0013875417864,45.7484775027769,-55.8713833924002));
#183817=CARTESIAN_POINT('Ctrl Pts',(13.0013845863314,45.7615135336423,-55.8814054242532));
#183818=CARTESIAN_POINT('Ctrl Pts',(13.0013814246616,45.7745560975569,-55.8916015678972));
#183819=CARTESIAN_POINT('Ctrl Pts',(13.001378047929,45.7876015846557,-55.9019767609528));
#183820=CARTESIAN_POINT('Ctrl Pts',(13.001364045054,45.8416995386273,-55.9450013496182));
#183821=CARTESIAN_POINT('Ctrl Pts',(13.0013463714257,45.8958236427124,-55.9910913928745));
#183822=CARTESIAN_POINT('Ctrl Pts',(13.0013248738051,45.9494882400812,-56.0403852266349));
#183823=CARTESIAN_POINT('Ctrl Pts',(13.0013043548959,46.0007096762087,-56.0874348847192));
#183824=CARTESIAN_POINT('Ctrl Pts',(13.0012803522366,46.05151236301,-56.1374034046404));
#183825=CARTESIAN_POINT('Ctrl Pts',(13.0012527501323,46.1015059085735,-56.1903752317056));
#183826=CARTESIAN_POINT('Ctrl Pts',(13.0012438014241,46.117714008136,-56.2075489015745));
#183827=CARTESIAN_POINT('Ctrl Pts',(13.0012344745285,46.1338373274142,-56.2250379434666));
#183828=CARTESIAN_POINT('Ctrl Pts',(13.0012247659273,46.1498633603297,-56.2428443395582));
#183829=CARTESIAN_POINT('Ctrl Pts',(13.0012122281624,46.1705595068598,-56.2658396612717));
#183830=CARTESIAN_POINT('Ctrl Pts',(13.0011990522377,46.1910800397285,-56.2893686136245));
#183831=CARTESIAN_POINT('Ctrl Pts',(13.0011852444629,46.2113780675757,-56.3134034792177));
#183832=CARTESIAN_POINT('Ctrl Pts',(13.0011589283363,46.2500639152882,-56.3592113358786));
#183833=CARTESIAN_POINT('Ctrl Pts',(13.0011302667257,46.2880812313484,-56.407022697181));
#183834=CARTESIAN_POINT('Ctrl Pts',(13.0010995292298,46.3251101019611,-56.4566907268017));
#183835=CARTESIAN_POINT('Ctrl Pts',(13.001068713536,46.3622331759606,-56.5064851144921));
#183836=CARTESIAN_POINT('Ctrl Pts',(13.0010358113699,46.3983627102444,-56.5581456580717));
#183837=CARTESIAN_POINT('Ctrl Pts',(13.0010011156225,46.4331522164086,-56.6114777846261));
#183838=CARTESIAN_POINT('Ctrl Pts',(13.00098565621,46.448653405088,-56.6352410238193));
#183839=CARTESIAN_POINT('Ctrl Pts',(13.0009698409937,46.4638882394776,-56.6593355083877));
#183840=CARTESIAN_POINT('Ctrl Pts',(13.0009536972384,46.4788245868152,-56.6837410472069));
#183841=CARTESIAN_POINT('Ctrl Pts',(13.0009158262526,46.5138631629177,-56.7409930185162));
#183842=CARTESIAN_POINT('Ctrl Pts',(13.0008760648962,46.5474441336558,-56.8001434760018));
#183843=CARTESIAN_POINT('Ctrl Pts',(13.0008346277944,46.579354801289,-56.8612467488641));
#183844=CARTESIAN_POINT('Ctrl Pts',(13.0007667564146,46.6316224779404,-56.9613300860422));
#183845=CARTESIAN_POINT('Ctrl Pts',(13.0006948249235,46.6789483102667,-57.0657671806725));
#183846=CARTESIAN_POINT('Ctrl Pts',(13.0006212178572,46.7207925144095,-57.1747907392822));
#183847=CARTESIAN_POINT('Ctrl Pts',(13.0005547235128,46.7585932726127,-57.2732792459199));
#183848=CARTESIAN_POINT('Ctrl Pts',(13.0004873134537,46.7914885412403,-57.3744677788747));
#183849=CARTESIAN_POINT('Ctrl Pts',(13.0004209511923,46.8190634696687,-57.4780082586315));
#183850=CARTESIAN_POINT('Ctrl Pts',(13.0004110986384,46.8231574149527,-57.493380521878));
#183851=CARTESIAN_POINT('Ctrl Pts',(13.0004012692221,46.8271340931422,-57.5088045337419));
#183852=CARTESIAN_POINT('Ctrl Pts',(13.0003914694124,46.8309921521592,-57.5242790574659));
#183853=CARTESIAN_POINT('Ctrl Pts',(13.0003482734639,46.8479978415686,-57.592488212134));
#183854=CARTESIAN_POINT('Ctrl Pts',(13.0003057279034,46.862674870022,-57.6616003148738));
#183855=CARTESIAN_POINT('Ctrl Pts',(13.0002646122398,46.8749074169579,-57.7313289963579));
#183856=CARTESIAN_POINT('Ctrl Pts',(13.0002235302982,46.8871299310971,-57.801000488306));
#183857=CARTESIAN_POINT('Ctrl Pts',(13.0001838760848,46.8969118661664,-57.8712871464115));
#183858=CARTESIAN_POINT('Ctrl Pts',(13.0001464311036,46.9041881318259,-57.9418906507672));
#183859=CARTESIAN_POINT('Ctrl Pts',(13.0001090362543,46.911454655917,-58.0123996301437));
#183860=CARTESIAN_POINT('Ctrl Pts',(13.0000738449037,46.9162221582274,-58.0832241957229));
#183861=CARTESIAN_POINT('Ctrl Pts',(13.0000416366651,46.9184773550183,-58.1540607093264));
#183862=CARTESIAN_POINT('Ctrl Pts',(13.0000271287854,46.919493185916,-58.1859683102483));
#183863=CARTESIAN_POINT('Ctrl Pts',(13.0000132261682,46.91999998,-58.2178782852586));
#183864=CARTESIAN_POINT('Ctrl Pts',(13.,46.91999998,-58.2497627936531));
#183865=CARTESIAN_POINT('Ctrl Pts',(13.,46.91999998,-58.2497627936531));
#183866=CARTESIAN_POINT('Ctrl Pts',(13.5,46.9199999800001,-58.2497627936531));
#183867=CARTESIAN_POINT('Ctrl Pts',(13.5,46.41999998,-58.2497627936531));
#183868=CARTESIAN_POINT('Ctrl Pts',(13.0001524477397,46.91999998,-57.8822548982638));
#183869=CARTESIAN_POINT('Ctrl Pts',(13.5,46.9198475451862,-57.8823102041449));
#183870=CARTESIAN_POINT('Ctrl Pts',(13.5,46.4199999716718,-57.9435058971265));
#183871=CARTESIAN_POINT('Ctrl Pts',(13.0003057176052,46.8526943145044,-57.5184560311191));
#183872=CARTESIAN_POINT('Ctrl Pts',(13.5000000000013,46.8524085179432,-57.5185641386525));
#183873=CARTESIAN_POINT('Ctrl Pts',(13.5,46.363911922201,-57.6403398562409));
#183874=CARTESIAN_POINT('Ctrl Pts',(13.0005259614006,46.6548418679923,-57.0029579960184));
#183875=CARTESIAN_POINT('Ctrl Pts',(13.4999999999993,46.6543661205181,-57.0031847607698));
#183876=CARTESIAN_POINT('Ctrl Pts',(13.5,46.1990348882699,-57.2107576948721));
#183877=CARTESIAN_POINT('Ctrl Pts',(13.0005963858014,46.5740565196337,-56.8393464452647));
#183878=CARTESIAN_POINT('Ctrl Pts',(13.5000000000001,46.5735338055633,-56.8396334804064));
#183879=CARTESIAN_POINT('Ctrl Pts',(13.5,46.1317137634759,-57.0744145874655));
#183880=CARTESIAN_POINT('Ctrl Pts',(13.0007311732941,46.3835934539471,-56.5281351595755));
#183881=CARTESIAN_POINT('Ctrl Pts',(13.4999999999999,46.3829981626758,-56.5285611340859));
#183882=CARTESIAN_POINT('Ctrl Pts',(13.5,45.9729945411748,-56.8150715642796));
#183883=CARTESIAN_POINT('Ctrl Pts',(13.0007961467471,46.2725429511699,-56.3791516167841));
#183884=CARTESIAN_POINT('Ctrl Pts',(13.4999999999992,46.2719244986749,-56.3796526797414));
#183885=CARTESIAN_POINT('Ctrl Pts',(13.5,45.8804524549659,-56.6909184744131));
#183886=CARTESIAN_POINT('Ctrl Pts',(13.0009156805798,46.0271849103864,-56.1065360355095));
#183887=CARTESIAN_POINT('Ctrl Pts',(13.5000000000008,46.0265477969208,-56.1071944318285));
#183888=CARTESIAN_POINT('Ctrl Pts',(13.5,45.6759874229978,-56.4637385666375));
#183889=CARTESIAN_POINT('Ctrl Pts',(13.0009702923331,45.8933503604458,-55.9827597531144));
#183890=CARTESIAN_POINT('Ctrl Pts',(13.5,45.892718112414,-55.9834952073023));
#183891=CARTESIAN_POINT('Ctrl Pts',(13.5,45.5644586309065,-56.3605915480362));
#183892=CARTESIAN_POINT('Ctrl Pts',(13.0010689871371,45.6036057246554,-55.7600056274797));
#183893=CARTESIAN_POINT('Ctrl Pts',(13.5,45.6030118434335,-55.7608945639374));
#183894=CARTESIAN_POINT('Ctrl Pts',(13.5,45.3230047666778,-56.1749628998404));
#183895=CARTESIAN_POINT('Ctrl Pts',(13.0011133171869,45.4461379323356,-55.6604821166903));
#183896=CARTESIAN_POINT('Ctrl Pts',(13.5,45.4455768559353,-55.6614429290966));
#183897=CARTESIAN_POINT('Ctrl Pts',(13.5,45.1917816064929,-56.0920265457655));
#183898=CARTESIAN_POINT('Ctrl Pts',(13.0012246935303,44.9574289489744,-55.4111808336381));
#183899=CARTESIAN_POINT('Ctrl Pts',(13.5,44.9570225707288,-55.4123450088757));
#183900=CARTESIAN_POINT('Ctrl Pts',(13.5,44.7845241217188,-55.8842752341532));
#183901=CARTESIAN_POINT('Ctrl Pts',(13.0012724779463,44.6023831565444,-55.3052501647884));
#183902=CARTESIAN_POINT('Ctrl Pts',(13.4999999999989,44.6020983302816,-55.3064963379004));
#183903=CARTESIAN_POINT('Ctrl Pts',(13.5,44.4886526268701,-55.795999572546));
#183904=CARTESIAN_POINT('Ctrl Pts',(13.0012899687735,44.235970178777,-55.2664423715086));
#183905=CARTESIAN_POINT('Ctrl Pts',(13.5,44.2358346644988,-55.2677218601875));
#183906=CARTESIAN_POINT('Ctrl Pts',(13.5,44.1833084789809,-55.7636597096568));
#183907=CARTESIAN_POINT('',(13.5,44.2316053598049,-55.7692503840784));
#183908=CARTESIAN_POINT('Ctrl Pts',(13.0012809046046,44.3884784470435,-55.2865609246976));
#183909=CARTESIAN_POINT('Ctrl Pts',(13.0227142078398,44.3801663262956,-55.2853023719116));
#183910=CARTESIAN_POINT('Ctrl Pts',(13.0440107500575,44.3720139890709,-55.2855217204714));
#183911=CARTESIAN_POINT('Ctrl Pts',(13.0649088497358,44.3641004291774,-55.2871102328437));
#183912=CARTESIAN_POINT('Ctrl Pts',(13.07963394808,44.3585244222926,-55.2882295212604));
#183913=CARTESIAN_POINT('Ctrl Pts',(13.0941615775764,44.3530667901527,-55.2900276155907));
#183914=CARTESIAN_POINT('Ctrl Pts',(13.1084088949827,44.3477516451068,-55.2924539725048));
#183915=CARTESIAN_POINT('Ctrl Pts',(13.1263525788297,44.3410575230077,-55.2955098306798));
#183916=CARTESIAN_POINT('Ctrl Pts',(13.1438410905178,44.3345933820395,-55.2995626257775));
#183917=CARTESIAN_POINT('Ctrl Pts',(13.1606968582402,44.3284113220637,-55.3044726413883));
#183918=CARTESIAN_POINT('Ctrl Pts',(13.1707483356885,44.3247248191731,-55.3074005953086));
#183919=CARTESIAN_POINT('Ctrl Pts',(13.1805753892938,44.3211383949467,-55.3106326202861));
#183920=CARTESIAN_POINT('Ctrl Pts',(13.1901463329097,44.3176608512962,-55.3141329365288));
#183921=CARTESIAN_POINT('Ctrl Pts',(13.2062128737933,44.3118231722252,-55.3200088434692));
#183922=CARTESIAN_POINT('Ctrl Pts',(13.2215361856163,44.3062995177508,-55.3266347825946));
#183923=CARTESIAN_POINT('Ctrl Pts',(13.2360675230861,44.3011033236774,-55.3338157321858));
#183924=CARTESIAN_POINT('Ctrl Pts',(13.2508326372236,44.2958235344816,-55.3411122071695));
#183925=CARTESIAN_POINT('Ctrl Pts',(13.2647743335246,44.2908839262016,-55.3489796349329));
#183926=CARTESIAN_POINT('Ctrl Pts',(13.2778504785041,44.2862936857036,-55.3572086642283));
#183927=CARTESIAN_POINT('Ctrl Pts',(13.2917257824545,44.2814229090171,-55.3659406171754));
#183928=CARTESIAN_POINT('Ctrl Pts',(13.3046252124269,44.276945916979,-55.3750777732145));
#183929=CARTESIAN_POINT('Ctrl Pts',(13.3165555674972,44.2728515348509,-55.3843944010043));
#183930=CARTESIAN_POINT('Ctrl Pts',(13.3257156128518,44.2697078961434,-55.3915476443573));
#183931=CARTESIAN_POINT('Ctrl Pts',(13.334304802766,44.2667896094788,-55.3988066151504));
#183932=CARTESIAN_POINT('Ctrl Pts',(13.3423419835487,44.2640855375983,-55.4060797210799));
#183933=CARTESIAN_POINT('Ctrl Pts',(13.3437380359519,44.2636158422972,-55.4073430542419));
#183934=CARTESIAN_POINT('Ctrl Pts',(13.3447368700783,44.2632803863473,-55.4082577144236));
#183935=CARTESIAN_POINT('Ctrl Pts',(13.3460250420018,44.2628483898243,-55.4094489617215));
#183936=CARTESIAN_POINT('Ctrl Pts',(13.3468856642166,44.2625597747741,-55.4102448290038));
#183937=CARTESIAN_POINT('Ctrl Pts',(13.3478751830343,44.2622281818022,-55.4111644618157));
#183938=CARTESIAN_POINT('Ctrl Pts',(13.3491900716332,44.2617885001658,-55.4124034829403));
#183939=CARTESIAN_POINT('Ctrl Pts',(13.3502012869711,44.2614503629161,-55.413356352382));
#183940=CARTESIAN_POINT('Ctrl Pts',(13.3512075120241,44.2611143783486,-55.4143131401545));
#183941=CARTESIAN_POINT('Ctrl Pts',(13.3522087210251,44.2607805556637,-55.4152737974554));
#183942=CARTESIAN_POINT('Ctrl Pts',(13.3693116047043,44.2550781193665,-55.4316839676167));
#183943=CARTESIAN_POINT('Ctrl Pts',(13.385004867505,44.2499909927695,-55.4493057513444));
#183944=CARTESIAN_POINT('Ctrl Pts',(13.399206340252,44.2455733147497,-55.4677825303627));
#183945=CARTESIAN_POINT('Ctrl Pts',(13.4057661780247,44.2435327340538,-55.4763171855412));
#183946=CARTESIAN_POINT('Ctrl Pts',(13.4120080885646,44.2416347832483,-55.4850348789939));
#183947=CARTESIAN_POINT('Ctrl Pts',(13.4179258006775,44.2398837690247,-55.4939035459242));
#183948=CARTESIAN_POINT('Ctrl Pts',(13.4267579302379,44.2372703967975,-55.5071399477399));
#183949=CARTESIAN_POINT('Ctrl Pts',(13.434866597522,44.2349850099162,-55.5207117442571));
#183950=CARTESIAN_POINT('Ctrl Pts',(13.4422285502336,44.2330409773694,-55.5345026349037));
#183951=CARTESIAN_POINT('Ctrl Pts',(13.4466064922102,44.2318849170109,-55.5427036817486));
#183952=CARTESIAN_POINT('Ctrl Pts',(13.4507229889113,44.2308488595923,-55.5509872047721));
#183953=CARTESIAN_POINT('Ctrl Pts',(13.4545706886585,44.22993571514,-55.5593210232526));
#183954=CARTESIAN_POINT('Ctrl Pts',(13.45698655648,44.2293623761468,-55.564553605112));
#183955=CARTESIAN_POINT('Ctrl Pts',(13.4592960808803,44.2288375697856,-55.5698051015885));
#183956=CARTESIAN_POINT('Ctrl Pts',(13.4614975299841,44.2283617435815,-55.5750655327987));
#183957=CARTESIAN_POINT('Ctrl Pts',(13.4646117992954,44.2276886183467,-55.5825071763295));
#183958=CARTESIAN_POINT('Ctrl Pts',(13.4675178248527,44.2271123449583,-55.5899868231329));
#183959=CARTESIAN_POINT('Ctrl Pts',(13.4702175294607,44.2266320008153,-55.5974728767516));
#183960=CARTESIAN_POINT('Ctrl Pts',(13.4767530004062,44.2254691790824,-55.6155951875323));
#183961=CARTESIAN_POINT('Ctrl Pts',(13.482090699869,44.2248660187073,-55.6337741617638));
#183962=CARTESIAN_POINT('Ctrl Pts',(13.4863540935445,44.2247860760356,-55.6518477306354));
#183963=CARTESIAN_POINT('Ctrl Pts',(13.4884747832457,44.224746311094,-55.6608378531263));
#183964=CARTESIAN_POINT('Ctrl Pts',(13.4903294038769,44.2248360355357,-55.6698027247168));
#183965=CARTESIAN_POINT('Ctrl Pts',(13.4919316006163,44.2250510335979,-55.6787268228452));
#183966=CARTESIAN_POINT('Ctrl Pts',(13.495482214722,44.2255274889129,-55.6985034382359));
#183967=CARTESIAN_POINT('Ctrl Pts',(13.4977914721084,44.2266204765841,-55.7180759667749));
#183968=CARTESIAN_POINT('Ctrl Pts',(13.4989942129331,44.2282757402414,-55.7372300434814));
#183969=CARTESIAN_POINT('Ctrl Pts',(13.4996734185077,44.2292104921684,-55.7480466345614));
#183970=CARTESIAN_POINT('Ctrl Pts',(13.5,44.2303242845141,-55.7587306797949));
#183971=CARTESIAN_POINT('Ctrl Pts',(13.5,44.231605359804,-55.7692503840715));
#183972=CARTESIAN_POINT('Ctrl Pts',(13.5,46.41999998,-58.2497627936531));
#183973=CARTESIAN_POINT('Ctrl Pts',(13.5,46.41999998,-58.1672776827351));
#183974=CARTESIAN_POINT('Ctrl Pts',(13.5,46.4159357655689,-58.0853150765277));
#183975=CARTESIAN_POINT('Ctrl Pts',(13.5,46.4079129436513,-58.0040039069953));
#183976=CARTESIAN_POINT('Ctrl Pts',(13.5,46.3998480609524,-57.9222664521286));
#183977=CARTESIAN_POINT('Ctrl Pts',(13.5,46.3877828714201,-57.8411867135009));
#183978=CARTESIAN_POINT('Ctrl Pts',(13.4999999999999,46.3717717336869,-57.7608954152443));
#183979=CARTESIAN_POINT('Ctrl Pts',(13.4999999999999,46.3557907741678,-57.6807554521413));
#183980=CARTESIAN_POINT('Ctrl Pts',(13.4999999999998,46.3358786103981,-57.6014003971058));
#183981=CARTESIAN_POINT('Ctrl Pts',(13.4999999999993,46.3120383093697,-57.5229684754947));
#183982=CARTESIAN_POINT('Ctrl Pts',(13.499999999999,46.2959527721241,-57.4700488586318));
#183983=CARTESIAN_POINT('Ctrl Pts',(13.4999999999985,46.2780779115088,-57.4175496722019));
#183984=CARTESIAN_POINT('Ctrl Pts',(13.4999999999976,46.2584018781846,-57.3655174652213));
#183985=CARTESIAN_POINT('Ctrl Pts',(13.4999999999975,46.2569427240896,-57.361658811059));
#183986=CARTESIAN_POINT('Ctrl Pts',(13.4999999999974,46.2554739003334,-57.3578033707196));
#183987=CARTESIAN_POINT('Ctrl Pts',(13.4999999999974,46.2539954124749,-57.3539511680007));
#183988=CARTESIAN_POINT('Ctrl Pts',(13.4999999999961,46.219672138924,-57.2645218183184));
#183989=CARTESIAN_POINT('Ctrl Pts',(13.4999999999986,46.1805716042438,-57.1778714284205));
#183990=CARTESIAN_POINT('Ctrl Pts',(13.4999999999971,46.1367457679112,-57.0938423224731));
#183991=CARTESIAN_POINT('Ctrl Pts',(13.4999999999963,46.1131655316061,-57.0486309508129));
#183992=CARTESIAN_POINT('Ctrl Pts',(13.4999999999953,46.0882165583815,-57.0041788421777));
#183993=CARTESIAN_POINT('Ctrl Pts',(13.4999999999852,46.0619014378574,-56.9604643403198));
#183994=CARTESIAN_POINT('Ctrl Pts',(13.499999999984,46.0587398032398,-56.9552122540816));
#183995=CARTESIAN_POINT('Ctrl Pts',(13.4999999999826,46.0555586143243,-56.9499710767904));
#183996=CARTESIAN_POINT('Ctrl Pts',(13.4999999999808,46.0523578866491,-56.9447407904478));
#183997=CARTESIAN_POINT('Ctrl Pts',(13.4999999999437,45.9841670777467,-56.8333106743359));
#183998=CARTESIAN_POINT('Ctrl Pts',(13.4999999995698,45.9062654719836,-56.7259689765119));
#183999=CARTESIAN_POINT('Ctrl Pts',(13.4999999997703,45.8207975744062,-56.6258771140376));
#184000=CARTESIAN_POINT('Ctrl Pts',(13.4999999997905,45.8121551558405,-56.6157559364371));
#184001=CARTESIAN_POINT('Ctrl Pts',(13.4999999998158,45.803435351967,-56.6057089285334));
#184002=CARTESIAN_POINT('Ctrl Pts',(13.4999999998434,45.7946403691178,-56.5957393884661));
#184003=CARTESIAN_POINT('Ctrl Pts',(13.4999999998604,45.7891977407958,-56.5895699050165));
#184004=CARTESIAN_POINT('Ctrl Pts',(13.4999999998752,45.7837267069275,-56.5834303340926));
#184005=CARTESIAN_POINT('Ctrl Pts',(13.4999999998881,45.778227802301,-56.5773214434301));
#184006=CARTESIAN_POINT('Ctrl Pts',(13.5000000001116,45.6828400874147,-56.4713524986363));
#184007=CARTESIAN_POINT('Ctrl Pts',(13.5000000000272,45.5794120988332,-56.3745067808491));
#184008=CARTESIAN_POINT('Ctrl Pts',(13.4999999999695,45.4679575974401,-56.2866310284186));
#184009=CARTESIAN_POINT('Ctrl Pts',(13.4999999999653,45.4599257124734,-56.2802983282937));
#184010=CARTESIAN_POINT('Ctrl Pts',(13.4999999999594,45.4518518043016,-56.2740118496439));
#184011=CARTESIAN_POINT('Ctrl Pts',(13.4999999999509,45.443735968515,-56.2677716701563));
#184012=CARTESIAN_POINT('Ctrl Pts',(13.4999999998703,45.3663292591542,-56.2082544777622));
#184013=CARTESIAN_POINT('Ctrl Pts',(13.4999999992365,45.2845712727012,-56.1527648487191));
#184014=CARTESIAN_POINT('Ctrl Pts',(13.4999999991445,45.2001155591256,-56.102385462588));
#184015=CARTESIAN_POINT('Ctrl Pts',(13.4999999991047,45.1634675983677,-56.0805242801082));
#184016=CARTESIAN_POINT('Ctrl Pts',(13.4999999992486,45.1263121785355,-56.0596248906738));
#184017=CARTESIAN_POINT('Ctrl Pts',(13.4999999995196,45.0887860427418,-56.0397731680737));
#184018=CARTESIAN_POINT('Ctrl Pts',(13.4999999995982,45.0778983802498,-56.0340134794998));
#184019=CARTESIAN_POINT('Ctrl Pts',(13.4999999996575,45.0669811451102,-56.0283421588346));
#184020=CARTESIAN_POINT('Ctrl Pts',(13.4999999997046,45.0560369222135,-56.022760797256));
#184021=CARTESIAN_POINT('Ctrl Pts',(13.4999999999911,44.9893496905531,-55.988751479638));
#184022=CARTESIAN_POINT('Ctrl Pts',(13.4999999999377,44.9212851553068,-55.9578058140961));
#184023=CARTESIAN_POINT('Ctrl Pts',(13.4999999999181,44.8519312666017,-55.9299466722255));
#184024=CARTESIAN_POINT('Ctrl Pts',(13.4999999999016,44.7935541183739,-55.906496837114));
#184025=CARTESIAN_POINT('Ctrl Pts',(13.4999999998496,44.7342628547591,-55.8852345670544));
#184026=CARTESIAN_POINT('Ctrl Pts',(13.4999999998385,44.6741009867898,-55.8662006918549));
#184027=CARTESIAN_POINT('Ctrl Pts',(13.4999999998289,44.6219934836799,-55.8497150383233));
#184028=CARTESIAN_POINT('Ctrl Pts',(13.4999999998617,44.5690884019705,-55.8348617736589));
#184029=CARTESIAN_POINT('Ctrl Pts',(13.4999999998979,44.5156559887646,-55.8217533863186));
#184030=CARTESIAN_POINT('Ctrl Pts',(13.4999999999339,44.4624243034296,-55.8086942428459));
#184031=CARTESIAN_POINT('Ctrl Pts',(13.4999999999687,44.4086696615075,-55.7973670287964));
#184032=CARTESIAN_POINT('Ctrl Pts',(13.4999999999845,44.3546736478472,-55.7878333559404));
#184033=CARTESIAN_POINT('Ctrl Pts',(13.4999999999965,44.3137472492196,-55.7806072873986));
#184034=CARTESIAN_POINT('Ctrl Pts',(13.4999999999993,44.2726825223299,-55.7744105877406));
#184035=CARTESIAN_POINT('Ctrl Pts',(13.4999999999998,44.2316053598049,-55.7692503840784));
#184036=CARTESIAN_POINT('Origin',(13.5,-9.33460238845303,-92.34995));
#184037=CARTESIAN_POINT('',(13.5,44.2316053598056,-60.42825533736));
#184038=CARTESIAN_POINT('',(13.5,44.2316053598056,-92.34995));
#184039=CARTESIAN_POINT('Origin',(13.4999995641033,42.8035277781091,-60.4528540700958));
#184040=CARTESIAN_POINT('',(13.5,46.41999998,-91.84995));
#184041=CARTESIAN_POINT('Ctrl Pts',(13.5000000114112,44.2302441743789,-60.3624063574045));
#184042=CARTESIAN_POINT('Ctrl Pts',(13.4999161431561,43.8380646295733,-60.3801294486319));
#184043=CARTESIAN_POINT('Ctrl Pts',(13.8812391026075,43.7449355503387,-60.3843616038035));
#184044=CARTESIAN_POINT('Ctrl Pts',(13.5000000113849,44.2419957581615,-60.6261785981702));
#184045=CARTESIAN_POINT('Ctrl Pts',(13.4999163945295,43.8475317166231,-60.5727811392321));
#184046=CARTESIAN_POINT('Ctrl Pts',(13.8803600752771,43.7529853273083,-60.5601847150614));
#184047=CARTESIAN_POINT('Ctrl Pts',(13.5000000115167,44.1831007301227,-60.8859969728056));
#184048=CARTESIAN_POINT('Ctrl Pts',(13.4999151269544,43.7997377261502,-60.7643333157514));
#184049=CARTESIAN_POINT('Ctrl Pts',(13.884762026428,43.7126430688856,-60.7334063315744));
#184050=CARTESIAN_POINT('Ctrl Pts',(13.5000000118016,44.056847986027,-61.1216298968641));
#184051=CARTESIAN_POINT('Ctrl Pts',(13.4999123453879,43.7012956163657,-60.9308210213385));
#184052=CARTESIAN_POINT('Ctrl Pts',(13.8942821039575,43.6261495705425,-60.8904677863889));
#184053=CARTESIAN_POINT('',(13.8811292719168,43.7459411239336,-60.42825533736));
#184054=CARTESIAN_POINT('Origin',(14.,44.2316053598056,-60.42825533736));
#184055=CARTESIAN_POINT('Origin',(14.0325246236231,42.3694154213074,-60.3603044162484));
#184056=CARTESIAN_POINT('Origin',(0.,-12.9675000200281,-60.64995));
#184057=CARTESIAN_POINT('Origin',(0.,-12.9675000200281,-60.8508735991007));
#184058=CARTESIAN_POINT('Ctrl Pts',(20.4999999961793,42.2396703210244,-61.1205979678028));
#184059=CARTESIAN_POINT('Ctrl Pts',(20.5000844423969,41.6420275017582,-60.7898798297297));
#184060=CARTESIAN_POINT('Ctrl Pts',(19.8489174898872,41.8225779837155,-60.8897941554007));
#184061=CARTESIAN_POINT('Ctrl Pts',(20.4999999961011,42.3674932175841,-60.8894198661636));
#184062=CARTESIAN_POINT('Ctrl Pts',(20.5000878549352,41.6934063086951,-60.6536629857367));
#184063=CARTESIAN_POINT('Ctrl Pts',(19.8355865710622,41.9126116301234,-60.7356962259096));
#184064=CARTESIAN_POINT('Ctrl Pts',(20.4999999960627,42.4307087138456,-60.6291716490909));
#184065=CARTESIAN_POINT('Ctrl Pts',(20.5000896090864,41.7106252645569,-60.5273413240714));
#184066=CARTESIAN_POINT('Ctrl Pts',(19.8290476963325,41.9571155016239,-60.5621838877489));
#184067=CARTESIAN_POINT('Ctrl Pts',(20.4999999960703,42.4181586164624,-60.3615059809689));
#184068=CARTESIAN_POINT('Ctrl Pts',(20.5000892602553,41.7070302221805,-60.3953720501034));
#184069=CARTESIAN_POINT('Ctrl Pts',(19.8303467534611,41.9482798096484,-60.3837601067579));
#184070=CARTESIAN_POINT('',(19.8301846741669,41.9493820112901,-60.42825533736));
#184071=CARTESIAN_POINT('',(20.5,42.4196614549321,-60.42825533736));
#184072=CARTESIAN_POINT('Origin',(20.,42.4196614549321,-60.42825533736));
#184073=CARTESIAN_POINT('Origin',(20.5000001497348,40.8982420780939,-60.4432551283903));
#184074=CARTESIAN_POINT('Origin',(20.0202631746512,40.6646653164194,-60.3952359560179));
#184075=CARTESIAN_POINT('Origin',(20.5,-9.33460238845303,-92.34995));
#184076=CARTESIAN_POINT('',(20.5,42.4196614549321,-55.74995));
#184077=CARTESIAN_POINT('',(20.5,42.4196614549321,-92.34995));
#184078=CARTESIAN_POINT('',(20.5,43.91999998,-55.74995));
#184079=CARTESIAN_POINT('',(20.5,29.41999998,-91.84995));
#184080=CARTESIAN_POINT('Origin',(21.,-9.33460238845303,-55.74995));
#184081=CARTESIAN_POINT('',(21.,42.0482945870964,-55.24995));
#184082=CARTESIAN_POINT('Ctrl Pts',(20.5,42.4196614549321,-55.74995));
#184083=CARTESIAN_POINT('Ctrl Pts',(20.5,42.4196614516742,-55.7252336462626));
#184084=CARTESIAN_POINT('Ctrl Pts',(20.5018810104879,42.4183057454763,-55.7004056886026));
#184085=CARTESIAN_POINT('Ctrl Pts',(20.5056026268981,42.4156171851572,-55.6757346618476));
#184086=CARTESIAN_POINT('Ctrl Pts',(20.5072707200331,42.4144121257108,-55.6646766790177));
#184087=CARTESIAN_POINT('Ctrl Pts',(20.5093091111243,42.4129389164194,-55.6536504525491));
#184088=CARTESIAN_POINT('Ctrl Pts',(20.5117166035502,42.4111978238051,-55.6426817760817));
#184089=CARTESIAN_POINT('Ctrl Pts',(20.5156059801789,42.408385036172,-55.6249615484114));
#184090=CARTESIAN_POINT('Ctrl Pts',(20.5204586741507,42.4048731188197,-55.6073877775764));
#184091=CARTESIAN_POINT('Ctrl Pts',(20.5262807670998,42.4006531055946,-55.5900728502967));
#184092=CARTESIAN_POINT('Ctrl Pts',(20.5291918135744,42.3985430989821,-55.5814153866568));
#184093=CARTESIAN_POINT('Ctrl Pts',(20.5323453818808,42.396255277344,-55.572822881862));
#184094=CARTESIAN_POINT('Ctrl Pts',(20.5357431944094,42.3937914700978,-55.5643110251239));
#184095=CARTESIAN_POINT('Ctrl Pts',(20.5371996176046,42.3927353947577,-55.5606625408467));
#184096=CARTESIAN_POINT('Ctrl Pts',(20.538779463254,42.3915902962302,-55.5568379466272));
#184097=CARTESIAN_POINT('Ctrl Pts',(20.5403859724756,42.3904256854597,-55.5530872414329));
#184098=CARTESIAN_POINT('Ctrl Pts',(20.5422793680974,42.3890531014094,-55.5486667446824));
#184099=CARTESIAN_POINT('Ctrl Pts',(20.5442112770272,42.3876522392155,-55.5443462699024));
#184100=CARTESIAN_POINT('Ctrl Pts',(20.5459814138442,42.3863675094681,-55.5405139093958));
#184101=CARTESIAN_POINT('Ctrl Pts',(20.5462133215967,42.3861991954794,-55.5400118272385));
#184102=CARTESIAN_POINT('Ctrl Pts',(20.5464423987541,42.3860329144334,-55.5395180940952));
#184103=CARTESIAN_POINT('Ctrl Pts',(20.5466681499119,42.3858690241902,-55.5390335577791));
#184104=CARTESIAN_POINT('Ctrl Pts',(20.5557618200603,42.3792672249949,-55.5195155474249));
#184105=CARTESIAN_POINT('Ctrl Pts',(20.566266949781,42.3716306571955,-55.5003023874531));
#184106=CARTESIAN_POINT('Ctrl Pts',(20.5781780765197,42.3629513503403,-55.481597463984));
#184107=CARTESIAN_POINT('Ctrl Pts',(20.5841379506068,42.3586085558124,-55.4722382328104));
#184108=CARTESIAN_POINT('Ctrl Pts',(20.5904496883736,42.3540047687641,-55.4630069755533));
#184109=CARTESIAN_POINT('Ctrl Pts',(20.5971114211574,42.3491396151076,-55.4539339992414));
#184110=CARTESIAN_POINT('Ctrl Pts',(20.6070992019679,42.3418454035403,-55.4403310971674));
#184111=CARTESIAN_POINT('Ctrl Pts',(20.6178748962852,42.333960942261,-55.4270812214323));
#184112=CARTESIAN_POINT('Ctrl Pts',(20.6294360364031,42.3254888876759,-55.4142951564802));
#184113=CARTESIAN_POINT('Ctrl Pts',(20.6352166064621,42.3212528603834,-55.4079021240042));
#184114=CARTESIAN_POINT('Ctrl Pts',(20.6411936694523,42.3168699308927,-55.4016252063396));
#184115=CARTESIAN_POINT('Ctrl Pts',(20.6473664072578,42.3123400985445,-55.3954807245231));
#184116=CARTESIAN_POINT('Ctrl Pts',(20.6489354846463,42.3111886390568,-55.393918829658));
#184117=CARTESIAN_POINT('Ctrl Pts',(20.6505955882827,42.3099701456555,-55.3922880019796));
#184118=CARTESIAN_POINT('Ctrl Pts',(20.652288151315,42.3087274579678,-55.3906500274103));
#184119=CARTESIAN_POINT('Ctrl Pts',(20.6553966463593,42.3064451863802,-55.3876417874015));
#184120=CARTESIAN_POINT('Ctrl Pts',(20.6586197595993,42.3040773966064,-55.3846084828431));
#184121=CARTESIAN_POINT('Ctrl Pts',(20.6615675916911,42.3019102893165,-55.3819000447302));
#184122=CARTESIAN_POINT('Ctrl Pts',(20.6633290593156,42.3006153412967,-55.3802816262111));
#184123=CARTESIAN_POINT('Ctrl Pts',(20.6649914729747,42.2993926349966,-55.3787783400392));
#184124=CARTESIAN_POINT('Ctrl Pts',(20.6664667151896,42.2983070444802,-55.3774588325365));
#184125=CARTESIAN_POINT('Ctrl Pts',(20.6795781583414,42.2886586910115,-55.3657315057044));
#184126=CARTESIAN_POINT('Ctrl Pts',(20.693699816926,42.2782395230549,-55.3543567742932));
#184127=CARTESIAN_POINT('Ctrl Pts',(20.7088448932229,42.2670360188918,-55.3435177790002));
#184128=CARTESIAN_POINT('Ctrl Pts',(20.7181341509916,42.2601643309555,-55.3368696631865));
#184129=CARTESIAN_POINT('Ctrl Pts',(20.7278079142016,42.2529979095219,-55.3304237404641));
#184130=CARTESIAN_POINT('Ctrl Pts',(20.73786336317,42.2455375240791,-55.3242291726904));
#184131=CARTESIAN_POINT('Ctrl Pts',(20.7510882195251,42.2357256771745,-55.3160821203563));
#184132=CARTESIAN_POINT('Ctrl Pts',(20.7649759751849,42.2254056105031,-55.3083675584016));
#184133=CARTESIAN_POINT('Ctrl Pts',(20.7795148740232,42.2145773218488,-55.3012102632954));
#184134=CARTESIAN_POINT('Ctrl Pts',(20.7867843234423,42.2091631775217,-55.2976316157423));
#184135=CARTESIAN_POINT('Ctrl Pts',(20.7942163726021,42.2036219771159,-55.2941925896406));
#184136=CARTESIAN_POINT('Ctrl Pts',(20.8018081090145,42.1979537193815,-55.2909108896379));
#184137=CARTESIAN_POINT('Ctrl Pts',(20.8056039772207,42.1951195905143,-55.2892700396365));
#184138=CARTESIAN_POINT('Ctrl Pts',(20.8094397672318,42.1922536973269,-55.2876685379919));
#184139=CARTESIAN_POINT('Ctrl Pts',(20.81331496872,42.1893560400312,-55.2861087627962));
#184140=CARTESIAN_POINT('Ctrl Pts',(20.8134763372388,42.1892353777464,-55.2860438116927));
#184141=CARTESIAN_POINT('Ctrl Pts',(20.8136400186047,42.1891129814804,-55.2859780296338));
#184142=CARTESIAN_POINT('Ctrl Pts',(20.8138057335169,42.1889890598484,-55.2859115369424));
#184143=CARTESIAN_POINT('Ctrl Pts',(20.8161824273861,42.1872117678775,-55.28495789451));
#184144=CARTESIAN_POINT('Ctrl Pts',(20.818981029976,42.1851178159589,-55.2838618636164));
#184145=CARTESIAN_POINT('Ctrl Pts',(20.8213680973811,42.183330845312,-55.2829496179739));
#184146=CARTESIAN_POINT('Ctrl Pts',(20.8228115398189,42.1822502770544,-55.2823979896155));
#184147=CARTESIAN_POINT('Ctrl Pts',(20.8241039729083,42.1812824064973,-55.2819122535834));
#184148=CARTESIAN_POINT('Ctrl Pts',(20.8250580089822,42.1805677763321,-55.2815563854263));
#184149=CARTESIAN_POINT('Ctrl Pts',(20.8356250604287,42.1726524218427,-55.2776147345526));
#184150=CARTESIAN_POINT('Ctrl Pts',(20.8471636556639,42.1639963345819,-55.2737212004608));
#184151=CARTESIAN_POINT('Ctrl Pts',(20.8597159721465,42.1545594711244,-55.2700623357848));
#184152=CARTESIAN_POINT('Ctrl Pts',(20.8715417960198,42.1456687866585,-55.2666152358575));
#184153=CARTESIAN_POINT('Ctrl Pts',(20.8842679311292,42.1360846843665,-55.2633765413884));
#184154=CARTESIAN_POINT('Ctrl Pts',(20.8979055823712,42.1257902400343,-55.2605340913107));
#184155=CARTESIAN_POINT('Ctrl Pts',(20.910887194157,42.1159910101303,-55.2578283773446));
#184156=CARTESIAN_POINT('Ctrl Pts',(20.9246952124769,42.1055477777859,-55.2554817619339));
#184157=CARTESIAN_POINT('Ctrl Pts',(20.9393096591675,42.0944667980502,-55.2536848471438));
#184158=CARTESIAN_POINT('Ctrl Pts',(20.9530056083917,42.0840822423413,-55.2520008659267));
#184159=CARTESIAN_POINT('Ctrl Pts',(20.9674100846602,42.0731373698124,-55.2507997850775));
#184160=CARTESIAN_POINT('Ctrl Pts',(20.9824748540747,42.0616599653893,-55.2502628085272));
#184161=CARTESIAN_POINT('Ctrl Pts',(20.9882222136164,42.0572812213137,-55.2500579466262));
#184162=CARTESIAN_POINT('Ctrl Pts',(20.9940653121634,42.0528252294229,-55.24995));
#184163=CARTESIAN_POINT('Ctrl Pts',(21.,42.0482945870964,-55.24995));
#184164=CARTESIAN_POINT('',(21.,41.7028772994424,-55.24995));
#184165=CARTESIAN_POINT('Origin',(0.,0.,-55.24995));
#184166=CARTESIAN_POINT('',(21.5,41.8548280612684,-55.24995));
#184167=CARTESIAN_POINT('Origin',(0.,-12.9675000200281,-55.24995));
#184168=CARTESIAN_POINT('',(21.5,43.91999998,-55.24995));
#184169=CARTESIAN_POINT('Origin',(21.5,0.,-55.74995));
#184170=CARTESIAN_POINT('',(22.,41.4520521304013,-55.74995));
#184171=CARTESIAN_POINT('Ctrl Pts',(21.5,41.8548280612684,-55.24995));
#184172=CARTESIAN_POINT('Ctrl Pts',(21.583715168139,41.7891659057934,-55.24995));
#184173=CARTESIAN_POINT('Ctrl Pts',(21.6546620826866,41.7342782074004,-55.2706498665447));
#184174=CARTESIAN_POINT('Ctrl Pts',(21.7369340153389,41.6681083454341,-55.3086173399654));
#184175=CARTESIAN_POINT('Ctrl Pts',(21.7605396074291,41.6487453390492,-55.3225002178965));
#184176=CARTESIAN_POINT('Ctrl Pts',(21.7907977214966,41.6237412508776,-55.3430283417078));
#184177=CARTESIAN_POINT('Ctrl Pts',(21.8000301990784,41.616079958388,-55.3498287160269));
#184178=CARTESIAN_POINT('Ctrl Pts',(21.812698596049,41.6055981250051,-55.3597598174085));
#184179=CARTESIAN_POINT('Ctrl Pts',(21.8187378809943,41.6006097346515,-55.3646586201736));
#184180=CARTESIAN_POINT('Ctrl Pts',(21.8252905599244,41.5952318669969,-55.3702183104546));
#184181=CARTESIAN_POINT('Ctrl Pts',(21.8279956516036,41.5930217639502,-55.3725639246649));
#184182=CARTESIAN_POINT('Ctrl Pts',(21.8297763865557,41.5915694057806,-55.374119011126));
#184183=CARTESIAN_POINT('Ctrl Pts',(21.8297528299007,41.5915871184344,-55.3740927601813));
#184184=CARTESIAN_POINT('Ctrl Pts',(21.9448313704802,41.498084291402,-55.4760225654778));
#184185=CARTESIAN_POINT('Ctrl Pts',(22.,41.4520521304013,-55.6193427204272));
#184186=CARTESIAN_POINT('Ctrl Pts',(22.,41.4520521304013,-55.74995));
#184187=CARTESIAN_POINT('',(22.,41.1166950488946,-55.74995));
#184188=CARTESIAN_POINT('Origin',(22.,-9.33460238845303,-92.34995));
#184189=CARTESIAN_POINT('',(22.,41.4520521304013,-60.5010370523947));
#184190=CARTESIAN_POINT('',(22.,41.4520521304013,-92.34995));
#184191=CARTESIAN_POINT('Origin',(22.,40.1816528160858,-60.6046736522147));
#184192=CARTESIAN_POINT('',(22.,46.41999998,-91.84995));
#184193=CARTESIAN_POINT('Ctrl Pts',(22.,41.4520521304013,-60.5010370523947));
#184194=CARTESIAN_POINT('Ctrl Pts',(22.,41.1177283573993,-60.5010370523946));
#184195=CARTESIAN_POINT('Ctrl Pts',(22.3089577584378,40.9899884313956,-60.5010370523947));
#184196=CARTESIAN_POINT('Ctrl Pts',(22.,41.4520521024983,-60.811367390836));
#184197=CARTESIAN_POINT('Ctrl Pts',(22.,41.1177283336776,-60.7368788147381));
#184198=CARTESIAN_POINT('Ctrl Pts',(22.3089577682091,40.9899884273556,-60.7079658702078));
#184199=CARTESIAN_POINT('Ctrl Pts',(22.,41.345292929857,-61.115492429943));
#184200=CARTESIAN_POINT('Ctrl Pts',(21.9999999999979,41.0241336396768,-60.969503986646));
#184201=CARTESIAN_POINT('Ctrl Pts',(22.3211558478618,40.913825471773,-60.9106181484486));
#184202=CARTESIAN_POINT('Ctrl Pts',(22.,41.1573899115079,-61.3627217630986));
#184203=CARTESIAN_POINT('Ctrl Pts',(22.,40.8698280768405,-61.1441646043173));
#184204=CARTESIAN_POINT('Ctrl Pts',(22.3428990418276,40.7794755973204,-61.0754935261973));
#184205=CARTESIAN_POINT('',(22.3089577584378,40.9899884313956,-60.5010370523947));
#184206=CARTESIAN_POINT('Origin',(22.5,41.4520521304013,-60.5010370523947));
#184207=CARTESIAN_POINT('Ctrl Pts',(22.3428990418276,40.7794755973204,-61.0754935261973));
#184208=CARTESIAN_POINT('Ctrl Pts',(22.3377419172472,40.8113411518324,-61.0363878307135));
#184209=CARTESIAN_POINT('Ctrl Pts',(22.3331666192763,40.8396559950365,-60.9954985853989));
#184210=CARTESIAN_POINT('Ctrl Pts',(22.3291795158032,40.8643584296857,-60.9533649602018));
#184211=CARTESIAN_POINT('Ctrl Pts',(22.3251648482087,40.8892316401655,-60.9109400517796));
#184212=CARTESIAN_POINT('Ctrl Pts',(22.3217465334641,40.9104423379139,-60.867253492917));
#184213=CARTESIAN_POINT('Ctrl Pts',(22.318927347672,40.9279527481794,-60.8228093460738));
#184214=CARTESIAN_POINT('Ctrl Pts',(22.3160956734992,40.9455407257593,-60.7781683213132));
#184215=CARTESIAN_POINT('Ctrl Pts',(22.3138684433435,40.9593955910944,-60.7327629502039));
#184216=CARTESIAN_POINT('Ctrl Pts',(22.3122447822525,40.9695040445439,-60.6870577134218));
#184217=CARTESIAN_POINT('Ctrl Pts',(22.3106095906062,40.9796842839609,-60.6410278973498));
#184218=CARTESIAN_POINT('Ctrl Pts',(22.309586567221,40.9860647363956,-60.5946939227373));
#184219=CARTESIAN_POINT('Ctrl Pts',(22.309171148035,40.9886566936033,-60.548483719008));
#184220=CARTESIAN_POINT('Ctrl Pts',(22.3090287948283,40.9895448890273,-60.5326487000593));
#184221=CARTESIAN_POINT('Ctrl Pts',(22.3089577584378,40.9899884313956,-60.5168278168827));
#184222=CARTESIAN_POINT('Ctrl Pts',(22.3089577584378,40.9899884313956,-60.5010370523947));
#184223=CARTESIAN_POINT('Origin',(0.,-12.9675000200281,-61.64995));
#184224=CARTESIAN_POINT('',(23.7057274034393,40.1924568448808,-61.0754935261973));
#184225=CARTESIAN_POINT('Origin',(0.,-12.9675000200281,-61.0754935261978));
#184226=CARTESIAN_POINT('',(25.572468850428,39.5210489290882,-60.8798615124594));
#184227=CARTESIAN_POINT('Ctrl Pts',(23.7057274034393,40.1924568448808,-61.0754935261973));
#184228=CARTESIAN_POINT('Ctrl Pts',(23.7856215193862,40.1568294998727,-61.0754935259541));
#184229=CARTESIAN_POINT('Ctrl Pts',(23.866734154227,40.1215775850188,-61.0739308915428));
#184230=CARTESIAN_POINT('Ctrl Pts',(23.9491177092649,40.08673029059,-61.0708731209178));
#184231=CARTESIAN_POINT('Ctrl Pts',(24.0222987307133,40.0557755618236,-61.0681569140535));
#184232=CARTESIAN_POINT('Ctrl Pts',(24.0964813835287,40.025140878248,-61.064260490718));
#184233=CARTESIAN_POINT('Ctrl Pts',(24.1716800708621,39.9948688249072,-61.0592331555073));
#184234=CARTESIAN_POINT('Ctrl Pts',(24.2654661289297,39.9571142223586,-61.0529631796778));
#184235=CARTESIAN_POINT('Ctrl Pts',(24.3608469638927,39.9199159378361,-61.0449325668214));
#184236=CARTESIAN_POINT('Ctrl Pts',(24.4578931367489,39.8833739107453,-61.0352435975212));
#184237=CARTESIAN_POINT('Ctrl Pts',(24.4948792676916,39.8694470534658,-61.03155094817));
#184238=CARTESIAN_POINT('Ctrl Pts',(24.5321075118773,39.8556158911211,-61.0276175607063));
#184239=CARTESIAN_POINT('Ctrl Pts',(24.5695823113615,39.8418876611333,-61.0234498250998));
#184240=CARTESIAN_POINT('Ctrl Pts',(24.5835560000295,39.8367686474373,-61.0218957503451));
#184241=CARTESIAN_POINT('Ctrl Pts',(24.5985392591505,39.8313093182609,-61.020197828724));
#184242=CARTESIAN_POINT('Ctrl Pts',(24.6125102748754,39.826246917928,-61.0185854547281));
#184243=CARTESIAN_POINT('Ctrl Pts',(24.618761985811,39.8239816092242,-61.0178639541342));
#184244=CARTESIAN_POINT('Ctrl Pts',(24.6248112932983,39.8217952378057,-61.0171600142893));
#184245=CARTESIAN_POINT('Ctrl Pts',(24.6304783782186,39.8197514190012,-61.0164960432401));
#184246=CARTESIAN_POINT('Ctrl Pts',(24.6384559079717,39.8168743445348,-61.0155613742039));
#184247=CARTESIAN_POINT('Ctrl Pts',(24.6464463947879,39.8140013804444,-61.0146162258341));
#184248=CARTESIAN_POINT('Ctrl Pts',(24.6544495579384,39.8111327371535,-61.0136606912691));
#184249=CARTESIAN_POINT('Ctrl Pts',(24.7320816974161,39.7833063750169,-61.0043918320403));
#184250=CARTESIAN_POINT('Ctrl Pts',(24.8111148007942,39.7557842793819,-60.9942079554682));
#184251=CARTESIAN_POINT('Ctrl Pts',(24.8915816511647,39.7286727517594,-60.9832055061413));
#184252=CARTESIAN_POINT('Ctrl Pts',(24.9702730942374,39.7021594084049,-60.9724458130394));
#184253=CARTESIAN_POINT('Ctrl Pts',(25.0503356257557,39.6760387443915,-60.9609030790891));
#184254=CARTESIAN_POINT('Ctrl Pts',(25.1318184288227,39.6504095486071,-60.94871246542));
#184255=CARTESIAN_POINT('Ctrl Pts',(25.2106570898813,39.6256120281047,-60.9369174409121));
#184256=CARTESIAN_POINT('Ctrl Pts',(25.2908253028013,39.6012746209597,-60.9245158192693));
#184257=CARTESIAN_POINT('Ctrl Pts',(25.3723860166305,39.5774858297392,-60.9116744369215));
#184258=CARTESIAN_POINT('Ctrl Pts',(25.4381601942134,39.558301493252,-60.9013185765654));
#184259=CARTESIAN_POINT('Ctrl Pts',(25.5048403019683,39.5394739391454,-60.8906774714747));
#184260=CARTESIAN_POINT('Ctrl Pts',(25.572468850428,39.5210489290882,-60.8798615124595));
#184261=CARTESIAN_POINT('Ctrl Pts',(25.572468850428,39.5210489290882,-60.8798615124595));
#184262=CARTESIAN_POINT('Ctrl Pts',(25.6431029505261,39.5018050733993,-60.8685648702497));
#184263=CARTESIAN_POINT('Ctrl Pts',(25.7138823092578,39.4824629375756,-60.857758843244));
#184264=CARTESIAN_POINT('Ctrl Pts',(25.7847107517024,39.4630487724035,-60.8474361505734));
#184265=CARTESIAN_POINT('Ctrl Pts',(25.8308068264298,39.4504137803346,-60.8407180074614));
#184266=CARTESIAN_POINT('Ctrl Pts',(25.8769227933553,39.4377485444914,-60.834204548861));
#184267=CARTESIAN_POINT('Ctrl Pts',(25.9230504277369,39.4250553877985,-60.8278902493107));
#184268=CARTESIAN_POINT('Ctrl Pts',(26.0189121987724,39.3986766563304,-60.8147679648959));
#184269=CARTESIAN_POINT('Ctrl Pts',(26.1148365047503,39.3721740320321,-60.802503877652));
#184270=CARTESIAN_POINT('Ctrl Pts',(26.2108418493022,39.3455428505808,-60.7910366361297));
#184271=CARTESIAN_POINT('Ctrl Pts',(26.3373732051069,39.3104439765394,-60.7759232523495));
#184272=CARTESIAN_POINT('Ctrl Pts',(26.4640345619824,39.2751247126816,-60.7621958302966));
#184273=CARTESIAN_POINT('Ctrl Pts',(26.5907640035296,39.2396032095401,-60.7497269836428));
#184274=CARTESIAN_POINT('Ctrl Pts',(26.7373460877471,39.1985171296091,-60.7353048453615));
#184275=CARTESIAN_POINT('Ctrl Pts',(26.8840228587755,39.1572049156071,-60.722550892655));
#184276=CARTESIAN_POINT('Ctrl Pts',(27.0306967963677,39.1155727408901,-60.7113062733474));
#184277=CARTESIAN_POINT('Ctrl Pts',(27.0336145588422,39.1147445583301,-60.7110825858348));
#184278=CARTESIAN_POINT('Ctrl Pts',(27.0365323211635,39.1139163090821,-60.710859474163));
#184279=CARTESIAN_POINT('Ctrl Pts',(27.0394500838819,39.1130879917084,-60.7106369372409));
#184280=CARTESIAN_POINT('Ctrl Pts',(27.0975646374211,39.0965899762741,-60.7062045569802));
#184281=CARTESIAN_POINT('Ctrl Pts',(27.1556813189417,39.0800646342817,-60.7020077089736));
#184282=CARTESIAN_POINT('Ctrl Pts',(27.2138073132673,39.063498894174,-60.6980512411089));
#184283=CARTESIAN_POINT('Ctrl Pts',(27.3964586715723,39.0114437858338,-60.6856186928498));
#184284=CARTESIAN_POINT('Ctrl Pts',(27.5792042711961,38.9589865331188,-60.6755585565127));
#184285=CARTESIAN_POINT('Ctrl Pts',(27.761941720716,38.906196118852,-60.6679131829684));
#184286=CARTESIAN_POINT('Ctrl Pts',(27.8960426829491,38.8674561377017,-60.6623026638788));
#184287=CARTESIAN_POINT('Ctrl Pts',(28.0301318919162,38.8285192033564,-60.6579982788021));
#184288=CARTESIAN_POINT('Ctrl Pts',(28.1641720722495,38.7893376413634,-60.65501386678));
#184289=CARTESIAN_POINT('Ctrl Pts',(28.2739136266319,38.7572588609145,-60.6525704650074));
#184290=CARTESIAN_POINT('Ctrl Pts',(28.3836422506653,38.7250861587992,-60.6510040856624));
#184291=CARTESIAN_POINT('Ctrl Pts',(28.493364741833,38.6927858841118,-60.6503273734803));
#184292=CARTESIAN_POINT('Origin',(24.2,-73.08000002,-55.74995));
#184293=CARTESIAN_POINT('',(24.2,-66.6526716808631,-55.24995));
#184294=CARTESIAN_POINT('',(24.2,-73.08000002,-55.24995));
#184295=CARTESIAN_POINT('',(23.7,-67.0923340267327,-55.74995));
#184296=CARTESIAN_POINT('Ctrl Pts',(24.2,-66.6526716808631,-55.24995));
#184297=CARTESIAN_POINT('Ctrl Pts',(24.1759721551885,-66.6743340439622,
-55.24995));
#184298=CARTESIAN_POINT('Ctrl Pts',(24.152826179152,-66.6949988683232,-55.2516491172883));
#184299=CARTESIAN_POINT('Ctrl Pts',(24.13068348082,-66.7146565642086,-55.2547374293595));
#184300=CARTESIAN_POINT('Ctrl Pts',(24.1180297981078,-66.7258901655909,
-55.2565022784524));
#184301=CARTESIAN_POINT('Ctrl Pts',(24.1057033057649,-66.7367955085337,
-55.2587201954649));
#184302=CARTESIAN_POINT('Ctrl Pts',(24.0937224210386,-66.7473756878393,
-55.2613292670619));
#184303=CARTESIAN_POINT('Ctrl Pts',(24.0772492946111,-66.7619229132994,
-55.2649166120082));
#184304=CARTESIAN_POINT('Ctrl Pts',(24.0614340950303,-66.775851731569,-55.2692432542138));
#184305=CARTESIAN_POINT('Ctrl Pts',(24.0463294237835,-66.7891621442409,
-55.274133644209));
#184306=CARTESIAN_POINT('Ctrl Pts',(24.0387770881601,-66.7958173505768,
-55.2765788392066));
#184307=CARTESIAN_POINT('Ctrl Pts',(24.0314022714302,-66.8023179571051,
-55.279164741744));
#184308=CARTESIAN_POINT('Ctrl Pts',(24.0242106428603,-66.8086639704726,
-55.2818681998208));
#184309=CARTESIAN_POINT('Ctrl Pts',(24.0213602322104,-66.811179220518,-55.2829397186873));
#184310=CARTESIAN_POINT('Ctrl Pts',(24.018539123137,-66.8136696853031,-55.2840294773983));
#184311=CARTESIAN_POINT('Ctrl Pts',(24.0157447324672,-66.8161379878207,
-55.2851371841595));
#184312=CARTESIAN_POINT('Ctrl Pts',(24.0114888338122,-66.8198972493579,
-55.2868242380731));
#184313=CARTESIAN_POINT('Ctrl Pts',(24.0073073500582,-66.8235941097571,
-55.2885480177634));
#184314=CARTESIAN_POINT('Ctrl Pts',(24.0031907212466,-66.8272382341148,
-55.2903085862464));
#184315=CARTESIAN_POINT('Ctrl Pts',(23.9829089320758,-66.8451920903692,
-55.2989825474966));
#184316=CARTESIAN_POINT('Ctrl Pts',(23.9642328599911,-66.86178060286,-55.3085399422178));
#184317=CARTESIAN_POINT('Ctrl Pts',(23.9471249453662,-66.8769984520897,
-55.318559493563));
#184318=CARTESIAN_POINT('Ctrl Pts',(23.9412233074604,-66.8822480829084,
-55.3220158916872));
#184319=CARTESIAN_POINT('Ctrl Pts',(23.9355078950893,-66.8873348856796,
-55.3255272894897));
#184320=CARTESIAN_POINT('Ctrl Pts',(23.9299760697225,-66.8922594645355,
-55.3290764557181));
#184321=CARTESIAN_POINT('Ctrl Pts',(23.919192213749,-66.9018595414706,-55.3359952745339));
#184322=CARTESIAN_POINT('Ctrl Pts',(23.9091037294454,-66.9108412221197,
-55.3430586687082));
#184323=CARTESIAN_POINT('Ctrl Pts',(23.8996731398199,-66.9192045149494,
-55.3501525154962));
#184324=CARTESIAN_POINT('Ctrl Pts',(23.8949578450071,-66.9233861613642,
-55.3536994388901));
#184325=CARTESIAN_POINT('Ctrl Pts',(23.8904068208279,-66.9274132107852,
-55.3572541745423));
#184326=CARTESIAN_POINT('Ctrl Pts',(23.8860143747022,-66.9312856634615,
-55.3608037660014));
#184327=CARTESIAN_POINT('Ctrl Pts',(23.8838181516394,-66.9332218897997,
-55.3625785617309));
#184328=CARTESIAN_POINT('Ctrl Pts',(23.8816615756776,-66.9351194669366,
-55.3643520766352));
#184329=CARTESIAN_POINT('Ctrl Pts',(23.8795438764403,-66.9369783948365,
-55.366122790075));
#184330=CARTESIAN_POINT('Ctrl Pts',(23.8784850268217,-66.9379078587864,
-55.3670081467949));
#184331=CARTESIAN_POINT('Ctrl Pts',(23.8774358966177,-66.9388276604262,
-55.3678928035676));
#184332=CARTESIAN_POINT('Ctrl Pts',(23.8763963890696,-66.939737799748,-55.3687765744431));
#184333=CARTESIAN_POINT('Ctrl Pts',(23.8755708968128,-66.9404605582929,
-55.3694783933149));
#184334=CARTESIAN_POINT('Ctrl Pts',(23.8752370420761,-66.9407532450194,
-55.3697629895785));
#184335=CARTESIAN_POINT('Ctrl Pts',(23.8742375999357,-66.9416259151707,
-55.3706224726781));
#184336=CARTESIAN_POINT('Ctrl Pts',(23.8739784867836,-66.9418521616982,
-55.3708453003597));
#184337=CARTESIAN_POINT('Ctrl Pts',(23.8736747333741,-66.9421173022114,
-55.3711069295282));
#184338=CARTESIAN_POINT('Ctrl Pts',(23.8733064912044,-66.9424386456662,
-55.3714251723656));
#184339=CARTESIAN_POINT('Ctrl Pts',(23.8669822397958,-66.9479574508522,
-55.3768907270425));
#184340=CARTESIAN_POINT('Ctrl Pts',(23.8608071175581,-66.9533361614165,
-55.3825025454305));
#184341=CARTESIAN_POINT('Ctrl Pts',(23.854778934738,-66.9585783373303,-55.3882561842759));
#184342=CARTESIAN_POINT('Ctrl Pts',(23.8379273040769,-66.9732327058185,
-55.4043403342882));
#184343=CARTESIAN_POINT('Ctrl Pts',(23.8224506346135,-66.9866238435088,
-55.4213586770294));
#184344=CARTESIAN_POINT('Ctrl Pts',(23.8083326526315,-66.9988025045773,
-55.4391491120011));
#184345=CARTESIAN_POINT('Ctrl Pts',(23.793908545267,-67.0112452400215,-55.4573253035009));
#184346=CARTESIAN_POINT('Ctrl Pts',(23.780902068212,-67.0224228512157,-55.4763077982106));
#184347=CARTESIAN_POINT('Ctrl Pts',(23.7693045786636,-67.0323770023654,
-55.4959754807223));
#184348=CARTESIAN_POINT('Ctrl Pts',(23.7647881472762,-67.0362534654999,
-55.5036347019911));
#184349=CARTESIAN_POINT('Ctrl Pts',(23.7604855416912,-67.0399442097422,
-55.5113983533584));
#184350=CARTESIAN_POINT('Ctrl Pts',(23.7563969204059,-67.0434509476726,
-55.5192611609635));
#184351=CARTESIAN_POINT('Ctrl Pts',(23.7510293947303,-67.0480545792065,
-55.5295834233493));
#184352=CARTESIAN_POINT('Ctrl Pts',(23.7460378255205,-67.0523366189893,
-55.5400629061549));
#184353=CARTESIAN_POINT('Ctrl Pts',(23.7414232710247,-67.0562986848684,
-55.5506824062784));
#184354=CARTESIAN_POINT('Ctrl Pts',(23.7308438701964,-67.0653821799449,
-55.5750288406965));
#184355=CARTESIAN_POINT('Ctrl Pts',(23.7223346138157,-67.07270992344,-55.5998560569635));
#184356=CARTESIAN_POINT('Ctrl Pts',(23.7158399969348,-67.0783500466653,
-55.6249940165964));
#184357=CARTESIAN_POINT('Ctrl Pts',(23.7151405459333,-67.078957471231,-55.6277013003919));
#184358=CARTESIAN_POINT('Ctrl Pts',(23.7144644807411,-67.0795453050864,
-55.630412231224));
#184359=CARTESIAN_POINT('Ctrl Pts',(23.7138117462416,-67.0801136209466,
-55.6331266267316));
#184360=CARTESIAN_POINT('Ctrl Pts',(23.7090188656243,-67.0842866347413,
-55.6530578141074));
#184361=CARTESIAN_POINT('Ctrl Pts',(23.705503143361,-67.0873988103307,-55.6731086055997));
#184362=CARTESIAN_POINT('Ctrl Pts',(23.7032227806793,-67.089434092737,-55.6931075567179));
#184363=CARTESIAN_POINT('Ctrl Pts',(23.7010511586342,-67.0913723213252,
-55.712152844327));
#184364=CARTESIAN_POINT('Ctrl Pts',(23.7,-67.0923340254841,-55.7311508771076));
#184365=CARTESIAN_POINT('Ctrl Pts',(23.7,-67.0923340267327,-55.74995));
#184366=CARTESIAN_POINT('',(23.7,67.7009572055632,-55.74995));
#184367=CARTESIAN_POINT('Origin',(23.7,67.7009572055632,-55.24995));
#184368=CARTESIAN_POINT('',(23.7,-67.0923340267327,-60.42825533736));
#184369=CARTESIAN_POINT('',(23.7,-67.0923340267327,-55.24995));
#184370=CARTESIAN_POINT('Origin',(23.7000000338415,-65.5006105042907,-60.4353544159677));
#184371=CARTESIAN_POINT('',(23.7,-67.2147119299503,-176.84995));
#184372=CARTESIAN_POINT('Ctrl Pts',(23.6999999991391,-67.091907941908,-60.3927543614583));
#184373=CARTESIAN_POINT('Ctrl Pts',(23.7000444961003,-66.3339120499587,
-60.4123961703813));
#184374=CARTESIAN_POINT('Ctrl Pts',(23.0030676793154,-66.6324461755816,
-60.4045898193842));
#184375=CARTESIAN_POINT('Ctrl Pts',(23.6999999991382,-67.0981649919348,
-60.6366434264883));
#184376=CARTESIAN_POINT('Ctrl Pts',(23.7000445996745,-66.3350862497407,
-60.5213661743368));
#184377=CARTESIAN_POINT('Ctrl Pts',(23.0023333098335,-66.6369323384171,
-60.5671687383292));
#184378=CARTESIAN_POINT('Ctrl Pts',(23.6999999991466,-67.0398545336994,
-60.8767984170649));
#184379=CARTESIAN_POINT('Ctrl Pts',(23.7000436587852,-66.3247262225054,
-60.6279370962731));
#184380=CARTESIAN_POINT('Ctrl Pts',(23.0091746715062,-66.5951265090932,
-60.7272889592882));
#184381=CARTESIAN_POINT('Ctrl Pts',(23.6999999991637,-66.9227827756908,
-61.0939974638106));
#184382=CARTESIAN_POINT('Ctrl Pts',(23.7000418676227,-66.2856006592058,
-60.7504731406958));
#184383=CARTESIAN_POINT('Ctrl Pts',(23.0230090051523,-66.5111384208581,
-60.8720725995973));
#184384=CARTESIAN_POINT('',(23.0030142220336,-66.6327727106072,-60.42825533736));
#184385=CARTESIAN_POINT('Origin',(23.2,-67.0923340267327,-60.42825533736));
#184386=CARTESIAN_POINT('Origin',(23.2063851675584,-65.3975925798871,-60.4139429821593));
#184387=CARTESIAN_POINT('Origin',(0.,-12.9675000200281,-60.64995));
#184388=CARTESIAN_POINT('Origin',(0.,-12.9675000200281,-60.8508735991007));
#184389=CARTESIAN_POINT('Origin',(17.05,67.7009572055632,-55.24995));
#184390=CARTESIAN_POINT('',(17.05,-69.2968662511513,-171.871644662643));
#184391=CARTESIAN_POINT('',(17.05,-69.1790215814778,-60.42825533736));
#184392=CARTESIAN_POINT('Origin',(17.0499997344964,-67.70076355866,-60.4478804501376));
#184393=CARTESIAN_POINT('',(17.05,-69.1790215814778,-55.74995));
#184394=CARTESIAN_POINT('',(17.05,-69.1790215814778,-55.24995));
#184395=CARTESIAN_POINT('',(17.05,67.7009572055632,-55.74995));
#184396=CARTESIAN_POINT('Ctrl Pts',(17.0500000072448,-69.0016232241721,
-61.1207587448991));
#184397=CARTESIAN_POINT('Ctrl Pts',(17.0499351254479,-68.6669792326861,
-60.9382791396779));
#184398=CARTESIAN_POINT('Ctrl Pts',(17.4174322081753,-68.5782862263167,
-60.8898940315426));
#184399=CARTESIAN_POINT('Ctrl Pts',(17.0500000070135,-69.1279231312628,
-60.8888915170785));
#184400=CARTESIAN_POINT('Ctrl Pts',(17.0499377736316,-68.768366090799,-60.7724682610327));
#184401=CARTESIAN_POINT('Ctrl Pts',(17.4057007122192,-68.6661491518679,
-60.7353408116852));
#184402=CARTESIAN_POINT('Ctrl Pts',(17.0500000069009,-69.1898773189587,
-60.6289947788348));
#184403=CARTESIAN_POINT('Ctrl Pts',(17.0499390370914,-68.8203021885316,
-60.5773600099809));
#184404=CARTESIAN_POINT('Ctrl Pts',(17.3999941136478,-68.7092345420341,
-60.5620638496915));
#184405=CARTESIAN_POINT('Ctrl Pts',(17.0500000069233,-69.1775691162164,
-60.3615671969807));
#184406=CARTESIAN_POINT('Ctrl Pts',(17.0499387884128,-68.8100686727309,
-60.3786737910309));
#184407=CARTESIAN_POINT('Ctrl Pts',(17.4011286297274,-68.7006746954154,
-60.3838015812945));
#184408=CARTESIAN_POINT('',(17.4009870515814,-68.7017426890012,-60.42825533736));
#184409=CARTESIAN_POINT('Origin',(17.5775644535055,-67.3782391193926,-60.380625282891));
#184410=CARTESIAN_POINT('Origin',(17.55,-69.1790215814778,-60.42825533736));
#184411=CARTESIAN_POINT('Origin',(16.55,67.7009572055632,-55.74995));
#184412=CARTESIAN_POINT('',(16.55,-69.4815262104643,-55.24995));
#184413=CARTESIAN_POINT('Ctrl Pts',(17.05,-69.1790215814778,-55.74995));
#184414=CARTESIAN_POINT('Ctrl Pts',(17.05,-69.1790215814778,-55.6863354647393));
#184415=CARTESIAN_POINT('Ctrl Pts',(17.0376836641811,-69.1872430679557,
-55.62011998619));
#184416=CARTESIAN_POINT('Ctrl Pts',(16.9980239220187,-69.2119075273894,
-55.5253450968975));
#184417=CARTESIAN_POINT('Ctrl Pts',(16.9813062406437,-69.2221843854867,
-55.4945430062267));
#184418=CARTESIAN_POINT('Ctrl Pts',(16.9510291215394,-69.2406827300619,
-55.4508010486414));
#184419=CARTESIAN_POINT('Ctrl Pts',(16.9400731279519,-69.2473626878252,
-55.4366317733573));
#184420=CARTESIAN_POINT('Ctrl Pts',(16.9223801176293,-69.2581533888275,
-55.4161620627276));
#184421=CARTESIAN_POINT('Ctrl Pts',(16.9132191956801,-69.2637414304179,
-55.4061233109409));
#184422=CARTESIAN_POINT('Ctrl Pts',(16.9019928706252,-69.2705980216798,
-55.3947915321209));
#184423=CARTESIAN_POINT('Ctrl Pts',(16.8970676687462,-69.2736088199504,
-55.3900204673471));
#184424=CARTESIAN_POINT('Ctrl Pts',(16.8937590578697,-69.2756320763883,
-55.3868591776192));
#184425=CARTESIAN_POINT('Ctrl Pts',(16.8912710328977,-69.2771542353966,
-55.3845249666426));
#184426=CARTESIAN_POINT('Ctrl Pts',(16.8629500306956,-69.2944853013176,
-55.3581999174045));
#184427=CARTESIAN_POINT('Ctrl Pts',(16.8233316225938,-69.3198754749745,
-55.3266480832757));
#184428=CARTESIAN_POINT('Ctrl Pts',(16.7108981077624,-69.3878244053918,
-55.2724497512768));
#184429=CARTESIAN_POINT('Ctrl Pts',(16.6373202287544,-69.4303831621522,
-55.24995));
#184430=CARTESIAN_POINT('Ctrl Pts',(16.55,-69.4815262104643,-55.24995));
#184431=CARTESIAN_POINT('',(16.55,-73.08000002,-55.24995));
#184432=CARTESIAN_POINT('Origin',(41.5,-73.08000002,-55.24995));
#184433=CARTESIAN_POINT('',(16.05,-69.6255546658886,-55.24995));
#184434=CARTESIAN_POINT('Origin',(0.,-12.9675000200281,-55.24995));
#184435=CARTESIAN_POINT('',(16.05,-73.08000002,-55.24995));
#184436=CARTESIAN_POINT('Origin',(16.05,-73.08000002,-55.74995));
#184437=CARTESIAN_POINT('',(15.55,-69.8993466109593,-55.74995));
#184438=CARTESIAN_POINT('Ctrl Pts',(16.05,-69.6255546658886,-55.24995));
#184439=CARTESIAN_POINT('Ctrl Pts',(16.0288722037061,-69.6375247602604,
-55.24995));
#184440=CARTESIAN_POINT('Ctrl Pts',(16.0083301026716,-69.6490223109434,
-55.2512895581316));
#184441=CARTESIAN_POINT('Ctrl Pts',(15.9885162403179,-69.6600473179374,
-55.2537446520891));
#184442=CARTESIAN_POINT('Ctrl Pts',(15.9681617141798,-69.6713731659234,
-55.2562667385575));
#184443=CARTESIAN_POINT('Ctrl Pts',(15.9485754876161,-69.6822003296312,
-55.2599653874695));
#184444=CARTESIAN_POINT('Ctrl Pts',(15.9298569819113,-69.6925288090609,
-55.2645989361251));
#184445=CARTESIAN_POINT('Ctrl Pts',(15.9103217854581,-69.7033079213419,
-55.2694346470888));
#184446=CARTESIAN_POINT('Ctrl Pts',(15.8917314336212,-69.7135438847403,
-55.2752879340727));
#184447=CARTESIAN_POINT('Ctrl Pts',(15.8741431710191,-69.7232366992563,
-55.2818961829012));
#184448=CARTESIAN_POINT('Ctrl Pts',(15.8560955088269,-69.7331826868751,
-55.2886770369989));
#184449=CARTESIAN_POINT('Ctrl Pts',(15.8391024265034,-69.7425567813175,
-55.2962522526717));
#184450=CARTESIAN_POINT('Ctrl Pts',(15.8231746650905,-69.7513589825835,
-55.3043602027165));
#184451=CARTESIAN_POINT('Ctrl Pts',(15.8066197703906,-69.7605077581903,
-55.3127873919331));
#184452=CARTESIAN_POINT('Ctrl Pts',(15.7912151617321,-69.7690387190412,
-55.321789591021));
#184453=CARTESIAN_POINT('Ctrl Pts',(15.7769270004145,-69.776951865136,-55.3311049965711));
#184454=CARTESIAN_POINT('Ctrl Pts',(15.7738353234149,-69.7786641142653,
-55.3331206670581));
#184455=CARTESIAN_POINT('Ctrl Pts',(15.7707957734989,-69.7803474370327,
-55.3351511317179));
#184456=CARTESIAN_POINT('Ctrl Pts',(15.7678077818739,-69.782001833438,-55.3371939557934));
#184457=CARTESIAN_POINT('Ctrl Pts',(15.756555490458,-69.7882320217404,-55.3448868996478));
#184458=CARTESIAN_POINT('Ctrl Pts',(15.7460352862097,-69.7940519898752,
-55.3527538808861));
#184459=CARTESIAN_POINT('Ctrl Pts',(15.7362087545715,-69.7994617378423,
-55.3606749631784));
#184460=CARTESIAN_POINT('Ctrl Pts',(15.7312954887525,-69.8021666118259,
-55.3646355043245));
#184461=CARTESIAN_POINT('Ctrl Pts',(15.7265554551632,-69.8047689307675,
-55.3686098210218));
#184462=CARTESIAN_POINT('Ctrl Pts',(15.721982899875,-69.8072686946673,-55.3725844185997));
#184463=CARTESIAN_POINT('Ctrl Pts',(15.719696622231,-69.8085185766171,-55.3745717173886));
#184464=CARTESIAN_POINT('Ctrl Pts',(15.7174522181041,-69.8097428198065,
-55.3765590908577));
#184465=CARTESIAN_POINT('Ctrl Pts',(15.7152489034228,-69.8109414242354,
-55.3785449605345));
#184466=CARTESIAN_POINT('Ctrl Pts',(15.7139033590177,-69.8116734011504,
-55.3797577132364));
#184467=CARTESIAN_POINT('Ctrl Pts',(15.7130061596117,-69.812164167094,-55.3805748440141));
#184468=CARTESIAN_POINT('Ctrl Pts',(15.7117619226199,-69.8128381202302,
-55.3817177322528));
#184469=CARTESIAN_POINT('Ctrl Pts',(15.7109687347443,-69.813267758201,-55.382446311374));
#184470=CARTESIAN_POINT('Ctrl Pts',(15.7100347608739,-69.8137718421128,
-55.383307570602));
#184471=CARTESIAN_POINT('Ctrl Pts',(15.7087614611218,-69.8144603212408,
-55.3844965014748));
#184472=CARTESIAN_POINT('Ctrl Pts',(15.6900035624944,-69.8246028047116,
-55.4020115011831));
#184473=CARTESIAN_POINT('Ctrl Pts',(15.6727531453279,-69.8338363960813,
-55.4208270616741));
#184474=CARTESIAN_POINT('Ctrl Pts',(15.6571396559972,-69.84216109535,-55.4406592789784));
#184475=CARTESIAN_POINT('Ctrl Pts',(15.6413283311722,-69.8505912752681,
-55.460742786461));
#184476=CARTESIAN_POINT('Ctrl Pts',(15.6271956225887,-69.8580893843722,
-55.4818682723947));
#184477=CARTESIAN_POINT('Ctrl Pts',(15.6148225747989,-69.8646554226621,
-55.5037374727083));
#184478=CARTESIAN_POINT('Ctrl Pts',(15.6022021547712,-69.8713527346377,
-55.5260439002204));
#184479=CARTESIAN_POINT('Ctrl Pts',(15.5914123584404,-69.8770803337719,
-55.5491234737585));
#184480=CARTESIAN_POINT('Ctrl Pts',(15.5824851075871,-69.8818382200647,
-55.5726654113518));
#184481=CARTESIAN_POINT('Ctrl Pts',(15.573457165996,-69.8866497707038,-55.5964728791855));
#184482=CARTESIAN_POINT('Ctrl Pts',(15.5663337420152,-69.890469610296,-55.6207526467196));
#184483=CARTESIAN_POINT('Ctrl Pts',(15.5610961173292,-69.8932977388412,
-55.6451979426959));
#184484=CARTESIAN_POINT('Ctrl Pts',(15.5557670007162,-69.8961752697293,
-55.6700702542321));
#184485=CARTESIAN_POINT('Ctrl Pts',(15.5523898151382,-69.898026140128,-55.6951134072476));
#184486=CARTESIAN_POINT('Ctrl Pts',(15.5508961531647,-69.8988503500373,
-55.7200275991231));
#184487=CARTESIAN_POINT('Ctrl Pts',(15.5502965922522,-69.899181190652,-55.7300282390814));
#184488=CARTESIAN_POINT('Ctrl Pts',(15.55,-69.8993466109593,-55.7400084027481));
#184489=CARTESIAN_POINT('Ctrl Pts',(15.55,-69.8993466109593,-55.74995));
#184490=CARTESIAN_POINT('',(15.55,67.7009572055632,-55.74995));
#184491=CARTESIAN_POINT('Origin',(15.55,67.7009572055632,-55.24995));
#184492=CARTESIAN_POINT('',(15.55,-69.8993466109592,-60.4282553373601));
#184493=CARTESIAN_POINT('',(15.55,-69.8993466109593,-55.24995));
#184494=CARTESIAN_POINT('Origin',(15.5500003881169,-68.4591876509329,-60.4515855208539));
#184495=CARTESIAN_POINT('',(15.55,-70.015703322148,-176.84995));
#184496=CARTESIAN_POINT('Ctrl Pts',(15.5499999897346,-69.8979710840162,
-60.3623910423524));
#184497=CARTESIAN_POINT('Ctrl Pts',(15.5501315664229,-69.2493490991427,
-60.3919718313354));
#184498=CARTESIAN_POINT('Ctrl Pts',(14.9223321947707,-69.4149357692034,
-60.3843514923986));
#184499=CARTESIAN_POINT('Ctrl Pts',(15.5499999897191,-69.909794297014,-60.6262209796107));
#184500=CARTESIAN_POINT('Ctrl Pts',(15.5501319338923,-69.254225424885,-60.5374367820963));
#184501=CARTESIAN_POINT('Ctrl Pts',(14.9213859066283,-69.4230681799894,
-60.5602124639497));
#184502=CARTESIAN_POINT('Ctrl Pts',(15.5499999897966,-69.8505276805174,
-60.8861498986541));
#184503=CARTESIAN_POINT('Ctrl Pts',(15.5501300981793,-69.2303831032415,
-60.678769908775));
#184504=CARTESIAN_POINT('Ctrl Pts',(14.9261257169452,-69.3823033916894,
-60.7335097961699));
#184505=CARTESIAN_POINT('Ctrl Pts',(15.5499999899638,-69.7237798948102,
-61.1215831761309));
#184506=CARTESIAN_POINT('Ctrl Pts',(15.5501262723864,-69.1690548338264,
-60.822436019398));
#184507=CARTESIAN_POINT('Ctrl Pts',(14.9363515075123,-69.2951068303029,
-60.89043888838));
#184508=CARTESIAN_POINT('',(15.05,-69.3993466109593,-60.4282553373601));
#184509=CARTESIAN_POINT('Origin',(15.05,-69.8993466109592,-60.4282553373601));
#184510=CARTESIAN_POINT('',(14.9222139673106,-69.4159516070034,-60.4282553373601));
#184511=CARTESIAN_POINT('Origin',(15.05,-69.8993466109592,-60.4282553373601));
#184512=CARTESIAN_POINT('Origin',(15.0817285037655,-68.054728362522,-60.3659193157066));
#184513=CARTESIAN_POINT('Origin',(0.,-12.9675000200281,-60.64995));
#184514=CARTESIAN_POINT('Origin',(0.,-12.9675000200281,-60.8508735991007));
#184515=CARTESIAN_POINT('Origin',(8.9,67.7009572055632,-55.24995));
#184516=CARTESIAN_POINT('',(8.9,-71.2138732976838,-171.871644662643));
#184517=CARTESIAN_POINT('',(8.9,-71.0999148696911,-60.4282553373601));
#184518=CARTESIAN_POINT('Origin',(8.89999938777026,-69.7158521501157,-60.4580628686921));
#184519=CARTESIAN_POINT('',(8.89999999157093,-71.0999148696892,-55.8925850873042));
#184520=CARTESIAN_POINT('',(8.9,-71.0999148696911,-55.24995));
#184521=CARTESIAN_POINT('Ctrl Pts',(8.89999996628377,-71.0999148696861,
-55.8925850873112));
#184522=CARTESIAN_POINT('Ctrl Pts',(8.89999995709263,-71.1271912455156,
-55.9047800168435));
#184523=CARTESIAN_POINT('Ctrl Pts',(8.89999995405378,-71.1542893399126,
-55.9174976277303));
#184524=CARTESIAN_POINT('Ctrl Pts',(8.89999995711454,-71.1811814737311,
-55.9307199810309));
#184525=CARTESIAN_POINT('Ctrl Pts',(8.89999996594249,-71.2587447432654,
-55.9688563728791));
#184526=CARTESIAN_POINT('Ctrl Pts',(8.89999997989509,-71.334738576959,-56.0111644614647));
#184527=CARTESIAN_POINT('Ctrl Pts',(8.89999998822403,-71.4082909897899,
-56.0572656901885));
#184528=CARTESIAN_POINT('Ctrl Pts',(8.89999999429182,-71.4618752880493,
-56.0908512911903));
#184529=CARTESIAN_POINT('Ctrl Pts',(8.89999999762151,-71.5141639062427,
-56.1264488763495));
#184530=CARTESIAN_POINT('Ctrl Pts',(8.89999999894661,-71.5648287885728,
-56.1638971934456));
#184531=CARTESIAN_POINT('Ctrl Pts',(8.90000000021705,-71.6134037334432,
-56.1998007592839));
#184532=CARTESIAN_POINT('Ctrl Pts',(8.9,-71.6605183672425,-56.2373236964706));
#184533=CARTESIAN_POINT('Ctrl Pts',(8.9,-71.7061534805117,-56.276424902386));
#184534=CARTESIAN_POINT('Ctrl Pts',(8.9,-71.7586958576709,-56.3214444095464));
#184535=CARTESIAN_POINT('Ctrl Pts',(8.90000000000525,-71.8093442969672,
-56.3686312342461));
#184536=CARTESIAN_POINT('Ctrl Pts',(8.89999999994877,-71.8580831316161,
-56.4179650024181));
#184537=CARTESIAN_POINT('Ctrl Pts',(8.89999999986101,-71.9338178277761,
-56.4946241587122));
#184538=CARTESIAN_POINT('Ctrl Pts',(8.89999999955086,-72.0053843762005,
-56.5771518376463));
#184539=CARTESIAN_POINT('Ctrl Pts',(8.89999999953632,-72.0709679837606,
-56.6635131964722));
#184540=CARTESIAN_POINT('Ctrl Pts',(8.89999999953336,-72.0842871673865,
-56.6810520730174));
#184541=CARTESIAN_POINT('Ctrl Pts',(8.89999999954423,-72.0973597365653,
-56.6987489820034));
#184542=CARTESIAN_POINT('Ctrl Pts',(8.89999999957055,-72.1101707466964,
-56.7165867802331));
#184543=CARTESIAN_POINT('Ctrl Pts',(8.89999999961887,-72.1337005884473,
-56.7493492685329));
#184544=CARTESIAN_POINT('Ctrl Pts',(8.89999999972697,-72.1563957720432,
-56.7826109127347));
#184545=CARTESIAN_POINT('Ctrl Pts',(8.89999999983668,-72.1782434639423,
-56.8163461536645));
#184546=CARTESIAN_POINT('Ctrl Pts',(8.90000000003969,-72.2186712712155,
-56.8787711377284));
#184547=CARTESIAN_POINT('Ctrl Pts',(8.89999999999795,-72.2562052259125,
-56.9428012878312));
#184548=CARTESIAN_POINT('Ctrl Pts',(8.89999999999952,-72.2908444043654,
-57.0084360093222));
#184549=CARTESIAN_POINT('Ctrl Pts',(8.90000000000048,-72.3119017301615,
-57.0483356771464));
#184550=CARTESIAN_POINT('Ctrl Pts',(8.9,-72.3318884210686,-57.0888288165431));
#184551=CARTESIAN_POINT('Ctrl Pts',(8.9,-72.3507957900478,-57.1299193914404));
#184552=CARTESIAN_POINT('Ctrl Pts',(8.9,-72.3746230901592,-57.1817022418682));
#184553=CARTESIAN_POINT('Ctrl Pts',(8.89999999998365,-72.3967864402965,
-57.2345342704725));
#184554=CARTESIAN_POINT('Ctrl Pts',(8.89999999972024,-72.4171503424455,
-57.288197632296));
#184555=CARTESIAN_POINT('Ctrl Pts',(8.89999999952357,-72.4323543754486,
-57.3282636038496));
#184556=CARTESIAN_POINT('Ctrl Pts',(8.89999999921991,-72.4465562092313,
-57.3687924002643));
#184557=CARTESIAN_POINT('Ctrl Pts',(8.89999999918092,-72.4597162071225,
-57.4096844656319));
#184558=CARTESIAN_POINT('Ctrl Pts',(8.89999999916252,-72.4659246935418,
-57.428976097332));
#184559=CARTESIAN_POINT('Ctrl Pts',(8.89999999920801,-72.4718879323416,
-57.4482939264422));
#184560=CARTESIAN_POINT('Ctrl Pts',(8.89999999932168,-72.4776042453442,
-57.4676297862024));
#184561=CARTESIAN_POINT('Ctrl Pts',(8.90000000038932,-72.5312977767249,
-57.649252204767));
#184562=CARTESIAN_POINT('Ctrl Pts',(8.89999999999947,-72.5639591690373,
-57.8344657871011));
#184563=CARTESIAN_POINT('Ctrl Pts',(8.89999999999994,-72.5753897578169,
-58.0232925566211));
#184564=CARTESIAN_POINT('Ctrl Pts',(8.90000000000006,-72.5784617700065,
-58.0740404357435));
#184565=CARTESIAN_POINT('Ctrl Pts',(8.9,-72.58000002,-58.1250492743389));
#184566=CARTESIAN_POINT('Ctrl Pts',(8.9,-72.58000002,-58.1763194612681));
#184567=CARTESIAN_POINT('Ctrl Pts',(8.90000001675659,-70.928272917477,-61.1211126854555));
#184568=CARTESIAN_POINT('Ctrl Pts',(8.89988778396233,-70.5448235085214,
-60.918842206156));
#184569=CARTESIAN_POINT('Ctrl Pts',(9.32900358361251,-70.4903946571405,
-60.8901185898342));
#184570=CARTESIAN_POINT('Ctrl Pts',(8.90000001650961,-71.0511602413471,
-60.887714756578));
#184571=CARTESIAN_POINT('Ctrl Pts',(8.89989004681885,-70.6365947859941,
-60.7567344379851));
#184572=CARTESIAN_POINT('Ctrl Pts',(9.32267960676822,-70.5733355012344,
-60.7345408641471));
#184573=CARTESIAN_POINT('Ctrl Pts',(8.9000000163917,-71.110350340576,-60.6286014156989));
#184574=CARTESIAN_POINT('Ctrl Pts',(8.89989111303313,-70.682184857852,-60.5709595618158));
#184575=CARTESIAN_POINT('Ctrl Pts',(9.31966069353146,-70.6132825269153,
-60.5618033393074));
#184576=CARTESIAN_POINT('Ctrl Pts',(8.90000001641518,-71.0985729052349,
-60.3617033877878));
#184577=CARTESIAN_POINT('Ctrl Pts',(8.89989090319397,-70.6731622220975,
-60.3808238190959));
#184578=CARTESIAN_POINT('Ctrl Pts',(9.32026185019719,-70.6053339699646,
-60.3838922942772));
#184579=CARTESIAN_POINT('',(9.32018679685842,-70.6063261212332,-60.4282553373601));
#184580=CARTESIAN_POINT('Origin',(9.42949994728011,-69.1714755465159,-60.3396721918004));
#184581=CARTESIAN_POINT('Origin',(9.4,-71.0999148696911,-60.4282553373601));
#184582=CARTESIAN_POINT('Ctrl Pts',(8.9,-72.58000002,-58.1763194612681));
#184583=CARTESIAN_POINT('Ctrl Pts',(8.89999999999996,-73.0800000199999,
-58.1763194612681));
#184584=CARTESIAN_POINT('Ctrl Pts',(8.4,-73.08000002,-58.1763194612681));
#184585=CARTESIAN_POINT('Ctrl Pts',(8.9,-72.5800000128814,-57.9140108579591));
#184586=CARTESIAN_POINT('Ctrl Pts',(8.89999999999996,-73.0782816065607,
-57.8621442504892));
#184587=CARTESIAN_POINT('Ctrl Pts',(8.40172135040051,-73.08000002,-57.8616056776356));
#184588=CARTESIAN_POINT('Ctrl Pts',(8.9,-72.5397349720259,-57.6584337450815));
#184589=CARTESIAN_POINT('Ctrl Pts',(8.89999999999997,-73.0284577192567,
-57.5559934180811));
#184590=CARTESIAN_POINT('Ctrl Pts',(8.40340362484077,-73.0316819589995,
-57.5549684855522));
#184591=CARTESIAN_POINT('Ctrl Pts',(8.9,-72.3796429547841,-57.1609527205255));
#184592=CARTESIAN_POINT('Ctrl Pts',(8.89999999999997,-72.8336034512039,
-56.9611013895289));
#184593=CARTESIAN_POINT('Ctrl Pts',(8.40668695336401,-72.8395715451724,
-56.9580994114807));
#184594=CARTESIAN_POINT('Ctrl Pts',(8.9,-72.262073445265,-56.9281157265161));
#184595=CARTESIAN_POINT('Ctrl Pts',(8.89999999999995,-72.6915892789857,
-56.6830185073362));
#184596=CARTESIAN_POINT('Ctrl Pts',(8.40822820346396,-72.6984881279278,
-56.6787458682451));
#184597=CARTESIAN_POINT('Ctrl Pts',(8.9,-72.0341941498609,-56.6108404408522));
#184598=CARTESIAN_POINT('Ctrl Pts',(8.89999999999996,-72.4171612181699,
-56.3044762227344));
#184599=CARTESIAN_POINT('Ctrl Pts',(8.41033280652841,-72.4250329770282,
-56.2980850295082));
#184600=CARTESIAN_POINT('Ctrl Pts',(8.9,-71.9491494655935,-56.5101636182542));
#184601=CARTESIAN_POINT('Ctrl Pts',(8.9000000000003,-72.3149747479787,-56.1845060329552));
#184602=CARTESIAN_POINT('Ctrl Pts',(8.41100144942456,-72.322979355276,-56.1772949390326));
#184603=CARTESIAN_POINT('Ctrl Pts',(8.9,-71.7670066137261,-56.3257764465383));
#184604=CARTESIAN_POINT('Ctrl Pts',(8.89999999999963,-72.0963975739119,
-55.9649406347444));
#184605=CARTESIAN_POINT('Ctrl Pts',(8.41222718544652,-72.1044079319076,
-55.9560708595913));
#184606=CARTESIAN_POINT('Ctrl Pts',(8.9,-71.6692649365715,-56.2410779083558));
#184607=CARTESIAN_POINT('Ctrl Pts',(8.89999999999951,-71.9792314944188,
-55.8641264120645));
#184608=CARTESIAN_POINT('Ctrl Pts',(8.41279083164671,-71.9871179192065,
-55.8544512596825));
#184609=CARTESIAN_POINT('Ctrl Pts',(8.9,-71.3558986429072,-56.0096140831459));
#184610=CARTESIAN_POINT('Ctrl Pts',(8.90000000000086,-71.6041352856071,
-55.588933048404));
#184611=CARTESIAN_POINT('Ctrl Pts',(8.41433230457371,-71.6110783688472,
-55.5767456783554));
#184612=CARTESIAN_POINT('Ctrl Pts',(8.9,-71.1195373961099,-55.8869904035305));
#184613=CARTESIAN_POINT('Ctrl Pts',(8.89999999999818,-71.3214288330036,
-55.443108937543));
#184614=CARTESIAN_POINT('Ctrl Pts',(8.41515058995443,-71.3274449382984,
-55.429624391176));
#184615=CARTESIAN_POINT('Ctrl Pts',(8.9,-70.8760630000525,-55.8051600336001));
#184616=CARTESIAN_POINT('Ctrl Pts',(8.89999999999995,-71.0304294360218,
-55.3458650785795));
#184617=CARTESIAN_POINT('Ctrl Pts',(8.41569693570581,-71.0352755960629,
-55.3314460318215));
#184618=CARTESIAN_POINT('',(8.41560828703704,-71.0814003738044,-55.3473768767704));
#184619=CARTESIAN_POINT('Ctrl Pts',(8.9,-71.0999148696911,-55.8925850873));
#184620=CARTESIAN_POINT('Ctrl Pts',(8.9,-71.0917569396884,-55.8670436478413));
#184621=CARTESIAN_POINT('Ctrl Pts',(8.89879514641371,-71.0842969126188,
-55.8417769940206));
#184622=CARTESIAN_POINT('Ctrl Pts',(8.89633575766726,-71.0775620353416,
-55.8169812460787));
#184623=CARTESIAN_POINT('Ctrl Pts',(8.89546270726179,-71.0751712431799,
-55.8081790842302));
#184624=CARTESIAN_POINT('Ctrl Pts',(8.8944319555344,-71.0728715932264,-55.7994361429263));
#184625=CARTESIAN_POINT('Ctrl Pts',(8.89324259912972,-71.0706635285073,
-55.7907607345806));
#184626=CARTESIAN_POINT('Ctrl Pts',(8.89097270851189,-71.0664494297141,
-55.7742036891632));
#184627=CARTESIAN_POINT('Ctrl Pts',(8.88812453435926,-71.062569970447,-55.7578953071278));
#184628=CARTESIAN_POINT('Ctrl Pts',(8.88470313888677,-71.0590262147759,
-55.7419018510144));
#184629=CARTESIAN_POINT('Ctrl Pts',(8.88325156030962,-71.057522723041,-55.7351163862952));
#184630=CARTESIAN_POINT('Ctrl Pts',(8.88176022108365,-71.0561390037238,
-55.7286645371772));
#184631=CARTESIAN_POINT('Ctrl Pts',(8.88015840509708,-71.0547945234521,
-55.722195200418));
#184632=CARTESIAN_POINT('Ctrl Pts',(8.87860148389261,-71.0534877255043,
-55.7159071825286));
#184633=CARTESIAN_POINT('Ctrl Pts',(8.87694017157194,-71.0522180593377,
-55.7096025647674));
#184634=CARTESIAN_POINT('Ctrl Pts',(8.87507019836549,-71.0509326662682,
-55.7029762075288));
#184635=CARTESIAN_POINT('Ctrl Pts',(8.87432941318369,-71.0504234610371,
-55.7003511927774));
#184636=CARTESIAN_POINT('Ctrl Pts',(8.87355543624803,-71.0499120229146,
-55.6976758891632));
#184637=CARTESIAN_POINT('Ctrl Pts',(8.87273988365555,-71.0493960567217,
-55.6949322108189));
#184638=CARTESIAN_POINT('Ctrl Pts',(8.87072835501306,-71.0481234462425,
-55.6881650352544));
#184639=CARTESIAN_POINT('Ctrl Pts',(8.86859773578304,-71.0469083241857,
-55.6814343500413));
#184640=CARTESIAN_POINT('Ctrl Pts',(8.86634547526123,-71.045751189175,-55.674743166039));
#184641=CARTESIAN_POINT('Ctrl Pts',(8.85507553034525,-71.0399610739979,
-55.6412615708154));
#184642=CARTESIAN_POINT('Ctrl Pts',(8.84089085739564,-71.0356842930815,
-55.6091873630217));
#184643=CARTESIAN_POINT('Ctrl Pts',(8.82376193805604,-71.0328761747199,
-55.5790161842937));
#184644=CARTESIAN_POINT('Ctrl Pts',(8.81033080789415,-71.030674272634,-55.5553583562312));
#184645=CARTESIAN_POINT('Ctrl Pts',(8.79509006677787,-71.0293748193011,
-55.5328713397496));
#184646=CARTESIAN_POINT('Ctrl Pts',(8.77803915034933,-71.0289449158603,
-55.5118076651523));
#184647=CARTESIAN_POINT('Ctrl Pts',(8.77375593123921,-71.0288369233873,
-55.5065164343881));
#184648=CARTESIAN_POINT('Ctrl Pts',(8.76935125432371,-71.0287837954292,
-55.5013061479734));
#184649=CARTESIAN_POINT('Ctrl Pts',(8.76482428326351,-71.0287853916737,
-55.4961820802034));
#184650=CARTESIAN_POINT('Ctrl Pts',(8.74779107634948,-71.0287913977125,
-55.4769022338321));
#184651=CARTESIAN_POINT('Ctrl Pts',(8.72908197860236,-71.0295822993029,
-55.458973225983));
#184652=CARTESIAN_POINT('Ctrl Pts',(8.70888162163445,-71.0311233825918,
-55.4427172100486));
#184653=CARTESIAN_POINT('Ctrl Pts',(8.70741300418116,-71.031235423276,-55.4415353562447));
#184654=CARTESIAN_POINT('Ctrl Pts',(8.70593652454071,-71.0313514220976,
-55.4403623533746));
#184655=CARTESIAN_POINT('Ctrl Pts',(8.7044522630751,-71.0314713623944,-55.4391983289897));
#184656=CARTESIAN_POINT('Ctrl Pts',(8.69616488178655,-71.0321410496392,
-55.432698993037));
#184657=CARTESIAN_POINT('Ctrl Pts',(8.68749347126554,-71.0329463519757,
-55.4263738514522));
#184658=CARTESIAN_POINT('Ctrl Pts',(8.67858198159518,-71.0338775435445,
-55.4203637320546));
#184659=CARTESIAN_POINT('Ctrl Pts',(8.66968930617718,-71.0348067691487,
-55.4143663014338));
#184660=CARTESIAN_POINT('Ctrl Pts',(8.66055796015982,-71.0358612349136,
-55.4086829050489));
#184661=CARTESIAN_POINT('Ctrl Pts',(8.65135665870045,-71.0370157116539,
-55.4034110626757));
#184662=CARTESIAN_POINT('Ctrl Pts',(8.64203670453801,-71.0381850756127,
-55.3980712387946));
#184663=CARTESIAN_POINT('Ctrl Pts',(8.63264545478659,-71.0394568806338,
-55.3931538649237));
#184664=CARTESIAN_POINT('Ctrl Pts',(8.62337802331042,-71.0407910350239,
-55.3887122670778));
#184665=CARTESIAN_POINT('Ctrl Pts',(8.62073171866857,-71.0411720013104,
-55.3874439738051));
#184666=CARTESIAN_POINT('Ctrl Pts',(8.61809560649366,-71.0415579751156,
-55.3862141696892));
#184667=CARTESIAN_POINT('Ctrl Pts',(8.615474432557,-71.0419478523178,-55.3850233723615));
#184668=CARTESIAN_POINT('Ctrl Pts',(8.61241983732061,-71.0424021972309,
-55.3836356720665));
#184669=CARTESIAN_POINT('Ctrl Pts',(8.60934133814994,-71.0428683753267,
-55.3822808217115));
#184670=CARTESIAN_POINT('Ctrl Pts',(8.60623983960316,-71.0433462841332,
-55.3809601346928));
#184671=CARTESIAN_POINT('Ctrl Pts',(8.58930959822934,-71.0459550589972,
-55.3737508616046));
#184672=CARTESIAN_POINT('Ctrl Pts',(8.57166297875426,-71.0489168177501,
-55.367543437794));
#184673=CARTESIAN_POINT('Ctrl Pts',(8.55347665375656,-71.0522143880086,
-55.3624867791543));
#184674=CARTESIAN_POINT('Ctrl Pts',(8.53515596710212,-71.0555363209133,
-55.3573927616181));
#184675=CARTESIAN_POINT('Ctrl Pts',(8.51628826305535,-71.0591989361935,
-55.3534669775368));
#184676=CARTESIAN_POINT('Ctrl Pts',(8.49708344608809,-71.0631697725525,
-55.3508199238887));
#184677=CARTESIAN_POINT('Ctrl Pts',(8.47782643478517,-71.0671514007439,
-55.3481656761492));
#184678=CARTESIAN_POINT('Ctrl Pts',(8.45823131035549,-71.0714427669999,
-55.3467974390802));
#184679=CARTESIAN_POINT('Ctrl Pts',(8.43852743622952,-71.0759982761646,
-55.3467793842152));
#184680=CARTESIAN_POINT('Ctrl Pts',(8.43089942989955,-71.0777618609562,
-55.3467723945935));
#184681=CARTESIAN_POINT('Ctrl Pts',(8.42325524547048,-71.0795649100216,
-55.3469672331109));
#184682=CARTESIAN_POINT('Ctrl Pts',(8.41560847893818,-71.0814043465126,
-55.3473655849103));
#184683=CARTESIAN_POINT('Ctrl Pts',(8.4,-73.08000002,-58.1763194612681));
#184684=CARTESIAN_POINT('Ctrl Pts',(8.40035672389639,-73.08000002,-58.1110997784471));
#184685=CARTESIAN_POINT('Ctrl Pts',(8.40073754463678,-73.0779206981902,
-58.0450936526532));
#184686=CARTESIAN_POINT('Ctrl Pts',(8.40113458127941,-73.0735758450926,
-57.978552610913));
#184687=CARTESIAN_POINT('Ctrl Pts',(8.40152353070599,-73.0693194920526,
-57.9133669397449));
#184688=CARTESIAN_POINT('Ctrl Pts',(8.40192804222985,-73.0628889081674,
-57.8476679403423));
#184689=CARTESIAN_POINT('Ctrl Pts',(8.40234076967212,-73.0541584892345,
-57.7816841227729));
#184690=CARTESIAN_POINT('Ctrl Pts',(8.40275020169798,-73.045497778208,-57.7162271520608));
#184691=CARTESIAN_POINT('Ctrl Pts',(8.40316771887553,-73.0345737249397,
-57.6504899174073));
#184692=CARTESIAN_POINT('Ctrl Pts',(8.40358621253362,-73.0213140539565,
-57.5846872495408));
#184693=CARTESIAN_POINT('Ctrl Pts',(8.4040017342091,-73.0081485481076,-57.519351887165));
#184694=CARTESIAN_POINT('Ctrl Pts',(8.40441821842852,-72.9926804455084,
-57.4539520333922));
#184695=CARTESIAN_POINT('Ctrl Pts',(8.40482877076465,-72.974889733916,-57.3886895117376));
#184696=CARTESIAN_POINT('Ctrl Pts',(8.4050299722353,-72.966170949436,-57.3567059759489));
#184697=CARTESIAN_POINT('Ctrl Pts',(8.40522975001004,-72.9568951136423,
-57.3247552929955));
#184698=CARTESIAN_POINT('Ctrl Pts',(8.40542729839457,-72.94706438667,-57.2928604536989));
#184699=CARTESIAN_POINT('Ctrl Pts',(8.40550227634482,-72.9433332108387,
-57.2807550159361));
#184700=CARTESIAN_POINT('Ctrl Pts',(8.40557697894183,-72.9395187712762,
-57.2686466985916));
#184701=CARTESIAN_POINT('Ctrl Pts',(8.40565135799998,-72.9356205804985,
-57.2565359345658));
#184702=CARTESIAN_POINT('Ctrl Pts',(8.40619760549404,-72.9069918643403,
-57.1675932312636));
#184703=CARTESIAN_POINT('Ctrl Pts',(8.40672108609692,-72.8740822822173,
-57.0794847544457));
#184704=CARTESIAN_POINT('Ctrl Pts',(8.40720150496587,-72.8368274130977,
-56.9926068087741));
#184705=CARTESIAN_POINT('Ctrl Pts',(8.40745556118681,-72.8171262067712,
-56.94666381197));
#184706=CARTESIAN_POINT('Ctrl Pts',(8.40769757664703,-72.7962107080569,
-56.9010649498654));
#184707=CARTESIAN_POINT('Ctrl Pts',(8.40792456334921,-72.7740772741753,
-56.8558686291175));
#184708=CARTESIAN_POINT('Ctrl Pts',(8.40824535919252,-72.7427965272451,
-56.7919935576286));
#184709=CARTESIAN_POINT('Ctrl Pts',(8.40853569883156,-72.7091163079819,
-56.7289987036777));
#184710=CARTESIAN_POINT('Ctrl Pts',(8.40878697458908,-72.6731278697012,
-56.6671446660938));
#184711=CARTESIAN_POINT('Ctrl Pts',(8.40881559250486,-72.6690291293133,
-56.6601000802737));
#184712=CARTESIAN_POINT('Ctrl Pts',(8.40884370389039,-72.6649004993438,
-56.6530702685158));
#184713=CARTESIAN_POINT('Ctrl Pts',(8.40887129616344,-72.6607421532749,
-56.6460555971729));
#184714=CARTESIAN_POINT('Ctrl Pts',(8.40900622741974,-72.6404070812704,
-56.6117525727297));
#184715=CARTESIAN_POINT('Ctrl Pts',(8.40912875293662,-72.6193610983144,
-56.5778119325455));
#184716=CARTESIAN_POINT('Ctrl Pts',(8.40923748796417,-72.5976273704848,
-56.5442753574122));
#184717=CARTESIAN_POINT('Ctrl Pts',(8.40929185547795,-72.58676050657,-56.5275070698456));
#184718=CARTESIAN_POINT('Ctrl Pts',(8.40934277697055,-72.5757217691974,
-56.5108397496895));
#184719=CARTESIAN_POINT('Ctrl Pts',(8.40939008649233,-72.5645144644975,
-56.4942783667926));
#184720=CARTESIAN_POINT('Ctrl Pts',(8.40941709131399,-72.5581172054839,
-56.4848249380822));
#184721=CARTESIAN_POINT('Ctrl Pts',(8.40944431705732,-72.5512762083545,
-56.4748395208255));
#184722=CARTESIAN_POINT('Ctrl Pts',(8.40947678617871,-72.544654112667,-56.4652954501693));
#184723=CARTESIAN_POINT('Ctrl Pts',(8.40950119944023,-72.5396750141612,
-56.4581193430598));
#184724=CARTESIAN_POINT('Ctrl Pts',(8.40952858023405,-72.5348207940818,
-56.4511920813509));
#184725=CARTESIAN_POINT('Ctrl Pts',(8.40956111525206,-72.5303897605329,
-56.4449172192676));
#184726=CARTESIAN_POINT('Ctrl Pts',(8.40959563855584,-72.5256879368788,
-56.4382588867039));
#184727=CARTESIAN_POINT('Ctrl Pts',(8.40963023878015,-72.5209528390535,
-56.431610605939));
#184728=CARTESIAN_POINT('Ctrl Pts',(8.40966490858559,-72.5161841667267,
-56.424972354458));
#184729=CARTESIAN_POINT('Ctrl Pts',(8.40992896618708,-72.4798642577818,
-56.3744130639842));
#184730=CARTESIAN_POINT('Ctrl Pts',(8.41019734451649,-72.4415022725631,
-56.3243841045374));
#184731=CARTESIAN_POINT('Ctrl Pts',(8.41046552964781,-72.4011582747068,
-56.2751057922352));
#184732=CARTESIAN_POINT('Ctrl Pts',(8.41071616361799,-72.3634545574798,
-56.2290524596161));
#184733=CARTESIAN_POINT('Ctrl Pts',(8.41096663041762,-72.3240192051747,
-56.1836544928687));
#184734=CARTESIAN_POINT('Ctrl Pts',(8.41121299955242,-72.2829028029665,
-56.1391378648765));
#184735=CARTESIAN_POINT('Ctrl Pts',(8.4112764114403,-72.2723200297268,-56.1276799222031));
#184736=CARTESIAN_POINT('Ctrl Pts',(8.41133955045791,-72.2616259229582,
-56.1162806284349));
#184737=CARTESIAN_POINT('Ctrl Pts',(8.41140234650254,-72.2508214301511,
-56.1049444090467));
#184738=CARTESIAN_POINT('Ctrl Pts',(8.41147347283705,-72.2385836534875,
-56.0921043689301));
#184739=CARTESIAN_POINT('Ctrl Pts',(8.41154415246921,-72.226205355973,-56.0793464580293));
#184740=CARTESIAN_POINT('Ctrl Pts',(8.41161431743554,-72.2136936435918,
-56.066682899312));
#184741=CARTESIAN_POINT('Ctrl Pts',(8.41185965065156,-72.1699461896023,
-56.022404511554));
#184742=CARTESIAN_POINT('Ctrl Pts',(8.41209972464812,-72.124441480344,-55.979092815899));
#184743=CARTESIAN_POINT('Ctrl Pts',(8.41233324066691,-72.0772624573489,
-55.9369797476933));
#184744=CARTESIAN_POINT('Ctrl Pts',(8.41253881658477,-72.0357283861281,
-55.8999054917393));
#184745=CARTESIAN_POINT('Ctrl Pts',(8.41273931262493,-71.9928971384868,
-55.8637596924157));
#184746=CARTESIAN_POINT('Ctrl Pts',(8.4129339808891,-71.9488479037631,-55.8286752066144));
#184747=CARTESIAN_POINT('Ctrl Pts',(8.4130399900923,-71.9248603046815,-55.80956948129));
#184748=CARTESIAN_POINT('Ctrl Pts',(8.4131442757425,-71.9005112029568,-55.7907776395893));
#184749=CARTESIAN_POINT('Ctrl Pts',(8.41324670514547,-71.8758233350021,
-55.7723232379903));
#184750=CARTESIAN_POINT('Ctrl Pts',(8.4132660877491,-71.8711516768159,-55.7688311318085));
#184751=CARTESIAN_POINT('Ctrl Pts',(8.41328540470802,-71.8664677096972,
-55.7653509601608));
#184752=CARTESIAN_POINT('Ctrl Pts',(8.41330465595571,-71.8617714024201,
-55.7618827325735));
#184753=CARTESIAN_POINT('Ctrl Pts',(8.41363128196581,-71.7820915742357,
-55.7030391003416));
#184754=CARTESIAN_POINT('Ctrl Pts',(8.41393799526188,-71.6987858561321,
-55.647812970034));
#184755=CARTESIAN_POINT('Ctrl Pts',(8.41422246514108,-71.6125045136972,
-55.5966136090959));
#184756=CARTESIAN_POINT('Ctrl Pts',(8.41449855328811,-71.5287653986031,
-55.5469228062253));
#184757=CARTESIAN_POINT('Ctrl Pts',(8.41475369066292,-71.4422227019064,
-55.5010247736432));
#184758=CARTESIAN_POINT('Ctrl Pts',(8.41498549912693,-71.3534940238151,
-55.4593377991568));
#184759=CARTESIAN_POINT('Ctrl Pts',(8.41520278482016,-71.2703241861167,
-55.4202625083179));
#184760=CARTESIAN_POINT('Ctrl Pts',(8.41539957263635,-71.1852333264852,
-55.384887255107));
#184761=CARTESIAN_POINT('Ctrl Pts',(8.41557368114123,-71.0987580297025,
-55.3535961962895));
#184762=CARTESIAN_POINT('Ctrl Pts',(8.41558531806895,-71.0929782616274,
-55.3515047890378));
#184763=CARTESIAN_POINT('Ctrl Pts',(8.41559685359719,-71.0871923211226,
-55.3494316420719));
#184764=CARTESIAN_POINT('Ctrl Pts',(8.41560828703704,-71.0814003738044,
-55.3473768767704));
#184765=CARTESIAN_POINT('Ctrl Pts',(7.81557216061077,-73.08000002,-58.1565578346149));
#184766=CARTESIAN_POINT('Ctrl Pts',(7.88787222497771,-73.08000002,-56.0696654600803));
#184767=CARTESIAN_POINT('Ctrl Pts',(7.91297989639773,-71.1218111846181,
-55.3449495350315));
#184768=CARTESIAN_POINT('Ctrl Pts',(8.01154341310716,-73.08000002,-58.1633472285769));
#184769=CARTESIAN_POINT('Ctrl Pts',(8.08415144386654,-73.0800000199999,
-56.0574351382549));
#184770=CARTESIAN_POINT('Ctrl Pts',(8.10803398103684,-71.0978479138796,
-55.3428278238728));
#184771=CARTESIAN_POINT('Ctrl Pts',(8.20751459243696,-73.08000002,-58.1699994619965));
#184772=CARTESIAN_POINT('Ctrl Pts',(8.27957773899348,-73.080000019995,-56.0443052546218));
#184773=CARTESIAN_POINT('Ctrl Pts',(8.30261637241262,-71.0730051020405,
-55.3405756034005));
#184774=CARTESIAN_POINT('Ctrl Pts',(8.40348565123649,-73.08000002,-58.1764339313253));
#184775=CARTESIAN_POINT('Ctrl Pts',(8.47395476320647,-73.08000002,-56.0301952716572));
#184776=CARTESIAN_POINT('Ctrl Pts',(8.49667612020153,-71.0472900720475,
-55.3381835033849));
#184777=CARTESIAN_POINT('',(7.91618841388596,-71.1413938388782,-55.3523953317199));
#184778=CARTESIAN_POINT('Origin',(0.0693744628069737,-4.69854457220239,
-43.5232227885957));
#184779=CARTESIAN_POINT('Ctrl Pts',(7.91618834474436,-71.1413930828737,
-55.3523973277251));
#184780=CARTESIAN_POINT('Ctrl Pts',(7.91605153909874,-71.2034746521269,
-55.3759080424155));
#184781=CARTESIAN_POINT('Ctrl Pts',(7.91590005671631,-71.2659341313245,
-55.4019927616619));
#184782=CARTESIAN_POINT('Ctrl Pts',(7.91573324782657,-71.328557341725,-55.4307509004807));
#184783=CARTESIAN_POINT('Ctrl Pts',(7.91558128376081,-71.385607524595,-55.4569497661747));
#184784=CARTESIAN_POINT('Ctrl Pts',(7.91541659756771,-71.4427935588638,
-55.4853677620711));
#184785=CARTESIAN_POINT('Ctrl Pts',(7.9152386469442,-71.4999079010297,-55.5160892262258));
#184786=CARTESIAN_POINT('Ctrl Pts',(7.91506676331057,-71.5550750056455,
-55.545763282911));
#184787=CARTESIAN_POINT('Ctrl Pts',(7.91488250297984,-71.6101755625449,
-55.5775866415003));
#184788=CARTESIAN_POINT('Ctrl Pts',(7.91468535064406,-71.6649751653101,
-55.6116402864228));
#184789=CARTESIAN_POINT('Ctrl Pts',(7.91449742712847,-71.717209565496,-55.6440998596117));
#184790=CARTESIAN_POINT('Ctrl Pts',(7.91429778919425,-71.7691707021736,
-55.6785859971176));
#184791=CARTESIAN_POINT('Ctrl Pts',(7.91408598336362,-71.8206083105627,
-55.7151704742676));
#184792=CARTESIAN_POINT('Ctrl Pts',(7.91399247664347,-71.843316665843,-55.7313215615922));
#184793=CARTESIAN_POINT('Ctrl Pts',(7.9138965984125,-71.8659223339732,-55.7478816187245));
#184794=CARTESIAN_POINT('Ctrl Pts',(7.91379831004409,-71.888400490254,-55.7648567817402));
#184795=CARTESIAN_POINT('Ctrl Pts',(7.91375750815433,-71.8977317190606,
-55.7719035843405));
#184796=CARTESIAN_POINT('Ctrl Pts',(7.91371629392849,-71.9070408946849,
-55.7790218888929));
#184797=CARTESIAN_POINT('Ctrl Pts',(7.91367467121773,-71.9163247705886,
-55.7862110477586));
#184798=CARTESIAN_POINT('Ctrl Pts',(7.91344559186313,-71.9674205368459,
-55.8257780976412));
#184799=CARTESIAN_POINT('Ctrl Pts',(7.91320420359684,-72.0178756635473,
-55.8674802576463));
#184800=CARTESIAN_POINT('Ctrl Pts',(7.91295060237791,-72.0674131211372,
-55.9113042692579));
#184801=CARTESIAN_POINT('Ctrl Pts',(7.91278763230622,-72.0992470494138,
-55.9394666035865));
#184802=CARTESIAN_POINT('Ctrl Pts',(7.91261962316456,-72.1307026933166,
-55.9685044232441));
#184803=CARTESIAN_POINT('Ctrl Pts',(7.91244665070092,-72.1617142526647,
-55.9984055386534));
#184804=CARTESIAN_POINT('Ctrl Pts',(7.91233172832566,-72.1823182377497,
-56.0182717481853));
#184805=CARTESIAN_POINT('Ctrl Pts',(7.91221461584245,-72.2027263192037,
-56.038518895424));
#184806=CARTESIAN_POINT('Ctrl Pts',(7.91209534542699,-72.2229207324772,
-56.0591416827554));
#184807=CARTESIAN_POINT('Ctrl Pts',(7.9120350990377,-72.2331214220513,-56.0695587544905));
#184808=CARTESIAN_POINT('Ctrl Pts',(7.91197429303426,-72.2432690765559,
-56.08007323039));
#184809=CARTESIAN_POINT('Ctrl Pts',(7.91191298560901,-72.2533528906614,
-56.0906750808164));
#184810=CARTESIAN_POINT('Ctrl Pts',(7.91170698464258,-72.2872358247832,
-56.1262986847231));
#184811=CARTESIAN_POINT('Ctrl Pts',(7.91149455903653,-72.3204838435951,
-56.1630410022271));
#184812=CARTESIAN_POINT('Ctrl Pts',(7.91127619570105,-72.3529964672989,
-56.2008190342108));
#184813=CARTESIAN_POINT('Ctrl Pts',(7.91113867876851,-72.3734716824736,
-56.2246102034745));
#184814=CARTESIAN_POINT('Ctrl Pts',(7.91099882009844,-72.3936530793658,
-56.2488098609766));
#184815=CARTESIAN_POINT('Ctrl Pts',(7.9108566916282,-72.4135189243128,-56.2734059029323));
#184816=CARTESIAN_POINT('Ctrl Pts',(7.9106970878667,-72.4358273581791,-56.30102613136));
#184817=CARTESIAN_POINT('Ctrl Pts',(7.91053459989681,-72.4577411046642,
-56.3291500043599));
#184818=CARTESIAN_POINT('Ctrl Pts',(7.9103693134689,-72.4792240409969,-56.3577632330128));
#184819=CARTESIAN_POINT('Ctrl Pts',(7.91028667025495,-72.4899655091633,
-56.3720698473392));
#184820=CARTESIAN_POINT('Ctrl Pts',(7.91020332703685,-72.5005992083201,
-56.3864988690585));
#184821=CARTESIAN_POINT('Ctrl Pts',(7.91011929378563,-72.5111199845664,
-56.4010486482998));
#184822=CARTESIAN_POINT('Ctrl Pts',(7.91010814227553,-72.51251612884,-56.402979455542));
#184823=CARTESIAN_POINT('Ctrl Pts',(7.91009699085137,-72.513908771587,-56.4049102703791));
#184824=CARTESIAN_POINT('Ctrl Pts',(7.9100857447223,-72.515309674263,-56.4068575059994));
#184825=CARTESIAN_POINT('Ctrl Pts',(7.91002258730152,-72.5231770390477,
-56.4177930357892));
#184826=CARTESIAN_POINT('Ctrl Pts',(7.90995716291352,-72.531209313664,-56.4291218453457));
#184827=CARTESIAN_POINT('Ctrl Pts',(7.9098939454102,-72.5388590978003,-56.4400692573546));
#184828=CARTESIAN_POINT('Ctrl Pts',(7.9098835928595,-72.5401118327867,-56.4418620146129));
#184829=CARTESIAN_POINT('Ctrl Pts',(7.9098732997821,-72.541354412209,-56.4436444925833));
#184830=CARTESIAN_POINT('Ctrl Pts',(7.90986308615092,-72.5425845514597,
-56.4454132317544));
#184831=CARTESIAN_POINT('Ctrl Pts',(7.90984507450521,-72.5447538908436,
-56.4485323872007));
#184832=CARTESIAN_POINT('Ctrl Pts',(7.90982730837562,-72.5468849317012,
-56.4516090843173));
#184833=CARTESIAN_POINT('Ctrl Pts',(7.90980989769223,-72.5489653972306,
-56.4546242799526));
#184834=CARTESIAN_POINT('Ctrl Pts',(7.90943253237259,-72.5940581441442,
-56.5199766983186));
#184835=CARTESIAN_POINT('Ctrl Pts',(7.90901970086401,-72.6363853652346,
-56.586848561989));
#184836=CARTESIAN_POINT('Ctrl Pts',(7.9085826566518,-72.675894254675,-56.6550786162537));
#184837=CARTESIAN_POINT('Ctrl Pts',(7.90820073287228,-72.7104202453145,
-56.7147034310293));
#184838=CARTESIAN_POINT('Ctrl Pts',(7.90780032030306,-72.7427947088886,
-56.7753650383112));
#184839=CARTESIAN_POINT('Ctrl Pts',(7.90738899215006,-72.7730108753014,
-56.8369399773851));
#184840=CARTESIAN_POINT('Ctrl Pts',(7.90692956490218,-72.8067604012585,
-56.9057152474241));
#184841=CARTESIAN_POINT('Ctrl Pts',(7.90645485946628,-72.8379002618168,
-56.9759187116765));
#184842=CARTESIAN_POINT('Ctrl Pts',(7.90597814647801,-72.8662221236656,
-57.0468995536857));
#184843=CARTESIAN_POINT('Ctrl Pts',(7.90552849392276,-72.8929363057061,
-57.1138511949638));
#184844=CARTESIAN_POINT('Ctrl Pts',(7.90507706021611,-72.9171434174572,
-57.1814935793758));
#184845=CARTESIAN_POINT('Ctrl Pts',(7.90463487950093,-72.9387159615222,
-57.2492917775834));
#184846=CARTESIAN_POINT('Ctrl Pts',(7.90460826872894,-72.9400142136436,
-57.2533719247549));
#184847=CARTESIAN_POINT('Ctrl Pts',(7.9045816914238,-72.9413029388677,-57.2574526420199));
#184848=CARTESIAN_POINT('Ctrl Pts',(7.90455514997215,-72.9425821151501,
-57.2615338151869));
#184849=CARTESIAN_POINT('Ctrl Pts',(7.90449310528884,-72.9455723844232,
-57.2710741786905));
#184850=CARTESIAN_POINT('Ctrl Pts',(7.90443128316216,-72.9485108109217,
-57.2806123946304));
#184851=CARTESIAN_POINT('Ctrl Pts',(7.90436970799662,-72.9513975879421,
-57.2901480548786));
#184852=CARTESIAN_POINT('Ctrl Pts',(7.90394961648964,-72.9710923869453,
-57.3552043133363));
#184853=CARTESIAN_POINT('Ctrl Pts',(7.90353978491141,-72.9884844749361,
-57.420491090881));
#184854=CARTESIAN_POINT('Ctrl Pts',(7.90314750826272,-73.003568062194,-57.4858113326828));
#184855=CARTESIAN_POINT('Ctrl Pts',(7.90275224687669,-73.0187664167882,
-57.5516285802714));
#184856=CARTESIAN_POINT('Ctrl Pts',(7.90237480900421,-73.0316210069439,
-57.6174797935744));
#184857=CARTESIAN_POINT('Ctrl Pts',(7.90202267091283,-73.0421783087771,
-57.6831546116925));
#184858=CARTESIAN_POINT('Ctrl Pts',(7.90166792717642,-73.0528137293421,
-57.7493153904834));
#184859=CARTESIAN_POINT('Ctrl Pts',(7.90133885955718,-73.061117798216,-57.8152971347828));
#184860=CARTESIAN_POINT('Ctrl Pts',(7.90104311783998,-73.0671905619965,
-57.8808761274596));
#184861=CARTESIAN_POINT('Ctrl Pts',(7.900742514705,-73.0733631501847,-57.9475331110384));
#184862=CARTESIAN_POINT('Ctrl Pts',(7.90047634278182,-73.0772305249596,
-58.0137739762241));
#184863=CARTESIAN_POINT('Ctrl Pts',(7.90025263259021,-73.078951103751,-58.0793551407081));
#184864=CARTESIAN_POINT('Ctrl Pts',(7.90016113595277,-73.0796548140859,
-58.1061775933928));
#184865=CARTESIAN_POINT('Ctrl Pts',(7.90007674213687,-73.08000002,-58.1328895949801));
#184866=CARTESIAN_POINT('Ctrl Pts',(7.9,-73.08000002,-58.1594740865074));
#184867=CARTESIAN_POINT('Ctrl Pts',(7.9,-73.08000002,-58.1594740865074));
#184868=CARTESIAN_POINT('Ctrl Pts',(7.39999999999995,-73.0800000199999,
-58.1594740865073));
#184869=CARTESIAN_POINT('Ctrl Pts',(7.4,-72.58000002,-58.1594740865074));
#184870=CARTESIAN_POINT('Ctrl Pts',(7.9017604405896,-73.08000002,-57.8524302618023));
#184871=CARTESIAN_POINT('Ctrl Pts',(7.39999999999985,-73.0817635435305,
-57.8518911502672));
#184872=CARTESIAN_POINT('Ctrl Pts',(7.4,-72.5800000130548,-57.9035537157173));
#184873=CARTESIAN_POINT('Ctrl Pts',(7.90348019558611,-73.0339592231946,
-57.5530891712348));
#184874=CARTESIAN_POINT('Ctrl Pts',(7.40000000000007,-73.0373043377172,
-57.5520537815894));
#184875=CARTESIAN_POINT('Ctrl Pts',(7.4,-72.5416326919704,-57.6540534055839));
#184876=CARTESIAN_POINT('Ctrl Pts',(7.90599716341333,-72.896885176701,-57.1157587646024));
#184877=CARTESIAN_POINT('Ctrl Pts',(7.3999999999999,-72.9025581822962,-57.1135670536862));
#184878=CARTESIAN_POINT('Ctrl Pts',(7.4,-72.42740431593,-57.2895390365225));
#184879=CARTESIAN_POINT('Ctrl Pts',(7.90681948691283,-72.8397791179241,
-56.9730119912525));
#184880=CARTESIAN_POINT('Ctrl Pts',(7.39999999999985,-72.846103402619,-56.9702086770063));
#184881=CARTESIAN_POINT('Ctrl Pts',(7.4,-72.3798159344887,-57.1705597381646));
#184882=CARTESIAN_POINT('Ctrl Pts',(7.9083884819823,-72.7062368443098,-56.70087080336));
#184883=CARTESIAN_POINT('Ctrl Pts',(7.40000000000008,-72.7136696095191,
-56.6966550709085));
#184884=CARTESIAN_POINT('Ctrl Pts',(7.4,-72.2685307073729,-56.9437302645456));
#184885=CARTESIAN_POINT('Ctrl Pts',(7.90914169806791,-72.6294692039913,
-56.5703391604345));
#184886=CARTESIAN_POINT('Ctrl Pts',(7.39999999999996,-72.6373398680779,
-56.5653507289509));
#184887=CARTESIAN_POINT('Ctrl Pts',(7.4,-72.2045576741781,-56.8349322106875));
#184888=CARTESIAN_POINT('Ctrl Pts',(7.91058447423394,-72.4556998989282,
-56.3204873030743));
#184889=CARTESIAN_POINT('Ctrl Pts',(7.39999999999996,-72.4642201336178,
-56.3138046122562));
#184890=CARTESIAN_POINT('Ctrl Pts',(7.4,-72.0597499182548,-56.6266807792285));
#184891=CARTESIAN_POINT('Ctrl Pts',(7.91127644455456,-72.3580508393546,
-56.2007516828216));
#184892=CARTESIAN_POINT('Ctrl Pts',(7.39999999999996,-72.366765643856,-56.1931795440353));
#184893=CARTESIAN_POINT('Ctrl Pts',(7.4,-71.9783757021874,-56.5268811589555));
#184894=CARTESIAN_POINT('Ctrl Pts',(7.91254952666346,-72.1486549419682,
-55.9805984788111));
#184895=CARTESIAN_POINT('Ctrl Pts',(7.39999999999996,-72.1574857101496,
-55.9712111947932));
#184896=CARTESIAN_POINT('Ctrl Pts',(7.4,-71.8038791222482,-56.3433834633767));
#184897=CARTESIAN_POINT('Ctrl Pts',(7.91313676360239,-72.0363041630141,
-55.879119540041));
#184898=CARTESIAN_POINT('Ctrl Pts',(7.39999999999952,-72.0450577059424,
-55.8688410357779));
#184899=CARTESIAN_POINT('Ctrl Pts',(7.4,-71.710253472938,-56.2588007503857));
#184900=CARTESIAN_POINT('Ctrl Pts',(7.9147504864484,-71.6763659857377,-55.6003940631938));
#184901=CARTESIAN_POINT('Ctrl Pts',(7.40000000000084,-71.6842770741658,
-55.5873067274671));
#184902=CARTESIAN_POINT('Ctrl Pts',(7.4,-71.4103049905956,-56.0264829839341));
#184903=CARTESIAN_POINT('Ctrl Pts',(7.91562717321909,-71.4030569333749,
-55.449171357324));
#184904=CARTESIAN_POINT('Ctrl Pts',(7.40000000000019,-71.4100611802463,
-55.4345719679896));
#184905=CARTESIAN_POINT('Ctrl Pts',(7.4,-71.1825473819866,-55.9004387386915));
#184906=CARTESIAN_POINT('Ctrl Pts',(7.91623251645313,-71.1210872664424,
-55.3447940747887));
#184907=CARTESIAN_POINT('Ctrl Pts',(7.39999999999996,-71.1269094387434,
-55.3290689454198));
#184908=CARTESIAN_POINT('Ctrl Pts',(7.4,-70.9475727253686,-55.8134402200258));
#184909=CARTESIAN_POINT('',(7.40000000638209,-71.4493575166324,-56.0666111687524));
#184910=CARTESIAN_POINT('Ctrl Pts',(7.91618843693206,-71.1413940909408,
-55.352394666395));
#184911=CARTESIAN_POINT('Ctrl Pts',(7.89640718675846,-71.1458420666493,
-55.3533930281891));
#184912=CARTESIAN_POINT('Ctrl Pts',(7.87623144639825,-71.1506401421049,
-55.3558165327541));
#184913=CARTESIAN_POINT('Ctrl Pts',(7.8558979626605,-71.1557708852316,-55.3597440199642));
#184914=CARTESIAN_POINT('Ctrl Pts',(7.83950012223097,-71.1599085484163,
-55.3629113231863));
#184915=CARTESIAN_POINT('Ctrl Pts',(7.82300052698497,-71.1642623278572,
-55.3670559830725));
#184916=CARTESIAN_POINT('Ctrl Pts',(7.8065381012743,-71.1688178845881,-55.3722003240005));
#184917=CARTESIAN_POINT('Ctrl Pts',(7.78854780695949,-71.1737962400139,
-55.3778221083583));
#184918=CARTESIAN_POINT('Ctrl Pts',(7.7705985227141,-71.1790163264486,-55.384638034101));
#184919=CARTESIAN_POINT('Ctrl Pts',(7.7528637382243,-71.1844612784818,-55.3926687943192));
#184920=CARTESIAN_POINT('Ctrl Pts',(7.74067935838542,-71.1882021394895,
-55.3981861905384));
#184921=CARTESIAN_POINT('Ctrl Pts',(7.72858942076698,-71.1920513333967,
-55.4042803599328));
#184922=CARTESIAN_POINT('Ctrl Pts',(7.71666532190953,-71.195999024024,-55.4109499585248));
#184923=CARTESIAN_POINT('Ctrl Pts',(7.71368430355678,-71.1969859445748,
-55.4126173546145));
#184924=CARTESIAN_POINT('Ctrl Pts',(7.7107136939813,-71.1979790030223,-55.4143206650124));
#184925=CARTESIAN_POINT('Ctrl Pts',(7.70775465049132,-71.1989780231378,
-55.4160597890549));
#184926=CARTESIAN_POINT('Ctrl Pts',(7.69950783403543,-71.2017622794544,
-55.4209067055744));
#184927=CARTESIAN_POINT('Ctrl Pts',(7.69133583163375,-71.2045985436463,
-55.4260385615872));
#184928=CARTESIAN_POINT('Ctrl Pts',(7.68327221711032,-71.2074785661779,
-55.4314358850195));
#184929=CARTESIAN_POINT('Ctrl Pts',(7.66246480526368,-71.2149101980804,
-55.4453631791875));
#184930=CARTESIAN_POINT('Ctrl Pts',(7.64235304315307,-71.2226426260351,
-55.4610765570766));
#184931=CARTESIAN_POINT('Ctrl Pts',(7.62319591956619,-71.2306314343771,
-55.478378275891));
#184932=CARTESIAN_POINT('Ctrl Pts',(7.60671393753606,-71.2375046685,-55.4932639458245));
#184933=CARTESIAN_POINT('Ctrl Pts',(7.59094155712043,-71.2445660091722,
-55.5093204534968));
#184934=CARTESIAN_POINT('Ctrl Pts',(7.57601858380446,-71.2517900510317,
-55.526411754027));
#184935=CARTESIAN_POINT('Ctrl Pts',(7.56579096848368,-71.2567411234243,
-55.5381254550068));
#184936=CARTESIAN_POINT('Ctrl Pts',(7.555961737699,-71.2617687656666,-55.5503253156747));
#184937=CARTESIAN_POINT('Ctrl Pts',(7.54657201875478,-71.2668653200254,
-55.5629668564504));
#184938=CARTESIAN_POINT('Ctrl Pts',(7.54416897604539,-71.2681696442408,
-55.5662021143507));
#184939=CARTESIAN_POINT('Ctrl Pts',(7.54179496034111,-71.2694783484373,
-55.5694659659879));
#184940=CARTESIAN_POINT('Ctrl Pts',(7.53945105296537,-71.2707910522752,
-55.5727570060984));
#184941=CARTESIAN_POINT('Ctrl Pts',(7.53513871124294,-71.2732061765195,
-55.5788118910846));
#184942=CARTESIAN_POINT('Ctrl Pts',(7.5309232906607,-71.2756374896449,-55.5849635221776));
#184943=CARTESIAN_POINT('Ctrl Pts',(7.52680908600444,-71.2780824878212,
-55.5912018872169));
#184944=CARTESIAN_POINT('Ctrl Pts',(7.52498538384955,-71.2791662813647,
-55.5939671652513));
#184945=CARTESIAN_POINT('Ctrl Pts',(7.52291658093658,-71.2804108673737,
-55.5971588684365));
#184946=CARTESIAN_POINT('Ctrl Pts',(7.52107659255899,-71.2815341427215,
-55.6000507784099));
#184947=CARTESIAN_POINT('Ctrl Pts',(7.51981528719233,-71.2823041439028,
-55.6020331722195));
#184948=CARTESIAN_POINT('Ctrl Pts',(7.51866042720015,-71.2830169397287,
-55.6038735813195));
#184949=CARTESIAN_POINT('Ctrl Pts',(7.5177546815274,-71.283579827305,-55.6053281505645));
#184950=CARTESIAN_POINT('Ctrl Pts',(7.50884650286416,-71.2891159322487,
-55.6196341120529));
#184951=CARTESIAN_POINT('Ctrl Pts',(7.50024952653351,-71.2948630784978,
-55.6346931994416));
#184952=CARTESIAN_POINT('Ctrl Pts',(7.49204715080729,-71.3007868659789,
-55.6504666068426));
#184953=CARTESIAN_POINT('Ctrl Pts',(7.48063639476581,-71.3090277581357,
-55.6724098230282));
#184954=CARTESIAN_POINT('Ctrl Pts',(7.46999669255816,-71.3176307939435,
-55.6957377083987));
#184955=CARTESIAN_POINT('Ctrl Pts',(7.46034213011195,-71.326574450456,-55.7203187323114));
#184956=CARTESIAN_POINT('Ctrl Pts',(7.45322822633404,-71.333164527656,-55.7384311055911));
#184957=CARTESIAN_POINT('Ctrl Pts',(7.44664909626611,-71.3399387392636,
-55.7572206846394));
#184958=CARTESIAN_POINT('Ctrl Pts',(7.44067748575595,-71.3468921359277,
-55.7766331127628));
#184959=CARTESIAN_POINT('Ctrl Pts',(7.43854478555646,-71.3493754711063,
-55.7835660648133));
#184960=CARTESIAN_POINT('Ctrl Pts',(7.43648958483996,-71.3518816220817,
-55.7905782755251));
#184961=CARTESIAN_POINT('Ctrl Pts',(7.43451563366501,-71.3544095298621,
-55.7976646694261));
#184962=CARTESIAN_POINT('Ctrl Pts',(7.43334182825126,-71.3559127442656,
-55.8018785768573));
#184963=CARTESIAN_POINT('Ctrl Pts',(7.43219623109102,-71.3574242320433,
-55.8061199279847));
#184964=CARTESIAN_POINT('Ctrl Pts',(7.43107929389869,-71.3589437211669,
-55.8103877195221));
#184965=CARTESIAN_POINT('Ctrl Pts',(7.4236300003487,-71.3690777919146,-55.8388513002773));
#184966=CARTESIAN_POINT('Ctrl Pts',(7.41747275315307,-71.3795491841635,
-55.8684398208395));
#184967=CARTESIAN_POINT('Ctrl Pts',(7.41266945915069,-71.3903109707646,
-55.898939933161));
#184968=CARTESIAN_POINT('Ctrl Pts',(7.4076670564432,-71.4015188606843,-55.9307043524075));
#184969=CARTESIAN_POINT('Ctrl Pts',(7.40413342652849,-71.4130416748627,
-55.9634570188779));
#184970=CARTESIAN_POINT('Ctrl Pts',(7.4020940672613,-71.4248176732263,-55.996921242169));
#184971=CARTESIAN_POINT('Ctrl Pts',(7.40069675959774,-71.4328862333001,
-56.0198499219811));
#184972=CARTESIAN_POINT('Ctrl Pts',(7.4,-71.4410734654608,-56.0431118800405));
#184973=CARTESIAN_POINT('Ctrl Pts',(7.4,-71.4493575166339,-56.06661116875));
#184974=CARTESIAN_POINT('Ctrl Pts',(7.4,-72.58000002,-58.1594740865074));
#184975=CARTESIAN_POINT('Ctrl Pts',(7.4,-72.58000002,-58.0551776270551));
#184976=CARTESIAN_POINT('Ctrl Pts',(7.4,-72.5736287847411,-57.9519715312753));
#184977=CARTESIAN_POINT('Ctrl Pts',(7.4,-72.5609286762394,-57.8498358231105));
#184978=CARTESIAN_POINT('Ctrl Pts',(7.4,-72.5482285677376,-57.7477001149456));
#184979=CARTESIAN_POINT('Ctrl Pts',(7.39999999935597,-72.529198463361,-57.6466357793308));
#184980=CARTESIAN_POINT('Ctrl Pts',(7.40000000064314,-72.5039045953935,
-57.5466462680235));
#184981=CARTESIAN_POINT('Ctrl Pts',(7.40000000122792,-72.4924131270627,
-57.5012191983453));
#184982=CARTESIAN_POINT('Ctrl Pts',(7.40000000179748,-72.4796171505751,
-57.4560136230692));
#184983=CARTESIAN_POINT('Ctrl Pts',(7.40000000193861,-72.4655224562879,
-57.4110306599075));
#184984=CARTESIAN_POINT('Ctrl Pts',(7.40000000231984,-72.4274510918893,
-57.2895265855827));
#184985=CARTESIAN_POINT('Ctrl Pts',(7.4000000004226,-72.3798384459848,-57.1705512406855));
#184986=CARTESIAN_POINT('Ctrl Pts',(7.40000000013593,-72.3241837880397,
-57.0571398660674));
#184987=CARTESIAN_POINT('Ctrl Pts',(7.40000000006153,-72.3097383663643,
-57.0277034237349));
#184988=CARTESIAN_POINT('Ctrl Pts',(7.40000000003645,-72.2947325387356,
-56.9985778271777));
#184989=CARTESIAN_POINT('Ctrl Pts',(7.40000000002765,-72.279165204543,-56.9697637092872));
#184990=CARTESIAN_POINT('Ctrl Pts',(7.40000000000257,-72.2347715487634,
-56.8875939546328));
#184991=CARTESIAN_POINT('Ctrl Pts',(7.40000000007907,-72.18577952644,-56.8079051030792));
#184992=CARTESIAN_POINT('Ctrl Pts',(7.40000000044821,-72.1321711779399,
-56.7307944085666));
#184993=CARTESIAN_POINT('Ctrl Pts',(7.40000000085049,-72.0737492661551,
-56.6467598445757));
#184994=CARTESIAN_POINT('Ctrl Pts',(7.40000000144702,-72.0094938737862,
-56.5655636032011));
#184995=CARTESIAN_POINT('Ctrl Pts',(7.40000000089367,-71.941102656717,-56.4892360541651));
#184996=CARTESIAN_POINT('Ctrl Pts',(7.40000000083676,-71.9340690507475,
-56.4813862464333));
#184997=CARTESIAN_POINT('Ctrl Pts',(7.40000000077119,-71.9269917258042,
-56.4735878952506));
#184998=CARTESIAN_POINT('Ctrl Pts',(7.4000000007,-71.9198725431757,-56.465843179204));
#184999=CARTESIAN_POINT('Ctrl Pts',(7.40000000060499,-71.9103706657815,
-56.4555064107617));
#185000=CARTESIAN_POINT('Ctrl Pts',(7.40000000052617,-71.9007927917902,
-56.4452629042245));
#185001=CARTESIAN_POINT('Ctrl Pts',(7.40000000046129,-71.8911429761284,
-56.4351175107121));
#185002=CARTESIAN_POINT('Ctrl Pts',(7.39999999996768,-71.817727207018,-56.357931386775));
#185003=CARTESIAN_POINT('Ctrl Pts',(7.39999999939412,-71.7397944141584,
-56.285795401294));
#185004=CARTESIAN_POINT('Ctrl Pts',(7.40000000114364,-71.6572752456049,
-56.2186315211947));
#185005=CARTESIAN_POINT('Ctrl Pts',(7.40000000147217,-71.6417795999254,
-56.206019328092));
#185006=CARTESIAN_POINT('Ctrl Pts',(7.40000000193345,-71.6261221119199,
-56.1935825531786));
#185007=CARTESIAN_POINT('Ctrl Pts',(7.40000000264863,-71.6103021593138,
-56.1813208069962));
#185008=CARTESIAN_POINT('Ctrl Pts',(7.40000000499281,-71.558447829008,-56.1411294959033));
#185009=CARTESIAN_POINT('Ctrl Pts',(7.40000000927177,-71.5046891439978,
-56.1028356287388));
#185010=CARTESIAN_POINT('Ctrl Pts',(7.40000002552836,-71.4493575166295,
-56.0666111687568));
#185011=CARTESIAN_POINT('Origin',(7.4,67.7009572055632,-55.24995));
#185012=CARTESIAN_POINT('',(7.4,-71.449357516634,-60.42825533736));
#185013=CARTESIAN_POINT('',(7.4,-71.449357516634,-55.24995));
#185014=CARTESIAN_POINT('Origin',(7.4,-69.2744516168521,-60.2813964156253));
#185015=CARTESIAN_POINT('',(7.4,-71.5626363369615,-176.798439391084));
#185016=CARTESIAN_POINT('Ctrl Pts',(7.4,-71.449357516634,-60.42825533736));
#185017=CARTESIAN_POINT('Ctrl Pts',(7.39999999999997,-70.886896756869,-60.42825533736));
#185018=CARTESIAN_POINT('Ctrl Pts',(6.84141371258755,-70.9528017323285,
-60.42825533736));
#185019=CARTESIAN_POINT('Ctrl Pts',(7.4,-71.4493574998816,-60.6471383113761));
#185020=CARTESIAN_POINT('Ctrl Pts',(7.39999999999996,-70.8868967471692,
-60.5644399462782));
#185021=CARTESIAN_POINT('Ctrl Pts',(6.84141371452047,-70.9528017321005,
-60.574175588166));
#185022=CARTESIAN_POINT('Ctrl Pts',(7.4,-71.4018249198588,-60.8620307958147));
#185023=CARTESIAN_POINT('Ctrl Pts',(7.39999999999997,-70.85979500338,-60.6978441698658));
#185024=CARTESIAN_POINT('Ctrl Pts',(6.84320633698782,-70.9209010052172,
-60.7174412822399));
#185025=CARTESIAN_POINT('Ctrl Pts',(7.4,-71.3078420373655,-61.0621827299711));
#185026=CARTESIAN_POINT('Ctrl Pts',(7.39999999999996,-70.8042142666047,
-60.8257004209668));
#185027=CARTESIAN_POINT('Ctrl Pts',(6.84677576889373,-70.8578246683297,
-60.8508735991007));
#185028=CARTESIAN_POINT('',(6.9,-70.949357516634,-60.42825533736));
#185029=CARTESIAN_POINT('Origin',(6.9,-71.449357516634,-60.42825533736));
#185030=CARTESIAN_POINT('',(6.84141371258755,-70.9528017323285,-60.42825533736));
#185031=CARTESIAN_POINT('Origin',(6.9,-71.449357516634,-60.42825533736));
#185032=CARTESIAN_POINT('Origin',(6.92387266608663,-69.4955362780865,-60.3306855231676));
#185033=CARTESIAN_POINT('Origin',(0.,-12.9675000200281,-60.64995));
#185034=CARTESIAN_POINT('Origin',(0.,-12.9675000200281,-60.8508735991007));
#185035=CARTESIAN_POINT('Origin',(0.750000000000035,67.7009572055632,-55.24995));
#185036=CARTESIAN_POINT('',(0.749999999999964,-72.58000002,-174.689806803098));
#185037=CARTESIAN_POINT('',(0.749999999999965,-71.9542570083556,-176.344247731786));
#185038=CARTESIAN_POINT('Ctrl Pts',(0.749999999999964,-72.58000002,-174.689806803098));
#185039=CARTESIAN_POINT('Ctrl Pts',(0.749999999999964,-72.58000002,-174.831376286945));
#185040=CARTESIAN_POINT('Ctrl Pts',(0.750000000181377,-72.5681788618565,
-174.970941599173));
#185041=CARTESIAN_POINT('Ctrl Pts',(0.749999999141365,-72.5447649315039,
-175.108599805088));
#185042=CARTESIAN_POINT('Ctrl Pts',(0.749999998625103,-72.5331422713358,
-175.176933251143));
#185043=CARTESIAN_POINT('Ctrl Pts',(0.749999997778457,-72.5186622030691,
-175.244796569616));
#185044=CARTESIAN_POINT('Ctrl Pts',(0.749999996441189,-72.501348066122,
-175.312200510247));
#185045=CARTESIAN_POINT('Ctrl Pts',(0.749999994685787,-72.4786201957877,
-175.400680116672));
#185046=CARTESIAN_POINT('Ctrl Pts',(0.749999992058193,-72.4508191867992,
-175.488345833607));
#185047=CARTESIAN_POINT('Ctrl Pts',(0.749999988588697,-72.4183069147095,
-175.574298130555));
#185048=CARTESIAN_POINT('Ctrl Pts',(0.749999986546665,-72.3991712571463,
-175.624886834926));
#185049=CARTESIAN_POINT('Ctrl Pts',(0.749999987460588,-72.3784930874995,
-175.674621364589));
#185050=CARTESIAN_POINT('Ctrl Pts',(0.749999990785369,-72.3562980983165,
-175.723514264027));
#185051=CARTESIAN_POINT('Ctrl Pts',(0.749999992115961,-72.3474155677618,
-175.743081413602));
#185052=CARTESIAN_POINT('Ctrl Pts',(0.749999993758535,-72.3382895360991,
-175.762513592359));
#185053=CARTESIAN_POINT('Ctrl Pts',(0.749999995341682,-72.3289194940821,
-175.781810711456));
#185054=CARTESIAN_POINT('Ctrl Pts',(0.749999998527987,-72.3100609827057,
-175.820648844666));
#185055=CARTESIAN_POINT('Ctrl Pts',(0.749999999364237,-72.2901904086323,
-175.8590152493));
#185056=CARTESIAN_POINT('Ctrl Pts',(0.749999999592108,-72.2694003762988,
-175.896717968815));
#185057=CARTESIAN_POINT('Ctrl Pts',(0.749999999760363,-72.2540495109208,
-175.924556760134));
#185058=CARTESIAN_POINT('Ctrl Pts',(0.749999999832536,-72.2381324361931,
-175.952153763115));
#185059=CARTESIAN_POINT('Ctrl Pts',(0.749999998887563,-72.22169996255,-175.979441154676));
#185060=CARTESIAN_POINT('Ctrl Pts',(0.749999996495687,-72.1801067750972,
-176.048509854673));
#185061=CARTESIAN_POINT('Ctrl Pts',(0.749999993208358,-72.1348499287514,
-176.116013152083));
#185062=CARTESIAN_POINT('Ctrl Pts',(0.749999994093549,-72.0863465370719,
-176.181265394638));
#185063=CARTESIAN_POINT('Ctrl Pts',(0.749999994855056,-72.0446203524776,
-176.237400172511));
#185064=CARTESIAN_POINT('Ctrl Pts',(0.749999998190332,-72.0004927389814,
-176.291868658537));
#185065=CARTESIAN_POINT('Ctrl Pts',(0.749999999535633,-71.9542570083559,
-176.344247731786));
#185066=CARTESIAN_POINT('',(0.749999999999965,-71.9542570083556,-171.871644662643));
#185067=CARTESIAN_POINT('',(0.749999999999965,-71.8417317029411,-60.42825533736));
#185068=CARTESIAN_POINT('Origin',(0.749999999999965,-69.6146150315905,-60.2676349698354));
#185069=CARTESIAN_POINT('',(0.749999999999963,-71.8417317505524,-56.1920013490171));
#185070=CARTESIAN_POINT('',(0.749999999999965,-71.8417317029411,-55.24995));
#185071=CARTESIAN_POINT('',(0.749999999999964,-72.58000002,-57.9657868813819));
#185072=CARTESIAN_POINT('Ctrl Pts',(0.749999999999965,-71.8417319269066,
-56.1920012792715));
#185073=CARTESIAN_POINT('Ctrl Pts',(0.749999999999965,-71.8444758759865,
-56.1947266143563));
#185074=CARTESIAN_POINT('Ctrl Pts',(0.749999999999854,-71.8472142189877,
-56.1974588803415));
#185075=CARTESIAN_POINT('Ctrl Pts',(0.7499999999996,-71.849946925556,-56.2001980449111));
#185076=CARTESIAN_POINT('Ctrl Pts',(0.749999999995322,-71.8957971239686,
-56.2461565976726));
#185077=CARTESIAN_POINT('Ctrl Pts',(0.750000000361229,-71.9401028597197,
-56.2942420626375));
#185078=CARTESIAN_POINT('Ctrl Pts',(0.74999999895657,-71.9825277370108,
-56.3440358937271));
#185079=CARTESIAN_POINT('Ctrl Pts',(0.749999998672542,-71.9911062235932,
-56.3541044134062));
#185080=CARTESIAN_POINT('Ctrl Pts',(0.749999998292393,-71.9996079282015,
-56.3642426607221));
#185081=CARTESIAN_POINT('Ctrl Pts',(0.749999997746176,-72.0080302616703,
-56.3744470046658));
#185082=CARTESIAN_POINT('Ctrl Pts',(0.74999999604191,-72.0343090036282,
-56.4062858439066));
#185083=CARTESIAN_POINT('Ctrl Pts',(0.749999992814762,-72.0598149071135,
-56.4387765753063));
#185084=CARTESIAN_POINT('Ctrl Pts',(0.749999990764931,-72.0844669777911,
-56.471823595159));
#185085=CARTESIAN_POINT('Ctrl Pts',(0.7499999887151,-72.1091190484687,-56.5048706150116));
#185086=CARTESIAN_POINT('Ctrl Pts',(0.74999998878556,-72.1329172515315,
-56.5384738714876));
#185087=CARTESIAN_POINT('Ctrl Pts',(0.749999992523647,-72.1557838559918,
-56.5725357961293));
#185088=CARTESIAN_POINT('Ctrl Pts',(0.749999997741391,-72.1877018007307,
-56.6200805302109));
#185089=CARTESIAN_POINT('Ctrl Pts',(0.749999998819484,-72.2179714721241,
-56.6686674551481));
#185090=CARTESIAN_POINT('Ctrl Pts',(0.749999999429074,-72.2464142286222,
-56.7180788042008));
#185091=CARTESIAN_POINT('Ctrl Pts',(0.750000000419556,-72.2926289656526,
-56.7983640080259));
#185092=CARTESIAN_POINT('Ctrl Pts',(0.749999999999578,-72.3344223494519,
-56.8812169184766));
#185093=CARTESIAN_POINT('Ctrl Pts',(0.749999999999555,-72.3716419026412,
-56.9665912683872));
#185094=CARTESIAN_POINT('Ctrl Pts',(0.749999999999551,-72.3771587620865,
-56.9792458611572));
#185095=CARTESIAN_POINT('Ctrl Pts',(0.749999999999476,-72.3825752068175,
-56.9919557956391));
#185096=CARTESIAN_POINT('Ctrl Pts',(0.749999999999378,-72.3878908196252,
-57.0047208623372));
#185097=CARTESIAN_POINT('Ctrl Pts',(0.749999999999364,-72.3886377760633,
-57.0065146251825));
#185098=CARTESIAN_POINT('Ctrl Pts',(0.749999999999346,-72.389382748593,
-57.0083094879105));
#185099=CARTESIAN_POINT('Ctrl Pts',(0.749999999999324,-72.3901257364801,
-57.0101054509238));
#185100=CARTESIAN_POINT('Ctrl Pts',(0.749999999998099,-72.4318199510488,
-57.1108894186501));
#185101=CARTESIAN_POINT('Ctrl Pts',(0.749999999915445,-72.4672597866091,
-57.2155313871763));
#185102=CARTESIAN_POINT('Ctrl Pts',(0.749999999861768,-72.4953436211357,
-57.3206699820973));
#185103=CARTESIAN_POINT('Ctrl Pts',(0.749999999835408,-72.5091351036103,
-57.3723017166415));
#185104=CARTESIAN_POINT('Ctrl Pts',(0.749999999849788,-72.5212576085903,
-57.4242193465116));
#185105=CARTESIAN_POINT('Ctrl Pts',(0.749999999908996,-72.53169711994,-57.4764233217448));
#185106=CARTESIAN_POINT('Ctrl Pts',(0.75000000009092,-72.5637736078163,
-57.6368254825896));
#185107=CARTESIAN_POINT('Ctrl Pts',(0.749999999999964,-72.58000002,-57.7999242188348));
#185108=CARTESIAN_POINT('Ctrl Pts',(0.749999999999964,-72.58000002,-57.9657868813819));
#185109=CARTESIAN_POINT('',(0.749999999999964,-72.58000002,-174.687529226493));
#185110=CARTESIAN_POINT('Ctrl Pts',(0.749999999999965,-71.701161634982,
-61.0621827299711));
#185111=CARTESIAN_POINT('Ctrl Pts',(0.749999999999965,-71.2566817467534,
-60.8548714197835));
#185112=CARTESIAN_POINT('Ctrl Pts',(1.24035792914739,-71.2481103336038,
-60.8508735991007));
#185113=CARTESIAN_POINT('Ctrl Pts',(0.749999999999965,-71.7936527766986,
-60.8638797025928));
#185114=CARTESIAN_POINT('Ctrl Pts',(0.749999999999964,-71.3194598672011,
-60.7217601410268));
#185115=CARTESIAN_POINT('Ctrl Pts',(1.23971725581624,-71.3097847042778,
-60.7186716617645));
#185116=CARTESIAN_POINT('Ctrl Pts',(0.749999999999965,-71.8417316989903,
-60.6492890757558));
#185117=CARTESIAN_POINT('Ctrl Pts',(0.749999999999964,-71.3522348667501,
-60.5771488614746));
#185118=CARTESIAN_POINT('Ctrl Pts',(1.23938654221847,-71.3418443611191,
-60.5756111021815));
#185119=CARTESIAN_POINT('Ctrl Pts',(0.749999999999965,-71.8417317029411,
-60.42825533736));
#185120=CARTESIAN_POINT('Ctrl Pts',(0.749999999999964,-71.3522348691612,
-60.4282553373599));
#185121=CARTESIAN_POINT('Ctrl Pts',(1.2393865421354,-71.3418443611208,-60.42825533736));
#185122=CARTESIAN_POINT('',(1.2393865421354,-71.3418443611208,-60.42825533736));
#185123=CARTESIAN_POINT('Origin',(1.25481291792095,-69.8566648529799,-60.3211428649281));
#185124=CARTESIAN_POINT('Origin',(1.24999999999996,-71.8417317029411,-60.42825533736));
#185125=CARTESIAN_POINT('Ctrl Pts',(0.749999999999964,-72.58000002,-57.9657868813819));
#185126=CARTESIAN_POINT('Ctrl Pts',(0.749999999999964,-73.08000002,-57.9657868813819));
#185127=CARTESIAN_POINT('Ctrl Pts',(0.249999999999964,-73.08000002,-57.9657868813819));
#185128=CARTESIAN_POINT('Ctrl Pts',(0.749999999999964,-72.5800000140225,
-57.7459735178474));
#185129=CARTESIAN_POINT('Ctrl Pts',(0.749999999999964,-73.0799097169388,
-57.7020347823602));
#185130=CARTESIAN_POINT('Ctrl Pts',(0.250090304006367,-73.08000002,-57.7020110302663));
#185131=CARTESIAN_POINT('Ctrl Pts',(0.749999999999964,-72.5514958309333,
-57.5309525432158));
#185132=CARTESIAN_POINT('Ctrl Pts',(0.749999999999975,-73.0456227684187,
-57.4440313928443));
#185133=CARTESIAN_POINT('Ctrl Pts',(0.250178150913126,-73.0457949912512,
-57.4439860415223));
#185134=CARTESIAN_POINT('Ctrl Pts',(0.749999999999964,-72.4672504799085,
-57.2155332517716));
#185135=CARTESIAN_POINT('Ctrl Pts',(0.749999999999959,-72.9444091558477,
-57.0655786327141));
#185136=CARTESIAN_POINT('Ctrl Pts',(0.250306370454135,-72.9447005728246,
-57.0654831530319));
#185137=CARTESIAN_POINT('Ctrl Pts',(0.749999999999964,-72.4318183244811,
-57.1108895827629));
#185138=CARTESIAN_POINT('Ctrl Pts',(0.749999999999965,-72.9018554492066,
-56.9400333127282));
#185139=CARTESIAN_POINT('Ctrl Pts',(0.25034879630597,-72.9021819864826,
-56.9399108365871));
#185140=CARTESIAN_POINT('Ctrl Pts',(0.749999999999964,-72.3484316704448,
-56.9093219305338));
#185141=CARTESIAN_POINT('Ctrl Pts',(0.749999999999964,-72.8017292323873,
-56.6982147960383));
#185142=CARTESIAN_POINT('Ctrl Pts',(0.250430320614374,-72.8021179994285,
-56.6980298209841));
#185143=CARTESIAN_POINT('Ctrl Pts',(0.749999999999965,-72.300481803901,
-56.8120054092621));
#185144=CARTESIAN_POINT('Ctrl Pts',(0.749999999999975,-72.7441631076294,
-56.581469426742));
#185145=CARTESIAN_POINT('Ctrl Pts',(0.250469580226035,-72.744578160532,
-56.5812500750007));
#185146=CARTESIAN_POINT('Ctrl Pts',(0.749999999999965,-72.1382169632082,
-56.5302613678863));
#185147=CARTESIAN_POINT('Ctrl Pts',(0.74999999999994,-72.5493874743356,
-56.2435031793822));
#185148=CARTESIAN_POINT('Ctrl Pts',(0.250582991914968,-72.5498603521484,
-56.2431574556907));
#185149=CARTESIAN_POINT('Ctrl Pts',(0.749999999999965,-72.0032732927043,
-56.3539043654751));
#185150=CARTESIAN_POINT('Ctrl Pts',(0.749999999999422,-72.3874332788213,
-56.0319576106046));
#185151=CARTESIAN_POINT('Ctrl Pts',(0.250653625589273,-72.3879279481205,
-56.0315291953545));
#185152=CARTESIAN_POINT('Ctrl Pts',(0.749999999999965,-71.6966197023802,
-56.0464925782632));
#185153=CARTESIAN_POINT('Ctrl Pts',(0.750000000000507,-72.0194499168863,
-55.6632379181992));
#185154=CARTESIAN_POINT('Ctrl Pts',(0.250776334581247,-72.0199436379809,
-55.6626353009023));
#185155=CARTESIAN_POINT('Ctrl Pts',(0.749999999999965,-71.5244049571092,
-55.9134072123415));
#185156=CARTESIAN_POINT('Ctrl Pts',(0.749999999997373,-71.8128142650138,
-55.5036164406726));
#185157=CARTESIAN_POINT('Ctrl Pts',(0.250829232083772,-71.8132859417639,
-55.5029329728744));
#185158=CARTESIAN_POINT('Ctrl Pts',(0.749999999999965,-71.3337760574596,
-55.8029033796444));
#185159=CARTESIAN_POINT('Ctrl Pts',(0.749999999999965,-71.5840941797283,
-55.3710824677091));
#185160=CARTESIAN_POINT('Ctrl Pts',(0.250873059487692,-71.5845312649516,
-55.3703284570208));
#185161=CARTESIAN_POINT('',(0.250869887203108,-71.6009673739886,-55.3799259279409));
#185162=CARTESIAN_POINT('Ctrl Pts',(0.749999999999961,-71.841731660912,
-56.1920013789646));
#185163=CARTESIAN_POINT('Ctrl Pts',(0.749999996232492,-71.8203840101541,
-56.128102426568));
#185164=CARTESIAN_POINT('Ctrl Pts',(0.747131052735305,-71.8000607354501,
-56.0666787373699));
#185165=CARTESIAN_POINT('Ctrl Pts',(0.741078423025563,-71.7810191778214,
-56.0081419188211));
#185166=CARTESIAN_POINT('Ctrl Pts',(0.737825285209295,-71.770784814549,
-55.9766798358593));
#185167=CARTESIAN_POINT('Ctrl Pts',(0.733652115393616,-71.7609200326615,
-55.9460509739298));
#185168=CARTESIAN_POINT('Ctrl Pts',(0.728509395282827,-71.7514597327231,
-55.9163159881819));
#185169=CARTESIAN_POINT('Ctrl Pts',(0.722846494412134,-71.7410425333414,
-55.8835733397285));
#185170=CARTESIAN_POINT('Ctrl Pts',(0.716008517443964,-71.7311170853223,
-55.8519328895509));
#185171=CARTESIAN_POINT('Ctrl Pts',(0.707973883712583,-71.7217347566402,
-55.8215590914709));
#185172=CARTESIAN_POINT('Ctrl Pts',(0.705572376408577,-71.7189304308163,
-55.812480532276));
#185173=CARTESIAN_POINT('Ctrl Pts',(0.703064221368542,-71.716174534353,
-55.8035149179954));
#185174=CARTESIAN_POINT('Ctrl Pts',(0.70044952091513,-71.7134681966337,
-55.7946660664912));
#185175=CARTESIAN_POINT('Ctrl Pts',(0.69476821762457,-71.707587781013,-55.7754390039406));
#185176=CARTESIAN_POINT('Ctrl Pts',(0.688583995937285,-71.701942135274,
-55.7567665704553));
#185177=CARTESIAN_POINT('Ctrl Pts',(0.681909838458245,-71.6965464723651,
-55.7386975291575));
#185178=CARTESIAN_POINT('Ctrl Pts',(0.678572759718724,-71.6938486409106,
-55.7296630085086));
#185179=CARTESIAN_POINT('Ctrl Pts',(0.675113361509717,-71.6912133527727,
-55.7207792739838));
#185180=CARTESIAN_POINT('Ctrl Pts',(0.671534603530799,-71.6886427442802,
-55.7120524393633));
#185181=CARTESIAN_POINT('Ctrl Pts',(0.669745224541341,-71.6873574400339,
-55.7076890220531));
#185182=CARTESIAN_POINT('Ctrl Pts',(0.667926017606087,-71.6860883098401,
-55.7033648240785));
#185183=CARTESIAN_POINT('Ctrl Pts',(0.666077427506471,-71.6848356434166,
-55.6990805767485));
#185184=CARTESIAN_POINT('Ctrl Pts',(0.664935253287673,-71.6840616679993,
-55.6964335016354));
#185185=CARTESIAN_POINT('Ctrl Pts',(0.663995068024676,-71.6834353209859,
-55.6942867742518));
#185186=CARTESIAN_POINT('Ctrl Pts',(0.662863955044102,-71.6826935920275,
-55.691739575195));
#185187=CARTESIAN_POINT('Ctrl Pts',(0.662164380356346,-71.6822348449233,
-55.6901641746688));
#185188=CARTESIAN_POINT('Ctrl Pts',(0.661391294896625,-71.6817321390306,
-55.6884359887418));
#185189=CARTESIAN_POINT('Ctrl Pts',(0.660444402984383,-71.6811259913739,
-55.6863481504284));
#185190=CARTESIAN_POINT('Ctrl Pts',(0.650608220603443,-71.6748294132496,
-55.6646599744419));
#185191=CARTESIAN_POINT('Ctrl Pts',(0.639939411226591,-71.668891690002,
-55.6438739328685));
#185192=CARTESIAN_POINT('Ctrl Pts',(0.628369170664437,-71.6633099906125,
-55.6239326668601));
#185193=CARTESIAN_POINT('Ctrl Pts',(0.616621675343986,-71.6576427802286,
-55.6036859029437));
#185194=CARTESIAN_POINT('Ctrl Pts',(0.604083829173103,-71.652372581358,
-55.5845338609078));
#185195=CARTESIAN_POINT('Ctrl Pts',(0.590719085952487,-71.6474786056494,
-55.5664598731969));
#185196=CARTESIAN_POINT('Ctrl Pts',(0.57770892323427,-71.6427144721935,
-55.5488654071301));
#185197=CARTESIAN_POINT('Ctrl Pts',(0.563942592492347,-71.6383206108158,
-55.532342364749));
#185198=CARTESIAN_POINT('Ctrl Pts',(0.549514613866369,-71.6343052814187,
-55.5170103376903));
#185199=CARTESIAN_POINT('Ctrl Pts',(0.541878516611505,-71.6321801434087,
-55.5088957671903));
#185200=CARTESIAN_POINT('Ctrl Pts',(0.53405774216662,-71.6301608945464,
-55.5011144209525));
#185201=CARTESIAN_POINT('Ctrl Pts',(0.526071135343876,-71.6282476732945,
-55.4936805695738));
#185202=CARTESIAN_POINT('Ctrl Pts',(0.522626356583135,-71.6274224637807,
-55.4904742049801));
#185203=CARTESIAN_POINT('Ctrl Pts',(0.519393187313092,-71.6266733711271,
-55.4875523510514));
#185204=CARTESIAN_POINT('Ctrl Pts',(0.516052248208152,-71.6259220367257,
-55.4846129885499));
#185205=CARTESIAN_POINT('Ctrl Pts',(0.512850492195839,-71.6252020028186,
-55.4817960795116));
#185206=CARTESIAN_POINT('Ctrl Pts',(0.509549728098309,-71.6244799207866,
-55.4789630294608));
#185207=CARTESIAN_POINT('Ctrl Pts',(0.505845569683937,-71.623698353505,
-55.4758859675463));
#185208=CARTESIAN_POINT('Ctrl Pts',(0.504783854460946,-71.6234743345005,
-55.475003995689));
#185209=CARTESIAN_POINT('Ctrl Pts',(0.503688841818574,-71.6232455061024,
-55.4741022375036));
#185210=CARTESIAN_POINT('Ctrl Pts',(0.502552953881557,-71.6230107197811,
-55.4731760177748));
#185211=CARTESIAN_POINT('Ctrl Pts',(0.490275767922547,-71.6204730439836,
-55.4631650197884));
#185212=CARTESIAN_POINT('Ctrl Pts',(0.477525582018539,-71.6181363231932,
-55.4538148724768));
#185213=CARTESIAN_POINT('Ctrl Pts',(0.464337021242048,-71.6160065604269,
-55.4451889526195));
#185214=CARTESIAN_POINT('Ctrl Pts',(0.447262090742039,-71.6132492048798,
-55.4340211698296));
#185215=CARTESIAN_POINT('Ctrl Pts',(0.429665697481203,-71.6108662887343,
-55.4242021638032));
#185216=CARTESIAN_POINT('Ctrl Pts',(0.411688401881651,-71.6088670387269,
-55.4158238229682));
#185217=CARTESIAN_POINT('Ctrl Pts',(0.393843346884726,-71.6068824951599,
-55.4075071130295));
#185218=CARTESIAN_POINT('Ctrl Pts',(0.375623361038916,-71.6052759751029,
-55.4006101353856));
#185219=CARTESIAN_POINT('Ctrl Pts',(0.35717783270288,-71.6040442407152,
-55.3951748301981));
#185220=CARTESIAN_POINT('Ctrl Pts',(0.338866566196649,-71.6028214719104,
-55.3897790876626));
#185221=CARTESIAN_POINT('Ctrl Pts',(0.320333393067772,-71.6019680183095,
-55.3858239119413));
#185222=CARTESIAN_POINT('Ctrl Pts',(0.301730629650085,-71.6014689796738,
-55.3833008360601));
#185223=CARTESIAN_POINT('Ctrl Pts',(0.28479589526439,-71.6010146876659,
-55.3810039934392));
#185224=CARTESIAN_POINT('Ctrl Pts',(0.267803743668673,-71.6008539429058,
-55.3798933886721));
#185225=CARTESIAN_POINT('Ctrl Pts',(0.250869887203208,-71.6009673739965,
-55.3799259279328));
#185226=CARTESIAN_POINT('',(0.249999999999964,-73.08000002,-57.9657868813819));
#185227=CARTESIAN_POINT('Ctrl Pts',(0.249999999999963,-73.08000002,-57.9657868813819));
#185228=CARTESIAN_POINT('Ctrl Pts',(0.250042469931417,-73.080000019999,
-57.8920441993433));
#185229=CARTESIAN_POINT('Ctrl Pts',(0.250086371965619,-73.0772779883399,
-57.8175078453759));
#185230=CARTESIAN_POINT('Ctrl Pts',(0.250131098523594,-73.0716768447104,
-57.7424712607537));
#185231=CARTESIAN_POINT('Ctrl Pts',(0.250175351214089,-73.0661350438948,
-57.668229671293));
#185232=CARTESIAN_POINT('Ctrl Pts',(0.250220410087223,-73.0577743703455,
-57.5934988530362));
#185233=CARTESIAN_POINT('Ctrl Pts',(0.250265626043886,-73.0464826175312,
-57.5185941346588));
#185234=CARTESIAN_POINT('Ctrl Pts',(0.250310434748604,-73.0352925674925,
-57.4443640695335));
#185235=CARTESIAN_POINT('Ctrl Pts',(0.250355396587183,-73.0212236537723,
-57.3699637680883));
#185236=CARTESIAN_POINT('Ctrl Pts',(0.250399835547614,-73.0042119982681,
-57.2957233809505));
#185237=CARTESIAN_POINT('Ctrl Pts',(0.25044394534943,-72.9873263478039,
-57.2220328910844));
#185238=CARTESIAN_POINT('Ctrl Pts',(0.250487538732826,-72.9675411584413,
-57.1485005658174));
#185239=CARTESIAN_POINT('Ctrl Pts',(0.250529928559043,-72.9448431246011,
-57.0754636929159));
#185240=CARTESIAN_POINT('Ctrl Pts',(0.250572072640272,-72.9222766772416,
-57.0028502340045));
#185241=CARTESIAN_POINT('Ctrl Pts',(0.250613025749873,-72.8968309609008,
-56.9307271493267));
#185242=CARTESIAN_POINT('Ctrl Pts',(0.250652106105929,-72.8685441528253,
-56.8594307921769));
#185243=CARTESIAN_POINT('Ctrl Pts',(0.250691023114669,-72.8403755774027,
-56.7884324381607));
#185244=CARTESIAN_POINT('Ctrl Pts',(0.250728081651377,-72.8093896477869,
-56.7182545754342));
#185245=CARTESIAN_POINT('Ctrl Pts',(0.250762621939711,-72.7756755277479,
-56.6492244236476));
#185246=CARTESIAN_POINT('Ctrl Pts',(0.250797078194219,-72.7420434315326,
-56.5803622168345));
#185247=CARTESIAN_POINT('Ctrl Pts',(0.250829027144611,-72.7056965763661,
-56.5126427849829));
#185248=CARTESIAN_POINT('Ctrl Pts',(0.250857847047447,-72.6667732478891,
-56.4463762751986));
#185249=CARTESIAN_POINT('Ctrl Pts',(0.250886657396073,-72.6278628230513,
-56.3801317337086));
#185250=CARTESIAN_POINT('Ctrl Pts',(0.250912339577454,-72.586377932768,
-56.3153397478542));
#185251=CARTESIAN_POINT('Ctrl Pts',(0.250934324442956,-72.5425029977862,
-56.2522861365262));
#185252=CARTESIAN_POINT('Ctrl Pts',(0.250956333737572,-72.4985793099114,
-56.1891624613686));
#185253=CARTESIAN_POINT('Ctrl Pts',(0.250974636461275,-72.452260682586,
-56.1277815480868));
#185254=CARTESIAN_POINT('Ctrl Pts',(0.250988730474407,-72.4037731304877,
-56.0683976530279));
#185255=CARTESIAN_POINT('Ctrl Pts',(0.25100286048415,-72.3551617394526,
-56.0088620893836));
#185256=CARTESIAN_POINT('Ctrl Pts',(0.251012759433403,-72.3043708505095,
-55.9513341800841));
#185257=CARTESIAN_POINT('Ctrl Pts',(0.25101800459919,-72.2516623010505,
-55.8960303301876));
#185258=CARTESIAN_POINT('Ctrl Pts',(0.251023288789269,-72.1985615973934,
-55.8403150169303));
#185259=CARTESIAN_POINT('Ctrl Pts',(0.251023849052114,-72.1435151798975,
-55.7868573130842));
#185260=CARTESIAN_POINT('Ctrl Pts',(0.251019348764074,-72.086816969245,
-55.7358323645543));
#185261=CARTESIAN_POINT('Ctrl Pts',(0.251014826609809,-72.0298432704859,
-55.6845594934481));
#185262=CARTESIAN_POINT('Ctrl Pts',(0.251005194309946,-71.9712023416134,
-55.6357432440695));
#185263=CARTESIAN_POINT('Ctrl Pts',(0.25099021352996,-71.911209329447,-55.5895111537473));
#185264=CARTESIAN_POINT('Ctrl Pts',(0.25097507537099,-71.8505860671018,
-55.5427933771403));
#185265=CARTESIAN_POINT('Ctrl Pts',(0.250954475679539,-71.7885828358966,
-55.4987144045882));
#185266=CARTESIAN_POINT('Ctrl Pts',(0.250928276758545,-71.7255319930884,
-55.4573528781666));
#185267=CARTESIAN_POINT('Ctrl Pts',(0.250911195986817,-71.684425069125,
-55.4303866229051));
#185268=CARTESIAN_POINT('Ctrl Pts',(0.25089173745834,-71.6428729679957,
-55.4045743425418));
#185269=CARTESIAN_POINT('Ctrl Pts',(0.250869887203029,-71.6009673739763,
-55.3799259279683));
#185270=CARTESIAN_POINT('Origin',(0.249999999999964,-72.58000002,-57.9657868813819));
#185271=CARTESIAN_POINT('Origin',(0.249999999999964,-72.58000002,-55.24995));
#185272=CARTESIAN_POINT('',(0.249999999999962,-73.08000002,-174.689806803098));
#185273=CARTESIAN_POINT('Origin',(0.249999999999964,-72.58000002,-174.689806803098));
#185274=CARTESIAN_POINT('',(0.249999999999964,-73.08000002,-57.9678366169137));
#185275=CARTESIAN_POINT('Ctrl Pts',(0.249999999999964,-73.08000002,-174.689806803097));
#185276=CARTESIAN_POINT('Ctrl Pts',(0.749999999999964,-73.08000002,-174.689806803097));
#185277=CARTESIAN_POINT('Ctrl Pts',(0.749999999999964,-72.58000002,-174.689806803097));
#185278=CARTESIAN_POINT('Ctrl Pts',(0.250096721285987,-73.08000002,-174.944087763949));
#185279=CARTESIAN_POINT('Ctrl Pts',(0.749999999999963,-73.0799033011073,
-174.944063234271));
#185280=CARTESIAN_POINT('Ctrl Pts',(0.749999999999964,-72.5800000142362,
-174.901707787501));
#185281=CARTESIAN_POINT('Ctrl Pts',(0.25019084538922,-73.0481762528639,
-175.193013365813));
#185282=CARTESIAN_POINT('Ctrl Pts',(0.749999999999965,-73.047991321912,
-175.192966486363));
#185283=CARTESIAN_POINT('Ctrl Pts',(0.749999999999964,-72.5534802154039,
-175.109145968138));
#185284=CARTESIAN_POINT('Ctrl Pts',(0.250374112266224,-72.9229204323206,
-175.680308208816));
#185285=CARTESIAN_POINT('Ctrl Pts',(0.749999999999964,-72.9225699879354,
-175.680169902411));
#185286=CARTESIAN_POINT('Ctrl Pts',(0.749999999999964,-72.4491003622499,
-175.515225349862));
#185287=CARTESIAN_POINT('Ctrl Pts',(0.250463183534996,-72.8282888567225,
-175.918532203572));
#185288=CARTESIAN_POINT('Ctrl Pts',(0.750000000001369,-72.8278715101479,
-175.918330718485));
#185289=CARTESIAN_POINT('Ctrl Pts',(0.749999999999965,-72.3702407172373,
-175.713745513771));
#185290=CARTESIAN_POINT('Ctrl Pts',(0.25062659166413,-72.5862295913911,
-176.357642327882));
#185291=CARTESIAN_POINT('Ctrl Pts',(0.74999999999856,-72.5857133666792,
-176.357282462775));
#185292=CARTESIAN_POINT('Ctrl Pts',(0.749999999999965,-72.1685246628573,
-176.079670924798));
#185293=CARTESIAN_POINT('Ctrl Pts',(0.250703242845797,-72.4354180409157,
-176.564734305741));
#185294=CARTESIAN_POINT('Ctrl Pts',(0.749999999997952,-72.4348744309047,
-176.56428717754));
#185295=CARTESIAN_POINT('Ctrl Pts',(0.749999999999965,-72.0428483696925,
-176.252247715791));
#185296=CARTESIAN_POINT('Ctrl Pts',(0.250838284668646,-72.090128509306,
-176.930952892336));
#185297=CARTESIAN_POINT('Ctrl Pts',(0.750000000001977,-72.0895755229708,
-176.930319469104));
#185298=CARTESIAN_POINT('Ctrl Pts',(0.749999999999965,-71.7551070954922,
-176.557430126179));
#185299=CARTESIAN_POINT('Ctrl Pts',(0.250896921774036,-71.8966556096658,
-177.090711302921));
#185300=CARTESIAN_POINT('Ctrl Pts',(0.749999999997485,-71.8961205198801,
-177.08999030776));
#185301=CARTESIAN_POINT('Ctrl Pts',(0.749999999999965,-71.5938796749303,
-176.690562238895));
#185302=CARTESIAN_POINT('Ctrl Pts',(0.250946592270043,-71.6818193327012,
-177.226378685119));
#185303=CARTESIAN_POINT('Ctrl Pts',(0.749999999999965,-71.6813148644928,
-177.225579834422));
#185304=CARTESIAN_POINT('Ctrl Pts',(0.749999999999965,-71.414849447251,
-176.803618488051));
#185305=CARTESIAN_POINT('',(0.250942965994138,-71.6973962901444,-177.216474798299));
#185306=CARTESIAN_POINT('Ctrl Pts',(0.25094296599405,-71.6973962901389,
-177.216474798276));
#185307=CARTESIAN_POINT('Ctrl Pts',(0.250976479214862,-71.760322042129,
-177.176193884541));
#185308=CARTESIAN_POINT('Ctrl Pts',(0.251003803266757,-71.822289052444,
-177.133208560261));
#185309=CARTESIAN_POINT('Ctrl Pts',(0.251025052218208,-71.8829682618455,
-177.087581567843));
#185310=CARTESIAN_POINT('Ctrl Pts',(0.251046127790315,-71.9431523634545,
-177.0423268657));
#185311=CARTESIAN_POINT('Ctrl Pts',(0.251061226926392,-72.0020689462363,
-176.994473421731));
#185312=CARTESIAN_POINT('Ctrl Pts',(0.251070576134496,-72.0594007051876,
-176.944133320408));
#185313=CARTESIAN_POINT('Ctrl Pts',(0.25107986405914,-72.1163566581376,
-176.89412319522));
#185314=CARTESIAN_POINT('Ctrl Pts',(0.251083477423211,-72.1717478547756,
-176.841659032887));
#185315=CARTESIAN_POINT('Ctrl Pts',(0.251081751302264,-72.2252765394361,
-176.786900255691));
#185316=CARTESIAN_POINT('Ctrl Pts',(0.251080033711072,-72.2785407081389,
-176.732412073046));
#185317=CARTESIAN_POINT('Ctrl Pts',(0.251073029808676,-72.3299601210376,
-176.675652156158));
#185318=CARTESIAN_POINT('Ctrl Pts',(0.251061176284639,-72.3792640075592,
-176.616823910038));
#185319=CARTESIAN_POINT('Ctrl Pts',(0.251049362132091,-72.4284041311798,
-176.558191061989));
#185320=CARTESIAN_POINT('Ctrl Pts',(0.251032731334361,-72.4754422161327,
-176.497503982321));
#185321=CARTESIAN_POINT('Ctrl Pts',(0.251011812305099,-72.520141292388,
-176.435005426744));
#185322=CARTESIAN_POINT('Ctrl Pts',(0.250990240328152,-72.5662355652342,
-176.370556097707));
#185323=CARTESIAN_POINT('Ctrl Pts',(0.250964108948217,-72.6098417978143,
-176.30418078364));
#185324=CARTESIAN_POINT('Ctrl Pts',(0.250934089145355,-72.6507433908404,
-176.236184599534));
#185325=CARTESIAN_POINT('Ctrl Pts',(0.25090499157123,-72.6903884591434,
-176.170277304395));
#185326=CARTESIAN_POINT('Ctrl Pts',(0.25087224249439,-72.727492393518,-176.10284794613));
#185327=CARTESIAN_POINT('Ctrl Pts',(0.250836518310456,-72.7619035974977,
-176.034201619033));
#185328=CARTESIAN_POINT('Ctrl Pts',(0.250800722749006,-72.7963835556372,
-175.965418135428));
#185329=CARTESIAN_POINT('Ctrl Pts',(0.250761941597354,-72.8281597947364,
-175.895413450691));
#185330=CARTESIAN_POINT('Ctrl Pts',(0.250720899474743,-72.8571292191755,
-175.824512204359));
#185331=CARTESIAN_POINT('Ctrl Pts',(0.250679716181218,-72.8861982885607,
-175.753367081905));
#185332=CARTESIAN_POINT('Ctrl Pts',(0.250636257835567,-72.9124411218246,
-175.681319886333));
#185333=CARTESIAN_POINT('Ctrl Pts',(0.250591278953596,-72.9358055216485,
-175.608706599455));
#185334=CARTESIAN_POINT('Ctrl Pts',(0.250544145622038,-72.9602890560385,
-175.532615198869));
#185335=CARTESIAN_POINT('Ctrl Pts',(0.250495344354186,-72.981611464156,
-175.455902966511));
#185336=CARTESIAN_POINT('Ctrl Pts',(0.250445742789475,-72.9997735060265,
-175.378953996231));
#185337=CARTESIAN_POINT('Ctrl Pts',(0.250397681398313,-73.0173716000327,
-175.304394361233));
#185338=CARTESIAN_POINT('Ctrl Pts',(0.250348870046398,-73.0320031038598,
-175.229613064406));
#185339=CARTESIAN_POINT('Ctrl Pts',(0.250300073860922,-73.0437215355442,
-175.154946852542));
#185340=CARTESIAN_POINT('Ctrl Pts',(0.250248932094337,-73.0560032598656,
-175.076691514717));
#185341=CARTESIAN_POINT('Ctrl Pts',(0.250197808860602,-73.0650851592926,
-174.99856341985));
#185342=CARTESIAN_POINT('Ctrl Pts',(0.250147532330345,-73.0710841986421,
-174.920924864984));
#185343=CARTESIAN_POINT('Ctrl Pts',(0.250097255800088,-73.0770832379916,
-174.843286310117));
#185344=CARTESIAN_POINT('Ctrl Pts',(0.25004782720234,-73.0800000199989,
-174.766137816945));
#185345=CARTESIAN_POINT('Ctrl Pts',(0.249999999999961,-73.08000002,-174.689806803098));
#185346=CARTESIAN_POINT('Ctrl Pts',(0.250942965994174,-71.697396290156,
-177.216474798319));
#185347=CARTESIAN_POINT('Ctrl Pts',(0.270264526385401,-71.6972689123026,
-177.216513071422));
#185348=CARTESIAN_POINT('Ctrl Pts',(0.289719933294543,-71.6975397265544,
-177.214938644682));
#185349=CARTESIAN_POINT('Ctrl Pts',(0.30909956798559,-71.6982247726489,
-177.211737182828));
#185350=CARTESIAN_POINT('Ctrl Pts',(0.328957416411424,-71.698926723007,
-177.208456721393));
#185351=CARTESIAN_POINT('Ctrl Pts',(0.348735110265057,-71.7000636457951,
-177.203467956048));
#185352=CARTESIAN_POINT('Ctrl Pts',(0.368198254111624,-71.7016407715696,
-177.196808079087));
#185353=CARTESIAN_POINT('Ctrl Pts',(0.374482450132035,-71.7021499887646,
-177.194657759867));
#185354=CARTESIAN_POINT('Ctrl Pts',(0.380733825865396,-71.7027050024855,
-177.192333627024));
#185355=CARTESIAN_POINT('Ctrl Pts',(0.386944469709064,-71.7033057202149,
-177.189838046772));
#185356=CARTESIAN_POINT('Ctrl Pts',(0.401084223294227,-71.7046733724069,
-177.184156366947));
#185357=CARTESIAN_POINT('Ctrl Pts',(0.415014553244461,-71.7062782430979,
-177.177584716033));
#185358=CARTESIAN_POINT('Ctrl Pts',(0.428650066650391,-71.7081181561605,
-177.170155344181));
#185359=CARTESIAN_POINT('Ctrl Pts',(0.437491216212795,-71.7093111399582,
-177.165338203401));
#185360=CARTESIAN_POINT('Ctrl Pts',(0.446206744620982,-71.7106026105523,
-177.160161774));
#185361=CARTESIAN_POINT('Ctrl Pts',(0.454779260000809,-71.7119923408229,
-177.154633350333));
#185362=CARTESIAN_POINT('Ctrl Pts',(0.459427949347712,-71.7127459614369,
-177.151635405965));
#185363=CARTESIAN_POINT('Ctrl Pts',(0.46403489949683,-71.7135285745735,
-177.148533580525));
#185364=CARTESIAN_POINT('Ctrl Pts',(0.468589071742487,-71.7143385748615,
-177.1453352109));
#185365=CARTESIAN_POINT('Ctrl Pts',(0.473063010586619,-71.715134304921,
-177.142193188744));
#185366=CARTESIAN_POINT('Ctrl Pts',(0.477498484508432,-71.7159593880345,
-177.138948316893));
#185367=CARTESIAN_POINT('Ctrl Pts',(0.481883829164943,-71.716811182357,
-177.135612221786));
#185368=CARTESIAN_POINT('Ctrl Pts',(0.485757118468243,-71.7175635168019,
-177.132665666269));
#185369=CARTESIAN_POINT('Ctrl Pts',(0.489837937730701,-71.7183834985899,
-177.129457083549));
#185370=CARTESIAN_POINT('Ctrl Pts',(0.493835191553745,-71.7192185065134,
-177.126200136524));
#185371=CARTESIAN_POINT('Ctrl Pts',(0.498075833628816,-71.7201043571225,
-177.122744877689));
#185372=CARTESIAN_POINT('Ctrl Pts',(0.502221922901849,-71.7210071255079,
-177.11923531805));
#185373=CARTESIAN_POINT('Ctrl Pts',(0.505950388940999,-71.7218478956593,
-177.115981351614));
#185374=CARTESIAN_POINT('Ctrl Pts',(0.507713663755773,-71.7222455146311,
-177.114442478253));
#185375=CARTESIAN_POINT('Ctrl Pts',(0.509383932591482,-71.7226290411988,
-177.112961523303));
#185376=CARTESIAN_POINT('Ctrl Pts',(0.510928956307166,-71.7229891444007,
-177.111574477354));
#185377=CARTESIAN_POINT('Ctrl Pts',(0.525744610702608,-71.7264422723574,
-177.098273714909));
#185378=CARTESIAN_POINT('Ctrl Pts',(0.540145094113651,-71.7302846063745,
-177.083683222483));
#185379=CARTESIAN_POINT('Ctrl Pts',(0.553845466478309,-71.7344794501829,
-177.068004345852));
#185380=CARTESIAN_POINT('Ctrl Pts',(0.5557948104403,-71.7350763093946,-177.065773492363));
#185381=CARTESIAN_POINT('Ctrl Pts',(0.557729972543417,-71.7356802828448,
-177.06352068727));
#185382=CARTESIAN_POINT('Ctrl Pts',(0.55965012674352,-71.7362912430783,
-177.061246589637));
#185383=CARTESIAN_POINT('Ctrl Pts',(0.572987316213086,-71.7405349087129,
-177.045450946246));
#185384=CARTESIAN_POINT('Ctrl Pts',(0.585704230882826,-71.7451282375326,
-177.028575967441));
#185385=CARTESIAN_POINT('Ctrl Pts',(0.597763139675443,-71.7500808478573,
-177.010630935905));
#185386=CARTESIAN_POINT('Ctrl Pts',(0.610239883661992,-71.7552050636673,
-176.992064117948));
#185387=CARTESIAN_POINT('Ctrl Pts',(0.621956874734709,-71.7606986066875,
-176.97242882321));
#185388=CARTESIAN_POINT('Ctrl Pts',(0.632911144964776,-71.7665625189615,
-176.951783782017));
#185389=CARTESIAN_POINT('Ctrl Pts',(0.633369156063166,-71.7668076961248,
-176.950920588231));
#185390=CARTESIAN_POINT('Ctrl Pts',(0.633825564774752,-71.7670534314148,
-176.950056147609));
#185391=CARTESIAN_POINT('Ctrl Pts',(0.634280373130207,-71.7672997213183,
-176.949190468659));
#185392=CARTESIAN_POINT('Ctrl Pts',(0.639946612355886,-71.7703681291322,
-176.938405389707));
#185393=CARTESIAN_POINT('Ctrl Pts',(0.645400236066963,-71.7735423162463,
-176.927359520256));
#185394=CARTESIAN_POINT('Ctrl Pts',(0.650639754836452,-71.7768027187209,
-176.916069509228));
#185395=CARTESIAN_POINT('Ctrl Pts',(0.653259514221201,-71.7784329199583,
-176.910424503714));
#185396=CARTESIAN_POINT('Ctrl Pts',(0.655825527594471,-71.7800854028515,
-176.904718297703));
#185397=CARTESIAN_POINT('Ctrl Pts',(0.658336622015916,-71.7817616184398,
-176.898952175483));
#185398=CARTESIAN_POINT('Ctrl Pts',(0.65982011992222,-71.7827518887755,
-176.895545680622));
#185399=CARTESIAN_POINT('Ctrl Pts',(0.661488202284415,-71.7838900418682,
-176.891639326401));
#185400=CARTESIAN_POINT('Ctrl Pts',(0.662976735295404,-71.7849296832095,
-176.888079828907));
#185401=CARTESIAN_POINT('Ctrl Pts',(0.664007819551247,-71.7856498270093,
-176.885614218942));
#185402=CARTESIAN_POINT('Ctrl Pts',(0.664953887829225,-71.7863222897559,
-176.883316006929));
#185403=CARTESIAN_POINT('Ctrl Pts',(0.665704692784938,-71.7868612729392,
-176.881475844081));
#185404=CARTESIAN_POINT('Ctrl Pts',(0.673043534861993,-71.7921296351606,
-176.863488929597));
#185405=CARTESIAN_POINT('Ctrl Pts',(0.679883034351907,-71.7976623272424,
-176.844889471199));
#185406=CARTESIAN_POINT('Ctrl Pts',(0.686226766441959,-71.8034367538504,
-176.825696233573));
#185407=CARTESIAN_POINT('Ctrl Pts',(0.697394959541523,-71.8136026799144,
-176.791906379121));
#185408=CARTESIAN_POINT('Ctrl Pts',(0.707022095169632,-71.8244891229403,
-176.756302654074));
#185409=CARTESIAN_POINT('Ctrl Pts',(0.715145536483142,-71.8360319850039,
-176.7189895102));
#185410=CARTESIAN_POINT('Ctrl Pts',(0.723451411044401,-71.8478340724048,
-176.680838401508));
#185411=CARTESIAN_POINT('Ctrl Pts',(0.730185480967119,-71.8603223275583,
-176.640900304655));
#185412=CARTESIAN_POINT('Ctrl Pts',(0.735428754255368,-71.873409659994,
-176.599320597914));
#185413=CARTESIAN_POINT('Ctrl Pts',(0.740933102500712,-71.8871486416127,
-176.555670539399));
#185414=CARTESIAN_POINT('Ctrl Pts',(0.744794629914615,-71.9015477772457,
-176.510211301259));
#185415=CARTESIAN_POINT('Ctrl Pts',(0.747149609679553,-71.9164869468611,
-176.463147664823));
#185416=CARTESIAN_POINT('Ctrl Pts',(0.749080992754893,-71.9287389669356,
-176.424549494159));
#185417=CARTESIAN_POINT('Ctrl Pts',(0.749999999999965,-71.9413537743572,
-176.384872959276));
#185418=CARTESIAN_POINT('Ctrl Pts',(0.749999999999965,-71.9542570083556,
-176.344247731786));
#185419=CARTESIAN_POINT('Origin',(0.,-12.9675000200281,-177.84995));
#185420=CARTESIAN_POINT('',(23.9949152542395,-66.3200448697526,-177.84995));
#185421=CARTESIAN_POINT('Origin',(24.200000000006,-66.7760495265862,-177.84995));
#185422=CARTESIAN_POINT('',(24.4906779661044,-66.0942982743985,-177.84995));
#185423=CARTESIAN_POINT('Origin',(0.,-12.9675000200281,-177.84995));
#185424=CARTESIAN_POINT('Origin',(24.7000000000027,-66.5483734731538,-177.84995));
#185425=CARTESIAN_POINT('Ctrl Pts',(25.166383622031,-65.7775666303703,-177.581785882201));
#185426=CARTESIAN_POINT('Ctrl Pts',(24.9516549782085,-65.8798945343463,
-177.298823774072));
#185427=CARTESIAN_POINT('Ctrl Pts',(25.0407404589729,-66.228934721057,-177.2158679411));
#185428=CARTESIAN_POINT('Ctrl Pts',(24.9795558812766,-65.8665984929838,
-177.757245548006));
#185429=CARTESIAN_POINT('Ctrl Pts',(24.8039770572177,-65.9493003143299,
-177.391803085524));
#185430=CARTESIAN_POINT('Ctrl Pts',(24.9465334973015,-66.3187224932389,
-177.303592864513));
#185431=CARTESIAN_POINT('Ctrl Pts',(24.7362442762044,-65.9810957924573,
-177.84994999494));
#185432=CARTESIAN_POINT('Ctrl Pts',(24.6278738771108,-66.0310529650264,
-177.399536111675));
#185433=CARTESIAN_POINT('Ctrl Pts',(24.8237985595108,-66.4342348178924,
-177.34995));
#185434=CARTESIAN_POINT('Ctrl Pts',(24.4906779661017,-66.0942982743997,
-177.84995));
#185435=CARTESIAN_POINT('Ctrl Pts',(24.4906779661017,-66.0942982743998,
-177.34995));
#185436=CARTESIAN_POINT('Ctrl Pts',(24.7,-66.548373473155,-177.34995));
#185437=CARTESIAN_POINT('Ctrl Pts',(25.166383622031,-65.7775666303703,-177.581785882201));
#185438=CARTESIAN_POINT('Ctrl Pts',(25.1415920409418,-65.7893809392764,
-177.605068947741));
#185439=CARTESIAN_POINT('Ctrl Pts',(25.1158854587622,-65.8016057771408,
-177.626825178572));
#185440=CARTESIAN_POINT('Ctrl Pts',(25.0893171817991,-65.8142137722865,
-177.64711393097));
#185441=CARTESIAN_POINT('Ctrl Pts',(25.067740038687,-65.8244532212351,-177.663591225101));
#185442=CARTESIAN_POINT('Ctrl Pts',(25.0455930316585,-65.8349461067523,
-177.67910099763));
#185443=CARTESIAN_POINT('Ctrl Pts',(25.0228835124146,-65.845687478185,-177.693662139191));
#185444=CARTESIAN_POINT('Ctrl Pts',(25.0179522289245,-65.8480199250782,
-177.696824034263));
#185445=CARTESIAN_POINT('Ctrl Pts',(25.0129943890564,-65.8503641038013,
-177.699941201796));
#185446=CARTESIAN_POINT('Ctrl Pts',(25.008000291213,-65.8527245791014,-177.703019463535));
#185447=CARTESIAN_POINT('Ctrl Pts',(24.9863105885612,-65.8629762820078,
-177.7163885612));
#185448=CARTESIAN_POINT('Ctrl Pts',(24.9639883366338,-65.8735110172848,
-177.728985587561));
#185449=CARTESIAN_POINT('Ctrl Pts',(24.9412183470617,-65.8842397535242,
-177.740690014451));
#185450=CARTESIAN_POINT('Ctrl Pts',(24.9235937056763,-65.8925441108073,
-177.749749584984));
#185451=CARTESIAN_POINT('Ctrl Pts',(24.9057018486688,-65.9009642216675,
-177.758274996804));
#185452=CARTESIAN_POINT('Ctrl Pts',(24.8876387414352,-65.9094542954476,
-177.766228663939));
#185453=CARTESIAN_POINT('Ctrl Pts',(24.8749962615991,-65.9153965502981,
-177.77179548448));
#185454=CARTESIAN_POINT('Ctrl Pts',(24.8622705967981,-65.9213727527722,
-177.777082364443));
#185455=CARTESIAN_POINT('Ctrl Pts',(24.8494947047088,-65.9273672725666,
-177.782082032575));
#185456=CARTESIAN_POINT('Ctrl Pts',(24.8190218618827,-65.9416653003081,
-177.794007156872));
#185457=CARTESIAN_POINT('Ctrl Pts',(24.788219590087,-65.9560881393781,-177.804322161695));
#185458=CARTESIAN_POINT('Ctrl Pts',(24.7570997784996,-65.9706278171961,
-177.813083012314));
#185459=CARTESIAN_POINT('Ctrl Pts',(24.7258330121357,-65.9852361546556,
-177.821885233647));
#185460=CARTESIAN_POINT('Ctrl Pts',(24.6942450261371,-65.9999627695759,
-177.829118717227));
#185461=CARTESIAN_POINT('Ctrl Pts',(24.6623322245521,-66.0148059325099,
-177.834790172697));
#185462=CARTESIAN_POINT('Ctrl Pts',(24.6308159404476,-66.029464668716,-177.840391160168));
#185463=CARTESIAN_POINT('Ctrl Pts',(24.5989822036623,-66.0442373978369,
-177.844468742953));
#185464=CARTESIAN_POINT('Ctrl Pts',(24.5668222618469,-66.0591237512874,
-177.846979582025));
#185465=CARTESIAN_POINT('Ctrl Pts',(24.5416418773983,-66.0707793725903,
-177.848945502656));
#185466=CARTESIAN_POINT('Ctrl Pts',(24.5162613043884,-66.0825047291482,
-177.849949999473));
#185467=CARTESIAN_POINT('Ctrl Pts',(24.4906779661043,-66.0942982743985,
-177.84995));
#185468=CARTESIAN_POINT('Origin',(26.4569673975197,-68.4857751744904,-179.64995));
#185469=CARTESIAN_POINT('',(25.166383622031,-65.7775666303703,-179.39995));
#185470=CARTESIAN_POINT('',(25.166383622031,-65.7775666303703,-179.64995));
#185471=CARTESIAN_POINT('Origin',(26.4569673975197,-68.4857751744904,-179.39995));
#185472=CARTESIAN_POINT('Ctrl Pts',(1.23783545400211,-71.4544141842476,
-176.238260704663));
#185473=CARTESIAN_POINT('Ctrl Pts',(0.721132232531162,-71.4643985224633,
-176.261250303005));
#185474=CARTESIAN_POINT('Ctrl Pts',(0.748751140187461,-71.9810613292915,
-176.259802934377));
#185475=CARTESIAN_POINT('Ctrl Pts',(1.25321977150542,-71.4540136938127,
-176.572353761973));
#185476=CARTESIAN_POINT('Ctrl Pts',(0.81377284711986,-71.4627451452814,
-176.500715567558));
#185477=CARTESIAN_POINT('Ctrl Pts',(0.756542354171283,-71.895138681302,
-176.530753994678));
#185478=CARTESIAN_POINT('Ctrl Pts',(1.19860343374803,-71.4555315991133,
-176.926629115674));
#185479=CARTESIAN_POINT('Ctrl Pts',(0.841287188135883,-71.4620507681087,
-176.792597259361));
#185480=CARTESIAN_POINT('Ctrl Pts',(0.729058399664653,-71.8180309468073,
-176.770579193097));
#185481=CARTESIAN_POINT('Ctrl Pts',(0.965096742606605,-71.4595547413853,
-177.27331690312));
#185482=CARTESIAN_POINT('Ctrl Pts',(0.713294749850913,-71.4632595324917,
-177.074901556755));
#185483=CARTESIAN_POINT('Ctrl Pts',(0.611402945447152,-71.7550490002612,
-176.992319359077));
#185484=CARTESIAN_POINT('Ctrl Pts',(0.916779319039344,-71.4603417028127,
-177.331361977737));
#185485=CARTESIAN_POINT('Ctrl Pts',(0.685390263968729,-71.4635316607953,
-177.121001585987));
#185486=CARTESIAN_POINT('Ctrl Pts',(0.587057849709363,-71.7450124422729,
-177.02878681156));
#185487=CARTESIAN_POINT('Ctrl Pts',(0.807976114834587,-71.4619457720088,
-177.435774845394));
#185488=CARTESIAN_POINT('Ctrl Pts',(0.61920619489495,-71.4641477944332,
-177.203686314583));
#185489=CARTESIAN_POINT('Ctrl Pts',(0.532234779142866,-71.7275925135231,
-177.093698009026));
#185490=CARTESIAN_POINT('Ctrl Pts',(0.746606781238387,-71.4627719946713,
-177.482505016316));
#185491=CARTESIAN_POINT('Ctrl Pts',(0.580314974840451,-71.4644967134863,
-177.240847062286));
#185492=CARTESIAN_POINT('Ctrl Pts',(0.501311469386272,-71.7201585461063,
-177.122354454569));
#185493=CARTESIAN_POINT('Ctrl Pts',(0.521249492735721,-71.4653981046342,
-177.613426214874));
#185494=CARTESIAN_POINT('Ctrl Pts',(0.434920719988867,-71.4656764551474,
-177.343994523926));
#185495=CARTESIAN_POINT('Ctrl Pts',(0.387756225423206,-71.6999617297923,
-177.202103665492));
#185496=CARTESIAN_POINT('Ctrl Pts',(0.330983066508931,-71.4669014486956,
-177.656473197042));
#185497=CARTESIAN_POINT('Ctrl Pts',(0.304420776205656,-71.4665113043489,
-177.379037765856));
#185498=CARTESIAN_POINT('Ctrl Pts',(0.291876596246233,-71.6944798744154,
-177.227398366312));
#185499=CARTESIAN_POINT('Ctrl Pts',(0.141805636875531,-71.4673186419509,
-177.630934590095));
#185500=CARTESIAN_POINT('Ctrl Pts',(0.176963829132147,-71.4669036380682,
-177.358245566005));
#185501=CARTESIAN_POINT('Ctrl Pts',(0.196547809098401,-71.698807761693,
-177.212077768614));
#185502=CARTESIAN_POINT('',(0.249751305446096,-71.4669668918333,-177.637584354353));
#185503=CARTESIAN_POINT('Origin',(0.25188593198836,-71.966962335182,-177.637584354353));
#185504=CARTESIAN_POINT('',(1.23940677966098,-71.4543692372681,-176.344247731786));
#185505=CARTESIAN_POINT('Ctrl Pts',(1.23940677966098,-71.4543692372681,
-176.344247731786));
#185506=CARTESIAN_POINT('Ctrl Pts',(1.23940677966098,-71.4543692372681,
-176.517170194872));
#185507=CARTESIAN_POINT('Ctrl Pts',(1.22017060769392,-71.4547863693157,
-176.675572408682));
#185508=CARTESIAN_POINT('Ctrl Pts',(1.1624603379848,-71.4559523518045,-176.891395355483));
#185509=CARTESIAN_POINT('Ctrl Pts',(1.12639114428662,-71.4566677449925,
-176.993861735405));
#185510=CARTESIAN_POINT('Ctrl Pts',(1.07168494602295,-71.4576871945188,
-177.103876931726));
#185511=CARTESIAN_POINT('Ctrl Pts',(1.04117534582081,-71.4582351623851,
-177.156502301489));
#185512=CARTESIAN_POINT('Ctrl Pts',(1.02742339564269,-71.4584772975563,
-177.178545553874));
#185513=CARTESIAN_POINT('Ctrl Pts',(1.01810511453015,-71.4586402353632,
-177.193127616017));
#185514=CARTESIAN_POINT('Ctrl Pts',(1.01411410582161,-71.4587096452574,
-177.199252649036));
#185515=CARTESIAN_POINT('Ctrl Pts',(0.964139403507473,-71.4595713554461,
-177.273834478609));
#185516=CARTESIAN_POINT('Ctrl Pts',(0.890131256064229,-71.4607724720151,
-177.362452390043));
#185517=CARTESIAN_POINT('Ctrl Pts',(0.805059306817399,-71.4619677502115,
-177.434833509482));
#185518=CARTESIAN_POINT('Ctrl Pts',(0.745885964242655,-71.4627522175639,
-177.479479413109));
#185519=CARTESIAN_POINT('Ctrl Pts',(0.716981135486837,-71.463116020377,
-177.498882122092));
#185520=CARTESIAN_POINT('Ctrl Pts',(0.547198059716821,-71.4650984803593,
-177.598036775321));
#185521=CARTESIAN_POINT('Ctrl Pts',(0.40277284172198,-71.4663135982139,
-177.637660542527));
#185522=CARTESIAN_POINT('Ctrl Pts',(0.249751305446096,-71.4669668918333,
-177.637584354353));
#185523=CARTESIAN_POINT('Origin',(1.24999999999996,-71.9542570083556,-176.344247731786));
#185524=CARTESIAN_POINT('Origin',(1.24999999999996,-71.9542570083556,-179.64995));
#185525=CARTESIAN_POINT('',(1.23940677966098,-71.4543692372681,-179.64995));
#185526=CARTESIAN_POINT('Origin',(0.,-12.9675000200281,-171.871644662643));
#185527=CARTESIAN_POINT('Origin',(0.,-12.9675000200281,-171.871644662643));
#185528=CARTESIAN_POINT('Origin',(6.9,-71.5626363369615,-179.64995));
#185529=CARTESIAN_POINT('',(6.84152542372878,-71.066067385123,-176.485569595297));
#185530=CARTESIAN_POINT('Origin',(6.9,-71.5626363369615,-176.485569595297));
#185531=CARTESIAN_POINT('',(6.84152542372878,-71.066067385123,-179.64995));
#185532=CARTESIAN_POINT('Ctrl Pts',(7.86991817520074,-70.935718794764,-177.700825662764));
#185533=CARTESIAN_POINT('Ctrl Pts',(7.87530650495354,-70.9349872609141,
-177.368681451895));
#185534=CARTESIAN_POINT('Ctrl Pts',(7.91859121655422,-71.2381488509314,
-177.239961484007));
#185535=CARTESIAN_POINT('Ctrl Pts',(7.72465595207765,-70.9554399770617,
-177.698405110518));
#185536=CARTESIAN_POINT('Ctrl Pts',(7.7814869526158,-70.9477382671599,-177.362180852783));
#185537=CARTESIAN_POINT('Ctrl Pts',(7.84535391894273,-71.2544423085659,
-177.236091643156));
#185538=CARTESIAN_POINT('Ctrl Pts',(7.57909439591914,-70.9746058127342,
-177.660005031717));
#185539=CARTESIAN_POINT('Ctrl Pts',(7.68873678647519,-70.9601668953933,
-177.328725158091));
#185540=CARTESIAN_POINT('Ctrl Pts',(7.77193648886645,-71.274739088698,-177.212399058377));
#185541=CARTESIAN_POINT('Ctrl Pts',(7.32049271153216,-71.0078082615326,
-177.524965998388));
#185542=CARTESIAN_POINT('Ctrl Pts',(7.53187921075035,-70.98103712284,-177.221702886533));
#185543=CARTESIAN_POINT('Ctrl Pts',(7.64153051403658,-71.3201342851139,
-177.131947985374));
#185544=CARTESIAN_POINT('Ctrl Pts',(7.20559474882705,-71.0221114770482,
-177.427818678983));
#185545=CARTESIAN_POINT('Ctrl Pts',(7.46634030528468,-70.9896817811965,
-177.14630380948));
#185546=CARTESIAN_POINT('Ctrl Pts',(7.58359051438092,-71.3455846992379,
-177.074841178091));
#185547=CARTESIAN_POINT('Ctrl Pts',(7.0224958330043,-71.0445441888331,-177.19789774704));
#185548=CARTESIAN_POINT('Ctrl Pts',(7.3754100247025,-71.0018071186815,-176.974926941462));
#185549=CARTESIAN_POINT('Ctrl Pts',(7.49125858243999,-71.4004398176271,
-176.937641167035));
#185550=CARTESIAN_POINT('Ctrl Pts',(6.95330228061017,-71.0528136932555,
-177.064676392973));
#185551=CARTESIAN_POINT('Ctrl Pts',(7.35016748493995,-71.0052818262832,
-176.876651794266));
#185552=CARTESIAN_POINT('Ctrl Pts',(7.45636610731683,-71.4300660132009,
-176.85726439743));
#185553=CARTESIAN_POINT('Ctrl Pts',(6.86278910799687,-71.0635773642165,
-176.782076502575));
#185554=CARTESIAN_POINT('Ctrl Pts',(7.34226626007839,-71.0069144630253,
-176.677678014477));
#185555=CARTESIAN_POINT('Ctrl Pts',(7.41072271257901,-71.4935573295699,
-176.680998879949));
#185556=CARTESIAN_POINT('Ctrl Pts',(6.8415254209523,-71.06606738545,-176.633819401763));
#185557=CARTESIAN_POINT('Ctrl Pts',(7.36167840976143,-71.0048156182874,
-176.575906600101));
#185558=CARTESIAN_POINT('Ctrl Pts',(7.4,-71.5272255526701,-176.585813210379));
#185559=CARTESIAN_POINT('Ctrl Pts',(6.84152542372878,-71.066067385123,-176.485569595297));
#185560=CARTESIAN_POINT('Ctrl Pts',(7.40000000000002,-71.0003029749946,
-176.485569595297));
#185561=CARTESIAN_POINT('Ctrl Pts',(7.4,-71.5626363369615,-176.485569595297));
#185562=CARTESIAN_POINT('',(7.86991817520075,-70.935718794764,-177.700825662763));
#185563=CARTESIAN_POINT('Origin',(7.93718243310846,-71.4311736560866,-177.700825662763));
#185564=CARTESIAN_POINT('Ctrl Pts',(7.86991817520075,-70.935718794764,-177.700825662763));
#185565=CARTESIAN_POINT('Ctrl Pts',(7.84145915028903,-70.9395824669992,
-177.700351440663));
#185566=CARTESIAN_POINT('Ctrl Pts',(7.81325306985417,-70.9433890026599,
-177.698505055736));
#185567=CARTESIAN_POINT('Ctrl Pts',(7.78529419147432,-70.9471417642783,
-177.695385832037));
#185568=CARTESIAN_POINT('Ctrl Pts',(7.7769616359882,-70.9482601959259,-177.694456213038));
#185569=CARTESIAN_POINT('Ctrl Pts',(7.76865098308067,-70.9493738524319,
-177.693413186647));
#185570=CARTESIAN_POINT('Ctrl Pts',(7.76036198762536,-70.9504828203398,
-177.692258509338));
#185571=CARTESIAN_POINT('Ctrl Pts',(7.7317172038824,-70.9543151479204,-177.688268221013));
#185572=CARTESIAN_POINT('Ctrl Pts',(7.7033289936208,-70.9580918229642,-177.682948350417));
#185573=CARTESIAN_POINT('Ctrl Pts',(7.675186105217,-70.9618160028387,-177.676335993945));
#185574=CARTESIAN_POINT('Ctrl Pts',(7.66343218081142,-70.9633714127913,
-177.673574332207));
#185575=CARTESIAN_POINT('Ctrl Pts',(7.65172493394877,-70.964917145146,-177.670587723933));
#185576=CARTESIAN_POINT('Ctrl Pts',(7.64004659107783,-70.9664556187766,
-177.667371199649));
#185577=CARTESIAN_POINT('Ctrl Pts',(7.60920468562832,-70.9705186488466,
-177.65887652374));
#185578=CARTESIAN_POINT('Ctrl Pts',(7.57859346491502,-70.9745271017102,
-177.648778373647));
#185579=CARTESIAN_POINT('Ctrl Pts',(7.54854310099584,-70.9784389453262,
-177.637166030246));
#185580=CARTESIAN_POINT('Ctrl Pts',(7.52067144326505,-70.9820671731458,
-177.626395602919));
#185581=CARTESIAN_POINT('Ctrl Pts',(7.49328227206074,-70.9856123005526,
-177.614321694518));
#185582=CARTESIAN_POINT('Ctrl Pts',(7.46663887751155,-70.9890415496572,
-177.601070367657));
#185583=CARTESIAN_POINT('Ctrl Pts',(7.46098971645219,-70.9897686484685,
-177.598260707666));
#185584=CARTESIAN_POINT('Ctrl Pts',(7.45537399181972,-70.9904905521545,
-177.595398277761));
#185585=CARTESIAN_POINT('Ctrl Pts',(7.44979405295273,-70.9912069730377,
-177.59248453496));
#185586=CARTESIAN_POINT('Ctrl Pts',(7.44926963945517,-70.9912743036645,
-177.59221069575));
#185587=CARTESIAN_POINT('Ctrl Pts',(7.44874551143164,-70.9913415902563,
-177.591936395013));
#185588=CARTESIAN_POINT('Ctrl Pts',(7.44822167031192,-70.9914088326578,
-177.591661634332));
#185589=CARTESIAN_POINT('Ctrl Pts',(7.36341668565129,-71.0022947494199,
-177.547180446295));
#185590=CARTESIAN_POINT('Ctrl Pts',(7.28492054201756,-71.0121779828271,
-177.489997024811));
#185591=CARTESIAN_POINT('Ctrl Pts',(7.21521421994463,-71.0208423096966,
-177.423514614651));
#185592=CARTESIAN_POINT('Ctrl Pts',(7.17900585541714,-71.0253429216403,
-177.388980884135));
#185593=CARTESIAN_POINT('Ctrl Pts',(7.14516858273338,-71.0295147031061,
-177.35193750338));
#185594=CARTESIAN_POINT('Ctrl Pts',(7.11404633506787,-71.0333277050162,
-177.3128573618));
#185595=CARTESIAN_POINT('Ctrl Pts',(7.11356074608127,-71.033387197883,-177.312247608721));
#185596=CARTESIAN_POINT('Ctrl Pts',(7.11307579006788,-71.0334466073515,
-177.311637347152));
#185597=CARTESIAN_POINT('Ctrl Pts',(7.11259146723154,-71.0335059334348,
-177.311026578643));
#185598=CARTESIAN_POINT('Ctrl Pts',(7.05806005587485,-71.0401856412932,
-177.242258256468));
#185599=CARTESIAN_POINT('Ctrl Pts',(7.01156780675731,-71.0458068303084,
-177.167083119785));
#185600=CARTESIAN_POINT('Ctrl Pts',(6.97337953735775,-71.0503909874143,
-177.087652956309));
#185601=CARTESIAN_POINT('Ctrl Pts',(6.94786514373312,-71.0534537601107,
-177.034583977576));
#185602=CARTESIAN_POINT('Ctrl Pts',(6.92605814997056,-71.0560535184279,
-176.979614410751));
#185603=CARTESIAN_POINT('Ctrl Pts',(6.90804579110999,-71.058195517224,-176.923376416061));
#185604=CARTESIAN_POINT('Ctrl Pts',(6.90788807893848,-71.0582142720847,
-176.922884008801));
#185605=CARTESIAN_POINT('Ctrl Pts',(6.90773065840123,-71.0582329917957,
-176.922391517884));
#185606=CARTESIAN_POINT('Ctrl Pts',(6.90757352937676,-71.0582516763749,
-176.921898943596));
#185607=CARTESIAN_POINT('Ctrl Pts',(6.89200677785444,-71.0601027551398,
-176.873099674503));
#185608=CARTESIAN_POINT('Ctrl Pts',(6.87933106860591,-71.0616054747707,
-176.82359063585));
#185609=CARTESIAN_POINT('Ctrl Pts',(6.86938539001924,-71.0627821611452,
-176.773553029938));
#185610=CARTESIAN_POINT('Ctrl Pts',(6.85903549341787,-71.0640066710871,
-176.72148176674));
#185611=CARTESIAN_POINT('Ctrl Pts',(6.85164206564097,-71.0648780949575,
-176.668837206011));
#185612=CARTESIAN_POINT('Ctrl Pts',(6.84707944646843,-71.065414925157,-176.615812182358));
#185613=CARTESIAN_POINT('Ctrl Pts',(6.84336254226504,-71.0658522499368,
-176.572615736228));
#185614=CARTESIAN_POINT('Ctrl Pts',(6.84152542372878,-71.066067385123,-176.529166339213));
#185615=CARTESIAN_POINT('Ctrl Pts',(6.84152542372878,-71.066067385123,-176.485569595297));
#185616=CARTESIAN_POINT('Ctrl Pts',(7.91859121655416,-71.2381488509313,
-177.239961484006));
#185617=CARTESIAN_POINT('Ctrl Pts',(7.87530650495358,-70.9349872609141,
-177.368681451894));
#185618=CARTESIAN_POINT('Ctrl Pts',(7.86991817520098,-70.935718794764,-177.700825662763));
#185619=CARTESIAN_POINT('Ctrl Pts',(8.08517348178868,-71.21877443556,-177.241356202481));
#185620=CARTESIAN_POINT('Ctrl Pts',(8.04094447940713,-70.9124841487064,
-177.368907517599));
#185621=CARTESIAN_POINT('Ctrl Pts',(8.03499989482399,-70.9133068653807,
-177.703576433696));
#185622=CARTESIAN_POINT('Ctrl Pts',(8.25170137526425,-71.1987909763519,
-177.242846915875));
#185623=CARTESIAN_POINT('Ctrl Pts',(8.20613182703653,-70.889318969813,-177.369144269326));
#185624=CARTESIAN_POINT('Ctrl Pts',(8.19998119128136,-70.8901904062617,
-177.706427680957));
#185625=CARTESIAN_POINT('Ctrl Pts',(8.41817827172741,-71.1781985203567,
-177.244444626904));
#185626=CARTESIAN_POINT('Ctrl Pts',(8.3707824215504,-70.8655141261623,-177.369392503912));
#185627=CARTESIAN_POINT('Ctrl Pts',(8.36486199647703,-70.866369471684,-177.709383806605));
#185628=CARTESIAN_POINT('',(8.36486199647649,-70.8663694716841,-177.709383806605));
#185629=CARTESIAN_POINT('Origin',(0.0230368111365542,-14.1525797472871,
-185.975887612657));
#185630=CARTESIAN_POINT('Origin',(8.43635654345535,-71.3612316037495,-177.709383806605));
#185631=CARTESIAN_POINT('Ctrl Pts',(9.31194471985222,-70.7216281469411,
-176.521703250262));
#185632=CARTESIAN_POINT('Ctrl Pts',(8.86316466557432,-70.7927544609078,
-176.577904846168));
#185633=CARTESIAN_POINT('Ctrl Pts',(8.89511833477312,-71.2491795873182,
-176.583278767617));
#185634=CARTESIAN_POINT('Ctrl Pts',(9.33426782231391,-70.7179921647292,
-176.707671693767));
#185635=CARTESIAN_POINT('Ctrl Pts',(8.91524414222188,-70.7846676236483,
-176.691761787883));
#185636=CARTESIAN_POINT('Ctrl Pts',(8.90639454875205,-71.2042306696945,
-176.699592289102));
#185637=CARTESIAN_POINT('Ctrl Pts',(9.31861749655483,-70.7205733106781,
-176.894655311153));
#185638=CARTESIAN_POINT('Ctrl Pts',(8.93334931956903,-70.7817419161099,
-176.820727622377));
#185639=CARTESIAN_POINT('Ctrl Pts',(8.8985376639078,-71.1725272604627,-176.808271319893));
#185640=CARTESIAN_POINT('Ctrl Pts',(9.21240345628522,-70.7375942109218,
-177.194427742108));
#185641=CARTESIAN_POINT('Ctrl Pts',(8.89508753920652,-70.7873478881673,
-177.027386013335));
#185642=CARTESIAN_POINT('Ctrl Pts',(8.84506581279844,-71.1392355158483,
-176.976329963003));
#185643=CARTESIAN_POINT('Ctrl Pts',(9.14614340920233,-70.7481724076873,
-177.308522414764));
#185644=CARTESIAN_POINT('Ctrl Pts',(8.86032021978074,-70.7925702591893,
-177.107065661507));
#185645=CARTESIAN_POINT('Ctrl Pts',(8.81169873029936,-71.1320753660863,
-177.038360991276));
#185646=CARTESIAN_POINT('Ctrl Pts',(8.84766881369401,-70.7949534600523,
-177.640884592286));
#185647=CARTESIAN_POINT('Ctrl Pts',(8.68613018229932,-70.8186420493741,
-177.333034085865));
#185648=CARTESIAN_POINT('Ctrl Pts',(8.66138036999789,-71.1267167292917,
-177.215887692752));
#185649=CARTESIAN_POINT('Ctrl Pts',(8.52372344713472,-70.8442550810108,
-177.757261114079));
#185650=CARTESIAN_POINT('Ctrl Pts',(8.4669598281481,-70.8511504969647,-177.410277645602));
#185651=CARTESIAN_POINT('Ctrl Pts',(8.49812639039677,-71.1551635236587,
-177.272472653023));
#185652=CARTESIAN_POINT('Ctrl Pts',(8.2060354143041,-70.8890492358094,-177.693193871778));
#185653=CARTESIAN_POINT('Ctrl Pts',(8.27002543687626,-70.8792234239869,
-177.351033919866));
#185654=CARTESIAN_POINT('Ctrl Pts',(8.33823067532437,-71.1985789270941,
-177.232285602531));
#185655=CARTESIAN_POINT('',(9.32033898305081,-70.7202599648223,-176.681036188741));
#185656=CARTESIAN_POINT('Ctrl Pts',(9.32033898305081,-70.7202599648223,
-176.681036188741));
#185657=CARTESIAN_POINT('Ctrl Pts',(9.3203389830508,-70.7202599648223,-176.749135893056));
#185658=CARTESIAN_POINT('Ctrl Pts',(9.31498446872546,-70.7211248588454,
-176.815409677274));
#185659=CARTESIAN_POINT('Ctrl Pts',(9.30427471976772,-70.7228501785986,
-176.879857541395));
#185660=CARTESIAN_POINT('Ctrl Pts',(9.29891984528884,-70.7237128384752,
-176.912081473456));
#185661=CARTESIAN_POINT('Ctrl Pts',(9.29222613967396,-70.7247904651451,
-176.943848925492));
#185662=CARTESIAN_POINT('Ctrl Pts',(9.28419337855619,-70.7260816621493,
-176.975159897504));
#185663=CARTESIAN_POINT('Ctrl Pts',(9.27616061743841,-70.7273728591534,
-177.006470869516));
#185664=CARTESIAN_POINT('Ctrl Pts',(9.26728977127031,-70.7287973499507,
-177.035903622681));
#185665=CARTESIAN_POINT('Ctrl Pts',(9.25607761587008,-70.7305940089151,
-177.067723373468));
#185666=CARTESIAN_POINT('Ctrl Pts',(9.23365330506961,-70.7341873268439,
-177.131362875041));
#185667=CARTESIAN_POINT('Ctrl Pts',(9.20602077392941,-70.7386025493298,
-177.191198784361));
#185668=CARTESIAN_POINT('Ctrl Pts',(9.17317647543608,-70.74381725599,-177.247231101426));
#185669=CARTESIAN_POINT('Ctrl Pts',(9.14033217694275,-70.7490319626502,
-177.303263418491));
#185670=CARTESIAN_POINT('Ctrl Pts',(9.10348192879145,-70.7548571469264,
-177.354142742939));
#185671=CARTESIAN_POINT('Ctrl Pts',(9.05900346753984,-70.7618289474852,
-177.403917275858));
#185672=CARTESIAN_POINT('Ctrl Pts',(8.98900499154369,-70.7728008966113,
-177.48225050389));
#185673=CARTESIAN_POINT('Ctrl Pts',(8.90992354066234,-70.7850704087956,
-177.545955215629));
#185674=CARTESIAN_POINT('Ctrl Pts',(8.82049689367651,-70.7987098858838,
-177.595581650182));
#185675=CARTESIAN_POINT('Ctrl Pts',(8.79627650488861,-70.802404013407,-177.609022515736));
#185676=CARTESIAN_POINT('Ctrl Pts',(8.77129720830665,-70.8061983474297,
-177.621430672585));
#185677=CARTESIAN_POINT('Ctrl Pts',(8.74553383831428,-70.810093650353,-177.632817052588));
#185678=CARTESIAN_POINT('Ctrl Pts',(8.6246468180102,-70.8283712112355,-177.686244284778));
#185679=CARTESIAN_POINT('Ctrl Pts',(8.49776106948925,-70.8471690552384,
-177.711766536117));
#185680=CARTESIAN_POINT('Ctrl Pts',(8.36486199647649,-70.8663694716841,
-177.709383806605));
#185681=CARTESIAN_POINT('Origin',(9.4,-71.2138732976838,-176.681036188741));
#185682=CARTESIAN_POINT('Origin',(9.4,-71.2138732976838,-179.64995));
#185683=CARTESIAN_POINT('',(9.32033898305081,-70.7202599648223,-179.64995));
#185684=CARTESIAN_POINT('Origin',(0.,-12.9675000200281,-171.871644662643));
#185685=CARTESIAN_POINT('Origin',(0.,-12.9675000200281,-171.871644662643));
#185686=CARTESIAN_POINT('Origin',(15.05,-70.015703322148,-179.64995));
#185687=CARTESIAN_POINT('',(14.9224576271186,-69.53224397213,-176.84995));
#185688=CARTESIAN_POINT('Origin',(15.05,-70.015703322148,-176.84995));
#185689=CARTESIAN_POINT('',(14.9224576271186,-69.5322439721301,-179.64995));
#185690=CARTESIAN_POINT('Ctrl Pts',(16.0658981859834,-69.2181101857427,
-177.83843816103));
#185691=CARTESIAN_POINT('Ctrl Pts',(16.0005358602646,-69.2358256555765,
-177.36456142736));
#185692=CARTESIAN_POINT('Ctrl Pts',(16.1265631343295,-69.6989087749272,
-177.34368264398));
#185693=CARTESIAN_POINT('Ctrl Pts',(15.7646054310406,-69.3044096982964,
-177.889038147364));
#185694=CARTESIAN_POINT('Ctrl Pts',(15.8105690999498,-69.289401681716,-177.348580470172));
#185695=CARTESIAN_POINT('Ctrl Pts',(15.9746754260325,-69.785917294809,-177.368934418229));
#185696=CARTESIAN_POINT('Ctrl Pts',(15.4414114400423,-69.3932567531528,
-177.784709035369));
#185697=CARTESIAN_POINT('Ctrl Pts',(15.682807240394,-69.3252572316702,-177.238537996438));
#185698=CARTESIAN_POINT('Ctrl Pts',(15.8119354596535,-69.8753938355129,
-177.316789718218));
#185699=CARTESIAN_POINT('Ctrl Pts',(14.9965996919493,-69.5131029391016,
-177.344861768588));
#185700=CARTESIAN_POINT('Ctrl Pts',(15.549956079405,-69.3641921133352,-177.008091533137));
#185701=CARTESIAN_POINT('Ctrl Pts',(15.5879032634866,-69.9961227595722,
-177.097095005978));
#185702=CARTESIAN_POINT('Ctrl Pts',(14.879290383782,-69.5434999409872,-177.013244119206));
#185703=CARTESIAN_POINT('Ctrl Pts',(15.547119708319,-69.3663509905523,-176.898252015644));
#185704=CARTESIAN_POINT('Ctrl Pts',(15.5288419201426,-70.0267333379905,
-176.931492946677));
#185705=CARTESIAN_POINT('Ctrl Pts',(14.935107290865,-69.5289450233885,-176.686865358248));
#185706=CARTESIAN_POINT('Ctrl Pts',(15.5511428301757,-69.3646343509962,
-176.799766495381));
#185707=CARTESIAN_POINT('Ctrl Pts',(15.5569471014035,-70.0120745403484,
-176.768510892379));
#185708=CARTESIAN_POINT('',(15.9139830508475,-69.2613286645371,-177.84995));
#185709=CARTESIAN_POINT('Origin',(16.0500000000002,-69.7424724991055,-177.84995));
#185710=CARTESIAN_POINT('Ctrl Pts',(15.9139830508475,-69.2613286645371,
-177.84995));
#185711=CARTESIAN_POINT('Ctrl Pts',(15.7965712698714,-69.2945203862127,
-177.84995));
#185712=CARTESIAN_POINT('Ctrl Pts',(15.6837640763244,-69.3260183464345,
-177.829973206133));
#185713=CARTESIAN_POINT('Ctrl Pts',(15.5736771291949,-69.3564225197141,
-177.789235002346));
#185714=CARTESIAN_POINT('Ctrl Pts',(15.5622378038961,-69.3595818700064,
-177.78500182505));
#185715=CARTESIAN_POINT('Ctrl Pts',(15.5508278378011,-69.3627293657972,
-177.780544473358));
#185716=CARTESIAN_POINT('Ctrl Pts',(15.5394451078152,-69.3658656500816,
-177.77586206693));
#185717=CARTESIAN_POINT('Ctrl Pts',(15.4185200786613,-69.3991841307096,
-177.726118276597));
#185718=CARTESIAN_POINT('Ctrl Pts',(15.3111353387459,-69.4283571390207,
-177.654683080351));
#185719=CARTESIAN_POINT('Ctrl Pts',(15.2182598314156,-69.453379385614,-177.562452499716));
#185720=CARTESIAN_POINT('Ctrl Pts',(15.14774018584,-69.4723785815483,-177.492422541931));
#185721=CARTESIAN_POINT('Ctrl Pts',(15.0892668418245,-69.4879953157288,
-177.413800201241));
#185722=CARTESIAN_POINT('Ctrl Pts',(15.0422976393026,-69.5004928802211,
-177.325216521744));
#185723=CARTESIAN_POINT('Ctrl Pts',(15.0274076467375,-69.5044548091529,
-177.297134070728));
#185724=CARTESIAN_POINT('Ctrl Pts',(15.0136737030358,-69.5081028798345,
-177.268050513167));
#185725=CARTESIAN_POINT('Ctrl Pts',(15.0010782474499,-69.5114444474722,
-177.237922234316));
#185726=CARTESIAN_POINT('Ctrl Pts',(14.9647660441677,-69.5210780556028,
-177.151063590839));
#185727=CARTESIAN_POINT('Ctrl Pts',(14.9410265060011,-69.5273431954927,
-177.062202234145));
#185728=CARTESIAN_POINT('Ctrl Pts',(14.9298722292227,-69.5302873914005,
-176.971338164234));
#185729=CARTESIAN_POINT('Ctrl Pts',(14.9249529310265,-69.5315858509875,
-176.931264974005));
#185730=CARTESIAN_POINT('Ctrl Pts',(14.9224813123119,-69.5322377236921,
-176.890802252594));
#185731=CARTESIAN_POINT('Ctrl Pts',(14.9224576271186,-69.53224397213,-176.84995));
#185732=CARTESIAN_POINT('Origin',(0.,-12.9675000200281,-177.84995));
#185733=CARTESIAN_POINT('',(16.4097457627119,-69.1188156235219,-177.84995));
#185734=CARTESIAN_POINT('Origin',(0.,-12.9675000200281,-177.84995));
#185735=CARTESIAN_POINT('Origin',(16.55,-69.5987413979107,-177.84995));
#185736=CARTESIAN_POINT('Ctrl Pts',(17.3880466788383,-68.8236353260961,
-176.690807598274));
#185737=CARTESIAN_POINT('Ctrl Pts',(17.038994500873,-68.9322836414647,-176.752287790566));
#185738=CARTESIAN_POINT('Ctrl Pts',(17.0433452950906,-69.3023910050376,
-176.770445463412));
#185739=CARTESIAN_POINT('Ctrl Pts',(17.4191280954739,-68.8139047586067,
-176.874276825325));
#185740=CARTESIAN_POINT('Ctrl Pts',(17.0626089168816,-68.9251254936702,
-176.864255982328));
#185741=CARTESIAN_POINT('Ctrl Pts',(17.0589896637034,-69.292572888558,-176.862105468243));
#185742=CARTESIAN_POINT('Ctrl Pts',(17.394639930152,-68.8216149564082,-177.068700056101));
#185743=CARTESIAN_POINT('Ctrl Pts',(17.0432848595555,-68.9310044443038,
-176.986133124776));
#185744=CARTESIAN_POINT('Ctrl Pts',(17.0466665865239,-69.3003518068395,
-176.959226205544));
#185745=CARTESIAN_POINT('Ctrl Pts',(17.271522613636,-68.8597838444499,-177.362008470827));
#185746=CARTESIAN_POINT('Ctrl Pts',(16.9544868301422,-68.9577361986752,
-177.158772927448));
#185747=CARTESIAN_POINT('Ctrl Pts',(16.9846783298497,-69.3388689248328,
-177.105787340716));
#185748=CARTESIAN_POINT('Ctrl Pts',(17.1958580434816,-68.8831664553272,
-177.473129011102));
#185749=CARTESIAN_POINT('Ctrl Pts',(16.8998209438857,-68.9741481933376,
-177.221234746742));
#185750=CARTESIAN_POINT('Ctrl Pts',(16.9465808939194,-69.3624640417944,
-177.161324454504));
#185751=CARTESIAN_POINT('Ctrl Pts',(17.0115440055365,-68.9395167543114,
-177.65527913718));
#185752=CARTESIAN_POINT('Ctrl Pts',(16.7731937352441,-69.0119018737478,
-177.313591442829));
#185753=CARTESIAN_POINT('Ctrl Pts',(16.8537504063022,-69.4193302850168,
-177.252399550336));
#185754=CARTESIAN_POINT('Ctrl Pts',(16.901371584146,-68.9729353808306,-177.727810792065));
#185755=CARTESIAN_POINT('Ctrl Pts',(16.6994218041251,-69.0337699903486,
-177.343918516311));
#185756=CARTESIAN_POINT('Ctrl Pts',(16.7982523396534,-69.4530549873958,
-177.288688678996));
#185757=CARTESIAN_POINT('Ctrl Pts',(16.618372268784,-69.0576898916785,-177.843950929236));
#185758=CARTESIAN_POINT('Ctrl Pts',(16.521465396758,-69.0861983475692,-177.375991886255));
#185759=CARTESIAN_POINT('Ctrl Pts',(16.6556481050719,-69.5385895805552,
-177.346851666338));
#185760=CARTESIAN_POINT('Ctrl Pts',(16.4326032723997,-69.1124772258283,
-177.866548824772));
#185761=CARTESIAN_POINT('Ctrl Pts',(16.4142810526698,-69.1175007347054,
-177.359511295888));
#185762=CARTESIAN_POINT('Ctrl Pts',(16.5619959483196,-69.5938880549685,
-177.358242713103));
#185763=CARTESIAN_POINT('Ctrl Pts',(16.2582586240097,-69.1628382672821,
-177.837630803223));
#185764=CARTESIAN_POINT('Ctrl Pts',(16.3327830474041,-69.141293341008,-177.320021141446));
#185765=CARTESIAN_POINT('Ctrl Pts',(16.4740613080989,-69.6447181033276,
-177.343862647942));
#185766=CARTESIAN_POINT('',(17.4012711864406,-68.8194987407181,-176.84995));
#185767=CARTESIAN_POINT('Ctrl Pts',(17.4012711864406,-68.8194987407181,
-176.84995));
#185768=CARTESIAN_POINT('Ctrl Pts',(17.4012711797275,-68.8194987428096,
-176.887694684675));
#185769=CARTESIAN_POINT('Ctrl Pts',(17.3991058038741,-68.8201748588276,
-176.925251096234));
#185770=CARTESIAN_POINT('Ctrl Pts',(17.3948976591097,-68.8214863041692,
-176.962447012708));
#185771=CARTESIAN_POINT('Ctrl Pts',(17.3906053585138,-68.8228239762163,
-177.000386785074));
#185772=CARTESIAN_POINT('Ctrl Pts',(17.3841876175728,-68.8248226995135,
-177.037952567699));
#185773=CARTESIAN_POINT('Ctrl Pts',(17.3757224555706,-68.8274555088436,
-177.074968429999));
#185774=CARTESIAN_POINT('Ctrl Pts',(17.3672590966796,-68.8300877573754,
-177.11197640778));
#185775=CARTESIAN_POINT('Ctrl Pts',(17.356748909814,-68.83335391904,-177.148435801524));
#185776=CARTESIAN_POINT('Ctrl Pts',(17.3442218215212,-68.837241948804,-177.184161144092));
#185777=CARTESIAN_POINT('Ctrl Pts',(17.3378147381211,-68.839230513934,-177.202433167405));
#185778=CARTESIAN_POINT('Ctrl Pts',(17.3308793073379,-68.8413819840089,
-177.22051291325));
#185779=CARTESIAN_POINT('Ctrl Pts',(17.3234150119904,-68.8436961361599,
-177.238373157981));
#185780=CARTESIAN_POINT('Ctrl Pts',(17.323216781765,-68.8437575933882,-177.238847474735));
#185781=CARTESIAN_POINT('Ctrl Pts',(17.3230181873272,-68.8438191626283,
-177.239321615502));
#185782=CARTESIAN_POINT('Ctrl Pts',(17.3228192288394,-68.8438808438229,
-177.23979557955));
#185783=CARTESIAN_POINT('Ctrl Pts',(17.2882744024223,-68.8545904455369,
-177.322089157366));
#185784=CARTESIAN_POINT('Ctrl Pts',(17.2426551334793,-68.8686994417092,
-177.39942640593));
#185785=CARTESIAN_POINT('Ctrl Pts',(17.1883023464386,-68.8854065190396,
-177.46904491663));
#185786=CARTESIAN_POINT('Ctrl Pts',(17.1624825557959,-68.8933430621758,
-177.502116548629));
#185787=CARTESIAN_POINT('Ctrl Pts',(17.1346920798654,-68.9018658361706,
-177.533445664936));
#185788=CARTESIAN_POINT('Ctrl Pts',(17.1051831298931,-68.9108884594798,
-177.562732114831));
#185789=CARTESIAN_POINT('Ctrl Pts',(17.104688915706,-68.9110395698531,-177.5632226026));
#185790=CARTESIAN_POINT('Ctrl Pts',(17.1041942190907,-68.9111908205538,
-177.563712518466));
#185791=CARTESIAN_POINT('Ctrl Pts',(17.1036990412529,-68.9113422111695,
-177.564201860987));
#185792=CARTESIAN_POINT('Ctrl Pts',(17.0462278720981,-68.928912859572,-177.620995773435));
#185793=CARTESIAN_POINT('Ctrl Pts',(16.9816775189014,-68.9485450280233,
-177.670649891561));
#185794=CARTESIAN_POINT('Ctrl Pts',(16.9125398584853,-68.9694257059557,
-177.71172930656));
#185795=CARTESIAN_POINT('Ctrl Pts',(16.8713991530569,-68.9818508562253,
-177.736173814828));
#185796=CARTESIAN_POINT('Ctrl Pts',(16.8286352683534,-68.9947177370481,
-177.757582237901));
#185797=CARTESIAN_POINT('Ctrl Pts',(16.7847809634131,-69.007852694924,-177.775654990622));
#185798=CARTESIAN_POINT('Ctrl Pts',(16.78433889104,-69.007985101583,-177.775837172615));
#185799=CARTESIAN_POINT('Ctrl Pts',(16.7838967203631,-69.008117531739,-177.776019010763));
#185800=CARTESIAN_POINT('Ctrl Pts',(16.7834544517973,-69.0082499852543,
-177.776200504879));
#185801=CARTESIAN_POINT('Ctrl Pts',(16.7449698092193,-69.0197756205531,
-177.791993479437));
#185802=CARTESIAN_POINT('Ctrl Pts',(16.7054466746898,-69.0315662591249,
-177.805303057386));
#185803=CARTESIAN_POINT('Ctrl Pts',(16.6651986963193,-69.0435261398608,
-177.816095296664));
#185804=CARTESIAN_POINT('Ctrl Pts',(16.6237252999668,-69.0558501594554,
-177.827216123976));
#185805=CARTESIAN_POINT('Ctrl Pts',(16.5814808439821,-69.0683543171783,
-177.835664557351));
#185806=CARTESIAN_POINT('Ctrl Pts',(16.5387947985051,-69.0809368867563,
-177.841347934728));
#185807=CARTESIAN_POINT('Ctrl Pts',(16.4988275773256,-69.0927180282443,
-177.84666931782));
#185808=CARTESIAN_POINT('Ctrl Pts',(16.458472065883,-69.1045682551433,-177.849566394706));
#185809=CARTESIAN_POINT('Ctrl Pts',(16.4180055598673,-69.1164010707451,
-177.849914459328));
#185810=CARTESIAN_POINT('Ctrl Pts',(16.4152527710431,-69.1172060140366,
-177.849938136895));
#185811=CARTESIAN_POINT('Ctrl Pts',(16.41249947515,-69.1180108744162,-177.849949999677));
#185812=CARTESIAN_POINT('Ctrl Pts',(16.4097457627119,-69.1188156235219,
-177.84995));
#185813=CARTESIAN_POINT('Origin',(17.55,-69.2968662511513,-176.84995));
#185814=CARTESIAN_POINT('Origin',(17.55,-69.2968662511513,-179.64995));
#185815=CARTESIAN_POINT('',(17.4012711864406,-68.8194987407181,-179.64995));
#185816=CARTESIAN_POINT('Origin',(0.,-12.9675000200281,-171.871644662643));
#185817=CARTESIAN_POINT('Origin',(0.,-12.9675000200281,-171.871644662643));
#185818=CARTESIAN_POINT('Origin',(23.2,-67.2147119299503,-179.64995));
#185819=CARTESIAN_POINT('',(23.0033898305085,-66.7549897951205,-176.84995));
#185820=CARTESIAN_POINT('Origin',(23.2,-67.2147119299503,-176.84995));
#185821=CARTESIAN_POINT('',(23.0033898305085,-66.7549897951205,-179.64995));
#185822=CARTESIAN_POINT('Ctrl Pts',(23.9949152542395,-66.3200448697526,
-177.84995));
#185823=CARTESIAN_POINT('Ctrl Pts',(23.9949152542386,-66.320044869753,-177.34995));
#185824=CARTESIAN_POINT('Ctrl Pts',(24.2000000000011,-66.7760495265879,
-177.34995));
#185825=CARTESIAN_POINT('Ctrl Pts',(23.8703538324233,-66.3760654545035,
-177.849949984965));
#185826=CARTESIAN_POINT('Ctrl Pts',(23.9206657457682,-66.3534380400361,
-177.323497139763));
#185827=CARTESIAN_POINT('Ctrl Pts',(24.1371859654851,-66.8325498277328,
-177.34995));
#185828=CARTESIAN_POINT('Ctrl Pts',(23.7477652296632,-66.4306666697135,
-177.82675752222));
#185829=CARTESIAN_POINT('Ctrl Pts',(23.85857311611,-66.3812761568117,-177.28202856183));
#185830=CARTESIAN_POINT('Ctrl Pts',(24.0753687900163,-66.8876168115863,
-177.338353763422));
#185831=CARTESIAN_POINT('Ctrl Pts',(23.5124556672824,-66.534569849442,-177.732855161513));
#185832=CARTESIAN_POINT('Ctrl Pts',(23.7605684693856,-66.4255018631538,
-177.182659406882));
#185833=CARTESIAN_POINT('Ctrl Pts',(23.9567084144264,-66.9924080535444,
-177.291402578445));
#185834=CARTESIAN_POINT('Ctrl Pts',(23.4045112120254,-66.5817650498296,
-177.66401934989));
#185835=CARTESIAN_POINT('Ctrl Pts',(23.728650188117,-66.4401283754592,-177.126465197113));
#185836=CARTESIAN_POINT('Ctrl Pts',(23.9022748831747,-67.0400066306863,
-177.256984676403));
#185837=CARTESIAN_POINT('Ctrl Pts',(23.2160104726183,-66.6636583322845,
-177.482533676026));
#185838=CARTESIAN_POINT('Ctrl Pts',(23.6923095199098,-66.4575908379652,
-177.01948600884));
#185839=CARTESIAN_POINT('Ctrl Pts',(23.8072189577995,-67.1225998569154,
-177.166241836555));
#185840=CARTESIAN_POINT('Ctrl Pts',(23.1390036429345,-66.6968206283899,
-177.372560789955));
#185841=CARTESIAN_POINT('Ctrl Pts',(23.6901782519314,-66.4593985440301,
-176.972463316884));
#185842=CARTESIAN_POINT('Ctrl Pts',(23.7683864506384,-67.1560455904002,
-177.111255395708));
#185843=CARTESIAN_POINT('Ctrl Pts',(23.0321233068433,-66.742723669979,-177.12454316851));
#185844=CARTESIAN_POINT('Ctrl Pts',(23.6945043498585,-66.4589699067553,
-176.898771091495));
#185845=CARTESIAN_POINT('Ctrl Pts',(23.7144895325829,-67.2023409665867,
-176.987246583524));
#185846=CARTESIAN_POINT('Ctrl Pts',(23.0033898412675,-66.7549897905191,
-176.989728313577));
#185847=CARTESIAN_POINT('Ctrl Pts',(23.6999999982817,-66.4570693060762,
-176.874118380146));
#185848=CARTESIAN_POINT('Ctrl Pts',(23.7,-67.2147119253083,-176.919839157335));
#185849=CARTESIAN_POINT('Ctrl Pts',(23.0033898305084,-66.7549897951205,
-176.84995));
#185850=CARTESIAN_POINT('Ctrl Pts',(23.6999999999999,-66.45706930551,-176.84995));
#185851=CARTESIAN_POINT('Ctrl Pts',(23.7,-67.2147119299503,-176.84995));
#185852=CARTESIAN_POINT('Ctrl Pts',(23.9949152542395,-66.3200448697526,
-177.84995));
#185853=CARTESIAN_POINT('Ctrl Pts',(23.9428551887954,-66.3434585018855,
-177.849949993716));
#185854=CARTESIAN_POINT('Ctrl Pts',(23.8912891629463,-66.3665571088583,
-177.845903065055));
#185855=CARTESIAN_POINT('Ctrl Pts',(23.8403424606449,-66.3892926538624,
-177.83781160242));
#185856=CARTESIAN_POINT('Ctrl Pts',(23.7898936124082,-66.411806025831,-177.829799210017));
#185857=CARTESIAN_POINT('Ctrl Pts',(23.740051601186,-66.4339635775751,-177.817820923569));
#185858=CARTESIAN_POINT('Ctrl Pts',(23.6909420374968,-66.4557157061558,
-177.801828391251));
#185859=CARTESIAN_POINT('Ctrl Pts',(23.6705352998632,-66.4647544747291,
-177.795182935934));
#185860=CARTESIAN_POINT('Ctrl Pts',(23.6502551185154,-66.4737231883062,
-177.78784373804));
#185861=CARTESIAN_POINT('Ctrl Pts',(23.6301109846052,-66.4826180228466,
-177.779804722709));
#185862=CARTESIAN_POINT('Ctrl Pts',(23.6296825902114,-66.4828071844789,
-177.779633761321));
#185863=CARTESIAN_POINT('Ctrl Pts',(23.6292543206867,-66.4829962847601,
-177.77946250822));
#185864=CARTESIAN_POINT('Ctrl Pts',(23.628826176177,-66.4831853236384,-177.779290963367));
#185865=CARTESIAN_POINT('Ctrl Pts',(23.549083605048,-66.5183941044447,-177.747340471676));
#185866=CARTESIAN_POINT('Ctrl Pts',(23.4738664381757,-66.5513895428365,
-177.705344056631));
#185867=CARTESIAN_POINT('Ctrl Pts',(23.4044230513637,-66.5817044397988,
-177.653364341203));
#185868=CARTESIAN_POINT('Ctrl Pts',(23.3717123604556,-66.5959840029072,
-177.628879757676));
#185869=CARTESIAN_POINT('Ctrl Pts',(23.340282339806,-66.6096689890179,-177.60218062655));
#185870=CARTESIAN_POINT('Ctrl Pts',(23.3102608826734,-66.6227116735265,
-177.57327646271));
#185871=CARTESIAN_POINT('Ctrl Pts',(23.3097552045839,-66.6229313630558,
-177.572789604185));
#185872=CARTESIAN_POINT('Ctrl Pts',(23.3092500282568,-66.6231508261632,
-177.572302197161));
#185873=CARTESIAN_POINT('Ctrl Pts',(23.3087453546535,-66.6233700624812,
-177.571814242488));
#185874=CARTESIAN_POINT('Ctrl Pts',(23.2428791470159,-66.6519831398302,
-177.508130064148));
#185875=CARTESIAN_POINT('Ctrl Pts',(23.1855484931327,-66.6767452815919,
-177.435089847604));
#185876=CARTESIAN_POINT('Ctrl Pts',(23.1388722340366,-66.696846286165,-177.354542469168));
#185877=CARTESIAN_POINT('Ctrl Pts',(23.1191486795936,-66.7053401814714,
-177.320506309574));
#185878=CARTESIAN_POINT('Ctrl Pts',(23.101326993937,-66.7130020216598,-177.285129627946));
#185879=CARTESIAN_POINT('Ctrl Pts',(23.0855644128598,-66.7197717463455,
-177.248551496375));
#185880=CARTESIAN_POINT('Ctrl Pts',(23.0853517691174,-66.7198630727333,
-177.248058042242));
#185881=CARTESIAN_POINT('Ctrl Pts',(23.0851395181392,-66.7199542292592,
-177.24756442059));
#185882=CARTESIAN_POINT('Ctrl Pts',(23.0849276601637,-66.7200452158304,
-177.247070631801));
#185883=CARTESIAN_POINT('Ctrl Pts',(23.0685067964827,-66.7270974784524,
-177.208797640755));
#185884=CARTESIAN_POINT('Ctrl Pts',(23.0544044796133,-66.7331469401741,
-177.169412579499));
#185885=CARTESIAN_POINT('Ctrl Pts',(23.0427873419503,-66.7381263973539,
-177.129172865924));
#185886=CARTESIAN_POINT('Ctrl Pts',(23.0313107069201,-66.7430456308483,
-177.08941982866));
#185887=CARTESIAN_POINT('Ctrl Pts',(23.022259763421,-66.746920485885,-177.048833228896));
#185888=CARTESIAN_POINT('Ctrl Pts',(23.015750900502,-66.7497052241091,-177.007676413085));
#185889=CARTESIAN_POINT('Ctrl Pts',(23.0093646056923,-66.7524375230511,
-176.967294619449));
#185890=CARTESIAN_POINT('Ctrl Pts',(23.0054256948345,-66.7541203250939,
-176.926364378225));
#185891=CARTESIAN_POINT('Ctrl Pts',(23.0039983429948,-66.7547299427615,
-176.88514146636));
#185892=CARTESIAN_POINT('Ctrl Pts',(23.0035929213886,-66.7549030971072,
-176.873432608967));
#185893=CARTESIAN_POINT('Ctrl Pts',(23.0033898314129,-66.7549897947337,
-176.861700158874));
#185894=CARTESIAN_POINT('Ctrl Pts',(23.0033898305084,-66.7549897951205,
-176.84995));
#185895=CARTESIAN_POINT('Origin',(44.5079524583208,31.5404524382925,-171.64995));
#185896=CARTESIAN_POINT('',(44.5079524583208,28.7904524382925,-179.64995));
#185897=CARTESIAN_POINT('',(44.5079524583208,28.7904524382925,-171.64995));
#185898=CARTESIAN_POINT('Origin',(44.5079524583208,31.5404524382925,-179.64995));
#185899=CARTESIAN_POINT('Origin',(44.5079524583208,-57.4754524783487,-171.64995));
#185900=CARTESIAN_POINT('',(44.5079524583208,-60.2254524783487,-179.64995));
#185901=CARTESIAN_POINT('',(44.5079524583208,-60.2254524783487,-171.64995));
#185902=CARTESIAN_POINT('Origin',(44.5079524583208,-57.4754524783487,-179.64995));
#185903=CARTESIAN_POINT('Origin',(26.4569673975197,-68.4857751744904,-179.39995));
#185904=CARTESIAN_POINT('',(25.0588349740736,-65.5518825850269,-179.64995));
#185905=CARTESIAN_POINT('Origin',(25.0588349740736,-65.5518825850269,-179.39995));
#185906=CARTESIAN_POINT('',(26.0046548193995,-65.2674039510802,-179.64995));
#185907=CARTESIAN_POINT('Origin',(26.4569673975197,-68.4857751744904,-179.64995));
#185908=CARTESIAN_POINT('Origin',(26.0046548193995,-65.2674039510803,-179.39995));
#185909=CARTESIAN_POINT('Origin',(51.7734815964994,-61.6458315265255,-179.39995));
#185910=CARTESIAN_POINT('',(44.5938155824071,-62.6548677810304,-179.64995));
#185911=CARTESIAN_POINT('',(26.0046548193995,-65.2674039510802,-179.64995));
#185912=CARTESIAN_POINT('Origin',(44.5938155824071,-62.6548677810303,-179.39995));
#185913=CARTESIAN_POINT('Origin',(44.2110895547669,-59.9316305919911,-179.39995));
#185914=CARTESIAN_POINT('',(46.0960584892725,-61.9339772442841,-179.64995));
#185915=CARTESIAN_POINT('Origin',(44.2110895547669,-59.9316305919911,-179.64995));
#185916=CARTESIAN_POINT('Origin',(46.0960584892725,-61.9339772442841,-179.39995));
#185917=CARTESIAN_POINT('Origin',(0.,-12.9675000200281,-179.39995));
#185918=CARTESIAN_POINT('',(48.9664772242561,-59.0635585093003,-179.64995));
#185919=CARTESIAN_POINT('Origin',(0.,-12.9675000200281,-179.64995));
#185920=CARTESIAN_POINT('Origin',(48.9664772242561,-59.0635585093003,-179.39995));
#185921=CARTESIAN_POINT('Origin',(46.9641305719631,-57.1785895747948,-179.39995));
#185922=CARTESIAN_POINT('',(49.6873677610024,-57.561315602435,-179.64995));
#185923=CARTESIAN_POINT('Origin',(46.9641305719631,-57.1785895747948,-179.64995));
#185924=CARTESIAN_POINT('Origin',(49.6873677610024,-57.561315602435,-179.39995));
#185925=CARTESIAN_POINT('Origin',(50.3220654694669,-53.04520674476,-179.39995));
#185926=CARTESIAN_POINT('',(52.2574626216431,-39.2741404473771,-179.64995));
#185927=CARTESIAN_POINT('',(49.6873677610024,-57.561315602435,-179.64995));
#185928=CARTESIAN_POINT('Origin',(52.2574626216431,-39.2741404473771,-179.39995));
#185929=CARTESIAN_POINT('Origin',(57.4563699825363,-40.0047992274175,-179.39995));
#185930=CARTESIAN_POINT('',(52.7060401808306,-37.7694319701137,-179.64995));
#185931=CARTESIAN_POINT('Origin',(57.4563699825363,-40.0047992274175,-179.64995));
#185932=CARTESIAN_POINT('Origin',(52.7060401808306,-37.7694319701137,-179.39995));
#185933=CARTESIAN_POINT('Origin',(0.,-12.9675000200281,-179.39995));
#185934=CARTESIAN_POINT('',(52.7060401808306,11.8344319300573,-179.64995));
#185935=CARTESIAN_POINT('Origin',(0.,-12.9675000200281,-179.64995));
#185936=CARTESIAN_POINT('Origin',(52.7060401808306,11.8344319300573,-179.39995));
#185937=CARTESIAN_POINT('Origin',(57.4563699825364,14.0697991873612,-179.39995));
#185938=CARTESIAN_POINT('',(52.2574626216432,13.3391404073208,-179.64995));
#185939=CARTESIAN_POINT('Origin',(57.4563699825364,14.0697991873612,-179.64995));
#185940=CARTESIAN_POINT('Origin',(52.2574626216431,13.3391404073208,-179.39995));
#185941=CARTESIAN_POINT('Origin',(61.3785689046687,-51.5609030735669,-179.39995));
#185942=CARTESIAN_POINT('',(49.6873677610025,31.6263155623787,-179.64995));
#185943=CARTESIAN_POINT('',(52.2574626216432,13.3391404073208,-179.64995));
#185944=CARTESIAN_POINT('Origin',(49.6873677610024,31.6263155623787,-179.39995));
#185945=CARTESIAN_POINT('Origin',(46.9641305719631,31.2435895347386,-179.39995));
#185946=CARTESIAN_POINT('',(48.9664772242561,33.1285584692441,-179.64995));
#185947=CARTESIAN_POINT('Origin',(46.9641305719631,31.2435895347386,-179.64995));
#185948=CARTESIAN_POINT('Origin',(48.9664772242561,33.1285584692441,-179.39995));
#185949=CARTESIAN_POINT('Origin',(0.,-12.9675000200281,-179.39995));
#185950=CARTESIAN_POINT('',(46.0960584892724,35.9989772042278,-179.64995));
#185951=CARTESIAN_POINT('Origin',(0.,-12.9675000200281,-179.64995));
#185952=CARTESIAN_POINT('Origin',(46.0960584892724,35.9989772042278,-179.39995));
#185953=CARTESIAN_POINT('Origin',(44.2110895547669,33.9966305519348,-179.39995));
#185954=CARTESIAN_POINT('',(44.593815582407,36.7198677409741,-179.64995));
#185955=CARTESIAN_POINT('Origin',(44.2110895547669,33.9966305519348,-179.64995));
#185956=CARTESIAN_POINT('Origin',(44.593815582407,36.7198677409741,-179.39995));
#185957=CARTESIAN_POINT('Origin',(62.8299850317005,34.1569412647963,-179.39995));
#185958=CARTESIAN_POINT('',(26.3066404273498,39.2899626016146,-179.64995));
#185959=CARTESIAN_POINT('',(44.593815582407,36.7198677409741,-179.64995));
#185960=CARTESIAN_POINT('Origin',(26.3066404273498,39.2899626016146,-179.39995));
#185961=CARTESIAN_POINT('Origin',(27.0372992073901,44.4888699625078,-179.39995));
#185962=CARTESIAN_POINT('',(24.8019319500862,39.7385401608021,-179.64995));
#185963=CARTESIAN_POINT('Origin',(27.0372992073901,44.4888699625078,-179.64995));
#185964=CARTESIAN_POINT('',(24.9083780099579,39.9647463418357,-179.39995));
#185965=CARTESIAN_POINT('Origin',(24.8019319500862,39.7385401608021,-179.39995));
#185966=CARTESIAN_POINT('Origin',(27.0372992073901,44.4888699625078,-179.39995));
#185967=CARTESIAN_POINT('Origin',(27.0372992073901,44.4888699625078,-179.64995));
#185968=CARTESIAN_POINT('',(24.9083780099579,39.9647463418357,-177.84995));
#185969=CARTESIAN_POINT('',(24.9083780099579,39.9647463418357,-179.64995));
#185970=CARTESIAN_POINT('Origin',(27.0372992073901,44.4888699625078,-177.84995));
#185971=CARTESIAN_POINT('Origin',(45.6308101826775,37.3314983336592,-177.84995));
#185972=CARTESIAN_POINT('',(26.4110202530699,40.0326636531708,-177.34995));
#185973=CARTESIAN_POINT('Origin',(26.4110202530699,40.0326636531708,-177.84995));
#185974=CARTESIAN_POINT('',(-42.7876488459256,49.7579023686377,-177.34995));
#185975=CARTESIAN_POINT('Origin',(27.0372992073901,44.4888699625078,-177.84995));
#185976=CARTESIAN_POINT('',(25.121270129701,40.4171587039029,-177.34995));
#185977=CARTESIAN_POINT('Origin',(25.121270129701,40.4171587039029,-177.84995));
#185978=CARTESIAN_POINT('Origin',(27.0372992073901,44.4888699625078,-177.34995));
#185979=CARTESIAN_POINT('Origin',(38.5,58.91999998,-174.34995));
#185980=CARTESIAN_POINT('',(41.5,58.91999998,-174.34995));
#185981=CARTESIAN_POINT('',(41.5,58.91999998,-174.34995));
#185982=CARTESIAN_POINT('',(38.5,58.91999998,-177.34995));
#185983=CARTESIAN_POINT('',(38.5,58.91999998,-177.34995));
#185984=CARTESIAN_POINT('Origin',(38.5,58.91999998,-174.34995));
#185985=CARTESIAN_POINT('Origin',(41.5,58.91999998,-92.34995));
#185986=CARTESIAN_POINT('',(41.5,58.91999998,-95.34995));
#185987=CARTESIAN_POINT('',(41.5,58.91999998,-92.34995));
#185988=CARTESIAN_POINT('',(41.5,58.91999998,-95.34995));
#185989=CARTESIAN_POINT('Origin',(37.,58.91999998,-91.84995));
#185990=CARTESIAN_POINT('',(37.,46.41999998,-92.34995));
#185991=CARTESIAN_POINT('Origin',(37.,46.41999998,-91.84995));
#185992=CARTESIAN_POINT('',(37.,46.41999998,-92.34995));
#185993=CARTESIAN_POINT('Origin',(60.,29.41999998,-91.34995));
#185994=CARTESIAN_POINT('',(37.5,29.41999998,-92.34995));
#185995=CARTESIAN_POINT('Origin',(31.,-9.33460238845303,-91.84995));
#185996=CARTESIAN_POINT('',(31.,46.41999998,-92.34995));
#185997=CARTESIAN_POINT('Origin',(31.,46.41999998,-91.84995));
#185998=CARTESIAN_POINT('',(31.,29.41999998,-92.34995));
#185999=CARTESIAN_POINT('Origin',(30.,46.41999998,-91.84995));
#186000=CARTESIAN_POINT('',(30.,47.41999998,-92.34995));
#186001=CARTESIAN_POINT('Origin',(30.,47.41999998,-91.84995));
#186002=CARTESIAN_POINT('Origin',(30.,46.41999998,-92.34995));
#186003=CARTESIAN_POINT('Origin',(-41.5,47.41999998,-91.84995));
#186004=CARTESIAN_POINT('',(29.5,47.41999998,-92.34995));
#186005=CARTESIAN_POINT('Origin',(29.5,47.41999998,-91.84995));
#186006=CARTESIAN_POINT('',(-41.5,47.41999998,-92.34995));
#186007=CARTESIAN_POINT('Origin',(29.5,46.41999998,-91.84995));
#186008=CARTESIAN_POINT('',(28.5,46.41999998,-92.34995));
#186009=CARTESIAN_POINT('Origin',(28.5,46.41999998,-91.84995));
#186010=CARTESIAN_POINT('Origin',(29.5,46.41999998,-92.34995));
#186011=CARTESIAN_POINT('Origin',(28.5,58.91999998,-91.84995));
#186012=CARTESIAN_POINT('',(28.5,46.41999998,-92.34995));
#186013=CARTESIAN_POINT('Origin',(60.,29.41999998,-91.34995));
#186014=CARTESIAN_POINT('',(29.,29.41999998,-92.34995));
#186015=CARTESIAN_POINT('Origin',(22.5,-9.33460238845303,-91.84995));
#186016=CARTESIAN_POINT('',(22.5,46.41999998,-92.34995));
#186017=CARTESIAN_POINT('Origin',(22.5,46.41999998,-91.84995));
#186018=CARTESIAN_POINT('',(22.5,29.41999998,-92.34995));
#186019=CARTESIAN_POINT('Origin',(21.5,46.41999998,-91.84995));
#186020=CARTESIAN_POINT('',(21.5,47.41999998,-92.34995));
#186021=CARTESIAN_POINT('Origin',(21.5,47.41999998,-91.84995));
#186022=CARTESIAN_POINT('Origin',(21.5,46.41999998,-92.34995));
#186023=CARTESIAN_POINT('Origin',(-41.5,47.41999998,-91.84995));
#186024=CARTESIAN_POINT('',(21.,47.41999998,-92.34995));
#186025=CARTESIAN_POINT('Origin',(21.,47.41999998,-91.84995));
#186026=CARTESIAN_POINT('',(-41.5,47.41999998,-92.34995));
#186027=CARTESIAN_POINT('Origin',(21.,46.41999998,-91.84995));
#186028=CARTESIAN_POINT('',(20.,46.41999998,-92.34995));
#186029=CARTESIAN_POINT('Origin',(20.,46.41999998,-91.84995));
#186030=CARTESIAN_POINT('Origin',(21.,46.41999998,-92.34995));
#186031=CARTESIAN_POINT('Origin',(20.,58.91999998,-91.84995));
#186032=CARTESIAN_POINT('',(20.,46.41999998,-92.34995));
#186033=CARTESIAN_POINT('Origin',(60.,29.41999998,-91.34995));
#186034=CARTESIAN_POINT('',(17.5283605562717,29.41999998,-92.34995));
#186035=CARTESIAN_POINT('',(20.5,29.41999998,-92.34995));
#186036=CARTESIAN_POINT('Origin',(17.5283605562717,29.41999998,-91.34995));
#186037=CARTESIAN_POINT('Ctrl Pts',(17.5283605562717,28.4199999800001,-91.34995));
#186038=CARTESIAN_POINT('Ctrl Pts',(17.5283605562716,28.41999998,-92.34995));
#186039=CARTESIAN_POINT('Ctrl Pts',(17.5283605562717,29.4199999800001,-92.34995));
#186040=CARTESIAN_POINT('Ctrl Pts',(16.8748117549663,28.4199999800001,-91.2778699709694));
#186041=CARTESIAN_POINT('Ctrl Pts',(16.8501904102942,28.3452044605545,-92.3499500000001));
#186042=CARTESIAN_POINT('Ctrl Pts',(16.9294484484718,29.4199999819522,-92.34995));
#186043=CARTESIAN_POINT('Ctrl Pts',(16.233134779349,28.4803469141606,-91.2065756291954));
#186044=CARTESIAN_POINT('Ctrl Pts',(16.1934854928648,28.3221299458475,-92.34995));
#186045=CARTESIAN_POINT('Ctrl Pts',(16.3387077693293,29.4682775272991,-92.34995));
#186046=CARTESIAN_POINT('Ctrl Pts',(14.9727946058278,28.7108958947333,-91.0656179778369));
#186047=CARTESIAN_POINT('Ctrl Pts',(14.8701093399109,28.3452025116243,-92.34995));
#186048=CARTESIAN_POINT('Ctrl Pts',(15.1723882243972,29.6527167118161,-92.34995));
#186049=CARTESIAN_POINT('Ctrl Pts',(14.3539522178783,28.8809201843631,-90.9959326732687));
#186050=CARTESIAN_POINT('Ctrl Pts',(14.194875318369,28.3987342821361,-92.3499499999805));
#186051=CARTESIAN_POINT('Ctrl Pts',(14.5966754937866,29.7887243470281,-92.34995));
#186052=CARTESIAN_POINT('Ctrl Pts',(13.7480613600421,29.1125253108927,-90.92733173826));
#186053=CARTESIAN_POINT('Ctrl Pts',(13.5420441920761,28.4819485757734,-92.3499500000002));
#186054=CARTESIAN_POINT('Ctrl Pts',(14.0295223410746,29.9740202447142,-92.34995));
#186055=CARTESIAN_POINT('',(14.0295223410747,29.9740202447141,-92.34995));
#186056=CARTESIAN_POINT('Origin',(14.0295223410747,29.9740202447144,-91.34995));
#186057=CARTESIAN_POINT('Ctrl Pts',(14.0295223410747,29.9740202447141,-92.34995));
#186058=CARTESIAN_POINT('Ctrl Pts',(14.5967291533814,29.7887068092282,-92.34995));
#186059=CARTESIAN_POINT('Ctrl Pts',(15.1723882243932,29.6527167117912,-92.34995));
#186060=CARTESIAN_POINT('Ctrl Pts',(16.3387077693334,29.4682775273239,-92.34995));
#186061=CARTESIAN_POINT('Ctrl Pts',(16.9293976390415,29.4199999800001,-92.34995));
#186062=CARTESIAN_POINT('Ctrl Pts',(17.5283605562717,29.41999998,-92.34995));
#186063=CARTESIAN_POINT('Origin',(1.1373643128445E-15,-12.9675000200281,
-91.34995));
#186064=CARTESIAN_POINT('Origin',(1.1373643128445E-15,-12.9675000200281,
-92.34995));
#186065=CARTESIAN_POINT('Origin',(14.,-9.33460238845303,-91.84995));
#186066=CARTESIAN_POINT('',(14.,46.41999998,-92.34995));
#186067=CARTESIAN_POINT('Origin',(14.,46.41999998,-91.84995));
#186068=CARTESIAN_POINT('',(14.,30.1434227231235,-92.34995));
#186069=CARTESIAN_POINT('Origin',(13.,46.41999998,-91.84995));
#186070=CARTESIAN_POINT('',(13.,47.41999998,-92.34995));
#186071=CARTESIAN_POINT('Origin',(13.,47.41999998,-91.84995));
#186072=CARTESIAN_POINT('Origin',(13.,46.41999998,-92.34995));
#186073=CARTESIAN_POINT('Origin',(-41.5,47.41999998,-91.84995));
#186074=CARTESIAN_POINT('',(12.5,47.41999998,-92.34995));
#186075=CARTESIAN_POINT('Origin',(12.5,47.41999998,-91.84995));
#186076=CARTESIAN_POINT('',(-41.5,47.41999998,-92.34995));
#186077=CARTESIAN_POINT('Origin',(12.5,46.41999998,-91.84995));
#186078=CARTESIAN_POINT('',(11.5,46.41999998,-92.34995));
#186079=CARTESIAN_POINT('Origin',(11.5,46.41999998,-91.84995));
#186080=CARTESIAN_POINT('Origin',(12.5,46.41999998,-92.34995));
#186081=CARTESIAN_POINT('Origin',(11.5,58.91999998,-91.84995));
#186082=CARTESIAN_POINT('',(11.5,46.41999998,-92.34995));
#186083=CARTESIAN_POINT('Origin',(1.1373643128445E-15,-12.9675000200281,
-91.34995));
#186084=CARTESIAN_POINT('Origin',(1.1373643128445E-15,-12.9675000200281,
-92.34995));
#186085=CARTESIAN_POINT('Origin',(5.5,-9.33460238845303,-91.84995));
#186086=CARTESIAN_POINT('',(5.5,46.41999998,-92.34995));
#186087=CARTESIAN_POINT('Origin',(5.5,46.41999998,-91.84995));
#186088=CARTESIAN_POINT('',(5.5,31.9301798728793,-92.34995));
#186089=CARTESIAN_POINT('Origin',(4.5,46.41999998,-91.84995));
#186090=CARTESIAN_POINT('',(4.5,47.41999998,-92.34995));
#186091=CARTESIAN_POINT('Origin',(4.5,47.41999998,-91.84995));
#186092=CARTESIAN_POINT('Origin',(4.5,46.41999998,-92.34995));
#186093=CARTESIAN_POINT('Origin',(-41.5,47.41999998,-91.84995));
#186094=CARTESIAN_POINT('',(4.,47.41999998,-92.34995));
#186095=CARTESIAN_POINT('Origin',(4.,47.41999998,-91.84995));
#186096=CARTESIAN_POINT('',(-41.5,47.41999998,-92.34995));
#186097=CARTESIAN_POINT('Origin',(4.,46.41999998,-91.84995));
#186098=CARTESIAN_POINT('',(3.,46.41999998,-92.34995));
#186099=CARTESIAN_POINT('Origin',(3.,46.41999998,-91.84995));
#186100=CARTESIAN_POINT('Origin',(4.,46.41999998,-92.34995));
#186101=CARTESIAN_POINT('Origin',(3.,58.91999998,-91.84995));
#186102=CARTESIAN_POINT('',(3.,32.1080106234021,-92.34995));
#186103=CARTESIAN_POINT('Origin',(3.,32.1080106234021,-91.84995));
#186104=CARTESIAN_POINT('',(3.,46.41999998,-92.34995));
#186105=CARTESIAN_POINT('Origin',(38.5,58.91999998,-95.34995));
#186106=CARTESIAN_POINT('',(38.5,58.91999998,-92.34995));
#186107=CARTESIAN_POINT('Origin',(38.5,58.91999998,-95.34995));
#186108=CARTESIAN_POINT('',(38.5,58.91999998,-92.34995));
#186109=CARTESIAN_POINT('Origin',(-41.5,47.41999998,-91.84995));
#186110=CARTESIAN_POINT('',(38.,47.41999998,-92.34995));
#186111=CARTESIAN_POINT('Origin',(38.,47.41999998,-91.84995));
#186112=CARTESIAN_POINT('',(-41.5,47.41999998,-92.34995));
#186113=CARTESIAN_POINT('Origin',(38.,46.41999998,-91.84995));
#186114=CARTESIAN_POINT('Origin',(38.,46.41999998,-92.34995));
#186115=CARTESIAN_POINT('Ctrl Pts',(2.9730852099506,31.3045898136069,-90.7567930161436));
#186116=CARTESIAN_POINT('Ctrl Pts',(3.50093046722966,31.2817579610315,-90.7398891378361));
#186117=CARTESIAN_POINT('Ctrl Pts',(3.49999922403526,31.7061080469582,-91.0538938313493));
#186118=CARTESIAN_POINT('Ctrl Pts',(2.96831480394843,31.1636040483254,-90.9411472609555));
#186119=CARTESIAN_POINT('Ctrl Pts',(3.50094375794647,31.1316900065056,-90.9272767748672));
#186120=CARTESIAN_POINT('Ctrl Pts',(3.49999921701682,31.6355825669373,-91.1459119172329));
#186121=CARTESIAN_POINT('Ctrl Pts',(2.96597720456975,31.0948501016434,-91.1829665694402));
#186122=CARTESIAN_POINT('Ctrl Pts',(3.50095025048169,31.0578808190773,-91.1768644172926));
#186123=CARTESIAN_POINT('Ctrl Pts',(3.49999921357759,31.6011902598928,-91.2666067024717));
#186124=CARTESIAN_POINT('Ctrl Pts',(2.9666837372529,31.1156607402492,-91.4988149931348));
#186125=CARTESIAN_POINT('Ctrl Pts',(3.50094827348241,31.0802559450011,-91.5041387140221));
#186126=CARTESIAN_POINT('Ctrl Pts',(3.49999921461707,31.6116002328841,-91.4242502749333));
#186127=CARTESIAN_POINT('Ctrl Pts',(2.96723234610694,31.1318174446344,-91.5823694312293));
#186128=CARTESIAN_POINT('Ctrl Pts',(3.50094674031663,31.0976044869907,-91.5905362019412));
#186129=CARTESIAN_POINT('Ctrl Pts',(3.49999921542421,31.6196822275484,-91.4659533973627));
#186130=CARTESIAN_POINT('Ctrl Pts',(2.96900087342029,31.1839643938508,-91.7412472447188));
#186131=CARTESIAN_POINT('Ctrl Pts',(3.50094181368991,31.1534426029942,-91.7542039764945));
#186132=CARTESIAN_POINT('Ctrl Pts',(3.49999921802616,31.6457674414273,-91.5452519327685));
#186133=CARTESIAN_POINT('Ctrl Pts',(2.97020720291435,31.2195539123312,-91.8165845933835));
#186134=CARTESIAN_POINT('Ctrl Pts',(3.50093846494821,31.1914250734018,-91.8313961753176));
#186135=CARTESIAN_POINT('Ctrl Pts',(3.49999921980099,31.6635702854767,-91.582854393305));
#186136=CARTESIAN_POINT('Ctrl Pts',(2.97327686342368,31.3102833845102,-91.9588329995341));
#186137=CARTESIAN_POINT('Ctrl Pts',(3.50092999134622,31.2877769651877,-91.976055099741));
#186138=CARTESIAN_POINT('Ctrl Pts',(3.49999922431731,31.7089557758124,-91.6538544608224));
#186139=CARTESIAN_POINT('Ctrl Pts',(2.97508200188551,31.363705231644,-92.0229770344444));
#186140=CARTESIAN_POINT('Ctrl Pts',(3.50092503769121,31.3442016959818,-92.0406579023939));
#186141=CARTESIAN_POINT('Ctrl Pts',(3.4999992269732,31.735679025568,-91.6858710465136));
#186142=CARTESIAN_POINT('Ctrl Pts',(2.97918951587053,31.4855444640944,-92.1370301830535));
#186143=CARTESIAN_POINT('Ctrl Pts',(3.50091385025873,31.4720404315998,-92.154150157461));
#186144=CARTESIAN_POINT('Ctrl Pts',(3.49999923301664,31.7966270247391,-91.7428001834818));
#186145=CARTESIAN_POINT('Ctrl Pts',(2.98150917200635,31.5544802723793,-92.1869191253344));
#186146=CARTESIAN_POINT('Ctrl Pts',(3.5009075812992,31.5438634599872,-92.2030139201566));
#186147=CARTESIAN_POINT('Ctrl Pts',(3.49999923642963,31.8311111796843,-91.7677027010548));
#186148=CARTESIAN_POINT('Ctrl Pts',(2.99080944970468,31.8316005441471,-92.3387964507699));
#186149=CARTESIAN_POINT('Ctrl Pts',(3.50088278313963,31.8290484154313,-92.3480335721559));
#186150=CARTESIAN_POINT('Ctrl Pts',(3.49999925011377,31.9697383525658,-91.8435168239899));
#186151=CARTESIAN_POINT('Ctrl Pts',(2.99906263916586,32.0790639346103,-92.3785629445754));
#186152=CARTESIAN_POINT('Ctrl Pts',(3.50086123689989,32.0791891259729,-92.3794444887817));
#186153=CARTESIAN_POINT('Ctrl Pts',(3.49999926225773,32.0935311034211,-91.8633729799761));
#186154=CARTESIAN_POINT('Ctrl Pts',(3.00656307387834,32.3061821416724,-92.3288442122165));
#186155=CARTESIAN_POINT('Ctrl Pts',(3.50084207052921,32.3047067774897,-92.3225109654136));
#186156=CARTESIAN_POINT('Ctrl Pts',(3.49999927329452,32.2071461725455,-91.8385626593203));
#186157=CARTESIAN_POINT('',(2.96960200166493,31.2017108282785,-90.9273317382593));
#186158=CARTESIAN_POINT('Origin',(3.,31.6538440087773,-91.1386408691297));
#186159=CARTESIAN_POINT('',(2.96642827403755,31.1080789525293,-91.3499500965915));
#186160=CARTESIAN_POINT('Ctrl Pts',(2.96642827403755,31.1080789525293,-91.3499500965915));
#186161=CARTESIAN_POINT('Ctrl Pts',(2.96642678046511,31.1080459325444,-91.3718155306746));
#186162=CARTESIAN_POINT('Ctrl Pts',(2.96644996804348,31.1087378443562,-91.3937457112765));
#186163=CARTESIAN_POINT('Ctrl Pts',(2.9664988473075,31.1101841867365,-91.4156969915003));
#186164=CARTESIAN_POINT('Ctrl Pts',(2.96658204510027,31.1126460178633,-91.4530604440709));
#186165=CARTESIAN_POINT('Ctrl Pts',(2.96673926306768,31.1172834424333,-91.4908103834415));
#186166=CARTESIAN_POINT('Ctrl Pts',(2.96697200208073,31.1241452740858,-91.5285793415084));
#186167=CARTESIAN_POINT('Ctrl Pts',(2.96718969499616,31.1305635024613,-91.563906614262));
#186168=CARTESIAN_POINT('Ctrl Pts',(2.96747346980304,31.1389281132673,-91.5992509320773));
#186169=CARTESIAN_POINT('Ctrl Pts',(2.96782515711633,31.1492971045932,-91.6342689486014));
#186170=CARTESIAN_POINT('Ctrl Pts',(2.96791760205605,31.1520227098165,-91.6434738255027));
#186171=CARTESIAN_POINT('Ctrl Pts',(2.9680147424783,31.1548868999422,-91.6526558966934));
#186172=CARTESIAN_POINT('Ctrl Pts',(2.96811661795246,31.1578909187456,-91.6618083381375));
#186173=CARTESIAN_POINT('Ctrl Pts',(2.96834122380717,31.1645139083954,-91.6819868153449));
#186174=CARTESIAN_POINT('Ctrl Pts',(2.96858796167743,31.1717904982887,-91.7020221689901));
#186175=CARTESIAN_POINT('Ctrl Pts',(2.96885783449233,31.1797517323839,-91.7219119918425));
#186176=CARTESIAN_POINT('Ctrl Pts',(2.9693297949791,31.1936745423575,-91.7566958231767));
#186177=CARTESIAN_POINT('Ctrl Pts',(2.96987110529427,31.2096497893136,-91.7909173348017));
#186178=CARTESIAN_POINT('Ctrl Pts',(2.97048317220471,31.2277257567495,-91.8244266948797));
#186179=CARTESIAN_POINT('Ctrl Pts',(2.97087397256257,31.2392671330634,-91.8458221823448));
#186180=CARTESIAN_POINT('Ctrl Pts',(2.97129358683363,31.2516639907196,-91.8669277438773));
#186181=CARTESIAN_POINT('Ctrl Pts',(2.97174203316901,31.2649186484207,-91.8877087964588));
#186182=CARTESIAN_POINT('Ctrl Pts',(2.97188629124988,31.269182461795,-91.8943937318173));
#186183=CARTESIAN_POINT('Ctrl Pts',(2.97203290085651,31.2735163747235,-91.9010157806221));
#186184=CARTESIAN_POINT('Ctrl Pts',(2.97218246192385,31.2779381969121,-91.9076009010963));
#186185=CARTESIAN_POINT('Ctrl Pts',(2.97279243835603,31.2959723509214,-91.9344579459385));
#186186=CARTESIAN_POINT('Ctrl Pts',(2.97345013747225,31.3154282321948,-91.9606258130146));
#186187=CARTESIAN_POINT('Ctrl Pts',(2.97415449702867,31.3362801043901,-91.9859303053176));
#186188=CARTESIAN_POINT('Ctrl Pts',(2.97474456601411,31.3537485165932,-92.0071288479712));
#186189=CARTESIAN_POINT('Ctrl Pts',(2.97536733810749,31.3721953750359,-92.0277208595378));
#186190=CARTESIAN_POINT('Ctrl Pts',(2.97602129399163,31.3915791216418,-92.0476150004765));
#186191=CARTESIAN_POINT('Ctrl Pts',(2.97609144185887,31.3936583574381,-92.0497489847272));
#186192=CARTESIAN_POINT('Ctrl Pts',(2.97618040919332,31.3962956170435,-92.0524293242319));
#186193=CARTESIAN_POINT('Ctrl Pts',(2.97625004760575,31.3983599125,-92.0545074783175));
#186194=CARTESIAN_POINT('Ctrl Pts',(2.9762813755989,31.3992885699988,-92.0554423703501));
#186195=CARTESIAN_POINT('Ctrl Pts',(2.97630876917177,31.4001005898352,-92.0562560290692));
#186196=CARTESIAN_POINT('Ctrl Pts',(2.97632867593465,31.4006906176559,-92.0568461220599));
#186197=CARTESIAN_POINT('Ctrl Pts',(2.97658533779428,31.4082979638933,-92.0644543085469));
#186198=CARTESIAN_POINT('Ctrl Pts',(2.97685413045719,31.4162673444773,-92.072180195945));
#186199=CARTESIAN_POINT('Ctrl Pts',(2.97713591686397,31.4246248429328,-92.0800036140342));
#186200=CARTESIAN_POINT('Ctrl Pts',(2.97762383390965,31.4390959666555,-92.0935499702442));
#186201=CARTESIAN_POINT('Ctrl Pts',(2.97815174851592,31.45476186078,-92.107390661295));
#186202=CARTESIAN_POINT('Ctrl Pts',(2.97872268282718,31.4717153663622,-92.1213593491614));
#186203=CARTESIAN_POINT('Ctrl Pts',(2.9792693842564,31.4879492930143,-92.1347351464646));
#186204=CARTESIAN_POINT('Ctrl Pts',(2.97985554597519,31.5053642854582,-92.1482285118527));
#186205=CARTESIAN_POINT('Ctrl Pts',(2.98048308745592,31.5240210210283,-92.1616525687454));
#186206=CARTESIAN_POINT('Ctrl Pts',(2.98107284624726,31.5415544816169,-92.1742683970388));
#186207=CARTESIAN_POINT('Ctrl Pts',(2.98169916121911,31.5601849324601,-92.1868230399458));
#186208=CARTESIAN_POINT('Ctrl Pts',(2.98236279914083,31.5799391110566,-92.1991231155207));
#186209=CARTESIAN_POINT('Ctrl Pts',(2.9828721293334,31.5951000885405,-92.2085632027373));
#186210=CARTESIAN_POINT('Ctrl Pts',(2.98340343022638,31.6109225867108,-92.217852654633));
#186211=CARTESIAN_POINT('Ctrl Pts',(2.98395662917302,31.6274066594453,-92.2268868429956));
#186212=CARTESIAN_POINT('Ctrl Pts',(2.98435229799388,31.6391966920572,-92.2333484363853));
#186213=CARTESIAN_POINT('Ctrl Pts',(2.98476048602021,31.6513647799655,-92.2396977532999));
#186214=CARTESIAN_POINT('Ctrl Pts',(2.98518137990977,31.6639171754063,-92.2459029934989));
#186215=CARTESIAN_POINT('Ctrl Pts',(2.98601398420453,31.6887480855549,-92.2581780817527));
#186216=CARTESIAN_POINT('Ctrl Pts',(2.98689570726584,31.7150655813268,-92.2698795468468));
#186217=CARTESIAN_POINT('Ctrl Pts',(2.98782458083186,31.7428170652605,-92.2807176036799));
#186218=CARTESIAN_POINT('Ctrl Pts',(2.98873306176462,31.7699592888437,-92.2913177201448));
#186219=CARTESIAN_POINT('Ctrl Pts',(2.98968665019425,31.7984733669073,-92.3010917718003));
#186220=CARTESIAN_POINT('Ctrl Pts',(2.99068186466826,31.8282616120353,-92.3097564908611));
#186221=CARTESIAN_POINT('Ctrl Pts',(2.99107431360402,31.8400081906916,-92.3131733018732));
#186222=CARTESIAN_POINT('Ctrl Pts',(2.99147321684361,31.8519523538066,-92.3164174876833));
#186223=CARTESIAN_POINT('Ctrl Pts',(2.99187828661466,31.8640859130555,-92.3194712210215));
#186224=CARTESIAN_POINT('Ctrl Pts',(2.99279119518676,31.8914314002778,-92.3263534411737));
#186225=CARTESIAN_POINT('Ctrl Pts',(2.99373551476277,31.919741474585,-92.332271745838));
#186226=CARTESIAN_POINT('Ctrl Pts',(2.99471042887811,31.9489972704144,-92.3370248940461));
#186227=CARTESIAN_POINT('Ctrl Pts',(2.99563020838728,31.9765985545735,-92.3415092360585));
#186228=CARTESIAN_POINT('Ctrl Pts',(2.9965772290768,32.0050418930296,-92.3449564431487));
#186229=CARTESIAN_POINT('Ctrl Pts',(2.99754983431874,32.0342833809711,-92.3471621364646));
#186230=CARTESIAN_POINT('Ctrl Pts',(2.99834977367418,32.0583336492687,-92.3489762546837));
#186231=CARTESIAN_POINT('Ctrl Pts',(2.9991670082457,32.0829234978557,-92.34995));
#186232=CARTESIAN_POINT('Ctrl Pts',(3.,32.1080106234021,-92.34995));
#186233=CARTESIAN_POINT('Origin',(2.99219087770694,31.868484915383,-91.2979036528092));
#186234=CARTESIAN_POINT('Ctrl Pts',(3.5,31.6538440087773,-91.1386408691297));
#186235=CARTESIAN_POINT('Ctrl Pts',(3.5,31.1724436113174,-90.9136534008893));
#186236=CARTESIAN_POINT('Ctrl Pts',(2.96960200166493,31.2017108282785,-90.9273317382593));
#186237=CARTESIAN_POINT('Ctrl Pts',(3.5,36.338906312512,-81.114123180147));
#186238=CARTESIAN_POINT('Ctrl Pts',(3.50000000000001,35.8447898541155,-80.9243218897256));
#186239=CARTESIAN_POINT('Ctrl Pts',(2.97277930784816,35.8865598281193,-80.9028133775132));
#186240=CARTESIAN_POINT('Ctrl Pts',(3.5,41.0213995348936,-71.0884053145847));
#186241=CARTESIAN_POINT('Ctrl Pts',(3.49999999995192,40.5360321489106,-70.8854859061211));
#186242=CARTESIAN_POINT('Ctrl Pts',(2.97501738453455,40.5689313038002,-70.8770956617078));
#186243=CARTESIAN_POINT('Ctrl Pts',(3.5,45.7028119503364,-61.0621827299711));
#186244=CARTESIAN_POINT('Ctrl Pts',(3.5,45.2282873890496,-60.8406192095206));
#186245=CARTESIAN_POINT('Ctrl Pts',(2.97685902995381,45.2502493063675,-60.8508735991007));
#186246=CARTESIAN_POINT('',(2.97685902995381,45.2502493063675,-60.8508735991007));
#186247=CARTESIAN_POINT('Origin',(3.,45.7028119503364,-61.0621827299711));
#186248=CARTESIAN_POINT('Ctrl Pts',(2.97685902995381,45.2502493063675,-60.8508735991007));
#186249=CARTESIAN_POINT('Ctrl Pts',(2.97608222207012,43.2756646801029,-65.079944115883));
#186250=CARTESIAN_POINT('Ctrl Pts',(2.9752678572138,41.3885517362141,-69.1211703991517));
#186251=CARTESIAN_POINT('Ctrl Pts',(2.97440329692527,39.5888778999211,-72.974536173095));
#186252=CARTESIAN_POINT('Ctrl Pts',(2.97345929524181,37.6238383836545,-77.1819741342009));
#186253=CARTESIAN_POINT('Ctrl Pts',(2.97245555482809,35.7630454531903,-81.1654419117765));
#186254=CARTESIAN_POINT('Ctrl Pts',(2.97139650992555,34.0065114235406,-84.9249450806595));
#186255=CARTESIAN_POINT('Ctrl Pts',(2.97081378910475,33.0400094848007,-86.9935455404804));
#186256=CARTESIAN_POINT('Ctrl Pts',(2.97021467020169,32.1050734276472,-88.9943398821521));
#186257=CARTESIAN_POINT('Ctrl Pts',(2.96960200166741,31.2017108282783,-90.9273317382593));
#186258=CARTESIAN_POINT('Ctrl Pts',(3.5,45.7028119503364,-61.0621827299711));
#186259=CARTESIAN_POINT('Ctrl Pts',(3.50000000000001,45.2282873890497,-60.8406192095206));
#186260=CARTESIAN_POINT('Ctrl Pts',(2.97685902995381,45.2502493063675,-60.8508735991007));
#186261=CARTESIAN_POINT('Ctrl Pts',(3.5,45.7953890262578,-60.8639095446885));
#186262=CARTESIAN_POINT('Ctrl Pts',(3.49999999999858,45.287151661289,-60.7107288313437));
#186263=CARTESIAN_POINT('Ctrl Pts',(2.97532164922327,45.3120457868827,-60.7186918897092));
#186264=CARTESIAN_POINT('Ctrl Pts',(3.5,45.8435334327792,-60.6493041067215));
#186265=CARTESIAN_POINT('Ctrl Pts',(3.50000000000077,45.317377912702,-60.5716465029093));
#186266=CARTESIAN_POINT('Ctrl Pts',(2.97452770132487,45.3441826962796,-60.5756208725641));
#186267=CARTESIAN_POINT('Ctrl Pts',(3.5,45.8435334367418,-60.42825533736));
#186268=CARTESIAN_POINT('Ctrl Pts',(3.5,45.3173779148743,-60.42825533736));
#186269=CARTESIAN_POINT('Ctrl Pts',(2.97452770112504,45.3441826962898,-60.42825533736));
#186270=CARTESIAN_POINT('',(2.97452770112504,45.3441826962898,-60.42825533736));
#186271=CARTESIAN_POINT('Origin',(3.01136102441785,43.8634705376828,-60.3227888586894));
#186272=CARTESIAN_POINT('Origin',(3.,45.8435334367418,-60.42825533736));
#186273=CARTESIAN_POINT('Origin',(24.7,67.7009572055632,-55.74995));
#186274=CARTESIAN_POINT('',(24.8935146892254,-66.4063101061761,-55.2889163081141));
#186275=CARTESIAN_POINT('Ctrl Pts',(25.2,-66.3526821257161,-55.74995));
#186276=CARTESIAN_POINT('Ctrl Pts',(25.2,-66.352682125716,-55.721081183649));
#186277=CARTESIAN_POINT('Ctrl Pts',(25.1974331879958,-66.3531312596204,
-55.6919499699875));
#186278=CARTESIAN_POINT('Ctrl Pts',(25.1922799898092,-66.3540329524655,
-55.6630004684243));
#186279=CARTESIAN_POINT('Ctrl Pts',(25.1889659954452,-66.3546128263415,
-55.644383197839));
#186280=CARTESIAN_POINT('Ctrl Pts',(25.1845828022603,-66.3553797857692,
-55.6258420559621));
#186281=CARTESIAN_POINT('Ctrl Pts',(25.1791300982028,-66.3563338853502,
-55.6075053780511));
#186282=CARTESIAN_POINT('Ctrl Pts',(25.1715115231656,-66.3576669632459,
-55.5818851802329));
#186283=CARTESIAN_POINT('Ctrl Pts',(25.1618029424538,-66.3593657447479,
-55.5566554601816));
#186284=CARTESIAN_POINT('Ctrl Pts',(25.150005285251,-66.3614300672704,-55.5321823974089));
#186285=CARTESIAN_POINT('Ctrl Pts',(25.145622779736,-66.362196906371,-55.5230913269764));
#186286=CARTESIAN_POINT('Ctrl Pts',(25.1409521535631,-66.3630141600543,
-55.5141052166639));
#186287=CARTESIAN_POINT('Ctrl Pts',(25.1359942361077,-66.3638816831983,
-55.5052447720227));
#186288=CARTESIAN_POINT('Ctrl Pts',(25.1334491307288,-66.3643270189345,
-55.5006963370159));
#186289=CARTESIAN_POINT('Ctrl Pts',(25.1306700660852,-66.3648132922397,
-55.4959068094754));
#186290=CARTESIAN_POINT('Ctrl Pts',(25.1278462777817,-66.3653073850614,
-55.4912277069156));
#186291=CARTESIAN_POINT('Ctrl Pts',(25.1249297654731,-66.365817702281,-55.4863949578771));
#186292=CARTESIAN_POINT('Ctrl Pts',(25.121965606198,-66.3663363501209,-55.4816803024046));
#186293=CARTESIAN_POINT('Ctrl Pts',(25.1192114572054,-66.3668182376422,
-55.4774411221205));
#186294=CARTESIAN_POINT('Ctrl Pts',(25.1182394326667,-66.3669883106836,
-55.4759449840135));
#186295=CARTESIAN_POINT('Ctrl Pts',(25.1172939855352,-66.3671537316268,
-55.4745077921305));
#186296=CARTESIAN_POINT('Ctrl Pts',(25.1163876444297,-66.3673123079502,
-55.4731444191925));
#186297=CARTESIAN_POINT('Ctrl Pts',(25.1055064504905,-66.3692161162602,
-55.4567762711959));
#186298=CARTESIAN_POINT('Ctrl Pts',(25.0932998315912,-66.3713519177965,
-55.4405626004351));
#186299=CARTESIAN_POINT('Ctrl Pts',(25.0797034238071,-66.3737309494593,
-55.4247364723726));
#186300=CARTESIAN_POINT('Ctrl Pts',(25.0666803568155,-66.376009660808,-55.4095777091722));
#186301=CARTESIAN_POINT('Ctrl Pts',(25.0523821103081,-66.3785115442445,
-55.3947744975832));
#186302=CARTESIAN_POINT('Ctrl Pts',(25.0367814521774,-66.381241342281,-55.3805688465406));
#186303=CARTESIAN_POINT('Ctrl Pts',(25.0215171215312,-66.3839122898447,
-55.3666694486599));
#186304=CARTESIAN_POINT('Ctrl Pts',(25.0050057348895,-66.386801465097,-55.3533420190667));
#186305=CARTESIAN_POINT('Ctrl Pts',(24.9872529759462,-66.3899078520514,
-55.3408505682589));
#186306=CARTESIAN_POINT('Ctrl Pts',(24.9700316183068,-66.3929212541304,
-55.3287330296565));
#186307=CARTESIAN_POINT('Ctrl Pts',(24.9516419793518,-66.3961390786697,
-55.3174021413002));
#186308=CARTESIAN_POINT('Ctrl Pts',(24.9321210832928,-66.3995548271715,
-55.307135300076));
#186309=CARTESIAN_POINT('Ctrl Pts',(24.919703751785,-66.4017276004585,-55.3006045152886));
#186310=CARTESIAN_POINT('Ctrl Pts',(24.9068293227691,-66.403980347188,-55.2945050041632));
#186311=CARTESIAN_POINT('Ctrl Pts',(24.8935146892254,-66.4063101061761,
-55.2889163081141));
#186312=CARTESIAN_POINT('',(24.7,-66.4710859610356,-55.24995));
#186313=CARTESIAN_POINT('Ctrl Pts',(24.8935146892254,-66.4063101061761,
-55.2889163081141));
#186314=CARTESIAN_POINT('Ctrl Pts',(24.8743436827644,-66.4096645924202,
-55.2808694529217));
#186315=CARTESIAN_POINT('Ctrl Pts',(24.8548198692694,-66.4139932223095,
-55.2740625582484));
#186316=CARTESIAN_POINT('Ctrl Pts',(24.8350955380933,-66.4193328230275,
-55.2685172310238));
#186317=CARTESIAN_POINT('Ctrl Pts',(24.8153425491825,-66.4246801817201,
-55.2629638469218));
#186318=CARTESIAN_POINT('Ctrl Pts',(24.7953888759615,-66.4310416706885,
-55.2586755730986));
#186319=CARTESIAN_POINT('Ctrl Pts',(24.7753941434843,-66.4384223361908,
-55.2556332240216));
#186320=CARTESIAN_POINT('Ctrl Pts',(24.7553495325246,-66.445821413362,-55.252583285558));
#186321=CARTESIAN_POINT('Ctrl Pts',(24.7352640798756,-66.4542449394322,
-55.2507853224051));
#186322=CARTESIAN_POINT('Ctrl Pts',(24.7152989762785,-66.4636628855439,
-55.2501811880231));
#186323=CARTESIAN_POINT('Ctrl Pts',(24.7101905706034,-66.4660726245733,
-55.2500266101373));
#186324=CARTESIAN_POINT('Ctrl Pts',(24.7050900275942,-66.4685472800516,
-55.24995));
#186325=CARTESIAN_POINT('Ctrl Pts',(24.7,-66.4710859610356,-55.24995));
#186326=CARTESIAN_POINT('',(24.7,-73.08000002,-55.24995));
#186327=CARTESIAN_POINT('Origin',(41.5,-73.08000002,-55.24995));
#186328=CARTESIAN_POINT('',(24.2743783673579,-66.6190816475223,-55.24995));
#186329=CARTESIAN_POINT('Origin',(25.30491873532,-68.8967968514054,-55.24995));
#186330=CARTESIAN_POINT('Origin',(0.,-12.9675000200281,-55.24995));
#186331=CARTESIAN_POINT('Origin',(0.,-12.9675000200281,-60.64995));
#186332=CARTESIAN_POINT('',(43.0192624284939,-63.3317132462777,-60.64995));
#186333=CARTESIAN_POINT('',(4.6996065532056,-66.6842487255793,-60.64995));
#186334=CARTESIAN_POINT('',(50.3642132262497,-55.9867624485218,-60.64995));
#186335=CARTESIAN_POINT('',(53.7167487055513,-17.6671065732338,-60.64995));
#186336=CARTESIAN_POINT('',(49.7860373924393,-57.2266645253997,-60.64995));
#186337=CARTESIAN_POINT('Origin',(48.3718238300662,-55.8124509630266,-60.64995));
#186338=CARTESIAN_POINT('',(44.2591645053717,-62.7535374124673,-60.64995));
#186339=CARTESIAN_POINT('',(47.0226009489055,-59.9901009689335,-60.64995));
#186340=CARTESIAN_POINT('Origin',(42.8449509429986,-61.3393238500942,-60.64995));
#186341=CARTESIAN_POINT('Origin',(0.,-12.9675000200281,-60.64995));
#186342=CARTESIAN_POINT('',(50.3642132262496,30.0517624084658,-60.64995));
#186343=CARTESIAN_POINT('',(53.7167487055517,-8.26789346682159,-60.64995));
#186344=CARTESIAN_POINT('',(43.019262428494,37.3967132062212,-60.64995));
#186345=CARTESIAN_POINT('',(4.69960655320655,40.7492486855235,-60.64995));
#186346=CARTESIAN_POINT('',(44.2591645053719,36.8185373724109,-60.64995));
#186347=CARTESIAN_POINT('Origin',(42.8449509429988,35.4043238100378,-60.64995));
#186348=CARTESIAN_POINT('',(49.7860373924392,31.2916644853436,-60.64995));
#186349=CARTESIAN_POINT('',(47.0226009489055,34.0551009288773,-60.64995));
#186350=CARTESIAN_POINT('Origin',(48.3718238300661,29.8774509229704,-60.64995));
#186351=CARTESIAN_POINT('Origin',(53.7167487055513,-17.6671065732338,-59.64995));
#186352=CARTESIAN_POINT('',(52.6206164493,-41.6696688386047,-59.64995));
#186353=CARTESIAN_POINT('',(52.9858497431864,-37.4950331867729,-59.64995));
#186354=CARTESIAN_POINT('Origin',(51.6244217512083,-41.5825130958571,-59.64995));
#186355=CARTESIAN_POINT('Origin',(52.8810286821225,-44.43000002,-52.64995));
#186356=CARTESIAN_POINT('',(52.3810286821225,-44.43000002,-55.74995));
#186357=CARTESIAN_POINT('Origin',(52.8810286821225,-44.43000002,-55.74995));
#186358=CARTESIAN_POINT('',(52.3829313330767,-44.3864221486262,-55.74995));
#186359=CARTESIAN_POINT('',(52.3829313330767,-44.3864221486262,-52.64995));
#186360=CARTESIAN_POINT('Origin',(52.8810286821225,-44.43000002,-55.74995));
#186361=CARTESIAN_POINT('Ctrl Pts',(52.8810286821225,-44.93000002,-55.74995));
#186362=CARTESIAN_POINT('Ctrl Pts',(52.3353744315879,-44.93000002,-55.74995));
#186363=CARTESIAN_POINT('Ctrl Pts',(52.3829313330767,-44.3864221486262,
-55.74995));
#186364=CARTESIAN_POINT('Ctrl Pts',(52.8810286821171,-44.93000002,-55.6186826543063));
#186365=CARTESIAN_POINT('Ctrl Pts',(52.3353744315888,-44.9300000200045,
-55.6317784220498));
#186366=CARTESIAN_POINT('Ctrl Pts',(52.3829313330709,-44.3864221486917,
-55.4874153086129));
#186367=CARTESIAN_POINT('Ctrl Pts',(52.8715997552662,-44.9838865835627,
-55.4889566552507));
#186368=CARTESIAN_POINT('Ctrl Pts',(52.3317239990966,-44.9717246542945,
-55.5133819370972));
#186369=CARTESIAN_POINT('Ctrl Pts',(52.3735024062205,-44.4941952757516,
-55.2279633105015));
#186370=CARTESIAN_POINT('Ctrl Pts',(52.8392079364393,-45.1690066752507,
-55.3038365635627));
#186371=CARTESIAN_POINT('Ctrl Pts',(52.317584547802,-45.1333393221421,-55.3274496218433));
#186372=CARTESIAN_POINT('Ctrl Pts',(52.3411105873933,-44.8644354591276,
-54.8577231271254));
#186373=CARTESIAN_POINT('Ctrl Pts',(52.8165088278734,-45.2987326743059,
-55.24995));
#186374=CARTESIAN_POINT('Ctrl Pts',(52.3071965192496,-45.252075031829,-55.2615708605687));
#186375=CARTESIAN_POINT('Ctrl Pts',(52.3184114788294,-45.1238874572391,
-54.7499500000658));
#186376=CARTESIAN_POINT('Ctrl Pts',(52.7935400185966,-45.43000002,-55.24995));
#186377=CARTESIAN_POINT('Ctrl Pts',(52.2954426695507,-45.3864221486261,
-55.2499499999999));
#186378=CARTESIAN_POINT('Ctrl Pts',(52.2954426695508,-45.3864221486262,
-54.74995));
#186379=CARTESIAN_POINT('',(52.2954426695508,-45.3864221486261,-54.74995));
#186380=CARTESIAN_POINT('Origin',(52.7935400185966,-45.43000002,-54.74995));
#186381=CARTESIAN_POINT('Ctrl Pts',(52.2954426695508,-45.3864221486261,
-54.74995));
#186382=CARTESIAN_POINT('Ctrl Pts',(52.3184114788294,-45.123887457239,-54.7499500000658));
#186383=CARTESIAN_POINT('Ctrl Pts',(52.3411105873933,-44.8644354591276,
-54.8577231271254));
#186384=CARTESIAN_POINT('Ctrl Pts',(52.3573064968069,-44.6793153674396,
-55.0428432188135));
#186385=CARTESIAN_POINT('Ctrl Pts',(52.3735024062205,-44.4941952757516,
-55.2279633105015));
#186386=CARTESIAN_POINT('Ctrl Pts',(52.3829313330709,-44.3864221486917,
-55.4874153086129));
#186387=CARTESIAN_POINT('Ctrl Pts',(52.3829313330767,-44.3864221486262,
-55.74995));
#186388=CARTESIAN_POINT('Origin',(53.4839470922323,-37.5386110581466,-54.74995));
#186389=CARTESIAN_POINT('',(52.2516983377878,-45.8864221486262,-54.74995));
#186390=CARTESIAN_POINT('Origin',(52.7497956868337,-45.93000002,-54.74995));
#186391=CARTESIAN_POINT('',(52.9858497431864,-37.4950331867729,-54.74995));
#186392=CARTESIAN_POINT('Ctrl Pts',(52.7497956868337,-45.93000002,-55.24995));
#186393=CARTESIAN_POINT('Ctrl Pts',(52.2516983377878,-45.8864221486262,
-55.24995));
#186394=CARTESIAN_POINT('Ctrl Pts',(52.2516983377878,-45.8864221486262,
-54.74995));
#186395=CARTESIAN_POINT('Ctrl Pts',(52.7268268775569,-46.0612673656941,
-55.24995));
#186396=CARTESIAN_POINT('Ctrl Pts',(52.2402778440398,-46.0169589895406,
-55.2386587236919));
#186397=CARTESIAN_POINT('Ctrl Pts',(52.2287295285091,-46.1489568400132,
-54.7499500000658));
#186398=CARTESIAN_POINT('Ctrl Pts',(52.704127768991,-46.1909933647493,-55.3038365635627));
#186399=CARTESIAN_POINT('Ctrl Pts',(52.227884321682,-46.1586175982532,-55.2822894538777));
#186400=CARTESIAN_POINT('Ctrl Pts',(52.2060304199453,-46.4084088381247,
-54.8577231271255));
#186401=CARTESIAN_POINT('Ctrl Pts',(52.6717359501641,-46.3761134564373,
-55.4889566552507));
#186402=CARTESIAN_POINT('Ctrl Pts',(52.2097524154255,-46.3658662351156,
-55.4680441063688));
#186403=CARTESIAN_POINT('Ctrl Pts',(52.1736386011181,-46.7786490215007,
-55.2279633105015));
#186404=CARTESIAN_POINT('Ctrl Pts',(52.6623070233132,-46.43000002,-55.6186826543062));
#186405=CARTESIAN_POINT('Ctrl Pts',(52.2041414362981,-46.4300000199443,
-55.6078478088784));
#186406=CARTESIAN_POINT('Ctrl Pts',(52.1642096742676,-46.8864221485606,
-55.487415308613));
#186407=CARTESIAN_POINT('Ctrl Pts',(52.6623070233078,-46.43000002,-55.74995));
#186408=CARTESIAN_POINT('Ctrl Pts',(52.2041414362991,-46.43000002,-55.74995));
#186409=CARTESIAN_POINT('Ctrl Pts',(52.1642096742619,-46.8864221486262,
-55.74995));
#186410=CARTESIAN_POINT('',(52.1642096742619,-46.8864221486262,-55.74995));
#186411=CARTESIAN_POINT('Origin',(52.6623070233078,-46.93000002,-55.74995));
#186412=CARTESIAN_POINT('Ctrl Pts',(52.1642096742619,-46.8864221486262,
-55.74995));
#186413=CARTESIAN_POINT('Ctrl Pts',(52.1642096742676,-46.8864221485606,
-55.487415308613));
#186414=CARTESIAN_POINT('Ctrl Pts',(52.1736386011181,-46.7786490215007,
-55.2279633105015));
#186415=CARTESIAN_POINT('Ctrl Pts',(52.1898345105317,-46.5935289298127,
-55.0428432188135));
#186416=CARTESIAN_POINT('Ctrl Pts',(52.2060304199453,-46.4084088381247,
-54.8577231271255));
#186417=CARTESIAN_POINT('Ctrl Pts',(52.2287295285091,-46.1489568400132,
-54.7499500000658));
#186418=CARTESIAN_POINT('Ctrl Pts',(52.2516983377878,-45.8864221486262,
-54.74995));
#186419=CARTESIAN_POINT('Origin',(52.6623070233078,-46.93000002,-52.64995));
#186420=CARTESIAN_POINT('',(52.1642096742619,-46.8864221486262,-52.64995));
#186421=CARTESIAN_POINT('Origin',(53.7167487055513,-17.6671065732338,-59.64995));
#186422=CARTESIAN_POINT('',(52.9858497431864,-37.4950331867729,-59.64995));
#186423=CARTESIAN_POINT('Origin',(52.1679960743864,-52.58000002,-55.2499500000008));
#186424=CARTESIAN_POINT('',(51.6698987253405,-52.5364221486262,-55.74995));
#186425=CARTESIAN_POINT('Origin',(52.1679960743864,-52.58000002,-55.74995));
#186426=CARTESIAN_POINT('',(51.6698987253405,-52.5364221486262,-52.64995));
#186427=CARTESIAN_POINT('Ctrl Pts',(52.1679960743864,-53.08000002,-55.74995));
#186428=CARTESIAN_POINT('Ctrl Pts',(51.6223418238518,-53.08000002,-55.74995));
#186429=CARTESIAN_POINT('Ctrl Pts',(51.6698987253405,-52.5364221486262,
-55.74995));
#186430=CARTESIAN_POINT('Ctrl Pts',(52.1679960743809,-53.08000002,-55.6186826543066));
#186431=CARTESIAN_POINT('Ctrl Pts',(51.6223418238527,-53.0800000200045,
-55.6317784220505));
#186432=CARTESIAN_POINT('Ctrl Pts',(51.6698987253348,-52.5364221486917,
-55.4874153086129));
#186433=CARTESIAN_POINT('Ctrl Pts',(52.1585671475301,-53.1338865835632,
-55.4889566552503));
#186434=CARTESIAN_POINT('Ctrl Pts',(51.6186913913614,-53.1217246542964,
-55.5133819370962));
#186435=CARTESIAN_POINT('Ctrl Pts',(51.6604697984843,-52.6441952757516,
-55.2279633105015));
#186436=CARTESIAN_POINT('Ctrl Pts',(52.1261753287031,-53.3190066752503,
-55.3038365635632));
#186437=CARTESIAN_POINT('Ctrl Pts',(51.6045519400649,-53.2833393221403,
-55.327449621844));
#186438=CARTESIAN_POINT('Ctrl Pts',(51.6280779796571,-53.0144354591276,
-54.8577231271254));
#186439=CARTESIAN_POINT('Ctrl Pts',(52.1034762201372,-53.4487326743062,
-55.24995));
#186440=CARTESIAN_POINT('Ctrl Pts',(51.5941639115132,-53.4020750318305,
-55.2615708605685));
#186441=CARTESIAN_POINT('Ctrl Pts',(51.6053788710933,-53.2738874572391,
-54.7499500000658));
#186442=CARTESIAN_POINT('Ctrl Pts',(52.0805074108605,-53.58000002,-55.24995));
#186443=CARTESIAN_POINT('Ctrl Pts',(51.5824100618146,-53.5364221486261,
-55.2499499999999));
#186444=CARTESIAN_POINT('Ctrl Pts',(51.5824100618146,-53.5364221486262,
-54.74995));
#186445=CARTESIAN_POINT('',(51.5824100618146,-53.5364221486262,-54.74995));
#186446=CARTESIAN_POINT('Origin',(52.0805074108605,-53.58000002,-54.74995));
#186447=CARTESIAN_POINT('Ctrl Pts',(51.5824100618146,-53.5364221486262,
-54.74995));
#186448=CARTESIAN_POINT('Ctrl Pts',(51.6053788710933,-53.2738874572391,
-54.7499500000658));
#186449=CARTESIAN_POINT('Ctrl Pts',(51.6280779796571,-53.0144354591276,
-54.8577231271254));
#186450=CARTESIAN_POINT('Ctrl Pts',(51.6442738890707,-52.8293153674396,
-55.0428432188135));
#186451=CARTESIAN_POINT('Ctrl Pts',(51.6604697984843,-52.6441952757516,
-55.2279633105015));
#186452=CARTESIAN_POINT('Ctrl Pts',(51.6698987253348,-52.5364221486917,
-55.4874153086129));
#186453=CARTESIAN_POINT('Ctrl Pts',(51.6698987253405,-52.5364221486262,
-55.74995));
#186454=CARTESIAN_POINT('Origin',(53.4839470922323,-37.5386110581466,-54.74995));
#186455=CARTESIAN_POINT('',(51.5386657300517,-54.0364221486261,-54.74995));
#186456=CARTESIAN_POINT('Origin',(52.0367630790975,-54.08000002,-54.74995));
#186457=CARTESIAN_POINT('',(52.9858497431864,-37.4950331867729,-54.74995));
#186458=CARTESIAN_POINT('Ctrl Pts',(52.0367630790975,-54.08000002,-55.24995));
#186459=CARTESIAN_POINT('Ctrl Pts',(51.5386657300516,-54.0364221486262,
-55.24995));
#186460=CARTESIAN_POINT('Ctrl Pts',(51.5386657300517,-54.0364221486262,
-54.74995));
#186461=CARTESIAN_POINT('Ctrl Pts',(52.0137942698207,-54.2112673656937,
-55.24995));
#186462=CARTESIAN_POINT('Ctrl Pts',(51.5272452363036,-54.1669589895393,
-55.2386587236848));
#186463=CARTESIAN_POINT('Ctrl Pts',(51.5156969207731,-54.2989568400126,
-54.7499500000658));
#186464=CARTESIAN_POINT('Ctrl Pts',(51.9910951612549,-54.3409933647497,
-55.3038365635632));
#186465=CARTESIAN_POINT('Ctrl Pts',(51.5148517139458,-54.308617598254,-55.2822894538766));
#186466=CARTESIAN_POINT('Ctrl Pts',(51.4929978122091,-54.5584088381255,
-54.8577231271254));
#186467=CARTESIAN_POINT('Ctrl Pts',(51.958703342428,-54.5261134564368,-55.4889566552503));
#186468=CARTESIAN_POINT('Ctrl Pts',(51.4967198076894,-54.5158662351146,
-55.4680441063697));
#186469=CARTESIAN_POINT('Ctrl Pts',(51.460605993382,-54.9286490214999,-55.2279633105015));
#186470=CARTESIAN_POINT('Ctrl Pts',(51.9492744155771,-54.58000002,-55.6186826543065));
#186471=CARTESIAN_POINT('Ctrl Pts',(51.491108828562,-54.5800000199489,-55.6078478088776));
#186472=CARTESIAN_POINT('Ctrl Pts',(51.4511770665315,-55.0364221485606,
-55.4874153086129));
#186473=CARTESIAN_POINT('Ctrl Pts',(51.9492744155716,-54.58000002,-55.74995));
#186474=CARTESIAN_POINT('Ctrl Pts',(51.491108828563,-54.58000002,-55.74995));
#186475=CARTESIAN_POINT('Ctrl Pts',(51.4511770665258,-55.0364221486262,
-55.74995));
#186476=CARTESIAN_POINT('',(51.4511770665258,-55.0364221486262,-55.74995));
#186477=CARTESIAN_POINT('Origin',(51.9492744155716,-55.08000002,-55.74995));
#186478=CARTESIAN_POINT('Ctrl Pts',(51.4511770665258,-55.0364221486262,
-55.74995));
#186479=CARTESIAN_POINT('Ctrl Pts',(51.4511770665315,-55.0364221485606,
-55.4874153086129));
#186480=CARTESIAN_POINT('Ctrl Pts',(51.460605993382,-54.9286490214999,-55.2279633105015));
#186481=CARTESIAN_POINT('Ctrl Pts',(51.4768019027956,-54.7435289298127,
-55.0428432188135));
#186482=CARTESIAN_POINT('Ctrl Pts',(51.4929978122091,-54.5584088381255,
-54.8577231271254));
#186483=CARTESIAN_POINT('Ctrl Pts',(51.5156969207731,-54.2989568400126,
-54.7499500000658));
#186484=CARTESIAN_POINT('Ctrl Pts',(51.5386657300517,-54.0364221486262,
-54.74995));
#186485=CARTESIAN_POINT('Origin',(51.9492744155716,-55.08000002,-52.64995));
#186486=CARTESIAN_POINT('',(51.4511770665258,-55.0364221486262,-52.64995));
#186487=CARTESIAN_POINT('Origin',(53.7167487055513,-17.6671065732338,-59.64995));
#186488=CARTESIAN_POINT('',(51.3604079243415,-56.0739181912695,-59.64995));
#186489=CARTESIAN_POINT('',(52.9858497431864,-37.4950331867729,-59.64995));
#186490=CARTESIAN_POINT('Origin',(50.3642132262497,-55.9867624485218,-59.64995));
#186491=CARTESIAN_POINT('Ctrl Pts',(53.4093483797613,-38.0856391317044,
-55.3542421110299));
#186492=CARTESIAN_POINT('Ctrl Pts',(52.9364314216307,-38.0597244105783,
-55.3342259538136));
#186493=CARTESIAN_POINT('Ctrl Pts',(52.9112502355242,-38.3477094636814,
-54.9585223635782));
#186494=CARTESIAN_POINT('Ctrl Pts',(53.3880736387225,-38.2072248331335,
-55.448153047952));
#186495=CARTESIAN_POINT('Ctrl Pts',(52.9247563553463,-38.1931762538392,
-55.4246794702588));
#186496=CARTESIAN_POINT('Ctrl Pts',(52.889976625843,-38.5908679349475,-55.1463344612842));
#186497=CARTESIAN_POINT('Ctrl Pts',(53.375339024416,-38.2800034869308,-55.5963379967406));
#186498=CARTESIAN_POINT('Ctrl Pts',(52.9171601694683,-38.2800041317283,
-55.5832548498195));
#186499=CARTESIAN_POINT('Ctrl Pts',(52.87724039479,-38.7364437219894,-55.4427310705271));
#186500=CARTESIAN_POINT('Ctrl Pts',(53.3753396310656,-38.2800000198762,
-55.7499609770277));
#186501=CARTESIAN_POINT('Ctrl Pts',(52.9171605282557,-38.2800000198531,
-55.7499619127669));
#186502=CARTESIAN_POINT('Ctrl Pts',(52.8772410016055,-38.736436786057,-55.7499719536926));
#186503=CARTESIAN_POINT('',(52.9112495105562,-38.347717747534,-54.9585476429427));
#186504=CARTESIAN_POINT('Origin',(53.4093468596021,-38.3912956189078,-54.9585476429427));
#186505=CARTESIAN_POINT('',(52.877242281998,-38.7364221486262,-55.74995));
#186506=CARTESIAN_POINT('Origin',(52.954126623731,-37.8576301013555,-55.6904184160469));
#186507=CARTESIAN_POINT('Origin',(53.3753396310439,-38.78000002,-55.74995));
#186508=CARTESIAN_POINT('Origin',(53.3753396310439,-38.78000002,-55.2499500000007));
#186509=CARTESIAN_POINT('',(52.877242281998,-38.7364221486262,-52.64995));
#186510=CARTESIAN_POINT('Ctrl Pts',(52.903095448475,-38.4409191036023,-60.08258062683));
#186511=CARTESIAN_POINT('Ctrl Pts',(52.8907789702838,-38.5816970935142,
-60.5786901973488));
#186512=CARTESIAN_POINT('Ctrl Pts',(52.4648996019023,-38.6266655296175,
-60.866265313415));
#186513=CARTESIAN_POINT('Ctrl Pts',(52.8569709369232,-38.9681246830787,
-59.9318336272105));
#186514=CARTESIAN_POINT('Ctrl Pts',(52.8442212423788,-39.1138543585791,
-60.5019204415683));
#186515=CARTESIAN_POINT('Ctrl Pts',(52.3309754745585,-39.1170130132287,
-60.7908684306025));
#186516=CARTESIAN_POINT('Ctrl Pts',(52.8102637225239,-39.5019905865797,
-59.8278758615346));
#186517=CARTESIAN_POINT('Ctrl Pts',(52.7984570004479,-39.6369420374376,
-60.4756484953684));
#186518=CARTESIAN_POINT('Ctrl Pts',(52.1936254351686,-39.6095793654924,
-60.7389129305601));
#186519=CARTESIAN_POINT('Ctrl Pts',(52.7160699755127,-40.5786300415107,
-59.6865014144928));
#186520=CARTESIAN_POINT('Ctrl Pts',(52.7078841622538,-40.6721943151964,
-60.4973085875933));
#186521=CARTESIAN_POINT('Ctrl Pts',(51.9132529272684,-40.5953951229239,
-60.6682257074536));
#186522=CARTESIAN_POINT('Ctrl Pts',(52.6685584273161,-41.1216895223836,
-59.6499500020974));
#186523=CARTESIAN_POINT('Ctrl Pts',(52.662477767809,-41.1911917785403,-60.5526719649898));
#186524=CARTESIAN_POINT('Ctrl Pts',(51.7702028983306,-41.0887654988916,
-60.64995));
#186525=CARTESIAN_POINT('Ctrl Pts',(52.6206164493,-41.6696688386047,-59.64995));
#186526=CARTESIAN_POINT('Ctrl Pts',(52.6206164493,-41.6696688386047,-60.64995));
#186527=CARTESIAN_POINT('Ctrl Pts',(51.6244217512083,-41.5825130958571,
-60.64995));
#186528=CARTESIAN_POINT('Ctrl Pts',(52.6206164493,-41.6696688386047,-59.64995));
#186529=CARTESIAN_POINT('Ctrl Pts',(52.647177193844,-41.3660781392669,-59.649950001162));
#186530=CARTESIAN_POINT('Ctrl Pts',(52.6736027803761,-41.0640322847493,
-59.6612277190034));
#186531=CARTESIAN_POINT('Ctrl Pts',(52.6998985433583,-40.763470321929,-59.6832689389187));
#186532=CARTESIAN_POINT('Ctrl Pts',(52.7166476389893,-40.5720272722755,
-59.6973081018224));
#186533=CARTESIAN_POINT('Ctrl Pts',(52.7333441220441,-40.3811856094009,
-59.7157148983376));
#186534=CARTESIAN_POINT('Ctrl Pts',(52.7499897489645,-40.1909252438875,
-59.7383666003327));
#186535=CARTESIAN_POINT('Ctrl Pts',(52.7543856861046,-40.1406794579502,
-59.7443486795034));
#186536=CARTESIAN_POINT('Ctrl Pts',(52.7587779570344,-40.0904755740926,
-59.7506312543479));
#186537=CARTESIAN_POINT('Ctrl Pts',(52.7631665715902,-40.0403134816151,
-59.7572129455377));
#186538=CARTESIAN_POINT('Ctrl Pts',(52.7801318002604,-39.8464000361233,
-59.7826560311971));
#186539=CARTESIAN_POINT('Ctrl Pts',(52.7970456659898,-39.6530737072156,
-59.8124579292866));
#186540=CARTESIAN_POINT('Ctrl Pts',(52.8138987094321,-39.4604424150672,
-59.8472750881764));
#186541=CARTESIAN_POINT('Ctrl Pts',(52.8286848633259,-39.2914357937869,
-59.877822203969));
#186542=CARTESIAN_POINT('Ctrl Pts',(52.8434252414643,-39.1229522134604,
-59.9121898106578));
#186543=CARTESIAN_POINT('Ctrl Pts',(52.8581158408277,-38.9550379662969,
-59.9506823384307));
#186544=CARTESIAN_POINT('Ctrl Pts',(52.8645007938109,-38.882057651007,-59.9674122875603));
#186545=CARTESIAN_POINT('Ctrl Pts',(52.8708763604388,-38.8091846968994,
-59.9849220508816));
#186546=CARTESIAN_POINT('Ctrl Pts',(52.877242268511,-38.7364221474456,-60.003239652154));
#186547=CARTESIAN_POINT('Origin',(52.6819919725962,20.76999998,-52.64995));
#186548=CARTESIAN_POINT('',(52.1838946235503,20.7264221086262,-55.74995));
#186549=CARTESIAN_POINT('',(52.1838946235503,20.7264221086262,-52.64995));
#186550=CARTESIAN_POINT('Origin',(52.6819919725962,20.76999998,-55.74995));
#186551=CARTESIAN_POINT('Ctrl Pts',(52.6819919725962,20.26999998,-55.74995));
#186552=CARTESIAN_POINT('Ctrl Pts',(52.2238263855875,20.26999998,-55.74995));
#186553=CARTESIAN_POINT('Ctrl Pts',(52.1838946235503,20.7264221086262,-55.74995));
#186554=CARTESIAN_POINT('Ctrl Pts',(52.6819919726017,20.26999998,-55.6186826543063));
#186555=CARTESIAN_POINT('Ctrl Pts',(52.2238263855902,20.2699999799516,-55.6078478088784));
#186556=CARTESIAN_POINT('Ctrl Pts',(52.1838946235561,20.7264221085606,-55.487415308613));
#186557=CARTESIAN_POINT('Ctrl Pts',(52.6914208994525,20.2161134164373,-55.4889566552507));
#186558=CARTESIAN_POINT('Ctrl Pts',(52.229437364714,20.2058661951152,-55.4680441063689));
#186559=CARTESIAN_POINT('Ctrl Pts',(52.1933235504066,20.6186489815003,-55.2279633105015));
#186560=CARTESIAN_POINT('Ctrl Pts',(52.7238127182794,20.0309933247493,-55.3038365635627));
#186561=CARTESIAN_POINT('Ctrl Pts',(52.2475692709704,19.9986175582537,-55.2822894538776));
#186562=CARTESIAN_POINT('Ctrl Pts',(52.2257153692336,20.2484087981252,-54.8577231271255));
#186563=CARTESIAN_POINT('Ctrl Pts',(52.746511826845,19.901267325694,-55.24995));
#186564=CARTESIAN_POINT('Ctrl Pts',(52.2599627933277,19.8569589495402,-55.2386587236914));
#186565=CARTESIAN_POINT('Ctrl Pts',(52.2484144777976,19.9889568000129,-54.7499500000658));
#186566=CARTESIAN_POINT('Ctrl Pts',(52.7694806361221,19.76999998,-55.24995));
#186567=CARTESIAN_POINT('Ctrl Pts',(52.2713832870762,19.7264221086262,-55.2499499999999));
#186568=CARTESIAN_POINT('Ctrl Pts',(52.2713832870762,19.7264221086262,-54.74995));
#186569=CARTESIAN_POINT('',(52.2713832870762,19.7264221086262,-54.74995));
#186570=CARTESIAN_POINT('Origin',(52.7694806361221,19.76999998,-54.74995));
#186571=CARTESIAN_POINT('Ctrl Pts',(52.2713832870762,19.7264221086262,-54.74995));
#186572=CARTESIAN_POINT('Ctrl Pts',(52.2484144777976,19.9889568000129,-54.7499500000658));
#186573=CARTESIAN_POINT('Ctrl Pts',(52.2257153692336,20.2484087981252,-54.8577231271255));
#186574=CARTESIAN_POINT('Ctrl Pts',(52.2095194598201,20.4335288898127,-55.0428432188135));
#186575=CARTESIAN_POINT('Ctrl Pts',(52.1933235504066,20.6186489815003,-55.2279633105015));
#186576=CARTESIAN_POINT('Ctrl Pts',(52.1838946235561,20.7264221085606,-55.487415308613));
#186577=CARTESIAN_POINT('Ctrl Pts',(52.1838946235503,20.7264221086262,-55.74995));
#186578=CARTESIAN_POINT('Origin',(51.7633389850707,31.2702516755049,-54.74995));
#186579=CARTESIAN_POINT('',(52.3151276188392,19.2264221086262,-54.74995));
#186580=CARTESIAN_POINT('Origin',(52.8132249678851,19.26999998,-54.74995));
#186581=CARTESIAN_POINT('',(51.2652416360248,31.226673804131,-54.74995));
#186582=CARTESIAN_POINT('Ctrl Pts',(52.8132511574963,19.2700238915803,-55.2499499996828));
#186583=CARTESIAN_POINT('Ctrl Pts',(52.3151257340121,19.2264436522985,-55.2499781675605));
#186584=CARTESIAN_POINT('Ctrl Pts',(52.3151238928183,19.2264646972402,-54.7499500009454));
#186585=CARTESIAN_POINT('Ctrl Pts',(52.8362215618991,19.1387494339943,-55.2499434816102));
#186586=CARTESIAN_POINT('Ctrl Pts',(52.3268796769205,19.0920954701104,-55.26159490362));
#186587=CARTESIAN_POINT('Ctrl Pts',(52.3380939732538,18.9639154764634,-54.7499383449302));
#186588=CARTESIAN_POINT('Ctrl Pts',(52.8589226187611,19.0090137328179,-55.3038301720458));
#186589=CARTESIAN_POINT('Ctrl Pts',(52.3372676751065,18.9733601075009,-55.3274735569165));
#186590=CARTESIAN_POINT('Ctrl Pts',(52.3607946609107,18.7044454292369,-54.8577131170158));
#186591=CARTESIAN_POINT('Ctrl Pts',(52.8913167201329,18.823882239107,-55.4889602509492));
#186592=CARTESIAN_POINT('Ctrl Pts',(52.3514067244284,18.8117500342473,-55.5134049012176));
#186593=CARTESIAN_POINT('Ctrl Pts',(52.39318823128,18.3341852256424,-55.2279733206111));
#186594=CARTESIAN_POINT('Ctrl Pts',(52.9007459593775,18.7699941513777,-55.6186959323247));
#186595=CARTESIAN_POINT('Ctrl Pts',(52.3550567877969,18.7700296190381,-55.6318003689065));
#186596=CARTESIAN_POINT('Ctrl Pts',(52.4026173020516,18.2264104535562,-55.4874433678369));
#186597=CARTESIAN_POINT('Ctrl Pts',(52.9007449425538,18.7699999794923,-55.7499712944291));
#186598=CARTESIAN_POINT('Ctrl Pts',(52.3550563912364,18.770034151741,-55.7499691665881));
#186599=CARTESIAN_POINT('Ctrl Pts',(52.4026162822824,18.2264221095716,-55.749992588614));
#186600=CARTESIAN_POINT('',(52.4026162823651,18.2264221086262,-55.74995));
#186601=CARTESIAN_POINT('Origin',(52.900713631411,18.26999998,-55.74995));
#186602=CARTESIAN_POINT('Ctrl Pts',(52.4026162823651,18.2264221086262,-55.74995));
#186603=CARTESIAN_POINT('Ctrl Pts',(52.4026162823594,18.2264221086918,-55.4874153086129));
#186604=CARTESIAN_POINT('Ctrl Pts',(52.3931873555089,18.334195235752,-55.2279633105015));
#186605=CARTESIAN_POINT('Ctrl Pts',(52.3769914460954,18.5193153274396,-55.0428432188135));
#186606=CARTESIAN_POINT('Ctrl Pts',(52.3607955366818,18.7044354191273,-54.8577231271254));
#186607=CARTESIAN_POINT('Ctrl Pts',(52.3380964281178,18.9638874172394,-54.7499500000658));
#186608=CARTESIAN_POINT('Ctrl Pts',(52.3151276188392,19.2264221086262,-54.74995));
#186609=CARTESIAN_POINT('Origin',(52.900713631411,18.26999998,-52.64995));
#186610=CARTESIAN_POINT('',(52.4026162823651,18.2264221086262,-52.64995));
#186611=CARTESIAN_POINT('Origin',(53.7167487055517,-8.26789346682159,-59.64995));
#186612=CARTESIAN_POINT('',(52.6206164493001,15.7346687985483,-59.64995));
#186613=CARTESIAN_POINT('',(51.2652416360248,31.226673804131,-59.64995));
#186614=CARTESIAN_POINT('Origin',(51.6244217512084,15.6475130558006,-59.64995));
#186615=CARTESIAN_POINT('Ctrl Pts',(52.6206164493001,15.7346687985483,-59.64995));
#186616=CARTESIAN_POINT('Ctrl Pts',(52.6206164493002,15.7346687985482,-60.64995));
#186617=CARTESIAN_POINT('Ctrl Pts',(51.6244217512084,15.6475130558006,-60.64995));
#186618=CARTESIAN_POINT('Ctrl Pts',(52.6699713539896,15.1705396565499,-59.6499500021592));
#186619=CARTESIAN_POINT('Ctrl Pts',(52.6636514122595,15.2427769209991,-60.5499446302911));
#186620=CARTESIAN_POINT('Ctrl Pts',(51.7744992817202,15.1392139958173,-60.64995));
#186621=CARTESIAN_POINT('Ctrl Pts',(52.7188714030742,14.6116095379051,-59.6886254732604));
#186622=CARTESIAN_POINT('Ctrl Pts',(52.7104450878319,14.7079227618566,-60.4941916839025));
#186623=CARTESIAN_POINT('Ctrl Pts',(51.921686259274,14.6313008059217,-60.6692877368673));
#186624=CARTESIAN_POINT('Ctrl Pts',(52.8157906892286,13.5038170280144,-59.8384384618772));
#186625=CARTESIAN_POINT('Ctrl Pts',(52.8037229951722,13.64175140224,-60.4769182500017));
#186626=CARTESIAN_POINT('Ctrl Pts',(52.209973495227,13.6164898397673,-60.7441942307015));
#186627=CARTESIAN_POINT('Ctrl Pts',(52.8638414531199,12.954594283549,-59.9484723594913));
#186628=CARTESIAN_POINT('Ctrl Pts',(52.850859560631,13.1029779936029,-60.5072438893719));
#186629=CARTESIAN_POINT('Ctrl Pts',(52.3511088881553,13.109439201609,-60.799180633384));
#186630=CARTESIAN_POINT('Ctrl Pts',(52.9112495105564,12.4127177074772,-60.1097730249189));
#186631=CARTESIAN_POINT('Ctrl Pts',(52.8987763848902,12.5552861862208,-60.5923862926586));
#186632=CARTESIAN_POINT('Ctrl Pts',(52.4885489491165,12.6049688303995,-60.8798615124595));
#186633=CARTESIAN_POINT('Ctrl Pts',(52.8969272285826,12.5764221083876,-60.0627241236307));
#186634=CARTESIAN_POINT('Ctrl Pts',(52.8810850690579,12.757498700804,-60.0124953264531));
#186635=CARTESIAN_POINT('Ctrl Pts',(52.8651783101952,12.9393136629288,-59.9676531117601));
#186636=CARTESIAN_POINT('Ctrl Pts',(52.8492129207352,13.1217989910806,-59.9276740961144));
#186637=CARTESIAN_POINT('Ctrl Pts',(52.8424237249517,13.1993998929284,-59.9106732352752));
#186638=CARTESIAN_POINT('Ctrl Pts',(52.8356239352222,13.2771218944127,-59.8945524608647));
#186639=CARTESIAN_POINT('Ctrl Pts',(52.8288140636152,13.354959116562,-59.879274237381));
#186640=CARTESIAN_POINT('Ctrl Pts',(52.8084063492457,13.5882204595985,-59.8334887014819));
#186641=CARTESIAN_POINT('Ctrl Pts',(52.7879062369248,13.822537779029,-59.7953375078724));
#186642=CARTESIAN_POINT('Ctrl Pts',(52.7673307740641,14.0577163898014,-59.7635551171396));
#186643=CARTESIAN_POINT('Ctrl Pts',(52.7648947458015,14.0855603195582,-59.7597922466466));
#186644=CARTESIAN_POINT('Ctrl Pts',(52.7624575809797,14.1134172399927,-59.7561214184401));
#186645=CARTESIAN_POINT('Ctrl Pts',(52.7600192757781,14.1412871946384,-59.7525428773024));
#186646=CARTESIAN_POINT('Ctrl Pts',(52.7305287650649,14.4783652583484,-59.7092615826992));
#186647=CARTESIAN_POINT('Ctrl Pts',(52.7008776982777,14.8172785115573,-59.6793561042855));
#186648=CARTESIAN_POINT('Ctrl Pts',(52.6710582492637,15.1581163818755,-59.6634323280937));
#186649=CARTESIAN_POINT('Ctrl Pts',(52.6542978767187,15.3496883214269,-59.6544821821278));
#186650=CARTESIAN_POINT('Ctrl Pts',(52.6374843263043,15.5418680821543,-59.6499500007379));
#186651=CARTESIAN_POINT('Ctrl Pts',(52.6206164493001,15.7346687985482,-59.64995));
#186652=CARTESIAN_POINT('Origin',(53.3950245803324,12.61999998,-55.24995));
#186653=CARTESIAN_POINT('',(52.8969272312866,12.5764221086262,-55.74995));
#186654=CARTESIAN_POINT('Origin',(53.3950245803325,12.61999998,-55.74995));
#186655=CARTESIAN_POINT('',(52.8969272312866,12.5764221086262,-52.64995));
#186656=CARTESIAN_POINT('Ctrl Pts',(53.3950245803324,12.11999998,-55.74995));
#186657=CARTESIAN_POINT('Ctrl Pts',(52.9368589933237,12.11999998,-55.74995));
#186658=CARTESIAN_POINT('Ctrl Pts',(52.8969272312866,12.5764221086262,-55.74995));
#186659=CARTESIAN_POINT('Ctrl Pts',(53.3950245803365,12.11999998,-55.6530085475485));
#186660=CARTESIAN_POINT('Ctrl Pts',(52.9368589933258,12.1199999799653,-55.6451138110298));
#186661=CARTESIAN_POINT('Ctrl Pts',(52.8969272312908,12.5764221085778,-55.5560711921817));
#186662=CARTESIAN_POINT('Ctrl Pts',(53.4000464934415,12.0912996152796,-55.5568836545521));
#186663=CARTESIAN_POINT('Ctrl Pts',(52.9398152308639,12.0862100303001,-55.5412722521129));
#186664=CARTESIAN_POINT('Ctrl Pts',(52.9019494572905,12.5190178027248,-55.3638118539785));
#186665=CARTESIAN_POINT('Ctrl Pts',(53.4093468596023,12.0381477794255,-55.4758105868621));
#186666=CARTESIAN_POINT('Ctrl Pts',(52.9450883668941,12.0259378096709,-55.4571865884902));
#186667=CARTESIAN_POINT('Ctrl Pts',(52.9112495105564,12.4127177074772,-55.2016711737242));
#186668=CARTESIAN_POINT('',(52.9112495105564,12.4127177074773,-55.2016711737242));
#186669=CARTESIAN_POINT('Origin',(53.4093468596018,12.4562955788561,-55.2016711737319));
#186670=CARTESIAN_POINT('Origin',(52.9691152015747,11.7513098326049,-55.69773241533));
#186671=CARTESIAN_POINT('Origin',(53.7167487055517,-8.26789346682159,-59.64995));
#186672=CARTESIAN_POINT('',(51.3604079243413,30.1389181512134,-59.64995));
#186673=CARTESIAN_POINT('',(51.2652416360248,31.226673804131,-59.64995));
#186674=CARTESIAN_POINT('Origin',(50.3642132262496,30.0517624084658,-59.64995));
#186675=CARTESIAN_POINT('Origin',(51.9689593648599,28.91999998,-52.64995));
#186676=CARTESIAN_POINT('',(51.4708620158141,28.8764221086262,-55.74995));
#186677=CARTESIAN_POINT('',(51.4708620158141,28.8764221086262,-52.64995));
#186678=CARTESIAN_POINT('Origin',(51.9689593648599,28.91999998,-55.74995));
#186679=CARTESIAN_POINT('Ctrl Pts',(51.9689593648599,28.41999998,-55.74995));
#186680=CARTESIAN_POINT('Ctrl Pts',(51.5107937778512,28.41999998,-55.74995));
#186681=CARTESIAN_POINT('Ctrl Pts',(51.4708620158141,28.8764221086262,-55.74995));
#186682=CARTESIAN_POINT('Ctrl Pts',(51.9689593648654,28.41999998,-55.6186826543062));
#186683=CARTESIAN_POINT('Ctrl Pts',(51.5107937778567,28.4199999799462,-55.6078478088784));
#186684=CARTESIAN_POINT('Ctrl Pts',(51.4708620158198,28.8764221085606,-55.4874153086129));
#186685=CARTESIAN_POINT('Ctrl Pts',(51.9783882917162,28.3661134164373,-55.4889566552507));
#186686=CARTESIAN_POINT('Ctrl Pts',(51.5164047569777,28.3558661951151,-55.4680441063688));
#186687=CARTESIAN_POINT('Ctrl Pts',(51.4802909426703,28.7686489815003,-55.2279633105015));
#186688=CARTESIAN_POINT('Ctrl Pts',(52.0107801105432,28.1809933247493,-55.3038365635627));
#186689=CARTESIAN_POINT('Ctrl Pts',(51.5345366632341,28.1486175582537,-55.2822894538777));
#186690=CARTESIAN_POINT('Ctrl Pts',(51.5126827614974,28.3984087981251,-54.8577231271254));
#186691=CARTESIAN_POINT('Ctrl Pts',(52.033479219109,28.0512673256941,-55.24995));
#186692=CARTESIAN_POINT('Ctrl Pts',(51.5469301855916,28.0069589495408,-55.2386587236988));
#186693=CARTESIAN_POINT('Ctrl Pts',(51.5353818700614,28.1389568000129,-54.7499500000658));
#186694=CARTESIAN_POINT('Ctrl Pts',(52.0564480283858,27.91999998,-55.24995));
#186695=CARTESIAN_POINT('Ctrl Pts',(51.5583506793399,27.8764221086261,-55.24995));
#186696=CARTESIAN_POINT('Ctrl Pts',(51.55835067934,27.8764221086262,-54.74995));
#186697=CARTESIAN_POINT('',(51.55835067934,27.8764221086262,-54.74995));
#186698=CARTESIAN_POINT('Ctrl Pts',(51.55835067934,27.8764221086262,-54.74995));
#186699=CARTESIAN_POINT('Ctrl Pts',(51.5353818700614,28.1389568000129,-54.7499500000658));
#186700=CARTESIAN_POINT('Ctrl Pts',(51.5126827614974,28.3984087981251,-54.8577231271254));
#186701=CARTESIAN_POINT('Ctrl Pts',(51.4964868520838,28.5835288898127,-55.0428432188135));
#186702=CARTESIAN_POINT('Ctrl Pts',(51.4802909426703,28.7686489815003,-55.2279633105015));
#186703=CARTESIAN_POINT('Ctrl Pts',(51.4708620158198,28.8764221085606,-55.4874153086129));
#186704=CARTESIAN_POINT('Ctrl Pts',(51.4708620158141,28.8764221086262,-55.74995));
#186705=CARTESIAN_POINT('Origin',(52.0564480283858,27.91999998,-54.74995));
#186706=CARTESIAN_POINT('Origin',(51.7633389850707,31.2702516755049,-54.74995));
#186707=CARTESIAN_POINT('',(51.6020950111029,27.3764221086262,-54.74995));
#186708=CARTESIAN_POINT('',(51.2652416360248,31.226673804131,-54.74995));
#186709=CARTESIAN_POINT('Origin',(52.1001923601488,27.41999998,-54.74995));
#186710=CARTESIAN_POINT('Ctrl Pts',(52.1002185497626,27.4200238915827,-55.2499499996828));
#186711=CARTESIAN_POINT('Ctrl Pts',(51.6020931262756,27.3764436523005,-55.2499781675633));
#186712=CARTESIAN_POINT('Ctrl Pts',(51.6020912850816,27.3764646972444,-54.7499500009454));
#186713=CARTESIAN_POINT('Ctrl Pts',(52.1231889541655,27.288749433996,-55.2499434816096));
#186714=CARTESIAN_POINT('Ctrl Pts',(51.6138470691841,27.2420954701119,-55.2615949036223));
#186715=CARTESIAN_POINT('Ctrl Pts',(51.6250613655174,27.1139154764662,-54.7499383449291));
#186716=CARTESIAN_POINT('Ctrl Pts',(52.1458900110277,27.1590137328186,-55.3038301720452));
#186717=CARTESIAN_POINT('Ctrl Pts',(51.6242350673701,27.1233601075035,-55.327473556918));
#186718=CARTESIAN_POINT('Ctrl Pts',(51.6477620531743,26.8544454292379,-54.8577131170148));
#186719=CARTESIAN_POINT('Ctrl Pts',(52.1782841123997,26.9738822391066,-55.4889602509496));
#186720=CARTESIAN_POINT('Ctrl Pts',(51.6383741166919,26.9617500342493,-55.5134049012208));
#186721=CARTESIAN_POINT('Ctrl Pts',(51.6801556235438,26.4841852256414,-55.2279733206121));
#186722=CARTESIAN_POINT('Ctrl Pts',(52.1877133516444,26.9199941513771,-55.618695932326));
#186723=CARTESIAN_POINT('Ctrl Pts',(51.6420241800604,26.920029619041,-55.631800368908));
#186724=CARTESIAN_POINT('Ctrl Pts',(51.6895846943154,26.376410453555,-55.4874433678397));
#186725=CARTESIAN_POINT('Ctrl Pts',(52.1877123348205,26.9199999794923,-55.7499712944312));
#186726=CARTESIAN_POINT('Ctrl Pts',(51.6420237834999,26.9200341517443,-55.7499691665899));
#186727=CARTESIAN_POINT('Ctrl Pts',(51.6895836745461,26.3764221095716,-55.7499925886182));
#186728=CARTESIAN_POINT('',(51.6895836746288,26.3764221086262,-55.74995));
#186729=CARTESIAN_POINT('Ctrl Pts',(51.6895836746288,26.3764221086262,-55.74995));
#186730=CARTESIAN_POINT('Ctrl Pts',(51.6895836746231,26.3764221086917,-55.4874153086129));
#186731=CARTESIAN_POINT('Ctrl Pts',(51.6801547477726,26.484195235752,-55.2279633105015));
#186732=CARTESIAN_POINT('Ctrl Pts',(51.6639588383591,26.6693153274396,-55.0428432188135));
#186733=CARTESIAN_POINT('Ctrl Pts',(51.6477629289455,26.8544354191273,-54.8577231271254));
#186734=CARTESIAN_POINT('Ctrl Pts',(51.6250638203816,27.1138874172394,-54.7499500000658));
#186735=CARTESIAN_POINT('Ctrl Pts',(51.6020950111029,27.3764221086262,-54.74995));
#186736=CARTESIAN_POINT('Origin',(52.1876810236747,26.41999998,-55.74995));
#186737=CARTESIAN_POINT('Origin',(52.1876810236747,26.41999998,-52.64995));
#186738=CARTESIAN_POINT('',(51.6895836746288,26.3764221086262,-52.64995));
#186739=CARTESIAN_POINT('Origin',(53.7167487055517,-8.26789346682159,-59.64995));
#186740=CARTESIAN_POINT('',(51.2652416360248,31.226673804131,-59.64995));
#186741=CARTESIAN_POINT('Origin',(47.0226009489055,34.0551009288773,-59.64995));
#186742=CARTESIAN_POINT('',(50.4931441736257,31.9987712665301,-59.64995));
#186743=CARTESIAN_POINT('Origin',(49.7860373924392,31.2916644853435,-59.64995));
#186744=CARTESIAN_POINT('',(44.9662712865584,37.5256441535974,-59.64995));
#186745=CARTESIAN_POINT('Origin',(44.2591645053719,36.8185373724109,-59.64995));
#186746=CARTESIAN_POINT('',(44.1941738241593,38.2977416159964,-59.64995));
#186747=CARTESIAN_POINT('Origin',(37.,39.4290601878171,-92.34995));
#186748=CARTESIAN_POINT('',(36.9564221286262,38.9309628387712,-55.74995));
#186749=CARTESIAN_POINT('Origin',(37.,39.4290601878171,-55.74995));
#186750=CARTESIAN_POINT('',(36.9564221286262,38.9309628387712,-52.64995));
#186751=CARTESIAN_POINT('Ctrl Pts',(37.5,39.4290601878171,-55.74995));
#186752=CARTESIAN_POINT('Ctrl Pts',(37.5000000000001,38.8834059372824,-55.74995));
#186753=CARTESIAN_POINT('Ctrl Pts',(36.9564221286262,38.9309628387712,-55.74995));
#186754=CARTESIAN_POINT('Ctrl Pts',(37.5,39.4290601878116,-55.6186826543065));
#186755=CARTESIAN_POINT('Ctrl Pts',(37.5000000000036,38.8834059372834,-55.6317784220504));
#186756=CARTESIAN_POINT('Ctrl Pts',(36.9564221286917,38.9309628387654,-55.487415308613));
#186757=CARTESIAN_POINT('Ctrl Pts',(37.5538865635632,39.4196312609607,-55.4889566552503));
#186758=CARTESIAN_POINT('Ctrl Pts',(37.5417246342956,38.879755504792,-55.5133819370962));
#186759=CARTESIAN_POINT('Ctrl Pts',(37.0641952557516,38.9215339119149,-55.2279633105015));
#186760=CARTESIAN_POINT('Ctrl Pts',(37.7390066552503,39.3872394421337,-55.3038365635632));
#186761=CARTESIAN_POINT('Ctrl Pts',(37.7033393021412,38.8656160534955,-55.3274496218441));
#186762=CARTESIAN_POINT('Ctrl Pts',(37.4344354391277,38.8891420930878,-54.8577231271255));
#186763=CARTESIAN_POINT('Ctrl Pts',(37.8687326543062,39.3645403335679,-55.24995));
#186764=CARTESIAN_POINT('Ctrl Pts',(37.8220750118298,38.855228024944,-55.2615708605686));
#186765=CARTESIAN_POINT('Ctrl Pts',(37.6938874372391,38.8664429845239,-54.7499500000658));
#186766=CARTESIAN_POINT('Ctrl Pts',(38.,39.3415715242911,-55.24995));
#186767=CARTESIAN_POINT('Ctrl Pts',(37.9564221286261,38.8434741752452,-55.2499499999999));
#186768=CARTESIAN_POINT('Ctrl Pts',(37.9564221286262,38.8434741752452,-54.74995));
#186769=CARTESIAN_POINT('',(37.9564221286262,38.8434741752452,-54.74995));
#186770=CARTESIAN_POINT('Origin',(38.,39.3415715242911,-54.74995));
#186771=CARTESIAN_POINT('Ctrl Pts',(37.9564221286262,38.8434741752452,-54.74995));
#186772=CARTESIAN_POINT('Ctrl Pts',(37.6938874372391,38.8664429845239,-54.7499500000658));
#186773=CARTESIAN_POINT('Ctrl Pts',(37.4344354391277,38.8891420930878,-54.8577231271255));
#186774=CARTESIAN_POINT('Ctrl Pts',(37.2493153474397,38.9053380025014,-55.0428432188135));
#186775=CARTESIAN_POINT('Ctrl Pts',(37.0641952557516,38.9215339119149,-55.2279633105015));
#186776=CARTESIAN_POINT('Ctrl Pts',(36.9564221286917,38.9309628387654,-55.487415308613));
#186777=CARTESIAN_POINT('Ctrl Pts',(36.9564221286262,38.9309628387712,-55.74995));
#186778=CARTESIAN_POINT('Origin',(3.70444879364117,42.3420434642203,-54.74995));
#186779=CARTESIAN_POINT('',(38.4564221286262,38.7997298434823,-54.74995));
#186780=CARTESIAN_POINT('Origin',(38.5,39.2978271925282,-54.74995));
#186781=CARTESIAN_POINT('',(38.,38.8396616055195,-54.74995));
#186782=CARTESIAN_POINT('Ctrl Pts',(38.5,39.2978271925282,-55.24995));
#186783=CARTESIAN_POINT('Ctrl Pts',(38.4564221286261,38.7997298434823,-55.2499499999999));
#186784=CARTESIAN_POINT('Ctrl Pts',(38.4564221286262,38.7997298434823,-54.74995));
#186785=CARTESIAN_POINT('Ctrl Pts',(38.6312673456941,39.2748583832512,-55.24995));
#186786=CARTESIAN_POINT('Ctrl Pts',(38.5869589695399,38.788309349734,-55.2386587236917));
#186787=CARTESIAN_POINT('Ctrl Pts',(38.7189568200132,38.7767610342036,-54.7499500000658));
#186788=CARTESIAN_POINT('Ctrl Pts',(38.7609933447493,39.2521592746855,-55.3038365635627));
#186789=CARTESIAN_POINT('Ctrl Pts',(38.7286175782541,38.7759158273764,-55.2822894538767));
#186790=CARTESIAN_POINT('Ctrl Pts',(38.9784088181247,38.7540619256397,-54.8577231271255));
#186791=CARTESIAN_POINT('Ctrl Pts',(38.9461134364373,39.2197674558585,-55.4889566552507));
#186792=CARTESIAN_POINT('Ctrl Pts',(38.9358662151147,38.7577839211201,-55.4680441063697));
#186793=CARTESIAN_POINT('Ctrl Pts',(39.3486490015007,38.7216701068126,-55.2279633105015));
#186794=CARTESIAN_POINT('Ctrl Pts',(39.,39.2103385290077,-55.6186826543063));
#186795=CARTESIAN_POINT('Ctrl Pts',(38.9999999999489,38.7521729419962,-55.6078478088777));
#186796=CARTESIAN_POINT('Ctrl Pts',(39.4564221285606,38.7122411799621,-55.487415308613));
#186797=CARTESIAN_POINT('Ctrl Pts',(39.,39.2103385290022,-55.74995));
#186798=CARTESIAN_POINT('Ctrl Pts',(39.,38.7521729419935,-55.74995));
#186799=CARTESIAN_POINT('Ctrl Pts',(39.4564221286262,38.7122411799564,-55.74995));
#186800=CARTESIAN_POINT('',(39.4564221286262,38.7122411799564,-55.74995));
#186801=CARTESIAN_POINT('Origin',(39.5,39.2103385290022,-55.74995));
#186802=CARTESIAN_POINT('Ctrl Pts',(39.4564221286262,38.7122411799564,-55.74995));
#186803=CARTESIAN_POINT('Ctrl Pts',(39.4564221285606,38.7122411799621,-55.487415308613));
#186804=CARTESIAN_POINT('Ctrl Pts',(39.3486490015007,38.7216701068126,-55.2279633105015));
#186805=CARTESIAN_POINT('Ctrl Pts',(39.1635289098127,38.7378660162261,-55.0428432188135));
#186806=CARTESIAN_POINT('Ctrl Pts',(38.9784088181247,38.7540619256397,-54.8577231271255));
#186807=CARTESIAN_POINT('Ctrl Pts',(38.7189568200132,38.7767610342036,-54.7499500000658));
#186808=CARTESIAN_POINT('Ctrl Pts',(38.4564221286262,38.7997298434823,-54.74995));
#186809=CARTESIAN_POINT('Origin',(39.5,39.2103385290023,-129.34995));
#186810=CARTESIAN_POINT('',(39.4564221286262,38.7122411799564,-55.74995));
#186811=CARTESIAN_POINT('Origin',(4.69960655320655,40.7492486855235,-59.64995));
#186812=CARTESIAN_POINT('',(43.1064181712417,38.392907904313,-59.64995));
#186813=CARTESIAN_POINT('',(24.5275331667447,40.0183497231583,-59.64995));
#186814=CARTESIAN_POINT('Origin',(43.019262428494,37.3967132062212,-59.64995));
#186815=CARTESIAN_POINT('Ctrl Pts',(25.3802177275058,39.9437494905281,-60.1097730249189));
#186816=CARTESIAN_POINT('Ctrl Pts',(25.5227862062494,39.9312763648619,-60.5923862926587));
#186817=CARTESIAN_POINT('Ctrl Pts',(25.572468850428,39.5210489290882,-60.8798615124595));
#186818=CARTESIAN_POINT('Ctrl Pts',(25.9036128690389,39.8979583490994,-59.9539737371434));
#186819=CARTESIAN_POINT('Ctrl Pts',(26.0512576071349,39.8850411082851,-60.5102318318317));
#186820=CARTESIAN_POINT('Ctrl Pts',(26.059719336348,39.3883003271754,-60.8019346414671));
#186821=CARTESIAN_POINT('Ctrl Pts',(26.4338688782163,39.8515669595299,-59.8461489023585));
#186822=CARTESIAN_POINT('Ctrl Pts',(26.5712796028832,39.8395450788764,-60.4792397999495));
#186823=CARTESIAN_POINT('Ctrl Pts',(26.5494003841727,39.2520983829515,-60.748049450926));
#186824=CARTESIAN_POINT('Ctrl Pts',(27.5031785292772,39.7580144872632,-59.6965141185183));
#186825=CARTESIAN_POINT('Ctrl Pts',(27.601298997848,39.7494300586015,-60.4901498725136));
#186826=CARTESIAN_POINT('Ctrl Pts',(27.529498834359,38.9740545371747,-60.6732320595124));
#186827=CARTESIAN_POINT('Ctrl Pts',(28.0425516254864,39.710825455934,-59.6557090289434));
#186828=CARTESIAN_POINT('Ctrl Pts',(28.1179039179461,39.7042329845701,-60.5392590138154));
#186829=CARTESIAN_POINT('Ctrl Pts',(28.0200529940657,38.8321810243987,-60.6528294999755));
#186830=CARTESIAN_POINT('Ctrl Pts',(28.5867228014573,39.663216647019,-59.6505032458185));
#186831=CARTESIAN_POINT('Ctrl Pts',(28.5960141520618,39.6624037591722,-60.6291816703115));
#186832=CARTESIAN_POINT('Ctrl Pts',(28.5109323535812,38.6876131939284,-60.6502266229092));
#186833=CARTESIAN_POINT('',(25.3802177275058,39.9437494905281,-60.1097730249189));
#186834=CARTESIAN_POINT('Ctrl Pts',(28.4564221286157,39.6746164786217,-59.6524466674074));
#186835=CARTESIAN_POINT('Ctrl Pts',(28.1317998821407,39.7030172440177,-59.6590182799319));
#186836=CARTESIAN_POINT('Ctrl Pts',(27.8089020756387,39.7312671410707,-59.6781506934664));
#186837=CARTESIAN_POINT('Ctrl Pts',(27.4876982951917,39.7593688309396,-59.7096215394412));
#186838=CARTESIAN_POINT('Ctrl Pts',(27.3141484358393,39.7745524764045,-59.7266255762088));
#186839=CARTESIAN_POINT('Ctrl Pts',(27.1410937670796,39.7896927982219,-59.7472310046323));
#186840=CARTESIAN_POINT('Ctrl Pts',(26.9685328542776,39.8047899206072,-59.7713974032318));
#186841=CARTESIAN_POINT('Ctrl Pts',(26.9471826335434,39.8066578227303,-59.7743874079558));
#186842=CARTESIAN_POINT('Ctrl Pts',(26.9258394639526,39.8085251079323,-59.7774303163423));
#186843=CARTESIAN_POINT('Ctrl Pts',(26.904503506364,39.8103917621319,-59.7805271013239));
#186844=CARTESIAN_POINT('Ctrl Pts',(26.5372951385086,39.8425183277728,-59.8338251712117));
#186845=CARTESIAN_POINT('Ctrl Pts',(26.172250803663,39.874455574155,-59.9028698737259));
#186846=CARTESIAN_POINT('Ctrl Pts',(25.8100560257878,39.9061435120092,-59.9926952104099));
#186847=CARTESIAN_POINT('Ctrl Pts',(25.6663124460363,39.9187194460103,-60.0283440276653));
#186848=CARTESIAN_POINT('Ctrl Pts',(25.5230181721596,39.9312560704744,-60.0672655467143));
#186849=CARTESIAN_POINT('Ctrl Pts',(25.3802177275058,39.9437494905281,-60.1097730249189));
#186850=CARTESIAN_POINT('Origin',(25.2930619847582,38.9475547924363,-60.1097730249189));
#186851=CARTESIAN_POINT('Origin',(28.5,40.1727138277873,-52.64995));
#186852=CARTESIAN_POINT('',(28.4564221286262,39.6746164787415,-55.74995));
#186853=CARTESIAN_POINT('Origin',(28.5,40.1727138277873,-55.74995));
#186854=CARTESIAN_POINT('',(28.4564221286262,39.6746164787415,-52.64995));
#186855=CARTESIAN_POINT('Ctrl Pts',(29.,40.1727138277873,-55.74995));
#186856=CARTESIAN_POINT('Ctrl Pts',(29.,39.6270595772528,-55.74995));
#186857=CARTESIAN_POINT('Ctrl Pts',(28.4564221286262,39.6746164787415,-55.74995));
#186858=CARTESIAN_POINT('Ctrl Pts',(29.,40.1727138277819,-55.6186826543062));
#186859=CARTESIAN_POINT('Ctrl Pts',(29.0000000000046,39.6270595772536,-55.6317784220498));
#186860=CARTESIAN_POINT('Ctrl Pts',(28.4564221286917,39.6746164787358,-55.487415308613));
#186861=CARTESIAN_POINT('Ctrl Pts',(29.0538865635627,40.163284900931,-55.4889566552507));
#186862=CARTESIAN_POINT('Ctrl Pts',(29.0417246342951,39.6234091447624,-55.5133819370971));
#186863=CARTESIAN_POINT('Ctrl Pts',(28.5641952557521,39.6651875518853,-55.2279633105015));
#186864=CARTESIAN_POINT('Ctrl Pts',(29.2390066552507,40.1308930821041,-55.3038365635627));
#186865=CARTESIAN_POINT('Ctrl Pts',(29.2033393021417,39.6092696934658,-55.3274496218431));
#186866=CARTESIAN_POINT('Ctrl Pts',(28.9344354391272,39.6327957330582,-54.8577231271255));
#186867=CARTESIAN_POINT('Ctrl Pts',(29.368732654306,40.1081939735386,-55.24995));
#186868=CARTESIAN_POINT('Ctrl Pts',(29.3220750118295,39.5988816649146,-55.2615708605689));
#186869=CARTESIAN_POINT('Ctrl Pts',(29.1938874372395,39.6100966244942,-54.7499500000658));
#186870=CARTESIAN_POINT('Ctrl Pts',(29.5,40.0852251642615,-55.24995));
#186871=CARTESIAN_POINT('Ctrl Pts',(29.4564221286262,39.5871278152156,-55.24995));
#186872=CARTESIAN_POINT('Ctrl Pts',(29.4564221286262,39.5871278152156,-54.74995));
#186873=CARTESIAN_POINT('',(29.4564221286262,39.5871278152156,-54.74995));
#186874=CARTESIAN_POINT('Ctrl Pts',(29.4564221286262,39.5871278152156,-54.74995));
#186875=CARTESIAN_POINT('Ctrl Pts',(29.1938874372394,39.6100966244942,-54.7499500000658));
#186876=CARTESIAN_POINT('Ctrl Pts',(28.9344354391271,39.6327957330582,-54.8577231271255));
#186877=CARTESIAN_POINT('Ctrl Pts',(28.7493153474396,39.6489916424717,-55.0428432188135));
#186878=CARTESIAN_POINT('Ctrl Pts',(28.5641952557521,39.6651875518853,-55.2279633105015));
#186879=CARTESIAN_POINT('Ctrl Pts',(28.4564221286917,39.6746164787358,-55.487415308613));
#186880=CARTESIAN_POINT('Ctrl Pts',(28.4564221286262,39.6746164787415,-55.74995));
#186881=CARTESIAN_POINT('Origin',(29.5,40.0852251642615,-54.74995));
#186882=CARTESIAN_POINT('Origin',(3.70444879364117,42.3420434642203,-54.74995));
#186883=CARTESIAN_POINT('',(29.9564221286262,39.5433834834526,-54.74995));
#186884=CARTESIAN_POINT('',(29.5,39.5833152454898,-54.74995));
#186885=CARTESIAN_POINT('Origin',(30.,40.0414808324985,-54.74995));
#186886=CARTESIAN_POINT('Ctrl Pts',(30.,40.0414808324985,-55.24995));
#186887=CARTESIAN_POINT('Ctrl Pts',(29.9564221286262,39.5433834834526,-55.24995));
#186888=CARTESIAN_POINT('Ctrl Pts',(29.9564221286262,39.5433834834526,-54.74995));
#186889=CARTESIAN_POINT('Ctrl Pts',(30.131267345694,40.0185120232214,-55.24995));
#186890=CARTESIAN_POINT('Ctrl Pts',(30.0869589695403,39.5319629897042,-55.2386587236916));
#186891=CARTESIAN_POINT('Ctrl Pts',(30.218956820013,39.520414674174,-54.7499500000658));
#186892=CARTESIAN_POINT('Ctrl Pts',(30.2609933447492,39.9958129146559,-55.3038365635627));
#186893=CARTESIAN_POINT('Ctrl Pts',(30.2286175782536,39.5195694673468,-55.2822894538777));
#186894=CARTESIAN_POINT('Ctrl Pts',(30.4784088181251,39.4977155656101,-54.8577231271254));
#186895=CARTESIAN_POINT('Ctrl Pts',(30.4461134364373,39.9634210958289,-55.4889566552508));
#186896=CARTESIAN_POINT('Ctrl Pts',(30.4358662151152,39.5014375610904,-55.4680441063689));
#186897=CARTESIAN_POINT('Ctrl Pts',(30.8486490015003,39.4653237467829,-55.2279633105015));
#186898=CARTESIAN_POINT('Ctrl Pts',(30.5,39.9539921689781,-55.6186826543063));
#186899=CARTESIAN_POINT('Ctrl Pts',(30.4999999999484,39.4958265819666,-55.6078478088783));
#186900=CARTESIAN_POINT('Ctrl Pts',(30.9564221285606,39.4558948199325,-55.4874153086129));
#186901=CARTESIAN_POINT('Ctrl Pts',(30.5,39.9539921689726,-55.74995));
#186902=CARTESIAN_POINT('Ctrl Pts',(30.5,39.4958265819639,-55.74995));
#186903=CARTESIAN_POINT('Ctrl Pts',(30.9564221286262,39.4558948199267,-55.74995));
#186904=CARTESIAN_POINT('',(30.9564221286262,39.4558948199267,-55.74995));
#186905=CARTESIAN_POINT('Ctrl Pts',(30.9564221286262,39.4558948199267,-55.74995));
#186906=CARTESIAN_POINT('Ctrl Pts',(30.9564221285606,39.4558948199325,-55.4874153086129));
#186907=CARTESIAN_POINT('Ctrl Pts',(30.8486490015003,39.4653237467829,-55.2279633105015));
#186908=CARTESIAN_POINT('Ctrl Pts',(30.6635289098127,39.4815196561965,-55.0428432188135));
#186909=CARTESIAN_POINT('Ctrl Pts',(30.4784088181251,39.4977155656101,-54.8577231271254));
#186910=CARTESIAN_POINT('Ctrl Pts',(30.218956820013,39.520414674174,-54.7499500000658));
#186911=CARTESIAN_POINT('Ctrl Pts',(29.9564221286262,39.5433834834526,-54.74995));
#186912=CARTESIAN_POINT('Origin',(31.,39.9539921689726,-55.74995));
#186913=CARTESIAN_POINT('Origin',(31.,39.9539921689726,-52.64995));
#186914=CARTESIAN_POINT('',(30.9564221286262,39.4558948199267,-52.64995));
#186915=CARTESIAN_POINT('Origin',(4.69960655320655,40.7492486855235,-59.64995));
#186916=CARTESIAN_POINT('',(24.5275331667447,40.0183497231583,-59.64995));
#186917=CARTESIAN_POINT('Ctrl Pts',(25.572468850428,39.5210489290882,-60.8798615124595));
#186918=CARTESIAN_POINT('Ctrl Pts',(25.5227862062494,39.9312763648619,-60.5923862926587));
#186919=CARTESIAN_POINT('Ctrl Pts',(25.3802177275058,39.943749490528,-60.1097730249189));
#186920=CARTESIAN_POINT('Ctrl Pts',(25.2694477113958,39.6036052974814,-60.9283242463865));
#186921=CARTESIAN_POINT('Ctrl Pts',(25.2414738675095,39.9482243711148,-60.6373384822398));
#186922=CARTESIAN_POINT('Ctrl Pts',(25.1089972874034,39.9674782043536,-60.2066542280814));
#186923=CARTESIAN_POINT('Ctrl Pts',(24.9650212889786,39.6997861053784,-60.9766079791613));
#186924=CARTESIAN_POINT('Ctrl Pts',(24.9493186357974,39.9900159541718,-60.6937268873635));
#186925=CARTESIAN_POINT('Ctrl Pts',(24.8422602775208,40.0127575956439,-60.3032659617329));
#186926=CARTESIAN_POINT('Ctrl Pts',(24.3438778196125,39.9224728282123,-61.0507205920708));
#186927=CARTESIAN_POINT('Ctrl Pts',(24.3665512677474,40.1299777240875,-60.7838744940585));
#186928=CARTESIAN_POINT('Ctrl Pts',(24.3096510677746,40.1491089179394,-60.4514911807313));
#186929=CARTESIAN_POINT('Ctrl Pts',(24.0238031468177,40.0506166841414,-61.0754935252291));
#186930=CARTESIAN_POINT('Ctrl Pts',(24.0669512606426,40.2300655352922,-60.8169267274199));
#186931=CARTESIAN_POINT('Ctrl Pts',(24.0409609718932,40.24165543605,-60.5010370503254));
#186932=CARTESIAN_POINT('Ctrl Pts',(23.7057274034393,40.1924568448808,-61.0754935261973));
#186933=CARTESIAN_POINT('Ctrl Pts',(23.7796330855957,40.3581899105084,-60.8169267287601));
#186934=CARTESIAN_POINT('Ctrl Pts',(23.7796330855957,40.3581899105085,-60.5010370523946));
#186935=CARTESIAN_POINT('',(23.7796330855957,40.3581899105085,-60.5010370523947));
#186936=CARTESIAN_POINT('Origin',(23.372360414466,39.4448832964128,-60.5010370523947));
#186937=CARTESIAN_POINT('Ctrl Pts',(25.3802177275058,39.943749490528,-60.1097730249189));
#186938=CARTESIAN_POINT('Ctrl Pts',(25.3377363135767,39.9474661326574,-60.1249475836356));
#186939=CARTESIAN_POINT('Ctrl Pts',(25.2979927848269,39.9514798686665,-60.1391717405498));
#186940=CARTESIAN_POINT('Ctrl Pts',(25.2609589409308,39.9556072078286,-60.1523839922766));
#186941=CARTESIAN_POINT('Ctrl Pts',(25.2220309924076,39.9599456407197,-60.166271987715));
#186942=CARTESIAN_POINT('Ctrl Pts',(25.1860970996603,39.9644092678141,-60.1790428287426));
#186943=CARTESIAN_POINT('Ctrl Pts',(25.1531400482302,39.9688089768955,-60.1906788704549));
#186944=CARTESIAN_POINT('Ctrl Pts',(25.1171272460509,39.9736166233906,-60.2033937964009));
#186945=CARTESIAN_POINT('Ctrl Pts',(25.0846688996706,39.9783471985322,-60.214754833184));
#186946=CARTESIAN_POINT('Ctrl Pts',(25.0557488187266,39.9827921994797,-60.2247897604492));
#186947=CARTESIAN_POINT('Ctrl Pts',(25.0404115499051,39.9851495294808,-60.230111611981));
#186948=CARTESIAN_POINT('Ctrl Pts',(25.0260697403982,39.9874272035645,-60.2350611282861));
#186949=CARTESIAN_POINT('Ctrl Pts',(25.0127218112758,39.9895989300769,-60.2396456694191));
#186950=CARTESIAN_POINT('Ctrl Pts',(25.0067601800825,39.9905688957099,-60.2416932786905));
#186951=CARTESIAN_POINT('Ctrl Pts',(25.0009985443053,39.9915174894833,-60.2436742905531));
#186952=CARTESIAN_POINT('Ctrl Pts',(24.9954346520016,39.9924429351662,-60.2455817846297));
#186953=CARTESIAN_POINT('Ctrl Pts',(24.9926527058498,39.9929056580077,-60.246535531668));
#186954=CARTESIAN_POINT('Ctrl Pts',(24.9899201612054,39.9933626023715,-60.2474707707647));
#186955=CARTESIAN_POINT('Ctrl Pts',(24.9872369808442,39.9938135212305,-60.2483875019273));
#186956=CARTESIAN_POINT('Ctrl Pts',(24.9845538004829,39.9942644400894,-60.2493042330899));
#186957=CARTESIAN_POINT('Ctrl Pts',(24.9839661492007,39.9943620659877,-60.2495059770713));
#186958=CARTESIAN_POINT('Ctrl Pts',(24.9793354964283,39.9951479630991,-60.2510821716195));
#186959=CARTESIAN_POINT('Ctrl Pts',(24.9279712430605,40.003865312539,-60.2685656799095));
#186960=CARTESIAN_POINT('Ctrl Pts',(24.8784655257637,40.0130996371524,-60.2850161933571));
#186961=CARTESIAN_POINT('Ctrl Pts',(24.8308013791055,40.0226898926197,-60.3003979240438));
#186962=CARTESIAN_POINT('Ctrl Pts',(24.8097123058818,40.0269331155444,-60.3072035938712));
#186963=CARTESIAN_POINT('Ctrl Pts',(24.788983882997,40.031246087386,-60.3138007330426));
#186964=CARTESIAN_POINT('Ctrl Pts',(24.7686152583926,40.0356152269098,-60.3201893531102));
#186965=CARTESIAN_POINT('Ctrl Pts',(24.7200988895179,40.0460221536866,-60.3354065144951));
#186966=CARTESIAN_POINT('Ctrl Pts',(24.6736205664744,40.0567475976147,-60.3494274338396));
#186967=CARTESIAN_POINT('Ctrl Pts',(24.6291674207005,40.067616735454,-60.3622788776091));
#186968=CARTESIAN_POINT('Ctrl Pts',(24.6203828382536,40.0697646337818,-60.3648185081659));
#186969=CARTESIAN_POINT('Ctrl Pts',(24.6116773469398,40.071918181481,-60.3673126301496));
#186970=CARTESIAN_POINT('Ctrl Pts',(24.6030508521459,40.0740760877997,-60.3697616771469));
#186971=CARTESIAN_POINT('Ctrl Pts',(24.597473538032,40.0754712455845,-60.3713450670069));
#186972=CARTESIAN_POINT('Ctrl Pts',(24.5930293483899,40.0765902002605,-60.3725999802461));
#186973=CARTESIAN_POINT('Ctrl Pts',(24.5872536899646,40.0780546948281,-60.3742211678561));
#186974=CARTESIAN_POINT('Ctrl Pts',(24.5852952247151,40.0785512895898,-60.3747708955864));
#186975=CARTESIAN_POINT('Ctrl Pts',(24.5831836712054,40.0790878901403,-60.3753624736458));
#186976=CARTESIAN_POINT('Ctrl Pts',(24.5808229576604,40.0796897628148,-60.376021988692));
#186977=CARTESIAN_POINT('Ctrl Pts',(24.5791995774519,40.0801036496203,-60.3764755141421));
#186978=CARTESIAN_POINT('Ctrl Pts',(24.5775771985916,40.0805181359584,-60.3769279325757));
#186979=CARTESIAN_POINT('Ctrl Pts',(24.5759558187269,40.0809332193942,-60.377379242392));
#186980=CARTESIAN_POINT('Ctrl Pts',(24.5180765447908,40.095750677295,-60.3934898929903));
#186981=CARTESIAN_POINT('Ctrl Pts',(24.4613393330448,40.1113972696723,-60.4080863642803));
#186982=CARTESIAN_POINT('Ctrl Pts',(24.405783193626,40.1277441546784,-60.4211041690535));
#186983=CARTESIAN_POINT('Ctrl Pts',(24.3457160996731,40.1454183467258,-60.4351789717766));
#186984=CARTESIAN_POINT('Ctrl Pts',(24.2870296504741,40.1639110071772,-60.4474085751543));
#186985=CARTESIAN_POINT('Ctrl Pts',(24.2297431097138,40.1830806284349,-60.4577626719886));
#186986=CARTESIAN_POINT('Ctrl Pts',(24.1695508319587,40.2032225876436,-60.4686419581922));
#186987=CARTESIAN_POINT('Ctrl Pts',(24.1109038743736,40.2241118573122,-60.4774512669829));
#186988=CARTESIAN_POINT('Ctrl Pts',(24.0537946101968,40.24560866413,-60.4842026045568));
#186989=CARTESIAN_POINT('Ctrl Pts',(23.9916402035452,40.2690045402969,-60.4915503683052));
#186990=CARTESIAN_POINT('Ctrl Pts',(23.9313070653885,40.2931197928505,-60.4964610838971));
#186991=CARTESIAN_POINT('Ctrl Pts',(23.8727530525808,40.317805125582,-60.4989952734271));
#186992=CARTESIAN_POINT('Ctrl Pts',(23.8412002274789,40.3311072367254,-60.5003608645315));
#186993=CARTESIAN_POINT('Ctrl Pts',(23.8101634964631,40.3445754224573,-60.5010370523947));
#186994=CARTESIAN_POINT('Ctrl Pts',(23.7796330855957,40.3581899105085,-60.5010370523947));
#186995=CARTESIAN_POINT('Origin',(47.0226009489055,-59.9901009689335,-59.64995));
#186996=CARTESIAN_POINT('',(44.9662712865582,-63.4606441936539,-59.64995));
#186997=CARTESIAN_POINT('Origin',(44.2591645053717,-62.7535374124673,-59.64995));
#186998=CARTESIAN_POINT('',(50.4931441736259,-57.9337713065862,-59.64995));
#186999=CARTESIAN_POINT('Origin',(49.7860373924393,-57.2266645253997,-59.64995));
#187000=CARTESIAN_POINT('',(51.265241636025,-57.1616738441871,-59.64995));
#187001=CARTESIAN_POINT('Origin',(33.85,-65.63964951798,-52.64995));
#187002=CARTESIAN_POINT('',(33.8064221286261,-65.1415521689341,-55.74995));
#187003=CARTESIAN_POINT('',(33.8064221286261,-65.1415521689341,-52.64995));
#187004=CARTESIAN_POINT('Origin',(33.85,-65.63964951798,-55.74995));
#187005=CARTESIAN_POINT('Ctrl Pts',(33.35,-65.63964951798,-55.74995));
#187006=CARTESIAN_POINT('Ctrl Pts',(33.3499999999999,-65.1814839309712,
-55.74995));
#187007=CARTESIAN_POINT('Ctrl Pts',(33.8064221286261,-65.1415521689341,
-55.74995));
#187008=CARTESIAN_POINT('Ctrl Pts',(33.35,-65.6396495179854,-55.6186826543062));
#187009=CARTESIAN_POINT('Ctrl Pts',(33.3499999999488,-65.1814839309712,
-55.607847808877));
#187010=CARTESIAN_POINT('Ctrl Pts',(33.8064221285606,-65.1415521689398,
-55.487415308613));
#187011=CARTESIAN_POINT('Ctrl Pts',(33.2961134364373,-65.6490784448363,
-55.4889566552507));
#187012=CARTESIAN_POINT('Ctrl Pts',(33.2858662151155,-65.1870949100978,
-55.4680441063706));
#187013=CARTESIAN_POINT('Ctrl Pts',(33.6986490015007,-65.1509810957903,
-55.2279633105015));
#187014=CARTESIAN_POINT('Ctrl Pts',(33.1109933447493,-65.6814702636632,
-55.3038365635628));
#187015=CARTESIAN_POINT('Ctrl Pts',(33.0786175782532,-65.2052268163542,
-55.2822894538758));
#187016=CARTESIAN_POINT('Ctrl Pts',(33.3284088181247,-65.1833729146174,
-54.8577231271255));
#187017=CARTESIAN_POINT('Ctrl Pts',(32.981267345694,-65.704169372229,-55.24995));
#187018=CARTESIAN_POINT('Ctrl Pts',(32.9369589695398,-65.2176203387053,
-55.2386587236917));
#187019=CARTESIAN_POINT('Ctrl Pts',(33.0689568200132,-65.2060720231813,
-54.7499500000659));
#187020=CARTESIAN_POINT('Ctrl Pts',(32.85,-65.7271381815059,-55.24995));
#187021=CARTESIAN_POINT('Ctrl Pts',(32.8064221286261,-65.22904083246,-55.24995));
#187022=CARTESIAN_POINT('Ctrl Pts',(32.8064221286262,-65.22904083246,-54.74995));
#187023=CARTESIAN_POINT('',(32.8064221286262,-65.22904083246,-54.74995));
#187024=CARTESIAN_POINT('Origin',(32.85,-65.7271381815059,-54.74995));
#187025=CARTESIAN_POINT('Ctrl Pts',(32.8064221286262,-65.22904083246,-54.74995));
#187026=CARTESIAN_POINT('Ctrl Pts',(33.0689568200132,-65.2060720231813,
-54.7499500000659));
#187027=CARTESIAN_POINT('Ctrl Pts',(33.3284088181247,-65.1833729146174,
-54.8577231271255));
#187028=CARTESIAN_POINT('Ctrl Pts',(33.5135289098127,-65.1671770052039,
-55.0428432188135));
#187029=CARTESIAN_POINT('Ctrl Pts',(33.6986490015007,-65.1509810957903,
-55.2279633105015));
#187030=CARTESIAN_POINT('Ctrl Pts',(33.8064221285606,-65.1415521689398,
-55.487415308613));
#187031=CARTESIAN_POINT('Ctrl Pts',(33.8064221286261,-65.1415521689341,
-55.74995));
#187032=CARTESIAN_POINT('Origin',(44.2377516955329,-64.7308390050988,-54.74995));
#187033=CARTESIAN_POINT('',(32.3064221286262,-65.2727851642229,-54.74995));
#187034=CARTESIAN_POINT('Origin',(32.35,-65.7708825132688,-54.74995));
#187035=CARTESIAN_POINT('',(44.1941738241591,-64.2327416560529,-54.74995));
#187036=CARTESIAN_POINT('Ctrl Pts',(32.350023911586,-65.7709087028862,-55.2499499996829));
#187037=CARTESIAN_POINT('Ctrl Pts',(32.3064436723035,-65.2727832793954,
-55.2499781675672));
#187038=CARTESIAN_POINT('Ctrl Pts',(32.3064647172502,-65.2727814382011,
-54.7499500009454));
#187039=CARTESIAN_POINT('Ctrl Pts',(32.2187494539986,-65.7938791072894,
-55.2499434816087));
#187040=CARTESIAN_POINT('Ctrl Pts',(32.1720954901142,-65.2845372222937,
-55.2615949036257));
#187041=CARTESIAN_POINT('Ctrl Pts',(32.0439154964703,-65.2957515186369,
-54.7499383449276));
#187042=CARTESIAN_POINT('Ctrl Pts',(32.089013752819,-65.8165801641519,-55.3038301720448));
#187043=CARTESIAN_POINT('Ctrl Pts',(32.0533601275064,-65.2949252204907,
-55.327473556922));
#187044=CARTESIAN_POINT('Ctrl Pts',(31.7844454492387,-65.3184522062943,
-54.8577131170134));
#187045=CARTESIAN_POINT('Ctrl Pts',(31.9038822591064,-65.8489742655241,
-55.4889602509496));
#187046=CARTESIAN_POINT('Ctrl Pts',(31.891750054253,-65.3090642698107,-55.5134049012229));
#187047=CARTESIAN_POINT('Ctrl Pts',(31.4141852456405,-65.3508457766639,
-55.2279733206136));
#187048=CARTESIAN_POINT('Ctrl Pts',(31.8499941713763,-65.8584035047689,
-55.6186959323283));
#187049=CARTESIAN_POINT('Ctrl Pts',(31.8500296390451,-65.3127143331746,
-55.6318003689116));
#187050=CARTESIAN_POINT('Ctrl Pts',(31.3064104735534,-65.3602748474356,
-55.4874433678435));
#187051=CARTESIAN_POINT('Ctrl Pts',(31.8499999994923,-65.8584024879449,
-55.7499712944341));
#187052=CARTESIAN_POINT('Ctrl Pts',(31.850034171749,-65.3127139366194,-55.7499691665926));
#187053=CARTESIAN_POINT('Ctrl Pts',(31.3064221295715,-65.3602738276662,
-55.7499925886241));
#187054=CARTESIAN_POINT('',(31.3064221286262,-65.3602738277489,-55.74995));
#187055=CARTESIAN_POINT('Origin',(31.35,-65.8583711767947,-55.74995));
#187056=CARTESIAN_POINT('Ctrl Pts',(31.3064221286262,-65.3602738277489,
-55.74995));
#187057=CARTESIAN_POINT('Ctrl Pts',(31.3064221286917,-65.3602738277431,
-55.4874153086129));
#187058=CARTESIAN_POINT('Ctrl Pts',(31.4141952557525,-65.3508449008926,
-55.2279633105016));
#187059=CARTESIAN_POINT('Ctrl Pts',(31.5993153474396,-65.3346489914791,
-55.0428432188135));
#187060=CARTESIAN_POINT('Ctrl Pts',(31.7844354391267,-65.3184530820656,
-54.8577231271254));
#187061=CARTESIAN_POINT('Ctrl Pts',(32.0438874372397,-65.2957539735015,
-54.7499500000659));
#187062=CARTESIAN_POINT('Ctrl Pts',(32.3064221286262,-65.2727851642229,
-54.74995));
#187063=CARTESIAN_POINT('Origin',(31.35,-65.8583711767947,-52.64995));
#187064=CARTESIAN_POINT('',(31.3064221286262,-65.3602738277489,-52.64995));
#187065=CARTESIAN_POINT('Origin',(4.6996065532056,-66.6842487255793,-59.64995));
#187066=CARTESIAN_POINT('',(28.7021688185769,-65.588116469328,-59.64995));
#187067=CARTESIAN_POINT('',(44.1941738241591,-64.2327416560529,-59.64995));
#187068=CARTESIAN_POINT('Origin',(28.6150130758292,-64.5919217712362,-59.64995));
#187069=CARTESIAN_POINT('Ctrl Pts',(28.7021688185769,-65.588116469328,-59.64995));
#187070=CARTESIAN_POINT('Ctrl Pts',(28.7021688185769,-65.588116469328,-60.64995));
#187071=CARTESIAN_POINT('Ctrl Pts',(28.6150130758292,-64.5919217712362,
-60.64995));
#187072=CARTESIAN_POINT('Ctrl Pts',(28.1296330247306,-65.6382068607523,
-59.649950002333));
#187073=CARTESIAN_POINT('Ctrl Pts',(28.2033028175763,-65.6317615890315,
-60.5485267380177));
#187074=CARTESIAN_POINT('Ctrl Pts',(28.0991390263463,-64.7442358506513,
-60.64995));
#187075=CARTESIAN_POINT('Ctrl Pts',(27.5637794550765,-65.6877126333127,
-59.6897495968387));
#187076=CARTESIAN_POINT('Ctrl Pts',(27.6612478839793,-65.6791852507322,
-60.4928259381272));
#187077=CARTESIAN_POINT('Ctrl Pts',(27.584859681119,-64.89321892758,-60.6698497986403));
#187078=CARTESIAN_POINT('Ctrl Pts',(26.4448676457179,-65.7856047321169,
-59.8430005124393));
#187079=CARTESIAN_POINT('Ctrl Pts',(26.5839609508645,-65.7734356447442,
-60.477600868097));
#187080=CARTESIAN_POINT('Ctrl Pts',(26.5596543334024,-65.1843117452004,
-60.7464752559987));
#187081=CARTESIAN_POINT('Ctrl Pts',(25.8914156146746,-65.8340255106386,
-59.9553384305595));
#187082=CARTESIAN_POINT('Ctrl Pts',(26.0406038710994,-65.8209732294689,
-60.5097186566584));
#187083=CARTESIAN_POINT('Ctrl Pts',(26.0485518825385,-65.3264611076661,
-60.802611641644));
#187084=CARTESIAN_POINT('Ctrl Pts',(25.3471476467368,-65.8816427877534,
-60.1196878110938));
#187085=CARTESIAN_POINT('Ctrl Pts',(25.4903329393053,-65.86911569787,-60.5974971539929));
#187086=CARTESIAN_POINT('Ctrl Pts',(25.5416884892005,-65.4644312001072,
-60.8848189055469));
#187087=CARTESIAN_POINT('Ctrl Pts',(25.6564221266688,-65.8545847543119,
-60.0322609860537));
#187088=CARTESIAN_POINT('Ctrl Pts',(25.7808509976504,-65.8436986122353,
-59.9993769765733));
#187089=CARTESIAN_POINT('Ctrl Pts',(25.9056363008897,-65.8327812988126,
-59.9689324054821));
#187090=CARTESIAN_POINT('Ctrl Pts',(26.0307566852339,-65.8218346938133,
-59.9407811370796));
#187091=CARTESIAN_POINT('Ctrl Pts',(26.252037221755,-65.80247517346,-59.8909944631614));
#187092=CARTESIAN_POINT('Ctrl Pts',(26.4743884950002,-65.7830219799129,
-59.8484921029725));
#187093=CARTESIAN_POINT('Ctrl Pts',(26.6976513564849,-65.7634890172034,
-59.812264924346));
#187094=CARTESIAN_POINT('Ctrl Pts',(26.7996931166677,-65.7545615230236,
-59.7957073784607));
#187095=CARTESIAN_POINT('Ctrl Pts',(26.9019251840858,-65.7456173770713,
-59.7804614113611));
#187096=CARTESIAN_POINT('Ctrl Pts',(27.0043315823481,-65.7366579782249,
-59.7664341473284));
#187097=CARTESIAN_POINT('Ctrl Pts',(27.0579416473936,-65.7319677053213,
-59.7590908313837));
#187098=CARTESIAN_POINT('Ctrl Pts',(27.1116030957325,-65.7272729367138,
-59.7520917680714));
#187099=CARTESIAN_POINT('Ctrl Pts',(27.1653166053581,-65.7225736127227,
-59.7454407818489));
#187100=CARTESIAN_POINT('Ctrl Pts',(27.4668119230827,-65.696196185709,-59.7081086242909));
#187101=CARTESIAN_POINT('Ctrl Pts',(27.7698631240487,-65.6696826439597,
-59.6814497127403));
#187102=CARTESIAN_POINT('Ctrl Pts',(28.0745495814197,-65.6430260356534,
-59.665944037988));
#187103=CARTESIAN_POINT('Ctrl Pts',(28.2829846777418,-65.6247903294528,
-59.655336652158));
#187104=CARTESIAN_POINT('Ctrl Pts',(28.4921848717869,-65.6064876841945,
-59.6499500008557));
#187105=CARTESIAN_POINT('Ctrl Pts',(28.7021688185769,-65.588116469328,-59.64995));
#187106=CARTESIAN_POINT('Origin',(25.7,-66.3526821257161,-52.64995));
#187107=CARTESIAN_POINT('',(25.6564221286262,-65.8545847766702,-55.74995));
#187108=CARTESIAN_POINT('',(25.6564221286262,-65.8545847766702,-52.64995));
#187109=CARTESIAN_POINT('Origin',(25.7,-66.3526821257161,-55.74995));
#187110=CARTESIAN_POINT('Ctrl Pts',(25.2,-66.3526821257161,-55.74995));
#187111=CARTESIAN_POINT('Ctrl Pts',(25.2,-65.8945165387074,-55.74995));
#187112=CARTESIAN_POINT('Ctrl Pts',(25.6564221286262,-65.8545847766702,
-55.74995));
#187113=CARTESIAN_POINT('Ctrl Pts',(25.2,-66.3526821257202,-55.6520807487743));
#187114=CARTESIAN_POINT('Ctrl Pts',(25.1999999999616,-65.8945165387115,
-55.6441589529833));
#187115=CARTESIAN_POINT('Ctrl Pts',(25.6564221285773,-65.8545847766745,
-55.5542114975488));
#187116=CARTESIAN_POINT('Ctrl Pts',(25.1705210566577,-66.3578402724271,
-55.5545751632329));
#187117=CARTESIAN_POINT('Ctrl Pts',(25.1652351487286,-65.8975580690824,
-55.5387129880067));
#187118=CARTESIAN_POINT('Ctrl Pts',(25.5974642419416,-65.8597429233806,
-55.3592003264656));
#187119=CARTESIAN_POINT('Ctrl Pts',(25.062254236699,-66.3767845111906,-55.391713681917));
#187120=CARTESIAN_POINT('Ctrl Pts',(25.0420941082282,-65.9083315141418,
-55.3693682972756));
#187121=CARTESIAN_POINT('Ctrl Pts',(25.3809306020242,-65.8786871621453,
-55.033477363834));
#187122=CARTESIAN_POINT('Ctrl Pts',(24.9837596261582,-66.3905192883359,
-55.3267957976874));
#187123=CARTESIAN_POINT('Ctrl Pts',(24.9535760611327,-65.9160758397827,
-55.3059410651653));
#187124=CARTESIAN_POINT('Ctrl Pts',(25.2239370702218,-65.892422316425,-54.9036397860402));
#187125=CARTESIAN_POINT('Ctrl Pts',(24.8935146892254,-66.4063101061761,
-55.2889163081141));
#187126=CARTESIAN_POINT('Ctrl Pts',(24.8576734148988,-65.9244662341272,
-55.273872259957));
#187127=CARTESIAN_POINT('Ctrl Pts',(25.043451507077,-65.9082127571302,-54.8278826162281));
#187128=CARTESIAN_POINT('',(25.043451507077,-65.9082127571302,-54.8278826162281));
#187129=CARTESIAN_POINT('Origin',(25.0870293784509,-66.4063101061761,-54.8278826162281));
#187130=CARTESIAN_POINT('Ctrl Pts',(25.043451507077,-65.9082127571302,-54.8278826162281));
#187131=CARTESIAN_POINT('Ctrl Pts',(25.0742713040834,-65.90551637428,-54.8408189450663));
#187132=CARTESIAN_POINT('Ctrl Pts',(25.104915072702,-65.9028353919181,-54.8555499531048));
#187133=CARTESIAN_POINT('Ctrl Pts',(25.1350929986057,-65.9001951655129,
-54.8720618327809));
#187134=CARTESIAN_POINT('Ctrl Pts',(25.1657431004607,-65.8975136290646,
-54.8888320639594));
#187135=CARTESIAN_POINT('Ctrl Pts',(25.1959121242359,-65.8948741814946,
-54.9074392518001));
#187136=CARTESIAN_POINT('Ctrl Pts',(25.2252929736523,-65.892303690246,-54.9278152010716));
#187137=CARTESIAN_POINT('Ctrl Pts',(25.2553889373856,-65.8896706346014,
-54.9486870901588));
#187138=CARTESIAN_POINT('Ctrl Pts',(25.2846571909018,-65.8871099942175,
-54.9714147499623));
#187139=CARTESIAN_POINT('Ctrl Pts',(25.3127736146752,-65.8846501258785,
-54.9958704922167));
#187140=CARTESIAN_POINT('Ctrl Pts',(25.3411372062356,-65.88216863316,-55.0205412216878));
#187141=CARTESIAN_POINT('Ctrl Pts',(25.3683278367126,-65.8797897612392,
-55.0469701419947));
#187142=CARTESIAN_POINT('Ctrl Pts',(25.3940301284273,-65.8775411020875,
-55.0749758606088));
#187143=CARTESIAN_POINT('Ctrl Pts',(25.4197097931075,-65.8752944225448,
-55.1029569243646));
#187144=CARTESIAN_POINT('Ctrl Pts',(25.4439029560561,-65.873177795052,-55.1325114406684));
#187145=CARTESIAN_POINT('Ctrl Pts',(25.4663241567112,-65.871216194172,-55.1634160027496));
#187146=CARTESIAN_POINT('Ctrl Pts',(25.4741688835925,-65.8705298695015,
-55.1742288870657));
#187147=CARTESIAN_POINT('Ctrl Pts',(25.4817970097154,-65.8698624949418,
-55.1852066986187));
#187148=CARTESIAN_POINT('Ctrl Pts',(25.4891974219829,-65.869215042763,-55.1963388451498));
#187149=CARTESIAN_POINT('Ctrl Pts',(25.510338242743,-65.8673654606088,-55.228140142967));
#187150=CARTESIAN_POINT('Ctrl Pts',(25.5295950731415,-65.8656807062535,
-55.2611692657123));
#187151=CARTESIAN_POINT('Ctrl Pts',(25.5468557307134,-65.864170594391,-55.295083999148));
#187152=CARTESIAN_POINT('Ctrl Pts',(25.5641515040968,-65.862657410293,-55.3290677301512));
#187153=CARTESIAN_POINT('Ctrl Pts',(25.5794427196934,-65.8613196022768,
-55.363939731283));
#187154=CARTESIAN_POINT('Ctrl Pts',(25.5926659905796,-65.8601627159795,
-55.3993402855053));
#187155=CARTESIAN_POINT('Ctrl Pts',(25.6056853291763,-65.8590236714457,
-55.4341948843334));
#187156=CARTESIAN_POINT('Ctrl Pts',(25.6166999804352,-65.8580600143278,
-55.4695609780295));
#187157=CARTESIAN_POINT('Ctrl Pts',(25.6256992872677,-65.8572726770004,
-55.5050939643816));
#187158=CARTESIAN_POINT('Ctrl Pts',(25.6345695399044,-65.8564966304521,
-55.5401173913793));
#187159=CARTESIAN_POINT('Ctrl Pts',(25.641481865841,-65.855891880294,-55.5753022272925));
#187160=CARTESIAN_POINT('Ctrl Pts',(25.6464749038184,-65.8554550460744,
-55.6103291116175));
#187161=CARTESIAN_POINT('Ctrl Pts',(25.6513699614093,-65.8550267840279,
-55.6446686493459));
#187162=CARTESIAN_POINT('Ctrl Pts',(25.6544204578572,-65.8547599001706,
-55.6788558270728));
#187163=CARTESIAN_POINT('Ctrl Pts',(25.6557087574904,-65.8546471885575,
-55.7126093508298));
#187164=CARTESIAN_POINT('Ctrl Pts',(25.6561862637138,-65.8546054121762,
-55.7251200410772));
#187165=CARTESIAN_POINT('Ctrl Pts',(25.6564221286231,-65.8545847766705,
-55.7375713926724));
#187166=CARTESIAN_POINT('Ctrl Pts',(25.6564221286262,-65.8545847766702,
-55.74995));
#187167=CARTESIAN_POINT('Origin',(4.6996065532056,-66.6842487255793,-59.64995));
#187168=CARTESIAN_POINT('',(43.1064181712415,-64.3279079443695,-59.64995));
#187169=CARTESIAN_POINT('',(44.1941738241591,-64.2327416560529,-59.64995));
#187170=CARTESIAN_POINT('Origin',(43.0192624284939,-63.3317132462777,-59.64995));
#187171=CARTESIAN_POINT('Origin',(42.,-64.9266169102438,-52.64995));
#187172=CARTESIAN_POINT('',(41.9564221286262,-64.428519561198,-55.74995));
#187173=CARTESIAN_POINT('Origin',(42.,-64.9266169102438,-55.74995));
#187174=CARTESIAN_POINT('',(41.9564221286262,-64.428519561198,-52.64995));
#187175=CARTESIAN_POINT('Ctrl Pts',(41.5,-64.9266169102438,-55.74995));
#187176=CARTESIAN_POINT('Ctrl Pts',(41.5,-64.4684513232351,-55.74995));
#187177=CARTESIAN_POINT('Ctrl Pts',(41.9564221286262,-64.428519561198,-55.74995));
#187178=CARTESIAN_POINT('Ctrl Pts',(41.5,-64.9266169102493,-55.6186826543063));
#187179=CARTESIAN_POINT('Ctrl Pts',(41.4999999999489,-64.4684513232351,
-55.6078478088783));
#187180=CARTESIAN_POINT('Ctrl Pts',(41.9564221285606,-64.4285195612037,
-55.487415308613));
#187181=CARTESIAN_POINT('Ctrl Pts',(41.4461134364372,-64.9360458371002,
-55.4889566552508));
#187182=CARTESIAN_POINT('Ctrl Pts',(41.4358662151155,-64.4740623023634,
-55.4680441063688));
#187183=CARTESIAN_POINT('Ctrl Pts',(41.8486490015007,-64.4379484880542,
-55.2279633105015));
#187184=CARTESIAN_POINT('Ctrl Pts',(41.2609933447493,-64.9684376559271,
-55.3038365635627));
#187185=CARTESIAN_POINT('Ctrl Pts',(41.2286175782531,-64.4921942086162,
-55.2822894538775));
#187186=CARTESIAN_POINT('Ctrl Pts',(41.4784088181247,-64.4703403068813,
-54.8577231271255));
#187187=CARTESIAN_POINT('Ctrl Pts',(41.1312673456941,-64.991136764493,-55.24995));
#187188=CARTESIAN_POINT('Ctrl Pts',(41.0869589695398,-64.5045877309693,
-55.2386587236917));
#187189=CARTESIAN_POINT('Ctrl Pts',(41.2189568200132,-64.4930394154452,
-54.7499500000659));
#187190=CARTESIAN_POINT('Ctrl Pts',(41.,-65.0141055737697,-55.24995));
#187191=CARTESIAN_POINT('Ctrl Pts',(40.9564221286262,-64.5160082247238,
-55.24995));
#187192=CARTESIAN_POINT('Ctrl Pts',(40.9564221286262,-64.5160082247239,
-54.74995));
#187193=CARTESIAN_POINT('',(40.9564221286262,-64.5160082247239,-54.74995));
#187194=CARTESIAN_POINT('Origin',(41.,-65.0141055737697,-54.74995));
#187195=CARTESIAN_POINT('Ctrl Pts',(40.9564221286262,-64.5160082247239,
-54.74995));
#187196=CARTESIAN_POINT('Ctrl Pts',(41.2189568200132,-64.4930394154452,
-54.7499500000659));
#187197=CARTESIAN_POINT('Ctrl Pts',(41.4784088181247,-64.4703403068813,
-54.8577231271255));
#187198=CARTESIAN_POINT('Ctrl Pts',(41.6635289098127,-64.4541443974678,
-55.0428432188135));
#187199=CARTESIAN_POINT('Ctrl Pts',(41.8486490015007,-64.4379484880542,
-55.2279633105015));
#187200=CARTESIAN_POINT('Ctrl Pts',(41.9564221285606,-64.4285195612037,
-55.487415308613));
#187201=CARTESIAN_POINT('Ctrl Pts',(41.9564221286262,-64.428519561198,-55.74995));
#187202=CARTESIAN_POINT('Origin',(44.2377516955329,-64.7308390050988,-54.74995));
#187203=CARTESIAN_POINT('',(40.4564221286262,-64.5597525564868,-54.74995));
#187204=CARTESIAN_POINT('Origin',(40.5,-65.0578499055327,-54.74995));
#187205=CARTESIAN_POINT('',(44.1941738241591,-64.2327416560529,-54.74995));
#187206=CARTESIAN_POINT('Ctrl Pts',(40.5000239115806,-65.0578760951442,
-55.2499499996828));
#187207=CARTESIAN_POINT('Ctrl Pts',(40.4564436722986,-64.5597506716597,
-55.2499781675608));
#187208=CARTESIAN_POINT('Ctrl Pts',(40.4564647172406,-64.5597488304658,
-54.7499500009454));
#187209=CARTESIAN_POINT('Ctrl Pts',(40.3687494539948,-65.080846499547,-55.2499434816101));
#187210=CARTESIAN_POINT('Ctrl Pts',(40.3220954901096,-64.571504614558,-55.2615949036203));
#187211=CARTESIAN_POINT('Ctrl Pts',(40.1939154964641,-64.5827189109014,
-54.7499383449302));
#187212=CARTESIAN_POINT('Ctrl Pts',(40.2390137528174,-65.1035475564089,
-55.3038301720462));
#187213=CARTESIAN_POINT('Ctrl Pts',(40.2033601275017,-64.581892612755,-55.3274735569167));
#187214=CARTESIAN_POINT('Ctrl Pts',(39.9344454492365,-64.6054195985583,
-54.8577131170157));
#187215=CARTESIAN_POINT('Ctrl Pts',(40.0538822591073,-65.1359416577808,
-55.4889602509488));
#187216=CARTESIAN_POINT('Ctrl Pts',(40.0417500542473,-64.5960316620751,
-55.5134049012177));
#187217=CARTESIAN_POINT('Ctrl Pts',(39.5641852456427,-64.6378131689275,
-55.2279733206113));
#187218=CARTESIAN_POINT('Ctrl Pts',(39.9999941713776,-65.1453708970254,
-55.6186959323252));
#187219=CARTESIAN_POINT('Ctrl Pts',(40.0000296390384,-64.5996817254391,
-55.6318003689066));
#187220=CARTESIAN_POINT('Ctrl Pts',(39.456410473556,-64.6472422396993,-55.4874433678372));
#187221=CARTESIAN_POINT('Ctrl Pts',(39.9999999994923,-65.1453698802017,
-55.7499712944293));
#187222=CARTESIAN_POINT('Ctrl Pts',(40.0000341717414,-64.5996813288839,
-55.7499691665883));
#187223=CARTESIAN_POINT('Ctrl Pts',(39.4564221295715,-64.64724121993,-55.7499925886145));
#187224=CARTESIAN_POINT('',(39.4564221286262,-64.6472412200127,-55.74995));
#187225=CARTESIAN_POINT('Origin',(39.5,-65.1453385690586,-55.74995));
#187226=CARTESIAN_POINT('Ctrl Pts',(39.4564221286262,-64.6472412200127,
-55.74995));
#187227=CARTESIAN_POINT('Ctrl Pts',(39.4564221286917,-64.647241220007,-55.4874153086129));
#187228=CARTESIAN_POINT('Ctrl Pts',(39.5641952557525,-64.6378122931564,
-55.2279633105016));
#187229=CARTESIAN_POINT('Ctrl Pts',(39.7493153474396,-64.6216163837429,
-55.0428432188135));
#187230=CARTESIAN_POINT('Ctrl Pts',(39.9344354391268,-64.6054204743294,
-54.8577231271254));
#187231=CARTESIAN_POINT('Ctrl Pts',(40.1938874372398,-64.5827213657654,
-54.7499500000659));
#187232=CARTESIAN_POINT('Ctrl Pts',(40.4564221286262,-64.5597525564868,
-54.74995));
#187233=CARTESIAN_POINT('Origin',(39.5,-65.1453385690586,-52.64995));
#187234=CARTESIAN_POINT('',(39.4564221286262,-64.6472412200127,-52.64995));
#187235=CARTESIAN_POINT('Origin',(4.6996065532056,-66.6842487255793,-59.64995));
#187236=CARTESIAN_POINT('',(44.1941738241591,-64.2327416560529,-59.64995));
#187237=CARTESIAN_POINT('Ctrl Pts',(53.7823432375846,11.067884690566,-55.2526734204115));
#187238=CARTESIAN_POINT('Ctrl Pts',(53.3054454943535,10.8575310968505,-55.2747187747876));
#187239=CARTESIAN_POINT('Ctrl Pts',(53.3256899305368,10.8121330655672,-54.7553968408231));
#187240=CARTESIAN_POINT('Ctrl Pts',(53.8861362179292,10.9515071084652,-55.2648699557477));
#187241=CARTESIAN_POINT('Ctrl Pts',(53.3650311600591,10.7244739426765,-55.3417466734359));
#187242=CARTESIAN_POINT('Ctrl Pts',(53.4285862862346,10.5813885818665,-54.7797862992586));
#187243=CARTESIAN_POINT('Ctrl Pts',(53.9838097653667,10.83974934456,-55.3179449795228));
#187244=CARTESIAN_POINT('Ctrl Pts',(53.3983781597441,10.6502596450882,-55.4540676493459));
#187245=CARTESIAN_POINT('Ctrl Pts',(53.5254458539065,10.3597364405483,-54.885939939012));
#187246=CARTESIAN_POINT('Ctrl Pts',(54.0930825652429,10.7133083132261,-55.4526385853652));
#187247=CARTESIAN_POINT('Ctrl Pts',(53.4176451441909,10.6111056725941,-55.596678279911));
#187248=CARTESIAN_POINT('Ctrl Pts',(53.633790842791,10.1090015716016,-55.1553271807471));
#187249=CARTESIAN_POINT('Ctrl Pts',(54.1219468150851,10.6796458924645,-55.5047178594674));
#187250=CARTESIAN_POINT('Ctrl Pts',(53.4186534680994,10.6106295502708,-55.6378844781733));
#187251=CARTESIAN_POINT('Ctrl Pts',(53.6624100137865,10.0422483461928,-55.2594857136242));
#187252=CARTESIAN_POINT('Ctrl Pts',(54.1624914359772,10.6322531187842,-55.6228534833935));
#187253=CARTESIAN_POINT('Ctrl Pts',(53.4178589543304,10.6154785181549,-55.7046481866627));
#187254=CARTESIAN_POINT('Ctrl Pts',(53.702610379063,9.94826762670561,-55.4957569720976));
#187255=CARTESIAN_POINT('Ctrl Pts',(54.172917586547,10.61999998,-55.685050712911));
#187256=CARTESIAN_POINT('Ctrl Pts',(53.4163125940233,10.619999979359,-55.7271468411276));
#187257=CARTESIAN_POINT('Ctrl Pts',(53.7129480039811,9.9239694167493,-55.6201514218302));
#187258=CARTESIAN_POINT('Ctrl Pts',(54.1729175880533,10.61999998,-55.74995));
#187259=CARTESIAN_POINT('Ctrl Pts',(53.4163125938068,10.61999998,-55.74995));
#187260=CARTESIAN_POINT('Ctrl Pts',(53.7129480054761,9.92396941324122,-55.74995));
#187261=CARTESIAN_POINT('',(53.3256899305368,10.8121330655672,-54.7553968408231));
#187262=CARTESIAN_POINT('Origin',(53.7823432375846,11.015769401132,-54.7553968408231));
#187263=CARTESIAN_POINT('',(53.7129480054761,9.92396941324122,-55.74995));
#187264=CARTESIAN_POINT('Ctrl Pts',(53.7129480054761,9.92396941324122,-55.74995));
#187265=CARTESIAN_POINT('Ctrl Pts',(53.7129480048637,9.92396941467835,-55.6967763512781));
#187266=CARTESIAN_POINT('Ctrl Pts',(53.7112147843802,9.92804334268761,-55.6443923193454));
#187267=CARTESIAN_POINT('Ctrl Pts',(53.7077550226655,9.93615769838508,-55.5927930680038));
#187268=CARTESIAN_POINT('Ctrl Pts',(53.7070427178468,9.93782830322472,-55.582169678763));
#187269=CARTESIAN_POINT('Ctrl Pts',(53.7062571614758,9.93967032838863,-55.57157960177));
#187270=CARTESIAN_POINT('Ctrl Pts',(53.7053983076824,9.94168372171603,-55.5610228702942));
#187271=CARTESIAN_POINT('Ctrl Pts',(53.7036268526,9.9458365075222,-55.5392487618595));
#187272=CARTESIAN_POINT('Ctrl Pts',(53.7015273912866,9.9507562630614,-55.5174450002407));
#187273=CARTESIAN_POINT('Ctrl Pts',(53.6991098272624,9.95641828381884,-55.4957961558367));
#187274=CARTESIAN_POINT('Ctrl Pts',(53.6966689320685,9.96213494700362,-55.473938385069));
#187275=CARTESIAN_POINT('Ctrl Pts',(53.693903757809,9.96860827125173,-55.452238612997));
#187276=CARTESIAN_POINT('Ctrl Pts',(53.6908450504304,9.9757648499092,-55.4308742653829));
#187277=CARTESIAN_POINT('Ctrl Pts',(53.6883304010962,9.98164847443693,-55.4133100345323));
#187278=CARTESIAN_POINT('Ctrl Pts',(53.6856177574555,9.98799296192938,-55.3959722863425));
#187279=CARTESIAN_POINT('Ctrl Pts',(53.6827342900112,9.99473409341425,-55.3789529390801));
#187280=CARTESIAN_POINT('Ctrl Pts',(53.6826591797317,9.99490969042721,-55.3785096089732));
#187281=CARTESIAN_POINT('Ctrl Pts',(53.6825839300607,9.9950856114844,-55.378066355819));
#187282=CARTESIAN_POINT('Ctrl Pts',(53.682508540985,9.99526185660251,-55.3776231795372));
#187283=CARTESIAN_POINT('Ctrl Pts',(53.6757958049232,10.0109549387852,-55.3381622180861));
#187284=CARTESIAN_POINT('Ctrl Pts',(53.6681180133557,10.0288871912831,-55.3001692589446));
#187285=CARTESIAN_POINT('Ctrl Pts',(53.6594755760649,10.0490364743368,-55.2635974761426));
#187286=CARTESIAN_POINT('Ctrl Pts',(53.6554675883568,10.0583808382114,-55.2466370689097));
#187287=CARTESIAN_POINT('Ctrl Pts',(53.6512518906864,10.0682025695934,-55.2299827533854));
#187288=CARTESIAN_POINT('Ctrl Pts',(53.6468273042282,10.07850218353,-55.2136321846475));
#187289=CARTESIAN_POINT('Ctrl Pts',(53.6421181547434,10.0894642072407,-55.1962300447914));
#187290=CARTESIAN_POINT('Ctrl Pts',(53.637124495453,10.1010789815322,-55.1790043701209));
#187291=CARTESIAN_POINT('Ctrl Pts',(53.6318875227673,10.1132475345242,-55.1621368610288));
#187292=CARTESIAN_POINT('Ctrl Pts',(53.626579315431,10.1255816073064,-55.1450399157357));
#187293=CARTESIAN_POINT('Ctrl Pts',(53.6210211374223,10.1384845723914,-55.1283110733852));
#187294=CARTESIAN_POINT('Ctrl Pts',(53.6152735870561,10.1518130379855,-55.1121076745932));
#187295=CARTESIAN_POINT('Ctrl Pts',(53.609746478553,10.1646303028765,-55.0965257418503));
#187296=CARTESIAN_POINT('Ctrl Pts',(53.604044430579,10.1778406037002,-55.0814294938097));
#187297=CARTESIAN_POINT('Ctrl Pts',(53.5982359111103,10.1912837029229,-55.0669307798463));
#187298=CARTESIAN_POINT('Ctrl Pts',(53.5980491569954,10.1917159222018,-55.0664646206972));
#187299=CARTESIAN_POINT('Ctrl Pts',(53.5978622041318,10.1921485874913,-55.065998854503));
#187300=CARTESIAN_POINT('Ctrl Pts',(53.5976750524344,10.1925816989101,-55.0655334806687));
#187301=CARTESIAN_POINT('Ctrl Pts',(53.5876493716261,10.2157833951786,-55.0406034929458));
#187302=CARTESIAN_POINT('Ctrl Pts',(53.5771573605076,10.2400161971565,-55.0171039053591));
#187303=CARTESIAN_POINT('Ctrl Pts',(53.5662062859971,10.2652563708093,-54.9949777152844));
#187304=CARTESIAN_POINT('Ctrl Pts',(53.5578688397943,10.2844726212124,-54.9781322523811));
#187305=CARTESIAN_POINT('Ctrl Pts',(53.5492649777567,10.3042735113455,-54.9620836922876));
#187306=CARTESIAN_POINT('Ctrl Pts',(53.5403934613312,10.3246581340979,-54.9468240992755));
#187307=CARTESIAN_POINT('Ctrl Pts',(53.5325206041197,10.3427480768479,-54.9332822659373));
#187308=CARTESIAN_POINT('Ctrl Pts',(53.5243691543248,10.3614533780027,-54.9202518509527));
#187309=CARTESIAN_POINT('Ctrl Pts',(53.5160082521778,10.3806116918597,-54.9078854214808));
#187310=CARTESIAN_POINT('Ctrl Pts',(53.5133554582639,10.3866903491033,-54.9039617313978));
#187311=CARTESIAN_POINT('Ctrl Pts',(53.5106816795215,10.3928143899775,-54.9001045739724));
#187312=CARTESIAN_POINT('Ctrl Pts',(53.5079893939122,10.3989780408986,-54.8963179394496));
#187313=CARTESIAN_POINT('Ctrl Pts',(53.499437108409,10.4185574281069,-54.8842893569607));
#187314=CARTESIAN_POINT('Ctrl Pts',(53.4907041389291,10.4385224734264,-54.8729481962707));
#187315=CARTESIAN_POINT('Ctrl Pts',(53.4818760853353,10.458675248751,-54.8623971539524));
#187316=CARTESIAN_POINT('Ctrl Pts',(53.479166060809,10.464861721774,-54.8591582085658));
#187317=CARTESIAN_POINT('Ctrl Pts',(53.4764471557122,10.4710657164826,-54.8559933977348));
#187318=CARTESIAN_POINT('Ctrl Pts',(53.4737220448059,10.4772810900949,-54.8529048290228));
#187319=CARTESIAN_POINT('Ctrl Pts',(53.4607634882216,10.5068366837629,-54.8382179433156));
#187320=CARTESIAN_POINT('Ctrl Pts',(53.4475736911319,10.536857104021,-54.8251456815363));
#187321=CARTESIAN_POINT('Ctrl Pts',(53.4341586380481,10.5673216564299,-54.8136257598735));
#187322=CARTESIAN_POINT('Ctrl Pts',(53.420641509875,10.5980180135051,-54.8020181831695));
#187323=CARTESIAN_POINT('Ctrl Pts',(53.406895419264,10.6291659382345,-54.7919864990641));
#187324=CARTESIAN_POINT('Ctrl Pts',(53.3929173025913,10.6607631354219,-54.7835158564423));
#187325=CARTESIAN_POINT('Ctrl Pts',(53.379019678782,10.6921783804239,-54.7750939919424));
#187326=CARTESIAN_POINT('Ctrl Pts',(53.3648924224103,10.7240383998955,-54.7682151279967));
#187327=CARTESIAN_POINT('Ctrl Pts',(53.3505275116743,10.756349667385,-54.7629146804316));
#187328=CARTESIAN_POINT('Ctrl Pts',(53.3423264209277,10.7747965371003,-54.7598885946954));
#187329=CARTESIAN_POINT('Ctrl Pts',(53.3340477989169,10.7933905939691,-54.7573779011054));
#187330=CARTESIAN_POINT('Ctrl Pts',(53.3256899305368,10.8121330655672,-54.7553968408231));
#187331=CARTESIAN_POINT('Origin',(54.1729175880533,10.11999998,-55.74995));
#187332=CARTESIAN_POINT('Origin',(54.1729175880533,10.11999998,-55.24995));
#187333=CARTESIAN_POINT('',(53.7129480054761,9.92396941324122,-55.24995));
#187334=CARTESIAN_POINT('Origin',(0.,-12.9675000200281,-60.42825533736));
#187335=CARTESIAN_POINT('Origin',(0.,-12.9675000200281,-60.42825533736));
#187336=CARTESIAN_POINT('Origin',(56.2465221147258,4.46999998000001,-55.24995));
#187337=CARTESIAN_POINT('',(55.7689460407313,4.32194224278905,-55.74995));
#187338=CARTESIAN_POINT('',(55.7689460407313,4.32194224278906,-55.24995));
#187339=CARTESIAN_POINT('Origin',(56.2465221147258,4.46999998000001,-55.74995));
#187340=CARTESIAN_POINT('Ctrl Pts',(56.2518760188067,3.96334729621203,-55.8294468689166));
#187341=CARTESIAN_POINT('Ctrl Pts',(55.8813420564174,3.95911837961328,-55.8475485519145));
#187342=CARTESIAN_POINT('Ctrl Pts',(55.7730598430189,4.30872548228013,-55.9090619298413));
#187343=CARTESIAN_POINT('Ctrl Pts',(56.2421124760699,3.97898568412623,-55.7377933134847));
#187344=CARTESIAN_POINT('Ctrl Pts',(55.8742327966825,3.9826937870183,-55.7356483282311));
#187345=CARTESIAN_POINT('Ctrl Pts',(55.7633830612446,4.33978792174147,-55.7256225368045));
#187346=CARTESIAN_POINT('Ctrl Pts',(56.2498472169413,3.96666903650799,-55.6406903017816));
#187347=CARTESIAN_POINT('Ctrl Pts',(55.8800704582515,3.96340574722032,-55.6138694439694));
#187348=CARTESIAN_POINT('Ctrl Pts',(55.7710496378194,4.31531871748535,-55.5312554109142));
#187349=CARTESIAN_POINT('Ctrl Pts',(56.2881583747582,3.90468933699336,-55.494132859849));
#187350=CARTESIAN_POINT('Ctrl Pts',(55.9066278983059,3.87472424751448,-55.4413052836556));
#187351=CARTESIAN_POINT('Ctrl Pts',(55.8090161453349,4.19224220492976,-55.2379754767005));
#187352=CARTESIAN_POINT('Ctrl Pts',(56.3116282654917,3.86659531774519,-55.4385935578195));
#187353=CARTESIAN_POINT('Ctrl Pts',(55.9229328254989,3.82012971028789,-55.3788565241339));
#187354=CARTESIAN_POINT('Ctrl Pts',(55.832275617124,4.11659879830721,-55.1268557913785));
#187355=CARTESIAN_POINT('Ctrl Pts',(56.3681986096508,3.77376027759107,-55.34750757013));
#187356=CARTESIAN_POINT('Ctrl Pts',(55.9604473236213,3.69364022912991,-55.2864718145835));
#187357=CARTESIAN_POINT('Ctrl Pts',(55.888335440433,3.9323045563208,-54.9446837986715));
#187358=CARTESIAN_POINT('Ctrl Pts',(56.4017509144347,3.71825300770064,-55.3112107227452));
#187359=CARTESIAN_POINT('Ctrl Pts',(55.9821791809102,3.61993921542383,-55.2561026101603));
#187360=CARTESIAN_POINT('Ctrl Pts',(55.9215848671782,3.82212901679781,-54.8721313715614));
#187361=CARTESIAN_POINT('Ctrl Pts',(56.4868459075913,3.57562280381526,-55.2530405928642));
#187362=CARTESIAN_POINT('Ctrl Pts',(56.0342869816528,3.44212912761038,-55.2238841518077));
#187363=CARTESIAN_POINT('Ctrl Pts',(56.005908358045,3.53910658458787,-54.7559557018408));
#187364=CARTESIAN_POINT('Ctrl Pts',(56.5418624571477,3.48194475398672,-55.2416519066958));
#187365=CARTESIAN_POINT('Ctrl Pts',(56.0654069380446,3.33499954426141,-55.2402241631574));
#187366=CARTESIAN_POINT('Ctrl Pts',(56.0604196755096,3.35329673808427,-54.7333414930262));
#187367=CARTESIAN_POINT('Ctrl Pts',(56.592425919442,3.39399197445088,-55.2560492201736));
#187368=CARTESIAN_POINT('Ctrl Pts',(56.0890816376392,3.25347227784392,-55.2795842141493));
#187369=CARTESIAN_POINT('Ctrl Pts',(56.110520856671,3.17891193839818,-54.7622758815643));
#187370=CARTESIAN_POINT('',(56.066723956657,3.33043300908072,-54.74995));
#187371=CARTESIAN_POINT('Ctrl Pts',(56.0667239566569,3.33043300908083,-54.74995));
#187372=CARTESIAN_POINT('Ctrl Pts',(56.054810110711,3.3714179800412,-54.7499500048111));
#187373=CARTESIAN_POINT('Ctrl Pts',(56.0428719096527,3.41230937921189,-54.7525736247989));
#187374=CARTESIAN_POINT('Ctrl Pts',(56.0309991957517,3.45281789175017,-54.7576881483825));
#187375=CARTESIAN_POINT('Ctrl Pts',(56.0183308037643,3.49604117835013,-54.7631454338967));
#187376=CARTESIAN_POINT('Ctrl Pts',(56.0057365602009,3.53882993079309,-54.7714383768922));
#187377=CARTESIAN_POINT('Ctrl Pts',(55.9933214348628,3.58084263808004,-54.7824678791719));
#187378=CARTESIAN_POINT('Ctrl Pts',(55.9809063095247,3.62285534536699,-54.7934973814515));
#187379=CARTESIAN_POINT('Ctrl Pts',(55.9686698102716,3.66409363256126,-54.8072637702972));
#187380=CARTESIAN_POINT('Ctrl Pts',(55.9567198801064,3.70420224798085,-54.8237268632943));
#187381=CARTESIAN_POINT('Ctrl Pts',(55.9565878111619,3.70464552274758,-54.8239088110787));
#187382=CARTESIAN_POINT('Ctrl Pts',(55.9564557655643,3.70508869905399,-54.8240911044694));
#187383=CARTESIAN_POINT('Ctrl Pts',(55.9563237434519,3.70553177648158,-54.8242737432782));
#187384=CARTESIAN_POINT('Ctrl Pts',(55.9343635745757,3.77923196927894,-54.8546533441933));
#187385=CARTESIAN_POINT('Ctrl Pts',(55.9131570004002,3.84984800741946,-54.8944556864574));
#187386=CARTESIAN_POINT('Ctrl Pts',(55.8935222184455,3.91485853316083,-54.9422511775329));
#187387=CARTESIAN_POINT('Ctrl Pts',(55.8818370634331,3.95354794017741,-54.970695482308));
#187388=CARTESIAN_POINT('Ctrl Pts',(55.8707083955309,3.99025269895495,-55.0019703122245));
#187389=CARTESIAN_POINT('Ctrl Pts',(55.8603061323666,4.02444969307579,-55.0357720069019));
#187390=CARTESIAN_POINT('Ctrl Pts',(55.8601552265094,4.02494578961079,-55.0362623688194));
#187391=CARTESIAN_POINT('Ctrl Pts',(55.8600044604701,4.02544140270094,-55.0367533059883));
#187392=CARTESIAN_POINT('Ctrl Pts',(55.859853834661,4.02593653113584,-55.0372448169564));
#187393=CARTESIAN_POINT('Ctrl Pts',(55.8409688317124,4.0880142189489,-55.0988689578539));
#187394=CARTESIAN_POINT('Ctrl Pts',(55.8242867117939,4.14247853961686,-55.1695258968661));
#187395=CARTESIAN_POINT('Ctrl Pts',(55.8106050241011,4.1869905311094,-55.2464345690386));
#187396=CARTESIAN_POINT('Ctrl Pts',(55.8040947258896,4.20817112995892,-55.2830308137518));
#187397=CARTESIAN_POINT('Ctrl Pts',(55.7982636966349,4.22709855295217,-55.3210433783436));
#187398=CARTESIAN_POINT('Ctrl Pts',(55.7931974644892,4.24352182478376,-55.3601764970326));
#187399=CARTESIAN_POINT('Ctrl Pts',(55.7931360049005,4.24372105914634,-55.3606512295973));
#187400=CARTESIAN_POINT('Ctrl Pts',(55.7930746570768,4.24391992824448,-55.3611261391855));
#187401=CARTESIAN_POINT('Ctrl Pts',(55.7930134210752,4.24411843191566,-55.3616012250647));
#187402=CARTESIAN_POINT('Ctrl Pts',(55.7885029443904,4.25873967037657,-55.3965947538371));
#187403=CARTESIAN_POINT('Ctrl Pts',(55.7846130556769,4.27133328431391,-55.4324278680426));
#187404=CARTESIAN_POINT('Ctrl Pts',(55.7813486835249,4.28189251196921,-55.4689029452562));
#187405=CARTESIAN_POINT('Ctrl Pts',(55.7780780325758,4.2924720495779,-55.5054481797902));
#187406=CARTESIAN_POINT('Ctrl Pts',(55.775435211876,4.30100963982806,-55.5426389688294));
#187407=CARTESIAN_POINT('Ctrl Pts',(55.7734395025711,4.30745180750473,-55.5802948673857));
#187408=CARTESIAN_POINT('Ctrl Pts',(55.7714984886898,4.31371741785941,-55.6169187492451));
#187409=CARTESIAN_POINT('Ctrl Pts',(55.7701695736421,4.31800094942098,-55.6539836247096));
#187410=CARTESIAN_POINT('Ctrl Pts',(55.7694848260442,4.32020701122525,-55.6913249513655));
#187411=CARTESIAN_POINT('Ctrl Pts',(55.7691277073319,4.32135754604051,-55.7107996987557));
#187412=CARTESIAN_POINT('Ctrl Pts',(55.7689460418115,4.32194223930484,-55.7303495724289));
#187413=CARTESIAN_POINT('Ctrl Pts',(55.7689460407313,4.32194224278906,-55.74995));
#187414=CARTESIAN_POINT('Origin',(56.5468500449175,3.46999998000001,-54.74995));
#187415=CARTESIAN_POINT('Origin',(0.,-12.9675000200281,-54.74995));
#187416=CARTESIAN_POINT('',(56.208463007634,2.83467839222654,-54.74995));
#187417=CARTESIAN_POINT('Origin',(0.,-12.9675000200281,-54.74995));
#187418=CARTESIAN_POINT('Origin',(56.6898028749653,2.96999998000001,-54.74995));
#187419=CARTESIAN_POINT('Ctrl Pts',(56.6516106473573,3.03773716318841,-55.2548395864932));
#187420=CARTESIAN_POINT('Ctrl Pts',(56.1862233638146,2.91063352623763,-55.2365176478553));
#187421=CARTESIAN_POINT('Ctrl Pts',(56.1704852303868,2.96901219974452,-54.7588470687756));
#187422=CARTESIAN_POINT('Ctrl Pts',(56.7365664636558,2.88838457711559,-55.2329986037404));
#187423=CARTESIAN_POINT('Ctrl Pts',(56.2378094923969,2.72675510356031,-55.2554023668191));
#187424=CARTESIAN_POINT('Ctrl Pts',(56.2547381424865,2.67276304505858,-54.7151058664062));
#187425=CARTESIAN_POINT('Ctrl Pts',(56.8232758616439,2.72973218222745,-55.2852577349349));
#187426=CARTESIAN_POINT('Ctrl Pts',(56.272540084895,2.60245677689778,-55.3631060048095));
#187427=CARTESIAN_POINT('Ctrl Pts',(56.3408153301335,2.35776462627681,-54.8196810538982));
#187428=CARTESIAN_POINT('Ctrl Pts',(56.9409610884963,2.51006427970322,-55.5006989132498));
#187429=CARTESIAN_POINT('Ctrl Pts',(56.3106636954826,2.47176602276538,-55.5888533041906));
#187430=CARTESIAN_POINT('Ctrl Pts',(56.4576103865826,1.92173897553581,-55.2509470312754));
#187431=CARTESIAN_POINT('Ctrl Pts',(56.9713444184252,2.4511633015209,-55.6620201884579));
#187432=CARTESIAN_POINT('Ctrl Pts',(56.3132427996389,2.46728529949762,-55.6970341949502));
#187433=CARTESIAN_POINT('Ctrl Pts',(56.4877712558399,1.80479876584888,-55.5739123475053));
#187434=CARTESIAN_POINT('Ctrl Pts',(56.9587711759279,2.47540554332925,-55.8218687400276));
#187435=CARTESIAN_POINT('Ctrl Pts',(56.3116760352399,2.47109535466139,-55.7946188306712));
#187436=CARTESIAN_POINT('Ctrl Pts',(56.4752909911635,1.85292504817076,-55.8939326223247));
#187437=CARTESIAN_POINT('',(56.4778207328943,1.8431691585182,-55.74995));
#187438=CARTESIAN_POINT('Ctrl Pts',(56.4778207328944,1.84316915851821,-55.74995));
#187439=CARTESIAN_POINT('Ctrl Pts',(56.4778064569306,1.84322359733619,-55.6560313317286));
#187440=CARTESIAN_POINT('Ctrl Pts',(56.4743371862811,1.85647090128218,-55.5635633305672));
#187441=CARTESIAN_POINT('Ctrl Pts',(56.4675209933656,1.88238984882649,-55.4737762830553));
#187442=CARTESIAN_POINT('Ctrl Pts',(56.4646552786549,1.89328688624677,-55.4360273422497));
#187443=CARTESIAN_POINT('Ctrl Pts',(56.4611973335471,1.90642358799506,-55.3987522848102));
#187444=CARTESIAN_POINT('Ctrl Pts',(56.4571525729354,1.92176052606978,-55.362042538798));
#187445=CARTESIAN_POINT('Ctrl Pts',(56.4466430200751,1.96161068702785,-55.2666591395701));
#187446=CARTESIAN_POINT('Ctrl Pts',(56.4329085143679,2.01353490739002,-55.1807492293272));
#187447=CARTESIAN_POINT('Ctrl Pts',(56.4157876207897,2.07773388906235,-55.1040867013627));
#187448=CARTESIAN_POINT('Ctrl Pts',(56.4106465751013,2.09701149840069,-55.0810665501625));
#187449=CARTESIAN_POINT('Ctrl Pts',(56.4051998459472,2.11739579758647,-55.0588802123864));
#187450=CARTESIAN_POINT('Ctrl Pts',(56.3994421718616,2.1388919699916,-55.0375215661014));
#187451=CARTESIAN_POINT('Ctrl Pts',(56.3745100863326,2.23197546186361,-54.9450335947364));
#187452=CARTESIAN_POINT('Ctrl Pts',(56.3453168238088,2.34004445713371,-54.8734764439432));
#187453=CARTESIAN_POINT('Ctrl Pts',(56.3124317677987,2.46007868339493,-54.8240658663659));
#187454=CARTESIAN_POINT('Ctrl Pts',(56.2795467117886,2.58011290965614,-54.7746552887886));
#187455=CARTESIAN_POINT('Ctrl Pts',(56.2449231123173,2.70498953592612,-54.74995));
#187456=CARTESIAN_POINT('Ctrl Pts',(56.2084630076341,2.83467839222655,-54.74995));
#187457=CARTESIAN_POINT('Origin',(56.9614672388491,1.96999998000001,-55.74995));
#187458=CARTESIAN_POINT('Origin',(56.9614672388491,1.96999998000001,-55.24995));
#187459=CARTESIAN_POINT('',(56.4778207328943,1.84316915851819,-55.24995));
#187460=CARTESIAN_POINT('Origin',(0.,-12.9675000200281,-60.42825533736));
#187461=CARTESIAN_POINT('Origin',(0.,-12.9675000200281,-60.42825533736));
#187462=CARTESIAN_POINT('Origin',(58.1504944089282,-3.68000001999999,-55.24995));
#187463=CARTESIAN_POINT('',(57.6567521511579,-3.75885801193397,-55.9233081330105));
#187464=CARTESIAN_POINT('',(57.6567521511579,-3.75885801193397,-55.24995));
#187465=CARTESIAN_POINT('Origin',(58.1504944089282,-3.68000001999999,-55.9233081330105));
#187466=CARTESIAN_POINT('Ctrl Pts',(58.1878043152552,-4.18472849816432,
-56.0217471588075));
#187467=CARTESIAN_POINT('Ctrl Pts',(57.7288017309817,-4.21869464918518,
-56.0268087650182));
#187468=CARTESIAN_POINT('Ctrl Pts',(57.6580782481123,-3.7670747753154,-56.0829545312913));
#187469=CARTESIAN_POINT('Ctrl Pts',(58.1423490001074,-4.17368834353939,
-55.9044937172376));
#187470=CARTESIAN_POINT('Ctrl Pts',(57.7207276063559,-4.16605409632374,
-55.912529187981));
#187471=CARTESIAN_POINT('Ctrl Pts',(57.6545081941398,-3.74493084812172,
-55.8965040979149));
#187472=CARTESIAN_POINT('Ctrl Pts',(58.11010891456,-4.18155527439172,-55.7954042268261));
#187473=CARTESIAN_POINT('Ctrl Pts',(57.7177405846301,-4.14730583030866,
-55.7833549220629));
#187474=CARTESIAN_POINT('Ctrl Pts',(57.6570350940306,-3.76040655228401,
-55.7095218572218));
#187475=CARTESIAN_POINT('Ctrl Pts',(58.0758010551818,-4.23492939420442,
-55.626523645907));
#187476=CARTESIAN_POINT('Ctrl Pts',(57.7231513907377,-4.18465995709919,
-55.5758965119262));
#187477=CARTESIAN_POINT('Ctrl Pts',(57.6738297434981,-3.86630826885906,
-55.4091279774612));
#187478=CARTESIAN_POINT('Ctrl Pts',(58.0682346046872,-4.2681708265488,-55.5642771712915));
#187479=CARTESIAN_POINT('Ctrl Pts',(57.7282596126722,-4.21904460184081,
-55.4959409277901));
#187480=CARTESIAN_POINT('Ctrl Pts',(57.6842607125848,-3.93233117446903,
-55.2948627293281));
#187481=CARTESIAN_POINT('Ctrl Pts',(58.0615640318237,-4.41832044615007,
-55.3857650708271));
#187482=CARTESIAN_POINT('Ctrl Pts',(57.7539337512875,-4.39250111928527,
-55.26869173567));
#187483=CARTESIAN_POINT('Ctrl Pts',(57.730526224235,-4.2306772427365,-54.9612377069699));
#187484=CARTESIAN_POINT('Ctrl Pts',(58.0893322115688,-4.58139785886709,
-55.3288487124944));
#187485=CARTESIAN_POINT('Ctrl Pts',(57.7860859134861,-4.61172772721033,
-55.1905959772978));
#187486=CARTESIAN_POINT('Ctrl Pts',(57.7793092684043,-4.5547357307314,-54.8442406125823));
#187487=CARTESIAN_POINT('Ctrl Pts',(58.132482042408,-4.74154412477497,-55.3691052207555));
#187488=CARTESIAN_POINT('Ctrl Pts',(57.8139022478951,-4.80923291831809,
-55.2499722576169));
#187489=CARTESIAN_POINT('Ctrl Pts',(57.8236816674951,-4.87324703899737,
-54.9084895606105));
#187490=CARTESIAN_POINT('',(57.8012193907064,-4.71406478367238,-54.8923577774473));
#187491=CARTESIAN_POINT('Origin',(58.2961987903268,-4.64338668274023,-54.8923577774473));
#187492=CARTESIAN_POINT('Ctrl Pts',(57.8012193907064,-4.71406478367238,
-54.8923577774473));
#187493=CARTESIAN_POINT('Ctrl Pts',(57.7836536578014,-4.59104682177848,
-54.8901832085045));
#187494=CARTESIAN_POINT('Ctrl Pts',(57.7662856874572,-4.47225223324713,
-54.9123724001228));
#187495=CARTESIAN_POINT('Ctrl Pts',(57.7495807450161,-4.36017290714565,
-54.9578152376692));
#187496=CARTESIAN_POINT('Ctrl Pts',(57.7482218313389,-4.35105547799513,
-54.9615119216709));
#187497=CARTESIAN_POINT('Ctrl Pts',(57.7468673329787,-4.34198248231328,
-54.9653624866117));
#187498=CARTESIAN_POINT('Ctrl Pts',(57.745517514559,-4.33295525906636,-54.9693663348943));
#187499=CARTESIAN_POINT('Ctrl Pts',(57.7365460375155,-4.27295642889168,
-54.9959776423346));
#187500=CARTESIAN_POINT('Ctrl Pts',(57.7280596798513,-4.2168386440149,-55.0284329935762));
#187501=CARTESIAN_POINT('Ctrl Pts',(57.7200923014674,-4.16459703502482,
-55.0667323886189));
#187502=CARTESIAN_POINT('Ctrl Pts',(57.7121249230835,-4.11235542603474,
-55.1050317836617));
#187503=CARTESIAN_POINT('Ctrl Pts',(57.70446832363,-4.06264749225641,-55.1506834849025));
#187504=CARTESIAN_POINT('Ctrl Pts',(57.6977762772175,-4.01949639254467,
-55.1991627051508));
#187505=CARTESIAN_POINT('Ctrl Pts',(57.6910842308049,-3.97634529283294,
-55.2476419253992));
#187506=CARTESIAN_POINT('Ctrl Pts',(57.6851484738385,-3.93838586919532,
-55.2999617303345));
#187507=CARTESIAN_POINT('Ctrl Pts',(57.6799997155797,-3.90561340277092,
-55.3561221199568));
#187508=CARTESIAN_POINT('Ctrl Pts',(57.6774253364502,-3.88922716955872,
-55.384202314768));
#187509=CARTESIAN_POINT('Ctrl Pts',(57.67504757604,-3.87413769627492,-55.4132426557509));
#187510=CARTESIAN_POINT('Ctrl Pts',(57.6728694851827,-3.8603445037118,-55.4432431429055));
#187511=CARTESIAN_POINT('Ctrl Pts',(57.6706913943255,-3.84655131114868,
-55.4732436300601));
#187512=CARTESIAN_POINT('Ctrl Pts',(57.6686282628525,-3.83352020962757,
-55.5057266054656));
#187513=CARTESIAN_POINT('Ctrl Pts',(57.6669367487985,-3.82285337494814,
-55.5361250428846));
#187514=CARTESIAN_POINT('Ctrl Pts',(57.6616870217134,-3.7897481395564,-55.6304686280757));
#187515=CARTESIAN_POINT('Ctrl Pts',(57.6584496886985,-3.76948979078947,
-55.7293075756491));
#187516=CARTESIAN_POINT('Ctrl Pts',(57.6572653615991,-3.76207187814138,
-55.8326418856047));
#187517=CARTESIAN_POINT('Ctrl Pts',(57.6569232810199,-3.75992929113468,
-55.8624889275369));
#187518=CARTESIAN_POINT('Ctrl Pts',(57.656752151158,-3.75885801193395,-55.8927110100055));
#187519=CARTESIAN_POINT('Ctrl Pts',(57.656752151158,-3.75885801193396,-55.9233081330105));
#187520=CARTESIAN_POINT('Ctrl Pts',(58.1110275345658,-4.66169335137012,
-55.3564444847807));
#187521=CARTESIAN_POINT('Ctrl Pts',(57.8003896508712,-4.70825387307828,
-55.2306628708486));
#187522=CARTESIAN_POINT('Ctrl Pts',(57.8012193907063,-4.71406478367217,
-54.8923577774473));
#187523=CARTESIAN_POINT('Ctrl Pts',(58.13138502781,-4.82819068711566,-55.3579993904125));
#187524=CARTESIAN_POINT('Ctrl Pts',(57.8239228782473,-4.87294575633325,
-55.2309062620395));
#187525=CARTESIAN_POINT('Ctrl Pts',(57.8247681406176,-4.8789835624615,-54.8952730204543));
#187526=CARTESIAN_POINT('Ctrl Pts',(58.1511322005955,-4.99473857781996,
-55.3594494677196));
#187527=CARTESIAN_POINT('Ctrl Pts',(57.8468132839757,-5.03816723372008,
-55.2311383656919));
#187528=CARTESIAN_POINT('Ctrl Pts',(57.8476108954267,-5.04400181406656,
-54.8980841413334));
#187529=CARTESIAN_POINT('Ctrl Pts',(58.1702690071153,-5.16134039100007,
-55.3608055405081));
#187530=CARTESIAN_POINT('Ctrl Pts',(57.8690388195133,-5.20383266421771,
-55.2313599550618));
#187531=CARTESIAN_POINT('Ctrl Pts',(57.8697476022662,-5.20911947359366,
-54.9007953984755));
#187532=CARTESIAN_POINT('',(57.8697476022662,-5.20911947359366,-54.9007953984755));
#187533=CARTESIAN_POINT('Origin',(58.3653138416346,-5.14268076199931,-54.9007953984755));
#187534=CARTESIAN_POINT('Origin',(1.16314418724182,-12.9460285170553,-46.7095980005158));
#187535=CARTESIAN_POINT('Ctrl Pts',(58.1702690071154,-5.16134039100007,
-55.3608055405082));
#187536=CARTESIAN_POINT('Ctrl Pts',(57.8690388195133,-5.20383266421795,
-55.2313599550619));
#187537=CARTESIAN_POINT('Ctrl Pts',(57.8697476022663,-5.20911947359449,
-54.9007953984755));
#187538=CARTESIAN_POINT('Ctrl Pts',(58.1863681399526,-5.2347113163298,-55.3646554087878));
#187539=CARTESIAN_POINT('Ctrl Pts',(57.8816711167897,-5.29795553030126,
-55.2377699288153));
#187540=CARTESIAN_POINT('Ctrl Pts',(57.8892576239528,-5.35464469293038,
-54.9031849800101));
#187541=CARTESIAN_POINT('Ctrl Pts',(58.206532806921,-5.30826342386473,-55.3884755439432));
#187542=CARTESIAN_POINT('Ctrl Pts',(57.8939857420187,-5.39104663027327,
-55.2713483619941));
#187543=CARTESIAN_POINT('Ctrl Pts',(57.9082088324435,-5.50047055831863,
-54.9417550134773));
#187544=CARTESIAN_POINT('Ctrl Pts',(58.2517768983759,-5.43880935502387,
-55.4693790307482));
#187545=CARTESIAN_POINT('Ctrl Pts',(57.9146461968408,-5.54837256073304,
-55.3788933751119));
#187546=CARTESIAN_POINT('Ctrl Pts',(57.9410017896518,-5.75934555612452,
-55.0773466647676));
#187547=CARTESIAN_POINT('Ctrl Pts',(58.2772082041435,-5.49676306934017,
-55.5268083141558));
#187548=CARTESIAN_POINT('Ctrl Pts',(57.9231956882672,-5.61406051834577,
-55.4547002829484));
#187549=CARTESIAN_POINT('Ctrl Pts',(57.9551095363294,-5.87426883806545,
-55.1748695369358));
#187550=CARTESIAN_POINT('Ctrl Pts',(58.3321412809957,-5.58904289089475,
-55.6647824032721));
#187551=CARTESIAN_POINT('Ctrl Pts',(57.9351757774934,-5.70509939430376,
-55.6270222213536));
#187552=CARTESIAN_POINT('Ctrl Pts',(57.9772132186836,-6.05726143051376,
-55.4055720426652));
#187553=CARTESIAN_POINT('Ctrl Pts',(58.3618432600141,-5.62384585378313,
-55.7455542887996));
#187554=CARTESIAN_POINT('Ctrl Pts',(57.9385982402169,-5.73028333208738,
-55.725786817627));
#187555=CARTESIAN_POINT('Ctrl Pts',(57.9853419314568,-6.12627634754757,
-55.5391049776385));
#187556=CARTESIAN_POINT('Ctrl Pts',(58.4256102669737,-5.66935462867838,
-55.922812372103));
#187557=CARTESIAN_POINT('Ctrl Pts',(57.9401928503808,-5.73799842569994,
-55.9259333604635));
#187558=CARTESIAN_POINT('Ctrl Pts',(57.9959179918116,-6.21652108864807,
-55.822399360329));
#187559=CARTESIAN_POINT('Ctrl Pts',(58.4594118188674,-5.68000001999999,
-56.0184103401194));
#187560=CARTESIAN_POINT('Ctrl Pts',(57.9381116944449,-5.71846326962249,
-56.0282143296095));
#187561=CARTESIAN_POINT('Ctrl Pts',(57.9983536021903,-6.2376310994186,-55.9707502487912));
#187562=CARTESIAN_POINT('Ctrl Pts',(58.4950211556756,-5.68000001999999,
-56.1192785199305));
#187563=CARTESIAN_POINT('Ctrl Pts',(57.9336485918015,-5.68000002,-56.1192785199305));
#187564=CARTESIAN_POINT('Ctrl Pts',(57.9983536018174,-6.23763109620483,
-56.1192785199305));
#187565=CARTESIAN_POINT('',(57.9983536018174,-6.23763109620483,-56.1192785199305));
#187566=CARTESIAN_POINT('Origin',(58.4950211556756,-6.18000001999999,-56.1192785199305));
#187567=CARTESIAN_POINT('Ctrl Pts',(57.9983536018174,-6.23763109620483,
-56.1192785199305));
#187568=CARTESIAN_POINT('Ctrl Pts',(57.9983536018174,-6.23763109620483,
-56.0644455264786));
#187569=CARTESIAN_POINT('Ctrl Pts',(57.9980221190057,-6.23475814249574,
-56.0098560074896));
#187570=CARTESIAN_POINT('Ctrl Pts',(57.9973433490653,-6.22891039019457,
-55.9557040569575));
#187571=CARTESIAN_POINT('Ctrl Pts',(57.9966909788379,-6.22329007722613,
-55.9036582632633));
#187572=CARTESIAN_POINT('Ctrl Pts',(57.9957178277956,-6.21492191913588,
-55.8520157782166));
#187573=CARTESIAN_POINT('Ctrl Pts',(57.9944044945626,-6.20366890587323,
-55.8009488806203));
#187574=CARTESIAN_POINT('Ctrl Pts',(57.9933769792934,-6.1948648623442,-55.7609955651095));
#187575=CARTESIAN_POINT('Ctrl Pts',(57.9921411410287,-6.1842941397813,-55.7213944424274));
#187576=CARTESIAN_POINT('Ctrl Pts',(57.9906851268661,-6.17186945082616,
-55.682233037996));
#187577=CARTESIAN_POINT('Ctrl Pts',(57.9906667712501,-6.17171281579784,
-55.6817393397059));
#187578=CARTESIAN_POINT('Ctrl Pts',(57.9906483809945,-6.17155588913671,
-55.681245721757));
#187579=CARTESIAN_POINT('Ctrl Pts',(57.9906299560812,-6.17139867071413,
-55.6807521844164));
#187580=CARTESIAN_POINT('Ctrl Pts',(57.9875046150389,-6.14473036685059,
-55.5970355082689));
#187581=CARTESIAN_POINT('Ctrl Pts',(57.9833865494891,-6.10971202599363,
-55.5161284707291));
#187582=CARTESIAN_POINT('Ctrl Pts',(57.9782530724075,-6.06658854500581,
-55.4400802261805));
#187583=CARTESIAN_POINT('Ctrl Pts',(57.9747553923278,-6.03720648329143,
-55.3882649700043));
#187584=CARTESIAN_POINT('Ctrl Pts',(57.9707862300964,-6.00406098349663,
-55.3387057443247));
#187585=CARTESIAN_POINT('Ctrl Pts',(57.9663371613776,-5.96722056379155,
-55.2920615727606));
#187586=CARTESIAN_POINT('Ctrl Pts',(57.9662786111709,-5.96673574004027,
-55.2914477306162));
#187587=CARTESIAN_POINT('Ctrl Pts',(57.9662199779913,-5.96625027756548,
-55.2908343949051));
#187588=CARTESIAN_POINT('Ctrl Pts',(57.9661612618222,-5.96576417654625,
-55.290221567164));
#187589=CARTESIAN_POINT('Ctrl Pts',(57.9589421887773,-5.90599871813124,
-55.2148752308583));
#187590=CARTESIAN_POINT('Ctrl Pts',(57.9504117107839,-5.83617450509476,
-55.1470534422411));
#187591=CARTESIAN_POINT('Ctrl Pts',(57.9407769623022,-5.75872949143219,
-55.0901422818071));
#187592=CARTESIAN_POINT('Ctrl Pts',(57.9357443409793,-5.7182768083291,-55.0604152660938));
#187593=CARTESIAN_POINT('Ctrl Pts',(57.9304104809609,-5.6757454289285,-55.0336657755819));
#187594=CARTESIAN_POINT('Ctrl Pts',(57.9248052326105,-5.6314864592146,-55.0103806480697));
#187595=CARTESIAN_POINT('Ctrl Pts',(57.9247386150578,-5.63096044786509,
-55.0101039077518));
#187596=CARTESIAN_POINT('Ctrl Pts',(57.9246719532792,-5.63043414597654,
-55.0098276317697));
#187597=CARTESIAN_POINT('Ctrl Pts',(57.9246052474285,-5.62990755498805,
-55.0095518217286));
#187598=CARTESIAN_POINT('Ctrl Pts',(57.9212703682262,-5.6035812685004,-54.9957630286864));
#187599=CARTESIAN_POINT('Ctrl Pts',(57.9178139721908,-5.57645251025445,
-54.9831217176357));
#187600=CARTESIAN_POINT('Ctrl Pts',(57.9142675773715,-5.54877950578547,
-54.971764271749));
#187601=CARTESIAN_POINT('Ctrl Pts',(57.913512817463,-5.54289001085152,-54.9693471283525));
#187602=CARTESIAN_POINT('Ctrl Pts',(57.9127539957423,-5.53697595914941,
-54.9669879747414));
#187603=CARTESIAN_POINT('Ctrl Pts',(57.91199143806,-5.5310399789474,-54.9646878564231));
#187604=CARTESIAN_POINT('Ctrl Pts',(57.9086784919242,-5.50525100176252,
-54.9546949493021));
#187605=CARTESIAN_POINT('Ctrl Pts',(57.9052948080902,-5.47904671417077,
-54.9458177116981));
#187606=CARTESIAN_POINT('Ctrl Pts',(57.9018664479803,-5.45263506176634,
-54.9381157197596));
#187607=CARTESIAN_POINT('Ctrl Pts',(57.9006211279107,-5.4430412735538,-54.9353180424943));
#187608=CARTESIAN_POINT('Ctrl Pts',(57.8993701409321,-5.43342183598718,
-54.9326755439205));
#187609=CARTESIAN_POINT('Ctrl Pts',(57.8981140995163,-5.42378169739113,
-54.9301886689187));
#187610=CARTESIAN_POINT('Ctrl Pts',(57.8944762323973,-5.39586100721126,
-54.9229859440048));
#187611=CARTESIAN_POINT('Ctrl Pts',(57.8907870927057,-5.36769806591993,
-54.9170666561105));
#187612=CARTESIAN_POINT('Ctrl Pts',(57.8870439982321,-5.33928354730464,
-54.9124555883763));
#187613=CARTESIAN_POINT('Ctrl Pts',(57.8834098871839,-5.31169634191586,
-54.9079787758577));
#187614=CARTESIAN_POINT('Ctrl Pts',(57.8797247293363,-5.28387052582338,
-54.9047349097721));
#187615=CARTESIAN_POINT('Ctrl Pts',(57.8759849933551,-5.25579526938749,
-54.902794710981));
#187616=CARTESIAN_POINT('Ctrl Pts',(57.8739226319616,-5.24031253871396,
-54.9017247447849));
#187617=CARTESIAN_POINT('Ctrl Pts',(57.8718436840546,-5.22475414416982,
-54.9010521259368));
#187618=CARTESIAN_POINT('Ctrl Pts',(57.8697476022663,-5.20911947359449,
-54.9007953984755));
#187619=CARTESIAN_POINT('Origin',(58.4950211556756,-6.18000001999999,-55.24995));
#187620=CARTESIAN_POINT('',(57.9983536018174,-6.23763109620483,-55.24995));
#187621=CARTESIAN_POINT('Origin',(0.,-12.9675000200281,-60.42825533736));
#187622=CARTESIAN_POINT('Origin',(0.,-12.9675000200281,-60.42825533736));
#187623=CARTESIAN_POINT('Origin',(58.8765127194474,-11.83000002,-55.24995));
#187624=CARTESIAN_POINT('',(58.376606009879,-11.839658266657,-56.2580153373943));
#187625=CARTESIAN_POINT('',(58.376606009879,-11.839658266657,-55.24995));
#187626=CARTESIAN_POINT('Origin',(58.8765127194474,-11.83000002,-56.2580153373923));
#187627=CARTESIAN_POINT('Ctrl Pts',(58.9204693868563,-12.3332405111934,
-56.3968205615773));
#187628=CARTESIAN_POINT('Ctrl Pts',(58.3858773874524,-12.3801702023644,
-56.3925855609961));
#187629=CARTESIAN_POINT('Ctrl Pts',(58.3767427611297,-11.8450339177556,
-56.4300980462111));
#187630=CARTESIAN_POINT('Ctrl Pts',(58.8276762845464,-12.3201365847109,
-56.1030402216339));
#187631=CARTESIAN_POINT('Ctrl Pts',(58.3841915353992,-12.2706483349671,
-56.1428486906975));
#187632=CARTESIAN_POINT('Ctrl Pts',(58.3760938044882,-11.8191230277002,
-56.0766739558416));
#187633=CARTESIAN_POINT('Ctrl Pts',(58.7434563338895,-12.3445753573015,
-55.8427359981275));
#187634=CARTESIAN_POINT('Ctrl Pts',(58.3834159308919,-12.231047346678,-55.8250036101692));
#187635=CARTESIAN_POINT('Ctrl Pts',(58.377497118127,-11.8677221198328,-55.6935276731622));
#187636=CARTESIAN_POINT('Ctrl Pts',(58.6765740898316,-12.4686431832956,
-55.6084324108456));
#187637=CARTESIAN_POINT('Ctrl Pts',(58.3844523423634,-12.3662466486663,
-55.5259929392754));
#187638=CARTESIAN_POINT('Ctrl Pts',(58.3812774173441,-12.1139782222975,
-55.3274681950692));
#187639=CARTESIAN_POINT('Ctrl Pts',(58.6664450477116,-12.4930003730007,
-55.5718694403823));
#187640=CARTESIAN_POINT('Ctrl Pts',(58.3846738120602,-12.3941454433015,
-55.4797853161406));
#187641=CARTESIAN_POINT('Ctrl Pts',(58.3819739476742,-12.162324552265,-55.2693146819956));
#187642=CARTESIAN_POINT('Ctrl Pts',(58.6488234778106,-12.5478651152317,
-55.5067647140881));
#187643=CARTESIAN_POINT('Ctrl Pts',(58.3851684019452,-12.4603487355267,
-55.3968754406393));
#187644=CARTESIAN_POINT('Ctrl Pts',(58.3833741817178,-12.2712209921738,
-55.1646750530484));
#187645=CARTESIAN_POINT('Ctrl Pts',(58.6412804318072,-12.5788151444312,
-55.4780148049617));
#187646=CARTESIAN_POINT('Ctrl Pts',(58.3854452700191,-12.4992609451243,
-55.359601343505));
#187647=CARTESIAN_POINT('Ctrl Pts',(58.3840852347027,-12.3326490346772,
-55.1178342268099));
#187648=CARTESIAN_POINT('Ctrl Pts',(58.6189489342569,-12.7021410587872,
-55.3911723350316));
#187649=CARTESIAN_POINT('Ctrl Pts',(58.3864295862247,-12.6569413001418,
-55.2474388094329));
#187650=CARTESIAN_POINT('Ctrl Pts',(58.386474193177,-12.5774201145556,-54.9754185610577));
#187651=CARTESIAN_POINT('Ctrl Pts',(58.6136591241034,-12.8116339481853,
-55.3668837279628));
#187652=CARTESIAN_POINT('Ctrl Pts',(58.3870807295506,-12.8069198757032,
-55.212974677113));
#187653=CARTESIAN_POINT('Ctrl Pts',(58.3876968043474,-12.7947167262509,
-54.9337374850759));
#187654=CARTESIAN_POINT('Ctrl Pts',(58.6208473456642,-12.9180978208483,
-55.3950294078271));
#187655=CARTESIAN_POINT('Ctrl Pts',(58.3871216621357,-12.9488461390236,
-55.2514801948388));
#187656=CARTESIAN_POINT('Ctrl Pts',(58.3874545650717,-13.0060107626915,
-54.9810563880024));
#187657=CARTESIAN_POINT('',(58.3873384184922,-12.8301367871357,-54.9623589764041));
#187658=CARTESIAN_POINT('Origin',(58.8873370347925,-12.8289604802815,-54.9623589764042));
#187659=CARTESIAN_POINT('Ctrl Pts',(58.3873384184922,-12.8301367871357,
-54.9623589764041));
#187660=CARTESIAN_POINT('Ctrl Pts',(58.3871582402025,-12.7535505671015,
-54.962337964741));
#187661=CARTESIAN_POINT('Ctrl Pts',(58.3866696814845,-12.6418858505425,
-54.9772287565121));
#187662=CARTESIAN_POINT('Ctrl Pts',(58.3857822010939,-12.5172370713889,
-55.0207153881268));
#187663=CARTESIAN_POINT('Ctrl Pts',(58.3853403721938,-12.46502197154,-55.0449483819363));
#187664=CARTESIAN_POINT('Ctrl Pts',(58.3850328759368,-12.4304798696505,
-55.0623472369148));
#187665=CARTESIAN_POINT('Ctrl Pts',(58.384863102533,-12.4123661419375,-55.0722395517767));
#187666=CARTESIAN_POINT('Ctrl Pts',(58.3840791937441,-12.3322340243949,
-55.1190986956505));
#187667=CARTESIAN_POINT('Ctrl Pts',(58.3830530216899,-12.2434331788292,
-55.1861910548624));
#187668=CARTESIAN_POINT('Ctrl Pts',(58.3818235406729,-12.1527075458442,
-55.283472900429));
#187669=CARTESIAN_POINT('Ctrl Pts',(58.381213203161,-12.1105634443595,-55.3368656798338));
#187670=CARTESIAN_POINT('Ctrl Pts',(58.380953857786,-12.0931913982438,-55.3607665545691));
#187671=CARTESIAN_POINT('Ctrl Pts',(58.380781592723,-12.0817633019031,-55.376926749946));
#187672=CARTESIAN_POINT('Ctrl Pts',(58.3806842527656,-12.0753758242722,
-55.3862403887367));
#187673=CARTESIAN_POINT('Ctrl Pts',(58.378245228469,-11.9166221344459,-55.6233775609728));
#187674=CARTESIAN_POINT('Ctrl Pts',(58.3766060098791,-11.8396582666571,
-55.9115738855532));
#187675=CARTESIAN_POINT('Ctrl Pts',(58.376606009879,-11.839658266657,-56.2580153373943));
#187676=CARTESIAN_POINT('Ctrl Pts',(58.6177174583935,-12.8294802501408,
-55.3834349955049));
#187677=CARTESIAN_POINT('Ctrl Pts',(58.3873382434228,-12.8300623725117,
-55.2359199480943));
#187678=CARTESIAN_POINT('Ctrl Pts',(58.3873384184922,-12.8301367871357,
-54.9623589764042));
#187679=CARTESIAN_POINT('Ctrl Pts',(58.6180560895148,-12.9967778686933,
-55.3834453150663));
#187680=CARTESIAN_POINT('Ctrl Pts',(58.3877303689834,-12.9966482737698,
-55.2359230050539));
#187681=CARTESIAN_POINT('Ctrl Pts',(58.3877301336919,-12.9966384589807,
-54.9624046566442));
#187682=CARTESIAN_POINT('Ctrl Pts',(58.617779029823,-13.1640733250721,-55.3834369075807));
#187683=CARTESIAN_POINT('Ctrl Pts',(58.3874094466061,-13.1632604597666,
-55.2359205049346));
#187684=CARTESIAN_POINT('Ctrl Pts',(58.3874096419063,-13.1631387418538,
-54.9623672844226));
#187685=CARTESIAN_POINT('Ctrl Pts',(58.6168862797194,-13.3313694061421,
-55.3834096347596));
#187686=CARTESIAN_POINT('Ctrl Pts',(58.3863757263072,-13.3298338968439,
-55.2359124429047));
#187687=CARTESIAN_POINT('Ctrl Pts',(58.3863769436068,-13.3296376352283,
-54.9622468511542));
#187688=CARTESIAN_POINT('',(58.3863769436068,-13.3296376352283,-54.9622468511542));
#187689=CARTESIAN_POINT('Origin',(58.8863673263393,-13.3327387922841,-54.9622468511542));
#187690=CARTESIAN_POINT('Origin',(0.783669006986427,-12.9675005471716,-48.2446834721308));
#187691=CARTESIAN_POINT('Ctrl Pts',(58.6186775397123,-13.2733227804916,
-55.388616176824));
#187692=CARTESIAN_POINT('Ctrl Pts',(58.3866003242463,-13.2520322171712,
-55.2428270583313));
#187693=CARTESIAN_POINT('Ctrl Pts',(58.386962112441,-13.2144813034654,-54.9704131764568));
#187694=CARTESIAN_POINT('Ctrl Pts',(58.6137221237977,-13.3676448320215,
-55.3717404151163));
#187695=CARTESIAN_POINT('Ctrl Pts',(58.3859840071227,-13.3780470899907,
-55.2199040746864));
#187696=CARTESIAN_POINT('Ctrl Pts',(58.3862324741917,-13.4016008615142,
-54.9423444295408));
#187697=CARTESIAN_POINT('Ctrl Pts',(58.6187510133404,-13.4663403062683,
-55.3964780242175));
#187698=CARTESIAN_POINT('Ctrl Pts',(58.3848758374799,-13.5124773652813,
-55.2543020165157));
#187699=CARTESIAN_POINT('Ctrl Pts',(58.3843307468424,-13.5974054698093,
-54.9846201136219));
#187700=CARTESIAN_POINT('Ctrl Pts',(58.6445475220142,-13.6142160529627,
-55.4999871066229));
#187701=CARTESIAN_POINT('Ctrl Pts',(58.3829825750198,-13.7025676579945,
-55.3887162988093));
#187702=CARTESIAN_POINT('Ctrl Pts',(58.3803445916225,-13.8907847695389,
-55.1547197684422));
#187703=CARTESIAN_POINT('Ctrl Pts',(58.661975771747,-13.6701810246484,-55.5666033099607));
#187704=CARTESIAN_POINT('Ctrl Pts',(58.3821783788648,-13.7708664553361,
-55.4756510335785));
#187705=CARTESIAN_POINT('Ctrl Pts',(58.3784002394851,-14.0018188962434,
-55.2630243475737));
#187706=CARTESIAN_POINT('Ctrl Pts',(58.70763761142,-13.7560113852979,-55.728182562924));
#187707=CARTESIAN_POINT('Ctrl Pts',(58.3811768765057,-13.8615861427662,
-55.675458539348));
#187708=CARTESIAN_POINT('Ctrl Pts',(58.3751345491859,-14.1721158329694,
-55.515820517695));
#187709=CARTESIAN_POINT('Ctrl Pts',(58.7355603527933,-13.7855764942266,
-55.8218098030616));
#187710=CARTESIAN_POINT('Ctrl Pts',(58.3810006665601,-13.8831469670814,
-55.7888512930239));
#187711=CARTESIAN_POINT('Ctrl Pts',(58.3738438065525,-14.2307829272749,
-55.6580807676195));
#187712=CARTESIAN_POINT('Ctrl Pts',(58.8069643993684,-13.8272064381204,
-56.0513753893604));
#187713=CARTESIAN_POINT('Ctrl Pts',(58.3813803134092,-13.8862762339219,
-56.0506342944055));
#187714=CARTESIAN_POINT('Ctrl Pts',(58.3720039090521,-14.3134065083042,
-55.9886327543262));
#187715=CARTESIAN_POINT('Ctrl Pts',(58.8522139297507,-13.8331326129651,
-56.1908063572759));
#187716=CARTESIAN_POINT('Ctrl Pts',(58.3821759711571,-13.8532144093832,
-56.2013060500146));
#187717=CARTESIAN_POINT('Ctrl Pts',(58.3717055999094,-14.3251897822734,
-56.1779359856761));
#187718=CARTESIAN_POINT('Ctrl Pts',(58.9012188893463,-13.828579144379,-56.3461607940094));
#187719=CARTESIAN_POINT('Ctrl Pts',(58.3832944048987,-13.7981222944649,
-56.3451627200497));
#187720=CARTESIAN_POINT('Ctrl Pts',(58.3719245331925,-14.3161844310707,
-56.3703692758833));
#187721=CARTESIAN_POINT('',(58.3718694303385,-14.3184313509278,-56.2531111209796));
#187722=CARTESIAN_POINT('Origin',(58.871735578318,-14.33000002,-56.2531111209796));
#187723=CARTESIAN_POINT('Ctrl Pts',(58.3718694303385,-14.3184313509278,
-56.2531111209796));
#187724=CARTESIAN_POINT('Ctrl Pts',(58.3718694303385,-14.3184313509278,
-56.1315282681123));
#187725=CARTESIAN_POINT('Ctrl Pts',(58.3720934589562,-14.3089057630787,
-56.0113829394871));
#187726=CARTESIAN_POINT('Ctrl Pts',(58.372602521148,-14.2863749805017,-55.8932001781189));
#187727=CARTESIAN_POINT('Ctrl Pts',(58.3727280602367,-14.2808186968923,
-55.8640552987669));
#187728=CARTESIAN_POINT('Ctrl Pts',(58.3728706983335,-14.274471486997,-55.8350297744669));
#187729=CARTESIAN_POINT('Ctrl Pts',(58.3730308041295,-14.2672811529287,
-55.8061314796515));
#187730=CARTESIAN_POINT('Ctrl Pts',(58.3735850259137,-14.2423911122432,
-55.7060972215946));
#187731=CARTESIAN_POINT('Ctrl Pts',(58.3743558983076,-14.2072301125135,
-55.6079785795892));
#187732=CARTESIAN_POINT('Ctrl Pts',(58.3753143408088,-14.1603251811705,
-55.5154726363337));
#187733=CARTESIAN_POINT('Ctrl Pts',(58.3757555226855,-14.138734313063,-55.4728911089164));
#187734=CARTESIAN_POINT('Ctrl Pts',(58.3762357928548,-14.114655053344,-55.431498836353));
#187735=CARTESIAN_POINT('Ctrl Pts',(58.3767484727564,-14.0879436829683,
-55.3916564088811));
#187736=CARTESIAN_POINT('Ctrl Pts',(58.3783749205468,-14.0032033816892,
-55.2652585767906));
#187737=CARTESIAN_POINT('Ctrl Pts',(58.3803191831255,-13.8924014500595,
-55.1564962213834));
#187738=CARTESIAN_POINT('Ctrl Pts',(58.382091437956,-13.7622047346492,-55.0806296262956));
#187739=CARTESIAN_POINT('Ctrl Pts',(58.3829775653712,-13.6971063769441,
-55.0426963287517));
#187740=CARTESIAN_POINT('Ctrl Pts',(58.3838281227637,-13.6263468744968,
-55.0125723550395));
#187741=CARTESIAN_POINT('Ctrl Pts',(58.3845593996408,-13.5534863365101,
-54.9925162587396));
#187742=CARTESIAN_POINT('Ctrl Pts',(58.385290676518,-13.4806257985234,-54.9724601624396));
#187743=CARTESIAN_POINT('Ctrl Pts',(58.3859030562338,-13.4060410952294,
-54.9621915864083));
#187744=CARTESIAN_POINT('Ctrl Pts',(58.3863769436069,-13.3296376352283,
-54.9622468511542));
#187745=CARTESIAN_POINT('Origin',(58.871735578318,-14.33000002,-55.24995));
#187746=CARTESIAN_POINT('',(58.3718694303385,-14.3184313509278,-55.24995));
#187747=CARTESIAN_POINT('Origin',(0.,-12.9675000200281,-60.42825533736));
#187748=CARTESIAN_POINT('Origin',(0.,-12.9675000200281,-60.42825533736));
#187749=CARTESIAN_POINT('Origin',(58.4684744114614,-19.98000002,-55.24995));
#187750=CARTESIAN_POINT('',(57.9720322598041,-19.92045852138,-56.1088024963483));
#187751=CARTESIAN_POINT('',(57.9720322598041,-19.92045852138,-55.24995));
#187752=CARTESIAN_POINT('Origin',(58.4684744114614,-19.98000002,-56.108802496345));
#187753=CARTESIAN_POINT('Ctrl Pts',(58.4684744114589,-20.48000002,-56.1088024963516));
#187754=CARTESIAN_POINT('Ctrl Pts',(57.9049228508699,-20.4800000199972,
-56.108802496352));
#187755=CARTESIAN_POINT('Ctrl Pts',(57.9720322598041,-19.92045852138,-56.1088024963483));
#187756=CARTESIAN_POINT('Ctrl Pts',(58.4330292345976,-20.4800000200005,
-56.0085121468718));
#187757=CARTESIAN_POINT('Ctrl Pts',(57.9095337666328,-20.4415553517815,
-56.0186397573414));
#187758=CARTESIAN_POINT('Ctrl Pts',(57.972032259745,-19.920458521873,-55.9596727479179));
#187759=CARTESIAN_POINT('Ctrl Pts',(58.4001436082512,-20.4906502319919,
-55.9155728413271));
#187760=CARTESIAN_POINT('Ctrl Pts',(57.9116095949012,-20.4226888878798,
-55.9192309942947));
#187761=CARTESIAN_POINT('Ctrl Pts',(57.9695132223445,-19.9415780781022,
-55.8143395431684));
#187762=CARTESIAN_POINT('Ctrl Pts',(58.336964041887,-20.5362234599901,-55.7404218332007));
#187763=CARTESIAN_POINT('Ctrl Pts',(57.9099756200818,-20.4304312900862,
-55.7217019778744));
#187764=CARTESIAN_POINT('Ctrl Pts',(57.9585693859923,-20.0319506515215,
-55.5325899309841));
#187765=CARTESIAN_POINT('Ctrl Pts',(58.3075894202415,-20.5708407676795,
-55.6609201576627));
#187766=CARTESIAN_POINT('Ctrl Pts',(57.9064908388997,-20.4553081180622,
-55.624563633487));
#187767=CARTESIAN_POINT('Ctrl Pts',(57.9502161720285,-20.1005973934661,
-55.4004673410398));
#187768=CARTESIAN_POINT('Ctrl Pts',(58.2664303444063,-20.6399469122455,
-55.5584001983321));
#187769=CARTESIAN_POINT('Ctrl Pts',(57.8972223460235,-20.5236291209351,
-55.4954672167701));
#187770=CARTESIAN_POINT('Ctrl Pts',(57.9331286547812,-20.2376361665866,
-55.2282616560402));
#187771=CARTESIAN_POINT('Ctrl Pts',(58.252990069642,-20.6662757908246,-55.526584865508));
#187772=CARTESIAN_POINT('Ctrl Pts',(57.8934574975699,-20.5515587218466,
-55.4548005580757));
#187773=CARTESIAN_POINT('Ctrl Pts',(57.9265619920107,-20.2898468150981,
-55.1744487967193));
#187774=CARTESIAN_POINT('Ctrl Pts',(58.2277581334007,-20.7227877352239,
-55.4712423952938));
#187775=CARTESIAN_POINT('Ctrl Pts',(57.8849360912282,-20.614784763174,-55.3832820627753));
#187776=CARTESIAN_POINT('Ctrl Pts',(57.9122860844342,-20.4019110441904,
-55.0807659948788));
#187777=CARTESIAN_POINT('Ctrl Pts',(58.2157933021909,-20.7532073937065,
-55.4472489303381));
#187778=CARTESIAN_POINT('Ctrl Pts',(57.8801540568373,-20.6502674204662,
-55.3516348732274));
#187779=CARTESIAN_POINT('Ctrl Pts',(57.9045197753069,-20.4622337862451,
-55.0401096877444));
#187780=CARTESIAN_POINT('Ctrl Pts',(58.1812959053717,-20.8514432878938,
-55.3865915677339));
#187781=CARTESIAN_POINT('Ctrl Pts',(57.8642971460945,-20.7674694003889,
-55.2713260639177));
#187782=CARTESIAN_POINT('Ctrl Pts',(57.8790836561167,-20.6570373864694,
-54.9381051588475));
#187783=CARTESIAN_POINT('Ctrl Pts',(58.1608566910152,-20.9243786591062,
-55.3628734830557));
#187784=CARTESIAN_POINT('Ctrl Pts',(57.851773276413,-20.8594120817092,-55.2377696368355));
#187785=CARTESIAN_POINT('Ctrl Pts',(57.8597273248566,-20.8016654950799,
-54.8995711242948));
#187786=CARTESIAN_POINT('Ctrl Pts',(58.1440639002148,-20.9985364556096,
-55.3589167601806));
#187787=CARTESIAN_POINT('Ctrl Pts',(57.838673217243,-20.9542432701794,-55.2310547627909));
#187788=CARTESIAN_POINT('Ctrl Pts',(57.8394345625603,-20.9487258492222,
-54.8970741880307));
#187789=CARTESIAN_POINT('',(57.8394345625603,-20.9487258492221,-54.8970741880307));
#187790=CARTESIAN_POINT('Origin',(58.3347412169172,-21.017072891219,-54.8970741880307));
#187791=CARTESIAN_POINT('Ctrl Pts',(57.8394345625603,-20.9487258492221,
-54.8970741880307));
#187792=CARTESIAN_POINT('Ctrl Pts',(57.8483315717593,-20.8842497909848,
-54.8981689263708));
#187793=CARTESIAN_POINT('Ctrl Pts',(57.8570330166362,-20.8203546606247,
-54.9061845094689));
#187794=CARTESIAN_POINT('Ctrl Pts',(57.8654251279068,-20.7580154570746,
-54.9205228428019));
#187795=CARTESIAN_POINT('Ctrl Pts',(57.8742541462857,-20.6924307721091,
-54.9356076533388));
#187796=CARTESIAN_POINT('Ctrl Pts',(57.8827409478669,-20.6285669203539,
-54.9576909614068));
#187797=CARTESIAN_POINT('Ctrl Pts',(57.8907523071727,-20.5675574167704,
-54.9861327822005));
#187798=CARTESIAN_POINT('Ctrl Pts',(57.8925393734123,-20.5539482376052,
-54.9924772008932));
#187799=CARTESIAN_POINT('Ctrl Pts',(57.8943027736333,-20.5404811271438,
-54.9991382130752));
#187800=CARTESIAN_POINT('Ctrl Pts',(57.8960410108923,-20.5271687639928,
-55.0061090485496));
#187801=CARTESIAN_POINT('Ctrl Pts',(57.8961104580828,-20.5266368997638,
-55.0063875519222));
#187802=CARTESIAN_POINT('Ctrl Pts',(57.8961798575478,-20.5261053444105,
-55.0066665020562));
#187803=CARTESIAN_POINT('Ctrl Pts',(57.8962492093382,-20.5255740977204,
-55.0069458987164));
#187804=CARTESIAN_POINT('Ctrl Pts',(57.9046540977693,-20.4611912009517,
-55.0408065639478));
#187805=CARTESIAN_POINT('Ctrl Pts',(57.9123517927205,-20.4013952311835,
-55.0812026657775));
#187806=CARTESIAN_POINT('Ctrl Pts',(57.9194238609353,-20.3458803213664,
-55.1276091020937));
#187807=CARTESIAN_POINT('Ctrl Pts',(57.9194970031007,-20.3453061639072,
-55.1280890560674));
#187808=CARTESIAN_POINT('Ctrl Pts',(57.9195700843622,-20.3447324149112,
-55.1285697353016));
#187809=CARTESIAN_POINT('Ctrl Pts',(57.9196431043984,-20.3441590772921,
-55.1290511360631));
#187810=CARTESIAN_POINT('Ctrl Pts',(57.9261585705981,-20.2930010380225,
-55.1720057900754));
#187811=CARTESIAN_POINT('Ctrl Pts',(57.9321919519941,-20.2450759632038,
-55.2207529417662));
#187812=CARTESIAN_POINT('Ctrl Pts',(57.9375117382139,-20.2024766659963,
-55.2726481082499));
#187813=CARTESIAN_POINT('Ctrl Pts',(57.9379542983799,-20.1989327732039,
-55.2769653369019));
#187814=CARTESIAN_POINT('Ctrl Pts',(57.9383919237743,-20.1954257087606,
-55.2813043482889));
#187815=CARTESIAN_POINT('Ctrl Pts',(57.938824483381,-20.1919566596153,-55.2856636195628));
#187816=CARTESIAN_POINT('Ctrl Pts',(57.938884960972,-20.1914716403672,-55.2862731037146));
#187817=CARTESIAN_POINT('Ctrl Pts',(57.9389453520762,-20.1909872680675,
-55.2868830674044));
#187818=CARTESIAN_POINT('Ctrl Pts',(57.9390056567172,-20.1905035428319,
-55.2874935092313));
#187819=CARTESIAN_POINT('Ctrl Pts',(57.9476291333811,-20.121331532001,-55.3747858097982));
#187820=CARTESIAN_POINT('Ctrl Pts',(57.9544934737034,-20.0653204626869,
-55.4719393844623));
#187821=CARTESIAN_POINT('Ctrl Pts',(57.9596779034763,-20.022713941091,-55.5751875387868));
#187822=CARTESIAN_POINT('Ctrl Pts',(57.9612949610576,-20.0094246881208,
-55.6073913139397));
#187823=CARTESIAN_POINT('Ctrl Pts',(57.9627485647956,-19.997439611234,-55.640188380711));
#187824=CARTESIAN_POINT('Ctrl Pts',(57.964041058706,-19.9867663918423,-55.6734654024398));
#187825=CARTESIAN_POINT('Ctrl Pts',(57.9640600250566,-19.9866097705855,
-55.6739537170499));
#187826=CARTESIAN_POINT('Ctrl Pts',(57.9640789558543,-19.9864534391018,
-55.6744420834266));
#187827=CARTESIAN_POINT('Ctrl Pts',(57.964097851118,-19.9862973972617,-55.6749305015429));
#187828=CARTESIAN_POINT('Ctrl Pts',(57.9681300897667,-19.9529981564453,
-55.7791586525505));
#187829=CARTESIAN_POINT('Ctrl Pts',(57.9705461679584,-19.9328724060776,
-55.885764707647));
#187830=CARTESIAN_POINT('Ctrl Pts',(57.9715251367094,-19.9246984926926,
-55.9945278474385));
#187831=CARTESIAN_POINT('Ctrl Pts',(57.9718656735483,-19.9218551755562,
-56.0323613899058));
#187832=CARTESIAN_POINT('Ctrl Pts',(57.9720322597889,-19.9204585215068,
-56.0704559927497));
#187833=CARTESIAN_POINT('Ctrl Pts',(57.9720322598041,-19.92045852138,-56.1088024963483));
#187834=CARTESIAN_POINT('Ctrl Pts',(58.1440639002148,-20.9985364556095,
-55.3589167601806));
#187835=CARTESIAN_POINT('Ctrl Pts',(57.8386732172432,-20.9542432701794,
-55.231054762791));
#187836=CARTESIAN_POINT('Ctrl Pts',(57.8394345625603,-20.9487258492223,
-54.8970741880307));
#187837=CARTESIAN_POINT('Ctrl Pts',(58.124377168252,-21.1650956023415,-55.357473843553));
#187838=CARTESIAN_POINT('Ctrl Pts',(57.8158059697175,-21.1198442176536,
-55.2308230742677));
#187839=CARTESIAN_POINT('Ctrl Pts',(57.8166617235658,-21.1137591610236,
-54.8942721021231));
#187840=CARTESIAN_POINT('Ctrl Pts',(58.1040803997663,-21.3315995267041,
-55.3559321998119));
#187841=CARTESIAN_POINT('Ctrl Pts',(57.7922771725925,-21.2849855841189,
-55.2305804544121));
#187842=CARTESIAN_POINT('Ctrl Pts',(57.7931832180155,-21.2786902591483,
-54.8913683748515));
#187843=CARTESIAN_POINT('Ctrl Pts',(58.0831736437665,-21.4980516416408,
-55.3542805420642));
#187844=CARTESIAN_POINT('Ctrl Pts',(57.7681097820422,-21.4495803068845,
-55.2303260732311));
#187845=CARTESIAN_POINT('Ctrl Pts',(57.7689991024637,-21.4435190710235,
-54.8883584020537));
#187846=CARTESIAN_POINT('',(57.7689991024637,-21.4435190710235,-54.8883584020537));
#187847=CARTESIAN_POINT('Origin',(58.2637025843942,-21.516103263282,-54.8883584020538));
#187848=CARTESIAN_POINT('Origin',(1.20679687888321,-12.9924344910764,-46.5556728739474));
#187849=CARTESIAN_POINT('Ctrl Pts',(58.0831736437665,-21.4980516416407,
-55.3542805420643));
#187850=CARTESIAN_POINT('Ctrl Pts',(57.7681097820422,-21.4495803068843,
-55.2303260732311));
#187851=CARTESIAN_POINT('Ctrl Pts',(57.7689991024638,-21.4435190710229,
-54.8883584020538));
#187852=CARTESIAN_POINT('Ctrl Pts',(58.0674311963076,-21.5630475770342,
-55.3506990738629));
#187853=CARTESIAN_POINT('Ctrl Pts',(57.7561082976292,-21.5312836766001,
-55.2240269539558));
#187854=CARTESIAN_POINT('Ctrl Pts',(57.7500908600563,-21.5723897392102,
-54.8860050875463));
#187855=CARTESIAN_POINT('Ctrl Pts',(58.0543804972822,-21.6287810566872,
-55.3623310903062));
#187856=CARTESIAN_POINT('Ctrl Pts',(57.7435735661121,-21.6157110452939,
-55.2378962877635));
#187857=CARTESIAN_POINT('Ctrl Pts',(57.7304928612488,-21.702757912867,-54.9116382623115));
#187858=CARTESIAN_POINT('Ctrl Pts',(58.0368385085867,-21.7483268550824,
-55.4143541528288));
#187859=CARTESIAN_POINT('Ctrl Pts',(57.720944678806,-21.7667785312353,-55.3041336540307));
#187860=CARTESIAN_POINT('Ctrl Pts',(57.6941246628956,-21.9398194436421,
-55.0150801896028));
#187861=CARTESIAN_POINT('Ctrl Pts',(58.0322828839583,-21.8027029130102,
-55.4549704742887));
#187862=CARTESIAN_POINT('Ctrl Pts',(57.7106605173207,-21.8347350541072,
-55.3571283178239));
#187863=CARTESIAN_POINT('Ctrl Pts',(57.6771952780886,-22.0476481665544,
-55.0933432841215));
#187864=CARTESIAN_POINT('Ctrl Pts',(58.0344578164564,-21.8906114651791,
-55.5576238485917));
#187865=CARTESIAN_POINT('Ctrl Pts',(57.695076042676,-21.9376161761805,-55.488705776954));
#187866=CARTESIAN_POINT('Ctrl Pts',(57.6494812249724,-22.2219724523816,
-55.2860232465006));
#187867=CARTESIAN_POINT('Ctrl Pts',(58.0412481050148,-21.9247947465257,
-55.6203478572209));
#187868=CARTESIAN_POINT('Ctrl Pts',(57.689647002784,-21.9734580917706,-55.5692031110363));
#187869=CARTESIAN_POINT('Ctrl Pts',(57.6385084201743,-22.2897585279143,
-55.4017143890713));
#187870=CARTESIAN_POINT('Ctrl Pts',(58.0678405993018,-21.9693186886025,
-55.7585030512593));
#187871=CARTESIAN_POINT('Ctrl Pts',(57.6849292160892,-22.0058199931385,
-55.7382976471412));
#187872=CARTESIAN_POINT('Ctrl Pts',(57.6241589914286,-22.3780503291714,
-55.6490268368888));
#187873=CARTESIAN_POINT('Ctrl Pts',(58.0878569699436,-21.9800000199996,
-55.8347456438184));
#187874=CARTESIAN_POINT('Ctrl Pts',(57.6857286259381,-22.0018252542719,
-55.8292768225565));
#187875=CARTESIAN_POINT('Ctrl Pts',(57.6206785404325,-22.3992316104322,
-55.7821117710573));
#187876=CARTESIAN_POINT('Ctrl Pts',(58.1141118834632,-21.98000002,-55.9136064684135));
#187877=CARTESIAN_POINT('Ctrl Pts',(57.6893011240825,-21.9800000200013,
-55.9136064684131));
#187878=CARTESIAN_POINT('Ctrl Pts',(57.6206785412152,-22.3992316056509,
-55.9136064684106));
#187879=CARTESIAN_POINT('',(57.6206785412152,-22.3992316056509,-55.9136064684106));
#187880=CARTESIAN_POINT('Origin',(58.1141118834647,-22.48000002,-55.9136064684106));
#187881=CARTESIAN_POINT('Ctrl Pts',(57.6206785412152,-22.3992316056509,
-55.9136064684106));
#187882=CARTESIAN_POINT('Ctrl Pts',(57.6206785412152,-22.3992316056506,
-55.8712576139305));
#187883=CARTESIAN_POINT('Ctrl Pts',(57.6210388568449,-22.3970387396972,
-55.8289927265007));
#187884=CARTESIAN_POINT('Ctrl Pts',(57.6217580713774,-22.3926459443346,
-55.7870504595467));
#187885=CARTESIAN_POINT('Ctrl Pts',(57.6224751991257,-22.3882658945648,
-55.7452298870977));
#187886=CARTESIAN_POINT('Ctrl Pts',(57.6235491311395,-22.3816988155787,
-55.7037286574053));
#187887=CARTESIAN_POINT('Ctrl Pts',(57.6249866999783,-22.3728877575665,
-55.6627754268272));
#187888=CARTESIAN_POINT('Ctrl Pts',(57.6263702144474,-22.364408006253,-55.6233620884624));
#187889=CARTESIAN_POINT('Ctrl Pts',(57.6280905589435,-22.353849749917,-55.5844551760951));
#187890=CARTESIAN_POINT('Ctrl Pts',(57.6301613121382,-22.341116023378,-55.5462695907389));
#187891=CARTESIAN_POINT('Ctrl Pts',(57.6305151022056,-22.3389404546126,
-55.5397455487364));
#187892=CARTESIAN_POINT('Ctrl Pts',(57.6308791385552,-22.3367012727077,
-55.533242612179));
#187893=CARTESIAN_POINT('Ctrl Pts',(57.6312535111585,-22.3343978551758,
-55.5267619228708));
#187894=CARTESIAN_POINT('Ctrl Pts',(57.631280295686,-22.3342330569249,-55.5262982612688));
#187895=CARTESIAN_POINT('Ctrl Pts',(57.6313071321696,-22.3340679357285,
-55.525834729741));
#187896=CARTESIAN_POINT('Ctrl Pts',(57.6313340206222,-22.3339024914829,
-55.525371328865));
#187897=CARTESIAN_POINT('Ctrl Pts',(57.6359864322556,-22.305276272468,-55.4451907525303));
#187898=CARTESIAN_POINT('Ctrl Pts',(57.6422382498633,-22.2666955115386,
-55.3683025756002));
#187899=CARTESIAN_POINT('Ctrl Pts',(57.6498495152222,-22.2192637924304,
-55.2978189119911));
#187900=CARTESIAN_POINT('Ctrl Pts',(57.6538973328718,-22.1940386898093,
-55.2603343408838));
#187901=CARTESIAN_POINT('Ctrl Pts',(57.6583296672911,-22.166310049833,-55.2246619070089));
#187902=CARTESIAN_POINT('Ctrl Pts',(57.6631104665851,-22.1362429894798,
-55.1912758544359));
#187903=CARTESIAN_POINT('Ctrl Pts',(57.6631864482776,-22.1357651308643,
-55.1907452467652));
#187904=CARTESIAN_POINT('Ctrl Pts',(57.663262518071,-22.1352866810589,-55.1902152153126));
#187905=CARTESIAN_POINT('Ctrl Pts',(57.6633386758179,-22.1348076407421,
-55.1896857620266));
#187906=CARTESIAN_POINT('Ctrl Pts',(57.6719065247416,-22.0809149610449,
-55.1301215555118));
#187907=CARTESIAN_POINT('Ctrl Pts',(57.6816602960296,-22.0190502353779,
-55.0773873317807));
#187908=CARTESIAN_POINT('Ctrl Pts',(57.6921719467781,-21.9515533423725,
-55.0335672587661));
#187909=CARTESIAN_POINT('Ctrl Pts',(57.6985643073562,-21.9105070321098,
-55.0069193312453));
#187910=CARTESIAN_POINT('Ctrl Pts',(57.705236739167,-21.867379079,-54.9835681411996));
#187911=CARTESIAN_POINT('Ctrl Pts',(57.7120915003347,-21.8227047516213,
-54.9639818384176));
#187912=CARTESIAN_POINT('Ctrl Pts',(57.7121639633474,-21.8222324906232,
-54.9637747878039));
#187913=CARTESIAN_POINT('Ctrl Pts',(57.7122364434107,-21.8217600784835,
-54.9635681670512));
#187914=CARTESIAN_POINT('Ctrl Pts',(57.7123089404443,-21.8212875156173,
-54.9633619764799));
#187915=CARTESIAN_POINT('Ctrl Pts',(57.7175256896612,-21.7872827868695,
-54.9485248935223));
#187916=CARTESIAN_POINT('Ctrl Pts',(57.7228431420999,-21.7524063113003,
-54.935873883604));
#187917=CARTESIAN_POINT('Ctrl Pts',(57.7282261110468,-21.716879990905,-54.9253981395351));
#187918=CARTESIAN_POINT('Ctrl Pts',(57.7336334907217,-21.6811925654856,
-54.9148748899834));
#187919=CARTESIAN_POINT('Ctrl Pts',(57.7391071704681,-21.6448481995524,
-54.9065464760172));
#187920=CARTESIAN_POINT('Ctrl Pts',(57.7446130540746,-21.6080564477772,
-54.9004521188838));
#187921=CARTESIAN_POINT('Ctrl Pts',(57.7499689591833,-21.5722668914811,
-54.8945237700776));
#187922=CARTESIAN_POINT('Ctrl Pts',(57.7553555069844,-21.5360528976765,
-54.8907094534876));
#187923=CARTESIAN_POINT('Ctrl Pts',(57.7607401663574,-21.49960966879,-54.8890935200766));
#187924=CARTESIAN_POINT('Ctrl Pts',(57.7634952382929,-21.4809634165034,
-54.8882667244556));
#187925=CARTESIAN_POINT('Ctrl Pts',(57.7662497818651,-21.4622572897838,
-54.8880162223889));
#187926=CARTESIAN_POINT('Ctrl Pts',(57.7689991024637,-21.4435190710235,
-54.8883584020538));
#187927=CARTESIAN_POINT('Origin',(58.1141118834647,-22.48000002,-55.24995));
#187928=CARTESIAN_POINT('',(57.6206785412152,-22.3992316056509,-55.24995));
#187929=CARTESIAN_POINT('Origin',(0.,-12.9675000200281,-60.42825533736));
#187930=CARTESIAN_POINT('Origin',(0.,-12.9675000200281,-60.42825533736));
#187931=CARTESIAN_POINT('Origin',(56.9019881023868,-28.13000002,-55.24995));
#187932=CARTESIAN_POINT('',(56.418846619879,-28.0012587761031,-55.74995));
#187933=CARTESIAN_POINT('',(56.418846619879,-28.0012587761031,-55.24995));
#187934=CARTESIAN_POINT('Origin',(56.9019881023868,-28.13000002,-55.74995));
#187935=CARTESIAN_POINT('Ctrl Pts',(56.9019881023868,-28.63000002,-55.74995));
#187936=CARTESIAN_POINT('Ctrl Pts',(56.2513078496445,-28.6300000199999,
-55.74995));
#187937=CARTESIAN_POINT('Ctrl Pts',(56.418846619879,-28.0012587761031,-55.74995));
#187938=CARTESIAN_POINT('Ctrl Pts',(56.9019880961229,-28.63000002,-55.6833917541491));
#187939=CARTESIAN_POINT('Ctrl Pts',(56.2513078484208,-28.6300000235388,
-55.7066092661189));
#187940=CARTESIAN_POINT('Ctrl Pts',(56.4188466136678,-28.0012587994123,
-55.6168335059946));
#187941=CARTESIAN_POINT('Ctrl Pts',(56.8947679354133,-28.6435819282218,
-55.6165654527396));
#187942=CARTESIAN_POINT('Ctrl Pts',(56.2500205046201,-28.6336048267405,
-55.662915181482));
#187943=CARTESIAN_POINT('Ctrl Pts',(56.4116877572674,-28.0281919581543,
-55.4831809085995));
#187944=CARTESIAN_POINT('Ctrl Pts',(56.8671374536179,-28.6951410554417,
-55.4944276362032));
#187945=CARTESIAN_POINT('Ctrl Pts',(56.2435792593614,-28.6535512137473,
-55.5706051556274));
#187946=CARTESIAN_POINT('Ctrl Pts',(56.3842918802123,-28.1304346451459,
-55.2389052692862));
#187947=CARTESIAN_POINT('Ctrl Pts',(56.8466599215264,-28.733218160043,-55.438805637664));
#187948=CARTESIAN_POINT('Ctrl Pts',(56.2384193392041,-28.6700167701719,
-55.5221237308774));
#187949=CARTESIAN_POINT('Ctrl Pts',(56.3639882171558,-28.2059422564823,
-55.1276612780425));
#187950=CARTESIAN_POINT('Ctrl Pts',(56.7960439448031,-28.8262229205127,
-55.3474998385745));
#187951=CARTESIAN_POINT('Ctrl Pts',(56.2221065093684,-28.7248002564605,
-55.4263976661905));
#187952=CARTESIAN_POINT('Ctrl Pts',(56.313802009893,-28.3903724090483,-54.9450496744345));
#187953=CARTESIAN_POINT('Ctrl Pts',(56.7654715266632,-28.8819195410099,
-55.3110999839041));
#187954=CARTESIAN_POINT('Ctrl Pts',(56.2109691262328,-28.7630648267862,
-55.3789982403422));
#187955=CARTESIAN_POINT('Ctrl Pts',(56.2834891741183,-28.5008198383441,
-54.8722499675113));
#187956=CARTESIAN_POINT('Ctrl Pts',(56.6991996177705,-29.0010091208419,
-55.2626158142325));
#187957=CARTESIAN_POINT('Ctrl Pts',(56.1824656282838,-28.8623399510796,
-55.300226361809));
#187958=CARTESIAN_POINT('Ctrl Pts',(56.2177799652687,-28.7369766748766,
-54.7752816287617));
#187959=CARTESIAN_POINT('Ctrl Pts',(56.6626879858136,-29.0658450537332,
-55.24995));
#187960=CARTESIAN_POINT('Ctrl Pts',(56.1650303807126,-28.9235240815735,
-55.2679072059029));
#187961=CARTESIAN_POINT('Ctrl Pts',(56.1815764992065,-28.8655539935311,
-54.749950013458));
#187962=CARTESIAN_POINT('Ctrl Pts',(56.6260651114328,-29.1300000200001,
-55.24995));
#187963=CARTESIAN_POINT('Ctrl Pts',(56.1452664265556,-28.9927680098115,
-55.24995));
#187964=CARTESIAN_POINT('Ctrl Pts',(56.1452664265556,-28.9927680098115,
-54.74995));
#187965=CARTESIAN_POINT('',(56.1452664265556,-28.9927680098114,-54.74995));
#187966=CARTESIAN_POINT('Ctrl Pts',(56.1452664265556,-28.9927680098114,
-54.74995));
#187967=CARTESIAN_POINT('Ctrl Pts',(56.157135481805,-28.951184226649,-54.7499500043992));
#187968=CARTESIAN_POINT('Ctrl Pts',(56.168934149989,-28.9096618081524,-54.7526528441348));
#187969=CARTESIAN_POINT('Ctrl Pts',(56.1805785937552,-28.8685154650404,
-54.7579280669059));
#187970=CARTESIAN_POINT('Ctrl Pts',(56.1927137076009,-28.825635309661,-54.7634255754322));
#187971=CARTESIAN_POINT('Ctrl Pts',(56.204681702463,-28.7831622366754,-54.7717167436038));
#187972=CARTESIAN_POINT('Ctrl Pts',(56.2163892898622,-28.7414427179697,
-54.7827110993106));
#187973=CARTESIAN_POINT('Ctrl Pts',(56.2280968772615,-28.699723199264,-54.7937054550173));
#187974=CARTESIAN_POINT('Ctrl Pts',(56.239544464813,-28.6587557436148,-54.8074032739245));
#187975=CARTESIAN_POINT('Ctrl Pts',(56.2506343384323,-28.6188990877768,
-54.8237679977477));
#187976=CARTESIAN_POINT('Ctrl Pts',(56.2507584702878,-28.618452961805,-54.823951172381));
#187977=CARTESIAN_POINT('Ctrl Pts',(56.2508825687622,-28.618006934334,-54.8241346982876));
#187978=CARTESIAN_POINT('Ctrl Pts',(56.2510066337442,-28.6175610058129,
-54.824318575259));
#187979=CARTESIAN_POINT('Ctrl Pts',(56.2715808747849,-28.543610720002,-54.8548117012852));
#187980=CARTESIAN_POINT('Ctrl Pts',(56.2911418613678,-28.4727130044645,
-54.8948321838621));
#187981=CARTESIAN_POINT('Ctrl Pts',(56.3090294712616,-28.4074824207886,
-54.9428936399917));
#187982=CARTESIAN_POINT('Ctrl Pts',(56.3196152133162,-28.3688794918917,
-54.9713360188438));
#187983=CARTESIAN_POINT('Ctrl Pts',(56.3296151020253,-28.3322606012602,
-55.0025940679603));
#187984=CARTESIAN_POINT('Ctrl Pts',(56.3388945722868,-28.2981593218029,
-55.0363576523063));
#187985=CARTESIAN_POINT('Ctrl Pts',(56.339029993733,-28.2976616592801,-55.036850386621));
#187986=CARTESIAN_POINT('Ctrl Pts',(56.3391652743153,-28.297164488402,-55.0373436962489));
#187987=CARTESIAN_POINT('Ctrl Pts',(56.3393004137533,-28.2966678103585,
-55.037837579714));
#187988=CARTESIAN_POINT('Ctrl Pts',(56.3561267590158,-28.2348259352745,
-55.0993314990782));
#187989=CARTESIAN_POINT('Ctrl Pts',(56.3707655818743,-28.1806225233929,
-55.1697303039634));
#187990=CARTESIAN_POINT('Ctrl Pts',(56.3826877315525,-28.1363072821715,
-55.2462670316364));
#187991=CARTESIAN_POINT('Ctrl Pts',(56.3884405285137,-28.1149238411049,
-55.2831983121737));
#187992=CARTESIAN_POINT('Ctrl Pts',(56.3935608278327,-28.0958424992937,
-55.3215595430154));
#187993=CARTESIAN_POINT('Ctrl Pts',(56.397989272594,-28.0793153399122,-55.3610440111482));
#187994=CARTESIAN_POINT('Ctrl Pts',(56.3980423761537,-28.0791171549869,
-55.3615174879381));
#187995=CARTESIAN_POINT('Ctrl Pts',(56.3980953812291,-28.0789193343635,
-55.3619911356046));
#187996=CARTESIAN_POINT('Ctrl Pts',(56.3981482877874,-28.0787218781893,
-55.3624649534454));
#187997=CARTESIAN_POINT('Ctrl Pts',(56.4020846045284,-28.0640308820639,
-55.3977176169507));
#187998=CARTESIAN_POINT('Ctrl Pts',(56.4054635861547,-28.0514021107091,
-55.4337954284409));
#187999=CARTESIAN_POINT('Ctrl Pts',(56.4082873243379,-28.0408381674741,
-55.4705044074015));
#188000=CARTESIAN_POINT('Ctrl Pts',(56.4111187646799,-28.030245409539,-55.5073135154709));
#188001=CARTESIAN_POINT('Ctrl Pts',(56.4133919882818,-28.0217284962734,
-55.5447583433603));
#188002=CARTESIAN_POINT('Ctrl Pts',(56.4150963311521,-28.0153374570685,
-55.5826612239241));
#188003=CARTESIAN_POINT('Ctrl Pts',(56.4167572958903,-28.0091090795838,
-55.6195994182211));
#188004=CARTESIAN_POINT('Ctrl Pts',(56.4178779761682,-28.0048996781119,
-55.6569736701745));
#188005=CARTESIAN_POINT('Ctrl Pts',(56.4184359903581,-28.0028025535954,
-55.6946207896264));
#188006=CARTESIAN_POINT('Ctrl Pts',(56.4187084931304,-28.0017784358308,
-55.7130055271623));
#188007=CARTESIAN_POINT('Ctrl Pts',(56.4188466190161,-28.0012587793416,
-55.7314552635405));
#188008=CARTESIAN_POINT('Ctrl Pts',(56.418846619879,-28.0012587761031,-55.74995));
#188009=CARTESIAN_POINT('Origin',(56.6260651114328,-29.13000002,-54.74995));
#188010=CARTESIAN_POINT('Origin',(0.,-12.9675000200281,-54.74995));
#188011=CARTESIAN_POINT('',(56.0013925566522,-29.4885226266656,-54.74995));
#188012=CARTESIAN_POINT('Origin',(0.,-12.9675000200281,-54.74995));
#188013=CARTESIAN_POINT('Origin',(56.4809591809864,-29.63000002,-54.74995));
#188014=CARTESIAN_POINT('Ctrl Pts',(56.4809591809864,-29.63000002,-55.24995));
#188015=CARTESIAN_POINT('Ctrl Pts',(56.0013925566522,-29.4885226266655,
-55.2499499999999));
#188016=CARTESIAN_POINT('Ctrl Pts',(56.0013925566522,-29.4885226266656,
-54.74995));
#188017=CARTESIAN_POINT('Ctrl Pts',(56.4430235619105,-29.6942952977694,
-55.24995));
#188018=CARTESIAN_POINT('Ctrl Pts',(55.9815963325889,-29.5556259878439,
-55.2320894585059));
#188019=CARTESIAN_POINT('Ctrl Pts',(55.9637778607192,-29.6160253486821,
-54.7499500197391));
#188020=CARTESIAN_POINT('Ctrl Pts',(56.4048920758008,-29.7580863098899,
-55.2623271401185));
#188021=CARTESIAN_POINT('Ctrl Pts',(55.9595264494602,-29.6302973578872,
-55.2276198610214));
#188022=CARTESIAN_POINT('Ctrl Pts',(55.9259713199402,-29.7425201026704,
-54.7747042862246));
#188023=CARTESIAN_POINT('Ctrl Pts',(56.3324398513309,-29.877933435243,-55.3109611929186));
#188024=CARTESIAN_POINT('Ctrl Pts',(55.9152124797534,-29.7792875750423,
-55.2543206061649));
#188025=CARTESIAN_POINT('Ctrl Pts',(55.8541342694537,-29.9801791700519,
-54.8719723798496));
#188026=CARTESIAN_POINT('Ctrl Pts',(56.2987519266105,-29.9329514036474,
-55.3468561181883));
#188027=CARTESIAN_POINT('Ctrl Pts',(55.8932648786607,-29.8526235485765,
-55.2844345178149));
#188028=CARTESIAN_POINT('Ctrl Pts',(55.8207323820705,-30.0892808127342,
-54.9437622390698));
#188029=CARTESIAN_POINT('Ctrl Pts',(56.2123326186624,-30.0729950473548,
-55.4838442327376));
#188030=CARTESIAN_POINT('Ctrl Pts',(55.8363250868006,-30.0417896984651,
-55.4221362713026));
#188031=CARTESIAN_POINT('Ctrl Pts',(55.7350468385274,-30.3669899517508,
-55.2177384600888));
#188032=CARTESIAN_POINT('Ctrl Pts',(56.1762739146114,-30.1300000200003,
-55.614004390749));
#188033=CARTESIAN_POINT('Ctrl Pts',(55.8093485438182,-30.1300000005986,
-55.5818806132723));
#188034=CARTESIAN_POINT('Ctrl Pts',(55.699294301712,-30.4800318342627,-55.4780587856325));
#188035=CARTESIAN_POINT('Ctrl Pts',(56.1762739063772,-30.1300000200003,
-55.74995));
#188036=CARTESIAN_POINT('Ctrl Pts',(55.8093485379488,-30.1300000200003,
-55.7499499999999));
#188037=CARTESIAN_POINT('Ctrl Pts',(55.6992942935022,-30.4800318603742,
-55.74995));
#188038=CARTESIAN_POINT('',(55.6992942935022,-30.4800318603739,-55.74995));
#188039=CARTESIAN_POINT('Ctrl Pts',(55.6992942935022,-30.4800318603742,
-55.74995));
#188040=CARTESIAN_POINT('Ctrl Pts',(55.6992942945104,-30.4800318571677,
-55.7165618050259));
#188041=CARTESIAN_POINT('Ctrl Pts',(55.6998330297483,-30.4783285093804,
-55.6833050175431));
#188042=CARTESIAN_POINT('Ctrl Pts',(55.7008904740051,-30.4749766534797,
-55.6502628336504));
#188043=CARTESIAN_POINT('Ctrl Pts',(55.7022012337469,-30.4708218455575,
-55.6093052473247));
#188044=CARTESIAN_POINT('Ctrl Pts',(55.704311824946,-30.4641251495371,-55.5686774361727));
#188045=CARTESIAN_POINT('Ctrl Pts',(55.7071988207748,-30.4549435229948,
-55.5285389205525));
#188046=CARTESIAN_POINT('Ctrl Pts',(55.7078054138863,-30.4530143510309,
-55.520105327806));
#188047=CARTESIAN_POINT('Ctrl Pts',(55.7084463261485,-30.4509753351475,
-55.5116934444067));
#188048=CARTESIAN_POINT('Ctrl Pts',(55.7091214061603,-30.4488267863995,
-55.5033049359167));
#188049=CARTESIAN_POINT('Ctrl Pts',(55.7110654210346,-30.4426396520572,
-55.4791487099962));
#188050=CARTESIAN_POINT('Ctrl Pts',(55.7132913748237,-30.4355486844701,
-55.4551844602832));
#188051=CARTESIAN_POINT('Ctrl Pts',(55.7157933833999,-30.4275683986656,
-55.4314477302124));
#188052=CARTESIAN_POINT('Ctrl Pts',(55.718295391976,-30.4195881128611,-55.4077110001416));
#188053=CARTESIAN_POINT('Ctrl Pts',(55.7210734551748,-30.4107185086403,
-55.3842017897311));
#188054=CARTESIAN_POINT('Ctrl Pts',(55.724121621672,-30.4009740809159,-55.3609556432104));
#188055=CARTESIAN_POINT('Ctrl Pts',(55.7281858436682,-30.3879815106165,
-55.3299607811827));
#188056=CARTESIAN_POINT('Ctrl Pts',(55.7326675876837,-30.373634015077,-55.2999843610343));
#188057=CARTESIAN_POINT('Ctrl Pts',(55.7375386580734,-30.3580127797202,
-55.2709916628686));
#188058=CARTESIAN_POINT('Ctrl Pts',(55.7422761695128,-30.3428198600378,
-55.2427939099668));
#188059=CARTESIAN_POINT('Ctrl Pts',(55.7473822073897,-30.3264213210404,
-55.2155261265394));
#188060=CARTESIAN_POINT('Ctrl Pts',(55.7528459976329,-30.3088429857846,
-55.1891766996987));
#188061=CARTESIAN_POINT('Ctrl Pts',(55.7585408389563,-30.2905213032979,
-55.1617130164057));
#188062=CARTESIAN_POINT('Ctrl Pts',(55.7646244097769,-30.2709177421356,
-55.1352460408554));
#188063=CARTESIAN_POINT('Ctrl Pts',(55.7710988761824,-30.2500142965945,
-55.1097968023626));
#188064=CARTESIAN_POINT('Ctrl Pts',(55.7772054795241,-30.230298532793,-55.0857935262488));
#188065=CARTESIAN_POINT('Ctrl Pts',(55.7836600583737,-30.2094256741772,
-55.0626953151138));
#188066=CARTESIAN_POINT('Ctrl Pts',(55.7904742625662,-30.1873473542624,
-55.0405578359032));
#188067=CARTESIAN_POINT('Ctrl Pts',(55.7908847516535,-30.186017351648,-55.0392242695204));
#188068=CARTESIAN_POINT('Ctrl Pts',(55.7912965483067,-30.1846829658094,
-55.0378942024439));
#188069=CARTESIAN_POINT('Ctrl Pts',(55.7917096560192,-30.1833441828804,
-55.0365676519554));
#188070=CARTESIAN_POINT('Ctrl Pts',(55.7918632993036,-30.1828462618782,
-55.0360742804503));
#188071=CARTESIAN_POINT('Ctrl Pts',(55.7920170835031,-30.1823478636952,
-55.0355815185873));
#188072=CARTESIAN_POINT('Ctrl Pts',(55.792171008419,-30.1818489888761,-55.0350893667936));
#188073=CARTESIAN_POINT('Ctrl Pts',(55.800290879717,-30.1555322662012,-55.0091272982118));
#188074=CARTESIAN_POINT('Ctrl Pts',(55.8087607420851,-30.1280129936589,
-54.9848694510044));
#188075=CARTESIAN_POINT('Ctrl Pts',(55.8175466321019,-30.0993860830431,
-54.9622897882634));
#188076=CARTESIAN_POINT('Ctrl Pts',(55.8264122965254,-30.0704992448839,
-54.9395051059746));
#188077=CARTESIAN_POINT('Ctrl Pts',(55.8355999692742,-30.0404839357451,
-54.9184288364593));
#188078=CARTESIAN_POINT('Ctrl Pts',(55.845084553161,-30.0094041347627,-54.8990745550387));
#188079=CARTESIAN_POINT('Ctrl Pts',(55.854533149884,-29.9784422592366,-54.8797937091743));
#188080=CARTESIAN_POINT('Ctrl Pts',(55.8642766342982,-29.946423293465,-54.8622214688159));
#188081=CARTESIAN_POINT('Ctrl Pts',(55.8742965418741,-29.913387106528,-54.8464163971206));
#188082=CARTESIAN_POINT('Ctrl Pts',(55.8793448400683,-29.8967425894409,
-54.8384533780713));
#188083=CARTESIAN_POINT('Ctrl Pts',(55.8844633853516,-29.8798395511654,
-54.8309396845163));
#188084=CARTESIAN_POINT('Ctrl Pts',(55.889650155579,-29.862681631768,-54.8238876164085));
#188085=CARTESIAN_POINT('Ctrl Pts',(55.8897844414451,-29.8622374119616,
-54.8237050378419));
#188086=CARTESIAN_POINT('Ctrl Pts',(55.8899187507015,-29.8617930951974,
-54.8235227993659));
#188087=CARTESIAN_POINT('Ctrl Pts',(55.8900530833078,-29.861348681574,-54.8233409008622));
#188088=CARTESIAN_POINT('Ctrl Pts',(55.8995504810642,-29.8299283654799,
-54.8104805649473));
#188089=CARTESIAN_POINT('Ctrl Pts',(55.9091201713665,-29.7981698989578,
-54.7993661329088));
#188090=CARTESIAN_POINT('Ctrl Pts',(55.9187569872376,-29.7660885799508,
-54.7899280455082));
#188091=CARTESIAN_POINT('Ctrl Pts',(55.9284529762139,-29.7338102714721,
-54.7804320052583));
#188092=CARTESIAN_POINT('Ctrl Pts',(55.938217108462,-29.7012045233227,-54.7726328698961));
#188093=CARTESIAN_POINT('Ctrl Pts',(55.9480481282842,-29.6682706672262,
-54.7665101842522));
#188094=CARTESIAN_POINT('Ctrl Pts',(55.9578188295005,-29.6355388780897,
-54.7604250645851));
#188095=CARTESIAN_POINT('Ctrl Pts',(55.9676557893865,-29.6024823867339,
-54.7559958377295));
#188096=CARTESIAN_POINT('Ctrl Pts',(55.9775588733957,-29.5690936714574,
-54.7532529199582));
#188097=CARTESIAN_POINT('Ctrl Pts',(55.9854615290049,-29.5424494949745,
-54.7510640730807));
#188098=CARTESIAN_POINT('Ctrl Pts',(55.9934063510512,-29.5155935075394,
-54.7499500041909));
#188099=CARTESIAN_POINT('Ctrl Pts',(56.0013925566522,-29.4885226266656,
-54.74995));
#188100=CARTESIAN_POINT('Origin',(56.1762739063772,-30.63000002,-55.74995));
#188101=CARTESIAN_POINT('Origin',(56.1762739063772,-30.63000002,-55.24995));
#188102=CARTESIAN_POINT('',(55.6992942935022,-30.4800318603739,-55.24995));
#188103=CARTESIAN_POINT('Origin',(0.,-12.9675000200281,-60.42825533736));
#188104=CARTESIAN_POINT('Origin',(0.,-12.9675000200281,-60.42825533736));
#188105=CARTESIAN_POINT('Origin',(54.076473627675,-36.28000002,-55.24995));
#188106=CARTESIAN_POINT('',(53.6173229282256,-36.0820590308261,-55.74995));
#188107=CARTESIAN_POINT('Origin',(54.076473627675,-36.28000002,-55.74995));
#188108=CARTESIAN_POINT('',(53.6173229282256,-36.0820590308261,-55.24995));
#188109=CARTESIAN_POINT('Ctrl Pts',(54.076473627675,-36.78000002,-55.74995));
#188110=CARTESIAN_POINT('Ctrl Pts',(53.3164388612999,-36.78000002,-55.7499499999999));
#188111=CARTESIAN_POINT('Ctrl Pts',(53.6173229282256,-36.0820590308261,
-55.74995));
#188112=CARTESIAN_POINT('Ctrl Pts',(54.07647361027,-36.78000002,-55.6425914202082));
#188113=CARTESIAN_POINT('Ctrl Pts',(53.3164388632929,-36.7800000140484,
-55.7160682965194));
#188114=CARTESIAN_POINT('Ctrl Pts',(53.6173229109667,-36.0820590708605,
-55.5352328299022));
#188115=CARTESIAN_POINT('Ctrl Pts',(54.0462927577141,-36.8151341090744,
-55.5384961709319));
#188116=CARTESIAN_POINT('Ctrl Pts',(53.3223470981189,-36.7637806572682,
-55.672084159207));
#188117=CARTESIAN_POINT('Ctrl Pts',(53.587398316273,-36.1517305970246,-55.3270423559178));
#188118=CARTESIAN_POINT('Ctrl Pts',(53.939326192416,-36.9379861363991,-55.370688163807));
#188119=CARTESIAN_POINT('Ctrl Pts',(53.3111802821853,-36.783202746029,-55.5229519438579));
#188120=CARTESIAN_POINT('Ctrl Pts',(53.481339980492,-36.3953483985127,-54.9914263135601));
#188121=CARTESIAN_POINT('Ctrl Pts',(53.8654589377065,-37.0221914881654,
-55.3103188190833));
#188122=CARTESIAN_POINT('Ctrl Pts',(53.293833750711,-36.8201344622738,-55.429912748872));
#188123=CARTESIAN_POINT('Ctrl Pts',(53.4080974646291,-36.562334686105,-54.8706857163843));
#188124=CARTESIAN_POINT('Ctrl Pts',(53.7823432375794,-37.1153847305999,
-55.2778252214766));
#188125=CARTESIAN_POINT('Ctrl Pts',(53.2549772028899,-36.9057059891941,
-55.3509337052243));
#188126=CARTESIAN_POINT('Ctrl Pts',(53.3256899305316,-36.747133105635,-54.8057004429533));
#188127=CARTESIAN_POINT('',(53.3256899305366,-36.7471331056238,-54.8057004429536));
#188128=CARTESIAN_POINT('Origin',(53.7823432375799,-36.9507694411988,-54.8057004429536));
#188129=CARTESIAN_POINT('Ctrl Pts',(53.3256899305362,-36.7471331056248,
-54.8057004429569));
#188130=CARTESIAN_POINT('Ctrl Pts',(53.3365047080717,-36.7228810294277,
-54.8142288048715));
#188131=CARTESIAN_POINT('Ctrl Pts',(53.347033550176,-36.6992232138251,-54.8236117045923));
#188132=CARTESIAN_POINT('Ctrl Pts',(53.3573294859536,-36.6760484250078,
-54.833842030096));
#188133=CARTESIAN_POINT('Ctrl Pts',(53.3676295626462,-36.6528643155391,
-54.8440764701269));
#188134=CARTESIAN_POINT('Ctrl Pts',(53.3776967400546,-36.6301631323027,
-54.855159268536));
#188135=CARTESIAN_POINT('Ctrl Pts',(53.3875763712775,-36.6078483738899,
-54.8671326577126));
#188136=CARTESIAN_POINT('Ctrl Pts',(53.3972846011521,-36.5859207533766,
-54.8788983210135));
#188137=CARTESIAN_POINT('Ctrl Pts',(53.406811903452,-36.5643658402485,-54.891524208438));
#188138=CARTESIAN_POINT('Ctrl Pts',(53.4161912134876,-36.5431130768774,
-54.9050940181005));
#188139=CARTESIAN_POINT('Ctrl Pts',(53.4247320031921,-36.5237603332428,
-54.9174506722911));
#188140=CARTESIAN_POINT('Ctrl Pts',(53.4331500860381,-36.5046580712458,
-54.9305905504039));
#188141=CARTESIAN_POINT('Ctrl Pts',(53.4414609284995,-36.4857733835863,
-54.9446070495014));
#188142=CARTESIAN_POINT('Ctrl Pts',(53.4509986505366,-36.4641008633228,
-54.9606927198705));
#188143=CARTESIAN_POINT('Ctrl Pts',(53.4601425635063,-36.4432889157824,
-54.9775073786436));
#188144=CARTESIAN_POINT('Ctrl Pts',(53.4689373117184,-36.4232432529379,
-54.9950729719853));
#188145=CARTESIAN_POINT('Ctrl Pts',(53.4776988122795,-36.4032733706824,
-55.0125721603883));
#188146=CARTESIAN_POINT('Ctrl Pts',(53.4861139520167,-36.3840635594153,
-55.0308169094228));
#188147=CARTESIAN_POINT('Ctrl Pts',(53.4942155666396,-36.3655444879779,
-55.0498730291534));
#188148=CARTESIAN_POINT('Ctrl Pts',(53.5021531960704,-36.3474002620039,
-55.0685434329988));
#188149=CARTESIAN_POINT('Ctrl Pts',(53.509789997807,-36.3299187504364,-55.0879929870304));
#188150=CARTESIAN_POINT('Ctrl Pts',(53.5171438153628,-36.3130633064965,
-55.1083215416835));
#188151=CARTESIAN_POINT('Ctrl Pts',(53.5230683586813,-36.2994838551412,
-55.1246990764445));
#188152=CARTESIAN_POINT('Ctrl Pts',(53.5288090292654,-36.2863111840396,
-55.1416478579265));
#188153=CARTESIAN_POINT('Ctrl Pts',(53.5343678189769,-36.2735425514815,
-55.1592369940626));
#188154=CARTESIAN_POINT('Ctrl Pts',(53.5344871593642,-36.2732684246241,
-55.1596146112107));
#188155=CARTESIAN_POINT('Ctrl Pts',(53.5346064010008,-36.272994519867,-55.1599924902182));
#188156=CARTESIAN_POINT('Ctrl Pts',(53.534725543904,-36.2727208371876,-55.1603706315252));
#188157=CARTESIAN_POINT('Ctrl Pts',(53.5416014628259,-36.2569261917407,
-55.1821937439223));
#188158=CARTESIAN_POINT('Ctrl Pts',(53.5480238717073,-36.2421576554038,
-55.2044892728991));
#188159=CARTESIAN_POINT('Ctrl Pts',(53.5540298412575,-36.2283345422306,
-55.2272840027525));
#188160=CARTESIAN_POINT('Ctrl Pts',(53.5600584943761,-36.2144592214114,
-55.2501648245862));
#188161=CARTESIAN_POINT('Ctrl Pts',(53.5656676548917,-36.2015362223129,
-55.2735491895684));
#188162=CARTESIAN_POINT('Ctrl Pts',(53.5708774015945,-36.1895232328314,
-55.2974947075211));
#188163=CARTESIAN_POINT('Ctrl Pts',(53.5760229208745,-36.1776583433246,
-55.3211450174732));
#188164=CARTESIAN_POINT('Ctrl Pts',(53.5807788918407,-36.1666809556098,
-55.3453432833983));
#188165=CARTESIAN_POINT('Ctrl Pts',(53.5851464697891,-36.1565918414746,
-55.3701663329474));
#188166=CARTESIAN_POINT('Ctrl Pts',(53.5890231720465,-36.1476366512055,
-55.3921994994665));
#188167=CARTESIAN_POINT('Ctrl Pts',(53.5925937005088,-36.139381680042,-55.4147254208055));
#188168=CARTESIAN_POINT('Ctrl Pts',(53.5958456670774,-36.1318578925515,
-55.4378070838457));
#188169=CARTESIAN_POINT('Ctrl Pts',(53.6001803589108,-36.1218290993573,
-55.4685736659031));
#188170=CARTESIAN_POINT('Ctrl Pts',(53.6038427283339,-36.1133454971332,
-55.4995748163826));
#188171=CARTESIAN_POINT('Ctrl Pts',(53.6068550156883,-36.1063621989411,
-55.5307884996878));
#188172=CARTESIAN_POINT('Ctrl Pts',(53.6098729740293,-36.0993657538655,
-55.5620609464382));
#188173=CARTESIAN_POINT('Ctrl Pts',(53.6122384934281,-36.0938750177308,
-55.5935474015465));
#188174=CARTESIAN_POINT('Ctrl Pts',(53.6139551145697,-36.0898877949595,
-55.6252487013041));
#188175=CARTESIAN_POINT('Ctrl Pts',(53.6156514736902,-36.0859476351017,
-55.6565758169199));
#188176=CARTESIAN_POINT('Ctrl Pts',(53.6167142276579,-36.0834755230399,
-55.6881133687363));
#188177=CARTESIAN_POINT('Ctrl Pts',(53.6171273211733,-36.0825142809585,
-55.7198748365422));
#188178=CARTESIAN_POINT('Ctrl Pts',(53.6172574163426,-36.0822115578542,
-55.7298774470373));
#188179=CARTESIAN_POINT('Ctrl Pts',(53.617322927418,-36.0820590326995,-55.7399023232672));
#188180=CARTESIAN_POINT('Ctrl Pts',(53.6173229282256,-36.0820590308261,
-55.74995));
#188181=CARTESIAN_POINT('Origin',(24.5275331667447,40.0183497231583,-52.64995));
#188182=CARTESIAN_POINT('',(25.3802177275058,39.9437494905281,-52.64995));
#188183=CARTESIAN_POINT('',(25.3802177275058,39.9437494905281,-52.64995));
#188184=CARTESIAN_POINT('',(43.1064181712417,38.392907904313,-52.64995));
#188185=CARTESIAN_POINT('',(24.5275331667447,40.0183497231583,-52.64995));
#188186=CARTESIAN_POINT('',(43.1064181712417,38.392907904313,-52.64995));
#188187=CARTESIAN_POINT('Origin',(42.8449509429988,35.4043238100378,-59.64995));
#188188=CARTESIAN_POINT('Origin',(42.8449509429988,35.4043238100378,-59.64995));
#188189=CARTESIAN_POINT('Origin',(44.1941738241593,38.2977416159964,-52.64995));
#188190=CARTESIAN_POINT('',(50.4931441736257,31.9987712665301,-52.64995));
#188191=CARTESIAN_POINT('',(50.4931441736257,31.9987712665301,-52.64995));
#188192=CARTESIAN_POINT('',(44.9662712865584,37.5256441535974,-52.64995));
#188193=CARTESIAN_POINT('',(44.9662712865584,37.5256441535974,-52.64995));
#188194=CARTESIAN_POINT('',(44.1941738241593,38.2977416159964,-52.64995));
#188195=CARTESIAN_POINT('Origin',(42.8449509429988,35.4043238100378,-52.64995));
#188196=CARTESIAN_POINT('Origin',(42.8449509429988,35.4043238100378,-52.64995));
#188197=CARTESIAN_POINT('Origin',(48.3718238300661,29.8774509229704,-59.64995));
#188198=CARTESIAN_POINT('Origin',(48.3718238300661,29.8774509229704,-59.64995));
#188199=CARTESIAN_POINT('Origin',(51.2652416360248,31.226673804131,-52.64995));
#188200=CARTESIAN_POINT('',(51.3604079243413,30.1389181512134,-52.64995));
#188201=CARTESIAN_POINT('',(51.3604079243413,30.1389181512134,-52.64995));
#188202=CARTESIAN_POINT('',(52.9112495105564,12.4127177074772,-52.64995));
#188203=CARTESIAN_POINT('',(51.2652416360248,31.226673804131,-52.64995));
#188204=CARTESIAN_POINT('',(52.9112495105564,12.4127177074773,-55.24995));
#188205=CARTESIAN_POINT('Origin',(48.3718238300661,29.8774509229704,-52.64995));
#188206=CARTESIAN_POINT('Origin',(48.3718238300661,29.8774509229704,-52.64995));
#188207=CARTESIAN_POINT('Ctrl Pts',(53.0821522164592,11.4835005182672,-54.749226640207));
#188208=CARTESIAN_POINT('Ctrl Pts',(53.0814553265489,11.4833027557155,-55.24995));
#188209=CARTESIAN_POINT('Ctrl Pts',(53.5631588418786,11.61999998,-55.24995));
#188210=CARTESIAN_POINT('Ctrl Pts',(53.0314894680352,11.6620294726881,-54.7492424048586));
#188211=CARTESIAN_POINT('Ctrl Pts',(53.0524992546297,11.5855117152954,-55.2284093535366));
#188212=CARTESIAN_POINT('Ctrl Pts',(53.5175339525391,11.7003881248737,-55.24995));
#188213=CARTESIAN_POINT('Ctrl Pts',(52.9910538795555,11.8458000768038,-54.7896174675006));
#188214=CARTESIAN_POINT('Ctrl Pts',(53.0226612146944,11.6989200777954,-55.238154595146));
#188215=CARTESIAN_POINT('Ctrl Pts',(53.481213741953,11.782936109662,-55.2701189042654));
#188216=CARTESIAN_POINT('Ctrl Pts',(52.9359085954001,12.1689324824227,-54.9449932254243));
#188217=CARTESIAN_POINT('Ctrl Pts',(52.9757607799671,11.8899765016028,-55.3144933675901));
#188218=CARTESIAN_POINT('Ctrl Pts',(53.4315945187188,11.9282552364233,-55.3477500998626));
#188219=CARTESIAN_POINT('Ctrl Pts',(52.9200762514753,12.3116974252973,-55.0618112506234));
#188220=CARTESIAN_POINT('Ctrl Pts',(52.9570824697211,11.9716603673777,-55.3811270199801));
#188221=CARTESIAN_POINT('Ctrl Pts',(53.4173436672944,11.9924457375215,-55.4061007701193));
#188222=CARTESIAN_POINT('Ctrl Pts',(52.9111992844441,12.4132973608818,-55.2012882697194));
#188223=CARTESIAN_POINT('Ctrl Pts',(52.9444394937624,12.0259207443505,-55.4571605585729));
#188224=CARTESIAN_POINT('Ctrl Pts',(53.4093468596018,12.0381477794281,-55.475810586866));
#188225=CARTESIAN_POINT('',(53.0821517130856,11.4835003754205,-54.74995));
#188226=CARTESIAN_POINT('Origin',(53.5631588418786,11.61999998,-54.74995));
#188227=CARTESIAN_POINT('Ctrl Pts',(53.0821517130856,11.4835003754205,-54.74995));
#188228=CARTESIAN_POINT('Ctrl Pts',(53.0564462519378,11.5740831291147,-54.74995));
#188229=CARTESIAN_POINT('Ctrl Pts',(53.0341440975299,11.6624073741825,-54.7594183008898));
#188230=CARTESIAN_POINT('Ctrl Pts',(53.0051082177742,11.79112063162,-54.7878232035592));
#188231=CARTESIAN_POINT('Ctrl Pts',(52.9916948966,11.8545354170554,-54.8055762677276));
#188232=CARTESIAN_POINT('Ctrl Pts',(52.9798127489238,11.9164774315466,-54.8286552511465));
#188233=CARTESIAN_POINT('Ctrl Pts',(52.9722178731516,11.9574389462162,-54.8452247777036));
#188234=CARTESIAN_POINT('Ctrl Pts',(52.9687758404164,11.9766401182258,-54.8535781982143));
#188235=CARTESIAN_POINT('Ctrl Pts',(52.9357472552443,12.1679591460758,-54.943500910384));
#188236=CARTESIAN_POINT('Ctrl Pts',(52.9205204470379,12.3067504185984,-55.0562014313995));
#188237=CARTESIAN_POINT('Ctrl Pts',(52.9112495105564,12.4127177074773,-55.2016711737242));
#188238=CARTESIAN_POINT('Origin',(57.8922230010151,12.8484964212155,-54.74995));
#188239=CARTESIAN_POINT('',(53.275786978871,10.927944819865,-54.74995));
#188240=CARTESIAN_POINT('Origin',(53.7374305810854,11.11999998,-54.74995));
#188241=CARTESIAN_POINT('Origin',(57.8922230010151,12.8484964212155,-54.74995));
#188242=CARTESIAN_POINT('Ctrl Pts',(53.3256899305368,10.8121330655672,-54.7553968408231));
#188243=CARTESIAN_POINT('Ctrl Pts',(53.3054454943535,10.8575310968505,-55.2747187747876));
#188244=CARTESIAN_POINT('Ctrl Pts',(53.7823432375846,11.067884690566,-55.2526734204115));
#188245=CARTESIAN_POINT('Ctrl Pts',(53.3086079255675,10.8504393631076,-54.7517837407593));
#188246=CARTESIAN_POINT('Ctrl Pts',(53.2957533879043,10.880281535778,-55.2650191833929));
#188247=CARTESIAN_POINT('Ctrl Pts',(53.7669694165083,11.0851225427625,-55.2508668691012));
#188248=CARTESIAN_POINT('Ctrl Pts',(53.2919715007789,10.8890420328302,-54.7499500043796));
#188249=CARTESIAN_POINT('Ctrl Pts',(53.2858304006402,10.9038034191885,-55.2567197573796));
#188250=CARTESIAN_POINT('Ctrl Pts',(53.7519966717624,11.1024937011227,-55.24995));
#188251=CARTESIAN_POINT('Ctrl Pts',(53.275786978871,10.927944819865,-54.74995));
#188252=CARTESIAN_POINT('Ctrl Pts',(53.275786978871,10.927944819865,-55.24995));
#188253=CARTESIAN_POINT('Ctrl Pts',(53.7374305810854,11.11999998,-55.24995));
#188254=CARTESIAN_POINT('Origin',(53.6412833044364,11.0802639242609,-56.1025073833426));
#188255=CARTESIAN_POINT('Origin',(0.,-12.9675000200281,-55.24995));
#188256=CARTESIAN_POINT('',(53.3256899305366,-36.7471331056238,-52.64995));
#188257=CARTESIAN_POINT('',(53.3256899305368,10.8121330655672,-52.64995));
#188258=CARTESIAN_POINT('Origin',(0.,-12.9675000200281,-52.64995));
#188259=CARTESIAN_POINT('',(53.3256899305366,-36.7471331056238,-55.24995));
#188260=CARTESIAN_POINT('',(53.3256899305368,10.8121330655672,-55.24995));
#188261=CARTESIAN_POINT('Origin',(57.8922230010151,12.8484964212155,-55.24995));
#188262=CARTESIAN_POINT('Origin',(57.8922230010151,12.8484964212155,-52.64995));
#188263=CARTESIAN_POINT('Ctrl Pts',(53.1795531264094,-37.1129448598586,
-54.74995));
#188264=CARTESIAN_POINT('Ctrl Pts',(53.1795531264094,-37.1129448598586,
-55.24995));
#188265=CARTESIAN_POINT('Ctrl Pts',(53.65082011387,-37.28000002,-55.24995));
#188266=CARTESIAN_POINT('Ctrl Pts',(53.2245914375472,-36.9858906030954,
-54.74995002559));
#188267=CARTESIAN_POINT('Ctrl Pts',(53.2071047405196,-37.0352210513017,
-55.2694186883497));
#188268=CARTESIAN_POINT('Ctrl Pts',(53.6913582052585,-37.222820517008,-55.24995));
#188269=CARTESIAN_POINT('Ctrl Pts',(53.2735999108999,-36.8639446739783,
-54.7690447340998));
#188270=CARTESIAN_POINT('Ctrl Pts',(53.233451048998,-36.9645829953838,-55.3049428618926));
#188271=CARTESIAN_POINT('Ctrl Pts',(53.7354566371443,-37.1679561903806,
-55.2594951814958));
#188272=CARTESIAN_POINT('Ctrl Pts',(53.3256899305359,-36.7471331056253,
-54.8057004429567));
#188273=CARTESIAN_POINT('Ctrl Pts',(53.2549772028919,-36.90570598919,-55.3509337052282));
#188274=CARTESIAN_POINT('Ctrl Pts',(53.7823432375838,-37.115384730595,-55.2778252214784));
#188275=CARTESIAN_POINT('',(53.1795531264094,-37.1129448598587,-54.74995));
#188276=CARTESIAN_POINT('Origin',(53.65082011387,-37.28000002,-54.74995));
#188277=CARTESIAN_POINT('Ctrl Pts',(53.1795531264094,-37.1129448598586,
-54.74995));
#188278=CARTESIAN_POINT('Ctrl Pts',(53.203745009962,-37.044698921971,-54.7499500137454));
#188279=CARTESIAN_POINT('Ctrl Pts',(53.229115357639,-36.9778304553021,-54.7554548649733));
#188280=CARTESIAN_POINT('Ctrl Pts',(53.2555724802121,-36.9122732840969,
-54.7662993117297));
#188281=CARTESIAN_POINT('Ctrl Pts',(53.2781697189556,-36.8562803829422,
-54.7755616399258));
#188282=CARTESIAN_POINT('Ctrl Pts',(53.301560005639,-36.8012443229208,-54.7887202323916));
#188283=CARTESIAN_POINT('Ctrl Pts',(53.3256899305359,-36.7471331056253,
-54.8057004429567));
#188284=CARTESIAN_POINT('Origin',(57.8922230010149,-38.7834964612722,-54.74995));
#188285=CARTESIAN_POINT('',(53.0181298732915,-37.6685004154142,-54.74995));
#188286=CARTESIAN_POINT('Origin',(53.5055391860638,-37.78000002,-54.74995));
#188287=CARTESIAN_POINT('Origin',(57.8922230010149,-38.7834964612722,-54.74995));
#188288=CARTESIAN_POINT('Ctrl Pts',(52.9112495105562,-38.347717747534,-54.9585476429427));
#188289=CARTESIAN_POINT('Ctrl Pts',(52.9364447521332,-38.0597348185281,
-55.3342330819689));
#188290=CARTESIAN_POINT('Ctrl Pts',(53.4093468596021,-38.0856478194539,
-55.3542488214713));
#188291=CARTESIAN_POINT('Ctrl Pts',(52.9283556128915,-38.1521941031454,
-54.8226237570584));
#188292=CARTESIAN_POINT('Ctrl Pts',(52.9572784319432,-37.9516014512281,
-55.2598937783695));
#188293=CARTESIAN_POINT('Ctrl Pts',(53.4247544927353,-37.9975926380036,
-55.2862331725394));
#188294=CARTESIAN_POINT('Ctrl Pts',(52.9626456126999,-37.9110442829472,
-54.7499500131212));
#188295=CARTESIAN_POINT('Ctrl Pts',(52.9868771633111,-37.8051184700684,
-55.2259980552998));
#188296=CARTESIAN_POINT('Ctrl Pts',(53.4555105552472,-37.889347597856,-55.24995));
#188297=CARTESIAN_POINT('Ctrl Pts',(53.0181298732915,-37.6685004154142,
-54.74995));
#188298=CARTESIAN_POINT('Ctrl Pts',(53.0181298732915,-37.6685004154141,
-55.2499499999999));
#188299=CARTESIAN_POINT('Ctrl Pts',(53.5055391860638,-37.78000002,-55.24995));
#188300=CARTESIAN_POINT('Ctrl Pts',(52.9112495105562,-38.347717747534,-54.9585476429427));
#188301=CARTESIAN_POINT('Ctrl Pts',(52.9138167203455,-38.3183744053704,
-54.9381487773268));
#188302=CARTESIAN_POINT('Ctrl Pts',(52.9167587015664,-38.288135817498,-54.9192611255627));
#188303=CARTESIAN_POINT('Ctrl Pts',(52.920093649339,-38.2570537209009,-54.901824465559));
#188304=CARTESIAN_POINT('Ctrl Pts',(52.9223677590233,-38.2358587572315,
-54.8899343611017));
#188305=CARTESIAN_POINT('Ctrl Pts',(52.9248248159382,-38.2142707844826,
-54.8787197886081));
#188306=CARTESIAN_POINT('Ctrl Pts',(52.9274736531865,-38.1922987278826,
-54.8681728665638));
#188307=CARTESIAN_POINT('Ctrl Pts',(52.9299589939906,-38.1716828713013,
-54.8582769411983));
#188308=CARTESIAN_POINT('Ctrl Pts',(52.9326383429721,-38.1505275158821,
-54.8488776493919));
#188309=CARTESIAN_POINT('Ctrl Pts',(52.9354970235834,-38.1290543071062,
-54.8400916455875));
#188310=CARTESIAN_POINT('Ctrl Pts',(52.9379577126515,-38.1105706437396,
-54.832528847761));
#188311=CARTESIAN_POINT('Ctrl Pts',(52.9405510514482,-38.0918525526911,
-54.8254200347525));
#188312=CARTESIAN_POINT('Ctrl Pts',(52.9432599418087,-38.0730559676527,
-54.8188132901669));
#188313=CARTESIAN_POINT('Ctrl Pts',(52.9456302208742,-38.0566089557442,
-54.8130323886545));
#188314=CARTESIAN_POINT('Ctrl Pts',(52.9480888658684,-38.0401021278493,
-54.8076355026166));
#188315=CARTESIAN_POINT('Ctrl Pts',(52.9506198739619,-38.0236452379292,
-54.8026387626986));
#188316=CARTESIAN_POINT('Ctrl Pts',(52.9513690438644,-38.0187740537363,
-54.8011597444501));
#188317=CARTESIAN_POINT('Ctrl Pts',(52.9521257433548,-38.0138993081238,
-54.7997132372211));
#188318=CARTESIAN_POINT('Ctrl Pts',(52.952890638887,-38.0090171068857,-54.7982978559824));
#188319=CARTESIAN_POINT('Ctrl Pts',(52.9583778797083,-37.9739929594029,
-54.7881441325221));
#188320=CARTESIAN_POINT('Ctrl Pts',(52.964275682584,-37.9386530390232,-54.7796085808392));
#188321=CARTESIAN_POINT('Ctrl Pts',(52.9706104876299,-37.9030233239771,
-54.7726555501025));
#188322=CARTESIAN_POINT('Ctrl Pts',(52.976957882613,-37.8673227976168,-54.7656887007527));
#188323=CARTESIAN_POINT('Ctrl Pts',(52.9837439516238,-37.8313305401564,
-54.7603105161544));
#188324=CARTESIAN_POINT('Ctrl Pts',(52.9910089773631,-37.7950582648799,
-54.75653337115));
#188325=CARTESIAN_POINT('Ctrl Pts',(52.9981747631865,-37.7592814672075,
-54.7528078217717));
#188326=CARTESIAN_POINT('Ctrl Pts',(53.0058064655273,-37.7232314999343,
-54.750639790985));
#188327=CARTESIAN_POINT('Ctrl Pts',(53.0139568096317,-37.6869169823467,
-54.7500895663837));
#188328=CARTESIAN_POINT('Ctrl Pts',(53.0153329135287,-37.6807856400957,
-54.7499966664756));
#188329=CARTESIAN_POINT('Ctrl Pts',(53.0167238361879,-37.6746467652684,
-54.7499500003325));
#188330=CARTESIAN_POINT('Ctrl Pts',(53.0181298732915,-37.6685004154142,
-54.74995));
#188331=CARTESIAN_POINT('Origin',(3.,45.8435334367418,-55.24995));
#188332=CARTESIAN_POINT('',(2.97452770112504,45.3441826962898,-56.3263223051814));
#188333=CARTESIAN_POINT('',(2.97452770112504,45.3441826962898,-55.24995));
#188334=CARTESIAN_POINT('Origin',(3.,45.8435334367418,-56.3263223051791));
#188335=CARTESIAN_POINT('Ctrl Pts',(3.5,45.8435334367382,-56.3263223051844));
#188336=CARTESIAN_POINT('Ctrl Pts',(3.49999999999616,45.3173779148746,-56.3263223051846));
#188337=CARTESIAN_POINT('Ctrl Pts',(2.97452770112504,45.3441826962898,-56.3263223051814));
#188338=CARTESIAN_POINT('Ctrl Pts',(3.50000000000048,45.8043701107064,-56.199422183327));
#188339=CARTESIAN_POINT('Ctrl Pts',(3.46044927957146,45.3193954300817,-56.2062114458595));
#188340=CARTESIAN_POINT('Ctrl Pts',(2.97452768320356,45.344182697204,-56.1669325210571));
#188341=CARTESIAN_POINT('Ctrl Pts',(3.50768789429957,45.7667515939358,-56.0829442465191));
#188342=CARTESIAN_POINT('Ctrl Pts',(3.43677818882601,45.3204789931111,-56.08184534982));
#188343=CARTESIAN_POINT('Ctrl Pts',(2.98977292660286,45.3434149603554,-56.0100642332945));
#188344=CARTESIAN_POINT('Ctrl Pts',(3.54526290572092,45.6961797895947,-55.8659417020081));
#188345=CARTESIAN_POINT('Ctrl Pts',(3.43477708310906,45.3200587327755,-55.8400245162723));
#188346=CARTESIAN_POINT('Ctrl Pts',(3.06428488995232,45.339546776353,-55.7037165501142));
#188347=CARTESIAN_POINT('Ctrl Pts',(3.57574585639141,45.6630233017381,-55.7649226433931));
#188348=CARTESIAN_POINT('Ctrl Pts',(3.45484122335623,45.3186462559097,-55.719311149436));
#188349=CARTESIAN_POINT('Ctrl Pts',(3.12473312373466,45.3363910645469,-55.5532476192867));
#188350=CARTESIAN_POINT('Ctrl Pts',(3.64122647661092,45.619502323306,-55.6349498078453));
#188351=CARTESIAN_POINT('Ctrl Pts',(3.52210194558877,45.3142897117584,-55.5588309593355));
#188352=CARTESIAN_POINT('Ctrl Pts',(3.2545824170552,45.329238556454,-55.3542910788838));
#188353=CARTESIAN_POINT('Ctrl Pts',(3.66673217579536,45.6057722112868,-55.5945395207919));
#188354=CARTESIAN_POINT('Ctrl Pts',(3.55052601940426,45.3124719950673,-55.508240833463));
#188355=CARTESIAN_POINT('Ctrl Pts',(3.30516068386241,45.3264035474275,-55.2914116693877));
#188356=CARTESIAN_POINT('Ctrl Pts',(3.72301031701685,45.5810344345382,-55.523890140111));
#188357=CARTESIAN_POINT('Ctrl Pts',(3.61713920495136,45.3082025597939,-55.418990846134));
#188358=CARTESIAN_POINT('Ctrl Pts',(3.4167612791713,45.3199688102369,-55.1805611737224));
#188359=CARTESIAN_POINT('Ctrl Pts',(3.75395740734289,45.5698505794225,-55.4931090773944));
#188360=CARTESIAN_POINT('Ctrl Pts',(3.65544514044212,45.3057432608012,-55.3793555355223));
#188361=CARTESIAN_POINT('Ctrl Pts',(3.47812992567118,45.3163517222977,-55.1317622002044));
#188362=CARTESIAN_POINT('Ctrl Pts',(3.85643479923312,45.5394893320724,-55.41516737719));
#188363=CARTESIAN_POINT('Ctrl Pts',(3.78526119814061,45.2973112081201,-55.2791383019779));
#188364=CARTESIAN_POINT('Ctrl Pts',(3.68134449873891,45.3039876967517,-55.0081141730616));
#188365=CARTESIAN_POINT('Ctrl Pts',(3.93416970441317,45.5245403614249,-55.3854368917647));
#188366=CARTESIAN_POINT('Ctrl Pts',(3.88948584507308,45.2904098439472,-55.2390222324484));
#188367=CARTESIAN_POINT('Ctrl Pts',(3.83550338599137,45.2941065762735,-54.961052531036));
#188368=CARTESIAN_POINT('Ctrl Pts',(4.01487932239363,45.5159631499936,-55.3828830175977));
#188369=CARTESIAN_POINT('Ctrl Pts',(3.99772850678843,45.282979186916,-55.2358129028005));
#188370=CARTESIAN_POINT('Ctrl Pts',(3.99554290592259,45.2831291022416,-54.9597685279837));
#188371=CARTESIAN_POINT('',(3.99554290592262,45.2831291022416,-54.9597685279837));
#188372=CARTESIAN_POINT('Ctrl Pts',(3.99554290592259,45.2831291022416,-54.9597685279837));
#188373=CARTESIAN_POINT('Ctrl Pts',(3.94364694050733,45.286688764336,-54.9601848912546));
#188374=CARTESIAN_POINT('Ctrl Pts',(3.89225569970065,45.2901408601658,-54.9654203274222));
#188375=CARTESIAN_POINT('Ctrl Pts',(3.84188163699711,45.2934612214904,-54.975154634361));
#188376=CARTESIAN_POINT('Ctrl Pts',(3.78940342464469,45.2969202759588,-54.9852955481412));
#188377=CARTESIAN_POINT('Ctrl Pts',(3.73803006365291,45.3002363143349,-55.000318715847));
#188378=CARTESIAN_POINT('Ctrl Pts',(3.68833368154415,45.3033833815734,-55.0198046066567));
#188379=CARTESIAN_POINT('Ctrl Pts',(3.63901329264086,45.3065066387104,-55.039143070989));
#188380=CARTESIAN_POINT('Ctrl Pts',(3.59134547691614,45.3094634363256,-55.0628761864957));
#188381=CARTESIAN_POINT('Ctrl Pts',(3.54586890420049,45.3122303325377,-55.0905475013328));
#188382=CARTESIAN_POINT('Ctrl Pts',(3.54528805073115,45.3122656729596,-55.0909009356016));
#188383=CARTESIAN_POINT('Ctrl Pts',(3.5447076792751,45.3123009754724,-55.0912549191843));
#188384=CARTESIAN_POINT('Ctrl Pts',(3.54412778939157,45.3123362401396,-55.0916094513196));
#188385=CARTESIAN_POINT('Ctrl Pts',(3.47701183225151,45.3164177424284,-55.1326426961998));
#188386=CARTESIAN_POINT('Ctrl Pts',(3.41622114944533,45.3199999518618,-55.181103831794));
#188387=CARTESIAN_POINT('Ctrl Pts',(3.36096258887421,45.3231860861595,-55.2359880590722));
#188388=CARTESIAN_POINT('Ctrl Pts',(3.36038241673501,45.3232195381049,-55.2365643010014));
#188389=CARTESIAN_POINT('Ctrl Pts',(3.35980281684021,45.3232529482704,-55.2371413403593));
#188390=CARTESIAN_POINT('Ctrl Pts',(3.35922379149642,45.3232863165813,-55.2377191725326));
#188391=CARTESIAN_POINT('Ctrl Pts',(3.30734351853634,45.3262760943051,-55.2894925382371));
#188392=CARTESIAN_POINT('Ctrl Pts',(3.26003938774549,45.328931962174,-55.3476821319182));
#188393=CARTESIAN_POINT('Ctrl Pts',(3.21898968010886,45.3311986016838,-55.4089811023496));
#188394=CARTESIAN_POINT('Ctrl Pts',(3.21640175023779,45.331341499269,-55.4128456228488));
#188395=CARTESIAN_POINT('Ctrl Pts',(3.21383866111205,45.3314828508092,-55.4167225044094));
#188396=CARTESIAN_POINT('Ctrl Pts',(3.21130082579067,45.3316226428383,-55.4206109203385));
#188397=CARTESIAN_POINT('Ctrl Pts',(3.21085284159181,45.3316473192307,-55.4212973119574));
#188398=CARTESIAN_POINT('Ctrl Pts',(3.21040556228037,45.3316719521366,-55.4219841720788));
#188399=CARTESIAN_POINT('Ctrl Pts',(3.20995898742772,45.3316965416118,-55.4226714985032));
#188400=CARTESIAN_POINT('Ctrl Pts',(3.1542985362487,45.3347613386447,-55.5083388813912));
#188401=CARTESIAN_POINT('Ctrl Pts',(3.10954127961328,45.337153729465,-55.6013158854463));
#188402=CARTESIAN_POINT('Ctrl Pts',(3.07484642277082,45.338981720226,-55.6975623037683));
#188403=CARTESIAN_POINT('Ctrl Pts',(3.05597305038916,45.3399761140204,-55.7499186083825));
#188404=CARTESIAN_POINT('Ctrl Pts',(3.04007792774143,45.34080344662,-55.8032432879277));
#188405=CARTESIAN_POINT('Ctrl Pts',(3.0270298121595,45.3414808214313,-55.8568906140328));
#188406=CARTESIAN_POINT('Ctrl Pts',(3.0269130014781,45.3414868854957,-55.8573708811394));
#188407=CARTESIAN_POINT('Ctrl Pts',(3.0267964073689,45.3414929380841,-55.8578511838465));
#188408=CARTESIAN_POINT('Ctrl Pts',(3.02668002962044,45.3414989792089,-55.8583315221214));
#188409=CARTESIAN_POINT('Ctrl Pts',(2.99362945634284,45.343214621947,-55.9947446729407));
#188410=CARTESIAN_POINT('Ctrl Pts',(2.97802127132288,45.3440061056745,-56.1340253984927));
#188411=CARTESIAN_POINT('Ctrl Pts',(2.9750567785663,45.3441559820078,-56.275384513425));
#188412=CARTESIAN_POINT('Ctrl Pts',(2.97470131764747,45.3441739531022,-56.2923343409352));
#188413=CARTESIAN_POINT('Ctrl Pts',(2.97452770112514,45.3441826962898,-56.3093140568108));
#188414=CARTESIAN_POINT('Ctrl Pts',(2.97452770112504,45.3441826962898,-56.3263223051814));
#188415=CARTESIAN_POINT('Origin',(4.02975864478749,45.7819570116602,-54.9597685279843));
#188416=CARTESIAN_POINT('Ctrl Pts',(4.49412912371062,45.2467848220336,-54.955514051414));
#188417=CARTESIAN_POINT('Ctrl Pts',(4.49662538953713,45.2465921108978,-55.2355242600995));
#188418=CARTESIAN_POINT('Ctrl Pts',(4.51630724703493,45.4845441383302,-55.3818234144886));
#188419=CARTESIAN_POINT('Ctrl Pts',(4.32798628668273,45.2596110100493,-54.9570167865889));
#188420=CARTESIAN_POINT('Ctrl Pts',(4.33057507588361,45.2594183143523,-55.2356268020846));
#188421=CARTESIAN_POINT('Ctrl Pts',(4.34919298261046,45.4956321595243,-55.3822130600194));
#188422=CARTESIAN_POINT('Ctrl Pts',(4.16179087919831,45.271725776299,-54.9584347299645));
#188423=CARTESIAN_POINT('Ctrl Pts',(4.16425328466829,45.2715506006274,-55.2357229472724));
#188424=CARTESIAN_POINT('Ctrl Pts',(4.18205130859575,45.5061051687682,-55.3825645302384));
#188425=CARTESIAN_POINT('Ctrl Pts',(3.9955429059226,45.2831291022416,-54.9597685279837));
#188426=CARTESIAN_POINT('Ctrl Pts',(3.99772850678838,45.2829791869159,-55.2358129028006));
#188427=CARTESIAN_POINT('Ctrl Pts',(4.01487932239355,45.5159631499936,-55.3828830175977));
#188428=CARTESIAN_POINT('',(4.49412912371054,45.2467848220337,-54.955514051414));
#188429=CARTESIAN_POINT('Origin',(0.000537877572094891,-12.1619648097437,
-48.139312741498));
#188430=CARTESIAN_POINT('Origin',(4.53261449406992,45.7453014980519,-54.955514051414));
#188431=CARTESIAN_POINT('Ctrl Pts',(4.47139039164512,45.4906548448225,-55.3863604038316));
#188432=CARTESIAN_POINT('Ctrl Pts',(4.43672341851431,45.2509948349534,-55.2414357815079));
#188433=CARTESIAN_POINT('Ctrl Pts',(4.40504871546121,45.2535845867532,-54.9609750843566));
#188434=CARTESIAN_POINT('Ctrl Pts',(4.55693219186144,45.4776416184101,-55.3719745613438));
#188435=CARTESIAN_POINT('Ctrl Pts',(4.55013513142212,45.2423482358409,-55.2221823835831));
#188436=CARTESIAN_POINT('Ctrl Pts',(4.57467261000343,45.2407903510215,-54.9401638606375));
#188437=CARTESIAN_POINT('Ctrl Pts',(4.64632152753948,45.4720450292502,-55.3906024673539));
#188438=CARTESIAN_POINT('Ctrl Pts',(4.67148999584471,45.2327453727894,-55.2479506024289));
#188439=CARTESIAN_POINT('Ctrl Pts',(4.75204967627739,45.2264957449184,-54.9756360521502));
#188440=CARTESIAN_POINT('Ctrl Pts',(4.78526231654569,45.4785391935409,-55.4758941943565));
#188441=CARTESIAN_POINT('Ctrl Pts',(4.85155529671713,45.2181899234016,-55.3600111127249));
#188442=CARTESIAN_POINT('Ctrl Pts',(5.02768780679811,45.2032674062285,-55.1236362709704));
#188443=CARTESIAN_POINT('Ctrl Pts',(4.83987531604392,45.4877168692796,-55.5336384447089));
#188444=CARTESIAN_POINT('Ctrl Pts',(4.91960725641842,45.2125663061104,-55.4362681462788));
#188445=CARTESIAN_POINT('Ctrl Pts',(5.13603339661033,45.193728067178,-55.2216356337625));
#188446=CARTESIAN_POINT('Ctrl Pts',(4.92459268013903,45.5188916935313,-55.6761597789111));
#188447=CARTESIAN_POINT('Ctrl Pts',(5.01304731809969,45.2048811773774,-55.6156547787452));
#188448=CARTESIAN_POINT('Ctrl Pts',(5.30411094495532,45.178640871319,-55.4541550621106));
#188449=CARTESIAN_POINT('Ctrl Pts',(4.95452456181636,45.5407314582523,-55.7600334675643));
#188450=CARTESIAN_POINT('Ctrl Pts',(5.03798355387793,45.2028686588532,-55.7195028114066));
#188451=CARTESIAN_POINT('Ctrl Pts',(5.3635004865346,45.1731436419375,-55.5870891782066));
#188452=CARTESIAN_POINT('Ctrl Pts',(4.99613220506374,45.6005437839053,-55.9629949137757));
#188453=CARTESIAN_POINT('Ctrl Pts',(5.04892271004841,45.2022954662183,-55.9561269088791));
#188454=CARTESIAN_POINT('Ctrl Pts',(5.44607043400786,45.165473055749,-55.8925951196528));
#188455=CARTESIAN_POINT('Ctrl Pts',(5.00281283901272,45.6402645497958,-56.0837699876345));
#188456=CARTESIAN_POINT('Ctrl Pts',(5.02368213791864,45.2047138612132,-56.0903086587098));
#188457=CARTESIAN_POINT('Ctrl Pts',(5.45934494047938,45.1642043041266,-56.0648075138964));
#188458=CARTESIAN_POINT('Ctrl Pts',(4.99898645253333,45.6858523253613,-56.217596972311));
#188459=CARTESIAN_POINT('Ctrl Pts',(4.97691572104403,45.208981116778,-56.2185887282702));
#188460=CARTESIAN_POINT('Ctrl Pts',(5.45177805579375,45.1649222445519,-56.2401344498715));
#188461=CARTESIAN_POINT('',(5.4533007853959,45.1647773033082,-56.1488993661993));
#188462=CARTESIAN_POINT('Ctrl Pts',(5.4533007853959,45.1647773033082,-56.1488993661993));
#188463=CARTESIAN_POINT('Ctrl Pts',(5.4533007853959,45.1647773033082,-56.0055674620926));
#188464=CARTESIAN_POINT('Ctrl Pts',(5.43788134491899,45.1662336319389,-55.8645506073504));
#188465=CARTESIAN_POINT('Ctrl Pts',(5.3637535993023,45.1731199385278,-55.5890146236025));
#188466=CARTESIAN_POINT('Ctrl Pts',(5.30482297007121,45.1785752810591,-55.4563513172782));
#188467=CARTESIAN_POINT('Ctrl Pts',(5.13740816361988,45.1936060305266,-55.2236271337424));
#188468=CARTESIAN_POINT('Ctrl Pts',(5.02927744515326,45.2031302456007,-55.1252272506259));
#188469=CARTESIAN_POINT('Ctrl Pts',(4.8419870330226,45.2189180089433,-55.0241597383142));
#188470=CARTESIAN_POINT('Ctrl Pts',(4.77441476074195,45.2245089469405,-54.9977644123794));
#188471=CARTESIAN_POINT('Ctrl Pts',(4.63647895825164,45.2356614644569,-54.9633053694043));
#188472=CARTESIAN_POINT('Ctrl Pts',(4.56605684297844,45.2412320189915,-54.9548634767888));
#188473=CARTESIAN_POINT('Ctrl Pts',(4.49412912371054,45.2467848220337,-54.955514051414));
#188474=CARTESIAN_POINT('Origin',(5.5,45.6625917098448,-56.1488993661993));
#188475=CARTESIAN_POINT('Origin',(5.5,45.6625917098448,-55.24995));
#188476=CARTESIAN_POINT('',(5.4533007853959,45.1647773033082,-55.24995));
#188477=CARTESIAN_POINT('Origin',(0.,-12.9675000200281,-60.42825533736));
#188478=CARTESIAN_POINT('Origin',(0.,-12.9675000200281,-60.42825533736));
#188479=CARTESIAN_POINT('Origin',(11.5,44.7861808691872,-55.24995));
#188480=CARTESIAN_POINT('',(11.402356187646,44.2958078622741,-55.9012688372262));
#188481=CARTESIAN_POINT('',(11.402356187646,44.2958078622741,-55.24995));
#188482=CARTESIAN_POINT('Origin',(11.5,44.7861808691872,-55.9012688372262));
#188483=CARTESIAN_POINT('Ctrl Pts',(12.0063585556897,44.8133988368639,-55.994729193492));
#188484=CARTESIAN_POINT('Ctrl Pts',(12.0432961608807,44.166306685066,-55.9714168634058));
#188485=CARTESIAN_POINT('Ctrl Pts',(11.4137787144181,44.2935713409156,-56.0670761670352));
#188486=CARTESIAN_POINT('Ctrl Pts',(11.9806229374089,44.7620399676921,-55.807622827858));
#188487=CARTESIAN_POINT('Ctrl Pts',(11.9479581346228,44.1860579521207,-55.8533126924881));
#188488=CARTESIAN_POINT('Ctrl Pts',(11.3625533696003,44.3036045439701,-55.7375862930343));
#188489=CARTESIAN_POINT('Ctrl Pts',(12.0342088179099,44.7020611377846,-55.618213877133));
#188490=CARTESIAN_POINT('Ctrl Pts',(11.9394256397489,44.1869658481102,-55.6416294054125));
#188491=CARTESIAN_POINT('Ctrl Pts',(11.4688213961376,44.2829757401497,-55.3880964587751));
#188492=CARTESIAN_POINT('Ctrl Pts',(12.2561025511723,44.5772902436325,-55.3546719045028));
#188493=CARTESIAN_POINT('Ctrl Pts',(12.1283065348885,44.1458422480371,-55.3228555036694));
#188494=CARTESIAN_POINT('Ctrl Pts',(11.9092544880125,44.1929801108985,-54.9017249097375));
#188495=CARTESIAN_POINT('Ctrl Pts',(12.4220919977125,44.5119954318218,-55.2820851549404));
#188496=CARTESIAN_POINT('Ctrl Pts',(12.3105489858414,44.1068007671422,-55.2078316060723));
#188497=CARTESIAN_POINT('Ctrl Pts',(12.2388210327084,44.124039351436,-54.76829873255));
#188498=CARTESIAN_POINT('Ctrl Pts',(12.5881212157209,44.4526104250917,-55.3021722916518));
#188499=CARTESIAN_POINT('Ctrl Pts',(12.5143053198889,44.0622780980818,-55.2189585580228));
#188500=CARTESIAN_POINT('Ctrl Pts',(12.5685011226759,44.0511648497893,-54.8168105684966));
#188501=CARTESIAN_POINT('',(12.4042000461459,44.0871753139748,-54.8084491013776));
#188502=CARTESIAN_POINT('Ctrl Pts',(12.4042000461459,44.0871753139748,-54.8084491013776));
#188503=CARTESIAN_POINT('Ctrl Pts',(12.3367608750176,44.101837196892,-54.8105480223147));
#188504=CARTESIAN_POINT('Ctrl Pts',(12.2704278259804,44.1161334117608,-54.8196434921937));
#188505=CARTESIAN_POINT('Ctrl Pts',(12.139979885891,44.1440180229867,-54.8518275298353));
#188506=CARTESIAN_POINT('Ctrl Pts',(12.0748636121213,44.1578169517408,-54.8753942762821));
#188507=CARTESIAN_POINT('Ctrl Pts',(11.8888586925018,44.1969229345987,-54.9642150903431));
#188508=CARTESIAN_POINT('Ctrl Pts',(11.7804034422216,44.2193085174476,-55.0453048135951));
#188509=CARTESIAN_POINT('Ctrl Pts',(11.5963788422947,44.2569088778311,-55.249379574632));
#188510=CARTESIAN_POINT('Ctrl Pts',(11.5252471488681,44.2712224279124,-55.366778251881));
#188511=CARTESIAN_POINT('Ctrl Pts',(11.4269419773585,44.2909287600296,-55.6267443723887));
#188512=CARTESIAN_POINT('Ctrl Pts',(11.402356187646,44.2958078622742,-55.7615802140858));
#188513=CARTESIAN_POINT('Ctrl Pts',(11.402356187646,44.2958078622741,-55.9012688372262));
#188514=CARTESIAN_POINT('Origin',(12.5104231251106,44.5757617009068,-54.8084491013774));
#188515=CARTESIAN_POINT('Ctrl Pts',(12.8921600942007,43.978899026433,-54.7926966592038));
#188516=CARTESIAN_POINT('Ctrl Pts',(12.9056883239205,43.9758363551094,-55.2210744412794));
#188517=CARTESIAN_POINT('Ctrl Pts',(13.0012809038513,44.3884784473357,-55.2865609247418));
#188518=CARTESIAN_POINT('Ctrl Pts',(12.7296669706488,44.015686029617,-54.798137418056));
#188519=CARTESIAN_POINT('Ctrl Pts',(12.743502264335,44.012594228669,-55.2216770608656));
#188520=CARTESIAN_POINT('Ctrl Pts',(12.8359967737338,44.4202801831072,-55.2911600797832));
#188521=CARTESIAN_POINT('Ctrl Pts',(12.5670134373343,44.0517782170206,-54.8033818322122));
#188522=CARTESIAN_POINT('Ctrl Pts',(12.5803648873612,44.0488388411796,-55.2222478741758));
#188523=CARTESIAN_POINT('Ctrl Pts',(12.6706421628547,44.4514812651211,-55.2954855956284));
#188524=CARTESIAN_POINT('Ctrl Pts',(12.4042000461459,44.0871753139748,-54.8084491013774));
#188525=CARTESIAN_POINT('Ctrl Pts',(12.4164090892806,44.0845209580867,-55.2227904669344));
#188526=CARTESIAN_POINT('Ctrl Pts',(12.5052115625551,44.4820814550629,-55.2995670619066));
#188527=CARTESIAN_POINT('',(12.8921600942007,43.978899026433,-54.7926966592038));
#188528=CARTESIAN_POINT('Origin',(0.36005249046184,-9.26137067386744,-40.4793207392961));
#188529=CARTESIAN_POINT('Origin',(13.0025618077027,44.4665581918916,-54.7926966592038));
#188530=CARTESIAN_POINT('Ctrl Pts',(13.0012809038513,44.3884784473357,-55.2865609247418));
#188531=CARTESIAN_POINT('Ctrl Pts',(12.9056883239205,43.9758363551094,-55.2210744412793));
#188532=CARTESIAN_POINT('Ctrl Pts',(12.8921600942007,43.978899026433,-54.7926966592038));
#188533=CARTESIAN_POINT('Ctrl Pts',(13.0654243459864,44.3636027691474,-55.2827944545873));
#188534=CARTESIAN_POINT('Ctrl Pts',(12.9784387965694,43.9593348061506,-55.2098637836594));
#188535=CARTESIAN_POINT('Ctrl Pts',(13.0193597758081,43.9501021457404,-54.7884376491597));
#188536=CARTESIAN_POINT('Ctrl Pts',(13.1299983077116,44.3395152672781,-55.2921354075477));
#188537=CARTESIAN_POINT('Ctrl Pts',(13.0552570243808,43.9418365181403,-55.2141810151918));
#188538=CARTESIAN_POINT('Ctrl Pts',(13.1474090807614,43.9206427834081,-54.8097712354121));
#188539=CARTESIAN_POINT('Ctrl Pts',(13.2502943581078,44.2958064353142,-55.3361304655099));
#188540=CARTESIAN_POINT('Ctrl Pts',(13.2011715416027,43.9084021006501,-55.25643129776));
#188541=CARTESIAN_POINT('Ctrl Pts',(13.3859583749986,43.8649843137035,-54.9019989045167));
#188542=CARTESIAN_POINT('Ctrl Pts',(13.3058135696287,44.2762488685004,-55.3707576859229));
#188543=CARTESIAN_POINT('Ctrl Pts',(13.2704159548698,43.8924342454859,-55.2940831522118));
#188544=CARTESIAN_POINT('Ctrl Pts',(13.496053992198,43.8388872267122,-54.9728361666051));
#188545=CARTESIAN_POINT('Ctrl Pts',(13.3986038888631,44.2453125071312,-55.4597899571993));
#188546=CARTESIAN_POINT('Ctrl Pts',(13.3860573147077,43.8656515577332,-55.3967868701307));
#188547=CARTESIAN_POINT('Ctrl Pts',(13.6800589131788,43.7948562869374,-55.1530004401584));
#188548=CARTESIAN_POINT('Ctrl Pts',(13.4362889542451,44.2338103823362,-55.514828855807));
#188549=CARTESIAN_POINT('Ctrl Pts',(13.4334072964209,43.8546223828157,-55.46277372953));
#188550=CARTESIAN_POINT('Ctrl Pts',(13.7547890917519,43.7767382792428,-55.2636104102621));
#188551=CARTESIAN_POINT('Ctrl Pts',(13.4867061057231,44.2229131048268,-55.6353022097904));
#188552=CARTESIAN_POINT('Ctrl Pts',(13.4931806941864,43.8407149886408,-55.6082533108594));
#188553=CARTESIAN_POINT('Ctrl Pts',(13.8547672339164,43.7524103115038,-55.5042410247415));
#188554=CARTESIAN_POINT('Ctrl Pts',(13.5,44.2234307110673,-55.7021231738994));
#188555=CARTESIAN_POINT('Ctrl Pts',(13.5063795391634,43.8376645208725,-55.6900657479952));
#188556=CARTESIAN_POINT('Ctrl Pts',(13.8811292609786,43.7459411266109,-55.6370500544614));
#188557=CARTESIAN_POINT('Ctrl Pts',(13.5,44.2316053598055,-55.7692503840715));
#188558=CARTESIAN_POINT('Ctrl Pts',(13.5,43.83922597116,-55.7692503840715));
#188559=CARTESIAN_POINT('Ctrl Pts',(13.8811292719168,43.7459411239336,-55.7692503840715));
#188560=CARTESIAN_POINT('',(13.8811292719168,43.7459411239337,-55.7692503840715));
#188561=CARTESIAN_POINT('Ctrl Pts',(13.8811292719168,43.7459411239336,-55.7692503840715));
#188562=CARTESIAN_POINT('Ctrl Pts',(13.8811292682097,43.745941124841,-55.7244458157436));
#188563=CARTESIAN_POINT('Ctrl Pts',(13.878105549578,43.7466831296689,-55.679736138466));
#188564=CARTESIAN_POINT('Ctrl Pts',(13.8722047277525,43.7481272051964,-55.6355346293339));
#188565=CARTESIAN_POINT('Ctrl Pts',(13.8662038608382,43.7495957642058,-55.590583708673));
#188566=CARTESIAN_POINT('Ctrl Pts',(13.8572273197945,43.7517904587082,-55.5461569097345));
#188567=CARTESIAN_POINT('Ctrl Pts',(13.8453776205413,43.7546819864356,-55.5026858819466));
#188568=CARTESIAN_POINT('Ctrl Pts',(13.8344632356934,43.7573452815743,-55.462646087107));
#188569=CARTESIAN_POINT('Ctrl Pts',(13.8211106222446,43.7605999346755,-55.4234162320198));
#188570=CARTESIAN_POINT('Ctrl Pts',(13.8053642538662,43.7644316776827,-55.3853473456883));
#188571=CARTESIAN_POINT('Ctrl Pts',(13.8051683359555,43.7644793526174,-55.3848736887475));
#188572=CARTESIAN_POINT('Ctrl Pts',(13.8049720511568,43.7645271159922,-55.3844002212373));
#188573=CARTESIAN_POINT('Ctrl Pts',(13.8047753996222,43.7645749677634,-55.3839269439647));
#188574=CARTESIAN_POINT('Ctrl Pts',(13.7718577708332,43.7725849069898,-55.3047047522695));
#188575=CARTESIAN_POINT('Ctrl Pts',(13.728178051487,43.7831849346504,-55.2296008411665));
#188576=CARTESIAN_POINT('Ctrl Pts',(13.6758172364472,43.7957998172932,-55.1617614773765));
#188577=CARTESIAN_POINT('Ctrl Pts',(13.6492141753589,43.8022090852412,-55.127294199934));
#188578=CARTESIAN_POINT('Ctrl Pts',(13.6203708268795,43.8091382966098,-55.0947027771945));
#188579=CARTESIAN_POINT('Ctrl Pts',(13.5895638615798,43.8165110245856,-55.0644031256242));
#188580=CARTESIAN_POINT('Ctrl Pts',(13.5890610147607,43.8166313659687,-55.0639085594356));
#188581=CARTESIAN_POINT('Ctrl Pts',(13.5885576424949,43.8167518260625,-55.0634146006456));
#188582=CARTESIAN_POINT('Ctrl Pts',(13.5880537459902,43.8168724045334,-55.0629212511039));
#188583=CARTESIAN_POINT('Ctrl Pts',(13.5330913533177,43.8300244728729,-55.0091092659332));
#188584=CARTESIAN_POINT('Ctrl Pts',(13.4715943783219,43.8446517471115,-54.9620890033291));
#188585=CARTESIAN_POINT('Ctrl Pts',(13.4054646975447,43.8602521578852,-54.9231113264467));
#188586=CARTESIAN_POINT('Ctrl Pts',(13.3615129962558,43.8706206427509,-54.8972056334033));
#188587=CARTESIAN_POINT('Ctrl Pts',(13.3155161569027,43.8814186797025,-54.8748524249676));
#188588=CARTESIAN_POINT('Ctrl Pts',(13.2680436044718,43.8924962435662,-54.8564136580933));
#188589=CARTESIAN_POINT('Ctrl Pts',(13.2675902582944,43.8926020304046,-54.8562375743555));
#188590=CARTESIAN_POINT('Ctrl Pts',(13.267136793244,43.89270783907,-54.8560618534164));
#188591=CARTESIAN_POINT('Ctrl Pts',(13.2666832096553,43.8928136694707,-54.8558864954404));
#188592=CARTESIAN_POINT('Ctrl Pts',(13.2297963270863,43.9014201395016,-54.8416258184039));
#188593=CARTESIAN_POINT('Ctrl Pts',(13.1921658567097,43.9101602729064,-54.82976688078));
#188594=CARTESIAN_POINT('Ctrl Pts',(13.1539812007031,43.9189886853961,-54.8202850097806));
#188595=CARTESIAN_POINT('Ctrl Pts',(13.1156262419325,43.9278564724202,-54.8107608498357));
#188596=CARTESIAN_POINT('Ctrl Pts',(13.0767111408946,43.9368135671448,-54.8036348844097));
#188597=CARTESIAN_POINT('Ctrl Pts',(13.037416426663,43.9458157565233,-54.7989332461647));
#188598=CARTESIAN_POINT('Ctrl Pts',(12.9988139657374,43.9546593547151,-54.7943144364803));
#188599=CARTESIAN_POINT('Ctrl Pts',(12.9598441948041,43.9635466980804,-54.7920353122774));
#188600=CARTESIAN_POINT('Ctrl Pts',(12.9206817922385,43.9724341406896,-54.7921703301218));
#188601=CARTESIAN_POINT('Ctrl Pts',(12.9111849603394,43.9745893340114,-54.7922030717742));
#188602=CARTESIAN_POINT('Ctrl Pts',(12.9016768542622,43.976744516291,-54.7923780107907));
#188603=CARTESIAN_POINT('Ctrl Pts',(12.8921600942007,43.978899026433,-54.7926966592038));
#188604=CARTESIAN_POINT('Origin',(14.,44.2316053598044,-55.7692503840718));
#188605=CARTESIAN_POINT('Origin',(14.,44.2316053598056,-55.24995));
#188606=CARTESIAN_POINT('',(13.8811292719168,43.7459411239336,-55.24995));
#188607=CARTESIAN_POINT('Origin',(0.,-12.9675000200281,-60.42825533736));
#188608=CARTESIAN_POINT('Origin',(0.,-12.9675000200281,-60.42825533736));
#188609=CARTESIAN_POINT('Origin',(20.,42.4196614549321,-55.24995));
#188610=CARTESIAN_POINT('',(19.8301846741669,41.9493820112901,-55.74995));
#188611=CARTESIAN_POINT('Origin',(20.,42.4196614549321,-55.74995));
#188612=CARTESIAN_POINT('',(19.8301846741669,41.9493820112901,-55.24995));
#188613=CARTESIAN_POINT('Ctrl Pts',(20.5,42.4196614549321,-55.74995));
#188614=CARTESIAN_POINT('Ctrl Pts',(20.5,41.7075153736088,-55.7499499999999));
#188615=CARTESIAN_POINT('Ctrl Pts',(19.8301846741669,41.9493820112901,-55.74995));
#188616=CARTESIAN_POINT('Ctrl Pts',(20.5,42.4196614460347,-55.6824493590803));
#188617=CARTESIAN_POINT('Ctrl Pts',(20.4999999995541,41.7075153734334,-55.7174757167052));
#188618=CARTESIAN_POINT('Ctrl Pts',(19.8301846986023,41.9493820024666,-55.6149487156912));
#188619=CARTESIAN_POINT('Ctrl Pts',(20.514053798786,42.4095322277552,-55.614564639731));
#188620=CARTESIAN_POINT('Ctrl Pts',(20.4987004734351,41.7075927453749,-55.6840485748926));
#188621=CARTESIAN_POINT('Ctrl Pts',(19.8580536242861,41.939338788612,-55.4791792828035));
#188622=CARTESIAN_POINT('Ctrl Pts',(20.5667184545259,42.3713246265636,-55.4916091232479));
#188623=CARTESIAN_POINT('Ctrl Pts',(20.5049952302095,41.704035376344,-55.6029041515887));
#188624=CARTESIAN_POINT('Ctrl Pts',(19.9624885940201,41.9014556000366,-55.2332682431543));
#188625=CARTESIAN_POINT('Ctrl Pts',(20.6054777681041,42.3431217478432,-55.4359504896237));
#188626=CARTESIAN_POINT('Ctrl Pts',(20.5131880407467,41.7002281457635,-55.5554275272938));
#188627=CARTESIAN_POINT('Ctrl Pts',(20.0393490386551,41.8734921844523,-55.1219509819824));
#188628=CARTESIAN_POINT('Ctrl Pts',(20.6991000803093,42.274341317199,-55.3453480693239));
#188629=CARTESIAN_POINT('Ctrl Pts',(20.5562936263709,41.682844191329,-55.4545960701533));
#188630=CARTESIAN_POINT('Ctrl Pts',(20.2250038078484,41.8052957533979,-54.9407461359128));
#188631=CARTESIAN_POINT('Ctrl Pts',(20.7546446997872,42.233248744276,-55.3096493999238));
#188632=CARTESIAN_POINT('Ctrl Pts',(20.5906196334233,41.6694809696074,-55.401758477076));
#188633=CARTESIAN_POINT('Ctrl Pts',(20.3351498160899,41.7645520870248,-54.8693487992283));
#188634=CARTESIAN_POINT('Ctrl Pts',(20.8729715384853,42.1447441871192,-55.2621717596744));
#188635=CARTESIAN_POINT('Ctrl Pts',(20.6877494411454,41.6322368154735,-55.3113977742726));
#188636=CARTESIAN_POINT('Ctrl Pts',(20.569794123189,41.6767990021169,-54.774393519968));
#188637=CARTESIAN_POINT('Ctrl Pts',(20.936865425116,42.0964926027484,-55.24995));
#188638=CARTESIAN_POINT('Ctrl Pts',(20.7498635250281,41.608586604298,-55.2730231656551));
#188639=CARTESIAN_POINT('Ctrl Pts',(20.6965038706024,41.6289544421905,-54.7499500128377));
#188640=CARTESIAN_POINT('Ctrl Pts',(21.,42.0482945870964,-55.24995));
#188641=CARTESIAN_POINT('Ctrl Pts',(20.8216939078753,41.5811683327377,-55.2499499999999));
#188642=CARTESIAN_POINT('Ctrl Pts',(20.8216939078753,41.5811683327377,-54.74995));
#188643=CARTESIAN_POINT('',(20.8216939078753,41.5811683327377,-54.74995));
#188644=CARTESIAN_POINT('Ctrl Pts',(20.8216939078753,41.5811683327377,-54.74995));
#188645=CARTESIAN_POINT('Ctrl Pts',(20.7819408740053,41.5963424062421,-54.7499500040765));
#188646=CARTESIAN_POINT('Ctrl Pts',(20.7422583702479,41.6114370651536,-54.7524107511961));
#188647=CARTESIAN_POINT('Ctrl Pts',(20.7028910580564,41.6263644244518,-54.7572302478587));
#188648=CARTESIAN_POINT('Ctrl Pts',(20.6627696815177,41.6415777110541,-54.7621420599578));
#188649=CARTESIAN_POINT('Ctrl Pts',(20.6229744854673,41.6566176734327,-54.769503891898));
#188650=CARTESIAN_POINT('Ctrl Pts',(20.5837549178884,41.671393724625,-54.7792610196498));
#188651=CARTESIAN_POINT('Ctrl Pts',(20.5448758646516,41.686041486352,-54.7889334335166));
#188652=CARTESIAN_POINT('Ctrl Pts',(20.5065612917292,41.7004303395793,-54.8009599654576));
#188653=CARTESIAN_POINT('Ctrl Pts',(20.4690629498568,41.7144677618964,-54.8153366743303));
#188654=CARTESIAN_POINT('Ctrl Pts',(20.4635146440735,41.7165447580391,-54.8174638717742));
#188655=CARTESIAN_POINT('Ctrl Pts',(20.4579842421571,41.7186140458698,-54.8196426059304));
#188656=CARTESIAN_POINT('Ctrl Pts',(20.452472600707,41.7206753085659,-54.8218729523577));
#188657=CARTESIAN_POINT('Ctrl Pts',(20.4520370571492,41.7208381946492,-54.8220491998562));
#188658=CARTESIAN_POINT('Ctrl Pts',(20.4516016002718,41.7210010421259,-54.8222257818663));
#188659=CARTESIAN_POINT('Ctrl Pts',(20.451166230457,41.7211638508663,-54.8224026982642));
#188660=CARTESIAN_POINT('Ctrl Pts',(20.3795793872688,41.747934112313,-54.8514926489224));
#188661=CARTESIAN_POINT('Ctrl Pts',(20.3107136334647,41.7735197491871,-54.8894829736804));
#188662=CARTESIAN_POINT('Ctrl Pts',(20.2468906651867,41.7971168064876,-54.9352464330092));
#188663=CARTESIAN_POINT('Ctrl Pts',(20.2064337192117,41.8120748207908,-54.9642555789586));
#188664=CARTESIAN_POINT('Ctrl Pts',(20.1680024696355,41.8262340118394,-54.9963875370291));
#188665=CARTESIAN_POINT('Ctrl Pts',(20.1321785809257,41.8393931763607,-55.0313510893754));
#188666=CARTESIAN_POINT('Ctrl Pts',(20.1316789419887,41.8395767083895,-55.0318387291252));
#188667=CARTESIAN_POINT('Ctrl Pts',(20.1311797709301,41.8397600607401,-55.0323269633832));
#188668=CARTESIAN_POINT('Ctrl Pts',(20.1306810690887,41.839943232968,-55.0328157906737));
#188669=CARTESIAN_POINT('Ctrl Pts',(20.0684907293821,41.8627856252234,-55.093774729926));
#188670=CARTESIAN_POINT('Ctrl Pts',(20.0135863047548,41.8828310295748,-55.1639774211747));
#188671=CARTESIAN_POINT('Ctrl Pts',(19.9685212499206,41.8992323516663,-55.2406426510358));
#188672=CARTESIAN_POINT('Ctrl Pts',(19.9467038340058,41.9071727495408,-55.2777587094149));
#188673=CARTESIAN_POINT('Ctrl Pts',(19.9271921606274,41.9142591786556,-55.3163901520181));
#188674=CARTESIAN_POINT('Ctrl Pts',(19.9102738131902,41.9203962134609,-55.3562250735781));
#188675=CARTESIAN_POINT('Ctrl Pts',(19.9100688061412,41.9204705786079,-55.356707770824));
#188676=CARTESIAN_POINT('Ctrl Pts',(19.9098641753246,41.9205448062603,-55.3571906629275));
#188677=CARTESIAN_POINT('Ctrl Pts',(19.9096599209391,41.9206188963538,-55.3576737490625));
#188678=CARTESIAN_POINT('Ctrl Pts',(19.8950560556066,41.9259162207946,-55.3922136432421));
#188679=CARTESIAN_POINT('Ctrl Pts',(19.8824223932141,41.9304937150683,-55.4276284386807));
#188680=CARTESIAN_POINT('Ctrl Pts',(19.8717730238587,41.934349206398,-55.4637108040147));
#188681=CARTESIAN_POINT('Ctrl Pts',(19.8611060292098,41.9382110787783,-55.4998528876529));
#188682=CARTESIAN_POINT('Ctrl Pts',(19.8524296011668,41.9413486539406,-55.5366659074257));
#188683=CARTESIAN_POINT('Ctrl Pts',(19.8458033807233,41.9437431691666,-55.5739608322421));
#188684=CARTESIAN_POINT('Ctrl Pts',(19.8393763220395,41.9460657133694,-55.6101347978451));
#188685=CARTESIAN_POINT('Ctrl Pts',(19.8348780094478,41.9476892093276,-55.6467631869937));
#188686=CARTESIAN_POINT('Ctrl Pts',(19.832407933269,41.9485802658015,-55.6836754313746));
#188687=CARTESIAN_POINT('Ctrl Pts',(19.8309355210528,41.9491114244956,-55.7056788173516));
#188688=CARTESIAN_POINT('Ctrl Pts',(19.8301846781792,41.9493820098413,-55.727783032076));
#188689=CARTESIAN_POINT('Ctrl Pts',(19.8301846741669,41.9493820112901,-55.74995));
#188690=CARTESIAN_POINT('Origin',(21.,42.0482945870964,-54.74995));
#188691=CARTESIAN_POINT('Origin',(0.,-12.9675000200281,-54.74995));
#188692=CARTESIAN_POINT('',(21.3174485247294,41.3893444859658,-54.74995));
#188693=CARTESIAN_POINT('Origin',(0.,-12.9675000200281,-54.74995));
#188694=CARTESIAN_POINT('Origin',(21.5,41.8548280612684,-54.74995));
#188695=CARTESIAN_POINT('Ctrl Pts',(21.4248453217881,41.9155375404332,-55.2558060812404));
#188696=CARTESIAN_POINT('Ctrl Pts',(21.2373195046609,41.4189578841863,-55.287441243185));
#188697=CARTESIAN_POINT('Ctrl Pts',(21.16696734776,41.4480708968741,-54.7603378535211));
#188698=CARTESIAN_POINT('Ctrl Pts',(21.5755391452687,41.7984791341951,-55.2320625140271));
#188699=CARTESIAN_POINT('Ctrl Pts',(21.3763896092289,41.3649167149439,-55.2050098024457));
#188700=CARTESIAN_POINT('Ctrl Pts',(21.4662789569412,41.3318824788528,-54.7124836923955));
#188701=CARTESIAN_POINT('Ctrl Pts',(21.7343014022012,41.6710710097369,-55.2811995739867));
#188702=CARTESIAN_POINT('Ctrl Pts',(21.5979757909207,41.2778556958534,-55.2005038282256));
#188703=CARTESIAN_POINT('Ctrl Pts',(21.7817024793388,41.2055241661255,-54.8106147759211));
#188704=CARTESIAN_POINT('Ctrl Pts',(21.9601498093564,41.4868864651448,-55.4991545802739));
#188705=CARTESIAN_POINT('Ctrl Pts',(21.9275787592104,41.1463611545831,-55.4234682828707));
#188706=CARTESIAN_POINT('Ctrl Pts',(22.2307370972024,41.022808583346,-55.2471700554705));
#188707=CARTESIAN_POINT('Ctrl Pts',(22.022056389361,41.4349102113225,-55.664992125143));
#188708=CARTESIAN_POINT('Ctrl Pts',(22.0359917549909,41.102279443332,-55.6402740406839));
#188709=CARTESIAN_POINT('Ctrl Pts',(22.3539243365364,40.9712467786474,-55.5796280897733));
#188710=CARTESIAN_POINT('Ctrl Pts',(21.9927742364993,41.4593862584412,-55.8338983075843));
#188711=CARTESIAN_POINT('Ctrl Pts',(21.9870900777401,41.1221165139417,-55.8584680429781));
#188712=CARTESIAN_POINT('Ctrl Pts',(22.2956640008395,40.9955277705935,-55.9182451071506));
#188713=CARTESIAN_POINT('',(22.3089577584378,40.9899884313956,-55.74995));
#188714=CARTESIAN_POINT('Ctrl Pts',(22.3089577584378,40.9899884313956,-55.74995));
#188715=CARTESIAN_POINT('Ctrl Pts',(22.3089183239675,40.9900047357485,-55.6813689895721));
#188716=CARTESIAN_POINT('Ctrl Pts',(22.302201262956,40.9927833854558,-55.6142067014708));
#188717=CARTESIAN_POINT('Ctrl Pts',(22.2754057040688,41.0038504086268,-55.4827195699211));
#188718=CARTESIAN_POINT('Ctrl Pts',(22.2547133491493,41.0123915139066,-55.4169521642664));
#188719=CARTESIAN_POINT('Ctrl Pts',(22.2024041852375,41.0339277820542,-55.2940250464356));
#188720=CARTESIAN_POINT('Ctrl Pts',(22.1708638248328,41.0468920147473,-55.2362766810164));
#188721=CARTESIAN_POINT('Ctrl Pts',(22.0969884151167,41.0771560766471,-55.1282103371706));
#188722=CARTESIAN_POINT('Ctrl Pts',(22.0534159784586,41.094959425968,-55.0766846507022));
#188723=CARTESIAN_POINT('Ctrl Pts',(21.9138847547741,41.1517377505672,-54.9404994200361));
#188724=CARTESIAN_POINT('Ctrl Pts',(21.8055277290851,41.1955447566139,-54.8700273400709));
#188725=CARTESIAN_POINT('Ctrl Pts',(21.568431879825,41.290395306512,-54.7739654680142));
#188726=CARTESIAN_POINT('Ctrl Pts',(21.4452658848218,41.3392175880729,-54.74995));
#188727=CARTESIAN_POINT('Ctrl Pts',(21.3174485247294,41.3893444859658,-54.74995));
#188728=CARTESIAN_POINT('Origin',(22.5,41.4520521304013,-55.74995));
#188729=CARTESIAN_POINT('Origin',(22.5,41.4520521304013,-55.24995));
#188730=CARTESIAN_POINT('',(22.3089577584378,40.9899884313956,-55.24995));
#188731=CARTESIAN_POINT('Origin',(0.,-12.9675000200281,-60.5010370523947));
#188732=CARTESIAN_POINT('Origin',(0.,-12.9675000200281,-60.5010370523947));
#188733=CARTESIAN_POINT('Origin',(25.8159964412441,44.9247229809868,-55.24995));
#188734=CARTESIAN_POINT('',(23.7796330855957,40.3581899105085,-52.64995));
#188735=CARTESIAN_POINT('',(23.7796330855957,40.3581899105085,-55.24995));
#188736=CARTESIAN_POINT('Origin',(25.8159964412441,44.9247229809868,-52.64995));
#188737=CARTESIAN_POINT('Origin',(0.,-12.9675000200281,-54.74995));
#188738=CARTESIAN_POINT('',(23.9945234557419,-66.1968434349636,-54.74995));
#188739=CARTESIAN_POINT('Origin',(24.2,-66.6526716808631,-54.74995));
#188740=CARTESIAN_POINT('',(24.0682702937655,-66.1635386067456,-54.74995));
#188741=CARTESIAN_POINT('Origin',(24.2743783673579,-66.6190816475223,-54.74995));
#188742=CARTESIAN_POINT('Origin',(0.,-12.9675000200281,-54.74995));
#188743=CARTESIAN_POINT('Ctrl Pts',(24.2,-66.6526716808631,-55.24995));
#188744=CARTESIAN_POINT('Ctrl Pts',(23.9945234557419,-66.1968434349636,
-55.24995));
#188745=CARTESIAN_POINT('Ctrl Pts',(23.9945234557419,-66.1968434349636,
-54.74995));
#188746=CARTESIAN_POINT('Ctrl Pts',(24.1371955572435,-66.7092931820382,
-55.24995));
#188747=CARTESIAN_POINT('Ctrl Pts',(23.9202432240961,-66.2303271978257,
-55.2764502978682));
#188748=CARTESIAN_POINT('Ctrl Pts',(23.8699830688991,-66.2529832826787,
-54.7499500150097));
#188749=CARTESIAN_POINT('Ctrl Pts',(24.0753940809144,-66.764472406879,-55.2615406660682));
#188750=CARTESIAN_POINT('Ctrl Pts',(23.8581370153758,-66.2582349963978,
-55.3179716549212));
#188751=CARTESIAN_POINT('Ctrl Pts',(23.7474276190468,-66.3076948875735,
-54.7731313367517));
#188752=CARTESIAN_POINT('Ctrl Pts',(23.9567432347527,-66.8694948932304,
-55.3084792096817));
#188753=CARTESIAN_POINT('Ctrl Pts',(23.7601274312421,-66.3025641007665,
-55.4174636561498));
#188754=CARTESIAN_POINT('Ctrl Pts',(23.5121407959317,-66.4118256516783,
-54.867008414748));
#188755=CARTESIAN_POINT('Ctrl Pts',(23.902316841733,-66.9171958169871,-55.3428841126209));
#188756=CARTESIAN_POINT('Ctrl Pts',(23.7282344734586,-66.3172128520127,
-55.4737170925055));
#188757=CARTESIAN_POINT('Ctrl Pts',(23.4042122584794,-66.4591215590598,
-54.9358182281615));
#188758=CARTESIAN_POINT('Ctrl Pts',(23.8072473920369,-66.9999887868491,
-55.4336221821879));
#188759=CARTESIAN_POINT('Ctrl Pts',(23.6919934707232,-66.3346728811278,
-55.5807863787511));
#188760=CARTESIAN_POINT('Ctrl Pts',(23.2156877780054,-66.5412115519831,
-55.117294361456));
#188761=CARTESIAN_POINT('Ctrl Pts',(23.7684105820677,-67.0335141101085,
-55.4886013829516));
#188762=CARTESIAN_POINT('Ctrl Pts',(23.6899497583265,-66.3364476351196,
-55.6278104638636));
#188763=CARTESIAN_POINT('Ctrl Pts',(23.138673673191,-66.5744522205999,-55.227252767375));
#188764=CARTESIAN_POINT('Ctrl Pts',(23.7144942998795,-67.079931038232,-55.6126301527277));
#188765=CARTESIAN_POINT('Ctrl Pts',(23.6944387661923,-66.3359499016387,
-55.7013955638849));
#188766=CARTESIAN_POINT('Ctrl Pts',(23.0317566828166,-66.6204750325317,
-55.4753103039836));
#188767=CARTESIAN_POINT('Ctrl Pts',(23.7,-67.0923340220896,-55.6800435061715));
#188768=CARTESIAN_POINT('Ctrl Pts',(23.6999999982635,-66.3340176139022,
-55.7259208430489));
#188769=CARTESIAN_POINT('Ctrl Pts',(23.0030142327697,-66.6327727060053,
-55.6101370134438));
#188770=CARTESIAN_POINT('Ctrl Pts',(23.7,-67.0923340267327,-55.74995));
#188771=CARTESIAN_POINT('Ctrl Pts',(23.6999999999999,-66.3340176133293,
-55.74995));
#188772=CARTESIAN_POINT('Ctrl Pts',(23.0030142220336,-66.6327727106072,
-55.74995));
#188773=CARTESIAN_POINT('',(23.0030142220336,-66.6327727106072,-55.74995));
#188774=CARTESIAN_POINT('Origin',(23.2,-67.0923340267327,-55.74995));
#188775=CARTESIAN_POINT('Ctrl Pts',(23.0030142220336,-66.6327727106072,
-55.74995));
#188776=CARTESIAN_POINT('Ctrl Pts',(23.0030142252181,-66.6327727092422,
-55.7084794961837));
#188777=CARTESIAN_POINT('Ctrl Pts',(23.0055473075491,-66.6316889244747,
-55.6672305708313));
#188778=CARTESIAN_POINT('Ctrl Pts',(23.01056277729,-66.6295393332012,-55.6264611420265));
#188779=CARTESIAN_POINT('Ctrl Pts',(23.0156442349954,-66.62736146,-55.5851553144879));
#188780=CARTESIAN_POINT('Ctrl Pts',(23.0232736525723,-66.6240896154022,
-55.5443421797598));
#188781=CARTESIAN_POINT('Ctrl Pts',(23.0333489722999,-66.6197635354292,
-55.5042845968465));
#188782=CARTESIAN_POINT('Ctrl Pts',(23.0435966387888,-66.6153634542441,
-55.4635417955116));
#188783=CARTESIAN_POINT('Ctrl Pts',(23.0563743830217,-66.6098728426923,
-55.4235811788327));
#188784=CARTESIAN_POINT('Ctrl Pts',(23.0715270926204,-66.6033540441774,
-55.3846656949085));
#188785=CARTESIAN_POINT('Ctrl Pts',(23.075698862771,-66.6015593203436,-55.373951673553));
#188786=CARTESIAN_POINT('Ctrl Pts',(23.08005038839,-66.5996867754406,-55.3633167653533));
#188787=CARTESIAN_POINT('Ctrl Pts',(23.0845778500673,-66.5977379631867,
-55.3527661917799));
#188788=CARTESIAN_POINT('Ctrl Pts',(23.084790216786,-66.5976465515099,-55.3522713028445));
#188789=CARTESIAN_POINT('Ctrl Pts',(23.0850029782865,-66.5975549687209,
-55.3517765816014));
#188790=CARTESIAN_POINT('Ctrl Pts',(23.0852161343291,-66.5974632149135,
-55.3512820284305));
#188791=CARTESIAN_POINT('Ctrl Pts',(23.1225303099352,-66.5814011899272,
-55.2647076876707));
#188792=CARTESIAN_POINT('Ctrl Pts',(23.1713738964051,-66.5603327052685,
-55.1848774594373));
#188793=CARTESIAN_POINT('Ctrl Pts',(23.2296539151218,-66.5350590387655,
-55.1136222625289));
#188794=CARTESIAN_POINT('Ctrl Pts',(23.2542820784798,-66.5243788090573,
-55.0835110053912));
#188795=CARTESIAN_POINT('Ctrl Pts',(23.2805947528019,-66.5129478823946,
-55.0549311560842));
#188796=CARTESIAN_POINT('Ctrl Pts',(23.3084314920874,-66.5008277482104,
-55.0280211962633));
#188797=CARTESIAN_POINT('Ctrl Pts',(23.3089371697075,-66.5006075758495,
-55.0275323543663));
#188798=CARTESIAN_POINT('Ctrl Pts',(23.3094433520675,-66.5003871752661,
-55.0270440618915));
#188799=CARTESIAN_POINT('Ctrl Pts',(23.3099500382032,-66.5001665468298,
-55.0265563196877));
#188800=CARTESIAN_POINT('Ctrl Pts',(23.3737418241067,-66.4723894260785,
-54.9651495748625));
#188801=CARTESIAN_POINT('Ctrl Pts',(23.4438814283176,-66.4417108192607,
-54.9137085371825));
#188802=CARTESIAN_POINT('Ctrl Pts',(23.5191429186078,-66.4085890914668,
-54.8723032869094));
#188803=CARTESIAN_POINT('Ctrl Pts',(23.5545073851334,-66.3930255910721,
-54.8528474592129));
#188804=CARTESIAN_POINT('Ctrl Pts',(23.59100222619,-66.3769228800036,-54.8356069181236));
#188805=CARTESIAN_POINT('Ctrl Pts',(23.6284978920678,-66.3603295348338,
-54.8205860088575));
#188806=CARTESIAN_POINT('Ctrl Pts',(23.6289267193329,-66.360139761465,-54.8204142189909));
#188807=CARTESIAN_POINT('Ctrl Pts',(23.6293556721511,-66.359949926291,-54.8202427216662));
#188808=CARTESIAN_POINT('Ctrl Pts',(23.629784750377,-66.3597600293637,-54.8200715168436));
#188809=CARTESIAN_POINT('Ctrl Pts',(23.67833901584,-66.3382713933413,-54.8006980695174));
#188810=CARTESIAN_POINT('Ctrl Pts',(23.7276801213795,-66.3163541582091,
-54.7853871133686));
#188811=CARTESIAN_POINT('Ctrl Pts',(23.7776797138642,-66.2940596674702,
-54.7740684617324));
#188812=CARTESIAN_POINT('Ctrl Pts',(23.8282083296008,-66.2715292887288,
-54.7626300525221));
#188813=CARTESIAN_POINT('Ctrl Pts',(23.8794098794649,-66.2486134489516,
-54.7552688611601));
#188814=CARTESIAN_POINT('Ctrl Pts',(23.93115878902,-66.2253609159868,-54.7519649331453));
#188815=CARTESIAN_POINT('Ctrl Pts',(23.9521926643963,-66.2159096853277,
-54.7506220176963));
#188816=CARTESIAN_POINT('Ctrl Pts',(23.9733170103899,-66.2064027967323,
-54.7499500025558));
#188817=CARTESIAN_POINT('Ctrl Pts',(23.9945234557419,-66.1968434349636,
-54.74995));
#188818=CARTESIAN_POINT('Origin',(23.2,-67.0923340267327,-55.24995));
#188819=CARTESIAN_POINT('',(23.0030142220336,-66.6327727106072,-55.24995));
#188820=CARTESIAN_POINT('Origin',(0.,-12.9675000200281,-60.42825533736));
#188821=CARTESIAN_POINT('Origin',(0.,-12.9675000200281,-60.42825533736));
#188822=CARTESIAN_POINT('Origin',(17.55,-69.1790215814778,-55.24995));
#188823=CARTESIAN_POINT('',(17.4009870515814,-68.7017426890012,-55.74995));
#188824=CARTESIAN_POINT('',(17.4009870515814,-68.7017426890012,-55.24995));
#188825=CARTESIAN_POINT('Origin',(17.55,-69.1790215814778,-55.74995));
#188826=CARTESIAN_POINT('Ctrl Pts',(17.0433420738134,-69.1844099825972,
-55.8294677650393));
#188827=CARTESIAN_POINT('Ctrl Pts',(17.0390945871937,-68.8146441411288,
-55.8476657194646));
#188828=CARTESIAN_POINT('Ctrl Pts',(17.3877596852339,-68.7058888483382,
-55.909104778956));
#188829=CARTESIAN_POINT('Ctrl Pts',(17.0589933399128,-69.1745693542014,
-55.7377938248974));
#188830=CARTESIAN_POINT('Ctrl Pts',(17.0627281269977,-68.8074648626002,
-55.7356378606241));
#188831=CARTESIAN_POINT('Ctrl Pts',(17.4188481420652,-68.6961356562758,
-55.7256234362817));
#188832=CARTESIAN_POINT('Ctrl Pts',(17.0466637029569,-69.1823667222349,
-55.6406520746839));
#188833=CARTESIAN_POINT('Ctrl Pts',(17.0433869297458,-68.8133616424342,
-55.6136877993486));
#188834=CARTESIAN_POINT('Ctrl Pts',(17.3943527552328,-68.7038643204319,
-55.5311773838691));
#188835=CARTESIAN_POINT('Ctrl Pts',(16.9846573898727,-69.2209669761278,
-55.4940755209577));
#188836=CARTESIAN_POINT('Ctrl Pts',(16.9545279172638,-68.8401687966803,
-55.4409633820653));
#188837=CARTESIAN_POINT('Ctrl Pts',(17.2712219065013,-68.7421173320939,
-55.237857759257));
#188838=CARTESIAN_POINT('Ctrl Pts',(16.9465498226589,-69.2446125343844,
-55.438535909464));
#188839=CARTESIAN_POINT('Ctrl Pts',(16.8998247159699,-68.8566269554238,
-55.378474281339));
#188840=CARTESIAN_POINT('Ctrl Pts',(17.1955506950046,-68.7655509085055,
-55.1267370897427));
#188841=CARTESIAN_POINT('Ctrl Pts',(16.8537040849283,-69.3015957225698,
-55.3474653979614));
#188842=CARTESIAN_POINT('Ctrl Pts',(16.7731194206628,-68.894483990695,-55.286087043994));
#188843=CARTESIAN_POINT('Ctrl Pts',(17.0112333722604,-68.8220198533602,
-54.9445960314883));
#188844=CARTESIAN_POINT('Ctrl Pts',(16.7982009500299,-69.3353877920995,
-55.3111829565324));
#188845=CARTESIAN_POINT('Ctrl Pts',(16.6993048554918,-68.9164109459874,
-55.2557565295156));
#188846=CARTESIAN_POINT('Ctrl Pts',(16.9010650546211,-68.8555068833233,
-54.8720727600904));
#188847=CARTESIAN_POINT('Ctrl Pts',(16.6555913240634,-69.4210909343955,
-55.2530368583418));
#188848=CARTESIAN_POINT('Ctrl Pts',(16.5212476377685,-68.9689791681947,
-55.223696330687));
#188849=CARTESIAN_POINT('Ctrl Pts',(16.6180815577824,-68.9404329890533,
-54.7559465968208));
#188850=CARTESIAN_POINT('Ctrl Pts',(16.5619443816715,-69.4764948536126,
-55.2416586756739));
#188851=CARTESIAN_POINT('Ctrl Pts',(16.4140091296541,-69.0003625620744,
-55.2402085606976));
#188852=CARTESIAN_POINT('Ctrl Pts',(16.4323327263914,-68.9953280686919,
-54.7333548544426));
#188853=CARTESIAN_POINT('Ctrl Pts',(16.474021195344,-69.527420504419,-55.2560439941876));
#188854=CARTESIAN_POINT('Ctrl Pts',(16.3324809063319,-69.0242130218807,
-55.279736482239));
#188855=CARTESIAN_POINT('Ctrl Pts',(16.2580067759255,-69.0457880333801,
-54.7622666492363));
#188856=CARTESIAN_POINT('',(16.4094778178732,-69.001678821881,-54.74995));
#188857=CARTESIAN_POINT('Origin',(16.55,-69.4815262104644,-54.74995));
#188858=CARTESIAN_POINT('Ctrl Pts',(16.4094778178732,-69.001678821881,-54.74995));
#188859=CARTESIAN_POINT('Ctrl Pts',(16.4504095598616,-68.9896920572568,
-54.7499500048056));
#188860=CARTESIAN_POINT('Ctrl Pts',(16.4912475287743,-68.9776812452657,
-54.7525666780149));
#188861=CARTESIAN_POINT('Ctrl Pts',(16.5317041745654,-68.965736321318,-54.757667934043));
#188862=CARTESIAN_POINT('Ctrl Pts',(16.5749366447118,-68.9529718284177,
-54.7631191990857));
#188863=CARTESIAN_POINT('Ctrl Pts',(16.6177350648204,-68.9402821612408,
-54.7714073705121));
#188864=CARTESIAN_POINT('Ctrl Pts',(16.6597585620131,-68.9277728443736,
-54.7824337221977));
#188865=CARTESIAN_POINT('Ctrl Pts',(16.7017820592057,-68.9152635275064,
-54.7934600738833));
#188866=CARTESIAN_POINT('Ctrl Pts',(16.7430322683556,-68.9029340622973,
-54.8072249335998));
#188867=CARTESIAN_POINT('Ctrl Pts',(16.7831545131606,-68.8908929861314,
-54.8236888710244));
#188868=CARTESIAN_POINT('Ctrl Pts',(16.7835975596796,-68.890760023559,-54.8238706726708));
#188869=CARTESIAN_POINT('Ctrl Pts',(16.7840405080022,-68.8906270844636,
-54.8240528195673));
#188870=CARTESIAN_POINT('Ctrl Pts',(16.7844833577117,-68.8904941689839,
-54.8242353115275));
#188871=CARTESIAN_POINT('Ctrl Pts',(16.8581304439983,-68.8683899706623,
-54.8545842106013));
#188872=CARTESIAN_POINT('Ctrl Pts',(16.9287006566087,-68.8470438209497,
-54.8943416412344));
#188873=CARTESIAN_POINT('Ctrl Pts',(16.9936792242012,-68.827277340243,-54.9420858838147));
#188874=CARTESIAN_POINT('Ctrl Pts',(17.0324101749556,-68.8154953847583,
-54.9705441890173));
#188875=CARTESIAN_POINT('Ctrl Pts',(17.0691551792512,-68.8042744590648,
-55.001839638253));
#188876=CARTESIAN_POINT('Ctrl Pts',(17.1033900455892,-68.7937859900155,
-55.0356687800906));
#188877=CARTESIAN_POINT('Ctrl Pts',(17.103886172442,-68.7936339926019,-55.0361590272412));
#188878=CARTESIAN_POINT('Ctrl Pts',(17.1043818163765,-68.7934821358841,
-55.0366498500402));
#188879=CARTESIAN_POINT('Ctrl Pts',(17.1048769761793,-68.7933304202781,
-55.0371412470353));
#188880=CARTESIAN_POINT('Ctrl Pts',(17.1669690008274,-68.7743055941547,
-55.0987614233149));
#188881=CARTESIAN_POINT('Ctrl Pts',(17.2214535479527,-68.7574981762718,
-55.1694239623163));
#188882=CARTESIAN_POINT('Ctrl Pts',(17.2659841189481,-68.743713328347,-55.2463463516036));
#188883=CARTESIAN_POINT('Ctrl Pts',(17.2871667241191,-68.7371560580402,
-55.2829373174201));
#188884=CARTESIAN_POINT('Ctrl Pts',(17.3060972390717,-68.7312826257116,
-55.3209455236334));
#188885=CARTESIAN_POINT('Ctrl Pts',(17.322524151481,-68.7261792841162,-55.3600753258131));
#188886=CARTESIAN_POINT('Ctrl Pts',(17.3227235277485,-68.7261173439796,
-55.3605502509672));
#188887=CARTESIAN_POINT('Ctrl Pts',(17.3229225385083,-68.7260555164805,
-55.3610253536613));
#188888=CARTESIAN_POINT('Ctrl Pts',(17.3231211835968,-68.7259938016769,
-55.3615006331605));
#188889=CARTESIAN_POINT('Ctrl Pts',(17.3377397858477,-68.7214521129136,
-55.3964771936486));
#188890=CARTESIAN_POINT('Ctrl Pts',(17.3503329508714,-68.7175347662069,
-55.4322944098897));
#188891=CARTESIAN_POINT('Ctrl Pts',(17.3608936617493,-68.7142467873541,
-55.4687543689716));
#188892=CARTESIAN_POINT('Ctrl Pts',(17.3714744037537,-68.7109525719968,
-55.5052834838196));
#188893=CARTESIAN_POINT('Ctrl Pts',(17.3800152474177,-68.70829001851,-55.5424589028239));
#188894=CARTESIAN_POINT('Ctrl Pts',(17.3864625050711,-68.7062785938727,
-55.5800999366542));
#188895=CARTESIAN_POINT('Ctrl Pts',(17.3927323721603,-68.7043225117965,
-55.616705310893));
#188896=CARTESIAN_POINT('Ctrl Pts',(17.3970223360455,-68.7029821923561,
-55.6537520599019));
#188897=CARTESIAN_POINT('Ctrl Pts',(17.399236871165,-68.7022899564979,-55.6910754862818));
#188898=CARTESIAN_POINT('Ctrl Pts',(17.4003972743764,-68.7019272290316,
-55.7106327393816));
#188899=CARTESIAN_POINT('Ctrl Pts',(17.4009870480798,-68.7017426900946,
-55.730265892737));
#188900=CARTESIAN_POINT('Ctrl Pts',(17.4009870515814,-68.7017426890013,
-55.74995));
#188901=CARTESIAN_POINT('Origin',(0.,-12.9675000200281,-54.74995));
#188902=CARTESIAN_POINT('',(15.913723201019,-69.1444843653509,-54.74995));
#188903=CARTESIAN_POINT('Origin',(16.05,-69.6255546658886,-54.74995));
#188904=CARTESIAN_POINT('Origin',(0.,-12.9675000200281,-54.74995));
#188905=CARTESIAN_POINT('Ctrl Pts',(16.0943918791427,-69.6003138753269,
-55.2520324188857));
#188906=CARTESIAN_POINT('Ctrl Pts',(15.9626541784119,-69.1297266675286,
-55.2398173309746));
#188907=CARTESIAN_POINT('Ctrl Pts',(16.0017964545034,-69.1194462603403,
-54.7532354575004));
#188908=CARTESIAN_POINT('Ctrl Pts',(15.9520563039833,-69.6815449359842,
-55.238583696008));
#188909=CARTESIAN_POINT('Ctrl Pts',(15.7933965067921,-69.1775635977428,
-55.2661930138944));
#188910=CARTESIAN_POINT('Ctrl Pts',(15.7194486319347,-69.2000152527435,
-54.7262790994806));
#188911=CARTESIAN_POINT('Ctrl Pts',(15.8040804369175,-69.7629913547991,
-55.2908208908606));
#188912=CARTESIAN_POINT('Ctrl Pts',(15.6782147462389,-69.2100275662615,
-55.3690735314078));
#188913=CARTESIAN_POINT('Ctrl Pts',(15.4256393014046,-69.2808712212567,
-54.8307953991629));
#188914=CARTESIAN_POINT('Ctrl Pts',(15.5957850814026,-69.8754701070241,
-55.4950681095302));
#188915=CARTESIAN_POINT('Ctrl Pts',(15.5548552071343,-69.2462930289052,
-55.5833321666787));
#188916=CARTESIAN_POINT('Ctrl Pts',(15.0121582713081,-69.3925053704125,
-55.2396491450935));
#188917=CARTESIAN_POINT('Ctrl Pts',(15.5374042125397,-69.9059409697286,
-55.6453900516724));
#188918=CARTESIAN_POINT('Ctrl Pts',(15.5478910318033,-69.2494990492648,
-55.6859501835156));
#188919=CARTESIAN_POINT('Ctrl Pts',(14.89623691968,-69.4227546427598,-55.5406072672281));
#188920=CARTESIAN_POINT('Ctrl Pts',(15.5523010752554,-69.89814066138,-55.797007806289));
#188921=CARTESIAN_POINT('Ctrl Pts',(15.55041942508,-69.2484839021119,-55.7792669100244));
#188922=CARTESIAN_POINT('Ctrl Pts',(14.92581406719,-69.4150115966434,-55.8441656371953));
#188923=CARTESIAN_POINT('',(14.9222139673106,-69.4159516070034,-55.74995));
#188924=CARTESIAN_POINT('Origin',(15.05,-69.8993466109593,-55.74995));
#188925=CARTESIAN_POINT('Ctrl Pts',(14.9222139673106,-69.4159516070035,
-55.74995));
#188926=CARTESIAN_POINT('Ctrl Pts',(14.9222684167837,-69.4159372132218,
-55.6560401405972));
#188927=CARTESIAN_POINT('Ctrl Pts',(14.9355158903724,-69.4124399177686,
-55.563575015399));
#188928=CARTESIAN_POINT('Ctrl Pts',(14.9614297127064,-69.4055703024629,
-55.4737974919486));
#188929=CARTESIAN_POINT('Ctrl Pts',(14.9723367261448,-69.4026789117027,
-55.4360105286005));
#188930=CARTESIAN_POINT('Ctrl Pts',(14.985487454912,-69.3991894720854,-55.3986996822186));
#188931=CARTESIAN_POINT('Ctrl Pts',(15.0008419271996,-69.3951076046889,
-55.3619576246799));
#188932=CARTESIAN_POINT('Ctrl Pts',(15.0407650708988,-69.3844943465073,
-55.2664246480044));
#188933=CARTESIAN_POINT('Ctrl Pts',(15.0928106079671,-69.3706175165969,
-55.180386190476));
#188934=CARTESIAN_POINT('Ctrl Pts',(15.1571532348986,-69.3533214831149,
-55.1036416590134));
#188935=CARTESIAN_POINT('Ctrl Pts',(15.1763510453595,-69.348160892254,-55.0807435114059));
#188936=CARTESIAN_POINT('Ctrl Pts',(15.1966434942269,-69.3426955736518,
-55.0586727438326));
#188937=CARTESIAN_POINT('Ctrl Pts',(15.2180349745493,-69.3369205223421,
-55.037424028165));
#188938=CARTESIAN_POINT('Ctrl Pts',(15.3111212994845,-69.3117900360626,
-54.9449589522898));
#188939=CARTESIAN_POINT('Ctrl Pts',(15.4192055462156,-69.2823626792043,
-54.8734147542759));
#188940=CARTESIAN_POINT('Ctrl Pts',(15.5392134434446,-69.249228865297,-54.8240288525655));
#188941=CARTESIAN_POINT('Ctrl Pts',(15.6592213406736,-69.2160950513897,
-54.7746429508552));
#188942=CARTESIAN_POINT('Ctrl Pts',(15.7840680515859,-69.1812128616152,
-54.74995));
#188943=CARTESIAN_POINT('Ctrl Pts',(15.913723201019,-69.1444843653509,-54.74995));
#188944=CARTESIAN_POINT('Origin',(15.05,-69.8993466109593,-55.24995));
#188945=CARTESIAN_POINT('',(14.9222139673106,-69.4159516070034,-55.24995));
#188946=CARTESIAN_POINT('Origin',(0.,-12.9675000200281,-60.42825533736));
#188947=CARTESIAN_POINT('Origin',(0.,-12.9675000200281,-60.42825533736));
#188948=CARTESIAN_POINT('Origin',(9.4,-71.0999148696911,-55.24995));
#188949=CARTESIAN_POINT('',(9.32018679685842,-70.6063261212332,-55.8925850873));
#188950=CARTESIAN_POINT('',(9.32018679685842,-70.6063261212332,-55.24995));
#188951=CARTESIAN_POINT('Origin',(9.4,-71.0999148696911,-55.8925850873));
#188952=CARTESIAN_POINT('Ctrl Pts',(8.9,-71.0999148696911,-55.8925850873));
#188953=CARTESIAN_POINT('Ctrl Pts',(8.89999999999995,-70.674270243298,-55.8925850872999));
#188954=CARTESIAN_POINT('Ctrl Pts',(9.32018679685842,-70.6063261212332,
-55.8925850873));
#188955=CARTESIAN_POINT('Ctrl Pts',(8.9,-71.0753963340341,-55.8158206410579));
#188956=CARTESIAN_POINT('Ctrl Pts',(8.92045674363156,-70.670962391591,-55.8099505084873));
#188957=CARTESIAN_POINT('Ctrl Pts',(9.32018679646957,-70.606326121296,-55.7609765242912));
#188958=CARTESIAN_POINT('Ctrl Pts',(8.88914819160783,-71.0574685211989,
-55.7424878932553));
#188959=CARTESIAN_POINT('Ctrl Pts',(8.92288173642606,-70.6704214883702,
-55.7222104842267));
#188960=CARTESIAN_POINT('Ctrl Pts',(9.29866745626329,-70.6098198655576,
-55.6301334688925));
#188961=CARTESIAN_POINT('Ctrl Pts',(8.84354256567003,-71.0340357122248,
-55.606998619986));
#188962=CARTESIAN_POINT('Ctrl Pts',(8.88787909971282,-70.6754793338957,
-55.5563944136962));
#188963=CARTESIAN_POINT('Ctrl Pts',(9.20823066610786,-70.6243360556297,
-55.3829240249879));
#188964=CARTESIAN_POINT('Ctrl Pts',(8.80933590722104,-71.0287732217429,
-55.5465658668829));
#188965=CARTESIAN_POINT('Ctrl Pts',(8.8515542998134,-70.6809070626089,-55.4791108159719));
#188966=CARTESIAN_POINT('Ctrl Pts',(9.14039822217997,-70.6351795268323,
-55.2697323706429));
#188967=CARTESIAN_POINT('Ctrl Pts',(8.72031210976081,-71.028802992332,-55.4457995958176));
#188968=CARTESIAN_POINT('Ctrl Pts',(8.74741150404566,-70.6964574226719,
-55.3507681953891));
#188969=CARTESIAN_POINT('Ctrl Pts',(8.96386239650929,-70.6628838067398,
-55.0780797399289));
#188970=CARTESIAN_POINT('Ctrl Pts',(8.66589931539796,-71.0341559413013,
-55.4063653507054));
#188971=CARTESIAN_POINT('Ctrl Pts',(8.67980906181995,-70.7065384951403,
-55.2998814604829));
#188972=CARTESIAN_POINT('Ctrl Pts',(8.85596081453515,-70.679599541712,-55.0012953993776));
#188973=CARTESIAN_POINT('Ctrl Pts',(8.54658037248409,-71.0525391488741,
-55.3555557927535));
#188974=CARTESIAN_POINT('Ctrl Pts',(8.53037007175229,-70.7286009969626,
-55.2361886195966));
#188975=CARTESIAN_POINT('Ctrl Pts',(8.61934915026951,-70.7154116132197,
-54.8994528680703));
#188976=CARTESIAN_POINT('Ctrl Pts',(8.48132333269991,-71.0655965765405,
-55.3439422058851));
#188977=CARTESIAN_POINT('Ctrl Pts',(8.44749087161535,-70.7407315090392,
-55.2227831389152));
#188978=CARTESIAN_POINT('Ctrl Pts',(8.48994814797731,-70.7346037655486,
-54.8739206038906));
#188979=CARTESIAN_POINT('Ctrl Pts',(8.41560835021371,-71.0814043774774,
-55.3473655916161));
#188980=CARTESIAN_POINT('Ctrl Pts',(8.36589323739407,-70.7525502203441,
-55.2292031667485));
#188981=CARTESIAN_POINT('Ctrl Pts',(8.35962920986983,-70.7534564084689,
-54.8763024037294));
#188982=CARTESIAN_POINT('',(8.35962920986979,-70.7534564084689,-54.8763024037297));
#188983=CARTESIAN_POINT('Origin',(8.4312167004274,-71.248305103724,-54.8763024037297));
#188984=CARTESIAN_POINT('Ctrl Pts',(8.35962920986984,-70.7534564084689,
-54.8763024037297));
#188985=CARTESIAN_POINT('Ctrl Pts',(8.4266932097628,-70.7437545672695,-54.8750766952757));
#188986=CARTESIAN_POINT('Ctrl Pts',(8.49356141096506,-70.7339558949385,
-54.8812481493054));
#188987=CARTESIAN_POINT('Ctrl Pts',(8.55878406018679,-70.724290971257,-54.8944764365469));
#188988=CARTESIAN_POINT('Ctrl Pts',(8.62027176255571,-70.715179505258,-54.9069472116298));
#188989=CARTESIAN_POINT('Ctrl Pts',(8.68029576330459,-70.7061871116828,
-54.9256889700024));
#188990=CARTESIAN_POINT('Ctrl Pts',(8.73765415640112,-70.6975057024889,
-54.9503761135537));
#188991=CARTESIAN_POINT('Ctrl Pts',(8.73812533670876,-70.6974343875717,
-54.950578910307));
#188992=CARTESIAN_POINT('Ctrl Pts',(8.7385963482321,-70.6973630921029,-54.9507821155763));
#188993=CARTESIAN_POINT('Ctrl Pts',(8.7390671903714,-70.697291816191,-54.9509857288995));
#188994=CARTESIAN_POINT('Ctrl Pts',(8.81806341257938,-70.6853333967864,
-54.985147249244));
#188995=CARTESIAN_POINT('Ctrl Pts',(8.89230145001324,-70.673924118985,-55.030799607521));
#188996=CARTESIAN_POINT('Ctrl Pts',(8.95909820842037,-70.6635530304581,
-55.0858633072555));
#188997=CARTESIAN_POINT('Ctrl Pts',(8.99202329694071,-70.658440970892,-55.1130050014223));
#188998=CARTESIAN_POINT('Ctrl Pts',(9.02314073107693,-70.6535810854978,
-55.1424341547092));
#188999=CARTESIAN_POINT('Ctrl Pts',(9.05213028602996,-70.6490316704449,
-55.1739060774789));
#189000=CARTESIAN_POINT('Ctrl Pts',(9.05261593139239,-70.6489554567077,
-55.1744333085235));
#189001=CARTESIAN_POINT('Ctrl Pts',(9.05310095531287,-70.6488793344915,
-55.1749610621635));
#189002=CARTESIAN_POINT('Ctrl Pts',(9.05358535746146,-70.6488033038874,
-55.1754893372344));
#189003=CARTESIAN_POINT('Ctrl Pts',(9.10207551699106,-70.6411924042821,
-55.2283713125429));
#189004=CARTESIAN_POINT('Ctrl Pts',(9.14429186553919,-70.634506376804,-55.2864243412893));
#189005=CARTESIAN_POINT('Ctrl Pts',(9.17994788064258,-70.6288295105427,
-55.3485029540396));
#189006=CARTESIAN_POINT('Ctrl Pts',(9.20880098471937,-70.6242357495015,
-55.3987374143245));
#189007=CARTESIAN_POINT('Ctrl Pts',(9.23335776597275,-70.6203028545583,
-55.4516091557793));
#189008=CARTESIAN_POINT('Ctrl Pts',(9.25344901950571,-70.6170779672838,
-55.5065287627148));
#189009=CARTESIAN_POINT('Ctrl Pts',(9.25361952044245,-70.6170505998375,
-55.506994828429));
#189010=CARTESIAN_POINT('Ctrl Pts',(9.25378968425506,-70.6170232859403,
-55.5074609965585));
#189011=CARTESIAN_POINT('Ctrl Pts',(9.25395951106862,-70.6169960255762,
-55.5079272667724));
#189012=CARTESIAN_POINT('Ctrl Pts',(9.26917261736367,-70.6145540388982,
-55.5496958083666));
#189013=CARTESIAN_POINT('Ctrl Pts',(9.28164780823389,-70.6125470433612,
-55.5921779695173));
#189014=CARTESIAN_POINT('Ctrl Pts',(9.29152034880348,-70.6109563835461,
-55.6352174890367));
#189015=CARTESIAN_POINT('Ctrl Pts',(9.30173630321663,-70.609310393029,-55.6797541274304));
#189016=CARTESIAN_POINT('Ctrl Pts',(9.30916540444182,-70.6081101941254,
-55.7248883638107));
#189017=CARTESIAN_POINT('Ctrl Pts',(9.31390296845355,-70.6073438342246,
-55.7704597578364));
#189018=CARTESIAN_POINT('Ctrl Pts',(9.31810307746836,-70.606664414354,-55.8108612853706));
#189019=CARTESIAN_POINT('Ctrl Pts',(9.32018679673735,-70.6063261212527,
-55.8516070077995));
#189020=CARTESIAN_POINT('Ctrl Pts',(9.32018679685842,-70.6063261212332,
-55.8925850873));
#189021=CARTESIAN_POINT('Ctrl Pts',(8.41560835021369,-71.0814043774777,
-55.3473655916165));
#189022=CARTESIAN_POINT('Ctrl Pts',(8.36589323739404,-70.752550220344,-55.2292031667489));
#189023=CARTESIAN_POINT('Ctrl Pts',(8.35962920986988,-70.7534564084689,
-54.8763024037297));
#189024=CARTESIAN_POINT('Ctrl Pts',(8.24918690883785,-71.102010310254,-55.3491521481271));
#189025=CARTESIAN_POINT('Ctrl Pts',(8.2013544983267,-70.7763714724242,-55.2294679275358));
#189026=CARTESIAN_POINT('Ctrl Pts',(8.19486187074245,-70.7772925435282,
-54.8793138184774));
#189027=CARTESIAN_POINT('Ctrl Pts',(8.08271475024063,-71.1220068981801,
-55.3508246944299));
#189028=CARTESIAN_POINT('Ctrl Pts',(8.03626733023182,-70.7995543826982,
-55.2297202388378));
#189029=CARTESIAN_POINT('Ctrl Pts',(8.02999374674379,-70.8004238120746,
-54.8822160506073));
#189030=CARTESIAN_POINT('Ctrl Pts',(7.91618843693366,-71.141394090941,-55.3523946663951));
#189031=CARTESIAN_POINT('Ctrl Pts',(7.87072047725699,-70.8220758845274,
-55.2299609924931));
#189032=CARTESIAN_POINT('Ctrl Pts',(7.86502491569137,-70.8228501557662,
-54.8850140141151));
#189033=CARTESIAN_POINT('',(7.86502491569136,-70.8228501557662,-54.8850140141151));
#189034=CARTESIAN_POINT('Origin',(7.93237687386467,-71.3182931027643,-54.8850140141151));
#189035=CARTESIAN_POINT('Origin',(0.0280298706655902,-14.2420762575896,
-46.3192185165476));
#189036=CARTESIAN_POINT('Ctrl Pts',(7.91618843693208,-71.1413940909409,
-55.352394666395));
#189037=CARTESIAN_POINT('Ctrl Pts',(7.87072047725574,-70.8220758845275,
-55.2299609924928));
#189038=CARTESIAN_POINT('Ctrl Pts',(7.86502491569091,-70.8228501557662,
-54.8850140141151));
#189039=CARTESIAN_POINT('Ctrl Pts',(7.844285602846,-71.157562039706,-55.3560236134997));
#189040=CARTESIAN_POINT('Ctrl Pts',(7.77985413280654,-70.8344428879727,
-55.236521459352));
#189041=CARTESIAN_POINT('Ctrl Pts',(7.72241706825884,-70.8422366821738,
-54.8874327557878));
#189042=CARTESIAN_POINT('Ctrl Pts',(7.77219443565847,-71.177222127411,-55.3781864762555));
#189043=CARTESIAN_POINT('Ctrl Pts',(7.69016530757976,-70.8464897855799,
-55.2681271844367));
#189044=CARTESIAN_POINT('Ctrl Pts',(7.5794821547774,-70.8610938450093,-54.9239881329105));
#189045=CARTESIAN_POINT('Ctrl Pts',(7.64331486532417,-71.2207339188645,
-55.4539331018544));
#189046=CARTESIAN_POINT('Ctrl Pts',(7.53737924067218,-70.8668804541439,
-55.3692852810369));
#189047=CARTESIAN_POINT('Ctrl Pts',(7.32391158111293,-70.8939799308472,
-55.0534925677837));
#189048=CARTESIAN_POINT('Ctrl Pts',(7.58567352642291,-71.2449041853563,
-55.5078568245776));
#189049=CARTESIAN_POINT('Ctrl Pts',(7.47303212720142,-70.8754018535837,
-55.4405214339084));
#189050=CARTESIAN_POINT('Ctrl Pts',(7.20960774580809,-70.9082476913312,
-55.1469663768362));
#189051=CARTESIAN_POINT('Ctrl Pts',(7.49322857950783,-71.2966779191941,
-55.6376571876191));
#189052=CARTESIAN_POINT('Ctrl Pts',(7.38267219174721,-70.8874980297502,
-55.6027965247728));
#189053=CARTESIAN_POINT('Ctrl Pts',(7.02628770602923,-70.9307639518508,
-55.3693141862512));
#189054=CARTESIAN_POINT('Ctrl Pts',(7.45777202258463,-71.3246266217341,
-55.7141753031788));
#189055=CARTESIAN_POINT('Ctrl Pts',(7.35664509914443,-70.8910885028411,
-55.6963616877968));
#189056=CARTESIAN_POINT('Ctrl Pts',(6.95597670016225,-70.9391888126349,
-55.4992549495758));
#189057=CARTESIAN_POINT('Ctrl Pts',(7.41125924474539,-71.38419243799,-55.8811540356734));
#189058=CARTESIAN_POINT('Ctrl Pts',(7.34624804767826,-70.8930407983775,
-55.8848711139694));
#189059=CARTESIAN_POINT('Ctrl Pts',(6.86374100295758,-70.950181682438,-55.7748476118441));
#189060=CARTESIAN_POINT('Ctrl Pts',(7.4,-71.4160375965177,-55.9720928529598));
#189061=CARTESIAN_POINT('Ctrl Pts',(7.36384050363832,-70.8911630457611,
-55.9819410866112));
#189062=CARTESIAN_POINT('Ctrl Pts',(6.84141371299613,-70.9528017322803,
-55.9212771125469));
#189063=CARTESIAN_POINT('Ctrl Pts',(7.4,-71.4493575166339,-56.06661116875));
#189064=CARTESIAN_POINT('Ctrl Pts',(7.3999999999998,-70.8868967568689,-56.06661116875));
#189065=CARTESIAN_POINT('Ctrl Pts',(6.84141371258755,-70.9528017323285,
-56.0666111687498));
#189066=CARTESIAN_POINT('',(6.84141371258755,-70.9528017323285,-56.0666111687498));
#189067=CARTESIAN_POINT('',(6.9,-70.949357516634,-56.0666111687498));
#189068=CARTESIAN_POINT('Origin',(6.9,-71.449357516634,-56.0666111687498));
#189069=CARTESIAN_POINT('Origin',(6.9,-71.449357516634,-56.0666111687498));
#189070=CARTESIAN_POINT('Ctrl Pts',(6.84141371258755,-70.9528017323285,
-56.0666111687498));
#189071=CARTESIAN_POINT('Ctrl Pts',(6.84141371272281,-70.9528017323125,
-56.0185004951022));
#189072=CARTESIAN_POINT('Ctrl Pts',(6.84385625486988,-70.9525150960356,
-55.9705185340177));
#189073=CARTESIAN_POINT('Ctrl Pts',(6.8487439595216,-70.951938515923,-55.9228849154069));
#189074=CARTESIAN_POINT('Ctrl Pts',(6.85371160739849,-70.9513525052747,
-55.8744722020329));
#189075=CARTESIAN_POINT('Ctrl Pts',(6.86120476133719,-70.9504670347036,
-55.8264180258316));
#189076=CARTESIAN_POINT('Ctrl Pts',(6.87128050874745,-70.9492722819139,
-55.7789472465282));
#189077=CARTESIAN_POINT('Ctrl Pts',(6.88084558986923,-70.9481380824459,
-55.7338824154578));
#189078=CARTESIAN_POINT('Ctrl Pts',(6.89273836925604,-70.9467251353176,
-55.6893423359324));
#189079=CARTESIAN_POINT('Ctrl Pts',(6.90705554696957,-70.9450193012211,
-55.6455309032989));
#189080=CARTESIAN_POINT('Ctrl Pts',(6.9078199210414,-70.9449282291272,-55.6431918722535));
#189081=CARTESIAN_POINT('Ctrl Pts',(6.90859121688159,-70.9448363208197,
-55.6408549230079));
#189082=CARTESIAN_POINT('Ctrl Pts',(6.90936945309023,-70.944743573674,-55.638520088397));
#189083=CARTESIAN_POINT('Ctrl Pts',(6.90953264041296,-70.9447241256476,
-55.6380305000112));
#189084=CARTESIAN_POINT('Ctrl Pts',(6.90969612810931,-70.9447046413087,
-55.6375410188016));
#189085=CARTESIAN_POINT('Ctrl Pts',(6.90985991625218,-70.9446851206452,
-55.6370516451987));
#189086=CARTESIAN_POINT('Ctrl Pts',(6.93890470840672,-70.9412234926851,
-55.5502703047937));
#189087=CARTESIAN_POINT('Ctrl Pts',(6.97755496303265,-70.9365992546703,
-55.4665613054823));
#189088=CARTESIAN_POINT('Ctrl Pts',(7.02515534568111,-70.9308292795786,
-55.388637952601));
#189089=CARTESIAN_POINT('Ctrl Pts',(7.052652463843,-70.9274961616905,-55.3436242883712));
#189090=CARTESIAN_POINT('Ctrl Pts',(7.08313672341692,-70.92378064339,-55.3005419198593));
#189091=CARTESIAN_POINT('Ctrl Pts',(7.11648530834342,-70.9196854249332,
-55.2599212236758));
#189092=CARTESIAN_POINT('Ctrl Pts',(7.11697272521332,-70.9196255699628,
-55.2593275189465));
#189093=CARTESIAN_POINT('Ctrl Pts',(7.11746075366589,-70.9195656339149,
-55.2587343401393));
#189094=CARTESIAN_POINT('Ctrl Pts',(7.11794939330103,-70.9195056167998,
-55.2581416889457));
#189095=CARTESIAN_POINT('Ctrl Pts',(7.17766958662853,-70.9121704899281,
-55.1857094887866));
#189096=CARTESIAN_POINT('Ctrl Pts',(7.24707274855584,-70.9035491680659,
-55.1207030262999));
#189097=CARTESIAN_POINT('Ctrl Pts',(7.32365993963188,-70.8938669826863,
-55.0662525944808));
#189098=CARTESIAN_POINT('Ctrl Pts',(7.36395975880566,-70.8887722623484,
-55.0376010337509));
#189099=CARTESIAN_POINT('Ctrl Pts',(7.40624788203792,-70.8833838941673,
-55.011872736897));
#189100=CARTESIAN_POINT('Ctrl Pts',(7.450155212976,-70.8777352422905,-54.9895263260323));
#189101=CARTESIAN_POINT('Ctrl Pts',(7.45066930715087,-70.8776691043822,
-54.989264680439));
#189102=CARTESIAN_POINT('Ctrl Pts',(7.45118359869241,-70.877602933957,-54.9890035107279));
#189103=CARTESIAN_POINT('Ctrl Pts',(7.45169808724107,-70.8775367310404,
-54.9887428173532));
#189104=CARTESIAN_POINT('Ctrl Pts',(7.48702485166254,-70.8729909839197,
-54.9708426066328));
#189105=CARTESIAN_POINT('Ctrl Pts',(7.52340553096597,-70.8682741670682,
-54.9551443604244));
#189106=CARTESIAN_POINT('Ctrl Pts',(7.5606036934083,-70.8634146986663,-54.9417107539087));
#189107=CARTESIAN_POINT('Ctrl Pts',(7.59755058615544,-70.8585880554651,
-54.9283678899994));
#189108=CARTESIAN_POINT('Ctrl Pts',(7.63530511490774,-70.8536205390166,
-54.9172587967144));
#189109=CARTESIAN_POINT('Ctrl Pts',(7.67365359691508,-70.8485368945066,
-54.9084923483496));
#189110=CARTESIAN_POINT('Ctrl Pts',(7.71043547056373,-70.8436609265346,
-54.9000840260582));
#189111=CARTESIAN_POINT('Ctrl Pts',(7.74776474509213,-70.8386779998652,
-54.8938307755624));
#189112=CARTESIAN_POINT('Ctrl Pts',(7.78545391476942,-70.8336090347271,
-54.8898753244176));
#189113=CARTESIAN_POINT('Ctrl Pts',(7.81182391853935,-70.8300624288733,
-54.887107811562));
#189114=CARTESIAN_POINT('Ctrl Pts',(7.83837014274921,-70.8264736832847,
-54.8854661001065));
#189115=CARTESIAN_POINT('Ctrl Pts',(7.86502491569091,-70.8228501557662,
-54.8850140141151));
#189116=CARTESIAN_POINT('Origin',(6.9,-71.449357516634,-55.24995));
#189117=CARTESIAN_POINT('',(6.84141371258755,-70.9528017323285,-55.24995));
#189118=CARTESIAN_POINT('Origin',(0.,-12.9675000200281,-60.42825533736));
#189119=CARTESIAN_POINT('Origin',(0.,-12.9675000200281,-60.42825533736));
#189120=CARTESIAN_POINT('Origin',(1.24999999999996,-71.8417317029411,-55.24995));
#189121=CARTESIAN_POINT('',(1.2393865421354,-71.3418443611208,-56.1920015047684));
#189122=CARTESIAN_POINT('',(1.2393865421354,-71.3418443611208,-55.24995));
#189123=CARTESIAN_POINT('Origin',(1.24999999999996,-71.8417317029411,-56.1920015047684));
#189124=CARTESIAN_POINT('Ctrl Pts',(0.74992832526643,-71.8476124042683,
-56.2095834390661));
#189125=CARTESIAN_POINT('Ctrl Pts',(0.744108865482373,-71.351962221307,
-56.2095867879049));
#189126=CARTESIAN_POINT('Ctrl Pts',(1.23964458126955,-71.341839523454,-56.2153597573814));
#189127=CARTESIAN_POINT('Ctrl Pts',(0.751776125714688,-71.7713204575019,
-55.9817509371667));
#189128=CARTESIAN_POINT('Ctrl Pts',(0.816837216474583,-71.3505250778188,
-55.9987951501326));
#189129=CARTESIAN_POINT('Ctrl Pts',(1.24327926489108,-71.3417496291435,
-55.9137659627895));
#189130=CARTESIAN_POINT('Ctrl Pts',(0.718072267663703,-71.7066743634015,
-55.7785946996364));
#189131=CARTESIAN_POINT('Ctrl Pts',(0.824825378281954,-71.350036513351,
-55.7487495717777));
#189132=CARTESIAN_POINT('Ctrl Pts',(1.17639466159895,-71.3434192147202,
-55.6016397278362));
#189133=CARTESIAN_POINT('Ctrl Pts',(0.584670453989408,-71.6422004184537,
-55.5485996630821));
#189134=CARTESIAN_POINT('Ctrl Pts',(0.68043710643303,-71.3513071664449,
-55.4568954173326));
#189135=CARTESIAN_POINT('Ctrl Pts',(0.911756750913512,-71.34794523375,-55.2318343014585));
#189136=CARTESIAN_POINT('Ctrl Pts',(0.529612862082923,-71.6265518657637,
-55.4878844649265));
#189137=CARTESIAN_POINT('Ctrl Pts',(0.61348963780591,-71.3519450763092,
-55.3771436564239));
#189138=CARTESIAN_POINT('Ctrl Pts',(0.802538014423018,-71.3496280189885,
-55.1308312312545));
#189139=CARTESIAN_POINT('Ctrl Pts',(0.395598613078437,-71.6049256773685,
-55.4002431537929));
#189140=CARTESIAN_POINT('Ctrl Pts',(0.442382077620753,-71.3532818922767,
-55.2625191895523));
#189141=CARTESIAN_POINT('Ctrl Pts',(0.53669485310282,-71.3526926510771,
-54.9837531096389));
#189142=CARTESIAN_POINT('Ctrl Pts',(0.318989062465326,-71.5999429306173,
-55.3774294426603));
#189143=CARTESIAN_POINT('Ctrl Pts',(0.339989995154795,-71.3539406609335,
-55.2314667911085));
#189144=CARTESIAN_POINT('Ctrl Pts',(0.3847301999498,-71.3539511178465,-54.9445588028));
#189145=CARTESIAN_POINT('Ctrl Pts',(0.238798012754718,-71.6010945930311,
-55.3801419188632));
#189146=CARTESIAN_POINT('Ctrl Pts',(0.233742017347619,-71.3543709520858,
-55.2351306094688));
#189147=CARTESIAN_POINT('Ctrl Pts',(0.225655240690842,-71.354563899099,
-54.9490093924302));
#189148=CARTESIAN_POINT('',(0.249602310815417,-71.3544665017672,-54.9489505784606));
#189149=CARTESIAN_POINT('Ctrl Pts',(0.249602310815417,-71.3544665017672,
-54.9489505784606));
#189150=CARTESIAN_POINT('Ctrl Pts',(0.324383151711637,-71.3541468161967,
-54.9489131643343));
#189151=CARTESIAN_POINT('Ctrl Pts',(0.433588595141249,-71.35346461301,-54.9628114661091));
#189152=CARTESIAN_POINT('Ctrl Pts',(0.538344474802224,-71.3525282945736,
-54.9976414023299));
#189153=CARTESIAN_POINT('Ctrl Pts',(0.607192878775931,-71.3518528742047,
-55.0255128341318));
#189154=CARTESIAN_POINT('Ctrl Pts',(0.642806300227351,-71.3514701198547,
-55.0427102506267));
#189155=CARTESIAN_POINT('Ctrl Pts',(0.73806134014663,-71.3503695531929,
-55.0956639309939));
#189156=CARTESIAN_POINT('Ctrl Pts',(0.8263152279403,-71.3491952833432,-55.1589825749407));
#189157=CARTESIAN_POINT('Ctrl Pts',(0.917026830650857,-71.3478072668677,
-55.2509930124761));
#189158=CARTESIAN_POINT('Ctrl Pts',(0.953278076391069,-71.3472187265559,
-55.2943129184764));
#189159=CARTESIAN_POINT('Ctrl Pts',(0.97686221842195,-71.346828857815,-55.3240566027749));
#189160=CARTESIAN_POINT('Ctrl Pts',(0.989578654400162,-71.3466143523215,
-55.3410674841052));
#189161=CARTESIAN_POINT('Ctrl Pts',(1.15945421218685,-71.3437057224535,
-55.5795506821725));
#189162=CARTESIAN_POINT('Ctrl Pts',(1.23938654213546,-71.3418443611209,
-55.8585192145883));
#189163=CARTESIAN_POINT('Ctrl Pts',(1.2393865421354,-71.3418443611208,-56.1920015047684));
#189164=CARTESIAN_POINT('Origin',(0.251739774406202,-71.8544619329957,-54.9489505784606));
#189165=CARTESIAN_POINT('Origin',(0.,-12.9675000200281,-55.24995));
#189166=CARTESIAN_POINT('',(24.0682702937655,-66.1635386067456,-52.64995));
#189167=CARTESIAN_POINT('Origin',(0.,-12.9675000200281,-52.64995));
#189168=CARTESIAN_POINT('Origin',(8.64724958304919E-13,-13.7566898295974,
-48.2080483433929));
#189169=CARTESIAN_POINT('',(24.0682702937655,-66.1635386067456,-55.24995));
#189170=CARTESIAN_POINT('Origin',(52.9858497431864,-37.4950331867729,-52.64995));
#189171=CARTESIAN_POINT('',(52.9112495105562,-38.347717747534,-52.64995));
#189172=CARTESIAN_POINT('',(52.9112495105562,-38.347717747534,-52.64995));
#189173=CARTESIAN_POINT('',(51.3604079243415,-56.0739181912695,-52.64995));
#189174=CARTESIAN_POINT('',(52.9858497431864,-37.4950331867729,-52.64995));
#189175=CARTESIAN_POINT('',(51.3604079243415,-56.0739181912695,-52.64995));
#189176=CARTESIAN_POINT('Origin',(48.3718238300662,-55.8124509630266,-59.64995));
#189177=CARTESIAN_POINT('Origin',(48.3718238300662,-55.8124509630266,-59.64995));
#189178=CARTESIAN_POINT('Origin',(51.265241636025,-57.1616738441871,-52.64995));
#189179=CARTESIAN_POINT('',(44.9662712865582,-63.4606441936539,-52.64995));
#189180=CARTESIAN_POINT('',(44.9662712865582,-63.4606441936539,-52.64995));
#189181=CARTESIAN_POINT('',(50.4931441736259,-57.9337713065862,-52.64995));
#189182=CARTESIAN_POINT('',(50.4931441736259,-57.9337713065862,-52.64995));
#189183=CARTESIAN_POINT('',(51.265241636025,-57.1616738441871,-52.64995));
#189184=CARTESIAN_POINT('Origin',(48.3718238300662,-55.8124509630266,-52.64995));
#189185=CARTESIAN_POINT('Origin',(48.3718238300662,-55.8124509630266,-52.64995));
#189186=CARTESIAN_POINT('Origin',(42.8449509429986,-61.3393238500942,-59.64995));
#189187=CARTESIAN_POINT('Origin',(42.8449509429986,-61.3393238500942,-59.64995));
#189188=CARTESIAN_POINT('Origin',(44.1941738241591,-64.2327416560529,-52.64995));
#189189=CARTESIAN_POINT('',(43.1064181712415,-64.3279079443695,-52.64995));
#189190=CARTESIAN_POINT('',(43.1064181712415,-64.3279079443695,-52.64995));
#189191=CARTESIAN_POINT('',(25.043451507077,-65.9082127571302,-52.64995));
#189192=CARTESIAN_POINT('',(44.1941738241591,-64.2327416560529,-52.64995));
#189193=CARTESIAN_POINT('',(25.043451507077,-65.9082127571302,-55.24995));
#189194=CARTESIAN_POINT('Origin',(42.8449509429986,-61.3393238500942,-52.64995));
#189195=CARTESIAN_POINT('Origin',(42.8449509429986,-61.3393238500942,-52.64995));
#189196=CARTESIAN_POINT('Ctrl Pts',(24.579016252936,-65.9859437829616,-54.74995));
#189197=CARTESIAN_POINT('Ctrl Pts',(24.579016252936,-65.9859437829616,-55.24995));
#189198=CARTESIAN_POINT('Ctrl Pts',(24.7,-66.4710859610356,-55.24995));
#189199=CARTESIAN_POINT('Ctrl Pts',(24.7361092859404,-65.946768249212,-54.749950009163));
#189200=CARTESIAN_POINT('Ctrl Pts',(24.67310951117,-65.9624790000681,-55.2343403176332));
#189201=CARTESIAN_POINT('Ctrl Pts',(24.7654791450057,-66.4384278647148,
-55.24995));
#189202=CARTESIAN_POINT('Ctrl Pts',(24.8931309886626,-65.9213640983868,
-54.7753029040978));
#189203=CARTESIAN_POINT('Ctrl Pts',(24.7709452774937,-65.9414368141194,
-55.24317591549));
#189204=CARTESIAN_POINT('Ctrl Pts',(24.8308799729202,-66.4172697443503,
-55.2626259569449));
#189205=CARTESIAN_POINT('Ctrl Pts',(25.043451507077,-65.9082127571302,-54.8278826162281));
#189206=CARTESIAN_POINT('Ctrl Pts',(24.8576734148988,-65.9244662341272,
-55.273872259957));
#189207=CARTESIAN_POINT('Ctrl Pts',(24.8935146892254,-66.4063101061761,
-55.2889163081141));
#189208=CARTESIAN_POINT('',(24.579016252936,-65.9859437829616,-54.74995));
#189209=CARTESIAN_POINT('Origin',(24.7,-66.4710859610356,-54.74995));
#189210=CARTESIAN_POINT('Ctrl Pts',(24.579016252936,-65.9859437829616,-54.74995));
#189211=CARTESIAN_POINT('Ctrl Pts',(24.6281997735959,-65.9736784989023,
-54.7499500028688));
#189212=CARTESIAN_POINT('Ctrl Pts',(24.6769571248861,-65.9628648823717,
-54.7524316796293));
#189213=CARTESIAN_POINT('Ctrl Pts',(24.7252054215613,-65.9533744504568,
-54.757346690394));
#189214=CARTESIAN_POINT('Ctrl Pts',(24.7738214860051,-65.9438116786831,
-54.7622991653318));
#189215=CARTESIAN_POINT('Ctrl Pts',(24.8219213290088,-65.935592502924,-54.7697220721195));
#189216=CARTESIAN_POINT('Ctrl Pts',(24.8694314110454,-65.9286135012,-54.7796095236809));
#189217=CARTESIAN_POINT('Ctrl Pts',(24.9169285718598,-65.9216363975412,
-54.7894942861719));
#189218=CARTESIAN_POINT('Ctrl Pts',(24.9638369024156,-65.9158989677116,
-54.801842144168));
#189219=CARTESIAN_POINT('Ctrl Pts',(25.0100848485165,-65.9113231861505,
-54.8166923677705));
#189220=CARTESIAN_POINT('Ctrl Pts',(25.021245893932,-65.9102189099584,-54.8202761814105));
#189221=CARTESIAN_POINT('Ctrl Pts',(25.0323684634138,-65.9091823978081,
-54.8240059448895));
#189222=CARTESIAN_POINT('Ctrl Pts',(25.043451507077,-65.9082127571302,-54.8278826162281));
#189223=CARTESIAN_POINT('Origin',(25.30491873532,-68.8967968514054,-54.74995));
#189224=CARTESIAN_POINT('Origin',(25.30491873532,-68.8967968514054,-54.74995));
#189225=CARTESIAN_POINT('Origin',(25.30491873532,-68.8967968514054,-55.24995));
#189226=CARTESIAN_POINT('Origin',(25.30491873532,-68.8967968514054,-52.64995));
#189227=CARTESIAN_POINT('Ctrl Pts',(0.250869887203161,-71.6009673739963,
-55.3799259279347));
#189228=CARTESIAN_POINT('Ctrl Pts',(0.249744175923989,-71.3544658952986,
-55.234934426789));
#189229=CARTESIAN_POINT('Ctrl Pts',(0.249602310815494,-71.3544665017672,
-54.948950578461));
#189230=CARTESIAN_POINT('Ctrl Pts',(0.0835826979643991,-71.6015824809948,
-55.3799500715247));
#189231=CARTESIAN_POINT('Ctrl Pts',(0.0832191858260445,-71.355178188438,
-55.2349402623292));
#189232=CARTESIAN_POINT('Ctrl Pts',(0.0831608417598922,-71.3551780334291,
-54.9490338518609));
#189233=CARTESIAN_POINT('Ctrl Pts',(-0.0836629414004135,-71.6015821858332,
-55.3799500598782));
#189234=CARTESIAN_POINT('Ctrl Pts',(-0.0832990585829135,-71.3551778467503,
-55.2349402595226));
#189235=CARTESIAN_POINT('Ctrl Pts',(-0.0832406798117105,-71.3551776921241,
-54.9490338120093));
#189236=CARTESIAN_POINT('Ctrl Pts',(-0.250869887202844,-71.6009673739968,
-55.3799259279345));
#189237=CARTESIAN_POINT('Ctrl Pts',(-0.249744175923751,-71.3544658952987,
-55.2349344267889));
#189238=CARTESIAN_POINT('Ctrl Pts',(-0.249602310815417,-71.3544665017672,
-54.9489505784605));
#189239=CARTESIAN_POINT('Origin',(-6.81954492876002E-12,-3.47778663927897,
-52.706487452645));
#189240=CARTESIAN_POINT('Ctrl Pts',(-0.252999996541928,-73.08000002,-57.9657930806539));
#189241=CARTESIAN_POINT('Ctrl Pts',(-0.256592825118373,-73.0800000199999,
-56.2374226811825));
#189242=CARTESIAN_POINT('Ctrl Pts',(-0.25839495935019,-71.5847761540179,
-55.3704858385599));
#189243=CARTESIAN_POINT('Ctrl Pts',(-0.084333524296533,-73.08000002,-57.9654424673068));
#189244=CARTESIAN_POINT('Ctrl Pts',(-0.0855465369638168,-73.0800000199968,
-56.2375896397646));
#189245=CARTESIAN_POINT('Ctrl Pts',(-0.0861369317764507,-71.585454968994,
-55.3705213407165));
#189246=CARTESIAN_POINT('Ctrl Pts',(0.0843331399670236,-73.08000002,-57.9654424664997));
#189247=CARTESIAN_POINT('Ctrl Pts',(0.0855461472403026,-73.0800000199999,
-56.2375896401512));
#189248=CARTESIAN_POINT('Ctrl Pts',(0.0861365392586797,-71.5854549705621,
-55.3705213407996));
#189249=CARTESIAN_POINT('Ctrl Pts',(0.253000003458008,-73.08000002,-57.9657930806683));
#189250=CARTESIAN_POINT('Ctrl Pts',(0.256592832132617,-73.08000002,-56.2374226811757));
#189251=CARTESIAN_POINT('Ctrl Pts',(0.25839496641364,-71.5847761539902,
-55.3704858385584));
#189252=CARTESIAN_POINT('Origin',(1.31216565391057E-11,-73.08000002,-179.672570889095));
#189253=CARTESIAN_POINT('Origin',(-3.54807775957937E-14,-73.08000002,3.11172719585489E-30));
#189254=CARTESIAN_POINT('Origin',(1.0476064460363E-11,-73.08000002,-65.1484573036958));
#189255=CARTESIAN_POINT('Ctrl Pts',(0.253000177461644,-73.08000002,-174.689799914929));
#189256=CARTESIAN_POINT('Ctrl Pts',(0.256818808114103,-73.0800000199999,
-176.343172927719));
#189257=CARTESIAN_POINT('Ctrl Pts',(0.258858142486708,-71.6821458347228,
-177.226154478591));
#189258=CARTESIAN_POINT('Ctrl Pts',(0.0843234703769069,-73.08000002,-174.69018949069));
#189259=CARTESIAN_POINT('Ctrl Pts',(0.0856112439477064,-73.0800000199999,
-176.343045073677));
#189260=CARTESIAN_POINT('Ctrl Pts',(0.0862809304106464,-71.6828245492958,
-177.226124337495));
#189261=CARTESIAN_POINT('Ctrl Pts',(-0.0843431922589527,-73.08000002,-174.690189444595));
#189262=CARTESIAN_POINT('Ctrl Pts',(-0.0856312602925202,-73.0800000199957,
-176.343045088817));
#189263=CARTESIAN_POINT('Ctrl Pts',(-0.0863011085778896,-71.6828244689879,
-177.226124341061));
#189264=CARTESIAN_POINT('Ctrl Pts',(-0.252999822559396,-73.08000002,-174.689799915749));
#189265=CARTESIAN_POINT('Ctrl Pts',(-0.25681844785831,-73.0800000199999,
-176.34317292745));
#189266=CARTESIAN_POINT('Ctrl Pts',(-0.258857779373677,-71.6821458361509,
-177.226154478528));
#189267=CARTESIAN_POINT('Origin',(-1.05821948426232E-11,-3.44156790446887,
-179.298801253201));
#189268=CARTESIAN_POINT('Ctrl Pts',(0.24975130544611,-71.4669668918333,
-177.637584354353));
#189269=CARTESIAN_POINT('Ctrl Pts',(0.249886372443607,-71.4669663151929,
-177.363982952545));
#189270=CARTESIAN_POINT('Ctrl Pts',(0.250942965994211,-71.697396290156,
-177.216474798318));
#189271=CARTESIAN_POINT('Ctrl Pts',(0.0832106206914701,-71.467677902645,
-177.637501435082));
#189272=CARTESIAN_POINT('Ctrl Pts',(0.0832664445309527,-71.4676780488509,
-177.363977402067));
#189273=CARTESIAN_POINT('Ctrl Pts',(0.0836071881580228,-71.698010936898,
-177.216456047988));
#189274=CARTESIAN_POINT('Ctrl Pts',(-0.0832902307503821,-71.4676775627664,
-177.637501474743));
#189275=CARTESIAN_POINT('Ctrl Pts',(-0.0833460872557474,-71.4676777086203,
-177.363977404876));
#189276=CARTESIAN_POINT('Ctrl Pts',(-0.0836871780041486,-71.6980106428669,
-177.216456057091));
#189277=CARTESIAN_POINT('Ctrl Pts',(-0.249751305446095,-71.4669668918333,
-177.637584354353));
#189278=CARTESIAN_POINT('Ctrl Pts',(-0.249886372443348,-71.4669663151928,
-177.363982952544));
#189279=CARTESIAN_POINT('Ctrl Pts',(-0.250942965993822,-71.6973962901568,
-177.216474798318));
#189280=CARTESIAN_POINT('Origin',(1.46650053212127E-12,-13.7527233284612,
-184.368315095325));
#189281=CARTESIAN_POINT('Origin',(0.,-12.9675000200281,-179.64995));
#189282=CARTESIAN_POINT('Origin',(0.,-12.9675000200281,-179.39995));
#189283=CARTESIAN_POINT('Origin',(0.,-12.9675000200281,-179.39995));
#189284=CARTESIAN_POINT('Origin',(0.,-12.9675000200281,-179.64995));
#189285=CARTESIAN_POINT('Origin',(50.5696324866523,-53.08000002,-179.64995));
#189286=CARTESIAN_POINT('Origin',(0.,-12.9675000200281,-179.64995));
#189287=CARTESIAN_POINT('Origin',(0.,-12.9675000200281,-179.39995));
#189288=CARTESIAN_POINT('Origin',(0.,-12.9675000200281,-179.39995));
#189289=CARTESIAN_POINT('Origin',(0.,-12.9675000200281,-179.64995));
#189290=CARTESIAN_POINT('Origin',(0.,-12.9675000200281,-177.84995));
#189291=CARTESIAN_POINT('Origin',(0.,-12.9675000200281,-177.84995));
#189292=CARTESIAN_POINT('Origin',(0.,-12.9675000200281,-177.34995));
#189293=CARTESIAN_POINT('Origin',(-41.5,58.91999998,-177.34995));
#189294=CARTESIAN_POINT('',(-41.5,58.91999998,-177.34995));
#189295=CARTESIAN_POINT('Origin',(0.,58.91999998,0.));
#189296=CARTESIAN_POINT('',(-41.5,58.91999998,-92.34995));
#189297=CARTESIAN_POINT('Origin',(-41.5,58.91999998,-92.34995));
#189298=CARTESIAN_POINT('Origin',(1.1373643128445E-15,-12.9675000200281,
-92.34995));
#189299=CARTESIAN_POINT('Origin',(1.1373643128445E-15,-12.9675000200281,
-91.34995));
#189300=CARTESIAN_POINT('Origin',(1.1373643128445E-15,-12.9675000200281,
-90.9273317382593));
#189301=CARTESIAN_POINT('Origin',(0.,-12.9675000200281,-60.64995));
#189302=CARTESIAN_POINT('Origin',(0.,-12.9675000200281,-60.8508735991007));
#189303=CARTESIAN_POINT('Origin',(0.,-12.9675000200281,-60.42825533736));
#189304=CARTESIAN_POINT('Origin',(0.,-12.9675000200281,-60.42825533736));
#189305=CARTESIAN_POINT('Origin',(0.,-12.9675000200281,-55.24995));
#189306=CARTESIAN_POINT('Origin',(0.,-12.9675000200281,-52.64995));
#189307=CARTESIAN_POINT('Origin',(57.8922230010149,-38.7834964612722,-55.24995));
#189308=CARTESIAN_POINT('Origin',(57.8922230010149,-38.7834964612722,-52.64995));
#189309=CARTESIAN_POINT('Origin',(80.1225000199719,-131.7,-52.64995));
#189310=CARTESIAN_POINT('Origin',(47.392180948596,37.1573950045021,-220.195349461621));
#189311=CARTESIAN_POINT('',(47.392180948596,37.1573950045021,-221.195349461621));
#189312=CARTESIAN_POINT('',(47.392180948596,37.1573950045021,-223.85005));
#189313=CARTESIAN_POINT('',(47.392180948596,37.1573950045021,-220.195349461621));
#189314=CARTESIAN_POINT('',(48.892180948596,38.0234204082866,-223.85005));
#189315=CARTESIAN_POINT('Ctrl Pts',(47.392180948596,37.1573950045022,-223.85005));
#189316=CARTESIAN_POINT('Ctrl Pts',(48.142180948596,37.5904077063944,-223.417037298108));
#189317=CARTESIAN_POINT('Ctrl Pts',(48.8921809485959,38.0234204082866,-223.85005));
#189318=CARTESIAN_POINT('',(48.892180948596,38.0234204082866,-221.195349461621));
#189319=CARTESIAN_POINT('',(48.892180948596,38.0234204082866,-220.195349461621));
#189320=CARTESIAN_POINT('Ctrl Pts',(48.8921809485959,38.0234204082865,-221.195349461621));
#189321=CARTESIAN_POINT('Ctrl Pts',(48.142180948596,37.5904077063944,-220.945349461621));
#189322=CARTESIAN_POINT('Ctrl Pts',(47.3921809485961,37.1573950045022,-221.195349461621));
#189323=CARTESIAN_POINT('Origin',(47.392180948596,35.4253441969333,-220.195349461621));
#189324=CARTESIAN_POINT('',(47.392180948596,35.4253441969333,-221.195349461621));
#189325=CARTESIAN_POINT('',(47.392180948596,35.4253441969333,-223.85005));
#189326=CARTESIAN_POINT('',(47.392180948596,35.4253441969333,-220.195349461621));
#189327=CARTESIAN_POINT('Ctrl Pts',(47.392180948596,35.4253441969333,-223.85005));
#189328=CARTESIAN_POINT('Ctrl Pts',(47.392180948596,36.2913696007178,-223.417037298108));
#189329=CARTESIAN_POINT('Ctrl Pts',(47.392180948596,37.1573950045023,-223.85005));
#189330=CARTESIAN_POINT('Ctrl Pts',(47.392180948596,37.1573950045021,-221.195349461621));
#189331=CARTESIAN_POINT('Ctrl Pts',(47.392180948596,36.2913696007177,-220.945349461621));
#189332=CARTESIAN_POINT('Ctrl Pts',(47.392180948596,35.4253441969334,-221.195349461621));
#189333=CARTESIAN_POINT('Origin',(48.892180948596,34.5593187931488,-220.195349461621));
#189334=CARTESIAN_POINT('',(48.892180948596,34.5593187931488,-221.195349461621));
#189335=CARTESIAN_POINT('',(48.892180948596,34.5593187931488,-223.85005));
#189336=CARTESIAN_POINT('',(48.892180948596,34.5593187931488,-220.195349461621));
#189337=CARTESIAN_POINT('Ctrl Pts',(48.892180948596,34.5593187931488,-223.85005));
#189338=CARTESIAN_POINT('Ctrl Pts',(48.142180948596,34.9923314950411,-223.417037298108));
#189339=CARTESIAN_POINT('Ctrl Pts',(47.392180948596,35.4253441969333,-223.85005));
#189340=CARTESIAN_POINT('Ctrl Pts',(47.3921809485957,35.4253441969335,-221.195349461621));
#189341=CARTESIAN_POINT('Ctrl Pts',(48.1421809485959,34.9923314950412,-220.945349461621));
#189342=CARTESIAN_POINT('Ctrl Pts',(48.8921809485959,34.5593187931489,-221.195349461621));
#189343=CARTESIAN_POINT('Origin',(50.392180948596,35.4253441969333,-220.195349461621));
#189344=CARTESIAN_POINT('',(50.392180948596,35.4253441969323,-221.19534946162));
#189345=CARTESIAN_POINT('',(50.392180948596,35.4253441969333,-223.85005));
#189346=CARTESIAN_POINT('',(50.392180948596,35.4253441969333,-220.195349461621));
#189347=CARTESIAN_POINT('Ctrl Pts',(50.392180948596,35.4253441969333,-223.85005));
#189348=CARTESIAN_POINT('Ctrl Pts',(49.642180948596,34.9923314950411,-223.417037298108));
#189349=CARTESIAN_POINT('Ctrl Pts',(48.8921809485959,34.5593187931488,-223.85005));
#189350=CARTESIAN_POINT('Ctrl Pts',(48.8921809485957,34.5593187931487,-221.195349461621));
#189351=CARTESIAN_POINT('Ctrl Pts',(49.6421809485957,34.9923314950409,-220.945349461621));
#189352=CARTESIAN_POINT('Ctrl Pts',(50.3921809485954,35.425344196933,-221.195349461621));
#189353=CARTESIAN_POINT('Origin',(50.392180948596,37.1573950045021,-220.195349461621));
#189354=CARTESIAN_POINT('',(50.392180948596,37.1573950045021,-221.195349461621));
#189355=CARTESIAN_POINT('',(50.392180948596,37.1573950045021,-223.85005));
#189356=CARTESIAN_POINT('',(50.392180948596,37.1573950045021,-220.195349461621));
#189357=CARTESIAN_POINT('Ctrl Pts',(50.392180948596,37.1573950045021,-223.85005));
#189358=CARTESIAN_POINT('Ctrl Pts',(50.392180948596,36.2913696007177,-223.417037298108));
#189359=CARTESIAN_POINT('Ctrl Pts',(50.392180948596,35.4253441969334,-223.85005));
#189360=CARTESIAN_POINT('Ctrl Pts',(50.392180948596,35.4253441969324,-221.195349461621));
#189361=CARTESIAN_POINT('Ctrl Pts',(50.392180948596,36.2913696007174,-220.945349461621));
#189362=CARTESIAN_POINT('Ctrl Pts',(50.392180948596,37.1573950045021,-221.195349461621));
#189363=CARTESIAN_POINT('Origin',(48.892180948596,38.0234204082866,-220.195349461621));
#189364=CARTESIAN_POINT('Ctrl Pts',(48.892180948596,38.0234204082866,-223.85005));
#189365=CARTESIAN_POINT('Ctrl Pts',(49.642180948596,37.5904077063944,-223.417037298108));
#189366=CARTESIAN_POINT('Ctrl Pts',(50.3921809485959,37.1573950045022,-223.85005));
#189367=CARTESIAN_POINT('Ctrl Pts',(50.392180948596,37.1573950045022,-221.195349461621));
#189368=CARTESIAN_POINT('Ctrl Pts',(49.642180948596,37.5904077063944,-220.945349461621));
#189369=CARTESIAN_POINT('Ctrl Pts',(48.892180948596,38.0234204082866,-221.195349461621));
#189370=CARTESIAN_POINT('Origin',(48.892180948596,36.2913696007177,-221.35005));
#189371=CARTESIAN_POINT('',(48.892180948596,36.2913696007177,-220.195349461621));
#189372=CARTESIAN_POINT('',(48.892180948596,34.2913696007177,-221.35005));
#189373=CARTESIAN_POINT('Origin',(48.892180948596,36.2913696007177,-223.85005));
#189374=CARTESIAN_POINT('Origin',(48.892180948596,36.2913696007177,-223.85005));
#189375=CARTESIAN_POINT('Origin',(48.892180948596,36.2913696007177,-223.85005));
#189376=CARTESIAN_POINT('Origin',(48.892180948596,36.2913696007177,-223.85005));
#189377=CARTESIAN_POINT('Origin',(48.892180948596,36.2913696007177,-223.85005));
#189378=CARTESIAN_POINT('Origin',(48.892180948596,36.2913696007177,-223.85005));
#189379=CARTESIAN_POINT('Origin',(48.892180948596,36.2913696007177,-223.85005));
#189380=CARTESIAN_POINT('Origin',(48.892180948596,36.2913696007177,-223.85005));
#189381=CARTESIAN_POINT('Origin',(48.892180948596,36.2913696007177,-223.85005));
#189382=CARTESIAN_POINT('Origin',(48.892180948596,36.2913696007177,-223.85005));
#189383=CARTESIAN_POINT('Origin',(48.892180948596,36.2913696007177,-223.85005));
#189384=CARTESIAN_POINT('Origin',(48.892180948596,36.2913696007177,-223.85005));
#189385=CARTESIAN_POINT('Origin',(48.892180948596,36.2913696007177,-223.60005));
#189386=CARTESIAN_POINT('',(48.892180948596,33.2913696007177,-223.85005));
#189387=CARTESIAN_POINT('Origin',(48.892180948596,36.2913696007177,-223.85005));
#189388=CARTESIAN_POINT('',(48.892180948596,33.0413696007177,-223.60005));
#189389=CARTESIAN_POINT('Origin',(48.892180948596,33.2913696007177,-223.60005));
#189390=CARTESIAN_POINT('',(48.892180948596,39.5413696007177,-223.60005));
#189391=CARTESIAN_POINT('Origin',(48.892180948596,36.2913696007177,-223.60005));
#189392=CARTESIAN_POINT('Origin',(48.892180948596,36.2913696007177,-223.60005));
#189393=CARTESIAN_POINT('Origin',(48.892180948596,36.2913696007177,-218.35005));
#189394=CARTESIAN_POINT('',(48.892180948596,39.5413696007177,-218.35005));
#189395=CARTESIAN_POINT('Origin',(48.892180948596,36.2913696007177,-218.35005));
#189396=CARTESIAN_POINT('Origin',(48.892180948596,36.2913696007177,-223.85005));
#189397=CARTESIAN_POINT('Origin',(48.892180948596,36.2913696007177,-223.85005));
#189398=CARTESIAN_POINT('',(48.892180948596,39.5413696007177,-223.85005));
#189399=CARTESIAN_POINT('Origin',(44.5079524583208,-57.4754524783487,-39.8944822890418));
#189400=CARTESIAN_POINT('',(46.5079524583208,-57.4754524783487,-40.4194822890418));
#189401=CARTESIAN_POINT('Origin',(44.5079524583208,-57.4754524783487,-40.4194822890418));
#189402=CARTESIAN_POINT('',(45.9829524583208,-57.4754524783487,-39.8944822890418));
#189403=CARTESIAN_POINT('',(45.9829524583208,-57.4754524783487,-39.8944822890418));
#189404=CARTESIAN_POINT('Origin',(44.5079524583208,-57.4754524783487,-39.8944822890418));
#189405=CARTESIAN_POINT('Origin',(44.5079524583208,-57.4754524783487,-39.8944822890418));
#189406=CARTESIAN_POINT('Origin',(44.5079524583208,-57.4754524783487,-39.8944822890418));
#189407=CARTESIAN_POINT('',(46.5079524583208,-57.4754524783487,-55.24995));
#189408=CARTESIAN_POINT('Origin',(44.5079524583208,-57.4754524783487,-55.24995));
#189409=CARTESIAN_POINT('',(46.5079524583208,-57.4754524783487,-39.8944822890418));
#189410=CARTESIAN_POINT('Origin',(0.,45.41999998,-55.24995));
#189411=CARTESIAN_POINT('',(47.0079524583208,-57.4754524783487,-55.24995));
#189412=CARTESIAN_POINT('Origin',(44.5079524583208,-57.4754524783487,-55.24995));
#189413=CARTESIAN_POINT('Origin',(44.5079524583208,-57.4754524783487,-48.1788821881345));
#189414=CARTESIAN_POINT('',(47.0079524583208,-57.4754524783487,-179.64995));
#189415=CARTESIAN_POINT('Origin',(44.5079524583208,-57.4754524783487,-179.64995));
#189416=CARTESIAN_POINT('',(47.0079524583208,-57.4754524783487,-48.1788821881345));
#189417=CARTESIAN_POINT('Origin',(44.5079524583208,-57.4754524783487,-179.64995));
#189418=CARTESIAN_POINT('Ctrl Pts',(-52.1258919562643,38.67266339879,-228.35005));
#189419=CARTESIAN_POINT('Ctrl Pts',(-51.7302447133037,38.3813101134616,
-228.35005));
#189420=CARTESIAN_POINT('Ctrl Pts',(-51.7233397168138,38.3762252975093,
-227.858776203219));
#189421=CARTESIAN_POINT('Ctrl Pts',(-52.0466039743291,38.878041220954,-228.35005));
#189422=CARTESIAN_POINT('Ctrl Pts',(-51.6128088111955,38.5425689461205,
-228.410692739194));
#189423=CARTESIAN_POINT('Ctrl Pts',(-51.6174495896917,38.5200202664566,
-227.858776175692));
#189424=CARTESIAN_POINT('Ctrl Pts',(-51.9333069568917,39.0542288907298,
-228.338384512236));
#189425=CARTESIAN_POINT('Ctrl Pts',(-51.5043449566927,38.6663650434491,
-228.441452922891));
#189426=CARTESIAN_POINT('Ctrl Pts',(-51.5002798258237,38.6559630716119,
-227.854887707304));
#189427=CARTESIAN_POINT('Ctrl Pts',(-51.6439737530735,39.342374196026,-228.3384118607));
#189428=CARTESIAN_POINT('Ctrl Pts',(-51.2577525408945,38.9120667908531,
-228.441337182113));
#189429=CARTESIAN_POINT('Ctrl Pts',(-51.247332174135,38.9079983209904,-227.854896823446));
#189430=CARTESIAN_POINT('Ctrl Pts',(-51.4685984426326,39.4543128793957,
-228.35005));
#189431=CARTESIAN_POINT('Ctrl Pts',(-51.1344983277446,39.0193462915006,
-228.410782960183));
#189432=CARTESIAN_POINT('Ctrl Pts',(-51.1119650116918,39.023887086559,-227.858776175352));
#189433=CARTESIAN_POINT('Ctrl Pts',(-51.2626335243565,39.533036088795,-228.35005));
#189434=CARTESIAN_POINT('Ctrl Pts',(-50.9726066716339,39.136415486161,-228.35005));
#189435=CARTESIAN_POINT('Ctrl Pts',(-50.9675450051224,39.1294935022024,
-227.858776203219));
#189436=CARTESIAN_POINT('',(-52.1258919562641,38.6726633987897,-228.35005));
#189437=CARTESIAN_POINT('',(-51.7233397168138,38.3762252975093,-227.858776203219));
#189438=CARTESIAN_POINT('Origin',(-52.1258919562641,38.6726633987897,-227.85005));
#189439=CARTESIAN_POINT('',(-51.2626335243563,39.5330360887948,-228.35005));
#189440=CARTESIAN_POINT('Ctrl Pts',(-52.1258919562641,38.6726633987897,
-228.35005));
#189441=CARTESIAN_POINT('Ctrl Pts',(-52.0466039743291,38.878041220954,-228.35005));
#189442=CARTESIAN_POINT('Ctrl Pts',(-51.9333069568917,39.0542288907298,
-228.338384512236));
#189443=CARTESIAN_POINT('Ctrl Pts',(-51.6439737530735,39.342374196026,-228.3384118607));
#189444=CARTESIAN_POINT('Ctrl Pts',(-51.4685984426326,39.4543128793957,
-228.35005));
#189445=CARTESIAN_POINT('Ctrl Pts',(-51.2626335243563,39.5330360887948,
-228.35005));
#189446=CARTESIAN_POINT('',(-50.9675450051224,39.1294935022024,-227.858776203219));
#189447=CARTESIAN_POINT('Origin',(-51.2626335243564,39.5330360887949,-227.85005));
#189448=CARTESIAN_POINT('Ctrl Pts',(-50.9675450051224,39.1294935022024,
-227.858776203219));
#189449=CARTESIAN_POINT('Ctrl Pts',(-51.1119650120529,39.0238870864862,
-227.858776184197));
#189450=CARTESIAN_POINT('Ctrl Pts',(-51.2473321742961,38.9079983210533,
-227.854896832514));
#189451=CARTESIAN_POINT('Ctrl Pts',(-51.5002798258866,38.6559630717727,
-227.854887716373));
#189452=CARTESIAN_POINT('Ctrl Pts',(-51.6174495896174,38.520020266818,-227.858776184536));
#189453=CARTESIAN_POINT('Ctrl Pts',(-51.7233397168138,38.3762252975093,
-227.858776203219));
#189454=CARTESIAN_POINT('Origin',(-48.1334350484927,-61.7961505568785,-227.85005));
#189455=CARTESIAN_POINT('',(-48.1334350484927,-57.7802512760377,-228.35005));
#189456=CARTESIAN_POINT('Origin',(-48.1334350484927,-61.7961505568785,-228.35005));
#189457=CARTESIAN_POINT('',(-48.1334350484927,-58.2801751236159,-227.858776203219));
#189458=CARTESIAN_POINT('Origin',(-48.1334350484927,-57.7802512760377,-227.85005));
#189459=CARTESIAN_POINT('',(-48.1334350484927,-65.3121259901411,-227.858776203219));
#189460=CARTESIAN_POINT('Origin',(-48.1334350484927,-61.7961505568785,-227.858776203219));
#189461=CARTESIAN_POINT('Origin',(-48.1334350484927,-61.7961505568785,-227.858776203219));
#189462=CARTESIAN_POINT('Ctrl Pts',(-54.3075179287798,-60.4058635314347,
-219.986910060041));
#189463=CARTESIAN_POINT('Ctrl Pts',(-53.9849086976504,-60.7491038125482,
-220.006959754302));
#189464=CARTESIAN_POINT('Ctrl Pts',(-54.2123842387114,-60.9809369188682,
-220.34872120014));
#189465=CARTESIAN_POINT('Ctrl Pts',(-54.4118428785764,-60.5120824447637,
-219.845412347007));
#189466=CARTESIAN_POINT('Ctrl Pts',(-54.0902539551932,-60.8227589927709,
-219.884871134182));
#189467=CARTESIAN_POINT('Ctrl Pts',(-54.2905773520916,-61.0606279145824,
-220.207250076519));
#189468=CARTESIAN_POINT('Ctrl Pts',(-54.5038491541938,-60.6290451815934,
-219.706184350974));
#189469=CARTESIAN_POINT('Ctrl Pts',(-54.1883692315684,-60.9105945733191,
-219.759116870628));
#189470=CARTESIAN_POINT('Ctrl Pts',(-54.359483942211,-61.1484321661822,
-220.068048613768));
#189471=CARTESIAN_POINT('Ctrl Pts',(-54.6622597796057,-60.8851359437949,
-219.432400986523));
#189472=CARTESIAN_POINT('Ctrl Pts',(-54.3601921871582,-61.1113013655168,
-219.509518223974));
#189473=CARTESIAN_POINT('Ctrl Pts',(-54.4780017311477,-61.3407746536632,
-219.794316977736));
#189474=CARTESIAN_POINT('Ctrl Pts',(-54.7291280292794,-61.0257268060043,
-219.296601153239));
#189475=CARTESIAN_POINT('Ctrl Pts',(-54.4358335264202,-61.2248747082992,
-219.383842189251));
#189476=CARTESIAN_POINT('Ctrl Pts',(-54.5279586596326,-61.446412888813,
-219.65854206581));
#189477=CARTESIAN_POINT('Ctrl Pts',(-54.8292130354716,-61.3244815513707,
-219.038012931782));
#189478=CARTESIAN_POINT('Ctrl Pts',(-54.5543689314778,-61.4719546649741,
-219.14339871115));
#189479=CARTESIAN_POINT('Ctrl Pts',(-54.6025429402354,-61.6709815877615,
-219.399995666978));
#189480=CARTESIAN_POINT('Ctrl Pts',(-54.8629184699328,-61.4823979173529,
-218.91503263841));
#189481=CARTESIAN_POINT('Ctrl Pts',(-54.5990060222798,-61.6050459038155,
-219.027646728977));
#189482=CARTESIAN_POINT('Ctrl Pts',(-54.6275380455226,-61.7897249373759,
-219.277032330244));
#189483=CARTESIAN_POINT('Ctrl Pts',(-54.8898067560436,-61.8191471195152,
-218.684386523561));
#189484=CARTESIAN_POINT('Ctrl Pts',(-54.6493563799718,-61.8922244718457,
-218.810400243034));
#189485=CARTESIAN_POINT('Ctrl Pts',(-54.647034139304,-62.0430255579662,
-219.046408327256));
#189486=CARTESIAN_POINT('Ctrl Pts',(-54.8823609599705,-61.9966926518129,
-218.577969748942));
#189487=CARTESIAN_POINT('Ctrl Pts',(-54.6555291975718,-62.0456431176188,
-218.709001772434));
#189488=CARTESIAN_POINT('Ctrl Pts',(-54.6410642456133,-62.1766218791827,
-218.939992225722));
#189489=CARTESIAN_POINT('Ctrl Pts',(-54.848380895554,-62.1772035872432,
-218.488025452359));
#189490=CARTESIAN_POINT('Ctrl Pts',(-54.6359260398381,-62.2035651560494,
-218.622717457036));
#189491=CARTESIAN_POINT('Ctrl Pts',(-54.6151554910244,-62.3124799546862,
-218.850050000001));
#189492=CARTESIAN_POINT('',(-54.8483808955536,-62.1772035872456,-218.488025452358));
#189493=CARTESIAN_POINT('',(-54.615155491024,-62.3124799546881,-218.85005));
#189494=CARTESIAN_POINT('Origin',(-55.1063041457817,-62.4061442430845,-218.85005));
#189495=CARTESIAN_POINT('',(-54.3075179287798,-60.4058635314347,-219.986910060041));
#189496=CARTESIAN_POINT('Ctrl Pts',(-54.848380895554,-62.1772035872432,
-218.488025452359));
#189497=CARTESIAN_POINT('Ctrl Pts',(-54.8595780951869,-62.1177211520375,
-218.517664132037));
#189498=CARTESIAN_POINT('Ctrl Pts',(-54.8678564354561,-62.0587810758137,
-218.548979039057));
#189499=CARTESIAN_POINT('Ctrl Pts',(-54.8734777099623,-62.0004951202735,
-218.581727253403));
#189500=CARTESIAN_POINT('Ctrl Pts',(-54.8794967639978,-61.938084662374,
-218.616792837108));
#189501=CARTESIAN_POINT('Ctrl Pts',(-54.8824693653365,-61.8764235088643,
-218.653502177912));
#189502=CARTESIAN_POINT('Ctrl Pts',(-54.8826645527091,-61.8156518057411,
-218.691591283871));
#189503=CARTESIAN_POINT('Ctrl Pts',(-54.8828436018076,-61.7599047637286,
-218.726531147015));
#189504=CARTESIAN_POINT('Ctrl Pts',(-54.8806845561614,-61.7049057976097,
-218.762632937314));
#189505=CARTESIAN_POINT('Ctrl Pts',(-54.8763620068721,-61.6507727587229,
-218.799709864555));
#189506=CARTESIAN_POINT('Ctrl Pts',(-54.8763424593423,-61.6505279570743,
-218.799877534671));
#189507=CARTESIAN_POINT('Ctrl Pts',(-54.8763228688493,-61.6502831758786,
-218.800045222108));
#189508=CARTESIAN_POINT('Ctrl Pts',(-54.8763032354027,-61.6500384151225,
-218.800212926867));
#189509=CARTESIAN_POINT('Ctrl Pts',(-54.8628119724682,-61.4818493143656,
-218.915452449409));
#189510=CARTESIAN_POINT('Ctrl Pts',(-54.8291146403181,-61.3241894585148,
-219.038266143607));
#189511=CARTESIAN_POINT('Ctrl Pts',(-54.7791703042592,-61.1751043200491,
-219.167307118481));
#189512=CARTESIAN_POINT('Ctrl Pts',(-54.7790856375892,-61.174851587843,
-219.167525871407));
#189513=CARTESIAN_POINT('Ctrl Pts',(-54.7790009228209,-61.1745988809923,
-219.167744642781));
#189514=CARTESIAN_POINT('Ctrl Pts',(-54.7789161599765,-61.1743461995148,
-219.167963432577));
#189515=CARTESIAN_POINT('Ctrl Pts',(-54.7321821211911,-61.0350301342545,
-219.28859330143));
#189516=CARTESIAN_POINT('Ctrl Pts',(-54.6708383603461,-60.9034276385766,
-219.414819506217));
#189517=CARTESIAN_POINT('Ctrl Pts',(-54.5985282010653,-60.7825291661754,
-219.542285530591));
#189518=CARTESIAN_POINT('Ctrl Pts',(-54.5934244574704,-60.7739959972504,
-219.55128224574));
#189519=CARTESIAN_POINT('Ctrl Pts',(-54.5882660645263,-60.7655161587595,
-219.560285146215));
#189520=CARTESIAN_POINT('Ctrl Pts',(-54.5830542956885,-60.757090705388,
-219.569292703597));
#189521=CARTESIAN_POINT('Ctrl Pts',(-54.5829701683847,-60.7569547034476,
-219.569438101741));
#189522=CARTESIAN_POINT('Ctrl Pts',(-54.5828860266502,-60.7568187140274,
-219.569583502502));
#189523=CARTESIAN_POINT('Ctrl Pts',(-54.5828018704853,-60.7566827371269,
-219.569728905881));
#189524=CARTESIAN_POINT('Ctrl Pts',(-54.5036381576416,-60.62877248456,-219.706506423312));
#189525=CARTESIAN_POINT('Ctrl Pts',(-54.4117181269149,-60.5119554283026,
-219.845581549818));
#189526=CARTESIAN_POINT('Ctrl Pts',(-54.3075179287798,-60.4058635314347,
-219.986910060041));
#189527=CARTESIAN_POINT('',(-54.2123842387114,-60.9809369188682,-220.34872120014));
#189528=CARTESIAN_POINT('Origin',(-54.5692758093764,-60.630753528645,-220.34872120014));
#189529=CARTESIAN_POINT('Ctrl Pts',(-54.2123842387114,-60.9809369188682,
-220.34872120014));
#189530=CARTESIAN_POINT('Ctrl Pts',(-54.2905773520916,-61.0606279145824,
-220.207250076519));
#189531=CARTESIAN_POINT('Ctrl Pts',(-54.359483942211,-61.1484321661822,
-220.068048613768));
#189532=CARTESIAN_POINT('Ctrl Pts',(-54.4780017311477,-61.3407746536632,
-219.794316977736));
#189533=CARTESIAN_POINT('Ctrl Pts',(-54.5279586596326,-61.446412888813,
-219.65854206581));
#189534=CARTESIAN_POINT('Ctrl Pts',(-54.6025429402354,-61.6709815877615,
-219.399995666978));
#189535=CARTESIAN_POINT('Ctrl Pts',(-54.6275380455226,-61.7897249373759,
-219.277032330244));
#189536=CARTESIAN_POINT('Ctrl Pts',(-54.647034139304,-62.0430255579662,
-219.046408327256));
#189537=CARTESIAN_POINT('Ctrl Pts',(-54.6410642456133,-62.1766218791827,
-218.939992225722));
#189538=CARTESIAN_POINT('Ctrl Pts',(-54.615155491024,-62.3124799546881,
-218.85005));
#189539=CARTESIAN_POINT('Ctrl Pts',(-54.2123842387114,-60.9809369188682,
-220.34872120014));
#189540=CARTESIAN_POINT('Ctrl Pts',(-53.9849086976503,-60.7491038125481,
-220.006959754301));
#189541=CARTESIAN_POINT('Ctrl Pts',(-54.3075179287798,-60.4058635314347,
-219.986910060041));
#189542=CARTESIAN_POINT('Ctrl Pts',(-52.433041068884,-59.1675083087135,
-222.763182656182));
#189543=CARTESIAN_POINT('Ctrl Pts',(-52.2079291156962,-58.9380840675622,
-222.419842682816));
#189544=CARTESIAN_POINT('Ctrl Pts',(-52.5270340116508,-58.593055911284,
-222.401810820094));
#189545=CARTESIAN_POINT('Ctrl Pts',(-50.6562579911382,-57.3566888322572,
-225.181485677498));
#189546=CARTESIAN_POINT('Ctrl Pts',(-50.428037288823,-57.124096290766,-224.842059161051));
#189547=CARTESIAN_POINT('Ctrl Pts',(-50.7503363279055,-56.7819842883116,
-224.820210504335));
#189548=CARTESIAN_POINT('Ctrl Pts',(-48.8796513269547,-55.5460491487752,
-227.60005));
#189549=CARTESIAN_POINT('Ctrl Pts',(-48.6520074870279,-55.3140445196239,
-227.259140997287));
#189550=CARTESIAN_POINT('Ctrl Pts',(-48.9740484537045,-54.9709070690089,
-227.238815650979));
#189551=CARTESIAN_POINT('',(-48.8796513269546,-55.5460491487752,-227.60005));
#189552=CARTESIAN_POINT('',(-48.9740484537045,-54.9709070690089,-227.238815650979));
#189553=CARTESIAN_POINT('Origin',(-49.2365428976196,-55.195865758552,-227.60005));
#189554=CARTESIAN_POINT('Ctrl Pts',(-48.8796513269547,-55.5460491487752,
-227.60005));
#189555=CARTESIAN_POINT('Ctrl Pts',(-50.6562583519279,-57.3566891999582,
-225.181485185797));
#189556=CARTESIAN_POINT('Ctrl Pts',(-52.4330406746144,-59.1675079068912,
-222.763183190988));
#189557=CARTESIAN_POINT('Ctrl Pts',(-54.2123842387114,-60.9809369188682,
-220.34872120014));
#189558=CARTESIAN_POINT('Ctrl Pts',(-54.3075179287797,-60.4058635314346,
-219.98691006004));
#189559=CARTESIAN_POINT('Ctrl Pts',(-53.9280885484023,-60.0195458200305,
-220.501536611982));
#189560=CARTESIAN_POINT('Ctrl Pts',(-53.5487761278274,-59.6334370507339,
-221.016322062621));
#189561=CARTESIAN_POINT('Ctrl Pts',(-53.1695953219721,-59.247391120128,
-221.531234538341));
#189562=CARTESIAN_POINT('Ctrl Pts',(-52.822845399714,-58.8943632390786,
-222.002107162083));
#189563=CARTESIAN_POINT('Ctrl Pts',(-52.4762070166413,-58.5413872899351,
-222.473086011508));
#189564=CARTESIAN_POINT('Ctrl Pts',(-52.1296859830356,-58.1883927825386,
-222.944146711797));
#189565=CARTESIAN_POINT('Ctrl Pts',(-51.8076614103319,-57.8603523625148,
-223.381906922627));
#189566=CARTESIAN_POINT('Ctrl Pts',(-51.4857387604864,-57.532295845902,
-223.81973782087));
#189567=CARTESIAN_POINT('Ctrl Pts',(-51.1639046996426,-57.204208016568,
-224.257619844239));
#189568=CARTESIAN_POINT('Ctrl Pts',(-50.9738908938116,-57.0105019279858,
-224.516149440352));
#189569=CARTESIAN_POINT('Ctrl Pts',(-50.7839075752795,-56.8167857278758,
-224.774696857818));
#189570=CARTESIAN_POINT('Ctrl Pts',(-50.5939477257631,-56.6230638244338,
-225.033258070589));
#189571=CARTESIAN_POINT('Ctrl Pts',(-50.2918176133923,-56.314950185659,
-225.444498279865));
#189572=CARTESIAN_POINT('Ctrl Pts',(-49.9897484304673,-56.006819869112,
-225.85577338675));
#189573=CARTESIAN_POINT('Ctrl Pts',(-49.6876934835399,-55.6987203846147,
-226.26706719271));
#189574=CARTESIAN_POINT('Ctrl Pts',(-49.4498154301899,-55.4560820621642,
-226.590974385465));
#189575=CARTESIAN_POINT('Ctrl Pts',(-49.211945725251,-55.2134636586754,
-226.914893175522));
#189576=CARTESIAN_POINT('Ctrl Pts',(-48.9740484537044,-54.9709070690088,
-227.238815650979));
#189577=CARTESIAN_POINT('Origin',(-55.1063041457817,-62.4061442430845,-218.85005));
#189578=CARTESIAN_POINT('',(-55.1063041458243,-62.4061442430364,-218.35005));
#189579=CARTESIAN_POINT('Origin',(-55.1063041458054,-62.4061442430575,-218.85005));
#189580=CARTESIAN_POINT('Origin',(-55.1063041457932,-62.4061442430715,-218.85005));
#189581=CARTESIAN_POINT('Ctrl Pts',(-47.09240585629,-55.1677510010868,-228.462945982586));
#189582=CARTESIAN_POINT('Ctrl Pts',(-47.2381429264814,-55.2254222593817,
-228.322991735478));
#189583=CARTESIAN_POINT('Ctrl Pts',(-47.4171327932804,-55.3325755327477,
-228.334859743751));
#189584=CARTESIAN_POINT('Ctrl Pts',(-47.2344276267258,-54.917085392156,
-228.523519253622));
#189585=CARTESIAN_POINT('Ctrl Pts',(-47.3356274805824,-55.0226067438265,
-228.38397647119));
#189586=CARTESIAN_POINT('Ctrl Pts',(-47.4809019204392,-55.1586334957497,
-228.371096678113));
#189587=CARTESIAN_POINT('Ctrl Pts',(-47.4670751686631,-54.738003414354,
-228.471361175594));
#189588=CARTESIAN_POINT('Ctrl Pts',(-47.5256804778557,-54.8863412485756,
-228.335161447142));
#189589=CARTESIAN_POINT('Ctrl Pts',(-47.6309431060146,-55.0605826721568,
-228.339785024153));
#189590=CARTESIAN_POINT('Ctrl Pts',(-47.8754484729887,-54.5910305088289,
-228.271269171667));
#189591=CARTESIAN_POINT('Ctrl Pts',(-47.8504418710462,-54.8033124018473,
-228.155509466566));
#189592=CARTESIAN_POINT('Ctrl Pts',(-47.9276993204187,-55.0230946822617,
-228.219783397522));
#189593=CARTESIAN_POINT('Ctrl Pts',(-48.0443924842659,-54.5757186289002,
-228.159050207984));
#189594=CARTESIAN_POINT('Ctrl Pts',(-47.9863174736057,-54.8118823401931,
-228.052588015267));
#189595=CARTESIAN_POINT('Ctrl Pts',(-48.0594981945084,-55.0442134699009,
-228.152500861763));
#189596=CARTESIAN_POINT('Ctrl Pts',(-48.3554209171899,-54.6057538752492,
-227.91548473754));
#189597=CARTESIAN_POINT('Ctrl Pts',(-48.2285289945118,-54.8818438998474,
-227.834638886779));
#189598=CARTESIAN_POINT('Ctrl Pts',(-48.3137201093166,-55.1299765132312,
-228.006463242484));
#189599=CARTESIAN_POINT('Ctrl Pts',(-48.4988095574202,-54.650729797923,
-227.78342703208));
#189600=CARTESIAN_POINT('Ctrl Pts',(-48.3367798591397,-54.9456151314884,
-227.716732009813));
#189601=CARTESIAN_POINT('Ctrl Pts',(-48.4371064446681,-55.1945753847142,
-227.927285297474));
#189602=CARTESIAN_POINT('Ctrl Pts',(-48.8101521013542,-54.8085677819245,
-227.459055716783));
#189603=CARTESIAN_POINT('Ctrl Pts',(-48.5612091036401,-55.1417548970017,
-227.432331867016));
#189604=CARTESIAN_POINT('Ctrl Pts',(-48.7169768560648,-55.3833010737937,
-227.732785637971));
#189605=CARTESIAN_POINT('Ctrl Pts',(-48.962196654591,-54.9393505733203,
-227.26705029275));
#189606=CARTESIAN_POINT('Ctrl Pts',(-48.6555172039462,-55.293056012404,
-227.269754320687));
#189607=CARTESIAN_POINT('Ctrl Pts',(-48.8643360818247,-55.5187090833383,
-227.617637443069));
#189608=CARTESIAN_POINT('Ctrl Pts',(-49.0890536832928,-55.1029800540788,
-227.073013622619));
#189609=CARTESIAN_POINT('Ctrl Pts',(-48.7110565412925,-55.4558374114165,
-227.127899351983));
#189610=CARTESIAN_POINT('Ctrl Pts',(-48.9981163054993,-55.6756001905466,
-227.501240761046));
#189611=CARTESIAN_POINT('',(-47.4910910659473,-55.2017568268661,-228.35005));
#189612=CARTESIAN_POINT('',(-47.2343490658922,-54.9709330687352,-228.488381729218));
#189613=CARTESIAN_POINT('Origin',(-47.4910910659474,-55.2017568268662,-228.85005));
#189614=CARTESIAN_POINT('Ctrl Pts',(-47.4910910659473,-55.2017568268661,
-228.35005));
#189615=CARTESIAN_POINT('Ctrl Pts',(-47.5089077383994,-55.1802048283969,
-228.35005));
#189616=CARTESIAN_POINT('Ctrl Pts',(-47.5286070144591,-55.1606954806881,
-228.348498778758));
#189617=CARTESIAN_POINT('Ctrl Pts',(-47.5498778530217,-55.1432566637227,
-228.345450688067));
#189618=CARTESIAN_POINT('Ctrl Pts',(-47.571248428113,-55.1257360781397,
-228.342388305228));
#189619=CARTESIAN_POINT('Ctrl Pts',(-47.5942048306929,-55.1103059835697,
-228.337815232383));
#189620=CARTESIAN_POINT('Ctrl Pts',(-47.6184440641068,-55.0969824475394,
-228.331836254939));
#189621=CARTESIAN_POINT('Ctrl Pts',(-47.6427626834775,-55.0836152755725,
-228.325837695735));
#189622=CARTESIAN_POINT('Ctrl Pts',(-47.6683721101493,-55.0723689149521,
-228.318424429409));
#189623=CARTESIAN_POINT('Ctrl Pts',(-47.694986021396,-55.0632403004126,
-228.309747053101));
#189624=CARTESIAN_POINT('Ctrl Pts',(-47.7218011327211,-55.0540426739213,
-228.301004076183));
#189625=CARTESIAN_POINT('Ctrl Pts',(-47.7496356054836,-55.0469952960427,
-228.29097833533));
#189626=CARTESIAN_POINT('Ctrl Pts',(-47.7782226616637,-55.0420694341252,
-228.279862071304));
#189627=CARTESIAN_POINT('Ctrl Pts',(-47.7866984206837,-55.0406089683005,
-228.276566216897));
#189628=CARTESIAN_POINT('Ctrl Pts',(-47.7952405287646,-55.0393348075036,
-228.273174722161));
#189629=CARTESIAN_POINT('Ctrl Pts',(-47.8038425343185,-55.0382457107992,
-228.269693122561));
#189630=CARTESIAN_POINT('Ctrl Pts',(-47.8373355981116,-55.0340051665251,
-228.256137046974));
#189631=CARTESIAN_POINT('Ctrl Pts',(-47.8714478407728,-55.0324380445811,
-228.241273865974));
#189632=CARTESIAN_POINT('Ctrl Pts',(-47.9058935132037,-55.0332769093997,
-228.225382280215));
#189633=CARTESIAN_POINT('Ctrl Pts',(-47.941344924102,-55.0341402672405,
-228.209026694831));
#189634=CARTESIAN_POINT('Ctrl Pts',(-47.9771500135531,-55.0375516776966,
-228.191582014499));
#189635=CARTESIAN_POINT('Ctrl Pts',(-48.0130258818976,-55.0431915097372,
-228.173311683241));
#189636=CARTESIAN_POINT('Ctrl Pts',(-48.0505695742846,-55.049093530483,
-228.154191987238));
#189637=CARTESIAN_POINT('Ctrl Pts',(-48.0881912505395,-55.0574355196171,
-228.134168324689));
#189638=CARTESIAN_POINT('Ctrl Pts',(-48.1255900814225,-55.0678282154976,
-228.113495063768));
#189639=CARTESIAN_POINT('Ctrl Pts',(-48.1459525590084,-55.0734867088762,
-228.102239128697));
#189640=CARTESIAN_POINT('Ctrl Pts',(-48.166249328711,-55.0797527784695,
-228.09078978545));
#189641=CARTESIAN_POINT('Ctrl Pts',(-48.1864338070466,-55.0865616605034,
-228.079182315661));
#189642=CARTESIAN_POINT('Ctrl Pts',(-48.2254371008043,-55.0997187419852,
-228.056752726625));
#189643=CARTESIAN_POINT('Ctrl Pts',(-48.2640817812442,-55.1149286557663,
-228.03370656281));
#189644=CARTESIAN_POINT('Ctrl Pts',(-48.3022877633549,-55.1319614950397,
-228.010221319788));
#189645=CARTESIAN_POINT('Ctrl Pts',(-48.3417574665396,-55.1495577214256,
-227.985959266568));
#189646=CARTESIAN_POINT('Ctrl Pts',(-48.3807595496667,-55.1690988911915,
-227.961228118431));
#189647=CARTESIAN_POINT('Ctrl Pts',(-48.4191997560302,-55.1903373681973,
-227.936167758128));
#189648=CARTESIAN_POINT('Ctrl Pts',(-48.4593464424128,-55.2125186870885,
-227.909994890682));
#189649=CARTESIAN_POINT('Ctrl Pts',(-48.4988808327079,-55.2365507915592,
-227.883462342538));
#189650=CARTESIAN_POINT('Ctrl Pts',(-48.5376800280217,-55.2621668115556,
-227.856677877223));
#189651=CARTESIAN_POINT('Ctrl Pts',(-48.5429562511707,-55.2656502816791,
-227.853035512612));
#189652=CARTESIAN_POINT('Ctrl Pts',(-48.5482188485838,-55.2691630721293,
-227.849388422952));
#189653=CARTESIAN_POINT('Ctrl Pts',(-48.5534674817022,-55.2727045407243,
-227.845736819723));
#189654=CARTESIAN_POINT('Ctrl Pts',(-48.5900388830808,-55.2973807690938,
-227.820293195764));
#189655=CARTESIAN_POINT('Ctrl Pts',(-48.6257862712802,-55.3233531933449,
-227.794749601736));
#189656=CARTESIAN_POINT('Ctrl Pts',(-48.6607701121414,-55.3505444605623,
-227.769136578206));
#189657=CARTESIAN_POINT('Ctrl Pts',(-48.6963360307854,-55.378188149016,
-227.743097393008));
#189658=CARTESIAN_POINT('Ctrl Pts',(-48.731113046917,-55.4070913174802,
-227.71698545506));
#189659=CARTESIAN_POINT('Ctrl Pts',(-48.765131866684,-55.4372048986578,
-227.690804458223));
#189660=CARTESIAN_POINT('Ctrl Pts',(-48.7994856980231,-55.4676150332795,
-227.664365635366));
#189661=CARTESIAN_POINT('Ctrl Pts',(-48.8330664766557,-55.4992593903386,
-227.637855322385));
#189662=CARTESIAN_POINT('Ctrl Pts',(-48.8658695253829,-55.5321230557835,
-227.611264277926));
#189663=CARTESIAN_POINT('Ctrl Pts',(-48.8704788993216,-55.5367409473793,
-227.607527793908));
#189664=CARTESIAN_POINT('Ctrl Pts',(-48.8750728571358,-55.5413829729072,
-227.603789710314));
#189665=CARTESIAN_POINT('Ctrl Pts',(-48.8796513269546,-55.5460491487752,
-227.60005));
#189666=CARTESIAN_POINT('Ctrl Pts',(-48.9740484537045,-54.9709070690089,
-227.238815650979));
#189667=CARTESIAN_POINT('Ctrl Pts',(-48.8729000175802,-54.8677776014257,
-227.376540018855));
#189668=CARTESIAN_POINT('Ctrl Pts',(-48.7582616773652,-54.7822614512576,
-227.513117602665));
#189669=CARTESIAN_POINT('Ctrl Pts',(-48.4988095574202,-54.650729797923,
-227.78342703208));
#189670=CARTESIAN_POINT('Ctrl Pts',(-48.3554209171899,-54.6057538752492,
-227.91548473754));
#189671=CARTESIAN_POINT('Ctrl Pts',(-48.0443924842659,-54.5757186289002,
-228.159050207984));
#189672=CARTESIAN_POINT('Ctrl Pts',(-47.8754484729887,-54.5910305088289,
-228.271269171667));
#189673=CARTESIAN_POINT('Ctrl Pts',(-47.5351373860507,-54.7135079300998,
-228.438012508273));
#189674=CARTESIAN_POINT('Ctrl Pts',(-47.3678237910099,-54.8223730605885,
-228.488444249231));
#189675=CARTESIAN_POINT('Ctrl Pts',(-47.2343490658922,-54.9709330687352,
-228.488381729218));
#189676=CARTESIAN_POINT('Origin',(-53.1417095267163,-62.031487089538,-218.85005));
#189677=CARTESIAN_POINT('',(-54.6082148364463,-63.3913996516292,-218.35005));
#189678=CARTESIAN_POINT('',(-54.2415885090138,-63.0514215111064,-218.85005));
#189679=CARTESIAN_POINT('Origin',(-54.6082148364463,-63.3913996516292,-218.85005));
#189680=CARTESIAN_POINT('Origin',(-53.1417095267163,-62.031487089538,-218.35005));
#189681=CARTESIAN_POINT('Origin',(-53.1417095267163,-62.031487089538,-218.85005));
#189682=CARTESIAN_POINT('Ctrl Pts',(-47.4910910659474,-55.2017568268662,
-228.35005));
#189683=CARTESIAN_POINT('Ctrl Pts',(-47.3421114593162,-55.0678167910323,
-228.35005));
#189684=CARTESIAN_POINT('Ctrl Pts',(-47.2343490658922,-54.9709330687353,
-228.488381729218));
#189685=CARTESIAN_POINT('Ctrl Pts',(-46.5610878289829,-56.2361862677858,
-228.35005));
#189686=CARTESIAN_POINT('Ctrl Pts',(-46.4160092042075,-56.0984512122452,
-228.350050000212));
#189687=CARTESIAN_POINT('Ctrl Pts',(-46.3105395613661,-55.9991515869664,
-228.487948838892));
#189688=CARTESIAN_POINT('Ctrl Pts',(-45.5947854895852,-57.2325158021754,
-228.35005));
#189689=CARTESIAN_POINT('Ctrl Pts',(-45.4531166269507,-57.091545569762,
-228.350050000038));
#189690=CARTESIAN_POINT('Ctrl Pts',(-45.350506384691,-56.9893433179289,
-228.48772415168));
#189691=CARTESIAN_POINT('Ctrl Pts',(-43.5860475125547,-59.145141081541,
-228.35005));
#189692=CARTESIAN_POINT('Ctrl Pts',(-43.4520711334389,-58.9967304277239,
-228.350049999962));
#189693=CARTESIAN_POINT('Ctrl Pts',(-43.3550620161755,-58.8891661040005,
-228.487824007409));
#189694=CARTESIAN_POINT('Ctrl Pts',(-42.5429028274419,-60.0607223439083,
-228.35005));
#189695=CARTESIAN_POINT('Ctrl Pts',(-42.4124726432155,-59.9088386926303,
-228.35005000027));
#189696=CARTESIAN_POINT('Ctrl Pts',(-42.3185849747264,-59.7984761650306,
-228.488134585451));
#189697=CARTESIAN_POINT('Ctrl Pts',(-41.4636310035132,-60.9383233439605,
-228.35005));
#189698=CARTESIAN_POINT('Ctrl Pts',(-41.3371131727634,-60.7827319875555,
-228.35005));
#189699=CARTESIAN_POINT('Ctrl Pts',(-41.2456587371609,-60.6702615191614,
-228.488620962447));
#189700=CARTESIAN_POINT('',(-41.4636310035131,-60.9383233439604,-228.35005));
#189701=CARTESIAN_POINT('',(-41.2456587371609,-60.6702615191614,-228.488620962447));
#189702=CARTESIAN_POINT('Origin',(-41.4636310035131,-60.9383233439605,-228.85005));
#189703=CARTESIAN_POINT('Ctrl Pts',(-41.4636310035131,-60.9383233439604,
-228.35005));
#189704=CARTESIAN_POINT('Ctrl Pts',(-42.5429085052274,-60.0607177270638,
-228.35005));
#189705=CARTESIAN_POINT('Ctrl Pts',(-43.5860475125577,-59.1451410815382,
-228.35005));
#189706=CARTESIAN_POINT('Ctrl Pts',(-44.5904165010271,-58.1888284418133,
-228.35005));
#189707=CARTESIAN_POINT('Ctrl Pts',(-45.5947854894966,-57.2325158020884,
-228.35005));
#189708=CARTESIAN_POINT('Ctrl Pts',(-46.5610786115705,-56.2361965201832,
-228.35005));
#189709=CARTESIAN_POINT('Ctrl Pts',(-47.4910910659473,-55.2017568268661,
-228.35005));
#189710=CARTESIAN_POINT('Ctrl Pts',(-47.2343490658922,-54.9709330687352,
-228.488381729218));
#189711=CARTESIAN_POINT('Ctrl Pts',(-46.310539561368,-55.9991515869682,
-228.48794883889));
#189712=CARTESIAN_POINT('Ctrl Pts',(-45.3505063846929,-56.9893433179308,
-228.487724151677));
#189713=CARTESIAN_POINT('Ctrl Pts',(-43.3550620161773,-58.8891661040025,
-228.487824007406));
#189714=CARTESIAN_POINT('Ctrl Pts',(-42.3185849747281,-59.7984761650326,
-228.488134585449));
#189715=CARTESIAN_POINT('Ctrl Pts',(-41.2456587371609,-60.6702615191614,
-228.488620962447));
#189716=CARTESIAN_POINT('Origin',(-0.127542579976414,-12.8706479699377,
-218.85005));
#189717=CARTESIAN_POINT('',(-49.6055526500885,-68.3000311480131,-218.35005));
#189718=CARTESIAN_POINT('',(-49.2725916132775,-67.9270204940557,-218.85005));
#189719=CARTESIAN_POINT('Origin',(-49.6055526500885,-68.3000311480131,-218.85005));
#189720=CARTESIAN_POINT('Origin',(-0.127542579976414,-12.8706479699377,
-218.35005));
#189721=CARTESIAN_POINT('Origin',(-0.127542579976414,-12.8706479699377,
-218.85005));
#189722=CARTESIAN_POINT('Ctrl Pts',(-41.3169485390149,-62.5017525488808,
-227.074161006174));
#189723=CARTESIAN_POINT('Ctrl Pts',(-41.6737883368886,-62.1442676134989,
-227.135099137228));
#189724=CARTESIAN_POINT('Ctrl Pts',(-41.8830720182286,-62.4278907679969,
-227.501554844865));
#189725=CARTESIAN_POINT('Ctrl Pts',(-41.1560049633168,-62.3716221357798,
-227.26702335738));
#189726=CARTESIAN_POINT('Ctrl Pts',(-41.511713989187,-62.0831419564948,
-227.276651470545));
#189727=CARTESIAN_POINT('Ctrl Pts',(-41.7288940022276,-62.291150852776,
-227.617227833887));
#189728=CARTESIAN_POINT('Ctrl Pts',(-41.0290389449415,-62.2181773292494,
-227.457737962392));
#189729=CARTESIAN_POINT('Ctrl Pts',(-41.36324217846,-61.9848792214323,-227.438029208627));
#189730=CARTESIAN_POINT('Ctrl Pts',(-41.5972134010529,-62.1423580722077,
-227.731615003921));
#189731=CARTESIAN_POINT('Ctrl Pts',(-40.8795052413922,-61.9086867290375,
-227.779669319346));
#189732=CARTESIAN_POINT('Ctrl Pts',(-41.1743549655657,-61.7587852725776,
-227.719332117853));
#189733=CARTESIAN_POINT('Ctrl Pts',(-41.4166557380291,-61.8634089393353,
-227.924695300817));
#189734=CARTESIAN_POINT('Ctrl Pts',(-40.83755717967,-61.7643747830512,-227.9134383294));
#189735=CARTESIAN_POINT('Ctrl Pts',(-41.1129123325295,-61.6488546563462,
-227.83820193251));
#189736=CARTESIAN_POINT('Ctrl Pts',(-41.3546304032729,-61.7388485235333,
-228.004924872379));
#189737=CARTESIAN_POINT('Ctrl Pts',(-40.8167874720303,-61.4561982274081,
-228.157939415417));
#189738=CARTESIAN_POINT('Ctrl Pts',(-41.0510076565582,-61.4074592210291,
-228.055814452642));
#189739=CARTESIAN_POINT('Ctrl Pts',(-41.2770779346333,-61.4865010709279,
-228.151579714695));
#189740=CARTESIAN_POINT('Ctrl Pts',(-40.8377574579089,-61.2894729474496,
-228.270955921441));
#189741=CARTESIAN_POINT('Ctrl Pts',(-41.0474958312304,-61.2728289507257,
-228.158745887246));
#189742=CARTESIAN_POINT('Ctrl Pts',(-41.2608207422257,-61.3563705227572,
-228.219373496776));
#189743=CARTESIAN_POINT('Ctrl Pts',(-41.0018595517499,-60.8897708053906,
-228.472378638458));
#189744=CARTESIAN_POINT('Ctrl Pts',(-41.1456365144707,-60.9545865414107,
-228.33766271302));
#189745=CARTESIAN_POINT('Ctrl Pts',(-41.312673756006,-61.0669702905819,
-228.340237378046));
#189746=CARTESIAN_POINT('Ctrl Pts',(-41.1915219835726,-60.6688302795396,
-228.523150593266));
#189747=CARTESIAN_POINT('Ctrl Pts',(-41.2921564536673,-60.7745584980989,
-228.383687823478));
#189748=CARTESIAN_POINT('Ctrl Pts',(-41.4201823771292,-60.9267119894641,
-228.37074419579));
#189749=CARTESIAN_POINT('Ctrl Pts',(-41.4493760765003,-60.5376437416951,
-228.463541011148));
#189750=CARTESIAN_POINT('Ctrl Pts',(-41.5006225893106,-60.6869549447557,
-228.322209460736));
#189751=CARTESIAN_POINT('Ctrl Pts',(-41.6002487944716,-60.8719910741376,
-228.335067908123));
#189752=CARTESIAN_POINT('',(-41.7563078823353,-62.3074742642099,-227.60005));
#189753=CARTESIAN_POINT('',(-41.1874522920715,-62.3844144545142,-227.238927571877));
#189754=CARTESIAN_POINT('Origin',(-41.3994163116703,-62.6576576544332,-227.60005));
#189755=CARTESIAN_POINT('Ctrl Pts',(-41.7563078823353,-62.3074742642099,
-227.60005));
#189756=CARTESIAN_POINT('Ctrl Pts',(-41.7235734346169,-62.2741127491088,
-227.626724054627));
#189757=CARTESIAN_POINT('Ctrl Pts',(-41.6921357158834,-62.2400471989624,
-227.653311433456));
#189758=CARTESIAN_POINT('Ctrl Pts',(-41.6620056207862,-62.2052910952259,
-227.67982091917));
#189759=CARTESIAN_POINT('Ctrl Pts',(-41.6307102746536,-62.1691908342363,
-227.707355632504));
#189760=CARTESIAN_POINT('Ctrl Pts',(-41.6008254854847,-62.1323457352978,
-227.73480764522));
#189761=CARTESIAN_POINT('Ctrl Pts',(-41.5724052856148,-62.0947298672639,
-227.762174519856));
#189762=CARTESIAN_POINT('Ctrl Pts',(-41.5459110186549,-62.0596630889099,
-227.787686841577));
#189763=CARTESIAN_POINT('Ctrl Pts',(-41.5206901179788,-62.0239259257339,
-227.81312595281));
#189764=CARTESIAN_POINT('Ctrl Pts',(-41.4968179503685,-61.9874663713984,
-227.838464695241));
#189765=CARTESIAN_POINT('Ctrl Pts',(-41.4950826242579,-61.9848160374341,
-227.840306630254));
#189766=CARTESIAN_POINT('Ctrl Pts',(-41.4933544377594,-61.9821618738057,
-227.842148020231));
#189767=CARTESIAN_POINT('Ctrl Pts',(-41.4916334256868,-61.9795038547827,
-227.843988847451));
#189768=CARTESIAN_POINT('Ctrl Pts',(-41.4653523060016,-61.9389139500517,
-227.872099632527));
#189769=CARTESIAN_POINT('Ctrl Pts',(-41.4406731366018,-61.8973165619484,
-227.900153206132));
#189770=CARTESIAN_POINT('Ctrl Pts',(-41.4180385765043,-61.8549835530777,
-227.927912489062));
#189771=CARTESIAN_POINT('Ctrl Pts',(-41.3964658547037,-61.8146364811921,
-227.954369521382));
#189772=CARTESIAN_POINT('Ctrl Pts',(-41.3767507922726,-61.7736208112622,
-227.980559137109));
#189773=CARTESIAN_POINT('Ctrl Pts',(-41.359264822195,-61.7321834942838,
-228.006233157985));
#189774=CARTESIAN_POINT('Ctrl Pts',(-41.3425707322791,-61.6926227325739,
-228.030744489705));
#189775=CARTESIAN_POINT('Ctrl Pts',(-41.3279087531751,-61.652677312538,
-228.05478569363));
#189776=CARTESIAN_POINT('Ctrl Pts',(-41.3155859261546,-61.6125780064951,
-228.078102621503));
#189777=CARTESIAN_POINT('Ctrl Pts',(-41.3044314784935,-61.5762806852913,
-228.099208772807));
#189778=CARTESIAN_POINT('Ctrl Pts',(-41.2951200838481,-61.5396758565221,
-228.119813195706));
#189779=CARTESIAN_POINT('Ctrl Pts',(-41.2880440076531,-61.5030587469111,
-228.13969080728));
#189780=CARTESIAN_POINT('Ctrl Pts',(-41.2811808243614,-61.4675433103978,
-228.158970375204));
#189781=CARTESIAN_POINT('Ctrl Pts',(-41.2764209319513,-61.4320158754815,
-228.177566170525));
#189782=CARTESIAN_POINT('Ctrl Pts',(-41.2741059440455,-61.3967618102316,
-228.195230844135));
#189783=CARTESIAN_POINT('Ctrl Pts',(-41.2718932011152,-61.3630647945998,
-228.212115330464));
#189784=CARTESIAN_POINT('Ctrl Pts',(-41.2719145388887,-61.3296171684738,
-228.228148884212));
#189785=CARTESIAN_POINT('Ctrl Pts',(-41.2744473106528,-61.2966887064693,
-228.243078764507));
#189786=CARTESIAN_POINT('Ctrl Pts',(-41.2760291667021,-61.2761230607388,
-228.252403300493));
#189787=CARTESIAN_POINT('Ctrl Pts',(-41.2785902266755,-61.2557603463957,
-228.261296602549));
#189788=CARTESIAN_POINT('Ctrl Pts',(-41.2821925706481,-61.2356716714283,
-228.269690042848));
#189789=CARTESIAN_POINT('Ctrl Pts',(-41.2875991018068,-61.2055218445455,
-228.282287228693));
#189790=CARTESIAN_POINT('Ctrl Pts',(-41.2954370433597,-61.1763140509013,
-228.293669306206));
#189791=CARTESIAN_POINT('Ctrl Pts',(-41.3057207923416,-61.1483324005503,
-228.303616281046));
#189792=CARTESIAN_POINT('Ctrl Pts',(-41.3155679856567,-61.1215385998879,
-228.313140996627));
#189793=CARTESIAN_POINT('Ctrl Pts',(-41.3276572099933,-61.0958695700185,
-228.321349528454));
#189794=CARTESIAN_POINT('Ctrl Pts',(-41.3419742882173,-61.0716010662815,
-228.328085190812));
#189795=CARTESIAN_POINT('Ctrl Pts',(-41.3562413419726,-61.0474173577093,
-228.334797318485));
#189796=CARTESIAN_POINT('Ctrl Pts',(-41.372720286929,-61.0246248189081,
-228.340046421585));
#189797=CARTESIAN_POINT('Ctrl Pts',(-41.3913766316035,-61.0035164026252,
-228.343720453028));
#189798=CARTESIAN_POINT('Ctrl Pts',(-41.4099793999867,-60.9824686043616,
-228.347383933585));
#189799=CARTESIAN_POINT('Ctrl Pts',(-41.430746593826,-60.9630957469574,
-228.349481090787));
#189800=CARTESIAN_POINT('Ctrl Pts',(-41.4536304454056,-60.9457015839643,
-228.349949039638));
#189801=CARTESIAN_POINT('Ctrl Pts',(-41.4569202857835,-60.9432009551014,
-228.350016313148));
#189802=CARTESIAN_POINT('Ctrl Pts',(-41.4602538570071,-60.9407412364663,
-228.35005));
#189803=CARTESIAN_POINT('Ctrl Pts',(-41.4636310035131,-60.9383233439604,
-228.35005));
#189804=CARTESIAN_POINT('Ctrl Pts',(-41.2456587371609,-60.6702615191614,
-228.488620962447));
#189805=CARTESIAN_POINT('Ctrl Pts',(-41.0908117131772,-60.7960794826395,
-228.488691139081));
#189806=CARTESIAN_POINT('Ctrl Pts',(-40.9745092027764,-60.9563878290671,
-228.438808185622));
#189807=CARTESIAN_POINT('Ctrl Pts',(-40.8377574579089,-61.2894729474496,
-228.270955921441));
#189808=CARTESIAN_POINT('Ctrl Pts',(-40.8167874720303,-61.4561982274081,
-228.157939415417));
#189809=CARTESIAN_POINT('Ctrl Pts',(-40.83755717967,-61.7643747830512,-227.9134383294));
#189810=CARTESIAN_POINT('Ctrl Pts',(-40.8795052413922,-61.9086867290375,
-227.779669319346));
#189811=CARTESIAN_POINT('Ctrl Pts',(-41.0041166610166,-62.1665955625474,
-227.511393188551));
#189812=CARTESIAN_POINT('Ctrl Pts',(-41.0866968731953,-62.2817278482174,
-227.375764657105));
#189813=CARTESIAN_POINT('Ctrl Pts',(-41.1874522920715,-62.3844144545142,
-227.238927571877));
#189814=CARTESIAN_POINT('Origin',(-48.2737085028446,-66.8079885321834,-218.85005));
#189815=CARTESIAN_POINT('',(-49.0417551583074,-68.6546353135231,-218.35005));
#189816=CARTESIAN_POINT('',(-48.8497434944417,-68.1929736181882,-218.85005));
#189817=CARTESIAN_POINT('Origin',(-49.0417551583074,-68.6546353135231,-218.85005));
#189818=CARTESIAN_POINT('Origin',(-48.2737085028446,-66.8079885321834,-218.35005));
#189819=CARTESIAN_POINT('Origin',(-48.2737085028446,-66.8079885321834,-218.85005));
#189820=CARTESIAN_POINT('Ctrl Pts',(-41.7563078823354,-62.3074742642099,
-227.60005));
#189821=CARTESIAN_POINT('Ctrl Pts',(-41.533590072875,-62.0804900295131,
-227.265723268608));
#189822=CARTESIAN_POINT('Ctrl Pts',(-41.1874522920715,-62.3844144545142,
-227.238927571877));
#189823=CARTESIAN_POINT('Ctrl Pts',(-43.5663090949841,-64.1521482085568,
-225.141881592783));
#189824=CARTESIAN_POINT('Ctrl Pts',(-43.3439332486946,-63.9255124877361,
-224.807072796208));
#189825=CARTESIAN_POINT('Ctrl Pts',(-42.9977586927641,-64.2294190860942,
-224.780329817623));
#189826=CARTESIAN_POINT('Ctrl Pts',(-45.3784193710744,-65.9989716179707,
-222.686835360681));
#189827=CARTESIAN_POINT('Ctrl Pts',(-45.1633560000594,-65.7797884513162,
-222.341036594742));
#189828=CARTESIAN_POINT('Ctrl Pts',(-44.8096404055398,-66.0773673148437,
-222.324535970207));
#189829=CARTESIAN_POINT('Ctrl Pts',(-47.2030337908495,-67.8585387028531,
-220.250747695207));
#189830=CARTESIAN_POINT('Ctrl Pts',(-46.9799636370447,-67.6311953742356,
-219.91012892279));
#189831=CARTESIAN_POINT('Ctrl Pts',(-46.6323854374629,-67.9411854921914,
-219.886423382228));
#189832=CARTESIAN_POINT('',(-47.2030337908494,-67.858538702853,-220.250747695207));
#189833=CARTESIAN_POINT('',(-46.6323854374629,-67.9411854921913,-219.886423382228));
#189834=CARTESIAN_POINT('Origin',(-46.8461422201844,-68.2087220930763,-220.250747695207));
#189835=CARTESIAN_POINT('Ctrl Pts',(-47.2030337908494,-67.858538702853,
-220.250747695207));
#189836=CARTESIAN_POINT('Ctrl Pts',(-45.378411470404,-65.9989635659536,
-222.68684590906));
#189837=CARTESIAN_POINT('Ctrl Pts',(-43.5663164045416,-64.1521556581376,
-225.14187166565));
#189838=CARTESIAN_POINT('Ctrl Pts',(-41.7563078823354,-62.3074742642099,
-227.60005));
#189839=CARTESIAN_POINT('Ctrl Pts',(-41.1874522920715,-62.3844144545142,
-227.238927571877));
#189840=CARTESIAN_POINT('Ctrl Pts',(-42.9977586927641,-64.2294190860942,
-224.780329817623));
#189841=CARTESIAN_POINT('Ctrl Pts',(-44.8096404055398,-66.0773673148437,
-222.324535970207));
#189842=CARTESIAN_POINT('Ctrl Pts',(-46.6323854374629,-67.9411854921913,
-219.886423382228));
#189843=CARTESIAN_POINT('Ctrl Pts',(-49.0417551583074,-68.6546353135231,
-218.35005));
#189844=CARTESIAN_POINT('Ctrl Pts',(-48.8497434944417,-68.1929736181882,
-218.35005));
#189845=CARTESIAN_POINT('Ctrl Pts',(-48.8497434944417,-68.1929736181882,
-218.85005));
#189846=CARTESIAN_POINT('Ctrl Pts',(-48.8914370751605,-68.6805168842225,
-218.35005));
#189847=CARTESIAN_POINT('Ctrl Pts',(-48.7557592223196,-68.232063046543,
-218.382837715704));
#189848=CARTESIAN_POINT('Ctrl Pts',(-48.7287312757308,-68.2433043207298,
-218.85004996112));
#189849=CARTESIAN_POINT('Ctrl Pts',(-48.7342750095003,-68.6918682705249,
-218.342169793108));
#189850=CARTESIAN_POINT('Ctrl Pts',(-48.6402644556944,-68.2689304282727,
-218.402170544444));
#189851=CARTESIAN_POINT('Ctrl Pts',(-48.6040131804169,-68.2768832027127,
-218.836912439222));
#189852=CARTESIAN_POINT('Ctrl Pts',(-48.5701931618903,-68.6892604152372,
-218.333619302448));
#189853=CARTESIAN_POINT('Ctrl Pts',(-48.5093251395215,-68.2897551158004,
-218.412348259396));
#189854=CARTESIAN_POINT('Ctrl Pts',(-48.4757604447939,-68.2943179077776,
-218.82266550408));
#189855=CARTESIAN_POINT('',(-48.5701931618903,-68.6892604152372,-218.333619302448));
#189856=CARTESIAN_POINT('',(-48.4757604447939,-68.2943179077777,-218.82266550408));
#189857=CARTESIAN_POINT('Origin',(-48.5431110921104,-68.7897610329756,-218.82266550408));
#189858=CARTESIAN_POINT('Ctrl Pts',(-48.5701931618903,-68.6892604152372,
-218.333619302448));
#189859=CARTESIAN_POINT('Ctrl Pts',(-48.7342750095003,-68.6918682705249,
-218.342169793108));
#189860=CARTESIAN_POINT('Ctrl Pts',(-48.8914370751605,-68.6805168842225,
-218.35005));
#189861=CARTESIAN_POINT('Ctrl Pts',(-49.0417551583074,-68.6546353135231,
-218.35005));
#189862=CARTESIAN_POINT('Ctrl Pts',(-48.8497434944417,-68.1929736181882,
-218.85005));
#189863=CARTESIAN_POINT('Ctrl Pts',(-48.7287312757308,-68.2433043207298,
-218.85004996112));
#189864=CARTESIAN_POINT('Ctrl Pts',(-48.6040131804169,-68.2768832027127,
-218.836912439222));
#189865=CARTESIAN_POINT('Ctrl Pts',(-48.4757604447939,-68.2943179077777,
-218.82266550408));
#189866=CARTESIAN_POINT('Ctrl Pts',(-48.3245605310988,-68.5271120961852,
-218.457629631481));
#189867=CARTESIAN_POINT('Ctrl Pts',(-48.3620966736425,-68.3097367575389,
-218.591561281049));
#189868=CARTESIAN_POINT('Ctrl Pts',(-48.4757880438389,-68.2943141599182,
-218.822721620273));
#189869=CARTESIAN_POINT('Ctrl Pts',(-47.9776226084146,-68.5733796207044,
-218.632054575151));
#189870=CARTESIAN_POINT('Ctrl Pts',(-48.0565913810317,-68.3304993120465,
-218.760316454659));
#189871=CARTESIAN_POINT('Ctrl Pts',(-48.2145407189483,-68.3298331219756,
-218.997206525336));
#189872=CARTESIAN_POINT('Ctrl Pts',(-47.649067081485,-68.5245197011584,
-218.86174158345));
#189873=CARTESIAN_POINT('Ctrl Pts',(-47.775376539589,-68.2571434268353,
-218.980794630082));
#189874=CARTESIAN_POINT('Ctrl Pts',(-47.9672967132033,-68.2939483901744,
-219.226826228492));
#189875=CARTESIAN_POINT('Ctrl Pts',(-47.0472977798015,-68.2996159355387,
-219.380401121619));
#189876=CARTESIAN_POINT('Ctrl Pts',(-47.2783353223672,-67.9981939744083,
-219.464723226566));
#189877=CARTESIAN_POINT('Ctrl Pts',(-47.5147244105,-68.1266034179018,-219.745199430154));
#189878=CARTESIAN_POINT('Ctrl Pts',(-46.777719874766,-68.1088664499766,
-219.677867280655));
#189879=CARTESIAN_POINT('Ctrl Pts',(-47.0707096179741,-67.7884048023075,
-219.740938168961));
#189880=CARTESIAN_POINT('Ctrl Pts',(-47.3121561538429,-67.9841014827788,
-220.042431566437));
#189881=CARTESIAN_POINT('Ctrl Pts',(-46.5633692293693,-67.867058771901,
-219.981377366936));
#189882=CARTESIAN_POINT('Ctrl Pts',(-46.9321463856559,-67.5557234715507,
-219.993833370428));
#189883=CARTESIAN_POINT('Ctrl Pts',(-47.1512692652038,-67.8031102433352,
-220.345690853212));
#189884=CARTESIAN_POINT('',(-48.3245605310987,-68.5271120961857,-218.45762963148));
#189885=CARTESIAN_POINT('Origin',(-48.5431110921103,-68.7897610329758,-218.82266550408));
#189886=CARTESIAN_POINT('',(-48.2737085028434,-68.3079885321834,-218.970433100048));
#189887=CARTESIAN_POINT('Origin',(-48.3025662442039,-65.8964824566508,-221.193464878497));
#189888=CARTESIAN_POINT('Ctrl Pts',(-48.2737085028434,-68.3079885321834,
-218.970433100048));
#189889=CARTESIAN_POINT('Ctrl Pts',(-48.2200078753576,-68.3079885321833,
-219.013078180332));
#189890=CARTESIAN_POINT('Ctrl Pts',(-48.1671265874068,-68.3051041946007,
-219.057745077571));
#189891=CARTESIAN_POINT('Ctrl Pts',(-48.1153121427422,-68.2996019516411,
-219.104050254264));
#189892=CARTESIAN_POINT('Ctrl Pts',(-48.0624290103477,-68.2939862233479,
-219.15131048846));
#189893=CARTESIAN_POINT('Ctrl Pts',(-48.0106569899895,-68.2856439945604,
-219.200277279003));
#189894=CARTESIAN_POINT('Ctrl Pts',(-47.9602041194346,-68.274861056155,
-219.250542863839));
#189895=CARTESIAN_POINT('Ctrl Pts',(-47.9081697144589,-68.2637401074826,
-219.302384112294));
#189896=CARTESIAN_POINT('Ctrl Pts',(-47.857538280142,-68.2500235216982,
-219.355606857271));
#189897=CARTESIAN_POINT('Ctrl Pts',(-47.8084827582267,-68.2340197403078,
-219.409763776065));
#189898=CARTESIAN_POINT('Ctrl Pts',(-47.7899076849436,-68.2279598432661,
-219.430270514066));
#189899=CARTESIAN_POINT('Ctrl Pts',(-47.7715580265398,-68.2215719219543,
-219.450911192888));
#189900=CARTESIAN_POINT('Ctrl Pts',(-47.7534412888826,-68.2148723319608,
-219.471661526933));
#189901=CARTESIAN_POINT('Ctrl Pts',(-47.7036959697479,-68.1964764569085,
-219.528638230396));
#189902=CARTESIAN_POINT('Ctrl Pts',(-47.6555204296105,-68.1756653808065,
-219.586645968365));
#189903=CARTESIAN_POINT('Ctrl Pts',(-47.6089704551965,-68.1526532963566,
-219.645524393526));
#189904=CARTESIAN_POINT('Ctrl Pts',(-47.5600388327744,-68.1284638388622,
-219.707415230311));
#189905=CARTESIAN_POINT('Ctrl Pts',(-47.5129023330372,-68.1018424910022,
-219.770268127841));
#189906=CARTESIAN_POINT('Ctrl Pts',(-47.4676123806305,-68.0729822245595,
-219.833896846445));
#189907=CARTESIAN_POINT('Ctrl Pts',(-47.4192068535602,-68.0421366101503,
-219.901902695363));
#189908=CARTESIAN_POINT('Ctrl Pts',(-47.3729092787754,-68.008733452613,
-219.97079477694));
#189909=CARTESIAN_POINT('Ctrl Pts',(-47.3287869283299,-67.9729448481097,
-220.040345711594));
#189910=CARTESIAN_POINT('Ctrl Pts',(-47.2846645778844,-67.9371562436065,
-220.109896646248));
#189911=CARTESIAN_POINT('Ctrl Pts',(-47.242716187926,-67.8989812635678,
-220.18010643398));
#189912=CARTESIAN_POINT('Ctrl Pts',(-47.2030337908494,-67.858538702853,
-220.250747695207));
#189913=CARTESIAN_POINT('Ctrl Pts',(-46.6323854374629,-67.9411854921913,
-219.886423382228));
#189914=CARTESIAN_POINT('Ctrl Pts',(-46.8345979831289,-68.1479546277646,
-219.615942902677));
#189915=CARTESIAN_POINT('Ctrl Pts',(-47.0804817541895,-68.3120180317859,
-219.351800153137));
#189916=CARTESIAN_POINT('Ctrl Pts',(-47.649067081485,-68.5245197011584,
-218.86174158345));
#189917=CARTESIAN_POINT('Ctrl Pts',(-47.9776226084146,-68.5733796207044,
-218.632054575151));
#189918=CARTESIAN_POINT('Ctrl Pts',(-48.3245605310987,-68.5271120961857,
-218.45762963148));
#189919=CARTESIAN_POINT('Origin',(-48.5431110921103,-68.7897610329758,-218.82266550408));
#189920=CARTESIAN_POINT('Origin',(-48.5431110921103,-68.7897610329758,-218.82266550408));
#189921=CARTESIAN_POINT('Ctrl Pts',(-49.9821530185534,29.7903768266301,
-227.087737588405));
#189922=CARTESIAN_POINT('Ctrl Pts',(-49.6198764783311,30.1429190036325,
-227.149984230661));
#189923=CARTESIAN_POINT('Ctrl Pts',(-49.9128620056376,30.3690936660469,
-227.499383229701));
#189924=CARTESIAN_POINT('Ctrl Pts',(-49.8651657433229,29.6382362842524,
-227.284518486594));
#189925=CARTESIAN_POINT('Ctrl Pts',(-49.5705461543588,29.9918313989471,
-227.291056067445));
#189926=CARTESIAN_POINT('Ctrl Pts',(-49.7889944489624,30.2238041797745,
-227.61742149242));
#189927=CARTESIAN_POINT('Ctrl Pts',(-49.7229062924001,29.5201055635575,
-227.47950311892));
#189928=CARTESIAN_POINT('Ctrl Pts',(-49.4843813968511,29.8539883550855,
-227.45309706292));
#189929=CARTESIAN_POINT('Ctrl Pts',(-49.6516188678455,30.100801435488,-227.73438694973));
#189930=CARTESIAN_POINT('Ctrl Pts',(-49.4273244905926,29.3876439546323,
-227.809457307428));
#189931=CARTESIAN_POINT('Ctrl Pts',(-49.274698524826,29.6835679295866,-227.737356551705));
#189932=CARTESIAN_POINT('Ctrl Pts',(-49.3886234115437,29.9359477677008,
-227.932297012233));
#189933=CARTESIAN_POINT('Ctrl Pts',(-49.2917843161281,29.3546860495185,
-227.942284411928));
#189934=CARTESIAN_POINT('Ctrl Pts',(-49.1736791703851,29.6317476033538,
-227.854117706657));
#189935=CARTESIAN_POINT('Ctrl Pts',(-49.2735381356863,29.8826576832388,
-228.011965974601));
#189936=CARTESIAN_POINT('Ctrl Pts',(-49.0688864384257,29.3512758295993,
-228.126445026147));
#189937=CARTESIAN_POINT('Ctrl Pts',(-49.0005354215612,29.5971993197923,
-228.017792073831));
#189938=CARTESIAN_POINT('Ctrl Pts',(-49.094353778077,29.8357918748608,-228.122426020868));
#189939=CARTESIAN_POINT('Ctrl Pts',(-48.9919998081944,29.3580678656198,
-228.184587230454));
#189940=CARTESIAN_POINT('Ctrl Pts',(-48.9405355047191,29.5928733395382,
-228.06937023996));
#189941=CARTESIAN_POINT('Ctrl Pts',(-49.034125806983,29.8260226021538,-228.157300396488));
#189942=CARTESIAN_POINT('Ctrl Pts',(-48.8359253199892,29.3900316449823,
-228.290207259017));
#189943=CARTESIAN_POINT('Ctrl Pts',(-48.8180798673065,29.6014212406182,
-228.162864494856));
#189944=CARTESIAN_POINT('Ctrl Pts',(-48.9154714515405,29.8207826964393,
-228.220654439149));
#189945=CARTESIAN_POINT('Ctrl Pts',(-48.7550774165302,29.4157509526954,
-228.33866597543));
#189946=CARTESIAN_POINT('Ctrl Pts',(-48.7540839008066,29.6143499072788,
-228.205991351778));
#189947=CARTESIAN_POINT('Ctrl Pts',(-48.8558242941532,29.8254233230326,
-228.249722296701));
#189948=CARTESIAN_POINT('Ctrl Pts',(-48.4543941551331,29.5520514607806,
-228.490868066449));
#189949=CARTESIAN_POINT('Ctrl Pts',(-48.5190268257732,29.6989473079643,
-228.339039615738));
#189950=CARTESIAN_POINT('Ctrl Pts',(-48.6420470598464,29.8753114465513,
-228.341027466389));
#189951=CARTESIAN_POINT('Ctrl Pts',(-48.2384142358766,29.739665517712,-228.538258948111));
#189952=CARTESIAN_POINT('Ctrl Pts',(-48.3453525961707,29.8434973019672,
-228.381204030932));
#189953=CARTESIAN_POINT('Ctrl Pts',(-48.5063911947406,29.9830169918788,
-228.369471344765));
#189954=CARTESIAN_POINT('Ctrl Pts',(-48.1067814994714,29.9754013777531,
-228.482341346825));
#189955=CARTESIAN_POINT('Ctrl Pts',(-48.2558206399642,30.0319935302987,
-228.324194018));
#189956=CARTESIAN_POINT('Ctrl Pts',(-48.4474782994608,30.1465062177761,
-228.335958788446));
#189957=CARTESIAN_POINT('',(-48.2384287873563,29.7860380279371,-228.505869818703));
#189958=CARTESIAN_POINT('',(-48.515339402069,30.020261242545,-228.35005));
#189959=CARTESIAN_POINT('Origin',(-48.515339402069,30.020261242545,-228.85005));
#189960=CARTESIAN_POINT('',(-49.8755750290351,29.6684593880862,-227.255950349386));
#189961=CARTESIAN_POINT('Ctrl Pts',(-48.2384287873563,29.7860380279371,
-228.505869818703));
#189962=CARTESIAN_POINT('Ctrl Pts',(-48.3622865299896,29.6395743915966,
-228.505892074711));
#189963=CARTESIAN_POINT('Ctrl Pts',(-48.5176958943746,29.5233566169732,
-228.458825520971));
#189964=CARTESIAN_POINT('Ctrl Pts',(-48.7550774165302,29.4157509526954,
-228.33866597543));
#189965=CARTESIAN_POINT('Ctrl Pts',(-48.8359253199892,29.3900316449823,
-228.290207259017));
#189966=CARTESIAN_POINT('Ctrl Pts',(-48.9919998081944,29.3580678656198,
-228.184587230454));
#189967=CARTESIAN_POINT('Ctrl Pts',(-49.0688864384257,29.3512758295993,
-228.126445026147));
#189968=CARTESIAN_POINT('Ctrl Pts',(-49.2917843161281,29.3546860495185,
-227.942284411928));
#189969=CARTESIAN_POINT('Ctrl Pts',(-49.4273244905926,29.3876439546323,
-227.809457307428));
#189970=CARTESIAN_POINT('Ctrl Pts',(-49.6736426587655,29.4980286287366,
-227.534495483671));
#189971=CARTESIAN_POINT('Ctrl Pts',(-49.7814123210161,29.5740686437592,
-227.395733267867));
#189972=CARTESIAN_POINT('Ctrl Pts',(-49.8755750290351,29.6684593880862,
-227.255950349386));
#189973=CARTESIAN_POINT('',(-49.8031531494471,30.2499539750197,-227.60005));
#189974=CARTESIAN_POINT('Origin',(-50.1572979707234,29.8969930061248,-227.60005));
#189975=CARTESIAN_POINT('Ctrl Pts',(-49.8031531494471,30.2499539750196,
-227.60005));
#189976=CARTESIAN_POINT('Ctrl Pts',(-49.7734448823229,30.2201460645754,
-227.626521883971));
#189977=CARTESIAN_POINT('Ctrl Pts',(-49.7429857046469,30.191563965602,-227.652920536918));
#189978=CARTESIAN_POINT('Ctrl Pts',(-49.7117854125283,30.1642213555141,
-227.679257545219));
#189979=CARTESIAN_POINT('Ctrl Pts',(-49.6808651108338,30.137124117135,-227.70535820605));
#189980=CARTESIAN_POINT('Ctrl Pts',(-49.6492168074017,30.1112443498472,
-227.731399362287));
#189981=CARTESIAN_POINT('Ctrl Pts',(-49.6168148938523,30.0866303917786,
-227.757381347539));
#189982=CARTESIAN_POINT('Ctrl Pts',(-49.5852289197423,30.0626362581879,
-227.782709058886));
#189983=CARTESIAN_POINT('Ctrl Pts',(-49.5529265342257,30.0398452627543,
-227.807981431008));
#189984=CARTESIAN_POINT('Ctrl Pts',(-49.5198536003906,30.0183324962131,
-227.833174321558));
#189985=CARTESIAN_POINT('Ctrl Pts',(-49.5126382797592,30.0136391869035,
-227.838670501119));
#189986=CARTESIAN_POINT('Ctrl Pts',(-49.5053861763458,30.0090068233215,
-227.844162774479));
#189987=CARTESIAN_POINT('Ctrl Pts',(-49.4980965508085,30.0044363617929,
-227.849650666463));
#189988=CARTESIAN_POINT('Ctrl Pts',(-49.4649798247165,29.9836727818563,
-227.874582127582));
#189989=CARTESIAN_POINT('Ctrl Pts',(-49.4313422743447,29.9643338165172,
-227.899219369963));
#189990=CARTESIAN_POINT('Ctrl Pts',(-49.3972404504349,29.9465778326619,
-227.923525661612));
#189991=CARTESIAN_POINT('Ctrl Pts',(-49.3639866371966,29.929263387178,-227.947227528266));
#189992=CARTESIAN_POINT('Ctrl Pts',(-49.3302909420142,29.9134545841207,
-227.970615436086));
#189993=CARTESIAN_POINT('Ctrl Pts',(-49.2961839213851,29.8993200737892,
-227.993617660293));
#189994=CARTESIAN_POINT('Ctrl Pts',(-49.2635064665614,29.8857779990406,
-228.01565576648));
#189995=CARTESIAN_POINT('Ctrl Pts',(-49.2304509638959,29.8737732842517,
-228.0373403047));
#189996=CARTESIAN_POINT('Ctrl Pts',(-49.1970304416516,29.8634680481683,
-228.058564819369));
#189997=CARTESIAN_POINT('Ctrl Pts',(-49.1827533566865,29.8590657013087,
-228.067631829067));
#189998=CARTESIAN_POINT('Ctrl Pts',(-49.1684095214318,29.8549736373304,
-228.076614292399));
#189999=CARTESIAN_POINT('Ctrl Pts',(-49.1539994837212,29.8512049615201,
-228.085501029504));
#190000=CARTESIAN_POINT('Ctrl Pts',(-49.1169547854528,29.8415166136428,
-228.10834666678));
#190001=CARTESIAN_POINT('Ctrl Pts',(-49.0797216134608,29.834075936904,-228.130440543945));
#190002=CARTESIAN_POINT('Ctrl Pts',(-49.0426240763788,29.8292022975051,
-228.151491221325));
#190003=CARTESIAN_POINT('Ctrl Pts',(-49.0199091815933,29.8262181585332,
-228.164380592412));
#190004=CARTESIAN_POINT('Ctrl Pts',(-48.9972457051912,29.8241958719105,
-228.176878325889));
#190005=CARTESIAN_POINT('Ctrl Pts',(-48.9747142044139,29.8232026173048,
-228.188913138851));
#190006=CARTESIAN_POINT('Ctrl Pts',(-48.9493717776647,29.822085448842,-228.202449359493));
#190007=CARTESIAN_POINT('Ctrl Pts',(-48.9239814908925,29.8222824170942,
-228.215521988452));
#190008=CARTESIAN_POINT('Ctrl Pts',(-48.8988128289049,29.8239088085271,
-228.227919221305));
#190009=CARTESIAN_POINT('Ctrl Pts',(-48.8739511938202,29.825515359973,-228.240165223074));
#190010=CARTESIAN_POINT('Ctrl Pts',(-48.849306086085,29.8285163971193,-228.251751617269));
#190011=CARTESIAN_POINT('Ctrl Pts',(-48.8251655012992,29.8329948799433,
-228.262505936811));
#190012=CARTESIAN_POINT('Ctrl Pts',(-48.8165309820697,29.8345967278856,
-228.266352503898));
#190013=CARTESIAN_POINT('Ctrl Pts',(-48.8079612516762,29.8363873459285,
-228.270092960664));
#190014=CARTESIAN_POINT('Ctrl Pts',(-48.799470260208,29.8383697609083,-228.273720624));
#190015=CARTESIAN_POINT('Ctrl Pts',(-48.7738910424793,29.8443418107669,
-228.284649005056));
#190016=CARTESIAN_POINT('Ctrl Pts',(-48.7489150276425,29.8521574393405,
-228.294624127528));
#190017=CARTESIAN_POINT('Ctrl Pts',(-48.7247444939762,29.8617843087228,
-228.3034703766));
#190018=CARTESIAN_POINT('Ctrl Pts',(-48.7007470557507,29.8713422360112,
-228.312253273932));
#190019=CARTESIAN_POINT('Ctrl Pts',(-48.67754399401,29.88268516539,-228.319922927921));
#190020=CARTESIAN_POINT('Ctrl Pts',(-48.6553561292837,29.8957586681485,
-228.326347457397));
#190021=CARTESIAN_POINT('Ctrl Pts',(-48.6332362468861,29.9087921144539,
-228.332752302488));
#190022=CARTESIAN_POINT('Ctrl Pts',(-48.6121258098598,29.9235450873337,
-228.337919283806));
#190023=CARTESIAN_POINT('Ctrl Pts',(-48.5922600597141,29.9399472673055,
-228.341763936109));
#190024=CARTESIAN_POINT('Ctrl Pts',(-48.5724227307226,29.956325981318,-228.345603088017));
#190025=CARTESIAN_POINT('Ctrl Pts',(-48.5538270410762,29.974348677228,-228.348123494146));
#190026=CARTESIAN_POINT('Ctrl Pts',(-48.5367163511529,29.9939362403649,
-228.349291389838));
#190027=CARTESIAN_POINT('Ctrl Pts',(-48.5293054173971,30.0024199504604,
-228.349797225526));
#190028=CARTESIAN_POINT('Ctrl Pts',(-48.5221731256271,30.0111971448433,
-228.35005));
#190029=CARTESIAN_POINT('Ctrl Pts',(-48.515339402069,30.020261242545,-228.35005));
#190030=CARTESIAN_POINT('Ctrl Pts',(-49.7445598344273,30.1911641344867,
-227.687068118445));
#190031=CARTESIAN_POINT('Ctrl Pts',(-49.5079616707949,29.9537724063299,
-227.367376825119));
#190032=CARTESIAN_POINT('Ctrl Pts',(-49.8170070935167,29.6096338345331,
-227.342971407313));
#190033=CARTESIAN_POINT('Ctrl Pts',(-51.3768241225023,31.8289031354474,
-225.262929889291));
#190034=CARTESIAN_POINT('Ctrl Pts',(-51.1414011469561,31.5926905373472,
-224.940062144777));
#190035=CARTESIAN_POINT('Ctrl Pts',(-51.4500767842084,31.2466813577455,
-224.918633333245));
#190036=CARTESIAN_POINT('Ctrl Pts',(-53.0099479863855,33.4675045952855,
-222.839953095868));
#190037=CARTESIAN_POINT('Ctrl Pts',(-52.7769579711113,33.2337331174656,
-222.511152157197));
#190038=CARTESIAN_POINT('Ctrl Pts',(-53.0845220861009,32.8841489423223,
-222.495325263031));
#190039=CARTESIAN_POINT('Ctrl Pts',(-54.6462557747613,35.1093006586908,
-220.421288892634));
#190040=CARTESIAN_POINT('Ctrl Pts',(-54.4073852385165,34.8696289362572,
-220.0969923867));
#190041=CARTESIAN_POINT('Ctrl Pts',(-54.7232341443935,34.5239834253819,
-220.076050819216));
#190042=CARTESIAN_POINT('',(-54.5875190481084,35.0503669255136,-220.508112862707));
#190043=CARTESIAN_POINT('',(-54.6643562096698,34.4651804296884,-220.162900223157));
#190044=CARTESIAN_POINT('Origin',(-54.9416638693848,34.6974059566189,-220.508112862707));
#190045=CARTESIAN_POINT('Ctrl Pts',(-54.5875190481084,35.0503669255136,
-220.508112862707));
#190046=CARTESIAN_POINT('Ctrl Pts',(-52.990443779671,33.4479349702851,-222.86899632084));
#190047=CARTESIAN_POINT('Ctrl Pts',(-51.3963761190905,31.8485207106117,
-225.233951400128));
#190048=CARTESIAN_POINT('Ctrl Pts',(-49.8031531494471,30.2499539750197,
-227.60005));
#190049=CARTESIAN_POINT('Ctrl Pts',(-49.8755750290351,29.6684593880862,
-227.255950349386));
#190050=CARTESIAN_POINT('Ctrl Pts',(-50.3041362735325,30.098058504813,-226.619758552752));
#190051=CARTESIAN_POINT('Ctrl Pts',(-50.7327920588234,30.5277322534597,
-225.983640132402));
#190052=CARTESIAN_POINT('Ctrl Pts',(-51.161601590644,30.9574566332008,-225.347649411111));
#190053=CARTESIAN_POINT('Ctrl Pts',(-51.6179083782284,31.4147369329968,
-224.670876015395));
#190054=CARTESIAN_POINT('Ctrl Pts',(-52.0743881629137,31.8720749432885,
-223.994247221146));
#190055=CARTESIAN_POINT('Ctrl Pts',(-52.5310972104373,32.3295031544124,
-223.317828485869));
#190056=CARTESIAN_POINT('Ctrl Pts',(-53.024051994686,32.8232341771425,-222.587727224425));
#190057=CARTESIAN_POINT('Ctrl Pts',(-53.5172714088493,33.3170716250959,
-221.857870686764));
#190058=CARTESIAN_POINT('Ctrl Pts',(-54.0108369280568,33.8111131722922,
-221.128341184644));
#190059=CARTESIAN_POINT('Ctrl Pts',(-54.2286056520954,34.0290919272257,
-220.806461509823));
#190060=CARTESIAN_POINT('Ctrl Pts',(-54.4464421227249,34.2471109897794,
-220.484645499357));
#190061=CARTESIAN_POINT('Ctrl Pts',(-54.6643562096698,34.4651804296884,
-220.162900223157));
#190062=CARTESIAN_POINT('Ctrl Pts',(-42.6824807550636,35.9538445605081,
-228.35005));
#190063=CARTESIAN_POINT('Ctrl Pts',(-42.5405392130025,35.7913421132894,
-228.35005));
#190064=CARTESIAN_POINT('Ctrl Pts',(-42.4431629103415,35.679860391633,-228.507034483728));
#190065=CARTESIAN_POINT('Ctrl Pts',(-43.7299304472252,35.0389252651105,
-228.35005));
#190066=CARTESIAN_POINT('Ctrl Pts',(-43.5839578161182,34.8805832623425,
-228.350049999846));
#190067=CARTESIAN_POINT('Ctrl Pts',(-43.4842614434386,34.7712285271383,
-228.506443516651));
#190068=CARTESIAN_POINT('Ctrl Pts',(-44.7400658047431,34.0873590008399,
-228.35005));
#190069=CARTESIAN_POINT('Ctrl Pts',(-44.590423195572,33.9329609873047,-228.350049999904));
#190070=CARTESIAN_POINT('Ctrl Pts',(-44.4876418177359,33.826550002353,-228.506035020985));
#190071=CARTESIAN_POINT('Ctrl Pts',(-46.6832166107726,32.108381759188,-228.35005));
#190072=CARTESIAN_POINT('Ctrl Pts',(-46.5261142282933,31.9620046547715,
-228.350050000096));
#190073=CARTESIAN_POINT('Ctrl Pts',(-46.4180861418825,31.8610058543969,
-228.505671567324));
#190074=CARTESIAN_POINT('Ctrl Pts',(-47.617275666974,31.0819979338032,-228.35005));
#190075=CARTESIAN_POINT('Ctrl Pts',(-47.4568224915956,30.9392657163356,
-228.350050000173));
#190076=CARTESIAN_POINT('Ctrl Pts',(-47.3461759565219,30.8411406013281,
-228.505709331207));
#190077=CARTESIAN_POINT('Ctrl Pts',(-48.515339402069,30.020261242545,-228.35005));
#190078=CARTESIAN_POINT('Ctrl Pts',(-48.3513278433713,29.8815330303712,
-228.35005));
#190079=CARTESIAN_POINT('Ctrl Pts',(-48.2384287873563,29.7860380279371,
-228.505869818703));
#190080=CARTESIAN_POINT('',(-42.4431629103415,35.679860391633,-228.507034483728));
#190081=CARTESIAN_POINT('',(-42.6824807550636,35.9538445605081,-228.35005));
#190082=CARTESIAN_POINT('Origin',(-42.6824807550636,35.9538445605081,-228.85005));
#190083=CARTESIAN_POINT('Ctrl Pts',(-42.4431629103415,35.679860391633,-228.507034483728));
#190084=CARTESIAN_POINT('Ctrl Pts',(-42.7614810097597,35.402044258979,-228.506853794282));
#190085=CARTESIAN_POINT('Ctrl Pts',(-43.076290124364,35.1208529422878,-228.506690163061));
#190086=CARTESIAN_POINT('Ctrl Pts',(-43.3875670018904,34.8362478331756,
-228.50654485622));
#190087=CARTESIAN_POINT('Ctrl Pts',(-43.7001585717382,34.5504406811923,
-228.506398935668));
#190088=CARTESIAN_POINT('Ctrl Pts',(-44.0091888390155,34.2611903638572,
-228.506271494611));
#190089=CARTESIAN_POINT('Ctrl Pts',(-44.3146116172886,33.9684109762988,
-228.506163815315));
#190090=CARTESIAN_POINT('Ctrl Pts',(-44.4471552006037,33.8413542146283,
-228.506117085992));
#190091=CARTESIAN_POINT('Ctrl Pts',(-44.579019031032,33.7136322786005,-228.506074078358));
#190092=CARTESIAN_POINT('Ctrl Pts',(-44.7101974035188,33.5852357646224,
-228.506034897212));
#190093=CARTESIAN_POINT('Ctrl Pts',(-44.9602123734819,33.3405227835339,
-228.505960221236));
#190094=CARTESIAN_POINT('Ctrl Pts',(-45.2077386206811,33.0933602183811,
-228.505899445037));
#190095=CARTESIAN_POINT('Ctrl Pts',(-45.4528639798092,32.843777928375,-228.505853294154));
#190096=CARTESIAN_POINT('Ctrl Pts',(-45.7541910954216,32.5369720074249,
-228.505796561907));
#190097=CARTESIAN_POINT('Ctrl Pts',(-46.0518578739747,32.22654482337,-228.505761221002));
#190098=CARTESIAN_POINT('Ctrl Pts',(-46.3459620452366,31.9125632804965,
-228.505744327283));
#190099=CARTESIAN_POINT('Ctrl Pts',(-46.6359601710032,31.6029652949666,
-228.505727669421));
#190100=CARTESIAN_POINT('Ctrl Pts',(-46.9224947730646,31.2899106893207,
-228.505728947252));
#190101=CARTESIAN_POINT('Ctrl Pts',(-47.205610866628,30.9734514217353,-228.50574533822));
#190102=CARTESIAN_POINT('Ctrl Pts',(-47.4798027284841,30.6669674112761,
-228.505761212521));
#190103=CARTESIAN_POINT('Ctrl Pts',(-47.7507883244766,30.3572892892455,
-228.5057912622));
#190104=CARTESIAN_POINT('Ctrl Pts',(-48.0185596969337,30.0444638109572,
-228.505832923288));
#190105=CARTESIAN_POINT('Ctrl Pts',(-48.0920923646595,29.9585588400857,
-228.505844363835));
#190106=CARTESIAN_POINT('Ctrl Pts',(-48.165382347877,29.8724165560943,-228.505856680005));
#190107=CARTESIAN_POINT('Ctrl Pts',(-48.2384287873562,29.786038027937,-228.505869818702));
#190108=CARTESIAN_POINT('Ctrl Pts',(-48.515339402069,30.020261242545,-228.35005));
#190109=CARTESIAN_POINT('Ctrl Pts',(-47.6172684110892,31.0820065120798,
-228.35005));
#190110=CARTESIAN_POINT('Ctrl Pts',(-46.6832166107701,32.1083817591879,
-228.35005));
#190111=CARTESIAN_POINT('Ctrl Pts',(-45.7116412077571,33.0978703800133,
-228.35005));
#190112=CARTESIAN_POINT('Ctrl Pts',(-44.7400658047442,34.0873590008387,
-228.35005));
#190113=CARTESIAN_POINT('Ctrl Pts',(-43.7299213057923,35.0389332497409,
-228.35005));
#190114=CARTESIAN_POINT('Ctrl Pts',(-42.6824807550636,35.9538445605081,
-228.35005));
#190115=CARTESIAN_POINT('Ctrl Pts',(-55.2146353748417,36.257836765148,-218.504776656654));
#190116=CARTESIAN_POINT('Ctrl Pts',(-55.018269151756,36.2900558272771,-218.637811171833));
#190117=CARTESIAN_POINT('Ctrl Pts',(-54.9968660030027,36.3988348033229,
-218.849954951747));
#190118=CARTESIAN_POINT('Ctrl Pts',(-55.2870795674723,35.8851781565843,
-218.703954005327));
#190119=CARTESIAN_POINT('Ctrl Pts',(-55.0614326261131,35.9588010119757,
-218.832425369537));
#190120=CARTESIAN_POINT('Ctrl Pts',(-55.0521021372359,36.1181036739044,
-219.049315831024));
#190121=CARTESIAN_POINT('Ctrl Pts',(-55.2466620625291,35.5359310914311,
-218.973388048176));
#190122=CARTESIAN_POINT('Ctrl Pts',(-54.9920018853069,35.6566773356509,
-219.093930954104));
#190123=CARTESIAN_POINT('Ctrl Pts',(-55.0225064544177,35.8553343499258,
-219.318743015259));
#190124=CARTESIAN_POINT('Ctrl Pts',(-55.0420621792248,34.9357811050992,
-219.543206859613));
#190125=CARTESIAN_POINT('Ctrl Pts',(-54.7478058041436,35.1574653296577,
-219.62907206067));
#190126=CARTESIAN_POINT('Ctrl Pts',(-54.8701701172644,35.4039199531623,
-219.888552047862));
#190127=CARTESIAN_POINT('Ctrl Pts',(-54.8753705653332,34.6763452196008,
-219.851342245784));
#190128=CARTESIAN_POINT('Ctrl Pts',(-54.5592271140415,34.9538518370352,
-219.918109540735));
#190129=CARTESIAN_POINT('Ctrl Pts',(-54.7455508540625,35.2089287796778,
-220.196631257502));
#190130=CARTESIAN_POINT('Ctrl Pts',(-54.6643562096698,34.4651804296883,
-220.162900223157));
#190131=CARTESIAN_POINT('Ctrl Pts',(-54.3487296401403,34.8107766034666,
-220.183958003048));
#190132=CARTESIAN_POINT('Ctrl Pts',(-54.5875190481085,35.0503669255137,
-220.508112862707));
#190133=CARTESIAN_POINT('',(-54.9968660030035,36.3988348033192,-218.84995495175));
#190134=CARTESIAN_POINT('',(-55.2146353748417,36.257836765148,-218.504776656654));
#190135=CARTESIAN_POINT('Origin',(-55.4874598092474,36.4953631270242,-218.849954951747));
#190136=CARTESIAN_POINT('Ctrl Pts',(-54.9968660030035,36.3988348033192,
-218.84995495175));
#190137=CARTESIAN_POINT('Ctrl Pts',(-55.0521021372359,36.1181036739044,
-219.049315831024));
#190138=CARTESIAN_POINT('Ctrl Pts',(-55.0225064544177,35.8553343499258,
-219.318743015259));
#190139=CARTESIAN_POINT('Ctrl Pts',(-54.8701701172644,35.4039199531623,
-219.888552047862));
#190140=CARTESIAN_POINT('Ctrl Pts',(-54.7455508540625,35.2089287796778,
-220.196631257502));
#190141=CARTESIAN_POINT('Ctrl Pts',(-54.5875190481084,35.0503669255136,
-220.508112862707));
#190142=CARTESIAN_POINT('Ctrl Pts',(-54.6643562096698,34.4651804296884,
-220.162900223157));
#190143=CARTESIAN_POINT('Ctrl Pts',(-54.8753705653332,34.6763452196008,
-219.851342245784));
#190144=CARTESIAN_POINT('Ctrl Pts',(-55.0420621792248,34.9357811050992,
-219.543206859613));
#190145=CARTESIAN_POINT('Ctrl Pts',(-55.2466620625291,35.5359310914311,
-218.973388048176));
#190146=CARTESIAN_POINT('Ctrl Pts',(-55.2870795674723,35.8851781565843,
-218.703954005327));
#190147=CARTESIAN_POINT('Ctrl Pts',(-55.2146353748417,36.257836765148,-218.504776656654));
#190148=CARTESIAN_POINT('Ctrl Pts',(-42.6314390030157,35.5442154791813,
-228.483430065205));
#190149=CARTESIAN_POINT('Ctrl Pts',(-42.6895757642938,35.6923542175536,
-228.324885333136));
#190150=CARTESIAN_POINT('Ctrl Pts',(-42.8067874347039,35.8824975081984,
-228.335962498089));
#190151=CARTESIAN_POINT('Ctrl Pts',(-42.3959770663564,35.6815375109877,
-228.539447094234));
#190152=CARTESIAN_POINT('Ctrl Pts',(-42.5018122545368,35.7869463556559,
-228.38104135445));
#190153=CARTESIAN_POINT('Ctrl Pts',(-42.645165635708,35.9461794675295,-228.36947199979));
#190154=CARTESIAN_POINT('Ctrl Pts',(-42.2127692669972,35.8992424363046,
-228.49209590616));
#190155=CARTESIAN_POINT('Ctrl Pts',(-42.3616279932723,35.9623936460538,
-228.337833952227));
#190156=CARTESIAN_POINT('Ctrl Pts',(-42.5415988206105,36.0845090848309,
-228.341008503893));
#190157=CARTESIAN_POINT('Ctrl Pts',(-42.0435120014734,36.2819711039298,
-228.300199623458));
#190158=CARTESIAN_POINT('Ctrl Pts',(-42.2573880832737,36.263076259625,-228.168110622012));
#190159=CARTESIAN_POINT('Ctrl Pts',(-42.4817768757597,36.3581540306266,
-228.225845771006));
#190160=CARTESIAN_POINT('Ctrl Pts',(-42.0144214928843,36.4424407209236,
-228.190025881898));
#190161=CARTESIAN_POINT('Ctrl Pts',(-42.252716826051,36.390518917248,-228.068439552117));
#190162=CARTESIAN_POINT('Ctrl Pts',(-42.4902323852614,36.4811949763934,
-228.15975250057));
#190163=CARTESIAN_POINT('Ctrl Pts',(-42.0186496945452,36.7395078303233,
-227.945638225626));
#190164=CARTESIAN_POINT('Ctrl Pts',(-42.298164022469,36.6184786186142,-227.853003287225));
#190165=CARTESIAN_POINT('Ctrl Pts',(-42.5524035821008,36.7205098054508,
-228.013154749775));
#190166=CARTESIAN_POINT('Ctrl Pts',(-42.0508817378213,36.875278360935,-227.812856844476));
#190167=CARTESIAN_POINT('Ctrl Pts',(-42.3494090109542,36.7193110047082,
-227.736210930231));
#190168=CARTESIAN_POINT('Ctrl Pts',(-42.6050823582478,36.8359013839835,
-227.933511896208));
#190169=CARTESIAN_POINT('Ctrl Pts',(-42.1814227629516,37.1709308823785,
-227.48240945426));
#190170=CARTESIAN_POINT('Ctrl Pts',(-42.5181628534428,36.9279710066237,
-227.45166684362));
#190171=CARTESIAN_POINT('Ctrl Pts',(-42.7681359376673,37.099160688942,-227.735306122663));
#190172=CARTESIAN_POINT('Ctrl Pts',(-42.2982676358245,37.3130407532213,
-227.28653339185));
#190173=CARTESIAN_POINT('Ctrl Pts',(-42.6548022753341,37.0131169679292,
-227.289212613848));
#190174=CARTESIAN_POINT('Ctrl Pts',(-42.8898428091843,37.236452809997,-227.617810159066));
#190175=CARTESIAN_POINT('Ctrl Pts',(-42.449568951912,37.4293929451652,-227.088404778768));
#190176=CARTESIAN_POINT('Ctrl Pts',(-42.8047936666804,37.0608530872242,
-227.147939763718));
#190177=CARTESIAN_POINT('Ctrl Pts',(-43.034057629565,37.3598991263913,-227.498955015399));
#190178=CARTESIAN_POINT('',(-42.3284659498332,37.323247286775,-227.257657541791));
#190179=CARTESIAN_POINT('',(-42.9157357330403,37.2503223096489,-227.60005));
#190180=CARTESIAN_POINT('Origin',(-42.561590911764,37.6032832785437,-227.60005));
#190181=CARTESIAN_POINT('Ctrl Pts',(-42.3284659498332,37.323247286775,-227.257657541791));
#190182=CARTESIAN_POINT('Ctrl Pts',(-42.2348212547173,37.2293572270255,
-227.398208277735));
#190183=CARTESIAN_POINT('Ctrl Pts',(-42.1596659254298,37.1216554621379,
-227.537484019296));
#190184=CARTESIAN_POINT('Ctrl Pts',(-42.0508817378213,36.875278360935,-227.812856844476));
#190185=CARTESIAN_POINT('Ctrl Pts',(-42.0186496945452,36.7395078303233,
-227.945638225626));
#190186=CARTESIAN_POINT('Ctrl Pts',(-42.0144214928843,36.4424407209236,
-228.190025881898));
#190187=CARTESIAN_POINT('Ctrl Pts',(-42.0435120014734,36.2819711039298,
-228.300199623458));
#190188=CARTESIAN_POINT('Ctrl Pts',(-42.1845597227432,35.9630305475754,
-228.460113192376));
#190189=CARTESIAN_POINT('Ctrl Pts',(-42.2981827642303,35.8063936694652,
-228.507116757362));
#190190=CARTESIAN_POINT('Ctrl Pts',(-42.4431629103415,35.679860391633,-228.507034483728));
#190191=CARTESIAN_POINT('Ctrl Pts',(-42.6824807550637,35.9538445605081,
-228.35005));
#190192=CARTESIAN_POINT('Ctrl Pts',(-42.6612421131876,35.9708237622937,
-228.35005));
#190193=CARTESIAN_POINT('Ctrl Pts',(-42.6416747886319,35.9894679971484,
-228.348584527935));
#190194=CARTESIAN_POINT('Ctrl Pts',(-42.6238483368174,36.0095108015785,
-228.345682187426));
#190195=CARTESIAN_POINT('Ctrl Pts',(-42.6059666673684,36.0296156888201,
-228.342770856886));
#190196=CARTESIAN_POINT('Ctrl Pts',(-42.5898371951945,36.051127301889,-228.338413910558));
#190197=CARTESIAN_POINT('Ctrl Pts',(-42.5755217393577,36.0737850501726,
-228.33269132462));
#190198=CARTESIAN_POINT('Ctrl Pts',(-42.5611722482051,36.0964966677587,
-228.326955133107));
#190199=CARTESIAN_POINT('Ctrl Pts',(-42.548645882488,36.1203594054282,-228.31984714813));
#190200=CARTESIAN_POINT('Ctrl Pts',(-42.5379889612067,36.1451266982139,
-228.311495283899));
#190201=CARTESIAN_POINT('Ctrl Pts',(-42.5272658827256,36.1700477441047,
-228.303091572054));
#190202=CARTESIAN_POINT('Ctrl Pts',(-42.5184359407265,36.1958842028134,
-228.293428964205));
#190203=CARTESIAN_POINT('Ctrl Pts',(-42.5115234927364,36.2224076420049,
-228.282679485579));
#190204=CARTESIAN_POINT('Ctrl Pts',(-42.5096639751583,36.2295427121681,
-228.279787768421));
#190205=CARTESIAN_POINT('Ctrl Pts',(-42.5079430742378,36.2367276415673,
-228.276817606924));
#190206=CARTESIAN_POINT('Ctrl Pts',(-42.5063609306933,36.2439583155883,
-228.273772785812));
#190207=CARTESIAN_POINT('Ctrl Pts',(-42.499116500259,36.2770666357026,-228.259830944183));
#190208=CARTESIAN_POINT('Ctrl Pts',(-42.494659406233,36.3109617038901,-228.244340883019));
#190209=CARTESIAN_POINT('Ctrl Pts',(-42.4927644141358,36.3453020509556,
-228.227596971681));
#190210=CARTESIAN_POINT('Ctrl Pts',(-42.4908247467518,36.3804519870738,
-228.210458315139));
#190211=CARTESIAN_POINT('Ctrl Pts',(-42.4915690756913,36.4160687787602,
-228.192006435094));
#190212=CARTESIAN_POINT('Ctrl Pts',(-42.4947199712114,36.4518219988906,
-228.17253425434));
#190213=CARTESIAN_POINT('Ctrl Pts',(-42.4979832092334,36.4888499696984,
-228.152367809531));
#190214=CARTESIAN_POINT('Ctrl Pts',(-42.5038273540626,36.5260245969845,
-228.131107425433));
#190215=CARTESIAN_POINT('Ctrl Pts',(-42.5119112524688,36.5630117033036,
-228.10904757488));
#190216=CARTESIAN_POINT('Ctrl Pts',(-42.5146625727291,36.575600106803,-228.10153959906));
#190217=CARTESIAN_POINT('Ctrl Pts',(-42.5176730846629,36.5881670385908,
-228.093938733431));
#190218=CARTESIAN_POINT('Ctrl Pts',(-42.5209286169307,36.6007000433444,
-228.086255696196));
#190219=CARTESIAN_POINT('Ctrl Pts',(-42.529961845291,36.6354757680692,-228.064937329756));
#190220=CARTESIAN_POINT('Ctrl Pts',(-42.5408322428461,36.6698780646667,
-228.043043933556));
#190221=CARTESIAN_POINT('Ctrl Pts',(-42.5533688063073,36.703887121906,-228.020713953601));
#190222=CARTESIAN_POINT('Ctrl Pts',(-42.5662746745788,36.7388980253429,
-227.997726172244));
#190223=CARTESIAN_POINT('Ctrl Pts',(-42.580945768289,36.7734927289696,-227.974275110284));
#190224=CARTESIAN_POINT('Ctrl Pts',(-42.5972074794775,36.8076377013941,
-227.950458060818));
#190225=CARTESIAN_POINT('Ctrl Pts',(-42.6140741981072,36.8430530175208,
-227.925754911975));
#190226=CARTESIAN_POINT('Ctrl Pts',(-42.6326515546369,36.877985051418,-227.900657335133));
#190227=CARTESIAN_POINT('Ctrl Pts',(-42.6527659342923,36.9123752433028,
-227.875226912736));
#190228=CARTESIAN_POINT('Ctrl Pts',(-42.6592357673371,36.923436921748,-227.867047163224));
#190229=CARTESIAN_POINT('Ctrl Pts',(-42.6658648129815,36.9344423497653,
-227.858832670863));
#190230=CARTESIAN_POINT('Ctrl Pts',(-42.6726478674913,36.9453890066653,
-227.850584698399));
#190231=CARTESIAN_POINT('Ctrl Pts',(-42.6935377611533,36.9791016206895,
-227.825183270849));
#190232=CARTESIAN_POINT('Ctrl Pts',(-42.7157356438111,37.0120035407902,
-227.799674957455));
#190233=CARTESIAN_POINT('Ctrl Pts',(-42.7391629924829,37.044155356842,-227.774091800136));
#190234=CARTESIAN_POINT('Ctrl Pts',(-42.7629835616951,37.0768468308236,
-227.748079237719));
#190235=CARTESIAN_POINT('Ctrl Pts',(-42.7880749469651,37.1087630767367,
-227.721988306624));
#190236=CARTESIAN_POINT('Ctrl Pts',(-42.8143869883701,37.1399355114056,
-227.695823652788));
#190237=CARTESIAN_POINT('Ctrl Pts',(-42.840965774659,37.1714239644078,-227.669393748246));
#190238=CARTESIAN_POINT('Ctrl Pts',(-42.8687899359095,37.2021536040928,
-227.642887555501));
#190239=CARTESIAN_POINT('Ctrl Pts',(-42.8978437135211,37.2321209902752,
-227.616296132796));
#190240=CARTESIAN_POINT('Ctrl Pts',(-42.9037566503552,37.2382198619588,
-227.610884326976));
#190241=CARTESIAN_POINT('Ctrl Pts',(-42.9097206386978,37.2442870403172,
-227.605468976743));
#190242=CARTESIAN_POINT('Ctrl Pts',(-42.9157357330403,37.2503223096489,
-227.60005));
#190243=CARTESIAN_POINT('Origin',(-55.4874598092496,36.4953631270247,-218.849954951747));
#190244=CARTESIAN_POINT('',(-55.4814981831708,36.4969369346298,-218.349992971048));
#190245=CARTESIAN_POINT('Origin',(-55.4874598092437,36.4953631270311,-218.849954951747));
#190246=CARTESIAN_POINT('Origin',(-55.4874598092496,36.4953631270247,-218.849954951747));
#190247=CARTESIAN_POINT('Ctrl Pts',(-47.6725669502457,42.0231082257046,
-220.466889015618));
#190248=CARTESIAN_POINT('Ctrl Pts',(-47.4323473287633,41.7820828931217,
-220.144369179074));
#190249=CARTESIAN_POINT('Ctrl Pts',(-47.0855208017344,42.0968841351482,
-220.123650503535));
#190250=CARTESIAN_POINT('Ctrl Pts',(-46.0707360771706,40.4159047152535,
-222.861099896523));
#190251=CARTESIAN_POINT('Ctrl Pts',(-45.8332096734332,40.1775816336063,
-222.536757805232));
#190252=CARTESIAN_POINT('Ctrl Pts',(-45.484400697872,40.4881098339549,-222.518656969387));
#190253=CARTESIAN_POINT('Ctrl Pts',(-44.4733723917422,38.813183375666,-225.261296765486));
#190254=CARTESIAN_POINT('Ctrl Pts',(-44.2319528875239,38.5709541354632,
-224.942221240203));
#190255=CARTESIAN_POINT('Ctrl Pts',(-43.8866629950407,38.8855972869987,
-224.918940663302));
#190256=CARTESIAN_POINT('Ctrl Pts',(-42.8753796545602,37.2098308744472,
-227.66064404434));
#190257=CARTESIAN_POINT('Ctrl Pts',(-42.6348178655346,36.9684622266801,
-227.339136087256));
#190258=CARTESIAN_POINT('Ctrl Pts',(-42.288052160332,37.2828082188042,-227.318248057395));
#190259=CARTESIAN_POINT('',(-47.045128487469,42.0562187287015,-220.184138377616));
#190260=CARTESIAN_POINT('',(-47.632114758242,41.9825203546087,-220.52735443572));
#190261=CARTESIAN_POINT('Origin',(-47.2779699369656,42.3354813235036,-220.52735443572));
#190262=CARTESIAN_POINT('Ctrl Pts',(-47.0451284874689,42.0562187287015,
-220.184138377615));
#190263=CARTESIAN_POINT('Ctrl Pts',(-46.7366960558646,41.7463211125423,
-220.645534816153));
#190264=CARTESIAN_POINT('Ctrl Pts',(-46.4284290381068,41.4366970979731,
-221.107125178941));
#190265=CARTESIAN_POINT('Ctrl Pts',(-46.120270683096,41.1272424048856,-221.568864745196));
#190266=CARTESIAN_POINT('Ctrl Pts',(-45.9716601344877,40.9780066922679,
-221.79154042197));
#190267=CARTESIAN_POINT('Ctrl Pts',(-45.8230746082339,40.8288112637528,
-222.014250798809));
#190268=CARTESIAN_POINT('Ctrl Pts',(-45.6745073115757,40.6796484353907,
-222.236990859958));
#190269=CARTESIAN_POINT('Ctrl Pts',(-45.3447900435204,40.3486094963428,
-222.731320676143));
#190270=CARTESIAN_POINT('Ctrl Pts',(-45.0151589288621,40.0177304633959,
-223.225796697889));
#190271=CARTESIAN_POINT('Ctrl Pts',(-44.6855353620086,39.6869690109204,
-223.720364098522));
#190272=CARTESIAN_POINT('Ctrl Pts',(-44.3702745988347,39.3706199436151,
-224.193381539759));
#190273=CARTESIAN_POINT('Ctrl Pts',(-44.0550203277662,39.0543798419438,
-224.666482570011));
#190274=CARTESIAN_POINT('Ctrl Pts',(-43.7397498044305,38.7382135573481,
-225.139619221798));
#190275=CARTESIAN_POINT('Ctrl Pts',(-43.4407153855777,38.4383295080099,
-225.588389827462));
#190276=CARTESIAN_POINT('Ctrl Pts',(-43.1416663361619,38.1385125871435,
-226.03719248019));
#190277=CARTESIAN_POINT('Ctrl Pts',(-42.8426281635058,37.838720016404,-226.485986248233));
#190278=CARTESIAN_POINT('Ctrl Pts',(-42.6712323665805,37.6668918309996,
-226.743215500424));
#190279=CARTESIAN_POINT('Ctrl Pts',(-42.4998409833723,37.4950713442305,
-227.000441833917));
#190280=CARTESIAN_POINT('Ctrl Pts',(-42.3284659498332,37.3232472867749,
-227.25765754179));
#190281=CARTESIAN_POINT('Ctrl Pts',(-42.9157357330403,37.2503223096489,
-227.60005));
#190282=CARTESIAN_POINT('Ctrl Pts',(-44.486815106976,38.8266711785776,-225.241083793951));
#190283=CARTESIAN_POINT('Ctrl Pts',(-46.0573252848254,40.4024489423018,
-222.881355908373));
#190284=CARTESIAN_POINT('Ctrl Pts',(-47.632114758242,41.9825203546087,-220.52735443572));
#190285=CARTESIAN_POINT('Ctrl Pts',(-55.4804763444372,36.5293010961029,
-218.35005));
#190286=CARTESIAN_POINT('Ctrl Pts',(-54.9916284043978,36.4242882801267,
-218.35005));
#190287=CARTESIAN_POINT('Ctrl Pts',(-54.9916284043978,36.4242882801268,
-218.85005));
#190288=CARTESIAN_POINT('Ctrl Pts',(-55.4808808567138,36.5185275155889,
-218.35005));
#190289=CARTESIAN_POINT('Ctrl Pts',(-54.9932481939215,36.4167479617736,
-218.351913756624));
#190290=CARTESIAN_POINT('Ctrl Pts',(-54.9934502776071,36.4158072299129,
-218.850049997976));
#190291=CARTESIAN_POINT('Ctrl Pts',(-55.4812212937741,36.5077394466269,
-218.350030277458));
#190292=CARTESIAN_POINT('Ctrl Pts',(-54.9948238206649,36.4091341749127,
-218.353722457588));
#190293=CARTESIAN_POINT('Ctrl Pts',(-54.9951959309483,36.4073227473215,
-218.85001713104));
#190294=CARTESIAN_POINT('Ctrl Pts',(-55.4814981831709,36.4969369346252,
-218.349992971048));
#190295=CARTESIAN_POINT('Ctrl Pts',(-54.9963513974766,36.4014502251401,
-218.35547736011));
#190296=CARTESIAN_POINT('Ctrl Pts',(-54.9968660030035,36.3988348033192,
-218.849954951747));
#190297=CARTESIAN_POINT('',(-54.9916284043978,36.4242882801268,-218.85005));
#190298=CARTESIAN_POINT('',(-55.4804763444372,36.529301096103,-218.35005));
#190299=CARTESIAN_POINT('Origin',(-55.4804763444372,36.529301096103,-218.85005));
#190300=CARTESIAN_POINT('Ctrl Pts',(-54.9916284043978,36.4242882801268,
-218.85005));
#190301=CARTESIAN_POINT('Ctrl Pts',(-54.9934477121007,36.4158191726697,
-218.850049997978));
#190302=CARTESIAN_POINT('Ctrl Pts',(-54.9951937291456,36.4073339377235,
-218.850017211078));
#190303=CARTESIAN_POINT('Ctrl Pts',(-54.9968660030035,36.3988348033193,
-218.849954951747));
#190304=CARTESIAN_POINT('Ctrl Pts',(-55.4814981831708,36.4969369346298,
-218.349992971048));
#190305=CARTESIAN_POINT('Ctrl Pts',(-55.4812216183662,36.507726772777,-218.350030233692));
#190306=CARTESIAN_POINT('Ctrl Pts',(-55.4808813172563,36.5185152497272,
-218.35005));
#190307=CARTESIAN_POINT('Ctrl Pts',(-55.4804763444372,36.5293010961029,
-218.35005));
#190308=CARTESIAN_POINT('Ctrl Pts',(-47.0451284874689,42.0562187287016,
-220.184138377616));
#190309=CARTESIAN_POINT('Ctrl Pts',(-47.3919300806125,41.7415300830818,
-220.204915325333));
#190310=CARTESIAN_POINT('Ctrl Pts',(-47.6321147582419,41.9825203546088,
-220.52735443572));
#190311=CARTESIAN_POINT('Ctrl Pts',(-47.255889523814,42.2679809657455,-219.868852497358));
#190312=CARTESIAN_POINT('Ctrl Pts',(-47.5344785649843,41.9530961111727,
-219.935794482803));
#190313=CARTESIAN_POINT('Ctrl Pts',(-47.7902484566451,42.1411844429755,
-220.212182607147));
#190314=CARTESIAN_POINT('Ctrl Pts',(-47.5083824724237,42.4326649364373,
-219.563965012339));
#190315=CARTESIAN_POINT('Ctrl Pts',(-47.7321494909123,42.1394451765273,
-219.649704637013));
#190316=CARTESIAN_POINT('Ctrl Pts',(-47.979916006804,42.2643583982894,-219.907394043497));
#190317=CARTESIAN_POINT('Ctrl Pts',(-47.9638307571195,42.5902413709234,
-219.126165729975));
#190318=CARTESIAN_POINT('Ctrl Pts',(-48.1175959253334,42.3304889669946,
-219.231029546912));
#190319=CARTESIAN_POINT('Ctrl Pts',(-48.3223344522033,42.3817233472697,
-219.469720269686));
#190320=CARTESIAN_POINT('Ctrl Pts',(-48.1257697081407,42.6260372470742,
-218.986746587153));
#190321=CARTESIAN_POINT('Ctrl Pts',(-48.2547747023755,42.3779588184046,
-219.098571457423));
#190322=CARTESIAN_POINT('Ctrl Pts',(-48.4441285568114,42.4082510978143,
-219.330335434309));
#190323=CARTESIAN_POINT('Ctrl Pts',(-48.4690711499925,42.6549505391913,
-218.728256059429));
#190324=CARTESIAN_POINT('Ctrl Pts',(-48.5489925463843,42.4312682822097,
-218.853050886545));
#190325=CARTESIAN_POINT('Ctrl Pts',(-48.7024187673646,42.4292025475747,
-219.071888450682));
#190326=CARTESIAN_POINT('Ctrl Pts',(-48.653008232648,42.6479010052333,-218.607549287091));
#190327=CARTESIAN_POINT('Ctrl Pts',(-48.7086549671031,42.4384217702358,
-218.737132750756));
#190328=CARTESIAN_POINT('Ctrl Pts',(-48.8408569866015,42.4234942721777,
-218.951187879954));
#190329=CARTESIAN_POINT('Ctrl Pts',(-48.841793010828,42.6113834075459,-218.506376562157));
#190330=CARTESIAN_POINT('Ctrl Pts',(-48.874649979175,42.4168725889835,-218.639304842979));
#190331=CARTESIAN_POINT('Ctrl Pts',(-48.9829866058019,42.3956441991541,
-218.850009606915));
#190332=CARTESIAN_POINT('',(-48.8417930108281,42.6113834075459,-218.506376562157));
#190333=CARTESIAN_POINT('',(-48.9829866058019,42.3956441991541,-218.850009606915));
#190334=CARTESIAN_POINT('Origin',(-49.0791324003789,42.8863131162308,-218.850009606915));
#190335=CARTESIAN_POINT('Ctrl Pts',(-48.8417930108281,42.6113834075459,
-218.506376562157));
#190336=CARTESIAN_POINT('Ctrl Pts',(-48.653008232648,42.6479010052333,-218.607549287091));
#190337=CARTESIAN_POINT('Ctrl Pts',(-48.4690711499925,42.6549505391913,
-218.728256059429));
#190338=CARTESIAN_POINT('Ctrl Pts',(-48.1257697081407,42.6260372470742,
-218.986746587153));
#190339=CARTESIAN_POINT('Ctrl Pts',(-47.9638307571195,42.5902413709234,
-219.126165729975));
#190340=CARTESIAN_POINT('Ctrl Pts',(-47.5083824724237,42.4326649364373,
-219.563965012339));
#190341=CARTESIAN_POINT('Ctrl Pts',(-47.255889523814,42.2679809657455,-219.868852497358));
#190342=CARTESIAN_POINT('Ctrl Pts',(-47.045128487469,42.0562187287015,-220.184138377616));
#190343=CARTESIAN_POINT('Ctrl Pts',(-47.632114758242,41.9825203546087,-220.52735443572));
#190344=CARTESIAN_POINT('Ctrl Pts',(-47.7902484566451,42.1411844429755,
-220.212182607147));
#190345=CARTESIAN_POINT('Ctrl Pts',(-47.979916006804,42.2643583982894,-219.907394043497));
#190346=CARTESIAN_POINT('Ctrl Pts',(-48.3223344522033,42.3817233472697,
-219.469720269686));
#190347=CARTESIAN_POINT('Ctrl Pts',(-48.4441285568114,42.4082510978143,
-219.330335434309));
#190348=CARTESIAN_POINT('Ctrl Pts',(-48.7024187673646,42.4292025475747,
-219.071888450682));
#190349=CARTESIAN_POINT('Ctrl Pts',(-48.8408569866015,42.4234942721777,
-218.951187879954));
#190350=CARTESIAN_POINT('Ctrl Pts',(-48.9829866058019,42.3956441991541,
-218.850009606915));
#190351=CARTESIAN_POINT('Origin',(-53.5250845842796,36.1092498321983,-218.85005));
#190352=CARTESIAN_POINT('',(-54.6328983814091,37.1205601658197,-218.85005));
#190353=CARTESIAN_POINT('',(-55.0021696471189,37.4576636103602,-218.35005));
#190354=CARTESIAN_POINT('Origin',(-55.0021696471189,37.4576636103602,-218.85005));
#190355=CARTESIAN_POINT('Origin',(-53.5250845842796,36.1092498321983,-218.85005));
#190356=CARTESIAN_POINT('Origin',(-53.5250845842796,36.1092498321983,-218.35005));
#190357=CARTESIAN_POINT('Origin',(-49.0791324003789,42.8863131162308,-218.850009606915));
#190358=CARTESIAN_POINT('',(-49.0801870931398,42.8824343798319,-218.350025764149));
#190359=CARTESIAN_POINT('Origin',(-49.0791324003789,42.8863131162308,-218.850009606915));
#190360=CARTESIAN_POINT('Origin',(-49.0791324003789,42.8863131162308,-218.850009606915));
#190361=CARTESIAN_POINT('Origin',(-0.128459562639233,-12.6359082483571,
-218.85005));
#190362=CARTESIAN_POINT('',(-49.7021444432209,42.0348313420379,-218.85005));
#190363=CARTESIAN_POINT('',(-50.0380095169376,42.4052293067426,-218.35005));
#190364=CARTESIAN_POINT('Origin',(-50.0380095169376,42.4052293067426,-218.85005));
#190365=CARTESIAN_POINT('Origin',(-0.128459562639233,-12.6359082483571,
-218.85005));
#190366=CARTESIAN_POINT('Origin',(-0.128459562639233,-12.6359082483571,
-218.35005));
#190367=CARTESIAN_POINT('Ctrl Pts',(-48.999474814567,42.392317257495,-218.85005));
#190368=CARTESIAN_POINT('Ctrl Pts',(-48.9994748145671,42.3923172574951,
-218.35005));
#190369=CARTESIAN_POINT('Ctrl Pts',(-49.1011166787324,42.8818771940186,
-218.35005));
#190370=CARTESIAN_POINT('Ctrl Pts',(-48.9939799633645,42.3934580921056,
-218.85004999869));
#190371=CARTESIAN_POINT('Ctrl Pts',(-48.994587444257,42.3933319685669,-218.351257450515));
#190372=CARTESIAN_POINT('Ctrl Pts',(-49.09414603136,42.8820897398471,-218.35005));
#190373=CARTESIAN_POINT('Ctrl Pts',(-48.9884838968603,42.394567013707,-218.850036211906));
#190374=CARTESIAN_POINT('Ctrl Pts',(-48.9896694475663,42.3943279693454,
-218.352441808199));
#190375=CARTESIAN_POINT('Ctrl Pts',(-49.0871694989175,42.882275419924,-218.350041726378));
#190376=CARTESIAN_POINT('Ctrl Pts',(-48.9829866058019,42.3956441991541,
-218.850009606915));
#190377=CARTESIAN_POINT('Ctrl Pts',(-48.9847217242793,42.3953042054457,
-218.353603405568));
#190378=CARTESIAN_POINT('Ctrl Pts',(-49.0801870931398,42.8824343798319,
-218.350025764149));
#190379=CARTESIAN_POINT('',(-49.1011166787325,42.8818771940186,-218.35005));
#190380=CARTESIAN_POINT('',(-48.999474814567,42.392317257495,-218.85005));
#190381=CARTESIAN_POINT('Origin',(-49.1011166787325,42.8818771940186,-218.85005));
#190382=CARTESIAN_POINT('Ctrl Pts',(-49.1011166787325,42.8818771940186,
-218.35005));
#190383=CARTESIAN_POINT('Ctrl Pts',(-49.0941409157939,42.8820898960309,
-218.35005));
#190384=CARTESIAN_POINT('Ctrl Pts',(-49.0871642720694,42.8822755387356,
-218.35004171443));
#190385=CARTESIAN_POINT('Ctrl Pts',(-49.0801870931398,42.8824343798319,
-218.350025764149));
#190386=CARTESIAN_POINT('Ctrl Pts',(-48.9829866058019,42.3956441991541,
-218.850009606915));
#190387=CARTESIAN_POINT('Ctrl Pts',(-48.9884887606911,42.3945660606471,
-218.85003623417));
#190388=CARTESIAN_POINT('Ctrl Pts',(-48.993985033412,42.3934570394682,-218.850049998691));
#190389=CARTESIAN_POINT('Ctrl Pts',(-48.999474814567,42.392317257495,-218.85005));
#190390=CARTESIAN_POINT('Origin',(-48.6945492220708,40.9236374479242,-218.85005));
#190391=CARTESIAN_POINT('Origin',(-48.6945492220708,40.9236374479242,-218.35005));
#190392=CARTESIAN_POINT('Origin',(-48.6945492220708,40.9236374479242,-218.85005));
#190393=CARTESIAN_POINT('Origin',(-41.3132181298675,38.0528376956935,-205.84995));
#190394=CARTESIAN_POINT('',(-48.8684365469981,47.38326056293,-205.34995));
#190395=CARTESIAN_POINT('',(-48.5538345628697,46.9947384336248,-205.841223796781));
#190396=CARTESIAN_POINT('Origin',(-48.8684365469981,47.38326056293,-205.84995));
#190397=CARTESIAN_POINT('',(-43.5622571193626,49.8460535351382,-205.34995));
#190398=CARTESIAN_POINT('Origin',(-41.3132181298675,38.0528376956935,-205.34995));
#190399=CARTESIAN_POINT('',(-43.4686063353067,49.3549798298524,-205.841223796781));
#190400=CARTESIAN_POINT('Origin',(-43.5622571193626,49.8460535351382,-205.84995));
#190401=CARTESIAN_POINT('Origin',(-41.3132181298675,38.0528376956935,-205.841223796781));
#190402=CARTESIAN_POINT('Origin',(0.,-12.9675000200281,-205.84995));
#190403=CARTESIAN_POINT('',(-59.9876878113059,36.3459434263872,-205.34995));
#190404=CARTESIAN_POINT('',(-59.6015030478428,36.0284766063157,-205.841223796781));
#190405=CARTESIAN_POINT('Origin',(-59.9876878113059,36.3459434263873,-205.84995));
#190406=CARTESIAN_POINT('Origin',(0.,-12.9675000200281,-205.34995));
#190407=CARTESIAN_POINT('Origin',(0.,-12.9675000200281,-205.841223796781));
#190408=CARTESIAN_POINT('Origin',(-50.7133971693864,28.7219255026674,-205.84995));
#190409=CARTESIAN_POINT('',(-62.7097829146859,29.1961040154388,-205.34995));
#190410=CARTESIAN_POINT('',(-62.2102491422031,29.1763590533857,-205.841223796781));
#190411=CARTESIAN_POINT('Origin',(-62.709782914686,29.1961040154388,-205.84995));
#190412=CARTESIAN_POINT('Origin',(-50.7133971693864,28.7219255026674,-205.34995));
#190413=CARTESIAN_POINT('Origin',(-50.7133971693864,28.7219255026674,-205.841223796781));
#190414=CARTESIAN_POINT('Origin',(1004.,-12.967500020028,-205.84995));
#190415=CARTESIAN_POINT('',(-62.7097829146858,-55.1311040554952,-205.34995));
#190416=CARTESIAN_POINT('',(-62.210249142203,-55.1113590934421,-205.841223796781));
#190417=CARTESIAN_POINT('Origin',(-62.7097829146858,-55.1311040554952,-205.84995));
#190418=CARTESIAN_POINT('Origin',(1004.,-12.967500020028,-205.34995));
#190419=CARTESIAN_POINT('Origin',(1004.,-12.967500020028,-205.841223796781));
#190420=CARTESIAN_POINT('Origin',(-50.7133971693864,-54.6569255427236,-205.84995));
#190421=CARTESIAN_POINT('',(-59.9876878113058,-62.2809434664435,-205.34995));
#190422=CARTESIAN_POINT('',(-59.6015030478428,-61.963476646372,-205.841223796781));
#190423=CARTESIAN_POINT('Origin',(-59.9876878113059,-62.2809434664436,-205.84995));
#190424=CARTESIAN_POINT('Origin',(-50.7133971693864,-54.6569255427236,-205.34995));
#190425=CARTESIAN_POINT('Origin',(-50.7133971693864,-54.6569255427236,-205.841223796781));
#190426=CARTESIAN_POINT('Origin',(0.,-12.9675000200281,-205.84995));
#190427=CARTESIAN_POINT('',(-49.142885306769,-73.0949913797652,-205.34995));
#190428=CARTESIAN_POINT('',(-48.8265164945923,-72.7079065982776,-205.841223796781));
#190429=CARTESIAN_POINT('Origin',(-49.142885306769,-73.0949913797652,-205.84995));
#190430=CARTESIAN_POINT('Origin',(0.,-12.9675000200281,-205.34995));
#190431=CARTESIAN_POINT('Origin',(0.,-12.9675000200281,-205.841223796781));
#190432=CARTESIAN_POINT('Origin',(-41.5452362233251,-63.7990866568863,-205.84995));
#190433=CARTESIAN_POINT('',(-42.0177747166746,-75.7955371145968,-205.34995));
#190434=CARTESIAN_POINT('',(-41.998098045614,-75.2960006474661,-205.841223796781));
#190435=CARTESIAN_POINT('Origin',(-42.0177747166746,-75.7955371145968,-205.84995));
#190436=CARTESIAN_POINT('Origin',(-41.5452362233251,-63.7990866568863,-205.34995));
#190437=CARTESIAN_POINT('Origin',(-41.5452362233251,-63.7990866568863,-205.841223796781));
#190438=CARTESIAN_POINT('Ctrl Pts',(-54.8483808955534,-62.1772035872459,
-218.488025452358));
#190439=CARTESIAN_POINT('Ctrl Pts',(-54.9567009523893,-62.2733518205983,
-218.35005));
#190440=CARTESIAN_POINT('Ctrl Pts',(-55.1063041457931,-62.4061442430716,
-218.35005));
#190441=CARTESIAN_POINT('Ctrl Pts',(-54.9311672479915,-62.0839582776417,
-218.488011964977));
#190442=CARTESIAN_POINT('Ctrl Pts',(-55.0396688463703,-62.1798977449628,
-218.350049999993));
#190443=CARTESIAN_POINT('Ctrl Pts',(-55.1895187430304,-62.3123951477066,
-218.35005));
#190444=CARTESIAN_POINT('Ctrl Pts',(-55.0136740740184,-61.9904901268691,
-218.487996778696));
#190445=CARTESIAN_POINT('Ctrl Pts',(-55.1223583736924,-62.0862177900411,
-218.350049999995));
#190446=CARTESIAN_POINT('Ctrl Pts',(-55.2724546449993,-62.2184167144339,
-218.35005));
#190447=CARTESIAN_POINT('Ctrl Pts',(-55.0958998011493,-61.8967941020366,
-218.487980161586));
#190448=CARTESIAN_POINT('Ctrl Pts',(-55.2047676214781,-61.9923073188158,
-218.35005));
#190449=CARTESIAN_POINT('Ctrl Pts',(-55.3551085347194,-62.1242062049498,
-218.35005));
#190450=CARTESIAN_POINT('',(-55.3551085347089,-62.1242062049619,-218.35005));
#190451=CARTESIAN_POINT('Origin',(-6.53661556842313,-19.2936642511711,-218.35005));
#190452=CARTESIAN_POINT('',(-55.0958998011388,-61.8967941020485,-218.487980161586));
#190453=CARTESIAN_POINT('Origin',(-55.3551085347089,-62.1242062049619,-218.85005));
#190454=CARTESIAN_POINT('Origin',(-6.32111522020743,-19.0925325781086,-218.204999057165));
#190455=CARTESIAN_POINT('Ctrl Pts',(-55.4938952567199,-61.9654919306031,
-218.35005));
#190456=CARTESIAN_POINT('Ctrl Pts',(-55.3431423575669,-61.8341015991581,
-218.35005));
#190457=CARTESIAN_POINT('Ctrl Pts',(-55.2339673727997,-61.7389489519143,
-218.487950878256));
#190458=CARTESIAN_POINT('Ctrl Pts',(-55.4477195716702,-62.0184723768345,
-218.35005));
#190459=CARTESIAN_POINT('Ctrl Pts',(-55.2971033694472,-61.8869121544979,
-218.350049999996));
#190460=CARTESIAN_POINT('Ctrl Pts',(-55.1880309233148,-61.7916386130721,
-218.487961072495));
#190461=CARTESIAN_POINT('Ctrl Pts',(-55.4014572374666,-62.0713770530022,
-218.35005));
#190462=CARTESIAN_POINT('Ctrl Pts',(-55.2509784443238,-61.9396472076622,
-218.350050000013));
#190463=CARTESIAN_POINT('Ctrl Pts',(-55.14200840849,-61.8442534512036,-218.487970843436));
#190464=CARTESIAN_POINT('Ctrl Pts',(-55.3551085347089,-62.1242062049619,
-218.35005));
#190465=CARTESIAN_POINT('Ctrl Pts',(-55.2047676214677,-61.9923073188278,
-218.35005));
#190466=CARTESIAN_POINT('Ctrl Pts',(-55.0958998011388,-61.8967941020486,
-218.487980161586));
#190467=CARTESIAN_POINT('',(-55.2339673727996,-61.7389489519143,-218.487950878256));
#190468=CARTESIAN_POINT('',(-55.4938952567199,-61.9654919306031,-218.35005));
#190469=CARTESIAN_POINT('Origin',(-55.4938952567198,-61.9654919306031,-218.85005));
#190470=CARTESIAN_POINT('Origin',(-7.62393634648824,-43.3515330069781,-218.305892816451));
#190471=CARTESIAN_POINT('Ctrl Pts',(-55.3551085347089,-62.1242062049619,
-218.35005));
#190472=CARTESIAN_POINT('Ctrl Pts',(-55.4014571755248,-62.0713771235952,
-218.35005));
#190473=CARTESIAN_POINT('Ctrl Pts',(-55.4477196335097,-62.0184723058819,
-218.35005));
#190474=CARTESIAN_POINT('Ctrl Pts',(-55.4938952567199,-61.9654919306031,
-218.35005));
#190475=CARTESIAN_POINT('Ctrl Pts',(-48.9443109379934,-69.7210624363874,
-217.233400031701));
#190476=CARTESIAN_POINT('Ctrl Pts',(-49.0991171386077,-69.4468461963774,
-217.336253844649));
#190477=CARTESIAN_POINT('Ctrl Pts',(-49.2925903552098,-69.4989817480832,
-217.60005));
#190478=CARTESIAN_POINT('Ctrl Pts',(-48.8106894467424,-69.6845014967476,
-217.338910655172));
#190479=CARTESIAN_POINT('Ctrl Pts',(-48.9711549960785,-69.4349010506438,
-217.421407154983));
#190480=CARTESIAN_POINT('Ctrl Pts',(-49.1585563021333,-69.4628633673211,
-217.663314872408));
#190481=CARTESIAN_POINT('Ctrl Pts',(-48.6852690846176,-69.6367945835064,
-217.447311197387));
#190482=CARTESIAN_POINT('Ctrl Pts',(-48.8462037291419,-69.4114072943244,
-217.512721374121));
#190483=CARTESIAN_POINT('Ctrl Pts',(-49.0313897910431,-69.4205569633974,
-217.728324544416));
#190484=CARTESIAN_POINT('Ctrl Pts',(-48.4569758615832,-69.5115061162924,
-217.672103262066));
#190485=CARTESIAN_POINT('Ctrl Pts',(-48.617833871194,-69.3350054470626,
-217.703310121074));
#190486=CARTESIAN_POINT('Ctrl Pts',(-48.7961868532913,-69.3194593473905,
-217.86308947659));
#190487=CARTESIAN_POINT('Ctrl Pts',(-48.3517740014028,-69.4325906117154,
-217.790828095074));
#190488=CARTESIAN_POINT('Ctrl Pts',(-48.5104100125145,-69.2819129896144,
-217.805106001601));
#190489=CARTESIAN_POINT('Ctrl Pts',(-48.685721809208,-69.2595955427122,
-217.934254584857));
#190490=CARTESIAN_POINT('Ctrl Pts',(-48.1937459441518,-69.2310798747107,
-218.028989271677));
#190491=CARTESIAN_POINT('Ctrl Pts',(-48.3463679525101,-69.1352844945817,
-218.007643735867));
#190492=CARTESIAN_POINT('Ctrl Pts',(-48.5116380513506,-69.117661111215,
-218.07697894517));
#190493=CARTESIAN_POINT('Ctrl Pts',(-48.1412202429506,-69.1061885177359,
-218.149957970462));
#190494=CARTESIAN_POINT('Ctrl Pts',(-48.2880154025268,-69.0395906692494,
-218.111013157341));
#190495=CARTESIAN_POINT('Ctrl Pts',(-48.448087208547,-69.0341807326189,
-218.14945588291));
#190496=CARTESIAN_POINT('Ctrl Pts',(-48.1485991473491,-68.8903805804807,
-218.301008298776));
#190497=CARTESIAN_POINT('Ctrl Pts',(-48.2845085174756,-68.8714073071909,
-218.233969642811));
#190498=CARTESIAN_POINT('Ctrl Pts',(-48.434090564434,-68.8996196892853,
-218.239916153685));
#190499=CARTESIAN_POINT('Ctrl Pts',(-48.1657471491621,-68.8149276007785,
-218.34519506975));
#190500=CARTESIAN_POINT('Ctrl Pts',(-48.2974742535841,-68.8121010312849,
-218.268894159576));
#190501=CARTESIAN_POINT('Ctrl Pts',(-48.4434199676664,-68.8540114137795,
-218.266370341262));
#190502=CARTESIAN_POINT('Ctrl Pts',(-48.2274460866499,-68.6669868960869,
-218.415001874049));
#190503=CARTESIAN_POINT('Ctrl Pts',(-48.3498583953795,-68.6963155179756,
-218.320852508057));
#190504=CARTESIAN_POINT('Ctrl Pts',(-48.4891230485367,-68.7673591858045,
-218.308143757591));
#190505=CARTESIAN_POINT('Ctrl Pts',(-48.2716020915273,-68.5947725811949,
-218.440653607377));
#190506=CARTESIAN_POINT('Ctrl Pts',(-48.3890987036532,-68.639745098431,
-218.338051990079));
#190507=CARTESIAN_POINT('Ctrl Pts',(-48.525123832139,-68.7264593463756,
-218.323478979764));
#190508=CARTESIAN_POINT('Ctrl Pts',(-48.3245605310991,-68.5271120961851,
-218.457629631481));
#190509=CARTESIAN_POINT('Ctrl Pts',(-48.4365020850992,-68.587560591765,
-218.34711549972));
#190510=CARTESIAN_POINT('Ctrl Pts',(-48.5701931618904,-68.6892604152372,
-218.333619302448));
#190511=CARTESIAN_POINT('',(-48.9443109379934,-69.7210624363875,-217.233400031701));
#190512=CARTESIAN_POINT('Ctrl Pts',(-48.3245605310987,-68.5271120961857,
-218.45762963148));
#190513=CARTESIAN_POINT('Ctrl Pts',(-48.2716020915273,-68.5947725811949,
-218.440653607377));
#190514=CARTESIAN_POINT('Ctrl Pts',(-48.2274460866499,-68.6669868960869,
-218.415001874049));
#190515=CARTESIAN_POINT('Ctrl Pts',(-48.1657471491621,-68.8149276007785,
-218.34519506975));
#190516=CARTESIAN_POINT('Ctrl Pts',(-48.1485991473491,-68.8903805804807,
-218.301008298776));
#190517=CARTESIAN_POINT('Ctrl Pts',(-48.1412202429506,-69.1061885177359,
-218.149957970462));
#190518=CARTESIAN_POINT('Ctrl Pts',(-48.1937459441518,-69.2310798747107,
-218.028989271677));
#190519=CARTESIAN_POINT('Ctrl Pts',(-48.3517740014028,-69.4325906117154,
-217.790828095074));
#190520=CARTESIAN_POINT('Ctrl Pts',(-48.4569758615832,-69.5115061162924,
-217.672103262066));
#190521=CARTESIAN_POINT('Ctrl Pts',(-48.6852690846176,-69.6367945835064,
-217.447311197387));
#190522=CARTESIAN_POINT('Ctrl Pts',(-48.8106894467424,-69.6845014967476,
-217.338910655172));
#190523=CARTESIAN_POINT('Ctrl Pts',(-48.9443109379934,-69.7210624363875,
-217.233400031701));
#190524=CARTESIAN_POINT('',(-49.2925903552098,-69.4989817480832,-217.60005));
#190525=CARTESIAN_POINT('Origin',(-49.1624951782473,-69.9817604188332,-217.60005));
#190526=CARTESIAN_POINT('Ctrl Pts',(-49.2925903552098,-69.4989817480832,
-217.60005));
#190527=CARTESIAN_POINT('Ctrl Pts',(-49.1585563021333,-69.4628633673211,
-217.663314872408));
#190528=CARTESIAN_POINT('Ctrl Pts',(-49.0313897910431,-69.4205569633974,
-217.728324544416));
#190529=CARTESIAN_POINT('Ctrl Pts',(-48.7961868532913,-69.3194593473905,
-217.86308947659));
#190530=CARTESIAN_POINT('Ctrl Pts',(-48.685721809208,-69.2595955427122,
-217.934254584857));
#190531=CARTESIAN_POINT('Ctrl Pts',(-48.5116380513506,-69.117661111215,
-218.07697894517));
#190532=CARTESIAN_POINT('Ctrl Pts',(-48.448087208547,-69.0341807326189,
-218.14945588291));
#190533=CARTESIAN_POINT('Ctrl Pts',(-48.434090564434,-68.8996196892853,
-218.239916153685));
#190534=CARTESIAN_POINT('Ctrl Pts',(-48.4434199676664,-68.8540114137795,
-218.266370341262));
#190535=CARTESIAN_POINT('Ctrl Pts',(-48.4891230485367,-68.7673591858045,
-218.308143757591));
#190536=CARTESIAN_POINT('Ctrl Pts',(-48.525123832139,-68.7264593463756,
-218.323478979764));
#190537=CARTESIAN_POINT('Ctrl Pts',(-48.5701931618903,-68.6892604152372,
-218.333619302448));
#190538=CARTESIAN_POINT('Ctrl Pts',(-55.0927945669581,-61.9237522605322,
-218.473143922888));
#190539=CARTESIAN_POINT('Ctrl Pts',(-55.2402662392572,-62.0019900264124,
-218.318365680583));
#190540=CARTESIAN_POINT('Ctrl Pts',(-55.4233494278323,-62.1325346783774,
-218.34109494148));
#190541=CARTESIAN_POINT('Ctrl Pts',(-55.2398731800779,-61.7035250203945,
-218.506633117061));
#190542=CARTESIAN_POINT('Ctrl Pts',(-55.339847442567,-61.8077216182083,
-218.369411334443));
#190543=CARTESIAN_POINT('Ctrl Pts',(-55.4942885846974,-61.9313224231195,
-218.361210102213));
#190544=CARTESIAN_POINT('Ctrl Pts',(-55.4522263025615,-61.487229681304,
-218.488253912002));
#190545=CARTESIAN_POINT('Ctrl Pts',(-55.5089980550799,-61.6041191053711,
-218.374487087645));
#190546=CARTESIAN_POINT('Ctrl Pts',(-55.6061969562536,-61.7409934655382,
-218.350218604685));
#190547=CARTESIAN_POINT('Ctrl Pts',(-55.774137059737,-61.3702400653051,
-218.328065200791));
#190548=CARTESIAN_POINT('Ctrl Pts',(-55.7613227347501,-61.506523014171,
-218.253037832299));
#190549=CARTESIAN_POINT('Ctrl Pts',(-55.796657340851,-61.6580344229345,
-218.254184099553));
#190550=CARTESIAN_POINT('Ctrl Pts',(-55.8574514448172,-61.3576561642577,
-218.275537189096));
#190551=CARTESIAN_POINT('Ctrl Pts',(-55.8267293193376,-61.4983471195505,
-218.210866812023));
#190552=CARTESIAN_POINT('Ctrl Pts',(-55.8476827468257,-61.653839850603,
-218.222689657358));
#190553=CARTESIAN_POINT('Ctrl Pts',(-56.0156427621496,-61.3668889087165,
-218.155327703159));
#190554=CARTESIAN_POINT('Ctrl Pts',(-55.9490748084097,-61.515028576828,
-218.112202025634));
#190555=CARTESIAN_POINT('Ctrl Pts',(-55.9478088686909,-61.6782199479451,
-218.150610277818));
#190556=CARTESIAN_POINT('Ctrl Pts',(-56.0882800272526,-61.3885186677252,
-218.089385782703));
#190557=CARTESIAN_POINT('Ctrl Pts',(-56.0046279913313,-61.5397831272315,
-218.056774547579));
#190558=CARTESIAN_POINT('Ctrl Pts',(-55.995486790882,-61.7063946791486,
-218.11106824763));
#190559=CARTESIAN_POINT('Ctrl Pts',(-56.282274388892,-61.4870635747884,
-217.88822842421));
#190560=CARTESIAN_POINT('Ctrl Pts',(-56.1504429355983,-61.6458021440819,
-217.885983497565));
#190561=CARTESIAN_POINT('Ctrl Pts',(-56.1268157801208,-61.8214573400613,
-217.990439031765));
#190562=CARTESIAN_POINT('Ctrl Pts',(-56.3812088475294,-61.5957603700639,
-217.749760076526));
#190563=CARTESIAN_POINT('Ctrl Pts',(-56.2193581582234,-61.7580490411378,
-217.766950789269));
#190564=CARTESIAN_POINT('Ctrl Pts',(-56.1995158790201,-61.9371995248376,
-217.907396389637));
#190565=CARTESIAN_POINT('Ctrl Pts',(-56.5652163308461,-61.8918982137455,
-217.434373456315));
#190566=CARTESIAN_POINT('Ctrl Pts',(-56.3362907798363,-62.05739085945,-217.497500852187));
#190567=CARTESIAN_POINT('Ctrl Pts',(-56.3439416689173,-62.2442222025972,
-217.718239387215));
#190568=CARTESIAN_POINT('Ctrl Pts',(-56.6321920140805,-62.0996608522455,
-217.257993584228));
#190569=CARTESIAN_POINT('Ctrl Pts',(-56.3635142722379,-62.2656775410818,
-217.348845863301));
#190570=CARTESIAN_POINT('Ctrl Pts',(-56.4063229321979,-62.453644092428,
-217.612415918528));
#190571=CARTESIAN_POINT('Ctrl Pts',(-56.6726055091992,-62.3181114609455,
-217.093587076475));
#190572=CARTESIAN_POINT('Ctrl Pts',(-56.3642389105003,-62.4681884271343,
-217.222073078002));
#190573=CARTESIAN_POINT('Ctrl Pts',(-56.4530481014242,-62.6707334235198,
-217.513854009698));
#190574=CARTESIAN_POINT('',(-56.6309943627598,-62.1341374253209,-217.237388612086));
#190575=CARTESIAN_POINT('',(-56.4090189474477,-62.4870630585556,-217.60005));
#190576=CARTESIAN_POINT('Origin',(-56.8921651292037,-62.3583394513399,-217.60005));
#190577=CARTESIAN_POINT('Ctrl Pts',(-56.6309943627598,-62.1341374253209,
-217.237388612086));
#190578=CARTESIAN_POINT('Ctrl Pts',(-56.6071938355743,-62.0458440727314,
-217.309112681226));
#190579=CARTESIAN_POINT('Ctrl Pts',(-56.578015172952,-61.9606625433887,
-217.382726354161));
#190580=CARTESIAN_POINT('Ctrl Pts',(-56.5424466867555,-61.8803805048941,
-217.457905536343));
#190581=CARTESIAN_POINT('Ctrl Pts',(-56.5174877480173,-61.8240453977575,
-217.510659892886));
#190582=CARTESIAN_POINT('Ctrl Pts',(-56.4893817115847,-61.7701241681472,
-217.564185112257));
#190583=CARTESIAN_POINT('Ctrl Pts',(-56.4577719221838,-61.7192435082347,
-217.618369210985));
#190584=CARTESIAN_POINT('Ctrl Pts',(-56.4144730234454,-61.6495474873803,
-217.692590262391));
#190585=CARTESIAN_POINT('Ctrl Pts',(-56.364065657814,-61.5845363129302,
-217.76906264081));
#190586=CARTESIAN_POINT('Ctrl Pts',(-56.3050972761405,-61.5293160073526,
-217.845728184291));
#190587=CARTESIAN_POINT('Ctrl Pts',(-56.2596681710779,-61.4867744114587,
-217.904791141942));
#190588=CARTESIAN_POINT('Ctrl Pts',(-56.2091562799757,-61.4500471971335,
-217.963968745491));
#190589=CARTESIAN_POINT('Ctrl Pts',(-56.1528857709326,-61.42145819393,-218.022319919453));
#190590=CARTESIAN_POINT('Ctrl Pts',(-56.10949285456,-61.3994118281464,-218.067317337372));
#190591=CARTESIAN_POINT('Ctrl Pts',(-56.0625109582255,-61.3824132905256,
-218.111814382599));
#190592=CARTESIAN_POINT('Ctrl Pts',(-56.0123938152309,-61.3722265064741,
-218.154382249795));
#190593=CARTESIAN_POINT('Ctrl Pts',(-55.9878361395995,-61.3672349262779,
-218.175240738776));
#190594=CARTESIAN_POINT('Ctrl Pts',(-55.9625258661404,-61.3638782470511,
-218.195636021717));
#190595=CARTESIAN_POINT('Ctrl Pts',(-55.9365178644268,-61.3623594488966,
-218.215399995439));
#190596=CARTESIAN_POINT('Ctrl Pts',(-55.8847053173817,-61.3593337338995,
-218.254773332519));
#190597=CARTESIAN_POINT('Ctrl Pts',(-55.8310846986675,-61.3636853719657,
-218.290894690184));
#190598=CARTESIAN_POINT('Ctrl Pts',(-55.77644267487,-61.3757084773317,-218.322977700074));
#190599=CARTESIAN_POINT('Ctrl Pts',(-55.7476809181567,-61.38203704292,-218.339865136904));
#190600=CARTESIAN_POINT('Ctrl Pts',(-55.7186365522078,-61.3904902984303,
-218.35563370025));
#190601=CARTESIAN_POINT('Ctrl Pts',(-55.6894269915266,-61.4011060019289,
-218.370168708992));
#190602=CARTESIAN_POINT('Ctrl Pts',(-55.6216481299243,-61.4257390426686,
-218.403896239396));
#190603=CARTESIAN_POINT('Ctrl Pts',(-55.5558942263105,-61.4610272231835,
-218.429484990556));
#190604=CARTESIAN_POINT('Ctrl Pts',(-55.4931147424837,-61.5039756163701,
-218.44805034278));
#190605=CARTESIAN_POINT('Ctrl Pts',(-55.4378792223867,-61.5417630700155,
-218.464384769625));
#190606=CARTESIAN_POINT('Ctrl Pts',(-55.384946788007,-61.5854798144667,
-218.475282328939));
#190607=CARTESIAN_POINT('Ctrl Pts',(-55.3349600132919,-61.6331274503392,
-218.481502690929));
#190608=CARTESIAN_POINT('Ctrl Pts',(-55.2997615967411,-61.6666787515517,
-218.485882787337));
#190609=CARTESIAN_POINT('Ctrl Pts',(-55.2660236404548,-61.7021800146365,
-218.487943771794));
#190610=CARTESIAN_POINT('Ctrl Pts',(-55.2339673727996,-61.7389489519143,
-218.487950878256));
#190611=CARTESIAN_POINT('Ctrl Pts',(-55.4938952567199,-61.9654919306031,
-218.35005));
#190612=CARTESIAN_POINT('Ctrl Pts',(-55.5605571120519,-61.8331100589488,
-218.35005));
#190613=CARTESIAN_POINT('Ctrl Pts',(-55.6462938793267,-61.7235284039374,
-218.33000081413));
#190614=CARTESIAN_POINT('Ctrl Pts',(-55.796657340851,-61.6580344229345,
-218.254184099553));
#190615=CARTESIAN_POINT('Ctrl Pts',(-55.8476827468257,-61.653839850603,
-218.222689657358));
#190616=CARTESIAN_POINT('Ctrl Pts',(-55.9478088686909,-61.6782199479451,
-218.150610277818));
#190617=CARTESIAN_POINT('Ctrl Pts',(-55.995486790882,-61.7063946791486,
-218.11106824763));
#190618=CARTESIAN_POINT('Ctrl Pts',(-56.1268157801208,-61.8214573400613,
-217.990439031765));
#190619=CARTESIAN_POINT('Ctrl Pts',(-56.1995158790201,-61.9371995248376,
-217.907396389637));
#190620=CARTESIAN_POINT('Ctrl Pts',(-56.3198707039344,-62.1930517563039,
-217.749765554285));
#190621=CARTESIAN_POINT('Ctrl Pts',(-56.3688914254939,-62.3364499780597,
-217.673255297864));
#190622=CARTESIAN_POINT('Ctrl Pts',(-56.4090189474477,-62.4870630585556,
-217.60005));
#190623=CARTESIAN_POINT('Ctrl Pts',(-49.2925903552098,-69.4989817480832,
-217.60005));
#190624=CARTESIAN_POINT('Ctrl Pts',(-49.0991171386076,-69.4468461963775,
-217.336253844649));
#190625=CARTESIAN_POINT('Ctrl Pts',(-48.9443109379934,-69.7210624363875,
-217.233400031701));
#190626=CARTESIAN_POINT('Ctrl Pts',(-49.479508186842,-69.5493508092223,
-217.453006109745));
#190627=CARTESIAN_POINT('Ctrl Pts',(-49.2856293770243,-69.4971059616069,
-217.188797196021));
#190628=CARTESIAN_POINT('Ctrl Pts',(-49.130620489061,-69.7720396651474,
-217.086285690494));
#190629=CARTESIAN_POINT('Ctrl Pts',(-49.6662875276291,-69.5996825510014,
-217.305773775928));
#190630=CARTESIAN_POINT('Ctrl Pts',(-49.4718979894171,-69.5473000765824,
-217.041226996676));
#190631=CARTESIAN_POINT('Ctrl Pts',(-49.3167847015304,-69.8229858522605,
-216.938985563531));
#190632=CARTESIAN_POINT('Ctrl Pts',(-49.8529236261983,-69.6499756930601,
-217.158346534073));
#190633=CARTESIAN_POINT('Ctrl Pts',(-49.6579114178628,-69.5974254266744,
-216.893543128263));
#190634=CARTESIAN_POINT('Ctrl Pts',(-49.502798597092,-69.8738997057058,
-216.791493525167));
#190635=CARTESIAN_POINT('',(-49.8529236261983,-69.6499756930601,-217.158346534073));
#190636=CARTESIAN_POINT('',(-49.5029651331548,-69.874078287392,-216.790767750036));
#190637=CARTESIAN_POINT('Origin',(-49.7228284492359,-70.13275436381,-217.158346534073));
#190638=CARTESIAN_POINT('Origin',(165.63543440526,-11.5819668880935,75.4526175248521));
#190639=CARTESIAN_POINT('Origin',(167.970418940429,-23.6135530814242,73.4534718919959));
#190640=CARTESIAN_POINT('Ctrl Pts',(-56.5555093174817,-63.0368943169927,
-217.153871927429));
#190641=CARTESIAN_POINT('Ctrl Pts',(-56.5025836743465,-62.8382452661243,
-216.892152466627));
#190642=CARTESIAN_POINT('Ctrl Pts',(-56.7788252534563,-62.6825329319095,
-216.79113809033));
#190643=CARTESIAN_POINT('Ctrl Pts',(-56.5067115045409,-62.8537385034605,
-217.302758005793));
#190644=CARTESIAN_POINT('Ctrl Pts',(-56.4539126170321,-62.6555652121921,
-217.041204177849));
#190645=CARTESIAN_POINT('Ctrl Pts',(-56.7295803718938,-62.4998572980931,
-216.940045714159));
#190646=CARTESIAN_POINT('Ctrl Pts',(-56.4578811804683,-62.6704606639105,
-217.451483035533));
#190647=CARTESIAN_POINT('Ctrl Pts',(-56.4051889499832,-62.4726876949562,
-217.190156301151));
#190648=CARTESIAN_POINT('Ctrl Pts',(-56.680302877991,-62.3170582944071,
-217.088794981881));
#190649=CARTESIAN_POINT('Ctrl Pts',(-56.4090189474476,-62.4870630585555,
-217.60005));
#190650=CARTESIAN_POINT('Ctrl Pts',(-56.3564132949791,-62.2896150482124,
-217.339009989763));
#190651=CARTESIAN_POINT('Ctrl Pts',(-56.6309943627598,-62.1341374253209,
-217.237388612086));
#190652=CARTESIAN_POINT('',(-56.7789312838428,-62.6826300027679,-216.790395777257));
#190653=CARTESIAN_POINT('',(-56.5555093174817,-63.0368943169928,-217.153871927429));
#190654=CARTESIAN_POINT('Origin',(-57.0386554992377,-62.9081707097771,-217.153871927429));
#190655=CARTESIAN_POINT('Origin',(10.1481943050527,195.398995247496,121.950798030302));
#190656=CARTESIAN_POINT('Origin',(11.7909588194732,193.492081547376,120.824020637011));
#190657=CARTESIAN_POINT('Ctrl Pts',(-49.8082839038352,-69.6379465523126,
-217.193274451484));
#190658=CARTESIAN_POINT('Ctrl Pts',(-49.6148311193225,-69.5858165064744,
-216.925438823195));
#190659=CARTESIAN_POINT('Ctrl Pts',(-49.4605536752757,-69.8644275978415,
-216.823211012323));
#190660=CARTESIAN_POINT('Ctrl Pts',(-50.2515020504862,-69.7573812885902,
-216.849764285521));
#190661=CARTESIAN_POINT('Ctrl Pts',(-50.0368968810474,-69.6995512741769,
-216.615769374028));
#190662=CARTESIAN_POINT('Ctrl Pts',(-49.8798577876633,-69.9587340309451,
-216.511180111009));
#190663=CARTESIAN_POINT('Ctrl Pts',(-50.6419967392048,-69.8626085463579,
-216.450334359214));
#190664=CARTESIAN_POINT('Ctrl Pts',(-50.4172229593767,-69.8020383794606,
-216.246268361137));
#190665=CARTESIAN_POINT('Ctrl Pts',(-50.2489216341879,-70.0420065040121,
-216.148268825924));
#190666=CARTESIAN_POINT('Ctrl Pts',(-50.9693220996876,-69.9508134594501,
-215.987095704752));
#190667=CARTESIAN_POINT('Ctrl Pts',(-50.7368031033667,-69.8881561760894,
-215.810948949264));
#190668=CARTESIAN_POINT('Ctrl Pts',(-50.558073933031,-70.1119355639638,
-215.727306267195));
#190669=CARTESIAN_POINT('',(-50.9355365677156,-69.9417092155658,-216.034373717099));
#190670=CARTESIAN_POINT('',(-50.5260956696589,-70.1045979817023,-215.770197056231));
#190671=CARTESIAN_POINT('Origin',(-50.8054413907531,-70.4244878863158,-216.034373717099));
#190672=CARTESIAN_POINT('Ctrl Pts',(-50.9355365677156,-69.9417092155658,
-216.034373717099));
#190673=CARTESIAN_POINT('Ctrl Pts',(-50.8116343558523,-69.9083210790241,
-216.205819948822));
#190674=CARTESIAN_POINT('Ctrl Pts',(-50.6790456275845,-69.8725921723588,
-216.368291840782));
#190675=CARTESIAN_POINT('Ctrl Pts',(-50.5382668565241,-69.8346562811456,
-216.522302092547));
#190676=CARTESIAN_POINT('Ctrl Pts',(-50.3916404967027,-69.7951446303954,
-216.682709534816));
#190677=CARTESIAN_POINT('Ctrl Pts',(-50.2361294127355,-69.7532387981495,
-216.83393773326));
#190678=CARTESIAN_POINT('Ctrl Pts',(-50.0722553986644,-69.7090793931224,
-216.976525935756));
#190679=CARTESIAN_POINT('Ctrl Pts',(-50.0007248884689,-69.689803946741,
-217.038765253748));
#190680=CARTESIAN_POINT('Ctrl Pts',(-49.9276005183846,-69.6700990002661,
-217.099357901493));
#190681=CARTESIAN_POINT('Ctrl Pts',(-49.8529236261983,-69.6499756930601,
-217.158346534073));
#190682=CARTESIAN_POINT('Ctrl Pts',(-49.5030054850469,-69.8741215579534,
-216.790591893832));
#190683=CARTESIAN_POINT('Ctrl Pts',(-49.6024122858318,-69.8963860707776,
-216.715257484827));
#190684=CARTESIAN_POINT('Ctrl Pts',(-49.6989189612008,-69.9180032597767,
-216.636941400134));
#190685=CARTESIAN_POINT('Ctrl Pts',(-49.7924273507199,-69.9389873829446,
-216.555586604588));
#190686=CARTESIAN_POINT('Ctrl Pts',(-49.8839999749823,-69.9595371029881,
-216.4759159765));
#190687=CARTESIAN_POINT('Ctrl Pts',(-49.9726976882578,-69.9794801981767,
-216.39333040445));
#190688=CARTESIAN_POINT('Ctrl Pts',(-50.0584047953187,-69.9987982846587,
-216.307747992276));
#190689=CARTESIAN_POINT('Ctrl Pts',(-50.1422610001375,-70.0176991841558,
-216.224013789476));
#190690=CARTESIAN_POINT('Ctrl Pts',(-50.2232547532238,-70.0360021258001,
-216.137409962399));
#190691=CARTESIAN_POINT('Ctrl Pts',(-50.3012483834477,-70.053652984946,
-216.047843888945));
#190692=CARTESIAN_POINT('Ctrl Pts',(-50.3792420136716,-70.0713038440919,
-215.958277815491));
#190693=CARTESIAN_POINT('Ctrl Pts',(-50.4542359145046,-70.088302998853,
-215.865748569618));
#190694=CARTESIAN_POINT('Ctrl Pts',(-50.5260568508924,-70.1045534073545,
-215.770160360593));
#190695=CARTESIAN_POINT('Ctrl Pts',(-56.8374074136193,-64.0949596691002,
-216.027524728913));
#190696=CARTESIAN_POINT('Ctrl Pts',(-56.7751359198338,-63.8612322658189,
-215.850745835606));
#190697=CARTESIAN_POINT('Ctrl Pts',(-57.0010400290729,-63.6829857423181,
-215.767369567569));
#190698=CARTESIAN_POINT('Ctrl Pts',(-56.7544062418932,-63.7834262987405,
-216.468486417733));
#190699=CARTESIAN_POINT('Ctrl Pts',(-56.6940755894548,-63.5569835739616,
-216.264965542136));
#190700=CARTESIAN_POINT('Ctrl Pts',(-56.9355417877511,-63.3885831929649,
-216.168198383641));
#190701=CARTESIAN_POINT('Ctrl Pts',(-56.6561228522777,-63.4145332460213,
-216.852342060961));
#190702=CARTESIAN_POINT('Ctrl Pts',(-56.5983764095674,-63.1977899935455,
-216.620143992135));
#190703=CARTESIAN_POINT('Ctrl Pts',(-56.8580526697591,-63.039825113586,
-216.517093115455));
#190704=CARTESIAN_POINT('Ctrl Pts',(-56.5449338627868,-62.9972008165799,
-217.185865065935));
#190705=CARTESIAN_POINT('Ctrl Pts',(-56.4923730636171,-62.7999211568584,
-216.921403846993));
#190706=CARTESIAN_POINT('Ctrl Pts',(-56.7705238988762,-62.644964025511,
-216.820205369791));
#190707=CARTESIAN_POINT('',(-56.9945525157696,-63.6542608153715,-215.805929292345));
#190708=CARTESIAN_POINT('',(-56.8293274051384,-64.0646324794683,-216.070020447202));
#190709=CARTESIAN_POINT('Origin',(-57.3124735868944,-63.9359088722526,-216.070020447202));
#190710=CARTESIAN_POINT('Ctrl Pts',(-56.9944699555911,-63.6541878226909,
-215.805860863005));
#190711=CARTESIAN_POINT('Ctrl Pts',(-56.9787502340432,-63.5835644531967,
-215.900063590448));
#190712=CARTESIAN_POINT('Ctrl Pts',(-56.9623149510134,-63.5098655678024,
-215.991340416441));
#190713=CARTESIAN_POINT('Ctrl Pts',(-56.9452529548364,-63.4332525162424,
-216.079782169333));
#190714=CARTESIAN_POINT('Ctrl Pts',(-56.9277954510961,-63.3548635270355,
-216.170274056442));
#190715=CARTESIAN_POINT('Ctrl Pts',(-56.9096816135882,-63.2734234339984,
-216.257798849252));
#190716=CARTESIAN_POINT('Ctrl Pts',(-56.8909632509908,-63.1890692673191,
-216.34244940172));
#190717=CARTESIAN_POINT('Ctrl Pts',(-56.8716003694178,-63.1018105805022,
-216.430014679612));
#190718=CARTESIAN_POINT('Ctrl Pts',(-56.8515902874278,-63.0114333079711,
-216.514505339738));
#190719=CARTESIAN_POINT('Ctrl Pts',(-56.8309486552413,-62.918056159024,
-216.596004588349));
#190720=CARTESIAN_POINT('Ctrl Pts',(-56.8140435960204,-62.8415822533479,
-216.662750745425));
#190721=CARTESIAN_POINT('Ctrl Pts',(-56.7967139865683,-62.7630954660381,
-216.727490258555));
#190722=CARTESIAN_POINT('Ctrl Pts',(-56.7789516318256,-62.6826486313538,
-216.790253322115));
#190723=CARTESIAN_POINT('Ctrl Pts',(-56.5555093174817,-63.0368943169928,
-217.153871927429));
#190724=CARTESIAN_POINT('Ctrl Pts',(-56.6017653589548,-63.2105099443376,
-217.012740999607));
#190725=CARTESIAN_POINT('Ctrl Pts',(-56.6457145720419,-63.3754672117225,
-216.862817131854));
#190726=CARTESIAN_POINT('Ctrl Pts',(-56.6872100613017,-63.53121476751,-216.703540565444));
#190727=CARTESIAN_POINT('Ctrl Pts',(-56.7270307212962,-63.6806760842605,
-216.550692675005));
#190728=CARTESIAN_POINT('Ctrl Pts',(-56.7645917777113,-63.8216562928037,
-216.389231897203));
#190729=CARTESIAN_POINT('Ctrl Pts',(-56.7997545451796,-63.9536348568741,
-216.218629552571));
#190730=CARTESIAN_POINT('Ctrl Pts',(-56.809809462033,-63.9913745907946,
-216.169845212947));
#190731=CARTESIAN_POINT('Ctrl Pts',(-56.8196682125201,-64.0283780415039,
-216.120313149196));
#190732=CARTESIAN_POINT('Ctrl Pts',(-56.8293274051384,-64.0646324794683,
-216.070020447202));
#190733=CARTESIAN_POINT('Ctrl Pts',(-51.8506358032468,-69.9286975854491,
-213.227536545097));
#190734=CARTESIAN_POINT('Ctrl Pts',(-51.9051927775541,-69.878934733823,
-213.231804164287));
#190735=CARTESIAN_POINT('Ctrl Pts',(-51.9718267086835,-69.8471376007481,
-213.236262748316));
#190736=CARTESIAN_POINT('Ctrl Pts',(-51.8365119911318,-69.9357794545355,
-213.472190089507));
#190737=CARTESIAN_POINT('Ctrl Pts',(-51.8922394802453,-69.8844506593677,
-213.488613551225));
#190738=CARTESIAN_POINT('Ctrl Pts',(-51.9608269631738,-69.8523865837487,
-213.505363447503));
#190739=CARTESIAN_POINT('Ctrl Pts',(-51.764852960797,-69.9722040426621,
-213.699187231714));
#190740=CARTESIAN_POINT('Ctrl Pts',(-51.8262156776006,-69.9127229374064,
-213.727945792467));
#190741=CARTESIAN_POINT('Ctrl Pts',(-51.9055967467288,-69.8788950207841,
-213.755167329611));
#190742=CARTESIAN_POINT('Ctrl Pts',(-51.5795633434493,-70.0451552734412,
-214.141675371395));
#190743=CARTESIAN_POINT('Ctrl Pts',(-51.6562512817975,-69.9633349698509,
-214.190606504019));
#190744=CARTESIAN_POINT('Ctrl Pts',(-51.7621689112058,-69.9305269210584,
-214.242088767328));
#190745=CARTESIAN_POINT('Ctrl Pts',(-51.4650229856105,-70.0818854461224,
-214.356506299955));
#190746=CARTESIAN_POINT('Ctrl Pts',(-51.5502085021597,-69.9858444846014,
-214.415523245079));
#190747=CARTESIAN_POINT('Ctrl Pts',(-51.6732637051828,-69.9557792147167,
-214.478511967556));
#190748=CARTESIAN_POINT('Ctrl Pts',(-51.0983339320408,-70.159079780817,
-214.982290817329));
#190749=CARTESIAN_POINT('Ctrl Pts',(-51.2098831872327,-70.0159755958657,
-215.071812476474));
#190750=CARTESIAN_POINT('Ctrl Pts',(-51.3873507266844,-70.0045324525619,
-215.167197191036));
#190751=CARTESIAN_POINT('Ctrl Pts',(-50.818061750232,-70.1707056698672,
-215.381706149951));
#190752=CARTESIAN_POINT('Ctrl Pts',(-50.9474626754076,-69.9829235319172,
-215.48727868552));
#190753=CARTESIAN_POINT('Ctrl Pts',(-51.16741865858,-70.0041948709461,-215.606559872798));
#190754=CARTESIAN_POINT('Ctrl Pts',(-50.5261810352842,-70.1046957156775,
-215.770277860521));
#190755=CARTESIAN_POINT('Ctrl Pts',(-50.704122433655,-69.8793496612892,
-215.854989245265));
#190756=CARTESIAN_POINT('Ctrl Pts',(-50.9355365677157,-69.9417092155658,
-216.034373717099));
#190757=CARTESIAN_POINT('',(-51.9718267086745,-69.8471376007524,-213.236262748316));
#190758=CARTESIAN_POINT('',(-51.8506358032439,-69.9286975854465,-213.227536545096));
#190759=CARTESIAN_POINT('Origin',(-52.1871615786983,-70.2983923998978,-213.236262748316));
#190760=CARTESIAN_POINT('Ctrl Pts',(-51.9718267086745,-69.8471376007524,
-213.236262748316));
#190761=CARTESIAN_POINT('Ctrl Pts',(-51.9608269631738,-69.8523865837487,
-213.505363447503));
#190762=CARTESIAN_POINT('Ctrl Pts',(-51.9055967467288,-69.8788950207841,
-213.755167329611));
#190763=CARTESIAN_POINT('Ctrl Pts',(-51.7621689112058,-69.9305269210584,
-214.242088767328));
#190764=CARTESIAN_POINT('Ctrl Pts',(-51.6732637051828,-69.9557792147167,
-214.478511967556));
#190765=CARTESIAN_POINT('Ctrl Pts',(-51.3873507266844,-70.0045324525619,
-215.167197191036));
#190766=CARTESIAN_POINT('Ctrl Pts',(-51.16741865858,-70.0041948709461,-215.606559872798));
#190767=CARTESIAN_POINT('Ctrl Pts',(-50.9355365677156,-69.9417092155658,
-216.034373717099));
#190768=CARTESIAN_POINT('Ctrl Pts',(-50.5261810442127,-70.1046957176967,
-215.770277848635));
#190769=CARTESIAN_POINT('Ctrl Pts',(-50.8180617559476,-70.1707056696301,
-215.381706141806));
#190770=CARTESIAN_POINT('Ctrl Pts',(-51.0983339345335,-70.1590797802923,
-214.982290813075));
#190771=CARTESIAN_POINT('Ctrl Pts',(-51.4650229856105,-70.0818854461224,
-214.356506299955));
#190772=CARTESIAN_POINT('Ctrl Pts',(-51.5795633434493,-70.0451552734412,
-214.141675371395));
#190773=CARTESIAN_POINT('Ctrl Pts',(-51.764852960797,-69.9722040426621,
-213.699187231714));
#190774=CARTESIAN_POINT('Ctrl Pts',(-51.8365119911318,-69.9357794545355,
-213.472190089507));
#190775=CARTESIAN_POINT('Ctrl Pts',(-51.8506358032439,-69.9286975854465,
-213.227536545096));
#190776=CARTESIAN_POINT('Ctrl Pts',(-56.9946437140725,-63.654341638523,
-215.806005173342));
#190777=CARTESIAN_POINT('Ctrl Pts',(-56.7673159108321,-63.831880948128,
-215.890327243741));
#190778=CARTESIAN_POINT('Ctrl Pts',(-56.8293274051384,-64.0646324794683,
-216.070020447202));
#190779=CARTESIAN_POINT('Ctrl Pts',(-57.0593493067881,-63.9452064704916,
-215.417908776751));
#190780=CARTESIAN_POINT('Ctrl Pts',(-56.8699337341761,-64.0745035962365,
-215.52327792109));
#190781=CARTESIAN_POINT('Ctrl Pts',(-56.8908615653413,-64.2955924035464,
-215.642832329437));
#190782=CARTESIAN_POINT('Ctrl Pts',(-57.0473852485484,-64.223762372941,
-215.01984571743));
#190783=CARTESIAN_POINT('Ctrl Pts',(-56.9027383376601,-64.3353675625261,
-215.109528851524));
#190784=CARTESIAN_POINT('Ctrl Pts',(-56.8910066584284,-64.5140548708215,
-215.205129354443));
#190785=CARTESIAN_POINT('Ctrl Pts',(-56.9693188990643,-64.5910795515543,
-214.391115626198));
#190786=CARTESIAN_POINT('Ctrl Pts',(-56.8722601349262,-64.6764145103723,
-214.450264068639));
#190787=CARTESIAN_POINT('Ctrl Pts',(-56.8418253372028,-64.8002473979207,
-214.513441216471));
#190788=CARTESIAN_POINT('Ctrl Pts',(-56.9323676074197,-64.7055133030553,
-214.175785907962));
#190789=CARTESIAN_POINT('Ctrl Pts',(-56.8496536435939,-64.782388944382,
-214.224865863035));
#190790=CARTESIAN_POINT('Ctrl Pts',(-56.8164834138299,-64.8889909543264,
-214.276550655991));
#190791=CARTESIAN_POINT('Ctrl Pts',(-56.858924334145,-64.8909827727899,
-213.732482787358));
#190792=CARTESIAN_POINT('Ctrl Pts',(-56.7988096612268,-64.9525255862112,
-213.761447447143));
#190793=CARTESIAN_POINT('Ctrl Pts',(-56.7646526681549,-65.0323886578414,
-213.78887047881));
#190794=CARTESIAN_POINT('Ctrl Pts',(-56.8216885415319,-64.9639058228799,
-213.501324323514));
#190795=CARTESIAN_POINT('Ctrl Pts',(-56.7699730410421,-65.019697176522,
-213.517778991486));
#190796=CARTESIAN_POINT('Ctrl Pts',(-56.7376407413534,-65.088500914211,
-213.534553551187));
#190797=CARTESIAN_POINT('Ctrl Pts',(-56.8144552965912,-64.9781464054153,
-213.256094899171));
#190798=CARTESIAN_POINT('Ctrl Pts',(-56.7643939904929,-65.0327211703679,
-213.2603619646));
#190799=CARTESIAN_POINT('Ctrl Pts',(-56.7323722878852,-65.0994854859681,
-213.26482110239));
#190800=CARTESIAN_POINT('',(-56.8144552965909,-64.9781464054155,-213.256094899172));
#190801=CARTESIAN_POINT('',(-56.7323722878851,-65.0994854859682,-213.264821102391));
#190802=CARTESIAN_POINT('Origin',(-57.1832000972235,-65.315712880919,-213.264821102391));
#190803=CARTESIAN_POINT('Ctrl Pts',(-56.8144552965909,-64.9781464054155,
-213.256094899172));
#190804=CARTESIAN_POINT('Ctrl Pts',(-56.8216885415319,-64.9639058228799,
-213.501324323514));
#190805=CARTESIAN_POINT('Ctrl Pts',(-56.858924334145,-64.8909827727899,
-213.732482787358));
#190806=CARTESIAN_POINT('Ctrl Pts',(-56.9323676074197,-64.7055133030553,
-214.175785907962));
#190807=CARTESIAN_POINT('Ctrl Pts',(-56.9693188990643,-64.5910795515543,
-214.391115626198));
#190808=CARTESIAN_POINT('Ctrl Pts',(-57.0473852477809,-64.2237623765521,
-215.019845711248));
#190809=CARTESIAN_POINT('Ctrl Pts',(-57.0593493064353,-63.9452064787071,
-215.417908765011));
#190810=CARTESIAN_POINT('Ctrl Pts',(-56.9946437169351,-63.6543416513909,
-215.806005156172));
#190811=CARTESIAN_POINT('Ctrl Pts',(-56.8293274051384,-64.0646324794683,
-216.070020447202));
#190812=CARTESIAN_POINT('Ctrl Pts',(-56.8908615653413,-64.2955924035464,
-215.642832329437));
#190813=CARTESIAN_POINT('Ctrl Pts',(-56.8910066584284,-64.5140548708215,
-215.205129354443));
#190814=CARTESIAN_POINT('Ctrl Pts',(-56.8418253372028,-64.8002473979207,
-214.513441216471));
#190815=CARTESIAN_POINT('Ctrl Pts',(-56.8164834138299,-64.8889909543264,
-214.276550655991));
#190816=CARTESIAN_POINT('Ctrl Pts',(-56.7646526681549,-65.0323886578414,
-213.78887047881));
#190817=CARTESIAN_POINT('Ctrl Pts',(-56.7376407413534,-65.088500914211,
-213.534553551187));
#190818=CARTESIAN_POINT('Ctrl Pts',(-56.7323722878851,-65.0994854859682,
-213.264821102391));
#190819=CARTESIAN_POINT('Ctrl Pts',(-51.9513667677563,-69.856765622058,
-213.744232219612));
#190820=CARTESIAN_POINT('Ctrl Pts',(-51.8804433982802,-69.8893245968629,
-213.7397430898));
#190821=CARTESIAN_POINT('Ctrl Pts',(-51.8228503443836,-69.941996586685,
-213.735470748631));
#190822=CARTESIAN_POINT('Ctrl Pts',(-51.991780071228,-69.8379778346573,
-212.728235356937));
#190823=CARTESIAN_POINT('Ctrl Pts',(-51.92847890016,-69.8695011096845,-212.726011510236));
#190824=CARTESIAN_POINT('Ctrl Pts',(-51.8765276514693,-69.9171366797835,
-212.719415019637));
#190825=CARTESIAN_POINT('Ctrl Pts',(-52.0346456619607,-69.816925009228,
-211.71249177384));
#190826=CARTESIAN_POINT('Ctrl Pts',(-51.9794687356775,-69.8470038946562,
-211.710263762613));
#190827=CARTESIAN_POINT('Ctrl Pts',(-51.9334544096019,-69.8892734758674,
-211.703692143478));
#190828=CARTESIAN_POINT('Ctrl Pts',(-52.1138191538044,-69.7700067918124,
-210.276283653453));
#190829=CARTESIAN_POINT('Ctrl Pts',(-52.0734597321496,-69.7950116391772,
-210.272241986443));
#190830=CARTESIAN_POINT('Ctrl Pts',(-52.0385712075063,-69.827125844513,
-210.267504272468));
#190831=CARTESIAN_POINT('Ctrl Pts',(-52.1391384959575,-69.7543237267294,
-209.854167521602));
#190832=CARTESIAN_POINT('Ctrl Pts',(-52.1034382988765,-69.7775433560356,
-209.850130119974));
#190833=CARTESIAN_POINT('Ctrl Pts',(-52.0721853887123,-69.8063480382507,
-209.845388043713));
#190834=CARTESIAN_POINT('Ctrl Pts',(-52.1868109938527,-69.7218145199576,
-209.222414495584));
#190835=CARTESIAN_POINT('Ctrl Pts',(-52.1597481032178,-69.740831362429,
-209.21810272547));
#190836=CARTESIAN_POINT('Ctrl Pts',(-52.1354652353082,-69.7632628363318,
-209.213638050098));
#190837=CARTESIAN_POINT('Ctrl Pts',(-52.2041584674497,-69.7096301545639,
-209.011927312326));
#190838=CARTESIAN_POINT('Ctrl Pts',(-52.1802056110659,-69.7270298301123,
-209.007617928732));
#190839=CARTESIAN_POINT('Ctrl Pts',(-52.158491006019,-69.7471128108018,
-209.003150816985));
#190840=CARTESIAN_POINT('Ctrl Pts',(-52.2371408246248,-69.6848794419398,
-208.698381586053));
#190841=CARTESIAN_POINT('Ctrl Pts',(-52.2190101918289,-69.6987724358088,
-208.694007820048));
#190842=CARTESIAN_POINT('Ctrl Pts',(-52.2022638893194,-69.714299255283,
-208.689605786204));
#190843=CARTESIAN_POINT('Ctrl Pts',(-52.249174245292,-69.6756642254024,
-208.594104390417));
#190844=CARTESIAN_POINT('Ctrl Pts',(-52.2331514504352,-69.6882319207143,
-208.589731796556));
#190845=CARTESIAN_POINT('Ctrl Pts',(-52.2182336078508,-69.7020812266944,
-208.585328566142));
#190846=CARTESIAN_POINT('Ctrl Pts',(-52.2723150773139,-69.6570951860835,
-208.439912289689));
#190847=CARTESIAN_POINT('Ctrl Pts',(-52.2602903339987,-69.6668890135686,
-208.435525620945));
#190848=CARTESIAN_POINT('Ctrl Pts',(-52.2489412320906,-69.677457827406,
-208.431136608511));
#190849=CARTESIAN_POINT('Ctrl Pts',(-52.2807846875617,-69.6502015352889,
-208.388797146169));
#190850=CARTESIAN_POINT('Ctrl Pts',(-52.270214924355,-69.6589558945369,
-208.384411029018));
#190851=CARTESIAN_POINT('Ctrl Pts',(-52.26018000973,-69.6683161240624,-208.380021453291));
#190852=CARTESIAN_POINT('Ctrl Pts',(-52.2972292893049,-69.6363602565428,
-208.314505613017));
#190853=CARTESIAN_POINT('Ctrl Pts',(-52.2894520983595,-69.6429772988715,
-208.310116951883));
#190854=CARTESIAN_POINT('Ctrl Pts',(-52.281999678196,-69.6499593019997,
-208.305729941084));
#190855=CARTESIAN_POINT('Ctrl Pts',(-52.3032976103578,-69.6311990926332,
-208.290014406272));
#190856=CARTESIAN_POINT('Ctrl Pts',(-52.2965464863421,-69.6370140514492,
-208.285625985819));
#190857=CARTESIAN_POINT('Ctrl Pts',(-52.2900513245555,-69.6431141725604,
-208.281238728998));
#190858=CARTESIAN_POINT('Ctrl Pts',(-52.3149497431651,-69.6210491476294,
-208.256089330814));
#190859=CARTESIAN_POINT('Ctrl Pts',(-52.3101508205055,-69.6252622995574,
-208.251700725001));
#190860=CARTESIAN_POINT('Ctrl Pts',(-52.3055109262684,-69.6296515882696,
-208.24731365204));
#190861=CARTESIAN_POINT('Ctrl Pts',(-52.3192905030199,-69.6172377131638,
-208.245104578722));
#190862=CARTESIAN_POINT('Ctrl Pts',(-52.3152163853501,-69.6208465529984,
-208.24071608881));
#190863=CARTESIAN_POINT('Ctrl Pts',(-52.3112700002316,-69.624596121335,
-208.236328897454));
#190864=CARTESIAN_POINT('Ctrl Pts',(-52.3980737175552,-69.546924914442,
-208.107889777235));
#190865=CARTESIAN_POINT('Ctrl Pts',(-52.4070413724991,-69.5392973207823,
-208.103538654047));
#190866=CARTESIAN_POINT('Ctrl Pts',(-52.4157911999454,-69.5313285632377,
-208.099113657561));
#190867=CARTESIAN_POINT('Ctrl Pts',(-52.6906841717837,-69.273483049227,
-208.269888341076));
#190868=CARTESIAN_POINT('Ctrl Pts',(-52.7473775130203,-69.2207759621715,
-208.265385690945));
#190869=CARTESIAN_POINT('Ctrl Pts',(-52.8039539674267,-69.1685749088725,
-208.261113958564));
#190870=CARTESIAN_POINT('Ctrl Pts',(-53.1203834433686,-68.5685596498648,
-225.080427005024));
#190871=CARTESIAN_POINT('Ctrl Pts',(-53.2526829041072,-68.3309162879946,
-225.681318331167));
#190872=CARTESIAN_POINT('Ctrl Pts',(-53.3726051882034,-68.2329805102018,
-225.065027635246));
#190873=CARTESIAN_POINT('',(-52.3440043138885,-69.594874440935,-208.218811515427));
#190874=CARTESIAN_POINT('',(-52.3440560052495,-69.5949303622595,-208.210085312208));
#190875=CARTESIAN_POINT('Origin',(-52.6833983856504,-69.9620415201413,-208.218811515427));
#190876=CARTESIAN_POINT('Ctrl Pts',(-52.3440043138885,-69.594874440935,
-208.218811515427));
#190877=CARTESIAN_POINT('Ctrl Pts',(-52.3364108319347,-69.6018935417895,
-208.21881325288));
#190878=CARTESIAN_POINT('Ctrl Pts',(-52.3299368833625,-69.6077359836068,
-208.22656203798));
#190879=CARTESIAN_POINT('Ctrl Pts',(-52.3192905030199,-69.6172377131638,
-208.245104578722));
#190880=CARTESIAN_POINT('Ctrl Pts',(-52.3149497431651,-69.6210491476294,
-208.256089330814));
#190881=CARTESIAN_POINT('Ctrl Pts',(-52.3032976103578,-69.6311990926332,
-208.290014406272));
#190882=CARTESIAN_POINT('Ctrl Pts',(-52.2972292893049,-69.6363602565428,
-208.314505613017));
#190883=CARTESIAN_POINT('Ctrl Pts',(-52.2807846875617,-69.6502015352889,
-208.388797146169));
#190884=CARTESIAN_POINT('Ctrl Pts',(-52.2723150773139,-69.6570951860835,
-208.439912289689));
#190885=CARTESIAN_POINT('Ctrl Pts',(-52.249174245292,-69.6756642254024,
-208.594104390417));
#190886=CARTESIAN_POINT('Ctrl Pts',(-52.2371408246248,-69.6848794419398,
-208.698381586053));
#190887=CARTESIAN_POINT('Ctrl Pts',(-52.2041584674497,-69.7096301545639,
-209.011927312326));
#190888=CARTESIAN_POINT('Ctrl Pts',(-52.1868109938527,-69.7218145199576,
-209.222414495584));
#190889=CARTESIAN_POINT('Ctrl Pts',(-52.1391384959575,-69.7543237267294,
-209.854167521602));
#190890=CARTESIAN_POINT('Ctrl Pts',(-52.1138191538044,-69.7700067918124,
-210.276283653453));
#190891=CARTESIAN_POINT('Ctrl Pts',(-52.0439601904129,-69.8114052189438,
-211.543526112619));
#190892=CARTESIAN_POINT('Ctrl Pts',(-52.0064303120272,-69.8306250618399,
-212.389708318565));
#190893=CARTESIAN_POINT('Ctrl Pts',(-51.9718267086745,-69.8471376007524,
-213.236262748316));
#190894=CARTESIAN_POINT('Ctrl Pts',(-51.8506358032439,-69.9286975854465,
-213.227536545096));
#190895=CARTESIAN_POINT('Ctrl Pts',(-51.8965359306666,-69.9068955059224,
-212.381067577369));
#190896=CARTESIAN_POINT('Ctrl Pts',(-51.9463091177219,-69.8815088904097,
-211.535021517202));
#190897=CARTESIAN_POINT('Ctrl Pts',(-52.0389353307874,-69.8267824525318,
-210.267914982609));
#190898=CARTESIAN_POINT('Ctrl Pts',(-52.0725035102325,-69.806045505995,
-209.8458402758));
#190899=CARTESIAN_POINT('Ctrl Pts',(-52.1356910661391,-69.7630436587203,
-209.214130441658));
#190900=CARTESIAN_POINT('Ctrl Pts',(-52.1586824184498,-69.7469248062077,
-209.003656181328));
#190901=CARTESIAN_POINT('Ctrl Pts',(-52.2023855392512,-69.7141755312691,
-208.690099641439));
#190902=CARTESIAN_POINT('Ctrl Pts',(-52.2183291852341,-69.7019815954277,
-208.585816112664));
#190903=CARTESIAN_POINT('Ctrl Pts',(-52.2489833267826,-69.6774084341258,
-208.431581516949));
#190904=CARTESIAN_POINT('Ctrl Pts',(-52.2602021616247,-69.6682855321809,
-208.380448072074));
#190905=CARTESIAN_POINT('Ctrl Pts',(-52.2819812944307,-69.6499675527577,
-208.306095531171));
#190906=CARTESIAN_POINT('Ctrl Pts',(-52.2900177211888,-69.6431370963428,
-208.281577994998));
#190907=CARTESIAN_POINT('Ctrl Pts',(-52.3054538148208,-69.6296980513237,
-208.247576563664));
#190908=CARTESIAN_POINT('Ctrl Pts',(-52.3112042959167,-69.6246512725098,
-208.236560595082));
#190909=CARTESIAN_POINT('Ctrl Pts',(-52.3253253083163,-69.6120530454534,
-208.217923065672));
#190910=CARTESIAN_POINT('Ctrl Pts',(-52.3341567138414,-69.6040808580668,
-208.210085312176));
#190911=CARTESIAN_POINT('Ctrl Pts',(-52.3440560052495,-69.5949303622595,
-208.210085312208));
#190912=CARTESIAN_POINT('Ctrl Pts',(-56.478494115784,-65.4721095684411,
-208.218811515427));
#190913=CARTESIAN_POINT('Ctrl Pts',(-56.4784941157842,-65.4721095684412,
-208.214448081532));
#190914=CARTESIAN_POINT('Ctrl Pts',(-56.4785498900846,-65.4721614184049,
-208.210085312209));
#190915=CARTESIAN_POINT('Ctrl Pts',(-56.4856347339016,-65.464428502687,
-208.218813480809));
#190916=CARTESIAN_POINT('Ctrl Pts',(-56.4867940706151,-65.4631813685704,
-208.214450046893));
#190917=CARTESIAN_POINT('Ctrl Pts',(-56.4880093612199,-65.4619859436241,
-208.210087277606));
#190918=CARTESIAN_POINT('Ctrl Pts',(-56.4916787645948,-65.4577664915776,
-208.226946403507));
#190919=CARTESIAN_POINT('Ctrl Pts',(-56.4938064756652,-65.455425583918,
-208.222583010898));
#190920=CARTESIAN_POINT('Ctrl Pts',(-56.4960155064695,-65.4531598633657,
-208.218220200296));
#190921=CARTESIAN_POINT('Ctrl Pts',(-56.5012774655679,-65.4470659442998,
-208.245963459985));
#190922=CARTESIAN_POINT('Ctrl Pts',(-56.5049328760549,-65.4429598777431,
-208.241599714584));
#190923=CARTESIAN_POINT('Ctrl Pts',(-56.5087297972239,-65.4389829337676,
-208.237237256758));
#190924=CARTESIAN_POINT('Ctrl Pts',(-56.5051439252244,-65.4426842233343,
-208.257244986379));
#190925=CARTESIAN_POINT('Ctrl Pts',(-56.5094087292744,-65.4378503136699,
-208.25288112094));
#190926=CARTESIAN_POINT('Ctrl Pts',(-56.5138509238801,-65.4331773923495,
-208.248518783163));
#190927=CARTESIAN_POINT('Ctrl Pts',(-56.5153591918106,-65.4310145177164,
-208.291764410647));
#190928=CARTESIAN_POINT('Ctrl Pts',(-56.5212265334526,-65.4242355589788,
-208.287400749103));
#190929=CARTESIAN_POINT('Ctrl Pts',(-56.5273807159321,-65.4177153790657,
-208.283038207423));
#190930=CARTESIAN_POINT('Ctrl Pts',(-56.5204776688227,-65.4250252363654,
-208.316259455579));
#190931=CARTESIAN_POINT('Ctrl Pts',(-56.5271357114541,-65.4172387338904,
-208.311895535072));
#190932=CARTESIAN_POINT('Ctrl Pts',(-56.5341593626729,-65.4097792264604,
-208.307533252362));
#190933=CARTESIAN_POINT('Ctrl Pts',(-56.5343427956335,-65.4086346803882,
-208.391050209511));
#190934=CARTESIAN_POINT('Ctrl Pts',(-56.5431294167638,-65.3980791094533,
-208.386688866059));
#190935=CARTESIAN_POINT('Ctrl Pts',(-56.5525209588637,-65.3880602085305,
-208.38232400629));
#190936=CARTESIAN_POINT('Ctrl Pts',(-56.5412952751588,-65.4001361493426,
-208.442727536444));
#190937=CARTESIAN_POINT('Ctrl Pts',(-56.5511242891444,-65.3881281081246,
-208.438365624418));
#190938=CARTESIAN_POINT('Ctrl Pts',(-56.5617269524415,-65.3767978707557,
-208.434001333226));
#190939=CARTESIAN_POINT('Ctrl Pts',(-56.5599119337509,-65.3770518735271,
-208.597713229276));
#190940=CARTESIAN_POINT('Ctrl Pts',(-56.5725061054697,-65.3610757695375,
-208.59336548035));
#190941=CARTESIAN_POINT('Ctrl Pts',(-56.5863764886281,-65.3462052619613,
-208.588987026056));
#190942=CARTESIAN_POINT('Ctrl Pts',(-56.5691529780988,-65.365046299052,
-208.702360956951));
#190943=CARTESIAN_POINT('Ctrl Pts',(-56.5830688742296,-65.3469778303877,
-208.698012046015));
#190944=CARTESIAN_POINT('Ctrl Pts',(-56.5986098697023,-65.3302929526477,
-208.693634753733));
#190945=CARTESIAN_POINT('Ctrl Pts',(-56.594014810857,-65.3320840644752,
-209.017499153971));
#190946=CARTESIAN_POINT('Ctrl Pts',(-56.6114339742289,-65.3082260137793,
-209.013214961635));
#190947=CARTESIAN_POINT('Ctrl Pts',(-56.6315194173109,-65.2866023733443,
-209.008772950752));
#190948=CARTESIAN_POINT('Ctrl Pts',(-56.6062646503943,-65.3147324550994,
-209.229067091402));
#190949=CARTESIAN_POINT('Ctrl Pts',(-56.6253012100655,-65.2877789793426,
-209.224780476847));
#190950=CARTESIAN_POINT('Ctrl Pts',(-56.6477298291647,-65.2635998038976,
-209.220340888184));
#190951=CARTESIAN_POINT('Ctrl Pts',(-56.6389405444651,-65.2670590859439,
-209.863840624216));
#190952=CARTESIAN_POINT('Ctrl Pts',(-56.6621798760702,-65.2315103701136,
-209.859829541482));
#190953=CARTESIAN_POINT('Ctrl Pts',(-56.6909645146964,-65.2003964473429,
-209.855114420997));
#190954=CARTESIAN_POINT('Ctrl Pts',(-56.6547249564177,-65.2417076178786,
-210.288240216126));
#190955=CARTESIAN_POINT('Ctrl Pts',(-56.6797528213393,-65.2015162456806,
-210.284225552072));
#190956=CARTESIAN_POINT('Ctrl Pts',(-56.7118396592687,-65.1667799745591,
-210.279514012908));
#190957=CARTESIAN_POINT('Ctrl Pts',(-56.6963931899382,-65.1717493422662,
-211.562592707913));
#190958=CARTESIAN_POINT('Ctrl Pts',(-56.7258904584642,-65.1185576981398,
-211.559720606721));
#190959=CARTESIAN_POINT('Ctrl Pts',(-56.7669337250065,-65.0740063908786,
-211.553866504694));
#190960=CARTESIAN_POINT('Ctrl Pts',(-56.7157486990471,-65.1341451836486,
-212.413730817787));
#190961=CARTESIAN_POINT('Ctrl Pts',(-56.7467526277092,-65.0738827156515,
-212.410853939053));
#190962=CARTESIAN_POINT('Ctrl Pts',(-56.7925037337705,-65.0241267882654,
-212.404990365038));
#190963=CARTESIAN_POINT('Ctrl Pts',(-56.7323722878852,-65.0994854859681,
-213.264821102391));
#190964=CARTESIAN_POINT('Ctrl Pts',(-56.7643939904929,-65.0327211703679,
-213.2603619646));
#190965=CARTESIAN_POINT('Ctrl Pts',(-56.8144552965912,-64.9781464054152,
-213.256094899172));
#190966=CARTESIAN_POINT('',(-56.4785498900846,-65.4721614184049,-208.210085312208));
#190967=CARTESIAN_POINT('',(-56.478494115784,-65.4721095684411,-208.218811515426));
#190968=CARTESIAN_POINT('Origin',(-56.8446958677552,-65.8125449908831,-208.218811515427));
#190969=CARTESIAN_POINT('Ctrl Pts',(-56.4785498900846,-65.4721614184049,
-208.210085312209));
#190970=CARTESIAN_POINT('Ctrl Pts',(-56.4880134607985,-65.4619815336005,
-208.210087283952));
#190971=CARTESIAN_POINT('Ctrl Pts',(-56.4960210114868,-65.4531537245717,
-208.218228453105));
#190972=CARTESIAN_POINT('Ctrl Pts',(-56.5023726430475,-65.4460714077127,
-208.227728741309));
#190973=CARTESIAN_POINT('Ctrl Pts',(-56.5087366507261,-65.4389752909997,
-208.23724754077));
#190974=CARTESIAN_POINT('Ctrl Pts',(-56.513854727351,-65.433173044492,-208.248528534057));
#190975=CARTESIAN_POINT('Ctrl Pts',(-56.5183608448225,-65.4280233981992,
-208.260025266392));
#190976=CARTESIAN_POINT('Ctrl Pts',(-56.527384064744,-65.4177115518456,
-208.283046757708));
#190977=CARTESIAN_POINT('Ctrl Pts',(-56.5341620389057,-65.4097760673606,
-208.307543894395));
#190978=CARTESIAN_POINT('Ctrl Pts',(-56.5402792876314,-65.4025401997578,
-208.332463842479));
#190979=CARTESIAN_POINT('Ctrl Pts',(-56.5525225633485,-65.3880580810659,
-208.382339498829));
#190980=CARTESIAN_POINT('Ctrl Pts',(-56.5617281325892,-65.3767964110653,
-208.434008552021));
#190981=CARTESIAN_POINT('Ctrl Pts',(-56.5699429720804,-65.3666008613971,
-208.485663414341));
#190982=CARTESIAN_POINT('Ctrl Pts',(-56.5863768923929,-65.346204498088,
-208.588999808438));
#190983=CARTESIAN_POINT('Ctrl Pts',(-56.5986107835984,-65.3302917454577,
-208.693643261059));
#190984=CARTESIAN_POINT('Ctrl Pts',(-56.6095793668545,-65.3157298046138,
-208.79868090921));
#190985=CARTESIAN_POINT('Ctrl Pts',(-56.6315196526886,-65.2866017817001,
-209.008786076848));
#190986=CARTESIAN_POINT('Ctrl Pts',(-56.6477302855814,-65.2635991432574,
-209.220347327344));
#190987=CARTESIAN_POINT('Ctrl Pts',(-56.6621411615825,-65.2425322660162,
-209.431932106333));
#190988=CARTESIAN_POINT('Ctrl Pts',(-56.6909646006573,-65.200396045247,
-209.855126434415));
#190989=CARTESIAN_POINT('Ctrl Pts',(-56.7118400320305,-65.1667793523224,
-210.279522418803));
#190990=CARTESIAN_POINT('Ctrl Pts',(-56.7302042319515,-65.1358555723291,
-210.704298191087));
#190991=CARTESIAN_POINT('Ctrl Pts',(-56.7669339286709,-65.0740058285095,
-211.553879733264));
#190992=CARTESIAN_POINT('Ctrl Pts',(-56.7925011773325,-65.0241321427268,
-212.404891259688));
#190993=CARTESIAN_POINT('Ctrl Pts',(-56.8144552965909,-64.9781464054155,
-213.256094899172));
#190994=CARTESIAN_POINT('Ctrl Pts',(-56.7323722878851,-65.0994854859682,
-213.264821102391));
#190995=CARTESIAN_POINT('Ctrl Pts',(-56.7157486990471,-65.1341451836486,
-212.413730817787));
#190996=CARTESIAN_POINT('Ctrl Pts',(-56.6963931899382,-65.1717493422662,
-211.562592707913));
#190997=CARTESIAN_POINT('Ctrl Pts',(-56.6547249564177,-65.2417076178786,
-210.288240216126));
#190998=CARTESIAN_POINT('Ctrl Pts',(-56.6389405444651,-65.2670590859439,
-209.863840624216));
#190999=CARTESIAN_POINT('Ctrl Pts',(-56.6062646503943,-65.3147324550994,
-209.229067091402));
#191000=CARTESIAN_POINT('Ctrl Pts',(-56.594014810857,-65.3320840644752,
-209.017499153971));
#191001=CARTESIAN_POINT('Ctrl Pts',(-56.5691529780988,-65.365046299052,
-208.702360956951));
#191002=CARTESIAN_POINT('Ctrl Pts',(-56.5599119337509,-65.3770518735271,
-208.597713229276));
#191003=CARTESIAN_POINT('Ctrl Pts',(-56.5412952751588,-65.4001361493426,
-208.442727536444));
#191004=CARTESIAN_POINT('Ctrl Pts',(-56.5343427956335,-65.4086346803882,
-208.391050209511));
#191005=CARTESIAN_POINT('Ctrl Pts',(-56.5204776688227,-65.4250252363654,
-208.316259455579));
#191006=CARTESIAN_POINT('Ctrl Pts',(-56.5153591918106,-65.4310145177164,
-208.291764410647));
#191007=CARTESIAN_POINT('Ctrl Pts',(-56.5051439252244,-65.4426842233343,
-208.257244986379));
#191008=CARTESIAN_POINT('Ctrl Pts',(-56.5012774655679,-65.4470659442998,
-208.245963459985));
#191009=CARTESIAN_POINT('Ctrl Pts',(-56.4916787645948,-65.4577664915776,
-208.226946403507));
#191010=CARTESIAN_POINT('Ctrl Pts',(-56.4856347339016,-65.464428502687,
-208.218813480809));
#191011=CARTESIAN_POINT('Ctrl Pts',(-56.478494115784,-65.4721095684411,
-208.218811515426));
#191012=CARTESIAN_POINT('Origin',(0.,-12.9675000200281,-208.218811515427));
#191013=CARTESIAN_POINT('Origin',(0.,-12.9675000200281,-208.210085312208));
#191014=CARTESIAN_POINT('Origin',(0.,-12.9675000200281,-208.218811515427));
#191015=CARTESIAN_POINT('Ctrl Pts',(-56.6260312186758,39.26699791474,-213.932877779247));
#191016=CARTESIAN_POINT('Ctrl Pts',(-56.6591708158967,39.1947585157316,
-213.928380187744));
#191017=CARTESIAN_POINT('Ctrl Pts',(-56.7131249770401,39.136390603742,-213.924107582135));
#191018=CARTESIAN_POINT('Ctrl Pts',(-56.6069323298669,39.308101280162,-212.882516880404));
#191019=CARTESIAN_POINT('Ctrl Pts',(-56.6390541381501,39.2436411705138,
-212.880445101553));
#191020=CARTESIAN_POINT('Ctrl Pts',(-56.6878438485494,39.1909973438446,
-212.873680972192));
#191021=CARTESIAN_POINT('Ctrl Pts',(-56.5855128843193,39.3516918804354,
-211.83240628728));
#191022=CARTESIAN_POINT('Ctrl Pts',(-56.6161967667701,39.2955248737877,
-211.830328584023));
#191023=CARTESIAN_POINT('Ctrl Pts',(-56.6594850052376,39.248900569515,-211.823591080281));
#191024=CARTESIAN_POINT('Ctrl Pts',(-56.5376887518409,39.4321195627096,
-210.347455422068));
#191025=CARTESIAN_POINT('Ctrl Pts',(-56.5632284029527,39.3910644172893,
-210.343434951173));
#191026=CARTESIAN_POINT('Ctrl Pts',(-56.5961170971406,39.3557075607436,
-210.338665903179));
#191027=CARTESIAN_POINT('Ctrl Pts',(-56.5216963051399,39.4578331766847,
-209.910997266658));
#191028=CARTESIAN_POINT('Ctrl Pts',(-56.5454235880735,39.4215267027753,
-209.906981158345));
#191029=CARTESIAN_POINT('Ctrl Pts',(-56.5749226987295,39.3898533622913,
-209.90220762928));
#191030=CARTESIAN_POINT('Ctrl Pts',(-56.4885248990568,39.506210827646,-209.257701934938));
#191031=CARTESIAN_POINT('Ctrl Pts',(-56.5079716151444,39.4786993973283,
-209.253391637796));
#191032=CARTESIAN_POINT('Ctrl Pts',(-56.5309467959293,39.4540847109594,
-209.24891615073));
#191033=CARTESIAN_POINT('Ctrl Pts',(-56.4760962345234,39.5238015154724,
-209.040146260381));
#191034=CARTESIAN_POINT('Ctrl Pts',(-56.4938957981811,39.4994537797928,
-209.035838362477));
#191035=CARTESIAN_POINT('Ctrl Pts',(-56.5144681134185,39.4774389991119,
-209.031360415952));
#191036=CARTESIAN_POINT('Ctrl Pts',(-56.4508419233835,39.557225742165,-208.715924510879));
#191037=CARTESIAN_POINT('Ctrl Pts',(-56.4650653119284,39.5387956857416,
-208.711547487502));
#191038=CARTESIAN_POINT('Ctrl Pts',(-56.4809774462897,39.5218092152179,
-208.707139552256));
#191039=CARTESIAN_POINT('Ctrl Pts',(-56.4414369686318,39.5694195255203,
-208.60807433386));
#191040=CARTESIAN_POINT('Ctrl Pts',(-56.4543082678724,39.5531313413699,
-208.603698519052));
#191041=CARTESIAN_POINT('Ctrl Pts',(-56.4685043569935,39.5379957558533,
-208.599289345334));
#191042=CARTESIAN_POINT('Ctrl Pts',(-56.4224946430317,39.5928429539091,
-208.448559464111));
#191043=CARTESIAN_POINT('Ctrl Pts',(-56.4325361263003,39.5806119265652,
-208.444168467643));
#191044=CARTESIAN_POINT('Ctrl Pts',(-56.4433791076362,39.5690861270511,
-208.439774659198));
#191045=CARTESIAN_POINT('Ctrl Pts',(-56.4154558353936,39.6014220979252,
-208.395625171312));
#191046=CARTESIAN_POINT('Ctrl Pts',(-56.4244358024192,39.5906684103489,
-208.391234746251));
#191047=CARTESIAN_POINT('Ctrl Pts',(-56.4340423777229,39.5804730986549,
-208.386840352034));
#191048=CARTESIAN_POINT('Ctrl Pts',(-56.4013424744876,39.6180493256973,
-208.318678862813));
#191049=CARTESIAN_POINT('Ctrl Pts',(-56.4081423174308,39.6101253887744,
-208.314285655015));
#191050=CARTESIAN_POINT('Ctrl Pts',(-56.4153197235611,39.602540640524,-208.309894071191));
#191051=CARTESIAN_POINT('Ctrl Pts',(-56.3960980548982,39.6241637622927,
-208.293342260033));
#191052=CARTESIAN_POINT('Ctrl Pts',(-56.4020826208256,39.6172758938669,
-208.288949312307));
#191053=CARTESIAN_POINT('Ctrl Pts',(-56.4083623316493,39.6106555249509,
-208.284557461711));
#191054=CARTESIAN_POINT('Ctrl Pts',(-56.3856941549037,39.6360014284045,
-208.257923126188));
#191055=CARTESIAN_POINT('Ctrl Pts',(-56.3900359410543,39.6311005791763,
-208.253529947332));
#191056=CARTESIAN_POINT('Ctrl Pts',(-56.3945592936364,39.6263652686867,
-208.249138326507));
#191057=CARTESIAN_POINT('Ctrl Pts',(-56.3818606603298,39.6403285142035,
-208.246633418771));
#191058=CARTESIAN_POINT('Ctrl Pts',(-56.3855943263936,39.6361515194816,
-208.24224035659));
#191059=CARTESIAN_POINT('Ctrl Pts',(-56.3894732411015,39.6321076620074,
-208.237848616086));
#191060=CARTESIAN_POINT('Ctrl Pts',(-56.3097336024218,39.7204021456198,
-208.102340277927));
#191061=CARTESIAN_POINT('Ctrl Pts',(-56.3019347808255,39.7295012949886,
-208.097988441706));
#191062=CARTESIAN_POINT('Ctrl Pts',(-56.2937742808158,39.7383680155035,
-208.093554903205));
#191063=CARTESIAN_POINT('Ctrl Pts',(-56.0141418475234,40.0342093581467,
-208.239693755738));
#191064=CARTESIAN_POINT('Ctrl Pts',(-55.9576541168319,40.0945682331347,
-208.235168290733));
#191065=CARTESIAN_POINT('Ctrl Pts',(-55.901541357958,40.1547597432569,-208.230910731216));
#191066=CARTESIAN_POINT('Ctrl Pts',(-55.4188282852024,40.3069503931471,
-226.764375983926));
#191067=CARTESIAN_POINT('Ctrl Pts',(-55.1914520133701,40.4117219444719,
-227.50020914733));
#191068=CARTESIAN_POINT('Ctrl Pts',(-55.1111144719458,40.5151527971883,
-226.746035420514));
#191069=CARTESIAN_POINT('',(-56.6994898617306,39.1647669078403,-213.398999669105));
#191070=CARTESIAN_POINT('',(-56.6162420139465,39.2878063792742,-213.407725872324));
#191071=CARTESIAN_POINT('Origin',(-57.0675004159511,39.5031336989999,-213.407725872324));
#191072=CARTESIAN_POINT('',(-56.3587983457046,39.6656826243185,-208.210085312216));
#191073=CARTESIAN_POINT('Ctrl Pts',(-56.6994898617306,39.1647669078403,
-213.398999669105));
#191074=CARTESIAN_POINT('Ctrl Pts',(-56.6773193211235,39.2114480278548,
-212.523894235562));
#191075=CARTESIAN_POINT('Ctrl Pts',(-56.651479770637,39.2620537363991,-211.649203631226));
#191076=CARTESIAN_POINT('Ctrl Pts',(-56.5956975036787,39.3561498317412,
-210.339090933364));
#191077=CARTESIAN_POINT('Ctrl Pts',(-56.5745517354038,39.3902416134919,
-209.902674994602));
#191078=CARTESIAN_POINT('Ctrl Pts',(-56.5306742644768,39.4543652326716,
-209.24942443662));
#191079=CARTESIAN_POINT('Ctrl Pts',(-56.5142321837007,39.4776795989311,
-209.03188052566));
#191080=CARTESIAN_POINT('Ctrl Pts',(-56.480816494081,39.5219692158454,-208.70764780547));
#191081=CARTESIAN_POINT('Ctrl Pts',(-56.4683713984661,39.5381257486172,
-208.599790912822));
#191082=CARTESIAN_POINT('Ctrl Pts',(-56.4433041343981,39.569154837062,-208.440233728844));
#191083=CARTESIAN_POINT('Ctrl Pts',(-56.4339894177057,39.5805185781009,
-208.387282545977));
#191084=CARTESIAN_POINT('Ctrl Pts',(-56.4153107858428,39.6025404853857,
-208.310273287259));
#191085=CARTESIAN_POINT('Ctrl Pts',(-56.4083698728123,39.6106383616431,
-208.284910555051));
#191086=CARTESIAN_POINT('Ctrl Pts',(-56.394596442102,39.6263182576719,-208.249418094709));
#191087=CARTESIAN_POINT('Ctrl Pts',(-56.3895186643059,39.6320526747255,
-208.238093899573));
#191088=CARTESIAN_POINT('Ctrl Pts',(-56.3765990499463,39.6464010040802,
-208.218501926116));
#191089=CARTESIAN_POINT('Ctrl Pts',(-56.3682899804801,39.6555191285273,
-208.210085312216));
#191090=CARTESIAN_POINT('Ctrl Pts',(-56.3587983457046,39.6656826243185,
-208.210085312216));
#191091=CARTESIAN_POINT('',(-56.3587426896623,39.6656306474361,-208.218811515434));
#191092=CARTESIAN_POINT('Origin',(-56.7241679835722,40.0068993898824,-208.218811515434));
#191093=CARTESIAN_POINT('Ctrl Pts',(-56.3587426896623,39.6656306474361,
-208.218811515434));
#191094=CARTESIAN_POINT('Ctrl Pts',(-56.3660413076723,39.6578154000967,
-208.21881254009));
#191095=CARTESIAN_POINT('Ctrl Pts',(-56.3721137606125,39.6511492752057,
-208.227134345684));
#191096=CARTESIAN_POINT('Ctrl Pts',(-56.3818606603298,39.6403285142035,
-208.246633418771));
#191097=CARTESIAN_POINT('Ctrl Pts',(-56.3856941549037,39.6360014284045,
-208.257923126188));
#191098=CARTESIAN_POINT('Ctrl Pts',(-56.3960980548982,39.6241637622927,
-208.293342260033));
#191099=CARTESIAN_POINT('Ctrl Pts',(-56.4013424744876,39.6180493256973,
-208.318678862813));
#191100=CARTESIAN_POINT('Ctrl Pts',(-56.4154558353936,39.6014220979252,
-208.395625171312));
#191101=CARTESIAN_POINT('Ctrl Pts',(-56.4224946430317,39.5928429539091,
-208.448559464111));
#191102=CARTESIAN_POINT('Ctrl Pts',(-56.4414369686318,39.5694195255203,
-208.60807433386));
#191103=CARTESIAN_POINT('Ctrl Pts',(-56.4508419233835,39.557225742165,-208.715924510879));
#191104=CARTESIAN_POINT('Ctrl Pts',(-56.4760962345234,39.5238015154724,
-209.040146260381));
#191105=CARTESIAN_POINT('Ctrl Pts',(-56.4885248990568,39.506210827646,-209.257701934938));
#191106=CARTESIAN_POINT('Ctrl Pts',(-56.5216963051399,39.4578331766847,
-209.910997266658));
#191107=CARTESIAN_POINT('Ctrl Pts',(-56.5376887518409,39.4321195627096,
-210.347455422068));
#191108=CARTESIAN_POINT('Ctrl Pts',(-56.5798865157924,39.3611539607029,
-211.657706185491));
#191109=CARTESIAN_POINT('Ctrl Pts',(-56.5994497711951,39.3229976436235,
-212.532533071095));
#191110=CARTESIAN_POINT('Ctrl Pts',(-56.6162420139465,39.2878063792742,
-213.407725872324));
#191111=CARTESIAN_POINT('Origin',(0.,-12.9675000200281,-208.218811515434));
#191112=CARTESIAN_POINT('',(-52.2148720050704,43.7789665035542,-208.218811515434));
#191113=CARTESIAN_POINT('',(-52.2149235689092,43.779022542486,-208.210085312216));
#191114=CARTESIAN_POINT('Origin',(-52.5534287939255,44.1469057658247,-208.218811515435));
#191115=CARTESIAN_POINT('Origin',(0.,-12.9675000200281,-208.218811515434));
#191116=CARTESIAN_POINT('Origin',(0.,-12.9675000200281,-208.210085312216));
#191117=CARTESIAN_POINT('Ctrl Pts',(-56.6994898617306,39.1647669078403,
-213.398999669105));
#191118=CARTESIAN_POINT('Ctrl Pts',(-56.6485891211103,39.2200170067656,
-213.40326396142));
#191119=CARTESIAN_POINT('Ctrl Pts',(-56.6162420139465,39.2878063792742,
-213.407725872324));
#191120=CARTESIAN_POINT('Ctrl Pts',(-56.7065185819046,39.150823857201,-213.643232131226));
#191121=CARTESIAN_POINT('Ctrl Pts',(-56.65401999933,39.2072427576227,-213.659624098485));
#191122=CARTESIAN_POINT('Ctrl Pts',(-56.6213962984542,39.2770046185252,
-213.676360638228));
#191123=CARTESIAN_POINT('Ctrl Pts',(-56.7424050849715,39.0804003802149,
-213.870334716274));
#191124=CARTESIAN_POINT('Ctrl Pts',(-56.6817938786107,39.1423247455582,
-213.899040022644));
#191125=CARTESIAN_POINT('Ctrl Pts',(-56.6474543007565,39.2227628260081,
-213.926243763817));
#191126=CARTESIAN_POINT('Ctrl Pts',(-56.8149567807673,38.8971968180779,
-214.313055955637));
#191127=CARTESIAN_POINT('Ctrl Pts',(-56.7320119538466,38.9741928361746,
-214.361884513898));
#191128=CARTESIAN_POINT('Ctrl Pts',(-56.6987085996655,39.0810160666721,
-214.413338469428));
#191129=CARTESIAN_POINT('Ctrl Pts',(-56.8517306517416,38.7836290914654,
-214.528047686166));
#191130=CARTESIAN_POINT('Ctrl Pts',(-56.7545477049515,38.8689917647235,
-214.586934745154));
#191131=CARTESIAN_POINT('Ctrl Pts',(-56.7239630070022,38.9928957520747,
-214.64988909805));
#191132=CARTESIAN_POINT('Ctrl Pts',(-56.9296676067097,38.4194837815438,
-215.154132254812));
#191133=CARTESIAN_POINT('Ctrl Pts',(-56.7853204957809,38.530818668951,-215.243449487387));
#191134=CARTESIAN_POINT('Ctrl Pts',(-56.7732185725244,38.7090403847746,
-215.338759568586));
#191135=CARTESIAN_POINT('Ctrl Pts',(-56.9425587655176,38.1405794851196,
-215.553519015804));
#191136=CARTESIAN_POINT('Ctrl Pts',(-56.7534747673294,38.2694300870757,
-215.658829235944));
#191137=CARTESIAN_POINT('Ctrl Pts',(-56.7738348833635,38.4902290986137,
-215.777992061446));
#191138=CARTESIAN_POINT('Ctrl Pts',(-56.8784089512595,37.8494072532151,
-215.942196083675));
#191139=CARTESIAN_POINT('Ctrl Pts',(-56.6513917750256,38.0264112674188,
-216.026572725176));
#191140=CARTESIAN_POINT('Ctrl Pts',(-56.7127812850717,38.2589564044561,
-216.205851068199));
#191141=CARTESIAN_POINT('',(-56.8783191528564,37.8493275727119,-215.942121479197));
#191142=CARTESIAN_POINT('',(-56.7127812850717,38.2589564044561,-216.205851068199));
#191143=CARTESIAN_POINT('Origin',(-57.1962194441171,38.1313337325768,-216.205851068199));
#191144=CARTESIAN_POINT('Ctrl Pts',(-56.8784089539157,37.8494072652715,
-215.942196067581));
#191145=CARTESIAN_POINT('Ctrl Pts',(-56.9425587651617,38.1405794928185,
-215.553519004779));
#191146=CARTESIAN_POINT('Ctrl Pts',(-56.9296676059926,38.4194837848944,
-215.154132249051));
#191147=CARTESIAN_POINT('Ctrl Pts',(-56.8517306517416,38.7836290914654,
-214.528047686166));
#191148=CARTESIAN_POINT('Ctrl Pts',(-56.8149567807673,38.8971968180779,
-214.313055955637));
#191149=CARTESIAN_POINT('Ctrl Pts',(-56.7424050849715,39.0804003802149,
-213.870334716274));
#191150=CARTESIAN_POINT('Ctrl Pts',(-56.7065185819046,39.150823857201,-213.643232131226));
#191151=CARTESIAN_POINT('Ctrl Pts',(-56.6994898617306,39.1647669078403,
-213.398999669105));
#191152=CARTESIAN_POINT('Ctrl Pts',(-56.6162420139465,39.2878063792742,
-213.407725872324));
#191153=CARTESIAN_POINT('Ctrl Pts',(-56.6213962984542,39.2770046185252,
-213.676360638228));
#191154=CARTESIAN_POINT('Ctrl Pts',(-56.6474543007565,39.2227628260081,
-213.926243763817));
#191155=CARTESIAN_POINT('Ctrl Pts',(-56.6987085996655,39.0810160666721,
-214.413338469428));
#191156=CARTESIAN_POINT('Ctrl Pts',(-56.7239630070022,38.9928957520747,
-214.64988909805));
#191157=CARTESIAN_POINT('Ctrl Pts',(-56.7732185725244,38.7090403847746,
-215.338759568586));
#191158=CARTESIAN_POINT('Ctrl Pts',(-56.7738348833635,38.4902290986137,
-215.777992061446));
#191159=CARTESIAN_POINT('Ctrl Pts',(-56.7127812850717,38.2589564044561,
-216.205851068199));
#191160=CARTESIAN_POINT('Ctrl Pts',(-52.2148720050704,43.7789665035542,
-208.218811515435));
#191161=CARTESIAN_POINT('Ctrl Pts',(-52.2148720050705,43.7789665035542,
-208.214448081539));
#191162=CARTESIAN_POINT('Ctrl Pts',(-52.2149235689092,43.779022542486,-208.210085312216));
#191163=CARTESIAN_POINT('Ctrl Pts',(-52.2069166839655,43.7862865377113,
-208.21881354139));
#191164=CARTESIAN_POINT('Ctrl Pts',(-52.2056250202409,43.7874750042174,
-208.214450107462));
#191165=CARTESIAN_POINT('Ctrl Pts',(-52.2043847769924,43.7887196915372,
-208.210087338187));
#191166=CARTESIAN_POINT('Ctrl Pts',(-52.2000848734438,43.7924159898367,
-208.227398819688));
#191167=CARTESIAN_POINT('Ctrl Pts',(-52.1976712649932,43.7945859134348,
-208.223035434656));
#191168=CARTESIAN_POINT('Ctrl Pts',(-52.195333723769,43.7968389605576,-208.218672616477));
#191169=CARTESIAN_POINT('Ctrl Pts',(-52.1891506941446,43.8021155648562,
-208.247190155172));
#191170=CARTESIAN_POINT('Ctrl Pts',(-52.1849330344943,43.8058281558383,
-208.242826402981));
#191171=CARTESIAN_POINT('Ctrl Pts',(-52.1808472399183,43.8096868118422,
-208.238463951946));
#191172=CARTESIAN_POINT('Ctrl Pts',(-52.1846836299068,43.8060124062017,
-208.258883232989));
#191173=CARTESIAN_POINT('Ctrl Pts',(-52.1797237791601,43.8103385591305,
-208.254519356384));
#191174=CARTESIAN_POINT('Ctrl Pts',(-52.1749286143212,43.8148481482676,
-208.250157029773));
#191175=CARTESIAN_POINT('Ctrl Pts',(-52.1728001724479,43.8162953562062,
-208.294562380182));
#191176=CARTESIAN_POINT('Ctrl Pts',(-52.1658591933782,43.8222328676652,
-208.290198743649));
#191177=CARTESIAN_POINT('Ctrl Pts',(-52.1591833603872,43.828467493664,-208.285836176959));
#191178=CARTESIAN_POINT('Ctrl Pts',(-52.1666971009815,43.8214493653102,
-208.3198471127));
#191179=CARTESIAN_POINT('Ctrl Pts',(-52.1587292093287,43.8281818395797,
-208.315483211337));
#191180=CARTESIAN_POINT('Ctrl Pts',(-52.1510964156406,43.8352931366209,
-208.311120909483));
#191181=CARTESIAN_POINT('Ctrl Pts',(-52.1499948920096,43.8354085050508,
-208.397025142829));
#191182=CARTESIAN_POINT('Ctrl Pts',(-52.1392045981911,43.8442802812313,
-208.392664031458));
#191183=CARTESIAN_POINT('Ctrl Pts',(-52.1289643871997,43.8537790486242,
-208.388298939608));
#191184=CARTESIAN_POINT('Ctrl Pts',(-52.141343336723,43.8423973674724,-208.450246795732));
#191185=CARTESIAN_POINT('Ctrl Pts',(-52.1290740876191,43.852314411835,-208.445885091517));
#191186=CARTESIAN_POINT('Ctrl Pts',(-52.1174992362576,43.8630330920583,
-208.441520592514));
#191187=CARTESIAN_POINT('Ctrl Pts',(-52.1178275724807,43.8611200325978,
-208.609901492046));
#191188=CARTESIAN_POINT('Ctrl Pts',(-52.1015151102266,43.8738103589885,
-208.605554907233));
#191189=CARTESIAN_POINT('Ctrl Pts',(-52.0863347270061,43.8878226116337,
-208.601175288826));
#191190=CARTESIAN_POINT('Ctrl Pts',(-52.1055914799472,43.8704111305645,
-208.717677837571));
#191191=CARTESIAN_POINT('Ctrl Pts',(-52.0871460895594,43.884425032588,-208.713330067135));
#191192=CARTESIAN_POINT('Ctrl Pts',(-52.0701168476483,43.9001220002185,
-208.708951634353));
#191193=CARTESIAN_POINT('Ctrl Pts',(-52.071995743712,43.8953985191085,-209.042218804019));
#191194=CARTESIAN_POINT('Ctrl Pts',(-52.0476481597434,43.9129173610403,
-209.037939859074));
#191195=CARTESIAN_POINT('Ctrl Pts',(-52.0255864626054,43.9331969723227,
-209.0334926008));
#191196=CARTESIAN_POINT('Ctrl Pts',(-52.0543127614129,43.9076935513658,
-209.259992694935));
#191197=CARTESIAN_POINT('Ctrl Pts',(-52.0268103251713,43.9268242456044,
-209.255711234979));
#191198=CARTESIAN_POINT('Ctrl Pts',(-52.0021445297993,43.949466653783,-209.251266491716));
#191199=CARTESIAN_POINT('Ctrl Pts',(-52.0057184578615,43.940477854794,-209.913465487369));
#191200=CARTESIAN_POINT('Ctrl Pts',(-51.9694532568106,43.9637905045621,
-209.909476451697));
#191201=CARTESIAN_POINT('Ctrl Pts',(-51.937720029348,43.9928431481926,-209.90473928415));
#191202=CARTESIAN_POINT('Ctrl Pts',(-51.9798728970522,43.9562851731636,
-210.350348060599));
#191203=CARTESIAN_POINT('Ctrl Pts',(-51.9388750336111,43.9813630646936,
-210.346355470779));
#191204=CARTESIAN_POINT('Ctrl Pts',(-51.9034482509577,44.0137474304281,
-210.34162185738));
#191205=CARTESIAN_POINT('Ctrl Pts',(-51.9085528218201,43.9979691256788,
-211.662166712722));
#191206=CARTESIAN_POINT('Ctrl Pts',(-51.8543012271538,44.0274385666118,
-211.659386088869));
#191207=CARTESIAN_POINT('Ctrl Pts',(-51.8088683580654,44.0688586918087,
-211.653440509504));
#191208=CARTESIAN_POINT('Ctrl Pts',(-51.870219684202,44.0172576131423,-212.538231376868));
#191209=CARTESIAN_POINT('Ctrl Pts',(-51.8087639397327,44.0481656078252,
-212.535446734955));
#191210=CARTESIAN_POINT('Ctrl Pts',(-51.7580215322863,44.0943375071556,
-212.529490943221));
#191211=CARTESIAN_POINT('Ctrl Pts',(-51.8348891643276,44.0337882456516,
-213.414282330697));
#191212=CARTESIAN_POINT('Ctrl Pts',(-51.7668122505506,44.0656404359961,
-213.409820292477));
#191213=CARTESIAN_POINT('Ctrl Pts',(-51.7111509881033,44.1161634878026,
-213.405556127478));
#191214=CARTESIAN_POINT('',(-51.8348891643276,44.0337882456516,-213.414282330697));
#191215=CARTESIAN_POINT('',(-51.7111509881036,44.1161634878024,-213.405556127478));
#191216=CARTESIAN_POINT('Origin',(-52.0467850062684,44.4866680886213,-213.414282330697));
#191217=CARTESIAN_POINT('Ctrl Pts',(-51.8348891643276,44.0337882456516,
-213.414282330697));
#191218=CARTESIAN_POINT('Ctrl Pts',(-51.870219684202,44.0172576131423,-212.538231376868));
#191219=CARTESIAN_POINT('Ctrl Pts',(-51.9085528218201,43.9979691256788,
-211.662166712722));
#191220=CARTESIAN_POINT('Ctrl Pts',(-51.9798728970522,43.9562851731636,
-210.350348060599));
#191221=CARTESIAN_POINT('Ctrl Pts',(-52.0057184578615,43.940477854794,-209.913465487369));
#191222=CARTESIAN_POINT('Ctrl Pts',(-52.0543127614129,43.9076935513658,
-209.259992694935));
#191223=CARTESIAN_POINT('Ctrl Pts',(-52.071995743712,43.8953985191085,-209.042218804019));
#191224=CARTESIAN_POINT('Ctrl Pts',(-52.1055914799472,43.8704111305645,
-208.717677837571));
#191225=CARTESIAN_POINT('Ctrl Pts',(-52.1178275724807,43.8611200325978,
-208.609901492046));
#191226=CARTESIAN_POINT('Ctrl Pts',(-52.141343336723,43.8423973674724,-208.450246795732));
#191227=CARTESIAN_POINT('Ctrl Pts',(-52.1499948920096,43.8354085050508,
-208.397025142829));
#191228=CARTESIAN_POINT('Ctrl Pts',(-52.1666971009815,43.8214493653102,
-208.3198471127));
#191229=CARTESIAN_POINT('Ctrl Pts',(-52.1728001724479,43.8162953562062,
-208.294562380182));
#191230=CARTESIAN_POINT('Ctrl Pts',(-52.1846836299068,43.8060124062017,
-208.258883232989));
#191231=CARTESIAN_POINT('Ctrl Pts',(-52.1891506941446,43.8021155648562,
-208.247190155172));
#191232=CARTESIAN_POINT('Ctrl Pts',(-52.2000848734438,43.7924159898367,
-208.227398819688));
#191233=CARTESIAN_POINT('Ctrl Pts',(-52.2069166839655,43.7862865377113,
-208.21881354139));
#191234=CARTESIAN_POINT('Ctrl Pts',(-52.2148720050704,43.7789665035542,
-208.218811515434));
#191235=CARTESIAN_POINT('Ctrl Pts',(-52.2149235689092,43.779022542486,-208.210085312216));
#191236=CARTESIAN_POINT('Ctrl Pts',(-52.2043801934833,43.7887239088728,
-208.210087344463));
#191237=CARTESIAN_POINT('Ctrl Pts',(-52.1953274288659,43.796844542981,-208.218681234754));
#191238=CARTESIAN_POINT('Ctrl Pts',(-52.1880904910527,43.8032628774376,
-208.228568296719));
#191239=CARTESIAN_POINT('Ctrl Pts',(-52.1808394389761,43.8096937296283,
-208.238474641509));
#191240=CARTESIAN_POINT('Ctrl Pts',(-52.1749242234792,43.8148519452172,
-208.250167023561));
#191241=CARTESIAN_POINT('Ctrl Pts',(-52.1696802065441,43.8193879205004,
-208.262050087041));
#191242=CARTESIAN_POINT('Ctrl Pts',(-52.1591795680454,43.8284707738317,
-208.28584477638));
#191243=CARTESIAN_POINT('Ctrl Pts',(-52.1510932946611,43.8352957489707,
-208.311131552955));
#191244=CARTESIAN_POINT('Ctrl Pts',(-52.1437197227052,43.8414545028842,
-208.336847252802));
#191245=CARTESIAN_POINT('Ctrl Pts',(-52.1289623042575,43.8537805924866,
-208.38831448545));
#191246=CARTESIAN_POINT('Ctrl Pts',(-52.117497806034,43.8630342337481,-208.441527742187));
#191247=CARTESIAN_POINT('Ctrl Pts',(-52.1071115904079,43.871295780733,-208.494739003265));
#191248=CARTESIAN_POINT('Ctrl Pts',(-52.0863339472228,43.8878230204506,
-208.601188227497));
#191249=CARTESIAN_POINT('Ctrl Pts',(-52.0701156440688,43.9001228988017,
-208.708960203697));
#191250=CARTESIAN_POINT('Ctrl Pts',(-52.0552737632954,43.9111466435138,
-208.817132044246));
#191251=CARTESIAN_POINT('Ctrl Pts',(-52.0255859242023,43.9331971615186,
-209.033505443658));
#191252=CARTESIAN_POINT('Ctrl Pts',(-52.0021438786448,43.9494670967064,
-209.251272899507));
#191253=CARTESIAN_POINT('Ctrl Pts',(-51.980669942658,43.9639252593981,-209.469090795394));
#191254=CARTESIAN_POINT('Ctrl Pts',(-51.9377196179987,43.9928432361475,
-209.904751465645));
#191255=CARTESIAN_POINT('Ctrl Pts',(-51.9034476265843,44.0137477974947,
-210.34163037533));
#191256=CARTESIAN_POINT('Ctrl Pts',(-51.8719217450993,44.032117736709,-210.778894755328));
#191257=CARTESIAN_POINT('Ctrl Pts',(-51.8088678222893,44.0688588736632,
-211.653453472328));
#191258=CARTESIAN_POINT('Ctrl Pts',(-51.7580264403492,44.0943352215171,
-212.529399211082));
#191259=CARTESIAN_POINT('Ctrl Pts',(-51.7111509881036,44.1161634878024,
-213.405556127478));
#191260=CARTESIAN_POINT('Ctrl Pts',(-56.493933359474,37.4299544982648,-217.120571662276));
#191261=CARTESIAN_POINT('Ctrl Pts',(-56.4397634983909,37.224757588248,-216.873345412929));
#191262=CARTESIAN_POINT('Ctrl Pts',(-56.7060833516158,37.0658058009135,
-216.773500778908));
#191263=CARTESIAN_POINT('Ctrl Pts',(-56.5765881122648,37.7430529543375,
-216.842569308717));
#191264=CARTESIAN_POINT('Ctrl Pts',(-56.5188765640458,37.5244400369599,
-216.620195693846));
#191265=CARTESIAN_POINT('Ctrl Pts',(-56.7710955429381,37.361906243833,-216.520874647208));
#191266=CARTESIAN_POINT('Ctrl Pts',(-56.6508914688365,38.0245160939405,
-216.533616118302));
#191267=CARTESIAN_POINT('Ctrl Pts',(-56.5910528040772,37.7978456011263,
-216.333918533896));
#191268=CARTESIAN_POINT('Ctrl Pts',(-56.8296189005624,37.6279227921511,
-216.240093840689));
#191269=CARTESIAN_POINT('Ctrl Pts',(-56.7157183655621,38.2700821453947,
-216.190356702619));
#191270=CARTESIAN_POINT('Ctrl Pts',(-56.654233824142,38.0371770269228,-216.012141918556));
#191271=CARTESIAN_POINT('Ctrl Pts',(-56.8807321403751,37.8599121389907,
-215.928110733678));
#191272=CARTESIAN_POINT('',(-56.7089756139177,37.0787993772561,-216.761772606351));
#191273=CARTESIAN_POINT('',(-56.4975419847624,37.4436240691992,-217.108396707512));
#191274=CARTESIAN_POINT('Origin',(-56.9809801438088,37.3160013973188,-217.108396707512));
#191275=CARTESIAN_POINT('Ctrl Pts',(-56.7089871854676,37.0788107123884,
-216.761648750883));
#191276=CARTESIAN_POINT('Ctrl Pts',(-56.7294957256895,37.1726092366223,
-216.681203054031));
#191277=CARTESIAN_POINT('Ctrl Pts',(-56.7493601478726,37.2633733311913,
-216.597849124767));
#191278=CARTESIAN_POINT('Ctrl Pts',(-56.7685769354936,37.3509956263222,
-216.511522123815));
#191279=CARTESIAN_POINT('Ctrl Pts',(-56.7882832885266,37.4408501803435,
-216.422995862789));
#191280=CARTESIAN_POINT('Ctrl Pts',(-56.8073094114385,37.5274016027229,
-216.331342347585));
#191281=CARTESIAN_POINT('Ctrl Pts',(-56.8256102466557,37.6105017357572,
-216.236465902513));
#191282=CARTESIAN_POINT('Ctrl Pts',(-56.8424913406294,37.687155130989,-216.148949777368));
#191283=CARTESIAN_POINT('Ctrl Pts',(-56.8587552053145,37.7608719482353,
-216.058690386204));
#191284=CARTESIAN_POINT('Ctrl Pts',(-56.8743281021412,37.8315042449062,
-215.965604323594));
#191285=CARTESIAN_POINT('Ctrl Pts',(-56.8756378208087,37.8374445936102,
-215.95777555832));
#191286=CARTESIAN_POINT('Ctrl Pts',(-56.8769426285927,37.8433631050215,
-215.949926799156));
#191287=CARTESIAN_POINT('Ctrl Pts',(-56.8782424684775,37.8492596800232,
-215.942057996922));
#191288=CARTESIAN_POINT('Ctrl Pts',(-56.7127812850717,38.2589564044562,
-216.205851068199));
#191289=CARTESIAN_POINT('Ctrl Pts',(-56.675820350007,38.1189473751743,-216.400115647765));
#191290=CARTESIAN_POINT('Ctrl Pts',(-56.6358255784857,37.9674460907173,
-216.583274967065));
#191291=CARTESIAN_POINT('Ctrl Pts',(-56.5929883959844,37.8051776760066,
-216.756029715358));
#191292=CARTESIAN_POINT('Ctrl Pts',(-56.5625833082106,37.6900023749221,
-216.878648033801));
#191293=CARTESIAN_POINT('Ctrl Pts',(-56.5307460013724,37.5694017889912,
-216.996023775216));
#191294=CARTESIAN_POINT('Ctrl Pts',(-56.4975419847624,37.4436240691992,
-217.108396707512));
#191295=CARTESIAN_POINT('Ctrl Pts',(-50.3946838675078,44.2853208550272,
-215.949517829821));
#191296=CARTESIAN_POINT('Ctrl Pts',(-50.5733927277608,44.0594460487845,
-216.033846066216));
#191297=CARTESIAN_POINT('Ctrl Pts',(-50.8056178277775,44.122591905242,-216.213154850206));
#191298=CARTESIAN_POINT('Ctrl Pts',(-50.6840782755553,44.3512988155942,
-215.562426526428));
#191299=CARTESIAN_POINT('Ctrl Pts',(-50.8146150821098,44.1628990192414,
-215.667558528646));
#191300=CARTESIAN_POINT('Ctrl Pts',(-51.0353932564851,44.1850716554394,
-215.787037343168));
#191301=CARTESIAN_POINT('Ctrl Pts',(-50.9615743000221,44.3410430024776,
-215.16541559435));
#191302=CARTESIAN_POINT('Ctrl Pts',(-51.0742087234282,44.1970539660852,
-215.254908907856));
#191303=CARTESIAN_POINT('Ctrl Pts',(-51.2530132713136,44.1864939716348,
-215.350454259388));
#191304=CARTESIAN_POINT('Ctrl Pts',(-51.3272201973583,44.2660193725917,
-214.53815525918));
#191305=CARTESIAN_POINT('Ctrl Pts',(-51.4134751324715,44.1691804565493,
-214.597183792391));
#191306=CARTESIAN_POINT('Ctrl Pts',(-51.5379400316186,44.1395671487007,
-214.660316432704));
#191307=CARTESIAN_POINT('Ctrl Pts',(-51.4410933404088,44.2301818679357,
-214.323225058398));
#191308=CARTESIAN_POINT('Ctrl Pts',(-51.5188806364346,44.1475373241685,
-214.372200521963));
#191309=CARTESIAN_POINT('Ctrl Pts',(-51.6262699955377,44.115047729854,-214.423842816164));
#191310=CARTESIAN_POINT('Ctrl Pts',(-51.6251804607438,44.1590287655627,
-213.880764647617));
#191311=CARTESIAN_POINT('Ctrl Pts',(-51.6877019825951,44.0986734814325,
-213.909653665353));
#191312=CARTESIAN_POINT('Ctrl Pts',(-51.7686497926484,44.0649060154392,
-213.937052332728));
#191313=CARTESIAN_POINT('Ctrl Pts',(-51.6971249390044,44.1231091971094,
-213.650130074529));
#191314=CARTESIAN_POINT('Ctrl Pts',(-51.7539747290057,44.0709837332505,
-213.666541516794));
#191315=CARTESIAN_POINT('Ctrl Pts',(-51.8240398734104,44.0388644698843,
-213.683299458677));
#191316=CARTESIAN_POINT('Ctrl Pts',(-51.7111509881034,44.1161634878026,
-213.405556127478));
#191317=CARTESIAN_POINT('Ctrl Pts',(-51.7668122505508,44.0656404359961,
-213.409820292478));
#191318=CARTESIAN_POINT('Ctrl Pts',(-51.8348891643277,44.0337882456516,
-213.414282330697));
#191319=CARTESIAN_POINT('',(-50.8056178277775,44.122591905242,-216.213154850206));
#191320=CARTESIAN_POINT('',(-50.3946596588565,44.2852932582017,-215.949495022928));
#191321=CARTESIAN_POINT('Origin',(-50.6744232242015,44.605072968075,-216.213154850206));
#191322=CARTESIAN_POINT('',(-51.199201564042,44.1751972079741,-215.438515911214));
#191323=CARTESIAN_POINT('Ctrl Pts',(-50.8056178277775,44.122591905242,-216.213154850206));
#191324=CARTESIAN_POINT('Ctrl Pts',(-50.942180477307,44.1597255547226,-215.959527204626));
#191325=CARTESIAN_POINT('Ctrl Pts',(-51.0744557978905,44.1752936552023,
-215.702232151633));
#191326=CARTESIAN_POINT('Ctrl Pts',(-51.1992016385053,44.1751487167426,
-215.438515960385));
#191327=CARTESIAN_POINT('Ctrl Pts',(-51.1992014957792,44.1752416613772,
-215.438515866138));
#191328=CARTESIAN_POINT('Ctrl Pts',(-51.2842504005282,44.1752065198926,
-215.25904635145));
#191329=CARTESIAN_POINT('Ctrl Pts',(-51.3657803296688,44.1679108384777,
-215.076578914644));
#191330=CARTESIAN_POINT('Ctrl Pts',(-51.4427636582211,44.1552425471702,
-214.890248844184));
#191331=CARTESIAN_POINT('Ctrl Pts',(-51.4993014431223,44.1459387518877,
-214.753405067195));
#191332=CARTESIAN_POINT('Ctrl Pts',(-51.5534831111867,44.1334894340395,
-214.614283009387));
#191333=CARTESIAN_POINT('Ctrl Pts',(-51.6030992923736,44.1196492385698,
-214.47277824517));
#191334=CARTESIAN_POINT('Ctrl Pts',(-51.6368787254434,44.1102266279344,
-214.376439700011));
#191335=CARTESIAN_POINT('Ctrl Pts',(-51.6685414748578,44.1001594496879,
-214.278996905908));
#191336=CARTESIAN_POINT('Ctrl Pts',(-51.6973902398397,44.0900014094681,
-214.180417040629));
#191337=CARTESIAN_POINT('Ctrl Pts',(-51.7686127338013,44.0649230063313,
-213.937040803763));
#191338=CARTESIAN_POINT('Ctrl Pts',(-51.8240227963017,44.0388724600132,
-213.683298339373));
#191339=CARTESIAN_POINT('Ctrl Pts',(-51.8348891643276,44.0337882456516,
-213.414282330697));
#191340=CARTESIAN_POINT('Ctrl Pts',(-51.7111509881036,44.1161634878024,
-213.405556127478));
#191341=CARTESIAN_POINT('Ctrl Pts',(-51.6971249390044,44.1231091971094,
-213.650130074529));
#191342=CARTESIAN_POINT('Ctrl Pts',(-51.6251804607438,44.1590287655627,
-213.880764647617));
#191343=CARTESIAN_POINT('Ctrl Pts',(-51.4410933404088,44.2301818679357,
-214.323225058398));
#191344=CARTESIAN_POINT('Ctrl Pts',(-51.3272201973583,44.2660193725917,
-214.53815525918));
#191345=CARTESIAN_POINT('Ctrl Pts',(-50.9615743000221,44.3410430024776,
-215.16541559435));
#191346=CARTESIAN_POINT('Ctrl Pts',(-50.6840782755553,44.3512988155942,
-215.562426526428));
#191347=CARTESIAN_POINT('Ctrl Pts',(-50.3946838675078,44.2853208550272,
-215.949517829821));
#191348=CARTESIAN_POINT('Ctrl Pts',(-56.351930605989,36.892044198215,-217.60005));
#191349=CARTESIAN_POINT('Ctrl Pts',(-56.2980271921268,36.6878565975336,
-217.354444173088));
#191350=CARTESIAN_POINT('Ctrl Pts',(-56.5618180211198,36.5289367340068,
-217.254048694966));
#191351=CARTESIAN_POINT('Ctrl Pts',(-56.4005154364319,37.0760848599628,
-217.436382427969));
#191352=CARTESIAN_POINT('Ctrl Pts',(-56.3465050213663,36.8714919357672,
-217.190493004533));
#191353=CARTESIAN_POINT('Ctrl Pts',(-56.6108961448827,36.7123872459292,
-217.09039277187));
#191354=CARTESIAN_POINT('Ctrl Pts',(-56.4490528535666,37.2599459188071,
-217.272499319579));
#191355=CARTESIAN_POINT('Ctrl Pts',(-56.394913005841,37.054862700115,-217.026399523816));
#191356=CARTESIAN_POINT('Ctrl Pts',(-56.6599284966586,36.8956552674856,
-216.926524548004));
#191357=CARTESIAN_POINT('Ctrl Pts',(-56.4975419847625,37.4436240691992,
-217.108396707512));
#191358=CARTESIAN_POINT('Ctrl Pts',(-56.4432500919346,37.2379648996087,
-216.862162585543));
#191359=CARTESIAN_POINT('Ctrl Pts',(-56.7089132278424,37.0787382657863,
-216.762440352386));
#191360=CARTESIAN_POINT('',(-56.5618180211198,36.5289367340069,-217.254048694966));
#191361=CARTESIAN_POINT('',(-56.351930605989,36.892044198215,-217.60005));
#191362=CARTESIAN_POINT('Origin',(-56.8353687650353,36.7644215263347,-217.60005));
#191363=CARTESIAN_POINT('Origin',(-3.60305208601888,-172.041642880457,32.426831165629));
#191364=CARTESIAN_POINT('Origin',(-1.571323227265,-170.618389531262,32.0043824393251));
#191365=CARTESIAN_POINT('Ctrl Pts',(-50.8056178277775,44.122591905242,-216.213154850206));
#191366=CARTESIAN_POINT('Ctrl Pts',(-50.5733927277608,44.0594460487845,
-216.033846066216));
#191367=CARTESIAN_POINT('Ctrl Pts',(-50.3946838675078,44.2853208550272,
-215.949517829821));
#191368=CARTESIAN_POINT('Ctrl Pts',(-50.5708296219181,44.0587490977934,
-216.539715105359));
#191369=CARTESIAN_POINT('Ctrl Pts',(-50.3446120279677,43.9972367818614,
-216.339838795389));
#191370=CARTESIAN_POINT('Ctrl Pts',(-50.1727811095107,44.2347300586007,
-216.246332930804));
#191371=CARTESIAN_POINT('Ctrl Pts',(-50.3034496116678,43.9860440381524,
-216.835170188754));
#191372=CARTESIAN_POINT('Ctrl Pts',(-50.0849672365085,43.9266350565256,
-216.613616901689));
#191373=CARTESIAN_POINT('Ctrl Pts',(-49.9199744021421,44.177167823471,-216.514858553214));
#191374=CARTESIAN_POINT('Ctrl Pts',(-50.0071669705522,43.9054798737905,
-217.102435280211));
#191375=CARTESIAN_POINT('Ctrl Pts',(-49.8012110043667,43.8494770305304,
-216.857236779929));
#191376=CARTESIAN_POINT('Ctrl Pts',(-49.6396803417508,44.1134564636836,
-216.757742122242));
#191377=CARTESIAN_POINT('',(-50.0071669705522,43.9054798737905,-217.102435280211));
#191378=CARTESIAN_POINT('',(-49.6397984855042,44.1135871370244,-216.757171052671));
#191379=CARTESIAN_POINT('Origin',(-49.8759723669763,44.3879609366236,-217.102435280211));
#191380=CARTESIAN_POINT('Ctrl Pts',(-50.0071669705522,43.9054798737905,
-217.102435280211));
#191381=CARTESIAN_POINT('Ctrl Pts',(-50.1847337846688,43.9537632357311,
-216.94225913611));
#191382=CARTESIAN_POINT('Ctrl Pts',(-50.3518605126697,43.9992077650942,
-216.772016153319));
#191383=CARTESIAN_POINT('Ctrl Pts',(-50.5078320264292,44.0416190066809,
-216.591016782861));
#191384=CARTESIAN_POINT('Ctrl Pts',(-50.6121600770689,44.0699875340696,
-216.469947806663));
#191385=CARTESIAN_POINT('Ctrl Pts',(-50.7114964522535,44.0969987421085,
-216.344065601425));
#191386=CARTESIAN_POINT('Ctrl Pts',(-50.8056178277775,44.1225919052419,
-216.213154850206));
#191387=CARTESIAN_POINT('Ctrl Pts',(-50.3945871449412,44.2852102294111,
-215.949426636203));
#191388=CARTESIAN_POINT('Ctrl Pts',(-50.3238862622841,44.2690849821772,
-216.043975317111));
#191389=CARTESIAN_POINT('Ctrl Pts',(-50.2500250536189,44.2522227786124,
-216.135639498551));
#191390=CARTESIAN_POINT('Ctrl Pts',(-50.1731582085826,44.234703660966,-216.224503324805));
#191391=CARTESIAN_POINT('Ctrl Pts',(-50.0909523255552,44.2159676957354,
-216.319539478597));
#191392=CARTESIAN_POINT('Ctrl Pts',(-50.0053087127001,44.196480421214,-216.411373899394));
#191393=CARTESIAN_POINT('Ctrl Pts',(-49.9163764443311,44.1762907631104,
-216.500100361556));
#191394=CARTESIAN_POINT('Ctrl Pts',(-49.8274441759621,44.1561011050067,
-216.588826823719));
#191395=CARTESIAN_POINT('Ctrl Pts',(-49.7352226059874,44.135208399256,-216.674446234173));
#191396=CARTESIAN_POINT('Ctrl Pts',(-49.6398281339213,44.1136199297675,
-216.75702774159));
#191397=CARTESIAN_POINT('Ctrl Pts',(-56.5998602975341,36.7010789093092,
-217.106689509426));
#191398=CARTESIAN_POINT('Ctrl Pts',(-56.3034738562376,36.8544199785542,
-217.235822749176));
#191399=CARTESIAN_POINT('Ctrl Pts',(-56.3924021524771,37.0639192723716,
-217.511774135751));
#191400=CARTESIAN_POINT('Ctrl Pts',(-56.5630402918383,36.4948001608833,
-217.276505175982));
#191401=CARTESIAN_POINT('Ctrl Pts',(-56.3049395852604,36.6634137058091,
-217.365820774673));
#191402=CARTESIAN_POINT('Ctrl Pts',(-56.3493441379948,36.8590087399585,
-217.613536138229));
#191403=CARTESIAN_POINT('Ctrl Pts',(-56.5022140574202,36.3057210321513,
-217.452921387449));
#191404=CARTESIAN_POINT('Ctrl Pts',(-56.2819498379186,36.4743061370055,
-217.512980511932));
#191405=CARTESIAN_POINT('Ctrl Pts',(-56.2928273312848,36.6682242676255,
-217.719433251733));
#191406=CARTESIAN_POINT('Ctrl Pts',(-56.3592256802117,36.0944966789716,
-217.709486784208));
#191407=CARTESIAN_POINT('Ctrl Pts',(-56.1906627010658,36.2589234334196,
-217.731867301705));
#191408=CARTESIAN_POINT('Ctrl Pts',(-56.1827206487482,36.4479723499478,
-217.873318464));
#191409=CARTESIAN_POINT('Ctrl Pts',(-56.3158477513733,36.0436491754657,
-217.778350695569));
#191410=CARTESIAN_POINT('Ctrl Pts',(-56.1617340323702,36.2072924601779,
-217.789891061158));
#191411=CARTESIAN_POINT('Ctrl Pts',(-56.1506047053284,36.3940866925176,
-217.914618813864));
#191412=CARTESIAN_POINT('Ctrl Pts',(-56.2165191994686,35.9575384315461,
-217.915549753192));
#191413=CARTESIAN_POINT('Ctrl Pts',(-56.0920748178132,36.1188836138303,
-217.905196077141));
#191414=CARTESIAN_POINT('Ctrl Pts',(-56.080012372023,36.3003319845699,-217.996894716944));
#191415=CARTESIAN_POINT('Ctrl Pts',(-56.1595137194348,35.9216038074791,
-217.985179826652));
#191416=CARTESIAN_POINT('Ctrl Pts',(-56.0506116715503,36.0810322659478,
-217.963789723577));
#191417=CARTESIAN_POINT('Ctrl Pts',(-56.0408099000175,36.2597047407171,
-218.038646786212));
#191418=CARTESIAN_POINT('Ctrl Pts',(-56.0329463188087,35.8737089536201,
-218.118234524917));
#191419=CARTESIAN_POINT('Ctrl Pts',(-55.9560538608286,36.0284179459394,
-218.074544890872));
#191420=CARTESIAN_POINT('Ctrl Pts',(-55.9568695408965,36.2006683602997,
-218.118420398712));
#191421=CARTESIAN_POINT('Ctrl Pts',(-55.9615748547198,35.8614000834378,
-218.183336655256));
#191422=CARTESIAN_POINT('Ctrl Pts',(-55.9014450628778,36.0129000216887,
-218.128423068974));
#191423=CARTESIAN_POINT('Ctrl Pts',(-55.9109641207449,36.1817435745309,
-218.157447664942));
#191424=CARTESIAN_POINT('Ctrl Pts',(-55.8107887600364,35.8683604687332,
-218.29848588497));
#191425=CARTESIAN_POINT('Ctrl Pts',(-55.7849297648133,36.0123283043043,
-218.221238015638));
#191426=CARTESIAN_POINT('Ctrl Pts',(-55.8171829211833,36.1739792798186,
-218.226464537285));
#191427=CARTESIAN_POINT('Ctrl Pts',(-55.7298626364341,35.8880162468266,
-218.349466700677));
#191428=CARTESIAN_POINT('Ctrl Pts',(-55.7215158157664,36.0274854463032,
-218.261222954536));
#191429=CARTESIAN_POINT('Ctrl Pts',(-55.7683976723683,36.1853714927186,
-218.257013741027));
#191430=CARTESIAN_POINT('Ctrl Pts',(-55.4296619555845,36.0173958780985,
-218.499755650958));
#191431=CARTESIAN_POINT('Ctrl Pts',(-55.4862779948566,36.1379559621716,
-218.372291428693));
#191432=CARTESIAN_POINT('Ctrl Pts',(-55.5929099869609,36.2828149556278,
-218.347040602773));
#191433=CARTESIAN_POINT('Ctrl Pts',(-55.2185504504437,36.2273017846528,
-218.523434776138));
#191434=CARTESIAN_POINT('Ctrl Pts',(-55.3189357882185,36.3340027933732,
-218.370415986585));
#191435=CARTESIAN_POINT('Ctrl Pts',(-55.4813933689204,36.4668980232678,
-218.361137187739));
#191436=CARTESIAN_POINT('Ctrl Pts',(-55.07865466989,36.4312359741192,-218.492424312504));
#191437=CARTESIAN_POINT('Ctrl Pts',(-55.2233495790564,36.5130164548146,
-218.321717122596));
#191438=CARTESIAN_POINT('Ctrl Pts',(-55.4128172491991,36.6541279382314,
-218.342470788226));
#191439=CARTESIAN_POINT('Ctrl Pts',(-55.2146353748416,36.2578367651479,
-218.504776656653));
#191440=CARTESIAN_POINT('Ctrl Pts',(-55.260640995775,36.2060885425481,-218.50402374007));
#191441=CARTESIAN_POINT('Ctrl Pts',(-55.3103353936485,36.1563189022288,
-218.498881370272));
#191442=CARTESIAN_POINT('Ctrl Pts',(-55.3626215551361,36.1106564380767,
-218.488767188068));
#191443=CARTESIAN_POINT('Ctrl Pts',(-55.4208549058936,36.0598001844186,
-218.477502587586));
#191444=CARTESIAN_POINT('Ctrl Pts',(-55.4823027833847,36.0140385603264,
-218.460070833374));
#191445=CARTESIAN_POINT('Ctrl Pts',(-55.5454444482828,35.9763822852642,
-218.435667388483));
#191446=CARTESIAN_POINT('Ctrl Pts',(-55.5801575945066,35.9556801421612,
-218.422251202005));
#191447=CARTESIAN_POINT('Ctrl Pts',(-55.6153826094992,35.9374290183054,
-218.406727872537));
#191448=CARTESIAN_POINT('Ctrl Pts',(-55.6508670966856,35.9221355025851,
-218.388963715956));
#191449=CARTESIAN_POINT('Ctrl Pts',(-55.7069895268485,35.8979472069096,
-218.36086784319));
#191450=CARTESIAN_POINT('Ctrl Pts',(-55.7640866152408,35.8810200808859,
-218.327001834227));
#191451=CARTESIAN_POINT('Ctrl Pts',(-55.8194769037915,35.8720024376452,
-218.28910047931));
#191452=CARTESIAN_POINT('Ctrl Pts',(-55.8420472117827,35.8683279490187,
-218.273656521963));
#191453=CARTESIAN_POINT('Ctrl Pts',(-55.8643344920639,35.8659663152427,
-218.257542543503));
#191454=CARTESIAN_POINT('Ctrl Pts',(-55.8861588306467,35.8649593048988,
-218.240875914317));
#191455=CARTESIAN_POINT('Ctrl Pts',(-55.9373480158733,35.8625973529513,
-218.201784183528));
#191456=CARTESIAN_POINT('Ctrl Pts',(-55.9866847804406,35.8675108571836,
-218.159221503107));
#191457=CARTESIAN_POINT('Ctrl Pts',(-56.0328916678397,35.87841171425,-218.115098527541));
#191458=CARTESIAN_POINT('Ctrl Pts',(-56.0547315098726,35.8835640413111,
-218.094243653503));
#191459=CARTESIAN_POINT('Ctrl Pts',(-56.075872431505,35.890053191864,-218.073040207613));
#191460=CARTESIAN_POINT('Ctrl Pts',(-56.0961809284015,35.8977394644203,
-218.051689938455));
#191461=CARTESIAN_POINT('Ctrl Pts',(-56.1510011476436,35.9184875852112,
-217.994057586731));
#191462=CARTESIAN_POINT('Ctrl Pts',(-56.2011095262357,35.9482317464444,
-217.934096211335));
#191463=CARTESIAN_POINT('Ctrl Pts',(-56.2458141616989,35.9838108579469,
-217.874493673553));
#191464=CARTESIAN_POINT('Ctrl Pts',(-56.2527092449539,35.9892984529895,
-217.865300791071));
#191465=CARTESIAN_POINT('Ctrl Pts',(-56.2594757994001,35.9949247576492,
-217.856116444932));
#191466=CARTESIAN_POINT('Ctrl Pts',(-56.2661113023919,36.0006780842024,
-217.846950497198));
#191467=CARTESIAN_POINT('Ctrl Pts',(-56.3157684385378,36.0437334065035,
-217.778356644542));
#191468=CARTESIAN_POINT('Ctrl Pts',(-56.3591396849303,36.0945805785127,
-217.709498213182));
#191469=CARTESIAN_POINT('Ctrl Pts',(-56.3967623186957,36.1501656861841,
-217.641985775927));
#191470=CARTESIAN_POINT('Ctrl Pts',(-56.4488863231582,36.2271756695461,
-217.548451160497));
#191471=CARTESIAN_POINT('Ctrl Pts',(-56.4901050623955,36.3123762454183,
-217.458009117953));
#191472=CARTESIAN_POINT('Ctrl Pts',(-56.5229117001721,36.403789675791,-217.369929486757));
#191473=CARTESIAN_POINT('Ctrl Pts',(-56.5374641297148,36.4443390156475,
-217.330858959754));
#191474=CARTESIAN_POINT('Ctrl Pts',(-56.5503610043736,36.4861112162022,
-217.292253272313));
#191475=CARTESIAN_POINT('Ctrl Pts',(-56.5618180211198,36.5289367340068,
-217.254048694965));
#191476=CARTESIAN_POINT('Ctrl Pts',(-56.351930605989,36.892044198215,-217.60005));
#191477=CARTESIAN_POINT('Ctrl Pts',(-56.3410707608223,36.8509068087716,
-217.622000115692));
#191478=CARTESIAN_POINT('Ctrl Pts',(-56.3294340028219,36.810586059083,-217.644150772639));
#191479=CARTESIAN_POINT('Ctrl Pts',(-56.316972640641,36.7712007085407,-217.66656467806));
#191480=CARTESIAN_POINT('Ctrl Pts',(-56.3047871817314,36.7326873771965,
-217.688482323943));
#191481=CARTESIAN_POINT('Ctrl Pts',(-56.2918130999229,36.6950685168439,
-217.710652428266));
#191482=CARTESIAN_POINT('Ctrl Pts',(-56.2779625738601,36.6584665837728,
-217.73311366749));
#191483=CARTESIAN_POINT('Ctrl Pts',(-56.2646565449826,36.6233035599128,
-217.754691901876));
#191484=CARTESIAN_POINT('Ctrl Pts',(-56.2505413393021,36.5890791553865,
-217.776539440422));
#191485=CARTESIAN_POINT('Ctrl Pts',(-56.2355019342317,36.5559117536623,
-217.798662381777));
#191486=CARTESIAN_POINT('Ctrl Pts',(-56.2278151589798,36.5389595962098,
-217.80996961616));
#191487=CARTESIAN_POINT('Ctrl Pts',(-56.2198863685553,36.522283716404,-217.821348279737));
#191488=CARTESIAN_POINT('Ctrl Pts',(-56.211696626409,36.5059008653988,-217.832795341709));
#191489=CARTESIAN_POINT('Ctrl Pts',(-56.1942955844922,36.471091628189,-217.857117329096));
#191490=CARTESIAN_POINT('Ctrl Pts',(-56.1757634090178,36.4377519073116,
-217.881721925024));
#191491=CARTESIAN_POINT('Ctrl Pts',(-56.156087765869,36.4065179517719,-217.90641657657));
#191492=CARTESIAN_POINT('Ctrl Pts',(-56.1430013470316,36.3857440120816,
-217.922841175793));
#191493=CARTESIAN_POINT('Ctrl Pts',(-56.129409171891,36.36590157531,-217.939304646675));
#191494=CARTESIAN_POINT('Ctrl Pts',(-56.1153105737103,36.3471770581247,
-217.95573781425));
#191495=CARTESIAN_POINT('Ctrl Pts',(-56.097662539009,36.3237384917642,-217.976308165138));
#191496=CARTESIAN_POINT('Ctrl Pts',(-56.0790532646516,36.3018583859476,
-217.997031481476));
#191497=CARTESIAN_POINT('Ctrl Pts',(-56.0595942388362,36.2821522564186,
-218.017599237196));
#191498=CARTESIAN_POINT('Ctrl Pts',(-56.0413143454399,36.26364023272,-218.036920676282));
#191499=CARTESIAN_POINT('Ctrl Pts',(-56.0222848102711,36.2470466354578,
-218.056104053989));
#191500=CARTESIAN_POINT('Ctrl Pts',(-56.0026479840161,36.232868550874,-218.074892230468));
#191501=CARTESIAN_POINT('Ctrl Pts',(-56.0013813235415,36.2319540029163,
-218.076104149351));
#191502=CARTESIAN_POINT('Ctrl Pts',(-56.0001121536374,36.2310495008554,
-218.077314425724));
#191503=CARTESIAN_POINT('Ctrl Pts',(-55.9988405197347,36.2301551761968,
-218.078522991535));
#191504=CARTESIAN_POINT('Ctrl Pts',(-55.982614871827,36.2187438753542,-218.093943910471));
#191505=CARTESIAN_POINT('Ctrl Pts',(-55.9658224751974,36.2089101273231,
-218.109248815916));
#191506=CARTESIAN_POINT('Ctrl Pts',(-55.9485977186156,36.2009205165005,
-218.124206031859));
#191507=CARTESIAN_POINT('Ctrl Pts',(-55.9316558911205,36.193062140815,-218.138917564711));
#191508=CARTESIAN_POINT('Ctrl Pts',(-55.9142960214289,36.1869877564012,
-218.153292102777));
#191509=CARTESIAN_POINT('Ctrl Pts',(-55.8966891686622,36.1829396254735,
-218.167132444769));
#191510=CARTESIAN_POINT('Ctrl Pts',(-55.8858924165189,36.1804572587014,
-218.175619523298));
#191511=CARTESIAN_POINT('Ctrl Pts',(-55.875003635279,36.1787366017489,-218.183906226277));
#191512=CARTESIAN_POINT('Ctrl Pts',(-55.8640697402949,36.177831544681,-218.191953009136));
#191513=CARTESIAN_POINT('Ctrl Pts',(-55.8481788303697,36.1765161689285,
-218.203647899363));
#191514=CARTESIAN_POINT('Ctrl Pts',(-55.8320883840851,36.176950108085,-218.214915947184));
#191515=CARTESIAN_POINT('Ctrl Pts',(-55.815945290253,36.1791009722208,-218.225602523972));
#191516=CARTESIAN_POINT('Ctrl Pts',(-55.7998227364087,36.1812490996618,
-218.23627550348));
#191517=CARTESIAN_POINT('Ctrl Pts',(-55.7836481345545,36.1851096628078,
-218.246368068025));
#191518=CARTESIAN_POINT('Ctrl Pts',(-55.7675980596044,36.190642410556,-218.25576790198));
#191519=CARTESIAN_POINT('Ctrl Pts',(-55.752295973037,36.1959173133376,-218.264729671525));
#191520=CARTESIAN_POINT('Ctrl Pts',(-55.7371077176356,36.2027120043589,
-218.273061888544));
#191521=CARTESIAN_POINT('Ctrl Pts',(-55.722205392293,36.2109865653631,-218.280706779267));
#191522=CARTESIAN_POINT('Ctrl Pts',(-55.7011794829243,36.2226612648305,
-218.2914930677));
#191523=CARTESIAN_POINT('Ctrl Pts',(-55.6806056930362,36.2373092093391,
-218.300970061113));
#191524=CARTESIAN_POINT('Ctrl Pts',(-55.6606091228319,36.2544567781787,
-218.309139768336));
#191525=CARTESIAN_POINT('Ctrl Pts',(-55.6403487815878,36.2718305374108,
-218.317417240647));
#191526=CARTESIAN_POINT('Ctrl Pts',(-55.6206817127348,36.2917701088602,
-218.324352790158));
#191527=CARTESIAN_POINT('Ctrl Pts',(-55.6017333911266,36.313784106472,-218.330001945528));
#191528=CARTESIAN_POINT('Ctrl Pts',(-55.5825988134805,36.336014494752,-218.335706630316));
#191529=CARTESIAN_POINT('Ctrl Pts',(-55.5641978473481,36.3603601160687,
-218.340099821307));
#191530=CARTESIAN_POINT('Ctrl Pts',(-55.5466443792723,36.3863189965771,
-218.34328980866));
#191531=CARTESIAN_POINT('Ctrl Pts',(-55.5287333517844,36.4128066524827,
-218.346544775195));
#191532=CARTESIAN_POINT('Ctrl Pts',(-55.5117053063507,36.4409738003648,
-218.348547462775));
#191533=CARTESIAN_POINT('Ctrl Pts',(-55.4956555114404,36.4702939519707,
-218.349460215191));
#191534=CARTESIAN_POINT('Ctrl Pts',(-55.4908481711963,36.479076116825,-218.349733608804));
#191535=CARTESIAN_POINT('Ctrl Pts',(-55.4861283912204,36.4879617787818,
-218.349909507227));
#191536=CARTESIAN_POINT('Ctrl Pts',(-55.4814981831708,36.4969369346298,
-218.349992971048));
#191537=CARTESIAN_POINT('Ctrl Pts',(-50.0071669705522,43.9054798737905,
-217.102435280211));
#191538=CARTESIAN_POINT('Ctrl Pts',(-49.8012110043674,43.8494770305306,
-216.85723677993));
#191539=CARTESIAN_POINT('Ctrl Pts',(-49.6396803417518,44.1134564636829,
-216.757742122242));
#191540=CARTESIAN_POINT('Ctrl Pts',(-49.8231124216493,43.8554323891537,
-217.268463758512));
#191541=CARTESIAN_POINT('Ctrl Pts',(-49.6176813002303,43.7995722598871,
-217.023443915385));
#191542=CARTESIAN_POINT('Ctrl Pts',(-49.4561530329476,44.062897140813,-216.9238167844));
#191543=CARTESIAN_POINT('Ctrl Pts',(-49.6389254121935,43.8053488862956,
-217.43433427542));
#191544=CARTESIAN_POINT('Ctrl Pts',(-49.4339330913007,43.7496080741896,
-217.18956917487));
#191545=CARTESIAN_POINT('Ctrl Pts',(-49.2724911599438,44.0123032282188,
-217.089736149786));
#191546=CARTESIAN_POINT('Ctrl Pts',(-49.4546085996559,43.7552300878266,
-217.60005));
#191547=CARTESIAN_POINT('Ctrl Pts',(-49.249970603928,43.6995856225942,-217.355612986355));
#191548=CARTESIAN_POINT('Ctrl Pts',(-49.0886970638134,43.9616759445554,
-217.255503157469));
#191549=CARTESIAN_POINT('',(-49.4546085996559,43.7552300878266,-217.60005));
#191550=CARTESIAN_POINT('',(-49.0886970638134,43.9616759445554,-217.255503157469));
#191551=CARTESIAN_POINT('Origin',(-49.3234139960799,44.2377111506597,-217.60005));
#191552=CARTESIAN_POINT('Origin',(243.323155334121,-35.8559000200963,132.120548472853));
#191553=CARTESIAN_POINT('Origin',(245.875985088577,-31.0780147762713,132.706328537592));
#191554=CARTESIAN_POINT('Ctrl Pts',(-49.0178780104163,42.4745424717828,
-218.493732307887));
#191555=CARTESIAN_POINT('Ctrl Pts',(-49.0980960592463,42.6213810568613,
-218.320853182002));
#191556=CARTESIAN_POINT('Ctrl Pts',(-49.2388084250474,42.8138811978774,
-218.342362758509));
#191557=CARTESIAN_POINT('Ctrl Pts',(-48.8091338983078,42.6181464793408,
-218.524253922672));
#191558=CARTESIAN_POINT('Ctrl Pts',(-48.9155380997046,42.7194421825587,
-218.369459248669));
#191559=CARTESIAN_POINT('Ctrl Pts',(-49.0487592764839,42.8836112867869,
-218.360708612845));
#191560=CARTESIAN_POINT('Ctrl Pts',(-48.6016721112025,42.8218000792465,
-218.503396057022));
#191561=CARTESIAN_POINT('Ctrl Pts',(-48.7218532551691,42.8806175866196,
-218.373498979651));
#191562=CARTESIAN_POINT('Ctrl Pts',(-48.8668242681005,42.9907156714763,
-218.348253213533));
#191563=CARTESIAN_POINT('Ctrl Pts',(-48.4661332059182,43.1213427546988,
-218.355050582701));
#191564=CARTESIAN_POINT('Ctrl Pts',(-48.605885875072,43.1153009772418,-218.2644789636));
#191565=CARTESIAN_POINT('Ctrl Pts',(-48.7642205550627,43.1653602564368,
-218.259357276092));
#191566=CARTESIAN_POINT('Ctrl Pts',(-48.4447516601516,43.2015723683891,
-218.304994898973));
#191567=CARTESIAN_POINT('Ctrl Pts',(-48.5891386757002,43.1781849693815,
-218.225378312719));
#191568=CARTESIAN_POINT('Ctrl Pts',(-48.7512938451062,43.2136227234323,
-218.22935608099));
#191569=CARTESIAN_POINT('Ctrl Pts',(-48.4340253069588,43.353231429575,-218.190096441368));
#191570=CARTESIAN_POINT('Ctrl Pts',(-48.5863164838715,43.2954705062034,
-218.133030438493));
#191571=CARTESIAN_POINT('Ctrl Pts',(-48.7558233667416,43.3078094106078,
-218.160482894395));
#191572=CARTESIAN_POINT('Ctrl Pts',(-48.4443958234858,43.4248105481098,
-218.125333427438));
#191573=CARTESIAN_POINT('Ctrl Pts',(-48.6000491587584,43.350341157598,-218.079542364176));
#191574=CARTESIAN_POINT('Ctrl Pts',(-48.7730167596744,43.3537994708901,
-218.121658642789));
#191575=CARTESIAN_POINT('Ctrl Pts',(-48.5123865938013,43.6182701882203,
-217.923222587033));
#191576=CARTESIAN_POINT('Ctrl Pts',(-48.6760379810556,43.4959492709514,
-217.910707343414));
#191577=CARTESIAN_POINT('Ctrl Pts',(-48.8584723261946,43.4820777039722,
-218.00048845563));
#191578=CARTESIAN_POINT('Ctrl Pts',(-48.6035264565663,43.717348604409,-217.781587449044));
#191579=CARTESIAN_POINT('Ctrl Pts',(-48.7709936545123,43.5654352430393,
-217.790234240818));
#191580=CARTESIAN_POINT('Ctrl Pts',(-48.9571822978595,43.553382015829,-217.915564471715));
#191581=CARTESIAN_POINT('Ctrl Pts',(-48.8654374280519,43.8999422120516,
-217.456900727715));
#191582=CARTESIAN_POINT('Ctrl Pts',(-49.0360392072996,43.6817910219716,
-217.51611428222));
#191583=CARTESIAN_POINT('Ctrl Pts',(-49.2307518461237,43.6941518993825,
-217.720864823318));
#191584=CARTESIAN_POINT('Ctrl Pts',(-49.0543447941743,43.9629792153545,
-217.278009186719));
#191585=CARTESIAN_POINT('Ctrl Pts',(-49.2254032660268,43.7067173749548,
-217.366834723765));
#191586=CARTESIAN_POINT('Ctrl Pts',(-49.4213823984297,43.752590477188,-217.613522274393));
#191587=CARTESIAN_POINT('Ctrl Pts',(-49.2609648429284,44.000805570189,-217.106705723199));
#191588=CARTESIAN_POINT('Ctrl Pts',(-49.4167540467718,43.705944922211,-217.235986860284));
#191589=CARTESIAN_POINT('Ctrl Pts',(-49.626471378184,43.7968795640925,-217.51089121997));
#191590=CARTESIAN_POINT('Ctrl Pts',(-49.0801870931398,42.8824343798319,
-218.350025764149));
#191591=CARTESIAN_POINT('Ctrl Pts',(-48.9534766000575,42.9465755146882,
-218.349260885044));
#191592=CARTESIAN_POINT('Ctrl Pts',(-48.8452234864083,43.0274829525206,
-218.329538279335));
#191593=CARTESIAN_POINT('Ctrl Pts',(-48.7642205550627,43.1653602564368,
-218.259357276092));
#191594=CARTESIAN_POINT('Ctrl Pts',(-48.7512938451062,43.2136227234323,
-218.22935608099));
#191595=CARTESIAN_POINT('Ctrl Pts',(-48.7558233667416,43.3078094106078,
-218.160482894395));
#191596=CARTESIAN_POINT('Ctrl Pts',(-48.7730167596744,43.3537994708901,
-218.121658642789));
#191597=CARTESIAN_POINT('Ctrl Pts',(-48.8584723261946,43.4820777039722,
-218.00048845563));
#191598=CARTESIAN_POINT('Ctrl Pts',(-48.9571822978595,43.553382015829,-217.915564471715));
#191599=CARTESIAN_POINT('Ctrl Pts',(-49.185156921413,43.6706902521236,-217.753314764718));
#191600=CARTESIAN_POINT('Ctrl Pts',(-49.3149852106482,43.7172641725154,
-217.675369628552));
#191601=CARTESIAN_POINT('Ctrl Pts',(-49.4546085996559,43.7552300878266,
-217.60005));
#191602=CARTESIAN_POINT('Ctrl Pts',(-49.0886970638135,43.9616759445554,
-217.255503157469));
#191603=CARTESIAN_POINT('Ctrl Pts',(-48.9996384348295,43.9371441712379,
-217.335826637108));
#191604=CARTESIAN_POINT('Ctrl Pts',(-48.9153759396057,43.9062608655704,
-217.417907561279));
#191605=CARTESIAN_POINT('Ctrl Pts',(-48.8376533259605,43.867295402887,-217.502023817251));
#191606=CARTESIAN_POINT('Ctrl Pts',(-48.7938257341564,43.8453228737497,
-217.54945676833));
#191607=CARTESIAN_POINT('Ctrl Pts',(-48.7520786392416,43.8207798060945,
-217.597536915137));
#191608=CARTESIAN_POINT('Ctrl Pts',(-48.7127298749802,43.7933510418827,
-217.646314085193));
#191609=CARTESIAN_POINT('Ctrl Pts',(-48.650249816921,43.7497981930802,-217.7237650668));
#191610=CARTESIAN_POINT('Ctrl Pts',(-48.5936606238927,43.6987010978059,
-217.803297027915));
#191611=CARTESIAN_POINT('Ctrl Pts',(-48.5481954561807,43.6387791465335,
-217.882424454102));
#191612=CARTESIAN_POINT('Ctrl Pts',(-48.5142503744661,43.5940403798072,
-217.941502361058));
#191613=CARTESIAN_POINT('Ctrl Pts',(-48.4865083692682,43.5443812052436,
-218.000354765105));
#191614=CARTESIAN_POINT('Ctrl Pts',(-48.4671318833214,43.4892557804674,
-218.057947213938));
#191615=CARTESIAN_POINT('Ctrl Pts',(-48.451525691629,43.4448567109691,-218.104333271708));
#191616=CARTESIAN_POINT('Ctrl Pts',(-48.4417433467026,43.3970966887457,
-218.149483053803));
#191617=CARTESIAN_POINT('Ctrl Pts',(-48.4389192647052,43.3468995389881,
-218.191860029397));
#191618=CARTESIAN_POINT('Ctrl Pts',(-48.4376420131691,43.3241968034818,
-218.211025923738));
#191619=CARTESIAN_POINT('Ctrl Pts',(-48.4377874434161,43.3009957695441,
-218.229624642104));
#191620=CARTESIAN_POINT('Ctrl Pts',(-48.4394571325143,43.2773831398461,
-218.247514037176));
#191621=CARTESIAN_POINT('Ctrl Pts',(-48.4431471229734,43.2251995456732,
-218.287049359771));
#191622=CARTESIAN_POINT('Ctrl Pts',(-48.4544207656835,43.1709349171637,
-218.323082627899));
#191623=CARTESIAN_POINT('Ctrl Pts',(-48.4727225097299,43.1164732147517,
-218.354432513868));
#191624=CARTESIAN_POINT('Ctrl Pts',(-48.4810127962298,43.0918032644386,
-218.368633320947));
#191625=CARTESIAN_POINT('Ctrl Pts',(-48.4907445774782,43.0670933250239,
-218.381873149416));
#191626=CARTESIAN_POINT('Ctrl Pts',(-48.5018636359549,43.0425207969075,
-218.394042199469));
#191627=CARTESIAN_POINT('Ctrl Pts',(-48.5333210340713,42.9730016194245,
-218.428470173117));
#191628=CARTESIAN_POINT('Ctrl Pts',(-48.575477165605,42.9051779351441,-218.45412189569));
#191629=CARTESIAN_POINT('Ctrl Pts',(-48.6249680219686,42.8403879458241,
-218.472156073002));
#191630=CARTESIAN_POINT('Ctrl Pts',(-48.6690863768606,42.7826312620184,
-218.48823254234));
#191631=CARTESIAN_POINT('Ctrl Pts',(-48.7190328297175,42.7272860740426,
-218.498255550998));
#191632=CARTESIAN_POINT('Ctrl Pts',(-48.7724676216828,42.675306362178,-218.503045934624));
#191633=CARTESIAN_POINT('Ctrl Pts',(-48.7950121526649,42.6533757401717,
-218.505067032641));
#191634=CARTESIAN_POINT('Ctrl Pts',(-48.8181782375201,42.6320442164686,
-218.506156693031));
#191635=CARTESIAN_POINT('Ctrl Pts',(-48.8417930108281,42.6113834075459,
-218.506376562157));
#191636=CARTESIAN_POINT('Origin',(2.81802535037841,-9.69927298715315,-227.60005));
#191637=CARTESIAN_POINT('',(-48.1633319901564,41.4530789012665,-228.35005));
#191638=CARTESIAN_POINT('',(-48.1633319901564,41.4530789012665,-228.35005));
#191639=CARTESIAN_POINT('',(-47.632114758242,41.9825203546087,-227.60005));
#191640=CARTESIAN_POINT('Origin',(-48.1633319901564,41.4530789012665,-227.60005));
#191641=CARTESIAN_POINT('',(-41.9598150400404,36.2911954009805,-227.60005));
#191642=CARTESIAN_POINT('Ctrl Pts',(-49.7021444432209,42.0348313420379,
-227.60005));
#191643=CARTESIAN_POINT('Ctrl Pts',(-48.6421799545279,42.9959733704936,
-227.60005));
#191644=CARTESIAN_POINT('Ctrl Pts',(-47.6321147582419,41.9825203546088,
-227.60005));
#191645=CARTESIAN_POINT('Ctrl Pts',(-49.7021444432209,42.0348313420379,
-228.35005));
#191646=CARTESIAN_POINT('Ctrl Pts',(-48.6421799545279,42.9959733704936,
-228.35005));
#191647=CARTESIAN_POINT('Ctrl Pts',(-47.6321147582419,41.9825203546088,
-228.35005));
#191648=CARTESIAN_POINT('Ctrl Pts',(-49.1983468326458,41.479234394981,-228.35005));
#191649=CARTESIAN_POINT('Ctrl Pts',(-48.6683645882994,41.9598054092088,
-228.35005));
#191650=CARTESIAN_POINT('Ctrl Pts',(-48.1633319901564,41.4530789012665,
-228.35005));
#191651=CARTESIAN_POINT('',(-49.7021444432209,42.0348313420379,-227.60005));
#191652=CARTESIAN_POINT('Origin',(-48.6945492220708,40.9236374479242,-227.60005));
#191653=CARTESIAN_POINT('',(-49.1983468326459,41.4792343949811,-228.35005));
#191654=CARTESIAN_POINT('Origin',(-48.6945492220708,40.9236374479242,-228.35005));
#191655=CARTESIAN_POINT('Origin',(-49.1983468326459,41.4792343949811,-227.60005));
#191656=CARTESIAN_POINT('Origin',(-0.128459562639233,-12.6359082483571,
-227.60005));
#191657=CARTESIAN_POINT('',(-54.0789914828443,36.6149049990089,-228.35005));
#191658=CARTESIAN_POINT('Origin',(-0.128459562639233,-12.6359082483571,
-228.35005));
#191659=CARTESIAN_POINT('',(-54.6328983814091,37.1205601658197,-227.60005));
#191660=CARTESIAN_POINT('Origin',(-54.0789914828443,36.6149049990089,-227.60005));
#191661=CARTESIAN_POINT('Origin',(-0.128459562639233,-12.6359082483571,
-227.60005));
#191662=CARTESIAN_POINT('Origin',(-0.128459562639233,-12.6359082483571,
-228.35005));
#191663=CARTESIAN_POINT('Ctrl Pts',(-54.5875190481084,35.0503669255137,
-227.60005));
#191664=CARTESIAN_POINT('Ctrl Pts',(-55.5975842443944,36.0638199413983,
-227.60005));
#191665=CARTESIAN_POINT('Ctrl Pts',(-54.6328983814091,37.1205601658197,
-227.60005));
#191666=CARTESIAN_POINT('Ctrl Pts',(-54.5875190481084,35.0503669255137,
-228.35005));
#191667=CARTESIAN_POINT('Ctrl Pts',(-55.5975842443944,36.0638199413983,
-228.35005));
#191668=CARTESIAN_POINT('Ctrl Pts',(-54.6328983814091,37.1205601658197,
-228.35005));
#191669=CARTESIAN_POINT('Ctrl Pts',(-54.056301816194,35.579808378856,-228.35005));
#191670=CARTESIAN_POINT('Ctrl Pts',(-54.5613344143369,36.0865348867983,
-228.35005));
#191671=CARTESIAN_POINT('Ctrl Pts',(-54.0789914828443,36.614904999009,-228.35005));
#191672=CARTESIAN_POINT('',(-54.5875190481084,35.0503669255136,-227.60005));
#191673=CARTESIAN_POINT('',(-54.056301816194,35.579808378856,-228.35005));
#191674=CARTESIAN_POINT('Origin',(-54.056301816194,35.579808378856,-227.60005));
#191675=CARTESIAN_POINT('Origin',(-53.5250845842796,36.1092498321983,-227.60005));
#191676=CARTESIAN_POINT('Origin',(-53.5250845842796,36.1092498321983,-228.35005));
#191677=CARTESIAN_POINT('Origin',(-3.07494447565784,-15.5725435095623,-227.60005));
#191678=CARTESIAN_POINT('',(-54.5875190481084,35.0503669255136,-227.60005));
#191679=CARTESIAN_POINT('',(-48.3142830765682,29.8185305620001,-228.35005));
#191680=CARTESIAN_POINT('Origin',(10.7603008067452,26.6045648983079,-217.60005));
#191681=CARTESIAN_POINT('',(-51.0024097331414,43.3988703109923,-218.35005));
#191682=CARTESIAN_POINT('',(10.7603008067452,26.6045648983079,-218.35005));
#191683=CARTESIAN_POINT('',(-50.8056178277775,44.122591905242,-217.60005));
#191684=CARTESIAN_POINT('Origin',(-51.0024097331414,43.3988703109923,-217.60005));
#191685=CARTESIAN_POINT('',(-51.6000409161409,44.3386087195339,-217.60005));
#191686=CARTESIAN_POINT('Ctrl Pts',(-52.2148720050704,43.7789665035542,
-217.60005));
#191687=CARTESIAN_POINT('Ctrl Pts',(-51.6051500510689,44.3399979780626,
-217.60005));
#191688=CARTESIAN_POINT('Ctrl Pts',(-50.8056178277775,44.1225919052419,
-217.60005));
#191689=CARTESIAN_POINT('Ctrl Pts',(-52.2148720050704,43.7789665035542,
-218.35005));
#191690=CARTESIAN_POINT('Ctrl Pts',(-51.6051500510689,44.3399979780626,
-218.35005));
#191691=CARTESIAN_POINT('Ctrl Pts',(-50.8056178277775,44.1225919052419,
-218.35005));
#191692=CARTESIAN_POINT('Ctrl Pts',(-51.7070368217878,43.2270576101484,
-218.35005));
#191693=CARTESIAN_POINT('Ctrl Pts',(-51.4021758447871,43.5075733474026,
-218.35005));
#191694=CARTESIAN_POINT('Ctrl Pts',(-51.0024097331414,43.3988703109923,
-218.35005));
#191695=CARTESIAN_POINT('',(-52.2148720050704,43.7789665035542,-217.60005));
#191696=CARTESIAN_POINT('Origin',(-51.1992016385053,42.6751487167426,-217.60005));
#191697=CARTESIAN_POINT('',(-51.7070368217878,43.2270576101484,-218.35005));
#191698=CARTESIAN_POINT('Origin',(-51.1992016385053,42.6751487167426,-218.35005));
#191699=CARTESIAN_POINT('Origin',(-51.7070368217878,43.2270576101484,-217.60005));
#191700=CARTESIAN_POINT('Origin',(0.,-12.9675000200281,-217.60005));
#191701=CARTESIAN_POINT('',(-56.3587426896623,39.6656306474361,-217.60005));
#191702=CARTESIAN_POINT('',(-55.8106047487975,39.1537275337666,-218.35005));
#191703=CARTESIAN_POINT('Origin',(-55.8106047487975,39.1537275337666,-217.60005));
#191704=CARTESIAN_POINT('Origin',(0.,-12.9675000200281,-217.60005));
#191705=CARTESIAN_POINT('Origin',(0.,-12.9675000200281,-218.35005));
#191706=CARTESIAN_POINT('Ctrl Pts',(-56.7127812850717,38.2589564044561,
-217.60005));
#191707=CARTESIAN_POINT('Ctrl Pts',(-56.9242682147177,39.0600746573811,
-217.60005));
#191708=CARTESIAN_POINT('Ctrl Pts',(-56.3587426896623,39.6656306474361,
-217.60005));
#191709=CARTESIAN_POINT('Ctrl Pts',(-56.7127812850717,38.2589564044561,
-218.35005));
#191710=CARTESIAN_POINT('Ctrl Pts',(-56.9242682147177,39.0600746573811,
-218.35005));
#191711=CARTESIAN_POINT('Ctrl Pts',(-56.3587426896623,39.6656306474361,
-218.35005));
#191712=CARTESIAN_POINT('Ctrl Pts',(-55.9876240465022,38.4503904122767,
-218.35005));
#191713=CARTESIAN_POINT('Ctrl Pts',(-56.0933675113252,38.8509495387392,
-218.35005));
#191714=CARTESIAN_POINT('Ctrl Pts',(-55.8106047487975,39.1537275337666,
-218.35005));
#191715=CARTESIAN_POINT('',(-56.7127812850717,38.2589564044561,-217.60005));
#191716=CARTESIAN_POINT('',(-55.9876240465022,38.4503904122767,-218.35005));
#191717=CARTESIAN_POINT('Origin',(-55.9876240465022,38.4503904122767,-217.60005));
#191718=CARTESIAN_POINT('Origin',(-55.2624668079327,38.6418244200972,-217.60005));
#191719=CARTESIAN_POINT('Origin',(-55.2624668079327,38.6418244200972,-218.35005));
#191720=CARTESIAN_POINT('Origin',(-39.6505639028577,-23.4348386281926,-217.60005));
#191721=CARTESIAN_POINT('',(-51.3278340104563,17.8606293780317,-217.60005));
#191722=CARTESIAN_POINT('',(-39.6505639028577,-23.4348386281926,-218.35005));
#191723=CARTESIAN_POINT('Origin',(-39.6266165499379,-2.40986505017056,-217.60005));
#191724=CARTESIAN_POINT('',(-56.1046081325044,-64.2577178902918,-218.35005));
#191725=CARTESIAN_POINT('',(-56.1046081325044,-64.2577178902918,-218.35005));
#191726=CARTESIAN_POINT('',(-56.8293274051384,-64.0646324794683,-217.60005));
#191727=CARTESIAN_POINT('Origin',(-56.1046081325044,-64.2577178902918,-217.60005));
#191728=CARTESIAN_POINT('',(-56.0236521904458,-61.0406424582598,-217.60005));
#191729=CARTESIAN_POINT('Ctrl Pts',(-56.1046081325044,-64.2577178902918,
-218.35005));
#191730=CARTESIAN_POINT('Ctrl Pts',(-56.2112637919648,-64.658035095081,
-218.35005));
#191731=CARTESIAN_POINT('Ctrl Pts',(-55.9291914878272,-64.9614564347782,
-218.35005));
#191732=CARTESIAN_POINT('Ctrl Pts',(-56.8293274051384,-64.0646324794683,
-218.35005));
#191733=CARTESIAN_POINT('Ctrl Pts',(-57.0426387240591,-64.8652668890467,
-218.35005));
#191734=CARTESIAN_POINT('Ctrl Pts',(-56.478494115784,-65.4721095684411,
-218.35005));
#191735=CARTESIAN_POINT('Ctrl Pts',(-56.8293274051384,-64.0646324794683,
-217.60005));
#191736=CARTESIAN_POINT('Ctrl Pts',(-57.0426387240591,-64.8652668890467,
-217.60005));
#191737=CARTESIAN_POINT('Ctrl Pts',(-56.478494115784,-65.4721095684411,
-217.60005));
#191738=CARTESIAN_POINT('',(-56.478494115784,-65.4721095684411,-217.60005));
#191739=CARTESIAN_POINT('',(-55.9291914878272,-64.9614564347782,-218.35005));
#191740=CARTESIAN_POINT('Origin',(-55.9291914878272,-64.9614564347782,-217.60005));
#191741=CARTESIAN_POINT('Origin',(-55.3798888598704,-64.4508033011153,-217.60005));
#191742=CARTESIAN_POINT('Origin',(-55.3798888598704,-64.4508033011153,-218.35005));
#191743=CARTESIAN_POINT('Origin',(0.,-12.9675000200281,-217.60005));
#191744=CARTESIAN_POINT('',(-52.3440043138885,-69.594874440935,-217.60005));
#191745=CARTESIAN_POINT('',(-51.8349132062458,-69.0441238221254,-218.35005));
#191746=CARTESIAN_POINT('Origin',(-51.8349132062458,-69.0441238221255,-217.60005));
#191747=CARTESIAN_POINT('Origin',(0.,-12.9675000200281,-217.60005));
#191748=CARTESIAN_POINT('Origin',(0.,-12.9675000200281,-218.35005));
#191749=CARTESIAN_POINT('Ctrl Pts',(-51.8349132062458,-69.0441238221254,
-218.35005));
#191750=CARTESIAN_POINT('Ctrl Pts',(-51.5306920318089,-69.3253333012854,
-218.35005));
#191751=CARTESIAN_POINT('Ctrl Pts',(-51.1306793331593,-69.2175412094409,
-218.35005));
#191752=CARTESIAN_POINT('Ctrl Pts',(-52.3440043138886,-69.5948744409349,
-218.35005));
#191753=CARTESIAN_POINT('Ctrl Pts',(-51.7355619650149,-70.1572933992548,
-218.35005));
#191754=CARTESIAN_POINT('Ctrl Pts',(-50.9355365677156,-69.9417092155658,
-218.35005));
#191755=CARTESIAN_POINT('Ctrl Pts',(-52.3440043138886,-69.5948744409349,
-217.60005));
#191756=CARTESIAN_POINT('Ctrl Pts',(-51.7355619650149,-70.1572933992548,
-217.60005));
#191757=CARTESIAN_POINT('Ctrl Pts',(-50.9355365677156,-69.9417092155658,
-217.60005));
#191758=CARTESIAN_POINT('',(-51.1306793331593,-69.2175412094409,-218.35005));
#191759=CARTESIAN_POINT('Origin',(-51.325822098603,-68.4933732033159,-218.35005));
#191760=CARTESIAN_POINT('',(-50.9355365677156,-69.9417092155658,-217.60005));
#191761=CARTESIAN_POINT('Origin',(-51.1306793331593,-69.2175412094409,-217.60005));
#191762=CARTESIAN_POINT('Origin',(-51.325822098603,-68.4933732033159,-217.60005));
#191763=CARTESIAN_POINT('Origin',(10.6701281871898,-52.5639741032288,-217.60005));
#191764=CARTESIAN_POINT('',(-50.9355365677156,-69.9417092155658,-217.60005));
#191765=CARTESIAN_POINT('',(-48.0054978778587,-68.3753933286417,-218.35005));
#191766=CARTESIAN_POINT('Origin',(-3.09688044790867,-9.95712216328114,-227.60005));
#191767=CARTESIAN_POINT('',(-53.6770468827139,-61.5062120042031,-228.35005));
#191768=CARTESIAN_POINT('',(-3.09688044790867,-9.95712216328114,-228.35005));
#191769=CARTESIAN_POINT('',(-54.2123842387114,-60.9809369188682,-227.60005));
#191770=CARTESIAN_POINT('Origin',(-53.6770468827139,-61.5062120042031,-227.60005));
#191771=CARTESIAN_POINT('',(-55.2047656166361,-61.9923285455256,-227.60005));
#191772=CARTESIAN_POINT('Ctrl Pts',(-53.6770468827138,-61.5062120042031,
-228.35005));
#191773=CARTESIAN_POINT('Ctrl Pts',(-54.1781051950386,-62.0168686860244,
-228.35005));
#191774=CARTESIAN_POINT('Ctrl Pts',(-53.6916490178651,-62.5414543003222,
-228.35005));
#191775=CARTESIAN_POINT('Ctrl Pts',(-54.2123842387114,-60.9809369188682,
-228.35005));
#191776=CARTESIAN_POINT('Ctrl Pts',(-55.2145008633609,-62.0022502825108,
-228.35005));
#191777=CARTESIAN_POINT('Ctrl Pts',(-54.2415885090139,-63.0514215111064,
-228.35005));
#191778=CARTESIAN_POINT('Ctrl Pts',(-54.2123842387114,-60.9809369188682,
-227.60005));
#191779=CARTESIAN_POINT('Ctrl Pts',(-55.2145008633609,-62.0022502825108,
-227.60005));
#191780=CARTESIAN_POINT('Ctrl Pts',(-54.2415885090139,-63.0514215111064,
-227.60005));
#191781=CARTESIAN_POINT('',(-54.2415885090138,-63.0514215111064,-227.60005));
#191782=CARTESIAN_POINT('',(-53.6916490178651,-62.5414543003222,-228.35005));
#191783=CARTESIAN_POINT('Origin',(-53.6916490178651,-62.5414543003222,-227.60005));
#191784=CARTESIAN_POINT('Origin',(-53.1417095267163,-62.031487089538,-227.60005));
#191785=CARTESIAN_POINT('Origin',(-53.1417095267163,-62.031487089538,-228.35005));
#191786=CARTESIAN_POINT('Origin',(-0.127542579976414,-12.8706479699377,
-227.60005));
#191787=CARTESIAN_POINT('',(-49.2725916132775,-67.9270204940557,-227.60005));
#191788=CARTESIAN_POINT('',(-48.7731500580611,-67.3675045131195,-228.35005));
#191789=CARTESIAN_POINT('Origin',(-48.7731500580611,-67.3675045131195,-227.60005));
#191790=CARTESIAN_POINT('Origin',(-0.127542579976414,-12.8706479699377,
-227.60005));
#191791=CARTESIAN_POINT('Origin',(-0.127542579976414,-12.8706479699377,
-228.35005));
#191792=CARTESIAN_POINT('Ctrl Pts',(-48.7731500580611,-67.3675045131195,
-228.35005));
#191793=CARTESIAN_POINT('Ctrl Pts',(-48.2394294591717,-67.8439202993396,
-228.35005));
#191794=CARTESIAN_POINT('Ctrl Pts',(-47.738371146847,-67.3332636175182,
-228.35005));
#191795=CARTESIAN_POINT('Ctrl Pts',(-49.2725916132776,-67.9270204940556,
-228.35005));
#191796=CARTESIAN_POINT('Ctrl Pts',(-48.2051504154989,-68.8798520664959,
-228.35005));
#191797=CARTESIAN_POINT('Ctrl Pts',(-47.2030337908494,-67.858538702853,
-228.35005));
#191798=CARTESIAN_POINT('Ctrl Pts',(-49.2725916132776,-67.9270204940556,
-227.60005));
#191799=CARTESIAN_POINT('Ctrl Pts',(-48.2051504154989,-68.8798520664959,
-227.60005));
#191800=CARTESIAN_POINT('Ctrl Pts',(-47.2030337908494,-67.858538702853,
-227.60005));
#191801=CARTESIAN_POINT('',(-47.738371146847,-67.3332636175182,-228.35005));
#191802=CARTESIAN_POINT('Origin',(-48.2737085028446,-66.8079885321834,-228.35005));
#191803=CARTESIAN_POINT('',(-47.2030337908494,-67.858538702853,-227.60005));
#191804=CARTESIAN_POINT('Origin',(-47.738371146847,-67.3332636175182,-227.60005));
#191805=CARTESIAN_POINT('Origin',(-48.2737085028446,-66.8079885321834,-227.60005));
#191806=CARTESIAN_POINT('Origin',(2.84179528795572,-15.7841737765938,-227.60005));
#191807=CARTESIAN_POINT('',(-48.1954151687739,-68.8699303295103,-227.60005));
#191808=CARTESIAN_POINT('',(2.84179528795573,-15.7841737765938,-228.35005));
#191809=CARTESIAN_POINT('Origin',(-55.2624668079327,38.6418244200972,-167.906149834141));
#191810=CARTESIAN_POINT('',(-56.3587426896623,39.6656306474361,-167.906149834141));
#191811=CARTESIAN_POINT('',(-56.7127812850717,38.2589564044561,-167.906149834141));
#191812=CARTESIAN_POINT('Origin',(-51.1992016385053,42.6751487167426,-167.906149834141));
#191813=CARTESIAN_POINT('',(-50.8056178277775,44.1225919052419,-167.906149834141));
#191814=CARTESIAN_POINT('',(-52.2148720050704,43.7789665035542,-167.906149834141));
#191815=CARTESIAN_POINT('Origin',(-53.5250845842796,36.1092498321983,-228.35005));
#191816=CARTESIAN_POINT('',(-54.6328983814091,37.1205601658197,-228.35005));
#191817=CARTESIAN_POINT('',(-54.5875190481084,35.0503669255136,-228.35005));
#191818=CARTESIAN_POINT('Origin',(-48.6945492220708,40.9236374479242,-228.35005));
#191819=CARTESIAN_POINT('',(-47.632114758242,41.9825203546087,-228.35005));
#191820=CARTESIAN_POINT('',(-49.7021444432209,42.0348313420379,-228.35005));
#191821=CARTESIAN_POINT('Origin',(-53.1417095267163,-62.031487089538,-228.35005));
#191822=CARTESIAN_POINT('',(-54.2123842387114,-60.9809369188682,-228.35005));
#191823=CARTESIAN_POINT('',(-54.2415885090138,-63.0514215111064,-228.35005));
#191824=CARTESIAN_POINT('Origin',(-48.2737085028446,-66.8079885321834,-228.35005));
#191825=CARTESIAN_POINT('',(-47.2030337908494,-67.858538702853,-228.35005));
#191826=CARTESIAN_POINT('',(-49.2725916132775,-67.9270204940557,-228.35005));
#191827=CARTESIAN_POINT('Origin',(-51.325822098603,-68.4933732033159,-167.906149834141));
#191828=CARTESIAN_POINT('',(-52.3440043138885,-69.594874440935,-167.906149834141));
#191829=CARTESIAN_POINT('',(-50.9355365677156,-69.9417092155658,-167.906149834141));
#191830=CARTESIAN_POINT('Origin',(-55.3798888598704,-64.4508033011153,-167.906149834141));
#191831=CARTESIAN_POINT('',(-56.8293274051384,-64.0646324794683,-167.906149834141));
#191832=CARTESIAN_POINT('',(-56.478494115784,-65.4721095684411,-167.906149834141));
#191833=CARTESIAN_POINT('Origin',(-21.5,29.0311209585238,-234.90005));
#191834=CARTESIAN_POINT('',(-21.6266284449832,30.2244211038859,-235.35005));
#191835=CARTESIAN_POINT('',(-20.3,29.0311209585238,-235.35005));
#191836=CARTESIAN_POINT('Origin',(-21.5,29.0311209585238,-235.35005));
#191837=CARTESIAN_POINT('',(-20.75,29.0311209585238,-234.90005));
#191838=CARTESIAN_POINT('Origin',(-20.3,29.0311209585238,-234.90005));
#191839=CARTESIAN_POINT('',(-21.5791427781145,29.7769335493751,-234.90005));
#191840=CARTESIAN_POINT('Origin',(-21.5,29.0311209585238,-234.90005));
#191841=CARTESIAN_POINT('Origin',(-21.6266284449832,30.2244211038859,-234.90005));
#191842=CARTESIAN_POINT('Origin',(-20.3,-25.4138432731711,-234.90005));
#191843=CARTESIAN_POINT('',(-20.75,21.5631368321642,-234.90005));
#191844=CARTESIAN_POINT('',(-20.3,21.5631368321642,-235.35005));
#191845=CARTESIAN_POINT('Origin',(-20.3,21.5631368321642,-234.90005));
#191846=CARTESIAN_POINT('',(-20.75,29.0311209585238,-234.90005));
#191847=CARTESIAN_POINT('',(-20.3,21.5631368321642,-235.35005));
#191848=CARTESIAN_POINT('Origin',(2.61456814389029E-14,-173.57701443073,
-234.90005));
#191849=CARTESIAN_POINT('',(-25.0152849219089,29.8362882417925,-235.35005));
#191850=CARTESIAN_POINT('',(-24.960358769668,29.3896529120211,-234.90005));
#191851=CARTESIAN_POINT('Origin',(-25.0152849219089,29.8362882417925,-234.90005));
#191852=CARTESIAN_POINT('Origin',(2.61456814389029E-14,-173.57701443073,
-235.35005));
#191853=CARTESIAN_POINT('Origin',(2.61456814389029E-14,-173.57701443073,
-234.90005));
#191854=CARTESIAN_POINT('Origin',(-21.5,21.5631368321642,-234.90005));
#191855=CARTESIAN_POINT('',(-21.5,20.8131368321642,-234.90005));
#191856=CARTESIAN_POINT('',(-21.5,20.3631368321642,-235.35005));
#191857=CARTESIAN_POINT('Origin',(-21.5,20.3631368321642,-234.90005));
#191858=CARTESIAN_POINT('Origin',(-21.5,21.5631368321642,-234.90005));
#191859=CARTESIAN_POINT('Origin',(-21.5,21.5631368321642,-235.35005));
#191860=CARTESIAN_POINT('Origin',(-24.838300653577,28.3971299569735,-234.90005));
#191861=CARTESIAN_POINT('',(-25.604588652464,29.6281062779325,-235.35005));
#191862=CARTESIAN_POINT('',(-25.366775135568,29.2460791438418,-234.90005));
#191863=CARTESIAN_POINT('Origin',(-25.604588652464,29.6281062779325,-234.90005));
#191864=CARTESIAN_POINT('Origin',(-24.838300653577,28.3971299569735,-235.35005));
#191865=CARTESIAN_POINT('Origin',(-24.838300653577,28.3971299569735,-234.90005));
#191866=CARTESIAN_POINT('Origin',(296.501483394397,20.3631368321642,-234.90005));
#191867=CARTESIAN_POINT('',(-29.125,20.8131368321642,-234.90005));
#191868=CARTESIAN_POINT('',(-29.125,20.3631368321642,-235.35005));
#191869=CARTESIAN_POINT('Origin',(-29.125,20.3631368321642,-234.90005));
#191870=CARTESIAN_POINT('',(1.23757166668304E-15,20.8131368321642,-234.90005));
#191871=CARTESIAN_POINT('',(296.501483394397,20.3631368321642,-235.35005));
#191872=CARTESIAN_POINT('Origin',(6.29739814579425E-15,-11.5034818258363,
-234.90005));
#191873=CARTESIAN_POINT('',(-29.8646825396825,26.6475763089516,-235.35005));
#191874=CARTESIAN_POINT('',(-29.5873015873016,26.2932321157492,-234.90005));
#191875=CARTESIAN_POINT('Origin',(-29.8646825396825,26.6475763089516,-234.90005));
#191876=CARTESIAN_POINT('Origin',(6.29739814579425E-15,-11.5034818258363,
-235.35005));
#191877=CARTESIAN_POINT('Origin',(6.29739814579425E-15,-11.5034818258363,
-234.90005));
#191878=CARTESIAN_POINT('Origin',(-29.125,21.5631368321642,-234.90005));
#191879=CARTESIAN_POINT('',(-29.875,21.5631368321642,-234.90005));
#191880=CARTESIAN_POINT('',(-30.325,21.5631368321642,-235.35005));
#191881=CARTESIAN_POINT('Origin',(-30.325,21.5631368321642,-234.90005));
#191882=CARTESIAN_POINT('Origin',(-29.125,21.5631368321642,-234.90005));
#191883=CARTESIAN_POINT('Origin',(-29.125,21.5631368321642,-235.35005));
#191884=CARTESIAN_POINT('Origin',(-29.125,25.702658460412,-234.90005));
#191885=CARTESIAN_POINT('',(-30.325,25.702658460412,-235.35005));
#191886=CARTESIAN_POINT('',(-29.875,25.702658460412,-234.90005));
#191887=CARTESIAN_POINT('Origin',(-30.325,25.702658460412,-234.90005));
#191888=CARTESIAN_POINT('Origin',(-29.125,25.702658460412,-235.35005));
#191889=CARTESIAN_POINT('Origin',(-29.125,25.702658460412,-234.90005));
#191890=CARTESIAN_POINT('Origin',(-30.325,-25.4138432731711,-234.90005));
#191891=CARTESIAN_POINT('',(-30.325,25.702658460412,-235.35005));
#191892=CARTESIAN_POINT('',(-29.875,21.5631368321642,-234.90005));
#191893=CARTESIAN_POINT('Origin',(-11.3749999999999,29.8508988479304,-234.90005));
#191894=CARTESIAN_POINT('',(-11.4419952819386,31.0490272351235,-235.35005));
#191895=CARTESIAN_POINT('',(-10.1749999999999,29.8508988479304,-235.35005));
#191896=CARTESIAN_POINT('Origin',(-11.3749999999999,29.8508988479304,-235.35005));
#191897=CARTESIAN_POINT('',(-10.6249999999999,29.8508988479304,-234.90005));
#191898=CARTESIAN_POINT('Origin',(-10.1749999999999,29.8508988479304,-234.90005));
#191899=CARTESIAN_POINT('',(-11.4168720512116,30.5997290899261,-234.90005));
#191900=CARTESIAN_POINT('Origin',(-11.3749999999999,29.8508988479304,-234.90005));
#191901=CARTESIAN_POINT('Origin',(-11.4419952819386,31.0490272351235,-234.90005));
#191902=CARTESIAN_POINT('Origin',(-10.1749999999999,-25.4138432731711,-234.90005));
#191903=CARTESIAN_POINT('',(-10.6249999999999,21.5631368321642,-234.90005));
#191904=CARTESIAN_POINT('',(-10.1749999999999,21.5631368321642,-235.35005));
#191905=CARTESIAN_POINT('Origin',(-10.1749999999999,21.5631368321642,-234.90005));
#191906=CARTESIAN_POINT('',(-10.6249999999999,29.8508988479304,-234.90005));
#191907=CARTESIAN_POINT('',(-10.1749999999999,21.5631368321642,-235.35005));
#191908=CARTESIAN_POINT('Origin',(2.61456814389029E-14,-173.57701443073,
-234.90005));
#191909=CARTESIAN_POINT('',(-19.1119042071944,30.4756045219376,-235.35005));
#191910=CARTESIAN_POINT('',(-19.0699401294965,30.0275654430807,-234.90005));
#191911=CARTESIAN_POINT('Origin',(-19.1119042071944,30.4756045219376,-234.90005));
#191912=CARTESIAN_POINT('Origin',(2.61456814389029E-14,-173.57701443073,
-235.35005));
#191913=CARTESIAN_POINT('Origin',(2.61456814389029E-14,-173.57701443073,
-234.90005));
#191914=CARTESIAN_POINT('Origin',(-11.3749999999999,21.5631368321642,-234.90005));
#191915=CARTESIAN_POINT('',(-11.3749999999999,20.8131368321642,-234.90005));
#191916=CARTESIAN_POINT('',(-11.3749999999999,20.3631368321642,-235.35005));
#191917=CARTESIAN_POINT('Origin',(-11.3749999999999,20.3631368321642,-234.90005));
#191918=CARTESIAN_POINT('Origin',(-11.3749999999999,21.5631368321642,-234.90005));
#191919=CARTESIAN_POINT('Origin',(-11.3749999999999,21.5631368321642,-235.35005));
#191920=CARTESIAN_POINT('Origin',(-19.,29.2808336449858,-234.90005));
#191921=CARTESIAN_POINT('',(-20.2,29.2808336449858,-235.35005));
#191922=CARTESIAN_POINT('',(-19.75,29.2808336449858,-234.90005));
#191923=CARTESIAN_POINT('Origin',(-20.2,29.2808336449858,-234.90005));
#191924=CARTESIAN_POINT('Origin',(-19.,29.2808336449858,-235.35005));
#191925=CARTESIAN_POINT('Origin',(-19.,29.2808336449858,-234.90005));
#191926=CARTESIAN_POINT('Origin',(296.501483394397,20.3631368321642,-234.90005));
#191927=CARTESIAN_POINT('',(-19.,20.8131368321642,-234.90005));
#191928=CARTESIAN_POINT('',(-19.,20.3631368321642,-235.35005));
#191929=CARTESIAN_POINT('Origin',(-19.,20.3631368321642,-234.90005));
#191930=CARTESIAN_POINT('',(1.23757166668304E-15,20.8131368321642,-234.90005));
#191931=CARTESIAN_POINT('',(296.501483394397,20.3631368321642,-235.35005));
#191932=CARTESIAN_POINT('Origin',(-20.2,-25.4138432731711,-234.90005));
#191933=CARTESIAN_POINT('',(-20.2,21.5631368321642,-235.35005));
#191934=CARTESIAN_POINT('',(-19.75,21.5631368321642,-234.90005));
#191935=CARTESIAN_POINT('Origin',(-20.2,21.5631368321642,-234.90005));
#191936=CARTESIAN_POINT('',(-20.2,29.2808336449858,-235.35005));
#191937=CARTESIAN_POINT('',(-19.75,21.5631368321642,-234.90005));
#191938=CARTESIAN_POINT('Origin',(-19.,21.5631368321642,-234.90005));
#191939=CARTESIAN_POINT('Origin',(-19.,21.5631368321642,-235.35005));
#191940=CARTESIAN_POINT('Origin',(-19.,21.5631368321642,-234.90005));
#191941=CARTESIAN_POINT('Origin',(-1.25,30.1648419118246,-234.90005));
#191942=CARTESIAN_POINT('',(-1.25736211889437,31.3648193279477,-235.35005));
#191943=CARTESIAN_POINT('',(-0.0499999999999979,30.1648419118246,-235.35005));
#191944=CARTESIAN_POINT('Origin',(-1.25,30.1648419118246,-235.35005));
#191945=CARTESIAN_POINT('',(-0.5,30.1648419118246,-234.90005));
#191946=CARTESIAN_POINT('Origin',(-0.05,30.1648419118246,-234.90005));
#191947=CARTESIAN_POINT('',(-1.25460132430898,30.9148277969016,-234.90005));
#191948=CARTESIAN_POINT('Origin',(-1.25,30.1648419118246,-234.90005));
#191949=CARTESIAN_POINT('Origin',(-1.25736211889437,31.3648193279477,-234.90005));
#191950=CARTESIAN_POINT('Origin',(-0.0499999999999945,-25.4138432731711,
-234.90005));
#191951=CARTESIAN_POINT('',(-0.5,21.5631368321642,-234.90005));
#191952=CARTESIAN_POINT('',(-0.0499999999999974,21.5631368321642,-235.35005));
#191953=CARTESIAN_POINT('Origin',(-0.05,21.5631368321642,-234.90005));
#191954=CARTESIAN_POINT('',(-0.5,30.1648419118246,-234.90005));
#191955=CARTESIAN_POINT('',(-0.0499999999999974,21.5631368321642,-235.35005));
#191956=CARTESIAN_POINT('Origin',(2.61456814389029E-14,-173.57701443073,
-234.90005));
#191957=CARTESIAN_POINT('',(-8.9272710441499,31.1741516601419,-235.35005));
#191958=CARTESIAN_POINT('',(-8.90766940259363,30.7245787787886,-234.90005));
#191959=CARTESIAN_POINT('Origin',(-8.9272710441499,31.1741516601419,-234.90005));
#191960=CARTESIAN_POINT('Origin',(2.61456814389029E-14,-173.57701443073,
-235.35005));
#191961=CARTESIAN_POINT('Origin',(2.61456814389029E-14,-173.57701443073,
-234.90005));
#191962=CARTESIAN_POINT('Origin',(-1.25,21.5631368321642,-234.90005));
#191963=CARTESIAN_POINT('',(-1.25,20.8131368321642,-234.90005));
#191964=CARTESIAN_POINT('',(-1.25,20.3631368321642,-235.35005));
#191965=CARTESIAN_POINT('Origin',(-1.25,20.3631368321642,-234.90005));
#191966=CARTESIAN_POINT('Origin',(-1.25,21.5631368321642,-234.90005));
#191967=CARTESIAN_POINT('Origin',(-1.25,21.5631368321642,-235.35005));
#191968=CARTESIAN_POINT('Origin',(-8.87499999999986,29.9752906431998,-234.90005));
#191969=CARTESIAN_POINT('',(-10.075,29.9752906431998,-235.35005));
#191970=CARTESIAN_POINT('',(-9.62499999999986,29.9752906431998,-234.90005));
#191971=CARTESIAN_POINT('Origin',(-10.075,29.9752906431998,-234.90005));
#191972=CARTESIAN_POINT('Origin',(-8.87499999999986,29.9752906431998,-235.35005));
#191973=CARTESIAN_POINT('Origin',(-8.87499999999986,29.9752906431998,-234.90005));
#191974=CARTESIAN_POINT('Origin',(296.501483394397,20.3631368321642,-234.90005));
#191975=CARTESIAN_POINT('',(-8.87499999999986,20.8131368321642,-234.90005));
#191976=CARTESIAN_POINT('',(-8.87499999999986,20.3631368321642,-235.35005));
#191977=CARTESIAN_POINT('Origin',(-8.87499999999986,20.3631368321642,-234.90005));
#191978=CARTESIAN_POINT('',(1.23757166668304E-15,20.8131368321642,-234.90005));
#191979=CARTESIAN_POINT('',(296.501483394397,20.3631368321642,-235.35005));
#191980=CARTESIAN_POINT('Origin',(-10.075,-25.4138432731712,-234.90005));
#191981=CARTESIAN_POINT('',(-10.0749999999999,21.5631368321642,-235.35005));
#191982=CARTESIAN_POINT('',(-9.62499999999986,21.5631368321642,-234.90005));
#191983=CARTESIAN_POINT('Origin',(-10.0749999999999,21.5631368321642,-234.90005));
#191984=CARTESIAN_POINT('',(-10.075,29.9752906431998,-235.35005));
#191985=CARTESIAN_POINT('',(-9.62499999999986,21.5631368321642,-234.90005));
#191986=CARTESIAN_POINT('Origin',(-8.87499999999986,21.5631368321642,-234.90005));
#191987=CARTESIAN_POINT('Origin',(-8.87499999999986,21.5631368321642,-235.35005));
#191988=CARTESIAN_POINT('Origin',(-8.87499999999986,21.5631368321642,-234.90005));
#191989=CARTESIAN_POINT('Origin',(-1.25,19.0631368321642,-234.90005));
#191990=CARTESIAN_POINT('',(-1.25,20.2631368321642,-235.35005));
#191991=CARTESIAN_POINT('',(-1.25,19.8131368321642,-234.90005));
#191992=CARTESIAN_POINT('Origin',(-1.25,20.2631368321642,-234.90005));
#191993=CARTESIAN_POINT('',(-0.0499999999999972,19.0631368321642,-235.35005));
#191994=CARTESIAN_POINT('Origin',(-1.25,19.0631368321642,-235.35005));
#191995=CARTESIAN_POINT('',(-0.5,19.0631368321642,-234.90005));
#191996=CARTESIAN_POINT('Origin',(-0.0499999999999994,19.0631368321642,
-234.90005));
#191997=CARTESIAN_POINT('Origin',(-1.25,19.0631368321642,-234.90005));
#191998=CARTESIAN_POINT('Origin',(-0.0499999999999945,-25.4138432731711,
-234.90005));
#191999=CARTESIAN_POINT('',(-0.5,10.9575972794973,-234.90005));
#192000=CARTESIAN_POINT('',(-0.0499999999999967,10.9575972794973,-235.35005));
#192001=CARTESIAN_POINT('Origin',(-0.0499999999999989,10.9575972794973,
-234.90005));
#192002=CARTESIAN_POINT('',(-0.5,19.0631368321642,-234.90005));
#192003=CARTESIAN_POINT('',(-0.0499999999999967,10.9575972794973,-235.35005));
#192004=CARTESIAN_POINT('Origin',(296.501483394397,20.2631368321643,-234.90005));
#192005=CARTESIAN_POINT('',(-8.87499999999986,20.2631368321642,-235.35005));
#192006=CARTESIAN_POINT('',(-8.87499999999986,19.8131368321642,-234.90005));
#192007=CARTESIAN_POINT('Origin',(-8.87499999999986,20.2631368321642,-234.90005));
#192008=CARTESIAN_POINT('',(296.501483394397,20.2631368321643,-235.35005));
#192009=CARTESIAN_POINT('',(1.54373336646988E-15,19.8131368321642,-234.90005));
#192010=CARTESIAN_POINT('Origin',(-1.25,10.9575972794973,-234.90005));
#192011=CARTESIAN_POINT('',(-1.25,10.2075972794973,-234.90005));
#192012=CARTESIAN_POINT('',(-1.25,9.75759727949733,-235.35005));
#192013=CARTESIAN_POINT('Origin',(-1.25,9.75759727949733,-234.90005));
#192014=CARTESIAN_POINT('Origin',(-1.25,10.9575972794973,-234.90005));
#192015=CARTESIAN_POINT('Origin',(-1.25,10.9575972794973,-235.35005));
#192016=CARTESIAN_POINT('Origin',(-8.87499999999986,19.0631368321642,-234.90005));
#192017=CARTESIAN_POINT('',(-10.075,19.0631368321642,-235.35005));
#192018=CARTESIAN_POINT('',(-9.62499999999986,19.0631368321642,-234.90005));
#192019=CARTESIAN_POINT('Origin',(-10.075,19.0631368321642,-234.90005));
#192020=CARTESIAN_POINT('Origin',(-8.87499999999986,19.0631368321642,-235.35005));
#192021=CARTESIAN_POINT('Origin',(-8.87499999999986,19.0631368321642,-234.90005));
#192022=CARTESIAN_POINT('Origin',(296.501483394397,9.75759727949737,-234.90005));
#192023=CARTESIAN_POINT('',(-8.87499999999986,10.2075972794973,-234.90005));
#192024=CARTESIAN_POINT('',(-8.87499999999986,9.75759727949733,-235.35005));
#192025=CARTESIAN_POINT('Origin',(-8.87499999999986,9.75759727949733,-234.90005));
#192026=CARTESIAN_POINT('',(2.53637567332344E-15,10.2075972794973,-234.90005));
#192027=CARTESIAN_POINT('',(296.501483394397,9.75759727949736,-235.35005));
#192028=CARTESIAN_POINT('Origin',(-10.075,-25.4138432731712,-234.90005));
#192029=CARTESIAN_POINT('',(-10.0749999999998,10.9575972794973,-235.35005));
#192030=CARTESIAN_POINT('',(-9.62499999999986,10.9575972794973,-234.90005));
#192031=CARTESIAN_POINT('Origin',(-10.0749999999998,10.9575972794973,-234.90005));
#192032=CARTESIAN_POINT('',(-10.075,19.0631368321642,-235.35005));
#192033=CARTESIAN_POINT('',(-9.62499999999986,10.9575972794973,-234.90005));
#192034=CARTESIAN_POINT('Origin',(-8.87499999999986,10.9575972794973,-234.90005));
#192035=CARTESIAN_POINT('Origin',(-8.87499999999986,10.9575972794973,-235.35005));
#192036=CARTESIAN_POINT('Origin',(-8.87499999999986,10.9575972794973,-234.90005));
#192037=CARTESIAN_POINT('Origin',(-1.25,8.45759727949731,-234.90005));
#192038=CARTESIAN_POINT('',(-1.25,9.65759727949731,-235.35005));
#192039=CARTESIAN_POINT('',(-1.25,9.20759727949731,-234.90005));
#192040=CARTESIAN_POINT('Origin',(-1.25,9.65759727949731,-234.90005));
#192041=CARTESIAN_POINT('',(-0.0499999999999966,8.45759727949731,-235.35005));
#192042=CARTESIAN_POINT('Origin',(-1.25,8.45759727949731,-235.35005));
#192043=CARTESIAN_POINT('',(-0.5,8.45759727949731,-234.90005));
#192044=CARTESIAN_POINT('Origin',(-0.0499999999999987,8.45759727949731,
-234.90005));
#192045=CARTESIAN_POINT('Origin',(-1.25,8.45759727949731,-234.90005));
#192046=CARTESIAN_POINT('Origin',(-0.0499999999999945,-25.4138432731711,
-234.90005));
#192047=CARTESIAN_POINT('',(-0.5,2.29555713691451,-234.90005));
#192048=CARTESIAN_POINT('',(-0.0499999999999962,2.29555713691451,-235.35005));
#192049=CARTESIAN_POINT('Origin',(-0.0499999999999985,2.29555713691451,
-234.90005));
#192050=CARTESIAN_POINT('',(-0.5,8.45759727949731,-234.90005));
#192051=CARTESIAN_POINT('',(-0.0499999999999962,2.29555713691451,-235.35005));
#192052=CARTESIAN_POINT('Origin',(296.501483394397,9.65759727949727,-234.90005));
#192053=CARTESIAN_POINT('',(-8.87499999999986,9.65759727949731,-235.35005));
#192054=CARTESIAN_POINT('',(-8.87499999999986,9.20759727949731,-234.90005));
#192055=CARTESIAN_POINT('Origin',(-8.87499999999986,9.65759727949731,-234.90005));
#192056=CARTESIAN_POINT('',(296.501483394397,9.65759727949727,-235.35005));
#192057=CARTESIAN_POINT('',(2.8425373731103E-15,9.20759727949731,-234.90005));
#192058=CARTESIAN_POINT('Origin',(-1.25,2.29555713691451,-234.90005));
#192059=CARTESIAN_POINT('',(-1.18233753211584,1.54861551239502,-234.90005));
#192060=CARTESIAN_POINT('',(-1.14174005138535,1.10045053768332,-235.35005));
#192061=CARTESIAN_POINT('Origin',(-1.14174005138535,1.10045053768332,-234.90005));
#192062=CARTESIAN_POINT('Origin',(-1.25,2.29555713691451,-234.90005));
#192063=CARTESIAN_POINT('Origin',(-1.25,2.29555713691451,-235.35005));
#192064=CARTESIAN_POINT('Origin',(-8.87499999999986,8.45759727949731,-234.90005));
#192065=CARTESIAN_POINT('',(-10.075,8.45759727949731,-235.35005));
#192066=CARTESIAN_POINT('',(-9.62499999999986,8.45759727949731,-234.90005));
#192067=CARTESIAN_POINT('Origin',(-10.075,8.45759727949731,-234.90005));
#192068=CARTESIAN_POINT('Origin',(-8.87499999999986,8.45759727949731,-235.35005));
#192069=CARTESIAN_POINT('Origin',(-8.87499999999986,8.45759727949731,-234.90005));
#192070=CARTESIAN_POINT('Origin',(0.,-11.5034818258363,-234.90005));
#192071=CARTESIAN_POINT('',(-5.33358654455957,0.46765101689032,-234.90005));
#192072=CARTESIAN_POINT('',(-5.1504491822704,0.0566027149430096,-235.35005));
#192073=CARTESIAN_POINT('Origin',(-5.1504491822704,0.0566027149430111,-234.90005));
#192074=CARTESIAN_POINT('Origin',(0.,-11.5034818258363,-234.90005));
#192075=CARTESIAN_POINT('Origin',(0.,-11.5034818258363,-235.35005));
#192076=CARTESIAN_POINT('Origin',(-10.075,-25.4138432731712,-234.90005));
#192077=CARTESIAN_POINT('',(-10.0749999999998,0.367156910880383,-235.35005));
#192078=CARTESIAN_POINT('',(-9.62499999999985,0.367156910880383,-234.90005));
#192079=CARTESIAN_POINT('Origin',(-10.0749999999998,0.367156910880383,-234.90005));
#192080=CARTESIAN_POINT('',(-10.075,8.45759727949732,-235.35005));
#192081=CARTESIAN_POINT('',(-9.62499999999985,0.367156910880385,-234.90005));
#192082=CARTESIAN_POINT('Origin',(-9.40330570654115,9.60205772683049,-234.90005));
#192083=CARTESIAN_POINT('',(-8.83216440217218,-0.38161883095341,-234.90005));
#192084=CARTESIAN_POINT('',(-8.80646304347558,-0.830884276053686,-235.35005));
#192085=CARTESIAN_POINT('Origin',(-8.80646304347558,-0.830884276053684,
-234.90005));
#192086=CARTESIAN_POINT('Origin',(-9.40330570654115,9.60205772683049,-234.90005));
#192087=CARTESIAN_POINT('Origin',(-9.40330570654115,9.60205772683049,-235.35005));
#192088=CARTESIAN_POINT('Origin',(-8.87499999999985,0.367156910880384,-234.90005));
#192089=CARTESIAN_POINT('Origin',(-8.87499999999985,0.367156910880384,-234.90005));
#192090=CARTESIAN_POINT('Origin',(-8.87499999999985,0.367156910880384,-235.35005));
#192091=CARTESIAN_POINT('Origin',(-11.3749999999999,8.45759727949731,-234.90005));
#192092=CARTESIAN_POINT('',(-11.3749999999999,9.65759727949731,-235.35005));
#192093=CARTESIAN_POINT('',(-11.3749999999999,9.20759727949731,-234.90005));
#192094=CARTESIAN_POINT('Origin',(-11.3749999999999,9.65759727949731,-234.90005));
#192095=CARTESIAN_POINT('',(-10.1749999999999,8.45759727949731,-235.35005));
#192096=CARTESIAN_POINT('Origin',(-11.3749999999999,8.45759727949731,-235.35005));
#192097=CARTESIAN_POINT('',(-10.6249999999999,8.45759727949731,-234.90005));
#192098=CARTESIAN_POINT('Origin',(-10.1749999999999,8.45759727949731,-234.90005));
#192099=CARTESIAN_POINT('Origin',(-11.3749999999999,8.45759727949731,-234.90005));
#192100=CARTESIAN_POINT('Origin',(-10.1749999999999,-25.4138432731711,-234.90005));
#192101=CARTESIAN_POINT('',(-10.6249999999999,0.352057726830487,-234.90005));
#192102=CARTESIAN_POINT('',(-10.1749999999999,0.352057726830488,-235.35005));
#192103=CARTESIAN_POINT('Origin',(-10.1749999999999,0.352057726830487,-234.90005));
#192104=CARTESIAN_POINT('',(-10.6249999999999,8.45759727949731,-234.90005));
#192105=CARTESIAN_POINT('',(-10.1749999999999,0.352057726830487,-235.35005));
#192106=CARTESIAN_POINT('Origin',(296.501483394397,9.65759727949727,-234.90005));
#192107=CARTESIAN_POINT('',(-19.,9.65759727949731,-235.35005));
#192108=CARTESIAN_POINT('',(-19.,9.20759727949731,-234.90005));
#192109=CARTESIAN_POINT('Origin',(-19.,9.65759727949731,-234.90005));
#192110=CARTESIAN_POINT('',(296.501483394397,9.65759727949727,-235.35005));
#192111=CARTESIAN_POINT('',(2.8425373731103E-15,9.20759727949731,-234.90005));
#192112=CARTESIAN_POINT('Origin',(-11.3749999999999,0.352057726830487,-234.90005));
#192113=CARTESIAN_POINT('',(-11.3749999999999,-0.397942273169513,-234.90005));
#192114=CARTESIAN_POINT('',(-11.3749999999999,-0.847942273169513,-235.35005));
#192115=CARTESIAN_POINT('Origin',(-11.3749999999999,-0.847942273169513,
-234.90005));
#192116=CARTESIAN_POINT('Origin',(-11.3749999999999,0.352057726830487,-234.90005));
#192117=CARTESIAN_POINT('Origin',(-11.3749999999999,0.352057726830487,-235.35005));
#192118=CARTESIAN_POINT('Origin',(-19.,8.45759727949731,-234.90005));
#192119=CARTESIAN_POINT('',(-20.2,8.45759727949731,-235.35005));
#192120=CARTESIAN_POINT('',(-19.75,8.45759727949731,-234.90005));
#192121=CARTESIAN_POINT('Origin',(-20.2,8.45759727949731,-234.90005));
#192122=CARTESIAN_POINT('Origin',(-19.,8.45759727949731,-235.35005));
#192123=CARTESIAN_POINT('Origin',(-19.,8.45759727949731,-234.90005));
#192124=CARTESIAN_POINT('Origin',(296.501483394397,-0.84794227316963,-234.90005));
#192125=CARTESIAN_POINT('',(-19.,-0.39794227316951,-234.90005));
#192126=CARTESIAN_POINT('',(-19.,-0.847942273169513,-235.35005));
#192127=CARTESIAN_POINT('Origin',(-19.,-0.84794227316951,-234.90005));
#192128=CARTESIAN_POINT('',(1.11087130309497E-13,-0.397942273169517,-234.90005));
#192129=CARTESIAN_POINT('',(296.501483394397,-0.84794227316963,-235.35005));
#192130=CARTESIAN_POINT('Origin',(-20.2,-25.4138432731711,-234.90005));
#192131=CARTESIAN_POINT('',(-20.2,0.352057726830487,-235.35005));
#192132=CARTESIAN_POINT('',(-19.75,0.352057726830487,-234.90005));
#192133=CARTESIAN_POINT('Origin',(-20.2,0.352057726830487,-234.90005));
#192134=CARTESIAN_POINT('',(-20.2,8.45759727949731,-235.35005));
#192135=CARTESIAN_POINT('',(-19.75,0.352057726830487,-234.90005));
#192136=CARTESIAN_POINT('Origin',(-19.,0.35205772683049,-234.90005));
#192137=CARTESIAN_POINT('Origin',(-19.,0.35205772683049,-235.35005));
#192138=CARTESIAN_POINT('Origin',(-19.,0.35205772683049,-234.90005));
#192139=CARTESIAN_POINT('Origin',(-11.3749999999999,19.0631368321642,-234.90005));
#192140=CARTESIAN_POINT('',(-11.3749999999999,20.2631368321642,-235.35005));
#192141=CARTESIAN_POINT('',(-11.3749999999999,19.8131368321642,-234.90005));
#192142=CARTESIAN_POINT('Origin',(-11.3749999999999,20.2631368321642,-234.90005));
#192143=CARTESIAN_POINT('',(-10.1749999999999,19.0631368321642,-235.35005));
#192144=CARTESIAN_POINT('Origin',(-11.3749999999999,19.0631368321642,-235.35005));
#192145=CARTESIAN_POINT('',(-10.6249999999999,19.0631368321642,-234.90005));
#192146=CARTESIAN_POINT('Origin',(-10.1749999999999,19.0631368321642,-234.90005));
#192147=CARTESIAN_POINT('Origin',(-11.3749999999999,19.0631368321642,-234.90005));
#192148=CARTESIAN_POINT('Origin',(-10.1749999999999,-25.4138432731711,-234.90005));
#192149=CARTESIAN_POINT('',(-10.6249999999999,10.9575972794973,-234.90005));
#192150=CARTESIAN_POINT('',(-10.1749999999999,10.9575972794973,-235.35005));
#192151=CARTESIAN_POINT('Origin',(-10.1749999999999,10.9575972794973,-234.90005));
#192152=CARTESIAN_POINT('',(-10.6249999999999,19.0631368321642,-234.90005));
#192153=CARTESIAN_POINT('',(-10.1749999999999,10.9575972794973,-235.35005));
#192154=CARTESIAN_POINT('Origin',(296.501483394397,20.2631368321643,-234.90005));
#192155=CARTESIAN_POINT('',(-19.,20.2631368321642,-235.35005));
#192156=CARTESIAN_POINT('',(-19.,19.8131368321642,-234.90005));
#192157=CARTESIAN_POINT('Origin',(-19.,20.2631368321642,-234.90005));
#192158=CARTESIAN_POINT('',(296.501483394397,20.2631368321643,-235.35005));
#192159=CARTESIAN_POINT('',(1.54373336646988E-15,19.8131368321642,-234.90005));
#192160=CARTESIAN_POINT('Origin',(-11.3749999999999,10.9575972794973,-234.90005));
#192161=CARTESIAN_POINT('',(-11.3749999999999,10.2075972794973,-234.90005));
#192162=CARTESIAN_POINT('',(-11.3749999999999,9.75759727949733,-235.35005));
#192163=CARTESIAN_POINT('Origin',(-11.3749999999999,9.75759727949733,-234.90005));
#192164=CARTESIAN_POINT('Origin',(-11.3749999999999,10.9575972794973,-234.90005));
#192165=CARTESIAN_POINT('Origin',(-11.3749999999999,10.9575972794973,-235.35005));
#192166=CARTESIAN_POINT('Origin',(-19.,19.0631368321642,-234.90005));
#192167=CARTESIAN_POINT('',(-20.2,19.0631368321642,-235.35005));
#192168=CARTESIAN_POINT('',(-19.75,19.0631368321642,-234.90005));
#192169=CARTESIAN_POINT('Origin',(-20.2,19.0631368321642,-234.90005));
#192170=CARTESIAN_POINT('Origin',(-19.,19.0631368321642,-235.35005));
#192171=CARTESIAN_POINT('Origin',(-19.,19.0631368321642,-234.90005));
#192172=CARTESIAN_POINT('Origin',(296.501483394397,9.75759727949737,-234.90005));
#192173=CARTESIAN_POINT('',(-19.,10.2075972794973,-234.90005));
#192174=CARTESIAN_POINT('',(-19.,9.75759727949733,-235.35005));
#192175=CARTESIAN_POINT('Origin',(-19.,9.75759727949733,-234.90005));
#192176=CARTESIAN_POINT('',(2.53637567332344E-15,10.2075972794973,-234.90005));
#192177=CARTESIAN_POINT('',(296.501483394397,9.75759727949737,-235.35005));
#192178=CARTESIAN_POINT('Origin',(-20.2,-25.4138432731711,-234.90005));
#192179=CARTESIAN_POINT('',(-20.2,10.9575972794973,-235.35005));
#192180=CARTESIAN_POINT('',(-19.75,10.9575972794973,-234.90005));
#192181=CARTESIAN_POINT('Origin',(-20.2,10.9575972794973,-234.90005));
#192182=CARTESIAN_POINT('',(-20.2,19.0631368321642,-235.35005));
#192183=CARTESIAN_POINT('',(-19.75,10.9575972794973,-234.90005));
#192184=CARTESIAN_POINT('Origin',(-19.,10.9575972794973,-234.90005));
#192185=CARTESIAN_POINT('Origin',(-19.,10.9575972794973,-235.35005));
#192186=CARTESIAN_POINT('Origin',(-19.,10.9575972794973,-234.90005));
#192187=CARTESIAN_POINT('Origin',(-21.5,19.0631368321642,-234.90005));
#192188=CARTESIAN_POINT('',(-21.5,20.2631368321642,-235.35005));
#192189=CARTESIAN_POINT('',(-21.5,19.8131368321642,-234.90005));
#192190=CARTESIAN_POINT('Origin',(-21.5,20.2631368321642,-234.90005));
#192191=CARTESIAN_POINT('',(-20.3,19.0631368321642,-235.35005));
#192192=CARTESIAN_POINT('Origin',(-21.5,19.0631368321642,-235.35005));
#192193=CARTESIAN_POINT('',(-20.75,19.0631368321642,-234.90005));
#192194=CARTESIAN_POINT('Origin',(-20.3,19.0631368321642,-234.90005));
#192195=CARTESIAN_POINT('Origin',(-21.5,19.0631368321642,-234.90005));
#192196=CARTESIAN_POINT('Origin',(-20.3,-25.4138432731711,-234.90005));
#192197=CARTESIAN_POINT('',(-20.75,10.9575972794973,-234.90005));
#192198=CARTESIAN_POINT('',(-20.3,10.9575972794973,-235.35005));
#192199=CARTESIAN_POINT('Origin',(-20.3,10.9575972794973,-234.90005));
#192200=CARTESIAN_POINT('',(-20.75,19.0631368321642,-234.90005));
#192201=CARTESIAN_POINT('',(-20.3,10.9575972794973,-235.35005));
#192202=CARTESIAN_POINT('Origin',(296.501483394397,20.2631368321643,-234.90005));
#192203=CARTESIAN_POINT('',(-29.125,20.2631368321642,-235.35005));
#192204=CARTESIAN_POINT('',(-29.125,19.8131368321642,-234.90005));
#192205=CARTESIAN_POINT('Origin',(-29.125,20.2631368321642,-234.90005));
#192206=CARTESIAN_POINT('',(296.501483394397,20.2631368321643,-235.35005));
#192207=CARTESIAN_POINT('',(1.54373336646988E-15,19.8131368321642,-234.90005));
#192208=CARTESIAN_POINT('Origin',(-21.5,10.9575972794973,-234.90005));
#192209=CARTESIAN_POINT('',(-21.5,10.2075972794973,-234.90005));
#192210=CARTESIAN_POINT('',(-21.5,9.75759727949733,-235.35005));
#192211=CARTESIAN_POINT('Origin',(-21.5,9.75759727949733,-234.90005));
#192212=CARTESIAN_POINT('Origin',(-21.5,10.9575972794973,-234.90005));
#192213=CARTESIAN_POINT('Origin',(-21.5,10.9575972794973,-235.35005));
#192214=CARTESIAN_POINT('Origin',(-29.125,19.0631368321642,-234.90005));
#192215=CARTESIAN_POINT('',(-30.325,19.0631368321642,-235.35005));
#192216=CARTESIAN_POINT('',(-29.875,19.0631368321642,-234.90005));
#192217=CARTESIAN_POINT('Origin',(-30.325,19.0631368321642,-234.90005));
#192218=CARTESIAN_POINT('Origin',(-29.125,19.0631368321642,-235.35005));
#192219=CARTESIAN_POINT('Origin',(-29.125,19.0631368321642,-234.90005));
#192220=CARTESIAN_POINT('Origin',(296.501483394397,9.75759727949737,-234.90005));
#192221=CARTESIAN_POINT('',(-29.125,10.2075972794973,-234.90005));
#192222=CARTESIAN_POINT('',(-29.125,9.75759727949733,-235.35005));
#192223=CARTESIAN_POINT('Origin',(-29.125,9.75759727949733,-234.90005));
#192224=CARTESIAN_POINT('',(2.53637567332344E-15,10.2075972794973,-234.90005));
#192225=CARTESIAN_POINT('',(296.501483394397,9.75759727949737,-235.35005));
#192226=CARTESIAN_POINT('Origin',(-30.325,-25.4138432731711,-234.90005));
#192227=CARTESIAN_POINT('',(-30.325,10.9575972794973,-235.35005));
#192228=CARTESIAN_POINT('',(-29.875,10.9575972794973,-234.90005));
#192229=CARTESIAN_POINT('Origin',(-30.325,10.9575972794973,-234.90005));
#192230=CARTESIAN_POINT('',(-30.325,19.0631368321642,-235.35005));
#192231=CARTESIAN_POINT('',(-29.875,10.9575972794973,-234.90005));
#192232=CARTESIAN_POINT('Origin',(-29.125,10.9575972794973,-234.90005));
#192233=CARTESIAN_POINT('Origin',(-29.125,10.9575972794973,-235.35005));
#192234=CARTESIAN_POINT('Origin',(-29.125,10.9575972794973,-234.90005));
#192235=CARTESIAN_POINT('Origin',(-21.5,8.45759727949731,-234.90005));
#192236=CARTESIAN_POINT('',(-21.5,9.65759727949731,-235.35005));
#192237=CARTESIAN_POINT('',(-21.5,9.20759727949731,-234.90005));
#192238=CARTESIAN_POINT('Origin',(-21.5,9.65759727949731,-234.90005));
#192239=CARTESIAN_POINT('',(-20.3,8.45759727949731,-235.35005));
#192240=CARTESIAN_POINT('Origin',(-21.5,8.45759727949731,-235.35005));
#192241=CARTESIAN_POINT('',(-20.75,8.45759727949731,-234.90005));
#192242=CARTESIAN_POINT('Origin',(-20.3,8.45759727949731,-234.90005));
#192243=CARTESIAN_POINT('Origin',(-21.5,8.45759727949731,-234.90005));
#192244=CARTESIAN_POINT('Origin',(-20.3,-25.4138432731711,-234.90005));
#192245=CARTESIAN_POINT('',(-20.75,0.352057726830487,-234.90005));
#192246=CARTESIAN_POINT('',(-20.3,0.352057726830486,-235.35005));
#192247=CARTESIAN_POINT('Origin',(-20.3,0.352057726830486,-234.90005));
#192248=CARTESIAN_POINT('',(-20.75,8.45759727949731,-234.90005));
#192249=CARTESIAN_POINT('',(-20.3,0.352057726830487,-235.35005));
#192250=CARTESIAN_POINT('Origin',(296.501483394397,9.65759727949727,-234.90005));
#192251=CARTESIAN_POINT('',(-29.125,9.65759727949731,-235.35005));
#192252=CARTESIAN_POINT('',(-29.125,9.20759727949731,-234.90005));
#192253=CARTESIAN_POINT('Origin',(-29.125,9.65759727949731,-234.90005));
#192254=CARTESIAN_POINT('',(296.501483394397,9.65759727949727,-235.35005));
#192255=CARTESIAN_POINT('',(2.8425373731103E-15,9.20759727949731,-234.90005));
#192256=CARTESIAN_POINT('Origin',(-21.5,0.352057726830491,-234.90005));
#192257=CARTESIAN_POINT('',(-21.5,-0.397942273169509,-234.90005));
#192258=CARTESIAN_POINT('',(-21.5,-0.847942273169509,-235.35005));
#192259=CARTESIAN_POINT('Origin',(-21.5,-0.847942273169509,-234.90005));
#192260=CARTESIAN_POINT('Origin',(-21.5,0.352057726830491,-234.90005));
#192261=CARTESIAN_POINT('Origin',(-21.5,0.352057726830491,-235.35005));
#192262=CARTESIAN_POINT('Origin',(-29.125,8.45759727949731,-234.90005));
#192263=CARTESIAN_POINT('',(-30.325,8.45759727949731,-235.35005));
#192264=CARTESIAN_POINT('',(-29.875,8.45759727949731,-234.90005));
#192265=CARTESIAN_POINT('Origin',(-30.325,8.45759727949731,-234.90005));
#192266=CARTESIAN_POINT('Origin',(-29.125,8.45759727949731,-235.35005));
#192267=CARTESIAN_POINT('Origin',(-29.125,8.45759727949731,-234.90005));
#192268=CARTESIAN_POINT('Origin',(296.501483394397,-0.84794227316963,-234.90005));
#192269=CARTESIAN_POINT('',(-29.125,-0.397942273169507,-234.90005));
#192270=CARTESIAN_POINT('',(-29.125,-0.847942273169509,-235.35005));
#192271=CARTESIAN_POINT('Origin',(-29.125,-0.847942273169506,-234.90005));
#192272=CARTESIAN_POINT('',(1.11087130309497E-13,-0.397942273169517,-234.90005));
#192273=CARTESIAN_POINT('',(296.501483394397,-0.84794227316963,-235.35005));
#192274=CARTESIAN_POINT('Origin',(-30.325,-25.4138432731711,-234.90005));
#192275=CARTESIAN_POINT('',(-30.325,0.352057726830494,-235.35005));
#192276=CARTESIAN_POINT('',(-29.875,0.352057726830494,-234.90005));
#192277=CARTESIAN_POINT('Origin',(-30.325,0.352057726830494,-234.90005));
#192278=CARTESIAN_POINT('',(-30.325,8.45759727949732,-235.35005));
#192279=CARTESIAN_POINT('',(-29.875,0.352057726830494,-234.90005));
#192280=CARTESIAN_POINT('Origin',(-29.125,0.352057726830494,-234.90005));
#192281=CARTESIAN_POINT('Origin',(-29.125,0.352057726830494,-235.35005));
#192282=CARTESIAN_POINT('Origin',(-29.125,0.352057726830494,-234.90005));
#192283=CARTESIAN_POINT('Origin',(-31.625,8.45759727949731,-234.90005));
#192284=CARTESIAN_POINT('',(-31.625,9.65759727949731,-235.35005));
#192285=CARTESIAN_POINT('',(-31.625,9.20759727949731,-234.90005));
#192286=CARTESIAN_POINT('Origin',(-31.625,9.65759727949731,-234.90005));
#192287=CARTESIAN_POINT('',(-30.425,8.45759727949731,-235.35005));
#192288=CARTESIAN_POINT('Origin',(-31.625,8.45759727949731,-235.35005));
#192289=CARTESIAN_POINT('',(-30.875,8.45759727949731,-234.90005));
#192290=CARTESIAN_POINT('Origin',(-30.425,8.45759727949731,-234.90005));
#192291=CARTESIAN_POINT('Origin',(-31.625,8.45759727949731,-234.90005));
#192292=CARTESIAN_POINT('Origin',(-30.425,-25.4138432731711,-234.90005));
#192293=CARTESIAN_POINT('',(-30.875,0.352057726830494,-234.90005));
#192294=CARTESIAN_POINT('',(-30.425,0.352057726830494,-235.35005));
#192295=CARTESIAN_POINT('Origin',(-30.425,0.352057726830494,-234.90005));
#192296=CARTESIAN_POINT('',(-30.875,8.45759727949732,-234.90005));
#192297=CARTESIAN_POINT('',(-30.425,0.352057726830494,-235.35005));
#192298=CARTESIAN_POINT('Origin',(296.501483394397,9.65759727949727,-234.90005));
#192299=CARTESIAN_POINT('',(-39.4555265729267,9.65759727949731,-235.35005));
#192300=CARTESIAN_POINT('',(-39.4555265729267,9.20759727949731,-234.90005));
#192301=CARTESIAN_POINT('Origin',(-39.4555265729267,9.65759727949731,-234.90005));
#192302=CARTESIAN_POINT('',(296.501483394397,9.65759727949727,-235.35005));
#192303=CARTESIAN_POINT('',(2.8425373731103E-15,9.20759727949731,-234.90005));
#192304=CARTESIAN_POINT('Origin',(-31.625,0.352057726830494,-234.90005));
#192305=CARTESIAN_POINT('',(-31.625,-0.397942273169506,-234.90005));
#192306=CARTESIAN_POINT('',(-31.625,-0.847942273169506,-235.35005));
#192307=CARTESIAN_POINT('Origin',(-31.625,-0.847942273169505,-234.90005));
#192308=CARTESIAN_POINT('Origin',(-31.625,0.352057726830494,-234.90005));
#192309=CARTESIAN_POINT('Origin',(-31.625,0.352057726830495,-235.35005));
#192310=CARTESIAN_POINT('Origin',(-39.4555265729267,8.45759727949731,-234.90005));
#192311=CARTESIAN_POINT('',(-40.6550043680477,8.49299528808125,-235.35005));
#192312=CARTESIAN_POINT('',(-40.2052001948774,8.47972103486227,-234.90005));
#192313=CARTESIAN_POINT('Origin',(-40.6550043680477,8.49299528808125,-234.90005));
#192314=CARTESIAN_POINT('Origin',(-39.4555265729267,8.45759727949731,-235.35005));
#192315=CARTESIAN_POINT('Origin',(-39.4555265729267,8.45759727949731,-234.90005));
#192316=CARTESIAN_POINT('Origin',(296.501483394397,-0.84794227316963,-234.90005));
#192317=CARTESIAN_POINT('',(-39.6461373136998,-0.397942273169503,-234.90005));
#192318=CARTESIAN_POINT('',(-39.6461373136998,-0.847942273169505,-235.35005));
#192319=CARTESIAN_POINT('Origin',(-39.6461373136998,-0.847942273169502,
-234.90005));
#192320=CARTESIAN_POINT('',(1.11087130309497E-13,-0.397942273169517,-234.90005));
#192321=CARTESIAN_POINT('',(296.501483394397,-0.84794227316963,-235.35005));
#192322=CARTESIAN_POINT('Origin',(636.934816028482,-11.5034818258361,-234.90005));
#192323=CARTESIAN_POINT('',(-40.8459531286544,0.37308176509206,-235.35005));
#192324=CARTESIAN_POINT('',(-40.3960221980464,0.365197750743974,-234.90005));
#192325=CARTESIAN_POINT('Origin',(-40.8459531286544,0.37308176509206,-234.90005));
#192326=CARTESIAN_POINT('Origin',(636.934816028482,-11.5034818258361,-235.35005));
#192327=CARTESIAN_POINT('Origin',(636.934816028482,-11.5034818258361,-234.90005));
#192328=CARTESIAN_POINT('Origin',(-39.6461373136998,0.352057726830498,-234.90005));
#192329=CARTESIAN_POINT('Origin',(-39.6461373136998,0.352057726830498,-235.35005));
#192330=CARTESIAN_POINT('Origin',(-39.6461373136998,0.352057726830498,-234.90005));
#192331=CARTESIAN_POINT('Origin',(-31.625,19.0631368321642,-234.90005));
#192332=CARTESIAN_POINT('',(-31.625,20.2631368321642,-235.35005));
#192333=CARTESIAN_POINT('',(-31.625,19.8131368321642,-234.90005));
#192334=CARTESIAN_POINT('Origin',(-31.625,20.2631368321642,-234.90005));
#192335=CARTESIAN_POINT('',(-30.425,19.0631368321642,-235.35005));
#192336=CARTESIAN_POINT('Origin',(-31.625,19.0631368321642,-235.35005));
#192337=CARTESIAN_POINT('',(-30.875,19.0631368321642,-234.90005));
#192338=CARTESIAN_POINT('Origin',(-30.425,19.0631368321642,-234.90005));
#192339=CARTESIAN_POINT('Origin',(-31.625,19.0631368321642,-234.90005));
#192340=CARTESIAN_POINT('Origin',(-30.425,-25.4138432731711,-234.90005));
#192341=CARTESIAN_POINT('',(-30.875,10.9575972794973,-234.90005));
#192342=CARTESIAN_POINT('',(-30.425,10.9575972794973,-235.35005));
#192343=CARTESIAN_POINT('Origin',(-30.425,10.9575972794973,-234.90005));
#192344=CARTESIAN_POINT('',(-30.875,19.0631368321642,-234.90005));
#192345=CARTESIAN_POINT('',(-30.425,10.9575972794973,-235.35005));
#192346=CARTESIAN_POINT('Origin',(296.501483394397,20.2631368321643,-234.90005));
#192347=CARTESIAN_POINT('',(-36.0311576807679,20.2631368321642,-235.35005));
#192348=CARTESIAN_POINT('',(-36.0311576807679,19.8131368321642,-234.90005));
#192349=CARTESIAN_POINT('Origin',(-36.0311576807679,20.2631368321642,-234.90005));
#192350=CARTESIAN_POINT('',(296.501483394397,20.2631368321643,-235.35005));
#192351=CARTESIAN_POINT('',(1.54373336646988E-15,19.8131368321642,-234.90005));
#192352=CARTESIAN_POINT('Origin',(-31.625,10.9575972794973,-234.90005));
#192353=CARTESIAN_POINT('',(-31.625,10.2075972794973,-234.90005));
#192354=CARTESIAN_POINT('',(-31.625,9.75759727949733,-235.35005));
#192355=CARTESIAN_POINT('Origin',(-31.625,9.75759727949733,-234.90005));
#192356=CARTESIAN_POINT('Origin',(-31.625,10.9575972794973,-234.90005));
#192357=CARTESIAN_POINT('Origin',(-31.625,10.9575972794973,-235.35005));
#192358=CARTESIAN_POINT('Origin',(-36.0311576807679,19.0631368321642,-234.90005));
#192359=CARTESIAN_POINT('',(-36.9462347012319,19.8394319091927,-235.35005));
#192360=CARTESIAN_POINT('',(-36.6030808185579,19.548321255307,-234.90005));
#192361=CARTESIAN_POINT('Origin',(-36.9462347012319,19.8394319091927,-234.90005));
#192362=CARTESIAN_POINT('Origin',(-36.0311576807679,19.0631368321642,-235.35005));
#192363=CARTESIAN_POINT('Origin',(-36.0311576807679,19.0631368321642,-234.90005));
#192364=CARTESIAN_POINT('Origin',(296.501483394397,9.75759727949737,-234.90005));
#192365=CARTESIAN_POINT('',(-39.3771239584772,10.2075972794973,-234.90005));
#192366=CARTESIAN_POINT('',(-39.3771239584772,9.75759727949732,-235.35005));
#192367=CARTESIAN_POINT('Origin',(-39.3771239584772,9.75759727949733,-234.90005));
#192368=CARTESIAN_POINT('',(2.53637567332344E-15,10.2075972794973,-234.90005));
#192369=CARTESIAN_POINT('',(296.501483394397,9.75759727949737,-235.35005));
#192370=CARTESIAN_POINT('Origin',(6.29739814579425E-15,-11.5034818258363,
-234.90005));
#192371=CARTESIAN_POINT('',(-40.1936303108393,15.5496988085284,-235.35005));
#192372=CARTESIAN_POINT('',(-39.8203148590359,15.2984308769399,-234.90005));
#192373=CARTESIAN_POINT('Origin',(-40.1936303108393,15.5496988085284,-234.90005));
#192374=CARTESIAN_POINT('Origin',(6.29739814579425E-15,-11.5034818258363,
-235.35005));
#192375=CARTESIAN_POINT('Origin',(6.29739814579425E-15,-11.5034818258363,
-234.90005));
#192376=CARTESIAN_POINT('Origin',(-39.3771239584772,10.9575972794973,-234.90005));
#192377=CARTESIAN_POINT('',(-40.1267106833092,10.9824918965036,-234.90005));
#192378=CARTESIAN_POINT('',(-40.5764627182082,10.9974286667074,-235.35005));
#192379=CARTESIAN_POINT('Origin',(-40.5764627182083,10.9974286667074,-234.90005));
#192380=CARTESIAN_POINT('Origin',(-39.3771239584772,10.9575972794973,-234.90005));
#192381=CARTESIAN_POINT('Origin',(-39.3771239584772,10.9575972794973,-235.35005));
#192382=CARTESIAN_POINT('Origin',(-38.9907249661392,14.740057695632,-234.90005));
#192383=CARTESIAN_POINT('',(-40.4396332884467,14.7963131269086,-235.35005));
#192384=CARTESIAN_POINT('',(-39.989972084972,14.7788545447883,-234.90005));
#192385=CARTESIAN_POINT('Origin',(-40.4396332884467,14.7963131269086,-234.90005));
#192386=CARTESIAN_POINT('Origin',(-38.9907249661392,14.740057695632,-235.35005));
#192387=CARTESIAN_POINT('Origin',(-38.9907249661392,14.740057695632,-234.90005));
#192388=CARTESIAN_POINT('Origin',(636.934816028482,-11.5034818258361,-234.90005));
#192389=CARTESIAN_POINT('Origin',(636.934816028482,-11.5034818258361,-235.35005));
#192390=CARTESIAN_POINT('Origin',(636.934816028482,-11.5034818258361,-234.90005));
#192391=CARTESIAN_POINT('Origin',(-31.625,-2.14794227316952,-234.90005));
#192392=CARTESIAN_POINT('',(-31.625,-0.947942273169512,-235.35005));
#192393=CARTESIAN_POINT('',(-31.625,-1.39794227316951,-234.90005));
#192394=CARTESIAN_POINT('Origin',(-31.625,-0.947942273169512,-234.90005));
#192395=CARTESIAN_POINT('',(-30.425,-2.14794227316951,-235.35005));
#192396=CARTESIAN_POINT('Origin',(-31.625,-2.14794227316952,-235.35005));
#192397=CARTESIAN_POINT('',(-30.875,-2.14794227316951,-234.90005));
#192398=CARTESIAN_POINT('Origin',(-30.425,-2.14794227316951,-234.90005));
#192399=CARTESIAN_POINT('Origin',(-31.625,-2.14794227316952,-234.90005));
#192400=CARTESIAN_POINT('Origin',(-30.425,-25.4138432731711,-234.90005));
#192401=CARTESIAN_POINT('',(-30.875,-10.2534818258363,-234.90005));
#192402=CARTESIAN_POINT('',(-30.425,-10.2534818258363,-235.35005));
#192403=CARTESIAN_POINT('Origin',(-30.425,-10.2534818258363,-234.90005));
#192404=CARTESIAN_POINT('',(-30.875,-2.14794227316951,-234.90005));
#192405=CARTESIAN_POINT('',(-30.425,-10.2534818258363,-235.35005));
#192406=CARTESIAN_POINT('Origin',(296.501483394397,-0.94794227316939,-234.90005));
#192407=CARTESIAN_POINT('',(-39.6853241707135,-0.947942273169515,-235.35005));
#192408=CARTESIAN_POINT('',(-39.6853241707135,-1.39794227316951,-234.90005));
#192409=CARTESIAN_POINT('Origin',(-39.6853241707135,-0.947942273169515,
-234.90005));
#192410=CARTESIAN_POINT('',(296.501483394397,-0.94794227316939,-235.35005));
#192411=CARTESIAN_POINT('',(1.11087130309497E-13,-1.3979422731695,-234.90005));
#192412=CARTESIAN_POINT('Origin',(-31.625,-10.2534818258363,-234.90005));
#192413=CARTESIAN_POINT('',(-31.625,-11.0034818258363,-234.90005));
#192414=CARTESIAN_POINT('',(-31.625,-11.4534818258363,-235.35005));
#192415=CARTESIAN_POINT('Origin',(-31.625,-11.4534818258363,-234.90005));
#192416=CARTESIAN_POINT('Origin',(-31.625,-10.2534818258363,-234.90005));
#192417=CARTESIAN_POINT('Origin',(-31.625,-10.2534818258363,-235.35005));
#192418=CARTESIAN_POINT('Origin',(-39.6853241707135,-2.14794227316952,-234.90005));
#192419=CARTESIAN_POINT('',(-40.8852094777378,-2.13135161353407,-235.35005));
#192420=CARTESIAN_POINT('',(-40.4352524876037,-2.13757311089736,-234.90005));
#192421=CARTESIAN_POINT('Origin',(-40.8852094777378,-2.13135161353407,-234.90005));
#192422=CARTESIAN_POINT('Origin',(-39.6853241707135,-2.14794227316952,-235.35005));
#192423=CARTESIAN_POINT('Origin',(-39.6853241707135,-2.14794227316952,-234.90005));
#192424=CARTESIAN_POINT('Origin',(296.501483394397,-11.4534818258365,-234.90005));
#192425=CARTESIAN_POINT('',(-39.7488454733312,-11.0034818258363,-234.90005));
#192426=CARTESIAN_POINT('',(-39.7488454733312,-11.4534818258363,-235.35005));
#192427=CARTESIAN_POINT('Origin',(-39.7488454733312,-11.4534818258363,-234.90005));
#192428=CARTESIAN_POINT('',(2.22174260618994E-13,-11.0034818258363,-234.90005));
#192429=CARTESIAN_POINT('',(296.501483394397,-11.4534818258365,-235.35005));
#192430=CARTESIAN_POINT('Origin',(636.934816028482,-11.5034818258361,-234.90005));
#192431=CARTESIAN_POINT('',(-40.9488434259496,-10.2512651365233,-235.35005));
#192432=CARTESIAN_POINT('',(-40.4988441937178,-10.2520963950157,-234.90005));
#192433=CARTESIAN_POINT('Origin',(-40.9488434259496,-10.2512651365233,-234.90005));
#192434=CARTESIAN_POINT('Origin',(636.934816028482,-11.5034818258361,-235.35005));
#192435=CARTESIAN_POINT('Origin',(636.934816028482,-11.5034818258361,-234.90005));
#192436=CARTESIAN_POINT('Origin',(-39.7488454733312,-10.2534818258363,-234.90005));
#192437=CARTESIAN_POINT('Origin',(-39.7488454733312,-10.2534818258363,-235.35005));
#192438=CARTESIAN_POINT('Origin',(-39.7488454733312,-10.2534818258363,-234.90005));
#192439=CARTESIAN_POINT('Origin',(-21.5,-2.14794227316951,-234.90005));
#192440=CARTESIAN_POINT('',(-21.5,-0.947942273169508,-235.35005));
#192441=CARTESIAN_POINT('',(-21.5,-1.39794227316951,-234.90005));
#192442=CARTESIAN_POINT('Origin',(-21.5,-0.947942273169508,-234.90005));
#192443=CARTESIAN_POINT('',(-20.3,-2.14794227316951,-235.35005));
#192444=CARTESIAN_POINT('Origin',(-21.5,-2.14794227316951,-235.35005));
#192445=CARTESIAN_POINT('',(-20.75,-2.14794227316951,-234.90005));
#192446=CARTESIAN_POINT('Origin',(-20.3,-2.14794227316951,-234.90005));
#192447=CARTESIAN_POINT('Origin',(-21.5,-2.14794227316951,-234.90005));
#192448=CARTESIAN_POINT('Origin',(-20.3,-25.4138432731711,-234.90005));
#192449=CARTESIAN_POINT('',(-20.75,-10.2534818258363,-234.90005));
#192450=CARTESIAN_POINT('',(-20.3,-10.2534818258363,-235.35005));
#192451=CARTESIAN_POINT('Origin',(-20.3,-10.2534818258363,-234.90005));
#192452=CARTESIAN_POINT('',(-20.75,-2.14794227316951,-234.90005));
#192453=CARTESIAN_POINT('',(-20.3,-10.2534818258363,-235.35005));
#192454=CARTESIAN_POINT('Origin',(296.501483394397,-0.94794227316939,-234.90005));
#192455=CARTESIAN_POINT('',(-29.125,-0.947942273169511,-235.35005));
#192456=CARTESIAN_POINT('',(-29.125,-1.39794227316951,-234.90005));
#192457=CARTESIAN_POINT('Origin',(-29.125,-0.947942273169511,-234.90005));
#192458=CARTESIAN_POINT('',(296.501483394397,-0.94794227316939,-235.35005));
#192459=CARTESIAN_POINT('',(1.11087130309497E-13,-1.3979422731695,-234.90005));
#192460=CARTESIAN_POINT('Origin',(-21.5,-10.2534818258363,-234.90005));
#192461=CARTESIAN_POINT('',(-21.5,-11.0034818258363,-234.90005));
#192462=CARTESIAN_POINT('',(-21.5,-11.4534818258363,-235.35005));
#192463=CARTESIAN_POINT('Origin',(-21.5,-11.4534818258363,-234.90005));
#192464=CARTESIAN_POINT('Origin',(-21.5,-10.2534818258363,-234.90005));
#192465=CARTESIAN_POINT('Origin',(-21.5,-10.2534818258363,-235.35005));
#192466=CARTESIAN_POINT('Origin',(-29.125,-2.14794227316951,-234.90005));
#192467=CARTESIAN_POINT('',(-30.325,-2.14794227316951,-235.35005));
#192468=CARTESIAN_POINT('',(-29.875,-2.14794227316951,-234.90005));
#192469=CARTESIAN_POINT('Origin',(-30.325,-2.14794227316951,-234.90005));
#192470=CARTESIAN_POINT('Origin',(-29.125,-2.14794227316951,-235.35005));
#192471=CARTESIAN_POINT('Origin',(-29.125,-2.14794227316951,-234.90005));
#192472=CARTESIAN_POINT('Origin',(296.501483394397,-11.4534818258365,-234.90005));
#192473=CARTESIAN_POINT('',(-29.125,-11.0034818258363,-234.90005));
#192474=CARTESIAN_POINT('',(-29.125,-11.4534818258363,-235.35005));
#192475=CARTESIAN_POINT('Origin',(-29.125,-11.4534818258363,-234.90005));
#192476=CARTESIAN_POINT('',(2.22174260618994E-13,-11.0034818258363,-234.90005));
#192477=CARTESIAN_POINT('',(296.501483394397,-11.4534818258365,-235.35005));
#192478=CARTESIAN_POINT('Origin',(-30.325,-25.4138432731711,-234.90005));
#192479=CARTESIAN_POINT('',(-30.325,-10.2534818258363,-235.35005));
#192480=CARTESIAN_POINT('',(-29.875,-10.2534818258363,-234.90005));
#192481=CARTESIAN_POINT('Origin',(-30.325,-10.2534818258363,-234.90005));
#192482=CARTESIAN_POINT('',(-30.325,-2.14794227316951,-235.35005));
#192483=CARTESIAN_POINT('',(-29.875,-10.2534818258363,-234.90005));
#192484=CARTESIAN_POINT('Origin',(-29.125,-10.2534818258363,-234.90005));
#192485=CARTESIAN_POINT('Origin',(-29.125,-10.2534818258363,-235.35005));
#192486=CARTESIAN_POINT('Origin',(-29.125,-10.2534818258363,-234.90005));
#192487=CARTESIAN_POINT('Origin',(-12.7946237611812,-10.2534818258363,-234.90005));
#192488=CARTESIAN_POINT('',(-11.6003099441285,-10.370163042821,-235.35005));
#192489=CARTESIAN_POINT('',(-12.0481776255232,-10.3264075864518,-234.90005));
#192490=CARTESIAN_POINT('Origin',(-11.6003099441285,-10.370163042821,-234.90005));
#192491=CARTESIAN_POINT('',(-12.7946237611812,-11.4534818258363,-235.35005));
#192492=CARTESIAN_POINT('Origin',(-12.7946237611812,-10.2534818258363,-235.35005));
#192493=CARTESIAN_POINT('',(-12.7946237611812,-11.0034818258363,-234.90005));
#192494=CARTESIAN_POINT('Origin',(-12.7946237611812,-11.4534818258363,-234.90005));
#192495=CARTESIAN_POINT('Origin',(-12.7946237611812,-10.2534818258363,-234.90005));
#192496=CARTESIAN_POINT('Origin',(296.501483394397,-11.4534818258365,-234.90005));
#192497=CARTESIAN_POINT('',(-19.,-11.0034818258363,-234.90005));
#192498=CARTESIAN_POINT('',(-19.,-11.4534818258363,-235.35005));
#192499=CARTESIAN_POINT('Origin',(-19.,-11.4534818258363,-234.90005));
#192500=CARTESIAN_POINT('',(2.22174260618994E-13,-11.0034818258363,-234.90005));
#192501=CARTESIAN_POINT('',(296.501483394397,-11.4534818258365,-235.35005));
#192502=CARTESIAN_POINT('Origin',(0.,-11.5034818258363,-234.90005));
#192503=CARTESIAN_POINT('',(-10.8748986968178,-7.30965533947201,-235.35005));
#192504=CARTESIAN_POINT('',(-11.294759518486,-7.14773903260897,-234.90005));
#192505=CARTESIAN_POINT('Origin',(-10.8748986968178,-7.30965533947201,-234.90005));
#192506=CARTESIAN_POINT('Origin',(0.,-11.5034818258363,-235.35005));
#192507=CARTESIAN_POINT('Origin',(0.,-11.5034818258363,-234.90005));
#192508=CARTESIAN_POINT('Origin',(-19.,-10.2534818258363,-234.90005));
#192509=CARTESIAN_POINT('',(-19.75,-10.2534818258363,-234.90005));
#192510=CARTESIAN_POINT('',(-20.2,-10.2534818258363,-235.35005));
#192511=CARTESIAN_POINT('Origin',(-20.2,-10.2534818258363,-234.90005));
#192512=CARTESIAN_POINT('Origin',(-19.,-10.2534818258363,-234.90005));
#192513=CARTESIAN_POINT('Origin',(-19.,-10.2534818258363,-235.35005));
#192514=CARTESIAN_POINT('Origin',(-20.625,-3.54959888009691,-234.90005));
#192515=CARTESIAN_POINT('',(-10.1749999999999,-3.54959888009691,-235.35005));
#192516=CARTESIAN_POINT('',(-10.6249999999999,-3.54959888009691,-234.90005));
#192517=CARTESIAN_POINT('Origin',(-10.1749999999999,-3.54959888009691,-234.90005));
#192518=CARTESIAN_POINT('Origin',(-20.625,-3.54959888009691,-235.35005));
#192519=CARTESIAN_POINT('Origin',(-20.625,-3.54959888009691,-234.90005));
#192520=CARTESIAN_POINT('Origin',(-20.2,-25.4138432731711,-234.90005));
#192521=CARTESIAN_POINT('',(-19.75,-2.14794227316951,-234.90005));
#192522=CARTESIAN_POINT('',(-20.2,-2.14794227316951,-235.35005));
#192523=CARTESIAN_POINT('Origin',(-20.2,-2.14794227316951,-234.90005));
#192524=CARTESIAN_POINT('',(-19.75,-10.2534818258363,-234.90005));
#192525=CARTESIAN_POINT('',(-20.2,-2.14794227316951,-235.35005));
#192526=CARTESIAN_POINT('Origin',(-10.1749999999999,-25.4138432731711,-234.90005));
#192527=CARTESIAN_POINT('',(-10.1749999999999,-2.14794227316951,-235.35005));
#192528=CARTESIAN_POINT('',(-10.6249999999999,-2.14794227316951,-234.90005));
#192529=CARTESIAN_POINT('Origin',(-10.1749999999999,-2.14794227316951,-234.90005));
#192530=CARTESIAN_POINT('',(-10.1749999999999,-3.54959888009691,-235.35005));
#192531=CARTESIAN_POINT('',(-10.6249999999999,-2.14794227316951,-234.90005));
#192532=CARTESIAN_POINT('Origin',(-19.,-2.14794227316951,-234.90005));
#192533=CARTESIAN_POINT('',(-19.,-1.39794227316951,-234.90005));
#192534=CARTESIAN_POINT('',(-19.,-0.947942273169507,-235.35005));
#192535=CARTESIAN_POINT('Origin',(-19.,-0.947942273169508,-234.90005));
#192536=CARTESIAN_POINT('Origin',(-19.,-2.14794227316951,-234.90005));
#192537=CARTESIAN_POINT('Origin',(-19.,-2.14794227316951,-235.35005));
#192538=CARTESIAN_POINT('Origin',(-11.3749999999999,-2.14794227316951,-234.90005));
#192539=CARTESIAN_POINT('',(-11.3749999999999,-0.947942273169504,-235.35005));
#192540=CARTESIAN_POINT('',(-11.3749999999999,-1.3979422731695,-234.90005));
#192541=CARTESIAN_POINT('Origin',(-11.3749999999999,-0.947942273169504,
-234.90005));
#192542=CARTESIAN_POINT('Origin',(-11.3749999999999,-2.14794227316951,-235.35005));
#192543=CARTESIAN_POINT('Origin',(-11.3749999999999,-2.14794227316951,-234.90005));
#192544=CARTESIAN_POINT('Origin',(296.501483394397,-0.94794227316939,-234.90005));
#192545=CARTESIAN_POINT('',(296.501483394397,-0.94794227316939,-235.35005));
#192546=CARTESIAN_POINT('',(1.11087130309497E-13,-1.3979422731695,-234.90005));
#192547=CARTESIAN_POINT('Origin',(-11.3749999999999,-20.8590213785032,-234.90005));
#192548=CARTESIAN_POINT('',(-10.1749999999999,-20.8590213785032,-235.35005));
#192549=CARTESIAN_POINT('',(-10.6249999999999,-20.8590213785032,-234.90005));
#192550=CARTESIAN_POINT('Origin',(-10.1749999999999,-20.8590213785032,-234.90005));
#192551=CARTESIAN_POINT('',(-11.3749999999999,-22.0590213785032,-235.35005));
#192552=CARTESIAN_POINT('Origin',(-11.3749999999999,-20.8590213785032,-235.35005));
#192553=CARTESIAN_POINT('',(-11.3749999999999,-21.6090213785032,-234.90005));
#192554=CARTESIAN_POINT('Origin',(-11.3749999999999,-22.0590213785032,-234.90005));
#192555=CARTESIAN_POINT('Origin',(-11.3749999999999,-20.8590213785032,-234.90005));
#192556=CARTESIAN_POINT('Origin',(296.501483394397,-22.0590213785033,-234.90005));
#192557=CARTESIAN_POINT('',(-19.,-21.6090213785031,-234.90005));
#192558=CARTESIAN_POINT('',(-19.,-22.0590213785031,-235.35005));
#192559=CARTESIAN_POINT('Origin',(-19.,-22.0590213785031,-234.90005));
#192560=CARTESIAN_POINT('',(3.33261390928491E-13,-21.6090213785032,-234.90005));
#192561=CARTESIAN_POINT('',(296.501483394397,-22.0590213785033,-235.35005));
#192562=CARTESIAN_POINT('Origin',(-10.1749999999999,-25.4138432731711,-234.90005));
#192563=CARTESIAN_POINT('',(-10.1749999999999,-19.4573647715757,-235.35005));
#192564=CARTESIAN_POINT('',(-10.6249999999999,-19.4573647715757,-234.90005));
#192565=CARTESIAN_POINT('Origin',(-10.1749999999999,-19.4573647715757,-234.90005));
#192566=CARTESIAN_POINT('',(-10.1749999999999,-20.8590213785032,-235.35005));
#192567=CARTESIAN_POINT('',(-10.6249999999999,-19.4573647715757,-234.90005));
#192568=CARTESIAN_POINT('Origin',(-19.,-20.8590213785032,-234.90005));
#192569=CARTESIAN_POINT('',(-19.75,-20.8590213785032,-234.90005));
#192570=CARTESIAN_POINT('',(-20.2,-20.8590213785032,-235.35005));
#192571=CARTESIAN_POINT('Origin',(-20.2,-20.8590213785032,-234.90005));
#192572=CARTESIAN_POINT('Origin',(-19.,-20.8590213785032,-234.90005));
#192573=CARTESIAN_POINT('Origin',(-19.,-20.8590213785032,-235.35005));
#192574=CARTESIAN_POINT('Origin',(-20.625,-19.4573647715757,-234.90005));
#192575=CARTESIAN_POINT('',(-10.8748986968178,-15.6973083122006,-235.35005));
#192576=CARTESIAN_POINT('',(-11.294759518486,-15.8592246190636,-234.90005));
#192577=CARTESIAN_POINT('Origin',(-10.8748986968178,-15.6973083122006,-234.90005));
#192578=CARTESIAN_POINT('Origin',(-20.625,-19.4573647715757,-235.35005));
#192579=CARTESIAN_POINT('Origin',(-20.625,-19.4573647715757,-234.90005));
#192580=CARTESIAN_POINT('Origin',(-20.2,-25.4138432731711,-234.90005));
#192581=CARTESIAN_POINT('',(-19.75,-12.7534818258363,-234.90005));
#192582=CARTESIAN_POINT('',(-20.2,-12.7534818258363,-235.35005));
#192583=CARTESIAN_POINT('Origin',(-20.2,-12.7534818258363,-234.90005));
#192584=CARTESIAN_POINT('',(-19.75,-20.8590213785032,-234.90005));
#192585=CARTESIAN_POINT('',(-20.2,-12.7534818258363,-235.35005));
#192586=CARTESIAN_POINT('Origin',(0.,-11.5034818258363,-234.90005));
#192587=CARTESIAN_POINT('',(-11.6003099441285,-12.6368006088516,-235.35005));
#192588=CARTESIAN_POINT('',(-12.0481776255232,-12.6805560652209,-234.90005));
#192589=CARTESIAN_POINT('Origin',(-11.6003099441285,-12.6368006088516,-234.90005));
#192590=CARTESIAN_POINT('Origin',(0.,-11.5034818258363,-235.35005));
#192591=CARTESIAN_POINT('Origin',(0.,-11.5034818258363,-234.90005));
#192592=CARTESIAN_POINT('Origin',(-19.,-12.7534818258363,-234.90005));
#192593=CARTESIAN_POINT('',(-19.,-12.0034818258363,-234.90005));
#192594=CARTESIAN_POINT('',(-19.,-11.5534818258363,-235.35005));
#192595=CARTESIAN_POINT('Origin',(-19.,-11.5534818258363,-234.90005));
#192596=CARTESIAN_POINT('Origin',(-19.,-12.7534818258363,-234.90005));
#192597=CARTESIAN_POINT('Origin',(-19.,-12.7534818258363,-235.35005));
#192598=CARTESIAN_POINT('Origin',(-12.7946237611812,-12.7534818258363,-234.90005));
#192599=CARTESIAN_POINT('',(-12.7946237611812,-11.5534818258363,-235.35005));
#192600=CARTESIAN_POINT('',(-12.7946237611812,-12.0034818258363,-234.90005));
#192601=CARTESIAN_POINT('Origin',(-12.7946237611812,-11.5534818258363,-234.90005));
#192602=CARTESIAN_POINT('Origin',(-12.7946237611812,-12.7534818258363,-235.35005));
#192603=CARTESIAN_POINT('Origin',(-12.7946237611812,-12.7534818258363,-234.90005));
#192604=CARTESIAN_POINT('Origin',(296.501483394397,-11.5534818258362,-234.90005));
#192605=CARTESIAN_POINT('',(296.501483394397,-11.5534818258362,-235.35005));
#192606=CARTESIAN_POINT('',(2.22174260618994E-13,-12.0034818258363,-234.90005));
#192607=CARTESIAN_POINT('Origin',(-21.5,-20.8590213785032,-234.90005));
#192608=CARTESIAN_POINT('',(-20.3,-20.8590213785032,-235.35005));
#192609=CARTESIAN_POINT('',(-20.75,-20.8590213785032,-234.90005));
#192610=CARTESIAN_POINT('Origin',(-20.3,-20.8590213785032,-234.90005));
#192611=CARTESIAN_POINT('',(-21.5,-22.0590213785031,-235.35005));
#192612=CARTESIAN_POINT('Origin',(-21.5,-20.8590213785032,-235.35005));
#192613=CARTESIAN_POINT('',(-21.5,-21.6090213785031,-234.90005));
#192614=CARTESIAN_POINT('Origin',(-21.5,-22.0590213785031,-234.90005));
#192615=CARTESIAN_POINT('Origin',(-21.5,-20.8590213785032,-234.90005));
#192616=CARTESIAN_POINT('Origin',(296.501483394397,-22.0590213785033,-234.90005));
#192617=CARTESIAN_POINT('',(-29.125,-21.6090213785031,-234.90005));
#192618=CARTESIAN_POINT('',(-29.125,-22.0590213785031,-235.35005));
#192619=CARTESIAN_POINT('Origin',(-29.125,-22.0590213785031,-234.90005));
#192620=CARTESIAN_POINT('',(3.33261390928491E-13,-21.6090213785032,-234.90005));
#192621=CARTESIAN_POINT('',(296.501483394397,-22.0590213785033,-235.35005));
#192622=CARTESIAN_POINT('Origin',(-20.3,-25.4138432731711,-234.90005));
#192623=CARTESIAN_POINT('',(-20.3,-12.7534818258363,-235.35005));
#192624=CARTESIAN_POINT('',(-20.75,-12.7534818258363,-234.90005));
#192625=CARTESIAN_POINT('Origin',(-20.3,-12.7534818258363,-234.90005));
#192626=CARTESIAN_POINT('',(-20.3,-20.8590213785032,-235.35005));
#192627=CARTESIAN_POINT('',(-20.75,-12.7534818258363,-234.90005));
#192628=CARTESIAN_POINT('Origin',(-29.125,-20.8590213785032,-234.90005));
#192629=CARTESIAN_POINT('',(-29.875,-20.8590213785032,-234.90005));
#192630=CARTESIAN_POINT('',(-30.325,-20.8590213785032,-235.35005));
#192631=CARTESIAN_POINT('Origin',(-30.325,-20.8590213785032,-234.90005));
#192632=CARTESIAN_POINT('Origin',(-29.125,-20.8590213785032,-234.90005));
#192633=CARTESIAN_POINT('Origin',(-29.125,-20.8590213785032,-235.35005));
#192634=CARTESIAN_POINT('Origin',(-21.5,-12.7534818258363,-234.90005));
#192635=CARTESIAN_POINT('',(-21.5,-11.5534818258363,-235.35005));
#192636=CARTESIAN_POINT('',(-21.5,-12.0034818258363,-234.90005));
#192637=CARTESIAN_POINT('Origin',(-21.5,-11.5534818258363,-234.90005));
#192638=CARTESIAN_POINT('Origin',(-21.5,-12.7534818258363,-235.35005));
#192639=CARTESIAN_POINT('Origin',(-21.5,-12.7534818258363,-234.90005));
#192640=CARTESIAN_POINT('Origin',(-30.325,-25.4138432731711,-234.90005));
#192641=CARTESIAN_POINT('',(-29.875,-12.7534818258363,-234.90005));
#192642=CARTESIAN_POINT('',(-30.325,-12.7534818258363,-235.35005));
#192643=CARTESIAN_POINT('Origin',(-30.325,-12.7534818258363,-234.90005));
#192644=CARTESIAN_POINT('',(-29.875,-20.8590213785032,-234.90005));
#192645=CARTESIAN_POINT('',(-30.325,-12.7534818258363,-235.35005));
#192646=CARTESIAN_POINT('Origin',(296.501483394397,-11.5534818258362,-234.90005));
#192647=CARTESIAN_POINT('',(-29.125,-11.5534818258363,-235.35005));
#192648=CARTESIAN_POINT('',(-29.125,-12.0034818258363,-234.90005));
#192649=CARTESIAN_POINT('Origin',(-29.125,-11.5534818258363,-234.90005));
#192650=CARTESIAN_POINT('',(296.501483394397,-11.5534818258362,-235.35005));
#192651=CARTESIAN_POINT('',(2.22174260618994E-13,-12.0034818258363,-234.90005));
#192652=CARTESIAN_POINT('Origin',(-29.125,-12.7534818258363,-234.90005));
#192653=CARTESIAN_POINT('Origin',(-29.125,-12.7534818258363,-235.35005));
#192654=CARTESIAN_POINT('Origin',(-29.125,-12.7534818258363,-234.90005));
#192655=CARTESIAN_POINT('Origin',(-31.625,-20.8590213785032,-234.90005));
#192656=CARTESIAN_POINT('',(-30.425,-20.8590213785032,-235.35005));
#192657=CARTESIAN_POINT('',(-30.875,-20.8590213785032,-234.90005));
#192658=CARTESIAN_POINT('Origin',(-30.425,-20.8590213785032,-234.90005));
#192659=CARTESIAN_POINT('',(-31.625,-22.0590213785031,-235.35005));
#192660=CARTESIAN_POINT('Origin',(-31.625,-20.8590213785032,-235.35005));
#192661=CARTESIAN_POINT('',(-31.625,-21.6090213785031,-234.90005));
#192662=CARTESIAN_POINT('Origin',(-31.625,-22.0590213785031,-234.90005));
#192663=CARTESIAN_POINT('Origin',(-31.625,-20.8590213785032,-234.90005));
#192664=CARTESIAN_POINT('Origin',(296.501483394397,-22.0590213785033,-234.90005));
#192665=CARTESIAN_POINT('',(-39.6853241707135,-21.6090213785031,-234.90005));
#192666=CARTESIAN_POINT('',(-39.6853241707135,-22.0590213785031,-235.35005));
#192667=CARTESIAN_POINT('Origin',(-39.6853241707135,-22.0590213785031,-234.90005));
#192668=CARTESIAN_POINT('',(3.33261390928491E-13,-21.6090213785032,-234.90005));
#192669=CARTESIAN_POINT('',(296.501483394397,-22.0590213785033,-235.35005));
#192670=CARTESIAN_POINT('Origin',(-30.425,-25.4138432731711,-234.90005));
#192671=CARTESIAN_POINT('',(-30.425,-12.7534818258363,-235.35005));
#192672=CARTESIAN_POINT('',(-30.875,-12.7534818258363,-234.90005));
#192673=CARTESIAN_POINT('Origin',(-30.425,-12.7534818258363,-234.90005));
#192674=CARTESIAN_POINT('',(-30.425,-20.8590213785032,-235.35005));
#192675=CARTESIAN_POINT('',(-30.875,-12.7534818258363,-234.90005));
#192676=CARTESIAN_POINT('Origin',(-39.6853241707135,-20.8590213785032,-234.90005));
#192677=CARTESIAN_POINT('',(-40.4352524876037,-20.8693905407753,-234.90005));
#192678=CARTESIAN_POINT('',(-40.8852094777378,-20.8756120381386,-235.35005));
#192679=CARTESIAN_POINT('Origin',(-40.8852094777378,-20.8756120381386,-234.90005));
#192680=CARTESIAN_POINT('Origin',(-39.6853241707135,-20.8590213785032,-234.90005));
#192681=CARTESIAN_POINT('Origin',(-39.6853241707135,-20.8590213785032,-235.35005));
#192682=CARTESIAN_POINT('Origin',(-31.625,-12.7534818258363,-234.90005));
#192683=CARTESIAN_POINT('',(-31.625,-11.5534818258363,-235.35005));
#192684=CARTESIAN_POINT('',(-31.625,-12.0034818258363,-234.90005));
#192685=CARTESIAN_POINT('Origin',(-31.625,-11.5534818258363,-234.90005));
#192686=CARTESIAN_POINT('Origin',(-31.625,-12.7534818258363,-235.35005));
#192687=CARTESIAN_POINT('Origin',(-31.625,-12.7534818258363,-234.90005));
#192688=CARTESIAN_POINT('Origin',(636.934816028482,-11.5034818258361,-234.90005));
#192689=CARTESIAN_POINT('',(-40.4988441937178,-12.754867256657,-234.90005));
#192690=CARTESIAN_POINT('',(-40.9488434259496,-12.7556985151494,-235.35005));
#192691=CARTESIAN_POINT('Origin',(-40.9488434259496,-12.7556985151494,-234.90005));
#192692=CARTESIAN_POINT('Origin',(636.934816028482,-11.5034818258361,-234.90005));
#192693=CARTESIAN_POINT('Origin',(636.934816028482,-11.5034818258361,-235.35005));
#192694=CARTESIAN_POINT('Origin',(296.501483394397,-11.5534818258362,-234.90005));
#192695=CARTESIAN_POINT('',(-39.7488454733312,-11.5534818258363,-235.35005));
#192696=CARTESIAN_POINT('',(-39.7488454733312,-12.0034818258363,-234.90005));
#192697=CARTESIAN_POINT('Origin',(-39.7488454733312,-11.5534818258363,-234.90005));
#192698=CARTESIAN_POINT('',(296.501483394397,-11.5534818258362,-235.35005));
#192699=CARTESIAN_POINT('',(2.22174260618994E-13,-12.0034818258363,-234.90005));
#192700=CARTESIAN_POINT('Origin',(-39.7488454733312,-12.7534818258363,-234.90005));
#192701=CARTESIAN_POINT('Origin',(-39.7488454733312,-12.7534818258363,-235.35005));
#192702=CARTESIAN_POINT('Origin',(-39.7488454733312,-12.7534818258363,-234.90005));
#192703=CARTESIAN_POINT('Origin',(-29.125,-23.3590213785032,-234.90005));
#192704=CARTESIAN_POINT('',(-30.325,-23.3590213785032,-235.35005));
#192705=CARTESIAN_POINT('',(-29.875,-23.3590213785032,-234.90005));
#192706=CARTESIAN_POINT('Origin',(-30.325,-23.3590213785032,-234.90005));
#192707=CARTESIAN_POINT('',(-29.125,-22.1590213785032,-235.35005));
#192708=CARTESIAN_POINT('Origin',(-29.125,-23.3590213785032,-235.35005));
#192709=CARTESIAN_POINT('',(-29.125,-22.6090213785032,-234.90005));
#192710=CARTESIAN_POINT('Origin',(-29.125,-22.1590213785032,-234.90005));
#192711=CARTESIAN_POINT('Origin',(-29.125,-23.3590213785032,-234.90005));
#192712=CARTESIAN_POINT('Origin',(296.501483394397,-22.1590213785031,-234.90005));
#192713=CARTESIAN_POINT('',(-21.5,-22.6090213785032,-234.90005));
#192714=CARTESIAN_POINT('',(-21.5,-22.1590213785032,-235.35005));
#192715=CARTESIAN_POINT('Origin',(-21.5,-22.1590213785032,-234.90005));
#192716=CARTESIAN_POINT('',(3.33261390928491E-13,-22.6090213785032,-234.90005));
#192717=CARTESIAN_POINT('',(296.501483394397,-22.1590213785031,-235.35005));
#192718=CARTESIAN_POINT('Origin',(-30.325,-25.4138432731711,-234.90005));
#192719=CARTESIAN_POINT('',(-30.325,-31.46456093117,-235.35005));
#192720=CARTESIAN_POINT('',(-29.875,-31.46456093117,-234.90005));
#192721=CARTESIAN_POINT('Origin',(-30.325,-31.46456093117,-234.90005));
#192722=CARTESIAN_POINT('',(-30.325,-23.3590213785032,-235.35005));
#192723=CARTESIAN_POINT('',(-29.875,-31.46456093117,-234.90005));
#192724=CARTESIAN_POINT('Origin',(-21.5,-23.3590213785032,-234.90005));
#192725=CARTESIAN_POINT('',(-20.75,-23.3590213785032,-234.90005));
#192726=CARTESIAN_POINT('',(-20.3,-23.3590213785032,-235.35005));
#192727=CARTESIAN_POINT('Origin',(-20.3,-23.3590213785032,-234.90005));
#192728=CARTESIAN_POINT('Origin',(-21.5,-23.3590213785032,-234.90005));
#192729=CARTESIAN_POINT('Origin',(-21.5,-23.3590213785032,-235.35005));
#192730=CARTESIAN_POINT('Origin',(-29.125,-31.46456093117,-234.90005));
#192731=CARTESIAN_POINT('',(-29.125,-32.66456093117,-235.35005));
#192732=CARTESIAN_POINT('',(-29.125,-32.21456093117,-234.90005));
#192733=CARTESIAN_POINT('Origin',(-29.125,-32.66456093117,-234.90005));
#192734=CARTESIAN_POINT('Origin',(-29.125,-31.46456093117,-235.35005));
#192735=CARTESIAN_POINT('Origin',(-29.125,-31.46456093117,-234.90005));
#192736=CARTESIAN_POINT('Origin',(-20.3,-25.4138432731711,-234.90005));
#192737=CARTESIAN_POINT('',(-20.75,-31.46456093117,-234.90005));
#192738=CARTESIAN_POINT('',(-20.3,-31.46456093117,-235.35005));
#192739=CARTESIAN_POINT('Origin',(-20.3,-31.46456093117,-234.90005));
#192740=CARTESIAN_POINT('',(-20.75,-23.3590213785032,-234.90005));
#192741=CARTESIAN_POINT('',(-20.3,-31.46456093117,-235.35005));
#192742=CARTESIAN_POINT('Origin',(296.501483394397,-32.6645609311701,-234.90005));
#192743=CARTESIAN_POINT('',(-21.5,-32.66456093117,-235.35005));
#192744=CARTESIAN_POINT('',(-21.5,-32.21456093117,-234.90005));
#192745=CARTESIAN_POINT('Origin',(-21.5,-32.66456093117,-234.90005));
#192746=CARTESIAN_POINT('',(296.501483394397,-32.6645609311701,-235.35005));
#192747=CARTESIAN_POINT('',(0.,-32.21456093117,-234.90005));
#192748=CARTESIAN_POINT('Origin',(-21.5,-31.46456093117,-234.90005));
#192749=CARTESIAN_POINT('Origin',(-21.5,-31.46456093117,-235.35005));
#192750=CARTESIAN_POINT('Origin',(-21.5,-31.46456093117,-234.90005));
#192751=CARTESIAN_POINT('Origin',(-19.,-23.3590213785032,-234.90005));
#192752=CARTESIAN_POINT('',(-20.2,-23.3590213785032,-235.35005));
#192753=CARTESIAN_POINT('',(-19.75,-23.3590213785032,-234.90005));
#192754=CARTESIAN_POINT('Origin',(-20.2,-23.3590213785032,-234.90005));
#192755=CARTESIAN_POINT('',(-19.,-22.1590213785032,-235.35005));
#192756=CARTESIAN_POINT('Origin',(-19.,-23.3590213785032,-235.35005));
#192757=CARTESIAN_POINT('',(-19.,-22.6090213785032,-234.90005));
#192758=CARTESIAN_POINT('Origin',(-19.,-22.1590213785032,-234.90005));
#192759=CARTESIAN_POINT('Origin',(-19.,-23.3590213785032,-234.90005));
#192760=CARTESIAN_POINT('Origin',(296.501483394397,-22.1590213785031,-234.90005));
#192761=CARTESIAN_POINT('',(-11.3749999999999,-22.6090213785032,-234.90005));
#192762=CARTESIAN_POINT('',(-11.3749999999999,-22.1590213785032,-235.35005));
#192763=CARTESIAN_POINT('Origin',(-11.3749999999999,-22.1590213785032,-234.90005));
#192764=CARTESIAN_POINT('',(3.33261390928491E-13,-22.6090213785032,-234.90005));
#192765=CARTESIAN_POINT('',(296.501483394397,-22.1590213785031,-235.35005));
#192766=CARTESIAN_POINT('Origin',(-20.2,-25.4138432731711,-234.90005));
#192767=CARTESIAN_POINT('',(-20.2,-31.46456093117,-235.35005));
#192768=CARTESIAN_POINT('',(-19.75,-31.46456093117,-234.90005));
#192769=CARTESIAN_POINT('Origin',(-20.2,-31.46456093117,-234.90005));
#192770=CARTESIAN_POINT('',(-20.2,-23.3590213785032,-235.35005));
#192771=CARTESIAN_POINT('',(-19.75,-31.46456093117,-234.90005));
#192772=CARTESIAN_POINT('Origin',(-11.3749999999999,-23.3590213785032,-234.90005));
#192773=CARTESIAN_POINT('',(-10.6249999999999,-23.3590213785032,-234.90005));
#192774=CARTESIAN_POINT('',(-10.1749999999999,-23.3590213785032,-235.35005));
#192775=CARTESIAN_POINT('Origin',(-10.1749999999999,-23.3590213785032,-234.90005));
#192776=CARTESIAN_POINT('Origin',(-11.3749999999999,-23.3590213785032,-234.90005));
#192777=CARTESIAN_POINT('Origin',(-11.3749999999999,-23.3590213785032,-235.35005));
#192778=CARTESIAN_POINT('Origin',(-19.,-31.46456093117,-234.90005));
#192779=CARTESIAN_POINT('',(-19.,-32.66456093117,-235.35005));
#192780=CARTESIAN_POINT('',(-19.,-32.21456093117,-234.90005));
#192781=CARTESIAN_POINT('Origin',(-19.,-32.66456093117,-234.90005));
#192782=CARTESIAN_POINT('Origin',(-19.,-31.46456093117,-235.35005));
#192783=CARTESIAN_POINT('Origin',(-19.,-31.46456093117,-234.90005));
#192784=CARTESIAN_POINT('Origin',(-10.1749999999999,-25.4138432731711,-234.90005));
#192785=CARTESIAN_POINT('',(-10.6249999999999,-31.46456093117,-234.90005));
#192786=CARTESIAN_POINT('',(-10.1749999999999,-31.46456093117,-235.35005));
#192787=CARTESIAN_POINT('Origin',(-10.1749999999999,-31.46456093117,-234.90005));
#192788=CARTESIAN_POINT('',(-10.6249999999999,-23.3590213785032,-234.90005));
#192789=CARTESIAN_POINT('',(-10.1749999999999,-31.46456093117,-235.35005));
#192790=CARTESIAN_POINT('Origin',(296.501483394397,-32.6645609311701,-234.90005));
#192791=CARTESIAN_POINT('',(-11.3749999999999,-32.66456093117,-235.35005));
#192792=CARTESIAN_POINT('',(-11.3749999999999,-32.21456093117,-234.90005));
#192793=CARTESIAN_POINT('Origin',(-11.3749999999999,-32.66456093117,-234.90005));
#192794=CARTESIAN_POINT('',(296.501483394397,-32.6645609311701,-235.35005));
#192795=CARTESIAN_POINT('',(0.,-32.21456093117,-234.90005));
#192796=CARTESIAN_POINT('Origin',(-11.3749999999999,-31.46456093117,-234.90005));
#192797=CARTESIAN_POINT('Origin',(-11.3749999999999,-31.46456093117,-235.35005));
#192798=CARTESIAN_POINT('Origin',(-11.3749999999999,-31.46456093117,-234.90005));
#192799=CARTESIAN_POINT('Origin',(-1.25,-31.46456093117,-234.90005));
#192800=CARTESIAN_POINT('',(-0.0499999999999941,-31.46456093117,-235.35005));
#192801=CARTESIAN_POINT('',(-0.5,-31.46456093117,-234.90005));
#192802=CARTESIAN_POINT('Origin',(-0.0499999999999941,-31.46456093117,-234.90005));
#192803=CARTESIAN_POINT('',(-1.25,-32.66456093117,-235.35005));
#192804=CARTESIAN_POINT('Origin',(-1.25,-31.46456093117,-235.35005));
#192805=CARTESIAN_POINT('',(-1.25,-32.21456093117,-234.90005));
#192806=CARTESIAN_POINT('Origin',(-1.25,-32.66456093117,-234.90005));
#192807=CARTESIAN_POINT('Origin',(-1.25,-31.46456093117,-234.90005));
#192808=CARTESIAN_POINT('Origin',(296.501483394397,-32.6645609311701,-234.90005));
#192809=CARTESIAN_POINT('',(-8.87499999999984,-32.21456093117,-234.90005));
#192810=CARTESIAN_POINT('',(-8.87499999999984,-32.66456093117,-235.35005));
#192811=CARTESIAN_POINT('Origin',(-8.87499999999984,-32.66456093117,-234.90005));
#192812=CARTESIAN_POINT('',(0.,-32.21456093117,-234.90005));
#192813=CARTESIAN_POINT('',(296.501483394397,-32.6645609311701,-235.35005));
#192814=CARTESIAN_POINT('Origin',(-0.0499999999999945,-25.4138432731711,
-234.90005));
#192815=CARTESIAN_POINT('',(-0.0499999999999967,-25.3025207885872,-235.35005));
#192816=CARTESIAN_POINT('',(-0.5,-25.3025207885872,-234.90005));
#192817=CARTESIAN_POINT('Origin',(-0.0499999999999967,-25.3025207885872,
-234.90005));
#192818=CARTESIAN_POINT('',(-0.0499999999999941,-31.46456093117,-235.35005));
#192819=CARTESIAN_POINT('',(-0.5,-25.3025207885872,-234.90005));
#192820=CARTESIAN_POINT('Origin',(-8.87499999999984,-31.46456093117,-234.90005));
#192821=CARTESIAN_POINT('',(-9.62499999999984,-31.46456093117,-234.90005));
#192822=CARTESIAN_POINT('',(-10.0749999999998,-31.46456093117,-235.35005));
#192823=CARTESIAN_POINT('Origin',(-10.0749999999998,-31.46456093117,-234.90005));
#192824=CARTESIAN_POINT('Origin',(-8.87499999999984,-31.46456093117,-234.90005));
#192825=CARTESIAN_POINT('Origin',(-8.87499999999984,-31.46456093117,-235.35005));
#192826=CARTESIAN_POINT('Origin',(-1.25,-25.3025207885872,-234.90005));
#192827=CARTESIAN_POINT('',(-1.14174005138534,-24.107414189356,-235.35005));
#192828=CARTESIAN_POINT('',(-1.18233753211584,-24.5555791640676,-234.90005));
#192829=CARTESIAN_POINT('Origin',(-1.14174005138534,-24.107414189356,-234.90005));
#192830=CARTESIAN_POINT('Origin',(-1.25,-25.3025207885872,-235.35005));
#192831=CARTESIAN_POINT('Origin',(-1.25,-25.3025207885872,-234.90005));
#192832=CARTESIAN_POINT('Origin',(-10.075,-25.4138432731712,-234.90005));
#192833=CARTESIAN_POINT('',(-9.62499999999985,-23.3741205625531,-234.90005));
#192834=CARTESIAN_POINT('',(-10.075,-23.3741205625531,-235.35005));
#192835=CARTESIAN_POINT('Origin',(-10.0749999999998,-23.3741205625531,-234.90005));
#192836=CARTESIAN_POINT('',(-9.62499999999984,-31.46456093117,-234.90005));
#192837=CARTESIAN_POINT('',(-10.075,-23.3741205625531,-235.35005));
#192838=CARTESIAN_POINT('Origin',(0.,-11.5034818258363,-234.90005));
#192839=CARTESIAN_POINT('',(-5.15044918227034,-23.0635663666157,-235.35005));
#192840=CARTESIAN_POINT('',(-5.33358654455951,-23.474614668563,-234.90005));
#192841=CARTESIAN_POINT('Origin',(-5.15044918227034,-23.0635663666157,-234.90005));
#192842=CARTESIAN_POINT('Origin',(0.,-11.5034818258363,-235.35005));
#192843=CARTESIAN_POINT('Origin',(0.,-11.5034818258363,-234.90005));
#192844=CARTESIAN_POINT('Origin',(-8.87499999999985,-23.3741205625531,-234.90005));
#192845=CARTESIAN_POINT('',(-8.80646304347558,-22.176079375619,-235.35005));
#192846=CARTESIAN_POINT('Origin',(-8.87499999999985,-23.3741205625531,-235.35005));
#192847=CARTESIAN_POINT('',(-8.83216440217218,-22.6253448207192,-234.90005));
#192848=CARTESIAN_POINT('Origin',(-8.80646304347558,-22.176079375619,-234.90005));
#192849=CARTESIAN_POINT('Origin',(-8.87499999999985,-23.3741205625531,-234.90005));
#192850=CARTESIAN_POINT('Origin',(-9.40330570654103,-32.6090213785032,-234.90005));
#192851=CARTESIAN_POINT('Origin',(-9.40330570654103,-32.6090213785032,-234.90005));
#192852=CARTESIAN_POINT('Origin',(-9.40330570654103,-32.6090213785032,-235.35005));
#192853=CARTESIAN_POINT('Origin',(-31.625,-31.46456093117,-234.90005));
#192854=CARTESIAN_POINT('',(-30.425,-31.46456093117,-235.35005));
#192855=CARTESIAN_POINT('',(-30.875,-31.46456093117,-234.90005));
#192856=CARTESIAN_POINT('Origin',(-30.425,-31.46456093117,-234.90005));
#192857=CARTESIAN_POINT('',(-31.625,-32.66456093117,-235.35005));
#192858=CARTESIAN_POINT('Origin',(-31.625,-31.46456093117,-235.35005));
#192859=CARTESIAN_POINT('',(-31.625,-32.21456093117,-234.90005));
#192860=CARTESIAN_POINT('Origin',(-31.625,-32.66456093117,-234.90005));
#192861=CARTESIAN_POINT('Origin',(-31.625,-31.46456093117,-234.90005));
#192862=CARTESIAN_POINT('Origin',(296.501483394397,-32.6645609311701,-234.90005));
#192863=CARTESIAN_POINT('',(-39.4555265729267,-32.21456093117,-234.90005));
#192864=CARTESIAN_POINT('',(-39.4555265729267,-32.66456093117,-235.35005));
#192865=CARTESIAN_POINT('Origin',(-39.4555265729267,-32.66456093117,-234.90005));
#192866=CARTESIAN_POINT('',(0.,-32.21456093117,-234.90005));
#192867=CARTESIAN_POINT('',(296.501483394397,-32.6645609311701,-235.35005));
#192868=CARTESIAN_POINT('Origin',(-30.425,-25.4138432731711,-234.90005));
#192869=CARTESIAN_POINT('',(-30.425,-23.3590213785032,-235.35005));
#192870=CARTESIAN_POINT('',(-30.875,-23.3590213785032,-234.90005));
#192871=CARTESIAN_POINT('Origin',(-30.425,-23.3590213785032,-234.90005));
#192872=CARTESIAN_POINT('',(-30.425,-31.46456093117,-235.35005));
#192873=CARTESIAN_POINT('',(-30.875,-23.3590213785032,-234.90005));
#192874=CARTESIAN_POINT('Origin',(-39.4555265729267,-31.46456093117,-234.90005));
#192875=CARTESIAN_POINT('',(-40.2052001948774,-31.486684686535,-234.90005));
#192876=CARTESIAN_POINT('',(-40.6550043680477,-31.499958939754,-235.35005));
#192877=CARTESIAN_POINT('Origin',(-40.6550043680476,-31.499958939754,-234.90005));
#192878=CARTESIAN_POINT('Origin',(-39.4555265729267,-31.46456093117,-234.90005));
#192879=CARTESIAN_POINT('Origin',(-39.4555265729267,-31.46456093117,-235.35005));
#192880=CARTESIAN_POINT('Origin',(-31.625,-23.3590213785032,-234.90005));
#192881=CARTESIAN_POINT('',(-31.625,-22.1590213785032,-235.35005));
#192882=CARTESIAN_POINT('',(-31.625,-22.6090213785032,-234.90005));
#192883=CARTESIAN_POINT('Origin',(-31.625,-22.1590213785032,-234.90005));
#192884=CARTESIAN_POINT('Origin',(-31.625,-23.3590213785032,-235.35005));
#192885=CARTESIAN_POINT('Origin',(-31.625,-23.3590213785032,-234.90005));
#192886=CARTESIAN_POINT('Origin',(636.934816028482,-11.5034818258361,-234.90005));
#192887=CARTESIAN_POINT('',(-40.3960221980465,-23.3721614024167,-234.90005));
#192888=CARTESIAN_POINT('',(-40.8459531286544,-23.3800454167648,-235.35005));
#192889=CARTESIAN_POINT('Origin',(-40.8459531286544,-23.3800454167648,-234.90005));
#192890=CARTESIAN_POINT('Origin',(636.934816028482,-11.5034818258361,-234.90005));
#192891=CARTESIAN_POINT('Origin',(636.934816028482,-11.5034818258361,-235.35005));
#192892=CARTESIAN_POINT('Origin',(296.501483394397,-22.1590213785031,-234.90005));
#192893=CARTESIAN_POINT('',(-39.6461373136998,-22.1590213785032,-235.35005));
#192894=CARTESIAN_POINT('',(-39.6461373136998,-22.6090213785032,-234.90005));
#192895=CARTESIAN_POINT('Origin',(-39.6461373136998,-22.1590213785032,-234.90005));
#192896=CARTESIAN_POINT('',(296.501483394397,-22.1590213785031,-235.35005));
#192897=CARTESIAN_POINT('',(3.33261390928491E-13,-22.6090213785032,-234.90005));
#192898=CARTESIAN_POINT('Origin',(-39.6461373136998,-23.3590213785032,-234.90005));
#192899=CARTESIAN_POINT('Origin',(-39.6461373136998,-23.3590213785032,-235.35005));
#192900=CARTESIAN_POINT('Origin',(-39.6461373136998,-23.3590213785032,-234.90005));
#192901=CARTESIAN_POINT('Origin',(-31.625,-42.0701004838368,-234.90005));
#192902=CARTESIAN_POINT('',(-30.425,-42.0701004838368,-235.35005));
#192903=CARTESIAN_POINT('',(-30.875,-42.0701004838368,-234.90005));
#192904=CARTESIAN_POINT('Origin',(-30.425,-42.0701004838368,-234.90005));
#192905=CARTESIAN_POINT('',(-31.625,-43.2701004838368,-235.35005));
#192906=CARTESIAN_POINT('Origin',(-31.625,-42.0701004838368,-235.35005));
#192907=CARTESIAN_POINT('',(-31.625,-42.8201004838368,-234.90005));
#192908=CARTESIAN_POINT('Origin',(-31.625,-43.2701004838368,-234.90005));
#192909=CARTESIAN_POINT('Origin',(-31.625,-42.0701004838368,-234.90005));
#192910=CARTESIAN_POINT('Origin',(296.501483394397,-43.270100483837,-234.90005));
#192911=CARTESIAN_POINT('',(-36.0311576807678,-42.8201004838368,-234.90005));
#192912=CARTESIAN_POINT('',(-36.0311576807678,-43.2701004838368,-235.35005));
#192913=CARTESIAN_POINT('Origin',(-36.0311576807678,-43.2701004838368,-234.90005));
#192914=CARTESIAN_POINT('',(1.54373336646987E-15,-42.8201004838369,-234.90005));
#192915=CARTESIAN_POINT('',(296.501483394397,-43.270100483837,-235.35005));
#192916=CARTESIAN_POINT('Origin',(-30.425,-25.4138432731711,-234.90005));
#192917=CARTESIAN_POINT('',(-30.425,-33.96456093117,-235.35005));
#192918=CARTESIAN_POINT('',(-30.875,-33.96456093117,-234.90005));
#192919=CARTESIAN_POINT('Origin',(-30.425,-33.96456093117,-234.90005));
#192920=CARTESIAN_POINT('',(-30.425,-42.0701004838368,-235.35005));
#192921=CARTESIAN_POINT('',(-30.875,-33.96456093117,-234.90005));
#192922=CARTESIAN_POINT('Origin',(-36.0311576807678,-42.0701004838368,-234.90005));
#192923=CARTESIAN_POINT('',(-36.6030808185578,-42.5552849069797,-234.90005));
#192924=CARTESIAN_POINT('',(-36.9462347012318,-42.8463955608654,-235.35005));
#192925=CARTESIAN_POINT('Origin',(-36.9462347012318,-42.8463955608654,-234.90005));
#192926=CARTESIAN_POINT('Origin',(-36.0311576807678,-42.0701004838368,-234.90005));
#192927=CARTESIAN_POINT('Origin',(-36.0311576807678,-42.0701004838368,-235.35005));
#192928=CARTESIAN_POINT('Origin',(-31.625,-33.96456093117,-234.90005));
#192929=CARTESIAN_POINT('',(-31.625,-32.76456093117,-235.35005));
#192930=CARTESIAN_POINT('',(-31.625,-33.21456093117,-234.90005));
#192931=CARTESIAN_POINT('Origin',(-31.625,-32.76456093117,-234.90005));
#192932=CARTESIAN_POINT('Origin',(-31.625,-33.96456093117,-235.35005));
#192933=CARTESIAN_POINT('Origin',(-31.625,-33.96456093117,-234.90005));
#192934=CARTESIAN_POINT('Origin',(6.29739814579425E-15,-11.5034818258363,
-234.90005));
#192935=CARTESIAN_POINT('',(-39.8203148590358,-38.3053945286125,-234.90005));
#192936=CARTESIAN_POINT('',(-40.1936303108393,-38.5566624602009,-235.35005));
#192937=CARTESIAN_POINT('Origin',(-40.1936303108393,-38.5566624602009,-234.90005));
#192938=CARTESIAN_POINT('Origin',(6.29739814579425E-15,-11.5034818258363,
-234.90005));
#192939=CARTESIAN_POINT('Origin',(6.29739814579425E-15,-11.5034818258363,
-235.35005));
#192940=CARTESIAN_POINT('Origin',(296.501483394397,-32.7645609311699,-234.90005));
#192941=CARTESIAN_POINT('',(-39.3771239584772,-32.76456093117,-235.35005));
#192942=CARTESIAN_POINT('',(-39.3771239584772,-33.21456093117,-234.90005));
#192943=CARTESIAN_POINT('Origin',(-39.3771239584772,-32.76456093117,-234.90005));
#192944=CARTESIAN_POINT('',(296.501483394397,-32.7645609311699,-235.35005));
#192945=CARTESIAN_POINT('',(0.,-33.21456093117,-234.90005));
#192946=CARTESIAN_POINT('Origin',(-38.9907249661392,-37.7470213473046,-234.90005));
#192947=CARTESIAN_POINT('',(-39.989972084972,-37.7858181964606,-234.90005));
#192948=CARTESIAN_POINT('',(-40.4396332884467,-37.8032767785809,-235.35005));
#192949=CARTESIAN_POINT('Origin',(-40.4396332884467,-37.8032767785809,-234.90005));
#192950=CARTESIAN_POINT('Origin',(-38.9907249661392,-37.7470213473046,-234.90005));
#192951=CARTESIAN_POINT('Origin',(-38.9907249661392,-37.7470213473046,-235.35005));
#192952=CARTESIAN_POINT('Origin',(-39.3771239584772,-33.96456093117,-234.90005));
#192953=CARTESIAN_POINT('',(-40.5764627182082,-34.0043923183801,-235.35005));
#192954=CARTESIAN_POINT('',(-40.1267106833092,-33.9894555481763,-234.90005));
#192955=CARTESIAN_POINT('Origin',(-40.5764627182082,-34.0043923183801,-234.90005));
#192956=CARTESIAN_POINT('Origin',(-39.3771239584772,-33.96456093117,-235.35005));
#192957=CARTESIAN_POINT('Origin',(-39.3771239584772,-33.96456093117,-234.90005));
#192958=CARTESIAN_POINT('Origin',(636.934816028482,-11.5034818258361,-234.90005));
#192959=CARTESIAN_POINT('Origin',(636.934816028482,-11.5034818258361,-235.35005));
#192960=CARTESIAN_POINT('Origin',(636.934816028482,-11.5034818258361,-234.90005));
#192961=CARTESIAN_POINT('Origin',(-21.5,-42.0701004838368,-234.90005));
#192962=CARTESIAN_POINT('',(-20.3,-42.0701004838368,-235.35005));
#192963=CARTESIAN_POINT('',(-20.75,-42.0701004838368,-234.90005));
#192964=CARTESIAN_POINT('Origin',(-20.3,-42.0701004838368,-234.90005));
#192965=CARTESIAN_POINT('',(-21.5,-43.2701004838368,-235.35005));
#192966=CARTESIAN_POINT('Origin',(-21.5,-42.0701004838368,-235.35005));
#192967=CARTESIAN_POINT('',(-21.5,-42.8201004838368,-234.90005));
#192968=CARTESIAN_POINT('Origin',(-21.5,-43.2701004838368,-234.90005));
#192969=CARTESIAN_POINT('Origin',(-21.5,-42.0701004838368,-234.90005));
#192970=CARTESIAN_POINT('Origin',(296.501483394397,-43.270100483837,-234.90005));
#192971=CARTESIAN_POINT('',(-29.125,-42.8201004838368,-234.90005));
#192972=CARTESIAN_POINT('',(-29.125,-43.2701004838368,-235.35005));
#192973=CARTESIAN_POINT('Origin',(-29.125,-43.2701004838368,-234.90005));
#192974=CARTESIAN_POINT('',(1.54373336646987E-15,-42.8201004838369,-234.90005));
#192975=CARTESIAN_POINT('',(296.501483394397,-43.270100483837,-235.35005));
#192976=CARTESIAN_POINT('Origin',(-20.3,-25.4138432731711,-234.90005));
#192977=CARTESIAN_POINT('',(-20.3,-33.96456093117,-235.35005));
#192978=CARTESIAN_POINT('',(-20.75,-33.96456093117,-234.90005));
#192979=CARTESIAN_POINT('Origin',(-20.3,-33.96456093117,-234.90005));
#192980=CARTESIAN_POINT('',(-20.3,-42.0701004838368,-235.35005));
#192981=CARTESIAN_POINT('',(-20.75,-33.96456093117,-234.90005));
#192982=CARTESIAN_POINT('Origin',(-29.125,-42.0701004838368,-234.90005));
#192983=CARTESIAN_POINT('',(-29.875,-42.0701004838368,-234.90005));
#192984=CARTESIAN_POINT('',(-30.325,-42.0701004838368,-235.35005));
#192985=CARTESIAN_POINT('Origin',(-30.325,-42.0701004838368,-234.90005));
#192986=CARTESIAN_POINT('Origin',(-29.125,-42.0701004838368,-234.90005));
#192987=CARTESIAN_POINT('Origin',(-29.125,-42.0701004838368,-235.35005));
#192988=CARTESIAN_POINT('Origin',(-21.5,-33.96456093117,-234.90005));
#192989=CARTESIAN_POINT('',(-21.5,-32.76456093117,-235.35005));
#192990=CARTESIAN_POINT('',(-21.5,-33.21456093117,-234.90005));
#192991=CARTESIAN_POINT('Origin',(-21.5,-32.76456093117,-234.90005));
#192992=CARTESIAN_POINT('Origin',(-21.5,-33.96456093117,-235.35005));
#192993=CARTESIAN_POINT('Origin',(-21.5,-33.96456093117,-234.90005));
#192994=CARTESIAN_POINT('Origin',(-30.325,-25.4138432731711,-234.90005));
#192995=CARTESIAN_POINT('',(-29.875,-33.96456093117,-234.90005));
#192996=CARTESIAN_POINT('',(-30.325,-33.96456093117,-235.35005));
#192997=CARTESIAN_POINT('Origin',(-30.325,-33.96456093117,-234.90005));
#192998=CARTESIAN_POINT('',(-29.875,-42.0701004838368,-234.90005));
#192999=CARTESIAN_POINT('',(-30.325,-33.96456093117,-235.35005));
#193000=CARTESIAN_POINT('Origin',(296.501483394397,-32.7645609311699,-234.90005));
#193001=CARTESIAN_POINT('',(-29.125,-32.76456093117,-235.35005));
#193002=CARTESIAN_POINT('',(-29.125,-33.21456093117,-234.90005));
#193003=CARTESIAN_POINT('Origin',(-29.125,-32.76456093117,-234.90005));
#193004=CARTESIAN_POINT('',(296.501483394397,-32.7645609311699,-235.35005));
#193005=CARTESIAN_POINT('',(0.,-33.21456093117,-234.90005));
#193006=CARTESIAN_POINT('Origin',(-29.125,-33.96456093117,-234.90005));
#193007=CARTESIAN_POINT('Origin',(-29.125,-33.96456093117,-235.35005));
#193008=CARTESIAN_POINT('Origin',(-29.125,-33.96456093117,-234.90005));
#193009=CARTESIAN_POINT('Origin',(-29.125,-44.5701004838368,-234.90005));
#193010=CARTESIAN_POINT('',(-30.325,-44.5701004838368,-235.35005));
#193011=CARTESIAN_POINT('',(-29.875,-44.5701004838368,-234.90005));
#193012=CARTESIAN_POINT('Origin',(-30.325,-44.5701004838368,-234.90005));
#193013=CARTESIAN_POINT('',(-29.125,-43.3701004838369,-235.35005));
#193014=CARTESIAN_POINT('Origin',(-29.125,-44.5701004838368,-235.35005));
#193015=CARTESIAN_POINT('',(-29.125,-43.8201004838368,-234.90005));
#193016=CARTESIAN_POINT('Origin',(-29.125,-43.3701004838369,-234.90005));
#193017=CARTESIAN_POINT('Origin',(-29.125,-44.5701004838368,-234.90005));
#193018=CARTESIAN_POINT('Origin',(296.501483394397,-43.3701004838369,-234.90005));
#193019=CARTESIAN_POINT('',(-21.5,-43.8201004838368,-234.90005));
#193020=CARTESIAN_POINT('',(-21.5,-43.3701004838369,-235.35005));
#193021=CARTESIAN_POINT('Origin',(-21.5,-43.3701004838369,-234.90005));
#193022=CARTESIAN_POINT('',(1.23757166668304E-15,-43.8201004838368,-234.90005));
#193023=CARTESIAN_POINT('',(296.501483394397,-43.3701004838369,-235.35005));
#193024=CARTESIAN_POINT('Origin',(-30.325,-25.4138432731711,-234.90005));
#193025=CARTESIAN_POINT('',(-30.325,-48.7096221120845,-235.35005));
#193026=CARTESIAN_POINT('',(-29.875,-48.7096221120845,-234.90005));
#193027=CARTESIAN_POINT('Origin',(-30.325,-48.7096221120845,-234.90005));
#193028=CARTESIAN_POINT('',(-30.325,-44.5701004838368,-235.35005));
#193029=CARTESIAN_POINT('',(-29.875,-48.7096221120845,-234.90005));
#193030=CARTESIAN_POINT('Origin',(-21.5,-44.5701004838368,-234.90005));
#193031=CARTESIAN_POINT('',(-20.75,-44.5701004838368,-234.90005));
#193032=CARTESIAN_POINT('',(-20.3,-44.5701004838368,-235.35005));
#193033=CARTESIAN_POINT('Origin',(-20.3,-44.5701004838368,-234.90005));
#193034=CARTESIAN_POINT('Origin',(-21.5,-44.5701004838368,-234.90005));
#193035=CARTESIAN_POINT('Origin',(-21.5,-44.5701004838368,-235.35005));
#193036=CARTESIAN_POINT('Origin',(-29.125,-48.7096221120845,-234.90005));
#193037=CARTESIAN_POINT('',(-29.8646825396825,-49.6545399606241,-235.35005));
#193038=CARTESIAN_POINT('',(-29.5873015873016,-49.3001957674217,-234.90005));
#193039=CARTESIAN_POINT('Origin',(-29.8646825396825,-49.6545399606241,-234.90005));
#193040=CARTESIAN_POINT('Origin',(-29.125,-48.7096221120845,-235.35005));
#193041=CARTESIAN_POINT('Origin',(-29.125,-48.7096221120845,-234.90005));
#193042=CARTESIAN_POINT('Origin',(-20.3,-25.4138432731711,-234.90005));
#193043=CARTESIAN_POINT('',(-20.75,-52.8339989151841,-234.90005));
#193044=CARTESIAN_POINT('',(-20.3,-52.8339989151841,-235.35005));
#193045=CARTESIAN_POINT('Origin',(-20.3,-52.8339989151841,-234.90005));
#193046=CARTESIAN_POINT('',(-20.75,-44.5701004838368,-234.90005));
#193047=CARTESIAN_POINT('',(-20.3,-52.8339989151841,-235.35005));
#193048=CARTESIAN_POINT('Origin',(6.29739814579425E-15,-11.5034818258363,
-234.90005));
#193049=CARTESIAN_POINT('',(-23.6248477671233,-53.8032344017111,-235.35005));
#193050=CARTESIAN_POINT('',(-23.4054219364689,-53.410357442802,-234.90005));
#193051=CARTESIAN_POINT('Origin',(-23.6248477671233,-53.8032344017111,-234.90005));
#193052=CARTESIAN_POINT('Origin',(6.29739814579425E-15,-11.5034818258363,
-235.35005));
#193053=CARTESIAN_POINT('Origin',(6.29739814579425E-15,-11.5034818258363,
-234.90005));
#193054=CARTESIAN_POINT('Origin',(-21.5,-52.8339989151841,-234.90005));
#193055=CARTESIAN_POINT('',(-21.5238294101154,-53.5836202590729,-234.90005));
#193056=CARTESIAN_POINT('',(-21.5381270561845,-54.0333930654061,-235.35005));
#193057=CARTESIAN_POINT('Origin',(-21.5381270561845,-54.0333930654061,-234.90005));
#193058=CARTESIAN_POINT('Origin',(-21.5,-52.8339989151841,-234.90005));
#193059=CARTESIAN_POINT('Origin',(-21.5,-52.8339989151841,-235.35005));
#193060=CARTESIAN_POINT('Origin',(-22.9178089794592,-52.5372975341153,-234.90005));
#193061=CARTESIAN_POINT('',(-22.9669354026308,-53.9864650863833,-235.35005));
#193062=CARTESIAN_POINT('',(-22.9516892713016,-53.5367234322311,-234.90005));
#193063=CARTESIAN_POINT('Origin',(-22.9669354026308,-53.9864650863833,-234.90005));
#193064=CARTESIAN_POINT('Origin',(-22.9178089794592,-52.5372975341153,-235.35005));
#193065=CARTESIAN_POINT('Origin',(-22.9178089794592,-52.5372975341153,-234.90005));
#193066=CARTESIAN_POINT('Origin',(-7.14692237356698E-14,623.509175991979,
-234.90005));
#193067=CARTESIAN_POINT('Origin',(-7.14692237356698E-14,623.509175991979,
-235.35005));
#193068=CARTESIAN_POINT('Origin',(-7.14692237356698E-14,623.509175991979,
-234.90005));
#193069=CARTESIAN_POINT('Origin',(-19.,-44.5701004838368,-234.90005));
#193070=CARTESIAN_POINT('',(-20.2,-44.5701004838368,-235.35005));
#193071=CARTESIAN_POINT('',(-19.75,-44.5701004838368,-234.90005));
#193072=CARTESIAN_POINT('Origin',(-20.2,-44.5701004838368,-234.90005));
#193073=CARTESIAN_POINT('',(-19.,-43.3701004838369,-235.35005));
#193074=CARTESIAN_POINT('Origin',(-19.,-44.5701004838368,-235.35005));
#193075=CARTESIAN_POINT('',(-19.,-43.8201004838368,-234.90005));
#193076=CARTESIAN_POINT('Origin',(-19.,-43.3701004838369,-234.90005));
#193077=CARTESIAN_POINT('Origin',(-19.,-44.5701004838368,-234.90005));
#193078=CARTESIAN_POINT('Origin',(296.501483394397,-43.3701004838369,-234.90005));
#193079=CARTESIAN_POINT('',(-11.3749999999999,-43.8201004838368,-234.90005));
#193080=CARTESIAN_POINT('',(-11.3749999999999,-43.3701004838369,-235.35005));
#193081=CARTESIAN_POINT('Origin',(-11.3749999999999,-43.3701004838369,-234.90005));
#193082=CARTESIAN_POINT('',(1.23757166668304E-15,-43.8201004838368,-234.90005));
#193083=CARTESIAN_POINT('',(296.501483394397,-43.3701004838369,-235.35005));
#193084=CARTESIAN_POINT('Origin',(-20.2,-25.4138432731711,-234.90005));
#193085=CARTESIAN_POINT('',(-20.2,-52.9088458284789,-235.35005));
#193086=CARTESIAN_POINT('',(-19.75,-52.9088458284789,-234.90005));
#193087=CARTESIAN_POINT('Origin',(-20.2,-52.9088458284789,-234.90005));
#193088=CARTESIAN_POINT('',(-20.2,-44.5701004838368,-235.35005));
#193089=CARTESIAN_POINT('',(-19.75,-52.9088458284789,-234.90005));
#193090=CARTESIAN_POINT('Origin',(-11.3749999999999,-44.5701004838369,-234.90005));
#193091=CARTESIAN_POINT('',(-10.6249999999999,-44.5701004838369,-234.90005));
#193092=CARTESIAN_POINT('',(-10.1749999999999,-44.5701004838369,-235.35005));
#193093=CARTESIAN_POINT('Origin',(-10.1749999999999,-44.5701004838369,-234.90005));
#193094=CARTESIAN_POINT('Origin',(-11.3749999999999,-44.5701004838369,-234.90005));
#193095=CARTESIAN_POINT('Origin',(-11.3749999999999,-44.5701004838369,-235.35005));
#193096=CARTESIAN_POINT('Origin',(-19.,-52.9088458284789,-234.90005));
#193097=CARTESIAN_POINT('',(-19.0336936775584,-54.1083727085831,-235.35005));
#193098=CARTESIAN_POINT('',(-19.021058548474,-53.6585501285442,-234.90005));
#193099=CARTESIAN_POINT('Origin',(-19.0336936775584,-54.1083727085831,-234.90005));
#193100=CARTESIAN_POINT('Origin',(-19.,-52.9088458284789,-235.35005));
#193101=CARTESIAN_POINT('Origin',(-19.,-52.9088458284789,-234.90005));
#193102=CARTESIAN_POINT('Origin',(-10.1749999999999,-25.4138432731711,-234.90005));
#193103=CARTESIAN_POINT('',(-10.6249999999999,-53.08002700974,-234.90005));
#193104=CARTESIAN_POINT('',(-10.1749999999999,-53.08002700974,-235.35005));
#193105=CARTESIAN_POINT('Origin',(-10.1749999999999,-53.08002700974,-234.90005));
#193106=CARTESIAN_POINT('',(-10.6249999999999,-44.5701004838369,-234.90005));
#193107=CARTESIAN_POINT('',(-10.1749999999999,-53.08002700974,-235.35005));
#193108=CARTESIAN_POINT('Origin',(-7.14692237356698E-14,623.509175991979,
-234.90005));
#193109=CARTESIAN_POINT('',(-11.3951718727487,-54.2798574542403,-235.35005));
#193110=CARTESIAN_POINT('',(-11.3876074204679,-53.8299210375529,-234.90005));
#193111=CARTESIAN_POINT('Origin',(-11.3951718727487,-54.2798574542403,-234.90005));
#193112=CARTESIAN_POINT('Origin',(-7.14692237356698E-14,623.509175991979,
-235.35005));
#193113=CARTESIAN_POINT('Origin',(-7.14692237356698E-14,623.509175991979,
-234.90005));
#193114=CARTESIAN_POINT('Origin',(-11.3749999999999,-53.08002700974,-234.90005));
#193115=CARTESIAN_POINT('Origin',(-11.3749999999999,-53.08002700974,-235.35005));
#193116=CARTESIAN_POINT('Origin',(-11.3749999999999,-53.08002700974,-234.90005));
#193117=CARTESIAN_POINT('Origin',(-11.3749999999999,-42.0701004838369,-234.90005));
#193118=CARTESIAN_POINT('',(-10.1749999999999,-42.0701004838368,-235.35005));
#193119=CARTESIAN_POINT('',(-10.6249999999999,-42.0701004838368,-234.90005));
#193120=CARTESIAN_POINT('Origin',(-10.1749999999999,-42.0701004838368,-234.90005));
#193121=CARTESIAN_POINT('',(-11.3749999999999,-43.2701004838368,-235.35005));
#193122=CARTESIAN_POINT('Origin',(-11.3749999999999,-42.0701004838369,-235.35005));
#193123=CARTESIAN_POINT('',(-11.3749999999999,-42.8201004838369,-234.90005));
#193124=CARTESIAN_POINT('Origin',(-11.3749999999999,-43.2701004838368,-234.90005));
#193125=CARTESIAN_POINT('Origin',(-11.3749999999999,-42.0701004838369,-234.90005));
#193126=CARTESIAN_POINT('Origin',(296.501483394397,-43.270100483837,-234.90005));
#193127=CARTESIAN_POINT('',(-19.,-42.8201004838368,-234.90005));
#193128=CARTESIAN_POINT('',(-19.,-43.2701004838368,-235.35005));
#193129=CARTESIAN_POINT('Origin',(-19.,-43.2701004838368,-234.90005));
#193130=CARTESIAN_POINT('',(1.54373336646987E-15,-42.8201004838369,-234.90005));
#193131=CARTESIAN_POINT('',(296.501483394397,-43.270100483837,-235.35005));
#193132=CARTESIAN_POINT('Origin',(-10.1749999999999,-25.4138432731711,-234.90005));
#193133=CARTESIAN_POINT('',(-10.1749999999999,-33.96456093117,-235.35005));
#193134=CARTESIAN_POINT('',(-10.6249999999999,-33.96456093117,-234.90005));
#193135=CARTESIAN_POINT('Origin',(-10.1749999999999,-33.96456093117,-234.90005));
#193136=CARTESIAN_POINT('',(-10.1749999999999,-42.0701004838368,-235.35005));
#193137=CARTESIAN_POINT('',(-10.6249999999999,-33.96456093117,-234.90005));
#193138=CARTESIAN_POINT('Origin',(-19.,-42.0701004838368,-234.90005));
#193139=CARTESIAN_POINT('',(-19.75,-42.0701004838368,-234.90005));
#193140=CARTESIAN_POINT('',(-20.2,-42.0701004838368,-235.35005));
#193141=CARTESIAN_POINT('Origin',(-20.2,-42.0701004838368,-234.90005));
#193142=CARTESIAN_POINT('Origin',(-19.,-42.0701004838368,-234.90005));
#193143=CARTESIAN_POINT('Origin',(-19.,-42.0701004838368,-235.35005));
#193144=CARTESIAN_POINT('Origin',(-11.3749999999999,-33.96456093117,-234.90005));
#193145=CARTESIAN_POINT('',(-11.3749999999999,-32.76456093117,-235.35005));
#193146=CARTESIAN_POINT('',(-11.3749999999999,-33.21456093117,-234.90005));
#193147=CARTESIAN_POINT('Origin',(-11.3749999999999,-32.76456093117,-234.90005));
#193148=CARTESIAN_POINT('Origin',(-11.3749999999999,-33.96456093117,-235.35005));
#193149=CARTESIAN_POINT('Origin',(-11.3749999999999,-33.96456093117,-234.90005));
#193150=CARTESIAN_POINT('Origin',(-20.2,-25.4138432731711,-234.90005));
#193151=CARTESIAN_POINT('',(-19.75,-33.96456093117,-234.90005));
#193152=CARTESIAN_POINT('',(-20.2,-33.96456093117,-235.35005));
#193153=CARTESIAN_POINT('Origin',(-20.2,-33.96456093117,-234.90005));
#193154=CARTESIAN_POINT('',(-19.75,-42.0701004838368,-234.90005));
#193155=CARTESIAN_POINT('',(-20.2,-33.96456093117,-235.35005));
#193156=CARTESIAN_POINT('Origin',(296.501483394397,-32.7645609311699,-234.90005));
#193157=CARTESIAN_POINT('',(-19.,-32.76456093117,-235.35005));
#193158=CARTESIAN_POINT('',(-19.,-33.21456093117,-234.90005));
#193159=CARTESIAN_POINT('Origin',(-19.,-32.76456093117,-234.90005));
#193160=CARTESIAN_POINT('',(296.501483394397,-32.7645609311699,-235.35005));
#193161=CARTESIAN_POINT('',(0.,-33.21456093117,-234.90005));
#193162=CARTESIAN_POINT('Origin',(-19.,-33.96456093117,-234.90005));
#193163=CARTESIAN_POINT('Origin',(-19.,-33.96456093117,-235.35005));
#193164=CARTESIAN_POINT('Origin',(-19.,-33.96456093117,-234.90005));
#193165=CARTESIAN_POINT('Origin',(-8.87499999999984,-44.5701004838369,-234.90005));
#193166=CARTESIAN_POINT('',(-10.075,-44.5701004838369,-235.35005));
#193167=CARTESIAN_POINT('',(-9.62499999999984,-44.5701004838369,-234.90005));
#193168=CARTESIAN_POINT('Origin',(-10.075,-44.5701004838369,-234.90005));
#193169=CARTESIAN_POINT('',(-8.87499999999984,-43.3701004838369,-235.35005));
#193170=CARTESIAN_POINT('Origin',(-8.87499999999984,-44.5701004838369,-235.35005));
#193171=CARTESIAN_POINT('',(-8.87499999999984,-43.8201004838368,-234.90005));
#193172=CARTESIAN_POINT('Origin',(-8.87499999999984,-43.3701004838369,-234.90005));
#193173=CARTESIAN_POINT('Origin',(-8.87499999999984,-44.5701004838369,-234.90005));
#193174=CARTESIAN_POINT('Origin',(296.501483394397,-43.3701004838369,-234.90005));
#193175=CARTESIAN_POINT('',(-1.25,-43.8201004838368,-234.90005));
#193176=CARTESIAN_POINT('',(-1.25,-43.3701004838369,-235.35005));
#193177=CARTESIAN_POINT('Origin',(-1.25,-43.3701004838369,-234.90005));
#193178=CARTESIAN_POINT('',(1.23757166668304E-15,-43.8201004838368,-234.90005));
#193179=CARTESIAN_POINT('',(296.501483394397,-43.3701004838369,-235.35005));
#193180=CARTESIAN_POINT('Origin',(-10.075,-25.4138432731712,-234.90005));
#193181=CARTESIAN_POINT('',(-10.0749999999998,-53.1174378937751,-235.35005));
#193182=CARTESIAN_POINT('',(-9.62499999999984,-53.1174378937751,-234.90005));
#193183=CARTESIAN_POINT('Origin',(-10.0749999999998,-53.1174378937751,-234.90005));
#193184=CARTESIAN_POINT('',(-10.075,-44.5701004838369,-235.35005));
#193185=CARTESIAN_POINT('',(-9.62499999999984,-53.1174378937751,-234.90005));
#193186=CARTESIAN_POINT('Origin',(-1.25,-44.5701004838369,-234.90005));
#193187=CARTESIAN_POINT('',(-0.5,-44.5701004838369,-234.90005));
#193188=CARTESIAN_POINT('',(-0.0499999999999953,-44.5701004838369,-235.35005));
#193189=CARTESIAN_POINT('Origin',(-0.0499999999999955,-44.5701004838369,
-234.90005));
#193190=CARTESIAN_POINT('Origin',(-1.25,-44.5701004838369,-234.90005));
#193191=CARTESIAN_POINT('Origin',(-1.25,-44.5701004838369,-235.35005));
#193192=CARTESIAN_POINT('Origin',(-8.87499999999984,-53.1174378937751,-234.90005));
#193193=CARTESIAN_POINT('',(-8.89073849412256,-54.3173346809209,-235.35005));
#193194=CARTESIAN_POINT('',(-8.88483655882654,-53.8673733857413,-234.90005));
#193195=CARTESIAN_POINT('Origin',(-8.89073849412256,-54.3173346809209,-234.90005));
#193196=CARTESIAN_POINT('Origin',(-8.87499999999984,-53.1174378937751,-235.35005));
#193197=CARTESIAN_POINT('Origin',(-8.87499999999984,-53.1174378937751,-234.90005));
#193198=CARTESIAN_POINT('Origin',(-0.0499999999999945,-25.4138432731711,
-234.90005));
#193199=CARTESIAN_POINT('',(-0.5,-53.1744855098348,-234.90005));
#193200=CARTESIAN_POINT('',(-0.0499999999999928,-53.1744855098348,-235.35005));
#193201=CARTESIAN_POINT('Origin',(-0.049999999999995,-53.1744855098348,
-234.90005));
#193202=CARTESIAN_POINT('',(-0.5,-44.5701004838369,-234.90005));
#193203=CARTESIAN_POINT('',(-0.0499999999999928,-53.1744855098348,-235.35005));
#193204=CARTESIAN_POINT('Origin',(-7.14692237356698E-14,623.509175991979,
-234.90005));
#193205=CARTESIAN_POINT('',(-1.25221668931305,-54.3744834624533,-235.35005));
#193206=CARTESIAN_POINT('',(-1.25138543082066,-53.9244842302215,-234.90005));
#193207=CARTESIAN_POINT('Origin',(-1.25221668931305,-54.3744834624533,-234.90005));
#193208=CARTESIAN_POINT('Origin',(-7.14692237356698E-14,623.509175991979,
-235.35005));
#193209=CARTESIAN_POINT('Origin',(-7.14692237356698E-14,623.509175991979,
-234.90005));
#193210=CARTESIAN_POINT('Origin',(-1.25,-53.1744855098348,-234.90005));
#193211=CARTESIAN_POINT('Origin',(-1.25,-53.1744855098348,-235.35005));
#193212=CARTESIAN_POINT('Origin',(-1.25,-53.1744855098348,-234.90005));
#193213=CARTESIAN_POINT('Origin',(-1.25,-42.0701004838369,-234.90005));
#193214=CARTESIAN_POINT('',(-0.0499999999999935,-42.0701004838369,-235.35005));
#193215=CARTESIAN_POINT('',(-0.5,-42.0701004838369,-234.90005));
#193216=CARTESIAN_POINT('Origin',(-0.0499999999999935,-42.0701004838369,
-234.90005));
#193217=CARTESIAN_POINT('',(-1.25,-43.2701004838368,-235.35005));
#193218=CARTESIAN_POINT('Origin',(-1.25,-42.0701004838369,-235.35005));
#193219=CARTESIAN_POINT('',(-1.25,-42.8201004838369,-234.90005));
#193220=CARTESIAN_POINT('Origin',(-1.25,-43.2701004838368,-234.90005));
#193221=CARTESIAN_POINT('Origin',(-1.25,-42.0701004838369,-234.90005));
#193222=CARTESIAN_POINT('Origin',(296.501483394397,-43.270100483837,-234.90005));
#193223=CARTESIAN_POINT('',(-8.87499999999984,-42.8201004838369,-234.90005));
#193224=CARTESIAN_POINT('',(-8.87499999999984,-43.2701004838368,-235.35005));
#193225=CARTESIAN_POINT('Origin',(-8.87499999999984,-43.2701004838368,-234.90005));
#193226=CARTESIAN_POINT('',(1.54373336646987E-15,-42.8201004838369,-234.90005));
#193227=CARTESIAN_POINT('',(296.501483394397,-43.270100483837,-235.35005));
#193228=CARTESIAN_POINT('Origin',(-0.0499999999999945,-25.4138432731711,
-234.90005));
#193229=CARTESIAN_POINT('',(-0.0499999999999959,-33.96456093117,-235.35005));
#193230=CARTESIAN_POINT('',(-0.5,-33.96456093117,-234.90005));
#193231=CARTESIAN_POINT('Origin',(-0.0499999999999959,-33.96456093117,-234.90005));
#193232=CARTESIAN_POINT('',(-0.0499999999999935,-42.0701004838369,-235.35005));
#193233=CARTESIAN_POINT('',(-0.5,-33.96456093117,-234.90005));
#193234=CARTESIAN_POINT('Origin',(-8.87499999999984,-42.0701004838369,-234.90005));
#193235=CARTESIAN_POINT('',(-9.62499999999984,-42.0701004838368,-234.90005));
#193236=CARTESIAN_POINT('',(-10.0749999999998,-42.0701004838368,-235.35005));
#193237=CARTESIAN_POINT('Origin',(-10.0749999999998,-42.0701004838368,-234.90005));
#193238=CARTESIAN_POINT('Origin',(-8.87499999999984,-42.0701004838369,-234.90005));
#193239=CARTESIAN_POINT('Origin',(-8.87499999999984,-42.0701004838369,-235.35005));
#193240=CARTESIAN_POINT('Origin',(-1.25,-33.96456093117,-234.90005));
#193241=CARTESIAN_POINT('',(-1.25,-32.76456093117,-235.35005));
#193242=CARTESIAN_POINT('',(-1.25,-33.21456093117,-234.90005));
#193243=CARTESIAN_POINT('Origin',(-1.25,-32.76456093117,-234.90005));
#193244=CARTESIAN_POINT('Origin',(-1.25,-33.96456093117,-235.35005));
#193245=CARTESIAN_POINT('Origin',(-1.25,-33.96456093117,-234.90005));
#193246=CARTESIAN_POINT('Origin',(-10.075,-25.4138432731712,-234.90005));
#193247=CARTESIAN_POINT('',(-9.62499999999984,-33.96456093117,-234.90005));
#193248=CARTESIAN_POINT('',(-10.075,-33.96456093117,-235.35005));
#193249=CARTESIAN_POINT('Origin',(-10.0749999999998,-33.96456093117,-234.90005));
#193250=CARTESIAN_POINT('',(-9.62499999999984,-42.0701004838368,-234.90005));
#193251=CARTESIAN_POINT('',(-10.075,-33.96456093117,-235.35005));
#193252=CARTESIAN_POINT('Origin',(296.501483394397,-32.7645609311699,-234.90005));
#193253=CARTESIAN_POINT('',(-8.87499999999984,-32.76456093117,-235.35005));
#193254=CARTESIAN_POINT('',(-8.87499999999984,-33.21456093117,-234.90005));
#193255=CARTESIAN_POINT('Origin',(-8.87499999999984,-32.76456093117,-234.90005));
#193256=CARTESIAN_POINT('',(296.501483394397,-32.7645609311699,-235.35005));
#193257=CARTESIAN_POINT('',(0.,-33.21456093117,-234.90005));
#193258=CARTESIAN_POINT('Origin',(-8.87499999999984,-33.96456093117,-234.90005));
#193259=CARTESIAN_POINT('Origin',(-8.87499999999984,-33.96456093117,-235.35005));
#193260=CARTESIAN_POINT('Origin',(-8.87499999999984,-33.96456093117,-234.90005));
#193261=CARTESIAN_POINT('Origin',(-33.7514626427707,-44.5701004838368,-234.90005));
#193262=CARTESIAN_POINT('',(-34.6086426463967,-45.4098876243575,-235.35005));
#193263=CARTESIAN_POINT('',(-34.2872001450369,-45.0949674466622,-234.90005));
#193264=CARTESIAN_POINT('Origin',(-34.6086426463967,-45.4098876243575,-234.90005));
#193265=CARTESIAN_POINT('',(-33.7514626427707,-43.3701004838369,-235.35005));
#193266=CARTESIAN_POINT('Origin',(-33.7514626427707,-44.5701004838368,-235.35005));
#193267=CARTESIAN_POINT('',(-33.7514626427707,-43.8201004838368,-234.90005));
#193268=CARTESIAN_POINT('Origin',(-33.7514626427707,-43.3701004838369,-234.90005));
#193269=CARTESIAN_POINT('Origin',(-33.7514626427707,-44.5701004838368,-234.90005));
#193270=CARTESIAN_POINT('Origin',(296.501483394397,-43.3701004838369,-234.90005));
#193271=CARTESIAN_POINT('',(-31.625,-43.8201004838368,-234.90005));
#193272=CARTESIAN_POINT('',(-31.625,-43.3701004838369,-235.35005));
#193273=CARTESIAN_POINT('Origin',(-31.625,-43.3701004838369,-234.90005));
#193274=CARTESIAN_POINT('',(1.23757166668304E-15,-43.8201004838368,-234.90005));
#193275=CARTESIAN_POINT('',(296.501483394397,-43.3701004838369,-235.35005));
#193276=CARTESIAN_POINT('Origin',(6.29739814579425E-15,-11.5034818258363,
-234.90005));
#193277=CARTESIAN_POINT('',(-32.4281746031746,-47.5009260671432,-235.35005));
#193278=CARTESIAN_POINT('',(-32.1269841269841,-47.1665844797626,-234.90005));
#193279=CARTESIAN_POINT('Origin',(-32.4281746031746,-47.5009260671432,-234.90005));
#193280=CARTESIAN_POINT('Origin',(6.29739814579425E-15,-11.5034818258363,
-235.35005));
#193281=CARTESIAN_POINT('Origin',(6.29739814579425E-15,-11.5034818258363,
-234.90005));
#193282=CARTESIAN_POINT('Origin',(-31.625,-44.5701004838368,-234.90005));
#193283=CARTESIAN_POINT('',(-30.875,-44.5701004838368,-234.90005));
#193284=CARTESIAN_POINT('',(-30.425,-44.5701004838368,-235.35005));
#193285=CARTESIAN_POINT('Origin',(-30.425,-44.5701004838368,-234.90005));
#193286=CARTESIAN_POINT('Origin',(-31.625,-44.5701004838368,-234.90005));
#193287=CARTESIAN_POINT('Origin',(-31.625,-44.5701004838368,-235.35005));
#193288=CARTESIAN_POINT('Origin',(-31.625,-46.609348500795,-234.90005));
#193289=CARTESIAN_POINT('',(-30.425,-46.609348500795,-235.35005));
#193290=CARTESIAN_POINT('',(-30.875,-46.609348500795,-234.90005));
#193291=CARTESIAN_POINT('Origin',(-30.425,-46.609348500795,-234.90005));
#193292=CARTESIAN_POINT('Origin',(-31.625,-46.609348500795,-235.35005));
#193293=CARTESIAN_POINT('Origin',(-31.625,-46.609348500795,-234.90005));
#193294=CARTESIAN_POINT('Origin',(-30.425,-25.4138432731711,-234.90005));
#193295=CARTESIAN_POINT('',(-30.425,-46.609348500795,-235.35005));
#193296=CARTESIAN_POINT('',(-30.875,-44.5701004838368,-234.90005));
#193297=CARTESIAN_POINT('Origin',(-31.625,23.6023848491226,-234.90005));
#193298=CARTESIAN_POINT('',(-32.4281746031746,24.4939624154707,-235.35005));
#193299=CARTESIAN_POINT('',(-30.425,23.6023848491226,-235.35005));
#193300=CARTESIAN_POINT('Origin',(-31.625,23.6023848491226,-235.35005));
#193301=CARTESIAN_POINT('',(-30.875,23.6023848491226,-234.90005));
#193302=CARTESIAN_POINT('Origin',(-30.425,23.6023848491226,-234.90005));
#193303=CARTESIAN_POINT('',(-32.1269841269841,24.1596208280901,-234.90005));
#193304=CARTESIAN_POINT('Origin',(-31.625,23.6023848491226,-234.90005));
#193305=CARTESIAN_POINT('Origin',(-32.4281746031746,24.4939624154707,-234.90005));
#193306=CARTESIAN_POINT('Origin',(-30.425,-25.4138432731711,-234.90005));
#193307=CARTESIAN_POINT('',(-30.875,21.5631368321642,-234.90005));
#193308=CARTESIAN_POINT('',(-30.425,21.5631368321642,-235.35005));
#193309=CARTESIAN_POINT('Origin',(-30.425,21.5631368321642,-234.90005));
#193310=CARTESIAN_POINT('',(-30.875,23.6023848491225,-234.90005));
#193311=CARTESIAN_POINT('',(-30.425,21.5631368321642,-235.35005));
#193312=CARTESIAN_POINT('Origin',(6.29739814579425E-15,-11.5034818258363,
-234.90005));
#193313=CARTESIAN_POINT('',(-34.6086426463969,22.4029239726848,-235.35005));
#193314=CARTESIAN_POINT('',(-34.2872001450371,22.0880037949896,-234.90005));
#193315=CARTESIAN_POINT('Origin',(-34.6086426463969,22.4029239726848,-234.90005));
#193316=CARTESIAN_POINT('Origin',(6.29739814579425E-15,-11.5034818258363,
-235.35005));
#193317=CARTESIAN_POINT('Origin',(6.29739814579425E-15,-11.5034818258363,
-234.90005));
#193318=CARTESIAN_POINT('Origin',(-31.625,21.5631368321642,-234.90005));
#193319=CARTESIAN_POINT('',(-31.625,20.8131368321642,-234.90005));
#193320=CARTESIAN_POINT('',(-31.625,20.3631368321642,-235.35005));
#193321=CARTESIAN_POINT('Origin',(-31.625,20.3631368321642,-234.90005));
#193322=CARTESIAN_POINT('Origin',(-31.625,21.5631368321642,-234.90005));
#193323=CARTESIAN_POINT('Origin',(-31.625,21.5631368321642,-235.35005));
#193324=CARTESIAN_POINT('Origin',(-33.751462642771,21.5631368321642,-234.90005));
#193325=CARTESIAN_POINT('',(-33.751462642771,20.3631368321642,-235.35005));
#193326=CARTESIAN_POINT('',(-33.751462642771,20.8131368321642,-234.90005));
#193327=CARTESIAN_POINT('Origin',(-33.751462642771,20.3631368321642,-234.90005));
#193328=CARTESIAN_POINT('Origin',(-33.751462642771,21.5631368321642,-235.35005));
#193329=CARTESIAN_POINT('Origin',(-33.751462642771,21.5631368321642,-234.90005));
#193330=CARTESIAN_POINT('Origin',(296.501483394397,20.3631368321642,-234.90005));
#193331=CARTESIAN_POINT('',(296.501483394397,20.3631368321642,-235.35005));
#193332=CARTESIAN_POINT('',(1.23757166668304E-15,20.8131368321642,-234.90005));
#193333=CARTESIAN_POINT('Origin',(-22.9178089794592,-52.5372975341153,-234.90005));
#193334=CARTESIAN_POINT('',(-25.8434867215177,-57.775656986236,-234.90005));
#193335=CARTESIAN_POINT('',(-26.0629125521721,-58.168533945145,-235.35005));
#193336=CARTESIAN_POINT('Origin',(-26.0629125521721,-58.168533945145,-234.90005));
#193337=CARTESIAN_POINT('',(-23.121090730514,-58.5338529228103,-234.90005));
#193338=CARTESIAN_POINT('Origin',(-22.9178089794592,-52.5372975341153,-234.90005));
#193339=CARTESIAN_POINT('',(-23.1363368618431,-58.9835945769624,-235.35005));
#193340=CARTESIAN_POINT('Origin',(-23.1363368618431,-58.9835945769624,-234.90005));
#193341=CARTESIAN_POINT('Origin',(-22.9178089794592,-52.5372975341153,-235.35005));
#193342=CARTESIAN_POINT('Origin',(6.29739814579425E-15,-11.5034818258363,
-234.90005));
#193343=CARTESIAN_POINT('',(-43.9682643235187,-41.0972604351516,-234.90005));
#193344=CARTESIAN_POINT('',(-44.3415797753222,-41.3485283667401,-235.35005));
#193345=CARTESIAN_POINT('Origin',(-44.3415797753222,-41.3485283667401,-234.90005));
#193346=CARTESIAN_POINT('Origin',(6.29739814579425E-15,-11.5034818258363,
-234.90005));
#193347=CARTESIAN_POINT('Origin',(6.29739814579425E-15,-11.5034818258363,
-235.35005));
#193348=CARTESIAN_POINT('Origin',(-38.9907249661392,-37.7470213473046,-234.90005));
#193349=CARTESIAN_POINT('',(-44.9862076791357,-37.9798024422418,-234.90005));
#193350=CARTESIAN_POINT('',(-45.4358688826104,-37.9972610243621,-235.35005));
#193351=CARTESIAN_POINT('Origin',(-45.4358688826105,-37.9972610243621,-234.90005));
#193352=CARTESIAN_POINT('Origin',(-38.9907249661392,-37.7470213473046,-234.90005));
#193353=CARTESIAN_POINT('Origin',(-38.9907249661392,-37.7470213473046,-235.35005));
#193354=CARTESIAN_POINT('Origin',(636.934816028482,-11.5034818258361,-234.90005));
#193355=CARTESIAN_POINT('',(-44.9862076791357,14.9728387905693,-234.90005));
#193356=CARTESIAN_POINT('',(-45.4358688826104,14.9902973726896,-235.35005));
#193357=CARTESIAN_POINT('Origin',(-45.4358688826104,14.9902973726896,-234.90005));
#193358=CARTESIAN_POINT('Origin',(636.934816028482,-11.5034818258361,-234.90005));
#193359=CARTESIAN_POINT('Origin',(636.934816028482,-11.5034818258361,-235.35005));
#193360=CARTESIAN_POINT('Origin',(-38.9907249661392,14.740057695632,-234.90005));
#193361=CARTESIAN_POINT('',(-43.9682643235187,18.0902967834791,-234.90005));
#193362=CARTESIAN_POINT('',(-44.3415797753222,18.3415647150676,-235.35005));
#193363=CARTESIAN_POINT('Origin',(-44.3415797753222,18.3415647150676,-234.90005));
#193364=CARTESIAN_POINT('Origin',(-38.9907249661392,14.740057695632,-234.90005));
#193365=CARTESIAN_POINT('Origin',(-38.9907249661392,14.740057695632,-235.35005));
#193366=CARTESIAN_POINT('Origin',(6.29739814579425E-15,-11.5034818258363,
-234.90005));
#193367=CARTESIAN_POINT('',(-28.0091475455229,33.4908250781833,-234.90005));
#193368=CARTESIAN_POINT('',(-28.2469610624189,33.872852212274,-235.35005));
#193369=CARTESIAN_POINT('Origin',(-28.2469610624189,33.872852212274,-234.90005));
#193370=CARTESIAN_POINT('Origin',(6.29739814579425E-15,-11.5034818258363,
-234.90005));
#193371=CARTESIAN_POINT('Origin',(6.29739814579425E-15,-11.5034818258363,
-235.35005));
#193372=CARTESIAN_POINT('Origin',(-24.838300653577,28.3971299569735,-234.90005));
#193373=CARTESIAN_POINT('',(-25.5706493501227,34.3522676872588,-234.90005));
#193374=CARTESIAN_POINT('',(-25.6255755023637,34.7989030170302,-235.35005));
#193375=CARTESIAN_POINT('Origin',(-25.6255755023637,34.7989030170302,-234.90005));
#193376=CARTESIAN_POINT('Origin',(-24.838300653577,28.3971299569735,-234.90005));
#193377=CARTESIAN_POINT('Origin',(-24.838300653577,28.3971299569735,-235.35005));
#193378=CARTESIAN_POINT('Origin',(-22.9178089794592,-52.5372975341153,-234.90005));
#193379=CARTESIAN_POINT('',(-25.0389253424516,-56.3351081369028,-235.35005));
#193380=CARTESIAN_POINT('',(-25.258351173106,-56.7279850958119,-234.90005));
#193381=CARTESIAN_POINT('Origin',(-25.0389253424516,-56.3351081369028,-234.90005));
#193382=CARTESIAN_POINT('',(-23.0651882489741,-56.8848001909192,-235.35005));
#193383=CARTESIAN_POINT('Origin',(-22.9178089794592,-52.5372975341153,-235.35005));
#193384=CARTESIAN_POINT('',(-23.0804343803032,-57.3345418450714,-234.90005));
#193385=CARTESIAN_POINT('Origin',(-23.0651882489741,-56.8848001909192,-234.90005));
#193386=CARTESIAN_POINT('Origin',(-22.9178089794592,-52.5372975341153,-234.90005));
#193387=CARTESIAN_POINT('Origin',(6.29739814579425E-15,-11.5034818258363,
-234.90005));
#193388=CARTESIAN_POINT('',(-42.5994410002394,-40.1759446859937,-235.35005));
#193389=CARTESIAN_POINT('',(-42.9727564520428,-40.4272126175822,-234.90005));
#193390=CARTESIAN_POINT('Origin',(-42.5994410002394,-40.1759446859937,-234.90005));
#193391=CARTESIAN_POINT('Origin',(6.29739814579425E-15,-11.5034818258363,
-235.35005));
#193392=CARTESIAN_POINT('Origin',(6.29739814579425E-15,-11.5034818258363,
-234.90005));
#193393=CARTESIAN_POINT('Origin',(-38.9907249661392,-37.7470213473046,-234.90005));
#193394=CARTESIAN_POINT('',(-43.3374499330618,-37.915787641134,-235.35005));
#193395=CARTESIAN_POINT('',(-43.7871111365364,-37.9332462232544,-234.90005));
#193396=CARTESIAN_POINT('Origin',(-43.3374499330618,-37.915787641134,-234.90005));
#193397=CARTESIAN_POINT('Origin',(-38.9907249661392,-37.7470213473046,-235.35005));
#193398=CARTESIAN_POINT('Origin',(-38.9907249661392,-37.7470213473046,-234.90005));
#193399=CARTESIAN_POINT('Origin',(636.934816028482,-11.5034818258361,-234.90005));
#193400=CARTESIAN_POINT('',(-43.3374499330618,14.9088239894616,-235.35005));
#193401=CARTESIAN_POINT('',(-43.7871111365364,14.9262825715819,-234.90005));
#193402=CARTESIAN_POINT('Origin',(-43.3374499330618,14.9088239894616,-234.90005));
#193403=CARTESIAN_POINT('Origin',(636.934816028482,-11.5034818258361,-235.35005));
#193404=CARTESIAN_POINT('Origin',(636.934816028482,-11.5034818258361,-234.90005));
#193405=CARTESIAN_POINT('Origin',(-38.9907249661392,14.740057695632,-234.90005));
#193406=CARTESIAN_POINT('',(-42.5994410002394,17.1689810343211,-235.35005));
#193407=CARTESIAN_POINT('',(-42.9727564520429,17.4202489659097,-234.90005));
#193408=CARTESIAN_POINT('Origin',(-42.5994410002394,17.1689810343211,-234.90005));
#193409=CARTESIAN_POINT('Origin',(-38.9907249661392,14.740057695632,-235.35005));
#193410=CARTESIAN_POINT('Origin',(-38.9907249661392,14.740057695632,-234.90005));
#193411=CARTESIAN_POINT('Origin',(6.29739814579425E-15,-11.5034818258363,
-234.90005));
#193412=CARTESIAN_POINT('',(-27.1371646502378,32.0900589198506,-235.35005));
#193413=CARTESIAN_POINT('',(-27.3749781671338,32.4720860539414,-234.90005));
#193414=CARTESIAN_POINT('Origin',(-27.1371646502378,32.0900589198506,-234.90005));
#193415=CARTESIAN_POINT('Origin',(6.29739814579425E-15,-11.5034818258363,
-235.35005));
#193416=CARTESIAN_POINT('Origin',(6.29739814579425E-15,-11.5034818258363,
-234.90005));
#193417=CARTESIAN_POINT('Origin',(-24.838300653577,28.3971299569735,-234.90005));
#193418=CARTESIAN_POINT('',(-25.3692534585727,32.7146048114303,-235.35005));
#193419=CARTESIAN_POINT('',(-25.4241796108136,33.1612401412018,-234.90005));
#193420=CARTESIAN_POINT('Origin',(-25.3692534585727,32.7146048114303,-234.90005));
#193421=CARTESIAN_POINT('Origin',(-24.838300653577,28.3971299569735,-235.35005));
#193422=CARTESIAN_POINT('Origin',(-24.838300653577,28.3971299569735,-234.90005));
#193423=CARTESIAN_POINT('Origin',(-6.95148506756697,-6.01736880073005,-234.90005));
#193424=CARTESIAN_POINT('',(-6.08254860609655,-5.18975208634635,-235.35005));
#193425=CARTESIAN_POINT('',(-6.40839977914796,-5.50010835424024,-234.90005));
#193426=CARTESIAN_POINT('Origin',(-6.08254860609655,-5.18975208634635,-234.90005));
#193427=CARTESIAN_POINT('',(-5.76949205973895,-5.81026368383122,-235.35005));
#193428=CARTESIAN_POINT('Origin',(-6.95148506756697,-6.01736880073005,-235.35005));
#193429=CARTESIAN_POINT('',(-6.36274467860838,-6.48200280121742,-234.90005));
#193430=CARTESIAN_POINT('Ctrl Pts',(-5.76949205973896,-5.81026368383122,
-235.35005));
#193431=CARTESIAN_POINT('Ctrl Pts',(-5.82092507341363,-5.86238576252255,
-235.35005));
#193432=CARTESIAN_POINT('Ctrl Pts',(-5.87146206806168,-5.91503600112616,
-235.33821291833));
#193433=CARTESIAN_POINT('Ctrl Pts',(-6.00423457196878,-6.05699737629989,
-235.282379503985));
#193434=CARTESIAN_POINT('Ctrl Pts',(-6.07889780142458,-6.14101690884917,
-235.222495970419));
#193435=CARTESIAN_POINT('Ctrl Pts',(-6.22023885093967,-6.30512731290958,
-235.083822800187));
#193436=CARTESIAN_POINT('Ctrl Pts',(-6.29326617328538,-6.39403176703484,
-234.990808270705));
#193437=CARTESIAN_POINT('Ctrl Pts',(-6.36151501319033,-6.48044497931282,
-234.901656863128));
#193438=CARTESIAN_POINT('Ctrl Pts',(-6.36212991841606,-6.48122383507554,
-234.900853430267));
#193439=CARTESIAN_POINT('Ctrl Pts',(-6.36274467860838,-6.48200280121742,
-234.90005));
#193440=CARTESIAN_POINT('Origin',(-6.95148506756697,-6.01736880073005,-234.90005));
#193441=CARTESIAN_POINT('Origin',(147.944423723881,-166.906703884593,-234.90005));
#193442=CARTESIAN_POINT('',(-7.1259980697973,-4.09420716929315,-235.35005));
#193443=CARTESIAN_POINT('',(-7.45184924284871,-4.40456343718705,-234.90005));
#193444=CARTESIAN_POINT('Origin',(-7.1259980697973,-4.09420716929315,-234.90005));
#193445=CARTESIAN_POINT('',(147.944423723881,-166.906703884593,-235.35005));
#193446=CARTESIAN_POINT('',(-6.10697827817035,-5.81657868152891,-234.90005));
#193447=CARTESIAN_POINT('Origin',(-7.99493453126772,-4.92182388367686,-234.90005));
#193448=CARTESIAN_POINT('',(-8.92138760391815,-4.15914131263135,-235.35005));
#193449=CARTESIAN_POINT('Origin',(-7.99493453126772,-4.92182388367686,-235.35005));
#193450=CARTESIAN_POINT('',(-8.57396770167424,-4.44514727677342,-234.90005));
#193451=CARTESIAN_POINT('Origin',(-7.99493453126772,-4.92182388367686,-234.90005));
#193452=CARTESIAN_POINT('Origin',(-8.92138760391815,-4.15914131263135,-234.90005));
#193453=CARTESIAN_POINT('Origin',(0.,-11.5034818258363,-234.90005));
#193454=CARTESIAN_POINT('',(-11.4710456282303,-10.1086318165856,-235.35005));
#193455=CARTESIAN_POINT('',(-11.0243360211906,-10.1629505700546,-234.90005));
#193456=CARTESIAN_POINT('Origin',(-11.4710456282303,-10.1086318165856,-234.90005));
#193457=CARTESIAN_POINT('Origin',(0.,-11.5034818258363,-235.35005));
#193458=CARTESIAN_POINT('Origin',(0.,-11.5034818258363,-234.90005));
#193459=CARTESIAN_POINT('Origin',(-10.2798200094577,-10.2534818258363,-234.90005));
#193460=CARTESIAN_POINT('',(-10.2798200094577,-11.4534818258363,-235.35005));
#193461=CARTESIAN_POINT('',(-10.2798200094577,-11.0034818258363,-234.90005));
#193462=CARTESIAN_POINT('Origin',(-10.2798200094577,-11.4534818258363,-234.90005));
#193463=CARTESIAN_POINT('Origin',(-10.2798200094577,-10.2534818258363,-235.35005));
#193464=CARTESIAN_POINT('Origin',(-10.2798200094577,-10.2534818258363,-234.90005));
#193465=CARTESIAN_POINT('Origin',(296.501483394397,-11.4534818258365,-234.90005));
#193466=CARTESIAN_POINT('',(-8.76687405914145,-11.4534818258363,-235.35005));
#193467=CARTESIAN_POINT('',(-8.76687405914145,-11.0034818258363,-234.90005));
#193468=CARTESIAN_POINT('Origin',(-8.76687405914145,-11.4534818258363,-234.90005));
#193469=CARTESIAN_POINT('',(296.501483394397,-11.4534818258365,-235.35005));
#193470=CARTESIAN_POINT('',(2.22174260618994E-13,-11.0034818258363,-234.90005));
#193471=CARTESIAN_POINT('Origin',(-8.76687405914145,-10.2534818258363,-234.90005));
#193472=CARTESIAN_POINT('',(-8.02438338364376,-10.3593477636964,-234.90005));
#193473=CARTESIAN_POINT('',(-8.1016440740309,-11.2522155575736,-235.35005));
#193474=CARTESIAN_POINT('Ctrl Pts',(-8.02438338364377,-10.3593477636964,
-234.90005));
#193475=CARTESIAN_POINT('Ctrl Pts',(-8.02452345554005,-10.3603301578355,
-234.900853430281));
#193476=CARTESIAN_POINT('Ctrl Pts',(-8.02466334747473,-10.3613125808142,
-234.901656863113));
#193477=CARTESIAN_POINT('Ctrl Pts',(-8.04016643948374,-10.4703300185996,
-234.990808271414));
#193478=CARTESIAN_POINT('Ctrl Pts',(-8.05417784702261,-10.5845257804583,
-235.083822800183));
#193479=CARTESIAN_POINT('Ctrl Pts',(-8.07553226267947,-10.8000565344901,
-235.222495970419));
#193480=CARTESIAN_POINT('Ctrl Pts',(-8.08487817822972,-10.9120678443883,
-235.282379503985));
#193481=CARTESIAN_POINT('Ctrl Pts',(-8.09610373786709,-11.1061182415686,
-235.33821291833));
#193482=CARTESIAN_POINT('Ctrl Pts',(-8.09937411333572,-11.1790246205581,
-235.35005));
#193483=CARTESIAN_POINT('Ctrl Pts',(-8.10164407403091,-11.2522155575736,
-235.35005));
#193484=CARTESIAN_POINT('Origin',(-8.76687405914145,-10.2534818258363,-235.35005));
#193485=CARTESIAN_POINT('Origin',(-8.76687405914145,-10.2534818258363,-234.90005));
#193486=CARTESIAN_POINT('Origin',(-8.76687405914144,-12.7534818258363,-234.90005));
#193487=CARTESIAN_POINT('',(-8.76687405914144,-11.5534818258363,-235.35005));
#193488=CARTESIAN_POINT('',(-8.76687405914144,-12.0034818258363,-234.90005));
#193489=CARTESIAN_POINT('Origin',(-8.76687405914144,-11.5534818258363,-234.90005));
#193490=CARTESIAN_POINT('',(-8.1016440740309,-11.7547480940991,-235.35005));
#193491=CARTESIAN_POINT('Origin',(-8.76687405914144,-12.7534818258363,-235.35005));
#193492=CARTESIAN_POINT('',(-8.02438338364376,-12.6476158879763,-234.90005));
#193493=CARTESIAN_POINT('Ctrl Pts',(-8.10164407403091,-11.7547480940991,
-235.35005));
#193494=CARTESIAN_POINT('Ctrl Pts',(-8.09937411333571,-11.8279390311146,
-235.35005));
#193495=CARTESIAN_POINT('Ctrl Pts',(-8.09610373786709,-11.9008454101041,
-235.33821291833));
#193496=CARTESIAN_POINT('Ctrl Pts',(-8.08487817822972,-12.0948958072843,
-235.282379503985));
#193497=CARTESIAN_POINT('Ctrl Pts',(-8.07553226267949,-12.2069071171824,
-235.222495970419));
#193498=CARTESIAN_POINT('Ctrl Pts',(-8.05417784702484,-12.4224378711919,
-235.083822800197));
#193499=CARTESIAN_POINT('Ctrl Pts',(-8.04016643880974,-12.5366336378126,
-234.990808267567));
#193500=CARTESIAN_POINT('Ctrl Pts',(-8.02466334748842,-12.6456510707622,
-234.90165686319));
#193501=CARTESIAN_POINT('Ctrl Pts',(-8.0245234555264,-12.6466334939328,
-234.900853430203));
#193502=CARTESIAN_POINT('Ctrl Pts',(-8.02438338364376,-12.6476158879763,
-234.90005));
#193503=CARTESIAN_POINT('Origin',(-8.76687405914144,-12.7534818258363,-234.90005));
#193504=CARTESIAN_POINT('Origin',(296.501483394397,-11.5534818258362,-234.90005));
#193505=CARTESIAN_POINT('',(-10.2798200094577,-11.5534818258363,-235.35005));
#193506=CARTESIAN_POINT('',(-10.2798200094577,-12.0034818258363,-234.90005));
#193507=CARTESIAN_POINT('Origin',(-10.2798200094577,-11.5534818258363,-234.90005));
#193508=CARTESIAN_POINT('',(296.501483394397,-11.5534818258362,-235.35005));
#193509=CARTESIAN_POINT('',(2.22174260618994E-13,-12.0034818258363,-234.90005));
#193510=CARTESIAN_POINT('Origin',(-10.2798200094577,-12.7534818258363,-234.90005));
#193511=CARTESIAN_POINT('',(-11.4710456282303,-12.8983318350871,-235.35005));
#193512=CARTESIAN_POINT('',(-11.0243360211906,-12.844013081618,-234.90005));
#193513=CARTESIAN_POINT('Origin',(-11.4710456282303,-12.8983318350871,-234.90005));
#193514=CARTESIAN_POINT('Origin',(-10.2798200094577,-12.7534818258363,-235.35005));
#193515=CARTESIAN_POINT('Origin',(-10.2798200094577,-12.7534818258363,-234.90005));
#193516=CARTESIAN_POINT('Origin',(0.,-11.5034818258363,-234.90005));
#193517=CARTESIAN_POINT('',(-8.92138760391814,-18.8478223390413,-235.35005));
#193518=CARTESIAN_POINT('',(-8.57396770167423,-18.5618163748993,-234.90005));
#193519=CARTESIAN_POINT('Origin',(-8.92138760391814,-18.8478223390413,-234.90005));
#193520=CARTESIAN_POINT('Origin',(0.,-11.5034818258363,-235.35005));
#193521=CARTESIAN_POINT('Origin',(0.,-11.5034818258363,-234.90005));
#193522=CARTESIAN_POINT('Origin',(-7.99493453126771,-18.0851397679958,-234.90005));
#193523=CARTESIAN_POINT('',(-7.1259980697973,-18.9127564823795,-235.35005));
#193524=CARTESIAN_POINT('',(-7.4518492428487,-18.6024002144856,-234.90005));
#193525=CARTESIAN_POINT('Origin',(-7.12599806979729,-18.9127564823795,-234.90005));
#193526=CARTESIAN_POINT('Origin',(-7.99493453126771,-18.0851397679958,-235.35005));
#193527=CARTESIAN_POINT('Origin',(-7.99493453126771,-18.0851397679958,-234.90005));
#193528=CARTESIAN_POINT('Origin',(5.70871573332976,-5.43725435410305,-234.90005));
#193529=CARTESIAN_POINT('',(-6.08254860609655,-17.8172115653263,-235.35005));
#193530=CARTESIAN_POINT('',(-6.40839977914795,-17.5068552974324,-234.90005));
#193531=CARTESIAN_POINT('Origin',(-6.08254860609655,-17.8172115653263,-234.90005));
#193532=CARTESIAN_POINT('',(-7.1259980697973,-18.9127564823795,-235.35005));
#193533=CARTESIAN_POINT('',(-6.40839977914795,-17.5068552974324,-234.90005));
#193534=CARTESIAN_POINT('Origin',(-6.95148506756696,-16.9895948509426,-234.90005));
#193535=CARTESIAN_POINT('',(-6.36274467860837,-16.5249608504553,-234.90005));
#193536=CARTESIAN_POINT('',(-5.76949205973894,-17.1966999678414,-235.35005));
#193537=CARTESIAN_POINT('Ctrl Pts',(-6.36274467860837,-16.5249608504552,
-234.90005));
#193538=CARTESIAN_POINT('Ctrl Pts',(-6.36212991839128,-16.5257398166285,
-234.900853430299));
#193539=CARTESIAN_POINT('Ctrl Pts',(-6.36151501321541,-16.5265186723281,
-234.901656863095));
#193540=CARTESIAN_POINT('Ctrl Pts',(-6.2932661720145,-16.6129318862469,
-234.990808272351));
#193541=CARTESIAN_POINT('Ctrl Pts',(-6.22023885094759,-16.7018363387539,
-235.083822800179));
#193542=CARTESIAN_POINT('Ctrl Pts',(-6.07889780142461,-16.8659467428234,
-235.222495970419));
#193543=CARTESIAN_POINT('Ctrl Pts',(-6.0042345719688,-16.9499662753727,
-235.282379503985));
#193544=CARTESIAN_POINT('Ctrl Pts',(-5.87146206806167,-17.0919276505465,
-235.33821291833));
#193545=CARTESIAN_POINT('Ctrl Pts',(-5.82092507341363,-17.1445778891501,
-235.35005));
#193546=CARTESIAN_POINT('Ctrl Pts',(-5.76949205973896,-17.1966999678414,
-235.35005));
#193547=CARTESIAN_POINT('Origin',(-6.95148506756696,-16.9895948509426,-235.35005));
#193548=CARTESIAN_POINT('Origin',(-6.95148506756696,-16.9895948509426,-234.90005));
#193549=CARTESIAN_POINT('Origin',(-1.25,-2.73660776669487,-234.90005));
#193550=CARTESIAN_POINT('',(-0.0499999999999959,-2.73660776669487,-235.35005));
#193551=CARTESIAN_POINT('',(-0.5,-2.73660776669487,-234.90005));
#193552=CARTESIAN_POINT('Origin',(-0.0499999999999959,-2.73660776669487,
-234.90005));
#193553=CARTESIAN_POINT('',(-0.251266268262739,-3.40183775180542,-235.35005));
#193554=CARTESIAN_POINT('Origin',(-1.25,-2.73660776669487,-235.35005));
#193555=CARTESIAN_POINT('',(-1.14413406213993,-3.47909844219256,-234.90005));
#193556=CARTESIAN_POINT('Ctrl Pts',(-0.251266268262739,-3.40183775180541,
-235.35005));
#193557=CARTESIAN_POINT('Ctrl Pts',(-0.32445720527824,-3.4041077125006,
-235.35005));
#193558=CARTESIAN_POINT('Ctrl Pts',(-0.397363584267787,-3.40737808796923,
-235.33821291833));
#193559=CARTESIAN_POINT('Ctrl Pts',(-0.59141398144801,-3.4186036476066,
-235.282379503985));
#193560=CARTESIAN_POINT('Ctrl Pts',(-0.703425291346146,-3.42794956315684,
-235.222495970419));
#193561=CARTESIAN_POINT('Ctrl Pts',(-0.918956045360097,-3.44930397881193,
-235.083822800194));
#193562=CARTESIAN_POINT('Ctrl Pts',(-1.03315181083036,-3.46331538686362,
-234.990808268497));
#193563=CARTESIAN_POINT('Ctrl Pts',(-1.14216924494834,-3.4788184783511,
-234.901656863172));
#193564=CARTESIAN_POINT('Ctrl Pts',(-1.14315166807396,-3.47895837030671,
-234.900853430222));
#193565=CARTESIAN_POINT('Ctrl Pts',(-1.14413406213993,-3.47909844219256,
-234.90005));
#193566=CARTESIAN_POINT('Origin',(-1.25,-2.73660776669487,-234.90005));
#193567=CARTESIAN_POINT('Origin',(-0.0499999999999945,-25.4138432731711,
-234.90005));
#193568=CARTESIAN_POINT('',(-0.0499999999999981,-1.22366181637858,-235.35005));
#193569=CARTESIAN_POINT('',(-0.5,-1.22366181637858,-234.90005));
#193570=CARTESIAN_POINT('Origin',(-0.0499999999999981,-1.22366181637858,
-234.90005));
#193571=CARTESIAN_POINT('',(-0.0499999999999959,-2.73660776669487,-235.35005));
#193572=CARTESIAN_POINT('',(-0.5,-1.22366181637858,-234.90005));
#193573=CARTESIAN_POINT('Origin',(-1.25,-1.22366181637858,-234.90005));
#193574=CARTESIAN_POINT('',(-1.39485000925072,-0.0324361976060192,-235.35005));
#193575=CARTESIAN_POINT('Origin',(-1.25,-1.22366181637858,-235.35005));
#193576=CARTESIAN_POINT('',(-1.3405312557817,-0.479145804645727,-234.90005));
#193577=CARTESIAN_POINT('Origin',(-1.25,-1.22366181637858,-234.90005));
#193578=CARTESIAN_POINT('Origin',(-1.39485000925072,-0.0324361976060193,
-234.90005));
#193579=CARTESIAN_POINT('Origin',(0.,-11.5034818258363,-234.90005));
#193580=CARTESIAN_POINT('',(-6.90132755171766,-2.23513934310776,-235.35005));
#193581=CARTESIAN_POINT('',(-6.63257355852517,-2.59607048770891,-234.90005));
#193582=CARTESIAN_POINT('Origin',(-6.90132755171766,-2.23513934310776,-234.90005));
#193583=CARTESIAN_POINT('Origin',(0.,-11.5034818258363,-235.35005));
#193584=CARTESIAN_POINT('Origin',(0.,-11.5034818258363,-234.90005));
#193585=CARTESIAN_POINT('Origin',(-6.18465023653769,-3.19762239537748,-234.90005));
#193586=CARTESIAN_POINT('',(-7.05358669800811,-4.02523910976119,-235.35005));
#193587=CARTESIAN_POINT('',(-6.7277355249567,-3.7148828418673,-234.90005));
#193588=CARTESIAN_POINT('Origin',(-7.05358669800812,-4.0252391097612,-234.90005));
#193589=CARTESIAN_POINT('Origin',(-6.18465023653769,-3.19762239537748,-235.35005));
#193590=CARTESIAN_POINT('Origin',(-6.18465023653769,-3.19762239537748,-234.90005));
#193591=CARTESIAN_POINT('Origin',(148.016835095671,-166.837735825062,-234.90005));
#193592=CARTESIAN_POINT('',(-6.01013723430737,-5.12078402681439,-235.35005));
#193593=CARTESIAN_POINT('',(-5.68428606125595,-4.81042775892049,-234.90005));
#193594=CARTESIAN_POINT('Origin',(-6.01013723430736,-5.12078402681438,-234.90005));
#193595=CARTESIAN_POINT('',(148.016835095671,-166.837735825062,-235.35005));
#193596=CARTESIAN_POINT('',(-5.38286456027834,-5.12689808620916,-234.90005));
#193597=CARTESIAN_POINT('Origin',(-5.14120077283694,-4.29316731243068,-234.90005));
#193598=CARTESIAN_POINT('',(-4.70577833960231,-4.90382867901287,-234.90005));
#193599=CARTESIAN_POINT('',(-5.40560135635379,-5.46367674487279,-235.35005));
#193600=CARTESIAN_POINT('Ctrl Pts',(-4.70577833960231,-4.90382867901288,
-234.90005));
#193601=CARTESIAN_POINT('Ctrl Pts',(-4.70658630946365,-4.90440478914896,
-234.900853430202));
#193602=CARTESIAN_POINT('Ctrl Pts',(-4.7073941763327,-4.9049810496594,-234.901656863192));
#193603=CARTESIAN_POINT('Ctrl Pts',(-4.7970273762009,-4.96894225656959,
-234.990808267499));
#193604=CARTESIAN_POINT('Ctrl Pts',(-4.88938149376754,-5.03755500803177,
-235.083822800199));
#193605=CARTESIAN_POINT('Ctrl Pts',(-5.06017799547275,-5.17073936145204,
-235.222495970419));
#193606=CARTESIAN_POINT('Ctrl Pts',(-5.14773261812954,-5.24122388268893,
-235.282379503985));
#193607=CARTESIAN_POINT('Ctrl Pts',(-5.29598922334359,-5.36692809441377,
-235.33821291833));
#193608=CARTESIAN_POINT('Ctrl Pts',(-5.35103724699188,-5.41484208553839,
-235.35005));
#193609=CARTESIAN_POINT('Ctrl Pts',(-5.40560135635379,-5.46367674487279,
-235.35005));
#193610=CARTESIAN_POINT('Origin',(-5.14120077283694,-4.29316731243068,-235.35005));
#193611=CARTESIAN_POINT('Origin',(-5.14120077283694,-4.29316731243068,-234.90005));
#193612=CARTESIAN_POINT('Origin',(-5.14120077283693,-18.713796339242,-234.90005));
#193613=CARTESIAN_POINT('',(-5.40560135635378,-17.5432869067998,-235.35005));
#193614=CARTESIAN_POINT('',(-4.7057783396023,-18.1031349726598,-234.90005));
#193615=CARTESIAN_POINT('Ctrl Pts',(-4.7057783396023,-18.1031349726598,
-234.90005));
#193616=CARTESIAN_POINT('Ctrl Pts',(-4.70658630927984,-18.1025588626547,
-234.900853430019));
#193617=CARTESIAN_POINT('Ctrl Pts',(-4.70739417651803,-18.101982601881,
-234.901656863374));
#193618=CARTESIAN_POINT('Ctrl Pts',(-4.79702736710127,-18.0380214015964,
-234.990808258517));
#193619=CARTESIAN_POINT('Ctrl Pts',(-4.88938149380989,-17.9694086436079,
-235.083822800233));
#193620=CARTESIAN_POINT('Ctrl Pts',(-5.06017799547342,-17.8362242902201,
-235.222495970419));
#193621=CARTESIAN_POINT('Ctrl Pts',(-5.14773261813007,-17.7657397689833,
-235.282379503985));
#193622=CARTESIAN_POINT('Ctrl Pts',(-5.29598922334368,-17.6400355572588,
-235.33821291833));
#193623=CARTESIAN_POINT('Ctrl Pts',(-5.35103724699192,-17.5921215661342,
-235.35005));
#193624=CARTESIAN_POINT('Ctrl Pts',(-5.40560135635379,-17.5432869067999,
-235.35005));
#193625=CARTESIAN_POINT('',(-5.68428606125594,-18.1965358927522,-234.90005));
#193626=CARTESIAN_POINT('Origin',(-5.14120077283693,-18.713796339242,-234.90005));
#193627=CARTESIAN_POINT('',(-6.01013723430735,-17.8861796248583,-235.35005));
#193628=CARTESIAN_POINT('Origin',(-6.01013723430735,-17.8861796248583,-234.90005));
#193629=CARTESIAN_POINT('Origin',(-5.14120077283693,-18.713796339242,-235.35005));
#193630=CARTESIAN_POINT('Origin',(5.78112710511895,-5.50622241363502,-234.90005));
#193631=CARTESIAN_POINT('',(-7.0535866980081,-18.9817245419115,-235.35005));
#193632=CARTESIAN_POINT('',(-6.72773552495669,-19.2920808098054,-234.90005));
#193633=CARTESIAN_POINT('Origin',(-7.0535866980081,-18.9817245419115,-234.90005));
#193634=CARTESIAN_POINT('',(-6.01013723430735,-17.8861796248583,-235.35005));
#193635=CARTESIAN_POINT('',(-6.7277355249567,-19.2920808098054,-234.90005));
#193636=CARTESIAN_POINT('Origin',(-6.18465023653768,-19.8093412562951,-234.90005));
#193637=CARTESIAN_POINT('',(-6.90132755171765,-20.7718243085649,-235.35005));
#193638=CARTESIAN_POINT('',(-6.63257355852516,-20.4108931639637,-234.90005));
#193639=CARTESIAN_POINT('Origin',(-6.90132755171765,-20.7718243085649,-234.90005));
#193640=CARTESIAN_POINT('Origin',(-6.18465023653768,-19.8093412562951,-235.35005));
#193641=CARTESIAN_POINT('Origin',(-6.18465023653768,-19.8093412562951,-234.90005));
#193642=CARTESIAN_POINT('Origin',(0.,-11.5034818258363,-234.90005));
#193643=CARTESIAN_POINT('',(-1.39485000925072,-22.9745274540666,-235.35005));
#193644=CARTESIAN_POINT('',(-1.3405312557817,-22.5278178470269,-234.90005));
#193645=CARTESIAN_POINT('Origin',(-1.39485000925072,-22.9745274540666,-234.90005));
#193646=CARTESIAN_POINT('Origin',(0.,-11.5034818258363,-235.35005));
#193647=CARTESIAN_POINT('Origin',(0.,-11.5034818258363,-234.90005));
#193648=CARTESIAN_POINT('Origin',(-1.25,-21.7833018352941,-234.90005));
#193649=CARTESIAN_POINT('',(-0.0499999999999969,-21.7833018352941,-235.35005));
#193650=CARTESIAN_POINT('',(-0.5,-21.7833018352941,-234.90005));
#193651=CARTESIAN_POINT('Origin',(-0.0499999999999947,-21.7833018352941,
-234.90005));
#193652=CARTESIAN_POINT('Origin',(-1.25,-21.7833018352941,-235.35005));
#193653=CARTESIAN_POINT('Origin',(-1.25,-21.7833018352941,-234.90005));
#193654=CARTESIAN_POINT('Origin',(-0.0499999999999945,-25.4138432731711,
-234.90005));
#193655=CARTESIAN_POINT('',(-0.0499999999999948,-20.2703558849778,-235.35005));
#193656=CARTESIAN_POINT('',(-0.5,-20.2703558849778,-234.90005));
#193657=CARTESIAN_POINT('Origin',(-0.049999999999997,-20.2703558849778,
-234.90005));
#193658=CARTESIAN_POINT('',(-0.0499999999999947,-21.7833018352941,-235.35005));
#193659=CARTESIAN_POINT('',(-0.5,-20.2703558849778,-234.90005));
#193660=CARTESIAN_POINT('Origin',(-1.25,-20.2703558849778,-234.90005));
#193661=CARTESIAN_POINT('',(-1.14413406213993,-19.5278652094801,-234.90005));
#193662=CARTESIAN_POINT('',(-0.251266268262739,-19.6051258998672,-235.35005));
#193663=CARTESIAN_POINT('Ctrl Pts',(-1.14413406213993,-19.5278652094801,
-234.90005));
#193664=CARTESIAN_POINT('Ctrl Pts',(-1.1431516683171,-19.5280052813313,
-234.900853430023));
#193665=CARTESIAN_POINT('Ctrl Pts',(-1.14216924470318,-19.5281451733564,
-234.90165686337));
#193666=CARTESIAN_POINT('Ctrl Pts',(-1.03315182292617,-19.5436482630889,
-234.990808258681));
#193667=CARTESIAN_POINT('Ctrl Pts',(-0.918956045301575,-19.5576596728665,
-235.083822800232));
#193668=CARTESIAN_POINT('Ctrl Pts',(-0.703425291345268,-19.5790140885159,
-235.222495970419));
#193669=CARTESIAN_POINT('Ctrl Pts',(-0.591413981447289,-19.5883600040661,
-235.282379503985));
#193670=CARTESIAN_POINT('Ctrl Pts',(-0.397363584267675,-19.5995855637034,
-235.33821291833));
#193671=CARTESIAN_POINT('Ctrl Pts',(-0.324457205278181,-19.602855939172,
-235.35005));
#193672=CARTESIAN_POINT('Ctrl Pts',(-0.25126626826274,-19.6051258998672,
-235.35005));
#193673=CARTESIAN_POINT('Origin',(-1.25,-20.2703558849778,-235.35005));
#193674=CARTESIAN_POINT('Origin',(-1.25,-20.2703558849778,-234.90005));
#193675=CARTESIAN_POINT('Origin',(-41.3132181298675,38.0528376956935,-203.84995));
#193676=CARTESIAN_POINT('',(-50.148669624411,48.964302343774,-203.876128609656));
#193677=CARTESIAN_POINT('',(-49.2048636720257,47.7987359558583,-205.34995));
#193678=CARTESIAN_POINT('Origin',(-49.2048636720257,47.7987359558583,-203.84995));
#193679=CARTESIAN_POINT('',(-43.9433571680673,51.844416014308,-203.876128609656));
#193680=CARTESIAN_POINT('Origin',(-41.3132181298675,38.0528376956935,-203.876128609656));
#193681=CARTESIAN_POINT('',(-43.6624048158998,50.3711948984507,-205.34995));
#193682=CARTESIAN_POINT('Origin',(-43.6624048158998,50.3711948984507,-203.84995));
#193683=CARTESIAN_POINT('Origin',(-41.3132181298675,38.0528376956935,-205.34995));
#193684=CARTESIAN_POINT('Origin',(0.,-12.9675000200281,-203.84995));
#193685=CARTESIAN_POINT('',(-61.5592179767879,37.6378345921813,-203.876128609656));
#193686=CARTESIAN_POINT('',(-60.4006636863987,36.6854341319664,-205.34995));
#193687=CARTESIAN_POINT('Origin',(-60.4006636863987,36.6854341319665,-203.84995));
#193688=CARTESIAN_POINT('Origin',(0.,-12.9675000200281,-203.876128609656));
#193689=CARTESIAN_POINT('Origin',(0.,-12.9675000200281,-205.34995));
#193690=CARTESIAN_POINT('Origin',(-50.7133971693864,28.7219255026674,-203.84995));
#193691=CARTESIAN_POINT('',(-64.7425725698088,29.2764536470619,-203.876128609656));
#193692=CARTESIAN_POINT('',(-63.2439712523603,29.2172187609027,-205.34995));
#193693=CARTESIAN_POINT('Origin',(-63.2439712523603,29.2172187609027,-203.84995));
#193694=CARTESIAN_POINT('Origin',(-50.7133971693864,28.7219255026673,-203.876128609656));
#193695=CARTESIAN_POINT('Origin',(-50.7133971693864,28.7219255026674,-205.34995));
#193696=CARTESIAN_POINT('Origin',(1004.,-12.967500020028,-203.84995));
#193697=CARTESIAN_POINT('',(-64.7425725698087,-55.2114536871185,-203.876128609656));
#193698=CARTESIAN_POINT('',(-63.2439712523603,-55.1522188009592,-205.34995));
#193699=CARTESIAN_POINT('Origin',(-63.2439712523603,-55.1522188009592,-203.84995));
#193700=CARTESIAN_POINT('Origin',(1004.,-12.967500020028,-203.87612860965));
#193701=CARTESIAN_POINT('Origin',(1004.,-12.967500020028,-205.34995));
#193702=CARTESIAN_POINT('Origin',(-50.7133971693864,-54.6569255427236,-203.84995));
#193703=CARTESIAN_POINT('',(-61.5592179767879,-63.5728346322375,-203.876128609656));
#193704=CARTESIAN_POINT('',(-60.4006636863987,-62.6204341720228,-205.34995));
#193705=CARTESIAN_POINT('Origin',(-60.4006636863987,-62.6204341720228,-203.84995));
#193706=CARTESIAN_POINT('Origin',(-50.7133971693864,-54.6569255427236,-203.876128609656));
#193707=CARTESIAN_POINT('Origin',(-50.7133971693864,-54.6569255427236,-205.34995));
#193708=CARTESIAN_POINT('Origin',(0.,-12.9675000200281,-203.84995));
#193709=CARTESIAN_POINT('',(-50.4303082679829,-74.6701840550325,-203.876128609656));
#193710=CARTESIAN_POINT('',(-49.481201831453,-73.5089297105696,-205.34995));
#193711=CARTESIAN_POINT('Origin',(-49.481201831453,-73.5089297105696,-203.84995));
#193712=CARTESIAN_POINT('Origin',(0.,-12.9675000200281,-203.876128609656));
#193713=CARTESIAN_POINT('Origin',(0.,-12.9675000200281,-205.34995));
#193714=CARTESIAN_POINT('Origin',(-41.5452362233251,-63.7990866568863,-203.84995));
#193715=CARTESIAN_POINT('',(-42.0978464467214,-77.8283377352489,-203.876128609656));
#193716=CARTESIAN_POINT('',(-42.0388164335396,-76.329728333857,-205.34995));
#193717=CARTESIAN_POINT('Origin',(-42.0388164335396,-76.329728333857,-203.84995));
#193718=CARTESIAN_POINT('Origin',(-41.5452362233251,-63.7990866568863,-203.876128609656));
#193719=CARTESIAN_POINT('Origin',(-41.5452362233251,-63.7990866568863,-205.34995));
#193720=CARTESIAN_POINT('Ctrl Pts',(-23.3965212694791,39.0700122934506,
-234.574197273323));
#193721=CARTESIAN_POINT('Ctrl Pts',(-23.441207715325,38.6446575693707,-235.35005));
#193722=CARTESIAN_POINT('Ctrl Pts',(-23.5337713018193,37.7635770079652,
-235.35005));
#193723=CARTESIAN_POINT('Ctrl Pts',(-21.5285729617573,38.8429287236754,
-234.629840683519));
#193724=CARTESIAN_POINT('Ctrl Pts',(-21.5595177806197,38.4044126698907,
-235.350049999891));
#193725=CARTESIAN_POINT('Ctrl Pts',(-21.5449677583916,37.5546394871488,
-235.35005));
#193726=CARTESIAN_POINT('Ctrl Pts',(-19.6686582940338,38.873624481404,-234.667826224195));
#193727=CARTESIAN_POINT('Ctrl Pts',(-19.6461032038161,38.4273266114594,
-235.350050000221));
#193728=CARTESIAN_POINT('Ctrl Pts',(-19.5728087819113,37.6143598891179,
-235.35005));
#193729=CARTESIAN_POINT('Ctrl Pts',(-17.3605227404968,39.2364170937257,
-234.700260615516));
#193730=CARTESIAN_POINT('Ctrl Pts',(-17.2775810752257,38.7970065033925,
-235.350049999945));
#193731=CARTESIAN_POINT('Ctrl Pts',(-17.1293181159922,38.0221098574478,
-235.35005));
#193732=CARTESIAN_POINT('Ctrl Pts',(-16.8996944960412,39.3254277923721,
-234.705962605482));
#193733=CARTESIAN_POINT('Ctrl Pts',(-16.8064955068198,38.8875662731569,
-235.350049999917));
#193734=CARTESIAN_POINT('Ctrl Pts',(-16.6417036623955,38.1205664042693,
-235.35005));
#193735=CARTESIAN_POINT('Ctrl Pts',(-16.4255331955625,39.4347061351644,
-234.711087809772));
#193736=CARTESIAN_POINT('Ctrl Pts',(-16.3214053907335,38.9990490260666,
-235.350050000003));
#193737=CARTESIAN_POINT('Ctrl Pts',(-16.1400046132382,38.2400981928593,
-235.35005));
#193738=CARTESIAN_POINT('Ctrl Pts',(-16.4084238303339,39.4389694488068,
-234.710829083432));
#193739=CARTESIAN_POINT('Ctrl Pts',(-16.3050101388373,39.0031621878097,
-235.35005));
#193740=CARTESIAN_POINT('Ctrl Pts',(-16.1248016481815,38.2437210060648,
-235.35005));
#193741=CARTESIAN_POINT('Ctrl Pts',(-16.3761129052093,39.4467740117303,
-234.710599688867));
#193742=CARTESIAN_POINT('Ctrl Pts',(-16.2734102840084,39.0108163690221,
-235.35005));
#193743=CARTESIAN_POINT('Ctrl Pts',(-16.0943932022442,38.2509106188218,
-235.35005));
#193744=CARTESIAN_POINT('Ctrl Pts',(-16.3599561657618,39.450655986529,-234.710484721543));
#193745=CARTESIAN_POINT('Ctrl Pts',(-16.2576091615606,39.0146236300189,
-235.35005));
#193746=CARTESIAN_POINT('Ctrl Pts',(-16.0791881138821,38.2544860972426,
-235.35005));
#193747=CARTESIAN_POINT('Ctrl Pts',(-16.3114821481724,39.4622410332486,
-234.710139015331));
#193748=CARTESIAN_POINT('Ctrl Pts',(-16.2102010812718,39.0259862502062,
-235.35005));
#193749=CARTESIAN_POINT('Ctrl Pts',(-16.033570255147,38.2651546046657,-235.35005));
#193750=CARTESIAN_POINT('Ctrl Pts',(-16.2791610701706,39.469883227432,-234.709907472259));
#193751=CARTESIAN_POINT('Ctrl Pts',(-16.1785917022065,39.0334818852873,
-235.350050000003));
#193752=CARTESIAN_POINT('Ctrl Pts',(-16.0031548911028,38.2721897057073,
-235.35005));
#193753=CARTESIAN_POINT('Ctrl Pts',(-16.1821828897582,39.4925666443581,
-234.709209671843));
#193754=CARTESIAN_POINT('Ctrl Pts',(-16.0837448349166,39.0557325021636,
-235.350049999995));
#193755=CARTESIAN_POINT('Ctrl Pts',(-15.9118984444987,38.293063747877,-235.35005));
#193756=CARTESIAN_POINT('Ctrl Pts',(-16.1175108380135,39.5073646989989,
-234.708740244041));
#193757=CARTESIAN_POINT('Ctrl Pts',(-16.0204977871684,39.0702489458226,
-235.350049999996));
#193758=CARTESIAN_POINT('Ctrl Pts',(-15.8510470074106,38.3066714267388,
-235.35005));
#193759=CARTESIAN_POINT('Ctrl Pts',(-15.923436929361,39.5507890631334,-234.707319617973));
#193760=CARTESIAN_POINT('Ctrl Pts',(-15.8306827227777,39.1128561089809,
-235.350050000009));
#193761=CARTESIAN_POINT('Ctrl Pts',(-15.6684514414679,38.3465730642683,
-235.35005));
#193762=CARTESIAN_POINT('Ctrl Pts',(-15.7939773013225,39.5784455268499,
-234.706356088967));
#193763=CARTESIAN_POINT('Ctrl Pts',(-15.7040775100839,39.1399955931374,
-235.350050000029));
#193764=CARTESIAN_POINT('Ctrl Pts',(-15.5466660570668,38.3719456051061,
-235.35005));
#193765=CARTESIAN_POINT('Ctrl Pts',(-15.4053840336983,39.6575602691303,
-234.703418469392));
#193766=CARTESIAN_POINT('Ctrl Pts',(-15.3239745423948,39.2176705993572,
-235.350049999942));
#193767=CARTESIAN_POINT('Ctrl Pts',(-15.1811462198576,38.4444074430163,
-235.35005));
#193768=CARTESIAN_POINT('Ctrl Pts',(-15.1460359232891,39.7051631376525,
-234.701397554764));
#193769=CARTESIAN_POINT('Ctrl Pts',(-15.0703368511065,39.2644253992522,
-235.350050000007));
#193770=CARTESIAN_POINT('Ctrl Pts',(-14.9372480705784,38.4878406764273,
-235.35005));
#193771=CARTESIAN_POINT('Ctrl Pts',(-13.8480945051425,39.9178513634478,
-234.690999263195));
#193772=CARTESIAN_POINT('Ctrl Pts',(-13.7992252388259,39.4738011152816,
-235.350049999972));
#193773=CARTESIAN_POINT('Ctrl Pts',(-13.7166846430007,38.681049143284,-235.35005));
#193774=CARTESIAN_POINT('Ctrl Pts',(-12.8051801439163,40.0076434448158,
-234.681621861006));
#193775=CARTESIAN_POINT('Ctrl Pts',(-12.7786604443217,39.5624349839993,
-235.350049999918));
#193776=CARTESIAN_POINT('Ctrl Pts',(-12.7368211885109,38.7593950182271,
-235.35005));
#193777=CARTESIAN_POINT('Ctrl Pts',(-11.2337410805306,40.0229720626152,
-234.665772580439));
#193778=CARTESIAN_POINT('Ctrl Pts',(-11.2431493991504,39.5795098549774,
-235.350050000041));
#193779=CARTESIAN_POINT('Ctrl Pts',(-11.2619727865364,38.7640531506757,
-235.35005));
#193780=CARTESIAN_POINT('Ctrl Pts',(-10.7088507580156,40.0081380134295,
-234.660205544568));
#193781=CARTESIAN_POINT('Ctrl Pts',(-10.7295202598973,39.5657289156652,
-235.350049999972));
#193782=CARTESIAN_POINT('Ctrl Pts',(-10.769512598989,38.7467544284794,-235.35005));
#193783=CARTESIAN_POINT('Ctrl Pts',(-9.91948648717853,39.955281844485,-234.651341964047));
#193784=CARTESIAN_POINT('Ctrl Pts',(-9.95765099397115,39.5153737946489,
-235.350050000014));
#193785=CARTESIAN_POINT('Ctrl Pts',(-10.0295286270685,38.6919125336202,
-235.35005));
#193786=CARTESIAN_POINT('Ctrl Pts',(-9.65606191081629,39.9325482704366,
-234.648309008783));
#193787=CARTESIAN_POINT('Ctrl Pts',(-9.69987071016349,39.4935906245988,
-235.350050000035));
#193788=CARTESIAN_POINT('Ctrl Pts',(-9.78265126312491,38.6688067780134,
-235.35005));
#193789=CARTESIAN_POINT('Ctrl Pts',(-9.37589591312305,39.9028851219532,
-234.645007706899));
#193790=CARTESIAN_POINT('Ctrl Pts',(-9.42585059617205,39.4651058329293,
-235.350049999998));
#193791=CARTESIAN_POINT('Ctrl Pts',(-9.52011153215911,38.6390634524768,
-235.35005));
#193792=CARTESIAN_POINT('Ctrl Pts',(-9.36305882799351,39.9011137141232,
-234.645527469892));
#193793=CARTESIAN_POINT('Ctrl Pts',(-9.41213306277311,39.4631587775859,
-235.350050000001));
#193794=CARTESIAN_POINT('Ctrl Pts',(-9.5046684958238,38.6373245043133,-235.35005));
#193795=CARTESIAN_POINT('Ctrl Pts',(-9.33400183059134,39.8976433794956,
-234.645901386584));
#193796=CARTESIAN_POINT('Ctrl Pts',(-9.38245770550587,39.4595650288394,
-235.350049999999));
#193797=CARTESIAN_POINT('Ctrl Pts',(-9.47378419368037,38.6338861514567,
-235.35005));
#193798=CARTESIAN_POINT('Ctrl Pts',(-9.31947356561741,39.8959244662302,
-234.646087475637));
#193799=CARTESIAN_POINT('Ctrl Pts',(-9.36762025207224,39.4577849263438,
-235.350049999996));
#193800=CARTESIAN_POINT('Ctrl Pts',(-9.4583427946727,38.6321837720633,-235.35005));
#193801=CARTESIAN_POINT('Ctrl Pts',(-9.27588952240145,39.8908164251014,
-234.64664315687));
#193802=CARTESIAN_POINT('Ctrl Pts',(-9.32311043679367,39.4524950861104,
-235.350050000007));
#193803=CARTESIAN_POINT('Ctrl Pts',(-9.41202085079896,38.6271269561732,
-235.35005));
#193804=CARTESIAN_POINT('Ctrl Pts',(-9.24683449671838,39.8874759952947,
-234.647010163276));
#193805=CARTESIAN_POINT('Ctrl Pts',(-9.29343696234345,39.4490353641227,
-235.350050000002));
#193806=CARTESIAN_POINT('Ctrl Pts',(-9.38114255901401,38.6238228412382,
-235.35005));
#193807=CARTESIAN_POINT('Ctrl Pts',(-9.15967282997768,39.8776490180443,
-234.64810100638));
#193808=CARTESIAN_POINT('Ctrl Pts',(-9.20442696746952,39.438857479744,-235.350049999996));
#193809=CARTESIAN_POINT('Ctrl Pts',(-9.28851667274619,38.6141112622619,
-235.35005));
#193810=CARTESIAN_POINT('Ctrl Pts',(-9.10156960385291,39.8713567716217,
-234.648814670252));
#193811=CARTESIAN_POINT('Ctrl Pts',(-9.14508625993128,39.4323387903818,
-235.35005));
#193812=CARTESIAN_POINT('Ctrl Pts',(-9.22677806679909,38.6079045517242,
-235.35005));
#193813=CARTESIAN_POINT('Ctrl Pts',(-8.92727674161121,39.853253826224,-234.650916177606));
#193814=CARTESIAN_POINT('Ctrl Pts',(-8.9671077921105,39.4135836156387,-235.350049999998));
#193815=CARTESIAN_POINT('Ctrl Pts',(-9.04159803735041,38.5900837326631,
-235.35005));
#193816=CARTESIAN_POINT('Ctrl Pts',(-8.81110395292333,39.8422167453627,
-234.652264586384));
#193817=CARTESIAN_POINT('Ctrl Pts',(-8.84845540125615,39.4021407470111,
-235.350049999988));
#193818=CARTESIAN_POINT('Ctrl Pts',(-8.91819239372934,38.5792687468256,
-235.35005));
#193819=CARTESIAN_POINT('Ctrl Pts',(-7.76582421746211,39.7521044618495,
-234.66395028747));
#193820=CARTESIAN_POINT('Ctrl Pts',(-7.78295296745438,39.3088433368614,
-235.350050000096));
#193821=CARTESIAN_POINT('Ctrl Pts',(-7.80796793853896,38.4914558623083,
-235.35005));
#193822=CARTESIAN_POINT('Ctrl Pts',(-6.84026829339966,39.7375184536817,
-234.671163119943));
#193823=CARTESIAN_POINT('Ctrl Pts',(-6.83602394718808,39.2929688862628,
-235.350050000027));
#193824=CARTESIAN_POINT('Ctrl Pts',(-6.82559161828985,38.4810313542666,
-235.35005));
#193825=CARTESIAN_POINT('Ctrl Pts',(-5.45752242742407,39.8114784377381,
-234.677676143363));
#193826=CARTESIAN_POINT('Ctrl Pts',(-5.4226222629611,39.3679214220723,-235.350049999987));
#193827=CARTESIAN_POINT('Ctrl Pts',(-5.35870347059637,38.5640529809275,
-235.35005));
#193828=CARTESIAN_POINT('Ctrl Pts',(-4.99769610645251,39.8521042185811,
-234.679138440416));
#193829=CARTESIAN_POINT('Ctrl Pts',(-4.95262310277034,39.4092970533836,
-235.350050000034));
#193830=CARTESIAN_POINT('Ctrl Pts',(-4.87084783106756,38.6081920654726,
-235.35005));
#193831=CARTESIAN_POINT('Ctrl Pts',(-4.30945715270495,39.9372528391947,
-234.680264606398));
#193832=CARTESIAN_POINT('Ctrl Pts',(-4.24936647991965,39.4961966039752,
-235.350049999983));
#193833=CARTESIAN_POINT('Ctrl Pts',(-4.14073989606153,38.699320253323,-235.35005));
#193834=CARTESIAN_POINT('Ctrl Pts',(-4.08028903034606,39.9696611739215,
-234.680464330858));
#193835=CARTESIAN_POINT('Ctrl Pts',(-4.01520883927272,39.5292913024185,
-235.350050000003));
#193836=CARTESIAN_POINT('Ctrl Pts',(-3.89764918017226,38.7338397861251,
-235.35005));
#193837=CARTESIAN_POINT('Ctrl Pts',(-3.79422129172372,40.0152320597201,
-234.680493511581));
#193838=CARTESIAN_POINT('Ctrl Pts',(-3.72292214062828,39.5758501073975,
-235.350049999999));
#193839=CARTESIAN_POINT('Ctrl Pts',(-3.59413684837652,38.7822104558047,
-235.35005));
#193840=CARTESIAN_POINT('Ctrl Pts',(-3.73702740263105,40.0245994768347,
-234.680488271922));
#193841=CARTESIAN_POINT('Ctrl Pts',(-3.66448423965549,39.585421766879,-235.350050000009));
#193842=CARTESIAN_POINT('Ctrl Pts',(-3.5334519508703,38.7921458859281,-235.35005));
#193843=CARTESIAN_POINT('Ctrl Pts',(-3.62268126481012,40.0438423896311,
-234.680455404551));
#193844=CARTESIAN_POINT('Ctrl Pts',(-3.54764974254042,39.6050865585617,
-235.350049999992));
#193845=CARTESIAN_POINT('Ctrl Pts',(-3.41211742808775,38.8125413393334,
-235.35005));
#193846=CARTESIAN_POINT('Ctrl Pts',(-3.5692122635324,40.0532709032775,-234.680346020914));
#193847=CARTESIAN_POINT('Ctrl Pts',(-3.49163377701029,39.6149697737271,
-235.350049999997));
#193848=CARTESIAN_POINT('Ctrl Pts',(-3.3514772908386,38.8231424750591,-235.35005));
#193849=CARTESIAN_POINT('Ctrl Pts',(-3.37543931947594,40.086677128215,-234.680722248495));
#193850=CARTESIAN_POINT('Ctrl Pts',(-3.30206245560333,39.6476048575096,
-235.350050000005));
#193851=CARTESIAN_POINT('Ctrl Pts',(-3.16954343953211,38.8547460000193,
-235.35005));
#193852=CARTESIAN_POINT('Ctrl Pts',(-3.24615627214412,40.107698597565,-234.680959769804));
#193853=CARTESIAN_POINT('Ctrl Pts',(-3.17558645022547,39.6681405857535,
-235.350050000007));
#193854=CARTESIAN_POINT('Ctrl Pts',(-3.04817458518233,38.8746308506878,
-235.35005));
#193855=CARTESIAN_POINT('Ctrl Pts',(-2.08187343433102,40.2856482090734,
-234.68297582909));
#193856=CARTESIAN_POINT('Ctrl Pts',(-2.03698344603342,39.8419168609564,
-235.350049999946));
#193857=CARTESIAN_POINT('Ctrl Pts',(-1.95514022672127,39.0429654436086,
-235.35005));
#193858=CARTESIAN_POINT('Ctrl Pts',(-1.03992589660121,40.3642807862687,
-234.683880644658));
#193859=CARTESIAN_POINT('Ctrl Pts',(-1.01727787524803,39.9187933007582,
-235.35004999981));
#193860=CARTESIAN_POINT('Ctrl Pts',(-0.976538624615736,39.1173940812476,
-235.35005));
#193861=CARTESIAN_POINT('Ctrl Pts',(1.55890162323515E-9,40.3642807857292,
-234.68388064352));
#193862=CARTESIAN_POINT('Ctrl Pts',(1.00185676570813E-9,39.9187933003983,
-235.35005));
#193863=CARTESIAN_POINT('Ctrl Pts',(-2.25962702508982E-13,39.1173940795976,
-235.35005));
#193864=CARTESIAN_POINT('',(-16.4332022013982,39.4328349445453,-234.711150502351));
#193865=CARTESIAN_POINT('',(-9.39019377446308,39.9042990656516,-234.645334714758));
#193866=CARTESIAN_POINT('Ctrl Pts',(-16.4332022013982,39.4328349445453,
-234.711150502351));
#193867=CARTESIAN_POINT('Ctrl Pts',(-16.3992276324636,39.4408576593895,
-234.711246833797));
#193868=CARTESIAN_POINT('Ctrl Pts',(-16.3607560482782,39.4503671063563,
-234.710664303478));
#193869=CARTESIAN_POINT('Ctrl Pts',(-16.2880944548047,39.4676591916655,
-234.7101449985));
#193870=CARTESIAN_POINT('Ctrl Pts',(-16.1790829189936,39.4932896670378,
-234.709361988129));
#193871=CARTESIAN_POINT('Ctrl Pts',(-15.9245911466271,39.5509439815655,
-234.707507047121));
#193872=CARTESIAN_POINT('Ctrl Pts',(-15.7062385667385,39.5966884073824,
-234.705870653621));
#193873=CARTESIAN_POINT('Ctrl Pts',(-15.2692680789422,39.683314194241,-234.702539239027));
#193874=CARTESIAN_POINT('Ctrl Pts',(-14.9776205594326,39.7345686697748,
-234.70024310695));
#193875=CARTESIAN_POINT('Ctrl Pts',(-14.1016635745331,39.86930023212,-234.693111997869));
#193876=CARTESIAN_POINT('Ctrl Pts',(-13.516248031243,39.9337488812737,-234.688020797378));
#193877=CARTESIAN_POINT('Ctrl Pts',(-12.3424751228906,40.0121804061296,
-234.677117952301));
#193878=CARTESIAN_POINT('Ctrl Pts',(-11.7541027116113,40.0262438052819,
-234.671305171419));
#193879=CARTESIAN_POINT('Ctrl Pts',(-10.8693864701415,40.0093800798719,
-234.662019550443));
#193880=CARTESIAN_POINT('Ctrl Pts',(-10.574107832413,39.997403078896,-234.658827716551));
#193881=CARTESIAN_POINT('Ctrl Pts',(-10.1305567950971,39.9697814600154,
-234.65387955676));
#193882=CARTESIAN_POINT('Ctrl Pts',(-9.98260217772238,39.9589639695816,
-234.65220378061));
#193883=CARTESIAN_POINT('Ctrl Pts',(-9.76053944083152,39.9402973568872,
-234.649654708411));
#193884=CARTESIAN_POINT('Ctrl Pts',(-9.68649604578775,39.9336687262222,
-234.648798971929));
#193885=CARTESIAN_POINT('Ctrl Pts',(-9.53836616196596,39.9195955120497,
-234.647075597267));
#193886=CARTESIAN_POINT('Ctrl Pts',(-9.46288115140502,39.9121528807897,
-234.645933903814));
#193887=CARTESIAN_POINT('Ctrl Pts',(-9.39019377446308,39.9042990656516,
-234.645334714758));
#193888=CARTESIAN_POINT('',(-4.87988937169148E-10,40.3641796532955,-234.68403185425));
#193889=CARTESIAN_POINT('Ctrl Pts',(-9.39019377446308,39.9042990656516,
-234.645334714758));
#193890=CARTESIAN_POINT('Ctrl Pts',(-9.3747535947859,39.9026279267357,-234.64521229516));
#193891=CARTESIAN_POINT('Ctrl Pts',(-9.36241902555493,39.9009373782415,
-234.645694440806));
#193892=CARTESIAN_POINT('Ctrl Pts',(-9.33401274103675,39.8975447406835,
-234.646059912463));
#193893=CARTESIAN_POINT('Ctrl Pts',(-9.31948440688403,39.8958258096469,
-234.646245966043));
#193894=CARTESIAN_POINT('Ctrl Pts',(-9.27590015649556,39.8907177156527,
-234.646801541329));
#193895=CARTESIAN_POINT('Ctrl Pts',(-9.24684499237614,39.8873772511015,
-234.647168477744));
#193896=CARTESIAN_POINT('Ctrl Pts',(-9.15968291175106,39.8775501713831,
-234.648259112729));
#193897=CARTESIAN_POINT('Ctrl Pts',(-9.10157940837895,39.8712578586117,
-234.648972640374));
#193898=CARTESIAN_POINT('Ctrl Pts',(-8.92728571984679,39.8531547210409,
-234.651073746281));
#193899=CARTESIAN_POINT('Ctrl Pts',(-8.81111237470077,39.8421175196824,
-234.652421897223));
#193900=CARTESIAN_POINT('Ctrl Pts',(-7.76582808922892,39.7520042646991,
-234.664105356224));
#193901=CARTESIAN_POINT('Ctrl Pts',(-6.84026733244978,39.737417809177,-234.671316797084));
#193902=CARTESIAN_POINT('Ctrl Pts',(-5.45751451507149,39.8113778773355,
-234.677828559475));
#193903=CARTESIAN_POINT('Ctrl Pts',(-4.9976858845813,39.8520037966934,-234.679290572791));
#193904=CARTESIAN_POINT('Ctrl Pts',(-4.30944352176845,39.9371527902381,
-234.680416520115));
#193905=CARTESIAN_POINT('Ctrl Pts',(-4.0802742669589,39.9695612763832,-234.680616205782));
#193906=CARTESIAN_POINT('Ctrl Pts',(-3.79420511746956,40.015132385667,-234.680645380837));
#193907=CARTESIAN_POINT('Ctrl Pts',(-3.73701094619056,40.024499849226,-234.680640142195));
#193908=CARTESIAN_POINT('Ctrl Pts',(-3.6226642440044,40.0437428584269,-234.680607281209));
#193909=CARTESIAN_POINT('Ctrl Pts',(-3.56919466536356,40.0531714775527,
-234.680497918817));
#193910=CARTESIAN_POINT('Ctrl Pts',(-3.37542267307509,40.0865775195304,
-234.680874073317));
#193911=CARTESIAN_POINT('Ctrl Pts',(-3.24614026173874,40.1075988736087,
-234.681111548481));
#193912=CARTESIAN_POINT('Ctrl Pts',(-2.08186324557725,40.285547494813,-234.683127215862));
#193913=CARTESIAN_POINT('Ctrl Pts',(-1.03992075515157,40.3641796537477,
-234.684031855518));
#193914=CARTESIAN_POINT('Ctrl Pts',(3.8825005278725E-15,40.3641796532956,
-234.68403185425));
#193915=CARTESIAN_POINT('',(-4.88066281613177E-10,39.1173940795976,-235.35005));
#193916=CARTESIAN_POINT('Origin',(-1.46397402467705E-9,39.1173940795976,
-233.85005));
#193917=CARTESIAN_POINT('',(-23.5337713018193,37.7635770079652,-235.35005));
#193918=CARTESIAN_POINT('Ctrl Pts',(-4.88056262071268E-10,39.1173940795976,
-235.35005));
#193919=CARTESIAN_POINT('Ctrl Pts',(-0.356337354408647,39.1173940801907,
-235.35005));
#193920=CARTESIAN_POINT('Ctrl Pts',(-0.712421386489358,39.1074881627783,
-235.35005));
#193921=CARTESIAN_POINT('Ctrl Pts',(-1.06804669090614,39.0877008682734,
-235.35005));
#193922=CARTESIAN_POINT('Ctrl Pts',(-1.42342102172174,39.0679275381532,
-235.35005));
#193923=CARTESIAN_POINT('Ctrl Pts',(-1.77833765771469,39.0382867855085,
-235.35005));
#193924=CARTESIAN_POINT('Ctrl Pts',(-2.13259508534334,38.9987512850576,
-235.35005));
#193925=CARTESIAN_POINT('Ctrl Pts',(-2.3977029451949,38.9691649698663,-235.35005));
#193926=CARTESIAN_POINT('Ctrl Pts',(-2.66244173694949,38.9340362908303,
-235.35005));
#193927=CARTESIAN_POINT('Ctrl Pts',(-2.92672632410968,38.8933347006997,
-235.35005));
#193928=CARTESIAN_POINT('Ctrl Pts',(-2.92737060582729,38.8932354770155,
-235.35005));
#193929=CARTESIAN_POINT('Ctrl Pts',(-2.92801488569497,38.8931362200352,
-235.35005));
#193930=CARTESIAN_POINT('Ctrl Pts',(-2.9286591637141,38.8930369297577,-235.35005));
#193931=CARTESIAN_POINT('Ctrl Pts',(-3.04946230530941,38.8744198466251,
-235.35005));
#193932=CARTESIAN_POINT('Ctrl Pts',(-3.17018687876639,38.8546342346527,
-235.35005));
#193933=CARTESIAN_POINT('Ctrl Pts',(-3.2908326746107,38.8336769884121,-235.35005));
#193934=CARTESIAN_POINT('Ctrl Pts',(-3.35147729175591,38.8231424798055,
-235.35005));
#193935=CARTESIAN_POINT('Ctrl Pts',(-3.41211742901483,38.8125413440661,
-235.35005));
#193936=CARTESIAN_POINT('Ctrl Pts',(-3.47278469039213,38.8023436180629,
-235.35005));
#193937=CARTESIAN_POINT('Ctrl Pts',(-3.53345195207147,38.792145892009,-235.35005));
#193938=CARTESIAN_POINT('Ctrl Pts',(-3.59413684982628,38.7822104632522,
-235.35005));
#193939=CARTESIAN_POINT('Ctrl Pts',(-3.65483931632616,38.7725363318486,
-235.35005));
#193940=CARTESIAN_POINT('Ctrl Pts',(-3.65546036670289,38.7724373552617,
-235.35005));
#193941=CARTESIAN_POINT('Ctrl Pts',(-3.65608141891697,38.7723384060014,
-235.35005));
#193942=CARTESIAN_POINT('Ctrl Pts',(-3.65670247296838,38.7722394840674,
-235.35005));
#193943=CARTESIAN_POINT('Ctrl Pts',(-3.89889272070765,38.7336632479809,
-235.35005));
#193944=CARTESIAN_POINT('Ctrl Pts',(-4.14136237950718,38.6992425871297,
-235.35005));
#193945=CARTESIAN_POINT('Ctrl Pts',(-4.38410921010885,38.6689442097637,
-235.35005));
#193946=CARTESIAN_POINT('Ctrl Pts',(-4.38470863655102,38.668869392521,-235.35005));
#193947=CARTESIAN_POINT('Ctrl Pts',(-4.3853080646873,38.668794600474,-235.35005));
#193948=CARTESIAN_POINT('Ctrl Pts',(-4.38590749451765,38.6687198336225,
-235.35005));
#193949=CARTESIAN_POINT('Ctrl Pts',(-4.87204943971823,38.6080833741381,
-235.35005));
#193950=CARTESIAN_POINT('Ctrl Pts',(-5.3593056525522,38.5640188990606,-235.35005));
#193951=CARTESIAN_POINT('Ctrl Pts',(-5.8476661903511,38.5363791735204,-235.35005));
#193952=CARTESIAN_POINT('Ctrl Pts',(-5.84822203537533,38.5363477143775,
-235.35005));
#193953=CARTESIAN_POINT('Ctrl Pts',(-5.84877788183748,38.5363162764838,
-235.35005));
#193954=CARTESIAN_POINT('Ctrl Pts',(-5.84933372973754,38.5362848598395,
-235.35005));
#193955=CARTESIAN_POINT('Ctrl Pts',(-6.82670834791507,38.4810434337014,
-235.35005));
#193956=CARTESIAN_POINT('Ctrl Pts',(-7.80852886358045,38.4915002286893,
-235.35005));
#193957=CARTESIAN_POINT('Ctrl Pts',(-8.79483412069355,38.5695117626516,
-235.35005));
#193958=CARTESIAN_POINT('Ctrl Pts',(-8.79530155976179,38.5695487346118,
-235.35005));
#193959=CARTESIAN_POINT('Ctrl Pts',(-8.79576899951021,38.5695857217635,
-235.35005));
#193960=CARTESIAN_POINT('Ctrl Pts',(-8.79623643993881,38.5696227241071,
-235.35005));
#193961=CARTESIAN_POINT('Ctrl Pts',(-8.91912763148384,38.5793507275409,
-235.35005));
#193962=CARTESIAN_POINT('Ctrl Pts',(-9.0420658365827,38.5901287540257,-235.35005));
#193963=CARTESIAN_POINT('Ctrl Pts',(-9.16505139013463,38.6019642805906,
-235.35005));
#193964=CARTESIAN_POINT('Ctrl Pts',(-9.22677806664333,38.6079045532363,
-235.35005));
#193965=CARTESIAN_POINT('Ctrl Pts',(-9.28851667261295,38.6141112633977,
-235.35005));
#193966=CARTESIAN_POINT('Ctrl Pts',(-9.35026726349676,38.6205856491488,
-235.35005));
#193967=CARTESIAN_POINT('Ctrl Pts',(-9.38114255892181,38.6238228420226,
-235.35005));
#193968=CARTESIAN_POINT('Ctrl Pts',(-9.41202085071314,38.6271269568751,
-235.35005));
#193969=CARTESIAN_POINT('Ctrl Pts',(-9.44290214664127,38.6304981674401,
-235.35005));
#193970=CARTESIAN_POINT('Ctrl Pts',(-9.45834279459725,38.6321837727217,
-235.35005));
#193971=CARTESIAN_POINT('Ctrl Pts',(-9.47378419360446,38.6338861521134,
-235.35005));
#193972=CARTESIAN_POINT('Ctrl Pts',(-9.48922634467739,38.6356053285559,
-235.35005));
#193973=CARTESIAN_POINT('Ctrl Pts',(-9.50466849574347,38.6373245049977,
-235.35005));
#193974=CARTESIAN_POINT('Ctrl Pts',(-9.5201115320738,38.6390634531904,-235.35005));
#193975=CARTESIAN_POINT('Ctrl Pts',(-9.53555504565915,38.6408130606221,
-235.35005));
#193976=CARTESIAN_POINT('Ctrl Pts',(-9.53599979614812,38.6408634467442,
-235.35005));
#193977=CARTESIAN_POINT('Ctrl Pts',(-9.53644454592807,38.6409138170309,
-235.35005));
#193978=CARTESIAN_POINT('Ctrl Pts',(-9.53688929499903,38.6409641714826,
-235.35005));
#193979=CARTESIAN_POINT('Ctrl Pts',(-9.78353997567394,38.6688899404139,
-235.35005));
#193980=CARTESIAN_POINT('Ctrl Pts',(-10.0299725958919,38.6919454677587,
-235.35005));
#193981=CARTESIAN_POINT('Ctrl Pts',(-10.2761899495318,38.7101931856168,
-235.35005));
#193982=CARTESIAN_POINT('Ctrl Pts',(-10.276610550529,38.7102243572958,-235.35005));
#193983=CARTESIAN_POINT('Ctrl Pts',(-10.2770311508993,38.7102555149728,
-235.35005));
#193984=CARTESIAN_POINT('Ctrl Pts',(-10.2774517506426,38.7102866586477,
-235.35005));
#193985=CARTESIAN_POINT('Ctrl Pts',(-10.7703523229537,38.7467839115718,
-235.35005));
#193986=CARTESIAN_POINT('Ctrl Pts',(-11.2623919369706,38.7640519886334,
-235.35005));
#193987=CARTESIAN_POINT('Ctrl Pts',(-11.7535889208686,38.7625005477271,
-235.35005));
#193988=CARTESIAN_POINT('Ctrl Pts',(-11.7539614951304,38.7624993709549,
-235.35005));
#193989=CARTESIAN_POINT('Ctrl Pts',(-11.7543340689085,38.7624981833791,
-235.35005));
#193990=CARTESIAN_POINT('Ctrl Pts',(-11.7547066422029,38.7624969849996,
-235.35005));
#193991=CARTESIAN_POINT('Ctrl Pts',(-12.7375637756362,38.7593356316055,
-235.35005));
#193992=CARTESIAN_POINT('Ctrl Pts',(-13.717054647793,38.6809905735713,-235.35005));
#193993=CARTESIAN_POINT('Ctrl Pts',(-14.6931353852465,38.5264823709591,
-235.35005));
#193994=CARTESIAN_POINT('Ctrl Pts',(-14.6934128886607,38.5264384436977,
-235.35005));
#193995=CARTESIAN_POINT('Ctrl Pts',(-14.6936903917976,38.5263945102443,
-235.35005));
#193996=CARTESIAN_POINT('Ctrl Pts',(-14.6939678946573,38.5263505705987,
-235.35005));
#193997=CARTESIAN_POINT('Ctrl Pts',(-14.9378025765395,38.4877419252278,
-235.35005));
#193998=CARTESIAN_POINT('Ctrl Pts',(-15.1814232314178,38.4443525285445,
-235.35005));
#193999=CARTESIAN_POINT('Ctrl Pts',(-15.4248261118799,38.3960995538484,
-235.35005));
#194000=CARTESIAN_POINT('Ctrl Pts',(-15.5466660626659,38.3719456077197,
-235.35005));
#194001=CARTESIAN_POINT('Ctrl Pts',(-15.6684514489775,38.3465730677093,
-235.35005));
#194002=CARTESIAN_POINT('Ctrl Pts',(-15.7901818202738,38.3199719794952,
-235.35005));
#194003=CARTESIAN_POINT('Ctrl Pts',(-15.8510470114032,38.3066714341903,
-235.35005));
#194004=CARTESIAN_POINT('Ctrl Pts',(-15.9118984489941,38.2930637564789,
-235.35005));
#194005=CARTESIAN_POINT('Ctrl Pts',(-15.9727360779946,38.2791477303716,
-235.35005));
#194006=CARTESIAN_POINT('Ctrl Pts',(-16.0031548943984,38.2721897168825,
-235.35005));
#194007=CARTESIAN_POINT('Ctrl Pts',(-16.0335702586684,38.2651546166131,
-235.35005));
#194008=CARTESIAN_POINT('Ctrl Pts',(-16.0639821640006,38.2580422793406,
-235.35005));
#194009=CARTESIAN_POINT('Ctrl Pts',(-16.0791881172091,38.2544861105775,
-235.35005));
#194010=CARTESIAN_POINT('Ctrl Pts',(-16.0943932056889,38.2509106325926,
-235.35005));
#194011=CARTESIAN_POINT('Ctrl Pts',(-16.1095974285865,38.2473158267122,
-235.35005));
#194012=CARTESIAN_POINT('Ctrl Pts',(-16.1248016518712,38.2437210207403,
-235.35005));
#194013=CARTESIAN_POINT('Ctrl Pts',(-16.1400046170681,38.2400982079978,
-235.35005));
#194014=CARTESIAN_POINT('Ctrl Pts',(-16.1552076184638,38.2364760331285,
-235.35005));
#194015=CARTESIAN_POINT('Ctrl Pts',(-16.1554380521512,38.2364211313963,
-235.35005));
#194016=CARTESIAN_POINT('Ctrl Pts',(-16.1556684860895,38.2363662335797,
-235.35005));
#194017=CARTESIAN_POINT('Ctrl Pts',(-16.1558989202786,38.2363113396788,
-235.35005));
#194018=CARTESIAN_POINT('Ctrl Pts',(-16.6421654926102,38.1204731945478,
-235.35005));
#194019=CARTESIAN_POINT('Ctrl Pts',(-17.12954963108,38.0220712232547,-235.35005));
#194020=CARTESIAN_POINT('Ctrl Pts',(-17.618016277175,37.9405600315694,-235.35005));
#194021=CARTESIAN_POINT('Ctrl Pts',(-17.6182014585966,37.9405291300565,
-235.35005));
#194022=CARTESIAN_POINT('Ctrl Pts',(-17.6183866401739,37.9404982309351,
-235.35005));
#194023=CARTESIAN_POINT('Ctrl Pts',(-17.6185718219071,37.9404673342052,
-235.35005));
#194024=CARTESIAN_POINT('Ctrl Pts',(-18.5958771217091,37.7774083899232,
-235.35005));
#194025=CARTESIAN_POINT('Ctrl Pts',(-19.5774518164939,37.6809633951768,
-235.35005));
#194026=CARTESIAN_POINT('Ctrl Pts',(-20.5633123297537,37.6513870472257,
-235.35005));
#194027=CARTESIAN_POINT('Ctrl Pts',(-21.5491728430134,37.6218106992746,
-235.35005));
#194028=CARTESIAN_POINT('Ctrl Pts',(-22.5393191900798,37.6591029589903,
-235.35005));
#194029=CARTESIAN_POINT('Ctrl Pts',(-23.5337713018193,37.7635770079652,
-235.35005));
#194030=CARTESIAN_POINT('',(-23.3965311730466,39.0699180248394,-234.574369193924));
#194031=CARTESIAN_POINT('Origin',(-23.5337713018193,37.7635770079652,-233.85005));
#194032=CARTESIAN_POINT('Ctrl Pts',(-23.3965311730097,39.0699180251917,
-234.574369193282));
#194033=CARTESIAN_POINT('Ctrl Pts',(-22.2279621072998,38.927851533746,-234.609178040102));
#194034=CARTESIAN_POINT('Ctrl Pts',(-20.4798185422076,38.8660796071235,
-234.651026311726));
#194035=CARTESIAN_POINT('Ctrl Pts',(-18.7417049717577,39.032269945489,-234.680423055754));
#194036=CARTESIAN_POINT('Ctrl Pts',(-17.8745669582133,39.1534396965386,
-234.693304161216));
#194037=CARTESIAN_POINT('Ctrl Pts',(-17.5858370342812,39.2001485327806,
-234.697297627868));
#194038=CARTESIAN_POINT('Ctrl Pts',(-17.0451048369348,39.2999745776045,
-234.704218024849));
#194039=CARTESIAN_POINT('Ctrl Pts',(-16.7930294294645,39.351547020454,-234.70721839636));
#194040=CARTESIAN_POINT('Ctrl Pts',(-16.5052918362263,39.4162808271944,
-234.710395408776));
#194041=CARTESIAN_POINT('Ctrl Pts',(-16.4710147540983,39.4239043905358,
-234.71104178217));
#194042=CARTESIAN_POINT('Ctrl Pts',(-16.4332022013982,39.4328349445453,
-234.711150502351));
#194043=CARTESIAN_POINT('Ctrl Pts',(-23.5337713018193,37.7635770079652,
-235.35005));
#194044=CARTESIAN_POINT('Ctrl Pts',(-23.4412215482421,38.6445258986454,
-235.35005));
#194045=CARTESIAN_POINT('Ctrl Pts',(-23.3965311730093,39.0699180251918,
-234.574369193281));
#194046=CARTESIAN_POINT('Ctrl Pts',(-23.6412313452744,37.7748664312125,
-235.35005));
#194047=CARTESIAN_POINT('Ctrl Pts',(-23.6100297261144,38.6346548826691,
-235.35005));
#194048=CARTESIAN_POINT('Ctrl Pts',(-23.5947564504146,39.0708169807221,
-234.610306553998));
#194049=CARTESIAN_POINT('Ctrl Pts',(-23.7487418755492,37.7752275005428,
-235.35005));
#194050=CARTESIAN_POINT('Ctrl Pts',(-23.778719103045,38.6109201787134,-235.35005));
#194051=CARTESIAN_POINT('Ctrl Pts',(-23.7949692188817,39.052344777689,-234.642115924617));
#194052=CARTESIAN_POINT('Ctrl Pts',(-23.8561664752437,37.7630917536255,
-235.35005));
#194053=CARTESIAN_POINT('Ctrl Pts',(-23.9474058055444,38.5707334611873,
-235.35005));
#194054=CARTESIAN_POINT('Ctrl Pts',(-23.9972286658429,39.0117605909835,
-234.669151698811));
#194055=CARTESIAN_POINT('',(-23.997228665843,39.0117605909833,-234.669151698811));
#194056=CARTESIAN_POINT('',(-23.8561664752437,37.7630917536256,-235.35005));
#194057=CARTESIAN_POINT('Origin',(-23.8561664752439,37.7630917536255,-233.85005));
#194058=CARTESIAN_POINT('Ctrl Pts',(-23.9972286658434,39.0117605909834,
-234.669151698811));
#194059=CARTESIAN_POINT('Ctrl Pts',(-23.7949692188817,39.052344777689,-234.642115924617));
#194060=CARTESIAN_POINT('Ctrl Pts',(-23.5947564504146,39.0708169807221,
-234.610306553998));
#194061=CARTESIAN_POINT('Ctrl Pts',(-23.3965311730097,39.0699180251917,
-234.574369193282));
#194062=CARTESIAN_POINT('Ctrl Pts',(-23.5337713018193,37.7635770079652,
-235.35005));
#194063=CARTESIAN_POINT('Ctrl Pts',(-23.6412535989187,37.7748687641791,
-235.35005));
#194064=CARTESIAN_POINT('Ctrl Pts',(-23.7487194439798,37.7752300509467,
-235.35005));
#194065=CARTESIAN_POINT('Ctrl Pts',(-23.8561664752437,37.7630917536256,
-235.35005));
#194066=CARTESIAN_POINT('Ctrl Pts',(-23.8561664752439,37.7630917536255,
-235.35005));
#194067=CARTESIAN_POINT('Ctrl Pts',(-23.9474058055448,38.5707334611872,
-235.35005));
#194068=CARTESIAN_POINT('Ctrl Pts',(-23.9972286658434,39.0117605909834,
-234.669151698811));
#194069=CARTESIAN_POINT('Ctrl Pts',(-25.0882853750842,37.6238992104159,
-235.35005));
#194070=CARTESIAN_POINT('Ctrl Pts',(-25.1842887597299,38.431109053993,-235.350049999742));
#194071=CARTESIAN_POINT('Ctrl Pts',(-25.2366484173464,38.8718330388058,
-234.669014852156));
#194072=CARTESIAN_POINT('Ctrl Pts',(-26.319091123968,37.47392953931,-235.35005));
#194073=CARTESIAN_POINT('Ctrl Pts',(-26.4198403391809,38.280686857661,-235.35005000043));
#194074=CARTESIAN_POINT('Ctrl Pts',(-26.4747606339603,38.7210799284767,
-234.668852342857));
#194075=CARTESIAN_POINT('Ctrl Pts',(-27.5485779004777,37.3131372941855,
-235.35005));
#194076=CARTESIAN_POINT('Ctrl Pts',(-27.654024085186,38.1194242486926,-235.35005));
#194077=CARTESIAN_POINT('Ctrl Pts',(-27.711570814231,38.5594513301076,-234.668667513818));
#194078=CARTESIAN_POINT('',(-27.7115708142298,38.5594513301044,-234.66866751382));
#194079=CARTESIAN_POINT('',(-27.5485779004777,37.3131372941855,-235.35005));
#194080=CARTESIAN_POINT('Origin',(-27.5485779004728,37.3131372941843,-233.850050000003));
#194081=CARTESIAN_POINT('Origin',(-0.0438186590672052,-173.169156331663,
-234.199437903576));
#194082=CARTESIAN_POINT('Origin',(-0.0633608499784,-172.860463397816,-235.350049999539));
#194083=CARTESIAN_POINT('Ctrl Pts',(-27.5485779004728,37.3131372941862,
-235.35005));
#194084=CARTESIAN_POINT('Ctrl Pts',(-27.654024085184,38.1194242486908,-235.35005));
#194085=CARTESIAN_POINT('Ctrl Pts',(-27.7115708142308,38.559451330106,-234.66866751382));
#194086=CARTESIAN_POINT('Ctrl Pts',(-27.6119495440962,37.3048495676945,
-235.35005));
#194087=CARTESIAN_POINT('Ctrl Pts',(-27.7265642955278,38.1035833263501,
-235.350049999996));
#194088=CARTESIAN_POINT('Ctrl Pts',(-27.7898688006155,38.543857161573,-234.676819323508));
#194089=CARTESIAN_POINT('Ctrl Pts',(-27.6750964089389,37.2953595442226,
-235.35005));
#194090=CARTESIAN_POINT('Ctrl Pts',(-27.803498135569,38.0832505563202,-235.350049999997));
#194091=CARTESIAN_POINT('Ctrl Pts',(-27.8754619604023,38.52353948073,-234.688258517325));
#194092=CARTESIAN_POINT('Ctrl Pts',(-27.7691733848276,37.2776980879525,
-235.35005));
#194093=CARTESIAN_POINT('Ctrl Pts',(-27.9226851009708,38.0444330714304,
-235.350050000001));
#194094=CARTESIAN_POINT('Ctrl Pts',(-28.0106528477426,38.4835354389051,
-234.709081676005));
#194095=CARTESIAN_POINT('Ctrl Pts',(-27.8004215724929,37.2712202551586,
-235.35005));
#194096=CARTESIAN_POINT('Ctrl Pts',(-27.962669518358,38.0303893933949,-235.350049999995));
#194097=CARTESIAN_POINT('Ctrl Pts',(-28.0564170190361,38.4688219126267,
-234.716327424367));
#194098=CARTESIAN_POINT('Ctrl Pts',(-27.8627200032187,37.2572093770216,
-235.35005));
#194099=CARTESIAN_POINT('Ctrl Pts',(-28.0390618914339,38.0040014727884,
-235.350050000004));
#194100=CARTESIAN_POINT('Ctrl Pts',(-28.1423078435221,38.4410402419925,
-234.727885440078));
#194101=CARTESIAN_POINT('Ctrl Pts',(-27.8937776977631,37.249697476023,-235.35005));
#194102=CARTESIAN_POINT('Ctrl Pts',(-28.07508312287,37.9920997651976,-235.350050000001));
#194103=CARTESIAN_POINT('Ctrl Pts',(-28.1816910211067,38.4285212429546,
-234.731834361418));
#194104=CARTESIAN_POINT('Ctrl Pts',(-27.9867858054616,37.226404790223,-235.35005));
#194105=CARTESIAN_POINT('Ctrl Pts',(-28.1793531401323,37.9589854504683,
-235.350049999998));
#194106=CARTESIAN_POINT('Ctrl Pts',(-28.2937808316253,38.3938810745564,
-234.740558887245));
#194107=CARTESIAN_POINT('Ctrl Pts',(-28.0485551598146,37.2098945175254,
-235.35005));
#194108=CARTESIAN_POINT('Ctrl Pts',(-28.251028133496,37.9337425924481,-235.35004999998));
#194109=CARTESIAN_POINT('Ctrl Pts',(-28.3724365366315,38.3671595974566,
-234.748243384598));
#194110=CARTESIAN_POINT('Ctrl Pts',(-28.1402497418155,37.1819908028498,
-235.35005));
#194111=CARTESIAN_POINT('Ctrl Pts',(-28.3633757810457,37.8864187374528,
-235.35005000001));
#194112=CARTESIAN_POINT('Ctrl Pts',(-28.499410390972,38.315752826462,-234.764279480932));
#194113=CARTESIAN_POINT('Ctrl Pts',(-28.1706617267493,37.1721527193585,
-235.35005));
#194114=CARTESIAN_POINT('Ctrl Pts',(-28.4004253047465,37.8701990320713,
-235.350049999998));
#194115=CARTESIAN_POINT('Ctrl Pts',(-28.541281614628,38.2980250294177,-234.769400544257));
#194116=CARTESIAN_POINT('Ctrl Pts',(-28.2311847426228,37.1515938768492,
-235.35005));
#194117=CARTESIAN_POINT('Ctrl Pts',(-28.4719778581327,37.8390215876304,
-235.350050000002));
#194118=CARTESIAN_POINT('Ctrl Pts',(-28.6209241135967,38.2641359479009,
-234.77768479838));
#194119=CARTESIAN_POINT('Ctrl Pts',(-28.2612972505945,37.1409013962204,
-235.35005));
#194120=CARTESIAN_POINT('Ctrl Pts',(-28.5064923453729,37.824118998956,-235.350049999988));
#194121=CARTESIAN_POINT('Ctrl Pts',(-28.6586684014758,38.248067198284,-234.780840885022));
#194122=CARTESIAN_POINT('Ctrl Pts',(-28.3512820909987,37.1078462406674,
-235.35005));
#194123=CARTESIAN_POINT('Ctrl Pts',(-28.6091714812706,37.7788267124199,
-235.350050000025));
#194124=CARTESIAN_POINT('Ctrl Pts',(-28.7708554177228,38.1992011674236,
-234.789873968856));
#194125=CARTESIAN_POINT('Ctrl Pts',(-28.4108519482495,37.0845842971443,
-235.35005));
#194126=CARTESIAN_POINT('Ctrl Pts',(-28.6757355642658,37.7490178712301,
-235.350049999991));
#194127=CARTESIAN_POINT('Ctrl Pts',(-28.8426158139035,38.1672985579224,
-234.794421341942));
#194128=CARTESIAN_POINT('Ctrl Pts',(-28.5284852992461,37.0351888006413,
-235.35005));
#194129=CARTESIAN_POINT('Ctrl Pts',(-28.8128694279278,37.6793814787632,
-235.350050000009));
#194130=CARTESIAN_POINT('Ctrl Pts',(-28.9946891933229,38.0909484466884,
-234.808461686233));
#194131=CARTESIAN_POINT('Ctrl Pts',(-28.5864462918562,37.0087322113245,
-235.35005));
#194132=CARTESIAN_POINT('Ctrl Pts',(-28.8808495685014,37.641668601605,-235.350050000012));
#194133=CARTESIAN_POINT('Ctrl Pts',(-29.0705233204497,38.0492577914762,
-234.816069500032));
#194134=CARTESIAN_POINT('Ctrl Pts',(-28.6725892746692,36.9674060120273,
-235.35005));
#194135=CARTESIAN_POINT('Ctrl Pts',(-28.9759803010192,37.5902912511275,
-235.350049999993));
#194136=CARTESIAN_POINT('Ctrl Pts',(-29.1727005271663,37.9941274022379,
-234.822565471198));
#194137=CARTESIAN_POINT('Ctrl Pts',(-28.7011808463655,36.9533782896452,
-235.35005));
#194138=CARTESIAN_POINT('Ctrl Pts',(-29.0070493823103,37.5734789125125,
-235.350049999995));
#194139=CARTESIAN_POINT('Ctrl Pts',(-29.2057300258169,37.9762393089045,
-234.824326831928));
#194140=CARTESIAN_POINT('Ctrl Pts',(-28.7439306930081,36.9320540547938,
-235.35005));
#194141=CARTESIAN_POINT('Ctrl Pts',(-29.0531052906671,37.5484365661045,
-235.350050000003));
#194142=CARTESIAN_POINT('Ctrl Pts',(-29.2544014035152,37.9497400570338,
-234.826647318416));
#194143=CARTESIAN_POINT('Ctrl Pts',(-28.7581616928441,36.9249070270844,
-235.35005));
#194144=CARTESIAN_POINT('Ctrl Pts',(-29.0681955001819,37.5403535418641,
-235.350050000002));
#194145=CARTESIAN_POINT('Ctrl Pts',(-29.2701706937271,37.9412800343878,
-234.827215664254));
#194146=CARTESIAN_POINT('Ctrl Pts',(-28.7865561585441,36.9104741568002,
-235.35005));
#194147=CARTESIAN_POINT('Ctrl Pts',(-29.100049296179,37.5217456532107,-235.350049999998));
#194148=CARTESIAN_POINT('Ctrl Pts',(-29.3048419252274,37.921051821916,-234.829913631261));
#194149=CARTESIAN_POINT('Ctrl Pts',(-28.8007140683774,36.9031768938705,
-235.35005));
#194150=CARTESIAN_POINT('Ctrl Pts',(-29.1166642642298,37.5113826540724,
-235.350049999998));
#194151=CARTESIAN_POINT('Ctrl Pts',(-29.3234878417255,37.9094999507468,
-234.831922289268));
#194152=CARTESIAN_POINT('Ctrl Pts',(-28.8711899004085,36.866045739172,-235.35005));
#194153=CARTESIAN_POINT('Ctrl Pts',(-29.2004368662993,37.4572474244772,
-235.350050000008));
#194154=CARTESIAN_POINT('Ctrl Pts',(-29.4185209864353,37.8485528906136,
-234.842993006465));
#194155=CARTESIAN_POINT('Ctrl Pts',(-28.9265109080764,36.8341627598888,
-235.35005));
#194156=CARTESIAN_POINT('Ctrl Pts',(-29.2654910265155,37.4132275967966,
-235.350050000058));
#194157=CARTESIAN_POINT('Ctrl Pts',(-29.4914664732662,37.799141309411,-234.849921198629));
#194158=CARTESIAN_POINT('Ctrl Pts',(-28.9814172171127,36.8014272692485,
-235.35005));
#194159=CARTESIAN_POINT('Ctrl Pts',(-29.3235739752808,37.3753174315542,
-235.35005));
#194160=CARTESIAN_POINT('Ctrl Pts',(-29.5524353619884,37.759180369309,-234.853368133768));
#194161=CARTESIAN_POINT('',(-29.5524353619882,37.7591803693089,-234.853368133768));
#194162=CARTESIAN_POINT('',(-28.9814172171126,36.8014272692484,-235.35005));
#194163=CARTESIAN_POINT('Origin',(-28.9814172171126,36.8014272692485,-233.85005));
#194164=CARTESIAN_POINT('Ctrl Pts',(-29.5524353619882,37.7591803693089,
-234.853368133768));
#194165=CARTESIAN_POINT('Ctrl Pts',(-29.4914664732662,37.799141309411,-234.849921198629));
#194166=CARTESIAN_POINT('Ctrl Pts',(-29.4185209864353,37.8485528906136,
-234.842993006465));
#194167=CARTESIAN_POINT('Ctrl Pts',(-29.3234878417255,37.9094999507468,
-234.831922289268));
#194168=CARTESIAN_POINT('Ctrl Pts',(-29.3048419252274,37.921051821916,-234.829913631261));
#194169=CARTESIAN_POINT('Ctrl Pts',(-29.2701706937271,37.9412800343878,
-234.827215664254));
#194170=CARTESIAN_POINT('Ctrl Pts',(-29.2544014035152,37.9497400570338,
-234.826647318416));
#194171=CARTESIAN_POINT('Ctrl Pts',(-29.2057300258169,37.9762393089045,
-234.824326831928));
#194172=CARTESIAN_POINT('Ctrl Pts',(-29.1727005271663,37.9941274022379,
-234.822565471198));
#194173=CARTESIAN_POINT('Ctrl Pts',(-29.0705233204497,38.0492577914762,
-234.816069500032));
#194174=CARTESIAN_POINT('Ctrl Pts',(-28.9946891933229,38.0909484466884,
-234.808461686233));
#194175=CARTESIAN_POINT('Ctrl Pts',(-28.8426158139035,38.1672985579224,
-234.794421341942));
#194176=CARTESIAN_POINT('Ctrl Pts',(-28.7708554177228,38.1992011674236,
-234.789873968856));
#194177=CARTESIAN_POINT('Ctrl Pts',(-28.6586684014758,38.248067198284,-234.780840885022));
#194178=CARTESIAN_POINT('Ctrl Pts',(-28.6209241135967,38.2641359479009,
-234.77768479838));
#194179=CARTESIAN_POINT('Ctrl Pts',(-28.541281614628,38.2980250294177,-234.769400544257));
#194180=CARTESIAN_POINT('Ctrl Pts',(-28.499410390972,38.315752826462,-234.764279480932));
#194181=CARTESIAN_POINT('Ctrl Pts',(-28.3724365366315,38.3671595974566,
-234.748243384598));
#194182=CARTESIAN_POINT('Ctrl Pts',(-28.2937808316253,38.3938810745564,
-234.740558887245));
#194183=CARTESIAN_POINT('Ctrl Pts',(-28.1816910211067,38.4285212429546,
-234.731834361418));
#194184=CARTESIAN_POINT('Ctrl Pts',(-28.1423078435221,38.4410402419925,
-234.727885440078));
#194185=CARTESIAN_POINT('Ctrl Pts',(-28.0564170190361,38.4688219126267,
-234.716327424367));
#194186=CARTESIAN_POINT('Ctrl Pts',(-28.0106528477426,38.4835354389051,
-234.709081676005));
#194187=CARTESIAN_POINT('Ctrl Pts',(-27.8754619604023,38.52353948073,-234.688258517325));
#194188=CARTESIAN_POINT('Ctrl Pts',(-27.7898688006155,38.543857161573,-234.676819323508));
#194189=CARTESIAN_POINT('Ctrl Pts',(-27.7115708142298,38.5594513301044,
-234.66866751382));
#194190=CARTESIAN_POINT('Ctrl Pts',(-27.5485779004777,37.3131372941856,
-235.35005));
#194191=CARTESIAN_POINT('Ctrl Pts',(-27.6119497053713,37.3048495466029,
-235.35005));
#194192=CARTESIAN_POINT('Ctrl Pts',(-27.6750965458531,37.2953595193401,
-235.35005));
#194193=CARTESIAN_POINT('Ctrl Pts',(-27.7378143932095,37.2835852418792,
-235.35005));
#194194=CARTESIAN_POINT('Ctrl Pts',(-27.7691734109443,37.2776980854911,
-235.35005));
#194195=CARTESIAN_POINT('Ctrl Pts',(-27.8004215957617,37.2712202529943,
-235.35005));
#194196=CARTESIAN_POINT('Ctrl Pts',(-27.8315707886446,37.2642148195972,
-235.35005));
#194197=CARTESIAN_POINT('Ctrl Pts',(-27.8627200211639,37.257209377286,-235.35005));
#194198=CARTESIAN_POINT('Ctrl Pts',(-27.8937777129896,37.2496974771633,
-235.35005));
#194199=CARTESIAN_POINT('Ctrl Pts',(-27.9247804016332,37.2419332526298,
-235.35005));
#194200=CARTESIAN_POINT('Ctrl Pts',(-27.9867858296455,37.2264047908593,
-235.35005));
#194201=CARTESIAN_POINT('Ctrl Pts',(-28.0485551618066,37.2098945246507,
-235.35005));
#194202=CARTESIAN_POINT('Ctrl Pts',(-28.1096848833639,37.191292048355,-235.35005));
#194203=CARTESIAN_POINT('Ctrl Pts',(-28.1402497358115,37.1819908127424,
-235.35005));
#194204=CARTESIAN_POINT('Ctrl Pts',(-28.1706617181454,37.1721527303683,
-235.35005));
#194205=CARTESIAN_POINT('Ctrl Pts',(-28.2009232370621,37.1618733050988,
-235.35005));
#194206=CARTESIAN_POINT('Ctrl Pts',(-28.2311847284776,37.151593889171,-235.35005));
#194207=CARTESIAN_POINT('Ctrl Pts',(-28.2612972337605,37.1409014094734,
-235.35005));
#194208=CARTESIAN_POINT('Ctrl Pts',(-28.2912921994267,37.129883016559,-235.35005));
#194209=CARTESIAN_POINT('Ctrl Pts',(-28.3512820882545,37.1078462463438,
-235.35005));
#194210=CARTESIAN_POINT('Ctrl Pts',(-28.4108519466395,37.0845843013711,
-235.35005));
#194211=CARTESIAN_POINT('Ctrl Pts',(-28.4696686246939,37.0598865511459,
-235.35005));
#194212=CARTESIAN_POINT('Ctrl Pts',(-28.5284852999082,37.0351888021132,
-235.35005));
#194213=CARTESIAN_POINT('Ctrl Pts',(-28.5864462936913,37.0087322116309,
-235.35005));
#194214=CARTESIAN_POINT('Ctrl Pts',(-28.6438749473726,36.9811814124344,
-235.35005));
#194215=CARTESIAN_POINT('Ctrl Pts',(-28.6725892757669,36.9674060120908,
-235.35005));
#194216=CARTESIAN_POINT('Ctrl Pts',(-28.7011808475711,36.9533782894892,
-235.35005));
#194217=CARTESIAN_POINT('Ctrl Pts',(-28.7296807442605,36.9391621333448,
-235.35005));
#194218=CARTESIAN_POINT('Ctrl Pts',(-28.7439306934412,36.9320540548556,
-235.35005));
#194219=CARTESIAN_POINT('Ctrl Pts',(-28.7581616932791,36.9249070270955,
-235.35005));
#194220=CARTESIAN_POINT('Ctrl Pts',(-28.7723589257722,36.9176905920959,
-235.35005));
#194221=CARTESIAN_POINT('Ctrl Pts',(-28.7865561589916,36.9104741567272,
-235.35005));
#194222=CARTESIAN_POINT('Ctrl Pts',(-28.8007140688312,36.9031768937556,
-235.350049999999));
#194223=CARTESIAN_POINT('Ctrl Pts',(-28.8148092348245,36.8957506630084,
-235.350049999999));
#194224=CARTESIAN_POINT('Ctrl Pts',(-28.8711899085552,36.8660457348789,
-235.35005));
#194225=CARTESIAN_POINT('Ctrl Pts',(-28.9265109173313,36.834162754371,-235.35005));
#194226=CARTESIAN_POINT('Ctrl Pts',(-28.9814172171126,36.8014272692486,
-235.35005));
#194227=CARTESIAN_POINT('Ctrl Pts',(-28.6235999918556,37.0129901885974,
-235.35005));
#194228=CARTESIAN_POINT('Ctrl Pts',(-28.9622480552984,37.5906356762342,
-235.350050000051));
#194229=CARTESIAN_POINT('Ctrl Pts',(-29.1883500929521,37.9763249213013,
-234.851571244636));
#194230=CARTESIAN_POINT('Ctrl Pts',(-30.6324251188938,35.835135935805,-235.35005));
#194231=CARTESIAN_POINT('Ctrl Pts',(-30.988382838386,36.3951824447949,-235.350049999742));
#194232=CARTESIAN_POINT('Ctrl Pts',(-31.2333771101203,36.7689146204159,
-234.859578762431));
#194233=CARTESIAN_POINT('Ctrl Pts',(-32.5473006228093,34.546799247056,-235.35005));
#194234=CARTESIAN_POINT('Ctrl Pts',(-32.9234562736393,35.0863223646416,
-235.350049999872));
#194235=CARTESIAN_POINT('Ctrl Pts',(-33.1818988153925,35.4495637346705,
-234.86713813913));
#194236=CARTESIAN_POINT('Ctrl Pts',(-36.0822840599884,31.8353365675869,
-235.35005));
#194237=CARTESIAN_POINT('Ctrl Pts',(-36.4952941667597,32.3353752136231,
-235.35005000012));
#194238=CARTESIAN_POINT('Ctrl Pts',(-36.7813559352307,32.6757871555092,
-234.878086065553));
#194239=CARTESIAN_POINT('Ctrl Pts',(-37.7150530376205,30.426874953249,-235.35005));
#194240=CARTESIAN_POINT('Ctrl Pts',(-38.145619897874,30.908582788892,-235.35004999988));
#194241=CARTESIAN_POINT('Ctrl Pts',(-38.4423674553364,31.2390085277979,
-234.881236143903));
#194242=CARTESIAN_POINT('Ctrl Pts',(-40.0413171754775,28.170164696784,-235.35005));
#194243=CARTESIAN_POINT('Ctrl Pts',(-40.498678297905,28.6233702148686,-235.35005000006));
#194244=CARTESIAN_POINT('Ctrl Pts',(-40.8139548555995,28.9354139317848,
-234.883441337666));
#194245=CARTESIAN_POINT('Ctrl Pts',(-40.7957050001434,27.3932780662659,
-235.35005));
#194246=CARTESIAN_POINT('Ctrl Pts',(-41.2617903522464,27.8372407096767,
-235.35005));
#194247=CARTESIAN_POINT('Ctrl Pts',(-41.5829037502019,28.1432199774246,
-234.883656797018));
#194248=CARTESIAN_POINT('Ctrl Pts',(-42.2637158381442,25.7917312522435,
-235.35005));
#194249=CARTESIAN_POINT('Ctrl Pts',(-42.7468027345624,26.2176715878726,
-235.35005));
#194250=CARTESIAN_POINT('Ctrl Pts',(-43.079491346636,26.5111087013005,-234.883221890728));
#194251=CARTESIAN_POINT('Ctrl Pts',(-42.9787004139624,24.9654368934267,
-235.35005));
#194252=CARTESIAN_POINT('Ctrl Pts',(-43.4703807122323,25.3822490016404,
-235.35005));
#194253=CARTESIAN_POINT('Ctrl Pts',(-43.8085884283688,25.6694567559007,
-234.88257445635));
#194254=CARTESIAN_POINT('Ctrl Pts',(-45.1373606477486,22.3164313732977,
-235.35005));
#194255=CARTESIAN_POINT('Ctrl Pts',(-45.6568207031231,22.7034238305282,
-235.35005));
#194256=CARTESIAN_POINT('Ctrl Pts',(-46.0121606676539,22.9702919294327,
-234.879269810321));
#194257=CARTESIAN_POINT('Ctrl Pts',(-46.4872712478119,20.4281942415639,
-235.350050000001));
#194258=CARTESIAN_POINT('Ctrl Pts',(-47.0253273852194,20.7945808946792,
-235.350049999074));
#194259=CARTESIAN_POINT('Ctrl Pts',(-47.391560949626,21.047345630817,-234.875206256712));
#194260=CARTESIAN_POINT('Ctrl Pts',(-47.7222658457636,18.4560958919691,
-235.350050000001));
#194261=CARTESIAN_POINT('Ctrl Pts',(-48.2758175822674,18.8027406871144,
-235.350050000176));
#194262=CARTESIAN_POINT('Ctrl Pts',(-48.6529331431024,19.0388789631468,
-234.871921744022));
#194263=CARTESIAN_POINT('',(-48.4260896922586,19.3965417854656,-234.872874618363));
#194264=CARTESIAN_POINT('',(-47.5004483343782,18.8074595529612,-235.35005));
#194265=CARTESIAN_POINT('Origin',(-47.5004483343794,18.8074595529594,-233.85005));
#194266=CARTESIAN_POINT('Ctrl Pts',(-48.4260896922585,19.3965417854656,
-234.872874618363));
#194267=CARTESIAN_POINT('Ctrl Pts',(-48.2336681176016,19.6980174947172,
-234.873382411966));
#194268=CARTESIAN_POINT('Ctrl Pts',(-48.0384640363657,19.9976369248559,
-234.873904410919));
#194269=CARTESIAN_POINT('Ctrl Pts',(-47.8405525939515,20.295311591735,-234.874431710577));
#194270=CARTESIAN_POINT('Ctrl Pts',(-47.6376543543754,20.6004868011085,
-234.874972296665));
#194271=CARTESIAN_POINT('Ctrl Pts',(-47.4319106874047,20.9036183295806,
-234.875518453947));
#194272=CARTESIAN_POINT('Ctrl Pts',(-47.2233678006824,21.2046536835508,
-234.876060587562));
#194273=CARTESIAN_POINT('Ctrl Pts',(-47.0069805666097,21.5170124919834,
-234.87662311355));
#194274=CARTESIAN_POINT('Ctrl Pts',(-46.7875797475729,21.82711474811,-234.877181307477));
#194275=CARTESIAN_POINT('Ctrl Pts',(-46.5651778092407,22.1349427753502,
-234.87772445051));
#194276=CARTESIAN_POINT('Ctrl Pts',(-46.338367265686,22.4488727829,-234.878278360099));
#194277=CARTESIAN_POINT('Ctrl Pts',(-46.1084355256474,22.760437932076,-234.878816616181));
#194278=CARTESIAN_POINT('Ctrl Pts',(-45.8753539608744,23.0696556340549,
-234.879327849776));
#194279=CARTESIAN_POINT('Ctrl Pts',(-45.6359567474781,23.387251992474,-234.87985293591));
#194280=CARTESIAN_POINT('Ctrl Pts',(-45.3932368521758,23.7023723875432,
-234.880349515298));
#194281=CARTESIAN_POINT('Ctrl Pts',(-45.1471176554437,24.0150669690212,
-234.880805269517));
#194282=CARTESIAN_POINT('Ctrl Pts',(-45.0039085531397,24.1970142161412,
-234.881070458716));
#194283=CARTESIAN_POINT('Ctrl Pts',(-44.8595476865727,24.3781406979818,
-234.881321825681));
#194284=CARTESIAN_POINT('Ctrl Pts',(-44.714012850909,24.5584600979606,-234.881556943632));
#194285=CARTESIAN_POINT('Ctrl Pts',(-44.6472900780137,24.641130410663,-234.881664737217));
#194286=CARTESIAN_POINT('Ctrl Pts',(-44.580320486115,24.7236311095871,-234.881769115404));
#194287=CARTESIAN_POINT('Ctrl Pts',(-44.5131079214061,24.8059600647562,
-234.881869844336));
#194288=CARTESIAN_POINT('Ctrl Pts',(-44.2745002008715,25.0982316721848,
-234.882227436712));
#194289=CARTESIAN_POINT('Ctrl Pts',(-44.0330777967232,25.3880385557821,
-234.882538122664));
#194290=CARTESIAN_POINT('Ctrl Pts',(-43.7890811769961,25.6752036410983,
-234.88280110814));
#194291=CARTESIAN_POINT('Ctrl Pts',(-43.5336383710576,25.975839999269,-234.883076430592));
#194292=CARTESIAN_POINT('Ctrl Pts',(-43.2753741805736,26.2735811812503,
-234.883299472219));
#194293=CARTESIAN_POINT('Ctrl Pts',(-43.0145135093598,26.5682532856333,
-234.883469321896));
#194294=CARTESIAN_POINT('Ctrl Pts',(-42.7885691451028,26.8234834089756,
-234.883616437124));
#194295=CARTESIAN_POINT('Ctrl Pts',(-42.5606759082898,27.0764117290122,
-234.883723646947));
#194296=CARTESIAN_POINT('Ctrl Pts',(-42.3309515524768,27.3269388059103,
-234.883790359317));
#194297=CARTESIAN_POINT('Ctrl Pts',(-42.0612872616582,27.6210225841997,
-234.883868670318));
#194298=CARTESIAN_POINT('Ctrl Pts',(-41.7889144466608,27.9120032296393,
-234.883890797532));
#194299=CARTESIAN_POINT('Ctrl Pts',(-41.5138321388492,28.1998649984553,
-234.883852686351));
#194300=CARTESIAN_POINT('Ctrl Pts',(-41.2299540147919,28.4969312095447,
-234.883813356558));
#194301=CARTESIAN_POINT('Ctrl Pts',(-40.9431900644798,28.7906768036788,
-234.88370987451));
#194302=CARTESIAN_POINT('Ctrl Pts',(-40.6534840262211,29.0810776426265,
-234.883537784092));
#194303=CARTESIAN_POINT('Ctrl Pts',(-40.4729316819002,29.262063004823,-234.883430532864));
#194304=CARTESIAN_POINT('Ctrl Pts',(-40.2912355238482,29.4417490417126,
-234.883296633411));
#194305=CARTESIAN_POINT('Ctrl Pts',(-40.1083724339856,29.6201262193833,
-234.883135007052));
#194306=CARTESIAN_POINT('Ctrl Pts',(-40.0800074003628,29.6477954152061,
-234.88310993618));
#194307=CARTESIAN_POINT('Ctrl Pts',(-40.051614276085,29.6754331110842,-234.88308419817));
#194308=CARTESIAN_POINT('Ctrl Pts',(-40.0231931536369,29.7030394061776,
-234.883057788995));
#194309=CARTESIAN_POINT('Ctrl Pts',(-39.7383427980406,29.9797231644769,
-234.882793103363));
#194310=CARTESIAN_POINT('Ctrl Pts',(-39.4508577652458,30.2530692798036,
-234.882473924431));
#194311=CARTESIAN_POINT('Ctrl Pts',(-39.1607632606661,30.5232243371498,
-234.882097470483));
#194312=CARTESIAN_POINT('Ctrl Pts',(-38.8687717624806,30.7951459995445,
-234.881718554817));
#194313=CARTESIAN_POINT('Ctrl Pts',(-38.5741356572691,31.0638353734139,
-234.881281612617));
#194314=CARTESIAN_POINT('Ctrl Pts',(-38.2768465821868,31.3294021629668,
-234.88078380724));
#194315=CARTESIAN_POINT('Ctrl Pts',(-37.9875650741985,31.5878158343478,
-234.880299410394));
#194316=CARTESIAN_POINT('Ctrl Pts',(-37.6957706557468,31.8432732365712,
-234.879757384948));
#194317=CARTESIAN_POINT('Ctrl Pts',(-37.401437189756,32.0958308802778,-234.879155117356));
#194318=CARTESIAN_POINT('Ctrl Pts',(-37.115266360764,32.3413844398245,-234.87856955222));
#194319=CARTESIAN_POINT('Ctrl Pts',(-36.8266945892579,32.5841971463957,
-234.877927039951));
#194320=CARTESIAN_POINT('Ctrl Pts',(-36.5356924808088,32.824273442989,-234.877225178471));
#194321=CARTESIAN_POINT('Ctrl Pts',(-36.2588701791423,33.0526514205671,
-234.876557516949));
#194322=CARTESIAN_POINT('Ctrl Pts',(-35.9798480396065,33.2785532299222,
-234.875836149178));
#194323=CARTESIAN_POINT('Ctrl Pts',(-35.6986053783016,33.5019368424606,
-234.875059007386));
#194324=CARTESIAN_POINT('Ctrl Pts',(-35.4793033421191,33.6761226535753,
-234.874453022588));
#194325=CARTESIAN_POINT('Ctrl Pts',(-35.2586511672865,33.8487765152758,
-234.873813125676));
#194326=CARTESIAN_POINT('Ctrl Pts',(-35.0366444584247,34.0198570237832,
-234.873138336286));
#194327=CARTESIAN_POINT('Ctrl Pts',(-34.9904940629195,34.0554209631404,
-234.87299806216));
#194328=CARTESIAN_POINT('Ctrl Pts',(-34.9442874985273,34.0909146676626,
-234.872856601922));
#194329=CARTESIAN_POINT('Ctrl Pts',(-34.8980249060694,34.1263375479426,
-234.872713978188));
#194330=CARTESIAN_POINT('Ctrl Pts',(-34.5916777753735,34.3609049847902,
-234.871769535396));
#194331=CARTESIAN_POINT('Ctrl Pts',(-34.2828722423169,34.5923705644,-234.870774073449));
#194332=CARTESIAN_POINT('Ctrl Pts',(-33.971520157457,34.8208350455687,-234.869734158406));
#194333=CARTESIAN_POINT('Ctrl Pts',(-33.6669144793353,35.0443491365196,
-234.868716776342));
#194334=CARTESIAN_POINT('Ctrl Pts',(-33.359870956103,35.2649906993816,-234.867656846737));
#194335=CARTESIAN_POINT('Ctrl Pts',(-33.0503299156795,35.4828099737801,
-234.866560518012));
#194336=CARTESIAN_POINT('Ctrl Pts',(-32.752262989056,35.6925550905844,-234.865504828164));
#194337=CARTESIAN_POINT('Ctrl Pts',(-32.4518799457129,35.8996831079268,
-234.864415387677));
#194338=CARTESIAN_POINT('Ctrl Pts',(-32.1491544499317,36.1041994670095,
-234.863297686268));
#194339=CARTESIAN_POINT('Ctrl Pts',(-31.8529815111427,36.3042890265084,
-234.862204177742));
#194340=CARTESIAN_POINT('Ctrl Pts',(-31.5545660682366,36.5018787132748,
-234.861083618481));
#194341=CARTESIAN_POINT('Ctrl Pts',(-31.2539148013445,36.696936587115,-234.859941149384));
#194342=CARTESIAN_POINT('Ctrl Pts',(-30.9639839854485,36.8850391988021,
-234.858839417798));
#194343=CARTESIAN_POINT('Ctrl Pts',(-30.6719737130795,37.0707872104706,
-234.857717311017));
#194344=CARTESIAN_POINT('Ctrl Pts',(-30.3779236186945,37.2541185543487,
-234.856579439382));
#194345=CARTESIAN_POINT('Ctrl Pts',(-30.1045036246594,37.4245876543653,
-234.855521399064));
#194346=CARTESIAN_POINT('Ctrl Pts',(-29.8293200171223,37.5929670251938,
-234.854449728371));
#194347=CARTESIAN_POINT('Ctrl Pts',(-29.5524353619882,37.7591803693088,
-234.853368133768));
#194348=CARTESIAN_POINT('Ctrl Pts',(-28.9814172171126,36.8014272692485,
-235.35005));
#194349=CARTESIAN_POINT('Ctrl Pts',(-30.4445221387403,35.9291153361899,
-235.35005));
#194350=CARTESIAN_POINT('Ctrl Pts',(-31.8571523563207,34.9976505207191,
-235.35005));
#194351=CARTESIAN_POINT('Ctrl Pts',(-33.2197493322593,34.0075501952557,
-235.35005));
#194352=CARTESIAN_POINT('Ctrl Pts',(-33.6068768507121,33.7262527252154,
-235.35005));
#194353=CARTESIAN_POINT('Ctrl Pts',(-33.9899655501571,33.4402220370472,
-235.35005));
#194354=CARTESIAN_POINT('Ctrl Pts',(-34.3690250580976,33.1494694133448,
-235.35005));
#194355=CARTESIAN_POINT('Ctrl Pts',(-36.0822840600053,31.8353365675737,
-235.35005));
#194356=CARTESIAN_POINT('Ctrl Pts',(-37.7150530376344,30.4268749532356,
-235.35005));
#194357=CARTESIAN_POINT('Ctrl Pts',(-39.2658957962434,28.9224014489936,
-235.35005));
#194358=CARTESIAN_POINT('Ctrl Pts',(-40.0413171755479,28.1701646968727,
-235.35005));
#194359=CARTESIAN_POINT('Ctrl Pts',(-40.7957050001266,27.3932780662842,
-235.35005));
#194360=CARTESIAN_POINT('Ctrl Pts',(-41.52971041916,26.5925046592713,-235.35005));
#194361=CARTESIAN_POINT('Ctrl Pts',(-42.2637158381934,25.7917312522584,
-235.35005));
#194362=CARTESIAN_POINT('Ctrl Pts',(-42.9787004139405,24.9654368934535,
-235.35005));
#194363=CARTESIAN_POINT('Ctrl Pts',(-43.669114034758,24.1181940231093,-235.35005));
#194364=CARTESIAN_POINT('Ctrl Pts',(-45.0499412763931,22.423708282421,-235.35005));
#194365=CARTESIAN_POINT('Ctrl Pts',(-46.3260905825898,20.6527606745438,
-235.350050000001));
#194366=CARTESIAN_POINT('Ctrl Pts',(-47.5004483343782,18.8074595529613,
-235.350050000001));
#194367=CARTESIAN_POINT('Ctrl Pts',(-47.5004483343777,18.8074595529617,
-235.35005));
#194368=CARTESIAN_POINT('Ctrl Pts',(-48.0508084453082,19.1577111488619,
-235.35005));
#194369=CARTESIAN_POINT('Ctrl Pts',(-48.4260896922579,19.3965417854669,
-234.872874618363));
#194370=CARTESIAN_POINT('Ctrl Pts',(-47.5233281555475,18.7715078669293,
-235.35005));
#194371=CARTESIAN_POINT('Ctrl Pts',(-48.0771976901895,19.1185775087876,
-235.350049999978));
#194372=CARTESIAN_POINT('Ctrl Pts',(-48.4542924222552,19.3549004456767,
-234.871334334863));
#194373=CARTESIAN_POINT('Ctrl Pts',(-47.5458232280531,18.7353573183218,
-235.35005));
#194374=CARTESIAN_POINT('Ctrl Pts',(-48.1039998334649,19.0785250138959,
-235.350050000005));
#194375=CARTESIAN_POINT('Ctrl Pts',(-48.4833024022839,19.3117585055263,
-234.869397699979));
#194376=CARTESIAN_POINT('Ctrl Pts',(-47.5895300323829,18.6623978031499,
-235.35005));
#194377=CARTESIAN_POINT('Ctrl Pts',(-48.1593257378831,18.9948843873186,
-235.350049999995));
#194378=CARTESIAN_POINT('Ctrl Pts',(-48.5444255909505,19.2196347103286,
-234.863872863852));
#194379=CARTESIAN_POINT('Ctrl Pts',(-47.6106972731343,18.625565406903,-235.35005));
#194380=CARTESIAN_POINT('Ctrl Pts',(-48.1884776688448,18.9506324984654,
-235.350050000003));
#194381=CARTESIAN_POINT('Ctrl Pts',(-48.5774448328292,19.1695186218693,
-234.85990679963));
#194382=CARTESIAN_POINT('Ctrl Pts',(-47.6410934853577,18.569620618322,-235.35005));
#194383=CARTESIAN_POINT('Ctrl Pts',(-48.229986112641,18.8839741987186,-235.350049999998));
#194384=CARTESIAN_POINT('Ctrl Pts',(-48.6241839653041,19.0944106548932,
-234.85414296838));
#194385=CARTESIAN_POINT('Ctrl Pts',(-47.6510095952452,18.550861366784,-235.35005));
#194386=CARTESIAN_POINT('Ctrl Pts',(-48.2431911415777,18.8619616358506,
-235.350049999998));
#194387=CARTESIAN_POINT('Ctrl Pts',(-48.638908043659,19.069857746375,-234.852410933521));
#194388=CARTESIAN_POINT('Ctrl Pts',(-47.6705745922183,18.513205530003,-235.35005));
#194389=CARTESIAN_POINT('Ctrl Pts',(-48.2671819452163,18.8197560443254,
-235.350050000002));
#194390=CARTESIAN_POINT('Ctrl Pts',(-48.6649527674787,19.024147533775,-234.850139144187));
#194391=CARTESIAN_POINT('Ctrl Pts',(-47.6802441619202,18.4943195741576,
-235.35005));
#194392=CARTESIAN_POINT('Ctrl Pts',(-48.2778090546859,18.799757048935,-235.350050000001));
#194393=CARTESIAN_POINT('Ctrl Pts',(-48.6760466930021,19.003315780373,-234.84970575966));
#194394=CARTESIAN_POINT('Ctrl Pts',(-47.7090490788398,18.4375569718045,
-235.35005));
#194395=CARTESIAN_POINT('Ctrl Pts',(-48.310705894182,18.7384640963053,-235.350049999999));
#194396=CARTESIAN_POINT('Ctrl Pts',(-48.7108682070929,18.9386166159486,
-234.847719038782));
#194397=CARTESIAN_POINT('Ctrl Pts',(-47.7279282401082,18.3995486637502,
-235.35005));
#194398=CARTESIAN_POINT('Ctrl Pts',(-48.3327596867691,18.6969547523118,
-235.350050000006));
#194399=CARTESIAN_POINT('Ctrl Pts',(-48.7343909692929,18.8944723982682,
-234.846132537133));
#194400=CARTESIAN_POINT('Ctrl Pts',(-47.7647487546851,18.3230500802882,
-235.35005));
#194401=CARTESIAN_POINT('Ctrl Pts',(-48.3775414056939,18.6116695818104,
-235.350049999994));
#194402=CARTESIAN_POINT('Ctrl Pts',(-48.7827487476233,18.8025467359427,
-234.841945226815));
#194403=CARTESIAN_POINT('Ctrl Pts',(-47.7827001660699,18.2845649741211,
-235.35005));
#194404=CARTESIAN_POINT('Ctrl Pts',(-48.4004562638174,18.5677247892466,
-235.350050000015));
#194405=CARTESIAN_POINT('Ctrl Pts',(-48.8078323528047,18.7544974911258,
-234.839249257519));
#194406=CARTESIAN_POINT('Ctrl Pts',(-47.81709615277,18.2068203539689,-235.35005));
#194407=CARTESIAN_POINT('Ctrl Pts',(-48.4474727822696,18.4757807159189,
-235.350049999985));
#194408=CARTESIAN_POINT('Ctrl Pts',(-48.8601288350238,18.6518909794679,
-234.832008606249));
#194409=CARTESIAN_POINT('Ctrl Pts',(-47.8335233281929,18.1675458631259,
-235.35005));
#194410=CARTESIAN_POINT('Ctrl Pts',(-48.4700885563297,18.4292216092512,
-235.350049999999));
#194411=CARTESIAN_POINT('Ctrl Pts',(-48.8852514246585,18.5999224430555,
-234.828363590487));
#194412=CARTESIAN_POINT('Ctrl Pts',(-47.8650504941538,18.0883394728593,
-235.35005));
#194413=CARTESIAN_POINT('Ctrl Pts',(-48.5118155154303,18.3374118427688,
-235.350050000001));
#194414=CARTESIAN_POINT('Ctrl Pts',(-48.931027462954,18.4988900212735,-234.822325836545));
#194415=CARTESIAN_POINT('Ctrl Pts',(-47.8801543850424,18.0485058523287,
-235.35005));
#194416=CARTESIAN_POINT('Ctrl Pts',(-48.530298509796,18.2930230307278,-235.350050000003));
#194417=CARTESIAN_POINT('Ctrl Pts',(-48.9508554755667,18.4512226738463,
-234.820369930511));
#194418=CARTESIAN_POINT('Ctrl Pts',(-47.9094666156693,17.9685258021276,
-235.35005));
#194419=CARTESIAN_POINT('Ctrl Pts',(-48.5670290414783,18.203228539971,-235.350049999996));
#194420=CARTESIAN_POINT('Ctrl Pts',(-48.990407903663,18.3543737889356,-234.815860390008));
#194421=CARTESIAN_POINT('Ctrl Pts',(-47.9236194657386,17.9283599903447,
-235.35005));
#194422=CARTESIAN_POINT('Ctrl Pts',(-48.5855270232061,18.1574071922804,
-235.350050000007));
#194423=CARTESIAN_POINT('Ctrl Pts',(-49.0104806988515,18.3045019253958,
-234.813092565269));
#194424=CARTESIAN_POINT('Ctrl Pts',(-47.9505381729848,17.8475439007782,
-235.35005));
#194425=CARTESIAN_POINT('Ctrl Pts',(-48.6229814684107,18.062872852205,-235.350049999994));
#194426=CARTESIAN_POINT('Ctrl Pts',(-49.0515011390314,18.2001358516365,
-234.805958241058));
#194427=CARTESIAN_POINT('Ctrl Pts',(-47.9632560597789,17.8068666429648,
-235.35005));
#194428=CARTESIAN_POINT('Ctrl Pts',(-48.6424408675579,18.0133995657985,
-235.350050000009));
#194429=CARTESIAN_POINT('Ctrl Pts',(-49.0730847555093,18.14440457461,-234.80115919183));
#194430=CARTESIAN_POINT('Ctrl Pts',(-47.9870034052699,17.7249653914156,
-235.35005));
#194431=CARTESIAN_POINT('Ctrl Pts',(-48.6779790062891,17.915615235708,-235.350049999991));
#194432=CARTESIAN_POINT('Ctrl Pts',(-49.112076978178,18.0354393113711,-234.792427668388));
#194433=CARTESIAN_POINT('Ctrl Pts',(-47.9980630400304,17.6838206475214,
-235.35005));
#194434=CARTESIAN_POINT('Ctrl Pts',(-48.6943197391833,17.8671438309789,
-235.35005000001));
#194435=CARTESIAN_POINT('Ctrl Pts',(-49.1298441237351,17.981860251528,-234.788349296066));
#194436=CARTESIAN_POINT('Ctrl Pts',(-48.0189197776842,17.6012300921137,
-235.35005));
#194437=CARTESIAN_POINT('Ctrl Pts',(-48.7242285116606,17.771770777776,-235.35004999999));
#194438=CARTESIAN_POINT('Ctrl Pts',(-49.162044625621,17.8776762330174,-234.781180866063));
#194439=CARTESIAN_POINT('Ctrl Pts',(-48.0287613458656,17.5597948840364,
-235.35005));
#194440=CARTESIAN_POINT('Ctrl Pts',(-48.7384179936011,17.7241346288096,
-235.350049999995));
#194441=CARTESIAN_POINT('Ctrl Pts',(-49.1772563366924,17.8258110055907,
-234.777634115965));
#194442=CARTESIAN_POINT('Ctrl Pts',(-48.0470227250193,17.4765854309817,
-235.35005));
#194443=CARTESIAN_POINT('Ctrl Pts',(-48.7670952112289,17.6259226184369,
-235.350050000005));
#194444=CARTESIAN_POINT('Ctrl Pts',(-49.2081218683014,17.7174394526145,
-234.76877506552));
#194445=CARTESIAN_POINT('Ctrl Pts',(-48.0554329780656,17.4347916601489,
-235.35005));
#194446=CARTESIAN_POINT('Ctrl Pts',(-48.7812919042116,17.5756645037128,
-235.350050000005));
#194447=CARTESIAN_POINT('Ctrl Pts',(-49.2234010254764,17.6615278352864,
-234.763682646456));
#194448=CARTESIAN_POINT('Ctrl Pts',(-48.0705953135359,17.3508835165529,
-235.35005));
#194449=CARTESIAN_POINT('Ctrl Pts',(-48.808104677187,17.4743257669527,-235.350049999995));
#194450=CARTESIAN_POINT('Ctrl Pts',(-49.2520548027181,17.5486925247621,
-234.75299425464));
#194451=CARTESIAN_POINT('Ctrl Pts',(-48.0773499548877,17.3088369763077,
-235.350050000001));
#194452=CARTESIAN_POINT('Ctrl Pts',(-48.8202836830788,17.4239614927865,
-235.35005));
#194453=CARTESIAN_POINT('Ctrl Pts',(-49.2649325810603,17.4929198622924,
-234.747809920555));
#194454=CARTESIAN_POINT('Ctrl Pts',(-48.0894592880343,17.2245872750773,
-235.350050000001));
#194455=CARTESIAN_POINT('Ctrl Pts',(-48.8422242267331,17.3243377880475,
-235.35005));
#194456=CARTESIAN_POINT('Ctrl Pts',(-49.2879043244386,17.3834514853175,
-234.738139816296));
#194457=CARTESIAN_POINT('Ctrl Pts',(-48.094834615712,17.1823864227582,-235.35005));
#194458=CARTESIAN_POINT('Ctrl Pts',(-48.8514819375229,17.2759479237276,
-235.350050000014));
#194459=CARTESIAN_POINT('Ctrl Pts',(-49.2974763354349,17.3311532118177,
-234.734202664179));
#194460=CARTESIAN_POINT('Ctrl Pts',(-48.1091464500575,17.0555809060241,
-235.35005));
#194461=CARTESIAN_POINT('Ctrl Pts',(-48.8799935741974,17.1259395893774,
-235.350049999972));
#194462=CARTESIAN_POINT('Ctrl Pts',(-49.3267656585904,17.1669449229297,
-234.719429103118));
#194463=CARTESIAN_POINT('Ctrl Pts',(-48.1154436500424,16.9706923807857,
-235.350050000001));
#194464=CARTESIAN_POINT('Ctrl Pts',(-48.8997687328372,17.016853275791,-235.35004999989));
#194465=CARTESIAN_POINT('Ctrl Pts',(-49.3465478480362,17.0432452943168,
-234.704309415519));
#194466=CARTESIAN_POINT('Ctrl Pts',(-48.1189208895433,16.8854655414009,
-235.350050000001));
#194467=CARTESIAN_POINT('Ctrl Pts',(-48.9115061644414,16.9178030353161,
-235.350050000001));
#194468=CARTESIAN_POINT('Ctrl Pts',(-49.3576635057813,16.9360062631172,
-234.694420988468));
#194469=CARTESIAN_POINT('',(-49.3576635057812,16.9360062631145,-234.694420988467));
#194470=CARTESIAN_POINT('',(-48.1189208895436,16.8854655414,-235.35005));
#194471=CARTESIAN_POINT('Origin',(-48.1189208895436,16.8854655414,-233.85005));
#194472=CARTESIAN_POINT('Ctrl Pts',(-49.3576635057812,16.9360062631145,
-234.694420988467));
#194473=CARTESIAN_POINT('Ctrl Pts',(-49.3465478480362,17.0432452943168,
-234.704309415519));
#194474=CARTESIAN_POINT('Ctrl Pts',(-49.3267656585904,17.1669449229297,
-234.719429103118));
#194475=CARTESIAN_POINT('Ctrl Pts',(-49.2974763354349,17.3311532118177,
-234.734202664179));
#194476=CARTESIAN_POINT('Ctrl Pts',(-49.2879043244386,17.3834514853175,
-234.738139816296));
#194477=CARTESIAN_POINT('Ctrl Pts',(-49.2649325810603,17.4929198622924,
-234.747809920555));
#194478=CARTESIAN_POINT('Ctrl Pts',(-49.2520548027181,17.5486925247621,
-234.75299425464));
#194479=CARTESIAN_POINT('Ctrl Pts',(-49.2234010254764,17.6615278352864,
-234.763682646456));
#194480=CARTESIAN_POINT('Ctrl Pts',(-49.2081218683014,17.7174394526145,
-234.76877506552));
#194481=CARTESIAN_POINT('Ctrl Pts',(-49.1772563366924,17.8258110055907,
-234.777634115965));
#194482=CARTESIAN_POINT('Ctrl Pts',(-49.162044625621,17.8776762330174,-234.781180866063));
#194483=CARTESIAN_POINT('Ctrl Pts',(-49.1298441237351,17.981860251528,-234.788349296066));
#194484=CARTESIAN_POINT('Ctrl Pts',(-49.112076978178,18.0354393113711,-234.792427668388));
#194485=CARTESIAN_POINT('Ctrl Pts',(-49.0730847555093,18.14440457461,-234.80115919183));
#194486=CARTESIAN_POINT('Ctrl Pts',(-49.0515011390314,18.2001358516365,
-234.805958241058));
#194487=CARTESIAN_POINT('Ctrl Pts',(-49.0104806988515,18.3045019253958,
-234.813092565269));
#194488=CARTESIAN_POINT('Ctrl Pts',(-48.990407903663,18.3543737889356,-234.815860390008));
#194489=CARTESIAN_POINT('Ctrl Pts',(-48.9508554755667,18.4512226738463,
-234.820369930511));
#194490=CARTESIAN_POINT('Ctrl Pts',(-48.931027462954,18.4988900212735,-234.822325836545));
#194491=CARTESIAN_POINT('Ctrl Pts',(-48.8852514246585,18.5999224430555,
-234.828363590487));
#194492=CARTESIAN_POINT('Ctrl Pts',(-48.8601288350238,18.6518909794679,
-234.832008606249));
#194493=CARTESIAN_POINT('Ctrl Pts',(-48.8078323528047,18.7544974911258,
-234.839249257519));
#194494=CARTESIAN_POINT('Ctrl Pts',(-48.7827487476233,18.8025467359427,
-234.841945226815));
#194495=CARTESIAN_POINT('Ctrl Pts',(-48.7343909692929,18.8944723982682,
-234.846132537133));
#194496=CARTESIAN_POINT('Ctrl Pts',(-48.7108682070929,18.9386166159486,
-234.847719038782));
#194497=CARTESIAN_POINT('Ctrl Pts',(-48.6760466930021,19.003315780373,-234.84970575966));
#194498=CARTESIAN_POINT('Ctrl Pts',(-48.6649527674787,19.024147533775,-234.850139144187));
#194499=CARTESIAN_POINT('Ctrl Pts',(-48.638908043659,19.069857746375,-234.852410933521));
#194500=CARTESIAN_POINT('Ctrl Pts',(-48.6241839653041,19.0944106548932,
-234.85414296838));
#194501=CARTESIAN_POINT('Ctrl Pts',(-48.5774448328292,19.1695186218693,
-234.85990679963));
#194502=CARTESIAN_POINT('Ctrl Pts',(-48.5444255909505,19.2196347103286,
-234.863872863852));
#194503=CARTESIAN_POINT('Ctrl Pts',(-48.4833024022839,19.3117585055263,
-234.869397699979));
#194504=CARTESIAN_POINT('Ctrl Pts',(-48.4542924222552,19.3549004456767,
-234.871334334863));
#194505=CARTESIAN_POINT('Ctrl Pts',(-48.4260896922586,19.3965417854656,
-234.872874618363));
#194506=CARTESIAN_POINT('Ctrl Pts',(-47.5004483343782,18.8074595529612,
-235.35005));
#194507=CARTESIAN_POINT('Ctrl Pts',(-47.523328218883,18.7715077674088,-235.35005));
#194508=CARTESIAN_POINT('Ctrl Pts',(-47.5458232845143,18.7353572240715,
-235.35005));
#194509=CARTESIAN_POINT('Ctrl Pts',(-47.5676766302509,18.6988775607556,
-235.35005));
#194510=CARTESIAN_POINT('Ctrl Pts',(-47.5895300808456,18.6623977224007,
-235.35005));
#194511=CARTESIAN_POINT('Ctrl Pts',(-47.6106973144047,18.6255653312655,
-235.35005));
#194512=CARTESIAN_POINT('Ctrl Pts',(-47.6309614148883,18.58826888133,-235.35005));
#194513=CARTESIAN_POINT('Ctrl Pts',(-47.6410934945813,18.5696206021569,
-235.35005));
#194514=CARTESIAN_POINT('Ctrl Pts',(-47.6510096037987,18.5508613513732,
-235.35005));
#194515=CARTESIAN_POINT('Ctrl Pts',(-47.6607920942703,18.5320334486734,
-235.35005));
#194516=CARTESIAN_POINT('Ctrl Pts',(-47.6705746000884,18.513205516437,-235.35005));
#194517=CARTESIAN_POINT('Ctrl Pts',(-47.6802441693448,18.4943195614609,
-235.35005));
#194518=CARTESIAN_POINT('Ctrl Pts',(-47.6898458018307,18.4753987071822,
-235.35005));
#194519=CARTESIAN_POINT('Ctrl Pts',(-47.70904910136,18.4375569305264,-235.35005));
#194520=CARTESIAN_POINT('Ctrl Pts',(-47.7279282587774,18.3995486292809,
-235.35005));
#194521=CARTESIAN_POINT('Ctrl Pts',(-47.7463384996528,18.3612993731052,
-235.35005));
#194522=CARTESIAN_POINT('Ctrl Pts',(-47.7647487677154,18.323050060445,-235.35005));
#194523=CARTESIAN_POINT('Ctrl Pts',(-47.7827001759863,18.2845649614141,
-235.35005));
#194524=CARTESIAN_POINT('Ctrl Pts',(-47.7998981639292,18.24569266604,-235.35005));
#194525=CARTESIAN_POINT('Ctrl Pts',(-47.8170961582275,18.2068203563009,
-235.35005));
#194526=CARTESIAN_POINT('Ctrl Pts',(-47.8335233318918,18.1675458731571,
-235.35005));
#194527=CARTESIAN_POINT('Ctrl Pts',(-47.8492869191686,18.127942671175,-235.35005));
#194528=CARTESIAN_POINT('Ctrl Pts',(-47.8650504948173,18.0883394984066,
-235.35005));
#194529=CARTESIAN_POINT('Ctrl Pts',(-47.8801543852333,18.0485058859946,
-235.35005));
#194530=CARTESIAN_POINT('Ctrl Pts',(-47.8948105132744,18.0085158319627,
-235.35005));
#194531=CARTESIAN_POINT('Ctrl Pts',(-47.909466614277,17.9685258517065,-235.35005));
#194532=CARTESIAN_POINT('Ctrl Pts',(-47.9236194654021,17.9283600484622,
-235.35005));
#194533=CARTESIAN_POINT('Ctrl Pts',(-47.9370788390041,17.887951952103,-235.35005));
#194534=CARTESIAN_POINT('Ctrl Pts',(-47.9505379989423,17.847544497211,-235.35005));
#194535=CARTESIAN_POINT('Ctrl Pts',(-47.9632559353684,17.8068671621608,
-235.35005));
#194536=CARTESIAN_POINT('Ctrl Pts',(-47.9751297575526,17.7659160244471,
-235.35005));
#194537=CARTESIAN_POINT('Ctrl Pts',(-47.9870033323709,17.7249657398638,
-235.35005));
#194538=CARTESIAN_POINT('Ctrl Pts',(-47.9980630011651,17.6838209125432,
-235.35005));
#194539=CARTESIAN_POINT('Ctrl Pts',(-48.0084914348375,17.6425253763784,
-235.35005));
#194540=CARTESIAN_POINT('Ctrl Pts',(-48.0189197816014,17.6012301843623,
-235.35005));
#194541=CARTESIAN_POINT('Ctrl Pts',(-48.0287613705984,17.5597948897797,
-235.35005));
#194542=CARTESIAN_POINT('Ctrl Pts',(-48.0378920589035,17.5181901626578,
-235.35005));
#194543=CARTESIAN_POINT('Ctrl Pts',(-48.0470227852353,17.4765852622638,
-235.35005));
#194544=CARTESIAN_POINT('Ctrl Pts',(-48.0554330459596,17.4347914019545,
-235.35005));
#194545=CARTESIAN_POINT('Ctrl Pts',(-48.063014164453,17.3928375917214,-235.35005));
#194546=CARTESIAN_POINT('Ctrl Pts',(-48.0705954092764,17.3508830823798,
-235.35005));
#194547=CARTESIAN_POINT('Ctrl Pts',(-48.0773500452528,17.3088364520712,
-235.350050000001));
#194548=CARTESIAN_POINT('Ctrl Pts',(-48.0834046340598,17.2667121275033,
-235.350050000001));
#194549=CARTESIAN_POINT('Ctrl Pts',(-48.0894593994455,17.2245865744039,
-235.350050000001));
#194550=CARTESIAN_POINT('Ctrl Pts',(-48.0948347135637,17.1823856312802,
-235.35005));
#194551=CARTESIAN_POINT('Ctrl Pts',(-48.0996052337066,17.140117917919,-235.35005));
#194552=CARTESIAN_POINT('Ctrl Pts',(-48.1091469299998,17.0555766788456,
-235.35005));
#194553=CARTESIAN_POINT('Ctrl Pts',(-48.115443852909,16.9706874085479,-235.350050000001));
#194554=CARTESIAN_POINT('Ctrl Pts',(-48.1189208895436,16.885465541401,-235.350050000001));
#194555=CARTESIAN_POINT('Ctrl Pts',(-48.1189208895436,16.8854655414,-235.35005));
#194556=CARTESIAN_POINT('Ctrl Pts',(-48.9115061644421,16.9178030353144,
-235.35005));
#194557=CARTESIAN_POINT('Ctrl Pts',(-49.357663505782,16.9360062631151,-234.694420988466));
#194558=CARTESIAN_POINT('Ctrl Pts',(-48.2232158057592,14.3292187542857,
-235.35005));
#194559=CARTESIAN_POINT('Ctrl Pts',(-49.0175817386228,14.3575637238871,
-235.350050000391));
#194560=CARTESIAN_POINT('Ctrl Pts',(-49.4635649335608,14.3752531202943,
-234.692333873014));
#194561=CARTESIAN_POINT('Ctrl Pts',(-48.3134219778347,11.7724738102799,
-235.35005));
#194562=CARTESIAN_POINT('Ctrl Pts',(-49.1092649251398,11.7982892962054,
-235.350049999822));
#194563=CARTESIAN_POINT('Ctrl Pts',(-49.5551530156078,11.8140213189959,
-234.690527234957));
#194564=CARTESIAN_POINT('Ctrl Pts',(-48.3895556141632,9.21523338364434,
-235.35005));
#194565=CARTESIAN_POINT('Ctrl Pts',(-49.1866080561977,9.23896306516062,
-235.35005));
#194566=CARTESIAN_POINT('Ctrl Pts',(-49.6324230235364,9.25223577675678,
-234.689044294154));
#194567=CARTESIAN_POINT('',(-49.6324230236214,9.25223577621558,-234.689044294051));
#194568=CARTESIAN_POINT('',(-48.3895556141631,9.21523338364434,-235.35005));
#194569=CARTESIAN_POINT('Origin',(-48.3895556141631,9.21523338364435,-233.85005));
#194570=CARTESIAN_POINT('Origin',(637.557461367465,-11.4839373498759,-249.18849675272));
#194571=CARTESIAN_POINT('Origin',(648.115804222845,-11.5202125233637,-235.35005));
#194572=CARTESIAN_POINT('Ctrl Pts',(-48.3895556141631,9.21523338364434,
-235.35005));
#194573=CARTESIAN_POINT('Ctrl Pts',(-49.1866080561976,9.2389630651606,-235.35005));
#194574=CARTESIAN_POINT('Ctrl Pts',(-49.6324230235363,9.25223577675675,
-234.689044294154));
#194575=CARTESIAN_POINT('Ctrl Pts',(-48.3941977967819,9.05930695550865,
-235.35005));
#194576=CARTESIAN_POINT('Ctrl Pts',(-49.2342501491402,9.001739953271,-235.35005));
#194577=CARTESIAN_POINT('Ctrl Pts',(-49.6757365198119,8.97285489239317,
-234.637202259114));
#194578=CARTESIAN_POINT('Ctrl Pts',(-48.3758516795198,8.90558680151918,
-235.35005));
#194579=CARTESIAN_POINT('Ctrl Pts',(-49.2516340201201,8.76786001619219,
-235.35005));
#194580=CARTESIAN_POINT('Ctrl Pts',(-49.6780275597748,8.70253397403411,
-234.577829926993));
#194581=CARTESIAN_POINT('Ctrl Pts',(-48.3395182384273,8.75410525715266,
-235.35005));
#194582=CARTESIAN_POINT('Ctrl Pts',(-49.2471092638204,8.53641604164419,
-235.35005));
#194583=CARTESIAN_POINT('Ctrl Pts',(-49.6480781836462,8.44024209637809,
-234.512742074857));
#194584=CARTESIAN_POINT('',(-49.6480781836462,8.4402420963781,-234.512742074857));
#194585=CARTESIAN_POINT('',(-48.3395182384274,8.75410525715259,-235.35005));
#194586=CARTESIAN_POINT('Origin',(-48.3395182384273,8.75410525715261,-233.85005));
#194587=CARTESIAN_POINT('Ctrl Pts',(-49.6480781836462,8.44024209637808,
-234.512742074857));
#194588=CARTESIAN_POINT('Ctrl Pts',(-49.6780275597748,8.70253397403411,
-234.577829926993));
#194589=CARTESIAN_POINT('Ctrl Pts',(-49.6757365198119,8.97285489239317,
-234.637202259114));
#194590=CARTESIAN_POINT('Ctrl Pts',(-49.6324230235363,9.25223577675679,
-234.689044294154));
#194591=CARTESIAN_POINT('Ctrl Pts',(-48.3895556141631,9.21523338364434,
-235.35005));
#194592=CARTESIAN_POINT('Ctrl Pts',(-48.3942007072891,9.05921010043768,
-235.35005));
#194593=CARTESIAN_POINT('Ctrl Pts',(-48.3758739100739,8.90567951512196,
-235.35005));
#194594=CARTESIAN_POINT('Ctrl Pts',(-48.3395182384274,8.75410525715259,
-235.35005));
#194595=CARTESIAN_POINT('Ctrl Pts',(-48.3395182384273,8.75410525715258,
-235.35005));
#194596=CARTESIAN_POINT('Ctrl Pts',(-49.2472715290903,8.53637712169199,
-235.35005));
#194597=CARTESIAN_POINT('Ctrl Pts',(-49.6481815209496,8.44021731052644,
-234.512526241039));
#194598=CARTESIAN_POINT('Ctrl Pts',(-48.1420785222883,7.9309385499425,-235.35005));
#194599=CARTESIAN_POINT('Ctrl Pts',(-49.0294131223446,7.77639740475676,
-235.350049999895));
#194600=CARTESIAN_POINT('Ctrl Pts',(-49.4453995747691,7.69019452166921,
-234.55773567316));
#194601=CARTESIAN_POINT('Ctrl Pts',(-48.0110562568883,7.10334135417386,
-235.35005));
#194602=CARTESIAN_POINT('Ctrl Pts',(-48.8755547320805,6.99587710352252,
-235.350049999977));
#194603=CARTESIAN_POINT('Ctrl Pts',(-49.3042975972362,6.93367143720089,
-234.594758063933));
#194604=CARTESIAN_POINT('Ctrl Pts',(-47.8801847113252,5.43950276679566,
-235.35005));
#194605=CARTESIAN_POINT('Ctrl Pts',(-48.7049699708569,5.42468658168255,
-235.350050000023));
#194606=CARTESIAN_POINT('Ctrl Pts',(-49.1474389986164,5.40777060896425,
-234.655599767885));
#194607=CARTESIAN_POINT('Ctrl Pts',(-47.8802911702592,4.60324650202951,
-235.35005));
#194608=CARTESIAN_POINT('Ctrl Pts',(-48.6857137786293,4.62945747049866,
-235.350049999965));
#194609=CARTESIAN_POINT('Ctrl Pts',(-49.1316168687632,4.63854634449982,
-234.679496688758));
#194610=CARTESIAN_POINT('Ctrl Pts',(-47.9840461137012,3.34200714134957,
-235.35005));
#194611=CARTESIAN_POINT('Ctrl Pts',(-48.7629781465623,3.42847856723455,
-235.350050000018));
#194612=CARTESIAN_POINT('Ctrl Pts',(-49.2081948431086,3.47653001453442,
-234.707152337111));
#194613=CARTESIAN_POINT('Ctrl Pts',(-48.0360840389224,2.92068200690756,
-235.35005));
#194614=CARTESIAN_POINT('Ctrl Pts',(-48.8063313608279,3.02739794392703,
-235.350050000023));
#194615=CARTESIAN_POINT('Ctrl Pts',(-49.2506302602395,3.08799066764764,
-234.714964437313));
#194616=CARTESIAN_POINT('Ctrl Pts',(-48.1401430583213,2.2930545562818,-235.35005));
#194617=CARTESIAN_POINT('Ctrl Pts',(-48.8978289995632,2.42958777593589,
-235.350049999988));
#194618=CARTESIAN_POINT('Ctrl Pts',(-49.3396413190743,2.5089581698339,-234.724628454032));
#194619=CARTESIAN_POINT('Ctrl Pts',(-48.1791846215008,2.08432209117866,
-235.35005));
#194620=CARTESIAN_POINT('Ctrl Pts',(-48.932713688424,2.23083484320497,-235.350050000003));
#194621=CARTESIAN_POINT('Ctrl Pts',(-49.3735508031399,2.31635516053753,
-234.727514226363));
#194622=CARTESIAN_POINT('Ctrl Pts',(-48.228072252525,1.85004158947422,-235.35005));
#194623=CARTESIAN_POINT('Ctrl Pts',(-48.9769897078866,2.0076757336604,-235.35005));
#194624=CARTESIAN_POINT('Ctrl Pts',(-49.4165272131256,2.10018771678728,
-234.730394424523));
#194625=CARTESIAN_POINT('Ctrl Pts',(-48.2336222089945,1.8240233376047,-235.35005));
#194626=CARTESIAN_POINT('Ctrl Pts',(-48.9818156073548,1.98338263954127,
-235.35005));
#194627=CARTESIAN_POINT('Ctrl Pts',(-49.421152047383,2.07696182865743,-234.730846041466));
#194628=CARTESIAN_POINT('Ctrl Pts',(-48.2445959867496,1.77197302819215,
-235.35005));
#194629=CARTESIAN_POINT('Ctrl Pts',(-48.9941558750127,1.92837971028397,
-235.35005));
#194630=CARTESIAN_POINT('Ctrl Pts',(-49.4338273118493,2.0201275975502,-234.729910687298));
#194631=CARTESIAN_POINT('Ctrl Pts',(-48.2500003143967,1.7459388370457,-235.35005));
#194632=CARTESIAN_POINT('Ctrl Pts',(-49.0002396819616,1.90086620641864,
-235.350049999998));
#194633=CARTESIAN_POINT('Ctrl Pts',(-49.4400753518836,1.99169798970336,
-234.729442130167));
#194634=CARTESIAN_POINT('Ctrl Pts',(-48.2659659469638,1.66780919078281,
-235.35005));
#194635=CARTESIAN_POINT('Ctrl Pts',(-49.0182341893565,1.81828164539219,
-235.350050000004));
#194636=CARTESIAN_POINT('Ctrl Pts',(-49.4585508766027,1.90637194168949,
-234.728033882328));
#194637=CARTESIAN_POINT('Ctrl Pts',(-48.2762799057323,1.61568666327167,
-235.35005));
#194638=CARTESIAN_POINT('Ctrl Pts',(-49.0298842521479,1.76318267619767,
-235.350049999997));
#194639=CARTESIAN_POINT('Ctrl Pts',(-49.4705097695714,1.84943827229719,
-234.727091615801));
#194640=CARTESIAN_POINT('Ctrl Pts',(-48.3062349042401,1.45921106566498,
-235.35005));
#194641=CARTESIAN_POINT('Ctrl Pts',(-49.0638081444409,1.59771048446028,
-235.350050000006));
#194642=CARTESIAN_POINT('Ctrl Pts',(-49.5053134343056,1.67849037267874,
-234.724254996978));
#194643=CARTESIAN_POINT('Ctrl Pts',(-48.3248891349689,1.35474998793845,
-235.35005));
#194644=CARTESIAN_POINT('Ctrl Pts',(-49.0850407737684,1.48722661629604,
-235.35005));
#194645=CARTESIAN_POINT('Ctrl Pts',(-49.5270852372327,1.56432923319846,
-234.722350837375));
#194646=CARTESIAN_POINT('Ctrl Pts',(-48.4809881192922,0.413309956198443,
-235.35005));
#194647=CARTESIAN_POINT('Ctrl Pts',(-49.2642810383497,0.488366675923553,
-235.35005));
#194648=CARTESIAN_POINT('Ctrl Pts',(-49.710183690821,0.535165240177996,
-234.705106054305));
#194649=CARTESIAN_POINT('Ctrl Pts',(-48.536801379512,-0.432603676106494,
-235.35005));
#194650=CARTESIAN_POINT('Ctrl Pts',(-49.3355324653308,-0.409176197440279,
-235.350050000012));
#194651=CARTESIAN_POINT('Ctrl Pts',(-49.7825193026416,-0.391551959040333,
-234.689053205068));
#194652=CARTESIAN_POINT('Ctrl Pts',(-48.4927543039942,-1.71545839400357,
-235.35005));
#194653=CARTESIAN_POINT('Ctrl Pts',(-49.3082764037978,-1.77136040509552,
-235.350049999994));
#194654=CARTESIAN_POINT('Ctrl Pts',(-49.7507288283362,-1.80056236505131,
-234.663753597616));
#194655=CARTESIAN_POINT('Ctrl Pts',(-48.4566916340738,-2.14207645769056,
-235.35005));
#194656=CARTESIAN_POINT('Ctrl Pts',(-49.2764210778577,-2.22581389857566,
-235.350050000023));
#194657=CARTESIAN_POINT('Ctrl Pts',(-49.7166012702585,-2.26961303439206,
-234.655203456267));
#194658=CARTESIAN_POINT('Ctrl Pts',(-48.3849699272127,-2.67235166449409,
-235.35005));
#194659=CARTESIAN_POINT('Ctrl Pts',(-49.2084397535132,-2.79078396174404,
-235.350049999994));
#194660=CARTESIAN_POINT('Ctrl Pts',(-49.6445034279608,-2.85342594052608,
-234.644346442065));
#194661=CARTESIAN_POINT('Ctrl Pts',(-48.3692885871419,-2.77828474965782,
-235.35005));
#194662=CARTESIAN_POINT('Ctrl Pts',(-49.193398982803,-2.90385097056055,
-235.350050000001));
#194663=CARTESIAN_POINT('Ctrl Pts',(-49.6286066062384,-2.97008785028305,
-234.642167439818));
#194664=CARTESIAN_POINT('Ctrl Pts',(-48.3437536505604,-2.93700076554913,
-235.35005));
#194665=CARTESIAN_POINT('Ctrl Pts',(-49.1686998051045,-3.07327329064321,
-235.350049999999));
#194666=CARTESIAN_POINT('Ctrl Pts',(-49.6025360173428,-3.14492002789723,
-234.638888778593));
#194667=CARTESIAN_POINT('Ctrl Pts',(-48.3349064994216,-2.98987550056776,
-235.35005));
#194668=CARTESIAN_POINT('Ctrl Pts',(-49.1601069182845,-3.12973803229213,
-235.350049999997));
#194669=CARTESIAN_POINT('Ctrl Pts',(-49.5934749193683,-3.20317062991129,
-234.637794194996));
#194670=CARTESIAN_POINT('Ctrl Pts',(-48.3234272698566,-3.05593058196302,
-235.35005));
#194671=CARTESIAN_POINT('Ctrl Pts',(-49.1489197764021,-3.20027698459844,
-235.350050000001));
#194672=CARTESIAN_POINT('Ctrl Pts',(-49.5816838579669,-3.27594936010119,
-234.636423946058));
#194673=CARTESIAN_POINT('Ctrl Pts',(-48.3211104090697,-3.06913968133917,
-235.35005));
#194674=CARTESIAN_POINT('Ctrl Pts',(-49.1466595294267,-3.21438584913259,
-235.350049999999));
#194675=CARTESIAN_POINT('Ctrl Pts',(-49.5793024111936,-3.29050337910297,
-234.636149795232));
#194676=CARTESIAN_POINT('Ctrl Pts',(-48.3164346335911,-3.09555404408755,
-235.35005));
#194677=CARTESIAN_POINT('Ctrl Pts',(-49.1420941838039,-3.24260063609391,
-235.350050000001));
#194678=CARTESIAN_POINT('Ctrl Pts',(-49.574493021136,-3.31960793810423,
-234.635601293727));
#194679=CARTESIAN_POINT('Ctrl Pts',(-48.3140690695237,-3.10875870092911,
-235.35005));
#194680=CARTESIAN_POINT('Ctrl Pts',(-49.1398758067619,-3.25784913209198,
-235.350049999999));
#194681=CARTESIAN_POINT('Ctrl Pts',(-49.5719898593111,-3.33586395411082,
-234.63494477827));
#194682=CARTESIAN_POINT('Ctrl Pts',(-48.3069527703726,-3.14837088297125,
-235.35005));
#194683=CARTESIAN_POINT('Ctrl Pts',(-49.1325141063836,-3.29520795233012,
-235.350050000002));
#194684=CARTESIAN_POINT('Ctrl Pts',(-49.5649563519778,-3.37212886380977,
-234.635775552688));
#194685=CARTESIAN_POINT('Ctrl Pts',(-48.3022780138372,-3.17478533866626,
-235.35005));
#194686=CARTESIAN_POINT('Ctrl Pts',(-49.1276759101128,-3.32012439113747,
-235.350050000001));
#194687=CARTESIAN_POINT('Ctrl Pts',(-49.5603339841976,-3.39631357393668,
-234.636323283642));
#194688=CARTESIAN_POINT('Ctrl Pts',(-48.260829396598,-3.41257237641022,
-235.35005));
#194689=CARTESIAN_POINT('Ctrl Pts',(-49.0847964911652,-3.54426580816513,
-235.350049999991));
#194690=CARTESIAN_POINT('Ctrl Pts',(-49.5193318923867,-3.61404804116118,
-234.641198325652));
#194691=CARTESIAN_POINT('Ctrl Pts',(-48.2284220495721,-3.6243432560285,
-235.35005));
#194692=CARTESIAN_POINT('Ctrl Pts',(-49.0511033314479,-3.74426713955755,
-235.350049999982));
#194693=CARTESIAN_POINT('Ctrl Pts',(-49.487144398575,-3.80810162390295,
-234.645144669832));
#194694=CARTESIAN_POINT('Ctrl Pts',(-48.144430583747,-4.26086274000263,
-235.35005));
#194695=CARTESIAN_POINT('Ctrl Pts',(-48.9634476725892,-4.34524549861128,
-235.350050000035));
#194696=CARTESIAN_POINT('Ctrl Pts',(-49.4033209083405,-4.39164979328187,
-234.655896371867));
#194697=CARTESIAN_POINT('Ctrl Pts',(-48.1060703916391,-4.68681758304716,
-235.35005));
#194698=CARTESIAN_POINT('Ctrl Pts',(-48.9226394477868,-4.74845242256804,
-235.350050000024));
#194699=CARTESIAN_POINT('Ctrl Pts',(-49.3644187765574,-4.7824530264519,
-234.661627301873));
#194700=CARTESIAN_POINT('Ctrl Pts',(-48.0648194622892,-5.541962664716,-235.35005));
#194701=CARTESIAN_POINT('Ctrl Pts',(-48.8768530903346,-5.55812616662415,
-235.350049999976));
#194702=CARTESIAN_POINT('Ctrl Pts',(-49.3208923248062,-5.56761936750886,
-234.670334826408));
#194703=CARTESIAN_POINT('Ctrl Pts',(-48.0619566741598,-5.9722387873912,
-235.35005));
#194704=CARTESIAN_POINT('Ctrl Pts',(-48.8717934133749,-5.96601881198723,
-235.350049999988));
#194705=CARTESIAN_POINT('Ctrl Pts',(-49.316286029903,-5.96285167976809,
-234.673332973669));
#194706=CARTESIAN_POINT('Ctrl Pts',(-48.10749380005,-7.25998633045287,-235.35005));
#194707=CARTESIAN_POINT('Ctrl Pts',(-48.9111302298558,-7.1858727298053,
-235.350050000024));
#194708=CARTESIAN_POINT('Ctrl Pts',(-49.3548824427616,-7.14594001291835,
-234.678250097988));
#194709=CARTESIAN_POINT('Ctrl Pts',(-48.2090347928457,-8.11012177193449,
-235.35005));
#194710=CARTESIAN_POINT('Ctrl Pts',(-49.0092881727724,-7.99360123144335,
-235.350050000012));
#194711=CARTESIAN_POINT('Ctrl Pts',(-49.4496009034112,-7.92719424599897,
-234.676205023672));
#194712=CARTESIAN_POINT('Ctrl Pts',(-48.3844338019353,-8.96504977313631,
-235.35005));
#194713=CARTESIAN_POINT('Ctrl Pts',(-49.1809368960491,-8.80091402256234,
-235.35005));
#194714=CARTESIAN_POINT('Ctrl Pts',(-49.6155653128172,-8.71134938327683,
-234.668556283135));
#194715=CARTESIAN_POINT('Ctrl Pts',(-48.3871335037843,-8.97820236411209,
-235.35005));
#194716=CARTESIAN_POINT('Ctrl Pts',(-49.1838435713664,-8.81569314774841,
-235.350050000001));
#194717=CARTESIAN_POINT('Ctrl Pts',(-49.6186704393278,-8.7269994720143,
-234.668716968957));
#194718=CARTESIAN_POINT('Ctrl Pts',(-48.392472005857,-9.00451470107218,
-235.35005));
#194719=CARTESIAN_POINT('Ctrl Pts',(-49.1894173582549,-8.84368723057296,
-235.35005));
#194720=CARTESIAN_POINT('Ctrl Pts',(-49.6244440767192,-8.75589699832511,
-234.668851427174));
#194721=CARTESIAN_POINT('Ctrl Pts',(-48.3951203393894,-9.01767332704875,
-235.35005));
#194722=CARTESIAN_POINT('Ctrl Pts',(-49.192181971171,-8.8576866421715,-235.35005));
#194723=CARTESIAN_POINT('Ctrl Pts',(-49.6273078813533,-8.77034819797795,
-234.668918648051));
#194724=CARTESIAN_POINT('Ctrl Pts',(-48.4030026471238,-9.05715657045287,
-235.35005));
#194725=CARTESIAN_POINT('Ctrl Pts',(-49.2004089183163,-8.89969141086334,
-235.35005));
#194726=CARTESIAN_POINT('Ctrl Pts',(-49.6358303332325,-8.81370915928673,
-234.669120288507));
#194727=CARTESIAN_POINT('Ctrl Pts',(-48.4081739296747,-9.08348855318983,
-235.35005));
#194728=CARTESIAN_POINT('Ctrl Pts',(-49.2058046086555,-8.92770451878634,
-235.350049999999));
#194729=CARTESIAN_POINT('Ctrl Pts',(-49.6414200199811,-8.84262628275649,
-234.669254685915));
#194730=CARTESIAN_POINT('Ctrl Pts',(-48.4234374397461,-9.16251391233196,
-235.35005));
#194731=CARTESIAN_POINT('Ctrl Pts',(-49.2217246547772,-9.01177023695605,
-235.350050000003));
#194732=CARTESIAN_POINT('Ctrl Pts',(-49.657913818345,-8.92940752669542,
-234.669657810828));
#194733=CARTESIAN_POINT('Ctrl Pts',(-48.4332793497998,-9.21523669725127,
-235.35005));
#194734=CARTESIAN_POINT('Ctrl Pts',(-49.2319829940889,-9.06785410630298,
-235.350050000001));
#194735=CARTESIAN_POINT('Ctrl Pts',(-49.668542693497,-8.98730151744689,
-234.669926470633));
#194736=CARTESIAN_POINT('Ctrl Pts',(-48.4618064955616,-9.37352237066705,
-235.35005));
#194737=CARTESIAN_POINT('Ctrl Pts',(-49.2616934080035,-9.23621342522619,
-235.350049999999));
#194738=CARTESIAN_POINT('Ctrl Pts',(-49.6993320627288,-9.16110643572959,
-234.67073236696));
#194739=CARTESIAN_POINT('Ctrl Pts',(-48.4794934628256,-9.47920254067735,
-235.35005));
#194740=CARTESIAN_POINT('Ctrl Pts',(-49.2800851841445,-9.34861599525297,
-235.350049999994));
#194741=CARTESIAN_POINT('Ctrl Pts',(-49.7183957005529,-9.277140274608,-234.671269513827));
#194742=CARTESIAN_POINT('Ctrl Pts',(-48.5285710814135,-9.79671102654565,
-235.35005));
#194743=CARTESIAN_POINT('Ctrl Pts',(-49.3310169468997,-9.68627262463685,
-235.350050000012));
#194744=CARTESIAN_POINT('Ctrl Pts',(-49.7712138422074,-9.6257621620448,
-234.672882347017));
#194745=CARTESIAN_POINT('Ctrl Pts',(-48.5559827004535,-10.0090068188063,
-235.35005));
#194746=CARTESIAN_POINT('Ctrl Pts',(-49.3593305570913,-9.91200108309528,
-235.350049999985));
#194747=CARTESIAN_POINT('Ctrl Pts',(-49.8005924106469,-9.8587900325559,
-234.673953662556));
#194748=CARTESIAN_POINT('Ctrl Pts',(-48.6223270802844,-10.6477610876399,
-235.35005));
#194749=CARTESIAN_POINT('Ctrl Pts',(-49.427355877287,-10.5909621394109,
-235.35005000003));
#194750=CARTESIAN_POINT('Ctrl Pts',(-49.8712887313567,-10.5599275885378,
-234.677167109714));
#194751=CARTESIAN_POINT('Ctrl Pts',(-48.6453046118701,-11.0773736644593,
-235.35005));
#194752=CARTESIAN_POINT('Ctrl Pts',(-49.4501374566631,-11.0475237351948,
-235.350050000012));
#194753=CARTESIAN_POINT('Ctrl Pts',(-49.8950789101635,-11.0313011583583,
-234.679301565053));
#194754=CARTESIAN_POINT('Ctrl Pts',(-48.6501328458788,-12.3566962654659,
-235.35005));
#194755=CARTESIAN_POINT('Ctrl Pts',(-49.4504015731985,-12.4060784579424,
-235.350049999976));
#194756=CARTESIAN_POINT('Ctrl Pts',(-49.8961844037889,-12.4347055151062,
-234.685595719225));
#194757=CARTESIAN_POINT('Ctrl Pts',(-48.5694097707421,-13.2010981453996,
-235.35005));
#194758=CARTESIAN_POINT('Ctrl Pts',(-49.3616578254152,-13.3025722383012,
-235.350050000024));
#194759=CARTESIAN_POINT('Ctrl Pts',(-49.8049050012374,-13.3604031808191,
-234.689647068821));
#194760=CARTESIAN_POINT('Ctrl Pts',(-48.3999288819756,-14.0631760578291,
-235.35005));
#194761=CARTESIAN_POINT('Ctrl Pts',(-49.1784903666304,-14.2179091212367,
-235.35005));
#194762=CARTESIAN_POINT('Ctrl Pts',(-49.6163897775734,-14.3049392848125,
-234.693720565574));
#194763=CARTESIAN_POINT('Ctrl Pts',(-48.3947106332052,-14.089291300339,
-235.35005));
#194764=CARTESIAN_POINT('Ctrl Pts',(-49.172856954301,-14.2456147707397,
-235.350050000001));
#194765=CARTESIAN_POINT('Ctrl Pts',(-49.6105868475141,-14.3335523084377,
-234.693843927845));
#194766=CARTESIAN_POINT('Ctrl Pts',(-48.3867592982998,-14.1284516414382,
-235.35005));
#194767=CARTESIAN_POINT('Ctrl Pts',(-49.1642752691847,-14.2871601252974,
-235.35005));
#194768=CARTESIAN_POINT('Ctrl Pts',(-49.6017465855193,-14.3764581150203,
-234.694028868984));
#194769=CARTESIAN_POINT('Ctrl Pts',(-48.3840780941576,-14.1415019811602,
-235.35005));
#194770=CARTESIAN_POINT('Ctrl Pts',(-49.1612266343483,-14.3016684110766,
-235.35005));
#194771=CARTESIAN_POINT('Ctrl Pts',(-49.5985360159632,-14.3917957223577,
-234.694115256963));
#194772=CARTESIAN_POINT('Ctrl Pts',(-48.3787223515611,-14.1676033339819,
-235.35005));
#194773=CARTESIAN_POINT('Ctrl Pts',(-49.1561371684305,-14.326418078323,
-235.35005));
#194774=CARTESIAN_POINT('Ctrl Pts',(-49.5936036508982,-14.415786266369,
-234.694129273138));
#194775=CARTESIAN_POINT('Ctrl Pts',(-48.3760618298762,-14.1806557630565,
-235.35005));
#194776=CARTESIAN_POINT('Ctrl Pts',(-49.1536098434105,-14.3387948688079,
-235.350050000001));
#194777=CARTESIAN_POINT('Ctrl Pts',(-49.5911542470628,-14.4277834533854,
-234.694134995679));
#194778=CARTESIAN_POINT('Ctrl Pts',(-48.3628458825965,-14.2459266629983,
-235.35005));
#194779=CARTESIAN_POINT('Ctrl Pts',(-49.1410602317348,-14.4006882956361,
-235.350049999995));
#194780=CARTESIAN_POINT('Ctrl Pts',(-49.5789910512861,-14.4877788919854,
-234.694157190572));
#194781=CARTESIAN_POINT('Ctrl Pts',(-48.3525504293568,-14.2981713963959,
-235.35005));
#194782=CARTESIAN_POINT('Ctrl Pts',(-49.1312987239013,-14.4502345980385,
-235.35005));
#194783=CARTESIAN_POINT('Ctrl Pts',(-49.5695287198168,-14.5358056523908,
-234.694154412176));
#194784=CARTESIAN_POINT('Ctrl Pts',(-48.3224929218234,-14.4549893276864,
-235.35005));
#194785=CARTESIAN_POINT('Ctrl Pts',(-49.1028465494228,-14.5989634011547,
-235.35005));
#194786=CARTESIAN_POINT('Ctrl Pts',(-49.5419439476953,-14.6799744510311,
-234.694084786526));
#194787=CARTESIAN_POINT('Ctrl Pts',(-48.3035595793916,-14.5596462424765,
-235.35005));
#194788=CARTESIAN_POINT('Ctrl Pts',(-49.0849874724743,-14.6982394950892,
-235.350049999998));
#194789=CARTESIAN_POINT('Ctrl Pts',(-49.5246236070435,-14.7762049884194,
-234.693956683334));
#194790=CARTESIAN_POINT('Ctrl Pts',(-48.2500551817889,-14.8739499130376,
-235.35005));
#194791=CARTESIAN_POINT('Ctrl Pts',(-49.0347221330771,-14.9964132146763,
-235.350050000003));
#194792=CARTESIAN_POINT('Ctrl Pts',(-49.4758559537979,-15.0652295831884,
-234.69332855221));
#194793=CARTESIAN_POINT('Ctrl Pts',(-48.2187775910813,-15.0839293763448,
-235.35005));
#194794=CARTESIAN_POINT('Ctrl Pts',(-49.0056251748038,-15.1956711360348,
-235.350049999997));
#194795=CARTESIAN_POINT('Ctrl Pts',(-49.447600122929,-15.2583563846847,
-234.692585242987));
#194796=CARTESIAN_POINT('Ctrl Pts',(-48.1380456036249,-15.7151912142403,
-235.35005));
#194797=CARTESIAN_POINT('Ctrl Pts',(-48.9315200735598,-15.7947230301441,
-235.350050000006));
#194798=CARTESIAN_POINT('Ctrl Pts',(-49.3755486131225,-15.8389090912121,
-234.689371821595));
#194799=CARTESIAN_POINT('Ctrl Pts',(-48.1017687499515,-16.1377801895033,
-235.35005));
#194800=CARTESIAN_POINT('Ctrl Pts',(-48.8997990349571,-16.1958775231026,
-235.350049999994));
#194801=CARTESIAN_POINT('Ctrl Pts',(-49.3445349115517,-16.2275468702548,
-234.68591772599));
#194802=CARTESIAN_POINT('Ctrl Pts',(-48.0452056587669,-17.4030250963116,
-235.35005));
#194803=CARTESIAN_POINT('Ctrl Pts',(-48.8571760735594,-17.3969404754266,
-235.350050000012));
#194804=CARTESIAN_POINT('Ctrl Pts',(-49.3020545258986,-17.3907951876548,
-234.671624111816));
#194805=CARTESIAN_POINT('Ctrl Pts',(-48.0765553834797,-18.2457723122435,
-235.35005));
#194806=CARTESIAN_POINT('Ctrl Pts',(-48.8989420124693,-18.1971730763996,
-235.350049999929));
#194807=CARTESIAN_POINT('Ctrl Pts',(-49.3406485147144,-18.164819270942,
-234.656852423361));
#194808=CARTESIAN_POINT('Ctrl Pts',(-48.202136382695,-19.2982688285888,
-235.35005));
#194809=CARTESIAN_POINT('Ctrl Pts',(-49.0372739509851,-19.1873904238028,
-235.350050000017));
#194810=CARTESIAN_POINT('Ctrl Pts',(-49.4718969222247,-19.1292954138514,
-234.630751354067));
#194811=CARTESIAN_POINT('Ctrl Pts',(-48.2315724527526,-19.5085474359625,
-235.35005));
#194812=CARTESIAN_POINT('Ctrl Pts',(-49.0694140435013,-19.3857696629781,
-235.350049999994));
#194813=CARTESIAN_POINT('Ctrl Pts',(-49.5022925238141,-19.3218807036188,
-234.625150148995));
#194814=CARTESIAN_POINT('Ctrl Pts',(-48.2737849902378,-19.7710257016811,
-235.35005));
#194815=CARTESIAN_POINT('Ctrl Pts',(-49.11500096125,-19.6328314628528,-235.350050000002));
#194816=CARTESIAN_POINT('Ctrl Pts',(-49.5454678269032,-19.5620862891172,
-234.617636622494));
#194817=CARTESIAN_POINT('Ctrl Pts',(-48.2824987027496,-19.82350433647,-235.35005));
#194818=CARTESIAN_POINT('Ctrl Pts',(-49.1244019347077,-19.682263630747,
-235.350049999999));
#194819=CARTESIAN_POINT('Ctrl Pts',(-49.5543622366061,-19.6101024448334,
-234.616108235133));
#194820=CARTESIAN_POINT('Ctrl Pts',(-48.2959770869867,-19.9021966978926,
-235.35005));
#194821=CARTESIAN_POINT('Ctrl Pts',(-49.1389129882989,-19.7563522352633,
-235.35005));
#194822=CARTESIAN_POINT('Ctrl Pts',(-49.5680934468262,-19.6820882105088,
-234.613776279329));
#194823=CARTESIAN_POINT('Ctrl Pts',(-48.3005378529525,-19.9284232197851,
-235.35005));
#194824=CARTESIAN_POINT('Ctrl Pts',(-49.1438196314223,-19.7810450643495,
-235.350050000005));
#194825=CARTESIAN_POINT('Ctrl Pts',(-49.5727354507713,-19.7060770526268,
-234.612992397751));
#194826=CARTESIAN_POINT('Ctrl Pts',(-48.3074811028276,-19.9677565956903,
-235.35005));
#194827=CARTESIAN_POINT('Ctrl Pts',(-49.1512821856062,-19.8180692694358,
-235.350049999998));
#194828=CARTESIAN_POINT('Ctrl Pts',(-49.5797959434908,-19.7420505664417,
-234.61180661903));
#194829=CARTESIAN_POINT('Ctrl Pts',(-48.3098125363869,-19.9808666531709,
-235.35005));
#194830=CARTESIAN_POINT('Ctrl Pts',(-49.1537871425354,-19.8304098086682,
-235.350050000001));
#194831=CARTESIAN_POINT('Ctrl Pts',(-49.5821656888743,-19.7540401124037,
-234.611409700054));
#194832=CARTESIAN_POINT('Ctrl Pts',(-48.3145094629338,-20.0070846308637,
-235.35005));
#194833=CARTESIAN_POINT('Ctrl Pts',(-49.1588315088273,-19.855086940684,
-235.350049999999));
#194834=CARTESIAN_POINT('Ctrl Pts',(-49.5869376908479,-19.7780159321077,
-234.610612524155));
#194835=CARTESIAN_POINT('Ctrl Pts',(-48.3168699427918,-20.0201928656617,
-235.35005));
#194836=CARTESIAN_POINT('Ctrl Pts',(-49.1609637431947,-19.869444669877,
-235.35005));
#194837=CARTESIAN_POINT('Ctrl Pts',(-49.5892803760666,-19.7929526511806,
-234.611191018229));
#194838=CARTESIAN_POINT('Ctrl Pts',(-48.3378149961279,-20.1381857579918,
-235.35005));
#194839=CARTESIAN_POINT('Ctrl Pts',(-49.1803832875034,-19.9958192386853,
-235.350050000002));
#194840=CARTESIAN_POINT('Ctrl Pts',(-49.6101145207749,-19.9233239035134,
-234.615047470178));
#194841=CARTESIAN_POINT('Ctrl Pts',(-48.3550896009133,-20.2431526171789,
-235.35005));
#194842=CARTESIAN_POINT('Ctrl Pts',(-49.1962287252122,-20.1082560487782,
-235.350049999994));
#194843=CARTESIAN_POINT('Ctrl Pts',(-49.6271396690249,-20.0392626516645,
-234.618456601287));
#194844=CARTESIAN_POINT('Ctrl Pts',(-48.4347895563001,-20.7684056538746,
-235.35005));
#194845=CARTESIAN_POINT('Ctrl Pts',(-49.2681921281626,-20.6693028847357,
-235.350050000023));
#194846=CARTESIAN_POINT('Ctrl Pts',(-49.7048510075002,-20.6191868386639,
-234.635401433285));
#194847=CARTESIAN_POINT('Ctrl Pts',(-48.4772403630273,-21.1899452510999,
-235.35005));
#194848=CARTESIAN_POINT('Ctrl Pts',(-49.3034028549804,-21.1195336358382,
-235.35005));
#194849=CARTESIAN_POINT('Ctrl Pts',(-49.7433516745446,-21.0837395665231,
-234.64859809159));
#194850=CARTESIAN_POINT('Ctrl Pts',(-48.5415386498259,-22.458520743411,
-235.35005));
#194851=CARTESIAN_POINT('Ctrl Pts',(-49.3419650219896,-22.4675064520562,
-235.35005));
#194852=CARTESIAN_POINT('Ctrl Pts',(-49.7892124454036,-22.4793485342635,
-234.687225534828));
#194853=CARTESIAN_POINT('Ctrl Pts',(-48.5005032094983,-23.311667738302,
-235.35005));
#194854=CARTESIAN_POINT('Ctrl Pts',(-49.2800794163868,-23.3730401250582,
-235.35005));
#194855=CARTESIAN_POINT('Ctrl Pts',(-49.7271015354622,-23.4144460560838,
-234.711697624812));
#194856=CARTESIAN_POINT('Ctrl Pts',(-48.3390590324706,-24.3778343529881,
-235.35005));
#194857=CARTESIAN_POINT('Ctrl Pts',(-49.086074667266,-24.5037177534246,
-235.35005));
#194858=CARTESIAN_POINT('Ctrl Pts',(-49.5294900946094,-24.5788354560032,
-234.740523989368));
#194859=CARTESIAN_POINT('Ctrl Pts',(-48.3012455308433,-24.5909867391319,
-235.35005));
#194860=CARTESIAN_POINT('Ctrl Pts',(-49.0416655455856,-24.7287449779651,
-235.350050000018));
#194861=CARTESIAN_POINT('Ctrl Pts',(-49.4839495431616,-24.8114203403136,
-234.746200830511));
#194862=CARTESIAN_POINT('Ctrl Pts',(-48.2523434883265,-24.8306899717521,
-235.35005));
#194863=CARTESIAN_POINT('Ctrl Pts',(-48.9850331973951,-24.9817901079185,
-235.350049999998));
#194864=CARTESIAN_POINT('Ctrl Pts',(-49.4258297714769,-25.0727001745,-234.752473563172));
#194865=CARTESIAN_POINT('Ctrl Pts',(-48.2468215385715,-24.857322369352,
-235.35005));
#194866=CARTESIAN_POINT('Ctrl Pts',(-48.9786554175451,-25.0098727669535,
-235.350049999997));
#194867=CARTESIAN_POINT('Ctrl Pts',(-49.4192763488556,-25.1017260271132,
-234.753168950875));
#194868=CARTESIAN_POINT('Ctrl Pts',(-48.2356002982336,-24.910584566504,
-235.35005));
#194869=CARTESIAN_POINT('Ctrl Pts',(-48.9657159328337,-25.0660281153669,
-235.350050000003));
#194870=CARTESIAN_POINT('Ctrl Pts',(-49.4059777280254,-25.1597670748574,
-234.754556505762));
#194871=CARTESIAN_POINT('Ctrl Pts',(-48.2299135975692,-24.9372145504824,
-235.35005));
#194872=CARTESIAN_POINT('Ctrl Pts',(-48.9608504508884,-25.0911588778292,
-235.350049999999));
#194873=CARTESIAN_POINT('Ctrl Pts',(-49.4013021218481,-25.1839185178113,
-234.753925525474));
#194874=CARTESIAN_POINT('Ctrl Pts',(-48.2132345171348,-25.0171100844526,
-235.35005));
#194875=CARTESIAN_POINT('Ctrl Pts',(-48.946142631535,-25.1674232304628,
-235.350050000002));
#194876=CARTESIAN_POINT('Ctrl Pts',(-49.3870431573761,-25.2578284787265,
-234.752406627079));
#194877=CARTESIAN_POINT('Ctrl Pts',(-48.2024091551349,-25.0703780812323,
-235.35005));
#194878=CARTESIAN_POINT('Ctrl Pts',(-48.9366357051972,-25.2182625009279,
-235.350049999999));
#194879=CARTESIAN_POINT('Ctrl Pts',(-49.3778231822086,-25.3071039363646,
-234.751372563654));
#194880=CARTESIAN_POINT('Ctrl Pts',(-48.1708085736138,-25.2301948978772,
-235.35005));
#194881=CARTESIAN_POINT('Ctrl Pts',(-48.9089945694079,-25.3708143302532,
-235.350050000001));
#194882=CARTESIAN_POINT('Ctrl Pts',(-49.3510150827827,-25.454934683882,
-234.748205410904));
#194883=CARTESIAN_POINT('Ctrl Pts',(-48.1509087141736,-25.3367565417747,
-235.35005));
#194884=CARTESIAN_POINT('Ctrl Pts',(-48.8917526157755,-25.4724994483113,
-235.350050000001));
#194885=CARTESIAN_POINT('Ctrl Pts',(-49.3342786576262,-25.5534943522782,
-234.746007383865));
#194886=CARTESIAN_POINT('Ctrl Pts',(-48.0571667807649,-25.8696491072789,
-235.35005));
#194887=CARTESIAN_POINT('Ctrl Pts',(-48.811261859734,-25.9816228925711,
-235.350049999994));
#194888=CARTESIAN_POINT('Ctrl Pts',(-49.2562000930912,-26.0462949080656,
-234.734575161191));
#194889=CARTESIAN_POINT('Ctrl Pts',(-48.000556289185,-26.2962324730956,
-235.35005));
#194890=CARTESIAN_POINT('Ctrl Pts',(-48.7656505977619,-26.3885598012182,
-235.350049999982));
#194891=CARTESIAN_POINT('Ctrl Pts',(-49.211634953002,-26.4405395961576,
-234.724022357095));
#194892=CARTESIAN_POINT('Ctrl Pts',(-47.8838810362842,-27.5767613139966,
-235.35005));
#194893=CARTESIAN_POINT('Ctrl Pts',(-48.6827507003063,-27.6106377649942,
-235.350050000036));
#194894=CARTESIAN_POINT('Ctrl Pts',(-49.1296257840991,-27.6223459390551,
-234.687604363246));
#194895=CARTESIAN_POINT('Ctrl Pts',(-47.876633025442,-28.431480559278,-235.35005));
#194896=CARTESIAN_POINT('Ctrl Pts',(-48.7005291317402,-28.4246911972351,
-235.350049999953));
#194897=CARTESIAN_POINT('Ctrl Pts',(-49.1434150770831,-28.4094549490855,
-234.657217580316));
#194898=CARTESIAN_POINT('Ctrl Pts',(-48.0026713456265,-30.1816730688289,
-235.35005));
#194899=CARTESIAN_POINT('Ctrl Pts',(-48.8799154192025,-30.0782314618698,
-235.35005000005));
#194900=CARTESIAN_POINT('Ctrl Pts',(-49.3058185785018,-30.0154916213199,
-234.579129604302));
#194901=CARTESIAN_POINT('Ctrl Pts',(-48.1423359832808,-31.0772709955632,
-235.35005));
#194902=CARTESIAN_POINT('Ctrl Pts',(-49.0516357944767,-30.9231333337257,
-235.350050000035));
#194903=CARTESIAN_POINT('Ctrl Pts',(-49.4605472095348,-30.8341434889496,
-234.530604785809));
#194904=CARTESIAN_POINT('Ctrl Pts',(-48.3606172463808,-31.9739539840651,
-235.35005));
#194905=CARTESIAN_POINT('Ctrl Pts',(-49.2988059683443,-31.7455385989255,
-235.350049999995));
#194906=CARTESIAN_POINT('Ctrl Pts',(-49.6872475187014,-31.6509467871898,
-234.471114721056));
#194907=CARTESIAN_POINT('',(-49.6580996754574,-31.5448418565169,-234.479004868619));
#194908=CARTESIAN_POINT('',(-48.3327003568643,-31.8574637039841,-235.35005));
#194909=CARTESIAN_POINT('Origin',(-48.3327003568642,-31.8574637039841,-233.85005));
#194910=CARTESIAN_POINT('',(-49.4065653148269,-25.1565430143321,-234.754641484296));
#194911=CARTESIAN_POINT('Ctrl Pts',(-49.6580996754575,-31.5448418565169,
-234.479004868619));
#194912=CARTESIAN_POINT('Ctrl Pts',(-49.590346126536,-31.2938113421995,
-234.497007566398));
#194913=CARTESIAN_POINT('Ctrl Pts',(-49.5294056430117,-31.0426055563327,
-234.513982723729));
#194914=CARTESIAN_POINT('Ctrl Pts',(-49.4752396727556,-30.7912125751541,
-234.529999882613));
#194915=CARTESIAN_POINT('Ctrl Pts',(-49.4410958566977,-30.6327456324031,
-234.540096386453));
#194916=CARTESIAN_POINT('Ctrl Pts',(-49.4096449111297,-30.4742042661059,
-234.549812231499));
#194917=CARTESIAN_POINT('Ctrl Pts',(-49.3808878256904,-30.3155859402117,
-234.559164835971));
#194918=CARTESIAN_POINT('Ctrl Pts',(-49.3353805488539,-30.0645769120863,
-234.57396506883));
#194919=CARTESIAN_POINT('Ctrl Pts',(-49.2966167553167,-29.8133745672487,
-234.587855668465));
#194920=CARTESIAN_POINT('Ctrl Pts',(-49.2645915793269,-29.5619803241126,
-234.600905660719));
#194921=CARTESIAN_POINT('Ctrl Pts',(-49.232878789184,-29.3130382768225,
-234.613828358344));
#194922=CARTESIAN_POINT('Ctrl Pts',(-49.2077738585867,-29.0639076727252,
-234.625926767819));
#194923=CARTESIAN_POINT('Ctrl Pts',(-49.1893215480184,-28.8146023258056,
-234.637267914711));
#194924=CARTESIAN_POINT('Ctrl Pts',(-49.1831955148801,-28.7318347606741,
-234.641033093139));
#194925=CARTESIAN_POINT('Ctrl Pts',(-49.177803131853,-28.6490480630386,
-234.644714806706));
#194926=CARTESIAN_POINT('Ctrl Pts',(-49.1731472439229,-28.5662431585057,
-234.64831550801));
#194927=CARTESIAN_POINT('Ctrl Pts',(-49.1692623684599,-28.497150700383,
-234.651319935169));
#194928=CARTESIAN_POINT('Ctrl Pts',(-49.1658902704926,-28.4280455697387,
-234.654267959623));
#194929=CARTESIAN_POINT('Ctrl Pts',(-49.163031882372,-28.3589283663495,
-234.65716100616));
#194930=CARTESIAN_POINT('Ctrl Pts',(-49.1525743380049,-28.1060598997706,
-234.667745349937));
#194931=CARTESIAN_POINT('Ctrl Pts',(-49.1489996771991,-27.8530509491739,
-234.677576545427));
#194932=CARTESIAN_POINT('Ctrl Pts',(-49.1523917163603,-27.5999159742951,
-234.68671666602));
#194933=CARTESIAN_POINT('Ctrl Pts',(-49.1555766840377,-27.362233956278,
-234.695298815952));
#194934=CARTESIAN_POINT('Ctrl Pts',(-49.1649042233204,-27.1244406564733,
-234.703271690739));
#194935=CARTESIAN_POINT('Ctrl Pts',(-49.1804897356957,-26.886572392946,
-234.71068667557));
#194936=CARTESIAN_POINT('Ctrl Pts',(-49.1815030317473,-26.8711073272851,
-234.711168762695));
#194937=CARTESIAN_POINT('Ctrl Pts',(-49.1825427958084,-26.8556419543378,
-234.711648491628));
#194938=CARTESIAN_POINT('Ctrl Pts',(-49.1836090661316,-26.8401762881947,
-234.712125876492));
#194939=CARTESIAN_POINT('Ctrl Pts',(-49.1854658975133,-26.8132439675545,
-234.712957207137));
#194940=CARTESIAN_POINT('Ctrl Pts',(-49.1874031105211,-26.7863107575068,
-234.713781429235));
#194941=CARTESIAN_POINT('Ctrl Pts',(-49.1894208472892,-26.7593767202999,
-234.714598617361));
#194942=CARTESIAN_POINT('Ctrl Pts',(-49.2071135019829,-26.5232038818332,
-234.721764184036));
#194943=CARTESIAN_POINT('Ctrl Pts',(-49.2310148167691,-26.2869277163969,
-234.728364686713));
#194944=CARTESIAN_POINT('Ctrl Pts',(-49.2612614314676,-26.0506127383107,
-234.734435211101));
#194945=CARTESIAN_POINT('Ctrl Pts',(-49.2651872190284,-26.019940796652,
-234.735223120405));
#194946=CARTESIAN_POINT('Ctrl Pts',(-49.2692199568921,-25.9892682458034,
-234.736002101628));
#194947=CARTESIAN_POINT('Ctrl Pts',(-49.2733599943998,-25.9585952679501,
-234.736772231484));
#194948=CARTESIAN_POINT('Ctrl Pts',(-49.2913786753514,-25.8250972982491,
-234.740124066862));
#194949=CARTESIAN_POINT('Ctrl Pts',(-49.3114284827361,-25.6915901763045,
-234.743309777531));
#194950=CARTESIAN_POINT('Ctrl Pts',(-49.3335417708821,-25.5580868232228,
-234.746335595632));
#194951=CARTESIAN_POINT('Ctrl Pts',(-49.344598414955,-25.4913351466819,
-234.747848504682));
#194952=CARTESIAN_POINT('Ctrl Pts',(-49.3561712624554,-25.4245844267277,
-234.749321105246));
#194953=CARTESIAN_POINT('Ctrl Pts',(-49.3682650086808,-25.3578363353345,
-234.750754002269));
#194954=CARTESIAN_POINT('Ctrl Pts',(-49.3743118817935,-25.3244622896378,
-234.751470450781));
#194955=CARTESIAN_POINT('Ctrl Pts',(-49.3804889830364,-25.2910889018601,
-234.752176976097));
#194956=CARTESIAN_POINT('Ctrl Pts',(-49.3867969582897,-25.2577163848095,
-234.752873621892));
#194957=CARTESIAN_POINT('Ctrl Pts',(-49.3913647572992,-25.233550318171,
-234.753378084551));
#194958=CARTESIAN_POINT('Ctrl Pts',(-49.3956861054634,-25.2101556288682,
-234.754075989134));
#194959=CARTESIAN_POINT('Ctrl Pts',(-49.4006156889099,-25.1854554901182,
-234.754424809087));
#194960=CARTESIAN_POINT('Ctrl Pts',(-49.4024936927336,-25.1760455763752,
-234.754557697639));
#194961=CARTESIAN_POINT('Ctrl Pts',(-49.4044604812417,-25.1664462685349,
-234.754639921753));
#194962=CARTESIAN_POINT('Ctrl Pts',(-49.4065653148269,-25.1565430143321,
-234.754641484296));
#194963=CARTESIAN_POINT('',(-49.5863631216035,-19.7758588045606,-234.610932138786));
#194964=CARTESIAN_POINT('Ctrl Pts',(-49.4065714250583,-25.1565443079239,
-234.754646206088));
#194965=CARTESIAN_POINT('Ctrl Pts',(-49.4083225452229,-25.1482850280493,
-234.754642899617));
#194966=CARTESIAN_POINT('Ctrl Pts',(-49.41020323589,-25.1397150740938,-234.754554876728));
#194967=CARTESIAN_POINT('Ctrl Pts',(-49.4122755477287,-25.1306724979893,
-234.754338313619));
#194968=CARTESIAN_POINT('Ctrl Pts',(-49.4166128694744,-25.111746503724,
-234.753885049844));
#194969=CARTESIAN_POINT('Ctrl Pts',(-49.4209094077061,-25.0928182406844,
-234.753431099368));
#194970=CARTESIAN_POINT('Ctrl Pts',(-49.4251652238492,-25.0738877287661,
-234.752976469689));
#194971=CARTESIAN_POINT('Ctrl Pts',(-49.427434911034,-25.0637918179333,
-234.752734009225));
#194972=CARTESIAN_POINT('Ctrl Pts',(-49.4296930160082,-25.0536952676186,
-234.752491355368));
#194973=CARTESIAN_POINT('Ctrl Pts',(-49.4319395478169,-25.0435980813769,
-234.752248509462));
#194974=CARTESIAN_POINT('Ctrl Pts',(-49.4359180394011,-25.0257164870321,
-234.751818441929));
#194975=CARTESIAN_POINT('Ctrl Pts',(-49.4398602422247,-25.0078328970427,
-234.751387773391));
#194976=CARTESIAN_POINT('Ctrl Pts',(-49.4437662024039,-24.9899473318732,
-234.750956510672));
#194977=CARTESIAN_POINT('Ctrl Pts',(-49.4559892738732,-24.9339773446458,
-234.749606943654));
#194978=CARTESIAN_POINT('Ctrl Pts',(-49.4678574396967,-24.8779880059922,
-234.748251547475));
#194979=CARTESIAN_POINT('Ctrl Pts',(-49.4793721424816,-24.8219799161756,
-234.746890499776));
#194980=CARTESIAN_POINT('Ctrl Pts',(-49.5024015480513,-24.7099637365424,
-234.744168404378));
#194981=CARTESIAN_POINT('Ctrl Pts',(-49.524017101493,-24.5978725522242,
-234.741423702898));
#194982=CARTESIAN_POINT('Ctrl Pts',(-49.5442303524539,-24.4857111577519,
-234.738657807323));
#194983=CARTESIAN_POINT('Ctrl Pts',(-49.552626376232,-24.4391224255984,
-234.73750893102));
#194984=CARTESIAN_POINT('Ctrl Pts',(-49.5607804549896,-24.3925215798048,
-234.736356398016));
#194985=CARTESIAN_POINT('Ctrl Pts',(-49.5686934164371,-24.3459089640037,
-234.735200309511));
#194986=CARTESIAN_POINT('Ctrl Pts',(-49.7268222749508,-23.4144246167288,
-234.71209758661));
#194987=CARTESIAN_POINT('Ctrl Pts',(-49.7889759213309,-22.4793462204463,
-234.687578993421));
#194988=CARTESIAN_POINT('Ctrl Pts',(-49.7584449475999,-21.548951679417,
-234.661775242303));
#194989=CARTESIAN_POINT('Ctrl Pts',(-49.7431794607344,-21.0837544089024,
-234.648873366744));
#194990=CARTESIAN_POINT('Ctrl Pts',(-49.704700149341,-20.6192049141822,
-234.63564923189));
#194991=CARTESIAN_POINT('Ctrl Pts',(-49.6425520532046,-20.155267103844,
-234.622064432487));
#194992=CARTESIAN_POINT('Ctrl Pts',(-49.6405496054477,-20.1403187581116,
-234.621626722359));
#194993=CARTESIAN_POINT('Ctrl Pts',(-49.6385225254361,-20.1253711747348,
-234.621188675716));
#194994=CARTESIAN_POINT('Ctrl Pts',(-49.636470789184,-20.1104243691117,
-234.620750295427));
#194995=CARTESIAN_POINT('Ctrl Pts',(-49.6249635842442,-20.0265949025698,
-234.618291630563));
#194996=CARTESIAN_POINT('Ctrl Pts',(-49.6126808048582,-19.9427899006565,
-234.615822470671));
#194997=CARTESIAN_POINT('Ctrl Pts',(-49.5996182194956,-19.8590120799471,
-234.613343321822));
#194998=CARTESIAN_POINT('Ctrl Pts',(-49.5969386465566,-19.8418264482341,
-234.612834765515));
#194999=CARTESIAN_POINT('Ctrl Pts',(-49.5942262585936,-19.824641947958,
-234.612325786926));
#195000=CARTESIAN_POINT('Ctrl Pts',(-49.5914810209125,-19.8074586253538,
-234.611816394022));
#195001=CARTESIAN_POINT('Ctrl Pts',(-49.5897653609845,-19.7967197599277,
-234.61149804454));
#195002=CARTESIAN_POINT('Ctrl Pts',(-49.5880344428409,-19.7857330389408,
-234.611097274937));
#195003=CARTESIAN_POINT('Ctrl Pts',(-49.5862818832396,-19.7758835630004,
-234.611073196375));
#195004=CARTESIAN_POINT('',(-49.6141588435918,-8.70526933620937,-234.668797542549));
#195005=CARTESIAN_POINT('Ctrl Pts',(-49.586393185248,-19.775849642277,-234.610879938015));
#195006=CARTESIAN_POINT('Ctrl Pts',(-49.5856686445096,-19.7724384225141,
-234.611065158657));
#195007=CARTESIAN_POINT('Ctrl Pts',(-49.585055184216,-19.7691449560952,
-234.61110291388));
#195008=CARTESIAN_POINT('Ctrl Pts',(-49.5820527790106,-19.7540602415442,
-234.61160435363));
#195009=CARTESIAN_POINT('Ctrl Pts',(-49.5796829880909,-19.7420706048251,
-234.612001185075));
#195010=CARTESIAN_POINT('Ctrl Pts',(-49.5726223597956,-19.7060968192221,
-234.613186702187));
#195011=CARTESIAN_POINT('Ctrl Pts',(-49.5679802665039,-19.6821077948723,
-234.613970410723));
#195012=CARTESIAN_POINT('Ctrl Pts',(-49.5542487923194,-19.6101214844369,
-234.616301851302));
#195013=CARTESIAN_POINT('Ctrl Pts',(-49.5453542107186,-19.5621049613933,
-234.617829900602));
#195014=CARTESIAN_POINT('Ctrl Pts',(-49.5021780821526,-19.3218975941556,
-234.625341761091));
#195015=CARTESIAN_POINT('Ctrl Pts',(-49.47178187823,-19.1293107914889,-234.630941719413));
#195016=CARTESIAN_POINT('Ctrl Pts',(-49.3405309283227,-18.1648278835588,
-234.657036929293));
#195017=CARTESIAN_POINT('Ctrl Pts',(-49.3019357180199,-17.3907968286783,
-234.671805261636));
#195018=CARTESIAN_POINT('Ctrl Pts',(-49.3444157773257,-16.2275383867562,
-234.686095603872));
#195019=CARTESIAN_POINT('Ctrl Pts',(-49.375429580623,-15.8388972460656,
-234.689548905031));
#195020=CARTESIAN_POINT('Ctrl Pts',(-49.447481559703,-15.2583395688747,
-234.692761586072));
#195021=CARTESIAN_POINT('Ctrl Pts',(-49.4757375974629,-15.065211119735,
-234.693504723861));
#195022=CARTESIAN_POINT('Ctrl Pts',(-49.5245056367494,-14.7761840674541,
-234.694132710065));
#195023=CARTESIAN_POINT('Ctrl Pts',(-49.541826118748,-14.6799527122396,
-234.694260783696));
#195024=CARTESIAN_POINT('Ctrl Pts',(-49.5694111218869,-14.5357826896111,
-234.694330393278));
#195025=CARTESIAN_POINT('Ctrl Pts',(-49.5788735335699,-14.4877555214266,
-234.694333171033));
#195026=CARTESIAN_POINT('Ctrl Pts',(-49.5910368335956,-14.4277595736188,
-234.694310981262));
#195027=CARTESIAN_POINT('Ctrl Pts',(-49.5934862584839,-14.4157622847663,
-234.694305260041));
#195028=CARTESIAN_POINT('Ctrl Pts',(-49.5984186660568,-14.3917715371195,
-234.694291247101));
#195029=CARTESIAN_POINT('Ctrl Pts',(-49.601629194319,-14.3764341527676,
-234.694204879058));
#195030=CARTESIAN_POINT('Ctrl Pts',(-49.6104693915555,-14.3335287121791,
-234.694019980594));
#195031=CARTESIAN_POINT('Ctrl Pts',(-49.6162722792166,-14.3049159326432,
-234.693896646787));
#195032=CARTESIAN_POINT('Ctrl Pts',(-49.8047861711799,-13.3603876769755,
-234.689824088937));
#195033=CARTESIAN_POINT('Ctrl Pts',(-49.8960649973424,-12.4346978471695,
-234.685773671066));
#195034=CARTESIAN_POINT('Ctrl Pts',(-49.8949598896238,-11.0313054978619,
-234.679480960353));
#195035=CARTESIAN_POINT('Ctrl Pts',(-49.8711700349691,-10.5599358864017,
-234.677346993428));
#195036=CARTESIAN_POINT('Ctrl Pts',(-49.8004745098102,-9.85880425002941,
-234.674134280509));
#195037=CARTESIAN_POINT('Ctrl Pts',(-49.7710962529965,-9.6257783261272,
-234.673063209476));
#195038=CARTESIAN_POINT('Ctrl Pts',(-49.7182786558539,-9.27715936120124,
-234.671450744111));
#195039=CARTESIAN_POINT('Ctrl Pts',(-49.6992152109465,-9.16112648968467,
-234.670913719678));
#195040=CARTESIAN_POINT('Ctrl Pts',(-49.6684261500172,-8.98732302167439,
-234.670108006972));
#195041=CARTESIAN_POINT('Ctrl Pts',(-49.6577973805173,-8.92942951287929,
-234.669839408363));
#195042=CARTESIAN_POINT('Ctrl Pts',(-49.641303745405,-8.84264899186087,
-234.669436375258));
#195043=CARTESIAN_POINT('Ctrl Pts',(-49.6357141138013,-8.81373210902702,
-234.669302008454));
#195044=CARTESIAN_POINT('Ctrl Pts',(-49.6271917458389,-8.77037150869081,
-234.669100413908));
#195045=CARTESIAN_POINT('Ctrl Pts',(-49.6243279693599,-8.75592042928144,
-234.669033208336));
#195046=CARTESIAN_POINT('Ctrl Pts',(-49.619010147934,-8.72930425914983,
-234.668909392277));
#195047=CARTESIAN_POINT('Ctrl Pts',(-49.6164243197397,-8.71628486654336,
-234.668786528383));
#195048=CARTESIAN_POINT('Ctrl Pts',(-49.6141588435918,-8.70526933620937,
-234.668797542549));
#195049=CARTESIAN_POINT('',(-49.5702506762146,-3.34422295956514,-234.635326079404));
#195050=CARTESIAN_POINT('Ctrl Pts',(-49.6141588435918,-8.70526933620937,
-234.668797542549));
#195051=CARTESIAN_POINT('Ctrl Pts',(-49.6137159717685,-8.7032079193402,
-234.668825566832));
#195052=CARTESIAN_POINT('Ctrl Pts',(-49.6132991067888,-8.70121390385896,
-234.668837203907));
#195053=CARTESIAN_POINT('Ctrl Pts',(-49.4494831990987,-7.92721199780516,
-234.676385127567));
#195054=CARTESIAN_POINT('Ctrl Pts',(-49.354763767086,-7.14595069243807,
-234.678429733985));
#195055=CARTESIAN_POINT('Ctrl Pts',(-49.3161672816753,-5.96285252589225,
-234.673513733305));
#195056=CARTESIAN_POINT('Ctrl Pts',(-49.3207737741258,-5.56761683301845,
-234.670516269794));
#195057=CARTESIAN_POINT('Ctrl Pts',(-49.3643010504721,-4.7824439659427,
-234.66181072458));
#195058=CARTESIAN_POINT('Ctrl Pts',(-49.4032038353068,-4.39163744274392,
-234.656081092301));
#195059=CARTESIAN_POINT('Ctrl Pts',(-49.4870286161152,-3.80808467387458,
-234.645331813477));
#195060=CARTESIAN_POINT('Ctrl Pts',(-49.5192166088196,-3.61402952773642,
-234.641386355201));
#195061=CARTESIAN_POINT('Ctrl Pts',(-49.5602193207635,-3.39629338221077,
-234.636512404777));
#195062=CARTESIAN_POINT('Ctrl Pts',(-49.5648417594533,-3.37210848059925,
-234.635964796292));
#195063=CARTESIAN_POINT('Ctrl Pts',(-49.569763243633,-3.34673339462103,
-234.63538362583));
#195064=CARTESIAN_POINT('Ctrl Pts',(-49.5699972088521,-3.34549415662508,
-234.63536535131));
#195065=CARTESIAN_POINT('Ctrl Pts',(-49.5702506762146,-3.34422295956515,
-234.635326079404));
#195066=CARTESIAN_POINT('',(-49.4221349129046,2.07190323615638,-234.730930503295));
#195067=CARTESIAN_POINT('Ctrl Pts',(-49.5702506762145,-3.34422295956514,
-234.635326079404));
#195068=CARTESIAN_POINT('Ctrl Pts',(-49.5725443585339,-3.33171731241385,
-234.635256188693));
#195069=CARTESIAN_POINT('Ctrl Pts',(-49.5749633883434,-3.31606110740682,
-234.635858145233));
#195070=CARTESIAN_POINT('Ctrl Pts',(-49.5772982878406,-3.30190915561709,
-234.63612532881));
#195071=CARTESIAN_POINT('Ctrl Pts',(-49.5796331873378,-3.28775720382736,
-234.636392512386));
#195072=CARTESIAN_POINT('Ctrl Pts',(-49.5819461014599,-3.27360360893774,
-234.636659600886));
#195073=CARTESIAN_POINT('Ctrl Pts',(-49.5842370427662,-3.2594483830597,
-234.636926593251));
#195074=CARTESIAN_POINT('Ctrl Pts',(-49.5888189253789,-3.23113793130363,
-234.637460577982));
#195075=CARTESIAN_POINT('Ctrl Pts',(-49.5933129168553,-3.20282095561616,
-234.637994178256));
#195076=CARTESIAN_POINT('Ctrl Pts',(-49.5977191159129,-3.1744975522657,
-234.63852738515));
#195077=CARTESIAN_POINT('Ctrl Pts',(-49.6065315140282,-3.1178507455648,
-234.639593798937));
#195078=CARTESIAN_POINT('Ctrl Pts',(-49.6149927444874,-3.0611782285275,
-234.64065864047));
#195079=CARTESIAN_POINT('Ctrl Pts',(-49.623103570814,-3.00448076372669,
-234.641721827183));
#195080=CARTESIAN_POINT('Ctrl Pts',(-49.6393252234671,-2.89108583412506,
-234.643848200611));
#195081=CARTESIAN_POINT('Ctrl Pts',(-49.6541442741062,-2.77759734013229,
-234.645968344266));
#195082=CARTESIAN_POINT('Ctrl Pts',(-49.6675699640164,-2.66399952726585,
-234.648080155094));
#195083=CARTESIAN_POINT('Ctrl Pts',(-49.6942342683747,-2.43838678952438,
-234.652274350481));
#195084=CARTESIAN_POINT('Ctrl Pts',(-49.7154039683314,-2.21232427078163,
-234.656434408125));
#195085=CARTESIAN_POINT('Ctrl Pts',(-49.7310906888788,-1.98596836913008,
-234.660568429307));
#195086=CARTESIAN_POINT('Ctrl Pts',(-49.731200746147,-1.98438026713683,
-234.660597433398));
#195087=CARTESIAN_POINT('Ctrl Pts',(-49.7313105335634,-1.98279215070767,
-234.660626436208));
#195088=CARTESIAN_POINT('Ctrl Pts',(-49.7314200511205,-1.98120401989647,
-234.660655437739));
#195089=CARTESIAN_POINT('Ctrl Pts',(-49.7440903886979,-1.79746952081599,
-234.664010691441));
#195090=CARTESIAN_POINT('Ctrl Pts',(-49.753152861207,-1.61344027535473,
-234.667348492208));
#195091=CARTESIAN_POINT('Ctrl Pts',(-49.7585935976184,-1.42950334434026,
-234.670659997496));
#195092=CARTESIAN_POINT('Ctrl Pts',(-49.7640516342342,-1.24498153909823,
-234.673982032556));
#195093=CARTESIAN_POINT('Ctrl Pts',(-49.7658648777063,-1.06055277865886,
-234.677277604645));
#195094=CARTESIAN_POINT('Ctrl Pts',(-49.7640718178133,-0.876606063108709,
-234.680537786596));
#195095=CARTESIAN_POINT('Ctrl Pts',(-49.7632599069805,-0.793313624531679,
-234.68201402119));
#195096=CARTESIAN_POINT('Ctrl Pts',(-49.761709289772,-0.710119984785798,
-234.683482999582));
#195097=CARTESIAN_POINT('Ctrl Pts',(-49.7594270415185,-0.627061021642988,
-234.684943892965));
#195098=CARTESIAN_POINT('Ctrl Pts',(-49.7593072107643,-0.62269996312015,
-234.68502059801));
#195099=CARTESIAN_POINT('Ctrl Pts',(-49.7591853635195,-0.61833927583606,
-234.685097280766));
#195100=CARTESIAN_POINT('Ctrl Pts',(-49.7590615007317,-0.613978964973898,
-234.685173941114));
#195101=CARTESIAN_POINT('Ctrl Pts',(-49.7511603447154,-0.33583653809922,
-234.690064072969));
#195102=CARTESIAN_POINT('Ctrl Pts',(-49.7350315142723,-0.0588012353609941,
-234.694898048003));
#195103=CARTESIAN_POINT('Ctrl Pts',(-49.7107736848362,0.21714818401575,
-234.699679453349));
#195104=CARTESIAN_POINT('Ctrl Pts',(-49.6957904178448,0.387593105213088,
-234.702632770878));
#195105=CARTESIAN_POINT('Ctrl Pts',(-49.677704809517,0.557623896906549,
-234.705566032397));
#195106=CARTESIAN_POINT('Ctrl Pts',(-49.6565302394471,0.727246567549798,
-234.708480083205));
#195107=CARTESIAN_POINT('Ctrl Pts',(-49.6560765351483,0.730881046766953,
-234.708542522129));
#195108=CARTESIAN_POINT('Ctrl Pts',(-49.6556214123894,0.734515338631977,
-234.708604952234));
#195109=CARTESIAN_POINT('Ctrl Pts',(-49.6551648711012,0.738149443195642,
-234.708667373527));
#195110=CARTESIAN_POINT('Ctrl Pts',(-49.6270351753479,0.962064033984754,
-234.712513448409));
#195111=CARTESIAN_POINT('Ctrl Pts',(-49.5935238039947,1.185267081603,-234.716323147795));
#195112=CARTESIAN_POINT('Ctrl Pts',(-49.5546302331264,1.40776084764246,
-234.720064924914));
#195113=CARTESIAN_POINT('Ctrl Pts',(-49.5351834476923,1.51900773066219,
-234.721935813473));
#195114=CARTESIAN_POINT('Ctrl Pts',(-49.5143888724467,1.63007607867294,
-234.723792668997));
#195115=CARTESIAN_POINT('Ctrl Pts',(-49.4922409964726,1.74095941338489,
-234.725638579284));
#195116=CARTESIAN_POINT('Ctrl Pts',(-49.4811670584855,1.79640108074087,
-234.726561534428));
#195117=CARTESIAN_POINT('Ctrl Pts',(-49.4697549987091,1.85179661207854,
-234.727481429318));
#195118=CARTESIAN_POINT('Ctrl Pts',(-49.4580044102124,1.90714539349383,
-234.728398121989));
#195119=CARTESIAN_POINT('Ctrl Pts',(-49.452129115964,1.93481978420148,-234.728856468325));
#195120=CARTESIAN_POINT('Ctrl Pts',(-49.4461691890908,1.96248248734993,
-234.729314013782));
#195121=CARTESIAN_POINT('Ctrl Pts',(-49.4401245757343,1.99013342604581,
-234.729770739067));
#195122=CARTESIAN_POINT('Ctrl Pts',(-49.4352881443074,2.0122575655073,-234.730136175264));
#195123=CARTESIAN_POINT('Ctrl Pts',(-49.4301142570603,2.03519025837516,
-234.730650175937));
#195124=CARTESIAN_POINT('Ctrl Pts',(-49.4254861417503,2.05638458372418,
-234.73084835146));
#195125=CARTESIAN_POINT('Ctrl Pts',(-49.4243299992465,2.06167910616649,
-234.730897857389));
#195126=CARTESIAN_POINT('Ctrl Pts',(-49.4232081718496,2.06686519529321,
-234.730927654475));
#195127=CARTESIAN_POINT('Ctrl Pts',(-49.4221349129046,2.07190323615638,
-234.730930503295));
#195128=CARTESIAN_POINT('Ctrl Pts',(-49.4221408870578,2.07190450442766,
-234.730934934417));
#195129=CARTESIAN_POINT('Ctrl Pts',(-49.4182221517136,2.09035813821035,
-234.730952342309));
#195130=CARTESIAN_POINT('Ctrl Pts',(-49.4148993121985,2.10705514859158,
-234.730657481109));
#195131=CARTESIAN_POINT('Ctrl Pts',(-49.411500307874,2.12415379256605,-234.730429273799));
#195132=CARTESIAN_POINT('Ctrl Pts',(-49.3733025605228,2.31630702928812,
-234.72786469773));
#195133=CARTESIAN_POINT('Ctrl Pts',(-49.3393967227227,2.50891424783426,
-234.724974624097));
#195134=CARTESIAN_POINT('Ctrl Pts',(-49.3097301337179,2.70192914560597,
-234.721749061531));
#195135=CARTESIAN_POINT('Ctrl Pts',(-49.2503969557082,3.08795894114938,
-234.7152979364));
#195136=CARTESIAN_POINT('Ctrl Pts',(-49.207969579461,3.47650574288954,-234.70747771265));
#195137=CARTESIAN_POINT('Ctrl Pts',(-49.1824520139602,3.86385136380115,
-234.698251165921));
#195138=CARTESIAN_POINT('Ctrl Pts',(-49.1314168829586,4.63854260562436,
-234.679798072463));
#195139=CARTESIAN_POINT('Ctrl Pts',(-49.1472577098392,5.40777762062993,
-234.655885603971));
#195140=CARTESIAN_POINT('Ctrl Pts',(-49.2257062624418,6.17073512744913,
-234.625448311592));
#195141=CARTESIAN_POINT('Ctrl Pts',(-49.3041548150444,6.93369263426832,
-234.595011019214));
#195142=CARTESIAN_POINT('Ctrl Pts',(-49.4452772362161,7.69022032934419,
-234.557971217237));
#195143=CARTESIAN_POINT('Ctrl Pts',(-49.6480781836462,8.44024209637807,
-234.512742074857));
#195144=CARTESIAN_POINT('Ctrl Pts',(-48.3395182384274,8.75410525715256,
-235.35005));
#195145=CARTESIAN_POINT('Ctrl Pts',(-48.1420743191374,7.93092102614352,
-235.35005));
#195146=CARTESIAN_POINT('Ctrl Pts',(-48.0110562569534,7.1033413541692,-235.35005));
#195147=CARTESIAN_POINT('Ctrl Pts',(-47.9456204841389,6.27142206048251,
-235.35005));
#195148=CARTESIAN_POINT('Ctrl Pts',(-47.8801847113245,5.43950276679582,
-235.35005));
#195149=CARTESIAN_POINT('Ctrl Pts',(-47.8802911706055,4.60324650205529,
-235.35005));
#195150=CARTESIAN_POINT('Ctrl Pts',(-47.9494611326687,3.76242026158568,
-235.35005));
#195151=CARTESIAN_POINT('Ctrl Pts',(-47.9840461137003,3.34200714135087,
-235.35005));
#195152=CARTESIAN_POINT('Ctrl Pts',(-48.0360840389923,2.92068200696516,
-235.35005));
#195153=CARTESIAN_POINT('Ctrl Pts',(-48.1054567185474,2.50226370649453,
-235.35005));
#195154=CARTESIAN_POINT('Ctrl Pts',(-48.140143058325,2.29305455625922,-235.35005));
#195155=CARTESIAN_POINT('Ctrl Pts',(-48.179184621567,2.08432209117834,-235.35005));
#195156=CARTESIAN_POINT('Ctrl Pts',(-48.222640293554,1.87607275633673,-235.35005));
#195157=CARTESIAN_POINT('Ctrl Pts',(-48.2280722525526,1.85004158948043,
-235.35005));
#195158=CARTESIAN_POINT('Ctrl Pts',(-48.2336222090191,1.82402333761035,
-235.35005));
#195159=CARTESIAN_POINT('Ctrl Pts',(-48.2391090978947,1.79799818290319,
-235.35005));
#195160=CARTESIAN_POINT('Ctrl Pts',(-48.2445959867701,1.77197302819679,
-235.35005));
#195161=CARTESIAN_POINT('Ctrl Pts',(-48.2500003144159,1.74593883705,-235.35005));
#195162=CARTESIAN_POINT('Ctrl Pts',(-48.2553221919377,1.71989562162854,
-235.35005));
#195163=CARTESIAN_POINT('Ctrl Pts',(-48.265965946981,1.66780919078707,-235.35005));
#195164=CARTESIAN_POINT('Ctrl Pts',(-48.2762799057507,1.61568666327577,
-235.35005));
#195165=CARTESIAN_POINT('Ctrl Pts',(-48.2862649052553,1.56352813074,-235.35005));
#195166=CARTESIAN_POINT('Ctrl Pts',(-48.3062349042647,1.45921106566753,
-235.35005));
#195167=CARTESIAN_POINT('Ctrl Pts',(-48.3248891350009,1.35474998793937,
-235.35005));
#195168=CARTESIAN_POINT('Ctrl Pts',(-48.3422334665882,1.25014553997188,
-235.35005));
#195169=CARTESIAN_POINT('Ctrl Pts',(-48.4809881192878,0.41330995622679,
-235.35005));
#195170=CARTESIAN_POINT('Ctrl Pts',(-48.5368013795039,-0.432603676297867,
-235.35005));
#195171=CARTESIAN_POINT('Ctrl Pts',(-48.5074366626247,-1.28784015470909,
-235.35005));
#195172=CARTESIAN_POINT('Ctrl Pts',(-48.492754304185,-1.7154583939147,-235.35005));
#195173=CARTESIAN_POINT('Ctrl Pts',(-48.4566916340691,-2.14207645772467,
-235.35005));
#195174=CARTESIAN_POINT('Ctrl Pts',(-48.3993142685993,-2.56629662313498,
-235.35005));
#195175=CARTESIAN_POINT('Ctrl Pts',(-48.3849699272317,-2.67235166448867,
-235.35005));
#195176=CARTESIAN_POINT('Ctrl Pts',(-48.369288587157,-2.77828474965553,
-235.35005));
#195177=CARTESIAN_POINT('Ctrl Pts',(-48.3522652960998,-2.88409542692066,
-235.35005));
#195178=CARTESIAN_POINT('Ctrl Pts',(-48.3437536505715,-2.93700076555113,
-235.35005));
#195179=CARTESIAN_POINT('Ctrl Pts',(-48.3349064994319,-2.98987550057009,
-235.35005));
#195180=CARTESIAN_POINT('Ctrl Pts',(-48.3257231157807,-3.0427195656859,
-235.35005));
#195181=CARTESIAN_POINT('Ctrl Pts',(-48.3234272698678,-3.05593058196506,
-235.35005));
#195182=CARTESIAN_POINT('Ctrl Pts',(-48.3211104090812,-3.06913968134127,
-235.35005));
#195183=CARTESIAN_POINT('Ctrl Pts',(-48.3187725213423,-3.08234686271546,
-235.35005));
#195184=CARTESIAN_POINT('Ctrl Pts',(-48.3164346336033,-3.09555404408982,
-235.35005));
#195185=CARTESIAN_POINT('Ctrl Pts',(-48.3140690695364,-3.1087587009315,
-235.35005));
#195186=CARTESIAN_POINT('Ctrl Pts',(-48.31169696982,-3.12196276161221,-235.35005));
#195187=CARTESIAN_POINT('Ctrl Pts',(-48.306952770387,-3.14837088297426,
-235.35005));
#195188=CARTESIAN_POINT('Ctrl Pts',(-48.3022780138533,-3.17478533866958,
-235.35005));
#195189=CARTESIAN_POINT('Ctrl Pts',(-48.2976726119403,-3.20120612064097,
-235.35005));
#195190=CARTESIAN_POINT('Ctrl Pts',(-48.2608293966366,-3.41257237640728,
-235.35005));
#195191=CARTESIAN_POINT('Ctrl Pts',(-48.2284220495736,-3.62434325601736,
-235.35005));
#195192=CARTESIAN_POINT('Ctrl Pts',(-48.2004248943047,-3.83651641735441,
-235.35005));
#195193=CARTESIAN_POINT('Ctrl Pts',(-48.144430583767,-4.2608627400285,-235.35005));
#195194=CARTESIAN_POINT('Ctrl Pts',(-48.1060703916864,-4.6868175831452,
-235.35005));
#195195=CARTESIAN_POINT('Ctrl Pts',(-48.0854449269901,-5.11439012388267,
-235.35005));
#195196=CARTESIAN_POINT('Ctrl Pts',(-48.0648194622937,-5.54196266462014,
-235.35005));
#195197=CARTESIAN_POINT('Ctrl Pts',(-48.0619566741596,-5.97223878738515,
-235.35005));
#195198=CARTESIAN_POINT('Ctrl Pts',(-48.0771357161752,-6.40148796840999,
-235.35005));
#195199=CARTESIAN_POINT('Ctrl Pts',(-48.1074938002064,-7.25998633045966,
-235.35005));
#195200=CARTESIAN_POINT('Ctrl Pts',(-48.2090347930406,-8.11012177188801,
-235.35005));
#195201=CARTESIAN_POINT('Ctrl Pts',(-48.3817353557071,-8.95189703464271,
-235.35005));
#195202=CARTESIAN_POINT('Ctrl Pts',(-48.3844338019987,-8.96504977312313,
-235.35005));
#195203=CARTESIAN_POINT('Ctrl Pts',(-48.3871335038458,-8.97820236409949,
-235.35005));
#195204=CARTESIAN_POINT('Ctrl Pts',(-48.3898027548802,-8.99135853258005,
-235.35005));
#195205=CARTESIAN_POINT('Ctrl Pts',(-48.3924720059147,-9.00451470106053,
-235.35005));
#195206=CARTESIAN_POINT('Ctrl Pts',(-48.3951203394452,-9.01767332703754,
-235.35005));
#195207=CARTESIAN_POINT('Ctrl Pts',(-48.3977477753549,-9.03083440817268,
-235.35005));
#195208=CARTESIAN_POINT('Ctrl Pts',(-48.4030026471742,-9.05715657044287,
-235.35005));
#195209=CARTESIAN_POINT('Ctrl Pts',(-48.4081739297218,-9.08348855318059,
-235.35005));
#195210=CARTESIAN_POINT('Ctrl Pts',(-48.4132617664092,-9.10983033956203,
-235.35005));
#195211=CARTESIAN_POINT('Ctrl Pts',(-48.4234374397839,-9.16251391232474,
-235.35005));
#195212=CARTESIAN_POINT('Ctrl Pts',(-48.4332793498323,-9.21523669724522,
-235.35005));
#195213=CARTESIAN_POINT('Ctrl Pts',(-48.4427883984152,-9.26799858838481,
-235.35005));
#195214=CARTESIAN_POINT('Ctrl Pts',(-48.4618064955809,-9.37352237066414,
-235.35005));
#195215=CARTESIAN_POINT('Ctrl Pts',(-48.4794934628395,-9.47920254067582,
-235.35005));
#195216=CARTESIAN_POINT('Ctrl Pts',(-48.4958526690327,-9.58503870263172,
-235.35005));
#195217=CARTESIAN_POINT('Ctrl Pts',(-48.5285710814205,-9.79671102655205,
-235.35005));
#195218=CARTESIAN_POINT('Ctrl Pts',(-48.5559827004663,-10.0090068188147,
-235.35005));
#195219=CARTESIAN_POINT('Ctrl Pts',(-48.5780974937539,-10.2219249084145,
-235.35005));
#195220=CARTESIAN_POINT('Ctrl Pts',(-48.6223270803283,-10.6477610876057,
-235.35005));
#195221=CARTESIAN_POINT('Ctrl Pts',(-48.6453046119738,-11.0773736644268,
-235.35005));
#195222=CARTESIAN_POINT('Ctrl Pts',(-48.6469140232755,-11.5038145314612,
-235.35005));
#195223=CARTESIAN_POINT('Ctrl Pts',(-48.6501328458788,-12.3566962655301,
-235.35005));
#195224=CARTESIAN_POINT('Ctrl Pts',(-48.5694097707119,-13.201098145554,
-235.35005));
#195225=CARTESIAN_POINT('Ctrl Pts',(-48.4050646665376,-14.0370524847357,
-235.35005));
#195226=CARTESIAN_POINT('Ctrl Pts',(-48.3999288820313,-14.0631760578391,
-235.35005));
#195227=CARTESIAN_POINT('Ctrl Pts',(-48.3947106332613,-14.0892913003493,
-235.35005));
#195228=CARTESIAN_POINT('Ctrl Pts',(-48.3894097433237,-14.1153981944164,
-235.35005));
#195229=CARTESIAN_POINT('Ctrl Pts',(-48.386759298355,-14.1284516414493,
-235.35005));
#195230=CARTESIAN_POINT('Ctrl Pts',(-48.3840780942122,-14.1415019811713,
-235.35005));
#195231=CARTESIAN_POINT('Ctrl Pts',(-48.3814002229133,-14.1545526575822,
-235.35005));
#195232=CARTESIAN_POINT('Ctrl Pts',(-48.3787223516144,-14.1676033339926,
-235.35005));
#195233=CARTESIAN_POINT('Ctrl Pts',(-48.3760618299286,-14.1806557630669,
-235.35005));
#195234=CARTESIAN_POINT('Ctrl Pts',(-48.3734186404716,-14.1937099430552,
-235.35005));
#195235=CARTESIAN_POINT('Ctrl Pts',(-48.3628458826442,-14.2459266630052,
-235.35005));
#195236=CARTESIAN_POINT('Ctrl Pts',(-48.3525504293979,-14.2981713964018,
-235.35005));
#195237=CARTESIAN_POINT('Ctrl Pts',(-48.3425312602132,-14.350444040166,
-235.35005));
#195238=CARTESIAN_POINT('Ctrl Pts',(-48.3224929218452,-14.4549893276876,
-235.35005));
#195239=CARTESIAN_POINT('Ctrl Pts',(-48.3035595794002,-14.5596462424789,
-235.35005));
#195240=CARTESIAN_POINT('Ctrl Pts',(-48.2857247802083,-14.6644141326663,
-235.35005));
#195241=CARTESIAN_POINT('Ctrl Pts',(-48.2500551818223,-14.8739499130538,
-235.35005));
#195242=CARTESIAN_POINT('Ctrl Pts',(-48.2187775910825,-15.0839293763357,
-235.35005));
#195243=CARTESIAN_POINT('Ctrl Pts',(-48.1918669286016,-15.2943499889772,
-235.35005));
#195244=CARTESIAN_POINT('Ctrl Pts',(-48.13804560364,-15.71519121426,-235.35005));
#195245=CARTESIAN_POINT('Ctrl Pts',(-48.1017687499494,-16.1377801895464,
-235.35005));
#195246=CARTESIAN_POINT('Ctrl Pts',(-48.0829143862637,-16.5595284917746,
-235.35005));
#195247=CARTESIAN_POINT('Ctrl Pts',(-48.0452056588921,-17.4030250962311,
-235.35005));
#195248=CARTESIAN_POINT('Ctrl Pts',(-48.0765553835769,-18.2457723122303,
-235.35005));
#195249=CARTESIAN_POINT('Ctrl Pts',(-48.1770201828715,-19.0877695253175,
-235.35005));
#195250=CARTESIAN_POINT('Ctrl Pts',(-48.2021363826951,-19.2982688285893,
-235.35005));
#195251=CARTESIAN_POINT('Ctrl Pts',(-48.2315724527786,-19.5085474359751,
-235.35005));
#195252=CARTESIAN_POINT('Ctrl Pts',(-48.2653424827524,-19.7185300485352,
-235.35005));
#195253=CARTESIAN_POINT('Ctrl Pts',(-48.2737849902462,-19.7710257016774,
-235.35005));
#195254=CARTESIAN_POINT('Ctrl Pts',(-48.282498702759,-19.8235043364666,
-235.35005));
#195255=CARTESIAN_POINT('Ctrl Pts',(-48.2914842922534,-19.8759659107496,
-235.35005));
#195256=CARTESIAN_POINT('Ctrl Pts',(-48.2959770870004,-19.9021966978899,
-235.35005));
#195257=CARTESIAN_POINT('Ctrl Pts',(-48.300537852968,-19.9284232197822,
-235.35005));
#195258=CARTESIAN_POINT('Ctrl Pts',(-48.3051666862202,-19.9546454703855,
-235.35005));
#195259=CARTESIAN_POINT('Ctrl Pts',(-48.3074811028462,-19.967756595687,
-235.35005));
#195260=CARTESIAN_POINT('Ctrl Pts',(-48.3098125364066,-19.9808666531674,
-235.35005));
#195261=CARTESIAN_POINT('Ctrl Pts',(-48.3121609996811,-19.9939756420136,
-235.35005));
#195262=CARTESIAN_POINT('Ctrl Pts',(-48.3145094629556,-20.0070846308597,
-235.35005));
#195263=CARTESIAN_POINT('Ctrl Pts',(-48.3168699428148,-20.0201928656576,
-235.35005));
#195264=CARTESIAN_POINT('Ctrl Pts',(-48.3191971709643,-20.0333031870275,
-235.35005));
#195265=CARTESIAN_POINT('Ctrl Pts',(-48.337814996161,-20.1381857579874,
-235.35005));
#195266=CARTESIAN_POINT('Ctrl Pts',(-48.3550896009549,-20.2431526171762,
-235.35005));
#195267=CARTESIAN_POINT('Ctrl Pts',(-48.3710295920234,-20.3482032245128,
-235.35005));
#195268=CARTESIAN_POINT('Ctrl Pts',(-48.4347895562984,-20.7684056538652,
-235.35005));
#195269=CARTESIAN_POINT('Ctrl Pts',(-48.4772403630263,-21.1899452510779,
-235.35005));
#195270=CARTESIAN_POINT('Ctrl Pts',(-48.4986731253089,-21.612803748536,
-235.35005));
#195271=CARTESIAN_POINT('Ctrl Pts',(-48.541538649874,-22.458520743452,-235.35005));
#195272=CARTESIAN_POINT('Ctrl Pts',(-48.5005032095075,-23.3116677382499,
-235.35005));
#195273=CARTESIAN_POINT('Ctrl Pts',(-48.3713478679476,-24.1646010300614,
-235.35005));
#195274=CARTESIAN_POINT('Ctrl Pts',(-48.3390590325577,-24.3778343530143,
-235.35005));
#195275=CARTESIAN_POINT('Ctrl Pts',(-48.3012455308435,-24.5909867391319,
-235.35005));
#195276=CARTESIAN_POINT('Ctrl Pts',(-48.2577770486563,-24.8040562792487,
-235.35005));
#195277=CARTESIAN_POINT('Ctrl Pts',(-48.2523434883829,-24.8306899717632,
-235.35005));
#195278=CARTESIAN_POINT('Ctrl Pts',(-48.2468215386317,-24.8573223693642,
-235.35005));
#195279=CARTESIAN_POINT('Ctrl Pts',(-48.2412109184648,-24.8839534679411,
-235.35005));
#195280=CARTESIAN_POINT('Ctrl Pts',(-48.235600298298,-24.9105845665175,
-235.35005));
#195281=CARTESIAN_POINT('Ctrl Pts',(-48.2299135976341,-24.9372145504959,
-235.35005));
#195282=CARTESIAN_POINT('Ctrl Pts',(-48.2243539041553,-24.9638463951525,
-235.35005));
#195283=CARTESIAN_POINT('Ctrl Pts',(-48.2132345171977,-25.0171100844654,
-235.35005));
#195284=CARTESIAN_POINT('Ctrl Pts',(-48.2024091551918,-25.0703780812439,
-235.35005));
#195285=CARTESIAN_POINT('Ctrl Pts',(-48.1918756280125,-25.1236503534574,
-235.35005));
#195286=CARTESIAN_POINT('Ctrl Pts',(-48.1708085736529,-25.2301948978888,
-235.35005));
#195287=CARTESIAN_POINT('Ctrl Pts',(-48.1509087142019,-25.3367565417865,
-235.35005));
#195288=CARTESIAN_POINT('Ctrl Pts',(-48.1321603275509,-25.4433350548857,
-235.35005));
#195289=CARTESIAN_POINT('Ctrl Pts',(-48.0571667809486,-25.8696491072753,
-235.35005));
#195290=CARTESIAN_POINT('Ctrl Pts',(-48.000556289184,-26.2962324731006,
-235.35005));
#195291=CARTESIAN_POINT('Ctrl Pts',(-47.9616645382749,-26.7230754200676,
-235.35005));
#195292=CARTESIAN_POINT('Ctrl Pts',(-47.8838810364566,-27.5767613140017,
-235.35005));
#195293=CARTESIAN_POINT('Ctrl Pts',(-47.87663302545,-28.4314805592623,-235.35005));
#195294=CARTESIAN_POINT('Ctrl Pts',(-47.9382574172368,-29.287208791445,
-235.35005));
#195295=CARTESIAN_POINT('Ctrl Pts',(-47.9998818090236,-30.1429370236277,
-235.35005));
#195296=CARTESIAN_POINT('Ctrl Pts',(-48.1303735979639,-30.9996741692801,
-235.35005));
#195297=CARTESIAN_POINT('Ctrl Pts',(-48.3327003568643,-31.8574637039839,
-235.35005));
#195298=CARTESIAN_POINT('Ctrl Pts',(-48.3307545488269,-31.8493376071772,
-235.35004999994));
#195299=CARTESIAN_POINT('Ctrl Pts',(-49.2665966890958,-31.6249695531388,
-235.350058621518));
#195300=CARTESIAN_POINT('Ctrl Pts',(-49.6566766583008,-31.531451804001,
-234.47528355851));
#195301=CARTESIAN_POINT('Ctrl Pts',(-48.372551678047,-32.0237574776621,
-235.350049999945));
#195302=CARTESIAN_POINT('Ctrl Pts',(-49.2656683159424,-31.8826538814243,
-235.350057688891));
#195303=CARTESIAN_POINT('Ctrl Pts',(-49.6877952499862,-31.818666798948,
-234.555234217691));
#195304=CARTESIAN_POINT('Ctrl Pts',(-48.393897970712,-32.2007826737009,
-235.35004999995));
#195305=CARTESIAN_POINT('Ctrl Pts',(-49.2406129702643,-32.143223893466,
-235.350056855992));
#195306=CARTESIAN_POINT('Ctrl Pts',(-49.6816879330612,-32.1154681493768,
-234.629557346798));
#195307=CARTESIAN_POINT('Ctrl Pts',(-48.3876860767769,-32.3803569706164,
-235.350049999955));
#195308=CARTESIAN_POINT('Ctrl Pts',(-49.1793203036772,-32.4078529308044,
-235.350056136573));
#195309=CARTESIAN_POINT('Ctrl Pts',(-49.6257204831723,-32.4233553155217,
-234.695894022066));
#195310=CARTESIAN_POINT('',(-49.628292312036,-32.4090169804993,-234.692797218033));
#195311=CARTESIAN_POINT('',(-48.3879672519817,-32.371991693197,-235.35005));
#195312=CARTESIAN_POINT('Origin',(-48.3879672519817,-32.371991693197,-233.85005));
#195313=CARTESIAN_POINT('Ctrl Pts',(-49.628292311974,-32.4090169808449,
-234.692797218109));
#195314=CARTESIAN_POINT('Ctrl Pts',(-49.6810233914157,-32.1110273722408,
-234.628281397553));
#195315=CARTESIAN_POINT('Ctrl Pts',(-49.687128176312,-31.8234236701372,
-234.556301998219));
#195316=CARTESIAN_POINT('Ctrl Pts',(-49.6580996754574,-31.544841856517,
-234.479004868619));
#195317=CARTESIAN_POINT('Ctrl Pts',(-48.3327003568643,-31.8574637039841,
-235.35005));
#195318=CARTESIAN_POINT('Ctrl Pts',(-48.3726098627487,-32.0266650324685,
-235.35005));
#195319=CARTESIAN_POINT('Ctrl Pts',(-48.3931627529261,-32.1979455093617,
-235.35005));
#195320=CARTESIAN_POINT('Ctrl Pts',(-48.3879672519817,-32.371991693197,
-235.35005));
#195321=CARTESIAN_POINT('Ctrl Pts',(-48.3879672519816,-32.371991693197,
-235.35005));
#195322=CARTESIAN_POINT('Ctrl Pts',(-49.1821150693849,-32.3956980201291,
-235.35005));
#195323=CARTESIAN_POINT('Ctrl Pts',(-49.6282923119739,-32.4090169808449,
-234.692797218109));
#195324=CARTESIAN_POINT('Ctrl Pts',(-48.3122036088614,-34.9100285686315,
-235.35005));
#195325=CARTESIAN_POINT('Ctrl Pts',(-49.1048103477618,-34.9355482471023,
-235.350050000493));
#195326=CARTESIAN_POINT('Ctrl Pts',(-49.5510892026461,-34.9515478422503,
-234.694718333571));
#195327=CARTESIAN_POINT('Ctrl Pts',(-48.2225732111533,-37.4475766604583,
-235.35005));
#195328=CARTESIAN_POINT('Ctrl Pts',(-49.0133760622712,-37.4755964900674,
-235.350049998731));
#195329=CARTESIAN_POINT('Ctrl Pts',(-49.4597789489883,-37.4935285423766,
-234.696950276065));
#195330=CARTESIAN_POINT('Ctrl Pts',(-48.1190600870606,-39.984633316822,
-235.35005));
#195331=CARTESIAN_POINT('Ctrl Pts',(-48.9077504789076,-40.0168122617172,
-235.35005));
#195332=CARTESIAN_POINT('Ctrl Pts',(-49.3543621196711,-40.035034230092,
-234.699454871761));
#195333=CARTESIAN_POINT('',(-49.354362119671,-40.035034230092,-234.699454871761));
#195334=CARTESIAN_POINT('',(-48.1190600870606,-39.9846333168228,-235.35005));
#195335=CARTESIAN_POINT('Origin',(-48.1190600870606,-39.9846333168229,-233.85005));
#195336=CARTESIAN_POINT('Origin',(637.300587775051,-11.5397323655281,-248.898224599212));
#195337=CARTESIAN_POINT('Origin',(647.878174797988,-11.588320224684,-235.350049996435));
#195338=CARTESIAN_POINT('Ctrl Pts',(-48.1190600870606,-39.9846333168228,
-235.35005));
#195339=CARTESIAN_POINT('Ctrl Pts',(-48.9077504789077,-40.0168122617177,
-235.35005));
#195340=CARTESIAN_POINT('Ctrl Pts',(-49.3543621196712,-40.0350342300922,
-234.69945487176));
#195341=CARTESIAN_POINT('Ctrl Pts',(-48.1156571344711,-40.0680385041539,
-235.35005));
#195342=CARTESIAN_POINT('Ctrl Pts',(-48.8941878304705,-40.1139469219292,
-235.350049999983));
#195343=CARTESIAN_POINT('Ctrl Pts',(-49.3415926503895,-40.1404174549493,
-234.711772602598));
#195344=CARTESIAN_POINT('Ctrl Pts',(-48.1094046180063,-40.1511102451508,
-235.35005));
#195345=CARTESIAN_POINT('Ctrl Pts',(-48.8709781715377,-40.2220121424719,
-235.35004999999));
#195346=CARTESIAN_POINT('Ctrl Pts',(-49.3183790954466,-40.2639303612825,
-234.731242016098));
#195347=CARTESIAN_POINT('Ctrl Pts',(-48.0952241561347,-40.2752167333539,
-235.35005));
#195348=CARTESIAN_POINT('Ctrl Pts',(-48.8404013751985,-40.3682352258384,
-235.350050000006));
#195349=CARTESIAN_POINT('Ctrl Pts',(-49.2869295306867,-40.4240408437502,
-234.748883360049));
#195350=CARTESIAN_POINT('Ctrl Pts',(-48.0899153448806,-40.3165225558374,
-235.35005));
#195351=CARTESIAN_POINT('Ctrl Pts',(-48.830421545654,-40.4157032323804,
-235.35005));
#195352=CARTESIAN_POINT('Ctrl Pts',(-49.2765808080252,-40.4755275655264,
-234.753809123677));
#195353=CARTESIAN_POINT('Ctrl Pts',(-48.0779218876032,-40.3989852515461,
-235.35005));
#195354=CARTESIAN_POINT('Ctrl Pts',(-48.8066893271687,-40.513370761674,
-235.350049999999));
#195355=CARTESIAN_POINT('Ctrl Pts',(-49.251626649492,-40.5832746725427,
-234.765851629537));
#195356=CARTESIAN_POINT('Ctrl Pts',(-48.0712183175412,-40.4401628322643,
-235.350050000001));
#195357=CARTESIAN_POINT('Ctrl Pts',(-48.7934838819703,-40.5628189902028,
-235.350050000007));
#195358=CARTESIAN_POINT('Ctrl Pts',(-49.2375840222482,-40.6383093361276,
-234.772359011183));
#195359=CARTESIAN_POINT('Ctrl Pts',(-48.0561422093234,-40.5222290742639,
-235.350050000001));
#195360=CARTESIAN_POINT('Ctrl Pts',(-48.764457764962,-40.6622349257811,
-235.350049999994));
#195361=CARTESIAN_POINT('Ctrl Pts',(-49.2063354527156,-40.7496495874624,
-234.785817239668));
#195362=CARTESIAN_POINT('Ctrl Pts',(-48.047773596518,-40.5630852304628,
-235.35005));
#195363=CARTESIAN_POINT('Ctrl Pts',(-48.7495575164579,-40.7110546556452,
-235.350050000008));
#195364=CARTESIAN_POINT('Ctrl Pts',(-49.1901931274652,-40.8040214971111,
-234.791881131089));
#195365=CARTESIAN_POINT('Ctrl Pts',(-48.0296425423562,-40.6445005636306,
-235.35005));
#195366=CARTESIAN_POINT('Ctrl Pts',(-48.7198529923868,-40.8064170701649,
-235.35004999999));
#195367=CARTESIAN_POINT('Ctrl Pts',(-49.1580329424021,-40.9092699497394,
-234.80233714665));
#195368=CARTESIAN_POINT('Ctrl Pts',(-48.0199029877981,-40.6850741153181,
-235.35005));
#195369=CARTESIAN_POINT('Ctrl Pts',(-48.7056393397796,-40.8523724308093,
-235.350049999989));
#195370=CARTESIAN_POINT('Ctrl Pts',(-49.1427597364121,-40.9590683152935,
-234.806236550506));
#195371=CARTESIAN_POINT('Ctrl Pts',(-47.9992940161415,-40.7659290146224,
-235.35005));
#195372=CARTESIAN_POINT('Ctrl Pts',(-48.6746942895135,-40.9454780254451,
-235.35005000001));
#195373=CARTESIAN_POINT('Ctrl Pts',(-49.1091912161129,-41.0610374960301,
-234.815043280514));
#195374=CARTESIAN_POINT('Ctrl Pts',(-47.9883597239418,-40.8062069855079,
-235.35005));
#195375=CARTESIAN_POINT('Ctrl Pts',(-48.6576049577959,-40.9929195436597,
-235.350049999994));
#195376=CARTESIAN_POINT('Ctrl Pts',(-49.0904332941573,-41.1137361405253,
-234.82018153471));
#195377=CARTESIAN_POINT('Ctrl Pts',(-47.9648484820867,-40.886240947879,
-235.35005));
#195378=CARTESIAN_POINT('Ctrl Pts',(-48.6202908038635,-41.0885568169624,
-235.350050000006));
#195379=CARTESIAN_POINT('Ctrl Pts',(-49.0490372574119,-41.2209607216622,
-234.831270117331));
#195380=CARTESIAN_POINT('Ctrl Pts',(-47.9522083925962,-40.9259746645696,
-235.35005));
#195381=CARTESIAN_POINT('Ctrl Pts',(-48.6000967774269,-41.136585315531,
-235.350050000005));
#195382=CARTESIAN_POINT('Ctrl Pts',(-49.0264208357049,-41.2752201799367,
-234.837105794306));
#195383=CARTESIAN_POINT('Ctrl Pts',(-47.9122208177014,-41.0445137282603,
-235.35005));
#195384=CARTESIAN_POINT('Ctrl Pts',(-48.5437175410231,-41.2731792254645,
-235.350049999989));
#195385=CARTESIAN_POINT('Ctrl Pts',(-48.964349840243,-41.4256874560579,
-234.84928310824));
#195386=CARTESIAN_POINT('Ctrl Pts',(-47.8834173029482,-41.1228515949417,
-235.35005));
#195387=CARTESIAN_POINT('Ctrl Pts',(-48.5108776537541,-41.3567902125311,
-235.350049999988));
#195388=CARTESIAN_POINT('Ctrl Pts',(-48.9298467764963,-41.513182231287,
-234.851751686106));
#195389=CARTESIAN_POINT('Ctrl Pts',(-47.8371337927352,-41.2386632571498,
-235.35005));
#195390=CARTESIAN_POINT('Ctrl Pts',(-48.4472327735751,-41.4907743916649,
-235.350050000005));
#195391=CARTESIAN_POINT('Ctrl Pts',(-48.8593613765109,-41.6611254214954,
-234.863347210043));
#195392=CARTESIAN_POINT('Ctrl Pts',(-47.8210253111431,-41.2769359664061,
-235.35005));
#195393=CARTESIAN_POINT('Ctrl Pts',(-48.4238255405523,-41.5362680262328,
-235.35005));
#195394=CARTESIAN_POINT('Ctrl Pts',(-48.832972869674,-41.7123406931751,
-234.868203498974));
#195395=CARTESIAN_POINT('Ctrl Pts',(-47.787220073548,-41.3527085858238,
-235.35005));
#195396=CARTESIAN_POINT('Ctrl Pts',(-48.3763605083435,-41.6250538530374,
-235.35005));
#195397=CARTESIAN_POINT('Ctrl Pts',(-48.7797020312914,-41.8115618811122,
-234.877028502702));
#195398=CARTESIAN_POINT('Ctrl Pts',(-47.7696001307559,-41.3902458706063,
-235.35005));
#195399=CARTESIAN_POINT('Ctrl Pts',(-48.3541637623008,-41.6669126397123,
-235.350050000011));
#195400=CARTESIAN_POINT('Ctrl Pts',(-48.7554615646751,-41.8568726544237,
-234.879814510279));
#195401=CARTESIAN_POINT('Ctrl Pts',(-47.7335555457799,-41.4649289014138,
-235.35005));
#195402=CARTESIAN_POINT('Ctrl Pts',(-48.3105107159968,-41.7488046878741,
-235.350049999989));
#195403=CARTESIAN_POINT('Ctrl Pts',(-48.7083373512675,-41.9445758791192,
-234.884369803896));
#195404=CARTESIAN_POINT('Ctrl Pts',(-47.7151163766151,-41.5020675791261,
-235.35005));
#195405=CARTESIAN_POINT('Ctrl Pts',(-48.2891485822549,-41.7887312087111,
-235.35005));
#195406=CARTESIAN_POINT('Ctrl Pts',(-48.6856039311336,-41.9867349750483,
-234.886044416602));
#195407=CARTESIAN_POINT('Ctrl Pts',(-47.6870475431915,-41.5575760651628,
-235.35005));
#195408=CARTESIAN_POINT('Ctrl Pts',(-48.2574046215262,-41.847779872134,
-235.35005));
#195409=CARTESIAN_POINT('Ctrl Pts',(-48.6521086576215,-42.0486144262277,
-234.888099431162));
#195410=CARTESIAN_POINT('Ctrl Pts',(-47.677640411345,-41.5760541500354,
-235.35005));
#195411=CARTESIAN_POINT('Ctrl Pts',(-48.2470403251889,-41.8672107704492,
-235.35005));
#195412=CARTESIAN_POINT('Ctrl Pts',(-48.6412778638178,-42.0688098769786,
-234.888619834342));
#195413=CARTESIAN_POINT('Ctrl Pts',(-47.6585760783126,-41.6128886447362,
-235.35005));
#195414=CARTESIAN_POINT('Ctrl Pts',(-48.2228963762585,-41.9084918903695,
-235.35005));
#195415=CARTESIAN_POINT('Ctrl Pts',(-48.6147495311229,-42.113763065292,
-234.891630453002));
#195416=CARTESIAN_POINT('Ctrl Pts',(-47.6488991764614,-41.6312354689061,
-235.35005));
#195417=CARTESIAN_POINT('Ctrl Pts',(-48.2093956206664,-41.9300731458053,
-235.350050000003));
#195418=CARTESIAN_POINT('Ctrl Pts',(-48.5994498402746,-42.1380513796496,
-234.893925232714));
#195419=CARTESIAN_POINT('Ctrl Pts',(-47.6191741486339,-41.6859381083017,
-235.35005));
#195420=CARTESIAN_POINT('Ctrl Pts',(-48.1671827615658,-41.9951014194116,
-235.350049999995));
#195421=CARTESIAN_POINT('Ctrl Pts',(-48.5512188371181,-42.211817336402,
-234.901278569161));
#195422=CARTESIAN_POINT('Ctrl Pts',(-47.5984065010933,-41.7219438293822,
-235.35005));
#195423=CARTESIAN_POINT('Ctrl Pts',(-48.1381497307774,-42.0377252505059,
-235.350050000006));
#195424=CARTESIAN_POINT('Ctrl Pts',(-48.5180631792116,-42.2600391416596,
-234.905912731492));
#195425=CARTESIAN_POINT('Ctrl Pts',(-47.5555678143129,-41.7933210863947,
-235.35005));
#195426=CARTESIAN_POINT('Ctrl Pts',(-48.0836613352502,-42.1183565908771,
-235.350049999994));
#195427=CARTESIAN_POINT('Ctrl Pts',(-48.457597592579,-42.3485528957682,
-234.91222746163));
#195428=CARTESIAN_POINT('Ctrl Pts',(-47.5335333913842,-41.8287112184799,
-235.35005));
#195429=CARTESIAN_POINT('Ctrl Pts',(-48.0574563285157,-42.1570164665365,
-235.350049999952));
#195430=CARTESIAN_POINT('Ctrl Pts',(-48.4291976744607,-42.3899883957637,
-234.914384660568));
#195431=CARTESIAN_POINT('Ctrl Pts',(-47.511140470057,-41.8639253579254,
-235.35005));
#195432=CARTESIAN_POINT('Ctrl Pts',(-48.0316514259825,-42.1949218242413,
-235.35005));
#195433=CARTESIAN_POINT('Ctrl Pts',(-48.4015825627194,-42.4301635567087,
-234.916111528175));
#195434=CARTESIAN_POINT('',(-48.4015825627194,-42.4301635567086,-234.916111528175));
#195435=CARTESIAN_POINT('',(-47.511140470057,-41.8639253579254,-235.35005));
#195436=CARTESIAN_POINT('Origin',(-47.5111404700569,-41.8639253579254,-233.85005));
#195437=CARTESIAN_POINT('Ctrl Pts',(-48.4015825627194,-42.4301635567086,
-234.916111528175));
#195438=CARTESIAN_POINT('Ctrl Pts',(-48.4291976744607,-42.3899883957637,
-234.914384660568));
#195439=CARTESIAN_POINT('Ctrl Pts',(-48.457597592579,-42.3485528957682,
-234.91222746163));
#195440=CARTESIAN_POINT('Ctrl Pts',(-48.5180631792116,-42.2600391416596,
-234.905912731492));
#195441=CARTESIAN_POINT('Ctrl Pts',(-48.5512188371181,-42.211817336402,
-234.901278569161));
#195442=CARTESIAN_POINT('Ctrl Pts',(-48.5994498402746,-42.1380513796496,
-234.893925232714));
#195443=CARTESIAN_POINT('Ctrl Pts',(-48.6147495311229,-42.113763065292,
-234.891630453002));
#195444=CARTESIAN_POINT('Ctrl Pts',(-48.6412778638178,-42.0688098769786,
-234.888619834342));
#195445=CARTESIAN_POINT('Ctrl Pts',(-48.6521086576215,-42.0486144262277,
-234.888099431162));
#195446=CARTESIAN_POINT('Ctrl Pts',(-48.6856039311336,-41.9867349750483,
-234.886044416602));
#195447=CARTESIAN_POINT('Ctrl Pts',(-48.7083373512675,-41.9445758791192,
-234.884369803896));
#195448=CARTESIAN_POINT('Ctrl Pts',(-48.7554615646751,-41.8568726544237,
-234.879814510279));
#195449=CARTESIAN_POINT('Ctrl Pts',(-48.7797020312914,-41.8115618811122,
-234.877028502702));
#195450=CARTESIAN_POINT('Ctrl Pts',(-48.832972869674,-41.7123406931751,
-234.868203498974));
#195451=CARTESIAN_POINT('Ctrl Pts',(-48.8593613765109,-41.6611254214954,
-234.863347210043));
#195452=CARTESIAN_POINT('Ctrl Pts',(-48.9298467764963,-41.513182231287,
-234.851751686106));
#195453=CARTESIAN_POINT('Ctrl Pts',(-48.964349840243,-41.4256874560579,
-234.84928310824));
#195454=CARTESIAN_POINT('Ctrl Pts',(-49.0264208357049,-41.2752201799367,
-234.837105794306));
#195455=CARTESIAN_POINT('Ctrl Pts',(-49.0490372574119,-41.2209607216622,
-234.831270117331));
#195456=CARTESIAN_POINT('Ctrl Pts',(-49.0904332941573,-41.1137361405253,
-234.82018153471));
#195457=CARTESIAN_POINT('Ctrl Pts',(-49.1091912161129,-41.0610374960301,
-234.815043280514));
#195458=CARTESIAN_POINT('Ctrl Pts',(-49.1427597364121,-40.9590683152935,
-234.806236550506));
#195459=CARTESIAN_POINT('Ctrl Pts',(-49.1580329424021,-40.9092699497394,
-234.80233714665));
#195460=CARTESIAN_POINT('Ctrl Pts',(-49.1901931274652,-40.8040214971111,
-234.791881131089));
#195461=CARTESIAN_POINT('Ctrl Pts',(-49.2063354527156,-40.7496495874624,
-234.785817239668));
#195462=CARTESIAN_POINT('Ctrl Pts',(-49.2375840222482,-40.6383093361276,
-234.772359011183));
#195463=CARTESIAN_POINT('Ctrl Pts',(-49.251626649492,-40.5832746725427,
-234.765851629537));
#195464=CARTESIAN_POINT('Ctrl Pts',(-49.2765808080252,-40.4755275655264,
-234.753809123677));
#195465=CARTESIAN_POINT('Ctrl Pts',(-49.2869295306867,-40.4240408437502,
-234.748883360049));
#195466=CARTESIAN_POINT('Ctrl Pts',(-49.3183790954466,-40.2639303612825,
-234.731242016098));
#195467=CARTESIAN_POINT('Ctrl Pts',(-49.3415926503895,-40.1404174549493,
-234.711772602598));
#195468=CARTESIAN_POINT('Ctrl Pts',(-49.354362119671,-40.035034230092,-234.699454871761));
#195469=CARTESIAN_POINT('Ctrl Pts',(-48.1190600870606,-39.9846333168228,
-235.35005));
#195470=CARTESIAN_POINT('Ctrl Pts',(-48.1156573562241,-40.0680330690653,
-235.35005));
#195471=CARTESIAN_POINT('Ctrl Pts',(-48.1094051493674,-40.1511056240727,
-235.35005));
#195472=CARTESIAN_POINT('Ctrl Pts',(-48.0999509844461,-40.2338479048312,
-235.35005));
#195473=CARTESIAN_POINT('Ctrl Pts',(-48.0952242649892,-40.2752158682241,
-235.35005));
#195474=CARTESIAN_POINT('Ctrl Pts',(-48.089915468827,-40.3165217899444,
-235.35005));
#195475=CARTESIAN_POINT('Ctrl Pts',(-48.0839186309937,-40.3577539058372,
-235.35005));
#195476=CARTESIAN_POINT('Ctrl Pts',(-48.0779219885029,-40.398984678624,
-235.35005));
#195477=CARTESIAN_POINT('Ctrl Pts',(-48.0712184248364,-40.4401623582127,
-235.350050000001));
#195478=CARTESIAN_POINT('Ctrl Pts',(-48.0636802851834,-40.4811959572599,
-235.350050000001));
#195479=CARTESIAN_POINT('Ctrl Pts',(-48.0561422858351,-40.5222287925639,
-235.350050000001));
#195480=CARTESIAN_POINT('Ctrl Pts',(-48.0477736645017,-40.563085046475,
-235.35005));
#195481=CARTESIAN_POINT('Ctrl Pts',(-48.0387080967012,-40.6037929031184,
-235.35005));
#195482=CARTESIAN_POINT('Ctrl Pts',(-48.0296425710794,-40.6445005703635,
-235.35005));
#195483=CARTESIAN_POINT('Ctrl Pts',(-48.0199029935916,-40.6850742166469,
-235.35005));
#195484=CARTESIAN_POINT('Ctrl Pts',(-48.0095985320967,-40.7255015726492,
-235.35005));
#195485=CARTESIAN_POINT('Ctrl Pts',(-47.9992939746968,-40.7659293049141,
-235.35005));
#195486=CARTESIAN_POINT('Ctrl Pts',(-47.9883596446658,-40.8062073663638,
-235.35005));
#195487=CARTESIAN_POINT('Ctrl Pts',(-47.9766041319244,-40.8462239751862,
-235.35005));
#195488=CARTESIAN_POINT('Ctrl Pts',(-47.9648483456559,-40.8862415151148,
-235.35005));
#195489=CARTESIAN_POINT('Ctrl Pts',(-47.9522082011025,-40.9259753165071,
-235.35005));
#195490=CARTESIAN_POINT('Ctrl Pts',(-47.9388792235724,-40.965487693427,
-235.35005));
#195491=CARTESIAN_POINT('Ctrl Pts',(-47.9122207498503,-41.0445139847866,
-235.35005));
#195492=CARTESIAN_POINT('Ctrl Pts',(-47.8834172501653,-41.1228517627344,
-235.35005));
#195493=CARTESIAN_POINT('Ctrl Pts',(-47.8525616386501,-41.2000593734148,
-235.35005));
#195494=CARTESIAN_POINT('Ctrl Pts',(-47.8371337962268,-41.2386632705008,
-235.35005));
#195495=CARTESIAN_POINT('Ctrl Pts',(-47.8210253173756,-41.2769359691183,
-235.35005));
#195496=CARTESIAN_POINT('Ctrl Pts',(-47.8041226974982,-41.3148222784138,
-235.35005));
#195497=CARTESIAN_POINT('Ctrl Pts',(-47.7872200865336,-41.3527085677318,
-235.35005));
#195498=CARTESIAN_POINT('Ctrl Pts',(-47.7696001482572,-41.3902458425851,
-235.35005));
#195499=CARTESIAN_POINT('Ctrl Pts',(-47.7515778408436,-41.4275873872532,
-235.35005));
#195500=CARTESIAN_POINT('Ctrl Pts',(-47.7335555714763,-41.4649288530907,
-235.35005));
#195501=CARTESIAN_POINT('Ctrl Pts',(-47.7151164076773,-41.5020675212465,
-235.35005));
#195502=CARTESIAN_POINT('Ctrl Pts',(-47.69640382207,-41.5390732370252,-235.35005));
#195503=CARTESIAN_POINT('Ctrl Pts',(-47.6870475533414,-41.5575760473041,
-235.35005));
#195504=CARTESIAN_POINT('Ctrl Pts',(-47.6776404221482,-41.5760541309719,
-235.35005));
#195505=CARTESIAN_POINT('Ctrl Pts',(-47.6681082454436,-41.594471397704,
-235.35005));
#195506=CARTESIAN_POINT('Ctrl Pts',(-47.6585760901228,-41.6128886231199,
-235.35005));
#195507=CARTESIAN_POINT('Ctrl Pts',(-47.6488991892717,-41.6312354462549,
-235.35005));
#195508=CARTESIAN_POINT('Ctrl Pts',(-47.6389908341615,-41.649469682206,
-235.35005));
#195509=CARTESIAN_POINT('Ctrl Pts',(-47.6191742063161,-41.6859380025145,
-235.35005));
#195510=CARTESIAN_POINT('Ctrl Pts',(-47.5984065690065,-41.7219437163951,
-235.35005));
#195511=CARTESIAN_POINT('Ctrl Pts',(-47.5769871577403,-41.7576324579108,
-235.35005));
#195512=CARTESIAN_POINT('Ctrl Pts',(-47.5555678934573,-41.7933209545252,
-235.35005));
#195513=CARTESIAN_POINT('Ctrl Pts',(-47.5335334800369,-41.8287110790685,
-235.35005));
#195514=CARTESIAN_POINT('Ctrl Pts',(-47.511140470057,-41.8639253579254,
-235.35005));
#195515=CARTESIAN_POINT('Ctrl Pts',(-47.8490613455157,-41.3259332563119,
-235.35005));
#195516=CARTESIAN_POINT('Ctrl Pts',(-48.3747699923712,-41.6520493882069,
-235.350050000092));
#195517=CARTESIAN_POINT('Ctrl Pts',(-48.7476545690025,-41.8833242138032,
-234.913932346582));
#195518=CARTESIAN_POINT('Ctrl Pts',(-46.4600121576292,-43.5649251296408,
-235.35005));
#195519=CARTESIAN_POINT('Ctrl Pts',(-46.9677567717061,-43.9091204986021,
-235.350049999619));
#195520=CARTESIAN_POINT('Ctrl Pts',(-47.3267956366018,-44.1603069972551,
-234.920895256829));
#195521=CARTESIAN_POINT('Ctrl Pts',(-44.9336721901564,-45.6801579018413,
-235.35005));
#195522=CARTESIAN_POINT('Ctrl Pts',(-45.4194497174212,-46.0456552594643,
-235.35005000036));
#195523=CARTESIAN_POINT('Ctrl Pts',(-45.766217636631,-46.3109458093001,
-234.927737734568));
#195524=CARTESIAN_POINT('Ctrl Pts',(-41.7430470430268,-49.5044128120585,
-235.35005));
#195525=CARTESIAN_POINT('Ctrl Pts',(-42.1885337805295,-49.9078910798639,
-235.350049999669));
#195526=CARTESIAN_POINT('Ctrl Pts',(-42.5090368690587,-50.2021749925663,
-234.935613379076));
#195527=CARTESIAN_POINT('Ctrl Pts',(-40.1030327246601,-51.2355371590317,
-235.35005));
#195528=CARTESIAN_POINT('Ctrl Pts',(-40.5296034202201,-51.6572713554155,
-235.350049999933));
#195529=CARTESIAN_POINT('Ctrl Pts',(-40.8393366907154,-51.9623573328398,
-234.937115568349));
#195530=CARTESIAN_POINT('Ctrl Pts',(-37.4698285345256,-53.6756545350797,
-235.35005));
#195531=CARTESIAN_POINT('Ctrl Pts',(-37.8681542571236,-54.12532384821,-235.350050000033));
#195532=CARTESIAN_POINT('Ctrl Pts',(-38.156565261625,-54.4506060236705,
-234.935579133827));
#195533=CARTESIAN_POINT('Ctrl Pts',(-36.5624534933628,-54.4622301034484,
-235.35005));
#195534=CARTESIAN_POINT('Ctrl Pts',(-36.9514272410634,-54.9212055845083,
-235.350050000067));
#195535=CARTESIAN_POINT('Ctrl Pts',(-37.2331480650446,-55.2526051792597,
-234.934472078277));
#195536=CARTESIAN_POINT('Ctrl Pts',(-34.6902365366833,-55.9834272130437,
-235.35005));
#195537=CARTESIAN_POINT('Ctrl Pts',(-35.0610225513123,-56.460769206042,
-235.350049999933));
#195538=CARTESIAN_POINT('Ctrl Pts',(-35.3287738309422,-56.8043909143739,
-234.931153092782));
#195539=CARTESIAN_POINT('Ctrl Pts',(-33.7267628103062,-56.7166866533048,
-235.35005));
#195540=CARTESIAN_POINT('Ctrl Pts',(-34.0882410053241,-57.2034119551093,
-235.35005000005));
#195541=CARTESIAN_POINT('Ctrl Pts',(-34.3491709331613,-57.5528337949308,
-234.928940594182));
#195542=CARTESIAN_POINT('Ctrl Pts',(-30.6073913272127,-58.9341159455743,
-235.35005));
#195543=CARTESIAN_POINT('Ctrl Pts',(-30.9368021706629,-59.4530013653618,
-235.350049999891));
#195544=CARTESIAN_POINT('Ctrl Pts',(-31.1761355813162,-59.8199396241448,
-234.919813894401));
#195545=CARTESIAN_POINT('Ctrl Pts',(-28.3683440394259,-60.2964424520783,
-235.35005));
#195546=CARTESIAN_POINT('Ctrl Pts',(-28.6756334162834,-60.836946555824,
-235.350050001328));
#195547=CARTESIAN_POINT('Ctrl Pts',(-28.8994459060213,-61.2157980870126,
-234.910838324051));
#195548=CARTESIAN_POINT('Ctrl Pts',(-26.0302603908518,-61.5065343641464,
-235.35005));
#195549=CARTESIAN_POINT('Ctrl Pts',(-26.3187522905012,-62.0639404421789,
-235.350049999653));
#195550=CARTESIAN_POINT('Ctrl Pts',(-26.5212311387933,-62.4552736145252,
-234.903064166399));
#195551=CARTESIAN_POINT('',(-27.0930165135311,-62.1526330725429,-234.905475377596));
#195552=CARTESIAN_POINT('',(-26.5926469327273,-61.2115127003622,-235.35005));
#195553=CARTESIAN_POINT('Origin',(-26.5926469327274,-61.2115127003622,-233.85005));
#195554=CARTESIAN_POINT('Ctrl Pts',(-27.0930165135311,-62.1526330725429,
-234.905475377596));
#195555=CARTESIAN_POINT('Ctrl Pts',(-27.413195626475,-61.9811958993946,
-234.906550894347));
#195556=CARTESIAN_POINT('Ctrl Pts',(-27.7316250998112,-61.806783331475,
-234.907642668818));
#195557=CARTESIAN_POINT('Ctrl Pts',(-28.0482019218833,-61.6294717423287,
-234.908740933506));
#195558=CARTESIAN_POINT('Ctrl Pts',(-28.3727830990628,-61.4476769919867,
-234.909866966812));
#195559=CARTESIAN_POINT('Ctrl Pts',(-28.6954170670635,-61.2628348870667,
-234.910999822682));
#195560=CARTESIAN_POINT('Ctrl Pts',(-29.0160394951108,-61.0749975381793,
-234.912128973837));
#195561=CARTESIAN_POINT('Ctrl Pts',(-29.3446312847752,-60.8824913214041,
-234.913286191069));
#195562=CARTESIAN_POINT('Ctrl Pts',(-29.6711106331574,-60.6868392410698,
-234.914439517128));
#195563=CARTESIAN_POINT('Ctrl Pts',(-29.9954516963743,-60.4880641482463,
-234.915577620065));
#195564=CARTESIAN_POINT('Ctrl Pts',(-30.3309190242629,-60.2824702324498,
-234.916754764727));
#195565=CARTESIAN_POINT('Ctrl Pts',(-30.6640991632103,-60.0735355716976,
-234.917915623919));
#195566=CARTESIAN_POINT('Ctrl Pts',(-30.995004380144,-59.8612476284684,
-234.919047659027));
#195567=CARTESIAN_POINT('Ctrl Pts',(-31.3472214532825,-59.6352873407472,
-234.920252602533));
#195568=CARTESIAN_POINT('Ctrl Pts',(-31.6968613621572,-59.405528414312,
-234.921424889581));
#195569=CARTESIAN_POINT('Ctrl Pts',(-32.0439803902238,-59.1719078383533,
-234.92254939954));
#195570=CARTESIAN_POINT('Ctrl Pts',(-32.3910994182905,-58.9382872623945,
-234.9236739095));
#195571=CARTESIAN_POINT('Ctrl Pts',(-32.7356982077542,-58.7008050508717,
-234.924750642371));
#195572=CARTESIAN_POINT('Ctrl Pts',(-33.0778659127508,-58.4593486694961,
-234.925764477524));
#195573=CARTESIAN_POINT('Ctrl Pts',(-33.1685786188303,-58.3953357266178,
-234.926033257216));
#195574=CARTESIAN_POINT('Ctrl Pts',(-33.2591205999179,-58.3310432043412,
-234.926297616187));
#195575=CARTESIAN_POINT('Ctrl Pts',(-33.349489416723,-58.2664755177344,
-234.926557272691));
#195576=CARTESIAN_POINT('Ctrl Pts',(-33.6805726000371,-58.0299196351103,
-234.927508573207));
#195577=CARTESIAN_POINT('Ctrl Pts',(-34.0095024056148,-57.7895622326326,
-234.92838728666));
#195578=CARTESIAN_POINT('Ctrl Pts',(-34.3359738414799,-57.5456966712594,
-234.929197374532));
#195579=CARTESIAN_POINT('Ctrl Pts',(-34.6775776197641,-57.290527648776,
-234.930045010948));
#195580=CARTESIAN_POINT('Ctrl Pts',(-35.0164901255299,-57.0315177572273,
-234.930817512589));
#195581=CARTESIAN_POINT('Ctrl Pts',(-35.3523953581095,-56.7689545310704,
-234.931519417723));
#195582=CARTESIAN_POINT('Ctrl Pts',(-35.6644839022428,-56.5250078251351,
-234.932171555677));
#195583=CARTESIAN_POINT('Ctrl Pts',(-35.9739771741295,-56.2779931164497,
-234.932762753228));
#195584=CARTESIAN_POINT('Ctrl Pts',(-36.2806420570433,-56.0281062971809,
-234.933296650138));
#195585=CARTESIAN_POINT('Ctrl Pts',(-36.5944525970113,-55.7723968173717,
-234.933842987482));
#195586=CARTESIAN_POINT('Ctrl Pts',(-36.9051332693568,-55.513819084103,
-234.934329384607));
#195587=CARTESIAN_POINT('Ctrl Pts',(-37.212676387903,-55.2523756338014,
-234.934754322762));
#195588=CARTESIAN_POINT('Ctrl Pts',(-37.5296715840886,-54.9828969401745,
-234.935192321032));
#195589=CARTESIAN_POINT('Ctrl Pts',(-37.843334309156,-54.7103734208553,
-234.9355650245));
#195590=CARTESIAN_POINT('Ctrl Pts',(-38.1536516617129,-54.4347520208089,
-234.935870770035));
#195591=CARTESIAN_POINT('Ctrl Pts',(-38.4373467668722,-54.1827762887848,
-234.93615028554));
#195592=CARTESIAN_POINT('Ctrl Pts',(-38.7182463400772,-53.9282104733727,
-234.936373838997));
#195593=CARTESIAN_POINT('Ctrl Pts',(-38.9963275074405,-53.6709782511683,
-234.936540159646));
#195594=CARTESIAN_POINT('Ctrl Pts',(-39.0143899505921,-53.6542700273271,
-234.936550962813));
#195595=CARTESIAN_POINT('Ctrl Pts',(-39.0324404966293,-53.6375505430169,
-234.936561524514));
#195596=CARTESIAN_POINT('Ctrl Pts',(-39.0504791753982,-53.6208198170148,
-234.936571844402));
#195597=CARTESIAN_POINT('Ctrl Pts',(-39.3472231023317,-53.345592268593,
-234.936741610941));
#195598=CARTESIAN_POINT('Ctrl Pts',(-39.6405448825184,-53.0675295916505,
-234.936841900903));
#195599=CARTESIAN_POINT('Ctrl Pts',(-39.9306089570722,-52.7866701993791,
-234.936873881775));
#195600=CARTESIAN_POINT('Ctrl Pts',(-40.2222927218382,-52.5042425149663,
-234.936906041225));
#195601=CARTESIAN_POINT('Ctrl Pts',(-40.5106828951419,-52.2189859602739,
-234.936869126592));
#195602=CARTESIAN_POINT('Ctrl Pts',(-40.795907303629,-51.9309049610937,
-234.936764325029));
#195603=CARTESIAN_POINT('Ctrl Pts',(-41.0810717798481,-51.6428844944174,
-234.936659545487));
#195604=CARTESIAN_POINT('Ctrl Pts',(-41.3630724097311,-51.3520399040605,
-234.936486907542));
#195605=CARTESIAN_POINT('Ctrl Pts',(-41.6419888382853,-51.0583539066569,
-234.936247597597));
#195606=CARTESIAN_POINT('Ctrl Pts',(-41.9064967149108,-50.7798394427705,
-234.936020650171));
#195607=CARTESIAN_POINT('Ctrl Pts',(-42.1682309029012,-50.4987687635823,
-234.935733741244));
#195608=CARTESIAN_POINT('Ctrl Pts',(-42.4272119239977,-50.2151197543423,
-234.935387882688));
#195609=CARTESIAN_POINT('Ctrl Pts',(-42.6786802319399,-49.9396990455156,
-234.935052057053));
#195610=CARTESIAN_POINT('Ctrl Pts',(-42.9275530115785,-49.661846815414,
-234.934660652292));
#195611=CARTESIAN_POINT('Ctrl Pts',(-43.1738006413473,-49.3815456163509,
-234.934214594749));
#195612=CARTESIAN_POINT('Ctrl Pts',(-43.4097500016249,-49.1129668338219,
-234.933787191683));
#195613=CARTESIAN_POINT('Ctrl Pts',(-43.6432892642155,-48.8421391713728,
-234.933309611494));
#195614=CARTESIAN_POINT('Ctrl Pts',(-43.8743453439068,-48.569057500808,
-234.932782669097));
#195615=CARTESIAN_POINT('Ctrl Pts',(-43.9394227130495,-48.4921435468224,
-234.932634254803));
#195616=CARTESIAN_POINT('Ctrl Pts',(-44.0043027963191,-48.4150508747269,
-234.932481924716));
#195617=CARTESIAN_POINT('Ctrl Pts',(-44.0689832334686,-48.3377796011446,
-234.932325697043));
#195618=CARTESIAN_POINT('Ctrl Pts',(-44.1257979573804,-48.2699051978728,
-234.932188468037));
#195619=CARTESIAN_POINT('Ctrl Pts',(-44.1824559314928,-48.2018963303122,
-234.932048170913));
#195620=CARTESIAN_POINT('Ctrl Pts',(-44.2389548542018,-48.1337537075507,
-234.931904903882));
#195621=CARTESIAN_POINT('Ctrl Pts',(-44.4921805476008,-47.8283414612372,
-234.931262787335));
#195622=CARTESIAN_POINT('Ctrl Pts',(-44.7422147854006,-47.5202407572862,
-234.930561011512));
#195623=CARTESIAN_POINT('Ctrl Pts',(-44.989159053384,-47.2093593138889,
-234.929808418714));
#195624=CARTESIAN_POINT('Ctrl Pts',(-45.2313979342307,-46.9044015453222,
-234.929070166157));
#195625=CARTESIAN_POINT('Ctrl Pts',(-45.4706633831556,-46.5967675687619,
-234.928283014753));
#195626=CARTESIAN_POINT('Ctrl Pts',(-45.7070074376436,-46.2863940216118,
-234.927455310917));
#195627=CARTESIAN_POINT('Ctrl Pts',(-45.9433319726432,-45.9760461079935,
-234.92662767544));
#195628=CARTESIAN_POINT('Ctrl Pts',(-46.1767356503047,-45.6629585377323,
-234.92575949423));
#195629=CARTESIAN_POINT('Ctrl Pts',(-46.4072264172074,-45.3470992417083,
-234.924859111632));
#195630=CARTESIAN_POINT('Ctrl Pts',(-46.6250331931149,-45.0486217979831,
-234.924008277417));
#195631=CARTESIAN_POINT('Ctrl Pts',(-46.8402385289181,-44.7476691212717,
-234.923128688407));
#195632=CARTESIAN_POINT('Ctrl Pts',(-47.0528122363433,-44.4442466607797,
-234.922227385789));
#195633=CARTESIAN_POINT('Ctrl Pts',(-47.2609703925988,-44.1471268489858,
-234.921344804901));
#195634=CARTESIAN_POINT('Ctrl Pts',(-47.4666050432284,-43.8476384603018,
-234.920441403102));
#195635=CARTESIAN_POINT('Ctrl Pts',(-47.6696538011198,-43.545822585116,
-234.919523791852));
#195636=CARTESIAN_POINT('Ctrl Pts',(-47.8666767356436,-43.2529636184694,
-234.918633412305));
#195637=CARTESIAN_POINT('Ctrl Pts',(-48.0612648724898,-42.9579130133239,
-234.917729654174));
#195638=CARTESIAN_POINT('Ctrl Pts',(-48.2533302009523,-42.6607466370678,
-234.916818557597));
#195639=CARTESIAN_POINT('Ctrl Pts',(-48.3029165880433,-42.5840258302391,
-234.916583335613));
#195640=CARTESIAN_POINT('Ctrl Pts',(-48.3523346590842,-42.5071642134369,
-234.916347624492));
#195641=CARTESIAN_POINT('Ctrl Pts',(-48.4015825627194,-42.4301635567086,
-234.916111528174));
#195642=CARTESIAN_POINT('Ctrl Pts',(-47.511140470057,-41.8639253579254,
-235.35005));
#195643=CARTESIAN_POINT('Ctrl Pts',(-46.5263591620702,-43.4125505315913,
-235.35005));
#195644=CARTESIAN_POINT('Ctrl Pts',(-45.4748377912678,-44.9008380775538,
-235.35005));
#195645=CARTESIAN_POINT('Ctrl Pts',(-44.3570056200861,-46.3291760712173,
-235.35005));
#195646=CARTESIAN_POINT('Ctrl Pts',(-44.0018587501911,-46.7829738600798,
-235.35005));
#195647=CARTESIAN_POINT('Ctrl Pts',(-43.6400181829371,-47.2307200839753,
-235.35005));
#195648=CARTESIAN_POINT('Ctrl Pts',(-43.2714968690733,-47.6724264514822,
-235.35005));
#195649=CARTESIAN_POINT('Ctrl Pts',(-41.7430470430284,-49.5044128120552,
-235.35005));
#195650=CARTESIAN_POINT('Ctrl Pts',(-40.1030327246406,-51.2355371590496,
-235.35005));
#195651=CARTESIAN_POINT('Ctrl Pts',(-38.3475632646338,-52.8622820764655,
-235.35005));
#195652=CARTESIAN_POINT('Ctrl Pts',(-37.4698285346305,-53.6756545351735,
-235.35005));
#195653=CARTESIAN_POINT('Ctrl Pts',(-36.5624534933633,-54.462230103448,
-235.35005));
#195654=CARTESIAN_POINT('Ctrl Pts',(-35.626345015024,-55.2228286582473,
-235.35005));
#195655=CARTESIAN_POINT('Ctrl Pts',(-34.6902365366847,-55.9834272130465,
-235.35005));
#195656=CARTESIAN_POINT('Ctrl Pts',(-33.7267628103146,-56.7166866532988,
-235.35005));
#195657=CARTESIAN_POINT('Ctrl Pts',(-32.7442779891666,-57.4150935706736,
-235.35005));
#195658=CARTESIAN_POINT('Ctrl Pts',(-30.9377005462682,-58.6993130881001,
-235.35005));
#195659=CARTESIAN_POINT('Ctrl Pts',(-29.058139432765,-59.8715157745017,
-235.35005));
#195660=CARTESIAN_POINT('Ctrl Pts',(-27.1073861239119,-60.9344512250895,
-235.35005));
#195661=CARTESIAN_POINT('Ctrl Pts',(-26.9363532638007,-61.0276443979026,
-235.35005));
#195662=CARTESIAN_POINT('Ctrl Pts',(-26.7647731343801,-61.119997610569,
-235.35005));
#195663=CARTESIAN_POINT('Ctrl Pts',(-26.5926469327273,-61.2115127003622,
-235.35005));
#195664=CARTESIAN_POINT('Ctrl Pts',(-26.5926469327274,-61.2115127003621,
-235.35005));
#195665=CARTESIAN_POINT('Ctrl Pts',(-26.8863570828205,-61.7639375806376,
-235.35005));
#195666=CARTESIAN_POINT('Ctrl Pts',(-27.0930165135311,-62.1526330725429,
-234.905475377596));
#195667=CARTESIAN_POINT('Ctrl Pts',(-26.5307880850042,-61.2444014821219,
-235.35005));
#195668=CARTESIAN_POINT('Ctrl Pts',(-26.821340159478,-61.8016677190097,
-235.350049999993));
#195669=CARTESIAN_POINT('Ctrl Pts',(-27.0252222584354,-62.1924330785486,
-234.902126572898));
#195670=CARTESIAN_POINT('Ctrl Pts',(-26.4686210255564,-61.2766595567632,
-235.35005));
#195671=CARTESIAN_POINT('Ctrl Pts',(-26.7519016982533,-61.843293170753,
-235.350049999997));
#195672=CARTESIAN_POINT('Ctrl Pts',(-26.9497402120697,-62.2385292812946,
-234.896449373983));
#195673=CARTESIAN_POINT('Ctrl Pts',(-26.3891388204284,-61.3131722991992,
-235.35005));
#195674=CARTESIAN_POINT('Ctrl Pts',(-26.6543883005772,-61.9032639296083,
-235.350050000001));
#195675=CARTESIAN_POINT('Ctrl Pts',(-26.8364482204274,-62.3082529158846,
-234.8795305279));
#195676=CARTESIAN_POINT('Ctrl Pts',(-26.3731447836042,-61.3202661527697,
-235.35005));
#195677=CARTESIAN_POINT('Ctrl Pts',(-26.634890969524,-61.9147711240481,
-235.350050000004));
#195678=CARTESIAN_POINT('Ctrl Pts',(-26.8139780721898,-62.3215114290266,
-234.876306139112));
#195679=CARTESIAN_POINT('Ctrl Pts',(-26.341052548261,-61.3342311248494,
-235.35005));
#195680=CARTESIAN_POINT('Ctrl Pts',(-26.5987725347511,-61.9335243765778,
-235.350049999996));
#195681=CARTESIAN_POINT('Ctrl Pts',(-26.7745169875525,-62.3421733148585,
-234.872883709682));
#195682=CARTESIAN_POINT('Ctrl Pts',(-26.324963993434,-61.3411228649431,
-235.35005));
#195683=CARTESIAN_POINT('Ctrl Pts',(-26.5822418971017,-61.9407189173202,
-235.350050000003));
#195684=CARTESIAN_POINT('Ctrl Pts',(-26.7576550280567,-62.3495221049909,
-234.872747949079));
#195685=CARTESIAN_POINT('Ctrl Pts',(-26.2766869482483,-61.3617737493097,
-235.35005));
#195686=CARTESIAN_POINT('Ctrl Pts',(-26.5322022210074,-61.9628463306943,
-235.350049999995));
#195687=CARTESIAN_POINT('Ctrl Pts',(-26.7062785831568,-62.3723269401802,
-234.871930575498));
#195688=CARTESIAN_POINT('Ctrl Pts',(-26.2444517981386,-61.3754399401447,
-235.35005));
#195689=CARTESIAN_POINT('Ctrl Pts',(-26.4983809904187,-61.9780069834906,
-235.350049999998));
#195690=CARTESIAN_POINT('Ctrl Pts',(-26.6712306199245,-62.3881303051001,
-234.871005091044));
#195691=CARTESIAN_POINT('Ctrl Pts',(-26.1797908377429,-61.4023344685258,
-235.35005));
#195692=CARTESIAN_POINT('Ctrl Pts',(-26.4290695787371,-62.0096639879438,
-235.350050000002));
#195693=CARTESIAN_POINT('Ctrl Pts',(-26.598219218148,-62.4217260874495,
-234.867787528297));
#195694=CARTESIAN_POINT('Ctrl Pts',(-26.1473795281051,-61.4155758832315,
-235.35005));
#195695=CARTESIAN_POINT('Ctrl Pts',(-26.3937643073098,-62.0259679052544,
-235.350050000003));
#195696=CARTESIAN_POINT('Ctrl Pts',(-26.5606263859936,-62.4392448432971,
-234.865676603548));
#195697=CARTESIAN_POINT('Ctrl Pts',(-26.0821804763413,-61.4411000467081,
-235.35005));
#195698=CARTESIAN_POINT('Ctrl Pts',(-26.3181216753443,-62.0629567534453,
-235.350049999997));
#195699=CARTESIAN_POINT('Ctrl Pts',(-26.4765766579827,-62.4804755152087,
-234.857183986946));
#195700=CARTESIAN_POINT('Ctrl Pts',(-26.0493312864126,-61.4532499966124,
-235.350050000001));
#195701=CARTESIAN_POINT('Ctrl Pts',(-26.2774828535028,-62.0835800223265,
-235.350050000008));
#195702=CARTESIAN_POINT('Ctrl Pts',(-26.4297212650746,-62.5040608637178,
-234.850690950979));
#195703=CARTESIAN_POINT('Ctrl Pts',(-25.9501566901715,-61.4879342004266,
-235.350050000001));
#195704=CARTESIAN_POINT('Ctrl Pts',(-26.1609807722306,-62.1355066696273,
-235.350049999986));
#195705=CARTESIAN_POINT('Ctrl Pts',(-26.299935026532,-62.5618001346298,
-234.837570256781));
#195706=CARTESIAN_POINT('Ctrl Pts',(-25.8834819572284,-61.509419252042,
-235.35005));
#195707=CARTESIAN_POINT('Ctrl Pts',(-26.0918719141122,-62.1577719822702,
-235.350049999986));
#195708=CARTESIAN_POINT('Ctrl Pts',(-26.2291985619127,-62.5845560253671,
-234.837502470078));
#195709=CARTESIAN_POINT('Ctrl Pts',(-25.7996807895498,-61.534730893345,
-235.35005));
#195710=CARTESIAN_POINT('Ctrl Pts',(-25.9958115105161,-62.1946041207473,
-235.350050000004));
#195711=CARTESIAN_POINT('Ctrl Pts',(-26.1237073939439,-62.6248724643351,
-234.828124366513));
#195712=CARTESIAN_POINT('Ctrl Pts',(-25.7828903569215,-61.5396828918313,
-235.35005));
#195713=CARTESIAN_POINT('Ctrl Pts',(-25.976181775626,-62.2022533875226,
-235.35005000001));
#195714=CARTESIAN_POINT('Ctrl Pts',(-26.1019429230186,-62.6332968405534,
-234.825896748429));
#195715=CARTESIAN_POINT('Ctrl Pts',(-25.7492255098059,-61.5492800686396,
-235.35005));
#195716=CARTESIAN_POINT('Ctrl Pts',(-25.9355808625229,-62.2185181387375,
-235.35004999999));
#195717=CARTESIAN_POINT('Ctrl Pts',(-26.056126511479,-62.651374227355,-234.820237176746));
#195718=CARTESIAN_POINT('Ctrl Pts',(-25.7323477164287,-61.5539129022783,
-235.35005));
#195719=CARTESIAN_POINT('Ctrl Pts',(-25.9142407405854,-62.2274858229347,
-235.350050000002));
#195720=CARTESIAN_POINT('Ctrl Pts',(-26.0314456183935,-62.6614557970582,
-234.816472473606));
#195721=CARTESIAN_POINT('Ctrl Pts',(-25.6815605387409,-61.5672495175189,
-235.35005));
#195722=CARTESIAN_POINT('Ctrl Pts',(-25.8513370817052,-62.2523278228314,
-235.350049999996));
#195723=CARTESIAN_POINT('Ctrl Pts',(-25.9596326032101,-62.6890827742206,
-234.806344353949));
#195724=CARTESIAN_POINT('Ctrl Pts',(-25.6474983161402,-61.5754339876196,
-235.35005));
#195725=CARTESIAN_POINT('Ctrl Pts',(-25.8103146214907,-62.2668945351399,
-235.350050000001));
#195726=CARTESIAN_POINT('Ctrl Pts',(-25.9135255401439,-62.7050301838465,
-234.800516173084));
#195727=CARTESIAN_POINT('Ctrl Pts',(-25.5791807904238,-61.5908730316921,
-235.35005));
#195728=CARTESIAN_POINT('Ctrl Pts',(-25.731028783567,-62.2921464778074,
-235.350049999999));
#195729=CARTESIAN_POINT('Ctrl Pts',(-25.8263731088601,-62.7322675488681,
-234.791463019912));
#195730=CARTESIAN_POINT('Ctrl Pts',(-25.5449390466137,-61.5981933980485,
-235.35005));
#195731=CARTESIAN_POINT('Ctrl Pts',(-25.6927227699064,-62.3029939210129,
-235.350050000007));
#195732=CARTESIAN_POINT('Ctrl Pts',(-25.7851988792686,-62.7437844019476,
-234.788172738052));
#195733=CARTESIAN_POINT('Ctrl Pts',(-25.4762602753847,-61.6118947761917,
-235.35005));
#195734=CARTESIAN_POINT('Ctrl Pts',(-25.6117842070045,-62.3276542792517,
-235.350049999993));
#195735=CARTESIAN_POINT('Ctrl Pts',(-25.6956346706304,-62.770238922023,
-234.777569028842));
#195736=CARTESIAN_POINT('Ctrl Pts',(-25.441793602875,-61.6182439225594,
-235.35005));
#195737=CARTESIAN_POINT('Ctrl Pts',(-25.5698816498182,-62.3406532746031,
-235.350049999995));
#195738=CARTESIAN_POINT('Ctrl Pts',(-25.6485908901075,-62.7841922736754,
-234.770997188221));
#195739=CARTESIAN_POINT('Ctrl Pts',(-25.3727171465013,-61.6295518156141,
-235.35005));
#195740=CARTESIAN_POINT('Ctrl Pts',(-25.4834982706708,-62.367218439294,
-235.350050000006));
#195741=CARTESIAN_POINT('Ctrl Pts',(-25.5504255841634,-62.8124292406126,
-234.755348365089));
#195742=CARTESIAN_POINT('Ctrl Pts',(-25.3381059806223,-61.6345074287981,
-235.35005));
#195743=CARTESIAN_POINT('Ctrl Pts',(-25.4409641703014,-62.3790113723438,
-235.350050000011));
#195744=CARTESIAN_POINT('Ctrl Pts',(-25.502603574716,-62.8247454634089,
-234.748093190059));
#195745=CARTESIAN_POINT('Ctrl Pts',(-25.2687752030225,-61.6433803535082,
-235.35005));
#195746=CARTESIAN_POINT('Ctrl Pts',(-25.3578642498523,-62.399590514639,
-235.350049999988));
#195747=CARTESIAN_POINT('Ctrl Pts',(-25.4105087856878,-62.8459575195944,
-234.735446711282));
#195748=CARTESIAN_POINT('Ctrl Pts',(-25.2340567625657,-61.647308878831,
-235.35005));
#195749=CARTESIAN_POINT('Ctrl Pts',(-25.3180366392519,-62.4077933846439,
-235.350049999987));
#195750=CARTESIAN_POINT('Ctrl Pts',(-25.3673989913123,-62.8542900606576,
-234.730725127778));
#195751=CARTESIAN_POINT('Ctrl Pts',(-25.1645355171699,-61.6543581913618,
-235.35005));
#195752=CARTESIAN_POINT('Ctrl Pts',(-25.2357480959957,-62.4254349365975,
-235.350050000013));
#195753=CARTESIAN_POINT('Ctrl Pts',(-25.277049571495,-62.8720350725204,
-234.718828491406));
#195754=CARTESIAN_POINT('Ctrl Pts',(-25.1297211288812,-61.6573680755603,
-235.350050000001));
#195755=CARTESIAN_POINT('Ctrl Pts',(-25.1911613073834,-62.4364284584908,
-235.350049999998));
#195756=CARTESIAN_POINT('Ctrl Pts',(-25.2264460848463,-62.8829206549938,
-234.709697846434));
#195757=CARTESIAN_POINT('Ctrl Pts',(-25.0599498736116,-61.6620236980061,
-235.350050000001));
#195758=CARTESIAN_POINT('Ctrl Pts',(-25.1032793349872,-62.4555089444949,
-235.350050000003));
#195759=CARTESIAN_POINT('Ctrl Pts',(-25.1276927878133,-62.9012647282465,
-234.692677918945));
#195760=CARTESIAN_POINT('Ctrl Pts',(-25.0249977138784,-61.6637138702923,
-235.35005));
#195761=CARTESIAN_POINT('Ctrl Pts',(-25.0601909996374,-62.4634558478501,
-235.350050000029));
#195762=CARTESIAN_POINT('Ctrl Pts',(-25.0798352875815,-62.9086680015632,
-234.685060290672));
#195763=CARTESIAN_POINT('Ctrl Pts',(-24.989999724813,-61.6649665253884,
-235.35005));
#195764=CARTESIAN_POINT('Ctrl Pts',(-25.0188032481003,-62.4697021984285,
-235.35005));
#195765=CARTESIAN_POINT('Ctrl Pts',(-25.0347190704466,-62.9143710634145,
-234.67889768232));
#195766=CARTESIAN_POINT('',(-25.0347190704488,-62.9143710634153,-234.678897682319));
#195767=CARTESIAN_POINT('',(-24.9899997248189,-61.6649665253882,-235.35005));
#195768=CARTESIAN_POINT('Origin',(-24.9899997248189,-61.6649665253882,-233.85005));
#195769=CARTESIAN_POINT('Ctrl Pts',(-25.0347190704488,-62.9143710634153,
-234.678897682319));
#195770=CARTESIAN_POINT('Ctrl Pts',(-25.0798352875815,-62.9086680015632,
-234.685060290672));
#195771=CARTESIAN_POINT('Ctrl Pts',(-25.1276927878133,-62.9012647282465,
-234.692677918945));
#195772=CARTESIAN_POINT('Ctrl Pts',(-25.2264460848463,-62.8829206549938,
-234.709697846434));
#195773=CARTESIAN_POINT('Ctrl Pts',(-25.277049571495,-62.8720350725204,
-234.718828491406));
#195774=CARTESIAN_POINT('Ctrl Pts',(-25.3673989913123,-62.8542900606576,
-234.730725127778));
#195775=CARTESIAN_POINT('Ctrl Pts',(-25.4105087856878,-62.8459575195944,
-234.735446711282));
#195776=CARTESIAN_POINT('Ctrl Pts',(-25.502603574716,-62.8247454634089,
-234.748093190059));
#195777=CARTESIAN_POINT('Ctrl Pts',(-25.5504255841634,-62.8124292406126,
-234.755348365089));
#195778=CARTESIAN_POINT('Ctrl Pts',(-25.6485908901075,-62.7841922736754,
-234.770997188221));
#195779=CARTESIAN_POINT('Ctrl Pts',(-25.6956346706304,-62.770238922023,
-234.777569028842));
#195780=CARTESIAN_POINT('Ctrl Pts',(-25.7851988792686,-62.7437844019476,
-234.788172738052));
#195781=CARTESIAN_POINT('Ctrl Pts',(-25.8263731088601,-62.7322675488681,
-234.791463019912));
#195782=CARTESIAN_POINT('Ctrl Pts',(-25.9135255401439,-62.7050301838465,
-234.800516173084));
#195783=CARTESIAN_POINT('Ctrl Pts',(-25.9596326032101,-62.6890827742206,
-234.806344353949));
#195784=CARTESIAN_POINT('Ctrl Pts',(-26.0314456183935,-62.6614557970582,
-234.816472473606));
#195785=CARTESIAN_POINT('Ctrl Pts',(-26.056126511479,-62.651374227355,-234.820237176746));
#195786=CARTESIAN_POINT('Ctrl Pts',(-26.1019429230186,-62.6332968405534,
-234.825896748429));
#195787=CARTESIAN_POINT('Ctrl Pts',(-26.1237073939439,-62.6248724643351,
-234.828124366513));
#195788=CARTESIAN_POINT('Ctrl Pts',(-26.2291985619127,-62.5845560253671,
-234.837502470078));
#195789=CARTESIAN_POINT('Ctrl Pts',(-26.299935026532,-62.5618001346298,
-234.837570256781));
#195790=CARTESIAN_POINT('Ctrl Pts',(-26.4297212650746,-62.5040608637178,
-234.850690950979));
#195791=CARTESIAN_POINT('Ctrl Pts',(-26.4765766579827,-62.4804755152087,
-234.857183986946));
#195792=CARTESIAN_POINT('Ctrl Pts',(-26.5606263859936,-62.4392448432971,
-234.865676603548));
#195793=CARTESIAN_POINT('Ctrl Pts',(-26.598219218148,-62.4217260874495,
-234.867787528297));
#195794=CARTESIAN_POINT('Ctrl Pts',(-26.6712306199245,-62.3881303051001,
-234.871005091044));
#195795=CARTESIAN_POINT('Ctrl Pts',(-26.7062785831568,-62.3723269401802,
-234.871930575498));
#195796=CARTESIAN_POINT('Ctrl Pts',(-26.7576550280567,-62.3495221049909,
-234.872747949079));
#195797=CARTESIAN_POINT('Ctrl Pts',(-26.7745169875525,-62.3421733148585,
-234.872883709682));
#195798=CARTESIAN_POINT('Ctrl Pts',(-26.8139780721898,-62.3215114290266,
-234.876306139112));
#195799=CARTESIAN_POINT('Ctrl Pts',(-26.8364482204274,-62.3082529158846,
-234.8795305279));
#195800=CARTESIAN_POINT('Ctrl Pts',(-26.9497402120697,-62.2385292812946,
-234.896449373983));
#195801=CARTESIAN_POINT('Ctrl Pts',(-27.0252222584354,-62.1924330785486,
-234.902126572898));
#195802=CARTESIAN_POINT('Ctrl Pts',(-27.0930165135311,-62.1526330725429,
-234.905475377596));
#195803=CARTESIAN_POINT('Ctrl Pts',(-26.5926469327273,-61.2115127003622,
-235.35005));
#195804=CARTESIAN_POINT('Ctrl Pts',(-26.5307857619515,-61.2444027172302,
-235.35005));
#195805=CARTESIAN_POINT('Ctrl Pts',(-26.4686189787879,-61.276660497005,
-235.35005));
#195806=CARTESIAN_POINT('Ctrl Pts',(-26.4050352616636,-61.3058697511684,
-235.35005));
#195807=CARTESIAN_POINT('Ctrl Pts',(-26.3891387194065,-61.3131723462998,
-235.35005));
#195808=CARTESIAN_POINT('Ctrl Pts',(-26.3731446870696,-61.3202661956383,
-235.35005));
#195809=CARTESIAN_POINT('Ctrl Pts',(-26.3570986663275,-61.327248639717,
-235.35005));
#195810=CARTESIAN_POINT('Ctrl Pts',(-26.3410524626378,-61.3342311634055,
-235.35005));
#195811=CARTESIAN_POINT('Ctrl Pts',(-26.3249639130519,-61.3411229008801,
-235.35005));
#195812=CARTESIAN_POINT('Ctrl Pts',(-26.3088716457128,-61.3480064946411,
-235.35005));
#195813=CARTESIAN_POINT('Ctrl Pts',(-26.2766866901153,-61.3617738622147,
-235.35005));
#195814=CARTESIAN_POINT('Ctrl Pts',(-26.2444515824955,-61.3754400331407,
-235.35005));
#195815=CARTESIAN_POINT('Ctrl Pts',(-26.212121319506,-61.3888872080985,
-235.35005));
#195816=CARTESIAN_POINT('Ctrl Pts',(-26.1797907095899,-61.4023345273539,
-235.35005));
#195817=CARTESIAN_POINT('Ctrl Pts',(-26.1473794430666,-61.4155759233805,
-235.350049999999));
#195818=CARTESIAN_POINT('Ctrl Pts',(-26.1147800051491,-61.4283379724439,
-235.350049999999));
#195819=CARTESIAN_POINT('Ctrl Pts',(-26.0821804798061,-61.4411000557326,
-235.35005));
#195820=CARTESIAN_POINT('Ctrl Pts',(-26.0493313347784,-61.4532499920652,
-235.350050000001));
#195821=CARTESIAN_POINT('Ctrl Pts',(-26.0162730923146,-61.464811411177,
-235.350050000001));
#195822=CARTESIAN_POINT('Ctrl Pts',(-25.9501574057461,-61.4879339701914,
-235.350050000001));
#195823=CARTESIAN_POINT('Ctrl Pts',(-25.8834830443658,-61.5094189499966,
-235.35005));
#195824=CARTESIAN_POINT('Ctrl Pts',(-25.816441032895,-61.5296685975531,
-235.35005));
#195825=CARTESIAN_POINT('Ctrl Pts',(-25.799680801709,-61.5347309273823,
-235.35005));
#195826=CARTESIAN_POINT('Ctrl Pts',(-25.7828903692931,-61.5396829277202,
-235.35005));
#195827=CARTESIAN_POINT('Ctrl Pts',(-25.7660579441618,-61.5444815181131,
-235.35005));
#195828=CARTESIAN_POINT('Ctrl Pts',(-25.7492255222735,-61.5492801075815,
-235.35005));
#195829=CARTESIAN_POINT('Ctrl Pts',(-25.7323477287723,-61.5539129424998,
-235.35005));
#195830=CARTESIAN_POINT('Ctrl Pts',(-25.7154186680902,-61.558358482165,
-235.35005));
#195831=CARTESIAN_POINT('Ctrl Pts',(-25.6815605534858,-61.5672495597203,
-235.35005));
#195832=CARTESIAN_POINT('Ctrl Pts',(-25.6474983294595,-61.5754340306918,
-235.35005));
#195833=CARTESIAN_POINT('Ctrl Pts',(-25.6133395630491,-61.5831535528751,
-235.35005));
#195834=CARTESIAN_POINT('Ctrl Pts',(-25.5791808006497,-61.590873074152,
-235.35005));
#195835=CARTESIAN_POINT('Ctrl Pts',(-25.5449390551878,-61.5981934391817,
-235.35005));
#195836=CARTESIAN_POINT('Ctrl Pts',(-25.510599668782,-61.6050441261316,
-235.35005));
#195837=CARTESIAN_POINT('Ctrl Pts',(-25.4762602802774,-61.6118948135003,
-235.35005));
#195838=CARTESIAN_POINT('Ctrl Pts',(-25.4417936057802,-61.6182439572411,
-235.35005));
#195839=CARTESIAN_POINT('Ctrl Pts',(-25.4072553797815,-61.6238979002003,
-235.35005));
#195840=CARTESIAN_POINT('Ctrl Pts',(-25.3727171455055,-61.6295518445145,
-235.35005));
#195841=CARTESIAN_POINT('Ctrl Pts',(-25.3381059777677,-61.6345074541881,
-235.35005));
#195842=CARTESIAN_POINT('Ctrl Pts',(-25.3034405945236,-61.6389439122599,
-235.35005));
#195843=CARTESIAN_POINT('Ctrl Pts',(-25.2687751967828,-61.643380372187,
-235.35005));
#195844=CARTESIAN_POINT('Ctrl Pts',(-25.234056754758,-61.6473088938803,
-235.35005));
#195845=CARTESIAN_POINT('Ctrl Pts',(-25.1992961409817,-61.6508335460814,
-235.35005));
#195846=CARTESIAN_POINT('Ctrl Pts',(-25.1645355064627,-61.6543582003856,
-235.35005));
#195847=CARTESIAN_POINT('Ctrl Pts',(-25.1297211167782,-61.6573680815383,
-235.350050000001));
#195848=CARTESIAN_POINT('Ctrl Pts',(-25.0948355014582,-61.6596958899581,
-235.350050000001));
#195849=CARTESIAN_POINT('Ctrl Pts',(-25.0599498590945,-61.6620237001823,
-235.350050000001));
#195850=CARTESIAN_POINT('Ctrl Pts',(-25.0249976982331,-61.6637138708523,
-235.35005));
#195851=CARTESIAN_POINT('Ctrl Pts',(-24.9899997248189,-61.6649665253882,
-235.35005));
#195852=CARTESIAN_POINT('Ctrl Pts',(-24.9899997248189,-61.6649665253882,
-235.35005));
#195853=CARTESIAN_POINT('Ctrl Pts',(-25.0188032481045,-62.4697021984296,
-235.35005));
#195854=CARTESIAN_POINT('Ctrl Pts',(-25.0347190704499,-62.9143710634155,
-234.678897682318));
#195855=CARTESIAN_POINT('Ctrl Pts',(-23.5944744924679,-61.7149158997446,
-235.35005));
#195856=CARTESIAN_POINT('Ctrl Pts',(-23.6213321581707,-62.5206566084218,
-235.350050000019));
#195857=CARTESIAN_POINT('Ctrl Pts',(-23.6367128243542,-62.9652114948589,
-234.677688363322));
#195858=CARTESIAN_POINT('Ctrl Pts',(-22.1988114399884,-61.7606622187164,
-235.35005));
#195859=CARTESIAN_POINT('Ctrl Pts',(-22.2241440176947,-62.5673064456533,
-235.350049999981));
#195860=CARTESIAN_POINT('Ctrl Pts',(-22.2385723540716,-63.0117706699204,
-234.676581567471));
#195861=CARTESIAN_POINT('Ctrl Pts',(-20.8030114294341,-61.8022299494809,
-235.35005));
#195862=CARTESIAN_POINT('Ctrl Pts',(-20.8270581434285,-62.6096929286678,
-235.35005));
#195863=CARTESIAN_POINT('Ctrl Pts',(-20.8402921969906,-63.0540783161444,
-234.675571538939));
#195864=CARTESIAN_POINT('',(-20.8402919613448,-63.0540783782995,-234.675571450239));
#195865=CARTESIAN_POINT('',(-20.803011429434,-61.8022299494809,-235.35005));
#195866=CARTESIAN_POINT('Origin',(-20.803011429434,-61.802229949481,-233.85005));
#195867=CARTESIAN_POINT('Origin',(-0.0417395060045145,624.033047422002,
-250.70813398415));
#195868=CARTESIAN_POINT('Origin',(-0.0402464098217781,635.457880431084,
-235.35004999212));
#195869=CARTESIAN_POINT('Ctrl Pts',(-20.8103261415008,-61.8019857359798,
-235.350049999965));
#195870=CARTESIAN_POINT('Ctrl Pts',(-20.8379442866863,-62.6073572538772,
-235.350055531337));
#195871=CARTESIAN_POINT('Ctrl Pts',(-20.8531893512146,-63.0519698953505,
-234.678137626134));
#195872=CARTESIAN_POINT('Ctrl Pts',(-20.6414007909339,-61.8077587731983,
-235.350049999962));
#195873=CARTESIAN_POINT('Ctrl Pts',(-20.5833425691332,-62.6623713318805,
-235.350056095672));
#195874=CARTESIAN_POINT('Ctrl Pts',(-20.5552714958317,-63.1013208767041,
-234.619006716613));
#195875=CARTESIAN_POINT('Ctrl Pts',(-20.4749301547618,-61.7876897269827,
-235.350049999958));
#195876=CARTESIAN_POINT('Ctrl Pts',(-20.332371777071,-62.6832275069745,
-235.350056755447));
#195877=CARTESIAN_POINT('Ctrl Pts',(-20.2675410707633,-63.1041069278272,
-234.551887687313));
#195878=CARTESIAN_POINT('Ctrl Pts',(-20.3109688043558,-61.7477838180328,
-235.350049999954));
#195879=CARTESIAN_POINT('Ctrl Pts',(-20.0839608523746,-62.6801181224961,
-235.350057499857));
#195880=CARTESIAN_POINT('Ctrl Pts',(-19.9887981368535,-63.070968475606,
-234.478875287122));
#195881=CARTESIAN_POINT('',(-20.0008767707152,-63.0723812833681,-234.482033933863));
#195882=CARTESIAN_POINT('',(-20.3180691938068,-61.7495111937247,-235.35005));
#195883=CARTESIAN_POINT('Origin',(-20.3180691938068,-61.7495111937247,-233.85005));
#195884=CARTESIAN_POINT('Ctrl Pts',(-20.0008767707152,-63.0723812833681,
-234.482033933863));
#195885=CARTESIAN_POINT('Ctrl Pts',(-20.271823216313,-63.1035533395417,
-234.552772407528));
#195886=CARTESIAN_POINT('Ctrl Pts',(-20.5512619539194,-63.1007007148801,
-234.617924419256));
#195887=CARTESIAN_POINT('Ctrl Pts',(-20.8402919498871,-63.0540783560036,
-234.675571489654));
#195888=CARTESIAN_POINT('Ctrl Pts',(-20.803011429434,-61.8022299494809,
-235.35005));
#195889=CARTESIAN_POINT('Ctrl Pts',(-20.6389224043824,-61.8071166154417,
-235.35005));
#195890=CARTESIAN_POINT('Ctrl Pts',(-20.4774719299468,-61.7877321350851,
-235.35005));
#195891=CARTESIAN_POINT('Ctrl Pts',(-20.3180691938068,-61.7495111937247,
-235.35005));
#195892=CARTESIAN_POINT('Ctrl Pts',(-56.7978769236249,-64.9962486583172,
-213.25615446688));
#195893=CARTESIAN_POINT('Ctrl Pts',(-56.7746082597229,-64.9675904302956,
-215.348143273993));
#195894=CARTESIAN_POINT('Ctrl Pts',(-55.6596124147223,-63.9410622767582,
-216.790642532039));
#195895=CARTESIAN_POINT('Ctrl Pts',(-57.7238224635574,-63.9855135774691,
-213.252837709814));
#195896=CARTESIAN_POINT('Ctrl Pts',(-57.7003423852215,-63.9568776618465,
-215.347378844935));
#195897=CARTESIAN_POINT('Ctrl Pts',(-56.564654667179,-62.9482476744094,
-216.790318465523));
#195898=CARTESIAN_POINT('Ctrl Pts',(-58.6299194066539,-62.941827293528,
-213.246154460261));
#195899=CARTESIAN_POINT('Ctrl Pts',(-58.6117008786858,-62.9065844937392,
-215.346095403409));
#195900=CARTESIAN_POINT('Ctrl Pts',(-57.4569850683431,-61.9095456343501,
-216.789947871074));
#195901=CARTESIAN_POINT('Ctrl Pts',(-59.5017489787801,-61.8814728748856,
-213.239284157696));
#195902=CARTESIAN_POINT('Ctrl Pts',(-59.4805126951739,-61.8494200250926,
-215.345222444811));
#195903=CARTESIAN_POINT('Ctrl Pts',(-58.3016167962822,-60.8701016111416,
-216.790073419041));
#195904=CARTESIAN_POINT('',(-59.5017489787801,-61.8814728748856,-213.239284157696));
#195905=CARTESIAN_POINT('Ctrl Pts',(-56.8144552965909,-64.9781464054155,
-213.256094899172));
#195906=CARTESIAN_POINT('Ctrl Pts',(-57.7346379419056,-63.9730537814781,
-213.25275810317));
#195907=CARTESIAN_POINT('Ctrl Pts',(-58.6351232191172,-62.9354982011503,
-213.246113635462));
#195908=CARTESIAN_POINT('Ctrl Pts',(-59.5017489787801,-61.8814728748856,
-213.239284157696));
#195909=CARTESIAN_POINT('',(-58.3016167962821,-60.8701016111416,-216.790073419041));
#195910=CARTESIAN_POINT('Origin',(-55.6399013441494,-58.7068046741696,-213.15202212551));
#195911=CARTESIAN_POINT('Origin',(-1.94290616455451,-15.0706582410416,-217.44150863223));
#195912=CARTESIAN_POINT('Ctrl Pts',(-58.6463245735781,-60.4071924582901,
-216.811211134516));
#195913=CARTESIAN_POINT('Ctrl Pts',(-59.9794428890559,-61.1951119486122,
-215.368374394716));
#195914=CARTESIAN_POINT('Ctrl Pts',(-60.0946517248888,-61.0923008758321,
-213.257460793579));
#195915=CARTESIAN_POINT('Ctrl Pts',(-58.5374530973566,-60.5671124334838,
-216.797054630904));
#195916=CARTESIAN_POINT('Ctrl Pts',(-59.8200433378109,-61.420251027068,
-215.35259069506));
#195917=CARTESIAN_POINT('Ctrl Pts',(-59.9074639858675,-61.3655831923351,
-213.24427462457));
#195918=CARTESIAN_POINT('Ctrl Pts',(-58.4224878547923,-60.721351931509,
-216.7900913853));
#195919=CARTESIAN_POINT('Ctrl Pts',(-59.6536675829205,-61.6382804704421,
-215.344967772293));
#195920=CARTESIAN_POINT('Ctrl Pts',(-59.7097127443643,-61.6285208837113,
-213.238301674026));
#195921=CARTESIAN_POINT('Ctrl Pts',(-58.3016167962821,-60.8701016111416,
-216.790073419041));
#195922=CARTESIAN_POINT('Ctrl Pts',(-59.4805126951738,-61.8494200250926,
-215.345222444811));
#195923=CARTESIAN_POINT('Ctrl Pts',(-59.5017489787801,-61.8814728748855,
-213.239284157696));
#195924=CARTESIAN_POINT('',(-58.6463245735781,-60.4071924582901,-216.811211134516));
#195925=CARTESIAN_POINT('',(-60.094651724889,-61.0923008758319,-213.257460793579));
#195926=CARTESIAN_POINT('Origin',(-55.9721510687884,-58.2643380616866,-213.170198761392));
#195927=CARTESIAN_POINT('Origin',(-55.2663427916624,-58.4039463264878,-220.170489403551));
#195928=CARTESIAN_POINT('Origin',(-52.480669683245,-56.0916407951787,-217.694018753789));
#195929=CARTESIAN_POINT('Ctrl Pts',(-60.0946517248887,-61.0923008758322,
-213.257460793579));
#195930=CARTESIAN_POINT('Ctrl Pts',(-59.9794428890558,-61.1951119486123,
-215.368374394716));
#195931=CARTESIAN_POINT('Ctrl Pts',(-58.6463245735781,-60.4071924582901,
-216.811211134516));
#195932=CARTESIAN_POINT('Ctrl Pts',(-60.1704014750534,-60.9817110085918,
-213.262796876316));
#195933=CARTESIAN_POINT('Ctrl Pts',(-60.0526858896249,-61.0914110515479,
-215.370164057538));
#195934=CARTESIAN_POINT('Ctrl Pts',(-58.7107161648513,-60.3252040601318,
-216.812171008252));
#195935=CARTESIAN_POINT('Ctrl Pts',(-60.2441117511573,-60.869896564576,
-213.268474581372));
#195936=CARTESIAN_POINT('Ctrl Pts',(-60.124312865506,-60.986260523149,-215.371696130155));
#195937=CARTESIAN_POINT('Ctrl Pts',(-58.774689151411,-60.2421218021171,
-216.812772355214));
#195938=CARTESIAN_POINT('Ctrl Pts',(-60.3516186472783,-60.7003634878465,
-213.277642216535));
#195939=CARTESIAN_POINT('Ctrl Pts',(-60.2274858612712,-60.8293599818386,
-215.375374274252));
#195940=CARTESIAN_POINT('Ctrl Pts',(-58.8650026632788,-60.119575817198,
-216.814991469675));
#195941=CARTESIAN_POINT('Ctrl Pts',(-60.3869441313356,-60.6435508076619,
-213.280811345681));
#195942=CARTESIAN_POINT('Ctrl Pts',(-60.2611846671316,-60.7771794814514,
-215.376816670917));
#195943=CARTESIAN_POINT('Ctrl Pts',(-58.8942226240245,-60.0790466940644,
-216.81593623579));
#195944=CARTESIAN_POINT('Ctrl Pts',(-60.4565718022257,-60.5293282074256,
-213.287428511106));
#195945=CARTESIAN_POINT('Ctrl Pts',(-60.3271928115902,-60.6731602773773,
-215.380263890201));
#195946=CARTESIAN_POINT('Ctrl Pts',(-58.9507651838229,-59.99875439683,-216.818366528164));
#195947=CARTESIAN_POINT('Ctrl Pts',(-60.4908728037509,-60.4719198229617,
-213.290891213231));
#195948=CARTESIAN_POINT('Ctrl Pts',(-60.3592441835178,-60.6217751917873,
-215.382474260201));
#195949=CARTESIAN_POINT('Ctrl Pts',(-58.9774007039939,-59.9596050477392,
-216.820063085709));
#195950=CARTESIAN_POINT('Ctrl Pts',(-60.5922460955565,-60.2987937844743,
-213.301646644734));
#195951=CARTESIAN_POINT('Ctrl Pts',(-60.4575958918302,-60.4609801138041,
-215.386947861197));
#195952=CARTESIAN_POINT('Ctrl Pts',(-59.065516004555,-59.8335652392552,
-216.822864771484));
#195953=CARTESIAN_POINT('Ctrl Pts',(-60.6577989462613,-60.1821636194365,
-213.309190814844));
#195954=CARTESIAN_POINT('Ctrl Pts',(-60.524785077188,-60.3468286312902,
-215.387646798153));
#195955=CARTESIAN_POINT('Ctrl Pts',(-59.1321238001163,-59.7406787706502,
-216.822297086344));
#195956=CARTESIAN_POINT('Ctrl Pts',(-60.7848819389683,-59.9464002293958,
-213.324386876108));
#195957=CARTESIAN_POINT('Ctrl Pts',(-60.6548197305022,-60.1165130022809,
-215.388612783322));
#195958=CARTESIAN_POINT('Ctrl Pts',(-59.2620524978691,-59.5533695928239,
-216.820501321751));
#195959=CARTESIAN_POINT('Ctrl Pts',(-60.846408364668,-59.8272707790866,
-213.332077521835));
#195960=CARTESIAN_POINT('Ctrl Pts',(-60.717483170112,-60.0008089880217,
-215.389142461384));
#195961=CARTESIAN_POINT('Ctrl Pts',(-59.3247742637059,-59.4595472933127,
-216.819551739489));
#195962=CARTESIAN_POINT('Ctrl Pts',(-61.0248485991141,-59.4661777525867,
-213.356063148721));
#195963=CARTESIAN_POINT('Ctrl Pts',(-60.8960486551615,-59.6575831535381,
-215.394209213837));
#195964=CARTESIAN_POINT('Ctrl Pts',(-59.4988121913041,-59.1848780549995,
-216.820109150524));
#195965=CARTESIAN_POINT('Ctrl Pts',(-61.1355702178952,-59.2205125002381,
-213.373562975861));
#195966=CARTESIAN_POINT('Ctrl Pts',(-61.0052724474296,-59.4293377571138,
-215.400754444119));
#195967=CARTESIAN_POINT('Ctrl Pts',(-59.6026295906798,-59.0049501184268,
-216.82348683657));
#195968=CARTESIAN_POINT('Ctrl Pts',(-61.2879458897718,-58.8475849978711,
-213.4017996738));
#195969=CARTESIAN_POINT('Ctrl Pts',(-61.1609971430838,-59.0727673884097,
-215.407072797124));
#195970=CARTESIAN_POINT('Ctrl Pts',(-59.7633470952239,-58.7169241462467,
-216.824211264365));
#195971=CARTESIAN_POINT('Ctrl Pts',(-61.3365745411413,-58.7222537892455,
-213.411505588854));
#195972=CARTESIAN_POINT('Ctrl Pts',(-61.2121129425345,-58.9499342096063,
-215.407804375258));
#195973=CARTESIAN_POINT('Ctrl Pts',(-59.8197452350376,-58.6155814760437,
-216.822862462453));
#195974=CARTESIAN_POINT('Ctrl Pts',(-61.4291203581917,-58.4706258868742,
-213.431043252622));
#195975=CARTESIAN_POINT('Ctrl Pts',(-61.3093836883139,-58.7040108957773,
-215.409273509837));
#195976=CARTESIAN_POINT('Ctrl Pts',(-59.9282088629343,-58.4125887823326,
-216.819930966461));
#195977=CARTESIAN_POINT('Ctrl Pts',(-61.4730253185692,-58.3443774822963,
-213.440939227881));
#195978=CARTESIAN_POINT('Ctrl Pts',(-61.3551954026654,-58.5820063400323,
-215.410605991783));
#195979=CARTESIAN_POINT('Ctrl Pts',(-59.9789475628393,-58.3124784035116,
-216.819006081135));
#195980=CARTESIAN_POINT('Ctrl Pts',(-61.597714293997,-57.9644548462852,
-213.471381381521));
#195981=CARTESIAN_POINT('Ctrl Pts',(-61.4853747357745,-58.2167534861039,
-215.415702792428));
#195982=CARTESIAN_POINT('Ctrl Pts',(-60.1242796010941,-58.0129426112489,
-216.817104343704));
#195983=CARTESIAN_POINT('Ctrl Pts',(-61.6714754954506,-57.7096224302906,
-213.492744357615));
#195984=CARTESIAN_POINT('Ctrl Pts',(-61.5626827464202,-57.9741101500247,
-215.420785448757));
#195985=CARTESIAN_POINT('Ctrl Pts',(-60.2117828099091,-57.8147192880101,
-216.81725313496));
#195986=CARTESIAN_POINT('Ctrl Pts',(-61.800714404647,-57.1969944640406,
-213.537796166935));
#195987=CARTESIAN_POINT('Ctrl Pts',(-61.7018747842135,-57.4797917294326,
-215.428818601372));
#195988=CARTESIAN_POINT('Ctrl Pts',(-60.3818196482663,-57.4046185752289,
-216.814021419008));
#195989=CARTESIAN_POINT('Ctrl Pts',(-61.8562081200387,-56.939151684957,
-213.561315895465));
#195990=CARTESIAN_POINT('Ctrl Pts',(-61.7636709827336,-57.2277557399495,
-215.431290276296));
#195991=CARTESIAN_POINT('Ctrl Pts',(-60.4646332997325,-57.1919561113795,
-216.810066154251));
#195992=CARTESIAN_POINT('Ctrl Pts',(-61.9491342563485,-56.4203496751014,
-213.610036002534));
#195993=CARTESIAN_POINT('Ctrl Pts',(-61.869519178268,-56.7212110326965,
-215.436505159072));
#195994=CARTESIAN_POINT('Ctrl Pts',(-60.6164006800181,-56.7621465040705,
-216.801040019797));
#195995=CARTESIAN_POINT('Ctrl Pts',(-61.9865582056648,-56.1594017177566,
-213.635279158387));
#195996=CARTESIAN_POINT('Ctrl Pts',(-61.9133916888105,-56.468424334395,
-215.440252708081));
#195997=CARTESIAN_POINT('Ctrl Pts',(-60.6835863552341,-56.54770132465,-216.797176937873));
#195998=CARTESIAN_POINT('Ctrl Pts',(-62.0431863828312,-55.6347775839173,
-213.688884450398));
#195999=CARTESIAN_POINT('Ctrl Pts',(-61.9838074416176,-55.9626753631027,
-215.450801296784));
#196000=CARTESIAN_POINT('Ctrl Pts',(-60.8026418999236,-56.1177717712389,
-216.79143672755));
#196001=CARTESIAN_POINT('Ctrl Pts',(-62.0623954799918,-55.3711251235972,
-213.717367123901));
#196002=CARTESIAN_POINT('Ctrl Pts',(-62.0107144541483,-55.7085961605345,
-215.45590742182));
#196003=CARTESIAN_POINT('Ctrl Pts',(-60.8571508863725,-55.9007000271699,
-216.787671355125));
#196004=CARTESIAN_POINT('Ctrl Pts',(-62.0723653519315,-55.1059089910526,
-213.746749287635));
#196005=CARTESIAN_POINT('Ctrl Pts',(-62.0291783705537,-55.4425764560866,
-215.457214771211));
#196006=CARTESIAN_POINT('Ctrl Pts',(-60.911917075676,-55.663399014185,-216.777770284882));
#196007=CARTESIAN_POINT('',(-60.9119170756758,-55.6633990141858,-216.777770284882));
#196008=CARTESIAN_POINT('',(-62.0723653519316,-55.1059089910534,-213.746749287634));
#196009=CARTESIAN_POINT('Origin',(-57.0770276271036,-54.9084593705222,-213.659487255448));
#196010=CARTESIAN_POINT('Ctrl Pts',(-60.9119170756758,-55.6633990141858,
-216.777770284882));
#196011=CARTESIAN_POINT('Ctrl Pts',(-60.8571508863725,-55.9007000271699,
-216.787671355125));
#196012=CARTESIAN_POINT('Ctrl Pts',(-60.8026418999236,-56.1177717712389,
-216.79143672755));
#196013=CARTESIAN_POINT('Ctrl Pts',(-60.6835863552341,-56.54770132465,-216.797176937873));
#196014=CARTESIAN_POINT('Ctrl Pts',(-60.6164006800181,-56.7621465040705,
-216.801040019797));
#196015=CARTESIAN_POINT('Ctrl Pts',(-60.4646332997325,-57.1919561113795,
-216.810066154251));
#196016=CARTESIAN_POINT('Ctrl Pts',(-60.3818196482663,-57.4046185752289,
-216.814021419008));
#196017=CARTESIAN_POINT('Ctrl Pts',(-60.2117828099091,-57.8147192880101,
-216.81725313496));
#196018=CARTESIAN_POINT('Ctrl Pts',(-60.1242796010941,-58.0129426112489,
-216.817104343704));
#196019=CARTESIAN_POINT('Ctrl Pts',(-59.9789475628393,-58.3124784035116,
-216.819006081135));
#196020=CARTESIAN_POINT('Ctrl Pts',(-59.9282088629343,-58.4125887823326,
-216.819930966461));
#196021=CARTESIAN_POINT('Ctrl Pts',(-59.8197452350376,-58.6155814760437,
-216.822862462453));
#196022=CARTESIAN_POINT('Ctrl Pts',(-59.7633470952239,-58.7169241462467,
-216.824211264365));
#196023=CARTESIAN_POINT('Ctrl Pts',(-59.6026295906798,-59.0049501184268,
-216.82348683657));
#196024=CARTESIAN_POINT('Ctrl Pts',(-59.4988121913041,-59.1848780549995,
-216.820109150524));
#196025=CARTESIAN_POINT('Ctrl Pts',(-59.3247742637059,-59.4595472933127,
-216.819551739489));
#196026=CARTESIAN_POINT('Ctrl Pts',(-59.2620524978691,-59.5533695928239,
-216.820501321751));
#196027=CARTESIAN_POINT('Ctrl Pts',(-59.1321238001163,-59.7406787706502,
-216.822297086344));
#196028=CARTESIAN_POINT('Ctrl Pts',(-59.065516004555,-59.8335652392552,
-216.822864771484));
#196029=CARTESIAN_POINT('Ctrl Pts',(-58.9774007039939,-59.9596050477392,
-216.820063085709));
#196030=CARTESIAN_POINT('Ctrl Pts',(-58.9507651838229,-59.99875439683,-216.818366528164));
#196031=CARTESIAN_POINT('Ctrl Pts',(-58.8942226240245,-60.0790466940644,
-216.81593623579));
#196032=CARTESIAN_POINT('Ctrl Pts',(-58.8650026632788,-60.119575817198,
-216.814991469675));
#196033=CARTESIAN_POINT('Ctrl Pts',(-58.774689151411,-60.2421218021171,
-216.812772355214));
#196034=CARTESIAN_POINT('Ctrl Pts',(-58.7107161648513,-60.3252040601318,
-216.812171008252));
#196035=CARTESIAN_POINT('Ctrl Pts',(-58.6463245735781,-60.4071924582901,
-216.811211134516));
#196036=CARTESIAN_POINT('Ctrl Pts',(-60.094651724889,-61.0923008758319,
-213.257460793579));
#196037=CARTESIAN_POINT('Ctrl Pts',(-60.1704014750534,-60.9817110085918,
-213.262796876316));
#196038=CARTESIAN_POINT('Ctrl Pts',(-60.2441117511573,-60.869896564576,
-213.268474581372));
#196039=CARTESIAN_POINT('Ctrl Pts',(-60.3516186472783,-60.7003634878465,
-213.277642216535));
#196040=CARTESIAN_POINT('Ctrl Pts',(-60.3869441313356,-60.6435508076619,
-213.280811345681));
#196041=CARTESIAN_POINT('Ctrl Pts',(-60.4565718022257,-60.5293282074256,
-213.287428511106));
#196042=CARTESIAN_POINT('Ctrl Pts',(-60.4908728037509,-60.4719198229617,
-213.290891213231));
#196043=CARTESIAN_POINT('Ctrl Pts',(-60.5922460955565,-60.2987937844743,
-213.301646644734));
#196044=CARTESIAN_POINT('Ctrl Pts',(-60.6577989462613,-60.1821636194365,
-213.309190814844));
#196045=CARTESIAN_POINT('Ctrl Pts',(-60.7848819389683,-59.9464002293958,
-213.324386876108));
#196046=CARTESIAN_POINT('Ctrl Pts',(-60.846408364668,-59.8272707790866,
-213.332077521835));
#196047=CARTESIAN_POINT('Ctrl Pts',(-61.0248485991141,-59.4661777525867,
-213.356063148721));
#196048=CARTESIAN_POINT('Ctrl Pts',(-61.1355702178952,-59.2205125002381,
-213.373562975861));
#196049=CARTESIAN_POINT('Ctrl Pts',(-61.2879458897718,-58.8475849978711,
-213.4017996738));
#196050=CARTESIAN_POINT('Ctrl Pts',(-61.3365745411413,-58.7222537892455,
-213.411505588854));
#196051=CARTESIAN_POINT('Ctrl Pts',(-61.4291203581917,-58.4706258868742,
-213.431043252622));
#196052=CARTESIAN_POINT('Ctrl Pts',(-61.4730253185692,-58.3443774822963,
-213.440939227881));
#196053=CARTESIAN_POINT('Ctrl Pts',(-61.597714293997,-57.9644548462852,
-213.471381381521));
#196054=CARTESIAN_POINT('Ctrl Pts',(-61.6714754954506,-57.7096224302906,
-213.492744357615));
#196055=CARTESIAN_POINT('Ctrl Pts',(-61.800714404647,-57.1969944640406,
-213.537796166935));
#196056=CARTESIAN_POINT('Ctrl Pts',(-61.8562081200387,-56.939151684957,
-213.561315895465));
#196057=CARTESIAN_POINT('Ctrl Pts',(-61.9491342563485,-56.4203496751014,
-213.610036002534));
#196058=CARTESIAN_POINT('Ctrl Pts',(-61.9865582056648,-56.1594017177566,
-213.635279158387));
#196059=CARTESIAN_POINT('Ctrl Pts',(-62.0431863828312,-55.6347775839173,
-213.688884450398));
#196060=CARTESIAN_POINT('Ctrl Pts',(-62.0623954799918,-55.3711251235972,
-213.717367123901));
#196061=CARTESIAN_POINT('Ctrl Pts',(-62.0723653519316,-55.1059089910534,
-213.746749287634));
#196062=CARTESIAN_POINT('Ctrl Pts',(-61.2313176176751,-54.1392424392483,
-216.589725631894));
#196063=CARTESIAN_POINT('Ctrl Pts',(-62.0809182617279,-54.1703109655338,
-215.350650293751));
#196064=CARTESIAN_POINT('Ctrl Pts',(-62.1072060041624,-54.1692103455255,
-213.848185004792));
#196065=CARTESIAN_POINT('Ctrl Pts',(-61.2063940314189,-54.2739747051073,
-216.618254256554));
#196066=CARTESIAN_POINT('Ctrl Pts',(-62.0763273182448,-54.2805873286282,
-215.369481660389));
#196067=CARTESIAN_POINT('Ctrl Pts',(-62.1041253019867,-54.2489750153891,
-213.848073204958));
#196068=CARTESIAN_POINT('Ctrl Pts',(-61.1772202905008,-54.4149797409396,
-216.647503745936));
#196069=CARTESIAN_POINT('Ctrl Pts',(-62.0715862894379,-54.394279767702,
-215.38841245438));
#196070=CARTESIAN_POINT('Ctrl Pts',(-62.1010994294235,-54.3282171953391,
-213.845465532169));
#196071=CARTESIAN_POINT('Ctrl Pts',(-61.1205413775905,-54.685792621321,
-216.694769237218));
#196072=CARTESIAN_POINT('Ctrl Pts',(-62.062453045182,-54.6155354879892,
-215.418086549984));
#196073=CARTESIAN_POINT('Ctrl Pts',(-62.0951493333573,-54.4857552569525,
-213.83553633607));
#196074=CARTESIAN_POINT('Ctrl Pts',(-61.0934782087293,-54.8149371689336,
-216.712721476424));
#196075=CARTESIAN_POINT('Ctrl Pts',(-62.058078131037,-54.7227047882016,
-215.428743044064));
#196076=CARTESIAN_POINT('Ctrl Pts',(-62.0922232746451,-54.5640610712258,
-213.828298048155));
#196077=CARTESIAN_POINT('Ctrl Pts',(-61.0165420227469,-55.1872292058749,
-216.753620691064));
#196078=CARTESIAN_POINT('Ctrl Pts',(-62.0453942577027,-55.0361844349794,
-215.450995476348));
#196079=CARTESIAN_POINT('Ctrl Pts',(-62.0835491986123,-54.7979388895741,
-213.801481239476));
#196080=CARTESIAN_POINT('Ctrl Pts',(-60.9675295053391,-55.4224312521647,
-216.767716225312));
#196081=CARTESIAN_POINT('Ctrl Pts',(-62.0373485839771,-55.237798506958,
-215.455648829851));
#196082=CARTESIAN_POINT('Ctrl Pts',(-62.0779017065461,-54.9524994590213,
-213.77694217629));
#196083=CARTESIAN_POINT('Ctrl Pts',(-60.9119170756759,-55.6633990141857,
-216.777770284882));
#196084=CARTESIAN_POINT('Ctrl Pts',(-62.0291783705539,-55.4425764560874,
-215.457214771212));
#196085=CARTESIAN_POINT('Ctrl Pts',(-62.0723653519316,-55.1059089910533,
-213.746749287634));
#196086=CARTESIAN_POINT('',(-61.2313176176752,-54.1392424392486,-216.589725631893));
#196087=CARTESIAN_POINT('',(-62.1072060041622,-54.1692103455281,-213.848185004792));
#196088=CARTESIAN_POINT('Origin',(-57.1116967348753,-53.976149530741,-213.760922972606));
#196089=CARTESIAN_POINT('Ctrl Pts',(-61.2313176176752,-54.1392424392486,
-216.589725631893));
#196090=CARTESIAN_POINT('Ctrl Pts',(-61.2241039156532,-54.1782415195011,
-216.597982568441));
#196091=CARTESIAN_POINT('Ctrl Pts',(-61.2128225788744,-54.2380631026322,
-216.610636660612));
#196092=CARTESIAN_POINT('Ctrl Pts',(-61.1926443983631,-54.3394047229831,
-216.63095046008));
#196093=CARTESIAN_POINT('Ctrl Pts',(-61.1881937267781,-54.361555288859,
-216.635330103797));
#196094=CARTESIAN_POINT('Ctrl Pts',(-61.1800246564408,-54.4018751062487,
-216.643185612872));
#196095=CARTESIAN_POINT('Ctrl Pts',(-61.1761441785378,-54.4208709408331,
-216.646828561234));
#196096=CARTESIAN_POINT('Ctrl Pts',(-61.1651728277633,-54.4743055729631,
-216.65692461498));
#196097=CARTESIAN_POINT('Ctrl Pts',(-61.1587578593242,-54.5051808903392,
-216.66254143341));
#196098=CARTESIAN_POINT('Ctrl Pts',(-61.1478391319696,-54.5574987649835,
-216.671816784675));
#196099=CARTESIAN_POINT('Ctrl Pts',(-61.1438644307081,-54.576427809643,
-216.675098825188));
#196100=CARTESIAN_POINT('Ctrl Pts',(-61.1344526503841,-54.621125696205,
-216.682563391224));
#196101=CARTESIAN_POINT('Ctrl Pts',(-61.1309617856826,-54.6376829199064,
-216.685279573515));
#196102=CARTESIAN_POINT('Ctrl Pts',(-61.1252140310211,-54.6649222567372,
-216.68962143623));
#196103=CARTESIAN_POINT('Ctrl Pts',(-61.1235283000098,-54.6729072328791,
-216.690884505207));
#196104=CARTESIAN_POINT('Ctrl Pts',(-61.118185976056,-54.6982145931637,
-216.694798416799));
#196105=CARTESIAN_POINT('Ctrl Pts',(-61.1157556494703,-54.7097314783994,
-216.69653968148));
#196106=CARTESIAN_POINT('Ctrl Pts',(-61.1091703270707,-54.7409497931566,
-216.701186611476));
#196107=CARTESIAN_POINT('Ctrl Pts',(-61.1057199535694,-54.75732388421,-216.703519943178));
#196108=CARTESIAN_POINT('Ctrl Pts',(-61.1006329227755,-54.7814840900207,
-216.706914183641));
#196109=CARTESIAN_POINT('Ctrl Pts',(-61.0994351791443,-54.7871763864764,
-216.707691861462));
#196110=CARTESIAN_POINT('Ctrl Pts',(-61.0950260074423,-54.8082043156478,
-216.710539837749));
#196111=CARTESIAN_POINT('Ctrl Pts',(-61.0901727033295,-54.8314262316928,
-216.713633471544));
#196112=CARTESIAN_POINT('Ctrl Pts',(-61.0768562795503,-54.8954423983165,
-216.721485807188));
#196113=CARTESIAN_POINT('Ctrl Pts',(-61.0684423125124,-54.9361308500724,
-216.726184275623));
#196114=CARTESIAN_POINT('Ctrl Pts',(-61.0570157190733,-54.9913415509466,
-216.73193045932));
#196115=CARTESIAN_POINT('Ctrl Pts',(-61.0557184685048,-54.9976077539097,
-216.732575505159));
#196116=CARTESIAN_POINT('Ctrl Pts',(-61.0530686957251,-55.010402144142,
-216.733876911098));
#196117=CARTESIAN_POINT('Ctrl Pts',(-61.0524981665959,-55.0131555164942,
-216.734152799324));
#196118=CARTESIAN_POINT('Ctrl Pts',(-61.0465955441629,-55.0416386881539,
-216.737003562727));
#196119=CARTESIAN_POINT('Ctrl Pts',(-61.0011802341201,-55.2603871152587,
-216.757910091499));
#196120=CARTESIAN_POINT('Ctrl Pts',(-60.9561319024597,-55.4718168818616,
-216.769776775062));
#196121=CARTESIAN_POINT('Ctrl Pts',(-60.9119170756758,-55.6633990141858,
-216.777770284882));
#196122=CARTESIAN_POINT('Ctrl Pts',(-62.0723653519316,-55.1059089910533,
-213.746749287634));
#196123=CARTESIAN_POINT('Ctrl Pts',(-62.0768793934835,-54.9808272269194,
-213.771366922062));
#196124=CARTESIAN_POINT('Ctrl Pts',(-62.0814562559514,-54.8552883758853,
-213.792161075494));
#196125=CARTESIAN_POINT('Ctrl Pts',(-62.0861030190532,-54.7293175792547,
-213.808641588779));
#196126=CARTESIAN_POINT('Ctrl Pts',(-62.0871755723782,-54.7002413397708,
-213.812445576401));
#196127=CARTESIAN_POINT('Ctrl Pts',(-62.0882518451934,-54.6711421311991,
-213.816019960739));
#196128=CARTESIAN_POINT('Ctrl Pts',(-62.0893319159675,-54.6420203440086,
-213.819359111929));
#196129=CARTESIAN_POINT('Ctrl Pts',(-62.0922302587963,-54.5638727585977,
-213.828319640385));
#196130=CARTESIAN_POINT('Ctrl Pts',(-62.0951568916024,-54.485555140642,
-213.835548948857));
#196131=CARTESIAN_POINT('Ctrl Pts',(-62.0981243813904,-54.4069862261458,
-213.840500934119));
#196132=CARTESIAN_POINT('Ctrl Pts',(-62.1011078230663,-54.327994960571,
-213.845479539022));
#196133=CARTESIAN_POINT('Ctrl Pts',(-62.10413438511,-54.2487398377294,-213.848073534587));
#196134=CARTESIAN_POINT('Ctrl Pts',(-62.1072060041623,-54.1692103455281,
-213.848185004792));
#196135=CARTESIAN_POINT('Ctrl Pts',(-62.1072060041624,-54.1692103455281,
-213.848185004792));
#196136=CARTESIAN_POINT('Ctrl Pts',(-62.080918261728,-54.1703109655354,
-215.35065029375));
#196137=CARTESIAN_POINT('Ctrl Pts',(-61.2313176176758,-54.1392424392492,
-216.589725631893));
#196138=CARTESIAN_POINT('Ctrl Pts',(-62.2073146990343,-51.5772242306456,
-213.851818178108));
#196139=CARTESIAN_POINT('Ctrl Pts',(-62.1810780798828,-51.5788094394115,
-215.350579261556));
#196140=CARTESIAN_POINT('Ctrl Pts',(-61.3352033241752,-51.5493321211721,
-216.587755286117));
#196141=CARTESIAN_POINT('Ctrl Pts',(-62.2979780119689,-48.9848138223874,
-213.855140923934));
#196142=CARTESIAN_POINT('Ctrl Pts',(-62.2718155003498,-48.9862078816536,
-215.350513478475));
#196143=CARTESIAN_POINT('Ctrl Pts',(-61.4293178843156,-48.9588621990226,
-216.585940879345));
#196144=CARTESIAN_POINT('Ctrl Pts',(-62.3791894693652,-46.3921971636372,
-213.85810601718));
#196145=CARTESIAN_POINT('Ctrl Pts',(-62.3531001006731,-46.3930946875274,
-215.350420378609));
#196146=CARTESIAN_POINT('Ctrl Pts',(-61.5136373793521,-46.3682170785133,
-216.584262774589));
#196147=CARTESIAN_POINT('',(-61.744621222757,-46.4961938535833,-216.203488008845));
#196148=CARTESIAN_POINT('',(-62.3685684251148,-46.7295482205574,-213.857736690702));
#196149=CARTESIAN_POINT('Ctrl Pts',(-61.744621222757,-46.4961938535833,
-216.203488008845));
#196150=CARTESIAN_POINT('Ctrl Pts',(-61.9444015485133,-46.53632319838,-215.842641422324));
#196151=CARTESIAN_POINT('Ctrl Pts',(-62.0956418404579,-46.575986655544,
-215.465343832456));
#196152=CARTESIAN_POINT('Ctrl Pts',(-62.3051774478038,-46.6542220635401,
-214.679483825453));
#196153=CARTESIAN_POINT('Ctrl Pts',(-62.3625672140424,-46.6930523819976,
-214.267454208411));
#196154=CARTESIAN_POINT('Ctrl Pts',(-62.3685683162547,-46.7295549501427,
-213.857737288663));
#196155=CARTESIAN_POINT('',(-61.5121276274155,-46.4145707938183,-216.584292819094));
#196156=CARTESIAN_POINT('Ctrl Pts',(-61.5121276273779,-46.414570793914,
-216.584292819144));
#196157=CARTESIAN_POINT('Ctrl Pts',(-61.5887158305549,-46.4514128718707,
-216.470096233485));
#196158=CARTESIAN_POINT('Ctrl Pts',(-61.6670075359489,-46.4806037630794,
-216.343675158136));
#196159=CARTESIAN_POINT('Ctrl Pts',(-61.744621222757,-46.4961938535833,
-216.203488008845));
#196160=CARTESIAN_POINT('Origin',(967.127514096642,-12.8777453687604,-231.930774818293));
#196161=CARTESIAN_POINT('Origin',(1003.27568749664,-12.9672887026865,-175.207747633911));
#196162=CARTESIAN_POINT('Ctrl Pts',(-61.5121276273784,-46.4145707939176,
-216.584292819143));
#196163=CARTESIAN_POINT('Ctrl Pts',(-61.6347030716742,-46.0974912749705,
-216.419279621934));
#196164=CARTESIAN_POINT('Ctrl Pts',(-61.6760242364037,-45.7878268313144,
-216.206690793879));
#196165=CARTESIAN_POINT('Ctrl Pts',(-61.5887158305549,-46.4514128718707,
-216.470096233485));
#196166=CARTESIAN_POINT('Ctrl Pts',(-61.683502987622,-46.1340834295878,
-216.336103167041));
#196167=CARTESIAN_POINT('Ctrl Pts',(-61.705984565682,-45.8233265979214,
-216.161095232372));
#196168=CARTESIAN_POINT('Ctrl Pts',(-61.6670075359489,-46.4806037630794,
-216.343675158136));
#196169=CARTESIAN_POINT('Ctrl Pts',(-61.734382175831,-46.1635375612304,
-216.245336224123));
#196170=CARTESIAN_POINT('Ctrl Pts',(-61.7366373868477,-45.8522624046448,
-216.111341099556));
#196171=CARTESIAN_POINT('Ctrl Pts',(-61.7446212227572,-46.4961938535835,
-216.203488008845));
#196172=CARTESIAN_POINT('Ctrl Pts',(-61.7864942538559,-46.180062496681,
-216.146540979352));
#196173=CARTESIAN_POINT('Ctrl Pts',(-61.7670197730424,-45.8692809645531,
-216.057260894206));
#196174=CARTESIAN_POINT('',(-61.7670229802613,-45.8692803056811,-216.057262488689));
#196175=CARTESIAN_POINT('',(-61.6760242364037,-45.7878268313144,-216.206690793879));
#196176=CARTESIAN_POINT('Ctrl Pts',(-61.7670197730424,-45.8692809645531,
-216.057260894206));
#196177=CARTESIAN_POINT('Ctrl Pts',(-61.7550845759282,-45.8625955281523,
-216.078505376257));
#196178=CARTESIAN_POINT('Ctrl Pts',(-61.7431797205979,-45.8541157626504,
-216.09895572827));
#196179=CARTESIAN_POINT('Ctrl Pts',(-61.7313327668648,-45.8441875369102,
-216.118692873593));
#196180=CARTESIAN_POINT('Ctrl Pts',(-61.7181196244691,-45.8331143898888,
-216.140706103113));
#196181=CARTESIAN_POINT('Ctrl Pts',(-61.7049782693999,-45.8202388887419,
-216.161832421571));
#196182=CARTESIAN_POINT('Ctrl Pts',(-61.691944049084,-45.8059771350208,
-216.18216400124));
#196183=CARTESIAN_POINT('Ctrl Pts',(-61.6866187518076,-45.8001503132848,
-216.190470727935));
#196184=CARTESIAN_POINT('Ctrl Pts',(-61.6813113292403,-45.7940914674599,
-216.198644554988));
#196185=CARTESIAN_POINT('Ctrl Pts',(-61.6760242364037,-45.7878268313144,
-216.206690793879));
#196186=CARTESIAN_POINT('Origin',(-59.0334256450291,-46.3348777618666,-214.896191665971));
#196187=CARTESIAN_POINT('Origin',(-59.1250215884199,-46.412156871143,-214.743818340268));
#196188=CARTESIAN_POINT('Ctrl Pts',(-61.744621222757,-46.4961938535834,
-216.203488008845));
#196189=CARTESIAN_POINT('Ctrl Pts',(-61.7864942538559,-46.1800624966811,
-216.146540979352));
#196190=CARTESIAN_POINT('Ctrl Pts',(-61.7670197730426,-45.8692809645531,
-216.057260894206));
#196191=CARTESIAN_POINT('Ctrl Pts',(-61.9444015484922,-46.5363231985591,
-215.842641422359));
#196192=CARTESIAN_POINT('Ctrl Pts',(-61.9754348687076,-46.2721634433876,
-215.791058678043));
#196193=CARTESIAN_POINT('Ctrl Pts',(-61.9631621369174,-46.0106807568515,
-215.721163036308));
#196194=CARTESIAN_POINT('Ctrl Pts',(-62.0956418404433,-46.5759866556878,
-215.465343832486));
#196195=CARTESIAN_POINT('Ctrl Pts',(-62.1171497321372,-46.3642951884269,
-215.421651993854));
#196196=CARTESIAN_POINT('Ctrl Pts',(-62.1106980495454,-46.1537572969976,
-215.368567684276));
#196197=CARTESIAN_POINT('Ctrl Pts',(-62.3051790602976,-46.6542226656792,
-214.679477777819));
#196198=CARTESIAN_POINT('Ctrl Pts',(-62.3119048875977,-46.5481874588022,
-214.656051542736));
#196199=CARTESIAN_POINT('Ctrl Pts',(-62.3127271221,-46.4421422876624,-214.631724106531));
#196200=CARTESIAN_POINT('Ctrl Pts',(-62.3625689806341,-46.6930535773299,
-214.267441525086));
#196201=CARTESIAN_POINT('Ctrl Pts',(-62.3644265280729,-46.6408054190759,
-214.25579858017));
#196202=CARTESIAN_POINT('Ctrl Pts',(-62.3662837353377,-46.5885519083916,
-214.24418481767));
#196203=CARTESIAN_POINT('Ctrl Pts',(-62.3685685933127,-46.7295566356152,
-213.857718370431));
#196204=CARTESIAN_POINT('Ctrl Pts',(-62.3685685933127,-46.7295566356152,
-213.857718370431));
#196205=CARTESIAN_POINT('Ctrl Pts',(-62.3685685933127,-46.7295566356152,
-213.857718370431));
#196206=CARTESIAN_POINT('Ctrl Pts',(-61.7670197730478,-45.8692809645569,
-216.057260894197));
#196207=CARTESIAN_POINT('Ctrl Pts',(-61.7860307089207,-45.8829860222033,
-216.024684888233));
#196208=CARTESIAN_POINT('Ctrl Pts',(-61.8063428741164,-45.8979710373087,
-215.988950140515));
#196209=CARTESIAN_POINT('Ctrl Pts',(-61.8277026039749,-45.914260388285,
-215.949926047446));
#196210=CARTESIAN_POINT('Ctrl Pts',(-61.8490085554087,-45.9305087267746,
-215.911000207224));
#196211=CARTESIAN_POINT('Ctrl Pts',(-61.8713568284104,-45.9480548595732,
-215.86880157429));
#196212=CARTESIAN_POINT('Ctrl Pts',(-61.8944466268228,-45.9669239189239,
-215.823183826969));
#196213=CARTESIAN_POINT('Ctrl Pts',(-61.9174819143512,-45.9857484318006,
-215.777673774989));
#196214=CARTESIAN_POINT('Ctrl Pts',(-61.9412552413371,-46.0058896543611,
-215.728760738867));
#196215=CARTESIAN_POINT('Ctrl Pts',(-61.9654187894528,-46.0273731743951,
-215.676282670045));
#196216=CARTESIAN_POINT('Ctrl Pts',(-61.9707824231834,-46.0321419166408,
-215.664634002444));
#196217=CARTESIAN_POINT('Ctrl Pts',(-61.9761650911893,-46.0369767977574,
-215.652809614194));
#196218=CARTESIAN_POINT('Ctrl Pts',(-61.9815626594367,-46.0418781000279,
-215.640807620315));
#196219=CARTESIAN_POINT('Ctrl Pts',(-62.0078995976887,-46.0657935540502,
-215.582244994109));
#196220=CARTESIAN_POINT('Ctrl Pts',(-62.0345910813097,-46.0912866876058,
-215.519464379018));
#196221=CARTESIAN_POINT('Ctrl Pts',(-62.0610868871434,-46.1183546518921,
-215.452322901564));
#196222=CARTESIAN_POINT('Ctrl Pts',(-62.0786458767962,-46.1362928156833,
-215.407827689179));
#196223=CARTESIAN_POINT('Ctrl Pts',(-62.0961186585576,-46.1549235122947,
-215.361414642324));
#196224=CARTESIAN_POINT('Ctrl Pts',(-62.1133307833226,-46.1742425534407,
-215.31304610448));
#196225=CARTESIAN_POINT('Ctrl Pts',(-62.128223696963,-46.1909584914978,
-215.271194882341));
#196226=CARTESIAN_POINT('Ctrl Pts',(-62.1429202037568,-46.208188641063,
-215.227882394232));
#196227=CARTESIAN_POINT('Ctrl Pts',(-62.1573003639315,-46.2259262935355,
-215.183092496691));
#196228=CARTESIAN_POINT('Ctrl Pts',(-62.1661086492019,-46.2367911449076,
-215.155657322814));
#196229=CARTESIAN_POINT('Ctrl Pts',(-62.1749359514523,-46.2480214779255,
-215.127224607864));
#196230=CARTESIAN_POINT('Ctrl Pts',(-62.1835512608191,-46.2593673508619,
-215.09841714778));
#196231=CARTESIAN_POINT('Ctrl Pts',(-62.192090487231,-46.2706130268697,
-215.069864090247));
#196232=CARTESIAN_POINT('Ctrl Pts',(-62.2004213907544,-46.2819722055932,
-215.04094285704));
#196233=CARTESIAN_POINT('Ctrl Pts',(-62.2083681674017,-46.2932002549787,
-215.012276600892));
#196234=CARTESIAN_POINT('Ctrl Pts',(-62.2094184292088,-46.2946841763169,
-215.008488011465));
#196235=CARTESIAN_POINT('Ctrl Pts',(-62.2104620521714,-46.2961658055334,
-215.004703899692));
#196236=CARTESIAN_POINT('Ctrl Pts',(-62.2114986946153,-46.2976445763721,
-215.000925725915));
#196237=CARTESIAN_POINT('Ctrl Pts',(-62.2115700245438,-46.2977463285421,
-215.000665755019));
#196238=CARTESIAN_POINT('Ctrl Pts',(-62.2116413216157,-46.297848067624,
-215.000405811611));
#196239=CARTESIAN_POINT('Ctrl Pts',(-62.2117125858462,-46.2979497936101,
-215.000145895713));
#196240=CARTESIAN_POINT('Ctrl Pts',(-62.2298446813421,-46.3238324177585,
-214.934014263643));
#196241=CARTESIAN_POINT('Ctrl Pts',(-62.2458179332301,-46.3489008751118,
-214.869560714848));
#196242=CARTESIAN_POINT('Ctrl Pts',(-62.2598734755854,-46.3729950016063,
-214.807262372277));
#196243=CARTESIAN_POINT('Ctrl Pts',(-62.2741714237111,-46.3975046620692,
-214.743889615262));
#196244=CARTESIAN_POINT('Ctrl Pts',(-62.2864855615421,-46.4210061172213,
-214.682747266005));
#196245=CARTESIAN_POINT('Ctrl Pts',(-62.297096987798,-46.4433539938431,
-214.624295756784));
#196246=CARTESIAN_POINT('Ctrl Pts',(-62.3081336004919,-46.4665973216352,
-214.563502169468));
#196247=CARTESIAN_POINT('Ctrl Pts',(-62.3173291366072,-46.4885928399262,
-214.505619582526));
#196248=CARTESIAN_POINT('Ctrl Pts',(-62.3250181713757,-46.5092013876676,
-214.451117556556));
#196249=CARTESIAN_POINT('Ctrl Pts',(-62.3295400872478,-46.5213212599191,
-214.419064953893));
#196250=CARTESIAN_POINT('Ctrl Pts',(-62.3335412504316,-46.53296189092,-214.388180620701));
#196251=CARTESIAN_POINT('Ctrl Pts',(-62.3370905398435,-46.5440983979919,
-214.3585525217));
#196252=CARTESIAN_POINT('Ctrl Pts',(-62.3431483131307,-46.563105705434,
-214.307984566864));
#196253=CARTESIAN_POINT('Ctrl Pts',(-62.3481974598883,-46.5816012447937,
-214.258543468685));
#196254=CARTESIAN_POINT('Ctrl Pts',(-62.3523753769479,-46.5997120229032,
-214.209924790467));
#196255=CARTESIAN_POINT('Ctrl Pts',(-62.3566237941043,-46.6181284106238,
-214.16048569828));
#196256=CARTESIAN_POINT('Ctrl Pts',(-62.3599712539605,-46.6361470995734,
-214.111896534487));
#196257=CARTESIAN_POINT('Ctrl Pts',(-62.3625099115766,-46.6539010598174,
-214.063821875696));
#196258=CARTESIAN_POINT('Ctrl Pts',(-62.3650776056205,-46.6718580846975,
-214.015197352934));
#196259=CARTESIAN_POINT('Ctrl Pts',(-62.3668178742564,-46.6895444447507,
-213.967098722728));
#196260=CARTESIAN_POINT('Ctrl Pts',(-62.3677738035265,-46.7070947829981,
-213.919170467337));
#196261=CARTESIAN_POINT('Ctrl Pts',(-62.3681826664685,-46.7146012828563,
-213.89867095119));
#196262=CARTESIAN_POINT('Ctrl Pts',(-62.3684473988348,-46.7220828491721,
-213.878202538093));
#196263=CARTESIAN_POINT('Ctrl Pts',(-62.3685684816626,-46.7295497479019,
-213.857737248298));
#196264=CARTESIAN_POINT('Ctrl Pts',(-61.7048393179462,20.3302886060538,
-216.296804750573));
#196265=CARTESIAN_POINT('Ctrl Pts',(-62.3412105997785,20.8703282681299,
-215.296246486213));
#196266=CARTESIAN_POINT('Ctrl Pts',(-62.3422326083537,21.4655488148376,
-214.137178092368));
#196267=CARTESIAN_POINT('Ctrl Pts',(-61.7197275390738,19.826031280405,-216.049349212268));
#196268=CARTESIAN_POINT('Ctrl Pts',(-62.3639049458357,20.3085254361885,
-215.01549277859));
#196269=CARTESIAN_POINT('Ctrl Pts',(-62.3680533687934,20.8390832880415,
-213.816997588));
#196270=CARTESIAN_POINT('Ctrl Pts',(-61.7308466500715,19.2797411012228,
-215.844507094054));
#196271=CARTESIAN_POINT('Ctrl Pts',(-62.3866177449706,19.7060437424658,
-214.781622878777));
#196272=CARTESIAN_POINT('Ctrl Pts',(-62.3936763768326,20.173797793921,-213.547199312721));
#196273=CARTESIAN_POINT('Ctrl Pts',(-61.7466079433738,18.1603035078498,
-215.528079628832));
#196274=CARTESIAN_POINT('Ctrl Pts',(-62.4297966614041,18.4809322317388,
-214.415601481719));
#196275=CARTESIAN_POINT('Ctrl Pts',(-62.4421294023084,18.8292102512286,
-213.116884807332));
#196276=CARTESIAN_POINT('Ctrl Pts',(-61.7513829905102,17.5842705648492,
-215.414156702354));
#196277=CARTESIAN_POINT('Ctrl Pts',(-62.4504311411109,17.8546566875628,
-214.280854067528));
#196278=CARTESIAN_POINT('Ctrl Pts',(-62.465140608479,18.1462075363528,-212.953486548188));
#196279=CARTESIAN_POINT('Ctrl Pts',(-61.75613865849,16.4063111425851,-215.262563594693));
#196280=CARTESIAN_POINT('Ctrl Pts',(-62.4897414461557,16.5806351950176,
-214.093342676416));
#196281=CARTESIAN_POINT('Ctrl Pts',(-62.5088056235126,16.7621631730818,
-212.713827714098));
#196282=CARTESIAN_POINT('Ctrl Pts',(-61.7560859039706,15.8044369348897,
-215.225019582751));
#196283=CARTESIAN_POINT('Ctrl Pts',(-62.5084194911065,15.9326272322602,
-214.040799041022));
#196284=CARTESIAN_POINT('Ctrl Pts',(-62.5294585302,16.0610980086206,-212.637681074466));
#196285=CARTESIAN_POINT('Ctrl Pts',(-61.75170975595,14.5794316584473,-215.219446270607));
#196286=CARTESIAN_POINT('Ctrl Pts',(-62.5437558590124,14.61854768797,-214.009629694108));
#196287=CARTESIAN_POINT('Ctrl Pts',(-62.568416048291,14.6428357290722,-212.563275779234));
#196288=CARTESIAN_POINT('Ctrl Pts',(-61.7474254168418,13.9650471940131,
-215.251428369238));
#196289=CARTESIAN_POINT('Ctrl Pts',(-62.5601618106751,13.9616961240068,
-214.031343271628));
#196290=CARTESIAN_POINT('Ctrl Pts',(-62.5864410346862,13.9358240577698,
-212.565541839207));
#196291=CARTESIAN_POINT('Ctrl Pts',(-61.7289261711493,12.1227396799969,
-215.437974674513));
#196292=CARTESIAN_POINT('Ctrl Pts',(-62.6058121860344,11.9946652158632,
-214.19272370704));
#196293=CARTESIAN_POINT('Ctrl Pts',(-62.6364325628104,11.8237195743705,
-212.673714044577));
#196294=CARTESIAN_POINT('Ctrl Pts',(-61.7091779624899,10.8934347501059,
-215.682357515454));
#196295=CARTESIAN_POINT('Ctrl Pts',(-62.6314451217397,10.6892364940185,
-214.428306849402));
#196296=CARTESIAN_POINT('Ctrl Pts',(-62.6643973443486,10.4250272317226,
-212.879944055009));
#196297=CARTESIAN_POINT('Ctrl Pts',(-61.6812232412141,9.63282158578171,
-216.039230989765));
#196298=CARTESIAN_POINT('Ctrl Pts',(-62.6532663489862,9.3570927525791,-214.780166408587));
#196299=CARTESIAN_POINT('Ctrl Pts',(-62.6882099634729,8.99324453840434,
-213.207737243319));
#196300=CARTESIAN_POINT('Ctrl Pts',(-61.6803687865461,9.59462850398232,
-216.050145822074));
#196301=CARTESIAN_POINT('Ctrl Pts',(-62.6539249040132,9.31663341093719,
-214.790961694005));
#196302=CARTESIAN_POINT('Ctrl Pts',(-62.6889267575668,8.94986797086315,
-213.217780919797));
#196303=CARTESIAN_POINT('Ctrl Pts',(-61.6790760497614,9.53735006211111,
-216.06666835234));
#196304=CARTESIAN_POINT('Ctrl Pts',(-62.6549061690901,9.25596256650207,
-214.807312410465));
#196305=CARTESIAN_POINT('Ctrl Pts',(-62.6899947648924,8.88481924518834,
-213.233011700938));
#196306=CARTESIAN_POINT('Ctrl Pts',(-61.6813278541514,9.51005174913774,
-216.070633460958));
#196307=CARTESIAN_POINT('Ctrl Pts',(-62.6553509085009,9.23107896539847,
-214.811457518833));
#196308=CARTESIAN_POINT('Ctrl Pts',(-62.6903499578521,8.86313707307296,
-213.238096257499));
#196309=CARTESIAN_POINT('Ctrl Pts',(-61.6842939631037,9.46010771421665,
-216.079339374395));
#196310=CARTESIAN_POINT('Ctrl Pts',(-62.6561734349085,9.18394861329238,
-214.820392132479));
#196311=CARTESIAN_POINT('Ctrl Pts',(-62.6910610727134,8.81976237959425,
-213.24815996515));
#196312=CARTESIAN_POINT('Ctrl Pts',(-61.6857737786881,9.43512707163234,
-216.083656167532));
#196313=CARTESIAN_POINT('Ctrl Pts',(-62.6565846451019,9.16037796026954,
-214.824824505124));
#196314=CARTESIAN_POINT('Ctrl Pts',(-62.6914166532021,8.79807157636304,
-213.253156652719));
#196315=CARTESIAN_POINT('Ctrl Pts',(-61.6931565890002,9.31018038032887,
-216.105058365171));
#196316=CARTESIAN_POINT('Ctrl Pts',(-62.6586400955044,9.04251720585592,
-214.846806972038));
#196317=CARTESIAN_POINT('Ctrl Pts',(-62.693194685499,8.68960018849763,-213.277963347887));
#196318=CARTESIAN_POINT('Ctrl Pts',(-61.6990107871747,9.21008393110796,
-216.12159850752));
#196319=CARTESIAN_POINT('Ctrl Pts',(-62.6602839455125,8.94812374264299,
-214.863834333959));
#196320=CARTESIAN_POINT('Ctrl Pts',(-62.6946175261465,8.60276749258736,
-213.297243169367));
#196321=CARTESIAN_POINT('Ctrl Pts',(-61.7164142065137,8.90936371264559,
-216.169436492099));
#196322=CARTESIAN_POINT('Ctrl Pts',(-62.665212603975,8.66473293878732,-214.913181982244));
#196323=CARTESIAN_POINT('Ctrl Pts',(-62.6988878681185,8.34209912341666,
-213.353350073391));
#196324=CARTESIAN_POINT('Ctrl Pts',(-61.7278043599611,8.70830926312332,
-216.198952520733));
#196325=CARTESIAN_POINT('Ctrl Pts',(-62.6684968108444,8.47539373639615,
-214.943794401356));
#196326=CARTESIAN_POINT('Ctrl Pts',(-62.7017371797689,8.16809322419483,
-213.388445162646));
#196327=CARTESIAN_POINT('Ctrl Pts',(-61.7613103499456,8.10330948564394,
-216.280050016991));
#196328=CARTESIAN_POINT('Ctrl Pts',(-62.6783432928825,7.90644691041792,
-215.028387072985));
#196329=CARTESIAN_POINT('Ctrl Pts',(-62.7102973061948,7.64536444873709,
-213.486494648338));
#196330=CARTESIAN_POINT('Ctrl Pts',(-61.7827637049333,7.69753105649767,
-216.324192904775));
#196331=CARTESIAN_POINT('Ctrl Pts',(-62.6849084717677,7.52538355400632,
-215.075235965833));
#196332=CARTESIAN_POINT('Ctrl Pts',(-62.7160201318226,7.29593153216955,
-213.542223849032));
#196333=CARTESIAN_POINT('Ctrl Pts',(-61.8441798777663,6.47185390193823,
-216.423878386747));
#196334=CARTESIAN_POINT('Ctrl Pts',(-62.7046282021264,6.37770422140462,
-215.184004366012));
#196335=CARTESIAN_POINT('Ctrl Pts',(-62.7332823333847,6.24451635056923,
-213.677692349319));
#196336=CARTESIAN_POINT('Ctrl Pts',(-61.8807935575335,5.64537503727213,
-216.447122146682));
#196337=CARTESIAN_POINT('Ctrl Pts',(-62.7178214583037,5.60536816135207,
-215.214862678102));
#196338=CARTESIAN_POINT('Ctrl Pts',(-62.7449139403618,5.53942734608012,
-213.725811404425));
#196339=CARTESIAN_POINT('Ctrl Pts',(-61.9276637801842,4.38900749273041,
-216.405043063736));
#196340=CARTESIAN_POINT('Ctrl Pts',(-62.737836834247,4.4352006251806,-215.186375172552));
#196341=CARTESIAN_POINT('Ctrl Pts',(-62.7627331655823,4.47441539748971,
-213.722866226851));
#196342=CARTESIAN_POINT('Ctrl Pts',(-61.9418614366659,3.96797397400649,
-216.378259335607));
#196343=CARTESIAN_POINT('Ctrl Pts',(-62.7445389526157,4.0435897159706,-215.164491462244));
#196344=CARTESIAN_POINT('Ctrl Pts',(-62.768735486043,4.11817803005001,-213.709326696003));
#196345=CARTESIAN_POINT('Ctrl Pts',(-61.9671948784838,3.12080313566866,
-216.297090847051));
#196346=CARTESIAN_POINT('Ctrl Pts',(-62.7580382224546,3.2566272438502,-215.093872524279));
#196347=CARTESIAN_POINT('Ctrl Pts',(-62.7808960763507,3.40303826439861,
-213.655109821494));
#196348=CARTESIAN_POINT('Ctrl Pts',(-61.9783399396214,2.69421717174147,
-216.242544071251));
#196349=CARTESIAN_POINT('Ctrl Pts',(-62.7648437006275,2.86082211157324,
-215.045005100094));
#196350=CARTESIAN_POINT('Ctrl Pts',(-62.7870578417518,3.04396622992889,
-213.614329768932));
#196351=CARTESIAN_POINT('Ctrl Pts',(-61.9971071789784,1.84291295407256,
-216.104949160831));
#196352=CARTESIAN_POINT('Ctrl Pts',(-62.7784709761191,2.07150539346803,
-214.919405013978));
#196353=CARTESIAN_POINT('Ctrl Pts',(-62.7994785535875,2.32831168170424,
-213.504372226852));
#196354=CARTESIAN_POINT('Ctrl Pts',(-62.0047577753412,1.41755300336648,
-216.021919722206));
#196355=CARTESIAN_POINT('Ctrl Pts',(-62.7853055583149,1.6772084331531,-214.842667949039));
#196356=CARTESIAN_POINT('Ctrl Pts',(-62.8057475169848,1.97109323824117,
-213.43520790963));
#196357=CARTESIAN_POINT('Ctrl Pts',(-62.01209734533,0.886092884169537,-215.899694254584));
#196358=CARTESIAN_POINT('Ctrl Pts',(-62.7938861397906,1.18486559069481,
-214.728722297667));
#196359=CARTESIAN_POINT('Ctrl Pts',(-62.8136699413683,1.52535840970665,
-213.330389729488));
#196360=CARTESIAN_POINT('Ctrl Pts',(-62.0134539642545,0.779812584027515,
-215.874326692892));
#196361=CARTESIAN_POINT('Ctrl Pts',(-62.7956043592763,1.08641018260874,
-214.705028633956));
#196362=CARTESIAN_POINT('Ctrl Pts',(-62.815258743729,1.43625087082071,-213.308507593622));
#196363=CARTESIAN_POINT('Ctrl Pts',(-62.0153204933596,0.620406471798272,
-215.834877732922));
#196364=CARTESIAN_POINT('Ctrl Pts',(-62.7981848937995,0.938758219164633,
-214.668121421941));
#196365=CARTESIAN_POINT('Ctrl Pts',(-62.8176486878298,1.30264926379029,
-213.27429362079));
#196366=CARTESIAN_POINT('Ctrl Pts',(-62.01591460122,0.567273487007788,-215.8214951353));
#196367=CARTESIAN_POINT('Ctrl Pts',(-62.7990456346484,0.889544467315833,
-214.655590802865));
#196368=CARTESIAN_POINT('Ctrl Pts',(-62.8184464593903,1.25812534522924,
-213.262657162745));
#196369=CARTESIAN_POINT('Ctrl Pts',(-62.0166219833978,0.500859866452599,
-215.804474193104));
#196370=CARTESIAN_POINT('Ctrl Pts',(-62.8001222578722,0.828033612066846,
-214.639641386032));
#196371=CARTESIAN_POINT('Ctrl Pts',(-62.8194451065877,1.20248294550228,
-213.247820438255));
#196372=CARTESIAN_POINT('Ctrl Pts',(-62.0167616971461,0.487577272851923,
-215.801055369767));
#196373=CARTESIAN_POINT('Ctrl Pts',(-62.8003376213968,0.815731527809191,
-214.636437135192));
#196374=CARTESIAN_POINT('Ctrl Pts',(-62.8196449076661,1.19135509048132,
-213.24483853566));
#196375=CARTESIAN_POINT('Ctrl Pts',(-62.0170375949548,0.461012336886231,
-215.79418841463));
#196376=CARTESIAN_POINT('Ctrl Pts',(-62.8007684207769,0.791127882266898,
-214.629999954911));
#196377=CARTESIAN_POINT('Ctrl Pts',(-62.8200446538203,1.16910063183232,
-213.238845579474));
#196378=CARTESIAN_POINT('Ctrl Pts',(-62.0171192435935,0.445144526651812,
-215.79019033046));
#196379=CARTESIAN_POINT('Ctrl Pts',(-62.8010073784724,0.777422914824527,
-214.626482823901));
#196380=CARTESIAN_POINT('Ctrl Pts',(-62.8202446769488,1.15797422718805,
-213.235829903834));
#196381=CARTESIAN_POINT('Ctrl Pts',(-62.0177632729019,0.416720308882189,
-215.782227774949));
#196382=CARTESIAN_POINT('Ctrl Pts',(-62.8015499256584,0.746719684915778,
-214.617992853663));
#196383=CARTESIAN_POINT('Ctrl Pts',(-62.820844450332,1.12459558461347,-213.226769479741));
#196384=CARTESIAN_POINT('Ctrl Pts',(-62.0181895523145,0.397765742510003,
-215.776959654906));
#196385=CARTESIAN_POINT('Ctrl Pts',(-62.8019103468331,0.726247045178752,
-214.612375378367));
#196386=CARTESIAN_POINT('Ctrl Pts',(-62.8212428505405,1.1023412309075,-213.220773750029));
#196387=CARTESIAN_POINT('Ctrl Pts',(-62.021998557213,0.227129297670825,
-215.729907595764));
#196388=CARTESIAN_POINT('Ctrl Pts',(-62.8051425298092,0.541966547718803,
-214.562201271057));
#196389=CARTESIAN_POINT('Ctrl Pts',(-62.8248154365297,0.902034785262884,
-213.16721163518));
#196390=CARTESIAN_POINT('Ctrl Pts',(-62.0251888105107,0.0751301734146063,
-215.69065008324));
#196391=CARTESIAN_POINT('Ctrl Pts',(-62.8079340444995,0.377915226937975,
-214.520310461555));
#196392=CARTESIAN_POINT('Ctrl Pts',(-62.8278985261067,0.72386189685476,
-213.122440498364));
#196393=CARTESIAN_POINT('Ctrl Pts',(-62.0522125573282,-1.29554564506861,
-215.359846846471));
#196394=CARTESIAN_POINT('Ctrl Pts',(-62.8323237597321,-1.10022488337052,
-214.167113276732));
#196395=CARTESIAN_POINT('Ctrl Pts',(-62.8548240427874,-0.880767445010574,
-212.744334484548));
#196396=CARTESIAN_POINT('Ctrl Pts',(-62.0645369285303,-2.53275074795512,
-215.223595176109));
#196397=CARTESIAN_POINT('Ctrl Pts',(-62.8488703095335,-2.42925885397665,
-214.019298532614));
#196398=CARTESIAN_POINT('Ctrl Pts',(-62.8729565843244,-2.31461725004268,
-212.582049783317));
#196399=CARTESIAN_POINT('Ctrl Pts',(-62.0693960981775,-5.02446259512134,
-215.234052482319));
#196400=CARTESIAN_POINT('Ctrl Pts',(-62.8719056110164,-5.1003827717422,
-214.019608088502));
#196401=CARTESIAN_POINT('Ctrl Pts',(-62.8981414605001,-5.19559191584348,
-212.564399664962));
#196402=CARTESIAN_POINT('Ctrl Pts',(-62.0618907988487,-6.27912184780759,
-215.381002476288));
#196403=CARTESIAN_POINT('Ctrl Pts',(-62.8783989700247,-6.4443743523136,
-214.168268362741));
#196404=CARTESIAN_POINT('Ctrl Pts',(-62.9051900334741,-6.64273030664321,
-212.709348944425));
#196405=CARTESIAN_POINT('Ctrl Pts',(-62.0408583819432,-7.6912959294504,
-215.713424151605));
#196406=CARTESIAN_POINT('Ctrl Pts',(-62.8798161172096,-7.9569135349361,
-214.509722650088));
#196407=CARTESIAN_POINT('Ctrl Pts',(-62.9066422728629,-8.27861416050181,
-213.053996708501));
#196408=CARTESIAN_POINT('Ctrl Pts',(-62.0383424658172,-7.84822778562573,
-215.752714376751));
#196409=CARTESIAN_POINT('Ctrl Pts',(-62.8798914154057,-8.12519201954069,
-214.550165533701));
#196410=CARTESIAN_POINT('Ctrl Pts',(-62.9067130375752,-8.46050513615589,
-213.09485254092));
#196411=CARTESIAN_POINT('Ctrl Pts',(-62.0342925038254,-8.08357756168836,
-215.815225127789));
#196412=CARTESIAN_POINT('Ctrl Pts',(-62.8798796987704,-8.37759392911409,
-214.614571441277));
#196413=CARTESIAN_POINT('Ctrl Pts',(-62.9066818269245,-8.7334636680148,
-213.160032454394));
#196414=CARTESIAN_POINT('Ctrl Pts',(-62.0328986542006,-8.16189402537491,
-215.836624633389));
#196415=CARTESIAN_POINT('Ctrl Pts',(-62.8798550144986,-8.46160075459694,
-214.636632184066));
#196416=CARTESIAN_POINT('Ctrl Pts',(-62.9066485485958,-8.82432470155739,
-213.182373733743));
#196417=CARTESIAN_POINT('Ctrl Pts',(-62.0311011014652,-8.25962032848021,
-215.864076645694));
#196418=CARTESIAN_POINT('Ctrl Pts',(-62.879798315969,-8.5664344313122,-214.664943966702));
#196419=CARTESIAN_POINT('Ctrl Pts',(-62.9065784769814,-8.9377445621295,
-213.211068643959));
#196420=CARTESIAN_POINT('Ctrl Pts',(-62.0307388286769,-8.27915712437951,
-215.869602181102));
#196421=CARTESIAN_POINT('Ctrl Pts',(-62.8797856829879,-8.58739394937797,
-214.670643537108));
#196422=CARTESIAN_POINT('Ctrl Pts',(-62.9065630389366,-8.96042071227823,
-213.21684604351));
#196423=CARTESIAN_POINT('Ctrl Pts',(-62.0301912677851,-8.30844957422519,
-215.877943176995));
#196424=CARTESIAN_POINT('Ctrl Pts',(-62.8797647971169,-8.6188202438996,
-214.679248133562));
#196425=CARTESIAN_POINT('Ctrl Pts',(-62.9065377484219,-8.99442320332278,
-213.225569775073));
#196426=CARTESIAN_POINT('Ctrl Pts',(-62.0296632681837,-8.31557091097187,
-215.880572879503));
#196427=CARTESIAN_POINT('Ctrl Pts',(-62.8797526332712,-8.62783903034508,
-214.682096820377));
#196428=CARTESIAN_POINT('Ctrl Pts',(-62.9065289038154,-9.00575475319362,
-213.228490523493));
#196429=CARTESIAN_POINT('Ctrl Pts',(-62.0302223796579,-8.34218925560487,
-215.886598433304));
#196430=CARTESIAN_POINT('Ctrl Pts',(-62.8797505157256,-8.65269102163767,
-214.687948520214));
#196431=CARTESIAN_POINT('Ctrl Pts',(-62.9065107565237,-9.02841676695755,
-213.234337353351));
#196432=CARTESIAN_POINT('Ctrl Pts',(-62.0305005605521,-8.35550200411735,
-215.889599207275));
#196433=CARTESIAN_POINT('Ctrl Pts',(-62.8797494596239,-8.66511992948451,
-214.690862545141));
#196434=CARTESIAN_POINT('Ctrl Pts',(-62.9065017229464,-9.03975023999172,
-213.237248654769));
#196435=CARTESIAN_POINT('Ctrl Pts',(-62.0318845638498,-8.4220835950757,
-215.904542950278));
#196436=CARTESIAN_POINT('Ctrl Pts',(-62.8797441930548,-8.72727623804196,
-214.705372782964));
#196437=CARTESIAN_POINT('Ctrl Pts',(-62.9064567562113,-9.0964299581106,
-213.251744484892));
#196438=CARTESIAN_POINT('Ctrl Pts',(-62.0329696818077,-8.47540598081262,
-215.916305535754));
#196439=CARTESIAN_POINT('Ctrl Pts',(-62.8797400235165,-8.77705017731475,
-214.716791984103));
#196440=CARTESIAN_POINT('Ctrl Pts',(-62.906421426558,-9.14181326257087,
-213.263146980914));
#196441=CARTESIAN_POINT('Ctrl Pts',(-62.0425339213031,-8.95581758539506,
-216.020424374309));
#196442=CARTESIAN_POINT('Ctrl Pts',(-62.8797029458838,-9.22525437208547,
-214.817805862891));
#196443=CARTESIAN_POINT('Ctrl Pts',(-62.9061093426684,-9.55062130297945,
-213.364009501424));
#196444=CARTESIAN_POINT('Ctrl Pts',(-62.0495923408927,-9.38642678550509,
-216.100559216461));
#196445=CARTESIAN_POINT('Ctrl Pts',(-62.8796731221476,-9.62683004577358,
-214.895428417083));
#196446=CARTESIAN_POINT('Ctrl Pts',(-62.9058739446102,-9.91655549914845,
-213.44114324688));
#196447=CARTESIAN_POINT('Ctrl Pts',(-62.0605543158907,-10.2546820187393,
-216.234694113546));
#196448=CARTESIAN_POINT('Ctrl Pts',(-62.8796223280864,-10.4359064752367,
-215.024917585528));
#196449=CARTESIAN_POINT('Ctrl Pts',(-62.9054945382152,-10.6537874440521,
-213.569065352509));
#196450=CARTESIAN_POINT('Ctrl Pts',(-62.0644591054324,-10.6938948125732,
-216.288789203932));
#196451=CARTESIAN_POINT('Ctrl Pts',(-62.8796013738763,-10.8450105623093,
-215.076911105874));
#196452=CARTESIAN_POINT('Ctrl Pts',(-62.905350423994,-11.0264379343114,
-213.619939162974));
#196453=CARTESIAN_POINT('Ctrl Pts',(-62.0688689645132,-11.5686947372008,
-216.368854953593));
#196454=CARTESIAN_POINT('Ctrl Pts',(-62.8795684212377,-11.6595117932001,
-215.153252185298));
#196455=CARTESIAN_POINT('Ctrl Pts',(-62.9051593336146,-11.7684901551169,
-213.693446645343));
#196456=CARTESIAN_POINT('Ctrl Pts',(-62.069391577455,-12.004576298268,-216.394995859349));
#196457=CARTESIAN_POINT('Ctrl Pts',(-62.8795563368116,-12.0653505367772,
-215.177787425828));
#196458=CARTESIAN_POINT('Ctrl Pts',(-62.9051117861205,-12.1381923296176,
-213.716251957739));
#196459=CARTESIAN_POINT('Ctrl Pts',(-62.0660431402244,-13.3071722247956,
-216.432951006704));
#196460=CARTESIAN_POINT('Ctrl Pts',(-62.8795272203036,-13.2782401253067,
-215.211670172273));
#196461=CARTESIAN_POINT('Ctrl Pts',(-62.9051036527997,-13.243445563085,
-213.744071341037));
#196462=CARTESIAN_POINT('Ctrl Pts',(-62.0572284163516,-14.1686539550577,
-216.404224735683));
#196463=CARTESIAN_POINT('Ctrl Pts',(-62.8795183650933,-14.0812399938794,
-215.181181755551));
#196464=CARTESIAN_POINT('Ctrl Pts',(-62.9052789204624,-13.9751373806058,
-213.708426173576));
#196465=CARTESIAN_POINT('Ctrl Pts',(-62.0352390706104,-15.4484326336701,
-216.286430648765));
#196466=CARTESIAN_POINT('Ctrl Pts',(-62.8794726572187,-15.2751677276984,
-215.062361671888));
#196467=CARTESIAN_POINT('Ctrl Pts',(-62.9057445940404,-15.0655774299771,
-213.580180828239));
#196468=CARTESIAN_POINT('Ctrl Pts',(-62.0264514220739,-15.8729863495462,
-216.234737322802));
#196469=CARTESIAN_POINT('Ctrl Pts',(-62.8794515889032,-15.6718235071092,
-215.010536635359));
#196470=CARTESIAN_POINT('Ctrl Pts',(-62.9059331942183,-15.4278764578916,
-213.524990067771));
#196471=CARTESIAN_POINT('Ctrl Pts',(-62.0112934704005,-16.5064765229115,
-216.139470449859));
#196472=CARTESIAN_POINT('Ctrl Pts',(-62.8794032606368,-16.2642082032074,
-214.915478455953));
#196473=CARTESIAN_POINT('Ctrl Pts',(-62.9062547760745,-15.9696430762714,
-213.424484058152));
#196474=CARTESIAN_POINT('Ctrl Pts',(-62.0059085609425,-16.7171041054341,
-216.104763566933));
#196475=CARTESIAN_POINT('Ctrl Pts',(-62.879384268395,-16.4613492368974,
-214.880888370633));
#196476=CARTESIAN_POINT('Ctrl Pts',(-62.9063683773708,-16.1499518187337,
-213.38803074649));
#196477=CARTESIAN_POINT('Ctrl Pts',(-61.9973599442118,-17.0322203070265,
-216.048392932234));
#196478=CARTESIAN_POINT('Ctrl Pts',(-62.8793503960171,-16.7564347142257,
-214.824791986014));
#196479=CARTESIAN_POINT('Ctrl Pts',(-62.9065468872613,-16.4200061599841,
-213.329044171076));
#196480=CARTESIAN_POINT('Ctrl Pts',(-61.9944321038605,-17.1371201989063,
-216.028884375262));
#196481=CARTESIAN_POINT('Ctrl Pts',(-62.8793382060926,-16.8547164489359,
-214.805385954228));
#196482=CARTESIAN_POINT('Ctrl Pts',(-62.9066077402092,-16.5099561526457,
-213.308664291015));
#196483=CARTESIAN_POINT('Ctrl Pts',(-61.9899270123872,-17.2942564226434,
-215.998559354035));
#196484=CARTESIAN_POINT('Ctrl Pts',(-62.8793184382364,-17.0019805803341,
-214.775238880667));
#196485=CARTESIAN_POINT('Ctrl Pts',(-62.9067008407091,-16.644780457911,
-213.277033722408));
#196486=CARTESIAN_POINT('Ctrl Pts',(-61.9884064283002,-17.3465995634399,
-215.98827398914));
#196487=CARTESIAN_POINT('Ctrl Pts',(-62.8793116007265,-17.0510484368828,
-214.765015498814));
#196488=CARTESIAN_POINT('Ctrl Pts',(-62.9067321776173,-16.6897051128861,
-213.266313413053));
#196489=CARTESIAN_POINT('Ctrl Pts',(-61.9860977496528,-17.4250602397112,
-215.972582374709));
#196490=CARTESIAN_POINT('Ctrl Pts',(-62.8793009553668,-17.1246105011707,
-214.749422813232));
#196491=CARTESIAN_POINT('Ctrl Pts',(-62.9067796117351,-16.7570671165656,
-213.249969786042));
#196492=CARTESIAN_POINT('Ctrl Pts',(-61.9853235564599,-17.4512047924259,
-215.967307909158));
#196493=CARTESIAN_POINT('Ctrl Pts',(-62.8792973418093,-17.1491261237452,
-214.744181975806));
#196494=CARTESIAN_POINT('Ctrl Pts',(-62.9067954945617,-16.7795169546794,
-213.244478050128));
#196495=CARTESIAN_POINT('Ctrl Pts',(-61.9841553829125,-17.4904080355635,
-215.959330569069));
#196496=CARTESIAN_POINT('Ctrl Pts',(-62.8792918218644,-17.1858896145504,
-214.736256555115));
#196497=CARTESIAN_POINT('Ctrl Pts',(-62.9068194226298,-16.8131854913724,
-213.236174910655));
#196498=CARTESIAN_POINT('Ctrl Pts',(-61.9837648444543,-17.5034735188566,
-215.956660515446));
#196499=CARTESIAN_POINT('Ctrl Pts',(-62.8792899652221,-17.1981428428804,
-214.733603968975));
#196500=CARTESIAN_POINT('Ctrl Pts',(-62.9068274159574,-16.8244073001866,
-213.233396274889));
#196501=CARTESIAN_POINT('Ctrl Pts',(-61.9829814841363,-17.5295999440097,
-215.951298569524));
#196502=CARTESIAN_POINT('Ctrl Pts',(-62.8792862182922,-17.2226462406558,
-214.728277392464));
#196503=CARTESIAN_POINT('Ctrl Pts',(-62.9068434366578,-16.8468488483916,
-213.227817200875));
#196504=CARTESIAN_POINT('Ctrl Pts',(-61.9837428929013,-17.5368644595024,
-215.948389601018));
#196505=CARTESIAN_POINT('Ctrl Pts',(-62.8793014620505,-17.231672318972,
-214.725294222846));
#196506=CARTESIAN_POINT('Ctrl Pts',(-62.9068512246001,-16.8580698646293,
-213.225030214802));
#196507=CARTESIAN_POINT('Ctrl Pts',(-62.0181703622904,-18.7944029448088,
-215.587225509336));
#196508=CARTESIAN_POINT('Ctrl Pts',(-62.880264860769,-18.5719548213566,
-214.360359994756));
#196509=CARTESIAN_POINT('Ctrl Pts',(-62.9078064251384,-18.3057228153494,
-212.867003491606));
#196510=CARTESIAN_POINT('Ctrl Pts',(-62.0423858502321,-20.0566437152891,
-215.359087336711));
#196511=CARTESIAN_POINT('Ctrl Pts',(-62.8762911738208,-19.9202073218907,
-214.133506617223));
#196512=CARTESIAN_POINT('Ctrl Pts',(-62.9033129898347,-19.7553919607571,
-212.653495577744));
#196513=CARTESIAN_POINT('Ctrl Pts',(-62.0716387653447,-22.571278684854,
-215.180930588057));
#196514=CARTESIAN_POINT('Ctrl Pts',(-62.8581514858358,-22.6113837391411,
-213.972570780553));
#196515=CARTESIAN_POINT('Ctrl Pts',(-62.8830851680151,-22.6547081034196,
-212.52986856343));
#196516=CARTESIAN_POINT('Ctrl Pts',(-62.0768709559833,-23.8284596089826,
-215.229198343105));
#196517=CARTESIAN_POINT('Ctrl Pts',(-62.8440002381499,-23.960868557364,
-214.035847577147));
#196518=CARTESIAN_POINT('Ctrl Pts',(-62.8673563795348,-24.1094370634132,
-212.617838162856));
#196519=CARTESIAN_POINT('Ctrl Pts',(-62.0687933625429,-25.3808544123227,
-215.497967942811));
#196520=CARTESIAN_POINT('Ctrl Pts',(-62.8194037351821,-25.6376387826187,
-214.336265031285));
#196521=CARTESIAN_POINT('Ctrl Pts',(-62.8399085993614,-25.9282456355465,
-212.959941102891));
#196522=CARTESIAN_POINT('Ctrl Pts',(-62.0664266960169,-25.6901805447464,
-215.562269443776));
#196523=CARTESIAN_POINT('Ctrl Pts',(-62.8141424132872,-25.9721673633214,
-214.407507976939));
#196524=CARTESIAN_POINT('Ctrl Pts',(-62.8340297350373,-26.2918276350188,
-213.04012465042));
#196525=CARTESIAN_POINT('Ctrl Pts',(-62.0624202311128,-26.0751062786157,
-215.656867415151));
#196526=CARTESIAN_POINT('Ctrl Pts',(-62.8071202348902,-26.3892914434607,
-214.511710407704));
#196527=CARTESIAN_POINT('Ctrl Pts',(-62.8261731592035,-26.7460613321195,
-213.156334850816));
#196528=CARTESIAN_POINT('Ctrl Pts',(-62.0615663934927,-26.1520046023118,
-215.676499151611));
#196529=CARTESIAN_POINT('Ctrl Pts',(-62.8056936212433,-26.4726579103633,
-214.533307712649));
#196530=CARTESIAN_POINT('Ctrl Pts',(-62.8245764208426,-26.8368958608041,
-213.180377302496));
#196531=CARTESIAN_POINT('Ctrl Pts',(-62.0604313366008,-26.2480138120354,
-215.701948095613));
#196532=CARTESIAN_POINT('Ctrl Pts',(-62.8038822013363,-26.5767984556868,
-214.561274047172));
#196533=CARTESIAN_POINT('Ctrl Pts',(-62.822548322552,-26.9504234038111,
-213.211454506226));
#196534=CARTESIAN_POINT('Ctrl Pts',(-62.0602009365971,-26.2672099682503,
-215.707083353122));
#196535=CARTESIAN_POINT('Ctrl Pts',(-62.8035185165143,-26.5976227967682,
-214.566915697153));
#196536=CARTESIAN_POINT('Ctrl Pts',(-62.8221410940186,-26.9731281314353,
-213.217721160276));
#196537=CARTESIAN_POINT('Ctrl Pts',(-62.0598502125763,-26.2959955735649,
-215.714854815994));
#196538=CARTESIAN_POINT('Ctrl Pts',(-62.8029708726847,-26.6288541544021,
-214.575451318361));
#196539=CARTESIAN_POINT('Ctrl Pts',(-62.8215278301374,-27.0071840444203,
-213.227198424034));
#196540=CARTESIAN_POINT('Ctrl Pts',(-62.0597324505761,-26.3055893371753,
-215.717456733094));
#196541=CARTESIAN_POINT('Ctrl Pts',(-62.8027879726431,-26.6392637102074,
-214.578308705998));
#196542=CARTESIAN_POINT('Ctrl Pts',(-62.8213230053295,-27.0185358190149,
-213.230370392442));
#196543=CARTESIAN_POINT('Ctrl Pts',(-62.0595545213414,-26.3199778126609,
-215.721376800301));
#196544=CARTESIAN_POINT('Ctrl Pts',(-62.8025130927215,-26.6548767478047,
-214.582613127237));
#196545=CARTESIAN_POINT('Ctrl Pts',(-62.8210151618606,-27.0355631854271,
-213.235147724465));
#196546=CARTESIAN_POINT('Ctrl Pts',(-62.0594949972346,-26.3247736095024,
-215.722686354616));
#196547=CARTESIAN_POINT('Ctrl Pts',(-62.8024213779408,-26.6600808682157,
-214.584050988303));
#196548=CARTESIAN_POINT('Ctrl Pts',(-62.8209124463284,-27.0412389249773,
-213.236743398352));
#196549=CARTESIAN_POINT('Ctrl Pts',(-62.0593755193932,-26.3343644777571,
-215.725311201717));
#196550=CARTESIAN_POINT('Ctrl Pts',(-62.8022377717518,-26.6704886693638,
-214.586932830867));
#196551=CARTESIAN_POINT('Ctrl Pts',(-62.8207068130132,-27.052590305443,
-213.239941215787));
#196552=CARTESIAN_POINT('Ctrl Pts',(-62.0591904267342,-26.3423678600797,
-215.727641643505));
#196553=CARTESIAN_POINT('Ctrl Pts',(-62.8021133629123,-26.6774201434905,
-214.588932611784));
#196554=CARTESIAN_POINT('Ctrl Pts',(-62.8206039569716,-27.0582660000666,
-213.241539781896));
#196555=CARTESIAN_POINT('Ctrl Pts',(-62.0579195947297,-26.4041206938665,
-215.745297553372));
#196556=CARTESIAN_POINT('Ctrl Pts',(-62.8010984184952,-26.7342691805765,
-214.605084908191));
#196557=CARTESIAN_POINT('Ctrl Pts',(-62.8196787974583,-27.1093480735134,
-213.255871682944));
#196558=CARTESIAN_POINT('Ctrl Pts',(-62.0567567001996,-26.4589929636436,
-215.760704173281));
#196559=CARTESIAN_POINT('Ctrl Pts',(-62.8001976805287,-26.7847921675662,
-214.619163948744));
#196560=CARTESIAN_POINT('Ctrl Pts',(-62.8188583609005,-27.154758511644,
-213.268331481196));
#196561=CARTESIAN_POINT('Ctrl Pts',(-62.0507778370158,-26.7332616168239,
-215.836316781018));
#196562=CARTESIAN_POINT('Ctrl Pts',(-62.7957006936856,-27.0373714949889,
-214.688185492659));
#196563=CARTESIAN_POINT('Ctrl Pts',(-62.8147655328416,-27.3818312159389,
-213.329248041551));
#196564=CARTESIAN_POINT('Ctrl Pts',(-62.0454689865543,-26.952380588705,
-215.892263197796));
#196565=CARTESIAN_POINT('Ctrl Pts',(-62.7921249336556,-27.2392985917041,
-214.739001463284));
#196566=CARTESIAN_POINT('Ctrl Pts',(-62.811521179222,-27.5635550010564,
-213.373559009004));
#196567=CARTESIAN_POINT('Ctrl Pts',(-62.0164077141018,-28.0466591076513,
-216.150292769558));
#196568=CARTESIAN_POINT('Ctrl Pts',(-62.7743327848849,-28.2486351141899,
-214.972122127568));
#196569=CARTESIAN_POINT('Ctrl Pts',(-62.7954319749737,-28.4724876729194,
-213.573958234288));
#196570=CARTESIAN_POINT('Ctrl Pts',(-61.9849863797742,-28.9185203866592,
-216.287393756369));
#196571=CARTESIAN_POINT('Ctrl Pts',(-62.7603778330476,-29.0550555751074,
-215.09135055822));
#196572=CARTESIAN_POINT('Ctrl Pts',(-62.7829855880221,-29.2006385623869,
-213.666528824391));
#196573=CARTESIAN_POINT('Ctrl Pts',(-61.8719372658986,-31.5146432828636,
-216.52155335041));
#196574=CARTESIAN_POINT('Ctrl Pts',(-62.7188819350269,-31.4677732499339,
-215.279252210143));
#196575=CARTESIAN_POINT('Ctrl Pts',(-62.7463293349613,-31.3876040978064,
-213.774365476491));
#196576=CARTESIAN_POINT('Ctrl Pts',(-61.7714592397433,-33.2214602041654,
-216.443548517691));
#196577=CARTESIAN_POINT('Ctrl Pts',(-62.6916591462751,-33.0686179338109,
-215.178100628118));
#196578=CARTESIAN_POINT('Ctrl Pts',(-62.7227759583433,-32.8489094530129,
-213.621230861645));
#196579=CARTESIAN_POINT('Ctrl Pts',(-61.6527757155717,-35.0048119699771,
-216.189409048519));
#196580=CARTESIAN_POINT('Ctrl Pts',(-62.6622409902955,-34.7480221415653,
-214.910242320336));
#196581=CARTESIAN_POINT('Ctrl Pts',(-62.6973153894391,-34.4039131251359,
-213.29729287427));
#196582=CARTESIAN_POINT('Ctrl Pts',(-61.6457452969654,-35.1096181707137,
-216.173825932635));
#196583=CARTESIAN_POINT('Ctrl Pts',(-62.660500652564,-34.8471952613371,
-214.89381401442));
#196584=CARTESIAN_POINT('Ctrl Pts',(-62.6958162562244,-34.4953927542598,
-213.277636702578));
#196585=CARTESIAN_POINT('Ctrl Pts',(-61.6368972733854,-35.2405100086795,
-216.153573540134));
#196586=CARTESIAN_POINT('Ctrl Pts',(-62.6583222139731,-34.9710950849282,
-214.872545527579));
#196587=CARTESIAN_POINT('Ctrl Pts',(-62.6939402205331,-34.6097530635753,
-213.252332432694));
#196588=CARTESIAN_POINT('Ctrl Pts',(-61.6351246682154,-35.2666825779689,
-216.149484383413));
#196589=CARTESIAN_POINT('Ctrl Pts',(-62.6578862571906,-34.9958784408532,
-214.868253991386));
#196590=CARTESIAN_POINT('Ctrl Pts',(-62.693564907493,-34.632625664116,-213.247234872735));
#196591=CARTESIAN_POINT('Ctrl Pts',(-61.6324612821853,-35.3059328288065,
-216.143292970413));
#196592=CARTESIAN_POINT('Ctrl Pts',(-62.6572320773096,-35.0330492303192,
-214.86176188503));
#196593=CARTESIAN_POINT('Ctrl Pts',(-62.6930017735533,-34.6669353682907,
-213.23953378686));
#196594=CARTESIAN_POINT('Ctrl Pts',(-61.6315727404868,-35.3190148116817,
-216.141219553062));
#196595=CARTESIAN_POINT('Ctrl Pts',(-62.6570139646951,-35.0454394602782,
-214.859588596064));
#196596=CARTESIAN_POINT('Ctrl Pts',(-62.6928140348453,-34.6783720702307,
-213.236957633838));
#196597=CARTESIAN_POINT('Ctrl Pts',(-61.6297941680007,-35.3451759247511,
-216.13705354844));
#196598=CARTESIAN_POINT('Ctrl Pts',(-62.6565776489529,-35.0702189633633,
-214.855223724628));
#196599=CARTESIAN_POINT('Ctrl Pts',(-62.6924385017243,-34.701245741126,
-213.231787130788));
#196600=CARTESIAN_POINT('Ctrl Pts',(-61.6310293684106,-35.3530107643184,
-216.133482239242));
#196601=CARTESIAN_POINT('Ctrl Pts',(-62.6564417977456,-35.0795905313491,
-214.851837785791));
#196602=CARTESIAN_POINT('Ctrl Pts',(-62.6922505031027,-34.712682531357,
-213.229204685838));
#196603=CARTESIAN_POINT('Ctrl Pts',(-61.6325094322944,-35.4037694797289,
-216.118959911289));
#196604=CARTESIAN_POINT('Ctrl Pts',(-62.6555787703405,-35.1331120907873,
-214.837616627857));
#196605=CARTESIAN_POINT('Ctrl Pts',(-62.6913088110132,-34.7698657850322,
-213.216337901175));
#196606=CARTESIAN_POINT('Ctrl Pts',(-61.6336864900504,-35.4443701357922,
-216.107444248921));
#196607=CARTESIAN_POINT('Ctrl Pts',(-62.6548838887415,-35.1759301641451,
-214.826347135623));
#196608=CARTESIAN_POINT('Ctrl Pts',(-62.6905505732429,-34.8156106395167,
-213.206157663245));
#196609=CARTESIAN_POINT('Ctrl Pts',(-61.639536989153,-35.647340776021,-216.050378480442));
#196610=CARTESIAN_POINT('Ctrl Pts',(-62.6513884920124,-35.3899422289628,
-214.770560243673));
#196611=CARTESIAN_POINT('Ctrl Pts',(-62.6867349314889,-35.0443261389348,
-213.155824498556));
#196612=CARTESIAN_POINT('Ctrl Pts',(-61.6441060885591,-35.8096128160609,
-216.006365733016));
#196613=CARTESIAN_POINT('Ctrl Pts',(-62.6485208043159,-35.5611635627003,
-214.727654113872));
#196614=CARTESIAN_POINT('Ctrl Pts',(-62.6836041752041,-35.227270469846,
-213.117375270572));
#196615=CARTESIAN_POINT('Ctrl Pts',(-61.6574855827294,-36.2960730265464,
-215.879313463721));
#196616=CARTESIAN_POINT('Ctrl Pts',(-62.6397088692154,-36.0744688616432,
-214.604282321189));
#196617=CARTESIAN_POINT('Ctrl Pts',(-62.6739757829555,-35.7760179301451,
-213.007568080921));
#196618=CARTESIAN_POINT('Ctrl Pts',(-61.6659645557888,-36.619740284584,
-215.801290160767));
#196619=CARTESIAN_POINT('Ctrl Pts',(-62.6335526368642,-36.4164413462367,
-214.529072745108));
#196620=CARTESIAN_POINT('Ctrl Pts',(-62.6672458339371,-36.1415480006374,
-212.941772621246));
#196621=CARTESIAN_POINT('Ctrl Pts',(-61.6901615834725,-37.590390336358,
-215.587521646834));
#196622=CARTESIAN_POINT('Ctrl Pts',(-62.6142130892345,-37.4422426685059,
-214.325282532427));
#196623=CARTESIAN_POINT('Ctrl Pts',(-62.6460655421939,-37.2394079985843,
-212.767180740501));
#196624=CARTESIAN_POINT('Ctrl Pts',(-61.7046609397659,-38.2370900188355,
-215.471974562704));
#196625=CARTESIAN_POINT('Ctrl Pts',(-62.6001319557833,-38.1277065556804,
-214.21795893023));
#196626=CARTESIAN_POINT('Ctrl Pts',(-62.6306238454685,-37.9731020338337,
-212.681065126222));
#196627=CARTESIAN_POINT('Ctrl Pts',(-61.7302717981392,-39.5279866016878,
-215.301479571241));
#196628=CARTESIAN_POINT('Ctrl Pts',(-62.5694775958684,-39.4998723159367,
-214.068577411316));
#196629=CARTESIAN_POINT('Ctrl Pts',(-62.5969132094274,-39.4445711917008,
-212.57789537765));
#196630=CARTESIAN_POINT('Ctrl Pts',(-61.7413754773038,-40.1722445347539,
-215.246464457873));
#196631=CARTESIAN_POINT('Ctrl Pts',(-62.5529100079014,-40.1867078641608,
-214.026226040623));
#196632=CARTESIAN_POINT('Ctrl Pts',(-62.5786465561158,-40.1823394734508,
-212.560726431139));
#196633=CARTESIAN_POINT('Ctrl Pts',(-61.7551693704691,-41.1348830401125,
-215.217380280251));
#196634=CARTESIAN_POINT('Ctrl Pts',(-62.5260264335553,-41.2178782666483,
-214.020805002663));
#196635=CARTESIAN_POINT('Ctrl Pts',(-62.5489095967685,-41.2926666211446,
-212.597076537354));
#196636=CARTESIAN_POINT('Ctrl Pts',(-61.7592997587092,-41.4560741015586,
-215.216683316051));
#196637=CARTESIAN_POINT('Ctrl Pts',(-62.5167061217927,-41.5624453099376,
-214.028776153341));
#196638=CARTESIAN_POINT('Ctrl Pts',(-62.538573302366,-41.664507942645,-212.619734584269));
#196639=CARTESIAN_POINT('Ctrl Pts',(-61.7663955397543,-42.090104539572,
-215.23491686589));
#196640=CARTESIAN_POINT('Ctrl Pts',(-62.4975638186773,-42.2442869424654,
-214.06597330712));
#196641=CARTESIAN_POINT('Ctrl Pts',(-62.5172963966413,-42.4017436060914,
-212.687617475151));
#196642=CARTESIAN_POINT('Ctrl Pts',(-61.7693696651392,-42.4032937510997,
-215.253774289279));
#196643=CARTESIAN_POINT('Ctrl Pts',(-62.4877344671727,-42.5819624883669,
-214.095102448274));
#196644=CARTESIAN_POINT('Ctrl Pts',(-62.5063477838443,-42.7675314704734,
-212.732780967688));
#196645=CARTESIAN_POINT('Ctrl Pts',(-61.776403466414,-43.3300284309475,
-215.341514528131));
#196646=CARTESIAN_POINT('Ctrl Pts',(-62.4575092043709,-43.5834625000428,
-214.216422194191));
#196647=CARTESIAN_POINT('Ctrl Pts',(-62.4725701813145,-43.8557232524164,
-212.904651540624));
#196648=CARTESIAN_POINT('Ctrl Pts',(-61.7786393212107,-43.9308451169452,
-215.441224005761));
#196649=CARTESIAN_POINT('Ctrl Pts',(-62.4363373124719,-44.2373732157453,
-214.342183062308));
#196650=CARTESIAN_POINT('Ctrl Pts',(-62.4488123543693,-44.5690597591983,
-213.067323574879));
#196651=CARTESIAN_POINT('Ctrl Pts',(-61.7768758323447,-44.799108393107,
-215.66489855191));
#196652=CARTESIAN_POINT('Ctrl Pts',(-62.4031169014029,-45.1908126884628,
-214.61302309293));
#196653=CARTESIAN_POINT('Ctrl Pts',(-62.4112691380312,-45.6166733720198,
-213.400195879714));
#196654=CARTESIAN_POINT('Ctrl Pts',(-61.7754229930674,-45.0830122299898,
-215.75187598791));
#196655=CARTESIAN_POINT('Ctrl Pts',(-62.391806053278,-45.5038767861212,
-214.716988414011));
#196656=CARTESIAN_POINT('Ctrl Pts',(-62.3984364151395,-45.9621252239228,
-213.526046844411));
#196657=CARTESIAN_POINT('Ctrl Pts',(-61.7703563686195,-45.6378757088274,
-215.953838120193));
#196658=CARTESIAN_POINT('Ctrl Pts',(-62.368710967822,-46.1191184830862,
-214.956162974242));
#196659=CARTESIAN_POINT('Ctrl Pts',(-62.3721154800584,-46.6444314431026,
-213.811880088338));
#196660=CARTESIAN_POINT('Ctrl Pts',(-61.766714425071,-45.9100219139299,
-216.069514739708));
#196661=CARTESIAN_POINT('Ctrl Pts',(-62.3568675933792,-46.4227073678569,
-215.092174735303));
#196662=CARTESIAN_POINT('Ctrl Pts',(-62.3585615338666,-46.9827912699289,
-213.972791370408));
#196663=CARTESIAN_POINT('Ctrl Pts',(-61.7617700838064,-46.1695632659449,
-216.198756570055));
#196664=CARTESIAN_POINT('Ctrl Pts',(-62.3450157861073,-46.7143916405499,
-215.243383403778));
#196665=CARTESIAN_POINT('Ctrl Pts',(-62.3449264240553,-47.3099624311764,
-214.150201433913));
#196666=CARTESIAN_POINT('',(-61.7131389055822,20.0389433648605,-216.160156268336));
#196667=CARTESIAN_POINT('',(-62.3650443003751,20.9007294710183,-213.866597158632));
#196668=CARTESIAN_POINT('Ctrl Pts',(-61.7131389055822,20.0389433648605,
-216.160156268336));
#196669=CARTESIAN_POINT('Ctrl Pts',(-61.7678693862137,20.0751773182081,
-216.070351472292));
#196670=CARTESIAN_POINT('Ctrl Pts',(-61.8190760855121,20.1115905721978,
-215.979264091882));
#196671=CARTESIAN_POINT('Ctrl Pts',(-61.8668444683366,20.1481502791898,
-215.886955305269));
#196672=CARTESIAN_POINT('Ctrl Pts',(-61.9150658374495,20.1850566808991,
-215.793771156917));
#196673=CARTESIAN_POINT('Ctrl Pts',(-61.9597841805652,20.2221126942381,
-215.699341685683));
#196674=CARTESIAN_POINT('Ctrl Pts',(-62.0010568508086,20.2593031022775,
-215.603689573791));
#196675=CARTESIAN_POINT('Ctrl Pts',(-62.0425779998727,20.2967174122036,
-215.507461595986));
#196676=CARTESIAN_POINT('Ctrl Pts',(-62.0806125017358,20.3342681742483,
-215.409995389685));
#196677=CARTESIAN_POINT('Ctrl Pts',(-62.1151769896773,20.3719525091287,
-215.311284621693));
#196678=CARTESIAN_POINT('Ctrl Pts',(-62.1441447947059,20.4035349953873,
-215.228557104182));
#196679=CARTESIAN_POINT('Ctrl Pts',(-62.1706747072058,20.4352116636552,
-215.144954624778));
#196680=CARTESIAN_POINT('Ctrl Pts',(-62.1947499260075,20.4669841010193,
-215.060464474434));
#196681=CARTESIAN_POINT('Ctrl Pts',(-62.222160692488,20.5031585120715,-214.964268473059));
#196682=CARTESIAN_POINT('Ctrl Pts',(-62.2464217468638,20.5395075487633,
-214.866780056301));
#196683=CARTESIAN_POINT('Ctrl Pts',(-62.2673852527365,20.5758942372261,
-214.768340219344));
#196684=CARTESIAN_POINT('Ctrl Pts',(-62.2876551758303,20.611077063098,-214.673157288751));
#196685=CARTESIAN_POINT('Ctrl Pts',(-62.3048421853943,20.646294816521,-214.57708549284));
#196686=CARTESIAN_POINT('Ctrl Pts',(-62.3188618795333,20.6814237204261,
-214.480452073967));
#196687=CARTESIAN_POINT('Ctrl Pts',(-62.3336011485597,20.7183556506185,
-214.378858847781));
#196688=CARTESIAN_POINT('Ctrl Pts',(-62.3448390172506,20.7551890290087,
-214.276645420069));
#196689=CARTESIAN_POINT('Ctrl Pts',(-62.3525380749027,20.7917848562111,
-214.174204593435));
#196690=CARTESIAN_POINT('Ctrl Pts',(-62.3602371325547,20.8283806834136,
-214.071763766801));
#196691=CARTESIAN_POINT('Ctrl Pts',(-62.3643974261569,20.8647386489197,
-213.969096262343));
#196692=CARTESIAN_POINT('Ctrl Pts',(-62.3650443003751,20.9007294710183,
-213.866597158632));
#196693=CARTESIAN_POINT('',(-61.6795259610279,9.54487883260503,-216.064115826141));
#196694=CARTESIAN_POINT('Ctrl Pts',(-61.7131389055531,20.0389433648412,
-216.160156268384));
#196695=CARTESIAN_POINT('Ctrl Pts',(-61.7230421999514,19.657421912819,-215.99031134923));
#196696=CARTESIAN_POINT('Ctrl Pts',(-61.7309654538443,19.2561357591709,
-215.843887564221));
#196697=CARTESIAN_POINT('Ctrl Pts',(-61.7371187378078,18.8464365470887,
-215.722479103759));
#196698=CARTESIAN_POINT('Ctrl Pts',(-61.7377497043543,18.8044254033654,
-215.710029706418));
#196699=CARTESIAN_POINT('Ctrl Pts',(-61.7383620608911,18.7623257911141,
-215.697843334498));
#196700=CARTESIAN_POINT('Ctrl Pts',(-61.7389560341596,18.7201499473734,
-215.685921705516));
#196701=CARTESIAN_POINT('Ctrl Pts',(-61.7468389712057,18.1604117593227,
-215.527703388753));
#196702=CARTESIAN_POINT('Ctrl Pts',(-61.7516168666685,17.5843608729145,
-215.413777537614));
#196703=CARTESIAN_POINT('Ctrl Pts',(-61.7539978140095,16.9953644593714,
-215.337979225164));
#196704=CARTESIAN_POINT('Ctrl Pts',(-61.7563787613503,16.4063680458282,
-215.262180912713));
#196705=CARTESIAN_POINT('Ctrl Pts',(-61.7563293945832,15.8044782872716,
-215.224636336423));
#196706=CARTESIAN_POINT('Ctrl Pts',(-61.7541448402693,15.1919610915637,
-215.221849976965));
#196707=CARTESIAN_POINT('Ctrl Pts',(-61.7519602859553,14.5794438958557,
-215.219063617507));
#196708=CARTESIAN_POINT('Ctrl Pts',(-61.7476795068394,13.965046025957,-215.251046967269));
#196709=CARTESIAN_POINT('Ctrl Pts',(-61.741516620175,13.350930867722,-215.313231000222));
#196710=CARTESIAN_POINT('Ctrl Pts',(-61.7332980686954,12.5319742135963,
-215.396156860111));
#196711=CARTESIAN_POINT('Ctrl Pts',(-61.7217826330292,11.7125302862904,
-215.532443369588));
#196712=CARTESIAN_POINT('Ctrl Pts',(-61.7069868899011,10.8949681526562,
-215.716652557842));
#196713=CARTESIAN_POINT('Ctrl Pts',(-61.700872312975,10.557097556047,-215.792779944099));
#196714=CARTESIAN_POINT('Ctrl Pts',(-61.6941974964507,10.2195483491066,
-215.877091985145));
#196715=CARTESIAN_POINT('Ctrl Pts',(-61.6869636101976,9.88248774578141,
-215.969204864317));
#196716=CARTESIAN_POINT('Ctrl Pts',(-61.6857579624888,9.82631097856056,
-215.984557010846));
#196717=CARTESIAN_POINT('Ctrl Pts',(-61.6845367850159,9.77014778356728,
-216.000125847253));
#196718=CARTESIAN_POINT('Ctrl Pts',(-61.6833001414503,9.71399890071897,
-216.015909525897));
#196719=CARTESIAN_POINT('Ctrl Pts',(-61.6829840313086,9.69964615445876,
-216.019944141069));
#196720=CARTESIAN_POINT('Ctrl Pts',(-61.6826668840306,9.68529435909321,
-216.023992826748));
#196721=CARTESIAN_POINT('Ctrl Pts',(-61.6823487176854,9.67094351669723,
-216.028055531282));
#196722=CARTESIAN_POINT('Ctrl Pts',(-61.6820445402464,9.65722364168979,
-216.031939609782));
#196723=CARTESIAN_POINT('Ctrl Pts',(-61.6817394113119,9.64350470966858,
-216.035836656236));
#196724=CARTESIAN_POINT('Ctrl Pts',(-61.6814333454261,9.62978671861984,
-216.039746637367));
#196725=CARTESIAN_POINT('Ctrl Pts',(-61.6811202416631,9.61575328719779,
-216.043746527138));
#196726=CARTESIAN_POINT('Ctrl Pts',(-61.6808061369332,9.60172085660555,
-216.047759977122));
#196727=CARTESIAN_POINT('Ctrl Pts',(-61.6804910519492,9.58768941584011,
-216.05178694695));
#196728=CARTESIAN_POINT('Ctrl Pts',(-61.6804122807032,9.58418155564876,
-216.052793689406));
#196729=CARTESIAN_POINT('Ctrl Pts',(-61.6803089880787,9.58074834654284,
-216.053815574226));
#196730=CARTESIAN_POINT('Ctrl Pts',(-61.6801992274307,9.57732260329995,
-216.054845098855));
#196731=CARTESIAN_POINT('Ctrl Pts',(-61.6800345864587,9.57218398843562,
-216.056389385797));
#196732=CARTESIAN_POINT('Ctrl Pts',(-61.6798553763802,9.56706216868915,
-216.057950850523));
#196733=CARTESIAN_POINT('Ctrl Pts',(-61.6797228065068,9.56173044678179,
-216.059504376507));
#196734=CARTESIAN_POINT('Ctrl Pts',(-61.6795902366675,9.55639872624344,
-216.061057902091));
#196735=CARTESIAN_POINT('Ctrl Pts',(-61.6795044690351,9.55085713443771,
-216.062603607648));
#196736=CARTESIAN_POINT('Ctrl Pts',(-61.6795253586028,9.54487871892934,
-216.064115384928));
#196737=CARTESIAN_POINT('',(-62.0174913981677,0.438806380665441,-215.788052143479));
#196738=CARTESIAN_POINT('Ctrl Pts',(-61.6795265634691,9.54487894167559,
-216.064116268519));
#196739=CARTESIAN_POINT('Ctrl Pts',(-61.6801741939043,9.52709136950118,
-216.067812212364));
#196740=CARTESIAN_POINT('Ctrl Pts',(-61.6818851148242,9.50527890530528,
-216.07109134272));
#196741=CARTESIAN_POINT('Ctrl Pts',(-61.684571979164,9.46002870807816,-216.078979205164));
#196742=CARTESIAN_POINT('Ctrl Pts',(-61.6860515048732,9.43504846440253,
-216.083296010875));
#196743=CARTESIAN_POINT('Ctrl Pts',(-61.6934328695196,9.31010377869919,
-216.104698272446));
#196744=CARTESIAN_POINT('Ctrl Pts',(-61.6992859244921,9.21000894480459,
-216.121238473637));
#196745=CARTESIAN_POINT('Ctrl Pts',(-61.7166859533339,8.90929364047332,
-216.169076652063));
#196746=CARTESIAN_POINT('Ctrl Pts',(-61.7280739009634,8.7082425179926,-216.198592840276));
#196747=CARTESIAN_POINT('Ctrl Pts',(-61.7615734406237,8.10325300133128,
-216.279690889332));
#196748=CARTESIAN_POINT('Ctrl Pts',(-61.7830227272411,7.69748162474272,
-216.32383427267));
#196749=CARTESIAN_POINT('Ctrl Pts',(-61.8444274680599,6.47182680783556,
-216.423521585247));
#196750=CARTESIAN_POINT('Ctrl Pts',(-61.8810347009149,5.64536351003889,
-216.446767106403));
#196751=CARTESIAN_POINT('Ctrl Pts',(-61.9278975062939,4.38902081980034,
-216.404691459093));
#196752=CARTESIAN_POINT('Ctrl Pts',(-61.9420930876676,3.96799579818035,
-216.377909012764));
#196753=CARTESIAN_POINT('Ctrl Pts',(-61.9674232473587,3.12084236030756,
-216.296743366476));
#196754=CARTESIAN_POINT('Ctrl Pts',(-61.9785671023287,2.6942652956053,-216.242198159345));
#196755=CARTESIAN_POINT('Ctrl Pts',(-61.9973329077485,1.84297899797596,
-216.104606636849));
#196756=CARTESIAN_POINT('Ctrl Pts',(-62.0049832725563,1.41762802329507,
-216.02157900986));
#196757=CARTESIAN_POINT('Ctrl Pts',(-62.0123231790164,0.88617919753532,
-215.899355967453));
#196758=CARTESIAN_POINT('Ctrl Pts',(-62.0136798966164,0.779901155695931,
-215.873988897971));
#196759=CARTESIAN_POINT('Ctrl Pts',(-62.0155466212184,0.620498434716868,
-215.834540688288));
#196760=CARTESIAN_POINT('Ctrl Pts',(-62.0161408021641,0.567366580471024,
-215.821158342626));
#196761=CARTESIAN_POINT('Ctrl Pts',(-62.0168482856434,0.500954373935468,
-215.804137717908));
#196762=CARTESIAN_POINT('Ctrl Pts',(-62.01698802015,0.48767206310896,-215.800718958175));
#196763=CARTESIAN_POINT('Ctrl Pts',(-62.017250081267,0.462443823410336,
-215.794197517145));
#196764=CARTESIAN_POINT('Ctrl Pts',(-62.0173286470213,0.448406688707245,
-215.790652827454));
#196765=CARTESIAN_POINT('Ctrl Pts',(-62.0174913981677,0.438806380665441,
-215.788052143479));
#196766=CARTESIAN_POINT('',(-62.030115892062,-8.32556237289759,-215.882468962491));
#196767=CARTESIAN_POINT('Ctrl Pts',(-62.0174913981677,0.438806380665441,
-215.788052143479));
#196768=CARTESIAN_POINT('Ctrl Pts',(-62.0175184759225,0.437736514029309,
-215.787747559075));
#196769=CARTESIAN_POINT('Ctrl Pts',(-62.0175387248819,0.436718687877101,
-215.787466956657));
#196770=CARTESIAN_POINT('Ctrl Pts',(-62.017989654052,0.416815630977219,
-215.781891478117));
#196771=CARTESIAN_POINT('Ctrl Pts',(-62.0184159156524,0.397860626607022,
-215.776623255365));
#196772=CARTESIAN_POINT('Ctrl Pts',(-62.0222247646125,0.227220244864405,
-215.72957027851));
#196773=CARTESIAN_POINT('Ctrl Pts',(-62.0254149107006,0.075217642154615,
-215.69031199341));
#196774=CARTESIAN_POINT('Ctrl Pts',(-62.052437955369,-1.2954892060821,-215.359502197812));
#196775=CARTESIAN_POINT('Ctrl Pts',(-62.0647635114806,-2.53272084807531,
-215.223247240007));
#196776=CARTESIAN_POINT('Ctrl Pts',(-62.0696277257875,-5.02448450998964,
-215.233701926329));
#196777=CARTESIAN_POINT('Ctrl Pts',(-62.0621262930632,-6.27916951367206,
-215.380652672016));
#196778=CARTESIAN_POINT('Ctrl Pts',(-62.041100054462,-7.69137245107917,
-215.713077377955));
#196779=CARTESIAN_POINT('Ctrl Pts',(-62.0385848503381,-7.84830756476466,
-215.752367984344));
#196780=CARTESIAN_POINT('Ctrl Pts',(-62.0345359973834,-8.08366223386927,
-215.814879358009));
#196781=CARTESIAN_POINT('Ctrl Pts',(-62.0331425236356,-8.16198032978614,
-215.83627908007));
#196782=CARTESIAN_POINT('Ctrl Pts',(-62.031345448701,-8.25970867107241,
-215.863731373079));
#196783=CARTESIAN_POINT('Ctrl Pts',(-62.0309832718629,-8.27924587491217,
-215.869256965251));
#196784=CARTESIAN_POINT('Ctrl Pts',(-62.0304520415348,-8.30767279756168,
-215.87735141746));
#196785=CARTESIAN_POINT('Ctrl Pts',(-62.0299989262911,-8.31437654383897,
-215.879760093338));
#196786=CARTESIAN_POINT('Ctrl Pts',(-62.030115892062,-8.32556237289759,
-215.882468962491));
#196787=CARTESIAN_POINT('',(-61.9835319875972,-17.519732572983,-215.952954107728));
#196788=CARTESIAN_POINT('Ctrl Pts',(-62.030115892062,-8.32556237289759,
-215.882468962491));
#196789=CARTESIAN_POINT('Ctrl Pts',(-62.0301442467716,-8.32665730522469,
-215.882709095953));
#196790=CARTESIAN_POINT('Ctrl Pts',(-62.0301626852208,-8.32778917970396,
-215.882973325792));
#196791=CARTESIAN_POINT('Ctrl Pts',(-62.0304669547665,-8.34227865585374,
-215.886253315709));
#196792=CARTESIAN_POINT('Ctrl Pts',(-62.0307450589222,-8.35559115122019,
-215.88925405955));
#196793=CARTESIAN_POINT('Ctrl Pts',(-62.0321286803914,-8.42217147455135,
-215.904197652088));
#196794=CARTESIAN_POINT('Ctrl Pts',(-62.0332134989248,-8.47549284357947,
-215.915960118575));
#196795=CARTESIAN_POINT('Ctrl Pts',(-62.042775097603,-8.95589521339918,
-216.020077885304));
#196796=CARTESIAN_POINT('Ctrl Pts',(-62.0498315656512,-9.38649607478912,
-216.100211872333));
#196797=CARTESIAN_POINT('Ctrl Pts',(-62.060790505385,-10.2547342820899,
-216.234345225865));
#196798=CARTESIAN_POINT('Ctrl Pts',(-62.0646942119403,-10.6939384019574,
-216.288439637279));
#196799=CARTESIAN_POINT('Ctrl Pts',(-62.0691028446192,-11.5687209395696,
-216.368504230108));
#196800=CARTESIAN_POINT('Ctrl Pts',(-62.0696253097439,-12.0045938332199,
-216.39464466293));
#196801=CARTESIAN_POINT('Ctrl Pts',(-62.0662777878625,-13.3071638786316,
-216.432598698728));
#196802=CARTESIAN_POINT('Ctrl Pts',(-62.0574654920844,-14.1686287502632,
-216.403872085794));
#196803=CARTESIAN_POINT('Ctrl Pts',(-62.0354821865879,-15.4483827335448,
-216.28607811805));
#196804=CARTESIAN_POINT('Ctrl Pts',(-62.0266969469883,-15.8729284420891,
-216.234384919981));
#196805=CARTESIAN_POINT('Ctrl Pts',(-62.0115431415321,-16.5064068392879,
-216.139118393046));
#196806=CARTESIAN_POINT('Ctrl Pts',(-62.0061597028118,-16.7170305638983,
-216.104411645275));
#196807=CARTESIAN_POINT('Ctrl Pts',(-61.9976134180043,-17.0321410420476,
-216.048041250619));
#196808=CARTESIAN_POINT('Ctrl Pts',(-61.994686375636,-17.1370390445088,
-216.028532778314));
#196809=CARTESIAN_POINT('Ctrl Pts',(-61.9901825112225,-17.2941724515911,
-215.998207893143));
#196810=CARTESIAN_POINT('Ctrl Pts',(-61.9886623411118,-17.3465146583208,
-215.987922574716));
#196811=CARTESIAN_POINT('Ctrl Pts',(-61.9863542907869,-17.4249739380202,
-215.972231032217));
#196812=CARTESIAN_POINT('Ctrl Pts',(-61.9851933169768,-17.4641900706523,
-215.964319370264));
#196813=CARTESIAN_POINT('Ctrl Pts',(-61.9840220202716,-17.5033858261321,
-215.956309246507));
#196814=CARTESIAN_POINT('Ctrl Pts',(-61.9835964522753,-17.5175828670638,
-215.953395539067));
#196815=CARTESIAN_POINT('Ctrl Pts',(-61.9835711461698,-17.518673228533,
-215.953161073408));
#196816=CARTESIAN_POINT('Ctrl Pts',(-61.9835319875972,-17.519732572983,
-215.952954107728));
#196817=CARTESIAN_POINT('',(-62.0596235416337,-26.3318125162586,-215.724256795808));
#196818=CARTESIAN_POINT('Ctrl Pts',(-61.9835319875972,-17.519732572983,
-215.952954107728));
#196819=CARTESIAN_POINT('Ctrl Pts',(-61.9833142085583,-17.5339497172701,
-215.949734813099));
#196820=CARTESIAN_POINT('Ctrl Pts',(-61.9841625478236,-17.5427031512807,
-215.946332937118));
#196821=CARTESIAN_POINT('Ctrl Pts',(-61.9866649807491,-17.6342468174392,
-215.92008209154));
#196822=CARTESIAN_POINT('Ctrl Pts',(-61.9912692518142,-17.8060184448602,
-215.872011733283));
#196823=CARTESIAN_POINT('Ctrl Pts',(-62.0003968515277,-18.1615280644974,
-215.777781255583));
#196824=CARTESIAN_POINT('Ctrl Pts',(-62.0157672317227,-18.8050666555655,
-215.622415496145));
#196825=CARTESIAN_POINT('Ctrl Pts',(-62.0270350697659,-19.3583964345396,
-215.514965174136));
#196826=CARTESIAN_POINT('Ctrl Pts',(-62.0470553637187,-20.4658877553282,
-215.335027953477));
#196827=CARTESIAN_POINT('Ctrl Pts',(-62.0570575007116,-21.2047372367089,
-215.261640165529));
#196828=CARTESIAN_POINT('Ctrl Pts',(-62.0704693967988,-22.6800067729646,
-215.21176681083));
#196829=CARTESIAN_POINT('Ctrl Pts',(-62.0738081330386,-23.4167268528398,
-215.235823868393));
#196830=CARTESIAN_POINT('Ctrl Pts',(-62.0730682231818,-24.5158481803566,
-215.354315196491));
#196831=CARTESIAN_POINT('Ctrl Pts',(-62.071872155047,-24.8812952930637,
-215.407491584122));
#196832=CARTESIAN_POINT('Ctrl Pts',(-62.0685244646623,-25.4271720126043,
-215.509160665575));
#196833=CARTESIAN_POINT('Ctrl Pts',(-62.0671442433642,-25.6087188491995,
-215.546736924888));
#196834=CARTESIAN_POINT('Ctrl Pts',(-62.0646509441297,-25.8803504572708,
-215.608882620349));
#196835=CARTESIAN_POINT('Ctrl Pts',(-62.0637494272904,-25.9707796803734,
-215.630560795157));
#196836=CARTESIAN_POINT('Ctrl Pts',(-62.0622878127024,-26.10624205979,-215.664557073559));
#196837=CARTESIAN_POINT('Ctrl Pts',(-62.0615296291845,-26.1739278170651,
-215.681925290365));
#196838=CARTESIAN_POINT('Ctrl Pts',(-62.0605962917712,-26.2528128366554,
-215.702843946589));
#196839=CARTESIAN_POINT('Ctrl Pts',(-62.0601857362366,-26.2866029536357,
-215.71195050125));
#196840=CARTESIAN_POINT('Ctrl Pts',(-62.0599096760567,-26.3091257269047,
-215.718053065345));
#196841=CARTESIAN_POINT('Ctrl Pts',(-62.059836967416,-26.3186805305512,
-215.720581183794));
#196842=CARTESIAN_POINT('Ctrl Pts',(-62.0596235416337,-26.3318125162586,
-215.724256795808));
#196843=CARTESIAN_POINT('',(-61.6307906481739,-35.3347454198004,-216.138336341698));
#196844=CARTESIAN_POINT('Ctrl Pts',(-62.0596235416337,-26.3318125162586,
-215.724256795808));
#196845=CARTESIAN_POINT('Ctrl Pts',(-62.0594646122662,-26.3415802983989,
-215.726990681004));
#196846=CARTESIAN_POINT('Ctrl Pts',(-62.0591414109411,-26.3555304260684,
-215.731043606804));
#196847=CARTESIAN_POINT('Ctrl Pts',(-62.0586451088583,-26.3794896926403,
-215.737866697814));
#196848=CARTESIAN_POINT('Ctrl Pts',(-62.0578959089358,-26.4154258672405,
-215.748060296758));
#196849=CARTESIAN_POINT('Ctrl Pts',(-62.0561146300557,-26.4992579889169,
-215.771558827276));
#196850=CARTESIAN_POINT('Ctrl Pts',(-62.0524202151427,-26.6668475808658,
-215.817416048729));
#196851=CARTESIAN_POINT('Ctrl Pts',(-62.0445088892061,-27.0017357453129,
-215.904616215262));
#196852=CARTESIAN_POINT('Ctrl Pts',(-62.0368501484612,-27.2883096841957,
-215.971779454331));
#196853=CARTESIAN_POINT('Ctrl Pts',(-62.0203905608737,-27.8609439770147,
-216.096385682438));
#196854=CARTESIAN_POINT('Ctrl Pts',(-62.007903346956,-28.2419562872458,
-216.166476359143));
#196855=CARTESIAN_POINT('Ctrl Pts',(-61.9663758722878,-29.3820316599105,
-216.340372092763));
#196856=CARTESIAN_POINT('Ctrl Pts',(-61.9332872087863,-30.1378403279775,
-216.40779180649));
#196857=CARTESIAN_POINT('Ctrl Pts',(-61.858695018778,-31.6397584228355,
-216.459727323568));
#196858=CARTESIAN_POINT('Ctrl Pts',(-61.7860430758083,-32.9456419949789,
-216.432292162243));
#196859=CARTESIAN_POINT('Ctrl Pts',(-61.7040063394451,-34.235878888517,
-216.295897196999));
#196860=CARTESIAN_POINT('Ctrl Pts',(-61.6615453643437,-34.8774627313319,
-216.20733693376));
#196861=CARTESIAN_POINT('Ctrl Pts',(-61.6554459518943,-34.9690313914074,
-216.194201358865));
#196862=CARTESIAN_POINT('Ctrl Pts',(-61.6462397539745,-35.1062806936728,
-216.173780952623));
#196863=CARTESIAN_POINT('Ctrl Pts',(-61.6416227919041,-35.1748782865785,
-216.163391786615));
#196864=CARTESIAN_POINT('Ctrl Pts',(-61.6369852304075,-35.2434360370502,
-216.152736975617));
#196865=CARTESIAN_POINT('Ctrl Pts',(-61.6338889661978,-35.289132405245,
-216.145575037068));
#196866=CARTESIAN_POINT('Ctrl Pts',(-61.6318678984275,-35.3131377401504,
-216.142292059632));
#196867=CARTESIAN_POINT('Ctrl Pts',(-61.6307906481739,-35.3347454198004,
-216.138336341698));
#196868=CARTESIAN_POINT('Ctrl Pts',(-61.630817075809,-35.334740583441,-216.138302962291));
#196869=CARTESIAN_POINT('Ctrl Pts',(-61.630258520597,-35.3462277829799,
-216.136181498867));
#196870=CARTESIAN_POINT('Ctrl Pts',(-61.6313429993451,-35.3536573552358,
-216.132909291467));
#196871=CARTESIAN_POINT('Ctrl Pts',(-61.6316177861922,-35.3630846532595,
-216.130212116335));
#196872=CARTESIAN_POINT('Ctrl Pts',(-61.6317600130997,-35.367964127875,
-216.128816085622));
#196873=CARTESIAN_POINT('Ctrl Pts',(-61.6319021390161,-35.3728435113644,
-216.127421530594));
#196874=CARTESIAN_POINT('Ctrl Pts',(-61.6320441647623,-35.3777228018413,
-216.126028451162));
#196875=CARTESIAN_POINT('Ctrl Pts',(-61.6324606058031,-35.3920296219691,
-216.121943730863));
#196876=CARTESIAN_POINT('Ctrl Pts',(-61.632876179423,-35.4063356552158,
-216.117871702025));
#196877=CARTESIAN_POINT('Ctrl Pts',(-61.6332908867424,-35.4206408919241,
-216.113812378814));
#196878=CARTESIAN_POINT('Ctrl Pts',(-61.6339117798235,-35.4420584606094,
-216.107734825855));
#196879=CARTESIAN_POINT('Ctrl Pts',(-61.6345307316567,-35.4634742441022,
-216.101685752426));
#196880=CARTESIAN_POINT('Ctrl Pts',(-61.6351477473426,-35.4848882106408,
-216.095665204135));
#196881=CARTESIAN_POINT('Ctrl Pts',(-61.6353549667106,-35.4920799056225,
-216.093643255196));
#196882=CARTESIAN_POINT('Ctrl Pts',(-61.6355619677589,-35.4992713957634,
-216.091624523017));
#196883=CARTESIAN_POINT('Ctrl Pts',(-61.6357687506611,-35.5064626798289,
-216.089609009526));
#196884=CARTESIAN_POINT('Ctrl Pts',(-61.6374137485988,-35.5636707339529,
-216.073575210303));
#196885=CARTESIAN_POINT('Ctrl Pts',(-61.6390449413356,-35.6208657466514,
-216.057745105776));
#196886=CARTESIAN_POINT('Ctrl Pts',(-61.6406624176502,-35.6780470970208,
-216.042119664109));
#196887=CARTESIAN_POINT('Ctrl Pts',(-61.6434323883464,-35.7759716622587,
-216.015360684616));
#196888=CARTESIAN_POINT('Ctrl Pts',(-61.6461621322568,-35.873856159352,
-215.98920192936));
#196889=CARTESIAN_POINT('Ctrl Pts',(-61.6488520954094,-35.9716974699246,
-215.963648260647));
#196890=CARTESIAN_POINT('Ctrl Pts',(-61.6577684374166,-36.2960091939178,
-215.878946264054));
#196891=CARTESIAN_POINT('Ctrl Pts',(-61.6662440943207,-36.6196815346019,
-215.800922589524));
#196892=CARTESIAN_POINT('Ctrl Pts',(-61.6743064449508,-36.9432367142385,
-215.729666205912));
#196893=CARTESIAN_POINT('Ctrl Pts',(-61.690431146211,-37.5903470735117,
-215.587153438688));
#196894=CARTESIAN_POINT('Ctrl Pts',(-61.7049238227888,-38.2370578570965,
-215.47160642675));
#196895=CARTESIAN_POINT('Ctrl Pts',(-61.717722543651,-38.8825180264413,
-215.386359753546));
#196896=CARTESIAN_POINT('Ctrl Pts',(-61.7305212645132,-39.5279781957861,
-215.301113080342));
#196897=CARTESIAN_POINT('Ctrl Pts',(-61.7416182124067,-40.1722488053015,
-215.24609947756));
#196898=CARTESIAN_POINT('Ctrl Pts',(-61.7508074253462,-40.8140216533927,
-215.226712561206));
#196899=CARTESIAN_POINT('Ctrl Pts',(-61.7554020318159,-41.1349080774383,
-215.217019103028));
#196900=CARTESIAN_POINT('Ctrl Pts',(-61.759529053594,-41.4561062910276,
-215.216323666665));
#196901=CARTESIAN_POINT('Ctrl Pts',(-61.7630736382772,-41.7731288880566,
-215.225442248004));
#196902=CARTESIAN_POINT('Ctrl Pts',(-61.7666182229604,-42.0901514850857,
-215.234560829344));
#196903=CARTESIAN_POINT('Ctrl Pts',(-61.7695890991181,-42.4033483152362,
-215.253420330887));
#196904=CARTESIAN_POINT('Ctrl Pts',(-61.7719305274043,-42.7122677019303,
-215.28266947677));
#196905=CARTESIAN_POINT('Ctrl Pts',(-61.7766133839768,-43.3301064753184,
-215.341167768535));
#196906=CARTESIAN_POINT('Ctrl Pts',(-61.7788431881158,-43.9309400562982,
-215.44088331143));
#196907=CARTESIAN_POINT('Ctrl Pts',(-61.777662100194,-44.509800555182,-215.590007618605));
#196908=CARTESIAN_POINT('Ctrl Pts',(-61.7775373295268,-44.570951642519,
-215.605761178487));
#196909=CARTESIAN_POINT('Ctrl Pts',(-61.7773739523109,-44.631856455737,
-215.62206914929));
#196910=CARTESIAN_POINT('Ctrl Pts',(-61.7771699370815,-44.6925059899769,
-215.638946475185));
#196911=CARTESIAN_POINT('Ctrl Pts',(-61.7764083411934,-44.9189127932377,
-215.701950114888));
#196912=CARTESIAN_POINT('Ctrl Pts',(-61.7750804204424,-45.141762233653,
-215.772888079167));
#196913=CARTESIAN_POINT('Ctrl Pts',(-61.7730805145089,-45.3605857093514,
-215.852537712049));
#196914=CARTESIAN_POINT('Ctrl Pts',(-61.7715068721449,-45.5327687534799,
-215.915210678053));
#196915=CARTESIAN_POINT('Ctrl Pts',(-61.7695063242332,-45.7029161773407,
-215.983543948429));
#196916=CARTESIAN_POINT('Ctrl Pts',(-61.7670326019116,-45.8692783289489,
-216.057267272104));
#196917=CARTESIAN_POINT('Ctrl Pts',(-62.3685680449237,-46.7295402395799,
-213.857753233788));
#196918=CARTESIAN_POINT('Ctrl Pts',(-62.3741929604051,-46.5883034476749,
-213.791721439529));
#196919=CARTESIAN_POINT('Ctrl Pts',(-62.3797697215036,-46.4460138537357,
-213.72875854686));
#196920=CARTESIAN_POINT('Ctrl Pts',(-62.385275944621,-46.3032780419763,
-213.668964158759));
#196921=CARTESIAN_POINT('Ctrl Pts',(-62.3975426118317,-45.9852937059672,
-213.535755270514));
#196922=CARTESIAN_POINT('Ctrl Pts',(-62.409516407143,-45.6637866234507,
-213.417460800487));
#196923=CARTESIAN_POINT('Ctrl Pts',(-62.4212099404421,-45.3390922912232,
-213.312250045486));
#196924=CARTESIAN_POINT('Ctrl Pts',(-62.4220692464071,-45.3152319430017,
-213.304518573138));
#196925=CARTESIAN_POINT('Ctrl Pts',(-62.4229270385012,-45.2913543786762,
-213.296857777048));
#196926=CARTESIAN_POINT('Ctrl Pts',(-62.423783321531,-45.2674597292978,
-213.289266941101));
#196927=CARTESIAN_POINT('Ctrl Pts',(-62.4306555056665,-45.0756908577149,
-213.228345936535));
#196928=CARTESIAN_POINT('Ctrl Pts',(-62.4374306715991,-44.8828278915337,
-213.171905711604));
#196929=CARTESIAN_POINT('Ctrl Pts',(-62.4441103360269,-44.6889056159381,
-213.119707758193));
#196930=CARTESIAN_POINT('Ctrl Pts',(-62.4591991205405,-44.2508519591279,
-213.001797093728));
#196931=CARTESIAN_POINT('Ctrl Pts',(-62.4737962281636,-43.8075866319174,
-212.905453163029));
#196932=CARTESIAN_POINT('Ctrl Pts',(-62.4879106189022,-43.359734523307,
-212.828052803901));
#196933=CARTESIAN_POINT('Ctrl Pts',(-62.4903171672674,-43.2833743190478,
-212.814855797302));
#196934=CARTESIAN_POINT('Ctrl Pts',(-62.4927096782803,-43.2068808386599,
-212.802209607456));
#196935=CARTESIAN_POINT('Ctrl Pts',(-62.4950881915082,-43.13025726092,-212.790101352928));
#196936=CARTESIAN_POINT('Ctrl Pts',(-62.5008761037457,-42.9438002178896,
-212.760636932155));
#196937=CARTESIAN_POINT('Ctrl Pts',(-62.5065809373471,-42.7565658493217,
-212.734385263862));
#196938=CARTESIAN_POINT('Ctrl Pts',(-62.5122027551557,-42.5685838171507,
-212.711227872825));
#196939=CARTESIAN_POINT('Ctrl Pts',(-62.5175209296255,-42.390754994103,
-212.689321249381));
#196940=CARTESIAN_POINT('Ctrl Pts',(-62.5227648065832,-42.2122634170404,
-212.67017411522));
#196941=CARTESIAN_POINT('Ctrl Pts',(-62.527934793664,-42.0331254267329,
-212.653679770053));
#196942=CARTESIAN_POINT('Ctrl Pts',(-62.5385750526628,-41.6644446962783,
-212.619733049907));
#196943=CARTESIAN_POINT('Ctrl Pts',(-62.5489103696866,-41.2926330468704,
-212.597082683307));
#196944=CARTESIAN_POINT('Ctrl Pts',(-62.5588215912841,-40.9225569182789,
-212.584979442362));
#196945=CARTESIAN_POINT('Ctrl Pts',(-62.5635469131376,-40.7461176367338,
-212.579209042782));
#196946=CARTESIAN_POINT('Ctrl Pts',(-62.5681836632462,-40.5698182404518,
-212.575793047696));
#196947=CARTESIAN_POINT('Ctrl Pts',(-62.572734055004,-40.3936434675017,
-212.574637782408));
#196948=CARTESIAN_POINT('Ctrl Pts',(-62.5872728250111,-39.8307546787403,
-212.570946641685));
#196949=CARTESIAN_POINT('Ctrl Pts',(-62.6009299850174,-39.2692127837142,
-212.590224636131));
#196950=CARTESIAN_POINT('Ctrl Pts',(-62.6137680988131,-38.7088381795338,
-212.629502632766));
#196951=CARTESIAN_POINT('Ctrl Pts',(-62.6174709897936,-38.5472096022708,
-212.640831566424));
#196952=CARTESIAN_POINT('Ctrl Pts',(-62.6211056256317,-38.3856786969395,
-212.653829961882));
#196953=CARTESIAN_POINT('Ctrl Pts',(-62.6246729139128,-38.2242434316533,
-212.668455765861));
#196954=CARTESIAN_POINT('Ctrl Pts',(-62.6373436782579,-37.6508363946416,
-212.720405622718));
#196955=CARTESIAN_POINT('Ctrl Pts',(-62.64916746512,-37.0786070163147,-212.792770228131));
#196956=CARTESIAN_POINT('Ctrl Pts',(-62.6601855978901,-36.5075023878094,
-212.883581944343));
#196957=CARTESIAN_POINT('Ctrl Pts',(-62.6630243100177,-36.3603629705484,
-212.906978678211));
#196958=CARTESIAN_POINT('Ctrl Pts',(-62.6658095819956,-36.2132944881781,
-212.931604448248));
#196959=CARTESIAN_POINT('Ctrl Pts',(-62.6685426178708,-36.0662511671651,
-212.957447775203));
#196960=CARTESIAN_POINT('Ctrl Pts',(-62.6726066835548,-35.847595524766,
-212.99587719327));
#196961=CARTESIAN_POINT('Ctrl Pts',(-62.6765563106204,-35.6289441132953,
-213.037001059769));
#196962=CARTESIAN_POINT('Ctrl Pts',(-62.6803946782106,-35.4101865945473,
-213.080774391967));
#196963=CARTESIAN_POINT('Ctrl Pts',(-62.6828563633539,-35.2698894184043,
-213.108847826575));
#196964=CARTESIAN_POINT('Ctrl Pts',(-62.6852717293956,-35.1295761809559,
-213.138007694814));
#196965=CARTESIAN_POINT('Ctrl Pts',(-62.6876407845122,-34.9892589138455,
-213.168238544914));
#196966=CARTESIAN_POINT('Ctrl Pts',(-62.6883605905981,-34.9466253667763,
-213.177423789163));
#196967=CARTESIAN_POINT('Ctrl Pts',(-62.6890761418333,-34.9039903123168,
-213.186708083958));
#196968=CARTESIAN_POINT('Ctrl Pts',(-62.6897874443054,-34.8613537452901,
-213.196091056989));
#196969=CARTESIAN_POINT('Ctrl Pts',(-62.6905505729894,-34.8156106352014,
-213.206157682852));
#196970=CARTESIAN_POINT('Ctrl Pts',(-62.6913088108163,-34.7698657837897,
-213.216337913902));
#196971=CARTESIAN_POINT('Ctrl Pts',(-62.6920621645107,-34.7241191838736,
-213.226631336799));
#196972=CARTESIAN_POINT('Ctrl Pts',(-62.6922505029487,-34.712682533017,
-213.22920469272));
#196973=CARTESIAN_POINT('Ctrl Pts',(-62.6924385015881,-34.7012457426654,
-213.231787136791));
#196974=CARTESIAN_POINT('Ctrl Pts',(-62.6926262681682,-34.6898089068761,
-213.234372387595));
#196975=CARTESIAN_POINT('Ctrl Pts',(-62.6928140347405,-34.6783720715574,
-213.236957638293));
#196976=CARTESIAN_POINT('Ctrl Pts',(-62.6930017734618,-34.666935369537,
-213.23953379065));
#196977=CARTESIAN_POINT('Ctrl Pts',(-62.6931894847934,-34.6554988009796,
-213.242100818803));
#196978=CARTESIAN_POINT('Ctrl Pts',(-62.6935649074066,-34.6326256669197,
-213.247234874422));
#196979=CARTESIAN_POINT('Ctrl Pts',(-62.693940220454,-34.6097530667601,
-213.252332433528));
#196980=CARTESIAN_POINT('Ctrl Pts',(-62.69431542765,-34.5868810019287,-213.257393287646));
#196981=CARTESIAN_POINT('Ctrl Pts',(-62.6950609186327,-34.5414369958665,
-213.267448588158));
#196982=CARTESIAN_POINT('Ctrl Pts',(-62.695805991523,-34.4959951029827,
-213.277359001672));
#196983=CARTESIAN_POINT('Ctrl Pts',(-62.6965506762908,-34.450555335486,
-213.28712284428));
#196984=CARTESIAN_POINT('Ctrl Pts',(-62.6973051981915,-34.4045153179852,
-213.297015665244));
#196985=CARTESIAN_POINT('Ctrl Pts',(-62.6980593192824,-34.3584776267204,
-213.306757986266));
#196986=CARTESIAN_POINT('Ctrl Pts',(-62.6988130699629,-34.3124423208934,
-213.316348049998));
#196987=CARTESIAN_POINT('Ctrl Pts',(-62.7009988974643,-34.1789429554945,
-213.34415860538));
#196988=CARTESIAN_POINT('Ctrl Pts',(-62.7031812969114,-34.0454633873908,
-213.370706259291));
#196989=CARTESIAN_POINT('Ctrl Pts',(-62.7053612372101,-33.9120052530651,
-213.395935334588));
#196990=CARTESIAN_POINT('Ctrl Pts',(-62.7241252898362,-32.7632511071928,
-213.61309710589));
#196991=CARTESIAN_POINT('Ctrl Pts',(-62.7427109555555,-31.6158500572718,
-213.732605675668));
#196992=CARTESIAN_POINT('Ctrl Pts',(-62.7617431230016,-30.4704148960704,
-213.718959479368));
#196993=CARTESIAN_POINT('Ctrl Pts',(-62.7647391297308,-30.2901027240271,
-213.716811321726));
#196994=CARTESIAN_POINT('Ctrl Pts',(-62.7677462013119,-30.1098392611621,
-213.711363635705));
#196995=CARTESIAN_POINT('Ctrl Pts',(-62.7707667754261,-29.929626890117,
-213.702478069896));
#196996=CARTESIAN_POINT('Ctrl Pts',(-62.7725414402335,-29.8237474974438,
-213.697257571958));
#196997=CARTESIAN_POINT('Ctrl Pts',(-62.7743209052534,-29.7178858577744,
-213.690842589644));
#196998=CARTESIAN_POINT('Ctrl Pts',(-62.7761057740119,-29.6120425444018,
-213.683199054813));
#196999=CARTESIAN_POINT('Ctrl Pts',(-62.7866097971823,-28.9891504629465,
-213.638216550309));
#197000=CARTESIAN_POINT('Ctrl Pts',(-62.7973012895261,-28.3668822616518,
-213.550676253008));
#197001=CARTESIAN_POINT('Ctrl Pts',(-62.8083033340944,-27.7453414694755,
-213.413639151456));
#197002=CARTESIAN_POINT('Ctrl Pts',(-62.8099338015368,-27.6532311331213,
-213.39333069596));
#197003=CARTESIAN_POINT('Ctrl Pts',(-62.811571077252,-27.5611367494673,
-213.371935988235));
#197004=CARTESIAN_POINT('Ctrl Pts',(-62.8132156027367,-27.4690586781088,
-213.349430181199));
#197005=CARTESIAN_POINT('Ctrl Pts',(-62.8148166574625,-27.3794145633366,
-213.327519284075));
#197006=CARTESIAN_POINT('Ctrl Pts',(-62.8164245864001,-27.2897858690337,
-213.304555131303));
#197007=CARTESIAN_POINT('Ctrl Pts',(-62.8180397952864,-27.2001730524582,
-213.280514793433));
#197008=CARTESIAN_POINT('Ctrl Pts',(-62.8188583605629,-27.1547585301661,
-213.268331486382));
#197009=CARTESIAN_POINT('Ctrl Pts',(-62.8196787972069,-27.1093480871546,
-213.25587168702));
#197010=CARTESIAN_POINT('Ctrl Pts',(-62.8205011614669,-27.063941785938,
-213.243132215583));
#197011=CARTESIAN_POINT('Ctrl Pts',(-62.820603956966,-27.0582660001277,
-213.241539782171));
#197012=CARTESIAN_POINT('Ctrl Pts',(-62.8207068130078,-27.0525903054942,
-213.23994121606));
#197013=CARTESIAN_POINT('Ctrl Pts',(-62.8208096296675,-27.0469146151422,
-213.238342307309));
#197014=CARTESIAN_POINT('Ctrl Pts',(-62.8209124463233,-27.0412389250094,
-213.23674339862));
#197015=CARTESIAN_POINT('Ctrl Pts',(-62.8210151618557,-27.0355631854498,
-213.23514772473));
#197016=CARTESIAN_POINT('Ctrl Pts',(-62.8211177763469,-27.0298873965555,
-213.233555280697));
#197017=CARTESIAN_POINT('Ctrl Pts',(-62.8213230053217,-27.0185358191958,
-213.23037039275));
#197018=CARTESIAN_POINT('Ctrl Pts',(-62.8215278301311,-27.007184044526,
-213.227198424317));
#197019=CARTESIAN_POINT('Ctrl Pts',(-62.821732251428,-26.9958320733605,
-213.224039336346));
#197020=CARTESIAN_POINT('Ctrl Pts',(-62.8221023145257,-26.9752816430542,
-213.218320451383));
#197021=CARTESIAN_POINT('Ctrl Pts',(-62.8224710552457,-26.9547305687705,
-213.212643777776));
#197022=CARTESIAN_POINT('Ctrl Pts',(-62.8228384774044,-26.9341788553176,
-213.207009087125));
#197023=CARTESIAN_POINT('Ctrl Pts',(-62.8228769801512,-26.9320252088911,
-213.206418619016));
#197024=CARTESIAN_POINT('Ctrl Pts',(-62.8229154684173,-26.9298715555,-213.205828611962));
#197025=CARTESIAN_POINT('Ctrl Pts',(-62.822953942207,-26.927717895148,-213.205239065704));
#197026=CARTESIAN_POINT('Ctrl Pts',(-62.8245764233091,-26.8368957212836,
-213.18037726579));
#197027=CARTESIAN_POINT('Ctrl Pts',(-62.8261731614531,-26.7460611681188,
-213.156334842912));
#197028=CARTESIAN_POINT('Ctrl Pts',(-62.8277444695765,-26.6552145055689,
-213.133093149386));
#197029=CARTESIAN_POINT('Ctrl Pts',(-62.8292202126583,-26.56989302612,-213.111264987285));
#197030=CARTESIAN_POINT('Ctrl Pts',(-62.8306735455578,-26.4845608838021,
-213.090141906315));
#197031=CARTESIAN_POINT('Ctrl Pts',(-62.8321046858337,-26.3992182785356,
-213.069710892685));
#197032=CARTESIAN_POINT('Ctrl Pts',(-62.8367688988908,-26.1210791607003,
-213.003124407662));
#197033=CARTESIAN_POINT('Ctrl Pts',(-62.8411971255009,-25.8428597458171,
-212.943883039818));
#197034=CARTESIAN_POINT('Ctrl Pts',(-62.8453976824702,-25.5644780440306,
-212.891551576526));
#197035=CARTESIAN_POINT('Ctrl Pts',(-62.8465846366303,-25.485815542499,
-212.876764240343));
#197036=CARTESIAN_POINT('Ctrl Pts',(-62.8477534065635,-25.4071494583571,
-212.862521456415));
#197037=CARTESIAN_POINT('Ctrl Pts',(-62.8489040944972,-25.3284786414784,
-212.848818315903));
#197038=CARTESIAN_POINT('Ctrl Pts',(-62.8589719385762,-24.6401551658149,
-212.728923878816));
#197039=CARTESIAN_POINT('Ctrl Pts',(-62.8676537352891,-23.9520875862977,
-212.65003766299));
#197040=CARTESIAN_POINT('Ctrl Pts',(-62.8750146865604,-23.2647003090938,
-212.608425061387));
#197041=CARTESIAN_POINT('Ctrl Pts',(-62.8823756378316,-22.5773130318898,
-212.566812459785));
#197042=CARTESIAN_POINT('Ctrl Pts',(-62.8884156923501,-21.8906064258753,
-212.562474309898));
#197043=CARTESIAN_POINT('Ctrl Pts',(-62.8931986251439,-21.205051121817,
-212.591707581156));
#197044=CARTESIAN_POINT('Ctrl Pts',(-62.8935577382081,-21.1535781288823,
-212.593902479154));
#197045=CARTESIAN_POINT('Ctrl Pts',(-62.8939097569274,-21.1021052395342,
-212.596289051621));
#197046=CARTESIAN_POINT('Ctrl Pts',(-62.8942546885952,-21.0506330432678,
-212.598866899387));
#197047=CARTESIAN_POINT('Ctrl Pts',(-62.8968212608728,-20.6676380203933,
-212.618048184355));
#197048=CARTESIAN_POINT('Ctrl Pts',(-62.898993894224,-20.2848774438099,
-212.64782882147));
#197049=CARTESIAN_POINT('Ctrl Pts',(-62.900778786722,-19.9023518511943,
-212.687972680865));
#197050=CARTESIAN_POINT('Ctrl Pts',(-62.9023087147126,-19.5744684565834,
-212.722382156061));
#197051=CARTESIAN_POINT('Ctrl Pts',(-62.9035537360166,-19.2467573919575,
-212.764406500889));
#197052=CARTESIAN_POINT('Ctrl Pts',(-62.9045166573415,-18.9192122497013,
-212.81392668013));
#197053=CARTESIAN_POINT('Ctrl Pts',(-62.9053466520591,-18.6368831218561,
-212.856610839387));
#197054=CARTESIAN_POINT('Ctrl Pts',(-62.9059670124065,-18.3545500700678,
-212.904900139621));
#197055=CARTESIAN_POINT('Ctrl Pts',(-62.9063776080623,-18.0726457860301,
-212.95869124202));
#197056=CARTESIAN_POINT('Ctrl Pts',(-62.9064830589281,-18.0002459678509,
-212.972506094273));
#197057=CARTESIAN_POINT('Ctrl Pts',(-62.9065746841136,-17.9278744301204,
-212.986683569855));
#197058=CARTESIAN_POINT('Ctrl Pts',(-62.9066525023395,-17.8555384962728,
-213.00122136616));
#197059=CARTESIAN_POINT('Ctrl Pts',(-62.9070069220114,-17.5260876814359,
-213.06743311714));
#197060=CARTESIAN_POINT('Ctrl Pts',(-62.9070749640207,-17.197340288906,
-213.141130341411));
#197061=CARTESIAN_POINT('Ctrl Pts',(-62.9068586171446,-16.8692921444043,
-213.222255473336));
#197062=CARTESIAN_POINT('Ctrl Pts',(-62.9068512161578,-16.8580699810933,
-213.225030674155));
#197063=CARTESIAN_POINT('Ctrl Pts',(-62.9068434310689,-16.8468489287218,
-213.227817504345));
#197064=CARTESIAN_POINT('Ctrl Pts',(-62.9068354227292,-16.8356281229708,
-213.230606932774));
#197065=CARTESIAN_POINT('Ctrl Pts',(-62.9068274143987,-16.824407330074,
-213.233396358007));
#197066=CARTESIAN_POINT('Ctrl Pts',(-62.9068194222443,-16.81318550769,-213.236174929377));
#197067=CARTESIAN_POINT('Ctrl Pts',(-62.9068114465212,-16.8019626469682,
-213.238942628495));
#197068=CARTESIAN_POINT('Ctrl Pts',(-62.9068100308831,-16.7999706633578,
-213.239433876798));
#197069=CARTESIAN_POINT('Ctrl Pts',(-62.9068086157626,-16.7979786470357,
-213.239924782582));
#197070=CARTESIAN_POINT('Ctrl Pts',(-62.9068072011611,-16.7959865979527,
-213.240415345746));
#197071=CARTESIAN_POINT('Ctrl Pts',(-62.9067926759976,-16.7755321875305,
-213.245452460734));
#197072=CARTESIAN_POINT('Ctrl Pts',(-62.9067782084953,-16.7550743640961,
-213.250453275771));
#197073=CARTESIAN_POINT('Ctrl Pts',(-62.9067638003454,-16.7346131155667,
-213.255417662646));
#197074=CARTESIAN_POINT('Ctrl Pts',(-62.9067321774736,-16.6897049597551,
-213.266313452264));
#197075=CARTESIAN_POINT('Ctrl Pts',(-62.9067008405294,-16.6447803048274,
-213.277033762557));
#197076=CARTESIAN_POINT('Ctrl Pts',(-62.9066698070808,-16.5998390244792,
-213.287577252305));
#197077=CARTESIAN_POINT('Ctrl Pts',(-62.9066077395427,-16.5099555355157,
-213.308664449577));
#197078=CARTESIAN_POINT('Ctrl Pts',(-62.9065468864317,-16.4200055414544,
-213.329044330242));
#197079=CARTESIAN_POINT('Ctrl Pts',(-62.9064873833149,-16.3299880540902,
-213.348706398678));
#197080=CARTESIAN_POINT('Ctrl Pts',(-62.9063683745862,-16.14994930492,-213.388031359981));
#197081=CARTESIAN_POINT('Ctrl Pts',(-62.9062547727652,-15.9696405404297,
-213.424484631685));
#197082=CARTESIAN_POINT('Ctrl Pts',(-62.9061475795573,-15.7890542301186,
-213.457986204279));
#197083=CARTESIAN_POINT('Ctrl Pts',(-62.9059331838863,-15.4278660176369,
-213.524992242));
#197084=CARTESIAN_POINT('Ctrl Pts',(-62.9057445834296,-15.0655667619647,
-213.58018242881));
#197085=CARTESIAN_POINT('Ctrl Pts',(-62.905589362047,-14.7020974635233,
-213.622929699832));
#197086=CARTESIAN_POINT('Ctrl Pts',(-62.9052798509934,-13.9773405794218,
-213.708167652755));
#197087=CARTESIAN_POINT('Ctrl Pts',(-62.9051047269463,-13.2479237446018,
-213.743849925036));
#197088=CARTESIAN_POINT('Ctrl Pts',(-62.9051090261727,-12.5134449350678,
-213.725695782834));
#197089=CARTESIAN_POINT('Ctrl Pts',(-62.9051090395082,-12.5111666950214,
-213.725639471484));
#197090=CARTESIAN_POINT('Ctrl Pts',(-62.9051090545696,-12.5088884062743,
-213.725582642177));
#197091=CARTESIAN_POINT('Ctrl Pts',(-62.9051090713583,-12.5066100688143,
-213.725525294786));
#197092=CARTESIAN_POINT('Ctrl Pts',(-62.9051117186635,-12.1473516978959,
-213.716482503419));
#197093=CARTESIAN_POINT('Ctrl Pts',(-62.9051569926989,-11.7868835043618,
-213.694572753784));
#197094=CARTESIAN_POINT('Ctrl Pts',(-62.9052478305722,-11.4251692471516,
-213.659411822611));
#197095=CARTESIAN_POINT('Ctrl Pts',(-62.9052501495695,-11.4159350548302,
-213.658514200263));
#197096=CARTESIAN_POINT('Ctrl Pts',(-62.905252498141,-11.4066999814362,
-213.657607942971));
#197097=CARTESIAN_POINT('Ctrl Pts',(-62.9052548763439,-11.3974640308012,
-213.656693043944));
#197098=CARTESIAN_POINT('Ctrl Pts',(-62.9053396597116,-11.0682006948933,
-213.624076725649));
#197099=CARTESIAN_POINT('Ctrl Pts',(-62.9054625664031,-10.7375855896767,
-213.580337710378));
#197100=CARTESIAN_POINT('Ctrl Pts',(-62.9056218033686,-10.4097786632115,
-213.526208718246));
#197101=CARTESIAN_POINT('Ctrl Pts',(-62.9056341733888,-10.3843136067641,
-213.522003810635));
#197102=CARTESIAN_POINT('Ctrl Pts',(-62.905646762572,-10.3588654933522,
-213.517736228732));
#197103=CARTESIAN_POINT('Ctrl Pts',(-62.9056595700396,-10.3334362698611,
-213.513406328741));
#197104=CARTESIAN_POINT('Ctrl Pts',(-62.9056676765601,-10.317340775653,
-213.510665707099));
#197105=CARTESIAN_POINT('Ctrl Pts',(-62.9056758700813,-10.3012520481916,
-213.507900031565));
#197106=CARTESIAN_POINT('Ctrl Pts',(-62.9056841503679,-10.2851705845394,
-213.505109387712));
#197107=CARTESIAN_POINT('Ctrl Pts',(-62.9058495001971,-9.96403831223826,
-213.449382756037));
#197108=CARTESIAN_POINT('Ctrl Pts',(-62.9060495440864,-9.64477667567909,
-213.383630454477));
#197109=CARTESIAN_POINT('Ctrl Pts',(-62.9062818494613,-9.32750692225147,
-213.308308849077));
#197110=CARTESIAN_POINT('Ctrl Pts',(-62.9062995203884,-9.30337295347418,
-213.302579310559));
#197111=CARTESIAN_POINT('Ctrl Pts',(-62.9063173779087,-9.27925050600288,
-213.296794425733));
#197112=CARTESIAN_POINT('Ctrl Pts',(-62.9063354209129,-9.25513963110861,
-213.290954407383));
#197113=CARTESIAN_POINT('Ctrl Pts',(-62.9063523663721,-9.23249540595939,
-213.28546963377));
#197114=CARTESIAN_POINT('Ctrl Pts',(-62.9063694755794,-9.20986097578642,
-213.279936139709));
#197115=CARTESIAN_POINT('Ctrl Pts',(-62.9063867476374,-9.18723633851541,
-213.274354087607));
#197116=CARTESIAN_POINT('Ctrl Pts',(-62.9064214242477,-9.14181351020547,
-213.263147163439));
#197117=CARTESIAN_POINT('Ctrl Pts',(-62.9064567545313,-9.09643013343645,
-213.251744618045));
#197118=CARTESIAN_POINT('Ctrl Pts',(-62.9064927284741,-9.05108616789961,
-213.240147881952));
#197119=CARTESIAN_POINT('Ctrl Pts',(-62.9065017219161,-9.03975023169194,
-213.23724871204));
#197120=CARTESIAN_POINT('Ctrl Pts',(-62.906510755583,-9.02841675862167,
-213.23433740548));
#197121=CARTESIAN_POINT('Ctrl Pts',(-62.9065198293118,-9.01708574800018,
-213.231413985003));
#197122=CARTESIAN_POINT('Ctrl Pts',(-62.9065289030347,-9.00575474453466,
-213.228490566373));
#197123=CARTESIAN_POINT('Ctrl Pts',(-62.9065377477119,-8.99442319446877,
-213.225569813864));
#197124=CARTESIAN_POINT('Ctrl Pts',(-62.9065461779452,-8.98308903056771,
-213.222661899751));
#197125=CARTESIAN_POINT('Ctrl Pts',(-62.9065630384181,-8.96042069442155,
-213.216846069384));
#197126=CARTESIAN_POINT('Ctrl Pts',(-62.9065784765558,-8.93774453557201,
-213.211068662567));
#197127=CARTESIAN_POINT('Ctrl Pts',(-62.9065924909309,-8.91506058486269,
-213.205329682185));
#197128=CARTESIAN_POINT('Ctrl Pts',(-62.906632507978,-8.85028818379569,
-213.188942433607));
#197129=CARTESIAN_POINT('Ctrl Pts',(-62.9066609166417,-8.7854522548987,
-213.172868479925));
#197130=CARTESIAN_POINT('Ctrl Pts',(-62.9066776826504,-8.72055350098855,
-213.157107960246));
#197131=CARTESIAN_POINT('Ctrl Pts',(-62.9066844034019,-8.69453846021989,
-213.1507902648));
#197132=CARTESIAN_POINT('Ctrl Pts',(-62.9066892533842,-8.66851311367876,
-213.144522883906));
#197133=CARTESIAN_POINT('Ctrl Pts',(-62.9066922303343,-8.64247748890024,
-213.13830582419));
#197134=CARTESIAN_POINT('Ctrl Pts',(-62.9067096741274,-8.48991865034706,
-213.101876223688));
#197135=CARTESIAN_POINT('Ctrl Pts',(-62.9066627545095,-8.33741593724109,
-213.067272060264));
#197136=CARTESIAN_POINT('Ctrl Pts',(-62.906552054195,-8.18500124845787,
-213.034473300197));
#197137=CARTESIAN_POINT('Ctrl Pts',(-62.9065307100423,-8.15561413774858,
-213.02814936383));
#197138=CARTESIAN_POINT('Ctrl Pts',(-62.906506993431,-8.12623007030402,
-213.021892565579));
#197139=CARTESIAN_POINT('Ctrl Pts',(-62.9064809085264,-8.09684923724608,
-213.015702751583));
#197140=CARTESIAN_POINT('Ctrl Pts',(-62.9056899601275,-7.20596145140544,
-212.828014755284));
#197141=CARTESIAN_POINT('Ctrl Pts',(-62.9027366747181,-6.31764267915001,
-212.700961335132));
#197142=CARTESIAN_POINT('Ctrl Pts',(-62.8976715771841,-5.43185195165884,
-212.632707606633));
#197143=CARTESIAN_POINT('Ctrl Pts',(-62.8947900085007,-4.92791953904604,
-212.593877592946));
#197144=CARTESIAN_POINT('Ctrl Pts',(-62.8912249487153,-4.42480439538553,
-212.574078170132));
#197145=CARTESIAN_POINT('Ctrl Pts',(-62.8869856905768,-3.92249156539548,
-212.572970530223));
#197146=CARTESIAN_POINT('Ctrl Pts',(-62.8865147226824,-3.8666862314995,
-212.572847475005));
#197147=CARTESIAN_POINT('Ctrl Pts',(-62.8860354164368,-3.81089071961118,
-212.572956060008));
#197148=CARTESIAN_POINT('Ctrl Pts',(-62.885547785291,-3.75510503118202,
-212.573295788909));
#197149=CARTESIAN_POINT('Ctrl Pts',(-62.8793243758262,-3.04313824163478,
-212.577631590838));
#197150=CARTESIAN_POINT('Ctrl Pts',(-62.8717459291031,-2.33277234486263,
-212.619539913621));
#197151=CARTESIAN_POINT('Ctrl Pts',(-62.862782948286,-1.62412895620602,
-212.701365863942));
#197152=CARTESIAN_POINT('Ctrl Pts',(-62.8546488502804,-0.981019828565347,
-212.775624675034));
#197153=CARTESIAN_POINT('Ctrl Pts',(-62.8453744839341,-0.339328956700993,
-212.882759122652));
#197154=CARTESIAN_POINT('Ctrl Pts',(-62.8349373318117,0.300889820690812,
-213.0245235881));
#197155=CARTESIAN_POINT('Ctrl Pts',(-62.833607314137,0.382473597532965,
-213.0425887885));
#197156=CARTESIAN_POINT('Ctrl Pts',(-62.8322582595392,0.46403334488501,
-213.0612252722));
#197157=CARTESIAN_POINT('Ctrl Pts',(-62.8308901810048,0.545568613619919,
-213.080433504715));
#197158=CARTESIAN_POINT('Ctrl Pts',(-62.8293216865052,0.639048349842208,
-213.102455637426));
#197159=CARTESIAN_POINT('Ctrl Pts',(-62.8277279878957,0.732495388151248,
-213.125241286058));
#197160=CARTESIAN_POINT('Ctrl Pts',(-62.8261090055383,0.82590908127445,
-213.148796974995));
#197161=CARTESIAN_POINT('Ctrl Pts',(-62.8246401331401,0.910661577071861,
-213.170168610789));
#197162=CARTESIAN_POINT('Ctrl Pts',(-62.8231504392872,0.995387120797636,
-213.192174253453));
#197163=CARTESIAN_POINT('Ctrl Pts',(-62.8216398034464,1.08008493804872,
-213.214822482476));
#197164=CARTESIAN_POINT('Ctrl Pts',(-62.8212428495944,1.10234121179649,
-213.220773818666));
#197165=CARTESIAN_POINT('Ctrl Pts',(-62.8208444494788,1.12459557042322,
-213.226769539358));
#197166=CARTESIAN_POINT('Ctrl Pts',(-62.8204446007164,1.14684799932478,
-213.232809812555));
#197167=CARTESIAN_POINT('Ctrl Pts',(-62.8202446762939,1.15797421607791,
-213.235829949778));
#197168=CARTESIAN_POINT('Ctrl Pts',(-62.8200446532189,1.16910062229217,
-213.238845621168));
#197169=CARTESIAN_POINT('Ctrl Pts',(-62.8198447802283,1.18022785110057,
-213.241842094701));
#197170=CARTESIAN_POINT('Ctrl Pts',(-62.8196449071673,1.19135508383139,
-213.24483856929));
#197171=CARTESIAN_POINT('Ctrl Pts',(-62.8194451061373,1.20248294022561,
-213.247820468072));
#197172=CARTESIAN_POINT('Ctrl Pts',(-62.8192453767934,1.21361141859872,
-213.250787808694));
#197173=CARTESIAN_POINT('Ctrl Pts',(-62.818446458071,1.25812540713443,-213.262657191196));
#197174=CARTESIAN_POINT('Ctrl Pts',(-62.8176486863071,1.30264934734857,
-213.274293643791));
#197175=CARTESIAN_POINT('Ctrl Pts',(-62.8168520397829,1.34718313255572,
-213.285698279351));
#197176=CARTESIAN_POINT('Ctrl Pts',(-62.8168331493294,1.3482391384167,-213.285968711382));
#197177=CARTESIAN_POINT('Ctrl Pts',(-62.8168142595085,1.3492951498132,-213.28623901307));
#197178=CARTESIAN_POINT('Ctrl Pts',(-62.8167953703201,1.35035116674384,
-213.28650918443));
#197179=CARTESIAN_POINT('Ctrl Pts',(-62.8152210633639,1.43836420130322,
-213.30902643819));
#197180=CARTESIAN_POINT('Ctrl Pts',(-62.8136511488777,1.52641572029817,
-213.330638365248));
#197181=CARTESIAN_POINT('Ctrl Pts',(-62.8120854563785,1.61450537353331,
-213.351353373466));
#197182=CARTESIAN_POINT('Ctrl Pts',(-62.8074297466586,1.87644688184623,
-213.412951078736));
#197183=CARTESIAN_POINT('Ctrl Pts',(-62.8028113125303,2.13872544174752,
-213.466621196678));
#197184=CARTESIAN_POINT('Ctrl Pts',(-62.7982260322374,2.40133274732117,
-213.512564584869));
#197185=CARTESIAN_POINT('Ctrl Pts',(-62.7965691479007,2.49622551363434,
-213.529166161088));
#197186=CARTESIAN_POINT('Ctrl Pts',(-62.7949165988104,2.59116092814595,
-213.544758707681));
#197187=CARTESIAN_POINT('Ctrl Pts',(-62.7932681861794,2.6861388388309,-213.559351754428));
#197188=CARTESIAN_POINT('Ctrl Pts',(-62.7870578081227,3.04396716487013,
-213.614330911704));
#197189=CARTESIAN_POINT('Ctrl Pts',(-62.7808961247399,3.40303459050701,
-213.655110348145));
#197190=CARTESIAN_POINT('Ctrl Pts',(-62.7748157638915,3.76060806585584,
-213.682219323134));
#197191=CARTESIAN_POINT('Ctrl Pts',(-62.7705733532615,4.01009548126256,
-213.701133891944));
#197192=CARTESIAN_POINT('Ctrl Pts',(-62.7663688307484,4.25893819616316,
-213.713443335564));
#197193=CARTESIAN_POINT('Ctrl Pts',(-62.7621968858993,4.50717455612263,
-213.719490676914));
#197194=CARTESIAN_POINT('Ctrl Pts',(-62.7603897273271,4.61470293486237,
-213.722110199739));
#197195=CARTESIAN_POINT('Ctrl Pts',(-62.7585886940891,4.72211697152003,
-213.723554528341));
#197196=CARTESIAN_POINT('Ctrl Pts',(-62.756793361705,4.82941936939531,-213.723851522444));
#197197=CARTESIAN_POINT('Ctrl Pts',(-62.7449145685473,5.53938427674049,
-213.72581658003));
#197198=CARTESIAN_POINT('Ctrl Pts',(-62.7332829196989,6.24447623947785,
-213.677701667467));
#197199=CARTESIAN_POINT('Ctrl Pts',(-62.7217741472389,6.94546014142215,
-213.58738262144));
#197200=CARTESIAN_POINT('Ctrl Pts',(-62.7160202469306,7.29592249555901,
-213.542226911863));
#197201=CARTESIAN_POINT('Ctrl Pts',(-62.7102974318188,7.64535562415708,
-213.486497387223));
#197202=CARTESIAN_POINT('Ctrl Pts',(-62.7045905440093,7.99385039894269,
-213.42112885562));
#197203=CARTESIAN_POINT('Ctrl Pts',(-62.7017372091525,8.16809112725469,
-213.388445838889));
#197204=CARTESIAN_POINT('Ctrl Pts',(-62.6988879008502,8.34209702777322,
-213.353350616143));
#197205=CARTESIAN_POINT('Ctrl Pts',(-62.6960409729441,8.51587804140929,
-213.31594549485));
#197206=CARTESIAN_POINT('Ctrl Pts',(-62.6953306860554,8.55923508435002,
-213.306613201199));
#197207=CARTESIAN_POINT('Ctrl Pts',(-62.6946205479401,8.60257812546093,
-213.297137089371));
#197208=CARTESIAN_POINT('Ctrl Pts',(-62.693910534767,8.64590730924635,-213.287518647044));
#197209=CARTESIAN_POINT('Ctrl Pts',(-62.6931976571302,8.68941129946275,
-213.277861400257));
#197210=CARTESIAN_POINT('Ctrl Pts',(-62.6924849069969,8.73290123523708,
-213.268060682277));
#197211=CARTESIAN_POINT('Ctrl Pts',(-62.6917722569378,8.77637732701844,
-213.258118114802));
#197212=CARTESIAN_POINT('Ctrl Pts',(-62.6914166494633,8.79807159758174,
-213.253156842064));
#197213=CARTESIAN_POINT('Ctrl Pts',(-62.6910610669502,8.8197624208846,-213.248160247015));
#197214=CARTESIAN_POINT('Ctrl Pts',(-62.6907055060663,8.84144982288414,
-213.243128526156));
#197215=CARTESIAN_POINT('Ctrl Pts',(-62.6903499459702,8.86313717683234,
-213.238096816445));
#197216=CARTESIAN_POINT('Ctrl Pts',(-62.6899947488889,8.88481939248657,
-213.233012444837));
#197217=CARTESIAN_POINT('Ctrl Pts',(-62.6896387405559,8.90650238461306,
-213.227935756798));
#197218=CARTESIAN_POINT('Ctrl Pts',(-62.6889267268058,8.94986819125594,
-213.217782422304));
#197219=CARTESIAN_POINT('Ctrl Pts',(-62.6882099166076,8.99324491620445,
-213.20773948302));
#197220=CARTESIAN_POINT('Ctrl Pts',(-62.6874882954834,9.03663265289044,
-213.197807426414));
#197221=CARTESIAN_POINT('Ctrl Pts',(-62.6868204901171,9.0767846972564,-213.1886160648));
#197222=CARTESIAN_POINT('Ctrl Pts',(-62.6861485996542,9.11694554599575,
-213.179518348821));
#197223=CARTESIAN_POINT('Ctrl Pts',(-62.6854726096978,9.15711522005327,
-213.170514913905));
#197224=CARTESIAN_POINT('Ctrl Pts',(-62.6826037415343,9.3275933432039,-213.132304778465));
#197225=CARTESIAN_POINT('Ctrl Pts',(-62.6796606062759,9.49823764842399,
-213.0958088569));
#197226=CARTESIAN_POINT('Ctrl Pts',(-62.6766425417446,9.66904980342632,
-213.061049681902));
#197227=CARTESIAN_POINT('Ctrl Pts',(-62.6706064126818,10.010674113431,-212.991531331906));
#197228=CARTESIAN_POINT('Ctrl Pts',(-62.664270812359,10.3529550669585,-212.928960848345));
#197229=CARTESIAN_POINT('Ctrl Pts',(-62.6576327768096,10.6957266313347,
-212.873621170708));
#197230=CARTESIAN_POINT('Ctrl Pts',(-62.6473143570134,11.2285440393067,
-212.787599030422));
#197231=CARTESIAN_POINT('Ctrl Pts',(-62.6362643202696,11.7626593744732,
-212.718966127623));
#197232=CARTESIAN_POINT('Ctrl Pts',(-62.6244492722702,12.2981837916612,
-212.669131165341));
#197233=CARTESIAN_POINT('Ctrl Pts',(-62.6210626304399,12.4516854441724,
-212.654846570993));
#197234=CARTESIAN_POINT('Ctrl Pts',(-62.6176131332117,12.6053025653781,
-212.642106558566));
#197235=CARTESIAN_POINT('Ctrl Pts',(-62.6140999935327,12.7590370278545,
-212.630944584506));
#197236=CARTESIAN_POINT('Ctrl Pts',(-62.6105014211192,12.9165100139118,
-212.619511172914));
#197237=CARTESIAN_POINT('Ctrl Pts',(-62.6068362958068,13.0740938080764,
-212.609737755954));
#197238=CARTESIAN_POINT('Ctrl Pts',(-62.6031038882691,13.2317919256033,
-212.60165208257));
#197239=CARTESIAN_POINT('Ctrl Pts',(-62.5920978382562,13.6968090361302,
-212.577809207764));
#197240=CARTESIAN_POINT('Ctrl Pts',(-62.5804979951207,14.1630944923736,
-212.568752968315));
#197241=CARTESIAN_POINT('Ctrl Pts',(-62.5682752556912,14.6305393235299,
-212.576049312116));
#197242=CARTESIAN_POINT('Ctrl Pts',(-62.5664789097222,14.69923854133,-212.577121637829));
#197243=CARTESIAN_POINT('Ctrl Pts',(-62.5646691057699,14.7679628409678,
-212.57854725337));
#197244=CARTESIAN_POINT('Ctrl Pts',(-62.5628457474452,14.8367119180636,
-212.580331218974));
#197245=CARTESIAN_POINT('Ctrl Pts',(-62.5582940634694,15.0083315434174,
-212.584784566154));
#197246=CARTESIAN_POINT('Ctrl Pts',(-62.5536582189233,15.1800866651594,
-212.591481763734));
#197247=CARTESIAN_POINT('Ctrl Pts',(-62.5489369347187,15.3519656949738,
-212.600500512768));
#197248=CARTESIAN_POINT('Ctrl Pts',(-62.5345339878628,15.8763070446555,
-212.628013485384));
#197249=CARTESIAN_POINT('Ctrl Pts',(-62.5194888785073,16.3962308632549,
-212.67684339347));
#197250=CARTESIAN_POINT('Ctrl Pts',(-62.5037997387389,16.9113773860642,
-212.748829194443));
#197251=CARTESIAN_POINT('Ctrl Pts',(-62.4982710429057,17.0929098649718,
-212.774196270251));
#197252=CARTESIAN_POINT('Ctrl Pts',(-62.4926620464246,17.2738497478374,
-212.802456316522));
#197253=CARTESIAN_POINT('Ctrl Pts',(-62.4869727360513,17.4541800510744,
-212.833687547544));
#197254=CARTESIAN_POINT('Ctrl Pts',(-62.471224815544,17.9533314585636,-212.920135097635));
#197255=CARTESIAN_POINT('Ctrl Pts',(-62.4548621630433,18.4478214139081,
-213.029285839066));
#197256=CARTESIAN_POINT('Ctrl Pts',(-62.4378715929549,18.937051788145,-213.164110067595));
#197257=CARTESIAN_POINT('Ctrl Pts',(-62.4313084944047,19.1260311539449,
-213.216189820905));
#197258=CARTESIAN_POINT('Ctrl Pts',(-62.4246524255105,19.3141920754881,
-213.272116519071));
#197259=CARTESIAN_POINT('Ctrl Pts',(-62.4179027766836,19.501499283875,-213.33205678481));
#197260=CARTESIAN_POINT('Ctrl Pts',(-62.4127593088451,19.6442339100696,
-213.377733358061));
#197261=CARTESIAN_POINT('Ctrl Pts',(-62.4075533326539,19.7866395914389,
-213.425870497305));
#197262=CARTESIAN_POINT('Ctrl Pts',(-62.4022963811676,19.9284129896732,
-213.476422874392));
#197263=CARTESIAN_POINT('Ctrl Pts',(-62.3923400029528,20.1969240416179,
-213.572166308062));
#197264=CARTESIAN_POINT('Ctrl Pts',(-62.3821761384096,20.4638252096883,
-213.676819486359));
#197265=CARTESIAN_POINT('Ctrl Pts',(-62.3718829556573,20.7269505848268,
-213.79019579402));
#197266=CARTESIAN_POINT('Ctrl Pts',(-62.3696094190237,20.7850691662223,
-213.815238115239));
#197267=CARTESIAN_POINT('Ctrl Pts',(-62.3673295817903,20.8430033470654,
-213.840705944902));
#197268=CARTESIAN_POINT('Ctrl Pts',(-62.3650443003751,20.9007294710183,
-213.866597158632));
#197269=CARTESIAN_POINT('Ctrl Pts',(-61.713103822739,20.0389506617614,-216.160137831685));
#197270=CARTESIAN_POINT('Ctrl Pts',(-61.7321110912357,20.3496658649069,
-216.247078381677));
#197271=CARTESIAN_POINT('Ctrl Pts',(-61.6907486315906,20.6657286340102,
-216.300532529068));
#197272=CARTESIAN_POINT('Ctrl Pts',(-61.9252463833055,20.1793980393595,
-215.812042320923));
#197273=CARTESIAN_POINT('Ctrl Pts',(-61.9373844794568,20.4413798330517,
-215.880084558757));
#197274=CARTESIAN_POINT('Ctrl Pts',(-61.9064790936528,20.7060595729952,
-215.92903923894));
#197275=CARTESIAN_POINT('Ctrl Pts',(-62.0850713031281,20.3222903717942,
-215.445236972404));
#197276=CARTESIAN_POINT('Ctrl Pts',(-62.0914940184093,20.5335632238432,
-215.496856996578));
#197277=CARTESIAN_POINT('Ctrl Pts',(-62.0699842872639,20.7460043187545,
-215.538658319552));
#197278=CARTESIAN_POINT('Ctrl Pts',(-62.3043696537349,20.611682425576,-214.675676922536));
#197279=CARTESIAN_POINT('Ctrl Pts',(-62.3035607512221,20.7183157084577,
-214.699282243487));
#197280=CARTESIAN_POINT('Ctrl Pts',(-62.2967890390184,20.824939865421,-214.721940813782));
#197281=CARTESIAN_POINT('Ctrl Pts',(-62.3625010497726,20.7591101230298,
-214.269920324208));
#197282=CARTESIAN_POINT('Ctrl Pts',(-62.36063660277,20.8116268449194,-214.281171503343));
#197283=CARTESIAN_POINT('Ctrl Pts',(-62.3587717320579,20.8641365401031,
-214.2924597236));
#197284=CARTESIAN_POINT('Ctrl Pts',(-62.3650472056256,20.9007985863674,
-213.86644416092));
#197285=CARTESIAN_POINT('Ctrl Pts',(-62.3650472056256,20.9007985863674,
-213.86644416092));
#197286=CARTESIAN_POINT('Ctrl Pts',(-62.3650472056256,20.9007985863674,
-213.86644416092));
#197287=CARTESIAN_POINT('',(-61.6907486315871,20.6657286340098,-216.300532529074));
#197288=CARTESIAN_POINT('Origin',(-59.1013738165116,20.5826972454933,-214.78783829177));
#197289=CARTESIAN_POINT('Ctrl Pts',(-61.6907486315871,20.66572863401,-216.300532529074));
#197290=CARTESIAN_POINT('Ctrl Pts',(-61.7776458854704,20.6819741262679,
-216.150893248708));
#197291=CARTESIAN_POINT('Ctrl Pts',(-61.8667307948559,20.7002117978156,
-215.979723760535));
#197292=CARTESIAN_POINT('Ctrl Pts',(-61.9936363408029,20.7302399848448,
-215.687912889814));
#197293=CARTESIAN_POINT('Ctrl Pts',(-62.034784576062,20.7406936090083,-215.584820111112));
#197294=CARTESIAN_POINT('Ctrl Pts',(-62.0932494709526,20.7569920861929,
-215.421377131638));
#197295=CARTESIAN_POINT('Ctrl Pts',(-62.121664872513,20.7652957504502,-215.337458316968));
#197296=CARTESIAN_POINT('Ctrl Pts',(-62.1530272418572,20.7752422475622,
-215.235736062925));
#197297=CARTESIAN_POINT('Ctrl Pts',(-62.166045121126,20.7795592499655,-215.191329117645));
#197298=CARTESIAN_POINT('Ctrl Pts',(-62.1746252349796,20.7824491595449,
-215.161544906292));
#197299=CARTESIAN_POINT('Ctrl Pts',(-62.179454484566,20.7841046857491,-215.144446131259));
#197300=CARTESIAN_POINT('Ctrl Pts',(-62.2982778852125,20.8254239556915,
-214.716977329717));
#197301=CARTESIAN_POINT('Ctrl Pts',(-62.3588454290314,20.8638984988155,
-214.288283562016));
#197302=CARTESIAN_POINT('Ctrl Pts',(-62.365046045184,20.9007916780701,-213.866523136266));
#197303=CARTESIAN_POINT('Ctrl Pts',(-61.6377935655245,19.9815886122025,
-216.280755810351));
#197304=CARTESIAN_POINT('Ctrl Pts',(-61.6055583132384,20.2909606839632,
-216.465410556112));
#197305=CARTESIAN_POINT('Ctrl Pts',(-61.499388181455,20.6071190721679,-216.605481304297));
#197306=CARTESIAN_POINT('Ctrl Pts',(-61.6652027952659,20.0090334790696,
-216.239468240032));
#197307=CARTESIAN_POINT('Ctrl Pts',(-61.6507949119044,20.3194192931518,
-216.390568004079));
#197308=CARTESIAN_POINT('Ctrl Pts',(-61.5691908701262,20.6359350302665,
-216.502281627839));
#197309=CARTESIAN_POINT('Ctrl Pts',(-61.6926044944854,20.0301302514809,
-216.195652941672));
#197310=CARTESIAN_POINT('Ctrl Pts',(-61.6967727624885,20.3410293418827,
-216.311297779654));
#197311=CARTESIAN_POINT('Ctrl Pts',(-61.6387815649118,20.6575029215266,
-216.391600777262));
#197312=CARTESIAN_POINT('Ctrl Pts',(-61.7199387591116,20.0421410735216,
-216.14839440092));
#197313=CARTESIAN_POINT('Ctrl Pts',(-61.7438559996858,20.35282222204,-216.225852774313));
#197314=CARTESIAN_POINT('Ctrl Pts',(-61.7080768938385,20.6687713493049,
-216.270467388274));
#197315=CARTESIAN_POINT('',(-61.516838435879,20.6141575017552,-216.579518431174));
#197316=CARTESIAN_POINT('',(-61.6446456814072,19.9883159925442,-216.270380726959));
#197317=CARTESIAN_POINT('Origin',(-59.0326817073425,20.5344053061246,-214.899457439615));
#197318=CARTESIAN_POINT('Ctrl Pts',(-61.6446456814073,19.9883159925441,
-216.270380726959));
#197319=CARTESIAN_POINT('Ctrl Pts',(-61.6589899513843,20.0021161049564,
-216.24854827085));
#197320=CARTESIAN_POINT('Ctrl Pts',(-61.6733754040443,20.0141614250312,
-216.225936040046));
#197321=CARTESIAN_POINT('Ctrl Pts',(-61.6878163893671,20.0240270532932,
-216.202356326574));
#197322=CARTESIAN_POINT('Ctrl Pts',(-61.6962257996766,20.0297720986736,
-216.18862516619));
#197323=CARTESIAN_POINT('Ctrl Pts',(-61.7046540329176,20.034777214409,-216.174565637937));
#197324=CARTESIAN_POINT('Ctrl Pts',(-61.7131038227345,20.0389506617863,
-216.160137831703));
#197325=CARTESIAN_POINT('Ctrl Pts',(-61.516838435851,20.614157501844,-216.579518431211));
#197326=CARTESIAN_POINT('Ctrl Pts',(-61.5771479675576,20.6380049970577,
-216.489212055522));
#197327=CARTESIAN_POINT('Ctrl Pts',(-61.6351552038294,20.6553354111624,
-216.396265812028));
#197328=CARTESIAN_POINT('Ctrl Pts',(-61.6907486315871,20.66572863401,-216.300532529074));
#197329=CARTESIAN_POINT('Ctrl Pts',(-61.235107328202,28.3894013135675,-216.583947161644));
#197330=CARTESIAN_POINT('Ctrl Pts',(-62.0737483304577,28.4205138141115,
-215.350417820742));
#197331=CARTESIAN_POINT('Ctrl Pts',(-62.0998335778874,28.4197995297673,
-213.858707258037));
#197332=CARTESIAN_POINT('Ctrl Pts',(-61.3394317178759,25.782537982878,-216.582300349965));
#197333=CARTESIAN_POINT('Ctrl Pts',(-62.1750190192476,25.8120069501401,
-215.350359724707));
#197334=CARTESIAN_POINT('Ctrl Pts',(-62.2010617731482,25.8108994796242,
-213.861712475948));
#197335=CARTESIAN_POINT('Ctrl Pts',(-61.4338508567495,23.1751069333097,
-216.580828347939));
#197336=CARTESIAN_POINT('Ctrl Pts',(-62.2667395005803,23.2024779691083,
-215.350312870121));
#197337=CARTESIAN_POINT('Ctrl Pts',(-62.2927210668524,23.2015642400677,
-213.864398964149));
#197338=CARTESIAN_POINT('Ctrl Pts',(-61.5183514407949,20.5675003107738,
-216.579494546858));
#197339=CARTESIAN_POINT('Ctrl Pts',(-62.3488810204336,20.5925259779214,
-215.350234406272));
#197340=CARTESIAN_POINT('Ctrl Pts',(-62.3748047396227,20.5920154834281,
-213.866720382044));
#197341=CARTESIAN_POINT('',(-62.099833577893,28.4197995297552,-213.858707258032));
#197342=CARTESIAN_POINT('Origin',(1003.25098428815,-12.9621320438613,-174.780968069139));
#197343=CARTESIAN_POINT('',(-61.2351073280272,28.3894013125172,-216.583947161963));
#197344=CARTESIAN_POINT('Origin',(-57.1043579940171,28.2258690560256,-213.771445225846));
#197345=CARTESIAN_POINT('Origin',(967.060476622167,-12.7722155952905,-232.807288933329));
#197346=CARTESIAN_POINT('Ctrl Pts',(-61.0271214515746,29.6036708476845,
-216.705447812142));
#197347=CARTESIAN_POINT('Ctrl Pts',(-62.0328771597131,29.432010466984,-215.416461273176));
#197348=CARTESIAN_POINT('Ctrl Pts',(-62.0715435503805,29.1708764678268,
-213.793867031503));
#197349=CARTESIAN_POINT('Ctrl Pts',(-61.0627413621019,29.4095488042208,
-216.699316444474));
#197350=CARTESIAN_POINT('Ctrl Pts',(-62.0394002938428,29.2676078599798,
-215.416801443606));
#197351=CARTESIAN_POINT('Ctrl Pts',(-62.0761251487726,29.0460828494865,
-213.81396536355));
#197352=CARTESIAN_POINT('Ctrl Pts',(-61.0959751735216,29.2176086084485,
-216.688979075795));
#197353=CARTESIAN_POINT('Ctrl Pts',(-62.045900321156,29.1044853538962,-215.413559895334));
#197354=CARTESIAN_POINT('Ctrl Pts',(-62.0807624949799,28.9211132693028,
-213.830014605952));
#197355=CARTESIAN_POINT('Ctrl Pts',(-61.1660917025604,28.812533486502,-216.649425062049));
#197356=CARTESIAN_POINT('Ctrl Pts',(-62.059522361877,28.7670896367546,-215.392285581265));
#197357=CARTESIAN_POINT('Ctrl Pts',(-62.0901763780839,28.6707891288636,
-213.852481398947));
#197358=CARTESIAN_POINT('Ctrl Pts',(-61.2033761954606,28.5977249793428,
-216.618438059186));
#197359=CARTESIAN_POINT('Ctrl Pts',(-62.0666989989455,28.5919001092215,
-215.373070477725));
#197360=CARTESIAN_POINT('Ctrl Pts',(-62.094959380688,28.5454196012504,-213.858562559592));
#197361=CARTESIAN_POINT('Ctrl Pts',(-61.2351073279008,28.3894013132804,
-216.583947162106));
#197362=CARTESIAN_POINT('Ctrl Pts',(-62.0737483304886,28.4205138133222,
-215.350417821044));
#197363=CARTESIAN_POINT('Ctrl Pts',(-62.0998335779475,28.4197995283645,
-213.858707258032));
#197364=CARTESIAN_POINT('',(-61.0271214515743,29.6036708476852,-216.705447812142));
#197365=CARTESIAN_POINT('',(-62.0715435503803,29.170876467827,-213.793867031503));
#197366=CARTESIAN_POINT('Origin',(-57.0762058255522,28.9734268472959,-213.706604999317));
#197367=CARTESIAN_POINT('Ctrl Pts',(-61.0271214515743,29.6036708476852,
-216.705447812142));
#197368=CARTESIAN_POINT('Ctrl Pts',(-61.0627413621019,29.4095488042208,
-216.699316444474));
#197369=CARTESIAN_POINT('Ctrl Pts',(-61.0959751735216,29.2176086084485,
-216.688979075795));
#197370=CARTESIAN_POINT('Ctrl Pts',(-61.1660917025604,28.812533486502,-216.649425062049));
#197371=CARTESIAN_POINT('Ctrl Pts',(-61.2033761954606,28.5977249793428,
-216.618438059186));
#197372=CARTESIAN_POINT('Ctrl Pts',(-61.2351073279234,28.3894013132814,
-216.583947162069));
#197373=CARTESIAN_POINT('Ctrl Pts',(-62.0998335778935,28.4197995297553,
-213.858707258032));
#197374=CARTESIAN_POINT('Ctrl Pts',(-62.094949600635,28.5456716573278,-213.858562269211));
#197375=CARTESIAN_POINT('Ctrl Pts',(-62.0901675429821,28.6710240626564,
-213.85246031345));
#197376=CARTESIAN_POINT('Ctrl Pts',(-62.0854694365319,28.7959511990832,
-213.841248002449));
#197377=CARTESIAN_POINT('Ctrl Pts',(-62.0807548271223,28.9213171649583,
-213.829996306153));
#197378=CARTESIAN_POINT('Ctrl Pts',(-62.0761182844883,29.0462698189252,
-213.813935251642));
#197379=CARTESIAN_POINT('Ctrl Pts',(-62.0715435503805,29.1708764678268,
-213.793867031503));
#197380=CARTESIAN_POINT('Ctrl Pts',(-62.0722753176769,29.1511380815083,
-213.795657702395));
#197381=CARTESIAN_POINT('Ctrl Pts',(-62.0340745338293,29.4127097517032,
-215.416670061812));
#197382=CARTESIAN_POINT('Ctrl Pts',(-61.030221352118,29.5865570284964,-216.704939048052));
#197383=CARTESIAN_POINT('Ctrl Pts',(-62.0620320829829,29.4340729912048,
-213.769970033114));
#197384=CARTESIAN_POINT('Ctrl Pts',(-62.0171383824692,29.6895867289819,
-215.413872853516));
#197385=CARTESIAN_POINT('Ctrl Pts',(-60.9858182348534,29.8316477735471,
-216.712544680079));
#197386=CARTESIAN_POINT('Ctrl Pts',(-62.0412495434026,29.7158438578209,
-213.745237314573));
#197387=CARTESIAN_POINT('Ctrl Pts',(-61.9892647258148,29.9729902357752,
-215.414291487854));
#197388=CARTESIAN_POINT('Ctrl Pts',(-60.9270407929623,30.0877775086874,
-216.723516257042));
#197389=CARTESIAN_POINT('Ctrl Pts',(-61.9794688757743,30.2707145068829,
-213.698186104697));
#197390=CARTESIAN_POINT('Ctrl Pts',(-61.9159025865061,30.5129372076058,
-215.407258353661));
#197391=CARTESIAN_POINT('Ctrl Pts',(-60.8096093037007,30.5582220616567,
-216.733419187575));
#197392=CARTESIAN_POINT('Ctrl Pts',(-61.938926317498,30.5439708220038,-213.676343773128));
#197393=CARTESIAN_POINT('Ctrl Pts',(-61.8707327962001,30.775264549444,-215.402898488695));
#197394=CARTESIAN_POINT('Ctrl Pts',(-60.747409441142,30.7826838238242,-216.736387709467));
#197395=CARTESIAN_POINT('Ctrl Pts',(-61.837636032495,31.0884065478961,-213.634598566576));
#197396=CARTESIAN_POINT('Ctrl Pts',(-61.7592484376381,31.3083441263931,
-215.399426388486));
#197397=CARTESIAN_POINT('Ctrl Pts',(-60.5980527039995,31.2446203390114,
-216.747650397627));
#197398=CARTESIAN_POINT('Ctrl Pts',(-61.7769096374044,31.3595164244479,
-213.614424841566));
#197399=CARTESIAN_POINT('Ctrl Pts',(-61.6932454520362,31.5755832712924,
-215.398384202842));
#197400=CARTESIAN_POINT('Ctrl Pts',(-60.5138367274016,31.4762486370728,
-216.753526488075));
#197401=CARTESIAN_POINT('Ctrl Pts',(-61.6347983988434,31.899450706002,-213.575433990368));
#197402=CARTESIAN_POINT('Ctrl Pts',(-61.5426774850893,32.1020267212171,
-215.393731279353));
#197403=CARTESIAN_POINT('Ctrl Pts',(-60.3359793889894,31.9259601738048,
-216.76111570899));
#197404=CARTESIAN_POINT('Ctrl Pts',(-61.5531858863137,32.1688271147634,
-213.556786982595));
#197405=CARTESIAN_POINT('Ctrl Pts',(-61.458472596998,32.3604331023391,-215.389897348667));
#197406=CARTESIAN_POINT('Ctrl Pts',(-60.2437451595173,32.1426522013982,
-216.762577010636));
#197407=CARTESIAN_POINT('Ctrl Pts',(-61.4159587545849,32.5674954665022,
-213.530743809019));
#197408=CARTESIAN_POINT('Ctrl Pts',(-61.3177400835575,32.7449412296482,
-215.385939876134));
#197409=CARTESIAN_POINT('Ctrl Pts',(-60.0928857706128,32.4655283166213,
-216.766110440268));
#197410=CARTESIAN_POINT('Ctrl Pts',(-61.3676767622843,32.6997212687758,
-213.522342385503));
#197411=CARTESIAN_POINT('Ctrl Pts',(-61.2682838922593,32.872909821302,-215.384883950169));
#197412=CARTESIAN_POINT('Ctrl Pts',(-60.0403931405282,32.572987171916,-216.767475838973));
#197413=CARTESIAN_POINT('Ctrl Pts',(-61.2664764445886,32.9616854374991,
-213.505934868461));
#197414=CARTESIAN_POINT('Ctrl Pts',(-61.16400924397,33.1287467154492,-215.383607108532));
#197415=CARTESIAN_POINT('Ctrl Pts',(-59.9294247387107,32.7889935283979,
-216.770953998618));
#197416=CARTESIAN_POINT('Ctrl Pts',(-61.2135447672718,33.091483145622,-213.497857516746));
#197417=CARTESIAN_POINT('Ctrl Pts',(-61.108560223271,33.2579834247729,-215.383794009871));
#197418=CARTESIAN_POINT('Ctrl Pts',(-59.8692253143189,32.8995596733306,
-216.773542513475));
#197419=CARTESIAN_POINT('Ctrl Pts',(-61.0478125873863,33.4773667643361,
-213.47408238772));
#197420=CARTESIAN_POINT('Ctrl Pts',(-60.939655477163,33.6324724880252,-215.380343496444));
#197421=CARTESIAN_POINT('Ctrl Pts',(-59.6963317184513,33.2127149517822,
-216.776352933466));
#197422=CARTESIAN_POINT('Ctrl Pts',(-60.9280440899178,33.7300206143803,
-213.459385328777));
#197423=CARTESIAN_POINT('Ctrl Pts',(-60.8222945421723,33.8691785847138,
-215.375378456549));
#197424=CARTESIAN_POINT('Ctrl Pts',(-59.5857444814115,33.4045989682938,
-216.77471811873));
#197425=CARTESIAN_POINT('Ctrl Pts',(-60.7344672841107,34.1022007074626,
-213.439632708162));
#197426=CARTESIAN_POINT('Ctrl Pts',(-60.6302881857557,34.2248170372617,
-215.371749277836));
#197427=CARTESIAN_POINT('Ctrl Pts',(-59.4018730546303,33.6971462711828,
-216.77599109459));
#197428=CARTESIAN_POINT('Ctrl Pts',(-60.6676250274419,34.2251152634526,
-213.433348725261));
#197429=CARTESIAN_POINT('Ctrl Pts',(-60.5629875662736,34.3444216969835,
-215.371371877201));
#197430=CARTESIAN_POINT('Ctrl Pts',(-59.3362053418023,33.7967893027105,
-216.777264657507));
#197431=CARTESIAN_POINT('Ctrl Pts',(-60.5293279502117,34.4685916588927,
-213.420959244589));
#197432=CARTESIAN_POINT('Ctrl Pts',(-60.4230895229254,34.5826588364461,
-215.370625427342));
#197433=CARTESIAN_POINT('Ctrl Pts',(-59.1998648193908,33.9959954562112,
-216.779653928204));
#197434=CARTESIAN_POINT('Ctrl Pts',(-60.4578772193282,34.5891494281844,
-213.414818675441));
#197435=CARTESIAN_POINT('Ctrl Pts',(-60.3505501995765,34.7010803776926,
-215.370127825967));
#197436=CARTESIAN_POINT('Ctrl Pts',(-59.1294078669496,34.095271216951,-216.780624801763));
#197437=CARTESIAN_POINT('Ctrl Pts',(-60.3471832550081,34.768251943839,-213.406087731132));
#197438=CARTESIAN_POINT('Ctrl Pts',(-60.2427301457655,34.8702456283936,
-215.36729429493));
#197439=CARTESIAN_POINT('Ctrl Pts',(-59.0316233263315,34.2327858157498,
-216.779602213422));
#197440=CARTESIAN_POINT('Ctrl Pts',(-60.3096963328013,34.8276667088433,
-213.403282057557));
#197441=CARTESIAN_POINT('Ctrl Pts',(-60.2073956626117,34.9245822814321,
-215.365838464165));
#197442=CARTESIAN_POINT('Ctrl Pts',(-59.0013384113356,34.2757719021763,
-216.778662998653));
#197443=CARTESIAN_POINT('Ctrl Pts',(-60.2335269589641,34.945932810334,-213.397980978197));
#197444=CARTESIAN_POINT('Ctrl Pts',(-60.1350035456452,35.0338818623324,
-215.363515549055));
#197445=CARTESIAN_POINT('Ctrl Pts',(-58.9384240938482,34.3630029801402,
-216.777376929373));
#197446=CARTESIAN_POINT('Ctrl Pts',(-60.1948462340149,35.0047819102021,
-213.395467604637));
#197447=CARTESIAN_POINT('Ctrl Pts',(-60.098003280493,35.0887243625003,-215.362587120194));
#197448=CARTESIAN_POINT('Ctrl Pts',(-58.9059517617724,34.4070761172112,
-216.776964413499));
#197449=CARTESIAN_POINT('Ctrl Pts',(-60.0732701737662,35.1860378427238,
-213.388026309707));
#197450=CARTESIAN_POINT('Ctrl Pts',(-59.9811145129592,35.2587196749933,
-215.360184867158));
#197451=CARTESIAN_POINT('Ctrl Pts',(-58.80275485317,34.5444172631871,-216.776133900962));
#197452=CARTESIAN_POINT('Ctrl Pts',(-59.9883366029424,35.3074524979782,
-213.38343869169));
#197453=CARTESIAN_POINT('Ctrl Pts',(-59.8985377265825,35.374186215073,-215.359237777425));
#197454=CARTESIAN_POINT('Ctrl Pts',(-58.7288550087989,34.6388163213973,
-216.776220299507));
#197455=CARTESIAN_POINT('Ctrl Pts',(-59.9016315893045,35.4263976750195,
-213.37931837001));
#197456=CARTESIAN_POINT('Ctrl Pts',(-59.8155211638331,35.4858202289832,
-215.357783188893));
#197457=CARTESIAN_POINT('Ctrl Pts',(-58.6567202300399,34.7293397325179,
-216.775594469212));
#197458=CARTESIAN_POINT('',(-58.6665914736623,34.7169872964315,-216.775646223556));
#197459=CARTESIAN_POINT('',(-59.9134443065973,35.4101621769153,-213.379883144535));
#197460=CARTESIAN_POINT('Origin',(-55.8698139418538,32.470529749032,-213.292621112349));
#197461=CARTESIAN_POINT('Ctrl Pts',(-58.6665914736623,34.7169872964315,
-216.775646223557));
#197462=CARTESIAN_POINT('Ctrl Pts',(-58.68891411473,34.6889262212036,-216.775820369084));
#197463=CARTESIAN_POINT('Ctrl Pts',(-58.7113614970553,34.6605567043895,
-216.775932488694));
#197464=CARTESIAN_POINT('Ctrl Pts',(-58.7337888387604,34.6319802064989,
-216.776022661718));
#197465=CARTESIAN_POINT('Ctrl Pts',(-58.7552226821379,34.6046696055318,
-216.776108840209));
#197466=CARTESIAN_POINT('Ctrl Pts',(-58.7766384767105,34.5771695739528,
-216.77617497345));
#197467=CARTESIAN_POINT('Ctrl Pts',(-58.7978896199004,34.5496113066691,
-216.776256046869));
#197468=CARTESIAN_POINT('Ctrl Pts',(-58.818445685349,34.5229544091615,-216.776334468557));
#197469=CARTESIAN_POINT('Ctrl Pts',(-58.8388478025107,34.4962428910996,
-216.776426869088));
#197470=CARTESIAN_POINT('Ctrl Pts',(-58.8589413273301,34.4696399854441,
-216.77656491206));
#197471=CARTESIAN_POINT('Ctrl Pts',(-58.8635229652065,34.4635741069449,
-216.776596388017));
#197472=CARTESIAN_POINT('Ctrl Pts',(-58.8680884632319,34.4575140665269,
-216.776630236976));
#197473=CARTESIAN_POINT('Ctrl Pts',(-58.8726358156898,34.4514621421053,
-216.776666834302));
#197474=CARTESIAN_POINT('Ctrl Pts',(-58.8993737676191,34.4158774660199,
-216.776882022713));
#197475=CARTESIAN_POINT('Ctrl Pts',(-58.9255521608924,34.3804868678643,
-216.777189950846));
#197476=CARTESIAN_POINT('Ctrl Pts',(-58.951098376918,34.3453668781434,-216.77763514187));
#197477=CARTESIAN_POINT('Ctrl Pts',(-58.9574067387464,34.3366943764177,
-216.77774507698));
#197478=CARTESIAN_POINT('Ctrl Pts',(-58.9636764242332,34.328038594042,-216.777863382238));
#197479=CARTESIAN_POINT('Ctrl Pts',(-58.9699061024711,34.3194010903381,
-216.777990728079));
#197480=CARTESIAN_POINT('Ctrl Pts',(-58.982028851275,34.3025927924298,-216.778238538894));
#197481=CARTESIAN_POINT('Ctrl Pts',(-58.9939827439098,34.2858621186605,
-216.778530335959));
#197482=CARTESIAN_POINT('Ctrl Pts',(-59.005958458314,34.2690364739751,-216.778814923197));
#197483=CARTESIAN_POINT('Ctrl Pts',(-59.0196242261173,34.2498363372941,
-216.77913967235));
#197484=CARTESIAN_POINT('Ctrl Pts',(-59.033317885381,34.2305136307765,-216.779455033138));
#197485=CARTESIAN_POINT('Ctrl Pts',(-59.047339665745,34.2107575527891,-216.779684931869));
#197486=CARTESIAN_POINT('Ctrl Pts',(-59.0529154730659,34.2029014830594,
-216.779776351859));
#197487=CARTESIAN_POINT('Ctrl Pts',(-59.0585434000204,34.1949763905612,
-216.779854257892));
#197488=CARTESIAN_POINT('Ctrl Pts',(-59.0642433014168,34.1869605874501,
-216.77991386644));
#197489=CARTESIAN_POINT('Ctrl Pts',(-59.0832958083669,34.1601669407071,
-216.780113114147));
#197490=CARTESIAN_POINT('Ctrl Pts',(-59.102779151996,34.1327728264599,-216.78017120186));
#197491=CARTESIAN_POINT('Ctrl Pts',(-59.1225303078593,34.1048954334528,
-216.780123799295));
#197492=CARTESIAN_POINT('Ctrl Pts',(-59.1415464599063,34.0780554475924,
-216.780078160731));
#197493=CARTESIAN_POINT('Ctrl Pts',(-59.1608108973337,34.0507670685685,
-216.779934737065));
#197494=CARTESIAN_POINT('Ctrl Pts',(-59.1801602203819,34.0231784383873,
-216.779725362211));
#197495=CARTESIAN_POINT('Ctrl Pts',(-59.1988920056233,33.9964703052722,
-216.7795226696));
#197496=CARTESIAN_POINT('Ctrl Pts',(-59.2177033230583,33.9694806014766,
-216.779258168316));
#197497=CARTESIAN_POINT('Ctrl Pts',(-59.2364287245647,33.9423895910669,
-216.778960740555));
#197498=CARTESIAN_POINT('Ctrl Pts',(-59.2470111671479,33.9270794220388,
-216.778792652719));
#197499=CARTESIAN_POINT('Ctrl Pts',(-59.2575658550351,33.9117377574434,
-216.77861404878));
#197500=CARTESIAN_POINT('Ctrl Pts',(-59.2680604524456,33.8964041258495,
-216.77843014182));
#197501=CARTESIAN_POINT('Ctrl Pts',(-59.2998335102196,33.8499805858637,
-216.777873351861));
#197502=CARTESIAN_POINT('Ctrl Pts',(-59.3310391548654,33.8035995166105,
-216.777299416541));
#197503=CARTESIAN_POINT('Ctrl Pts',(-59.3615252914712,33.7573947953899,
-216.776802311717));
#197504=CARTESIAN_POINT('Ctrl Pts',(-59.3795446970365,33.7300846241643,
-216.776508488542));
#197505=CARTESIAN_POINT('Ctrl Pts',(-59.3973125982864,33.7028372954064,
-216.776241507053));
#197506=CARTESIAN_POINT('Ctrl Pts',(-59.4147969421915,33.675688640263,-216.776020773));
#197507=CARTESIAN_POINT('Ctrl Pts',(-59.4311986392249,33.6502210551514,
-216.775813707006));
#197508=CARTESIAN_POINT('Ctrl Pts',(-59.4473498031528,33.6248420237438,
-216.775647338403));
#197509=CARTESIAN_POINT('Ctrl Pts',(-59.4631890571003,33.5996410081924,
-216.775537686686));
#197510=CARTESIAN_POINT('Ctrl Pts',(-59.4834075864701,33.5674723546204,
-216.775397718195));
#197511=CARTESIAN_POINT('Ctrl Pts',(-59.5033327223937,33.5352944108817,
-216.775325313048));
#197512=CARTESIAN_POINT('Ctrl Pts',(-59.5230054610261,33.5031054017674,
-216.775293584259));
#197513=CARTESIAN_POINT('Ctrl Pts',(-59.5438616272312,33.4689800399348,
-216.775259946801));
#197514=CARTESIAN_POINT('Ctrl Pts',(-59.5644345215814,33.4348418935606,
-216.775272026729));
#197515=CARTESIAN_POINT('Ctrl Pts',(-59.5847982540677,33.4006346487011,
-216.775297787095));
#197516=CARTESIAN_POINT('Ctrl Pts',(-59.607298462236,33.3628385260738,-216.77532625013));
#197517=CARTESIAN_POINT('Ctrl Pts',(-59.6295437657375,33.3249579524366,
-216.775371414775));
#197518=CARTESIAN_POINT('Ctrl Pts',(-59.6516573645725,33.2868558376646,
-216.77539006563));
#197519=CARTESIAN_POINT('Ctrl Pts',(-59.6753100926277,33.2461017765208,
-216.775410014604));
#197520=CARTESIAN_POINT('Ctrl Pts',(-59.6988130119915,33.2050936700177,
-216.775399630573));
#197521=CARTESIAN_POINT('Ctrl Pts',(-59.72233137803,33.1636031936252,-216.775306032011));
#197522=CARTESIAN_POINT('Ctrl Pts',(-59.7482947804579,33.1177992490086,
-216.775202702675));
#197523=CARTESIAN_POINT('Ctrl Pts',(-59.7742785554707,33.0714067381163,
-216.774997956963));
#197524=CARTESIAN_POINT('Ctrl Pts',(-59.8005028618899,33.0240569092213,
-216.77462064611));
#197525=CARTESIAN_POINT('Ctrl Pts',(-59.8042035822122,33.0173749985065,
-216.774567400777));
#197526=CARTESIAN_POINT('Ctrl Pts',(-59.807909064699,33.0106739440499,-216.774510718933));
#197527=CARTESIAN_POINT('Ctrl Pts',(-59.811619893991,33.003952637821,-216.774450400634));
#197528=CARTESIAN_POINT('Ctrl Pts',(-59.833977195716,32.9634575733704,-216.774086990108));
#197529=CARTESIAN_POINT('Ctrl Pts',(-59.8567504991726,32.9220364044774,
-216.773475005287));
#197530=CARTESIAN_POINT('Ctrl Pts',(-59.8794666670023,32.8801912149089,
-216.772760470042));
#197531=CARTESIAN_POINT('Ctrl Pts',(-59.8830729275937,32.8735481640557,
-216.772647035403));
#197532=CARTESIAN_POINT('Ctrl Pts',(-59.8866777641604,32.8668945322141,
-216.772531016234));
#197533=CARTESIAN_POINT('Ctrl Pts',(-59.8902793094997,32.8602324399893,
-216.772412996774));
#197534=CARTESIAN_POINT('Ctrl Pts',(-59.9147369266354,32.8149910545269,
-216.771611542259));
#197535=CARTESIAN_POINT('Ctrl Pts',(-59.9390402310768,32.7693558218133,
-216.770717842538));
#197536=CARTESIAN_POINT('Ctrl Pts',(-59.9626984288671,32.723963924159,-216.769914861649));
#197537=CARTESIAN_POINT('Ctrl Pts',(-59.9701796860638,32.7096099795344,
-216.769660940931));
#197538=CARTESIAN_POINT('Ctrl Pts',(-59.9775966733613,32.695280690391,-216.769416091802));
#197539=CARTESIAN_POINT('Ctrl Pts',(-59.9849345594905,32.6809970052011,
-216.769186099808));
#197540=CARTESIAN_POINT('Ctrl Pts',(-60.019976886076,32.6127847772576,-216.768087765163));
#197541=CARTESIAN_POINT('Ctrl Pts',(-60.0538230741447,32.5447837722497,
-216.767138487128));
#197542=CARTESIAN_POINT('Ctrl Pts',(-60.0866775699529,32.4768286872757,
-216.76629138433));
#197543=CARTESIAN_POINT('Ctrl Pts',(-60.1058431236745,32.4371873292306,
-216.765797229914));
#197544=CARTESIAN_POINT('Ctrl Pts',(-60.124670852594,32.3975605116188,-216.765337845025));
#197545=CARTESIAN_POINT('Ctrl Pts',(-60.143197685769,32.3579083385831,-216.7649039233));
#197546=CARTESIAN_POINT('Ctrl Pts',(-60.1789309577007,32.2814299750988,
-216.764067005147));
#197547=CARTESIAN_POINT('Ctrl Pts',(-60.2136112483601,32.2046803722813,
-216.76334298333));
#197548=CARTESIAN_POINT('Ctrl Pts',(-60.2474734670841,32.1274737896909,
-216.762587094311));
#197549=CARTESIAN_POINT('Ctrl Pts',(-60.2748213223657,32.0651200950118,
-216.761976622101));
#197550=CARTESIAN_POINT('Ctrl Pts',(-60.3016350479361,32.0024671247304,
-216.761345364431));
#197551=CARTESIAN_POINT('Ctrl Pts',(-60.3280143860689,31.9394105099008,
-216.760617063764));
#197552=CARTESIAN_POINT('Ctrl Pts',(-60.3609034404128,31.8607932064096,
-216.759709037941));
#197553=CARTESIAN_POINT('Ctrl Pts',(-60.3931182697554,31.7815511857832,
-216.758650164247));
#197554=CARTESIAN_POINT('Ctrl Pts',(-60.424932988713,31.7011072820459,-216.757292652615));
#197555=CARTESIAN_POINT('Ctrl Pts',(-60.455870616552,31.6228811138668,-216.755972565842));
#197556=CARTESIAN_POINT('Ctrl Pts',(-60.4862672508109,31.5438480239397,
-216.754400559193));
#197557=CARTESIAN_POINT('Ctrl Pts',(-60.5158738472255,31.4643026910919,
-216.752674579628));
#197558=CARTESIAN_POINT('Ctrl Pts',(-60.5449572973019,31.3861629183096,
-216.750979097992));
#197559=CARTESIAN_POINT('Ctrl Pts',(-60.5732787670902,31.3075277945667,
-216.749135036746));
#197560=CARTESIAN_POINT('Ctrl Pts',(-60.6006489223964,31.2286922513233,
-216.747235241906));
#197561=CARTESIAN_POINT('Ctrl Pts',(-60.6255053702117,31.1570970577745,
-216.745509926476));
#197562=CARTESIAN_POINT('Ctrl Pts',(-60.6495779600038,31.0853362075051,
-216.743738644629));
#197563=CARTESIAN_POINT('Ctrl Pts',(-60.6727550228659,31.0136526708201,
-216.741990938608));
#197564=CARTESIAN_POINT('Ctrl Pts',(-60.6750801349789,31.0064614119259,
-216.741815609557));
#197565=CARTESIAN_POINT('Ctrl Pts',(-60.6773925737596,30.9992764828879,
-216.741642861846));
#197566=CARTESIAN_POINT('Ctrl Pts',(-60.6796927546667,30.9920971874804,
-216.741472557014));
#197567=CARTESIAN_POINT('Ctrl Pts',(-60.7005717089029,30.926930060931,-216.739926684351));
#197568=CARTESIAN_POINT('Ctrl Pts',(-60.7204435599204,30.8622313445984,
-216.738582089287));
#197569=CARTESIAN_POINT('Ctrl Pts',(-60.739541788745,30.7977002662527,-216.73733521714));
#197570=CARTESIAN_POINT('Ctrl Pts',(-60.7595264935239,30.7301738709184,
-216.736030469355));
#197571=CARTESIAN_POINT('Ctrl Pts',(-60.7786648263104,30.6628289056779,
-216.734832726975));
#197572=CARTESIAN_POINT('Ctrl Pts',(-60.7971797973658,30.595283631511,-216.733623335648));
#197573=CARTESIAN_POINT('Ctrl Pts',(-60.8147795981204,30.5310770300697,
-216.73247372292));
#197574=CARTESIAN_POINT('Ctrl Pts',(-60.8318162353816,30.4666873557856,
-216.731313584368));
#197575=CARTESIAN_POINT('Ctrl Pts',(-60.8484370244407,30.4017854464693,
-216.730041005063));
#197576=CARTESIAN_POINT('Ctrl Pts',(-60.8549049587336,30.3765290471826,
-216.729545784331));
#197577=CARTESIAN_POINT('Ctrl Pts',(-60.8613094191775,30.3511952223564,
-216.729033536068));
#197578=CARTESIAN_POINT('Ctrl Pts',(-60.8676570670374,30.325765519308,-216.728498254352));
#197579=CARTESIAN_POINT('Ctrl Pts',(-60.8843043256454,30.2590739112798,
-216.727094431495));
#197580=CARTESIAN_POINT('Ctrl Pts',(-60.9009917813059,30.1909296264927,
-216.725222439664));
#197581=CARTESIAN_POINT('Ctrl Pts',(-60.9173043394106,30.1220021183896,
-216.723087543031));
#197582=CARTESIAN_POINT('Ctrl Pts',(-60.9255062185316,30.0873456846193,
-216.722014126832));
#197583=CARTESIAN_POINT('Ctrl Pts',(-60.9336138051568,30.0524920317603,
-216.720874247456));
#197584=CARTESIAN_POINT('Ctrl Pts',(-60.9415777804195,30.0175296824247,
-216.71969399568));
#197585=CARTESIAN_POINT('Ctrl Pts',(-60.9572804382746,29.9485940326622,
-216.717366880237));
#197586=CARTESIAN_POINT('Ctrl Pts',(-60.9724208023033,29.8792370463633,
-216.714882811262));
#197587=CARTESIAN_POINT('Ctrl Pts',(-60.9867512024517,29.8100625396009,
-216.712441782693));
#197588=CARTESIAN_POINT('Ctrl Pts',(-61.0003153409054,29.7445868670811,
-216.71013127851));
#197589=CARTESIAN_POINT('Ctrl Pts',(-61.0131545031479,29.6792758917845,
-216.707859334961));
#197590=CARTESIAN_POINT('Ctrl Pts',(-61.0251046935149,29.614621768833,-216.705795549183));
#197591=CARTESIAN_POINT('Ctrl Pts',(-61.0257797804844,29.6109693453498,
-216.705678962347));
#197592=CARTESIAN_POINT('Ctrl Pts',(-61.0264520416984,29.6073190097918,
-216.705563039808));
#197593=CARTESIAN_POINT('Ctrl Pts',(-61.0271214515743,29.6036708476852,
-216.705447812142));
#197594=CARTESIAN_POINT('Ctrl Pts',(-62.0715435503803,29.170876467827,-213.793867031503));
#197595=CARTESIAN_POINT('Ctrl Pts',(-62.0610597588881,29.4471784510282,
-213.768820140639));
#197596=CARTESIAN_POINT('Ctrl Pts',(-62.0405226885833,29.7223719582909,
-213.744683753079));
#197597=CARTESIAN_POINT('Ctrl Pts',(-61.9794688757743,30.2707145068829,
-213.698186104697));
#197598=CARTESIAN_POINT('Ctrl Pts',(-61.938926317498,30.5439708220038,-213.676343773128));
#197599=CARTESIAN_POINT('Ctrl Pts',(-61.837636032495,31.0884065478961,-213.634598566576));
#197600=CARTESIAN_POINT('Ctrl Pts',(-61.7769096374044,31.3595164244479,
-213.614424841566));
#197601=CARTESIAN_POINT('Ctrl Pts',(-61.6347983988434,31.899450706002,-213.575433990368));
#197602=CARTESIAN_POINT('Ctrl Pts',(-61.5531858863137,32.1688271147634,
-213.556786982595));
#197603=CARTESIAN_POINT('Ctrl Pts',(-61.4159587545849,32.5674954665022,
-213.530743809019));
#197604=CARTESIAN_POINT('Ctrl Pts',(-61.3676767622843,32.6997212687758,
-213.522342385503));
#197605=CARTESIAN_POINT('Ctrl Pts',(-61.2664764445886,32.9616854374991,
-213.505934868461));
#197606=CARTESIAN_POINT('Ctrl Pts',(-61.2135447672718,33.091483145622,-213.497857516746));
#197607=CARTESIAN_POINT('Ctrl Pts',(-61.0478125873863,33.4773667643361,
-213.47408238772));
#197608=CARTESIAN_POINT('Ctrl Pts',(-60.9280440899178,33.7300206143803,
-213.459385328777));
#197609=CARTESIAN_POINT('Ctrl Pts',(-60.7344672841107,34.1022007074626,
-213.439632708162));
#197610=CARTESIAN_POINT('Ctrl Pts',(-60.6676250274419,34.2251152634526,
-213.433348725261));
#197611=CARTESIAN_POINT('Ctrl Pts',(-60.5293279502117,34.4685916588927,
-213.420959244589));
#197612=CARTESIAN_POINT('Ctrl Pts',(-60.4578772193282,34.5891494281844,
-213.414818675441));
#197613=CARTESIAN_POINT('Ctrl Pts',(-60.3471832550081,34.768251943839,-213.406087731132));
#197614=CARTESIAN_POINT('Ctrl Pts',(-60.3096963328013,34.8276667088433,
-213.403282057557));
#197615=CARTESIAN_POINT('Ctrl Pts',(-60.2335269589641,34.945932810334,-213.397980978197));
#197616=CARTESIAN_POINT('Ctrl Pts',(-60.1948462340149,35.0047819102021,
-213.395467604637));
#197617=CARTESIAN_POINT('Ctrl Pts',(-60.0770110939153,35.180460560743,-213.388255279868));
#197618=CARTESIAN_POINT('Ctrl Pts',(-59.9960526307283,35.2964118099283,
-213.383856689781));
#197619=CARTESIAN_POINT('Ctrl Pts',(-59.9134443065973,35.4101621769153,
-213.379883144535));
#197620=CARTESIAN_POINT('Ctrl Pts',(-58.4265182736836,35.031835198701,-216.764384131257));
#197621=CARTESIAN_POINT('Ctrl Pts',(-59.4820528027665,35.9125166648153,
-215.346308247144));
#197622=CARTESIAN_POINT('Ctrl Pts',(-59.4999643211654,35.9450057402374,
-213.371639708519));
#197623=CARTESIAN_POINT('Ctrl Pts',(-58.5101635386642,34.9284713760212,
-216.764533686556));
#197624=CARTESIAN_POINT('Ctrl Pts',(-59.6013542567605,35.7669646494546,
-215.346152352703));
#197625=CARTESIAN_POINT('Ctrl Pts',(-59.6440986517759,35.7696968033849,
-213.370755972398));
#197626=CARTESIAN_POINT('Ctrl Pts',(-58.5901397589755,34.8235003567058,
-216.768336879113));
#197627=CARTESIAN_POINT('Ctrl Pts',(-59.716223702441,35.6196247157672,-215.350089533733));
#197628=CARTESIAN_POINT('Ctrl Pts',(-59.7818407313686,35.591378236295,-213.37355288053));
#197629=CARTESIAN_POINT('Ctrl Pts',(-58.6665914736623,34.7169872964315,
-216.775646223556));
#197630=CARTESIAN_POINT('Ctrl Pts',(-59.8268417476682,35.4705704696998,
-215.357954892849));
#197631=CARTESIAN_POINT('Ctrl Pts',(-59.9134443065992,35.4101621769128,
-213.379883144535));
#197632=CARTESIAN_POINT('',(-58.4265182736835,35.0318351987012,-216.764384131257));
#197633=CARTESIAN_POINT('',(-59.4999643211654,35.9450057402376,-213.371639708519));
#197634=CARTESIAN_POINT('Origin',(-55.6381166865346,32.7703375395218,-213.284377676332));
#197635=CARTESIAN_POINT('Origin',(-55.6093041639685,32.7570348834843,-220.18888881533));
#197636=CARTESIAN_POINT('Origin',(-52.7506200812507,30.3721960348575,-218.064222059651));
#197637=CARTESIAN_POINT('Ctrl Pts',(-59.4999643211654,35.9450057402375,
-213.371639708519));
#197638=CARTESIAN_POINT('Ctrl Pts',(-59.4820528027664,35.9125166648155,
-215.346308247144));
#197639=CARTESIAN_POINT('Ctrl Pts',(-58.4265182736835,35.0318351987011,
-216.764384131257));
#197640=CARTESIAN_POINT('Ctrl Pts',(-58.5926451028781,37.0484655333583,
-213.380920503251));
#197641=CARTESIAN_POINT('Ctrl Pts',(-58.5785030823812,37.0120312878948,
-215.346864153085));
#197642=CARTESIAN_POINT('Ctrl Pts',(-57.5486529224783,36.1166487545866,
-216.762814542594));
#197643=CARTESIAN_POINT('Ctrl Pts',(-57.6483853099767,38.133634981491,-213.391180664217));
#197644=CARTESIAN_POINT('Ctrl Pts',(-57.6304520414564,38.1023651317606,
-215.347861259614));
#197645=CARTESIAN_POINT('Ctrl Pts',(-56.6223825642859,37.199049975754,-216.761500614303));
#197646=CARTESIAN_POINT('Ctrl Pts',(-56.6821911570462,39.1835711849512,
-213.399142265953));
#197647=CARTESIAN_POINT('Ctrl Pts',(-56.6650296771565,39.1519706625635,
-215.348455523392));
#197648=CARTESIAN_POINT('Ctrl Pts',(-55.6813080372832,38.2352492592492,
-216.760202274403));
#197649=CARTESIAN_POINT('Origin',(-55.9261752750931,34.4804203345293,-216.774342624392));
#197650=CARTESIAN_POINT('Ctrl Pts',(-59.4999643211654,35.9450057402376,
-213.371639708519));
#197651=CARTESIAN_POINT('Ctrl Pts',(-58.5980606988345,37.0418792159154,
-213.380865108156));
#197652=CARTESIAN_POINT('Ctrl Pts',(-57.6596561667371,38.1206800373646,
-213.391058217659));
#197653=CARTESIAN_POINT('Ctrl Pts',(-56.6994898617306,39.1647669078403,
-213.398999669105));
#197654=CARTESIAN_POINT('Ctrl Pts',(-32.8165183688975,-74.6541274212728,
-216.51122887497));
#197655=CARTESIAN_POINT('Ctrl Pts',(-33.0091444114044,-74.6582518783947,
-216.541274916939));
#197656=CARTESIAN_POINT('Ctrl Pts',(-33.2026950400511,-74.6410958794286,
-216.55765515809));
#197657=CARTESIAN_POINT('Ctrl Pts',(-32.9887489376153,-75.1686242635311,
-215.738182558023));
#197658=CARTESIAN_POINT('Ctrl Pts',(-33.1223658470707,-75.1686649637887,
-215.755874084856));
#197659=CARTESIAN_POINT('Ctrl Pts',(-33.2561102111421,-75.1596478279591,
-215.769886156826));
#197660=CARTESIAN_POINT('Ctrl Pts',(-33.1761299750104,-75.4501086463177,
-214.823392642664));
#197661=CARTESIAN_POINT('Ctrl Pts',(-33.2421742173859,-75.4479136121607,
-214.830806918362));
#197662=CARTESIAN_POINT('Ctrl Pts',(-33.3081522704534,-75.4457107575812,
-214.838787544289));
#197663=CARTESIAN_POINT('Ctrl Pts',(-33.3513928282978,-75.4608560063641,
-213.894101968638));
#197664=CARTESIAN_POINT('Ctrl Pts',(-33.3513928282978,-75.4608560063641,
-213.894101968638));
#197665=CARTESIAN_POINT('Ctrl Pts',(-33.3513928282978,-75.4608560063641,
-213.894101968638));
#197666=CARTESIAN_POINT('',(-32.8638506286442,-74.7886412857388,-216.296958652099));
#197667=CARTESIAN_POINT('',(-33.2148661077876,-74.7769245833719,-216.339144130374));
#197668=CARTESIAN_POINT('Origin',(-33.132841491033,-72.1913959359691,-214.819830610287));
#197669=CARTESIAN_POINT('',(-33.3513928264996,-75.4608559488301,-213.894101967632));
#197670=CARTESIAN_POINT('Ctrl Pts',(-32.8638506286442,-74.7886412857387,
-216.296958652099));
#197671=CARTESIAN_POINT('Ctrl Pts',(-32.8933260548794,-74.8682190505126,
-216.162404628958));
#197672=CARTESIAN_POINT('Ctrl Pts',(-32.9231745954811,-74.9411675841871,
-216.02417466485));
#197673=CARTESIAN_POINT('Ctrl Pts',(-32.9532524920876,-75.0072119742557,
-215.88285862242));
#197674=CARTESIAN_POINT('Ctrl Pts',(-32.986261903726,-75.0796933211633,
-215.727769339525));
#197675=CARTESIAN_POINT('Ctrl Pts',(-33.0195475005087,-75.1438591184812,
-215.568962618225));
#197676=CARTESIAN_POINT('Ctrl Pts',(-33.0529294896422,-75.199412086906,
-215.407221678871));
#197677=CARTESIAN_POINT('Ctrl Pts',(-33.0852131460734,-75.2531372540669,
-215.250802332615));
#197678=CARTESIAN_POINT('Ctrl Pts',(-33.1175871783702,-75.2988078108743,
-215.091637931136));
#197679=CARTESIAN_POINT('Ctrl Pts',(-33.1498964378058,-75.3362055632975,
-214.930449437084));
#197680=CARTESIAN_POINT('Ctrl Pts',(-33.1812470981023,-75.372493743607,
-214.774043322893));
#197681=CARTESIAN_POINT('Ctrl Pts',(-33.2125369672066,-75.4009928593788,
-214.615730725899));
#197682=CARTESIAN_POINT('Ctrl Pts',(-33.2436284013859,-75.4215458554388,
-214.456193093629));
#197683=CARTESIAN_POINT('Ctrl Pts',(-33.2728936047542,-75.4408916214159,
-214.306026291212));
#197684=CARTESIAN_POINT('Ctrl Pts',(-33.3019831259178,-75.4531972400418,
-214.154773836299));
#197685=CARTESIAN_POINT('Ctrl Pts',(-33.3307835805188,-75.4583694968115,
-214.003031469667));
#197686=CARTESIAN_POINT('Ctrl Pts',(-33.3376703705436,-75.4596062913975,
-213.96674670155));
#197687=CARTESIAN_POINT('Ctrl Pts',(-33.3445406344615,-75.4604353932884,
-213.930434060699));
#197688=CARTESIAN_POINT('Ctrl Pts',(-33.3513928247577,-75.4608558931301,
-213.894101966659));
#197689=CARTESIAN_POINT('Ctrl Pts',(-33.214866107757,-74.7769245823989,
-216.339144129802));
#197690=CARTESIAN_POINT('Ctrl Pts',(-33.2161008212724,-74.7878219958422,
-216.320532532356));
#197691=CARTESIAN_POINT('Ctrl Pts',(-33.2175661619688,-74.8004930397082,
-216.298622713186));
#197692=CARTESIAN_POINT('Ctrl Pts',(-33.2192576796893,-74.8147968984671,
-216.273316347388));
#197693=CARTESIAN_POINT('Ctrl Pts',(-33.2209398407141,-74.8290216348776,
-216.248149964733));
#197694=CARTESIAN_POINT('Ctrl Pts',(-33.2228456900929,-74.8448613909909,
-216.219624134786));
#197695=CARTESIAN_POINT('Ctrl Pts',(-33.2249693770086,-74.8621308073514,
-216.187621059665));
#197696=CARTESIAN_POINT('Ctrl Pts',(-33.2270703464035,-74.8792154891719,
-216.155960328097));
#197697=CARTESIAN_POINT('Ctrl Pts',(-33.2293845234151,-74.8976995978964,
-216.120895865541));
#197698=CARTESIAN_POINT('Ctrl Pts',(-33.2319047062494,-74.9173546654421,
-216.082299276337));
#197699=CARTESIAN_POINT('Ctrl Pts',(-33.2322639276174,-74.9201562559283,
-216.07679780264));
#197700=CARTESIAN_POINT('Ctrl Pts',(-33.2326273317533,-74.922981551917,
-216.071224549988));
#197701=CARTESIAN_POINT('Ctrl Pts',(-33.232994895118,-74.9258298060492,
-216.065579132006));
#197702=CARTESIAN_POINT('Ctrl Pts',(-33.235521708764,-74.9454101236201,
-216.02676971692));
#197703=CARTESIAN_POINT('Ctrl Pts',(-33.2382452115044,-74.9660795535131,
-215.984549980128));
#197704=CARTESIAN_POINT('Ctrl Pts',(-33.2411568577201,-74.9875665385017,
-215.938792794573));
#197705=CARTESIAN_POINT('Ctrl Pts',(-33.2440204091037,-75.0086985995535,
-215.893791430295));
#197706=CARTESIAN_POINT('Ctrl Pts',(-33.2470659410344,-75.0306214817497,
-215.845367893565));
#197707=CARTESIAN_POINT('Ctrl Pts',(-33.2502837771814,-75.0530272134654,
-215.793405196313));
#197708=CARTESIAN_POINT('Ctrl Pts',(-33.2534413473024,-75.0750133139911,
-215.742415695061));
#197709=CARTESIAN_POINT('Ctrl Pts',(-33.2567648260833,-75.097464297192,
-215.688017709565));
#197710=CARTESIAN_POINT('Ctrl Pts',(-33.2602435735815,-75.1200409653675,
-215.630113880679));
#197711=CARTESIAN_POINT('Ctrl Pts',(-33.2636148807263,-75.1419203580994,
-215.573998398844));
#197712=CARTESIAN_POINT('Ctrl Pts',(-33.2671320060908,-75.1639175549083,
-215.514589701032));
#197713=CARTESIAN_POINT('Ctrl Pts',(-33.2707839210029,-75.1856803680515,
-215.45182058607));
#197714=CARTESIAN_POINT('Ctrl Pts',(-33.2743682890001,-75.2070406496675,
-215.390212467508));
#197715=CARTESIAN_POINT('Ctrl Pts',(-33.2780824983859,-75.2281748902149,
-215.325366493977));
#197716=CARTESIAN_POINT('Ctrl Pts',(-33.2819149163973,-75.2487109574915,
-215.257248779496));
#197717=CARTESIAN_POINT('Ctrl Pts',(-33.2856358268015,-75.2686495096442,
-215.191113010441));
#197718=CARTESIAN_POINT('Ctrl Pts',(-33.2894681543121,-75.288023788226,
-215.121892651973));
#197719=CARTESIAN_POINT('Ctrl Pts',(-33.2934002616768,-75.3064608341125,
-215.049592577771));
#197720=CARTESIAN_POINT('Ctrl Pts',(-33.2968272599527,-75.3225295012684,
-214.986579997834));
#197721=CARTESIAN_POINT('Ctrl Pts',(-33.3003300294583,-75.3378856082417,
-214.921228394508));
#197722=CARTESIAN_POINT('Ctrl Pts',(-33.3039003488338,-75.3522651902505,
-214.853568530225));
#197723=CARTESIAN_POINT('Ctrl Pts',(-33.3078221575319,-75.3680604073912,
-214.779247715656));
#197724=CARTESIAN_POINT('Ctrl Pts',(-33.3118254668097,-75.3826772453835,
-214.702140725086));
#197725=CARTESIAN_POINT('Ctrl Pts',(-33.3158988721731,-75.3957488225826,
-214.622330942384));
#197726=CARTESIAN_POINT('Ctrl Pts',(-33.3199055351263,-75.4086062230697,
-214.543828836376));
#197727=CARTESIAN_POINT('Ctrl Pts',(-33.3239799985301,-75.4199680325328,
-214.462711510984));
#197728=CARTESIAN_POINT('Ctrl Pts',(-33.3281111209217,-75.4294750184256,
-214.379106717126));
#197729=CARTESIAN_POINT('Ctrl Pts',(-33.3321439448228,-75.4387557891946,
-214.297491267632));
#197730=CARTESIAN_POINT('Ctrl Pts',(-33.3362307450562,-75.4462683685185,
-214.213505231994));
#197731=CARTESIAN_POINT('Ctrl Pts',(-33.3403611424482,-75.4516772452927,
-214.127316474386));
#197732=CARTESIAN_POINT('Ctrl Pts',(-33.3440067390281,-75.4564512611557,
-214.051244026592));
#197733=CARTESIAN_POINT('Ctrl Pts',(-33.3476862895492,-75.4595861164654,
-213.973456225545));
#197734=CARTESIAN_POINT('Ctrl Pts',(-33.3513928282415,-75.4608560045305,
-213.894101968605));
#197735=CARTESIAN_POINT('Ctrl Pts',(-32.8237598256931,-74.7342241033955,
-216.385388039321));
#197736=CARTESIAN_POINT('Ctrl Pts',(-32.9990492150883,-74.6974990623407,
-216.482388336084));
#197737=CARTESIAN_POINT('Ctrl Pts',(-33.1752262860966,-74.6372704537069,
-216.564961398279));
#197738=CARTESIAN_POINT('Ctrl Pts',(-32.8430811295134,-74.7517232841371,
-216.358132577358));
#197739=CARTESIAN_POINT('Ctrl Pts',(-33.0186275335316,-74.7272821064456,
-216.433478854629));
#197740=CARTESIAN_POINT('Ctrl Pts',(-33.1949631872871,-74.6820694401031,
-216.496303691409));
#197741=CARTESIAN_POINT('Ctrl Pts',(-32.8576392293324,-74.7701076430446,
-216.328432913936));
#197742=CARTESIAN_POINT('Ctrl Pts',(-33.0332084422395,-74.759074042344,
-216.380020841617));
#197743=CARTESIAN_POINT('Ctrl Pts',(-33.2094670740838,-74.7292736488408,
-216.42052674827));
#197744=CARTESIAN_POINT('Ctrl Pts',(-32.8638454862961,-74.788639230448,
-216.296979356596));
#197745=CARTESIAN_POINT('Ctrl Pts',(-33.0390297214682,-74.7918205915911,
-216.32328753345));
#197746=CARTESIAN_POINT('Ctrl Pts',(-33.2148661078031,-74.7769245838569,
-216.339144130663));
#197747=CARTESIAN_POINT('',(-33.1752262860962,-74.6372704537073,-216.564961398278));
#197748=CARTESIAN_POINT('',(-32.8237598256931,-74.7342241033955,-216.385388039321));
#197749=CARTESIAN_POINT('Origin',(-33.095784450501,-72.1361943004091,-214.910178309726));
#197750=CARTESIAN_POINT('Origin',(-31.6882418561644,-74.6383695538455,-216.347659410123));
#197751=CARTESIAN_POINT('Origin',(-32.1378318913552,-74.4550490310553,-216.331724211812));
#197752=CARTESIAN_POINT('Ctrl Pts',(-40.9214983009346,-74.359273050182,
-216.569709261874));
#197753=CARTESIAN_POINT('Ctrl Pts',(-40.9511754288283,-75.1706180168058,
-215.350418326104));
#197754=CARTESIAN_POINT('Ctrl Pts',(-40.9503927122519,-75.1962323486437,
-213.885776709122));
#197755=CARTESIAN_POINT('Ctrl Pts',(-38.3243446255231,-74.4622360878715,
-216.567950323542));
#197756=CARTESIAN_POINT('Ctrl Pts',(-38.3524464104668,-75.2704427049198,
-215.350356210397));
#197757=CARTESIAN_POINT('Ctrl Pts',(-38.3512480421798,-75.2960131238996,
-213.888896037155));
#197758=CARTESIAN_POINT('Ctrl Pts',(-35.7265937516252,-74.5554064320832,
-216.566381833796));
#197759=CARTESIAN_POINT('Ctrl Pts',(-35.7526446696953,-75.3607900950907,
-215.350336416776));
#197760=CARTESIAN_POINT('Ctrl Pts',(-35.75158731892,-75.3862982053642,-213.891764704332));
#197761=CARTESIAN_POINT('Ctrl Pts',(-33.1287433582892,-74.6387629869627,
-216.564935505388));
#197762=CARTESIAN_POINT('Ctrl Pts',(-33.152500416473,-75.4416278685767,
-215.350281850593));
#197763=CARTESIAN_POINT('Ctrl Pts',(-33.1518661790636,-75.4670741746134,
-213.89429696046));
#197764=CARTESIAN_POINT('',(-40.9503927122327,-75.1962323486441,-213.885776709122));
#197765=CARTESIAN_POINT('Origin',(0.00137741249504053,990.512728685443,
-181.064224899351));
#197766=CARTESIAN_POINT('',(-40.9214982998565,-74.359273049611,-216.569709262805));
#197767=CARTESIAN_POINT('Origin',(-40.758509388043,-70.2006777120066,-213.798514676938));
#197768=CARTESIAN_POINT('Origin',(0.00331736233953883,957.648657693644,
-233.042565174374));
#197769=CARTESIAN_POINT('Ctrl Pts',(-42.6506409244545,-73.9423397713714,
-216.824911934325));
#197770=CARTESIAN_POINT('Ctrl Pts',(-42.3889675192146,-75.111938779609,
-215.496580546143));
#197771=CARTESIAN_POINT('Ctrl Pts',(-41.9926628230245,-75.1580153204876,
-213.752528187964));
#197772=CARTESIAN_POINT('Ctrl Pts',(-42.5223146433586,-73.9743057102224,
-216.82138777715));
#197773=CARTESIAN_POINT('Ctrl Pts',(-42.2773680112826,-75.1163504965845,
-215.497499167852));
#197774=CARTESIAN_POINT('Ctrl Pts',(-41.9066793323656,-75.1610610934853,
-213.772054913983));
#197775=CARTESIAN_POINT('Ctrl Pts',(-42.3813794284866,-74.0123061097096,
-216.810485774898));
#197776=CARTESIAN_POINT('Ctrl Pts',(-42.1584887885793,-75.1211304958,-215.492781710654));
#197777=CARTESIAN_POINT('Ctrl Pts',(-41.8205323433735,-75.1641318505825,
-213.789924116924));
#197778=CARTESIAN_POINT('Ctrl Pts',(-42.1071714176858,-74.0810920561383,
-216.786773384891));
#197779=CARTESIAN_POINT('Ctrl Pts',(-41.9257553840099,-75.130477399032,
-215.482136500678));
#197780=CARTESIAN_POINT('Ctrl Pts',(-41.6477999581334,-75.1703415381604,
-213.821539717991));
#197781=CARTESIAN_POINT('Ctrl Pts',(-41.9710574680775,-74.1134796538365,
-216.773245626096));
#197782=CARTESIAN_POINT('Ctrl Pts',(-41.8102296619904,-75.1351214208382,
-215.475611436836));
#197783=CARTESIAN_POINT('Ctrl Pts',(-41.5612314342439,-75.1734777382292,
-213.835404439875));
#197784=CARTESIAN_POINT('Ctrl Pts',(-41.6930958560016,-74.1786675398529,
-216.738185296847));
#197785=CARTESIAN_POINT('Ctrl Pts',(-41.5763451014596,-75.1445888151811,
-215.456563678656));
#197786=CARTESIAN_POINT('Ctrl Pts',(-41.3876518834474,-75.1798203744337,
-213.85888373828));
#197787=CARTESIAN_POINT('Ctrl Pts',(-41.550883114529,-74.2117857468627,
-216.716530930408));
#197788=CARTESIAN_POINT('Ctrl Pts',(-41.4577834622525,-75.1494218955762,
-215.443955718173));
#197789=CARTESIAN_POINT('Ctrl Pts',(-41.3006463902462,-75.1830256709096,
-213.868551556967));
#197790=CARTESIAN_POINT('Ctrl Pts',(-41.242598522617,-74.2859889768,-216.652644382786));
#197791=CARTESIAN_POINT('Ctrl Pts',(-41.2077086856973,-75.1598056161709,
-215.404074252949));
#197792=CARTESIAN_POINT('Ctrl Pts',(-41.1260290981951,-75.1895400074146,
-213.882061105839));
#197793=CARTESIAN_POINT('Ctrl Pts',(-41.0767448132029,-74.3265280314252,
-216.609717214661));
#197794=CARTESIAN_POINT('Ctrl Pts',(-41.0764186051261,-75.16535240508,-215.376453037305));
#197795=CARTESIAN_POINT('Ctrl Pts',(-41.0384011165336,-75.1928537189709,
-213.885671097976));
#197796=CARTESIAN_POINT('Ctrl Pts',(-40.9214983001269,-74.359273049532,
-216.569709262896));
#197797=CARTESIAN_POINT('Ctrl Pts',(-40.9511754272514,-75.170618016854,
-215.350418326772));
#197798=CARTESIAN_POINT('Ctrl Pts',(-40.9503927097334,-75.1962323487397,
-213.885776709125));
#197799=CARTESIAN_POINT('',(-42.6506409244548,-73.9423397713703,-216.824911934326));
#197800=CARTESIAN_POINT('',(-41.992662823025,-75.1580153204871,-213.752528187964));
#197801=CARTESIAN_POINT('Origin',(-41.7958961124187,-70.1626506491805,-213.665266155779));
#197802=CARTESIAN_POINT('Ctrl Pts',(-42.6506409244548,-73.9423397713703,
-216.824911934326));
#197803=CARTESIAN_POINT('Ctrl Pts',(-42.5223146433586,-73.9743057102224,
-216.82138777715));
#197804=CARTESIAN_POINT('Ctrl Pts',(-42.3813794284866,-74.0123061097096,
-216.810485774898));
#197805=CARTESIAN_POINT('Ctrl Pts',(-42.1071714176858,-74.0810920561383,
-216.786773384891));
#197806=CARTESIAN_POINT('Ctrl Pts',(-41.9710574680775,-74.1134796538365,
-216.773245626096));
#197807=CARTESIAN_POINT('Ctrl Pts',(-41.6930958560016,-74.1786675398529,
-216.738185296847));
#197808=CARTESIAN_POINT('Ctrl Pts',(-41.550883114529,-74.2117857468627,
-216.716530930408));
#197809=CARTESIAN_POINT('Ctrl Pts',(-41.242598522617,-74.2859889768,-216.652644382786));
#197810=CARTESIAN_POINT('Ctrl Pts',(-41.0767448132029,-74.3265280314252,
-216.609717214661));
#197811=CARTESIAN_POINT('Ctrl Pts',(-40.921498300133,-74.359273049617,-216.569709262785));
#197812=CARTESIAN_POINT('Ctrl Pts',(-40.9503927122327,-75.1962323486438,
-213.885776709122));
#197813=CARTESIAN_POINT('Ctrl Pts',(-41.038474251468,-75.1928509113325,
-213.885671010147));
#197814=CARTESIAN_POINT('Ctrl Pts',(-41.1260976159204,-75.1895374500551,
-213.882055874295));
#197815=CARTESIAN_POINT('Ctrl Pts',(-41.2133377538232,-75.1862828366116,
-213.875306456161));
#197816=CARTESIAN_POINT('Ctrl Pts',(-41.3007070198063,-75.1830234058673,
-213.868547047908));
#197817=CARTESIAN_POINT('Ctrl Pts',(-41.3877081322113,-75.1798183151619,
-213.858876354798));
#197818=CARTESIAN_POINT('Ctrl Pts',(-41.4744416790084,-75.1766490529395,
-213.847144238352));
#197819=CARTESIAN_POINT('Ctrl Pts',(-41.5612776272754,-75.1734760489456,
-213.835398270449));
#197820=CARTESIAN_POINT('Ctrl Pts',(-41.6478454293514,-75.1703399027888,
-213.821531434941));
#197821=CARTESIAN_POINT('Ctrl Pts',(-41.7341661542901,-75.1672366938954,
-213.805731936782));
#197822=CARTESIAN_POINT('Ctrl Pts',(-41.8205769753023,-75.1641302460704,
-213.789915948114));
#197823=CARTESIAN_POINT('Ctrl Pts',(-41.9067233040908,-75.1610595358852,
-213.772044928068));
#197824=CARTESIAN_POINT('Ctrl Pts',(-41.9926628230246,-75.1580153204876,
-213.752528187964));
#197825=CARTESIAN_POINT('Ctrl Pts',(-41.9926628230233,-75.1580153204872,
-213.752528187965));
#197826=CARTESIAN_POINT('Ctrl Pts',(-42.3889675192142,-75.1119387796086,
-215.496580546144));
#197827=CARTESIAN_POINT('Ctrl Pts',(-42.650640924455,-73.9423397713704,
-216.824911934326));
#197828=CARTESIAN_POINT('Ctrl Pts',(-42.2441904201252,-75.1486693658634,
-213.720374383032));
#197829=CARTESIAN_POINT('Ctrl Pts',(-42.6352341484771,-75.0934987178605,
-215.491846788295));
#197830=CARTESIAN_POINT('Ctrl Pts',(-42.8635176930321,-73.8893123883119,
-216.830758067302));
#197831=CARTESIAN_POINT('Ctrl Pts',(-42.4949766531494,-75.1309696159339,
-213.689703299478));
#197832=CARTESIAN_POINT('Ctrl Pts',(-42.8751575352819,-75.0674875232695,
-215.483919014076));
#197833=CARTESIAN_POINT('Ctrl Pts',(-43.0658447951879,-73.8361356612473,
-216.831614746056));
#197834=CARTESIAN_POINT('Ctrl Pts',(-42.9950456426682,-75.0789259129276,
-213.631395393625));
#197835=CARTESIAN_POINT('Ctrl Pts',(-43.3573635301376,-74.9997783248717,
-215.472578146401));
#197836=CARTESIAN_POINT('Ctrl Pts',(-43.4723745746873,-73.7138512147641,
-216.837059076436));
#197837=CARTESIAN_POINT('Ctrl Pts',(-43.244282955429,-75.0445859118617,
-213.603599246343));
#197838=CARTESIAN_POINT('Ctrl Pts',(-43.6008375706358,-74.9576518167014,
-215.469588054037));
#197839=CARTESIAN_POINT('Ctrl Pts',(-43.6783947191598,-73.6431300259591,
-216.842077816832));
#197840=CARTESIAN_POINT('Ctrl Pts',(-43.7407999450918,-74.9592348987093,
-213.549700262593));
#197841=CARTESIAN_POINT('Ctrl Pts',(-44.0847915726919,-74.8574180597928,
-215.462932027522));
#197842=CARTESIAN_POINT('Ctrl Pts',(-44.0841000052998,-73.4910414674771,
-216.849773863078));
#197843=CARTESIAN_POINT('Ctrl Pts',(-43.9880896420054,-74.9082283395953,
-213.523624316504));
#197844=CARTESIAN_POINT('Ctrl Pts',(-44.3242556788489,-74.7995069031645,
-215.458703822069));
#197845=CARTESIAN_POINT('Ctrl Pts',(-44.2823909841006,-73.4109348364935,
-216.851832092541));
#197846=CARTESIAN_POINT('Ctrl Pts',(-44.4808857844271,-74.7891870797402,
-213.473791302964));
#197847=CARTESIAN_POINT('Ctrl Pts',(-44.7955537966533,-74.6692676550458,
-215.447631213062));
#197848=CARTESIAN_POINT('Ctrl Pts',(-44.6664888328127,-73.2472194754336,
-216.851891665016));
#197849=CARTESIAN_POINT('Ctrl Pts',(-44.7267891899937,-74.7210209447827,
-213.450088190094));
#197850=CARTESIAN_POINT('Ctrl Pts',(-45.0291379688623,-74.5965659081431,
-215.441811276339));
#197851=CARTESIAN_POINT('Ctrl Pts',(-44.8547955882521,-73.161697166002,
-216.851063156481));
#197852=CARTESIAN_POINT('Ctrl Pts',(-45.0928291473126,-74.606027152532,
-213.416036405768));
#197853=CARTESIAN_POINT('Ctrl Pts',(-45.3816384584871,-74.4740602974644,
-215.436515048508));
#197854=CARTESIAN_POINT('Ctrl Pts',(-45.1406078814123,-73.0181691132047,
-216.852776982251));
#197855=CARTESIAN_POINT('Ctrl Pts',(-45.2142260714279,-74.5656241152041,
-213.404928397061));
#197856=CARTESIAN_POINT('Ctrl Pts',(-45.5004898449934,-74.4305954967414,
-215.435878858443));
#197857=CARTESIAN_POINT('Ctrl Pts',(-45.2377029692462,-72.9663736632951,
-216.854423557714));
#197858=CARTESIAN_POINT('Ctrl Pts',(-45.4557176198781,-74.4806914809372,
-213.382939645029));
#197859=CARTESIAN_POINT('Ctrl Pts',(-45.7358730844374,-74.3399851570232,
-215.4337505975));
#197860=CARTESIAN_POINT('Ctrl Pts',(-45.4288319445799,-72.8615155438485,
-216.85653065457));
#197861=CARTESIAN_POINT('Ctrl Pts',(-45.5757446359476,-74.4361813329049,
-213.372122623239));
#197862=CARTESIAN_POINT('Ctrl Pts',(-45.8501188293173,-74.2937160035012,
-215.431078613902));
#197863=CARTESIAN_POINT('Ctrl Pts',(-45.5198481005889,-72.8116610800095,
-216.855759513965));
#197864=CARTESIAN_POINT('Ctrl Pts',(-45.9328087572912,-74.2968675255704,
-213.340776903277));
#197865=CARTESIAN_POINT('Ctrl Pts',(-46.1873653169248,-74.1508282744403,
-215.422045951277));
#197866=CARTESIAN_POINT('Ctrl Pts',(-45.7862796787808,-72.6630395831569,
-216.852106972262));
#197867=CARTESIAN_POINT('Ctrl Pts',(-46.1672258662825,-74.1961452862474,
-213.321432015398));
#197868=CARTESIAN_POINT('Ctrl Pts',(-46.4036505792935,-74.0508269587878,
-215.414220291772));
#197869=CARTESIAN_POINT('Ctrl Pts',(-45.9538518097036,-72.5669178021949,
-216.847424766396));
#197870=CARTESIAN_POINT('Ctrl Pts',(-46.5133864112104,-74.0333951639031,
-213.29438225272));
#197871=CARTESIAN_POINT('Ctrl Pts',(-46.7325370368903,-73.8859308362923,
-215.40853678471));
#197872=CARTESIAN_POINT('Ctrl Pts',(-46.2132892873817,-72.4014855733941,
-216.846116620724));
#197873=CARTESIAN_POINT('Ctrl Pts',(-46.6278478339336,-73.977206798173,
-213.285618874285));
#197874=CARTESIAN_POINT('Ctrl Pts',(-46.8439967269085,-73.8278355227286,
-215.408064094516));
#197875=CARTESIAN_POINT('Ctrl Pts',(-46.3023963850082,-72.3411661322158,
-216.847039252521));
#197876=CARTESIAN_POINT('Ctrl Pts',(-46.8548608425726,-73.8609873091134,
-213.268274976754));
#197877=CARTESIAN_POINT('Ctrl Pts',(-47.0648456467714,-73.7079559631609,
-215.406504660188));
#197878=CARTESIAN_POINT('Ctrl Pts',(-46.478613276723,-72.2185871221317,
-216.848037413775));
#197879=CARTESIAN_POINT('Ctrl Pts',(-46.9674078997609,-73.8009605736129,
-213.259666405965));
#197880=CARTESIAN_POINT('Ctrl Pts',(-47.1733859838122,-73.6465693372023,
-215.404947296863));
#197881=CARTESIAN_POINT('Ctrl Pts',(-46.5646834624717,-72.1575736757065,
-216.847643933755));
#197882=CARTESIAN_POINT('Ctrl Pts',(-47.1348908422149,-73.7079618268568,
-213.247450860245));
#197883=CARTESIAN_POINT('Ctrl Pts',(-47.3249946652538,-73.5575902386026,
-215.398041248184));
#197884=CARTESIAN_POINT('Ctrl Pts',(-46.6799581763352,-72.0805586557944,
-216.842417562875));
#197885=CARTESIAN_POINT('Ctrl Pts',(-47.1904997834943,-73.6764658823064,
-213.243519901462));
#197886=CARTESIAN_POINT('Ctrl Pts',(-47.3742816457676,-73.5281301342516,
-215.395327330629));
#197887=CARTESIAN_POINT('Ctrl Pts',(-46.7168699475549,-72.05633006151,-216.840249166734));
#197888=CARTESIAN_POINT('Ctrl Pts',(-47.3012779792568,-73.612476222395,
-213.235940031067));
#197889=CARTESIAN_POINT('Ctrl Pts',(-47.4738788426063,-73.4675943998322,
-215.39080987434));
#197890=CARTESIAN_POINT('Ctrl Pts',(-46.7922015926475,-72.005114703694,
-216.836785542713));
#197891=CARTESIAN_POINT('Ctrl Pts',(-47.3564465382692,-73.5799829806332,
-213.232287185893));
#197892=CARTESIAN_POINT('Ctrl Pts',(-47.5236661359778,-73.4368125264023,
-215.388740875334));
#197893=CARTESIAN_POINT('Ctrl Pts',(-46.8299530635768,-71.9789628961022,
-216.835225967646));
#197894=CARTESIAN_POINT('Ctrl Pts',(-47.5212831512919,-73.4810018009163,
-213.221720566444));
#197895=CARTESIAN_POINT('Ctrl Pts',(-47.6725708647175,-73.3431501790447,
-215.382801668109));
#197896=CARTESIAN_POINT('Ctrl Pts',(-46.9429621731836,-71.8996192326861,
-216.830756524433));
#197897=CARTESIAN_POINT('Ctrl Pts',(-47.6302808905533,-73.4130142912104,
-213.215183926779));
#197898=CARTESIAN_POINT('Ctrl Pts',(-47.7711941360104,-73.2789527469259,
-215.379175449449));
#197899=CARTESIAN_POINT('Ctrl Pts',(-47.017973525604,-71.8455276788576,
-216.82803305392));
#197900=CARTESIAN_POINT('Ctrl Pts',(-47.7383831769164,-73.3429891884104,
-213.20923907124));
#197901=CARTESIAN_POINT('Ctrl Pts',(-47.8674267413588,-73.2141877251374,
-215.374920075633));
#197902=CARTESIAN_POINT('Ctrl Pts',(-47.090555767608,-71.7934728593479,
-216.824560386716));
#197903=CARTESIAN_POINT('',(-47.0905557676078,-71.7934728593479,-216.824560386716));
#197904=CARTESIAN_POINT('',(-47.738383176916,-73.3429891884109,-213.20923907124));
#197905=CARTESIAN_POINT('Origin',(-45.0170666017296,-69.1493247484068,-213.121977039054));
#197906=CARTESIAN_POINT('Ctrl Pts',(-47.0905557676078,-71.7934728593479,
-216.824560386716));
#197907=CARTESIAN_POINT('Ctrl Pts',(-47.017973525604,-71.8455276788576,
-216.82803305392));
#197908=CARTESIAN_POINT('Ctrl Pts',(-46.9429621731836,-71.8996192326861,
-216.830756524433));
#197909=CARTESIAN_POINT('Ctrl Pts',(-46.8299530635768,-71.9789628961022,
-216.835225967646));
#197910=CARTESIAN_POINT('Ctrl Pts',(-46.7922015926475,-72.005114703694,
-216.836785542713));
#197911=CARTESIAN_POINT('Ctrl Pts',(-46.7168699475549,-72.05633006151,-216.840249166734));
#197912=CARTESIAN_POINT('Ctrl Pts',(-46.6799581763352,-72.0805586557944,
-216.842417562875));
#197913=CARTESIAN_POINT('Ctrl Pts',(-46.5646834624717,-72.1575736757065,
-216.847643933755));
#197914=CARTESIAN_POINT('Ctrl Pts',(-46.478613276723,-72.2185871221317,
-216.848037413775));
#197915=CARTESIAN_POINT('Ctrl Pts',(-46.3023963850082,-72.3411661322158,
-216.847039252521));
#197916=CARTESIAN_POINT('Ctrl Pts',(-46.2132892873817,-72.4014855733941,
-216.846116620724));
#197917=CARTESIAN_POINT('Ctrl Pts',(-45.9538518097036,-72.5669178021949,
-216.847424766396));
#197918=CARTESIAN_POINT('Ctrl Pts',(-45.7862796787808,-72.6630395831569,
-216.852106972262));
#197919=CARTESIAN_POINT('Ctrl Pts',(-45.5198481005889,-72.8116610800095,
-216.855759513965));
#197920=CARTESIAN_POINT('Ctrl Pts',(-45.4288319445799,-72.8615155438485,
-216.85653065457));
#197921=CARTESIAN_POINT('Ctrl Pts',(-45.2377029692462,-72.9663736632951,
-216.854423557714));
#197922=CARTESIAN_POINT('Ctrl Pts',(-45.1406078814123,-73.0181691132047,
-216.852776982251));
#197923=CARTESIAN_POINT('Ctrl Pts',(-44.8547955882521,-73.161697166002,
-216.851063156481));
#197924=CARTESIAN_POINT('Ctrl Pts',(-44.6664888328127,-73.2472194754336,
-216.851891665016));
#197925=CARTESIAN_POINT('Ctrl Pts',(-44.2823909841006,-73.4109348364935,
-216.851832092541));
#197926=CARTESIAN_POINT('Ctrl Pts',(-44.0841000052998,-73.4910414674771,
-216.849773863078));
#197927=CARTESIAN_POINT('Ctrl Pts',(-43.6783947191598,-73.6431300259591,
-216.842077816832));
#197928=CARTESIAN_POINT('Ctrl Pts',(-43.4723745746873,-73.7138512147641,
-216.837059076436));
#197929=CARTESIAN_POINT('Ctrl Pts',(-43.0658447951879,-73.8361356612473,
-216.831614746056));
#197930=CARTESIAN_POINT('Ctrl Pts',(-42.8635176930321,-73.8893123883119,
-216.830758067302));
#197931=CARTESIAN_POINT('Ctrl Pts',(-42.6506409244548,-73.9423397713703,
-216.824911934326));
#197932=CARTESIAN_POINT('Ctrl Pts',(-41.992662823025,-75.1580153204871,
-213.752528187964));
#197933=CARTESIAN_POINT('Ctrl Pts',(-42.2441904201252,-75.1486693658634,
-213.720374383032));
#197934=CARTESIAN_POINT('Ctrl Pts',(-42.4949766531494,-75.1309696159339,
-213.689703299478));
#197935=CARTESIAN_POINT('Ctrl Pts',(-42.9950456426682,-75.0789259129276,
-213.631395393625));
#197936=CARTESIAN_POINT('Ctrl Pts',(-43.244282955429,-75.0445859118617,
-213.603599246343));
#197937=CARTESIAN_POINT('Ctrl Pts',(-43.7407999450918,-74.9592348987093,
-213.549700262593));
#197938=CARTESIAN_POINT('Ctrl Pts',(-43.9880896420054,-74.9082283395953,
-213.523624316504));
#197939=CARTESIAN_POINT('Ctrl Pts',(-44.4808857844271,-74.7891870797402,
-213.473791302964));
#197940=CARTESIAN_POINT('Ctrl Pts',(-44.7267891899937,-74.7210209447827,
-213.450088190094));
#197941=CARTESIAN_POINT('Ctrl Pts',(-45.0928291473126,-74.606027152532,
-213.416036405768));
#197942=CARTESIAN_POINT('Ctrl Pts',(-45.2142260714279,-74.5656241152041,
-213.404928397061));
#197943=CARTESIAN_POINT('Ctrl Pts',(-45.4557176198781,-74.4806914809372,
-213.382939645029));
#197944=CARTESIAN_POINT('Ctrl Pts',(-45.5757446359476,-74.4361813329049,
-213.372122623239));
#197945=CARTESIAN_POINT('Ctrl Pts',(-45.9328087572912,-74.2968675255704,
-213.340776903277));
#197946=CARTESIAN_POINT('Ctrl Pts',(-46.1672258662825,-74.1961452862474,
-213.321432015398));
#197947=CARTESIAN_POINT('Ctrl Pts',(-46.5133864112104,-74.0333951639031,
-213.29438225272));
#197948=CARTESIAN_POINT('Ctrl Pts',(-46.6278478339336,-73.977206798173,
-213.285618874285));
#197949=CARTESIAN_POINT('Ctrl Pts',(-46.8548608425726,-73.8609873091134,
-213.268274976754));
#197950=CARTESIAN_POINT('Ctrl Pts',(-46.9674078997609,-73.8009605736129,
-213.259666405965));
#197951=CARTESIAN_POINT('Ctrl Pts',(-47.1348908422149,-73.7079618268568,
-213.247450860245));
#197952=CARTESIAN_POINT('Ctrl Pts',(-47.1904997834943,-73.6764658823064,
-213.243519901462));
#197953=CARTESIAN_POINT('Ctrl Pts',(-47.3012779792568,-73.612476222395,
-213.235940031067));
#197954=CARTESIAN_POINT('Ctrl Pts',(-47.3564465382692,-73.5799829806332,
-213.232287185893));
#197955=CARTESIAN_POINT('Ctrl Pts',(-47.5212831512919,-73.4810018009163,
-213.221720566444));
#197956=CARTESIAN_POINT('Ctrl Pts',(-47.6302808905533,-73.4130142912104,
-213.215183926779));
#197957=CARTESIAN_POINT('Ctrl Pts',(-47.738383176916,-73.3429891884109,
-213.20923907124));
#197958=CARTESIAN_POINT('Ctrl Pts',(-47.6826029798323,-71.3710801272352,
-216.791855002172));
#197959=CARTESIAN_POINT('Ctrl Pts',(-48.7033558856732,-72.5944415704724,
-215.339600005589));
#197960=CARTESIAN_POINT('Ctrl Pts',(-48.7454044931546,-72.6086641314349,
-213.184229057458));
#197961=CARTESIAN_POINT('Ctrl Pts',(-47.4907935026769,-71.5238447202,-216.792044585111));
#197962=CARTESIAN_POINT('Ctrl Pts',(-48.4312469413224,-72.815727223767,
-215.339098369127));
#197963=CARTESIAN_POINT('Ctrl Pts',(-48.4201758660461,-72.8745352082661,
-213.18165597563));
#197964=CARTESIAN_POINT('Ctrl Pts',(-47.2933342138992,-71.6644126162078,
-216.803168697205));
#197965=CARTESIAN_POINT('Ctrl Pts',(-48.1524733410987,-73.0220158932609,
-215.351128153924));
#197966=CARTESIAN_POINT('Ctrl Pts',(-48.0843074405244,-73.1189108367624,
-213.190215709169));
#197967=CARTESIAN_POINT('Ctrl Pts',(-47.0905557676078,-71.7934728593478,
-216.824560386716));
#197968=CARTESIAN_POINT('Ctrl Pts',(-47.8674267413582,-73.2141877251378,
-215.374920075632));
#197969=CARTESIAN_POINT('Ctrl Pts',(-47.7383831769152,-73.3429891884114,
-213.20923907124));
#197970=CARTESIAN_POINT('',(-47.6826029798323,-71.3710801272351,-216.791855002172));
#197971=CARTESIAN_POINT('',(-48.7454044931547,-72.6086641314348,-213.184229057458));
#197972=CARTESIAN_POINT('Origin',(-45.5817163713881,-68.7378163165586,-213.096967025272));
#197973=CARTESIAN_POINT('Ctrl Pts',(-47.6826029798323,-71.3710801272352,
-216.791855002172));
#197974=CARTESIAN_POINT('Ctrl Pts',(-47.5930241853469,-71.4424241944854,
-216.791943540536));
#197975=CARTESIAN_POINT('Ctrl Pts',(-47.5017703583274,-71.5114565089323,
-216.794420184509));
#197976=CARTESIAN_POINT('Ctrl Pts',(-47.4089903165443,-71.5780732055786,
-216.799270679166));
#197977=CARTESIAN_POINT('Ctrl Pts',(-47.3150167558955,-71.6455468568316,
-216.804183570399));
#197978=CARTESIAN_POINT('Ctrl Pts',(-47.21947748162,-71.7105423794927,-216.811531734658));
#197979=CARTESIAN_POINT('Ctrl Pts',(-47.1225445138657,-71.7729893063581,
-216.821266633423));
#197980=CARTESIAN_POINT('Ctrl Pts',(-47.1118983132863,-71.7798478863064,
-216.82233582265));
#197981=CARTESIAN_POINT('Ctrl Pts',(-47.1012353177767,-71.7866757595247,
-216.823433769832));
#197982=CARTESIAN_POINT('Ctrl Pts',(-47.0905557676078,-71.7934728593478,
-216.824560386716));
#197983=CARTESIAN_POINT('Origin',(-42.892397296669,-65.4915301102559,-217.548968570462));
#197984=CARTESIAN_POINT('Ctrl Pts',(-48.7454044931547,-72.6086641314348,
-213.184229057458));
#197985=CARTESIAN_POINT('Ctrl Pts',(-48.7033558856732,-72.5944415704724,
-215.339600005589));
#197986=CARTESIAN_POINT('Ctrl Pts',(-47.6826029798322,-71.3710801272353,
-216.791855002172));
#197987=CARTESIAN_POINT('Ctrl Pts',(-49.8084038141049,-71.7395463911352,
-213.19825784801));
#197988=CARTESIAN_POINT('Ctrl Pts',(-49.7617328576239,-71.7299417528012,
-215.340395531801));
#197989=CARTESIAN_POINT('Ctrl Pts',(-48.7278636856231,-70.5385934819214,
-216.79082188204));
#197990=CARTESIAN_POINT('Ctrl Pts',(-50.8549407258151,-70.835967150169,
-213.213888015999));
#197991=CARTESIAN_POINT('Ctrl Pts',(-50.8130965389169,-70.8232845235791,
-215.341943634174));
#197992=CARTESIAN_POINT('Ctrl Pts',(-49.772756291054,-69.6608348552585,
-216.790293600156));
#197993=CARTESIAN_POINT('Ctrl Pts',(-51.8687937432179,-69.9121576054873,
-213.227785479717));
#197994=CARTESIAN_POINT('Ctrl Pts',(-51.8269633350129,-69.9002951910831,
-215.34395680141));
#197995=CARTESIAN_POINT('Ctrl Pts',(-50.7746555306532,-68.7687177611616,
-216.79041881877));
#197996=CARTESIAN_POINT('Origin',(-46.9277583887874,-69.2440043695137,-216.824274994638));
#197997=CARTESIAN_POINT('Ctrl Pts',(-48.7454044931547,-72.6086641314348,
-213.184229057458));
#197998=CARTESIAN_POINT('Ctrl Pts',(-49.8020589781625,-71.7447339856784,
-213.198174112891));
#197999=CARTESIAN_POINT('Ctrl Pts',(-50.8424469892599,-70.8467524994813,
-213.213701486193));
#198000=CARTESIAN_POINT('Ctrl Pts',(-51.8506358032439,-69.9286975854465,
-213.227536545096));
#198001=CARTESIAN_POINT('Origin',(5.34244157628528E-6,47.3246585720436,
-196.660871591801));
#198002=CARTESIAN_POINT('',(0.,53.3225191912041,-213.879601465234));
#198003=CARTESIAN_POINT('',(-1.6965687653276E-15,52.4792326277482,-216.572278947217));
#198004=CARTESIAN_POINT('Origin',(1.82415280199159E-13,48.3232807154221,
-213.792339433049));
#198005=CARTESIAN_POINT('',(-0.0544835933803365,52.4792219709058,-216.572215033819));
#198006=CARTESIAN_POINT('Origin',(-0.0318049166815379,52.4691014048544,
-216.511517174968));
#198007=CARTESIAN_POINT('',(-0.0473571427401393,53.3225154460666,-213.879539002147));
#198008=CARTESIAN_POINT('Origin',(-0.0463362411570871,48.3232770745245,
-213.79227696996));
#198009=CARTESIAN_POINT('Origin',(-0.46976145343121,53.0041184688829,-208.56971754274));
#198010=CARTESIAN_POINT('Ctrl Pts',(-0.0544838121610982,52.4791654811938,
-216.572299482171));
#198011=CARTESIAN_POINT('Ctrl Pts',(-0.0513170628758878,53.2968486113713,
-215.349944618211));
#198012=CARTESIAN_POINT('Ctrl Pts',(-0.0473571427401181,53.3225154460666,
-213.879539002147));
#198013=CARTESIAN_POINT('Ctrl Pts',(-1.72631364479056,52.4785114930465,
-216.568377409431));
#198014=CARTESIAN_POINT('Ctrl Pts',(-1.6261124312647,53.2965689361806,-215.346119637512));
#198015=CARTESIAN_POINT('Ctrl Pts',(-1.50078629177953,53.3222855571144,
-213.875705279281));
#198016=CARTESIAN_POINT('Ctrl Pts',(-3.36619303951308,52.4477003743405,
-216.38454765132));
#198017=CARTESIAN_POINT('Ctrl Pts',(-3.17354336684182,53.2833995412461,
-215.166295535093));
#198018=CARTESIAN_POINT('Ctrl Pts',(-2.92702243085717,53.3114912412646,
-213.695947807356));
#198019=CARTESIAN_POINT('Ctrl Pts',(-5.02403903766868,52.3888604794127,
-216.029604597611));
#198020=CARTESIAN_POINT('Ctrl Pts',(-4.73705181005364,53.2579964078456,
-214.820557484925));
#198021=CARTESIAN_POINT('Ctrl Pts',(-4.37281940663811,53.2905575229658,
-213.348880503444));
#198022=CARTESIAN_POINT('Ctrl Pts',(-5.07424920625965,52.3870512560605,
-216.018691745657));
#198023=CARTESIAN_POINT('Ctrl Pts',(-4.78447983975736,53.2572141001589,
-214.809911386444));
#198024=CARTESIAN_POINT('Ctrl Pts',(-4.4166077184939,53.289913868413,-213.338209943704));
#198025=CARTESIAN_POINT('Ctrl Pts',(-5.1369792265556,52.3847567936962,-216.004854723837));
#198026=CARTESIAN_POINT('Ctrl Pts',(-4.84373380419663,53.2562221185161,
-214.79641336836));
#198027=CARTESIAN_POINT('Ctrl Pts',(-4.47131352346949,53.2890977177666,
-213.324680435774));
#198028=CARTESIAN_POINT('Ctrl Pts',(-5.14483151826084,52.385083371175,-216.002211218262));
#198029=CARTESIAN_POINT('Ctrl Pts',(-4.8529857001896,53.2560738876406,-214.793661486801));
#198030=CARTESIAN_POINT('Ctrl Pts',(-4.48225430767022,53.2889337622212,
-213.321972140265));
#198031=CARTESIAN_POINT('Ctrl Pts',(-5.16354659654888,52.3852300457096,
-215.996869330628));
#198032=CARTESIAN_POINT('Ctrl Pts',(-4.87315904092074,53.2557430575767,
-214.788216412269));
#198033=CARTESIAN_POINT('Ctrl Pts',(-4.50414007083122,53.2886037420393,
-213.316582951083));
#198034=CARTESIAN_POINT('Ctrl Pts',(-5.17290526355219,52.3853021345043,
-215.994206794316));
#198035=CARTESIAN_POINT('Ctrl Pts',(-4.88324702370802,53.2555768088776,
-214.78550260211));
#198036=CARTESIAN_POINT('Ctrl Pts',(-4.51508431353993,53.2884377751688,
-213.313897267951));
#198037=CARTESIAN_POINT('Ctrl Pts',(-5.20098465409101,52.385514651656,-215.986244424357));
#198038=CARTESIAN_POINT('Ctrl Pts',(-4.91351451474929,53.2550755663235,
-214.777387478169));
#198039=CARTESIAN_POINT('Ctrl Pts',(-4.54792112758205,53.2879370021236,
-213.30586696962));
#198040=CARTESIAN_POINT('Ctrl Pts',(-5.21970876708894,52.38565133079,-215.980969829665));
#198041=CARTESIAN_POINT('Ctrl Pts',(-4.93369836198372,53.254738063078,-214.772012254543));
#198042=CARTESIAN_POINT('Ctrl Pts',(-4.56981778482713,53.2875993235168,
-213.300549105442));
#198043=CARTESIAN_POINT('Ctrl Pts',(-5.31335200957375,52.3863096810235,
-215.954765336006));
#198044=CARTESIAN_POINT('Ctrl Pts',(-5.03463605558215,53.253033966418,-214.745313113829));
#198045=CARTESIAN_POINT('Ctrl Pts',(-4.67932834466443,53.2858917529302,
-213.274138348232));
#198046=CARTESIAN_POINT('Ctrl Pts',(-5.38833916300533,52.3867562150194,
-215.934340872373));
#198047=CARTESIAN_POINT('Ctrl Pts',(-5.11547694549389,53.2516171105571,
-214.724511598889));
#198048=CARTESIAN_POINT('Ctrl Pts',(-4.76702406702058,53.2844643286531,
-213.253581139954));
#198049=CARTESIAN_POINT('Ctrl Pts',(-5.61352154702286,52.3878534578465,
-215.874693437342));
#198050=CARTESIAN_POINT('Ctrl Pts',(-5.35822907168792,53.2472055317345,
-214.663801477364));
#198051=CARTESIAN_POINT('Ctrl Pts',(-5.03037439099589,53.2799968687432,
-213.193632432869));
#198052=CARTESIAN_POINT('Ctrl Pts',(-5.76393762412216,52.3882617916828,
-215.837096372224));
#198053=CARTESIAN_POINT('Ctrl Pts',(-5.52042156751042,53.2440489818281,
-214.625572928414));
#198054=CARTESIAN_POINT('Ctrl Pts',(-5.20629213894649,53.2767716505112,
-213.155963782957));
#198055=CARTESIAN_POINT('Ctrl Pts',(-6.21609808576436,52.3885024391131,
-215.730879287284));
#198056=CARTESIAN_POINT('Ctrl Pts',(-6.00793734859214,53.2339271751484,
-214.517735436117));
#198057=CARTESIAN_POINT('Ctrl Pts',(-5.7351090490271,53.2663464299268,-213.049921731156));
#198058=CARTESIAN_POINT('Ctrl Pts',(-6.51897325761332,52.3873481165059,
-215.6687950942));
#198059=CARTESIAN_POINT('Ctrl Pts',(-6.33464333385786,53.226300180748,-214.45488048842));
#198060=CARTESIAN_POINT('Ctrl Pts',(-6.08932836962055,53.2583903798102,
-212.988474563998));
#198061=CARTESIAN_POINT('Ctrl Pts',(-7.43009426840034,52.3798510205839,
-215.509670650059));
#198062=CARTESIAN_POINT('Ctrl Pts',(-7.31716856464453,53.2007824433048,
-214.294545088556));
#198063=CARTESIAN_POINT('Ctrl Pts',(-7.15467547994453,53.2314932970166,
-212.832839779496));
#198064=CARTESIAN_POINT('Ctrl Pts',(-8.03670071712731,52.3695847260312,
-215.440224224832));
#198065=CARTESIAN_POINT('Ctrl Pts',(-7.97197058059872,53.1803550515563,
-214.225561760305));
#198066=CARTESIAN_POINT('Ctrl Pts',(-7.86408306340235,53.2096427750673,
-212.767811172676));
#198067=CARTESIAN_POINT('Ctrl Pts',(-9.85173860809738,52.3231412296717,
-215.343152516339));
#198068=CARTESIAN_POINT('Ctrl Pts',(-9.93187025910714,53.108960624321,-214.134202008953));
#198069=CARTESIAN_POINT('Ctrl Pts',(-9.98981135051243,53.1323666949439,
-212.690409355922));
#198070=CARTESIAN_POINT('Ctrl Pts',(-11.0568111525605,52.2713911945477,
-215.42554273729));
#198071=CARTESIAN_POINT('Ctrl Pts',(-11.2368319229789,53.0477276627447,
-214.225816329401));
#198072=CARTESIAN_POINT('Ctrl Pts',(-11.4039030903532,53.0652276040471,
-212.794256396899));
#198073=CARTESIAN_POINT('Ctrl Pts',(-12.5473914277697,52.1795355667477,
-215.729436635764));
#198074=CARTESIAN_POINT('Ctrl Pts',(-12.8548033121088,52.9546875149451,
-214.549327186523));
#198075=CARTESIAN_POINT('Ctrl Pts',(-13.1664443334459,52.9616798229913,
-213.138287858349));
#198076=CARTESIAN_POINT('Ctrl Pts',(-12.8444100738279,52.1598101428135,
-215.800296334662));
#198077=CARTESIAN_POINT('Ctrl Pts',(-13.1775953389357,52.935263628279,-214.624547564513));
#198078=CARTESIAN_POINT('Ctrl Pts',(-13.5182905195363,52.9400113359771,
-213.217839110357));
#198079=CARTESIAN_POINT('Ctrl Pts',(-13.1588676265443,52.1373853379567,
-215.886637060861));
#198080=CARTESIAN_POINT('Ctrl Pts',(-13.5195142127268,52.9137765318947,
-214.715953380887));
#198081=CARTESIAN_POINT('Ctrl Pts',(-13.8914034372555,52.9159732378538,
-213.314153161469));
#198082=CARTESIAN_POINT('Ctrl Pts',(-13.1773609898638,52.1360608428166,
-215.891756568308));
#198083=CARTESIAN_POINT('Ctrl Pts',(-13.5396265714153,52.9125092524799,
-214.72137332412));
#198084=CARTESIAN_POINT('Ctrl Pts',(-13.913348594832,52.9145554991733,-213.319862053586));
#198085=CARTESIAN_POINT('Ctrl Pts',(-13.2143394524504,52.1334010639901,
-215.902077029165));
#198086=CARTESIAN_POINT('Ctrl Pts',(-13.5798441312398,52.9099684160984,
-214.732298003386));
#198087=CARTESIAN_POINT('Ctrl Pts',(-13.9572335779769,52.911712557551,-213.331366738555));
#198088=CARTESIAN_POINT('Ctrl Pts',(-13.2429336797444,52.1319007516476,
-215.909182860407));
#198089=CARTESIAN_POINT('Ctrl Pts',(-13.6054337990796,52.9083475768503,
-214.73874381139));
#198090=CARTESIAN_POINT('Ctrl Pts',(-13.9791751707463,52.9102878010619,
-213.337130942174));
#198091=CARTESIAN_POINT('Ctrl Pts',(-13.3196525905457,52.1275217648837,
-215.928540678133));
#198092=CARTESIAN_POINT('Ctrl Pts',(-13.6772913107925,52.9037880649127,
-214.756990320156));
#198093=CARTESIAN_POINT('Ctrl Pts',(-14.0450114907347,52.9060072619919,
-213.354204614097));
#198094=CARTESIAN_POINT('Ctrl Pts',(-13.3707958087157,52.1245713270207,
-215.94124689702));
#198095=CARTESIAN_POINT('Ctrl Pts',(-13.7251992193788,52.9007367776418,
-214.76896183255));
#198096=CARTESIAN_POINT('Ctrl Pts',(-14.088912169659,52.9031437987813,-213.36539506595));
#198097=CARTESIAN_POINT('Ctrl Pts',(-13.5242193311591,52.1156270333207,
-215.978772604734));
#198098=CARTESIAN_POINT('Ctrl Pts',(-13.8689295059075,52.891548129523,-214.804300670642));
#198099=CARTESIAN_POINT('Ctrl Pts',(-14.2206434120783,52.894523997485,-213.398393774552));
#198100=CARTESIAN_POINT('Ctrl Pts',(-13.6264935272095,52.109540209161,-216.002999208033));
#198101=CARTESIAN_POINT('Ctrl Pts',(-13.9647632011014,52.8853756812463,
-214.827093567687));
#198102=CARTESIAN_POINT('Ctrl Pts',(-14.3085031783526,52.8887382469479,
-213.419629432868));
#198103=CARTESIAN_POINT('Ctrl Pts',(-13.9333070017177,52.0909102906718,
-216.07333725522));
#198104=CARTESIAN_POINT('Ctrl Pts',(-14.2523014370409,52.8667178365155,
-214.893197226102));
#198105=CARTESIAN_POINT('Ctrl Pts',(-14.5721978639792,52.8712625751263,
-213.481070862543));
#198106=CARTESIAN_POINT('Ctrl Pts',(-14.1378374819569,52.0779979063538,
-216.117107824054));
#198107=CARTESIAN_POINT('Ctrl Pts',(-14.4440621069193,52.8540907200264,
-214.934238234567));
#198108=CARTESIAN_POINT('Ctrl Pts',(-14.7481481314415,52.8594542225781,
-213.519011772409));
#198109=CARTESIAN_POINT('Ctrl Pts',(-15.1606137321987,52.0109959618191,
-216.320693501189));
#198110=CARTESIAN_POINT('Ctrl Pts',(-15.4032365304224,52.7900018371231,
-215.124595810338));
#198111=CARTESIAN_POINT('Ctrl Pts',(-15.628651977767,52.799613377438,-213.693903709864));
#198112=CARTESIAN_POINT('Ctrl Pts',(-15.9800466985321,51.9494919248635,
-216.434735900354));
#198113=CARTESIAN_POINT('Ctrl Pts',(-16.1727115912884,52.7356122605164,
-215.22941057846));
#198114=CARTESIAN_POINT('Ctrl Pts',(-16.3354684202618,52.7491845407374,
-213.786320807126));
#198115=CARTESIAN_POINT('Ctrl Pts',(-18.4347031718877,51.7430432922917,
-216.639213100253));
#198116=CARTESIAN_POINT('Ctrl Pts',(-18.4831202248674,52.5631013698916,
-215.410445297568));
#198117=CARTESIAN_POINT('Ctrl Pts',(-18.4626009436692,52.5898921039121,
-213.930740442329));
#198118=CARTESIAN_POINT('Ctrl Pts',(-20.0708093960321,51.5754935237252,
-216.5932389759));
#198119=CARTESIAN_POINT('Ctrl Pts',(-20.0302851577021,52.4352453396046,
-215.353542049237));
#198120=CARTESIAN_POINT('Ctrl Pts',(-19.8895768543743,52.4730122776837,
-213.850322288872));
#198121=CARTESIAN_POINT('Ctrl Pts',(-22.106942925778,51.3343802180279,-216.337037616295));
#198122=CARTESIAN_POINT('Ctrl Pts',(-21.961050385352,52.2595837051689,-215.091027749643));
#198123=CARTESIAN_POINT('Ctrl Pts',(-21.6827252055939,52.3125514421292,
-213.558099210826));
#198124=CARTESIAN_POINT('Ctrl Pts',(-22.5140029611996,51.2845488712585,
-216.275810860144));
#198125=CARTESIAN_POINT('Ctrl Pts',(-22.3483346833126,52.2235374473467,
-215.028730453821));
#198126=CARTESIAN_POINT('Ctrl Pts',(-22.042080438038,52.2797161015951,-213.490009648206));
#198127=CARTESIAN_POINT('Ctrl Pts',(-23.020123969084,51.2205746604136,-216.187808497287));
#198128=CARTESIAN_POINT('Ctrl Pts',(-22.830207401887,52.1776766786295,-214.939815041818));
#198129=CARTESIAN_POINT('Ctrl Pts',(-22.4896859299856,52.237965427953,-213.393843363057));
#198130=CARTESIAN_POINT('Ctrl Pts',(-23.1212414946463,51.207692183615,-216.169631097871));
#198131=CARTESIAN_POINT('Ctrl Pts',(-22.9265597686305,52.1684559716392,
-214.921463855732));
#198132=CARTESIAN_POINT('Ctrl Pts',(-22.5791527085491,52.2295777954781,
-213.374053497716));
#198133=CARTESIAN_POINT('Ctrl Pts',(-23.2475111366351,51.1914790355507,
-216.146197182102));
#198134=CARTESIAN_POINT('Ctrl Pts',(-23.0468999380045,52.1568764972718,
-214.897838328728));
#198135=CARTESIAN_POINT('Ctrl Pts',(-22.690919027762,52.2190463850866,-213.34862868516));
#198136=CARTESIAN_POINT('Ctrl Pts',(-23.2727587011446,51.1882309027779,
-216.141474787588));
#198137=CARTESIAN_POINT('Ctrl Pts',(-23.0709668523537,52.1545575467334,
-214.893078113741));
#198138=CARTESIAN_POINT('Ctrl Pts',(-22.7132689336659,52.216937759573,-213.343509345961));
#198139=CARTESIAN_POINT('Ctrl Pts',(-23.3106206153721,51.1833504374298,
-216.134337938203));
#198140=CARTESIAN_POINT('Ctrl Pts',(-23.1070601888508,52.1510750563128,
-214.885886361002));
#198141=CARTESIAN_POINT('Ctrl Pts',(-22.7467887689227,52.2137713063518,
-213.335778919634));
#198142=CARTESIAN_POINT('Ctrl Pts',(-23.323239681318,51.1817222379552,-216.131950112096));
#198143=CARTESIAN_POINT('Ctrl Pts',(-23.1190905197751,52.1499135108851,
-214.88348045923));
#198144=CARTESIAN_POINT('Ctrl Pts',(-22.7579612100687,52.2127152361208,
-213.333193541222));
#198145=CARTESIAN_POINT('Ctrl Pts',(-23.3484746877927,51.1784630815982,
-216.127156733402));
#198146=CARTESIAN_POINT('Ctrl Pts',(-23.143149110136,52.1475890391182,-214.878651485124));
#198147=CARTESIAN_POINT('Ctrl Pts',(-22.7803044200115,52.2106019240511,
-213.328005669353));
#198148=CARTESIAN_POINT('Ctrl Pts',(-23.3634428804975,51.1759647735806,
-216.125067970779));
#198149=CARTESIAN_POINT('Ctrl Pts',(-23.1565316045267,52.1462872653411,
-214.876515197103));
#198150=CARTESIAN_POINT('Ctrl Pts',(-22.7914750239788,52.2095447316335,
-213.325401286811));
#198151=CARTESIAN_POINT('Ctrl Pts',(-23.4120169921601,51.1731488430113,
-216.111042278681));
#198152=CARTESIAN_POINT('Ctrl Pts',(-23.2083148973916,52.1413255461524,
-214.862589766122));
#198153=CARTESIAN_POINT('Ctrl Pts',(-22.8473256024096,52.204255320697,-213.312356521225));
#198154=CARTESIAN_POINT('Ctrl Pts',(-23.4508800621557,51.1708771222298,
-216.099941976412));
#198155=CARTESIAN_POINT('Ctrl Pts',(-23.2497524300108,52.1373416940334,
-214.851574226443));
#198156=CARTESIAN_POINT('Ctrl Pts',(-22.8920158443542,52.2000074805641,
-213.302049206936));
#198157=CARTESIAN_POINT('Ctrl Pts',(-23.6452138197032,51.1594235544229,
-216.045044240048));
#198158=CARTESIAN_POINT('Ctrl Pts',(-23.4569298224344,52.1173561427463,
-214.797140469721));
#198159=CARTESIAN_POINT('Ctrl Pts',(-23.1155161868917,52.1786865508139,
-213.251157958141));
#198160=CARTESIAN_POINT('Ctrl Pts',(-23.8007397230343,51.1499568445754,
-216.003057863675));
#198161=CARTESIAN_POINT('Ctrl Pts',(-23.6228464558013,52.1011357232831,
-214.755597580258));
#198162=CARTESIAN_POINT('Ctrl Pts',(-23.2944736580691,52.1613682854175,
-213.212509671925));
#198163=CARTESIAN_POINT('Ctrl Pts',(-24.5786315814621,51.1010976638087,
-215.802956909761));
#198164=CARTESIAN_POINT('Ctrl Pts',(-24.4522745552879,52.0189656145359,
-214.558346148694));
#198165=CARTESIAN_POINT('Ctrl Pts',(-24.1900632291284,52.0734578840123,
-213.029785590209));
#198166=CARTESIAN_POINT('Ctrl Pts',(-25.2017886349748,51.057136405924,-215.674251388706));
#198167=CARTESIAN_POINT('Ctrl Pts',(-25.1186390175671,51.9494941764341,
-214.433049242548));
#198168=CARTESIAN_POINT('Ctrl Pts',(-24.9090934498146,51.9989121398783,
-212.917162893819));
#198169=CARTESIAN_POINT('Ctrl Pts',(-26.4489126716066,50.9591801161871,
-215.485243101151));
#198170=CARTESIAN_POINT('Ctrl Pts',(-26.4549089350885,51.8030345541437,
-214.254227764677));
#198171=CARTESIAN_POINT('Ctrl Pts',(-26.3528137916878,51.8410386164186,
-212.765468959114));
#198172=CARTESIAN_POINT('Ctrl Pts',(-27.0728715321185,50.905194894437,-215.424895423793));
#198173=CARTESIAN_POINT('Ctrl Pts',(-27.1250812825516,51.7260329324047,
-214.200467363498));
#198174=CARTESIAN_POINT('Ctrl Pts',(-27.0774998387683,51.7577126118315,
-212.726350375003));
#198175=CARTESIAN_POINT('Ctrl Pts',(-28.0085736911846,50.8162816305668,
-215.391931350205));
#198176=CARTESIAN_POINT('Ctrl Pts',(-28.1331634770288,51.6046724004521,
-214.180352486964));
#198177=CARTESIAN_POINT('Ctrl Pts',(-28.1693846366018,51.6257897144443,
-212.730030329888));
#198178=CARTESIAN_POINT('Ctrl Pts',(-28.3204349415701,50.7853183616886,
-215.390561027108));
#198179=CARTESIAN_POINT('Ctrl Pts',(-28.4695064538021,51.5632633940243,
-214.183737492164));
#198180=CARTESIAN_POINT('Ctrl Pts',(-28.5341580008858,51.5806587006086,
-212.741678726193));
#198181=CARTESIAN_POINT('Ctrl Pts',(-28.9439153079118,50.7206314629095,
-215.408483182069));
#198182=CARTESIAN_POINT('Ctrl Pts',(-29.1429916828581,51.4784709974454,
-214.212257584902));
#198183=CARTESIAN_POINT('Ctrl Pts',(-29.2654690941946,51.4880085266708,
-212.78747147059));
#198184=CARTESIAN_POINT('Ctrl Pts',(-29.2565395236243,50.686794162671,-215.427879478665));
#198185=CARTESIAN_POINT('Ctrl Pts',(-29.4812692925636,51.4349391049166,
-214.237504523825));
#198186=CARTESIAN_POINT('Ctrl Pts',(-29.6331976033025,51.4403305324129,
-212.821772692263));
#198187=CARTESIAN_POINT('Ctrl Pts',(-30.806459665517,50.5117195096438,-215.579673099401));
#198188=CARTESIAN_POINT('Ctrl Pts',(-31.1599649096486,51.2141679617287,
-214.421214926244));
#198189=CARTESIAN_POINT('Ctrl Pts',(-31.462411304102,51.1976497020186,-213.05276291922));
#198190=CARTESIAN_POINT('Ctrl Pts',(-31.9843584339507,50.3555651024278,
-215.871251464859));
#198191=CARTESIAN_POINT('Ctrl Pts',(-32.4487874910326,51.0294672908337,
-214.747007973179));
#198192=CARTESIAN_POINT('Ctrl Pts',(-32.8718379543183,50.9930622692594,
-213.421070504801));
#198193=CARTESIAN_POINT('Ctrl Pts',(-33.0838397730299,50.1837035797222,
-216.356359025309));
#198194=CARTESIAN_POINT('Ctrl Pts',(-33.6643488510553,50.8420575943128,
-215.277907585224));
#198195=CARTESIAN_POINT('Ctrl Pts',(-34.2185104850841,50.7818638678805,
-214.004031647198));
#198196=CARTESIAN_POINT('',(-5.13104565674618,52.3850329666526,-216.006074884366));
#198197=CARTESIAN_POINT('',(-13.2064804354037,52.1340237047487,-215.899796183989));
#198198=CARTESIAN_POINT('Ctrl Pts',(-5.13104565674618,52.3850329666526,
-216.006074884366));
#198199=CARTESIAN_POINT('Ctrl Pts',(-5.13996129572555,52.3849305551879,
-216.003777638489));
#198200=CARTESIAN_POINT('Ctrl Pts',(-5.14656866651012,52.3851571564325,
-216.001626363912));
#198201=CARTESIAN_POINT('Ctrl Pts',(-5.16352658620013,52.3852900305971,
-215.996786043511));
#198202=CARTESIAN_POINT('Ctrl Pts',(-5.19160273719641,52.3855062500636,
-215.988798420711));
#198203=CARTESIAN_POINT('Ctrl Pts',(-5.21968905682423,52.3857112220787,
-215.980886515042));
#198204=CARTESIAN_POINT('Ctrl Pts',(-5.31333279951823,52.3863694172317,
-215.954681976519));
#198205=CARTESIAN_POINT('Ctrl Pts',(-5.38832035449837,52.3868158288539,
-215.93425747843));
#198206=CARTESIAN_POINT('Ctrl Pts',(-5.61350394434034,52.3879127096803,
-215.874609945188));
#198207=CARTESIAN_POINT('Ctrl Pts',(-5.76392083021292,52.3883208090405,
-215.837012820505));
#198208=CARTESIAN_POINT('Ctrl Pts',(-6.2160837221702,52.3885607740694,-215.730795577584));
#198209=CARTESIAN_POINT('Ctrl Pts',(-6.51896053409861,52.3874060244112,
-215.668711303004));
#198210=CARTESIAN_POINT('Ctrl Pts',(-7.43008646643842,52.3799077366994,
-215.509586698213));
#198211=CARTESIAN_POINT('Ctrl Pts',(-8.036696242775,52.3696407673332,-215.440140264245));
#198212=CARTESIAN_POINT('Ctrl Pts',(-9.85174415293088,52.3231956049535,
-215.343068860401));
#198213=CARTESIAN_POINT('Ctrl Pts',(-11.056823612227,52.2714449257332,-215.425459700954));
#198214=CARTESIAN_POINT('Ctrl Pts',(-12.5474126952812,52.1795891926595,
-215.729354992607));
#198215=CARTESIAN_POINT('Ctrl Pts',(-12.8444331215652,52.1598637829641,
-215.800215003222));
#198216=CARTESIAN_POINT('Ctrl Pts',(-13.1588925696086,52.1374390337435,
-215.886556093702));
#198217=CARTESIAN_POINT('Ctrl Pts',(-13.1773860446445,52.1361145420097,
-215.891675622758));
#198218=CARTESIAN_POINT('Ctrl Pts',(-13.199128592437,52.1345506623852,-215.897743822643));
#198219=CARTESIAN_POINT('Ctrl Pts',(-13.2026946227731,52.1343113922399,
-215.898712001111));
#198220=CARTESIAN_POINT('Ctrl Pts',(-13.2064791900476,52.1340213385469,
-215.899799904774));
#198221=CARTESIAN_POINT('',(-23.3713119210585,51.1755743233668,-216.12270611168));
#198222=CARTESIAN_POINT('Ctrl Pts',(-13.206503688621,52.1340678863285,-215.899726709711));
#198223=CARTESIAN_POINT('Ctrl Pts',(-13.224334936536,52.1329279875711,-215.9044768025));
#198224=CARTESIAN_POINT('Ctrl Pts',(-13.2474589747328,52.1316975834026,
-215.910237414342));
#198225=CARTESIAN_POINT('Ctrl Pts',(-13.268531608982,52.1304947844112,-215.915554491141));
#198226=CARTESIAN_POINT('Ctrl Pts',(-13.3196773257302,52.1275754523624,
-215.928459650536));
#198227=CARTESIAN_POINT('Ctrl Pts',(-13.3708203204711,52.1246250082557,
-215.941165817504));
#198228=CARTESIAN_POINT('Ctrl Pts',(-13.4219612714471,52.121643572068,-215.953674335297));
#198229=CARTESIAN_POINT('Ctrl Pts',(-13.524243173399,52.1156806996926,-215.978691370885));
#198230=CARTESIAN_POINT('Ctrl Pts',(-13.6265169244848,52.1095938707609,
-216.002917873277));
#198231=CARTESIAN_POINT('Ctrl Pts',(-13.7287876386344,52.1033838982336,
-216.02636378994));
#198232=CARTESIAN_POINT('Ctrl Pts',(-13.9333290669337,52.0909639531789,
-216.073255623266));
#198233=CARTESIAN_POINT('Ctrl Pts',(-14.1378586642913,52.0780515896709,
-216.117026001651));
#198234=CARTESIAN_POINT('Ctrl Pts',(-14.3424130345253,52.0646512413527,
-216.157742953632));
#198235=CARTESIAN_POINT('Ctrl Pts',(-15.1606305154611,52.0110498480797,
-216.320610761555));
#198236=CARTESIAN_POINT('Ctrl Pts',(-15.9800600230911,51.9495462915113,
-216.43465254041));
#198237=CARTESIAN_POINT('Ctrl Pts',(-16.7982755207299,51.8807308388097,
-216.502811102887));
#198238=CARTESIAN_POINT('Ctrl Pts',(-18.4347065160074,51.7430999334064,
-216.639128227839));
#198239=CARTESIAN_POINT('Ctrl Pts',(-20.0708066016568,51.5755528046511,
-216.593153495422));
#198240=CARTESIAN_POINT('Ctrl Pts',(-21.6997076367388,51.3826656205631,
-216.388192261383));
#198241=CARTESIAN_POINT('Ctrl Pts',(-22.1069328955093,51.3344438245411,
-216.336951952873));
#198242=CARTESIAN_POINT('Ctrl Pts',(-22.5139915785022,51.2846133848892,
-216.275725177028));
#198243=CARTESIAN_POINT('Ctrl Pts',(-22.9188870606657,51.2334349680578,
-216.205323293599));
#198244=CARTESIAN_POINT('Ctrl Pts',(-23.0201109312066,51.2206403638499,
-216.187722822743));
#198245=CARTESIAN_POINT('Ctrl Pts',(-23.121228131896,51.2077581272943,-216.169545425857));
#198246=CARTESIAN_POINT('Ctrl Pts',(-23.2222435222512,51.1947878519363,
-216.150798297381));
#198247=CARTESIAN_POINT('Ctrl Pts',(-23.2474973698401,51.1915452830968,
-216.146111515263));
#198248=CARTESIAN_POINT('Ctrl Pts',(-23.2727448539233,51.1882972112394,
-216.141389121832));
#198249=CARTESIAN_POINT('Ctrl Pts',(-23.2979860497664,51.1850436287764,
-216.136631223406));
#198250=CARTESIAN_POINT('Ctrl Pts',(-23.310606647688,51.1834168375448,-216.134252274193));
#198251=CARTESIAN_POINT('Ctrl Pts',(-23.3232256735435,51.1817886686391,
-216.131864448716));
#198252=CARTESIAN_POINT('Ctrl Pts',(-23.3358431367254,51.1801591210892,
-216.129467759999));
#198253=CARTESIAN_POINT('Ctrl Pts',(-23.3476897986568,51.1786291226539,
-216.127217485076));
#198254=CARTESIAN_POINT('Ctrl Pts',(-23.3616086485301,51.1763333384333,
-216.125238663377));
#198255=CARTESIAN_POINT('Ctrl Pts',(-23.3713060248739,51.1755923752032,
-216.122683482436));
#198256=CARTESIAN_POINT('',(-32.9259640526745,50.2082425591298,-216.288164109342));
#198257=CARTESIAN_POINT('Ctrl Pts',(-23.3713119210585,51.1755743233668,
-216.12270611168));
#198258=CARTESIAN_POINT('Ctrl Pts',(-23.3719383148078,51.1755440742727,
-216.122516863379));
#198259=CARTESIAN_POINT('Ctrl Pts',(-23.3725507139463,51.1755024990986,
-216.122348351235));
#198260=CARTESIAN_POINT('Ctrl Pts',(-23.4120030149939,51.1732152730112,
-216.110956616071));
#198261=CARTESIAN_POINT('Ctrl Pts',(-23.4508662604922,51.1709434402525,
-216.099856312516));
#198262=CARTESIAN_POINT('Ctrl Pts',(-23.6452008940486,51.1594893141098,
-216.044958572661));
#198263=CARTESIAN_POINT('Ctrl Pts',(-23.8007275067389,51.1500221617809,
-216.002972199005));
#198264=CARTESIAN_POINT('Ctrl Pts',(-24.5786228904514,51.1011607936348,
-215.802871305082));
#198265=CARTESIAN_POINT('Ctrl Pts',(-25.2017829090892,51.0571978530063,
-215.674165918587));
#198266=CARTESIAN_POINT('Ctrl Pts',(-26.4489130852517,50.9592383471587,
-215.485158151918));
#198267=CARTESIAN_POINT('Ctrl Pts',(-27.0728751382963,50.9052515915225,
-215.424810848009));
#198268=CARTESIAN_POINT('Ctrl Pts',(-28.0085823077969,50.8163361552934,
-215.391847556155));
#198269=CARTESIAN_POINT('Ctrl Pts',(-28.3204452554017,50.7853721850659,
-215.390477529248));
#198270=CARTESIAN_POINT('Ctrl Pts',(-28.9439290913914,50.7206839329619,
-215.408400357933));
#198271=CARTESIAN_POINT('Ctrl Pts',(-29.2565550883999,50.6868459785135,
-215.427797032548));
#198272=CARTESIAN_POINT('Ctrl Pts',(-30.7473218723846,50.518451120397,-215.57379855617));
#198273=CARTESIAN_POINT('Ctrl Pts',(-31.8718448202371,50.3704768331421,
-215.843735990856));
#198274=CARTESIAN_POINT('Ctrl Pts',(-32.9259571993476,50.2082406704928,
-216.288179546395));
#198275=CARTESIAN_POINT('',(-33.8288256170145,50.8425199003324,-213.842075049522));
#198276=CARTESIAN_POINT('Ctrl Pts',(-33.8288255478926,50.8425194315114,
-213.842075041245));
#198277=CARTESIAN_POINT('Ctrl Pts',(-33.7970774697237,50.8454126628531,
-213.943330969591));
#198278=CARTESIAN_POINT('Ctrl Pts',(-33.7646338917884,50.8450038051801,
-214.044775431056));
#198279=CARTESIAN_POINT('Ctrl Pts',(-33.7315935110065,50.8412526174688,
-214.146057915126));
#198280=CARTESIAN_POINT('Ctrl Pts',(-33.6986141665251,50.837508359418,-214.247153297596));
#198281=CARTESIAN_POINT('Ctrl Pts',(-33.6650404319365,50.8304340345761,
-214.348086736041));
#198282=CARTESIAN_POINT('Ctrl Pts',(-33.6309839083423,50.8200397985673,
-214.448509146524));
#198283=CARTESIAN_POINT('Ctrl Pts',(-33.5969409221117,50.8096496942354,
-214.548891639407));
#198284=CARTESIAN_POINT('Ctrl Pts',(-33.5624157675524,50.7959423557587,
-214.648762951211));
#198285=CARTESIAN_POINT('Ctrl Pts',(-33.5275300116972,50.7789783952727,
-214.747782348801));
#198286=CARTESIAN_POINT('Ctrl Pts',(-33.4925921263582,50.761989085687,-214.846949710222));
#198287=CARTESIAN_POINT('Ctrl Pts',(-33.4572928164849,50.7417335604387,
-214.945262074432));
#198288=CARTESIAN_POINT('Ctrl Pts',(-33.4217606234739,50.718321968533,-215.0423933864));
#198289=CARTESIAN_POINT('Ctrl Pts',(-33.4122602220973,50.712062306488,-215.068363819737));
#198290=CARTESIAN_POINT('Ctrl Pts',(-33.4027431956259,50.7055772843654,
-215.094249934778));
#198291=CARTESIAN_POINT('Ctrl Pts',(-33.3932120420313,50.6988695765327,
-215.120045768538));
#198292=CARTESIAN_POINT('Ctrl Pts',(-33.355198383497,50.672116832222,-215.222928804308));
#198293=CARTESIAN_POINT('Ctrl Pts',(-33.3169504134669,50.6418178055739,
-215.324410349766));
#198294=CARTESIAN_POINT('Ctrl Pts',(-33.2784700659473,50.6080102934018,
-215.424514371539));
#198295=CARTESIAN_POINT('Ctrl Pts',(-33.2404166725892,50.5745778884971,
-215.523507700935));
#198296=CARTESIAN_POINT('Ctrl Pts',(-33.2021355491518,50.5377139435189,
-215.621154855899));
#198297=CARTESIAN_POINT('Ctrl Pts',(-33.1636281482726,50.4974055580181,
-215.717462013326));
#198298=CARTESIAN_POINT('Ctrl Pts',(-33.1244726752926,50.4564187901941,
-215.815390001565));
#198299=CARTESIAN_POINT('Ctrl Pts',(-33.0850827260538,50.4118701743681,
-215.911933509871));
#198300=CARTESIAN_POINT('Ctrl Pts',(-33.0454669545182,50.3637017224098,
-216.00706645164));
#198301=CARTESIAN_POINT('Ctrl Pts',(-33.0058511829825,50.3155332704514,
-216.102199393409));
#198302=CARTESIAN_POINT('Ctrl Pts',(-32.9660090942418,50.2637441385916,
-216.195922559663));
#198303=CARTESIAN_POINT('Ctrl Pts',(-32.9259640526745,50.2082425591299,
-216.288164109342));
#198304=CARTESIAN_POINT('Ctrl Pts',(-33.8288255478898,50.8425194315119,
-213.842075041244));
#198305=CARTESIAN_POINT('Ctrl Pts',(-33.4284854297646,50.9043645560048,
-213.682497556561));
#198306=CARTESIAN_POINT('Ctrl Pts',(-33.0234151328446,50.9655031281662,
-213.541601729915));
#198307=CARTESIAN_POINT('Ctrl Pts',(-32.613891113486,51.0258461323052,-213.41828489294));
#198308=CARTESIAN_POINT('Ctrl Pts',(-32.3314320696816,51.0674662240305,
-213.33323016059));
#198309=CARTESIAN_POINT('Ctrl Pts',(-32.0468532024027,51.1087080491179,
-213.256538361901));
#198310=CARTESIAN_POINT('Ctrl Pts',(-31.760231540292,51.1495445945208,-213.187851585035));
#198311=CARTESIAN_POINT('Ctrl Pts',(-31.4098748863998,51.1994618104719,
-213.10389118535));
#198312=CARTESIAN_POINT('Ctrl Pts',(-31.0565047381091,51.2487669119008,
-213.031971638878));
#198313=CARTESIAN_POINT('Ctrl Pts',(-30.7001071876422,51.2974288982541,
-212.971577846918));
#198314=CARTESIAN_POINT('Ctrl Pts',(-30.4677048549224,51.3291607637747,
-212.932195819418));
#198315=CARTESIAN_POINT('Ctrl Pts',(-30.2340152995371,51.3606190826065,
-212.89771588442));
#198316=CARTESIAN_POINT('Ctrl Pts',(-29.9990356615488,51.3917943388598,
-212.868006986083));
#198317=CARTESIAN_POINT('Ctrl Pts',(-29.8721559396975,51.4086277456857,
-212.851965354604));
#198318=CARTESIAN_POINT('Ctrl Pts',(-29.7450788398495,51.4253538896652,
-212.837366281476));
#198319=CARTESIAN_POINT('Ctrl Pts',(-29.617962992439,51.4419530974049,-212.824189892615));
#198320=CARTESIAN_POINT('Ctrl Pts',(-29.3784059473116,51.4732352485967,
-212.799358238301));
#198321=CARTESIAN_POINT('Ctrl Pts',(-29.1386589564598,51.5040741022661,
-212.779534675774));
#198322=CARTESIAN_POINT('Ctrl Pts',(-28.899813341109,51.5343335838556,-212.764578265057));
#198323=CARTESIAN_POINT('Ctrl Pts',(-28.5341328390394,51.5806618465861,
-212.741679507747));
#198324=CARTESIAN_POINT('Ctrl Pts',(-28.1693740006546,51.6257909648441,
-212.730032265418));
#198325=CARTESIAN_POINT('Ctrl Pts',(-27.8054230251461,51.6697639760348,
-212.728805896948));
#198326=CARTESIAN_POINT('Ctrl Pts',(-27.2316173838903,51.7390918899084,
-212.72687240262));
#198327=CARTESIAN_POINT('Ctrl Pts',(-26.659813477437,51.8055490574399,-212.750767886994));
#198328=CARTESIAN_POINT('Ctrl Pts',(-26.0896437383804,51.8692665746801,
-212.798150758929));
#198329=CARTESIAN_POINT('Ctrl Pts',(-25.9366321166225,51.8863659048961,
-212.810866498789));
#198330=CARTESIAN_POINT('Ctrl Pts',(-25.783738207763,51.9032678957084,-212.825274044136));
#198331=CARTESIAN_POINT('Ctrl Pts',(-25.6309549565992,51.919975004434,-212.841328746581));
#198332=CARTESIAN_POINT('Ctrl Pts',(-25.5252626824023,51.9315326346259,
-212.852435055682));
#198333=CARTESIAN_POINT('Ctrl Pts',(-25.4196234520871,51.9429969636603,
-212.864330645339));
#198334=CARTESIAN_POINT('Ctrl Pts',(-25.3140353742909,51.954368608782,-212.877005898427));
#198335=CARTESIAN_POINT('Ctrl Pts',(-24.6986753884515,52.0206417669556,
-212.950876393311));
#198336=CARTESIAN_POINT('Ctrl Pts',(-24.0852465518143,52.0837464971762,
-213.051177399378));
#198337=CARTESIAN_POINT('Ctrl Pts',(-23.4735918363939,52.1437861556343,
-213.175966145474));
#198338=CARTESIAN_POINT('Ctrl Pts',(-23.3778558249174,52.1531835448578,
-213.195498042355));
#198339=CARTESIAN_POINT('Ctrl Pts',(-23.2821634538011,52.1625057785251,
-213.215631611061));
#198340=CARTESIAN_POINT('Ctrl Pts',(-23.186514300368,52.1717531873608,-213.236361158368));
#198341=CARTESIAN_POINT('Ctrl Pts',(-23.1032160300045,52.1798065065351,
-213.254413962539));
#198342=CARTESIAN_POINT('Ctrl Pts',(-23.0199493662676,52.1878031958512,
-213.27291866346));
#198343=CARTESIAN_POINT('Ctrl Pts',(-22.9367159200589,52.1957432933471,
-213.291870988623));
#198344=CARTESIAN_POINT('Ctrl Pts',(-22.8920159948608,52.2000074657478,
-213.302049198894));
#198345=CARTESIAN_POINT('Ctrl Pts',(-22.8473256517326,52.2042553156825,
-213.31235652924));
#198346=CARTESIAN_POINT('Ctrl Pts',(-22.8026451428253,52.2084868488979,
-213.322792347151));
#198347=CARTESIAN_POINT('Ctrl Pts',(-22.7914750218732,52.2095447316075,
-213.325401300163));
#198348=CARTESIAN_POINT('Ctrl Pts',(-22.7803044160517,52.2106019242221,
-213.328005681871));
#198349=CARTESIAN_POINT('Ctrl Pts',(-22.7691328173551,52.2116585796836,
-213.330599615203));
#198350=CARTESIAN_POINT('Ctrl Pts',(-22.7579612024765,52.2127152366757,
-213.333193552293));
#198351=CARTESIAN_POINT('Ctrl Pts',(-22.7467887595382,52.2137713070932,
-213.335778930067));
#198352=CARTESIAN_POINT('Ctrl Pts',(-22.7356154921234,52.2148267904768,
-213.338355735395));
#198353=CARTESIAN_POINT('Ctrl Pts',(-22.7132688713499,52.2169377653627,
-213.34350936587));
#198354=CARTESIAN_POINT('Ctrl Pts',(-22.690918952669,52.2190463920883,-213.348628706464));
#198355=CARTESIAN_POINT('Ctrl Pts',(-22.6685657646952,52.2211526670292,
-213.353713651063));
#198356=CARTESIAN_POINT('Ctrl Pts',(-22.6646488913256,52.2215217424486,
-213.354604668671));
#198357=CARTESIAN_POINT('Ctrl Pts',(-22.6607319175818,52.2218907456563,
-213.355494630255));
#198358=CARTESIAN_POINT('Ctrl Pts',(-22.6568148436157,52.2222596766335,
-213.356383535216));
#198359=CARTESIAN_POINT('Ctrl Pts',(-22.5713095630331,52.230313021297,-213.375787322021));
#198360=CARTESIAN_POINT('Ctrl Pts',(-22.4857590592482,52.2383317076775,
-213.394687120908));
#198361=CARTESIAN_POINT('Ctrl Pts',(-22.4001649179091,52.2463155472972,
-213.413077019702));
#198362=CARTESIAN_POINT('Ctrl Pts',(-22.3089921278341,52.2548197383815,
-213.432665491016));
#198363=CARTESIAN_POINT('Ctrl Pts',(-22.2177437865543,52.2632866458112,
-213.451679464809));
#198364=CARTESIAN_POINT('Ctrl Pts',(-22.1264553921399,52.2717131158806,
-213.470105691494));
#198365=CARTESIAN_POINT('Ctrl Pts',(-21.8592067817176,52.2963817764619,
-213.524048840657));
#198366=CARTESIAN_POINT('Ctrl Pts',(-21.5914443579229,52.3207197108699,
-213.572977568728));
#198367=CARTESIAN_POINT('Ctrl Pts',(-21.324095772452,52.3446435619462,-213.616545275384));
#198368=CARTESIAN_POINT('Ctrl Pts',(-21.2373298036558,52.3524078675337,
-213.630684846273));
#198369=CARTESIAN_POINT('Ctrl Pts',(-21.1505925461958,52.3601300382446,
-213.64426337592));
#198370=CARTESIAN_POINT('Ctrl Pts',(-21.0638877077023,52.367809951321,-213.657275547301));
#198371=CARTESIAN_POINT('Ctrl Pts',(-19.9403620371655,52.4673266523355,
-213.825887920386));
#198372=CARTESIAN_POINT('Ctrl Pts',(-18.8212977891659,52.5598365227201,
-213.899469703825));
#198373=CARTESIAN_POINT('Ctrl Pts',(-17.7073210864199,52.6457202413902,
-213.86667189224));
#198374=CARTESIAN_POINT('Ctrl Pts',(-17.4861825445344,52.6627692517255,
-213.860161109552));
#198375=CARTESIAN_POINT('Ctrl Pts',(-17.26524445948,52.6795571452203,-213.849458033042));
#198376=CARTESIAN_POINT('Ctrl Pts',(-17.0445116841459,52.6960869022231,
-213.834473635959));
#198377=CARTESIAN_POINT('Ctrl Pts',(-16.9763221692116,52.7011933306195,
-213.829844605372));
#198378=CARTESIAN_POINT('Ctrl Pts',(-16.9081523016014,52.7062751479287,
-213.824806041867));
#198379=CARTESIAN_POINT('Ctrl Pts',(-16.8400022396715,52.7113324526888,
-213.819355050391));
#198380=CARTESIAN_POINT('Ctrl Pts',(-16.1996233055735,52.7588539272107,
-213.768134258918));
#198381=CARTESIAN_POINT('Ctrl Pts',(-15.5609952942025,52.8042113945112,
-213.680469263933));
#198382=CARTESIAN_POINT('Ctrl Pts',(-14.9242487810738,52.8474860509722,
-213.553990748348));
#198383=CARTESIAN_POINT('Ctrl Pts',(-14.8649438022494,52.8515165443194,
-213.542210855512));
#198384=CARTESIAN_POINT('Ctrl Pts',(-14.8056550939682,52.8555289645465,
-213.53009494545));
#198385=CARTESIAN_POINT('Ctrl Pts',(-14.7463827693234,52.8595233836131,
-213.517640823917));
#198386=CARTESIAN_POINT('Ctrl Pts',(-14.6296583420251,52.8673895552326,
-213.493115040389));
#198387=CARTESIAN_POINT('Ctrl Pts',(-14.5129975854062,52.8751859177496,
-213.467277078931));
#198388=CARTESIAN_POINT('Ctrl Pts',(-14.3964014059856,52.8829130229972,
-213.440109913242));
#198389=CARTESIAN_POINT('Ctrl Pts',(-14.3392716131932,52.8866991498144,
-213.426798546143));
#198390=CARTESIAN_POINT('Ctrl Pts',(-14.2821573282444,52.8904686504834,
-213.413167990812));
#198391=CARTESIAN_POINT('Ctrl Pts',(-14.2250586750741,52.8942215948614,
-213.399215938864));
#198392=CARTESIAN_POINT('Ctrl Pts',(-14.1943088494084,52.8962427000705,
-213.391702221092));
#198393=CARTESIAN_POINT('Ctrl Pts',(-14.1635634419837,52.8982590111405,
-213.384095232765));
#198394=CARTESIAN_POINT('Ctrl Pts',(-14.1328225823483,52.9002705316721,
-213.376394641147));
#198395=CARTESIAN_POINT('Ctrl Pts',(-14.0889125166663,52.9031437759375,
-213.365395160724));
#198396=CARTESIAN_POINT('Ctrl Pts',(-14.0450117306304,52.9060072461915,
-213.354204687972));
#198397=CARTESIAN_POINT('Ctrl Pts',(-14.0011206054635,52.9088609546764,
-213.342822186058));
#198398=CARTESIAN_POINT('Ctrl Pts',(-13.97917518517,52.9102877996674,-213.337130972003));
#198399=CARTESIAN_POINT('Ctrl Pts',(-13.9572335774899,52.9117125570173,
-213.331366770807));
#198400=CARTESIAN_POINT('Ctrl Pts',(-13.9352910762425,52.9131340283109,
-213.325614433985));
#198401=CARTESIAN_POINT('Ctrl Pts',(-13.9133485638327,52.9145555003276,
-213.319862094238));
#198402=CARTESIAN_POINT('Ctrl Pts',(-13.8914033905366,52.9159732398363,
-213.314153208263));
#198403=CARTESIAN_POINT('Ctrl Pts',(-13.8694556009261,52.9173872435139,
-213.308487695886));
#198404=CARTESIAN_POINT('Ctrl Pts',(-13.814453489134,52.9209307980009,-213.294289676376));
#198405=CARTESIAN_POINT('Ctrl Pts',(-13.759434949972,52.9244508908472,-213.280363986675));
#198406=CARTESIAN_POINT('Ctrl Pts',(-13.7044006823105,52.9279474706966,
-213.266709421035));
#198407=CARTESIAN_POINT('Ctrl Pts',(-13.4080399531724,52.9467766292867,
-213.193179287882));
#198408=CARTESIAN_POINT('Ctrl Pts',(-13.1112381993239,52.9649231366514,
-213.127512319229));
#198409=CARTESIAN_POINT('Ctrl Pts',(-12.8139330465278,52.9823892815607,
-213.069496767474));
#198410=CARTESIAN_POINT('Ctrl Pts',(-12.762879858688,52.985388564851,-213.059534347269));
#198411=CARTESIAN_POINT('Ctrl Pts',(-12.7118203984012,52.9883673151379,
-213.049796876756));
#198412=CARTESIAN_POINT('Ctrl Pts',(-12.6607543476392,52.9913255531846,
-213.040283642668));
#198413=CARTESIAN_POINT('Ctrl Pts',(-11.9341248848113,53.0334189379416,
-212.904917855179));
#198414=CARTESIAN_POINT('Ctrl Pts',(-11.2065831243644,53.0713381842672,
-212.814853635294));
#198415=CARTESIAN_POINT('Ctrl Pts',(-10.4781602304721,53.1051020165539,
-212.767914849581));
#198416=CARTESIAN_POINT('Ctrl Pts',(-9.84364980408828,53.1345128214588,
-212.727027681994));
#198417=CARTESIAN_POINT('Ctrl Pts',(-9.20847120771161,53.1607704847659,
-212.718863838119));
#198418=CARTESIAN_POINT('Ctrl Pts',(-8.57265926894805,53.1838840251076,
-212.742013573981));
#198419=CARTESIAN_POINT('Ctrl Pts',(-8.53829774072196,53.1851331626599,
-212.743264667667));
#198420=CARTESIAN_POINT('Ctrl Pts',(-8.50393420974279,53.186373110042,-212.744608085481));
#198421=CARTESIAN_POINT('Ctrl Pts',(-8.46956866922752,53.1876038661027,
-212.746043776936));
#198422=CARTESIAN_POINT('Ctrl Pts',(-8.05134105999317,53.2025821308736,
-212.76351609939));
#198423=CARTESIAN_POINT('Ctrl Pts',(-7.63294373530001,53.2161951626093,
-212.794632608455));
#198424=CARTESIAN_POINT('Ctrl Pts',(-7.21417793555685,53.2284476001672,
-212.839302228768));
#198425=CARTESIAN_POINT('Ctrl Pts',(-6.95775348626208,53.2359501816941,
-212.866654946674));
#198426=CARTESIAN_POINT('Ctrl Pts',(-6.70119085797075,53.2429425029054,
-212.899090463671));
#198427=CARTESIAN_POINT('Ctrl Pts',(-6.44444424425753,53.2494246606916,
-212.936597453296));
#198428=CARTESIAN_POINT('Ctrl Pts',(-6.41857408693467,53.2500778122144,
-212.940376711406));
#198429=CARTESIAN_POINT('Ctrl Pts',(-6.39270791173976,53.2507256250243,
-212.944206865458));
#198430=CARTESIAN_POINT('Ctrl Pts',(-6.36684597343844,53.2513681007524,
-212.948087807708));
#198431=CARTESIAN_POINT('Ctrl Pts',(-6.07745447347717,53.2585573149735,
-212.991515012816));
#198432=CARTESIAN_POINT('Ctrl Pts',(-5.78889206506211,53.2650712747836,
-213.041253050323));
#198433=CARTESIAN_POINT('Ctrl Pts',(-5.50128321713575,53.2709193635982,
-213.097172231798));
#198434=CARTESIAN_POINT('Ctrl Pts',(-5.46169210092698,53.2717243887757,
-213.104869848988));
#198435=CARTESIAN_POINT('Ctrl Pts',(-5.4221190644421,53.2725167877183,-213.112684673472));
#198436=CARTESIAN_POINT('Ctrl Pts',(-5.38256444434725,53.2732965767615,
-213.120616442334));
#198437=CARTESIAN_POINT('Ctrl Pts',(-5.36110255433366,53.273719681487,-213.124920130513));
#198438=CARTESIAN_POINT('Ctrl Pts',(-5.33964513566361,53.2741390978143,
-213.129258387298));
#198439=CARTESIAN_POINT('Ctrl Pts',(-5.31819206008382,53.2745548325864,
-213.133631201848));
#198440=CARTESIAN_POINT('Ctrl Pts',(-5.16346960690779,53.2775531674209,
-213.165168525801));
#198441=CARTESIAN_POINT('Ctrl Pts',(-5.00900884762652,53.2803593125378,
-213.198496059744));
#198442=CARTESIAN_POINT('Ctrl Pts',(-4.85480750872648,53.2829751753132,
-213.233598239231));
#198443=CARTESIAN_POINT('Ctrl Pts',(-4.83548667519202,53.2833029328385,
-213.237996407052));
#198444=CARTESIAN_POINT('Ctrl Pts',(-4.81616991445761,53.2836277030469,
-213.242422436056));
#198445=CARTESIAN_POINT('Ctrl Pts',(-4.79685722222938,53.2839494896215,
-213.246876296773));
#198446=CARTESIAN_POINT('Ctrl Pts',(-4.7284277801666,53.2850896556584,-213.262657380025));
#198447=CARTESIAN_POINT('Ctrl Pts',(-4.66004791849701,53.2861923861427,
-213.278788317341));
#198448=CARTESIAN_POINT('Ctrl Pts',(-4.59171994251615,53.287257805251,-213.295267139756));
#198449=CARTESIAN_POINT('Ctrl Pts',(-4.56981793503112,53.2875993171567,
-213.300549299614));
#198450=CARTESIAN_POINT('Ctrl Pts',(-4.5479212585868,53.2879369954791,-213.305867203351));
#198451=CARTESIAN_POINT('Ctrl Pts',(-4.52602998880579,53.2882708445055,
-213.311220784633));
#198452=CARTESIAN_POINT('Ctrl Pts',(-4.51508439514851,53.2884377683898,
-213.313897565189));
#198453=CARTESIAN_POINT('Ctrl Pts',(-4.50414015314487,53.2886037349588,
-213.316583265059));
#198454=CARTESIAN_POINT('Ctrl Pts',(-4.49319727224013,53.2887687447573,
-213.319277875872));
#198455=CARTESIAN_POINT('Ctrl Pts',(-4.48225439119486,53.288933754558,-213.32197248672));
#198456=CARTESIAN_POINT('Ctrl Pts',(-4.47131360771902,53.2890977098182,
-213.324680797965));
#198457=CARTESIAN_POINT('Ctrl Pts',(-4.46037245702204,53.2892609395381,
-213.327386711908));
#198458=CARTESIAN_POINT('Ctrl Pts',(-4.41660743855001,53.2899138646194,
-213.338210470483));
#198459=CARTESIAN_POINT('Ctrl Pts',(-4.37281891468896,53.2905575212915,
-213.348881124148));
#198460=CARTESIAN_POINT('Ctrl Pts',(-4.32900749630775,53.2911918673437,
-213.359398181113));
#198461=CARTESIAN_POINT('Ctrl Pts',(-4.31174898704184,53.2914417535064,
-213.36354113589));
#198462=CARTESIAN_POINT('Ctrl Pts',(-4.29448693048956,53.2916901975378,
-213.367660294877));
#198463=CARTESIAN_POINT('Ctrl Pts',(-4.27722136169741,53.2919371969757,
-213.371755612804));
#198464=CARTESIAN_POINT('Ctrl Pts',(-3.34936233527052,53.305211052053,-213.591839743871));
#198465=CARTESIAN_POINT('Ctrl Pts',(-2.41131193880081,53.3143129931199,
-213.743095767743));
#198466=CARTESIAN_POINT('Ctrl Pts',(-1.46228217018108,53.3189491272515,
-213.820197476167));
#198467=CARTESIAN_POINT('Ctrl Pts',(-0.993352427707391,53.3212399101714,
-213.858294578566));
#198468=CARTESIAN_POINT('Ctrl Pts',(-0.521742197160567,53.3224404125564,
-213.878287712818));
#198469=CARTESIAN_POINT('Ctrl Pts',(-0.0473571427401393,53.3225154460666,
-213.879539002147));
#198470=CARTESIAN_POINT('Ctrl Pts',(-0.0544835933803345,52.4792219709059,
-216.57221503382));
#198471=CARTESIAN_POINT('Ctrl Pts',(-0.911160817479643,52.4788868661666,
-216.570205286074));
#198472=CARTESIAN_POINT('Ctrl Pts',(-1.76241895715707,52.4706614931604,
-216.520914925994));
#198473=CARTESIAN_POINT('Ctrl Pts',(-3.03147279341818,52.4469055640949,
-216.37863656052));
#198474=CARTESIAN_POINT('Ctrl Pts',(-3.45317987983679,52.437124954073,-216.319765648019));
#198475=CARTESIAN_POINT('Ctrl Pts',(-4.08382026129649,52.4196309296523,
-216.214709957797));
#198476=CARTESIAN_POINT('Ctrl Pts',(-4.29371035972386,52.4133485556671,
-216.176866822026));
#198477=CARTESIAN_POINT('Ctrl Pts',(-4.71285393159547,52.3998755739423,
-216.095622991724));
#198478=CARTESIAN_POINT('Ctrl Pts',(-4.92331707557612,52.3926407185815,
-216.051954867598));
#198479=CARTESIAN_POINT('Ctrl Pts',(-5.13104565674618,52.3850329666526,
-216.006074884366));
#198480=CARTESIAN_POINT('Ctrl Pts',(-33.4754093737626,49.9711874412034,
-216.637340091396));
#198481=CARTESIAN_POINT('Ctrl Pts',(-33.1531183251102,50.0508442845748,
-216.592238632432));
#198482=CARTESIAN_POINT('Ctrl Pts',(-32.8299704770403,50.0687939509079,
-216.505612191758));
#198483=CARTESIAN_POINT('Ctrl Pts',(-33.5583226571475,50.2807044023955,
-216.184599119136));
#198484=CARTESIAN_POINT('Ctrl Pts',(-33.2915590096021,50.3430190640451,
-216.141689042293));
#198485=CARTESIAN_POINT('Ctrl Pts',(-33.0227471817627,50.3616651708532,
-216.076225280147));
#198486=CARTESIAN_POINT('Ctrl Pts',(-33.6313141818038,50.506914657348,-215.69830350431));
#198487=CARTESIAN_POINT('Ctrl Pts',(-33.4219976724055,50.5521550190162,
-215.66141909055));
#198488=CARTESIAN_POINT('Ctrl Pts',(-33.2107462999537,50.5704649897337,
-215.613887593034));
#198489=CARTESIAN_POINT('Ctrl Pts',(-33.7472696093515,50.7753900150999,
-214.748451183307));
#198490=CARTESIAN_POINT('Ctrl Pts',(-33.6465861931775,50.793335292441,-214.728940081455));
#198491=CARTESIAN_POINT('Ctrl Pts',(-33.5452672954357,50.8058893973708,
-214.708515271655));
#198492=CARTESIAN_POINT('Ctrl Pts',(-33.7929819292232,50.8398470125736,
-214.293134446626));
#198493=CARTESIAN_POINT('Ctrl Pts',(-33.7432476178557,50.8473526001343,
-214.283376890363));
#198494=CARTESIAN_POINT('Ctrl Pts',(-33.6935058134431,50.8548585528471,
-214.273661258903));
#198495=CARTESIAN_POINT('Ctrl Pts',(-33.8288256585371,50.8425201819751,
-213.84207505449));
#198496=CARTESIAN_POINT('Ctrl Pts',(-33.8288256585371,50.8425201819751,
-213.84207505449));
#198497=CARTESIAN_POINT('Ctrl Pts',(-33.8288256585371,50.8425201819751,
-213.84207505449));
#198498=CARTESIAN_POINT('',(-33.5148860365099,50.1192982504879,-216.408010067648));
#198499=CARTESIAN_POINT('Ctrl Pts',(-33.828825603085,50.8425198058687,-213.84207504786));
#198500=CARTESIAN_POINT('Ctrl Pts',(-33.8198990676264,50.841864888462,-213.953795522105));
#198501=CARTESIAN_POINT('Ctrl Pts',(-33.8103998023479,50.8374948224705,
-214.066003151697));
#198502=CARTESIAN_POINT('Ctrl Pts',(-33.8003172610997,50.8293303724465,
-214.178318063006));
#198503=CARTESIAN_POINT('Ctrl Pts',(-33.7902347198515,50.8211659224224,
-214.290632974314));
#198504=CARTESIAN_POINT('Ctrl Pts',(-33.7795688729459,50.8092068754561,
-214.403054603578));
#198505=CARTESIAN_POINT('Ctrl Pts',(-33.7683167158641,50.7934249502469,
-214.515189821211));
#198506=CARTESIAN_POINT('Ctrl Pts',(-33.7570645587824,50.7776430250376,
-214.627325038844));
#198507=CARTESIAN_POINT('Ctrl Pts',(-33.7452260788453,50.7580381233537,
-214.739173241889));
#198508=CARTESIAN_POINT('Ctrl Pts',(-33.7328061316649,50.7346352575027,
-214.850336859306));
#198509=CARTESIAN_POINT('Ctrl Pts',(-33.7276482294165,50.7249162391657,
-214.896502198328));
#198510=CARTESIAN_POINT('Ctrl Pts',(-33.7223506794607,50.7144658367585,
-214.942895181462));
#198511=CARTESIAN_POINT('Ctrl Pts',(-33.7169619229803,50.7033744704336,
-214.989054517627));
#198512=CARTESIAN_POINT('Ctrl Pts',(-33.7115530693517,50.6922417393088,
-215.035386003159));
#198513=CARTESIAN_POINT('Ctrl Pts',(-33.7060523392326,50.6804633260605,
-215.081481730492));
#198514=CARTESIAN_POINT('Ctrl Pts',(-33.7005161572489,50.6681815307265,
-215.126887248828));
#198515=CARTESIAN_POINT('Ctrl Pts',(-33.6982866588628,50.6632354789248,
-215.145172689976));
#198516=CARTESIAN_POINT('Ctrl Pts',(-33.6960514937747,50.6582083562969,
-215.16334636011));
#198517=CARTESIAN_POINT('Ctrl Pts',(-33.6938146735602,50.6531116925866,
-215.181379319307));
#198518=CARTESIAN_POINT('Ctrl Pts',(-33.6804897647656,50.622750477744,-215.288803034027));
#198519=CARTESIAN_POINT('Ctrl Pts',(-33.6667462391996,50.5887152013327,
-215.395417267767));
#198520=CARTESIAN_POINT('Ctrl Pts',(-33.6525966745785,50.5510853335532,
-215.5008453749));
#198521=CARTESIAN_POINT('Ctrl Pts',(-33.63847268782,50.5135234884733,-215.606082901919));
#198522=CARTESIAN_POINT('Ctrl Pts',(-33.6239441491839,50.4723801664616,
-215.710138014617));
#198523=CARTESIAN_POINT('Ctrl Pts',(-33.6090308027503,50.4277843910374,
-215.812648418761));
#198524=CARTESIAN_POINT('Ctrl Pts',(-33.5940769452841,50.3830674743979,
-215.915437285043));
#198525=CARTESIAN_POINT('Ctrl Pts',(-33.5787362184851,50.3348795312152,
-216.01667248325));
#198526=CARTESIAN_POINT('Ctrl Pts',(-33.5630354218095,50.2833984427878,
-216.11600966241));
#198527=CARTESIAN_POINT('Ctrl Pts',(-33.5473346251338,50.2319173543604,
-216.21534684157));
#198528=CARTESIAN_POINT('Ctrl Pts',(-33.5312738087232,50.1771434563596,
-216.312785512755));
#198529=CARTESIAN_POINT('Ctrl Pts',(-33.5148860340387,50.1192982336582,
-216.408010056999));
#198530=CARTESIAN_POINT('Origin',(-33.1454591002416,47.6034469977721,-214.816150729402));
#198531=CARTESIAN_POINT('Ctrl Pts',(-42.5875626890161,49.379257463449,-213.836967828456));
#198532=CARTESIAN_POINT('Ctrl Pts',(-42.583706717545,49.3531444934432,-215.348104479787));
#198533=CARTESIAN_POINT('Ctrl Pts',(-42.4267736782988,48.5085693923201,
-216.591605848694));
#198534=CARTESIAN_POINT('Ctrl Pts',(-39.5843350108952,49.94028798542,-213.838955482324));
#198535=CARTESIAN_POINT('Ctrl Pts',(-39.5811128233999,49.9141052312931,
-215.348112574685));
#198536=CARTESIAN_POINT('Ctrl Pts',(-39.4353118162506,49.0695244128664,
-216.590608342324));
#198537=CARTESIAN_POINT('Ctrl Pts',(-36.5662930978432,50.4425286599318,
-213.840777098729));
#198538=CARTESIAN_POINT('Ctrl Pts',(-36.5632179392903,50.4163761409703,
-215.348234795315));
#198539=CARTESIAN_POINT('Ctrl Pts',(-36.4288305177724,49.5716582573572,
-216.589864155774));
#198540=CARTESIAN_POINT('Ctrl Pts',(-33.5455787101075,50.8841045229765,
-213.842210502424));
#198541=CARTESIAN_POINT('Ctrl Pts',(-33.542491458609,50.8579889698439,-215.348218150781));
#198542=CARTESIAN_POINT('Ctrl Pts',(-33.4195851394632,50.0130984955555,
-216.589106829638));
#198543=CARTESIAN_POINT('',(-33.4734406974179,50.0051916640197,-216.589120385861));
#198544=CARTESIAN_POINT('',(-42.426773677794,48.5085693922785,-216.591605848887));
#198545=CARTESIAN_POINT('Ctrl Pts',(-33.473440697418,50.0051916640197,-216.589120385862));
#198546=CARTESIAN_POINT('Ctrl Pts',(-36.464700907296,49.5656651085226,-216.589873039672));
#198547=CARTESIAN_POINT('Ctrl Pts',(-39.4531576785992,49.0661779829877,
-216.590614288892));
#198548=CARTESIAN_POINT('Ctrl Pts',(-42.4267736781731,48.508569392226,-216.591605848995));
#198549=CARTESIAN_POINT('',(-42.5875626890161,49.379257463449,-213.836967828456));
#198550=CARTESIAN_POINT('Origin',(-41.6694842675319,44.465041620637,-213.749705796269));
#198551=CARTESIAN_POINT('Origin',(-32.5100718388913,16.8405580785956,-213.686622269807));
#198552=CARTESIAN_POINT('Origin',(-31.3861213810748,49.6296476280943,-215.743606971984));
#198553=CARTESIAN_POINT('Ctrl Pts',(-33.4734406974176,50.0051916640201,
-216.589120385861));
#198554=CARTESIAN_POINT('Ctrl Pts',(-33.1846932575851,50.1143213461432,
-216.493132115846));
#198555=CARTESIAN_POINT('Ctrl Pts',(-32.8943360433596,50.1648136138274,
-216.360311415042));
#198556=CARTESIAN_POINT('Ctrl Pts',(-33.4901672823065,50.0432442151986,
-216.530872105694));
#198557=CARTESIAN_POINT('Ctrl Pts',(-33.1995861132119,50.1392297940238,
-216.451282693354));
#198558=CARTESIAN_POINT('Ctrl Pts',(-32.9074380702232,50.1790964451629,
-216.336991557182));
#198559=CARTESIAN_POINT('Ctrl Pts',(-33.5041153010602,50.0812800820291,
-216.470595425696));
#198560=CARTESIAN_POINT('Ctrl Pts',(-33.2118808797811,50.164531590063,-216.408280615884));
#198561=CARTESIAN_POINT('Ctrl Pts',(-32.9180956124776,50.1935640066322,
-216.312978006505));
#198562=CARTESIAN_POINT('Ctrl Pts',(-33.514886037746,50.119298258903,-216.408010072973));
#198563=CARTESIAN_POINT('Ctrl Pts',(-33.2211981697206,50.1902923385545,
-216.363964513645));
#198564=CARTESIAN_POINT('Ctrl Pts',(-32.9259571993478,50.2082406704929,
-216.288179546395));
#198565=CARTESIAN_POINT('',(-32.8943360433598,50.1648136138275,-216.360311415041));
#198566=CARTESIAN_POINT('Ctrl Pts',(-32.9259571993478,50.2082406704928,
-216.288179546395));
#198567=CARTESIAN_POINT('Ctrl Pts',(-32.9213942090144,50.1997220625587,
-216.302573035674));
#198568=CARTESIAN_POINT('Ctrl Pts',(-32.9158742467513,50.1912547814706,
-216.31673368404));
#198569=CARTESIAN_POINT('Ctrl Pts',(-32.9095161991152,50.1828980466778,
-216.330573580415));
#198570=CARTESIAN_POINT('Ctrl Pts',(-32.9048796509829,50.1768039742025,
-216.340666198364));
#198571=CARTESIAN_POINT('Ctrl Pts',(-32.8997987066695,50.1707685931225,
-216.350588603965));
#198572=CARTESIAN_POINT('Ctrl Pts',(-32.8943360433598,50.1648136138275,
-216.360311415041));
#198573=CARTESIAN_POINT('Origin',(-33.114566694526,47.5599010752717,-214.888601821826));
#198574=CARTESIAN_POINT('Ctrl Pts',(-43.4427334535925,49.2193110042462,
-213.753761106585));
#198575=CARTESIAN_POINT('Ctrl Pts',(-43.7363359520915,49.1333974713924,
-215.43762891935));
#198576=CARTESIAN_POINT('Ctrl Pts',(-43.7719279964167,48.0354975596101,
-216.750009718969));
#198577=CARTESIAN_POINT('Ctrl Pts',(-43.371956206762,49.2325823249756,-213.766498377489));
#198578=CARTESIAN_POINT('Ctrl Pts',(-43.6452593901831,49.1508522358615,
-215.438175221839));
#198579=CARTESIAN_POINT('Ctrl Pts',(-43.6692517245548,48.0727799897406,
-216.747093832485));
#198580=CARTESIAN_POINT('Ctrl Pts',(-43.3010795363893,49.2458600286701,
-213.778022394282));
#198581=CARTESIAN_POINT('Ctrl Pts',(-43.5493764245827,49.1692272064718,
-215.435455532993));
#198582=CARTESIAN_POINT('Ctrl Pts',(-43.5584791373048,48.11436895475,-216.739913980388));
#198583=CARTESIAN_POINT('Ctrl Pts',(-43.1590773754588,49.2724456764462,
-213.798159517644));
#198584=CARTESIAN_POINT('Ctrl Pts',(-43.3605441394919,49.205331988453,-215.428289388641));
#198585=CARTESIAN_POINT('Ctrl Pts',(-43.341150895191,48.1932191507075,-216.723471556235));
#198586=CARTESIAN_POINT('Ctrl Pts',(-43.0879593352488,49.2857509575935,
-213.806842606532));
#198587=CARTESIAN_POINT('Ctrl Pts',(-43.2666336864127,49.2232502933301,
-215.423678316261));
#198588=CARTESIAN_POINT('Ctrl Pts',(-43.2329905076982,48.2313985113306,
-216.713986670805));
#198589=CARTESIAN_POINT('Ctrl Pts',(-42.9454754545039,49.312391427417,-213.821265740755));
#198590=CARTESIAN_POINT('Ctrl Pts',(-43.0770958183574,49.2593635928723,
-215.410701334327));
#198591=CARTESIAN_POINT('Ctrl Pts',(-43.0131914262865,48.3080912144091,
-216.690257289732));
#198592=CARTESIAN_POINT('Ctrl Pts',(-42.8741106150187,49.3257262125301,
-213.827018288813));
#198593=CARTESIAN_POINT('Ctrl Pts',(-42.9810928107897,49.2776332485339,
-215.402139971414));
#198594=CARTESIAN_POINT('Ctrl Pts',(-42.9009270350625,48.3470115783392,
-216.675727916603));
#198595=CARTESIAN_POINT('Ctrl Pts',(-42.7310769616701,49.3524479316748,
-213.834879555374));
#198596=CARTESIAN_POINT('Ctrl Pts',(-42.7835366995418,49.3152096382395,
-215.378441131484));
#198597=CARTESIAN_POINT('Ctrl Pts',(-42.6662831546448,48.4283526107962,
-216.637893960711));
#198598=CARTESIAN_POINT('Ctrl Pts',(-42.6594046914523,49.3658367172642,
-213.836920285803));
#198599=CARTESIAN_POINT('Ctrl Pts',(-42.6823983172108,49.334434791349,-215.36340665766));
#198600=CARTESIAN_POINT('Ctrl Pts',(-42.5445646683703,48.470275506698,-216.614703255093));
#198601=CARTESIAN_POINT('Ctrl Pts',(-42.587562688342,49.3792574635749,-213.836967828456));
#198602=CARTESIAN_POINT('Ctrl Pts',(-42.5837067171795,49.3531444935084,
-215.348104479964));
#198603=CARTESIAN_POINT('Ctrl Pts',(-42.4267736781597,48.5085693921588,
-216.59160584896));
#198604=CARTESIAN_POINT('',(-43.4427334535923,49.2193110042465,-213.753761106585));
#198605=CARTESIAN_POINT('',(-43.7719279964152,48.0354975596111,-216.750009718968));
#198606=CARTESIAN_POINT('Origin',(-42.506225613034,44.3085739513886,-213.666499074398));
#198607=CARTESIAN_POINT('Ctrl Pts',(-43.4427334535923,49.2193110042462,
-213.753761106585));
#198608=CARTESIAN_POINT('Ctrl Pts',(-43.3719706400421,49.2325796186159,
-213.766495780036));
#198609=CARTESIAN_POINT('Ctrl Pts',(-43.3010945110548,49.2458572251129,
-213.778020270746));
#198610=CARTESIAN_POINT('Ctrl Pts',(-43.230078455924,49.2591528525582,-213.788090955963));
#198611=CARTESIAN_POINT('Ctrl Pts',(-43.1590933274853,49.2724426899074,
-213.79815725551));
#198612=CARTESIAN_POINT('Ctrl Pts',(-43.0879758381621,49.2857478720138,
-213.806840936001));
#198613=CARTESIAN_POINT('Ctrl Pts',(-43.0167173948763,49.2990711925053,
-213.814054173644));
#198614=CARTESIAN_POINT('Ctrl Pts',(-42.9454929340409,49.3123881592362,
-213.821263971364));
#198615=CARTESIAN_POINT('Ctrl Pts',(-42.874128659976,49.3257228413495,-213.827017297045));
#198616=CARTESIAN_POINT('Ctrl Pts',(-42.8025937883444,49.3390870721025,
-213.830948922093));
#198617=CARTESIAN_POINT('Ctrl Pts',(-42.7310959828176,49.3524443781212,
-213.834878509953));
#198618=CARTESIAN_POINT('Ctrl Pts',(-42.6594242987725,49.3658330544366,
-213.836920272815));
#198619=CARTESIAN_POINT('Ctrl Pts',(-42.5875626890161,49.379257463449,-213.836967828456));
#198620=CARTESIAN_POINT('Ctrl Pts',(-42.4267736781616,48.5085693921643,
-216.591605848952));
#198621=CARTESIAN_POINT('Ctrl Pts',(-42.4415254954543,48.503773861373,-216.594498092432));
#198622=CARTESIAN_POINT('Ctrl Pts',(-42.4593143860255,48.4979659020317,
-216.597960778204));
#198623=CARTESIAN_POINT('Ctrl Pts',(-42.480186767919,48.491088268847,-216.601973535425));
#198624=CARTESIAN_POINT('Ctrl Pts',(-42.4967271814369,48.4856380572956,
-216.60515346305));
#198625=CARTESIAN_POINT('Ctrl Pts',(-42.5152045567958,48.4795155730946,
-216.608678838495));
#198626=CARTESIAN_POINT('Ctrl Pts',(-42.5356174624875,48.4727022574992,
-216.612519977972));
#198627=CARTESIAN_POINT('Ctrl Pts',(-42.5515113833177,48.4673972656328,
-216.615510770546));
#198628=CARTESIAN_POINT('Ctrl Pts',(-42.5685785070712,48.461673503796,-216.618692765583));
#198629=CARTESIAN_POINT('Ctrl Pts',(-42.5868009760644,48.4555306364492,
-216.622040459405));
#198630=CARTESIAN_POINT('Ctrl Pts',(-42.6061677456185,48.4490020207962,
-216.625598375448));
#198631=CARTESIAN_POINT('Ctrl Pts',(-42.6262776792176,48.4421873747635,
-216.629237691355));
#198632=CARTESIAN_POINT('Ctrl Pts',(-42.645645819722,48.4355945626524,-216.632682797186));
#198633=CARTESIAN_POINT('Ctrl Pts',(-42.6618596565057,48.4300754587668,
-216.635566831594));
#198634=CARTESIAN_POINT('Ctrl Pts',(-42.6775524999369,48.4247129541951,
-216.638314861844));
#198635=CARTESIAN_POINT('Ctrl Pts',(-42.6918693280422,48.4198061888257,
-216.640789613044));
#198636=CARTESIAN_POINT('Ctrl Pts',(-42.715278653753,48.4117831778716,-216.644836058001));
#198637=CARTESIAN_POINT('Ctrl Pts',(-42.7364349552496,48.404496253462,-216.648396283454));
#198638=CARTESIAN_POINT('Ctrl Pts',(-42.7553494105702,48.3979643916984,
-216.651514294509));
#198639=CARTESIAN_POINT('Ctrl Pts',(-42.7618210576182,48.3957294923485,
-216.652581132897));
#198640=CARTESIAN_POINT('Ctrl Pts',(-42.7680306396195,48.3935827167038,
-216.653596337291));
#198641=CARTESIAN_POINT('Ctrl Pts',(-42.7739796041737,48.3915240995609,
-216.654561986672));
#198642=CARTESIAN_POINT('Ctrl Pts',(-42.7772862698949,48.3903798401393,
-216.65509873213));
#198643=CARTESIAN_POINT('Ctrl Pts',(-42.7805124230816,48.3892628125201,
-216.655620169018));
#198644=CARTESIAN_POINT('Ctrl Pts',(-42.7836583565613,48.3881729872862,
-216.656126663382));
#198645=CARTESIAN_POINT('Ctrl Pts',(-42.7916131605315,48.3854172563868,
-216.657407384481));
#198646=CARTESIAN_POINT('Ctrl Pts',(-42.7990521658508,48.3828376767049,
-216.658592151102));
#198647=CARTESIAN_POINT('Ctrl Pts',(-42.8059840566176,48.3804311709214,
-216.659688355632));
#198648=CARTESIAN_POINT('Ctrl Pts',(-42.8084023782922,48.3795916156987,
-216.660070787391));
#198649=CARTESIAN_POINT('Ctrl Pts',(-42.8095099314098,48.3792066589871,
-216.660245512224));
#198650=CARTESIAN_POINT('Ctrl Pts',(-42.8101772587533,48.3789746817772,
-216.660350971608));
#198651=CARTESIAN_POINT('Ctrl Pts',(-42.8108445860968,48.3787427045672,
-216.660456430992));
#198652=CARTESIAN_POINT('Ctrl Pts',(-42.8110716594233,48.3786635842834,
-216.660492534598));
#198653=CARTESIAN_POINT('Ctrl Pts',(-42.8117287721884,48.3784346229387,
-216.660596928192));
#198654=CARTESIAN_POINT('Ctrl Pts',(-42.8130429977186,48.3779767002494,
-216.660805715378));
#198655=CARTESIAN_POINT('Ctrl Pts',(-42.8151127707912,48.377255336016,-216.661134478143));
#198656=CARTESIAN_POINT('Ctrl Pts',(-42.8179347829778,48.3762716511989,
-216.661580299639));
#198657=CARTESIAN_POINT('Ctrl Pts',(-42.8239652219253,48.3741695868416,
-216.662532988406));
#198658=CARTESIAN_POINT('Ctrl Pts',(-42.8334335081744,48.3708687545685,
-216.664022789577));
#198659=CARTESIAN_POINT('Ctrl Pts',(-42.8462734480989,48.3663912789057,
-216.665990600897));
#198660=CARTESIAN_POINT('Ctrl Pts',(-42.8574678892586,48.3624876128337,
-216.667706227931));
#198661=CARTESIAN_POINT('Ctrl Pts',(-42.8712239810185,48.3576900086163,
-216.669784249758));
#198662=CARTESIAN_POINT('Ctrl Pts',(-42.8874753033194,48.3520199169081,
-216.672163514063));
#198663=CARTESIAN_POINT('Ctrl Pts',(-42.9049210367745,48.3459330947545,
-216.674717645359));
#198664=CARTESIAN_POINT('Ctrl Pts',(-42.9252414131555,48.338841234417,-216.677618487984));
#198665=CARTESIAN_POINT('Ctrl Pts',(-42.9483405988423,48.3307731838733,
-216.680772624931));
#198666=CARTESIAN_POINT('Ctrl Pts',(-42.9598901916857,48.3267391586014,
-216.682349693404));
#198667=CARTESIAN_POINT('Ctrl Pts',(-42.9721343606286,48.3224610817444,
-216.683989858753));
#198668=CARTESIAN_POINT('Ctrl Pts',(-42.9850612664934,48.3179421430536,
-216.685680657929));
#198669=CARTESIAN_POINT('Ctrl Pts',(-42.9896525342021,48.3163371451133,
-216.686281181499));
#198670=CARTESIAN_POINT('Ctrl Pts',(-42.995750004829,48.3142051330221,-216.687071085619));
#198671=CARTESIAN_POINT('Ctrl Pts',(-42.9995737114364,48.3128679604388,
-216.687562687561));
#198672=CARTESIAN_POINT('Ctrl Pts',(-43.0011329076028,48.3123227004124,
-216.687763148513));
#198673=CARTESIAN_POINT('Ctrl Pts',(-43.002314534652,48.3119094533396,-216.687914505546));
#198674=CARTESIAN_POINT('Ctrl Pts',(-43.0028633815164,48.3117175253772,
-216.68798476227));
#198675=CARTESIAN_POINT('Ctrl Pts',(-43.0047581971739,48.3110549214129,
-216.688227313606));
#198676=CARTESIAN_POINT('Ctrl Pts',(-43.0067444288693,48.3103606366143,
-216.688480302491));
#198677=CARTESIAN_POINT('Ctrl Pts',(-43.0088218770899,48.3096346619737,
-216.688743543246));
#198678=CARTESIAN_POINT('Ctrl Pts',(-43.0244229399528,48.3041827927562,
-216.690720408674));
#198679=CARTESIAN_POINT('Ctrl Pts',(-43.0451686616728,48.2969462008756,
-216.693276848829));
#198680=CARTESIAN_POINT('Ctrl Pts',(-43.0709184477644,48.2879624492166,
-216.696263099913));
#198681=CARTESIAN_POINT('Ctrl Pts',(-43.0725995349496,48.2873759406633,
-216.696458058753));
#198682=CARTESIAN_POINT('Ctrl Pts',(-43.0743019430858,48.2867819844123,
-216.696654834268));
#198683=CARTESIAN_POINT('Ctrl Pts',(-43.0760256312567,48.2861805899518,
-216.696853379208));
#198684=CARTESIAN_POINT('Ctrl Pts',(-43.0902687344933,48.2812111740613,
-216.698493986909));
#198685=CARTESIAN_POINT('Ctrl Pts',(-43.1059646008994,48.2757340625106,
-216.700255469844));
#198686=CARTESIAN_POINT('Ctrl Pts',(-43.1230914003588,48.2697535114062,
-216.702110542323));
#198687=CARTESIAN_POINT('Ctrl Pts',(-43.1397850747307,48.2639242043639,
-216.703918701284));
#198688=CARTESIAN_POINT('Ctrl Pts',(-43.157852453777,48.2576074670258,-216.705822337881));
#198689=CARTESIAN_POINT('Ctrl Pts',(-43.1772837610085,48.2507976758426,
-216.707797320349));
#198690=CARTESIAN_POINT('Ctrl Pts',(-43.1871254531832,48.247348609457,-216.70879762204));
#198691=CARTESIAN_POINT('Ctrl Pts',(-43.1965283228607,48.2440488814785,
-216.709734433479));
#198692=CARTESIAN_POINT('Ctrl Pts',(-43.2036246682312,48.2415563362908,
-216.710434118825));
#198693=CARTESIAN_POINT('Ctrl Pts',(-43.2816844673068,48.2141383392263,
-216.718130657632));
#198694=CARTESIAN_POINT('Ctrl Pts',(-43.3591363015399,48.1866286965368,
-216.724750583296));
#198695=CARTESIAN_POINT('Ctrl Pts',(-43.436799842652,48.1585111211586,-216.730701790525));
#198696=CARTESIAN_POINT('Ctrl Pts',(-43.441137525833,48.1569406914297,-216.731034178814));
#198697=CARTESIAN_POINT('Ctrl Pts',(-43.4454758694279,48.1553683652711,
-216.731364481053));
#198698=CARTESIAN_POINT('Ctrl Pts',(-43.4498150162479,48.1537940527302,
-216.73169276831));
#198699=CARTESIAN_POINT('Ctrl Pts',(-43.5584791373049,48.11436895475,-216.739913980388));
#198700=CARTESIAN_POINT('Ctrl Pts',(-43.6692517245548,48.0727799897407,
-216.747093832484));
#198701=CARTESIAN_POINT('Ctrl Pts',(-43.7719279964153,48.0354975596113,
-216.750009718968));
#198702=CARTESIAN_POINT('Ctrl Pts',(-47.5938143592254,47.5353276146289,
-213.404748058676));
#198703=CARTESIAN_POINT('Ctrl Pts',(-47.7151968771187,47.4137062867167,
-215.373807350724));
#198704=CARTESIAN_POINT('Ctrl Pts',(-47.0575921287075,46.1983743823902,
-216.787046295788));
#198705=CARTESIAN_POINT('Ctrl Pts',(-47.4361974911963,47.6395334582591,
-213.413799790385));
#198706=CARTESIAN_POINT('Ctrl Pts',(-47.5710170575155,47.5124761588416,
-215.378572627199));
#198707=CARTESIAN_POINT('Ctrl Pts',(-46.9439936233544,46.2838138436724,
-216.79016068369));
#198708=CARTESIAN_POINT('Ctrl Pts',(-47.2763792783413,47.7395307126687,
-213.423893656191));
#198709=CARTESIAN_POINT('Ctrl Pts',(-47.423589902594,47.6084784638584,-215.382114459135));
#198710=CARTESIAN_POINT('Ctrl Pts',(-46.8280682259696,46.3702652294506,
-216.791559853189));
#198711=CARTESIAN_POINT('Ctrl Pts',(-46.9524663169781,47.9311597954933,
-213.446422385042));
#198712=CARTESIAN_POINT('Ctrl Pts',(-47.1294827939091,47.7906783086273,
-215.393841476156));
#198713=CARTESIAN_POINT('Ctrl Pts',(-46.5987238205652,46.5304864276265,
-216.799043822533));
#198714=CARTESIAN_POINT('Ctrl Pts',(-46.7883227793929,48.0228296206103,
-213.458567219485));
#198715=CARTESIAN_POINT('Ctrl Pts',(-46.9655745538276,47.8868680864696,
-215.393218617728));
#198716=CARTESIAN_POINT('Ctrl Pts',(-46.4620613130109,46.632173235984,-216.795234897512));
#198717=CARTESIAN_POINT('Ctrl Pts',(-46.4554564499389,48.1980381642472,
-213.483257157288));
#198718=CARTESIAN_POINT('Ctrl Pts',(-46.645778329932,48.0640244167292,-215.396857720889));
#198719=CARTESIAN_POINT('Ctrl Pts',(-46.2017889155362,46.8105029195329,
-216.79265356856));
#198720=CARTESIAN_POINT('Ctrl Pts',(-46.2867982818254,48.281531361303,-213.496222696253));
#198721=CARTESIAN_POINT('Ctrl Pts',(-46.4887900152057,48.1462008970494,
-215.401226143536));
#198722=CARTESIAN_POINT('Ctrl Pts',(-46.0766746938607,46.8895727080125,
-216.794026584048));
#198723=CARTESIAN_POINT('Ctrl Pts',(-46.0305084677278,48.4005429744912,
-213.516940454077));
#198724=CARTESIAN_POINT('Ctrl Pts',(-46.2457844526878,48.2661209388548,
-215.406453553964));
#198725=CARTESIAN_POINT('Ctrl Pts',(-45.879944168228,47.0110043640158,-216.794144611354));
#198726=CARTESIAN_POINT('Ctrl Pts',(-45.9444636231603,48.4392026490648,
-213.524043422999));
#198727=CARTESIAN_POINT('Ctrl Pts',(-46.1636628855248,48.3054429426302,
-215.408017074389));
#198728=CARTESIAN_POINT('Ctrl Pts',(-45.8130123122325,47.051733779581,-216.79390894265));
#198729=CARTESIAN_POINT('Ctrl Pts',(-45.7716909901656,48.5142583186062,
-213.538427044995));
#198730=CARTESIAN_POINT('Ctrl Pts',(-45.9955375795966,48.3833424179063,
-215.409512738422));
#198731=CARTESIAN_POINT('Ctrl Pts',(-45.6738311416741,47.1362644708882,
-216.791413446998));
#198732=CARTESIAN_POINT('Ctrl Pts',(-45.6849221753783,48.5506755813429,
-213.545667919357));
#198733=CARTESIAN_POINT('Ctrl Pts',(-45.909485781788,48.4219041276403,-215.409378455852));
#198734=CARTESIAN_POINT('Ctrl Pts',(-45.6014976347732,47.180066238931,-216.789070533814));
#198735=CARTESIAN_POINT('Ctrl Pts',(-45.4234990388523,48.6566004797362,
-213.567641621074));
#198736=CARTESIAN_POINT('Ctrl Pts',(-45.6556174915683,48.5320412262081,
-215.411600281523));
#198737=CARTESIAN_POINT('Ctrl Pts',(-45.3906894073598,47.3016094353054,
-216.784909295631));
#198738=CARTESIAN_POINT('Ctrl Pts',(-45.2477531991542,48.7227706699221,
-213.582727977866));
#198739=CARTESIAN_POINT('Ctrl Pts',(-45.4876251235724,48.6001398788528,
-215.414556338723));
#198740=CARTESIAN_POINT('Ctrl Pts',(-45.2524231606292,47.3757390551069,
-216.783601115577));
#198741=CARTESIAN_POINT('Ctrl Pts',(-44.8934628219101,48.8462330088764,
-213.614222279575));
#198742=CARTESIAN_POINT('Ctrl Pts',(-45.1474114702805,48.7286790378217,
-215.42032956369));
#198743=CARTESIAN_POINT('Ctrl Pts',(-44.9704049771277,47.5202154420337,
-216.780178404985));
#198744=CARTESIAN_POINT('Ctrl Pts',(-44.7149101066689,48.9035307363901,
-213.630594481069));
#198745=CARTESIAN_POINT('Ctrl Pts',(-44.9742711452602,48.7893976468135,
-215.422593536637));
#198746=CARTESIAN_POINT('Ctrl Pts',(-44.8252363083432,47.5917545322963,
-216.777394875566));
#198747=CARTESIAN_POINT('Ctrl Pts',(-44.3548749878035,49.0092996064988,
-213.664137638318));
#198748=CARTESIAN_POINT('Ctrl Pts',(-44.622095897551,48.9031602696537,-215.425466313217));
#198749=CARTESIAN_POINT('Ctrl Pts',(-44.5266355180431,47.7322685705669,
-216.769090779705));
#198750=CARTESIAN_POINT('Ctrl Pts',(-44.1732412415974,49.0577948170664,
-213.681295718698));
#198751=CARTESIAN_POINT('Ctrl Pts',(-44.4434391165651,48.9560293640203,
-215.426301418401));
#198752=CARTESIAN_POINT('Ctrl Pts',(-44.3737734347551,47.8005712765384,
-216.763825997473));
#198753=CARTESIAN_POINT('Ctrl Pts',(-43.8089789068828,49.1454472082473,
-213.716585287098));
#198754=CARTESIAN_POINT('Ctrl Pts',(-44.0903037035521,49.0513958700251,
-215.431155804495));
#198755=CARTESIAN_POINT('Ctrl Pts',(-44.0737062319855,47.9238489048316,
-216.756518873734));
#198756=CARTESIAN_POINT('Ctrl Pts',(-43.6261771610655,49.1846631278254,
-213.734854145951));
#198757=CARTESIAN_POINT('Ctrl Pts',(-43.9151392929898,49.0942498031829,
-215.435089586124));
#198758=CARTESIAN_POINT('Ctrl Pts',(-43.9256354120413,47.9796853812831,
-216.75437483532));
#198759=CARTESIAN_POINT('Ctrl Pts',(-43.442733453593,49.219311004246,-213.753761106585));
#198760=CARTESIAN_POINT('Ctrl Pts',(-43.7363359520915,49.1333974713923,
-215.43762891935));
#198761=CARTESIAN_POINT('Ctrl Pts',(-43.7719279964163,48.0354975596104,
-216.750009718968));
#198762=CARTESIAN_POINT('',(-47.5938143592265,47.5353276146283,-213.404748058676));
#198763=CARTESIAN_POINT('',(-47.0575921287078,46.1983743823903,-216.787046295788));
#198764=CARTESIAN_POINT('Origin',(-44.8332438581234,43.3673981711062,-213.31748602649));
#198765=CARTESIAN_POINT('Ctrl Pts',(-47.5938143592265,47.5353276146283,
-213.404748058676));
#198766=CARTESIAN_POINT('Ctrl Pts',(-47.4361974915317,47.639533457943,-213.413799795273));
#198767=CARTESIAN_POINT('Ctrl Pts',(-47.2763792787077,47.7395307123426,
-213.423893661064));
#198768=CARTESIAN_POINT('Ctrl Pts',(-46.9524663174189,47.9311597951435,
-213.44642238989));
#198769=CARTESIAN_POINT('Ctrl Pts',(-46.7883227798346,48.0228296202715,
-213.458567224306));
#198770=CARTESIAN_POINT('Ctrl Pts',(-46.4554564504138,48.1980381639128,
-213.483257162063));
#198771=CARTESIAN_POINT('Ctrl Pts',(-46.2867982823297,48.2815313609651,
-213.496222701009));
#198772=CARTESIAN_POINT('Ctrl Pts',(-46.0305084682658,48.4005429741553,
-213.516940458798));
#198773=CARTESIAN_POINT('Ctrl Pts',(-45.9444636237083,48.4392026487304,
-213.524043427709));
#198774=CARTESIAN_POINT('Ctrl Pts',(-45.7716909907256,48.5142583182786,
-213.538427049676));
#198775=CARTESIAN_POINT('Ctrl Pts',(-45.6849221759404,48.5506755810206,
-213.545667924022));
#198776=CARTESIAN_POINT('Ctrl Pts',(-45.4234990394341,48.656600479424,-213.567641625695));
#198777=CARTESIAN_POINT('Ctrl Pts',(-45.2477531997558,48.7227706696145,
-213.58272798246));
#198778=CARTESIAN_POINT('Ctrl Pts',(-44.8934628225481,48.8462330085811,
-213.614222284111));
#198779=CARTESIAN_POINT('Ctrl Pts',(-44.7149101073209,48.9035307361032,
-213.630594485574));
#198780=CARTESIAN_POINT('Ctrl Pts',(-44.3548749884766,49.0092996062315,
-213.664137642754));
#198781=CARTESIAN_POINT('Ctrl Pts',(-44.1732412422787,49.0577948168098,
-213.681295723098));
#198782=CARTESIAN_POINT('Ctrl Pts',(-43.8089789075934,49.1454472080097,
-213.716585291428));
#198783=CARTESIAN_POINT('Ctrl Pts',(-43.626177161796,49.1846631275968,-213.734854150249));
#198784=CARTESIAN_POINT('Ctrl Pts',(-43.4427334535923,49.2193110042465,
-213.753761106585));
#198785=CARTESIAN_POINT('Ctrl Pts',(-43.7719279964163,48.0354975596108,
-216.750009718968));
#198786=CARTESIAN_POINT('Ctrl Pts',(-43.7811851272337,48.0321362342387,
-216.750272610989));
#198787=CARTESIAN_POINT('Ctrl Pts',(-43.7893021651862,48.0291829772161,
-216.750497126067));
#198788=CARTESIAN_POINT('Ctrl Pts',(-43.799178039926,48.0255804797839,-216.750762626771));
#198789=CARTESIAN_POINT('Ctrl Pts',(-43.8080192155758,48.0223554173551,
-216.751000310866));
#198790=CARTESIAN_POINT('Ctrl Pts',(-43.8182703799996,48.0186106696607,
-216.751270916601));
#198791=CARTESIAN_POINT('Ctrl Pts',(-43.831972963223,48.0135818234643,-216.751616944973));
#198792=CARTESIAN_POINT('Ctrl Pts',(-43.8335766018061,48.0129932883204,
-216.751657441312));
#198793=CARTESIAN_POINT('Ctrl Pts',(-43.835227458279,48.0123871498841,-216.751698951233));
#198794=CARTESIAN_POINT('Ctrl Pts',(-43.8369287587511,48.0117621670366,
-216.751741526661));
#198795=CARTESIAN_POINT('Ctrl Pts',(-43.8694055058916,47.9998316408073,
-216.752554264576));
#198796=CARTESIAN_POINT('Ctrl Pts',(-43.9008759562454,47.9881558224337,
-216.753270615293));
#198797=CARTESIAN_POINT('Ctrl Pts',(-43.9314332824726,47.976692143459,-216.753932760624));
#198798=CARTESIAN_POINT('Ctrl Pts',(-43.9686297051458,47.9627377861517,
-216.754738768236));
#198799=CARTESIAN_POINT('Ctrl Pts',(-44.0044739958948,47.9490971801564,
-216.755464878702));
#198800=CARTESIAN_POINT('Ctrl Pts',(-44.039093110119,47.9357219781021,-216.756167305868));
#198801=CARTESIAN_POINT('Ctrl Pts',(-44.0613540661284,47.9271213887681,
-216.756618984098));
#198802=CARTESIAN_POINT('Ctrl Pts',(-44.0831075367369,47.9186311582294,
-216.75706043696));
#198803=CARTESIAN_POINT('Ctrl Pts',(-44.1043786370355,47.9102443146154,
-216.757502456408));
#198804=CARTESIAN_POINT('Ctrl Pts',(-44.1397067224319,47.8963150338897,
-216.758236583959));
#198805=CARTESIAN_POINT('Ctrl Pts',(-44.1737062936049,47.8826695844048,
-216.758973260723));
#198806=CARTESIAN_POINT('Ctrl Pts',(-44.2064569138943,47.8692997410846,
-216.759744918243));
#198807=CARTESIAN_POINT('Ctrl Pts',(-44.2122572129562,47.8669318747974,
-216.759881582658));
#198808=CARTESIAN_POINT('Ctrl Pts',(-44.2180182348011,47.8645727207277,
-216.760019295337));
#198809=CARTESIAN_POINT('Ctrl Pts',(-44.2237402936187,47.8622223169866,
-216.760158175401));
#198810=CARTESIAN_POINT('Ctrl Pts',(-44.2579874141509,47.8481549047516,
-216.760989387112));
#198811=CARTESIAN_POINT('Ctrl Pts',(-44.2908804989542,47.8343590266573,
-216.761866207695));
#198812=CARTESIAN_POINT('Ctrl Pts',(-44.3223252327681,47.8209640907791,
-216.762743124348));
#198813=CARTESIAN_POINT('Ctrl Pts',(-44.3552906472565,47.8069213701161,
-216.763662449062));
#198814=CARTESIAN_POINT('Ctrl Pts',(-44.3866645471589,47.7933191305206,
-216.764582006858));
#198815=CARTESIAN_POINT('Ctrl Pts',(-44.4163794113386,47.7802696795038,
-216.765467472998));
#198816=CARTESIAN_POINT('Ctrl Pts',(-44.4487846007203,47.7660387569268,
-216.766433107496));
#198817=CARTESIAN_POINT('Ctrl Pts',(-44.479216953245,47.7524652205429,-216.767358276128));
#198818=CARTESIAN_POINT('Ctrl Pts',(-44.507632885208,47.7396533298788,-216.768218009436));
#198819=CARTESIAN_POINT('Ctrl Pts',(-44.5379039054705,47.726005035591,-216.769133869046));
#198820=CARTESIAN_POINT('Ctrl Pts',(-44.5658872349512,47.7132207550825,
-216.769975716415));
#198821=CARTESIAN_POINT('Ctrl Pts',(-44.5915712306527,47.7013845848144,
-216.770731900668));
#198822=CARTESIAN_POINT('Ctrl Pts',(-44.6203528538254,47.6881209090055,
-216.771579284793));
#198823=CARTESIAN_POINT('Ctrl Pts',(-44.6462477864905,47.6760476263165,
-216.772319371972));
#198824=CARTESIAN_POINT('Ctrl Pts',(-44.6692792696536,47.6652358761871,
-216.77295425634));
#198825=CARTESIAN_POINT('Ctrl Pts',(-44.6715286117851,47.6641799596007,
-216.773016261559));
#198826=CARTESIAN_POINT('Ctrl Pts',(-44.6737506639533,47.6631360444201,
-216.773077274141));
#198827=CARTESIAN_POINT('Ctrl Pts',(-44.6759454607542,47.6621041776483,
-216.773137302419));
#198828=CARTESIAN_POINT('Ctrl Pts',(-44.7037765107572,47.6490196243496,
-216.773898489067));
#198829=CARTESIAN_POINT('Ctrl Pts',(-44.7272086156641,47.6378971602701,
-216.774493853777));
#198830=CARTESIAN_POINT('Ctrl Pts',(-44.7463533295129,47.628772462078,-216.774960914982));
#198831=CARTESIAN_POINT('Ctrl Pts',(-44.7627930443094,47.6209370127176,
-216.775361984075));
#198832=CARTESIAN_POINT('Ctrl Pts',(-44.7760706843893,47.6145742802803,
-216.775668131786));
#198833=CARTESIAN_POINT('Ctrl Pts',(-44.7862332044631,47.6096979005449,
-216.775894447614));
#198834=CARTESIAN_POINT('Ctrl Pts',(-44.7941357857176,47.605905928986,-216.776070435381));
#198835=CARTESIAN_POINT('Ctrl Pts',(-44.8002363598239,47.6029767264898,
-216.776199286723));
#198836=CARTESIAN_POINT('Ctrl Pts',(-44.8083943648565,47.5990461730887,
-216.776372924679));
#198837=CARTESIAN_POINT('Ctrl Pts',(-44.8107273484308,47.5979221340024,
-216.776422580753));
#198838=CARTESIAN_POINT('Ctrl Pts',(-44.813228321892,47.5967161299053,-216.776475815531));
#198839=CARTESIAN_POINT('Ctrl Pts',(-44.8159867801204,47.5953843600175,
-216.776534542052));
#198840=CARTESIAN_POINT('Ctrl Pts',(-44.8314774654733,47.5879055343162,
-216.77686433282));
#198841=CARTESIAN_POINT('Ctrl Pts',(-44.8515740904643,47.5781633376041,
-216.777288516625));
#198842=CARTESIAN_POINT('Ctrl Pts',(-44.8761685367022,47.5661316606375,
-216.777775113872));
#198843=CARTESIAN_POINT('Ctrl Pts',(-44.9008453820597,47.5540596737741,
-216.778263341372));
#198844=CARTESIAN_POINT('Ctrl Pts',(-44.9300502849462,47.5396824427546,
-216.778814204285));
#198845=CARTESIAN_POINT('Ctrl Pts',(-44.9636231565079,47.522967707742,-216.779383698168));
#198846=CARTESIAN_POINT('Ctrl Pts',(-44.9971675948681,47.506267128606,-216.779952709741));
#198847=CARTESIAN_POINT('Ctrl Pts',(-45.0350726258933,47.4872324509082,
-216.780540039179));
#198848=CARTESIAN_POINT('Ctrl Pts',(-45.0771274087593,47.4658327612458,
-216.781093734266));
#198849=CARTESIAN_POINT('Ctrl Pts',(-45.0882843165739,47.4601555386197,
-216.781240626596));
#198850=CARTESIAN_POINT('Ctrl Pts',(-45.0997330089618,47.4543118970314,
-216.781385121284));
#198851=CARTESIAN_POINT('Ctrl Pts',(-45.1114689410713,47.4483013575709,
-216.781526195445));
#198852=CARTESIAN_POINT('Ctrl Pts',(-45.1395076970411,47.43394135211,-216.781863241017));
#198853=CARTESIAN_POINT('Ctrl Pts',(-45.1692394690722,47.4185847768683,
-216.78220619853));
#198854=CARTESIAN_POINT('Ctrl Pts',(-45.2006758201389,47.4021448352045,
-216.782569451285));
#198855=CARTESIAN_POINT('Ctrl Pts',(-45.2297367262886,47.3869471552708,
-216.782905255342));
#198856=CARTESIAN_POINT('Ctrl Pts',(-45.2602541421359,47.3708237485339,
-216.783258343756));
#198857=CARTESIAN_POINT('Ctrl Pts',(-45.2922640264201,47.3536723445899,
-216.783651004601));
#198858=CARTESIAN_POINT('Ctrl Pts',(-45.3230081294446,47.3371991663308,
-216.784028138281));
#198859=CARTESIAN_POINT('Ctrl Pts',(-45.3551287236645,47.3197779207588,
-216.784441678969));
#198860=CARTESIAN_POINT('Ctrl Pts',(-45.3886869395199,47.3012829987608,
-216.784923057149));
#198861=CARTESIAN_POINT('Ctrl Pts',(-45.4205801588626,47.2837057054223,
-216.785380551669));
#198862=CARTESIAN_POINT('Ctrl Pts',(-45.4537717327481,47.2651587428511,
-216.785899268647));
#198863=CARTESIAN_POINT('Ctrl Pts',(-45.4883440225305,47.2454997119075,
-216.786517961527));
#198864=CARTESIAN_POINT('Ctrl Pts',(-45.5024319813569,47.2374887985361,
-216.786770074415));
#198865=CARTESIAN_POINT('Ctrl Pts',(-45.5167495780152,47.2292928036801,
-216.787038933162));
#198866=CARTESIAN_POINT('Ctrl Pts',(-45.5313040065756,47.220900253631,-216.787327793623));
#198867=CARTESIAN_POINT('Ctrl Pts',(-45.5524181644651,47.2087251533791,
-216.787746844453));
#198868=CARTESIAN_POINT('Ctrl Pts',(-45.5741687627386,47.195992392959,-216.788262454171));
#198869=CARTESIAN_POINT('Ctrl Pts',(-45.5964324915328,47.1828114367862,
-216.788822892069));
#198870=CARTESIAN_POINT('Ctrl Pts',(-45.6157937849015,47.1713488304231,
-216.789310267865));
#198871=CARTESIAN_POINT('Ctrl Pts',(-45.6355427436437,47.1595476586865,
-216.789831377012));
#198872=CARTESIAN_POINT('Ctrl Pts',(-45.6555763820031,47.1475015125382,
-216.790342880917));
#198873=CARTESIAN_POINT('Ctrl Pts',(-45.6701261773398,47.1387527791373,
-216.79071436996));
#198874=CARTESIAN_POINT('Ctrl Pts',(-45.6848257139981,47.1298752419371,
-216.791080614918));
#198875=CARTESIAN_POINT('Ctrl Pts',(-45.6996282190663,47.1209119881337,
-216.791421896849));
#198876=CARTESIAN_POINT('Ctrl Pts',(-45.7074284250483,47.1161887858369,
-216.79160173596));
#198877=CARTESIAN_POINT('Ctrl Pts',(-45.7159680071028,47.1110106337719,
-216.791789776501));
#198878=CARTESIAN_POINT('Ctrl Pts',(-45.7236196209688,47.1063670490713,
-216.791947909506));
#198879=CARTESIAN_POINT('Ctrl Pts',(-45.7304885278804,47.1021984708337,
-216.792089866603));
#198880=CARTESIAN_POINT('Ctrl Pts',(-45.7366426222728,47.0984607701403,
-216.792208001644));
#198881=CARTESIAN_POINT('Ctrl Pts',(-45.7409359950755,47.0958528577209,
-216.792287234039));
#198882=CARTESIAN_POINT('Ctrl Pts',(-45.7417914642226,47.0953332222931,
-216.792303021364));
#198883=CARTESIAN_POINT('Ctrl Pts',(-45.7426465236319,47.094813812412,-216.792318647381));
#198884=CARTESIAN_POINT('Ctrl Pts',(-45.7435011644022,47.0942946370179,
-216.792334108291));
#198885=CARTESIAN_POINT('Ctrl Pts',(-45.7607808911895,47.0837975846006,
-216.792646707813));
#198886=CARTESIAN_POINT('Ctrl Pts',(-45.7778946723447,47.0733963572817,
-216.792896935563));
#198887=CARTESIAN_POINT('Ctrl Pts',(-45.7948624693683,47.0630713747316,
-216.793096051197));
#198888=CARTESIAN_POINT('Ctrl Pts',(-45.8304764893881,47.0414000797056,
-216.793513978649));
#198889=CARTESIAN_POINT('Ctrl Pts',(-45.8654477034202,47.0200642850446,
-216.793706933556));
#198890=CARTESIAN_POINT('Ctrl Pts',(-45.8999611384402,46.9988822608762,
-216.793779337632));
#198891=CARTESIAN_POINT('Ctrl Pts',(-45.9152590167607,46.9894934524855,
-216.793811430316));
#198892=CARTESIAN_POINT('Ctrl Pts',(-45.930466950287,46.9801348616291,-216.793819834911));
#198893=CARTESIAN_POINT('Ctrl Pts',(-45.945601020205,46.9707906928819,-216.793813626992));
#198894=CARTESIAN_POINT('Ctrl Pts',(-46.0405434277073,46.9121707788883,
-216.793774682097));
#198895=CARTESIAN_POINT('Ctrl Pts',(-46.1322571207837,46.8545743515597,
-216.793059832473));
#198896=CARTESIAN_POINT('Ctrl Pts',(-46.2249336316376,46.793472214907,-216.793167151654));
#198897=CARTESIAN_POINT('Ctrl Pts',(-46.2604025545799,46.7700873576591,
-216.793208224583));
#198898=CARTESIAN_POINT('Ctrl Pts',(-46.2960121446703,46.7461893965824,
-216.793369593332));
#198899=CARTESIAN_POINT('Ctrl Pts',(-46.3319960343607,46.7215258716012,
-216.793734755349));
#198900=CARTESIAN_POINT('Ctrl Pts',(-46.4053341178352,46.6712596088539,
-216.794478985135));
#198901=CARTESIAN_POINT('Ctrl Pts',(-46.4807017416469,46.6170461208078,
-216.796022478167));
#198902=CARTESIAN_POINT('Ctrl Pts',(-46.5530043796985,46.5649816566545,
-216.796566096102));
#198903=CARTESIAN_POINT('Ctrl Pts',(-46.6091179757941,46.5245747726023,
-216.796987994364));
#198904=CARTESIAN_POINT('Ctrl Pts',(-46.6633861233768,46.4854615099449,
-216.796807880319));
#198905=CARTESIAN_POINT('Ctrl Pts',(-46.7134409425736,46.4504754816595,
-216.795189569808));
#198906=CARTESIAN_POINT('Ctrl Pts',(-46.7687398835747,46.4118240521855,
-216.793401712837));
#198907=CARTESIAN_POINT('Ctrl Pts',(-46.8243036818415,46.3717158107884,
-216.792159988029));
#198908=CARTESIAN_POINT('Ctrl Pts',(-46.8797310108264,46.3309773553498,
-216.791008925619));
#198909=CARTESIAN_POINT('Ctrl Pts',(-46.9393413748466,46.2871644168086,
-216.789770993888));
#198910=CARTESIAN_POINT('Ctrl Pts',(-46.99879386052,46.2426226178321,-216.788637887748));
#198911=CARTESIAN_POINT('Ctrl Pts',(-47.0575921287076,46.1983743823903,
-216.787046295788));
#198912=CARTESIAN_POINT('Ctrl Pts',(-48.4710160211071,46.8924605148108,
-213.380827300298));
#198913=CARTESIAN_POINT('Ctrl Pts',(-48.4386236174112,46.8746099006705,
-215.343430354514));
#198914=CARTESIAN_POINT('Ctrl Pts',(-47.5746165801345,45.8238283676803,
-216.758537654376));
#198915=CARTESIAN_POINT('Ctrl Pts',(-48.18620705838,47.1231145402147,-213.379368669215));
#198916=CARTESIAN_POINT('Ctrl Pts',(-48.2020433443809,47.0656079993335,
-215.343093772686));
#198917=CARTESIAN_POINT('Ctrl Pts',(-47.4063346114126,45.9580463783679,
-216.758691640524));
#198918=CARTESIAN_POINT('Ctrl Pts',(-47.8936638370735,47.3370869807156,
-213.387528102977));
#198919=CARTESIAN_POINT('Ctrl Pts',(-47.960805927574,47.2450787050587,-215.353433308545));
#198920=CARTESIAN_POINT('Ctrl Pts',(-47.2339088845747,46.0827106122408,
-216.768384423919));
#198921=CARTESIAN_POINT('Ctrl Pts',(-47.5938143592261,47.5353276146285,
-213.404748058676));
#198922=CARTESIAN_POINT('Ctrl Pts',(-47.7151968771192,47.4137062867165,
-215.373807350724));
#198923=CARTESIAN_POINT('Ctrl Pts',(-47.0575921287078,46.1983743823903,
-216.787046295788));
#198924=CARTESIAN_POINT('',(-48.4710160211073,46.8924605148106,-213.380827300298));
#198925=CARTESIAN_POINT('',(-47.5746165801346,45.8238283676801,-216.758537654376));
#198926=CARTESIAN_POINT('Origin',(-45.3249961798233,43.0072392217583,-213.293565268111));
#198927=CARTESIAN_POINT('Origin',(-42.9552659882971,40.1115177027145,-218.083290145329));
#198928=CARTESIAN_POINT('Origin',(-45.3085773682635,42.9783608246564,-220.208955299598));
#198929=CARTESIAN_POINT('Ctrl Pts',(-51.7300796834963,44.0990078745201,
-213.405670914582));
#198930=CARTESIAN_POINT('Ctrl Pts',(-51.7004178351443,44.0801543735296,
-215.34722316631));
#198931=CARTESIAN_POINT('Ctrl Pts',(-50.7984099663007,43.0953291376926,
-216.756961257354));
#198932=CARTESIAN_POINT('Ctrl Pts',(-50.6732101690724,45.0571976655731,
-213.399273427569));
#198933=CARTESIAN_POINT('Ctrl Pts',(-50.6433589272572,45.0381703096645,
-215.345619228023));
#198934=CARTESIAN_POINT('Ctrl Pts',(-49.7561440689249,44.0321489495878,
-216.756606633385));
#198935=CARTESIAN_POINT('Ctrl Pts',(-49.5810652140705,45.993396027885,-213.390312554607));
#198936=CARTESIAN_POINT('Ctrl Pts',(-49.5465852937888,45.9777566735705,
-215.344527068816));
#198937=CARTESIAN_POINT('Ctrl Pts',(-48.6689534025116,44.9510092870384,
-216.757536292416));
#198938=CARTESIAN_POINT('Ctrl Pts',(-48.471016021107,46.8924605148109,-213.380827300298));
#198939=CARTESIAN_POINT('Ctrl Pts',(-48.4386236174111,46.8746099006705,
-215.343430354514));
#198940=CARTESIAN_POINT('Ctrl Pts',(-47.5746165801344,45.8238283676802,
-216.758537654376));
#198941=CARTESIAN_POINT('Ctrl Pts',(-51.7111509881036,44.1161634878024,
-213.405556127478));
#198942=CARTESIAN_POINT('Ctrl Pts',(-50.6601717838604,45.0683724383644,
-213.399166479425));
#198943=CARTESIAN_POINT('Ctrl Pts',(-49.5744394718705,45.9987624282913,
-213.390255981635));
#198944=CARTESIAN_POINT('Ctrl Pts',(-48.4710160211073,46.8924605148106,
-213.380827300298));
#198945=CARTESIAN_POINT('Ctrl Pts',(-47.5746165801346,45.8238283676801,
-216.758537654376));
#198946=CARTESIAN_POINT('Ctrl Pts',(-48.2691158909411,45.2699109287623,
-216.75790215973));
#198947=CARTESIAN_POINT('Ctrl Pts',(-48.960736291415,44.6974523761734,-216.757294260093));
#198948=CARTESIAN_POINT('Ctrl Pts',(-49.6398238003658,44.1136236554352,
-216.757027743291));
#198949=CARTESIAN_POINT('Ctrl Pts',(-33.311755802625,-74.7642469038882,
-216.366493231411));
#198950=CARTESIAN_POINT('Ctrl Pts',(-33.1370520886648,-74.8239894378111,
-216.284592934174));
#198951=CARTESIAN_POINT('Ctrl Pts',(-32.9632085045191,-74.8606208373411,
-216.188495172326));
#198952=CARTESIAN_POINT('Ctrl Pts',(-31.1602774969193,-72.7635470433165,
-219.49364146861));
#198953=CARTESIAN_POINT('Ctrl Pts',(-30.9603372594918,-72.8299657459105,
-219.402724042838));
#198954=CARTESIAN_POINT('Ctrl Pts',(-30.7643643263463,-72.869370950888,
-219.290077373128));
#198955=CARTESIAN_POINT('Ctrl Pts',(-29.0180188301449,-70.7601533693957,
-222.625390207514));
#198956=CARTESIAN_POINT('Ctrl Pts',(-28.7897411455683,-70.83439285059,-222.523822671102));
#198957=CARTESIAN_POINT('Ctrl Pts',(-28.568544162562,-70.8754191108834,
-222.392137619968));
#198958=CARTESIAN_POINT('Ctrl Pts',(-24.7728929630407,-66.7728546038162,
-228.85960306067));
#198959=CARTESIAN_POINT('Ctrl Pts',(-24.4825290072419,-66.8674311471827,
-228.729735935856));
#198960=CARTESIAN_POINT('Ctrl Pts',(-24.2020295713952,-66.9044734350692,
-228.556369888754));
#198961=CARTESIAN_POINT('Ctrl Pts',(-22.6699986370471,-64.7889483543043,
-231.9620410804));
#198962=CARTESIAN_POINT('Ctrl Pts',(-22.342807556714,-64.8931064786587,
-231.819117937466));
#198963=CARTESIAN_POINT('Ctrl Pts',(-22.031404906377,-64.9275141607773,
-231.618589156426));
#198964=CARTESIAN_POINT('Ctrl Pts',(-20.5752479313931,-62.80283290697,-235.068543705361));
#198965=CARTESIAN_POINT('Ctrl Pts',(-20.2128373512436,-62.9236980507114,
-234.901590690922));
#198966=CARTESIAN_POINT('Ctrl Pts',(-19.8613391097003,-62.9451022381765,
-234.678400237559));
#198967=CARTESIAN_POINT('Ctrl Pts',(-20.0008767707151,-63.0723812833681,
-234.482033933863));
#198968=CARTESIAN_POINT('Ctrl Pts',(-20.6994986722916,-63.7105120854193,
-233.496935192946));
#198969=CARTESIAN_POINT('Ctrl Pts',(-21.3982133314812,-64.3480811557091,
-232.511588190799));
#198970=CARTESIAN_POINT('Ctrl Pts',(-22.09694219437,-64.9851687951656,-231.52601338522));
#198971=CARTESIAN_POINT('Ctrl Pts',(-22.8095499458537,-65.6349109403151,
-230.520862054818));
#198972=CARTESIAN_POINT('Ctrl Pts',(-23.5221722228719,-66.2841526165371,
-229.515473781363));
#198973=CARTESIAN_POINT('Ctrl Pts',(-24.2347817439218,-66.9329758189411,
-228.509870266089));
#198974=CARTESIAN_POINT('Ctrl Pts',(-24.9473912649716,-67.5817990213451,
-227.504266750816));
#198975=CARTESIAN_POINT('Ctrl Pts',(-25.6599879657153,-68.2302039689098,
-226.498447993724));
#198976=CARTESIAN_POINT('Ctrl Pts',(-26.3726021547331,-68.8782657659646,
-225.492435696049));
#198977=CARTESIAN_POINT('Ctrl Pts',(-27.0584834080819,-69.502016239168,
-224.524162840629));
#198978=CARTESIAN_POINT('Ctrl Pts',(-27.7443776014784,-70.1254486506369,
-223.555710117061));
#198979=CARTESIAN_POINT('Ctrl Pts',(-28.4303298112128,-70.7485890029029,
-222.587148305811));
#198980=CARTESIAN_POINT('Ctrl Pts',(-29.113962572594,-71.3696222960424,
-221.621861546477));
#198981=CARTESIAN_POINT('Ctrl Pts',(-29.7976529446887,-71.9903656062306,
-220.656466435943));
#198982=CARTESIAN_POINT('Ctrl Pts',(-30.4814962405759,-72.6108344008091,
-219.691033039098));
#198983=CARTESIAN_POINT('Ctrl Pts',(-31.1627382119588,-73.2289429460596,
-218.729272129163));
#198984=CARTESIAN_POINT('Ctrl Pts',(-31.8441319441618,-73.8467791355826,
-217.767473223644));
#198985=CARTESIAN_POINT('Ctrl Pts',(-32.5258221696848,-74.4643467152214,
-216.805705590893));
#198986=CARTESIAN_POINT('Ctrl Pts',(-32.625128162791,-74.5543115695057,
-216.665599005333));
#198987=CARTESIAN_POINT('Ctrl Pts',(-32.7244405356851,-74.6442707023382,
-216.525493083429));
#198988=CARTESIAN_POINT('Ctrl Pts',(-32.8237598256929,-74.7342241033977,
-216.385388039322));
#198989=CARTESIAN_POINT('Ctrl Pts',(-33.175226286096,-74.6372704537072,
-216.564961398278));
#198990=CARTESIAN_POINT('Ctrl Pts',(-31.0696461183976,-72.6787866297426,
-219.626141064238));
#198991=CARTESIAN_POINT('Ctrl Pts',(-28.9728566675979,-70.7177341242162,
-222.691713455173));
#198992=CARTESIAN_POINT('Ctrl Pts',(-26.8829915137441,-68.754796626235,
-225.760801301184));
#198993=CARTESIAN_POINT('Ctrl Pts',(-24.8618782439252,-66.8564353766208,
-228.728923029217));
#198994=CARTESIAN_POINT('Ctrl Pts',(-22.8473703074868,-64.9562682462704,
-231.700386778281));
#198995=CARTESIAN_POINT('Ctrl Pts',(-20.8402917355536,-63.0540784606782,
-234.675571320252));
#198996=CARTESIAN_POINT('Ctrl Pts',(-48.394724810452,-30.9589748864444,
-236.571980303288));
#198997=CARTESIAN_POINT('Ctrl Pts',(-48.5327606194891,-30.5978875071193,
-236.384422495983));
#198998=CARTESIAN_POINT('Ctrl Pts',(-48.5655760584043,-30.2484467958801,
-236.13656993524));
#198999=CARTESIAN_POINT('Ctrl Pts',(-53.1357762583618,-36.5300914807295,
-229.349840256805));
#199000=CARTESIAN_POINT('Ctrl Pts',(-53.2603596661385,-36.1854606467053,
-229.182436919715));
#199001=CARTESIAN_POINT('Ctrl Pts',(-53.3041702101809,-35.8631937708939,
-228.944594002505));
#199002=CARTESIAN_POINT('Ctrl Pts',(-57.8701242734414,-42.1160518009944,
-222.134994554844));
#199003=CARTESIAN_POINT('Ctrl Pts',(-57.9936838628245,-41.7882503199416,
-221.968743812371));
#199004=CARTESIAN_POINT('Ctrl Pts',(-58.0357658478494,-41.4733525338354,
-221.746435886425));
#199005=CARTESIAN_POINT('Ctrl Pts',(-62.6038224850394,-47.7030040725398,
-214.920479869356));
#199006=CARTESIAN_POINT('Ctrl Pts',(-62.725814975539,-47.3874591829502,
-214.756341305096));
#199007=CARTESIAN_POINT('Ctrl Pts',(-62.767435183335,-47.0792819180526,
-214.544947314852));
#199008=CARTESIAN_POINT('Ctrl Pts',(-49.628292311974,-32.4090169808449,
-234.692797218109));
#199009=CARTESIAN_POINT('Ctrl Pts',(-53.5927125130264,-37.0706922464491,
-228.653306547473));
#199010=CARTESIAN_POINT('Ctrl Pts',(-57.552810123003,-41.7419121172879,
-222.6184966732));
#199011=CARTESIAN_POINT('Ctrl Pts',(-61.5121276273779,-46.414570793914,
-216.584292819144));
#199012=CARTESIAN_POINT('Ctrl Pts',(-61.6760242364037,-45.7878268313144,
-216.206690793879));
#199013=CARTESIAN_POINT('Ctrl Pts',(-61.1290793515412,-45.1397569490598,
-217.039067196821));
#199014=CARTESIAN_POINT('Ctrl Pts',(-60.5821634713164,-44.4918554909971,
-217.871396329666));
#199015=CARTESIAN_POINT('Ctrl Pts',(-60.0352403841908,-43.8439595660193,
-218.703673746095));
#199016=CARTESIAN_POINT('Ctrl Pts',(-59.4881996162324,-43.1959242339954,
-219.53613024273));
#199017=CARTESIAN_POINT('Ctrl Pts',(-58.9411516343724,-42.5478944393375,
-220.36853500069));
#199018=CARTESIAN_POINT('Ctrl Pts',(-58.3940681475654,-41.8997587412459,
-221.200883570786));
#199019=CARTESIAN_POINT('Ctrl Pts',(-57.8468424352846,-41.251454547104,
-222.033448526813));
#199020=CARTESIAN_POINT('Ctrl Pts',(-57.2995811930056,-40.6030443972108,
-222.865957265757));
#199021=CARTESIAN_POINT('Ctrl Pts',(-56.7522641358422,-39.9544683058983,
-223.698405334957));
#199022=CARTESIAN_POINT('Ctrl Pts',(-56.2047806782684,-39.3056950284643,
-224.531106492743));
#199023=CARTESIAN_POINT('Ctrl Pts',(-55.6572413649869,-38.6567557119309,
-225.363746943889));
#199024=CARTESIAN_POINT('Ctrl Pts',(-55.1096340281199,-38.0076418378489,
-226.196322231672));
#199025=CARTESIAN_POINT('Ctrl Pts',(-54.5617391016561,-37.3581870654904,
-227.02933476705));
#199026=CARTESIAN_POINT('Ctrl Pts',(-54.0137760751197,-36.7085575539615,
-227.862282070602));
#199027=CARTESIAN_POINT('Ctrl Pts',(-53.4657409963451,-36.0587963044242,
-228.695159678579));
#199028=CARTESIAN_POINT('Ctrl Pts',(-52.917521126298,-35.4088159626922,
-229.528318123531));
#199029=CARTESIAN_POINT('Ctrl Pts',(-52.3692291552187,-34.7587037974105,
-230.361406825898));
#199030=CARTESIAN_POINT('Ctrl Pts',(-51.8208694062986,-34.1085543663928,
-231.194421317416));
#199031=CARTESIAN_POINT('Ctrl Pts',(-51.272227397378,-33.4580702806543,
-232.027864590717));
#199032=CARTESIAN_POINT('Ctrl Pts',(-50.7235175473517,-32.8075488919341,
-232.861233576751));
#199033=CARTESIAN_POINT('Ctrl Pts',(-50.1747524277536,-32.1571364299523,
-233.694523800349));
#199034=CARTESIAN_POINT('Ctrl Pts',(-50.0025400417543,-31.9530252757239,
-233.956025292537));
#199035=CARTESIAN_POINT('Ctrl Pts',(-49.8303222731896,-31.7489252297835,
-234.217519028063));
#199036=CARTESIAN_POINT('Ctrl Pts',(-49.6580996754575,-31.5448418565169,
-234.479004868619));
#199037=CARTESIAN_POINT('Ctrl Pts',(-62.7235255475978,21.7695413998821,
-214.740437532627));
#199038=CARTESIAN_POINT('Ctrl Pts',(-62.8230072917154,21.4551226732318,
-214.60836056406));
#199039=CARTESIAN_POINT('Ctrl Pts',(-62.8511336743851,21.1472686270111,
-214.433330258979));
#199040=CARTESIAN_POINT('Ctrl Pts',(-57.9208187259037,17.1708899867545,
-222.060179301836));
#199041=CARTESIAN_POINT('Ctrl Pts',(-58.021494482598,16.8444023505525,-221.926546858332));
#199042=CARTESIAN_POINT('Ctrl Pts',(-58.0497358031121,16.5287545279998,
-221.741752515028));
#199043=CARTESIAN_POINT('Ctrl Pts',(-53.1176466678688,12.5728508607834,
-229.37998710404));
#199044=CARTESIAN_POINT('Ctrl Pts',(-53.218552259156,12.2298050378563,-229.246394945677));
#199045=CARTESIAN_POINT('Ctrl Pts',(-53.2484412443996,11.9055419092803,
-229.047156021484));
#199046=CARTESIAN_POINT('Ctrl Pts',(-48.3085599855162,7.99018616088097,
-236.705793683792));
#199047=CARTESIAN_POINT('Ctrl Pts',(-48.4218941664573,7.62742728044422,
-236.553636438645));
#199048=CARTESIAN_POINT('Ctrl Pts',(-48.4402788929552,7.27533655185505,
-236.345585245331));
#199049=CARTESIAN_POINT('Ctrl Pts',(-49.6480781836461,8.44024209637812,
-234.512742074857));
#199050=CARTESIAN_POINT('Ctrl Pts',(-50.20384928812,8.97542501790977,-233.668782076087));
#199051=CARTESIAN_POINT('Ctrl Pts',(-50.7595723119519,9.51073706975706,
-232.824733121525));
#199052=CARTESIAN_POINT('Ctrl Pts',(-51.3152323625987,10.0460216112609,
-231.980601369281));
#199053=CARTESIAN_POINT('Ctrl Pts',(-51.8706442281392,10.5810670683631,
-231.136846647792));
#199054=CARTESIAN_POINT('Ctrl Pts',(-52.4259931689815,11.1160850375145,
-230.293009202567));
#199055=CARTESIAN_POINT('Ctrl Pts',(-52.9812725114739,11.650970496052,-229.449095183471));
#199056=CARTESIAN_POINT('Ctrl Pts',(-53.5363226339063,12.1856351531522,
-228.605529533217));
#199057=CARTESIAN_POINT('Ctrl Pts',(-54.0913032149207,12.7201674059514,
-227.761887372297));
#199058=CARTESIAN_POINT('Ctrl Pts',(-54.6462158429117,13.2545137793697,
-226.918174842962));
#199059=CARTESIAN_POINT('Ctrl Pts',(-55.2296271481594,13.8163026078182,
-226.031131724526));
#199060=CARTESIAN_POINT('Ctrl Pts',(-55.8129632662219,14.3778854664311,
-225.144010824245));
#199061=CARTESIAN_POINT('Ctrl Pts',(-56.3962358505564,14.9392616066232,
-224.256819280148));
#199062=CARTESIAN_POINT('Ctrl Pts',(-56.9505543180094,15.4727705869074,
-223.413668632801));
#199063=CARTESIAN_POINT('Ctrl Pts',(-57.5048154823728,16.0060933155577,
-222.570454181187));
#199064=CARTESIAN_POINT('Ctrl Pts',(-58.0590376778228,16.539281928092,-221.727182052217));
#199065=CARTESIAN_POINT('Ctrl Pts',(-58.6131392156513,17.0723544621467,
-220.884093508838));
#199066=CARTESIAN_POINT('Ctrl Pts',(-59.1672018083433,17.6052929351375,
-220.040947313213));
#199067=CARTESIAN_POINT('Ctrl Pts',(-59.7212517903796,18.1382009308084,
-219.197749588254));
#199068=CARTESIAN_POINT('Ctrl Pts',(-60.2751697034323,18.6709818971143,
-218.354752856472));
#199069=CARTESIAN_POINT('Ctrl Pts',(-60.8290750163752,19.2037323987446,
-217.511704619919));
#199070=CARTESIAN_POINT('Ctrl Pts',(-61.3830019667998,19.7366074479272,
-216.668610997126));
#199071=CARTESIAN_POINT('Ctrl Pts',(-61.470215935575,19.8205068643843,-216.535868690877));
#199072=CARTESIAN_POINT('Ctrl Pts',(-61.5574304566285,19.9044094721162,
-216.403125259528));
#199073=CARTESIAN_POINT('Ctrl Pts',(-61.6446456814072,19.9883159925441,
-216.270380726959));
#199074=CARTESIAN_POINT('Ctrl Pts',(-61.516838435851,20.614157501844,-216.579518431211));
#199075=CARTESIAN_POINT('Ctrl Pts',(-57.5570112912469,16.8228354627662,
-222.614535941297));
#199076=CARTESIAN_POINT('Ctrl Pts',(-53.5965576606815,13.0327700456284,
-228.64993609011));
#199077=CARTESIAN_POINT('Ctrl Pts',(-49.6324230235363,9.25223577675679,
-234.689044294154));
#199078=CARTESIAN_POINT('Ctrl Pts',(-23.9003793742247,38.8880062428322,
-234.874538682189));
#199079=CARTESIAN_POINT('Ctrl Pts',(-23.6220334826828,38.9711510838488,
-234.795483705848));
#199080=CARTESIAN_POINT('Ctrl Pts',(-23.3436315228967,39.0028243075697,
-234.685354940774));
#199081=CARTESIAN_POINT('Ctrl Pts',(-25.3613763022199,40.7570726350447,
-231.772074582798));
#199082=CARTESIAN_POINT('Ctrl Pts',(-25.0911791370723,40.8413872876637,
-231.69349554685));
#199083=CARTESIAN_POINT('Ctrl Pts',(-24.8211729610243,40.8777894793531,
-231.583592072777));
#199084=CARTESIAN_POINT('Ctrl Pts',(-26.8976008470641,42.6201313632963,
-228.700804953167));
#199085=CARTESIAN_POINT('Ctrl Pts',(-26.6295221643462,42.7083584759227,
-228.618927707697));
#199086=CARTESIAN_POINT('Ctrl Pts',(-26.3601999892212,42.7472524558864,
-228.507951791168));
#199087=CARTESIAN_POINT('Ctrl Pts',(-30.0998495294269,46.3266672929645,
-222.608682403592));
#199088=CARTESIAN_POINT('Ctrl Pts',(-29.8266052300516,46.4238562842224,
-222.520666200209));
#199089=CARTESIAN_POINT('Ctrl Pts',(-29.5516593753034,46.4688062321367,
-222.401370424925));
#199090=CARTESIAN_POINT('Ctrl Pts',(-31.7641932541652,48.1699050147461,
-219.588919241872));
#199091=CARTESIAN_POINT('Ctrl Pts',(-31.4847343983961,48.2732692238746,
-219.496139318467));
#199092=CARTESIAN_POINT('Ctrl Pts',(-31.2025135348749,48.3205140505153,
-219.371535847534));
#199093=CARTESIAN_POINT('Ctrl Pts',(-33.4734406974175,50.0051916640201,
-216.589120385861));
#199094=CARTESIAN_POINT('Ctrl Pts',(-33.1846932575851,50.1143213461433,
-216.493132115845));
#199095=CARTESIAN_POINT('Ctrl Pts',(-32.8943360433596,50.1648136138276,
-216.360311415042));
#199096=CARTESIAN_POINT('Ctrl Pts',(-23.9972286658434,39.0117605909834,
-234.66915169881));
#199097=CARTESIAN_POINT('Ctrl Pts',(-25.4292211151269,40.839311165325,-231.636508421791));
#199098=CARTESIAN_POINT('Ctrl Pts',(-26.9329390257305,42.6610372183491,
-228.633571847125));
#199099=CARTESIAN_POINT('Ctrl Pts',(-30.0998477125744,46.3266679391917,
-222.608681818355));
#199100=CARTESIAN_POINT('Ctrl Pts',(-31.7641913965495,48.1699057018269,
-219.588918625145));
#199101=CARTESIAN_POINT('Ctrl Pts',(-33.473440697418,50.0051916640197,-216.589120385862));
#199102=CARTESIAN_POINT('Ctrl Pts',(-32.8943360433598,50.1648136138275,
-216.360311415042));
#199103=CARTESIAN_POINT('Ctrl Pts',(-31.2025135348749,48.3205140505153,
-219.371535847534));
#199104=CARTESIAN_POINT('Ctrl Pts',(-29.5516593753034,46.4688062321367,
-222.401370424925));
#199105=CARTESIAN_POINT('Ctrl Pts',(-26.3792344265555,42.76944847143,-228.471531042451));
#199106=CARTESIAN_POINT('Ctrl Pts',(-24.8578971641406,40.9223874961028,
-231.510220567283));
#199107=CARTESIAN_POINT('Ctrl Pts',(-23.3965311730097,39.0699180251917,
-234.574369193282));
#199108=CARTESIAN_POINT('Origin',(-7.99493453126772,-4.92182388367686,-192.281986444803));
#199109=CARTESIAN_POINT('',(-7.45184924284871,-4.40456343718705,-229.35005));
#199110=CARTESIAN_POINT('',(-8.57396770167424,-4.44514727677342,-229.35005));
#199111=CARTESIAN_POINT('Origin',(-7.99493453126772,-4.92182388367686,-229.35005));
#199112=CARTESIAN_POINT('',(-8.57396770167424,-4.44514727677342,-192.281986444803));
#199113=CARTESIAN_POINT('',(-7.45184924284871,-4.40456343718705,-192.281986444803));
#199114=CARTESIAN_POINT('Origin',(-1.25,-20.2703558849778,-192.281986444803));
#199115=CARTESIAN_POINT('',(-0.5,-20.2703558849778,-229.35005));
#199116=CARTESIAN_POINT('',(-0.5,-20.2703558849778,-235.35005));
#199117=CARTESIAN_POINT('',(-1.14413406213993,-19.5278652094801,-229.35005));
#199118=CARTESIAN_POINT('Origin',(-1.25,-20.2703558849778,-229.35005));
#199119=CARTESIAN_POINT('',(-1.14413406213993,-19.5278652094801,-192.281986444803));
#199120=CARTESIAN_POINT('Origin',(-10.2798200094577,-12.7534818258363,-192.281986444803));
#199121=CARTESIAN_POINT('',(-10.2798200094577,-12.0034818258363,-229.35005));
#199122=CARTESIAN_POINT('',(-10.2798200094577,-12.0034818258363,-229.35005));
#199123=CARTESIAN_POINT('',(-11.0243360211906,-12.844013081618,-229.35005));
#199124=CARTESIAN_POINT('Origin',(-10.2798200094577,-12.7534818258363,-229.35005));
#199125=CARTESIAN_POINT('',(-11.0243360211906,-12.844013081618,-192.281986444803));
#199126=CARTESIAN_POINT('Origin',(-8.76687405914144,-12.7534818258363,-192.281986444803));
#199127=CARTESIAN_POINT('',(-8.02438338364376,-12.6476158879763,-229.35005));
#199128=CARTESIAN_POINT('',(-8.02438338364376,-12.6476158879763,-192.281986444803));
#199129=CARTESIAN_POINT('',(-8.76687405914144,-12.0034818258363,-229.35005));
#199130=CARTESIAN_POINT('Origin',(-8.76687405914144,-12.7534818258363,-229.35005));
#199131=CARTESIAN_POINT('',(-8.76687405914144,-12.0034818258363,-235.35005));
#199132=CARTESIAN_POINT('Origin',(-8.76687405914145,-10.2534818258363,-192.281986444803));
#199133=CARTESIAN_POINT('',(-8.76687405914145,-11.0034818258363,-229.35005));
#199134=CARTESIAN_POINT('',(-8.76687405914145,-11.0034818258363,-229.35005));
#199135=CARTESIAN_POINT('',(-8.02438338364376,-10.3593477636964,-229.35005));
#199136=CARTESIAN_POINT('Origin',(-8.76687405914145,-10.2534818258363,-229.35005));
#199137=CARTESIAN_POINT('',(-8.02438338364376,-10.3593477636964,-192.281986444803));
#199138=CARTESIAN_POINT('Origin',(-10.2798200094577,-10.2534818258363,-192.281986444803));
#199139=CARTESIAN_POINT('',(-11.0243360211906,-10.1629505700546,-229.35005));
#199140=CARTESIAN_POINT('',(-11.0243360211906,-10.1629505700546,-192.281986444803));
#199141=CARTESIAN_POINT('',(-10.2798200094577,-11.0034818258363,-229.35005));
#199142=CARTESIAN_POINT('Origin',(-10.2798200094577,-10.2534818258363,-229.35005));
#199143=CARTESIAN_POINT('',(-10.2798200094577,-11.0034818258363,-229.35005));
#199144=CARTESIAN_POINT('Origin',(-6.95148506756697,-6.01736880073006,-192.281986444803));
#199145=CARTESIAN_POINT('',(-6.36274467860838,-6.48200280121742,-229.35005));
#199146=CARTESIAN_POINT('',(-6.36274467860838,-6.48200280121742,-192.281986444803));
#199147=CARTESIAN_POINT('',(-6.40839977914796,-5.50010835424024,-229.35005));
#199148=CARTESIAN_POINT('Origin',(-6.95148506756697,-6.01736880073006,-229.35005));
#199149=CARTESIAN_POINT('',(-6.40839977914796,-5.50010835424024,-235.35005));
#199150=CARTESIAN_POINT('Origin',(-5.14120077283694,-4.29316731243069,-192.281986444803));
#199151=CARTESIAN_POINT('',(-5.68428606125595,-4.81042775892049,-229.35005));
#199152=CARTESIAN_POINT('',(-5.68428606125595,-4.81042775892049,-229.35005));
#199153=CARTESIAN_POINT('',(-4.70577833960231,-4.90382867901287,-229.35005));
#199154=CARTESIAN_POINT('Origin',(-5.14120077283694,-4.29316731243068,-229.35005));
#199155=CARTESIAN_POINT('',(-4.70577833960231,-4.90382867901288,-192.281986444803));
#199156=CARTESIAN_POINT('Origin',(-1.25,-2.73660776669488,-192.281986444803));
#199157=CARTESIAN_POINT('',(-1.14413406213993,-3.47909844219256,-229.35005));
#199158=CARTESIAN_POINT('',(-1.14413406213993,-3.47909844219257,-192.281986444803));
#199159=CARTESIAN_POINT('',(-0.5,-2.73660776669487,-229.35005));
#199160=CARTESIAN_POINT('Origin',(-1.25,-2.73660776669487,-229.35005));
#199161=CARTESIAN_POINT('',(-0.5,-2.73660776669487,-235.35005));
#199162=CARTESIAN_POINT('Origin',(-8.87499999999985,-23.3741205625531,-192.281986444803));
#199163=CARTESIAN_POINT('',(-8.83216440217218,-22.6253448207192,-229.35005));
#199164=CARTESIAN_POINT('',(-9.62499999999985,-23.3741205625531,-229.35005));
#199165=CARTESIAN_POINT('Origin',(-8.87499999999985,-23.3741205625531,-229.35005));
#199166=CARTESIAN_POINT('',(-9.62499999999985,-23.3741205625531,-235.35005));
#199167=CARTESIAN_POINT('',(-8.83216440217218,-22.6253448207192,-192.281986444803));
#199168=CARTESIAN_POINT('Origin',(-12.7946237611812,-12.7534818258363,-192.281986444803));
#199169=CARTESIAN_POINT('',(-12.0481776255232,-12.6805560652209,-229.35005));
#199170=CARTESIAN_POINT('',(-12.0481776255232,-12.6805560652209,-192.281986444803));
#199171=CARTESIAN_POINT('',(-12.7946237611812,-12.0034818258363,-229.35005));
#199172=CARTESIAN_POINT('Origin',(-12.7946237611812,-12.7534818258363,-229.35005));
#199173=CARTESIAN_POINT('',(-12.7946237611812,-12.0034818258363,-235.35005));
#199174=CARTESIAN_POINT('Origin',(-11.3749999999999,-20.8590213785032,-229.35005));
#199175=CARTESIAN_POINT('',(-11.3749999999999,-21.6090213785032,-229.35005));
#199176=CARTESIAN_POINT('',(-11.3749999999999,-21.6090213785032,-229.35005));
#199177=CARTESIAN_POINT('',(-10.6249999999999,-20.8590213785032,-229.35005));
#199178=CARTESIAN_POINT('Origin',(-11.3749999999999,-20.8590213785032,-229.35005));
#199179=CARTESIAN_POINT('',(-10.6249999999999,-20.8590213785032,-235.35005));
#199180=CARTESIAN_POINT('Origin',(-19.,-20.8590213785032,-229.35005));
#199181=CARTESIAN_POINT('',(-19.75,-20.8590213785032,-229.35005));
#199182=CARTESIAN_POINT('',(-19.75,-20.8590213785032,-235.35005));
#199183=CARTESIAN_POINT('',(-19.,-21.6090213785031,-229.35005));
#199184=CARTESIAN_POINT('Origin',(-19.,-20.8590213785032,-229.35005));
#199185=CARTESIAN_POINT('',(-19.,-21.6090213785031,-229.35005));
#199186=CARTESIAN_POINT('Origin',(-19.,-12.7534818258363,-229.35005));
#199187=CARTESIAN_POINT('',(-19.,-12.0034818258363,-229.35005));
#199188=CARTESIAN_POINT('',(-19.,-12.0034818258363,-229.35005));
#199189=CARTESIAN_POINT('',(-19.75,-12.7534818258363,-229.35005));
#199190=CARTESIAN_POINT('Origin',(-19.,-12.7534818258363,-229.35005));
#199191=CARTESIAN_POINT('',(-19.75,-12.7534818258363,-235.35005));
#199192=CARTESIAN_POINT('Origin',(-12.7946237611812,-10.2534818258363,-192.281986444803));
#199193=CARTESIAN_POINT('',(-12.7946237611812,-11.0034818258363,-229.35005));
#199194=CARTESIAN_POINT('',(-12.7946237611812,-11.0034818258363,-229.35005));
#199195=CARTESIAN_POINT('',(-12.0481776255232,-10.3264075864518,-229.35005));
#199196=CARTESIAN_POINT('Origin',(-12.7946237611812,-10.2534818258363,-229.35005));
#199197=CARTESIAN_POINT('',(-12.0481776255232,-10.3264075864518,-192.281986444803));
#199198=CARTESIAN_POINT('Origin',(-19.,-10.2534818258363,-229.35005));
#199199=CARTESIAN_POINT('',(-19.75,-10.2534818258363,-229.35005));
#199200=CARTESIAN_POINT('',(-19.75,-10.2534818258363,-235.35005));
#199201=CARTESIAN_POINT('',(-19.,-11.0034818258363,-229.35005));
#199202=CARTESIAN_POINT('Origin',(-19.,-10.2534818258363,-229.35005));
#199203=CARTESIAN_POINT('',(-19.,-11.0034818258363,-229.35005));
#199204=CARTESIAN_POINT('Origin',(-19.,-2.14794227316951,-229.35005));
#199205=CARTESIAN_POINT('',(-19.,-1.39794227316951,-229.35005));
#199206=CARTESIAN_POINT('',(-19.,-1.39794227316951,-229.35005));
#199207=CARTESIAN_POINT('',(-19.75,-2.14794227316951,-229.35005));
#199208=CARTESIAN_POINT('Origin',(-19.,-2.14794227316951,-229.35005));
#199209=CARTESIAN_POINT('',(-19.75,-2.14794227316951,-235.35005));
#199210=CARTESIAN_POINT('Origin',(-11.3749999999999,-2.14794227316951,-229.35005));
#199211=CARTESIAN_POINT('',(-10.6249999999999,-2.14794227316951,-229.35005));
#199212=CARTESIAN_POINT('',(-10.6249999999999,-2.14794227316951,-235.35005));
#199213=CARTESIAN_POINT('',(-11.3749999999999,-1.3979422731695,-229.35005));
#199214=CARTESIAN_POINT('Origin',(-11.3749999999999,-2.14794227316951,-229.35005));
#199215=CARTESIAN_POINT('',(-11.3749999999999,-1.3979422731695,-229.35005));
#199216=CARTESIAN_POINT('Origin',(-8.87499999999985,0.367156910880378,-192.281986444803));
#199217=CARTESIAN_POINT('',(-9.62499999999985,0.367156910880385,-229.35005));
#199218=CARTESIAN_POINT('',(-9.62499999999985,0.367156910880383,-229.35005));
#199219=CARTESIAN_POINT('',(-8.83216440217218,-0.38161883095341,-229.35005));
#199220=CARTESIAN_POINT('Origin',(-8.87499999999985,0.367156910880383,-229.35005));
#199221=CARTESIAN_POINT('',(-8.83216440217218,-0.381618830953416,-192.281986444803));
#199222=CARTESIAN_POINT('Origin',(-8.87499999999986,8.45759727949731,-229.35005));
#199223=CARTESIAN_POINT('',(-8.87499999999986,9.20759727949731,-229.35005));
#199224=CARTESIAN_POINT('',(-8.87499999999986,9.20759727949731,-229.35005));
#199225=CARTESIAN_POINT('',(-9.62499999999986,8.45759727949731,-229.35005));
#199226=CARTESIAN_POINT('Origin',(-8.87499999999986,8.45759727949731,-229.35005));
#199227=CARTESIAN_POINT('',(-9.62499999999986,8.45759727949731,-235.35005));
#199228=CARTESIAN_POINT('Origin',(-1.25,8.45759727949731,-229.35005));
#199229=CARTESIAN_POINT('',(-0.5,8.45759727949731,-229.35005));
#199230=CARTESIAN_POINT('',(-0.5,8.45759727949731,-235.35005));
#199231=CARTESIAN_POINT('',(-1.25,9.20759727949731,-229.35005));
#199232=CARTESIAN_POINT('Origin',(-1.25,8.45759727949731,-229.35005));
#199233=CARTESIAN_POINT('',(-1.25,9.20759727949731,-229.35005));
#199234=CARTESIAN_POINT('Origin',(-1.25,2.29555713691451,-192.281986444803));
#199235=CARTESIAN_POINT('',(-1.18233753211584,1.54861551239502,-229.35005));
#199236=CARTESIAN_POINT('',(-1.18233753211584,1.54861551239501,-192.281986444803));
#199237=CARTESIAN_POINT('',(-0.5,2.29555713691451,-229.35005));
#199238=CARTESIAN_POINT('Origin',(-1.25,2.29555713691451,-229.35005));
#199239=CARTESIAN_POINT('',(-0.5,2.29555713691451,-235.35005));
#199240=CARTESIAN_POINT('Origin',(-1.25,-25.3025207885872,-192.281986444803));
#199241=CARTESIAN_POINT('',(-0.5,-25.3025207885872,-229.35005));
#199242=CARTESIAN_POINT('',(-0.5,-25.3025207885872,-235.35005));
#199243=CARTESIAN_POINT('',(-1.18233753211584,-24.5555791640676,-229.35005));
#199244=CARTESIAN_POINT('Origin',(-1.25,-25.3025207885872,-229.35005));
#199245=CARTESIAN_POINT('',(-1.18233753211584,-24.5555791640676,-192.281986444803));
#199246=CARTESIAN_POINT('Origin',(-1.25,-31.46456093117,-229.35005));
#199247=CARTESIAN_POINT('',(-1.25,-32.21456093117,-229.35005));
#199248=CARTESIAN_POINT('',(-1.25,-32.21456093117,-229.35005));
#199249=CARTESIAN_POINT('',(-0.5,-31.46456093117,-229.35005));
#199250=CARTESIAN_POINT('Origin',(-1.25,-31.46456093117,-229.35005));
#199251=CARTESIAN_POINT('',(-0.5,-31.46456093117,-235.35005));
#199252=CARTESIAN_POINT('Origin',(-8.87499999999984,-31.46456093117,-229.35005));
#199253=CARTESIAN_POINT('',(-9.62499999999984,-31.46456093117,-229.35005));
#199254=CARTESIAN_POINT('',(-9.62499999999984,-31.46456093117,-235.35005));
#199255=CARTESIAN_POINT('',(-8.87499999999984,-32.21456093117,-229.35005));
#199256=CARTESIAN_POINT('Origin',(-8.87499999999984,-31.46456093117,-229.35005));
#199257=CARTESIAN_POINT('',(-8.87499999999984,-32.21456093117,-229.35005));
#199258=CARTESIAN_POINT('Origin',(-31.625,21.5631368321642,-229.35005));
#199259=CARTESIAN_POINT('',(-31.625,20.8131368321642,-229.35005));
#199260=CARTESIAN_POINT('',(-31.625,20.8131368321642,-229.35005));
#199261=CARTESIAN_POINT('',(-30.875,21.5631368321642,-229.35005));
#199262=CARTESIAN_POINT('Origin',(-31.625,21.5631368321642,-229.35005));
#199263=CARTESIAN_POINT('',(-30.875,21.5631368321642,-235.35005));
#199264=CARTESIAN_POINT('Origin',(-33.751462642771,21.5631368321642,-229.35005));
#199265=CARTESIAN_POINT('',(-34.2872001450371,22.0880037949896,-229.35005));
#199266=CARTESIAN_POINT('',(-34.2872001450371,22.0880037949896,-229.35005));
#199267=CARTESIAN_POINT('',(-33.751462642771,20.8131368321642,-229.35005));
#199268=CARTESIAN_POINT('Origin',(-33.751462642771,21.5631368321642,-229.35005));
#199269=CARTESIAN_POINT('',(-33.751462642771,20.8131368321642,-229.35005));
#199270=CARTESIAN_POINT('Origin',(-31.625,23.6023848491226,-229.35005));
#199271=CARTESIAN_POINT('',(-30.875,23.6023848491226,-229.35005));
#199272=CARTESIAN_POINT('',(-32.1269841269841,24.1596208280901,-229.35005));
#199273=CARTESIAN_POINT('Origin',(-31.625,23.6023848491226,-229.35005));
#199274=CARTESIAN_POINT('',(-32.1269841269841,24.1596208280901,-229.35005));
#199275=CARTESIAN_POINT('',(-30.875,23.6023848491226,-229.35005));
#199276=CARTESIAN_POINT('Origin',(-29.125,19.0631368321642,-229.35005));
#199277=CARTESIAN_POINT('',(-29.125,19.8131368321642,-229.35005));
#199278=CARTESIAN_POINT('',(-29.125,19.8131368321642,-229.35005));
#199279=CARTESIAN_POINT('',(-29.875,19.0631368321642,-229.35005));
#199280=CARTESIAN_POINT('Origin',(-29.125,19.0631368321642,-229.35005));
#199281=CARTESIAN_POINT('',(-29.875,19.0631368321642,-235.35005));
#199282=CARTESIAN_POINT('Origin',(-21.5,19.0631368321642,-229.35005));
#199283=CARTESIAN_POINT('',(-20.75,19.0631368321642,-229.35005));
#199284=CARTESIAN_POINT('',(-20.75,19.0631368321642,-235.35005));
#199285=CARTESIAN_POINT('',(-21.5,19.8131368321642,-229.35005));
#199286=CARTESIAN_POINT('Origin',(-21.5,19.0631368321642,-229.35005));
#199287=CARTESIAN_POINT('',(-21.5,19.8131368321642,-229.35005));
#199288=CARTESIAN_POINT('Origin',(-21.5,10.9575972794973,-229.35005));
#199289=CARTESIAN_POINT('',(-21.5,10.2075972794973,-229.35005));
#199290=CARTESIAN_POINT('',(-21.5,10.2075972794973,-229.35005));
#199291=CARTESIAN_POINT('',(-20.75,10.9575972794973,-229.35005));
#199292=CARTESIAN_POINT('Origin',(-21.5,10.9575972794973,-229.35005));
#199293=CARTESIAN_POINT('',(-20.75,10.9575972794973,-235.35005));
#199294=CARTESIAN_POINT('Origin',(-29.125,10.9575972794973,-229.35005));
#199295=CARTESIAN_POINT('',(-29.875,10.9575972794973,-229.35005));
#199296=CARTESIAN_POINT('',(-29.875,10.9575972794973,-235.35005));
#199297=CARTESIAN_POINT('',(-29.125,10.2075972794973,-229.35005));
#199298=CARTESIAN_POINT('Origin',(-29.125,10.9575972794973,-229.35005));
#199299=CARTESIAN_POINT('',(-29.125,10.2075972794973,-229.35005));
#199300=CARTESIAN_POINT('Origin',(-29.125,8.45759727949731,-229.35005));
#199301=CARTESIAN_POINT('',(-29.125,9.20759727949731,-229.35005));
#199302=CARTESIAN_POINT('',(-29.125,9.20759727949731,-229.35005));
#199303=CARTESIAN_POINT('',(-29.875,8.45759727949731,-229.35005));
#199304=CARTESIAN_POINT('Origin',(-29.125,8.45759727949731,-229.35005));
#199305=CARTESIAN_POINT('',(-29.875,8.45759727949731,-235.35005));
#199306=CARTESIAN_POINT('Origin',(-21.5,8.45759727949731,-229.35005));
#199307=CARTESIAN_POINT('',(-20.75,8.45759727949731,-229.35005));
#199308=CARTESIAN_POINT('',(-20.75,8.45759727949731,-235.35005));
#199309=CARTESIAN_POINT('',(-21.5,9.20759727949731,-229.35005));
#199310=CARTESIAN_POINT('Origin',(-21.5,8.45759727949731,-229.35005));
#199311=CARTESIAN_POINT('',(-21.5,9.20759727949731,-229.35005));
#199312=CARTESIAN_POINT('Origin',(-21.5,0.35205772683049,-229.35005));
#199313=CARTESIAN_POINT('',(-21.5,-0.39794227316951,-229.35005));
#199314=CARTESIAN_POINT('',(-21.5,-0.39794227316951,-229.35005));
#199315=CARTESIAN_POINT('',(-20.75,0.352057726830487,-229.35005));
#199316=CARTESIAN_POINT('Origin',(-21.5,0.35205772683049,-229.35005));
#199317=CARTESIAN_POINT('',(-20.75,0.352057726830487,-235.35005));
#199318=CARTESIAN_POINT('Origin',(-29.125,0.352057726830493,-229.35005));
#199319=CARTESIAN_POINT('',(-29.875,0.352057726830494,-229.35005));
#199320=CARTESIAN_POINT('',(-29.875,0.352057726830494,-235.35005));
#199321=CARTESIAN_POINT('',(-29.125,-0.397942273169507,-229.35005));
#199322=CARTESIAN_POINT('Origin',(-29.125,0.352057726830493,-229.35005));
#199323=CARTESIAN_POINT('',(-29.125,-0.397942273169507,-229.35005));
#199324=CARTESIAN_POINT('Origin',(-29.125,-44.5701004838368,-229.35005));
#199325=CARTESIAN_POINT('',(-29.125,-43.8201004838368,-229.35005));
#199326=CARTESIAN_POINT('',(-29.125,-43.8201004838368,-229.35005));
#199327=CARTESIAN_POINT('',(-29.875,-44.5701004838368,-229.35005));
#199328=CARTESIAN_POINT('Origin',(-29.125,-44.5701004838368,-229.35005));
#199329=CARTESIAN_POINT('',(-29.875,-44.5701004838368,-235.35005));
#199330=CARTESIAN_POINT('Origin',(-21.5,-44.5701004838368,-229.35005));
#199331=CARTESIAN_POINT('',(-20.75,-44.5701004838368,-229.35005));
#199332=CARTESIAN_POINT('',(-20.75,-44.5701004838368,-235.35005));
#199333=CARTESIAN_POINT('',(-21.5,-43.8201004838368,-229.35005));
#199334=CARTESIAN_POINT('Origin',(-21.5,-44.5701004838368,-229.35005));
#199335=CARTESIAN_POINT('',(-21.5,-43.8201004838368,-229.35005));
#199336=CARTESIAN_POINT('Origin',(-21.5,-52.8339989151841,-229.35005));
#199337=CARTESIAN_POINT('',(-21.5238294101153,-53.5836202590728,-229.35005));
#199338=CARTESIAN_POINT('',(-21.5238294101154,-53.5836202590729,-229.35005));
#199339=CARTESIAN_POINT('',(-20.75,-52.8339989151841,-229.35005));
#199340=CARTESIAN_POINT('Origin',(-21.5,-52.8339989151841,-229.35005));
#199341=CARTESIAN_POINT('',(-20.75,-52.8339989151841,-235.35005));
#199342=CARTESIAN_POINT('Origin',(-29.125,-48.7096221120845,-229.35005));
#199343=CARTESIAN_POINT('',(-29.875,-48.7096221120845,-229.35005));
#199344=CARTESIAN_POINT('',(-29.875,-48.7096221120845,-229.35005));
#199345=CARTESIAN_POINT('',(-29.5873015873016,-49.3001957674217,-229.35005));
#199346=CARTESIAN_POINT('Origin',(-29.125,-48.7096221120845,-229.35005));
#199347=CARTESIAN_POINT('',(-29.5873015873016,-49.3001957674217,-229.35005));
#199348=CARTESIAN_POINT('Origin',(-31.625,-42.0701004838368,-229.35005));
#199349=CARTESIAN_POINT('',(-31.625,-42.8201004838368,-229.35005));
#199350=CARTESIAN_POINT('',(-31.625,-42.8201004838368,-229.35005));
#199351=CARTESIAN_POINT('',(-30.875,-42.0701004838368,-229.35005));
#199352=CARTESIAN_POINT('Origin',(-31.625,-42.0701004838368,-229.35005));
#199353=CARTESIAN_POINT('',(-30.875,-42.0701004838368,-235.35005));
#199354=CARTESIAN_POINT('Origin',(-36.0311576807678,-42.0701004838368,-229.35005));
#199355=CARTESIAN_POINT('',(-36.6030808185578,-42.5552849069797,-229.35005));
#199356=CARTESIAN_POINT('',(-36.6030808185578,-42.5552849069797,-229.35005));
#199357=CARTESIAN_POINT('',(-36.0311576807678,-42.8201004838368,-229.35005));
#199358=CARTESIAN_POINT('Origin',(-36.0311576807678,-42.0701004838368,-229.35005));
#199359=CARTESIAN_POINT('',(-36.0311576807678,-42.8201004838368,-229.35005));
#199360=CARTESIAN_POINT('Origin',(-39.3771239584772,-33.96456093117,-229.35005));
#199361=CARTESIAN_POINT('',(-39.3771239584772,-33.21456093117,-229.35005));
#199362=CARTESIAN_POINT('',(-39.3771239584772,-33.21456093117,-229.35005));
#199363=CARTESIAN_POINT('',(-40.1267106833091,-33.9894555481763,-229.35005));
#199364=CARTESIAN_POINT('Origin',(-39.3771239584772,-33.96456093117,-229.35005));
#199365=CARTESIAN_POINT('',(-40.1267106833092,-33.9894555481763,-229.35005));
#199366=CARTESIAN_POINT('Origin',(-31.625,-33.96456093117,-229.35005));
#199367=CARTESIAN_POINT('',(-30.875,-33.96456093117,-229.35005));
#199368=CARTESIAN_POINT('',(-30.875,-33.96456093117,-235.35005));
#199369=CARTESIAN_POINT('',(-31.625,-33.21456093117,-229.35005));
#199370=CARTESIAN_POINT('Origin',(-31.625,-33.96456093117,-229.35005));
#199371=CARTESIAN_POINT('',(-31.625,-33.21456093117,-229.35005));
#199372=CARTESIAN_POINT('Origin',(-29.125,-2.14794227316952,-229.35005));
#199373=CARTESIAN_POINT('',(-29.125,-1.39794227316951,-229.35005));
#199374=CARTESIAN_POINT('',(-29.125,-1.39794227316951,-229.35005));
#199375=CARTESIAN_POINT('',(-29.875,-2.14794227316951,-229.35005));
#199376=CARTESIAN_POINT('Origin',(-29.125,-2.14794227316952,-229.35005));
#199377=CARTESIAN_POINT('',(-29.875,-2.14794227316951,-235.35005));
#199378=CARTESIAN_POINT('Origin',(-21.5,-2.14794227316951,-229.35005));
#199379=CARTESIAN_POINT('',(-20.75,-2.14794227316951,-229.35005));
#199380=CARTESIAN_POINT('',(-20.75,-2.14794227316951,-235.35005));
#199381=CARTESIAN_POINT('',(-21.5,-1.39794227316951,-229.35005));
#199382=CARTESIAN_POINT('Origin',(-21.5,-2.14794227316951,-229.35005));
#199383=CARTESIAN_POINT('',(-21.5,-1.39794227316951,-229.35005));
#199384=CARTESIAN_POINT('Origin',(-21.5,-10.2534818258363,-229.35005));
#199385=CARTESIAN_POINT('',(-21.5,-11.0034818258363,-229.35005));
#199386=CARTESIAN_POINT('',(-21.5,-11.0034818258363,-229.35005));
#199387=CARTESIAN_POINT('',(-20.75,-10.2534818258363,-229.35005));
#199388=CARTESIAN_POINT('Origin',(-21.5,-10.2534818258363,-229.35005));
#199389=CARTESIAN_POINT('',(-20.75,-10.2534818258363,-235.35005));
#199390=CARTESIAN_POINT('Origin',(-29.125,-10.2534818258363,-229.35005));
#199391=CARTESIAN_POINT('',(-29.875,-10.2534818258363,-229.35005));
#199392=CARTESIAN_POINT('',(-29.875,-10.2534818258363,-235.35005));
#199393=CARTESIAN_POINT('',(-29.125,-11.0034818258363,-229.35005));
#199394=CARTESIAN_POINT('Origin',(-29.125,-10.2534818258363,-229.35005));
#199395=CARTESIAN_POINT('',(-29.125,-11.0034818258363,-229.35005));
#199396=CARTESIAN_POINT('Origin',(-29.125,-12.7534818258363,-229.35005));
#199397=CARTESIAN_POINT('',(-29.125,-12.0034818258363,-229.35005));
#199398=CARTESIAN_POINT('',(-29.125,-12.0034818258363,-229.35005));
#199399=CARTESIAN_POINT('',(-29.875,-12.7534818258363,-229.35005));
#199400=CARTESIAN_POINT('Origin',(-29.125,-12.7534818258363,-229.35005));
#199401=CARTESIAN_POINT('',(-29.875,-12.7534818258363,-235.35005));
#199402=CARTESIAN_POINT('Origin',(-21.5,-12.7534818258363,-229.35005));
#199403=CARTESIAN_POINT('',(-20.75,-12.7534818258363,-229.35005));
#199404=CARTESIAN_POINT('',(-20.75,-12.7534818258363,-235.35005));
#199405=CARTESIAN_POINT('',(-21.5,-12.0034818258363,-229.35005));
#199406=CARTESIAN_POINT('Origin',(-21.5,-12.7534818258363,-229.35005));
#199407=CARTESIAN_POINT('',(-21.5,-12.0034818258363,-229.35005));
#199408=CARTESIAN_POINT('Origin',(-21.5,-20.8590213785032,-229.35005));
#199409=CARTESIAN_POINT('',(-21.5,-21.6090213785031,-229.35005));
#199410=CARTESIAN_POINT('',(-21.5,-21.6090213785031,-229.35005));
#199411=CARTESIAN_POINT('',(-20.75,-20.8590213785032,-229.35005));
#199412=CARTESIAN_POINT('Origin',(-21.5,-20.8590213785032,-229.35005));
#199413=CARTESIAN_POINT('',(-20.75,-20.8590213785032,-235.35005));
#199414=CARTESIAN_POINT('Origin',(-29.125,-20.8590213785032,-229.35005));
#199415=CARTESIAN_POINT('',(-29.875,-20.8590213785032,-229.35005));
#199416=CARTESIAN_POINT('',(-29.875,-20.8590213785032,-235.35005));
#199417=CARTESIAN_POINT('',(-29.125,-21.6090213785031,-229.35005));
#199418=CARTESIAN_POINT('Origin',(-29.125,-20.8590213785032,-229.35005));
#199419=CARTESIAN_POINT('',(-29.125,-21.6090213785031,-229.35005));
#199420=CARTESIAN_POINT('Origin',(-29.125,-23.3590213785032,-229.35005));
#199421=CARTESIAN_POINT('',(-29.125,-22.6090213785032,-229.35005));
#199422=CARTESIAN_POINT('',(-29.125,-22.6090213785032,-229.35005));
#199423=CARTESIAN_POINT('',(-29.875,-23.3590213785032,-229.35005));
#199424=CARTESIAN_POINT('Origin',(-29.125,-23.3590213785032,-229.35005));
#199425=CARTESIAN_POINT('',(-29.875,-23.3590213785032,-235.35005));
#199426=CARTESIAN_POINT('Origin',(-21.5,-23.3590213785032,-229.35005));
#199427=CARTESIAN_POINT('',(-20.75,-23.3590213785032,-229.35005));
#199428=CARTESIAN_POINT('',(-20.75,-23.3590213785032,-235.35005));
#199429=CARTESIAN_POINT('',(-21.5,-22.6090213785032,-229.35005));
#199430=CARTESIAN_POINT('Origin',(-21.5,-23.3590213785032,-229.35005));
#199431=CARTESIAN_POINT('',(-21.5,-22.6090213785032,-229.35005));
#199432=CARTESIAN_POINT('Origin',(-21.5,-31.46456093117,-229.35005));
#199433=CARTESIAN_POINT('',(-21.5,-32.21456093117,-229.35005));
#199434=CARTESIAN_POINT('',(-21.5,-32.21456093117,-229.35005));
#199435=CARTESIAN_POINT('',(-20.75,-31.46456093117,-229.35005));
#199436=CARTESIAN_POINT('Origin',(-21.5,-31.46456093117,-229.35005));
#199437=CARTESIAN_POINT('',(-20.75,-31.46456093117,-235.35005));
#199438=CARTESIAN_POINT('Origin',(-29.125,-31.46456093117,-229.35005));
#199439=CARTESIAN_POINT('',(-29.875,-31.46456093117,-229.35005));
#199440=CARTESIAN_POINT('',(-29.875,-31.46456093117,-235.35005));
#199441=CARTESIAN_POINT('',(-29.125,-32.21456093117,-229.35005));
#199442=CARTESIAN_POINT('Origin',(-29.125,-31.46456093117,-229.35005));
#199443=CARTESIAN_POINT('',(-29.125,-32.21456093117,-229.35005));
#199444=CARTESIAN_POINT('Origin',(-31.625,-44.5701004838368,-229.35005));
#199445=CARTESIAN_POINT('',(-30.875,-44.5701004838368,-229.35005));
#199446=CARTESIAN_POINT('',(-30.875,-44.5701004838368,-235.35005));
#199447=CARTESIAN_POINT('',(-31.625,-43.8201004838368,-229.35005));
#199448=CARTESIAN_POINT('Origin',(-31.625,-44.5701004838368,-229.35005));
#199449=CARTESIAN_POINT('',(-31.625,-43.8201004838368,-229.35005));
#199450=CARTESIAN_POINT('Origin',(-31.625,-46.609348500795,-229.35005));
#199451=CARTESIAN_POINT('',(-32.1269841269841,-47.1665844797626,-229.35005));
#199452=CARTESIAN_POINT('',(-32.1269841269841,-47.1665844797626,-229.35005));
#199453=CARTESIAN_POINT('',(-30.875,-46.609348500795,-229.35005));
#199454=CARTESIAN_POINT('Origin',(-31.625,-46.609348500795,-229.35005));
#199455=CARTESIAN_POINT('',(-30.875,-46.609348500795,-235.35005));
#199456=CARTESIAN_POINT('Origin',(-33.7514626427707,-44.5701004838368,-229.35005));
#199457=CARTESIAN_POINT('',(-33.7514626427707,-43.8201004838368,-229.35005));
#199458=CARTESIAN_POINT('',(-33.7514626427707,-43.8201004838368,-229.35005));
#199459=CARTESIAN_POINT('',(-34.2872001450369,-45.0949674466622,-229.35005));
#199460=CARTESIAN_POINT('Origin',(-33.7514626427707,-44.5701004838368,-229.35005));
#199461=CARTESIAN_POINT('',(-34.2872001450369,-45.0949674466622,-229.35005));
#199462=CARTESIAN_POINT('Origin',(-29.125,-42.0701004838368,-229.35005));
#199463=CARTESIAN_POINT('',(-29.875,-42.0701004838368,-229.35005));
#199464=CARTESIAN_POINT('',(-29.875,-42.0701004838368,-235.35005));
#199465=CARTESIAN_POINT('',(-29.125,-42.8201004838368,-229.35005));
#199466=CARTESIAN_POINT('Origin',(-29.125,-42.0701004838368,-229.35005));
#199467=CARTESIAN_POINT('',(-29.125,-42.8201004838368,-229.35005));
#199468=CARTESIAN_POINT('Origin',(-29.125,-33.96456093117,-229.35005));
#199469=CARTESIAN_POINT('',(-29.125,-33.21456093117,-229.35005));
#199470=CARTESIAN_POINT('',(-29.125,-33.21456093117,-229.35005));
#199471=CARTESIAN_POINT('',(-29.875,-33.96456093117,-229.35005));
#199472=CARTESIAN_POINT('Origin',(-29.125,-33.96456093117,-229.35005));
#199473=CARTESIAN_POINT('',(-29.875,-33.96456093117,-235.35005));
#199474=CARTESIAN_POINT('Origin',(-21.5,-33.96456093117,-229.35005));
#199475=CARTESIAN_POINT('',(-20.75,-33.96456093117,-229.35005));
#199476=CARTESIAN_POINT('',(-20.75,-33.96456093117,-235.35005));
#199477=CARTESIAN_POINT('',(-21.5,-33.21456093117,-229.35005));
#199478=CARTESIAN_POINT('Origin',(-21.5,-33.96456093117,-229.35005));
#199479=CARTESIAN_POINT('',(-21.5,-33.21456093117,-229.35005));
#199480=CARTESIAN_POINT('Origin',(-21.5,-42.0701004838368,-229.35005));
#199481=CARTESIAN_POINT('',(-21.5,-42.8201004838368,-229.35005));
#199482=CARTESIAN_POINT('',(-21.5,-42.8201004838368,-229.35005));
#199483=CARTESIAN_POINT('',(-20.75,-42.0701004838368,-229.35005));
#199484=CARTESIAN_POINT('Origin',(-21.5,-42.0701004838368,-229.35005));
#199485=CARTESIAN_POINT('',(-20.75,-42.0701004838368,-235.35005));
#199486=CARTESIAN_POINT('Origin',(-31.625,-23.3590213785032,-229.35005));
#199487=CARTESIAN_POINT('',(-30.875,-23.3590213785032,-229.35005));
#199488=CARTESIAN_POINT('',(-30.875,-23.3590213785032,-235.35005));
#199489=CARTESIAN_POINT('',(-31.625,-22.6090213785032,-229.35005));
#199490=CARTESIAN_POINT('Origin',(-31.625,-23.3590213785032,-229.35005));
#199491=CARTESIAN_POINT('',(-31.625,-22.6090213785032,-229.35005));
#199492=CARTESIAN_POINT('Origin',(-31.625,-31.46456093117,-229.35005));
#199493=CARTESIAN_POINT('',(-31.625,-32.21456093117,-229.35005));
#199494=CARTESIAN_POINT('',(-31.625,-32.21456093117,-229.35005));
#199495=CARTESIAN_POINT('',(-30.875,-31.46456093117,-229.35005));
#199496=CARTESIAN_POINT('Origin',(-31.625,-31.46456093117,-229.35005));
#199497=CARTESIAN_POINT('',(-30.875,-31.46456093117,-235.35005));
#199498=CARTESIAN_POINT('Origin',(-39.4555265729267,-31.46456093117,-229.35005));
#199499=CARTESIAN_POINT('',(-40.2052001948773,-31.486684686535,-229.35005));
#199500=CARTESIAN_POINT('',(-40.2052001948774,-31.486684686535,-229.35005));
#199501=CARTESIAN_POINT('',(-39.4555265729267,-32.21456093117,-229.35005));
#199502=CARTESIAN_POINT('Origin',(-39.4555265729267,-31.46456093117,-229.35005));
#199503=CARTESIAN_POINT('',(-39.4555265729267,-32.21456093117,-229.35005));
#199504=CARTESIAN_POINT('Origin',(-39.6461373136998,-23.3590213785032,-229.35005));
#199505=CARTESIAN_POINT('',(-39.6461373136998,-22.6090213785032,-229.35005));
#199506=CARTESIAN_POINT('',(-39.6461373136998,-22.6090213785032,-229.35005));
#199507=CARTESIAN_POINT('',(-40.3960221980464,-23.3721614024167,-229.35005));
#199508=CARTESIAN_POINT('Origin',(-39.6461373136998,-23.3590213785032,-229.35005));
#199509=CARTESIAN_POINT('',(-40.3960221980465,-23.3721614024167,-229.35005));
#199510=CARTESIAN_POINT('Origin',(-31.625,-12.7534818258363,-229.35005));
#199511=CARTESIAN_POINT('',(-30.875,-12.7534818258363,-229.35005));
#199512=CARTESIAN_POINT('',(-30.875,-12.7534818258363,-235.35005));
#199513=CARTESIAN_POINT('',(-31.625,-12.0034818258363,-229.35005));
#199514=CARTESIAN_POINT('Origin',(-31.625,-12.7534818258363,-229.35005));
#199515=CARTESIAN_POINT('',(-31.625,-12.0034818258363,-229.35005));
#199516=CARTESIAN_POINT('Origin',(-31.625,-20.8590213785032,-229.35005));
#199517=CARTESIAN_POINT('',(-31.625,-21.6090213785031,-229.35005));
#199518=CARTESIAN_POINT('',(-31.625,-21.6090213785031,-229.35005));
#199519=CARTESIAN_POINT('',(-30.875,-20.8590213785032,-229.35005));
#199520=CARTESIAN_POINT('Origin',(-31.625,-20.8590213785032,-229.35005));
#199521=CARTESIAN_POINT('',(-30.875,-20.8590213785032,-235.35005));
#199522=CARTESIAN_POINT('Origin',(-39.6853241707135,-20.8590213785032,-229.35005));
#199523=CARTESIAN_POINT('',(-40.4352524876037,-20.8693905407753,-229.35005));
#199524=CARTESIAN_POINT('',(-40.4352524876037,-20.8693905407753,-229.35005));
#199525=CARTESIAN_POINT('',(-39.6853241707135,-21.6090213785031,-229.35005));
#199526=CARTESIAN_POINT('Origin',(-39.6853241707135,-20.8590213785032,-229.35005));
#199527=CARTESIAN_POINT('',(-39.6853241707135,-21.6090213785031,-229.35005));
#199528=CARTESIAN_POINT('Origin',(-39.7488454733312,-12.7534818258363,-229.35005));
#199529=CARTESIAN_POINT('',(-39.7488454733312,-12.0034818258363,-229.35005));
#199530=CARTESIAN_POINT('',(-39.7488454733312,-12.0034818258363,-229.35005));
#199531=CARTESIAN_POINT('',(-40.4988441937178,-12.754867256657,-229.35005));
#199532=CARTESIAN_POINT('Origin',(-39.7488454733312,-12.7534818258363,-229.35005));
#199533=CARTESIAN_POINT('',(-40.4988441937178,-12.754867256657,-229.35005));
#199534=CARTESIAN_POINT('Origin',(-31.625,-2.14794227316952,-229.35005));
#199535=CARTESIAN_POINT('',(-30.875,-2.14794227316951,-229.35005));
#199536=CARTESIAN_POINT('',(-30.875,-2.14794227316951,-235.35005));
#199537=CARTESIAN_POINT('',(-31.625,-1.39794227316951,-229.35005));
#199538=CARTESIAN_POINT('Origin',(-31.625,-2.14794227316952,-229.35005));
#199539=CARTESIAN_POINT('',(-31.625,-1.39794227316951,-229.35005));
#199540=CARTESIAN_POINT('Origin',(-31.625,-10.2534818258363,-229.35005));
#199541=CARTESIAN_POINT('',(-31.625,-11.0034818258363,-229.35005));
#199542=CARTESIAN_POINT('',(-31.625,-11.0034818258363,-229.35005));
#199543=CARTESIAN_POINT('',(-30.875,-10.2534818258363,-229.35005));
#199544=CARTESIAN_POINT('Origin',(-31.625,-10.2534818258363,-229.35005));
#199545=CARTESIAN_POINT('',(-30.875,-10.2534818258363,-235.35005));
#199546=CARTESIAN_POINT('Origin',(-39.7488454733312,-10.2534818258363,-229.35005));
#199547=CARTESIAN_POINT('',(-40.4988441937178,-10.2520963950157,-229.35005));
#199548=CARTESIAN_POINT('',(-40.4988441937178,-10.2520963950157,-229.35005));
#199549=CARTESIAN_POINT('',(-39.7488454733312,-11.0034818258363,-229.35005));
#199550=CARTESIAN_POINT('Origin',(-39.7488454733312,-10.2534818258363,-229.35005));
#199551=CARTESIAN_POINT('',(-39.7488454733312,-11.0034818258363,-229.35005));
#199552=CARTESIAN_POINT('Origin',(-39.6853241707135,-2.14794227316952,-229.35005));
#199553=CARTESIAN_POINT('',(-39.6853241707135,-1.39794227316952,-229.35005));
#199554=CARTESIAN_POINT('',(-39.6853241707135,-1.39794227316952,-229.35005));
#199555=CARTESIAN_POINT('',(-40.4352524876037,-2.13757311089736,-229.35005));
#199556=CARTESIAN_POINT('Origin',(-39.6853241707135,-2.14794227316952,-229.35005));
#199557=CARTESIAN_POINT('',(-40.4352524876037,-2.13757311089736,-229.35005));
#199558=CARTESIAN_POINT('Origin',(-31.625,8.45759727949731,-229.35005));
#199559=CARTESIAN_POINT('',(-30.875,8.45759727949731,-229.35005));
#199560=CARTESIAN_POINT('',(-30.875,8.45759727949731,-235.35005));
#199561=CARTESIAN_POINT('',(-31.625,9.20759727949731,-229.35005));
#199562=CARTESIAN_POINT('Origin',(-31.625,8.45759727949731,-229.35005));
#199563=CARTESIAN_POINT('',(-31.625,9.20759727949731,-229.35005));
#199564=CARTESIAN_POINT('Origin',(-31.625,0.352057726830494,-229.35005));
#199565=CARTESIAN_POINT('',(-31.625,-0.397942273169506,-229.35005));
#199566=CARTESIAN_POINT('',(-31.625,-0.397942273169506,-229.35005));
#199567=CARTESIAN_POINT('',(-30.875,0.352057726830494,-229.35005));
#199568=CARTESIAN_POINT('Origin',(-31.625,0.352057726830494,-229.35005));
#199569=CARTESIAN_POINT('',(-30.875,0.352057726830494,-235.35005));
#199570=CARTESIAN_POINT('Origin',(-39.6461373136998,0.352057726830498,-229.35005));
#199571=CARTESIAN_POINT('',(-40.3960221980465,0.365197750743975,-229.35005));
#199572=CARTESIAN_POINT('',(-40.3960221980464,0.365197750743973,-229.35005));
#199573=CARTESIAN_POINT('',(-39.6461373136998,-0.397942273169503,-229.35005));
#199574=CARTESIAN_POINT('Origin',(-39.6461373136998,0.352057726830498,-229.35005));
#199575=CARTESIAN_POINT('',(-39.6461373136998,-0.397942273169503,-229.35005));
#199576=CARTESIAN_POINT('Origin',(-39.4555265729267,8.45759727949731,-229.35005));
#199577=CARTESIAN_POINT('',(-39.4555265729267,9.20759727949731,-229.35005));
#199578=CARTESIAN_POINT('',(-39.4555265729267,9.20759727949731,-229.35005));
#199579=CARTESIAN_POINT('',(-40.2052001948774,8.47972103486228,-229.35005));
#199580=CARTESIAN_POINT('Origin',(-39.4555265729267,8.45759727949731,-229.35005));
#199581=CARTESIAN_POINT('',(-40.2052001948774,8.47972103486227,-229.35005));
#199582=CARTESIAN_POINT('Origin',(-31.625,19.0631368321642,-229.35005));
#199583=CARTESIAN_POINT('',(-30.875,19.0631368321642,-229.35005));
#199584=CARTESIAN_POINT('',(-30.875,19.0631368321642,-235.35005));
#199585=CARTESIAN_POINT('',(-31.625,19.8131368321642,-229.35005));
#199586=CARTESIAN_POINT('Origin',(-31.625,19.0631368321642,-229.35005));
#199587=CARTESIAN_POINT('',(-31.625,19.8131368321642,-229.35005));
#199588=CARTESIAN_POINT('Origin',(-31.625,10.9575972794973,-229.35005));
#199589=CARTESIAN_POINT('',(-31.625,10.2075972794973,-229.35005));
#199590=CARTESIAN_POINT('',(-31.625,10.2075972794973,-229.35005));
#199591=CARTESIAN_POINT('',(-30.875,10.9575972794973,-229.35005));
#199592=CARTESIAN_POINT('Origin',(-31.625,10.9575972794973,-229.35005));
#199593=CARTESIAN_POINT('',(-30.875,10.9575972794973,-235.35005));
#199594=CARTESIAN_POINT('Origin',(-39.3771239584772,10.9575972794973,-229.35005));
#199595=CARTESIAN_POINT('',(-40.1267106833092,10.9824918965036,-229.35005));
#199596=CARTESIAN_POINT('',(-40.1267106833092,10.9824918965036,-229.35005));
#199597=CARTESIAN_POINT('',(-39.3771239584772,10.2075972794973,-229.35005));
#199598=CARTESIAN_POINT('Origin',(-39.3771239584772,10.9575972794973,-229.35005));
#199599=CARTESIAN_POINT('',(-39.3771239584772,10.2075972794973,-229.35005));
#199600=CARTESIAN_POINT('Origin',(-36.0311576807679,19.0631368321642,-229.35005));
#199601=CARTESIAN_POINT('',(-36.0311576807679,19.8131368321642,-229.35005));
#199602=CARTESIAN_POINT('',(-36.0311576807679,19.8131368321642,-229.35005));
#199603=CARTESIAN_POINT('',(-36.6030808185579,19.548321255307,-229.35005));
#199604=CARTESIAN_POINT('Origin',(-36.0311576807679,19.0631368321642,-229.35005));
#199605=CARTESIAN_POINT('',(-36.6030808185579,19.548321255307,-229.35005));
#199606=CARTESIAN_POINT('Origin',(-29.125,21.5631368321642,-229.35005));
#199607=CARTESIAN_POINT('',(-29.875,21.5631368321642,-229.35005));
#199608=CARTESIAN_POINT('',(-29.875,21.5631368321642,-235.35005));
#199609=CARTESIAN_POINT('',(-29.125,20.8131368321642,-229.35005));
#199610=CARTESIAN_POINT('Origin',(-29.125,21.5631368321642,-229.35005));
#199611=CARTESIAN_POINT('',(-29.125,20.8131368321642,-229.35005));
#199612=CARTESIAN_POINT('Origin',(-29.125,25.702658460412,-229.35005));
#199613=CARTESIAN_POINT('',(-29.5873015873016,26.2932321157492,-229.35005));
#199614=CARTESIAN_POINT('',(-29.5873015873016,26.2932321157492,-229.35005));
#199615=CARTESIAN_POINT('',(-29.875,25.702658460412,-229.35005));
#199616=CARTESIAN_POINT('Origin',(-29.125,25.702658460412,-229.35005));
#199617=CARTESIAN_POINT('',(-29.875,25.702658460412,-235.35005));
#199618=CARTESIAN_POINT('Origin',(-21.5,29.0311209585238,-229.35005));
#199619=CARTESIAN_POINT('',(-20.75,29.0311209585238,-229.35005));
#199620=CARTESIAN_POINT('',(-21.5791427781145,29.776933549375,-229.35005));
#199621=CARTESIAN_POINT('Origin',(-21.5,29.0311209585238,-229.35005));
#199622=CARTESIAN_POINT('',(-21.5791427781145,29.7769335493751,-229.35005));
#199623=CARTESIAN_POINT('',(-20.75,29.0311209585238,-229.35005));
#199624=CARTESIAN_POINT('Origin',(-21.5,21.5631368321642,-229.35005));
#199625=CARTESIAN_POINT('',(-21.5,20.8131368321642,-229.35005));
#199626=CARTESIAN_POINT('',(-21.5,20.8131368321642,-229.35005));
#199627=CARTESIAN_POINT('',(-20.75,21.5631368321642,-229.35005));
#199628=CARTESIAN_POINT('Origin',(-21.5,21.5631368321642,-229.35005));
#199629=CARTESIAN_POINT('',(-20.75,21.5631368321642,-235.35005));
#199630=CARTESIAN_POINT('Origin',(-19.,-52.9088458284789,-229.35005));
#199631=CARTESIAN_POINT('',(-19.75,-52.9088458284789,-229.35005));
#199632=CARTESIAN_POINT('',(-19.75,-52.9088458284789,-229.35005));
#199633=CARTESIAN_POINT('',(-19.021058548474,-53.658550128544,-229.35005));
#199634=CARTESIAN_POINT('Origin',(-19.,-52.9088458284789,-229.35005));
#199635=CARTESIAN_POINT('',(-19.021058548474,-53.6585501285442,-229.35005));
#199636=CARTESIAN_POINT('Origin',(-19.,-44.5701004838368,-229.35005));
#199637=CARTESIAN_POINT('',(-19.,-43.8201004838368,-229.35005));
#199638=CARTESIAN_POINT('',(-19.,-43.8201004838368,-229.35005));
#199639=CARTESIAN_POINT('',(-19.75,-44.5701004838368,-229.35005));
#199640=CARTESIAN_POINT('Origin',(-19.,-44.5701004838368,-229.35005));
#199641=CARTESIAN_POINT('',(-19.75,-44.5701004838368,-235.35005));
#199642=CARTESIAN_POINT('Origin',(-11.3749999999999,-44.5701004838369,-229.35005));
#199643=CARTESIAN_POINT('',(-10.6249999999999,-44.5701004838369,-229.35005));
#199644=CARTESIAN_POINT('',(-10.6249999999999,-44.5701004838369,-235.35005));
#199645=CARTESIAN_POINT('',(-11.3749999999999,-43.8201004838368,-229.35005));
#199646=CARTESIAN_POINT('Origin',(-11.3749999999999,-44.5701004838369,-229.35005));
#199647=CARTESIAN_POINT('',(-11.3749999999999,-43.8201004838368,-229.35005));
#199648=CARTESIAN_POINT('Origin',(-11.3749999999999,-53.08002700974,-229.35005));
#199649=CARTESIAN_POINT('',(-11.3876074204679,-53.8299210375528,-229.35005));
#199650=CARTESIAN_POINT('',(-11.3876074204679,-53.8299210375529,-229.35005));
#199651=CARTESIAN_POINT('',(-10.6249999999999,-53.08002700974,-229.35005));
#199652=CARTESIAN_POINT('Origin',(-11.3749999999999,-53.08002700974,-229.35005));
#199653=CARTESIAN_POINT('',(-10.6249999999999,-53.08002700974,-235.35005));
#199654=CARTESIAN_POINT('Origin',(-19.,19.0631368321642,-229.35005));
#199655=CARTESIAN_POINT('',(-19.,19.8131368321642,-229.35005));
#199656=CARTESIAN_POINT('',(-19.,19.8131368321642,-229.35005));
#199657=CARTESIAN_POINT('',(-19.75,19.0631368321642,-229.35005));
#199658=CARTESIAN_POINT('Origin',(-19.,19.0631368321642,-229.35005));
#199659=CARTESIAN_POINT('',(-19.75,19.0631368321642,-235.35005));
#199660=CARTESIAN_POINT('Origin',(-11.3749999999999,19.0631368321642,-229.35005));
#199661=CARTESIAN_POINT('',(-10.6249999999999,19.0631368321642,-229.35005));
#199662=CARTESIAN_POINT('',(-10.6249999999999,19.0631368321642,-235.35005));
#199663=CARTESIAN_POINT('',(-11.3749999999999,19.8131368321642,-229.35005));
#199664=CARTESIAN_POINT('Origin',(-11.3749999999999,19.0631368321642,-229.35005));
#199665=CARTESIAN_POINT('',(-11.3749999999999,19.8131368321642,-229.35005));
#199666=CARTESIAN_POINT('Origin',(-11.3749999999999,10.9575972794973,-229.35005));
#199667=CARTESIAN_POINT('',(-11.3749999999999,10.2075972794973,-229.35005));
#199668=CARTESIAN_POINT('',(-11.3749999999999,10.2075972794973,-229.35005));
#199669=CARTESIAN_POINT('',(-10.6249999999999,10.9575972794973,-229.35005));
#199670=CARTESIAN_POINT('Origin',(-11.3749999999999,10.9575972794973,-229.35005));
#199671=CARTESIAN_POINT('',(-10.6249999999999,10.9575972794973,-235.35005));
#199672=CARTESIAN_POINT('Origin',(-19.,10.9575972794973,-229.35005));
#199673=CARTESIAN_POINT('',(-19.75,10.9575972794973,-229.35005));
#199674=CARTESIAN_POINT('',(-19.75,10.9575972794973,-235.35005));
#199675=CARTESIAN_POINT('',(-19.,10.2075972794973,-229.35005));
#199676=CARTESIAN_POINT('Origin',(-19.,10.9575972794973,-229.35005));
#199677=CARTESIAN_POINT('',(-19.,10.2075972794973,-229.35005));
#199678=CARTESIAN_POINT('Origin',(-19.,8.45759727949731,-229.35005));
#199679=CARTESIAN_POINT('',(-19.,9.20759727949731,-229.35005));
#199680=CARTESIAN_POINT('',(-19.,9.20759727949731,-229.35005));
#199681=CARTESIAN_POINT('',(-19.75,8.45759727949731,-229.35005));
#199682=CARTESIAN_POINT('Origin',(-19.,8.45759727949731,-229.35005));
#199683=CARTESIAN_POINT('',(-19.75,8.45759727949731,-235.35005));
#199684=CARTESIAN_POINT('Origin',(-11.3749999999999,8.45759727949731,-229.35005));
#199685=CARTESIAN_POINT('',(-10.6249999999999,8.45759727949731,-229.35005));
#199686=CARTESIAN_POINT('',(-10.6249999999999,8.45759727949731,-235.35005));
#199687=CARTESIAN_POINT('',(-11.3749999999999,9.20759727949731,-229.35005));
#199688=CARTESIAN_POINT('Origin',(-11.3749999999999,8.45759727949731,-229.35005));
#199689=CARTESIAN_POINT('',(-11.3749999999999,9.20759727949731,-229.35005));
#199690=CARTESIAN_POINT('Origin',(-11.3749999999999,0.352057726830486,-229.35005));
#199691=CARTESIAN_POINT('',(-11.3749999999999,-0.397942273169514,-229.35005));
#199692=CARTESIAN_POINT('',(-11.3749999999999,-0.397942273169514,-229.35005));
#199693=CARTESIAN_POINT('',(-10.6249999999999,0.352057726830487,-229.35005));
#199694=CARTESIAN_POINT('Origin',(-11.3749999999999,0.352057726830486,-229.35005));
#199695=CARTESIAN_POINT('',(-10.6249999999999,0.352057726830487,-235.35005));
#199696=CARTESIAN_POINT('Origin',(-19.,0.352057726830489,-229.35005));
#199697=CARTESIAN_POINT('',(-19.75,0.352057726830487,-229.35005));
#199698=CARTESIAN_POINT('',(-19.75,0.352057726830487,-235.35005));
#199699=CARTESIAN_POINT('',(-19.,-0.397942273169511,-229.35005));
#199700=CARTESIAN_POINT('Origin',(-19.,0.352057726830489,-229.35005));
#199701=CARTESIAN_POINT('',(-19.,-0.397942273169511,-229.35005));
#199702=CARTESIAN_POINT('Origin',(-19.,-23.3590213785032,-229.35005));
#199703=CARTESIAN_POINT('',(-19.,-22.6090213785032,-229.35005));
#199704=CARTESIAN_POINT('',(-19.,-22.6090213785032,-229.35005));
#199705=CARTESIAN_POINT('',(-19.75,-23.3590213785032,-229.35005));
#199706=CARTESIAN_POINT('Origin',(-19.,-23.3590213785032,-229.35005));
#199707=CARTESIAN_POINT('',(-19.75,-23.3590213785032,-235.35005));
#199708=CARTESIAN_POINT('Origin',(-11.3749999999999,-23.3590213785032,-229.35005));
#199709=CARTESIAN_POINT('',(-10.6249999999999,-23.3590213785032,-229.35005));
#199710=CARTESIAN_POINT('',(-10.6249999999999,-23.3590213785032,-235.35005));
#199711=CARTESIAN_POINT('',(-11.3749999999999,-22.6090213785032,-229.35005));
#199712=CARTESIAN_POINT('Origin',(-11.3749999999999,-23.3590213785032,-229.35005));
#199713=CARTESIAN_POINT('',(-11.3749999999999,-22.6090213785032,-229.35005));
#199714=CARTESIAN_POINT('Origin',(-11.3749999999999,-31.46456093117,-229.35005));
#199715=CARTESIAN_POINT('',(-11.3749999999999,-32.21456093117,-229.35005));
#199716=CARTESIAN_POINT('',(-11.3749999999999,-32.21456093117,-229.35005));
#199717=CARTESIAN_POINT('',(-10.6249999999999,-31.46456093117,-229.35005));
#199718=CARTESIAN_POINT('Origin',(-11.3749999999999,-31.46456093117,-229.35005));
#199719=CARTESIAN_POINT('',(-10.6249999999999,-31.46456093117,-235.35005));
#199720=CARTESIAN_POINT('Origin',(-19.,-31.46456093117,-229.35005));
#199721=CARTESIAN_POINT('',(-19.75,-31.46456093117,-229.35005));
#199722=CARTESIAN_POINT('',(-19.75,-31.46456093117,-235.35005));
#199723=CARTESIAN_POINT('',(-19.,-32.21456093117,-229.35005));
#199724=CARTESIAN_POINT('Origin',(-19.,-31.46456093117,-229.35005));
#199725=CARTESIAN_POINT('',(-19.,-32.21456093117,-229.35005));
#199726=CARTESIAN_POINT('Origin',(-19.,-42.0701004838368,-229.35005));
#199727=CARTESIAN_POINT('',(-19.75,-42.0701004838368,-229.35005));
#199728=CARTESIAN_POINT('',(-19.75,-42.0701004838368,-235.35005));
#199729=CARTESIAN_POINT('',(-19.,-42.8201004838368,-229.35005));
#199730=CARTESIAN_POINT('Origin',(-19.,-42.0701004838368,-229.35005));
#199731=CARTESIAN_POINT('',(-19.,-42.8201004838368,-229.35005));
#199732=CARTESIAN_POINT('Origin',(-19.,-33.96456093117,-229.35005));
#199733=CARTESIAN_POINT('',(-19.,-33.21456093117,-229.35005));
#199734=CARTESIAN_POINT('',(-19.,-33.21456093117,-229.35005));
#199735=CARTESIAN_POINT('',(-19.75,-33.96456093117,-229.35005));
#199736=CARTESIAN_POINT('Origin',(-19.,-33.96456093117,-229.35005));
#199737=CARTESIAN_POINT('',(-19.75,-33.96456093117,-235.35005));
#199738=CARTESIAN_POINT('Origin',(-11.3749999999999,-33.96456093117,-229.35005));
#199739=CARTESIAN_POINT('',(-10.6249999999999,-33.96456093117,-229.35005));
#199740=CARTESIAN_POINT('',(-10.6249999999999,-33.96456093117,-235.35005));
#199741=CARTESIAN_POINT('',(-11.3749999999999,-33.21456093117,-229.35005));
#199742=CARTESIAN_POINT('Origin',(-11.3749999999999,-33.96456093117,-229.35005));
#199743=CARTESIAN_POINT('',(-11.3749999999999,-33.21456093117,-229.35005));
#199744=CARTESIAN_POINT('Origin',(-11.3749999999999,-42.0701004838369,-229.35005));
#199745=CARTESIAN_POINT('',(-11.3749999999999,-42.8201004838369,-229.35005));
#199746=CARTESIAN_POINT('',(-11.3749999999999,-42.8201004838369,-229.35005));
#199747=CARTESIAN_POINT('',(-10.6249999999999,-42.0701004838368,-229.35005));
#199748=CARTESIAN_POINT('Origin',(-11.3749999999999,-42.0701004838369,-229.35005));
#199749=CARTESIAN_POINT('',(-10.6249999999999,-42.0701004838368,-235.35005));
#199750=CARTESIAN_POINT('Origin',(-19.,21.5631368321642,-229.35005));
#199751=CARTESIAN_POINT('',(-19.75,21.5631368321642,-229.35005));
#199752=CARTESIAN_POINT('',(-19.75,21.5631368321642,-235.35005));
#199753=CARTESIAN_POINT('',(-19.,20.8131368321642,-229.35005));
#199754=CARTESIAN_POINT('Origin',(-19.,21.5631368321642,-229.35005));
#199755=CARTESIAN_POINT('',(-19.,20.8131368321642,-229.35005));
#199756=CARTESIAN_POINT('Origin',(-19.,29.2808336449858,-229.35005));
#199757=CARTESIAN_POINT('',(-19.0699401294965,30.0275654430807,-229.35005));
#199758=CARTESIAN_POINT('',(-19.0699401294965,30.0275654430807,-229.35005));
#199759=CARTESIAN_POINT('',(-19.75,29.2808336449858,-229.35005));
#199760=CARTESIAN_POINT('Origin',(-19.,29.2808336449858,-229.35005));
#199761=CARTESIAN_POINT('',(-19.75,29.2808336449858,-235.35005));
#199762=CARTESIAN_POINT('Origin',(-11.3749999999999,29.8508988479304,-229.35005));
#199763=CARTESIAN_POINT('',(-10.6249999999999,29.8508988479304,-229.35005));
#199764=CARTESIAN_POINT('',(-11.4168720512116,30.5997290899261,-229.35005));
#199765=CARTESIAN_POINT('Origin',(-11.3749999999999,29.8508988479304,-229.35005));
#199766=CARTESIAN_POINT('',(-11.4168720512116,30.5997290899261,-229.35005));
#199767=CARTESIAN_POINT('',(-10.6249999999999,29.8508988479304,-229.35005));
#199768=CARTESIAN_POINT('Origin',(-11.3749999999999,21.5631368321642,-229.35005));
#199769=CARTESIAN_POINT('',(-11.3749999999999,20.8131368321642,-229.35005));
#199770=CARTESIAN_POINT('',(-11.3749999999999,20.8131368321642,-229.35005));
#199771=CARTESIAN_POINT('',(-10.6249999999999,21.5631368321642,-229.35005));
#199772=CARTESIAN_POINT('Origin',(-11.3749999999999,21.5631368321642,-229.35005));
#199773=CARTESIAN_POINT('',(-10.6249999999999,21.5631368321642,-235.35005));
#199774=CARTESIAN_POINT('Origin',(-8.87499999999984,-53.1174378937751,-229.35005));
#199775=CARTESIAN_POINT('',(-9.62499999999984,-53.1174378937751,-229.35005));
#199776=CARTESIAN_POINT('',(-9.62499999999984,-53.1174378937751,-229.35005));
#199777=CARTESIAN_POINT('',(-8.88483655882654,-53.8673733857413,-229.35005));
#199778=CARTESIAN_POINT('Origin',(-8.87499999999984,-53.1174378937751,-229.35005));
#199779=CARTESIAN_POINT('',(-8.88483655882654,-53.8673733857413,-229.35005));
#199780=CARTESIAN_POINT('Origin',(-8.87499999999984,-44.5701004838369,-229.35005));
#199781=CARTESIAN_POINT('',(-8.87499999999984,-43.8201004838368,-229.35005));
#199782=CARTESIAN_POINT('',(-8.87499999999984,-43.8201004838368,-229.35005));
#199783=CARTESIAN_POINT('',(-9.62499999999984,-44.5701004838369,-229.35005));
#199784=CARTESIAN_POINT('Origin',(-8.87499999999984,-44.5701004838369,-229.35005));
#199785=CARTESIAN_POINT('',(-9.62499999999984,-44.5701004838369,-235.35005));
#199786=CARTESIAN_POINT('Origin',(-1.25,-44.5701004838369,-229.35005));
#199787=CARTESIAN_POINT('',(-0.5,-44.5701004838369,-229.35005));
#199788=CARTESIAN_POINT('',(-0.5,-44.5701004838369,-235.35005));
#199789=CARTESIAN_POINT('',(-1.25,-43.8201004838368,-229.35005));
#199790=CARTESIAN_POINT('Origin',(-1.25,-44.5701004838369,-229.35005));
#199791=CARTESIAN_POINT('',(-1.25,-43.8201004838368,-229.35005));
#199792=CARTESIAN_POINT('Origin',(-1.25,-53.1744855098348,-229.35005));
#199793=CARTESIAN_POINT('',(-1.25138543082066,-53.9244842302215,-229.35005));
#199794=CARTESIAN_POINT('',(-1.25138543082066,-53.9244842302215,-229.35005));
#199795=CARTESIAN_POINT('',(-0.5,-53.1744855098348,-229.35005));
#199796=CARTESIAN_POINT('Origin',(-1.25,-53.1744855098348,-229.35005));
#199797=CARTESIAN_POINT('',(-0.5,-53.1744855098348,-235.35005));
#199798=CARTESIAN_POINT('Origin',(-8.87499999999986,19.0631368321642,-229.35005));
#199799=CARTESIAN_POINT('',(-8.87499999999986,19.8131368321642,-229.35005));
#199800=CARTESIAN_POINT('',(-8.87499999999986,19.8131368321642,-229.35005));
#199801=CARTESIAN_POINT('',(-9.62499999999986,19.0631368321642,-229.35005));
#199802=CARTESIAN_POINT('Origin',(-8.87499999999986,19.0631368321642,-229.35005));
#199803=CARTESIAN_POINT('',(-9.62499999999986,19.0631368321642,-235.35005));
#199804=CARTESIAN_POINT('Origin',(-1.25,19.0631368321642,-229.35005));
#199805=CARTESIAN_POINT('',(-0.5,19.0631368321642,-229.35005));
#199806=CARTESIAN_POINT('',(-0.5,19.0631368321642,-235.35005));
#199807=CARTESIAN_POINT('',(-1.25,19.8131368321642,-229.35005));
#199808=CARTESIAN_POINT('Origin',(-1.25,19.0631368321642,-229.35005));
#199809=CARTESIAN_POINT('',(-1.25,19.8131368321642,-229.35005));
#199810=CARTESIAN_POINT('Origin',(-1.25,10.9575972794973,-229.35005));
#199811=CARTESIAN_POINT('',(-1.25,10.2075972794973,-229.35005));
#199812=CARTESIAN_POINT('',(-1.25,10.2075972794973,-229.35005));
#199813=CARTESIAN_POINT('',(-0.5,10.9575972794973,-229.35005));
#199814=CARTESIAN_POINT('Origin',(-1.25,10.9575972794973,-229.35005));
#199815=CARTESIAN_POINT('',(-0.5,10.9575972794973,-235.35005));
#199816=CARTESIAN_POINT('Origin',(-8.87499999999986,10.9575972794973,-229.35005));
#199817=CARTESIAN_POINT('',(-9.62499999999986,10.9575972794973,-229.35005));
#199818=CARTESIAN_POINT('',(-9.62499999999986,10.9575972794973,-235.35005));
#199819=CARTESIAN_POINT('',(-8.87499999999986,10.2075972794973,-229.35005));
#199820=CARTESIAN_POINT('Origin',(-8.87499999999986,10.9575972794973,-229.35005));
#199821=CARTESIAN_POINT('',(-8.87499999999986,10.2075972794973,-229.35005));
#199822=CARTESIAN_POINT('Origin',(-8.87499999999984,-42.0701004838369,-229.35005));
#199823=CARTESIAN_POINT('',(-9.62499999999984,-42.0701004838368,-229.35005));
#199824=CARTESIAN_POINT('',(-9.62499999999984,-42.0701004838368,-235.35005));
#199825=CARTESIAN_POINT('',(-8.87499999999984,-42.8201004838369,-229.35005));
#199826=CARTESIAN_POINT('Origin',(-8.87499999999984,-42.0701004838369,-229.35005));
#199827=CARTESIAN_POINT('',(-8.87499999999984,-42.8201004838369,-229.35005));
#199828=CARTESIAN_POINT('Origin',(-8.87499999999984,-33.96456093117,-229.35005));
#199829=CARTESIAN_POINT('',(-8.87499999999984,-33.21456093117,-229.35005));
#199830=CARTESIAN_POINT('',(-8.87499999999984,-33.21456093117,-229.35005));
#199831=CARTESIAN_POINT('',(-9.62499999999984,-33.96456093117,-229.35005));
#199832=CARTESIAN_POINT('Origin',(-8.87499999999984,-33.96456093117,-229.35005));
#199833=CARTESIAN_POINT('',(-9.62499999999984,-33.96456093117,-235.35005));
#199834=CARTESIAN_POINT('Origin',(-1.25,-33.96456093117,-229.35005));
#199835=CARTESIAN_POINT('',(-0.5,-33.96456093117,-229.35005));
#199836=CARTESIAN_POINT('',(-0.5,-33.96456093117,-235.35005));
#199837=CARTESIAN_POINT('',(-1.25,-33.21456093117,-229.35005));
#199838=CARTESIAN_POINT('Origin',(-1.25,-33.96456093117,-229.35005));
#199839=CARTESIAN_POINT('',(-1.25,-33.21456093117,-229.35005));
#199840=CARTESIAN_POINT('Origin',(-1.25,-42.0701004838369,-229.35005));
#199841=CARTESIAN_POINT('',(-1.25,-42.8201004838369,-229.35005));
#199842=CARTESIAN_POINT('',(-1.25,-42.8201004838369,-229.35005));
#199843=CARTESIAN_POINT('',(-0.5,-42.0701004838369,-229.35005));
#199844=CARTESIAN_POINT('Origin',(-1.25,-42.0701004838369,-229.35005));
#199845=CARTESIAN_POINT('',(-0.5,-42.0701004838369,-235.35005));
#199846=CARTESIAN_POINT('Origin',(-8.87499999999986,21.5631368321642,-229.35005));
#199847=CARTESIAN_POINT('',(-9.62499999999986,21.5631368321642,-229.35005));
#199848=CARTESIAN_POINT('',(-9.62499999999986,21.5631368321642,-235.35005));
#199849=CARTESIAN_POINT('',(-8.87499999999986,20.8131368321642,-229.35005));
#199850=CARTESIAN_POINT('Origin',(-8.87499999999986,21.5631368321642,-229.35005));
#199851=CARTESIAN_POINT('',(-8.87499999999986,20.8131368321642,-229.35005));
#199852=CARTESIAN_POINT('Origin',(-8.87499999999986,29.9752906431998,-229.35005));
#199853=CARTESIAN_POINT('',(-8.90766940259363,30.7245787787886,-229.35005));
#199854=CARTESIAN_POINT('',(-8.90766940259363,30.7245787787886,-229.35005));
#199855=CARTESIAN_POINT('',(-9.62499999999986,29.9752906431998,-229.35005));
#199856=CARTESIAN_POINT('Origin',(-8.87499999999986,29.9752906431998,-229.35005));
#199857=CARTESIAN_POINT('',(-9.62499999999986,29.9752906431998,-235.35005));
#199858=CARTESIAN_POINT('Origin',(-1.25,30.1648419118246,-229.35005));
#199859=CARTESIAN_POINT('',(-0.5,30.1648419118246,-229.35005));
#199860=CARTESIAN_POINT('',(-1.25460132430898,30.9148277969016,-229.35005));
#199861=CARTESIAN_POINT('Origin',(-1.25,30.1648419118246,-229.35005));
#199862=CARTESIAN_POINT('',(-1.25460132430898,30.9148277969016,-229.35005));
#199863=CARTESIAN_POINT('',(-0.5,30.1648419118246,-229.35005));
#199864=CARTESIAN_POINT('Origin',(-1.25,21.5631368321642,-229.35005));
#199865=CARTESIAN_POINT('',(-1.25,20.8131368321642,-229.35005));
#199866=CARTESIAN_POINT('',(-1.25,20.8131368321642,-229.35005));
#199867=CARTESIAN_POINT('',(-0.5,21.5631368321642,-229.35005));
#199868=CARTESIAN_POINT('Origin',(-1.25,21.5631368321642,-229.35005));
#199869=CARTESIAN_POINT('',(-0.5,21.5631368321642,-235.35005));
#199870=CARTESIAN_POINT('Origin',(-7.99493453126771,-18.0851397679958,-192.281986444803));
#199871=CARTESIAN_POINT('',(-8.57396770167423,-18.5618163748993,-229.35005));
#199872=CARTESIAN_POINT('',(-8.57396770167423,-18.5618163748993,-192.281986444803));
#199873=CARTESIAN_POINT('',(-7.4518492428487,-18.6024002144856,-229.35005));
#199874=CARTESIAN_POINT('Origin',(-7.99493453126771,-18.0851397679958,-229.35005));
#199875=CARTESIAN_POINT('',(-7.4518492428487,-18.6024002144856,-235.35005));
#199876=CARTESIAN_POINT('Origin',(-6.18465023653768,-19.8093412562951,-192.281986444803));
#199877=CARTESIAN_POINT('',(-6.72773552495669,-19.2920808098054,-229.35005));
#199878=CARTESIAN_POINT('',(-6.72773552495669,-19.2920808098054,-229.35005));
#199879=CARTESIAN_POINT('',(-6.63257355852516,-20.4108931639637,-229.35005));
#199880=CARTESIAN_POINT('Origin',(-6.18465023653768,-19.8093412562951,-229.35005));
#199881=CARTESIAN_POINT('',(-6.63257355852516,-20.4108931639637,-192.281986444803));
#199882=CARTESIAN_POINT('Origin',(-6.18465023653769,-3.19762239537749,-192.281986444803));
#199883=CARTESIAN_POINT('',(-6.63257355852517,-2.59607048770891,-229.35005));
#199884=CARTESIAN_POINT('',(-6.63257355852517,-2.59607048770891,-192.281986444803));
#199885=CARTESIAN_POINT('',(-6.7277355249567,-3.7148828418673,-229.35005));
#199886=CARTESIAN_POINT('Origin',(-6.18465023653769,-3.19762239537748,-229.35005));
#199887=CARTESIAN_POINT('',(-6.7277355249567,-3.7148828418673,-192.281986444803));
#199888=CARTESIAN_POINT('Origin',(-1.25,-1.22366181637858,-192.281986444803));
#199889=CARTESIAN_POINT('',(-0.5,-1.22366181637858,-229.35005));
#199890=CARTESIAN_POINT('',(-1.3405312557817,-0.479145804645729,-229.35005));
#199891=CARTESIAN_POINT('Origin',(-1.25,-1.22366181637858,-229.35005));
#199892=CARTESIAN_POINT('',(-1.3405312557817,-0.479145804645732,-192.281986444803));
#199893=CARTESIAN_POINT('',(-0.5,-1.22366181637858,-229.35005));
#199894=CARTESIAN_POINT('Origin',(-1.25,-21.7833018352941,-192.281986444803));
#199895=CARTESIAN_POINT('',(-1.3405312557817,-22.5278178470269,-229.35005));
#199896=CARTESIAN_POINT('',(-1.3405312557817,-22.5278178470269,-192.281986444803));
#199897=CARTESIAN_POINT('',(-0.5,-21.7833018352941,-229.35005));
#199898=CARTESIAN_POINT('Origin',(-1.25,-21.7833018352941,-229.35005));
#199899=CARTESIAN_POINT('',(-0.5,-21.7833018352941,-235.35005));
#199900=CARTESIAN_POINT('Origin',(-5.14120077283693,-18.713796339242,-192.281986444803));
#199901=CARTESIAN_POINT('',(-4.7057783396023,-18.1031349726598,-229.35005));
#199902=CARTESIAN_POINT('',(-5.68428606125594,-18.1965358927522,-229.35005));
#199903=CARTESIAN_POINT('Origin',(-5.14120077283693,-18.713796339242,-229.35005));
#199904=CARTESIAN_POINT('',(-5.68428606125594,-18.1965358927522,-192.281986444803));
#199905=CARTESIAN_POINT('',(-4.7057783396023,-18.1031349726598,-192.281986444803));
#199906=CARTESIAN_POINT('Origin',(-6.95148506756696,-16.9895948509426,-192.281986444803));
#199907=CARTESIAN_POINT('',(-6.40839977914796,-17.5068552974324,-229.35005));
#199908=CARTESIAN_POINT('',(-6.40839977914795,-17.5068552974324,-192.281986444803));
#199909=CARTESIAN_POINT('',(-6.36274467860837,-16.5249608504553,-229.35005));
#199910=CARTESIAN_POINT('Origin',(-6.95148506756696,-16.9895948509426,-229.35005));
#199911=CARTESIAN_POINT('',(-6.36274467860837,-16.5249608504553,-192.281986444803));
#199912=CARTESIAN_POINT('Origin',(-20.625,-3.54959888009691,-192.281986444803));
#199913=CARTESIAN_POINT('',(-11.294759518486,-7.14773903260897,-229.35005));
#199914=CARTESIAN_POINT('',(-11.294759518486,-7.14773903260897,-192.281986444803));
#199915=CARTESIAN_POINT('',(-10.6249999999999,-3.54959888009691,-229.35005));
#199916=CARTESIAN_POINT('Origin',(-20.625,-3.54959888009691,-229.35005));
#199917=CARTESIAN_POINT('',(-10.6249999999999,-3.54959888009691,-235.35005));
#199918=CARTESIAN_POINT('Origin',(-20.625,-19.4573647715757,-192.281986444803));
#199919=CARTESIAN_POINT('',(-10.6249999999999,-19.4573647715757,-229.35005));
#199920=CARTESIAN_POINT('',(-10.6249999999999,-19.4573647715757,-235.35005));
#199921=CARTESIAN_POINT('',(-11.294759518486,-15.8592246190636,-229.35005));
#199922=CARTESIAN_POINT('Origin',(-20.625,-19.4573647715757,-229.35005));
#199923=CARTESIAN_POINT('',(-11.294759518486,-15.8592246190636,-192.281986444803));
#199924=CARTESIAN_POINT('Origin',(-9.40330570654103,-32.6090213785032,-192.281986444803));
#199925=CARTESIAN_POINT('',(-5.33358654455951,-23.474614668563,-229.35005));
#199926=CARTESIAN_POINT('',(-5.33358654455951,-23.474614668563,-192.281986444803));
#199927=CARTESIAN_POINT('Origin',(-9.40330570654103,-32.6090213785032,-229.35005));
#199928=CARTESIAN_POINT('Origin',(-9.40330570654115,9.60205772683048,-192.281986444803));
#199929=CARTESIAN_POINT('',(-5.33358654455957,0.46765101689032,-229.35005));
#199930=CARTESIAN_POINT('Origin',(-9.40330570654115,9.60205772683049,-229.35005));
#199931=CARTESIAN_POINT('',(-5.33358654455957,0.467651016890315,-192.281986444803));
#199932=CARTESIAN_POINT('Origin',(0.,-11.5034818258363,-192.281986444803));
#199933=CARTESIAN_POINT('Origin',(0.,-11.5034818258363,-229.35005));
#199934=CARTESIAN_POINT('Origin',(0.,-11.5034818258363,-192.281986444803));
#199935=CARTESIAN_POINT('Origin',(0.,-11.5034818258363,-229.35005));
#199936=CARTESIAN_POINT('Origin',(0.,-11.5034818258363,-192.281986444803));
#199937=CARTESIAN_POINT('Origin',(0.,-11.5034818258363,-229.35005));
#199938=CARTESIAN_POINT('Origin',(6.10697827817036,-5.81657868152891,-192.281986444803));
#199939=CARTESIAN_POINT('',(6.10697827817036,-5.81657868152891,-229.35005));
#199940=CARTESIAN_POINT('Origin',(5.38286456027835,-5.12689808620917,-192.281986444803));
#199941=CARTESIAN_POINT('',(5.38286456027835,-5.12689808620916,-229.35005));
#199942=CARTESIAN_POINT('Origin',(0.,-11.5034818258363,-192.281986444803));
#199943=CARTESIAN_POINT('Origin',(0.,-11.5034818258363,-229.35005));
#199944=CARTESIAN_POINT('Origin',(0.,-11.5034818258363,-192.281986444803));
#199945=CARTESIAN_POINT('Origin',(0.,-11.5034818258363,-229.35005));
#199946=CARTESIAN_POINT('Origin',(0.,-11.5034818258363,-192.281986444803));
#199947=CARTESIAN_POINT('Origin',(0.,-11.5034818258363,-229.35005));
#199948=CARTESIAN_POINT('Origin',(-5.38286456027834,-5.12689808620917,-192.281986444803));
#199949=CARTESIAN_POINT('',(-5.38286456027834,-5.12689808620916,-229.35005));
#199950=CARTESIAN_POINT('Origin',(-6.10697827817035,-5.81657868152891,-192.281986444803));
#199951=CARTESIAN_POINT('',(-6.10697827817035,-5.81657868152891,-229.35005));
#199952=CARTESIAN_POINT('Origin',(0.,-11.5034818258363,-192.281986444803));
#199953=CARTESIAN_POINT('Origin',(0.,-11.5034818258363,-229.35005));
#199954=CARTESIAN_POINT('Origin',(0.,-11.5034818258363,-192.281986444803));
#199955=CARTESIAN_POINT('Origin',(0.,-11.5034818258363,-229.35005));
#199956=CARTESIAN_POINT('Origin',(-29.875,26.0662450163965,-235.35005));
#199957=CARTESIAN_POINT('',(-29.875,26.0662450163965,-229.35005));
#199958=CARTESIAN_POINT('Origin',(-30.875,26.0662450163965,-235.35005));
#199959=CARTESIAN_POINT('',(-30.875,26.0662450163965,-229.35005));
#199960=CARTESIAN_POINT('Origin',(-30.875,26.0662450163965,-235.35005));
#199961=CARTESIAN_POINT('',(-30.875,26.0662450163965,-229.35005));
#199962=CARTESIAN_POINT('Origin',(-29.875,26.0662450163965,-235.35005));
#199963=CARTESIAN_POINT('',(-29.875,26.0662450163965,-229.35005));
#199964=CARTESIAN_POINT('Origin',(-30.875,26.0662450163965,-235.35005));
#199965=CARTESIAN_POINT('',(-30.875,26.0662450163965,-229.35005));
#199966=CARTESIAN_POINT('Origin',(-29.875,26.0662450163965,-235.35005));
#199967=CARTESIAN_POINT('',(-29.875,26.0662450163965,-229.35005));
#199968=CARTESIAN_POINT('Origin',(-30.875,26.0662450163965,-235.35005));
#199969=CARTESIAN_POINT('',(-30.875,26.0662450163965,-229.35005));
#199970=CARTESIAN_POINT('Origin',(-29.875,26.0662450163965,-235.35005));
#199971=CARTESIAN_POINT('',(-29.875,26.0662450163965,-229.35005));
#199972=CARTESIAN_POINT('Origin',(-30.875,26.0662450163965,-235.35005));
#199973=CARTESIAN_POINT('',(-30.875,26.0662450163965,-229.35005));
#199974=CARTESIAN_POINT('Origin',(-29.875,26.0662450163965,-235.35005));
#199975=CARTESIAN_POINT('',(-29.875,26.0662450163965,-229.35005));
#199976=CARTESIAN_POINT('Origin',(-30.875,26.0662450163965,-235.35005));
#199977=CARTESIAN_POINT('',(-30.875,26.0662450163965,-229.35005));
#199978=CARTESIAN_POINT('Origin',(-29.875,26.0662450163965,-235.35005));
#199979=CARTESIAN_POINT('',(-29.875,26.0662450163965,-229.35005));
#199980=CARTESIAN_POINT('Origin',(-30.875,26.0662450163965,-235.35005));
#199981=CARTESIAN_POINT('',(-30.875,26.0662450163965,-229.35005));
#199982=CARTESIAN_POINT('Origin',(-29.875,26.0662450163965,-235.35005));
#199983=CARTESIAN_POINT('',(-29.875,26.0662450163965,-229.35005));
#199984=CARTESIAN_POINT('Origin',(-30.875,26.0662450163965,-235.35005));
#199985=CARTESIAN_POINT('',(-30.875,26.0662450163965,-229.35005));
#199986=CARTESIAN_POINT('Origin',(-29.875,26.0662450163965,-235.35005));
#199987=CARTESIAN_POINT('',(-29.875,26.0662450163965,-229.35005));
#199988=CARTESIAN_POINT('Origin',(-19.75,32.818676384831,-235.35005));
#199989=CARTESIAN_POINT('',(-19.75,32.818676384831,-229.35005));
#199990=CARTESIAN_POINT('Origin',(-20.75,32.818676384831,-235.35005));
#199991=CARTESIAN_POINT('',(-20.75,32.818676384831,-229.35005));
#199992=CARTESIAN_POINT('Origin',(-20.75,32.818676384831,-235.35005));
#199993=CARTESIAN_POINT('',(-20.75,32.818676384831,-229.35005));
#199994=CARTESIAN_POINT('Origin',(-19.75,32.818676384831,-235.35005));
#199995=CARTESIAN_POINT('',(-19.75,32.818676384831,-229.35005));
#199996=CARTESIAN_POINT('Origin',(-20.75,32.818676384831,-235.35005));
#199997=CARTESIAN_POINT('',(-20.75,32.818676384831,-229.35005));
#199998=CARTESIAN_POINT('Origin',(-19.75,32.818676384831,-235.35005));
#199999=CARTESIAN_POINT('',(-19.75,32.818676384831,-229.35005));
#200000=CARTESIAN_POINT('Origin',(-20.75,32.818676384831,-235.35005));
#200001=CARTESIAN_POINT('',(-20.75,32.818676384831,-229.35005));
#200002=CARTESIAN_POINT('Origin',(-19.75,32.818676384831,-235.35005));
#200003=CARTESIAN_POINT('',(-19.75,32.818676384831,-229.35005));
#200004=CARTESIAN_POINT('Origin',(-20.75,32.818676384831,-235.35005));
#200005=CARTESIAN_POINT('',(-20.75,32.818676384831,-229.35005));
#200006=CARTESIAN_POINT('Origin',(-19.75,32.818676384831,-235.35005));
#200007=CARTESIAN_POINT('',(-19.75,32.818676384831,-229.35005));
#200008=CARTESIAN_POINT('Origin',(-20.75,32.818676384831,-235.35005));
#200009=CARTESIAN_POINT('',(-20.75,32.818676384831,-229.35005));
#200010=CARTESIAN_POINT('Origin',(-19.75,32.818676384831,-235.35005));
#200011=CARTESIAN_POINT('',(-19.75,32.818676384831,-229.35005));
#200012=CARTESIAN_POINT('Origin',(-20.75,32.818676384831,-235.35005));
#200013=CARTESIAN_POINT('',(-20.75,32.818676384831,-229.35005));
#200014=CARTESIAN_POINT('Origin',(-19.75,32.818676384831,-235.35005));
#200015=CARTESIAN_POINT('',(-19.75,32.818676384831,-229.35005));
#200016=CARTESIAN_POINT('Origin',(-20.75,32.818676384831,-235.35005));
#200017=CARTESIAN_POINT('',(-20.75,32.818676384831,-229.35005));
#200018=CARTESIAN_POINT('Origin',(-19.75,32.818676384831,-235.35005));
#200019=CARTESIAN_POINT('',(-19.75,32.818676384831,-229.35005));
#200020=CARTESIAN_POINT('Origin',(-20.75,32.818676384831,-235.35005));
#200021=CARTESIAN_POINT('',(-20.75,32.818676384831,-232.25005));
#200022=CARTESIAN_POINT('',(-20.75,32.818676384831,-229.35005));
#200023=CARTESIAN_POINT('',(-20.75,32.818676384831,-235.35005));
#200024=CARTESIAN_POINT('',(-19.75,32.818676384831,-229.35005));
#200025=CARTESIAN_POINT('',(-20.75,32.818676384831,-229.35005));
#200026=CARTESIAN_POINT('',(-19.75,32.818676384831,-232.25005));
#200027=CARTESIAN_POINT('',(-19.75,32.818676384831,-235.35005));
#200028=CARTESIAN_POINT('',(-11.4589044897296,32.818676384831,-232.25005));
#200029=CARTESIAN_POINT('Origin',(-20.75,32.818676384831,-235.35005));
#200030=CARTESIAN_POINT('',(-20.75,32.3760227311709,-232.25005));
#200031=CARTESIAN_POINT('',(-20.75,32.3760227311709,-229.35005));
#200032=CARTESIAN_POINT('',(-20.75,32.3760227311709,-229.35005));
#200033=CARTESIAN_POINT('',(-20.75,32.818676384831,-229.35005));
#200034=CARTESIAN_POINT('',(-20.75,-32.0203896799758,-232.25005));
#200035=CARTESIAN_POINT('Origin',(-19.75,32.818676384831,-235.35005));
#200036=CARTESIAN_POINT('',(-19.75,32.4743226583832,-229.35005));
#200037=CARTESIAN_POINT('',(-19.75,32.818676384831,-229.35005));
#200038=CARTESIAN_POINT('',(-19.75,32.4743226583831,-232.25005));
#200039=CARTESIAN_POINT('',(-19.75,32.4743226583832,-229.35005));
#200040=CARTESIAN_POINT('',(-19.75,-32.0203896799758,-232.25005));
#200041=CARTESIAN_POINT('Origin',(-9.62499999999986,32.818676384831,-235.35005));
#200042=CARTESIAN_POINT('',(-9.62499999999986,32.818676384831,-229.35005));
#200043=CARTESIAN_POINT('Origin',(-10.6249999999999,32.818676384831,-235.35005));
#200044=CARTESIAN_POINT('',(-10.6249999999999,32.818676384831,-229.35005));
#200045=CARTESIAN_POINT('Origin',(-10.6249999999999,32.818676384831,-235.35005));
#200046=CARTESIAN_POINT('',(-10.6249999999999,32.818676384831,-229.35005));
#200047=CARTESIAN_POINT('Origin',(-9.62499999999986,32.818676384831,-235.35005));
#200048=CARTESIAN_POINT('',(-9.62499999999986,32.818676384831,-229.35005));
#200049=CARTESIAN_POINT('Origin',(-10.6249999999999,32.818676384831,-235.35005));
#200050=CARTESIAN_POINT('',(-10.6249999999999,32.818676384831,-229.35005));
#200051=CARTESIAN_POINT('Origin',(-9.62499999999986,32.818676384831,-235.35005));
#200052=CARTESIAN_POINT('',(-9.62499999999986,32.818676384831,-229.35005));
#200053=CARTESIAN_POINT('Origin',(-10.6249999999999,32.818676384831,-235.35005));
#200054=CARTESIAN_POINT('',(-10.6249999999999,32.818676384831,-229.35005));
#200055=CARTESIAN_POINT('Origin',(-9.62499999999986,32.818676384831,-235.35005));
#200056=CARTESIAN_POINT('',(-9.62499999999986,32.818676384831,-229.35005));
#200057=CARTESIAN_POINT('Origin',(-10.6249999999999,32.818676384831,-235.35005));
#200058=CARTESIAN_POINT('',(-10.6249999999999,32.818676384831,-229.35005));
#200059=CARTESIAN_POINT('Origin',(-10.6249999999999,32.818676384831,-235.35005));
#200060=CARTESIAN_POINT('',(-10.6249999999999,32.818676384831,-229.35005));
#200061=CARTESIAN_POINT('Origin',(-10.6249999999999,32.818676384831,-235.35005));
#200062=CARTESIAN_POINT('',(-10.6249999999999,32.818676384831,-229.35005));
#200063=CARTESIAN_POINT('Origin',(-9.62499999999986,32.818676384831,-235.35005));
#200064=CARTESIAN_POINT('',(-9.62499999999986,32.818676384831,-229.35005));
#200065=CARTESIAN_POINT('Origin',(-10.6249999999999,32.818676384831,-235.35005));
#200066=CARTESIAN_POINT('',(-10.6249999999999,32.818676384831,-229.35005));
#200067=CARTESIAN_POINT('Origin',(-9.62499999999986,32.818676384831,-235.35005));
#200068=CARTESIAN_POINT('',(-9.62499999999986,32.818676384831,-229.35005));
#200069=CARTESIAN_POINT('Origin',(-0.5,32.818676384831,-235.35005));
#200070=CARTESIAN_POINT('',(-0.5,32.818676384831,-229.35005));
#200071=CARTESIAN_POINT('Origin',(-0.5,32.818676384831,-235.35005));
#200072=CARTESIAN_POINT('',(-0.5,32.818676384831,-229.35005));
#200073=CARTESIAN_POINT('Origin',(-0.5,32.818676384831,-235.35005));
#200074=CARTESIAN_POINT('',(-0.5,32.818676384831,-229.35005));
#200075=CARTESIAN_POINT('Origin',(-0.5,32.818676384831,-235.35005));
#200076=CARTESIAN_POINT('',(-0.5,32.818676384831,-229.35005));
#200077=CARTESIAN_POINT('Origin',(-0.5,32.818676384831,-235.35005));
#200078=CARTESIAN_POINT('',(-0.5,32.818676384831,-229.35005));
#200079=CARTESIAN_POINT('Origin',(-0.5,32.818676384831,-235.35005));
#200080=CARTESIAN_POINT('',(-0.5,32.818676384831,-229.35005));
#200081=CARTESIAN_POINT('Origin',(-0.5,32.818676384831,-235.35005));
#200082=CARTESIAN_POINT('',(-0.5,32.818676384831,-229.35005));
#200083=CARTESIAN_POINT('Origin',(-0.5,32.818676384831,-235.35005));
#200084=CARTESIAN_POINT('',(-0.5,32.818676384831,-229.35005));
#200085=CARTESIAN_POINT('Origin',(-24.838300653577,28.3971299569735,-229.35005));
#200086=CARTESIAN_POINT('',(-25.2655040598954,31.8709602996399,-229.35005));
#200087=CARTESIAN_POINT('',(-25.2655040598954,31.8709602996399,-232.25005));
#200088=CARTESIAN_POINT('',(-25.2655040598954,31.8709602996399,-229.35005));
#200089=CARTESIAN_POINT('',(-26.6879613405455,31.3684521110126,-232.25005));
#200090=CARTESIAN_POINT('Origin',(-24.838300653577,28.3971299569735,-232.25005));
#200091=CARTESIAN_POINT('',(-26.6879613405455,31.3684521110126,-229.35005));
#200092=CARTESIAN_POINT('',(-26.6879613405455,31.3684521110126,-229.35005));
#200093=CARTESIAN_POINT('Origin',(-24.838300653577,28.3971299569735,-229.35005));
#200094=CARTESIAN_POINT('Origin',(6.29739814579425E-15,-11.5034818258363,
-229.35005));
#200095=CARTESIAN_POINT('',(-41.8942895912773,16.6943638302095,-232.25005));
#200096=CARTESIAN_POINT('Origin',(6.29739814579425E-15,-11.5034818258363,
-232.25005));
#200097=CARTESIAN_POINT('',(-41.8942895912773,16.6943638302095,-229.35005));
#200098=CARTESIAN_POINT('',(-41.8942895912773,16.6943638302095,-229.35005));
#200099=CARTESIAN_POINT('Origin',(6.29739814579425E-15,-11.5034818258363,
-229.35005));
#200100=CARTESIAN_POINT('Origin',(-38.9907249661392,14.740057695632,-229.35005));
#200101=CARTESIAN_POINT('',(-42.4880898820539,14.8758466676788,-232.25005));
#200102=CARTESIAN_POINT('Origin',(-38.9907249661392,14.740057695632,-232.25005));
#200103=CARTESIAN_POINT('',(-42.4880898820539,14.8758466676788,-229.35005));
#200104=CARTESIAN_POINT('',(-42.4880898820538,14.8758466676788,-229.35005));
#200105=CARTESIAN_POINT('Origin',(-38.9907249661392,14.740057695632,-229.35005));
#200106=CARTESIAN_POINT('Origin',(636.934816028482,-11.5034818258361,-229.35005));
#200107=CARTESIAN_POINT('',(-42.4880898820539,-37.8828103193509,-232.25005));
#200108=CARTESIAN_POINT('Origin',(636.934816028482,-11.5034818258361,-232.25005));
#200109=CARTESIAN_POINT('',(-42.4880898820538,-37.8828103193512,-229.35005));
#200110=CARTESIAN_POINT('',(-42.4880898820539,-37.8828103193507,-229.35005));
#200111=CARTESIAN_POINT('Origin',(636.934816028482,-11.5034818258361,-229.35005));
#200112=CARTESIAN_POINT('Origin',(-38.9907249661392,-37.7470213473046,-229.35005));
#200113=CARTESIAN_POINT('',(-41.8942895912772,-39.701327481882,-232.25005));
#200114=CARTESIAN_POINT('Origin',(-38.9907249661392,-37.7470213473046,-232.25005));
#200115=CARTESIAN_POINT('',(-41.8942895912772,-39.701327481882,-229.35005));
#200116=CARTESIAN_POINT('',(-41.8942895912772,-39.701327481882,-229.35005));
#200117=CARTESIAN_POINT('Origin',(-38.9907249661392,-37.7470213473046,-229.35005));
#200118=CARTESIAN_POINT('Origin',(6.29739814579425E-15,-11.5034818258363,
-229.35005));
#200119=CARTESIAN_POINT('',(-24.6244543289934,-55.593007214519,-232.25005));
#200120=CARTESIAN_POINT('Origin',(6.29739814579425E-15,-11.5034818258363,
-232.25005));
#200121=CARTESIAN_POINT('',(-24.6244543289934,-55.593007214519,-229.35005));
#200122=CARTESIAN_POINT('',(-24.6244543289934,-55.593007214519,-229.35005));
#200123=CARTESIAN_POINT('Origin',(6.29739814579425E-15,-11.5034818258363,
-229.35005));
#200124=CARTESIAN_POINT('Origin',(-22.9178089794592,-52.5372975341153,-229.35005));
#200125=CARTESIAN_POINT('',(-23.036390000908,-56.0352881775208,-232.25005));
#200126=CARTESIAN_POINT('Origin',(-22.9178089794592,-52.5372975341153,-232.25005));
#200127=CARTESIAN_POINT('',(-23.0363900009079,-56.0352881775207,-229.35005));
#200128=CARTESIAN_POINT('',(-23.036390000908,-56.0352881775208,-229.35005));
#200129=CARTESIAN_POINT('Origin',(-22.9178089794592,-52.5372975341153,-229.35005));
#200130=CARTESIAN_POINT('Origin',(-0.127542579976414,-12.8706479699377,
-225.85005));
#200131=CARTESIAN_POINT('',(-45.4582832513426,-55.6286989103146,-225.85004999954));
#200132=CARTESIAN_POINT('',(-46.0196463796681,-56.2008156187296,-225.85005));
#200133=CARTESIAN_POINT('',(-1.84775995058105,-11.1827640290625,-225.85005));
#200134=CARTESIAN_POINT('',(-42.5792116384512,-59.576583500476,-225.85005));
#200135=CARTESIAN_POINT('Origin',(-48.1334350484927,-61.7961505568785,-225.85005));
#200136=CARTESIAN_POINT('',(-41.9650064389658,-58.9506113934371,-225.850044661983));
#200137=CARTESIAN_POINT('',(1.59267479062803,-14.5585319108126,-225.85005));
#200138=CARTESIAN_POINT('Ctrl Pts',(-45.4582832505119,-55.6286989095207,
-225.85005));
#200139=CARTESIAN_POINT('Ctrl Pts',(-44.9107918876255,-56.2015386026923,
-225.85005));
#200140=CARTESIAN_POINT('Ctrl Pts',(-44.349042231461,-56.7629778840832,
-225.85005));
#200141=CARTESIAN_POINT('Ctrl Pts',(-43.1825099491978,-57.8740631734374,
-225.85005));
#200142=CARTESIAN_POINT('Ctrl Pts',(-42.578325837185,-58.4209877839039,
-225.85005));
#200143=CARTESIAN_POINT('Ctrl Pts',(-41.9650009328216,-58.9506050170295,
-225.85005));
#200144=CARTESIAN_POINT('Origin',(-53.4203077633109,-63.7432454966418,-228.35005));
#200145=CARTESIAN_POINT('',(-46.030027498998,-56.2113956007998,-225.073027461918));
#200146=CARTESIAN_POINT('Ctrl Pts',(-46.030027499018,-56.2113956008005,
-225.073027461933));
#200147=CARTESIAN_POINT('Ctrl Pts',(-45.9347321456546,-56.1142747513013,
-225.202538647974));
#200148=CARTESIAN_POINT('Ctrl Pts',(-45.8394511612794,-56.0171685460456,
-225.332029751687));
#200149=CARTESIAN_POINT('Ctrl Pts',(-45.6488607659844,-55.8229271644452,
-225.591049471117));
#200150=CARTESIAN_POINT('Ctrl Pts',(-45.5535783484286,-55.7258194985544,
-225.720541401809));
#200151=CARTESIAN_POINT('Ctrl Pts',(-45.4582832511563,-55.6286989100522,
-225.850049999207));
#200152=CARTESIAN_POINT('',(-46.0300271011815,-56.2113951953429,-225.073057235855));
#200153=CARTESIAN_POINT('Origin',(-0.128459562639233,-12.6359082483571,
-225.85005));
#200154=CARTESIAN_POINT('',(-43.3207863665692,34.1152634411122,-225.85005));
#200155=CARTESIAN_POINT('',(-43.7661191577225,33.2092653453444,-225.850049986044));
#200156=CARTESIAN_POINT('Origin',(-48.892180948596,36.2913696007177,-225.85005));
#200157=CARTESIAN_POINT('',(-43.0713417429913,33.8649821651551,-225.850049999629));
#200158=CARTESIAN_POINT('Ctrl Pts',(-43.7661189699064,33.2092654881215,
-225.85005));
#200159=CARTESIAN_POINT('Ctrl Pts',(-43.6513378416623,33.3196167357978,
-225.85005));
#200160=CARTESIAN_POINT('Ctrl Pts',(-43.536034293583,33.4294426364236,-225.85005));
#200161=CARTESIAN_POINT('Ctrl Pts',(-43.3044413536273,33.6480087459458,
-225.85005));
#200162=CARTESIAN_POINT('Ctrl Pts',(-43.188133837425,33.7567660993298,-225.85005));
#200163=CARTESIAN_POINT('Ctrl Pts',(-43.0713417424048,33.8649821645222,
-225.85005));
#200164=CARTESIAN_POINT('',(-50.4030915963197,41.2213231498315,-225.85005));
#200165=CARTESIAN_POINT('Origin',(-50.4030915963197,41.2213231498315,-228.35005));
#200166=CARTESIAN_POINT('',(-43.3259173910555,34.1204116753589,-225.468974352258));
#200167=CARTESIAN_POINT('Ctrl Pts',(-43.3259173910559,34.1204116753647,
-225.468974352262));
#200168=CARTESIAN_POINT('Ctrl Pts',(-43.2834889553441,34.07784093212,-225.532489881091));
#200169=CARTESIAN_POINT('Ctrl Pts',(-43.2410614098359,34.0352710820648,
-225.59600200373));
#200170=CARTESIAN_POINT('Ctrl Pts',(-43.1562018220031,33.9501268700554,
-225.723028788387));
#200171=CARTESIAN_POINT('Ctrl Pts',(-43.1137729119589,33.9075556508875,
-225.786538761693));
#200172=CARTESIAN_POINT('Ctrl Pts',(-43.0713417427678,33.8649821649953,
-225.850049999372));
#200173=CARTESIAN_POINT('',(-43.3259171707406,34.1204114543102,-225.468990713749));
#200174=CARTESIAN_POINT('Origin',(-48.982196043432,-44.3222432618617,-167.906149834141));
#200175=CARTESIAN_POINT('',(-54.2707699605536,-64.1721709500326,-208.192630912054));
#200176=CARTESIAN_POINT('',(-54.238698329297,-64.0517945379221,-214.260116171494));
#200177=CARTESIAN_POINT('Ctrl Pts',(-54.2707699605539,-64.1721709500341,
-208.192630912048));
#200178=CARTESIAN_POINT('Ctrl Pts',(-54.2547227572974,-64.1119400013452,
-211.229354398965));
#200179=CARTESIAN_POINT('Ctrl Pts',(-54.2386983294438,-64.051794536968,
-214.260116171476));
#200180=CARTESIAN_POINT('',(-54.2707699605536,-64.1721709500326,-215.85005));
#200181=CARTESIAN_POINT('',(-54.2707699605536,-64.1721709500326,-208.192630912054));
#200182=CARTESIAN_POINT('',(-53.7300151844416,-62.1425230012532,-215.85005));
#200183=CARTESIAN_POINT('',(-53.272912245153,-60.426850603907,-215.85005));
#200184=CARTESIAN_POINT('Ctrl Pts',(-53.7300151844417,-62.1425230012532,
-215.85005));
#200185=CARTESIAN_POINT('Ctrl Pts',(-53.8150179700973,-62.461569151501,
-215.585784056343));
#200186=CARTESIAN_POINT('Ctrl Pts',(-53.8997787313594,-62.7797068968052,
-215.321544427158));
#200187=CARTESIAN_POINT('Ctrl Pts',(-54.0694761933671,-63.4166427518218,
-214.791113982276));
#200188=CARTESIAN_POINT('Ctrl Pts',(-54.1539754816099,-63.7337990944548,
-214.526290576097));
#200189=CARTESIAN_POINT('Ctrl Pts',(-54.238698329735,-64.0517945380611,
-214.260116171799));
#200190=CARTESIAN_POINT('Origin',(-52.3809255634408,-67.7420224291304,-167.906149834141));
#200191=CARTESIAN_POINT('',(-50.9302694872204,-67.3511117063321,-214.24934096818));
#200192=CARTESIAN_POINT('',(-51.0503406624406,-67.3834674874005,-208.192630912054));
#200193=CARTESIAN_POINT('Ctrl Pts',(-50.9302694862954,-67.35111170647,-214.249340968162));
#200194=CARTESIAN_POINT('Ctrl Pts',(-50.9902625163406,-67.3672781287523,
-211.223956213722));
#200195=CARTESIAN_POINT('Ctrl Pts',(-51.0503406624421,-67.3834674874009,
-208.192630912048));
#200196=CARTESIAN_POINT('',(-48.9715866554311,-66.8233021636441,-215.85005));
#200197=CARTESIAN_POINT('Ctrl Pts',(-50.930269487352,-67.3511117067548,
-214.249340968478));
#200198=CARTESIAN_POINT('Ctrl Pts',(-50.6074451104335,-67.2641196812418,
-214.515373951332));
#200199=CARTESIAN_POINT('Ctrl Pts',(-50.2841497321107,-67.1770007341929,
-214.780661946596));
#200200=CARTESIAN_POINT('Ctrl Pts',(-49.631251415414,-67.0010631313216,
-215.314234969152));
#200201=CARTESIAN_POINT('Ctrl Pts',(-49.3016472827222,-66.9122441536643,
-215.582485903116));
#200202=CARTESIAN_POINT('Ctrl Pts',(-48.9715866554311,-66.8233021636442,
-215.85005));
#200203=CARTESIAN_POINT('',(-51.0503406624406,-67.3834674874005,-215.85005));
#200204=CARTESIAN_POINT('',(-52.3809255634408,-67.7420224291304,-215.85005));
#200205=CARTESIAN_POINT('',(-51.0503406624406,-67.3834674874005,-208.192630912054));
#200206=CARTESIAN_POINT('Origin',(0.,-12.9675000200281,-167.906149834141));
#200207=CARTESIAN_POINT('Origin',(0.,-12.9675000200281,-208.192630912054));
#200208=CARTESIAN_POINT('Origin',(0.,-12.9675000200281,-215.85005));
#200209=CARTESIAN_POINT('Origin',(-48.9106432152246,18.4987427374335,-167.906149834141));
#200210=CARTESIAN_POINT('',(-54.1218033366501,38.2387592929899,-214.33352989342));
#200211=CARTESIAN_POINT('',(-54.1539855075907,38.3606662320892,-208.192630912062));
#200212=CARTESIAN_POINT('Ctrl Pts',(-54.1218033367874,38.2387592920601,
-214.333529893402));
#200213=CARTESIAN_POINT('Ctrl Pts',(-54.1378828568779,38.299668952361,-211.26613387672));
#200214=CARTESIAN_POINT('Ctrl Pts',(-54.1539855075911,38.3606662320908,
-208.192630912056));
#200215=CARTESIAN_POINT('',(-53.6858060762413,36.5871897873467,-215.85005));
#200216=CARTESIAN_POINT('Ctrl Pts',(-54.1218033370754,38.2387592931511,
-214.333529893716));
#200217=CARTESIAN_POINT('Ctrl Pts',(-54.0493242413351,37.964206503292,-214.587336490157));
#200218=CARTESIAN_POINT('Ctrl Pts',(-53.9768175206508,37.6895490693906,
-214.840391892303));
#200219=CARTESIAN_POINT('Ctrl Pts',(-53.8314491180661,37.1388895988311,
-215.346026703316));
#200220=CARTESIAN_POINT('Ctrl Pts',(-53.7586988751215,36.8633096959739,
-215.598218415201));
#200221=CARTESIAN_POINT('Ctrl Pts',(-53.6858060762413,36.5871897873468,
-215.85005));
#200222=CARTESIAN_POINT('',(-54.1539855075907,38.3606662320892,-215.85005));
#200223=CARTESIAN_POINT('',(-53.3004948454233,35.1276203445352,-215.85005));
#200224=CARTESIAN_POINT('',(-54.1539855075907,38.3606662320892,-208.192630912062));
#200225=CARTESIAN_POINT('Origin',(-52.2560139340206,41.9262034053684,-167.906149834141));
#200226=CARTESIAN_POINT('',(-50.9262492693411,41.5646183371225,-208.192630912063));
#200227=CARTESIAN_POINT('',(-50.8045364442235,41.5315226009329,-214.335913275013));
#200228=CARTESIAN_POINT('Ctrl Pts',(-50.9262492693426,41.5646183371229,
-208.192630912057));
#200229=CARTESIAN_POINT('Ctrl Pts',(-50.8653490995025,41.5480585708328,
-211.267327940101));
#200230=CARTESIAN_POINT('Ctrl Pts',(-50.8045364435665,41.5315226010249,
-214.335913275001));
#200231=CARTESIAN_POINT('',(-50.9262492693411,41.5646183371225,-215.85005));
#200232=CARTESIAN_POINT('',(-50.9262492693411,41.5646183371225,-208.192630912063));
#200233=CARTESIAN_POINT('',(-49.1680521502591,41.086535378401,-215.85005));
#200234=CARTESIAN_POINT('',(-47.6970590536189,40.6865479570431,-215.85005));
#200235=CARTESIAN_POINT('Ctrl Pts',(-49.1680521502592,41.086535378401,-215.85005));
#200236=CARTESIAN_POINT('Ctrl Pts',(-49.4414268426942,41.1608704915578,
-215.598356099776));
#200237=CARTESIAN_POINT('Ctrl Pts',(-49.7144017835719,41.2350969056357,
-215.346413106432));
#200238=CARTESIAN_POINT('Ctrl Pts',(-50.2599964077829,41.3834531333729,
-214.841609804261));
#200239=CARTESIAN_POINT('Ctrl Pts',(-50.532314182124,41.4575008529695,-214.589028866928));
#200240=CARTESIAN_POINT('Ctrl Pts',(-50.8045364443354,41.5315226012339,
-214.335913275222));
#200241=CARTESIAN_POINT('Origin',(0.,-12.9675000200281,-167.906149834141));
#200242=CARTESIAN_POINT('Origin',(0.,-12.9675000200281,-208.192630912063));
#200243=CARTESIAN_POINT('Origin',(0.,-12.9675000200281,-215.85005));
#200244=CARTESIAN_POINT('Origin',(-22.9178089794592,-52.5372975341153,-234.75005));
#200245=CARTESIAN_POINT('',(-27.0625191140422,-59.958306757953,-232.85005));
#200246=CARTESIAN_POINT('',(-23.2057914601203,-61.0324176680998,-232.85005));
#200247=CARTESIAN_POINT('Origin',(-22.9178089794592,-52.5372975341153,-232.85005));
#200248=CARTESIAN_POINT('',(-23.2057914601203,-61.0324176680998,-232.25005));
#200249=CARTESIAN_POINT('',(-23.2057914601203,-61.0324176680998,-234.75005));
#200250=CARTESIAN_POINT('',(-27.0625191140422,-59.958306757953,-232.25005));
#200251=CARTESIAN_POINT('Origin',(-22.9178089794592,-52.5372975341153,-232.25005));
#200252=CARTESIAN_POINT('',(-27.0625191140422,-59.958306757953,-234.75005));
#200253=CARTESIAN_POINT('Origin',(-24.838300653577,28.3971299569735,-234.75005));
#200254=CARTESIAN_POINT('',(-25.8757946403502,36.8335750748777,-232.85005));
#200255=CARTESIAN_POINT('',(-29.3303337505005,35.613198045354,-232.85005));
#200256=CARTESIAN_POINT('Origin',(-24.838300653577,28.3971299569735,-232.85005));
#200257=CARTESIAN_POINT('',(-29.3303337505005,35.613198045354,-232.25005));
#200258=CARTESIAN_POINT('',(-29.3303337505005,35.613198045354,-234.75005));
#200259=CARTESIAN_POINT('',(-25.8757946403502,36.8335750748777,-232.25005));
#200260=CARTESIAN_POINT('Origin',(-24.838300653577,28.3971299569735,-232.25005));
#200261=CARTESIAN_POINT('',(-25.8757946403502,36.8335750748777,-234.75005));
#200262=CARTESIAN_POINT('Origin',(6.29739814579425E-15,-11.5034818258363,
-234.75005));
#200263=CARTESIAN_POINT('',(-46.0422390557602,19.4862297367486,-232.85005));
#200264=CARTESIAN_POINT('Origin',(6.29739814579425E-15,-11.5034818258363,
-232.85005));
#200265=CARTESIAN_POINT('',(-46.0422390557602,19.4862297367486,-232.25005));
#200266=CARTESIAN_POINT('',(-46.0422390557602,19.4862297367486,-234.75005));
#200267=CARTESIAN_POINT('Origin',(6.29739814579425E-15,-11.5034818258363,
-232.25005));
#200268=CARTESIAN_POINT('Origin',(-38.9907249661392,14.740057695632,-234.75005));
#200269=CARTESIAN_POINT('',(-47.4843254762175,15.0698309134599,-232.85005));
#200270=CARTESIAN_POINT('Origin',(-38.9907249661392,14.740057695632,-232.85005));
#200271=CARTESIAN_POINT('',(-47.4843254762175,15.0698309134599,-232.25005));
#200272=CARTESIAN_POINT('',(-47.4843254762175,15.0698309134599,-234.75005));
#200273=CARTESIAN_POINT('Origin',(-38.9907249661392,14.740057695632,-232.25005));
#200274=CARTESIAN_POINT('Origin',(636.934816028482,-11.5034818258361,-234.75005));
#200275=CARTESIAN_POINT('',(-47.764411700877,6.45952891261038,-232.25005));
#200276=CARTESIAN_POINT('',(-47.7015217254648,8.71393888480408,-232.849988379285));
#200277=CARTESIAN_POINT('Ctrl Pts',(-47.764411700877,6.45952891261038,-232.25005));
#200278=CARTESIAN_POINT('Ctrl Pts',(-47.7543096879139,6.84458911076304,
-232.297638206554));
#200279=CARTESIAN_POINT('Ctrl Pts',(-47.743946362003,7.22712198577601,-232.368832317301));
#200280=CARTESIAN_POINT('Ctrl Pts',(-47.7228772190296,7.98214274175961,
-232.566012007014));
#200281=CARTESIAN_POINT('Ctrl Pts',(-47.7121682193403,8.3544760456171,-232.692635516398));
#200282=CARTESIAN_POINT('Ctrl Pts',(-47.7015533799491,8.71393371652249,
-232.849926758569));
#200283=CARTESIAN_POINT('Origin',(636.934816028482,-11.5034818258361,-232.25005));
#200284=CARTESIAN_POINT('Origin',(636.934816028482,-11.5034818258361,-232.85005));
#200285=CARTESIAN_POINT('Origin',(-38.9907249661392,-37.7470213473046,-234.75005));
#200286=CARTESIAN_POINT('',(-47.4843254762176,-38.0767945651323,-232.85005));
#200287=CARTESIAN_POINT('',(-46.0422390557601,-42.4931933884212,-232.85005));
#200288=CARTESIAN_POINT('Origin',(-38.9907249661392,-37.7470213473046,-232.85005));
#200289=CARTESIAN_POINT('',(-46.0422390557601,-42.4931933884212,-232.25005));
#200290=CARTESIAN_POINT('',(-46.0422390557601,-42.4931933884212,-234.75005));
#200291=CARTESIAN_POINT('',(-47.4843254762176,-38.0767945651323,-232.25005));
#200292=CARTESIAN_POINT('Origin',(-38.9907249661392,-37.7470213473046,-232.25005));
#200293=CARTESIAN_POINT('',(-47.4843254762176,-38.0767945651323,-234.75005));
#200294=CARTESIAN_POINT('Origin',(6.29739814579425E-15,-11.5034818258363,
-234.75005));
#200295=CARTESIAN_POINT('Origin',(6.29739814579425E-15,-11.5034818258363,
-232.85005));
#200296=CARTESIAN_POINT('Origin',(6.29739814579425E-15,-11.5034818258363,
-232.25005));
#200297=CARTESIAN_POINT('Ctrl Pts',(-47.269359813636,-39.9199414144257,
-233.323677937652));
#200298=CARTESIAN_POINT('Ctrl Pts',(-47.7852688958474,-40.5328114906027,
-232.537018038148));
#200299=CARTESIAN_POINT('Ctrl Pts',(-48.3011810934468,-41.1456737613432,
-231.750354102807));
#200300=CARTESIAN_POINT('Ctrl Pts',(-48.8170958227918,-41.7585296857986,
-230.963686885275));
#200301=CARTESIAN_POINT('Ctrl Pts',(-49.3330105521369,-42.3713856102541,
-230.177019667743));
#200302=CARTESIAN_POINT('Ctrl Pts',(-49.8489278162636,-42.9842351808713,
-229.390349164127));
#200303=CARTESIAN_POINT('Ctrl Pts',(-50.3648471682373,-43.5970795157942,
-228.603675952145));
#200304=CARTESIAN_POINT('Ctrl Pts',(-51.3966858721847,-44.82276818564,-227.03032952818));
#200305=CARTESIAN_POINT('Ctrl Pts',(-52.4285328613266,-46.0484360781329,
-225.456972356173));
#200306=CARTESIAN_POINT('Ctrl Pts',(-53.4603856521184,-47.2740894119757,
-223.883607650579));
#200307=CARTESIAN_POINT('Ctrl Pts',(-55.5240912337021,-49.7253960796616,
-220.736878239389));
#200308=CARTESIAN_POINT('Ctrl Pts',(-57.5878196113417,-52.1766455410871,
-217.590119225487));
#200309=CARTESIAN_POINT('Ctrl Pts',(-59.6515602724445,-54.6278641542595,
-214.443344242486));
#200310=CARTESIAN_POINT('Ctrl Pts',(-47.2844095710387,-40.0223529985484,
-233.29571384424));
#200311=CARTESIAN_POINT('Ctrl Pts',(-47.799865767177,-40.6397128949599,
-232.509454608122));
#200312=CARTESIAN_POINT('Ctrl Pts',(-48.3153486991529,-41.2570069665437,
-231.72316146998));
#200313=CARTESIAN_POINT('Ctrl Pts',(-48.8308531059458,-41.8742482184852,
-230.936841114977));
#200314=CARTESIAN_POINT('Ctrl Pts',(-49.3463575127387,-42.4914894704268,
-230.150520759975));
#200315=CARTESIAN_POINT('Ctrl Pts',(-49.8618834246415,-43.1086778283034,
-229.364173149988));
#200316=CARTESIAN_POINT('Ctrl Pts',(-50.3774268752988,-43.7258231065776,
-228.577803332719));
#200317=CARTESIAN_POINT('Ctrl Pts',(-51.4085137766134,-44.9601136631259,
-227.005063698182));
#200318=CARTESIAN_POINT('Ctrl Pts',(-52.4396702308542,-46.1942333889078,
-225.432235999036));
#200319=CARTESIAN_POINT('Ctrl Pts',(-53.4708746321289,-47.4282358136099,
-223.859347784982));
#200320=CARTESIAN_POINT('Ctrl Pts',(-55.5332834346784,-49.8962406630142,
-220.713571356874));
#200321=CARTESIAN_POINT('Ctrl Pts',(-57.5958804822797,-52.3637850919073,
-217.567557391373));
#200322=CARTESIAN_POINT('Ctrl Pts',(-59.658577156368,-54.831089092749,-214.42141923076));
#200323=CARTESIAN_POINT('Ctrl Pts',(-47.3011370887008,-40.083704476459,
-233.264807132349));
#200324=CARTESIAN_POINT('Ctrl Pts',(-47.8155006007713,-40.7086470422379,
-232.479276052542));
#200325=CARTESIAN_POINT('Ctrl Pts',(-48.330070971135,-41.3331587221332,
-231.693536730416));
#200326=CARTESIAN_POINT('Ctrl Pts',(-48.8447653455944,-41.957411102505,
-230.907671551986));
#200327=CARTESIAN_POINT('Ctrl Pts',(-49.3594597200538,-42.5816634828768,
-230.121806373556));
#200328=CARTESIAN_POINT('Ctrl Pts',(-49.8742800565343,-43.2056525867135,
-229.335813456774));
#200329=CARTESIAN_POINT('Ctrl Pts',(-50.3891818457356,-43.8294712170294,
-228.549737580672));
#200330=CARTESIAN_POINT('Ctrl Pts',(-51.4189854241382,-45.0771084776612,
-226.977585828468));
#200331=CARTESIAN_POINT('Ctrl Pts',(-52.4491078990803,-46.3240783396034,
-225.405109260953));
#200332=CARTESIAN_POINT('Ctrl Pts',(-53.4793832226061,-47.5707292968664,
-223.832476822232));
#200333=CARTESIAN_POINT('Ctrl Pts',(-55.5399338696578,-50.0640312113922,
-220.68721194479));
#200334=CARTESIAN_POINT('Ctrl Pts',(-57.6010852364915,-52.5560807120374,
-217.541335107067));
#200335=CARTESIAN_POINT('Ctrl Pts',(-59.6624305478473,-55.0477381521116,
-214.39526566237));
#200336=CARTESIAN_POINT('Ctrl Pts',(-47.3051413523369,-40.1629192793609,
-233.246904846954));
#200337=CARTESIAN_POINT('Ctrl Pts',(-47.819327369804,-40.7940757964512,
-232.460673323282));
#200338=CARTESIAN_POINT('Ctrl Pts',(-48.3336083951406,-41.4250391409392,
-231.674348554294));
#200339=CARTESIAN_POINT('Ctrl Pts',(-48.8479443642697,-42.0558912348621,
-230.88796994392));
#200340=CARTESIAN_POINT('Ctrl Pts',(-49.3622803333988,-42.6867433287849,
-230.101591333545));
#200341=CARTESIAN_POINT('Ctrl Pts',(-49.8766723259409,-43.3174819888763,
-229.315157839431));
#200342=CARTESIAN_POINT('Ctrl Pts',(-50.3910998220442,-43.9481493585103,
-228.52868979147));
#200343=CARTESIAN_POINT('Ctrl Pts',(-51.4199548142509,-45.2094840977783,
-226.955753695549));
#200344=CARTESIAN_POINT('Ctrl Pts',(-52.4489487693187,-46.4705399682764,
-225.382682428314));
#200345=CARTESIAN_POINT('Ctrl Pts',(-53.4780084556675,-47.7314680211233,
-223.809549063998));
#200346=CARTESIAN_POINT('Ctrl Pts',(-55.536127828365,-50.253324126817,-220.663282335366));
#200347=CARTESIAN_POINT('Ctrl Pts',(-57.5945065616385,-52.7746765489683,
-217.516770963173));
#200348=CARTESIAN_POINT('Ctrl Pts',(-59.6529740461698,-55.2958790062696,
-214.370186647608));
#200349=CARTESIAN_POINT('Ctrl Pts',(-47.3091454883712,-40.242131557965,
-233.229003132042));
#200350=CARTESIAN_POINT('Ctrl Pts',(-47.8231540168911,-40.8795018283497,
-232.442071186825));
#200351=CARTESIAN_POINT('Ctrl Pts',(-48.337145706421,-41.5169166318385,
-231.655160989632));
#200352=CARTESIAN_POINT('Ctrl Pts',(-48.8511232816408,-42.1543682290027,
-230.868268963674));
#200353=CARTESIAN_POINT('Ctrl Pts',(-49.3651008568606,-42.7918198261669,
-230.081376937717));
#200354=CARTESIAN_POINT('Ctrl Pts',(-49.8790645191143,-43.4293078274282,
-229.294502880311));
#200355=CARTESIAN_POINT('Ctrl Pts',(-50.3930177372337,-44.066823718135,
-228.507642672989));
#200356=CARTESIAN_POINT('Ctrl Pts',(-51.4209241734724,-45.3418554995486,
-226.933922258343));
#200357=CARTESIAN_POINT('Ctrl Pts',(-52.4487896446279,-46.616996929731,
-225.36025631034));
#200358=CARTESIAN_POINT('Ctrl Pts',(-53.4766337325378,-47.8922016232008,
-223.786622036391));
#200359=CARTESIAN_POINT('Ctrl Pts',(-55.5323219083575,-50.4426110101405,
-220.639353488495));
#200360=CARTESIAN_POINT('Ctrl Pts',(-57.5879280964248,-52.9932654200165,
-217.492207602051));
#200361=CARTESIAN_POINT('Ctrl Pts',(-59.6435178458378,-55.5440119530488,
-214.345108432027));
#200362=CARTESIAN_POINT('Ctrl Pts',(-47.3136637970655,-40.310070641192,
-233.20976892517));
#200363=CARTESIAN_POINT('Ctrl Pts',(-47.8271241660854,-40.955047815909,
-232.422048268856));
#200364=CARTESIAN_POINT('Ctrl Pts',(-48.3403579331886,-41.6004954572377,
-231.634553866964));
#200365=CARTESIAN_POINT('Ctrl Pts',(-48.8534714666716,-42.246191520782,
-230.847179503763));
#200366=CARTESIAN_POINT('Ctrl Pts',(-49.3665850001545,-42.8918875843263,
-230.059805140562));
#200367=CARTESIAN_POINT('Ctrl Pts',(-49.8795751912289,-43.537838701044,
-229.272553878112));
#200368=CARTESIAN_POINT('Ctrl Pts',(-50.3924934876008,-44.183938665318,
-228.485374488428));
#200369=CARTESIAN_POINT('Ctrl Pts',(-51.4183300803446,-45.476138593866,
-226.911015709061));
#200370=CARTESIAN_POINT('Ctrl Pts',(-52.4438863060015,-46.7689192505898,
-225.336937281619));
#200371=CARTESIAN_POINT('Ctrl Pts',(-53.4693312838495,-48.0619358471384,
-223.762972649457));
#200372=CARTESIAN_POINT('Ctrl Pts',(-55.5202212395457,-50.6479690402357,
-220.615043385133));
#200373=CARTESIAN_POINT('Ctrl Pts',(-57.5706688803884,-53.2349422023283,
-217.467567478191));
#200374=CARTESIAN_POINT('Ctrl Pts',(-59.6210250673444,-55.8221505796269,
-214.320205136697));
#200375=CARTESIAN_POINT('Ctrl Pts',(-47.3174213500927,-40.3725566206431,
-233.190758458866));
#200376=CARTESIAN_POINT('Ctrl Pts',(-47.8304331865629,-41.0247379875799,
-232.40178755381));
#200377=CARTESIAN_POINT('Ctrl Pts',(-48.3427237376172,-41.6782347797706,
-231.613445913152));
#200378=CARTESIAN_POINT('Ctrl Pts',(-48.8546863035239,-42.3323210585191,
-230.825382497106));
#200379=CARTESIAN_POINT('Ctrl Pts',(-49.3666488694307,-42.9864073372676,
-230.037319081059));
#200380=CARTESIAN_POINT('Ctrl Pts',(-49.8782662454544,-43.6411158354054,
-229.249550061497));
#200381=CARTESIAN_POINT('Ctrl Pts',(-50.3896983451462,-44.2961564367811,
-228.461936921534));
#200382=CARTESIAN_POINT('Ctrl Pts',(-51.4125625445298,-45.6062376395327,
-226.886710641608));
#200383=CARTESIAN_POINT('Ctrl Pts',(-52.4347028263001,-46.9176171020422,
-225.312093851176));
#200384=CARTESIAN_POINT('Ctrl Pts',(-53.4565811414505,-48.229468784563,
-223.737696459652));
#200385=CARTESIAN_POINT('Ctrl Pts',(-55.5003377717513,-50.8531721496045,
-220.588901676603));
#200386=CARTESIAN_POINT('Ctrl Pts',(-57.5430330553295,-53.4787928890259,
-217.440999537853));
#200387=CARTESIAN_POINT('Ctrl Pts',(-59.5855147104668,-56.1048379574655,
-214.293293254791));
#200388=CARTESIAN_POINT('Ctrl Pts',(-47.3211789031199,-40.4350426000942,
-233.171747992562));
#200389=CARTESIAN_POINT('Ctrl Pts',(-47.8337422070404,-41.0944281592508,
-232.381526838764));
#200390=CARTESIAN_POINT('Ctrl Pts',(-48.3450895420457,-41.7559741023036,
-231.59233795934));
#200391=CARTESIAN_POINT('Ctrl Pts',(-48.8559011403763,-42.4184505962563,
-230.803585490448));
#200392=CARTESIAN_POINT('Ctrl Pts',(-49.3667127387069,-43.080927090209,
-230.014833021558));
#200393=CARTESIAN_POINT('Ctrl Pts',(-49.87695729968,-43.7443929697667,-229.226546244883));
#200394=CARTESIAN_POINT('Ctrl Pts',(-50.3869032026916,-44.4083742082442,
-228.43849935464));
#200395=CARTESIAN_POINT('Ctrl Pts',(-51.4067950087149,-45.7363366851993,
-226.862405574156));
#200396=CARTESIAN_POINT('Ctrl Pts',(-52.4255193465988,-47.0663149534946,
-225.287250420734));
#200397=CARTESIAN_POINT('Ctrl Pts',(-53.4438309990515,-48.3970017219875,
-223.712420269846));
#200398=CARTESIAN_POINT('Ctrl Pts',(-55.4804543039569,-51.0583752589733,
-220.562759968072));
#200399=CARTESIAN_POINT('Ctrl Pts',(-57.5153972302706,-53.7226435757235,
-217.414431597513));
#200400=CARTESIAN_POINT('Ctrl Pts',(-59.5500043535892,-56.3875253353041,
-214.266381372884));
#200401=CARTESIAN_POINT('Ctrl Pts',(-47.320727875256,-40.4981900996217,
-233.155799645893));
#200402=CARTESIAN_POINT('Ctrl Pts',(-47.8322495334659,-41.1655802828307,
-232.364426098052));
#200403=CARTESIAN_POINT('Ctrl Pts',(-48.3419545189581,-41.8360548922265,
-231.574520658189));
#200404=CARTESIAN_POINT('Ctrl Pts',(-48.8509002126362,-42.507781144632,
-230.785196140269));
#200405=CARTESIAN_POINT('Ctrl Pts',(-49.3598459063144,-43.1795073970375,
-229.995871622349));
#200406=CARTESIAN_POINT('Ctrl Pts',(-49.8679794722695,-43.8525810620647,
-229.207175913618));
#200407=CARTESIAN_POINT('Ctrl Pts',(-50.3756978342709,-44.5263335458687,
-228.418792446769));
#200408=CARTESIAN_POINT('Ctrl Pts',(-51.3911345582736,-45.8738385134766,
-226.842025513071));
#200409=CARTESIAN_POINT('Ctrl Pts',(-52.4049464549377,-47.224002264507,
-225.266482347449));
#200410=CARTESIAN_POINT('Ctrl Pts',(-53.4182055248116,-48.5750603074809,
-223.691342941789));
#200411=CARTESIAN_POINT('Ctrl Pts',(-55.4447236645594,-51.2771763934287,
-220.541064130469));
#200412=CARTESIAN_POINT('Ctrl Pts',(-57.4689725824102,-53.9829798427017,
-217.392457267063));
#200413=CARTESIAN_POINT('Ctrl Pts',(-59.492784702789,-56.6895247738662,
-214.244180243974));
#200414=CARTESIAN_POINT('Ctrl Pts',(-47.3143897740156,-40.5659557077008,
-233.143618951735));
#200415=CARTESIAN_POINT('Ctrl Pts',(-47.8252832097387,-41.239862847313,
-232.350527479362));
#200416=CARTESIAN_POINT('Ctrl Pts',(-48.3335556171132,-41.9180591247534,
-231.559510554001));
#200417=CARTESIAN_POINT('Ctrl Pts',(-48.84072766068,-42.5979714018469,-230.769289654088));
#200418=CARTESIAN_POINT('Ctrl Pts',(-49.3478997042467,-43.2778836789405,
-229.979068754174));
#200419=CARTESIAN_POINT('Ctrl Pts',(-49.853896141919,-43.9596488205701,
-229.189715484531));
#200420=CARTESIAN_POINT('Ctrl Pts',(-50.3592905012865,-44.6423395873253,
-228.400785431186));
#200421=CARTESIAN_POINT('Ctrl Pts',(-51.3700792200214,-46.0077211208357,
-226.822925324494));
#200422=CARTESIAN_POINT('Ctrl Pts',(-52.3785121216331,-47.3767293468831,
-225.246725326938));
#200423=CARTESIAN_POINT('Ctrl Pts',(-53.3861409718259,-48.7469431347296,
-223.67105962423));
#200424=CARTESIAN_POINT('Ctrl Pts',(-55.4013986722116,-51.4873707104227,
-220.519728218813));
#200425=CARTESIAN_POINT('Ctrl Pts',(-57.4133569116451,-54.2327814391975,
-217.37062149599));
#200426=CARTESIAN_POINT('Ctrl Pts',(-59.4246687676614,-56.9791795051587,
-214.221940194738));
#200427=CARTESIAN_POINT('Ctrl Pts',(-47.3080516727752,-40.6337213157799,
-233.131438257577));
#200428=CARTESIAN_POINT('Ctrl Pts',(-47.8183168860115,-41.3141454117954,
-232.336628860671));
#200429=CARTESIAN_POINT('Ctrl Pts',(-48.3251567152684,-42.0000633572803,
-231.544500449812));
#200430=CARTESIAN_POINT('Ctrl Pts',(-48.8305551087238,-42.688161659062,
-230.753383167905));
#200431=CARTESIAN_POINT('Ctrl Pts',(-49.3359535021791,-43.3762599608436,
-229.962265885999));
#200432=CARTESIAN_POINT('Ctrl Pts',(-49.8398128115685,-44.0667165790755,
-229.172255055445));
#200433=CARTESIAN_POINT('Ctrl Pts',(-50.3428831683021,-44.7583456287819,
-228.382778415603));
#200434=CARTESIAN_POINT('Ctrl Pts',(-51.3490238817693,-46.1416037281948,
-226.803825135918));
#200435=CARTESIAN_POINT('Ctrl Pts',(-52.3520777883286,-47.5294564292592,
-225.226968306426));
#200436=CARTESIAN_POINT('Ctrl Pts',(-53.3540764188403,-48.9188259619783,
-223.65077630667));
#200437=CARTESIAN_POINT('Ctrl Pts',(-55.3580736798637,-51.6975650274167,
-220.498392307158));
#200438=CARTESIAN_POINT('Ctrl Pts',(-57.35774124088,-54.4825830356932,-217.348785724916));
#200439=CARTESIAN_POINT('Ctrl Pts',(-59.3565528325338,-57.2688342364512,
-214.199700145503));
#200440=CARTESIAN_POINT('Ctrl Pts',(-47.3048034248152,-40.692173181322,
-233.11661797197));
#200441=CARTESIAN_POINT('Ctrl Pts',(-47.8136028177951,-41.3798076595766,
-232.320613610482));
#200442=CARTESIAN_POINT('Ctrl Pts',(-48.3182607882955,-42.0738441576018,
-231.527752466761));
#200443=CARTESIAN_POINT('Ctrl Pts',(-48.8211728608215,-42.770397212734,
-230.736051725279));
#200444=CARTESIAN_POINT('Ctrl Pts',(-49.3240849333475,-43.4669502678662,
-229.944350983796));
#200445=CARTESIAN_POINT('Ctrl Pts',(-49.8251339017092,-44.1662308838252,
-229.153926426443));
#200446=CARTESIAN_POINT('Ctrl Pts',(-50.325227721477,-44.8668595754618,
-228.364110202531));
#200447=CARTESIAN_POINT('Ctrl Pts',(-51.3254153610126,-46.2681169587348,
-226.784477754705));
#200448=CARTESIAN_POINT('Ctrl Pts',(-52.3218662832923,-47.674658517871,
-225.207234282834));
#200449=CARTESIAN_POINT('Ctrl Pts',(-53.3170401441828,-49.0829298658951,
-223.630734549434));
#200450=CARTESIAN_POINT('Ctrl Pts',(-55.3073878659637,-51.8994725619434,
-220.477735082634));
#200451=CARTESIAN_POINT('Ctrl Pts',(-57.2924955409022,-54.7231886232885,
-217.327855954057));
#200452=CARTESIAN_POINT('Ctrl Pts',(-59.2765646638181,-57.5482976749593,
-214.178548151011));
#200453=CARTESIAN_POINT('Ctrl Pts',(-47.3009006987844,-40.7491010613005,
-233.101301752625));
#200454=CARTESIAN_POINT('Ctrl Pts',(-47.8070153253589,-41.445066041129,
-232.304686649286));
#200455=CARTESIAN_POINT('Ctrl Pts',(-48.3084583519731,-42.1479407187119,
-231.511460238167));
#200456=CARTESIAN_POINT('Ctrl Pts',(-48.8079303323174,-42.8535202192507,
-230.719470612188));
#200457=CARTESIAN_POINT('Ctrl Pts',(-49.3074023126618,-43.5590997197895,
-229.92748098621));
#200458=CARTESIAN_POINT('Ctrl Pts',(-49.8047715089351,-44.2676134042324,
-229.136855227393));
#200459=CARTESIAN_POINT('Ctrl Pts',(-50.3010627023117,-44.9775733943649,
-228.346875024182));
#200460=CARTESIAN_POINT('Ctrl Pts',(-51.293645089065,-46.3974933746299,
-226.766914617761));
#200461=CARTESIAN_POINT('Ctrl Pts',(-52.2820103247895,-47.8230831255928,
-225.189490258971));
#200462=CARTESIAN_POINT('Ctrl Pts',(-53.2689347752898,-49.2505213363517,
-223.612847133253));
#200463=CARTESIAN_POINT('Ctrl Pts',(-55.2427836762905,-52.1053977578695,
-220.459560881818));
#200464=CARTESIAN_POINT('Ctrl Pts',(-57.2107204090195,-54.9679461288674,
-217.309560330918));
#200465=CARTESIAN_POINT('Ctrl Pts',(-59.1774846171821,-57.8319751776559,
-214.160152831317));
#200466=CARTESIAN_POINT('Ctrl Pts',(-47.2969979727536,-40.8060289412791,
-233.085985533281));
#200467=CARTESIAN_POINT('Ctrl Pts',(-47.8004278329226,-41.5103244226814,
-232.28875968809));
#200468=CARTESIAN_POINT('Ctrl Pts',(-48.2986559156506,-42.2220372798219,
-231.495168009573));
#200469=CARTESIAN_POINT('Ctrl Pts',(-48.7946878038133,-42.9366432257674,
-230.702889499098));
#200470=CARTESIAN_POINT('Ctrl Pts',(-49.2907196919761,-43.6512491717128,
-229.910610988623));
#200471=CARTESIAN_POINT('Ctrl Pts',(-49.7844091161609,-44.3689959246396,
-229.119784028342));
#200472=CARTESIAN_POINT('Ctrl Pts',(-50.2768976831464,-45.088287213268,
-228.329639845834));
#200473=CARTESIAN_POINT('Ctrl Pts',(-51.2618748171174,-46.5268697905249,
-226.749351480816));
#200474=CARTESIAN_POINT('Ctrl Pts',(-52.2421543662867,-47.9715077333147,
-225.171746235109));
#200475=CARTESIAN_POINT('Ctrl Pts',(-53.2208294063969,-49.4181128068083,
-223.594959717073));
#200476=CARTESIAN_POINT('Ctrl Pts',(-55.1781794866173,-52.3113229537955,
-220.441386681001));
#200477=CARTESIAN_POINT('Ctrl Pts',(-57.1289452771368,-55.2127036344464,
-217.291264707778));
#200478=CARTESIAN_POINT('Ctrl Pts',(-59.078404570546,-58.1156526803525,
-214.141757511623));
#200479=CARTESIAN_POINT('Ctrl Pts',(-47.2838098592026,-40.8729843211449,
-233.075391456688));
#200480=CARTESIAN_POINT('Ctrl Pts',(-47.7845860001848,-41.584775131594,
-232.277142649072));
#200481=CARTESIAN_POINT('Ctrl Pts',(-48.2794983189707,-42.3046867305642,
-231.482901088115));
#200482=CARTESIAN_POINT('Ctrl Pts',(-48.7719103193318,-43.02777887034,-230.690101915866));
#200483=CARTESIAN_POINT('Ctrl Pts',(-49.2643223196929,-43.7508710101157,
-229.897302743617));
#200484=CARTESIAN_POINT('Ctrl Pts',(-49.7540733460123,-44.4774123295628,
-229.106099200524));
#200485=CARTESIAN_POINT('Ctrl Pts',(-50.2424538195015,-45.2056526956051,
-228.315643851313));
#200486=CARTESIAN_POINT('Ctrl Pts',(-51.2192147664799,-46.6621334276898,
-226.734733152891));
#200487=CARTESIAN_POINT('Ctrl Pts',(-52.1906157326061,-48.1252743043166,
-225.156762925491));
#200488=CARTESIAN_POINT('Ctrl Pts',(-53.160175528661,-49.5905823504069,
-223.57968507695));
#200489=CARTESIAN_POINT('Ctrl Pts',(-55.0992951207707,-52.5211984425875,
-220.425529379868));
#200490=CARTESIAN_POINT('Ctrl Pts',(-57.0308683476032,-55.4608117845694,
-217.275139764089));
#200491=CARTESIAN_POINT('Ctrl Pts',(-58.960931477471,-58.4021538834631,
-214.125415506933));
#200492=CARTESIAN_POINT('Ctrl Pts',(-47.2640162261029,-40.9447914059068,
-233.067937997558));
#200493=CARTESIAN_POINT('Ctrl Pts',(-47.7628369926546,-41.6622203630557,
-232.268067857029));
#200494=CARTESIAN_POINT('Ctrl Pts',(-48.2549965369399,-42.3887167282325,
-231.472771264582));
#200495=CARTESIAN_POINT('Ctrl Pts',(-48.7442220365055,-43.1188281595447,
-230.679129004258));
#200496=CARTESIAN_POINT('Ctrl Pts',(-49.2334475360712,-43.8489395908569,
-229.885486743933));
#200497=CARTESIAN_POINT('Ctrl Pts',(-49.7195709178301,-44.5829547593942,
-229.093671052645));
#200498=CARTESIAN_POINT('Ctrl Pts',(-50.2040684510243,-45.3189094985237,
-228.302711021656));
#200499=CARTESIAN_POINT('Ctrl Pts',(-51.1730635174128,-46.7908189767828,
-226.720790959677));
#200500=CARTESIAN_POINT('Ctrl Pts',(-52.1357048103052,-48.2703270275798,
-225.142232468079));
#200501=CARTESIAN_POINT('Ctrl Pts',(-53.0961142063379,-49.7523323833611,
-223.564687821978));
#200502=CARTESIAN_POINT('Ctrl Pts',(-55.0169329984032,-52.7163430949238,
-220.409598529776));
#200503=CARTESIAN_POINT('Ctrl Pts',(-56.9286455988057,-55.6906960308185,
-217.258791511269));
#200504=CARTESIAN_POINT('Ctrl Pts',(-58.8384812385968,-58.6670561134909,
-214.108729566325));
#200505=CARTESIAN_POINT('Ctrl Pts',(-47.2442225930031,-41.0165984906687,
-233.060484538427));
#200506=CARTESIAN_POINT('Ctrl Pts',(-47.7410879851243,-41.7396655945174,
-232.258993064984));
#200507=CARTESIAN_POINT('Ctrl Pts',(-48.2304947549091,-42.4727467259007,
-231.46264144105));
#200508=CARTESIAN_POINT('Ctrl Pts',(-48.7165337536793,-43.2098774487494,
-230.66815609265));
#200509=CARTESIAN_POINT('Ctrl Pts',(-49.2025727524494,-43.9470081715982,
-229.873670744249));
#200510=CARTESIAN_POINT('Ctrl Pts',(-49.6850684896479,-44.6884971892255,
-229.081242904766));
#200511=CARTESIAN_POINT('Ctrl Pts',(-50.1656830825472,-45.4321663014423,
-228.289778191998));
#200512=CARTESIAN_POINT('Ctrl Pts',(-51.1269122683457,-46.9195045258758,
-226.706848766463));
#200513=CARTESIAN_POINT('Ctrl Pts',(-52.0807938880043,-48.415379750843,
-225.127702010668));
#200514=CARTESIAN_POINT('Ctrl Pts',(-53.0320528840148,-49.9140824163154,
-223.549690567007));
#200515=CARTESIAN_POINT('Ctrl Pts',(-54.9345708760356,-52.9114877472602,
-220.393667679684));
#200516=CARTESIAN_POINT('Ctrl Pts',(-56.8264228500083,-55.9205802770675,
-217.24244325845));
#200517=CARTESIAN_POINT('Ctrl Pts',(-58.7160309997225,-58.9319583435186,
-214.092043625716));
#200518=CARTESIAN_POINT('Ctrl Pts',(-47.2331633716395,-41.074937962774,
-233.047719588827));
#200519=CARTESIAN_POINT('Ctrl Pts',(-47.7223958772293,-41.8099539540185,
-232.248012089236));
#200520=CARTESIAN_POINT('Ctrl Pts',(-48.2057678315329,-42.5524924864862,
-231.452175543568));
#200521=CARTESIAN_POINT('Ctrl Pts',(-48.6860560436761,-43.2986376795464,
-230.658029260724));
#200522=CARTESIAN_POINT('Ctrl Pts',(-49.1663442558194,-44.0447828726065,
-229.86388297788));
#200523=CARTESIAN_POINT('Ctrl Pts',(-49.6434655783611,-44.7946821653274,
-229.071521833792));
#200524=CARTESIAN_POINT('Ctrl Pts',(-50.1187524818162,-45.5466353134476,
-228.280074917719));
#200525=CARTESIAN_POINT('Ctrl Pts',(-51.0693262887264,-47.0505416096881,
-226.697181085572));
#200526=CARTESIAN_POINT('Ctrl Pts',(-52.0127499442126,-48.5624569502057,
-225.117853862002));
#200527=CARTESIAN_POINT('Ctrl Pts',(-52.9533507298994,-50.0773066236126,
-223.539705153474));
#200528=CARTESIAN_POINT('Ctrl Pts',(-54.8345523012729,-53.1070059704263,
-220.383407736418));
#200529=CARTESIAN_POINT('Ctrl Pts',(-56.7045075297636,-56.1485479679101,
-217.231955569755));
#200530=CARTESIAN_POINT('Ctrl Pts',(-58.5718893946176,-59.1926043098068,
-214.081397630038));
#200531=CARTESIAN_POINT('Ctrl Pts',(-47.2184619313714,-41.1386068777002,
-233.034226791445));
#200532=CARTESIAN_POINT('Ctrl Pts',(-47.6994633038231,-41.8843414973674,
-232.236899734718));
#200533=CARTESIAN_POINT('Ctrl Pts',(-48.1764662990288,-42.6351364657344,
-231.442184400327));
#200534=CARTESIAN_POINT('Ctrl Pts',(-48.6511105129755,-43.3886793381388,
-230.648777192266));
#200535=CARTESIAN_POINT('Ctrl Pts',(-49.1257547269221,-44.1422222105431,
-229.855369984204));
#200536=CARTESIAN_POINT('Ctrl Pts',(-49.5980020098404,-44.8985826028918,
-229.063316695606));
#200537=CARTESIAN_POINT('Ctrl Pts',(-50.0687290729088,-45.6566352866088,
-228.272029084797));
#200538=CARTESIAN_POINT('Ctrl Pts',(-51.0101831990457,-47.1727406540429,
-226.689453863181));
#200539=CARTESIAN_POINT('Ctrl Pts',(-51.9456932760972,-48.695455984225,
-225.109865596097));
#200540=CARTESIAN_POINT('Ctrl Pts',(-52.8784745199465,-50.2209883221406,
-223.531433290935));
#200541=CARTESIAN_POINT('Ctrl Pts',(-54.7440370076451,-53.2720529979718,
-220.374568680612));
#200542=CARTESIAN_POINT('Ctrl Pts',(-56.5988680832651,-56.3342829748578,
-217.222334895439));
#200543=CARTESIAN_POINT('Ctrl Pts',(-58.4505854057776,-59.3994904876393,
-214.071174978969));
#200544=CARTESIAN_POINT('Ctrl Pts',(-47.2037604911033,-41.2022757926265,
-233.020733994064));
#200545=CARTESIAN_POINT('Ctrl Pts',(-47.6765307304169,-41.9587290407164,
-232.2257873802));
#200546=CARTESIAN_POINT('Ctrl Pts',(-48.1471647665248,-42.7177804449826,
-231.432193257086));
#200547=CARTESIAN_POINT('Ctrl Pts',(-48.6161649822748,-43.4787209967311,
-230.639525123807));
#200548=CARTESIAN_POINT('Ctrl Pts',(-49.0851651980248,-44.2396615484797,
-229.846856990528));
#200549=CARTESIAN_POINT('Ctrl Pts',(-49.5525384413198,-45.0024830404561,
-229.055111557421));
#200550=CARTESIAN_POINT('Ctrl Pts',(-50.0187056640015,-45.76663525977,-228.263983251877));
#200551=CARTESIAN_POINT('Ctrl Pts',(-50.9510401093651,-47.2949396983977,
-226.68172664079));
#200552=CARTESIAN_POINT('Ctrl Pts',(-51.8786366079818,-48.8284550182444,
-225.101877330191));
#200553=CARTESIAN_POINT('Ctrl Pts',(-52.8035983099936,-50.3646700206687,
-223.523161428396));
#200554=CARTESIAN_POINT('Ctrl Pts',(-54.6535217140174,-53.4371000255173,
-220.365729624806));
#200555=CARTESIAN_POINT('Ctrl Pts',(-56.4932286367666,-56.5200179818056,
-217.212714221123));
#200556=CARTESIAN_POINT('Ctrl Pts',(-58.3292814169375,-59.6063766654718,
-214.060952327901));
#200557=CARTESIAN_POINT('Ctrl Pts',(-47.171541404707,-41.2857265086834,
-233.01310592162));
#200558=CARTESIAN_POINT('Ctrl Pts',(-47.639685387572,-42.0470753131842,
-232.218927162867));
#200559=CARTESIAN_POINT('Ctrl Pts',(-48.1062722861412,-42.8103918979816,
-231.425803682192));
#200560=CARTESIAN_POINT('Ctrl Pts',(-48.5716487660823,-43.5751432799917,
-230.633406080342));
#200561=CARTESIAN_POINT('Ctrl Pts',(-49.0370252460235,-44.3398946620018,
-229.841008478492));
#200562=CARTESIAN_POINT('Ctrl Pts',(-49.5011895680945,-45.1060858790577,
-229.049340752905));
#200563=CARTESIAN_POINT('Ctrl Pts',(-49.9644012667793,-45.8733524421474,
-228.25819056826));
#200564=CARTESIAN_POINT('Ctrl Pts',(-50.8908246641489,-47.4078855683268,
-226.675890198969));
#200565=CARTESIAN_POINT('Ctrl Pts',(-51.8134800494771,-48.9466583058251,
-225.095623133202));
#200566=CARTESIAN_POINT('Ctrl Pts',(-52.7337378890505,-50.4879249875678,
-223.516445892042));
#200567=CARTESIAN_POINT('Ctrl Pts',(-54.5742535681973,-53.5704583510531,
-220.358091409721));
#200568=CARTESIAN_POINT('Ctrl Pts',(-56.4054092509004,-56.6627147295212,
-217.203977876217));
#200569=CARTESIAN_POINT('Ctrl Pts',(-58.2323713080084,-59.7588964549113,
-214.051326981263));
#200570=CARTESIAN_POINT('Ctrl Pts',(-47.1301259245572,-41.3776365805516,
-233.007883276788));
#200571=CARTESIAN_POINT('Ctrl Pts',(-47.5942000936469,-42.1428559602882,
-232.214484939109));
#200572=CARTESIAN_POINT('Ctrl Pts',(-48.0571442886842,-42.9095264965149,
-231.42188110874));
#200573=CARTESIAN_POINT('Ctrl Pts',(-48.5191679953314,-43.677310151957,
-230.629855880101));
#200574=CARTESIAN_POINT('Ctrl Pts',(-48.9811917019786,-44.445093807399,
-229.837830651463));
#200575=CARTESIAN_POINT('Ctrl Pts',(-49.4422942329435,-45.2139930242057,
-229.046386055781));
#200576=CARTESIAN_POINT('Ctrl Pts',(-49.9026408989544,-45.9837637819335,
-228.255374275861));
#200577=CARTESIAN_POINT('Ctrl Pts',(-50.8233342309762,-47.5233052973892,
-226.673350716021));
#200578=CARTESIAN_POINT('Ctrl Pts',(-51.7410289944696,-49.0662933806299,
-225.093033330561));
#200579=CARTESIAN_POINT('Ctrl Pts',(-52.6566611088264,-50.611475717687,
-223.51371347964));
#200580=CARTESIAN_POINT('Ctrl Pts',(-54.4879253375398,-53.7018403918012,
-220.355073777797));
#200581=CARTESIAN_POINT('Ctrl Pts',(-56.3111024468989,-56.8007837303405,
-217.200320668143));
#200582=CARTESIAN_POINT('Ctrl Pts',(-58.1301468566089,-59.9036654708269,
-214.047106057761));
#200583=CARTESIAN_POINT('Ctrl Pts',(-47.1094181844823,-41.4235916164857,
-233.005271954373));
#200584=CARTESIAN_POINT('Ctrl Pts',(-47.5714574466843,-42.1907462838401,
-232.21226382723));
#200585=CARTESIAN_POINT('Ctrl Pts',(-48.0325802899557,-42.9590937957815,
-231.419919822014));
#200586=CARTESIAN_POINT('Ctrl Pts',(-48.4929276099559,-43.7283935879396,
-230.628080779981));
#200587=CARTESIAN_POINT('Ctrl Pts',(-48.9532749299561,-44.4976933800977,
-229.836241737948));
#200588=CARTESIAN_POINT('Ctrl Pts',(-49.4128465653679,-45.2679465967797,
-229.044908707219));
#200589=CARTESIAN_POINT('Ctrl Pts',(-49.8717607150419,-46.0389694518266,
-228.253966129662));
#200590=CARTESIAN_POINT('Ctrl Pts',(-50.7895890143898,-47.5810151619205,
-226.672080974546));
#200591=CARTESIAN_POINT('Ctrl Pts',(-51.7048034669659,-49.1261109180323,
-225.091738429241));
#200592=CARTESIAN_POINT('Ctrl Pts',(-52.6181227187143,-50.6732510827466,
-223.512347273439));
#200593=CARTESIAN_POINT('Ctrl Pts',(-54.4447612222111,-53.7675314121752,
-220.353564961834));
#200594=CARTESIAN_POINT('Ctrl Pts',(-56.2639490448981,-56.8698182307502,
-217.198492064106));
#200595=CARTESIAN_POINT('Ctrl Pts',(-58.0790346309092,-59.9760499787848,
-214.044995596012));
#200596=CARTESIAN_POINT('Ctrl Pts',(-47.1035243171495,-41.4544068124509,
-232.995787114217));
#200597=CARTESIAN_POINT('Ctrl Pts',(-47.5618182365402,-42.2252850495327,
-232.204165849507));
#200598=CARTESIAN_POINT('Ctrl Pts',(-48.0196603955539,-42.9967734838342,
-231.412895157786));
#200599=CARTESIAN_POINT('Ctrl Pts',(-48.4770833116826,-43.7688007487221,
-230.621922441887));
#200600=CARTESIAN_POINT('Ctrl Pts',(-48.9345062278113,-44.54082801361,-229.830949725988));
#200601=CARTESIAN_POINT('Ctrl Pts',(-49.391509938849,-45.313394184642,-229.040275082537));
#200602=CARTESIAN_POINT('Ctrl Pts',(-49.8481260220802,-46.0864367596275,
-228.249854204732));
#200603=CARTESIAN_POINT('Ctrl Pts',(-50.7613581885425,-47.6325219095984,
-226.669012449123));
#200604=CARTESIAN_POINT('Ctrl Pts',(-51.6730415942752,-49.1805060788742,
-225.089180182384));
#200605=CARTESIAN_POINT('Ctrl Pts',(-52.5834110903597,-50.7299791212212,
-223.510082333838));
#200606=CARTESIAN_POINT('Ctrl Pts',(-54.4041500825286,-53.8289252059152,
-220.351886636744));
#200607=CARTESIAN_POINT('Ctrl Pts',(-56.2196637687479,-56.9337600260798,
-217.196579358919));
#200608=CARTESIAN_POINT('Ctrl Pts',(-58.0314831441787,-60.0422631998226,
-214.04281865403));
#200609=CARTESIAN_POINT('Ctrl Pts',(-47.0912031843055,-41.4946844018168,
-232.986503298756));
#200610=CARTESIAN_POINT('Ctrl Pts',(-47.5465884139282,-42.2680813083878,
-232.195931935019));
#200611=CARTESIAN_POINT('Ctrl Pts',(-48.0017768129395,-43.0417829154583,
-231.40555195953));
#200612=CARTESIAN_POINT('Ctrl Pts',(-48.4567760318361,-43.8157641577748,
-230.615342754576));
#200613=CARTESIAN_POINT('Ctrl Pts',(-48.9117752507326,-44.5897454000911,
-229.825133549621));
#200614=CARTESIAN_POINT('Ctrl Pts',(-49.366585304478,-45.364006290321,-229.035095136287));
#200615=CARTESIAN_POINT('Ctrl Pts',(-49.8212141883276,-46.1385240104118,
-228.245209329223));
#200616=CARTESIAN_POINT('Ctrl Pts',(-50.7304719560267,-47.6875594505935,
-226.665437715093));
#200617=CARTESIAN_POINT('Ctrl Pts',(-51.6390050797513,-49.2376203690394,
-225.086274713309));
#200618=CARTESIAN_POINT('Ctrl Pts',(-52.5468787652607,-50.7885482821615,
-223.507599498114));
#200619=CARTESIAN_POINT('Ctrl Pts',(-54.3626261362793,-53.8904041084056,
-220.350249067725));
#200620=CARTESIAN_POINT('Ctrl Pts',(-56.1757402684043,-56.9957065400334,
-217.194831063113));
#200621=CARTESIAN_POINT('Ctrl Pts',(-57.9867151256432,-60.1034983677464,
-214.040672462087));
#200622=CARTESIAN_POINT('Ctrl Pts',(-47.0788820514615,-41.5349619911827,
-232.977219483294));
#200623=CARTESIAN_POINT('Ctrl Pts',(-47.5313585913162,-42.310877567243,
-232.187698020531));
#200624=CARTESIAN_POINT('Ctrl Pts',(-47.9838932303251,-43.0867923470826,
-231.398208761274));
#200625=CARTESIAN_POINT('Ctrl Pts',(-48.4364687519895,-43.8627275668274,
-230.608763067264));
#200626=CARTESIAN_POINT('Ctrl Pts',(-48.889044273654,-44.6386627865722,
-229.819317373254));
#200627=CARTESIAN_POINT('Ctrl Pts',(-49.3416606701069,-45.4146183959999,
-229.029915190037));
#200628=CARTESIAN_POINT('Ctrl Pts',(-49.7943023545749,-46.1906112611962,
-228.240564453713));
#200629=CARTESIAN_POINT('Ctrl Pts',(-50.6995857235109,-47.7425969915886,
-226.661862981063));
#200630=CARTESIAN_POINT('Ctrl Pts',(-51.6049685652275,-49.2947346592046,
-225.083369244233));
#200631=CARTESIAN_POINT('Ctrl Pts',(-52.5103464401617,-50.8471174431018,
-223.505116662391));
#200632=CARTESIAN_POINT('Ctrl Pts',(-54.3211021900301,-53.951883010896,
-220.348611498707));
#200633=CARTESIAN_POINT('Ctrl Pts',(-56.1318167680608,-57.0576530539869,
-217.193082767306));
#200634=CARTESIAN_POINT('Ctrl Pts',(-57.9419471071077,-60.1647335356702,
-214.038526270145));
#200635=CARTESIAN_POINT('Ctrl Pts',(-47.0588574073719,-41.5858000428048,
-232.968566523408));
#200636=CARTESIAN_POINT('Ctrl Pts',(-47.5093207248854,-42.363022265842,
-232.17977481419));
#200637=CARTESIAN_POINT('Ctrl Pts',(-47.9599297574655,-43.1401459593037,
-231.39096724535));
#200638=CARTESIAN_POINT('Ctrl Pts',(-48.4106907142535,-43.9171701566874,
-230.602146349555));
#200639=CARTESIAN_POINT('Ctrl Pts',(-48.8614516710415,-44.6941943540713,
-229.813325453759));
#200640=CARTESIAN_POINT('Ctrl Pts',(-49.3123645814213,-45.4711190318301,
-229.024491224305));
#200641=CARTESIAN_POINT('Ctrl Pts',(-49.7634348829592,-46.2479443404272,
-228.235646862402));
#200642=CARTESIAN_POINT('Ctrl Pts',(-50.6655754860351,-47.8015949576215,
-226.657958138597));
#200643=CARTESIAN_POINT('Ctrl Pts',(-51.5683478186111,-49.3548459662596,
-225.080227999184));
#200644=CARTESIAN_POINT('Ctrl Pts',(-52.4717770943224,-50.9077187028313,
-223.502491635481));
#200645=CARTESIAN_POINT('Ctrl Pts',(-54.2786356457449,-54.0134641759745,
-220.347018908076));
#200646=CARTESIAN_POINT('Ctrl Pts',(-56.0882389522679,-57.1176157229696,
-217.191507400736));
#200647=CARTESIAN_POINT('Ctrl Pts',(-57.8999640673718,-60.2209901065118,
-214.036411889894));
#200648=CARTESIAN_POINT('Ctrl Pts',(-47.0185565395742,-41.6609971057424,
-232.962224970815));
#200649=CARTESIAN_POINT('Ctrl Pts',(-47.4683098495203,-42.4379579278734,
-232.173885913265));
#200650=CARTESIAN_POINT('Ctrl Pts',(-47.9182404464189,-43.214781541947,
-231.385510833981));
#200651=CARTESIAN_POINT('Ctrl Pts',(-48.3683681238743,-43.9914549619569,
-230.597098052473));
#200652=CARTESIAN_POINT('Ctrl Pts',(-48.8184958013296,-44.7681283819668,
-229.808685270963));
#200653=CARTESIAN_POINT('Ctrl Pts',(-49.2688205234849,-45.5446516231764,
-229.020234782073));
#200654=CARTESIAN_POINT('Ctrl Pts',(-49.7193651569502,-46.321010055599,
-228.231745013587));
#200655=CARTESIAN_POINT('Ctrl Pts',(-50.6204544238808,-47.8737269204442,
-226.654765476616));
#200656=CARTESIAN_POINT('Ctrl Pts',(-51.5224188067103,-49.4257867780962,
-225.077628467932));
#200657=CARTESIAN_POINT('Ctrl Pts',(-52.4254879069396,-50.9770488729761,
-223.500324296104));
#200658=CARTESIAN_POINT('Ctrl Pts',(-54.2316261073984,-54.079573062736,
-220.345715952448));
#200659=CARTESIAN_POINT('Ctrl Pts',(-56.0420505223762,-57.178961519516,
-217.190418744692));
#200660=CARTESIAN_POINT('Ctrl Pts',(-57.8597736100785,-60.2735586547801,
-214.03449525351));
#200661=CARTESIAN_POINT('',(-47.5799752941295,-40.2889415902933,-232.85005));
#200662=CARTESIAN_POINT('',(-47.0825542278859,-41.7715518798765,-232.850050000968));
#200663=CARTESIAN_POINT('Ctrl Pts',(-47.5799752940314,-40.288941592692,
-232.85005));
#200664=CARTESIAN_POINT('Ctrl Pts',(-47.5775945735834,-40.3473480102004,
-232.85005));
#200665=CARTESIAN_POINT('Ctrl Pts',(-47.5746791399089,-40.3934055205313,
-232.85005));
#200666=CARTESIAN_POINT('Ctrl Pts',(-47.5660677925892,-40.4699741882521,
-232.85005));
#200667=CARTESIAN_POINT('Ctrl Pts',(-47.5635310902827,-40.4915421253747,
-232.850049999998));
#200668=CARTESIAN_POINT('Ctrl Pts',(-47.553195697107,-40.5727355795072,
-232.850049999998));
#200669=CARTESIAN_POINT('Ctrl Pts',(-47.5435314536243,-40.6342224880465,
-232.85005));
#200670=CARTESIAN_POINT('Ctrl Pts',(-47.4988634642814,-40.8512217221034,
-232.85005));
#200671=CARTESIAN_POINT('Ctrl Pts',(-47.4667238043787,-40.9561283632504,
-232.850050000041));
#200672=CARTESIAN_POINT('Ctrl Pts',(-47.4103530291719,-41.1136517563645,
-232.850050000041));
#200673=CARTESIAN_POINT('Ctrl Pts',(-47.388468896712,-41.1712462227268,
-232.850050000436));
#200674=CARTESIAN_POINT('Ctrl Pts',(-47.3415687150509,-41.2863061139755,
-232.850050000436));
#200675=CARTESIAN_POINT('Ctrl Pts',(-47.3098061173323,-41.3563636665165,
-232.850049999917));
#200676=CARTESIAN_POINT('Ctrl Pts',(-47.2385354932108,-41.4987551854794,
-232.850049999917));
#200677=CARTESIAN_POINT('Ctrl Pts',(-47.2078203686635,-41.5594829943073,
-232.850050000009));
#200678=CARTESIAN_POINT('Ctrl Pts',(-47.1722887236253,-41.6240970450122,
-232.850050000009));
#200679=CARTESIAN_POINT('Ctrl Pts',(-47.1600291819146,-41.6454764697112,
-232.85005));
#200680=CARTESIAN_POINT('Ctrl Pts',(-47.126386710567,-41.7020987848978,
-232.85005));
#200681=CARTESIAN_POINT('Ctrl Pts',(-47.1037445725666,-41.7383217641524,
-232.85005));
#200682=CARTESIAN_POINT('Ctrl Pts',(-47.0825542565969,-41.7715518684048,
-232.85005));
#200683=CARTESIAN_POINT('',(-59.5781472511572,-54.5406860123134,-214.555282751782));
#200684=CARTESIAN_POINT('Ctrl Pts',(-47.5799752942349,-40.2889415880665,
-232.85005));
#200685=CARTESIAN_POINT('Ctrl Pts',(-51.5792492625364,-45.0398156733569,
-226.7519456074));
#200686=CARTESIAN_POINT('Ctrl Pts',(-55.5786810873963,-49.7902940354523,
-220.653636556059));
#200687=CARTESIAN_POINT('Ctrl Pts',(-59.5781472511525,-54.540686011977,
-214.555282751822));
#200688=CARTESIAN_POINT('',(-59.5601545409129,-55.0066093843695,-214.536876504828));
#200689=CARTESIAN_POINT('Ctrl Pts',(-59.5601545409116,-55.0066093843695,
-214.53687650483));
#200690=CARTESIAN_POINT('Ctrl Pts',(-59.5631449158913,-54.928270959567,
-214.542949699432));
#200691=CARTESIAN_POINT('Ctrl Pts',(-59.566138639304,-54.8502579208168,
-214.547602707532));
#200692=CARTESIAN_POINT('Ctrl Pts',(-59.5721600832965,-54.6943310158058,
-214.553747671111));
#200693=CARTESIAN_POINT('Ctrl Pts',(-59.5751172054583,-54.6182288248312,
-214.555228314137));
#200694=CARTESIAN_POINT('Ctrl Pts',(-59.5781472511111,-54.540686012984,
-214.55528275182));
#200695=CARTESIAN_POINT('',(-57.733985310444,-60.0593815363208,-214.252907888001));
#200696=CARTESIAN_POINT('Ctrl Pts',(-59.5601545409136,-55.0066093843694,
-214.536876504827));
#200697=CARTESIAN_POINT('Ctrl Pts',(-59.5534103770657,-55.1832852782111,
-214.523179687618));
#200698=CARTESIAN_POINT('Ctrl Pts',(-59.5413857028285,-55.3595266936186,
-214.509940774979));
#200699=CARTESIAN_POINT('Ctrl Pts',(-59.5048392798775,-55.7306111572691,
-214.48359225017));
#200700=CARTESIAN_POINT('Ctrl Pts',(-59.4790426204911,-55.9255750604899,
-214.470456745239));
#200701=CARTESIAN_POINT('Ctrl Pts',(-59.4374186280887,-56.1761840160495,
-214.453298736124));
#200702=CARTESIAN_POINT('Ctrl Pts',(-59.4271923870096,-56.2341662571188,
-214.449364106516));
#200703=CARTESIAN_POINT('Ctrl Pts',(-59.3290041059246,-56.7600810924064,
-214.414327664565));
#200704=CARTESIAN_POINT('Ctrl Pts',(-59.2036000760255,-57.2212958977573,
-214.387817887296));
#200705=CARTESIAN_POINT('Ctrl Pts',(-58.9920439420377,-57.808059046763,
-214.354899874041));
#200706=CARTESIAN_POINT('Ctrl Pts',(-58.9383051097066,-57.9461281140529,
-214.347431324615));
#200707=CARTESIAN_POINT('Ctrl Pts',(-58.7834285639265,-58.3162123489879,
-214.328364513275));
#200708=CARTESIAN_POINT('Ctrl Pts',(-58.6754718372394,-58.5458967426817,
-214.316667298022));
#200709=CARTESIAN_POINT('Ctrl Pts',(-58.4793456692825,-58.9208033297017,
-214.298260215069));
#200710=CARTESIAN_POINT('Ctrl Pts',(-58.3955443144838,-59.0701807393182,
-214.291807992095));
#200711=CARTESIAN_POINT('Ctrl Pts',(-58.255439819926,-59.303876779064,-214.282137443959));
#200712=CARTESIAN_POINT('Ctrl Pts',(-58.2014468386663,-59.3905132232237,
-214.278624601648));
#200713=CARTESIAN_POINT('Ctrl Pts',(-58.0758641218483,-59.5844450019079,
-214.270199768697));
#200714=CARTESIAN_POINT('Ctrl Pts',(-58.0026577731471,-59.6923453371087,
-214.265296898901));
#200715=CARTESIAN_POINT('Ctrl Pts',(-57.8636814802857,-59.8874642716884,
-214.258285826271));
#200716=CARTESIAN_POINT('Ctrl Pts',(-57.7995878632373,-59.9740538268328,
-214.255565510063));
#200717=CARTESIAN_POINT('Ctrl Pts',(-57.7339853360531,-60.0593815526408,
-214.252907779837));
#200718=CARTESIAN_POINT('Ctrl Pts',(-47.0825542580294,-41.771551867666,
-232.85005));
#200719=CARTESIAN_POINT('Ctrl Pts',(-48.8467027002287,-44.8190048301195,
-229.757904206756));
#200720=CARTESIAN_POINT('Ctrl Pts',(-50.613532047441,-47.8643691189139,
-226.665199941971));
#200721=CARTESIAN_POINT('Ctrl Pts',(-54.1625939290642,-53.9611509924102,
-220.466183691575));
#200722=CARTESIAN_POINT('Ctrl Pts',(-55.944791066377,-57.0125677071401,
-217.359850769034));
#200723=CARTESIAN_POINT('Ctrl Pts',(-57.7339853814967,-60.059381488225,
-214.252907967141));
#200724=CARTESIAN_POINT('Ctrl Pts',(-26.4599578544128,-60.6835996873818,
-232.962469394759));
#200725=CARTESIAN_POINT('Ctrl Pts',(-27.3226882880111,-61.1109358874724,
-232.172413742166));
#200726=CARTESIAN_POINT('Ctrl Pts',(-28.1852243300615,-61.5385403473352,
-231.38229745923));
#200727=CARTESIAN_POINT('Ctrl Pts',(-29.0475520792886,-61.9664437404056,
-230.59212149004));
#200728=CARTESIAN_POINT('Ctrl Pts',(-29.9098798285159,-62.3943471334761,
-229.801945520851));
#200729=CARTESIAN_POINT('Ctrl Pts',(-30.7719992834121,-62.8225494254431,
-229.011709845514));
#200730=CARTESIAN_POINT('Ctrl Pts',(-31.6338956495273,-63.2510852212965,
-228.221416509758));
#200731=CARTESIAN_POINT('Ctrl Pts',(-33.3576883817577,-64.1081568130033,
-226.640829838246));
#200732=CARTESIAN_POINT('Ctrl Pts',(-35.0805895076854,-64.966557214572,
-225.060010587067));
#200733=CARTESIAN_POINT('Ctrl Pts',(-36.8024707859496,-65.826619215018,
-223.47899392047));
#200734=CARTESIAN_POINT('Ctrl Pts',(-40.2462333424779,-67.54674321591,-220.316960587274));
#200735=CARTESIAN_POINT('Ctrl Pts',(-43.6859139831841,-69.2733920499482,
-217.154070226751));
#200736=CARTESIAN_POINT('Ctrl Pts',(-47.1204141132129,-71.0104275193633,
-213.991161055977));
#200737=CARTESIAN_POINT('Ctrl Pts',(-26.3821787340349,-60.7171127522114,
-232.969564324364));
#200738=CARTESIAN_POINT('Ctrl Pts',(-27.2445605117317,-61.1462290233331,
-232.178536730278));
#200739=CARTESIAN_POINT('Ctrl Pts',(-28.1068458309989,-61.5755390840377,
-231.387516472179));
#200740=CARTESIAN_POINT('Ctrl Pts',(-28.9690444318655,-62.0050437616364,
-230.596514709636));
#200741=CARTESIAN_POINT('Ctrl Pts',(-29.8312430327322,-62.4345484392352,
-229.805512947091));
#200742=CARTESIAN_POINT('Ctrl Pts',(-30.6933548791156,-62.8642478097168,
-229.014529680654));
#200743=CARTESIAN_POINT('Ctrl Pts',(-31.5553928365677,-63.294139004949,
-228.223577554036));
#200744=CARTESIAN_POINT('Ctrl Pts',(-33.279468751472,-64.1539213954133,
-226.641673300801));
#200745=CARTESIAN_POINT('Ctrl Pts',(-35.0032446885496,-65.0144779934189,
-225.059892398919));
#200746=CARTESIAN_POINT('Ctrl Pts',(-36.7268700953622,-65.8757200976626,
-223.47835238333));
#200747=CARTESIAN_POINT('Ctrl Pts',(-40.1741209089872,-67.59820430615,-220.315272352152));
#200748=CARTESIAN_POINT('Ctrl Pts',(-43.6206707171006,-69.3236781200416,
-217.153178316448));
#200749=CARTESIAN_POINT('Ctrl Pts',(-47.0687185474759,-71.0494058698413,
-213.993041121244));
#200750=CARTESIAN_POINT('Ctrl Pts',(-26.3336571985367,-60.7298615784681,
-232.97989189577));
#200751=CARTESIAN_POINT('Ctrl Pts',(-27.1935442176352,-61.1624605165825,
-232.187307357553));
#200752=CARTESIAN_POINT('Ctrl Pts',(-28.0535703090899,-61.5950514826745,
-231.3948845311));
#200753=CARTESIAN_POINT('Ctrl Pts',(-28.9137915870808,-62.0275803216354,
-230.60265649712));
#200754=CARTESIAN_POINT('Ctrl Pts',(-29.7740128650717,-62.4601091605963,
-229.810428463141));
#200755=CARTESIAN_POINT('Ctrl Pts',(-30.6344288831099,-62.8925758112263,
-229.018394694299));
#200756=CARTESIAN_POINT('Ctrl Pts',(-31.4950740297321,-63.3249356024725,
-228.226569298064));
#200757=CARTESIAN_POINT('Ctrl Pts',(-33.2163643229766,-64.189655184965,
-226.642918505594));
#200758=CARTESIAN_POINT('Ctrl Pts',(-34.9385811609418,-65.0539386080163,
-225.060107632614));
#200759=CARTESIAN_POINT('Ctrl Pts',(-36.6618273110172,-65.9175410966594,
-223.478119078272));
#200760=CARTESIAN_POINT('Ctrl Pts',(-40.108319611168,-67.6447460739454,
-220.314141969587));
#200761=CARTESIAN_POINT('Ctrl Pts',(-43.5589622053215,-69.3691553263065,
-217.153452097777));
#200762=CARTESIAN_POINT('Ctrl Pts',(-47.01332562737,-71.0901106229208,-213.995220045295));
#200763=CARTESIAN_POINT('Ctrl Pts',(-26.2982843226441,-60.7344827742712,
-232.991392546795));
#200764=CARTESIAN_POINT('Ctrl Pts',(-27.1539710903761,-61.1717772412952,
-232.196575481186));
#200765=CARTESIAN_POINT('Ctrl Pts',(-28.0105205110111,-61.6084763232924,
-231.402405653547));
#200766=CARTESIAN_POINT('Ctrl Pts',(-28.8678178196021,-62.0446142255719,
-230.608774353877));
#200767=CARTESIAN_POINT('Ctrl Pts',(-29.725115128193,-62.4807521278514,
-229.815143054206));
#200768=CARTESIAN_POINT('Ctrl Pts',(-30.5831604852668,-62.9163290490967,
-229.022050566726));
#200769=CARTESIAN_POINT('Ctrl Pts',(-31.441855894783,-63.3513820288522,
-228.22940826535));
#200770=CARTESIAN_POINT('Ctrl Pts',(-33.1592467138153,-64.2214879883631,
-226.644123662598));
#200771=CARTESIAN_POINT('Ctrl Pts',(-34.879225924468,-65.0894996057218,
-225.060627483752));
#200772=CARTESIAN_POINT('Ctrl Pts',(-36.6011749254936,-65.955713208232,
-223.478393801851));
#200773=CARTESIAN_POINT('Ctrl Pts',(-40.045072927545,-67.6881404132524,
-220.313926438049));
#200774=CARTESIAN_POINT('Ctrl Pts',(-43.4967433028155,-69.4134193510673,
-217.154414312055));
#200775=CARTESIAN_POINT('Ctrl Pts',(-46.9530675926807,-71.1335421841428,
-213.997473502442));
#200776=CARTESIAN_POINT('Ctrl Pts',(-26.2629114467516,-60.7391039700744,
-233.002893197821));
#200777=CARTESIAN_POINT('Ctrl Pts',(-27.114397963117,-61.1810939660079,
-232.20584360482));
#200778=CARTESIAN_POINT('Ctrl Pts',(-27.9674707129322,-61.6219011639104,
-231.409926775993));
#200779=CARTESIAN_POINT('Ctrl Pts',(-28.8218440521233,-62.0616481295084,
-230.614892210633));
#200780=CARTESIAN_POINT('Ctrl Pts',(-29.6762173913143,-62.5013950951064,
-229.819857645272));
#200781=CARTESIAN_POINT('Ctrl Pts',(-30.5318920874236,-62.9400822869671,
-229.025706439153));
#200782=CARTESIAN_POINT('Ctrl Pts',(-31.3886377598337,-63.3778284552318,
-228.232247232636));
#200783=CARTESIAN_POINT('Ctrl Pts',(-33.102129104654,-64.2533207917612,
-226.645328819602));
#200784=CARTESIAN_POINT('Ctrl Pts',(-34.8198706879942,-65.1250606034272,
-225.061147334889));
#200785=CARTESIAN_POINT('Ctrl Pts',(-36.5405225399701,-65.9938853198046,
-223.478668525429));
#200786=CARTESIAN_POINT('Ctrl Pts',(-39.981826243922,-67.7315347525594,
-220.313710906511));
#200787=CARTESIAN_POINT('Ctrl Pts',(-43.4345244003096,-69.457683375828,
-217.155376526334));
#200788=CARTESIAN_POINT('Ctrl Pts',(-46.8928095579913,-71.1769737453648,
-213.999726959588));
#200789=CARTESIAN_POINT('Ctrl Pts',(-26.2384700826335,-60.7381106363183,
-233.014375819121));
#200790=CARTESIAN_POINT('Ctrl Pts',(-27.0842500022742,-61.1857245057431,
-232.21450624766));
#200791=CARTESIAN_POINT('Ctrl Pts',(-27.9329490724857,-61.6311192767247,
-231.416680870253));
#200792=CARTESIAN_POINT('Ctrl Pts',(-28.7837425502454,-62.0747440392428,
-230.620229257902));
#200793=CARTESIAN_POINT('Ctrl Pts',(-29.634536028005,-62.5183688017608,
-229.82377764555));
#200794=CARTESIAN_POINT('Ctrl Pts',(-30.487432035617,-62.960223154147,-229.028708571446));
#200795=CARTESIAN_POINT('Ctrl Pts',(-31.3418749575762,-63.4006637505655,
-228.234599595102));
#200796=CARTESIAN_POINT('Ctrl Pts',(-33.0507608014949,-64.2815449434024,
-226.646381642412));
#200797=CARTESIAN_POINT('Ctrl Pts',(-34.7657386962016,-65.1568306952181,
-225.061930422221));
#200798=CARTESIAN_POINT('Ctrl Pts',(-36.4842100442897,-66.0284770468812,
-223.479425721276));
#200799=CARTESIAN_POINT('Ctrl Pts',(-39.9211527404658,-67.7717697502073,
-220.314416319386));
#200800=CARTESIAN_POINT('Ctrl Pts',(-43.3717095799881,-69.5008533336608,
-217.156983031728));
#200801=CARTESIAN_POINT('Ctrl Pts',(-46.827583501196,-71.2232650351743,
-214.002012001263));
#200802=CARTESIAN_POINT('Ctrl Pts',(-26.1949495995768,-60.7559954632254,
-233.015310708939));
#200803=CARTESIAN_POINT('Ctrl Pts',(-27.0387644538443,-61.2057327308231,
-232.215070168042));
#200804=CARTESIAN_POINT('Ctrl Pts',(-27.8858336675415,-61.6529664487026,
-231.417079914153));
#200805=CARTESIAN_POINT('Ctrl Pts',(-28.7351647823697,-62.0982646553384,
-230.620551354198));
#200806=CARTESIAN_POINT('Ctrl Pts',(-29.5844958971979,-62.5435628619743,
-229.824022794242));
#200807=CARTESIAN_POINT('Ctrl Pts',(-30.4361008904608,-62.9869237960558,
-229.028968199982));
#200808=CARTESIAN_POINT('Ctrl Pts',(-31.2893382107612,-63.4287766497893,
-228.234911333144));
#200809=CARTESIAN_POINT('Ctrl Pts',(-32.9958128513619,-64.3124823572563,
-226.646797599469));
#200810=CARTESIAN_POINT('Ctrl Pts',(-34.7087066827471,-65.190229522585,
-225.062593091688));
#200811=CARTESIAN_POINT('Ctrl Pts',(-36.425148099657,-66.0642498543572,
-223.480334162157));
#200812=CARTESIAN_POINT('Ctrl Pts',(-39.8580309334768,-67.8122905179015,
-220.315816303095));
#200813=CARTESIAN_POINT('Ctrl Pts',(-43.304744476869,-69.545794357118,-217.158884043615));
#200814=CARTESIAN_POINT('Ctrl Pts',(-46.7566079538913,-71.2728084364657,
-214.004305067604));
#200815=CARTESIAN_POINT('Ctrl Pts',(-26.1079086334631,-60.7917651170397,
-233.017180488577));
#200816=CARTESIAN_POINT('Ctrl Pts',(-26.9477933569846,-61.2457491809832,
-232.216198008803));
#200817=CARTESIAN_POINT('Ctrl Pts',(-27.791602857653,-61.6966607926582,
-231.417878001952));
#200818=CARTESIAN_POINT('Ctrl Pts',(-28.6380092466183,-62.1453058875298,
-230.62119554679));
#200819=CARTESIAN_POINT('Ctrl Pts',(-29.4844156355837,-62.5939509824013,
-229.824513091628));
#200820=CARTESIAN_POINT('Ctrl Pts',(-30.3334386001484,-63.0403250798734,
-229.029487457053));
#200821=CARTESIAN_POINT('Ctrl Pts',(-31.1842647171309,-63.485002448237,
-228.23553480923));
#200822=CARTESIAN_POINT('Ctrl Pts',(-32.8859169510958,-64.3743571849642,
-226.647629513582));
#200823=CARTESIAN_POINT('Ctrl Pts',(-34.5946426558381,-65.2570271773188,
-225.063918430622));
#200824=CARTESIAN_POINT('Ctrl Pts',(-36.3070242103916,-66.1357954693092,
-223.482151043919));
#200825=CARTESIAN_POINT('Ctrl Pts',(-39.7317873194987,-67.8933320532899,
-220.318616270514));
#200826=CARTESIAN_POINT('Ctrl Pts',(-43.1708142706306,-69.6356764040323,
-217.162686067389));
#200827=CARTESIAN_POINT('Ctrl Pts',(-46.6146568592818,-71.3718952390485,
-214.008891200286));
#200828=CARTESIAN_POINT('Ctrl Pts',(-26.0271556717183,-60.8195050993445,
-233.023057709875));
#200829=CARTESIAN_POINT('Ctrl Pts',(-26.8614803279425,-61.2789736199002,
-232.220907138713));
#200830=CARTESIAN_POINT('Ctrl Pts',(-27.7006372905616,-61.7344790137215,
-231.421952061255));
#200831=CARTESIAN_POINT('Ctrl Pts',(-28.5430811002764,-62.1870353929875,
-230.62500928173));
#200832=CARTESIAN_POINT('Ctrl Pts',(-29.3855249099912,-62.6395917722535,
-229.828066502204));
#200833=CARTESIAN_POINT('Ctrl Pts',(-30.2312298015655,-63.0892242106365,
-229.033124256632));
#200834=CARTESIAN_POINT('Ctrl Pts',(-31.0790619662469,-63.5367969787612,
-228.239400097671));
#200835=CARTESIAN_POINT('Ctrl Pts',(-32.7747262956096,-64.4319425150107,
-226.651951779748));
#200836=CARTESIAN_POINT('Ctrl Pts',(-34.4786705837165,-65.3190393016261,
-225.069228384841));
#200837=CARTESIAN_POINT('Ctrl Pts',(-36.1863583725991,-66.202056470716,
-223.488410098027));
#200838=CARTESIAN_POINT('Ctrl Pts',(-39.6017339503642,-67.9680908088958,
-220.326773524398));
#200839=CARTESIAN_POINT('Ctrl Pts',(-43.0317527614028,-69.7182854025588,
-217.172664187274));
#200840=CARTESIAN_POINT('Ctrl Pts',(-46.4657689946141,-71.4633532268859,
-214.020279084284));
#200841=CARTESIAN_POINT('Ctrl Pts',(-25.9715990783732,-60.8263824397187,
-233.038076562284));
#200842=CARTESIAN_POINT('Ctrl Pts',(-26.7915895883623,-61.2972176688764,
-232.2311442104));
#200843=CARTESIAN_POINT('Ctrl Pts',(-27.6213469993979,-61.7602848222496,
-231.430540367037));
#200844=CARTESIAN_POINT('Ctrl Pts',(-28.4556335624375,-62.2192160084591,
-230.63258019833));
#200845=CARTESIAN_POINT('Ctrl Pts',(-29.289920125477,-62.6781471946685,
-229.834620029623));
#200846=CARTESIAN_POINT('Ctrl Pts',(-30.1289511322075,-63.1328363273331,
-229.039478997096));
#200847=CARTESIAN_POINT('Ctrl Pts',(-30.9705439434446,-63.5850360083551,
-228.245754373682));
#200848=CARTESIAN_POINT('Ctrl Pts',(-32.6537295659188,-64.4894353703992,
-226.658305126855));
#200849=CARTESIAN_POINT('Ctrl Pts',(-34.3469173915073,-65.3841225672083,
-225.076391213479));
#200850=CARTESIAN_POINT('Ctrl Pts',(-36.0437616605612,-66.2748188763012,
-223.496282027351));
#200851=CARTESIAN_POINT('Ctrl Pts',(-39.4374501986691,-68.0562114944868,
-220.336063655097));
#200852=CARTESIAN_POINT('Ctrl Pts',(-42.8459482063409,-69.8217123813687,
-217.183304075329));
#200853=CARTESIAN_POINT('Ctrl Pts',(-46.2577049582974,-71.5830236206181,
-214.031928620936));
#200854=CARTESIAN_POINT('Ctrl Pts',(-25.9160424850282,-60.8332597800929,
-233.053095414693));
#200855=CARTESIAN_POINT('Ctrl Pts',(-26.7216988487821,-61.3154617178527,
-232.241381282086));
#200856=CARTESIAN_POINT('Ctrl Pts',(-27.5420567082342,-61.7860906307777,
-231.439128672818));
#200857=CARTESIAN_POINT('Ctrl Pts',(-28.3681860245984,-62.2513966239306,
-230.64015111493));
#200858=CARTESIAN_POINT('Ctrl Pts',(-29.1943153409628,-62.7167026170834,
-229.841173557043));
#200859=CARTESIAN_POINT('Ctrl Pts',(-30.0266724628494,-63.1764484440297,
-229.045833737559));
#200860=CARTESIAN_POINT('Ctrl Pts',(-30.8620259206422,-63.633275037949,
-228.252108649693));
#200861=CARTESIAN_POINT('Ctrl Pts',(-32.5327328362278,-64.5469282257876,
-226.664658473961));
#200862=CARTESIAN_POINT('Ctrl Pts',(-34.215164199298,-65.4492058327905,
-225.083554042117));
#200863=CARTESIAN_POINT('Ctrl Pts',(-35.9011649485234,-66.3475812818863,
-223.504153956677));
#200864=CARTESIAN_POINT('Ctrl Pts',(-39.273166446974,-68.1443321800779,
-220.345353785796));
#200865=CARTESIAN_POINT('Ctrl Pts',(-42.6601436512792,-69.9251393601785,
-217.193943963384));
#200866=CARTESIAN_POINT('Ctrl Pts',(-46.0496409219808,-71.7026940143502,
-214.043578157589));
#200867=CARTESIAN_POINT('Ctrl Pts',(-25.8665286108953,-60.8381274420046,
-233.066411683095));
#200868=CARTESIAN_POINT('Ctrl Pts',(-26.6581633289744,-61.3291620138588,
-232.251762724729));
#200869=CARTESIAN_POINT('Ctrl Pts',(-27.4689810980677,-61.805659144746,
-231.449321410308));
#200870=CARTESIAN_POINT('Ctrl Pts',(-28.2858283440085,-62.276644660254,
-230.650185251577));
#200871=CARTESIAN_POINT('Ctrl Pts',(-29.1026755899493,-62.747630175762,
-229.851049092846));
#200872=CARTESIAN_POINT('Ctrl Pts',(-29.9264514304638,-63.2126139436637,
-229.055899144978));
#200873=CARTESIAN_POINT('Ctrl Pts',(-30.7532556538434,-63.6747328220346,
-228.26235895591));
#200874=CARTESIAN_POINT('Ctrl Pts',(-32.4068641006027,-64.5989705787766,
-226.675278577774));
#200875=CARTESIAN_POINT('Ctrl Pts',(-34.0724444645535,-65.5119690076117,
-225.094611701508));
#200876=CARTESIAN_POINT('Ctrl Pts',(-35.7413375761177,-66.4214664741137,
-223.515524234354));
#200877=CARTESIAN_POINT('Ctrl Pts',(-39.0791237992462,-68.2404614071178,
-220.357349300048));
#200878=CARTESIAN_POINT('Ctrl Pts',(-42.4312557792835,-70.0447514385552,
-217.206261484219));
#200879=CARTESIAN_POINT('Ctrl Pts',(-45.7856616296808,-71.8461945922107,
-214.056132477959));
#200880=CARTESIAN_POINT('Ctrl Pts',(-25.8011224073928,-60.8541224995348,
-233.072388186401));
#200881=CARTESIAN_POINT('Ctrl Pts',(-26.5882772139689,-61.345584476566,
-232.260902563554));
#200882=CARTESIAN_POINT('Ctrl Pts',(-27.3926111430279,-61.824140301072,
-231.460141397784));
#200883=CARTESIAN_POINT('Ctrl Pts',(-28.2023317845711,-62.2979002023416,
-230.662317129508));
#200884=CARTESIAN_POINT('Ctrl Pts',(-29.0120524261143,-62.7716601036112,
-229.864492861231));
#200885=CARTESIAN_POINT('Ctrl Pts',(-29.8279705672755,-63.2401673093096,
-229.070199114559));
#200886=CARTESIAN_POINT('Ctrl Pts',(-30.6466000725898,-63.7061844369386,
-228.277344321055));
#200887=CARTESIAN_POINT('Ctrl Pts',(-32.2838590832184,-64.6382186921966,
-226.691634734048));
#200888=CARTESIAN_POINT('Ctrl Pts',(-33.9318380253269,-65.5604762032412,
-225.111654172302));
#200889=CARTESIAN_POINT('Ctrl Pts',(-35.582792800409,-66.4797047104531,
-223.533108945327));
#200890=CARTESIAN_POINT('Ctrl Pts',(-38.884702350573,-68.3181617248767,
-220.376018491376));
#200891=CARTESIAN_POINT('Ctrl Pts',(-42.1994895547755,-70.143871943617,
-217.225335489343));
#200892=CARTESIAN_POINT('Ctrl Pts',(-45.5163300351324,-71.9671084389128,
-214.075544244624));
#200893=CARTESIAN_POINT('Ctrl Pts',(-25.7357162038904,-60.870117557065,
-233.078364689706));
#200894=CARTESIAN_POINT('Ctrl Pts',(-26.5183910989635,-61.3620069392732,
-232.270042402379));
#200895=CARTESIAN_POINT('Ctrl Pts',(-27.3162411879881,-61.842621457398,
-231.470961385261));
#200896=CARTESIAN_POINT('Ctrl Pts',(-28.1188352251337,-62.3191557444292,
-230.674449007438));
#200897=CARTESIAN_POINT('Ctrl Pts',(-28.9214292622792,-62.7956900314603,
-229.877936629616));
#200898=CARTESIAN_POINT('Ctrl Pts',(-29.7294897040872,-63.2677206749556,
-229.084499084141));
#200899=CARTESIAN_POINT('Ctrl Pts',(-30.5399444913362,-63.7376360518426,
-228.292329686201));
#200900=CARTESIAN_POINT('Ctrl Pts',(-32.1608540658341,-64.6774668056166,
-226.707990890321));
#200901=CARTESIAN_POINT('Ctrl Pts',(-33.7912315861003,-65.6089833988707,
-225.128696643096));
#200902=CARTESIAN_POINT('Ctrl Pts',(-35.4242480247001,-66.5379429467924,
-223.550693656299));
#200903=CARTESIAN_POINT('Ctrl Pts',(-38.6902809018998,-68.3958620426357,
-220.394687682705));
#200904=CARTESIAN_POINT('Ctrl Pts',(-41.9677233302676,-70.2429924486788,
-217.244409494466));
#200905=CARTESIAN_POINT('Ctrl Pts',(-45.2469984405841,-72.088022285615,
-214.09495601129));
#200906=CARTESIAN_POINT('Ctrl Pts',(-25.6764457543321,-60.8781185651427,
-233.089415099072));
#200907=CARTESIAN_POINT('Ctrl Pts',(-26.4517816472997,-61.3719375798059,
-232.282825348105));
#200908=CARTESIAN_POINT('Ctrl Pts',(-27.2411241731431,-61.8556224049542,
-231.484690141905));
#200909=CARTESIAN_POINT('Ctrl Pts',(-28.0348403941315,-62.3356735301276,
-230.688923056315));
#200910=CARTESIAN_POINT('Ctrl Pts',(-28.8285566151198,-62.8157246553009,
-229.893155970723));
#200911=CARTESIAN_POINT('Ctrl Pts',(-29.6273152575741,-63.2917540571251,
-229.100216973599));
#200912=CARTESIAN_POINT('Ctrl Pts',(-30.4282830173054,-63.7659009259987,
-228.308450386598));
#200913=CARTESIAN_POINT('Ctrl Pts',(-32.0302185367682,-64.7141946637459,
-226.724917212596));
#200914=CARTESIAN_POINT('Ctrl Pts',(-33.6408900276233,-65.6550862143651,
-225.14604576641));
#200915=CARTESIAN_POINT('Ctrl Pts',(-35.2539988230218,-66.5937075233338,
-223.568378062868));
#200916=CARTESIAN_POINT('Ctrl Pts',(-38.4802164138187,-68.4709501412712,
-220.413042655783));
#200917=CARTESIAN_POINT('Ctrl Pts',(-41.7169696970508,-70.3386046036742,
-217.263033043788));
#200918=CARTESIAN_POINT('Ctrl Pts',(-44.9554183644225,-72.2043881447385,
-214.113800504198));
#200919=CARTESIAN_POINT('Ctrl Pts',(-25.6298304748707,-60.8753734341798,
-233.107177069033));
#200920=CARTESIAN_POINT('Ctrl Pts',(-26.3965314717851,-61.3714239166506,
-232.301492490062));
#200921=CARTESIAN_POINT('Ctrl Pts',(-27.1765365083298,-61.8582017525339,
-231.503828898795));
#200922=CARTESIAN_POINT('Ctrl Pts',(-27.960699151696,-62.3416685933693,
-230.708430592375));
#200923=CARTESIAN_POINT('Ctrl Pts',(-28.7448617950622,-62.8251354342047,
-229.913032285956));
#200924=CARTESIAN_POINT('Ctrl Pts',(-29.5338172036037,-63.3049330183218,
-229.120332249855));
#200925=CARTESIAN_POINT('Ctrl Pts',(-30.3248744392529,-63.7830152939694,
-228.328756578445));
#200926=CARTESIAN_POINT('Ctrl Pts',(-31.9069889105511,-64.7391798452646,
-226.745605235623));
#200927=CARTESIAN_POINT('Ctrl Pts',(-33.4974147722857,-65.6885985452027,
-225.166922566632));
#200928=CARTESIAN_POINT('Ctrl Pts',(-35.0901638016772,-66.6359498673557,
-223.589403428947));
#200929=CARTESIAN_POINT('Ctrl Pts',(-38.2756618604604,-68.5306525116616,
-220.434365153576));
#200930=CARTESIAN_POINT('Ctrl Pts',(-41.4711974327502,-70.4166207416591,
-217.284462017333));
#200931=CARTESIAN_POINT('Ctrl Pts',(-44.6683526580257,-72.3008817462311,
-214.135317230106));
#200932=CARTESIAN_POINT('Ctrl Pts',(-25.5832151954094,-60.8726283032168,
-233.124939038994));
#200933=CARTESIAN_POINT('Ctrl Pts',(-26.3412812962705,-61.3709102534954,
-232.320159632019));
#200934=CARTESIAN_POINT('Ctrl Pts',(-27.1119488435164,-61.8607811001136,
-231.522967655684));
#200935=CARTESIAN_POINT('Ctrl Pts',(-27.8865579092606,-62.347663656611,
-230.727938128436));
#200936=CARTESIAN_POINT('Ctrl Pts',(-28.6611669750047,-62.8345462131084,
-229.932908601188));
#200937=CARTESIAN_POINT('Ctrl Pts',(-29.4403191496334,-63.3181119795184,
-229.140447526113));
#200938=CARTESIAN_POINT('Ctrl Pts',(-30.2214658612003,-63.8001296619401,
-228.349062770292));
#200939=CARTESIAN_POINT('Ctrl Pts',(-31.783759284334,-64.7641650267834,
-226.766293258651));
#200940=CARTESIAN_POINT('Ctrl Pts',(-33.353939516948,-65.7221108760403,
-225.187799366854));
#200941=CARTESIAN_POINT('Ctrl Pts',(-34.9263287803327,-66.6781922113775,
-223.610428795026));
#200942=CARTESIAN_POINT('Ctrl Pts',(-38.071107307102,-68.590354882052,-220.455687651369));
#200943=CARTESIAN_POINT('Ctrl Pts',(-41.2254251684497,-70.494636879644,
-217.305890990877));
#200944=CARTESIAN_POINT('Ctrl Pts',(-44.381286951629,-72.3973753477236,
-214.156833956015));
#200945=CARTESIAN_POINT('Ctrl Pts',(-25.5332663260497,-60.8715565679525,
-233.140620047442));
#200946=CARTESIAN_POINT('Ctrl Pts',(-26.2846593466459,-61.3702751859077,
-232.337976743902));
#200947=CARTESIAN_POINT('Ctrl Pts',(-27.0470683275914,-61.861877181739,
-231.541902635733));
#200948=CARTESIAN_POINT('Ctrl Pts',(-27.8129663979903,-62.3509604518928,
-230.747753285103));
#200949=CARTESIAN_POINT('Ctrl Pts',(-28.5788644683892,-62.8400437220466,
-229.953603934473));
#200950=CARTESIAN_POINT('Ctrl Pts',(-29.3487694431048,-63.3263269973223,
-229.161720142653));
#200951=CARTESIAN_POINT('Ctrl Pts',(-30.120445915247,-63.8113027794608,
-228.370799649172));
#200952=CARTESIAN_POINT('Ctrl Pts',(-31.6637988595316,-64.7812543437376,
-226.788958662211));
#200953=CARTESIAN_POINT('Ctrl Pts',(-33.2141526002521,-65.7460617730361,
-225.210938813702));
#200954=CARTESIAN_POINT('Ctrl Pts',(-34.7664868193848,-66.7092887992816,
-223.633944018777));
#200955=CARTESIAN_POINT('Ctrl Pts',(-37.8711552576499,-68.6357428517727,
-220.479954428925));
#200956=CARTESIAN_POINT('Ctrl Pts',(-40.9843522069086,-70.555519752599,
-217.330448431736));
#200957=CARTESIAN_POINT('Ctrl Pts',(-44.0989468098099,-72.4739730046678,
-214.18163152198));
#200958=CARTESIAN_POINT('Ctrl Pts',(-25.4734681104549,-60.8745649395491,
-233.152705479171));
#200959=CARTESIAN_POINT('Ctrl Pts',(-26.2191301593905,-61.3728030581697,
-232.352982827705));
#200960=CARTESIAN_POINT('Ctrl Pts',(-26.9737314089713,-61.8653651155087,
-231.558531400184));
#200961=CARTESIAN_POINT('Ctrl Pts',(-27.7312103498245,-62.3559170177131,
-230.765669056017));
#200962=CARTESIAN_POINT('Ctrl Pts',(-28.4886892906776,-62.8464689199175,
-229.972806711851));
#200963=CARTESIAN_POINT('Ctrl Pts',(-29.2494572009032,-63.3347856810085,
-229.181797847991));
#200964=CARTESIAN_POINT('Ctrl Pts',(-30.0116917876015,-63.8220563583486,
-228.391588810695));
#200965=CARTESIAN_POINT('Ctrl Pts',(-31.5361609609982,-64.7965977130286,
-226.811170736103));
#200966=CARTESIAN_POINT('Ctrl Pts',(-33.0664220838837,-65.7670232712464,
-225.233920858118));
#200967=CARTESIAN_POINT('Ctrl Pts',(-34.5983413220466,-66.7361768147042,
-223.657538786233));
#200968=CARTESIAN_POINT('Ctrl Pts',(-37.6621797983723,-68.6744839016197,
-220.504774642461));
#200969=CARTESIAN_POINT('Ctrl Pts',(-40.7331349268486,-70.6074216926982,
-217.355782960055));
#200970=CARTESIAN_POINT('Ctrl Pts',(-43.8052734509942,-72.5392749729601,
-214.207386766717));
#200971=CARTESIAN_POINT('Ctrl Pts',(-25.4136698948603,-60.8775733111457,
-233.1647909109));
#200972=CARTESIAN_POINT('Ctrl Pts',(-26.1536009721352,-61.3753309304317,
-232.367988911507));
#200973=CARTESIAN_POINT('Ctrl Pts',(-26.9003944903513,-61.8688530492783,
-231.575160164634));
#200974=CARTESIAN_POINT('Ctrl Pts',(-27.6494543016586,-62.3608735835334,
-230.783584826932));
#200975=CARTESIAN_POINT('Ctrl Pts',(-28.3985141129659,-62.8528941177885,
-229.992009489228));
#200976=CARTESIAN_POINT('Ctrl Pts',(-29.1501449587015,-63.3432443646947,
-229.201875553329));
#200977=CARTESIAN_POINT('Ctrl Pts',(-29.902937659956,-63.8328099372364,
-228.412377972218));
#200978=CARTESIAN_POINT('Ctrl Pts',(-31.4085230624649,-64.8119410823196,
-226.833382809995));
#200979=CARTESIAN_POINT('Ctrl Pts',(-32.9186915675153,-65.7879847694566,
-225.256902902535));
#200980=CARTESIAN_POINT('Ctrl Pts',(-34.4301958247084,-66.7630648301267,
-223.681133553689));
#200981=CARTESIAN_POINT('Ctrl Pts',(-37.4532043390948,-68.7132249514667,
-220.529594855996));
#200982=CARTESIAN_POINT('Ctrl Pts',(-40.4819176467888,-70.6593236327973,
-217.381117488375));
#200983=CARTESIAN_POINT('Ctrl Pts',(-43.5116000921785,-72.6045769412523,
-214.233142011455));
#200984=CARTESIAN_POINT('Ctrl Pts',(-25.3604578094675,-60.8735170241007,
-233.18242034351));
#200985=CARTESIAN_POINT('Ctrl Pts',(-26.0930283102741,-61.3713501637903,
-232.387708547763));
#200986=CARTESIAN_POINT('Ctrl Pts',(-26.8307495672501,-61.866135521907,
-231.595979029253));
#200987=CARTESIAN_POINT('Ctrl Pts',(-27.5702957875313,-62.3597741472074,
-230.805269005779));
#200988=CARTESIAN_POINT('Ctrl Pts',(-28.3098420078126,-62.8534127725078,
-230.014558982304));
#200989=CARTESIAN_POINT('Ctrl Pts',(-29.0514176428578,-63.3457952241198,
-229.224993612889));
#200990=CARTESIAN_POINT('Ctrl Pts',(-29.7939421742496,-63.8375690870219,
-228.435953327864));
#200991=CARTESIAN_POINT('Ctrl Pts',(-31.2789912370331,-64.8211168128261,
-226.857872757815));
#200992=CARTESIAN_POINT('Ctrl Pts',(-32.767772611159,-65.8022749106513,
-225.281860356042));
#200993=CARTESIAN_POINT('Ctrl Pts',(-34.2576895400343,-66.7826561972701,
-223.706461237247));
#200994=CARTESIAN_POINT('Ctrl Pts',(-37.237523397785,-68.7434187705077,
-220.555662999657));
#200995=CARTESIAN_POINT('Ctrl Pts',(-40.2221506876178,-70.7009385693032,
-217.407470987453));
#200996=CARTESIAN_POINT('Ctrl Pts',(-43.2076329024777,-72.657747925151,
-214.259730555427));
#200997=CARTESIAN_POINT('Ctrl Pts',(-25.3082796911041,-60.8654535469475,
-233.203637421846));
#200998=CARTESIAN_POINT('Ctrl Pts',(-26.0341343285133,-61.3629238744168,
-232.411039848471));
#200999=CARTESIAN_POINT('Ctrl Pts',(-26.7636013838676,-61.8583152760603,
-231.620533187723));
#201000=CARTESIAN_POINT('Ctrl Pts',(-27.4944243031966,-62.3528874641244,
-230.830789824077));
#201001=CARTESIAN_POINT('Ctrl Pts',(-28.2252472225255,-62.8474596521885,
-230.041046460431));
#201002=CARTESIAN_POINT('Ctrl Pts',(-28.9575562895767,-63.3411438699236,
-229.252145525666));
#201003=CARTESIAN_POINT('Ctrl Pts',(-29.6905827327532,-63.8343860369735,
-228.463645185323));
#201004=CARTESIAN_POINT('Ctrl Pts',(-31.1566356191065,-64.8208703710732,
-226.886644504638));
#201005=CARTESIAN_POINT('Ctrl Pts',(-32.6255046561051,-65.8056211821729,
-225.311217867621));
#201006=CARTESIAN_POINT('Ctrl Pts',(-34.0952688014063,-66.7897856212239,
-223.736281731367));
#201007=CARTESIAN_POINT('Ctrl Pts',(-37.034797092009,-68.7581144993257,
-220.58640945886));
#201008=CARTESIAN_POINT('Ctrl Pts',(-39.9780639773415,-70.7240153450236,
-217.438595831035));
#201009=CARTESIAN_POINT('Ctrl Pts',(-42.922034708619,-72.6893523415957,
-214.291161723059));
#201010=CARTESIAN_POINT('Ctrl Pts',(-25.2821906319223,-60.8614218083708,
-233.214245961014));
#201011=CARTESIAN_POINT('Ctrl Pts',(-26.0046873376329,-61.35871072973,-232.422705498826));
#201012=CARTESIAN_POINT('Ctrl Pts',(-26.7300272921764,-61.854405153137,
-231.632810266957));
#201013=CARTESIAN_POINT('Ctrl Pts',(-27.4564885610292,-62.3494441225829,
-230.843550233226));
#201014=CARTESIAN_POINT('Ctrl Pts',(-28.182949829882,-62.8444830920289,
-230.054290199494));
#201015=CARTESIAN_POINT('Ctrl Pts',(-28.9106256129361,-63.3388181928255,
-229.265721482054));
#201016=CARTESIAN_POINT('Ctrl Pts',(-29.6389030120051,-63.8327945119493,
-228.477491114052));
#201017=CARTESIAN_POINT('Ctrl Pts',(-31.0954578101431,-64.8207471501967,
-226.901030378049));
#201018=CARTESIAN_POINT('Ctrl Pts',(-32.5543706785782,-65.8072943179338,
-225.32589662341));
#201019=CARTESIAN_POINT('Ctrl Pts',(-34.0140584320924,-66.7933503332008,
-223.751191978427));
#201020=CARTESIAN_POINT('Ctrl Pts',(-36.933433939121,-68.7654623637348,
-220.60178268846));
#201021=CARTESIAN_POINT('Ctrl Pts',(-39.8560206222034,-70.7355537328838,
-217.454158252827));
#201022=CARTESIAN_POINT('Ctrl Pts',(-42.7792356116896,-72.705154549818,
-214.306877306875));
#201023=CARTESIAN_POINT('Ctrl Pts',(-25.2542808545004,-60.8576193179734,
-233.224589731722));
#201024=CARTESIAN_POINT('Ctrl Pts',(-25.9733613508541,-61.3547669345154,
-232.433994495002));
#201025=CARTESIAN_POINT('Ctrl Pts',(-26.6946341378572,-61.850707669122,
-231.644667681488));
#201026=CARTESIAN_POINT('Ctrl Pts',(-27.4168149846347,-62.3461306013993,
-230.855857430941));
#201027=CARTESIAN_POINT('Ctrl Pts',(-28.1389958314122,-62.8415535336766,
-230.067047180394));
#201028=CARTESIAN_POINT('Ctrl Pts',(-28.8621498208122,-63.3364251861756,
-229.278792485017));
#201029=CARTESIAN_POINT('Ctrl Pts',(-29.5857994425194,-63.8310086087711,
-228.490817987778));
#201030=CARTESIAN_POINT('Ctrl Pts',(-31.0330986859336,-64.8201754539622,
-226.914868993301));
#201031=CARTESIAN_POINT('Ctrl Pts',(-32.482338164911,-65.8082141619607,
-225.340017314949));
#201032=CARTESIAN_POINT('Ctrl Pts',(-33.9322394111677,-66.7958442294134,
-223.765535080096));
#201033=CARTESIAN_POINT('Ctrl Pts',(-36.8320419036812,-68.771104364319,
-220.61657061039));
#201034=CARTESIAN_POINT('Ctrl Pts',(-39.7345648061665,-70.7446942844296,
-217.469129121935));
#201035=CARTESIAN_POINT('Ctrl Pts',(-42.637644247718,-72.7178586955381,
-214.321995277256));
#201036=CARTESIAN_POINT('Ctrl Pts',(-25.2239774050683,-60.8541676049626,
-233.234470884236));
#201037=CARTESIAN_POINT('Ctrl Pts',(-25.9398083842247,-61.3511430455559,
-232.444758300872));
#201038=CARTESIAN_POINT('Ctrl Pts',(-26.6572825734193,-61.8472255929447,
-231.655996189968));
#201039=CARTESIAN_POINT('Ctrl Pts',(-27.3754647705453,-62.3429113806012,
-230.867638000096));
#201040=CARTESIAN_POINT('Ctrl Pts',(-28.0936469676712,-62.8385971682577,
-230.079279810225));
#201041=CARTESIAN_POINT('Ctrl Pts',(-28.8125820204444,-63.3338632665416,
-229.291352292986));
#201042=CARTESIAN_POINT('Ctrl Pts',(-29.5319096752348,-63.8289050323554,
-228.503647571677));
#201043=CARTESIAN_POINT('Ctrl Pts',(-30.9705649848157,-64.8189885639829,
-226.928238129057));
#201044=CARTESIAN_POINT('Ctrl Pts',(-32.4107560406701,-65.8081944618785,
-225.353700434162));
#201045=CARTESIAN_POINT('Ctrl Pts',(-33.8514884032197,-66.7970717553631,
-223.779466811102));
#201046=CARTESIAN_POINT('Ctrl Pts',(-36.732953128319,-68.7748263423323,
-220.630999564983));
#201047=CARTESIAN_POINT('Ctrl Pts',(-39.6166287632978,-70.7512448922044,
-217.483776946995));
#201048=CARTESIAN_POINT('Ctrl Pts',(-42.5007756355285,-72.7273057434785,
-214.336817183699));
#201049=CARTESIAN_POINT('Ctrl Pts',(-25.1936739556362,-60.8507158919519,
-233.244352036751));
#201050=CARTESIAN_POINT('Ctrl Pts',(-25.9062554175954,-61.3475191565963,
-232.455522106742));
#201051=CARTESIAN_POINT('Ctrl Pts',(-26.6199310089813,-61.8437435167674,
-231.667324698448));
#201052=CARTESIAN_POINT('Ctrl Pts',(-27.3341145564557,-62.3396921598031,
-230.879418569252));
#201053=CARTESIAN_POINT('Ctrl Pts',(-28.0482981039303,-62.8356408028389,
-230.091512440055));
#201054=CARTESIAN_POINT('Ctrl Pts',(-28.7630142200764,-63.3313013469077,
-229.303912100956));
#201055=CARTESIAN_POINT('Ctrl Pts',(-29.4780199079502,-63.8268014559396,
-228.516477155575));
#201056=CARTESIAN_POINT('Ctrl Pts',(-30.9080312836978,-64.8178016740036,
-226.941607264814));
#201057=CARTESIAN_POINT('Ctrl Pts',(-32.3391739164292,-65.8081747617964,
-225.367383553375));
#201058=CARTESIAN_POINT('Ctrl Pts',(-33.7707373952718,-66.7982992813128,
-223.793398542109));
#201059=CARTESIAN_POINT('Ctrl Pts',(-36.6338643529568,-68.7785483203456,
-220.645428519576));
#201060=CARTESIAN_POINT('Ctrl Pts',(-39.498692720429,-70.7577954999793,
-217.498424772054));
#201061=CARTESIAN_POINT('Ctrl Pts',(-42.363907023339,-72.7367527914189,
-214.351639090142));
#201062=CARTESIAN_POINT('Ctrl Pts',(-25.1598238196964,-60.8482202385386,
-233.25309688913));
#201063=CARTESIAN_POINT('Ctrl Pts',(-25.8694641248229,-61.3447486920278,
-232.465168808441));
#201064=CARTESIAN_POINT('Ctrl Pts',(-26.5797195835393,-61.8409546524082,
-231.677595750858));
#201065=CARTESIAN_POINT('Ctrl Pts',(-27.2902792575572,-62.3369977131888,
-230.890197499475));
#201066=CARTESIAN_POINT('Ctrl Pts',(-28.000838931575,-62.8330407739693,
-230.102799248092));
#201067=CARTESIAN_POINT('Ctrl Pts',(-28.711714550991,-63.3289150112138,
-229.315582660731));
#201068=CARTESIAN_POINT('Ctrl Pts',(-29.4227692929209,-63.8246912312197,
-228.528468791165));
#201069=CARTESIAN_POINT('Ctrl Pts',(-30.8448787767808,-64.8162436712314,
-226.954241052034));
#201070=CARTESIAN_POINT('Ctrl Pts',(-32.2676879017602,-65.8074128718581,
-225.380414529439));
#201071=CARTESIAN_POINT('Ctrl Pts',(-33.6907733702002,-66.7984195359043,
-223.806745992614));
#201072=CARTESIAN_POINT('Ctrl Pts',(-36.5369443070804,-68.7804328639968,
-220.659408918962));
#201073=CARTESIAN_POINT('Ctrl Pts',(-39.3842222584393,-70.7617958073898,
-217.512705107097));
#201074=CARTESIAN_POINT('Ctrl Pts',(-42.2317710074449,-72.7429480158072,
-214.366156356611));
#201075=CARTESIAN_POINT('Ctrl Pts',(-25.1256029177818,-60.8447964462213,
-233.262708527412));
#201076=CARTESIAN_POINT('Ctrl Pts',(-25.8323432559684,-61.3411439778804,
-232.475469715128));
#201077=CARTESIAN_POINT('Ctrl Pts',(-26.5393879179131,-61.8373317659467,
-231.688406549544));
#201078=CARTESIAN_POINT('Ctrl Pts',(-27.2465878469089,-62.3334358738351,
-230.90143275512));
#201079=CARTESIAN_POINT('Ctrl Pts',(-27.9537877759048,-62.8295399817235,
-230.114458960696));
#201080=CARTESIAN_POINT('Ctrl Pts',(-28.6611482655484,-63.3255577393973,
-229.327577621181));
#201081=CARTESIAN_POINT('Ctrl Pts',(-29.3686016850915,-63.8215238522036,
-228.540749713863));
#201082=CARTESIAN_POINT('Ctrl Pts',(-30.7835085241778,-64.8134560778162,
-226.967093899227));
#201083=CARTESIAN_POINT('Ctrl Pts',(-32.198778370749,-65.8051862301184,
-225.3936468087));
#201084=CARTESIAN_POINT('Ctrl Pts',(-33.6141958867398,-66.7968253706499,
-223.820284551445));
#201085=CARTESIAN_POINT('Ctrl Pts',(-36.4450309187215,-68.7801036517128,
-220.673560036935));
#201086=CARTESIAN_POINT('Ctrl Pts',(-39.2764551401188,-70.7630188613062,
-217.527174130311));
#201087=CARTESIAN_POINT('Ctrl Pts',(-42.1080287367154,-72.7457990899024,
-214.3808746454));
#201088=CARTESIAN_POINT('Ctrl Pts',(-25.0913820158672,-60.8413726539041,
-233.272320165694));
#201089=CARTESIAN_POINT('Ctrl Pts',(-25.7952223871138,-61.337539263733,
-232.485770621816));
#201090=CARTESIAN_POINT('Ctrl Pts',(-26.4990562522867,-61.8337088794851,
-231.699217348229));
#201091=CARTESIAN_POINT('Ctrl Pts',(-27.2028964362607,-62.3298740344814,
-230.912668010765));
#201092=CARTESIAN_POINT('Ctrl Pts',(-27.9067366202345,-62.8260391894777,
-230.126118673301));
#201093=CARTESIAN_POINT('Ctrl Pts',(-28.6105819801057,-63.3222004675808,
-229.339572581631));
#201094=CARTESIAN_POINT('Ctrl Pts',(-29.314434077262,-63.8183564731875,
-228.553030636562));
#201095=CARTESIAN_POINT('Ctrl Pts',(-30.7221382715748,-64.8106684844009,
-226.97994674642));
#201096=CARTESIAN_POINT('Ctrl Pts',(-32.1298688397377,-65.8029595883788,
-225.406879087961));
#201097=CARTESIAN_POINT('Ctrl Pts',(-33.5376184032793,-66.7952312053955,
-223.833823110276));
#201098=CARTESIAN_POINT('Ctrl Pts',(-36.3531175303626,-68.7797744394288,
-220.687711154908));
#201099=CARTESIAN_POINT('Ctrl Pts',(-39.1686880217984,-70.7642419152226,
-217.541643153526));
#201100=CARTESIAN_POINT('Ctrl Pts',(-41.9842864659859,-72.7486501639975,
-214.39559293419));
#201101=CARTESIAN_POINT('Ctrl Pts',(-25.0620255817184,-60.8342761915281,
-233.285941631018));
#201102=CARTESIAN_POINT('Ctrl Pts',(-25.7623705261304,-61.3306758976375,
-232.499505184585));
#201103=CARTESIAN_POINT('Ctrl Pts',(-26.4626944173704,-61.8270835434123,
-231.713056538299));
#201104=CARTESIAN_POINT('Ctrl Pts',(-27.1630058058958,-62.3234949649194,
-230.926600669881));
#201105=CARTESIAN_POINT('Ctrl Pts',(-27.8633171944211,-62.8199063864266,
-230.140144801462));
#201106=CARTESIAN_POINT('Ctrl Pts',(-28.5636158753459,-63.3163216831959,
-229.353681591601));
#201107=CARTESIAN_POINT('Ctrl Pts',(-29.2639064106539,-63.8127386310709,
-228.567213695831));
#201108=CARTESIAN_POINT('Ctrl Pts',(-30.6644874812699,-64.8055725268209,
-226.994277904292));
#201109=CARTESIAN_POINT('Ctrl Pts',(-32.0650366774472,-65.7984126816902,
-225.421323781149));
#201110=CARTESIAN_POINT('Ctrl Pts',(-33.4655708458739,-66.7912508691866,
-223.848361132451));
#201111=CARTESIAN_POINT('Ctrl Pts',(-36.2666391827274,-68.7769272441794,
-220.702435835054));
#201112=CARTESIAN_POINT('Ctrl Pts',(-39.0676484327315,-70.7625952457594,
-217.556477030254));
#201113=CARTESIAN_POINT('Ctrl Pts',(-41.8686390590285,-72.7482350521135,
-214.410508283843));
#201114=CARTESIAN_POINT('Ctrl Pts',(-25.028605078732,-60.8264461849104,
-233.300589177504));
#201115=CARTESIAN_POINT('Ctrl Pts',(-25.7257590504183,-61.3230773961178,
-232.514138876127));
#201116=CARTESIAN_POINT('Ctrl Pts',(-26.4228956738429,-61.8197151427821,
-231.727678440368));
#201117=CARTESIAN_POINT('Ctrl Pts',(-27.1200213189657,-62.3163563966737,
-230.941211605428));
#201118=CARTESIAN_POINT('Ctrl Pts',(-27.8171469640885,-62.8129976505652,
-230.154744770487));
#201119=CARTESIAN_POINT('Ctrl Pts',(-28.514261502952,-63.3096424726104,
-229.368271461406));
#201120=CARTESIAN_POINT('Ctrl Pts',(-29.2113685617452,-63.8062891397564,
-228.581793805278));
#201121=CARTESIAN_POINT('Ctrl Pts',(-30.6055826793317,-64.7995824740485,
-227.008838493021));
#201122=CARTESIAN_POINT('Ctrl Pts',(-31.9997674609787,-65.7928829112188,
-225.435866135329));
#201123=CARTESIAN_POINT('Ctrl Pts',(-33.393937296167,-66.786183616434,-223.862885177104));
#201124=CARTESIAN_POINT('Ctrl Pts',(-36.1822769665438,-68.7727850268643,
-220.716923260653));
#201125=CARTESIAN_POINT('Ctrl Pts',(-38.9705580867346,-70.7593869240872,
-217.570927667784));
#201126=CARTESIAN_POINT('Ctrl Pts',(-41.7588188049893,-72.745971187409,
-214.424920813073));
#201127=CARTESIAN_POINT('Ctrl Pts',(-25.0118948272389,-60.8225311816015,
-233.307912950748));
#201128=CARTESIAN_POINT('Ctrl Pts',(-25.7074533125622,-61.319278145358,
-232.521455721897));
#201129=CARTESIAN_POINT('Ctrl Pts',(-26.4029963020791,-61.8160309424671,
-231.734989391403));
#201130=CARTESIAN_POINT('Ctrl Pts',(-27.0985290755007,-62.3127871125508,
-230.948517073201));
#201131=CARTESIAN_POINT('Ctrl Pts',(-27.7940618489222,-62.8095432826346,
-230.162044755));
#201132=CARTESIAN_POINT('Ctrl Pts',(-28.489584316755,-63.3063028673177,
-229.375566396309));
#201133=CARTESIAN_POINT('Ctrl Pts',(-29.1850996372909,-63.8030643940992,
-228.589083860001));
#201134=CARTESIAN_POINT('Ctrl Pts',(-30.5761302783625,-64.7965874476622,
-227.016118787385));
#201135=CARTESIAN_POINT('Ctrl Pts',(-31.9671328527444,-65.7901180259831,
-225.443137312419));
#201136=CARTESIAN_POINT('Ctrl Pts',(-33.3581205213136,-66.7836499900577,
-223.870147199431));
#201137=CARTESIAN_POINT('Ctrl Pts',(-36.140095858452,-68.7707139182068,
-220.724166973453));
#201138=CARTESIAN_POINT('Ctrl Pts',(-38.9220129137361,-70.7577827632511,
-217.578152986549));
#201139=CARTESIAN_POINT('Ctrl Pts',(-41.7039086779697,-72.7448392550568,
-214.432127077688));
#201140=CARTESIAN_POINT('Ctrl Pts',(-24.9941555235601,-60.8184248975328,
-233.315484141906));
#201141=CARTESIAN_POINT('Ctrl Pts',(-25.6881907528502,-61.3152906961552,
-232.528985905911));
#201142=CARTESIAN_POINT('Ctrl Pts',(-26.3822204946216,-61.8121578773183,
-231.74248442401));
#201143=CARTESIAN_POINT('Ctrl Pts',(-27.0762463009327,-62.3090257464567,
-230.955980624069));
#201144=CARTESIAN_POINT('Ctrl Pts',(-27.7702721072438,-62.8058936155951,
-230.169476824128));
#201145=CARTESIAN_POINT('Ctrl Pts',(-28.4642939595846,-63.3027621809775,
-229.382970695078));
#201146=CARTESIAN_POINT('Ctrl Pts',(-29.1583128779801,-63.7996309859099,
-228.596462846723));
#201147=CARTESIAN_POINT('Ctrl Pts',(-30.5463507147712,-64.7933685957745,
-227.023447150014));
#201148=CARTESIAN_POINT('Ctrl Pts',(-31.9343769856396,-65.7871070878229,
-225.450424677593));
#201149=CARTESIAN_POINT('Ctrl Pts',(-33.3223964166864,-66.7808443446069,
-223.877398255344));
#201150=CARTESIAN_POINT('Ctrl Pts',(-36.0984352787801,-68.768318858175,
-220.731345410844));
#201151=CARTESIAN_POINT('Ctrl Pts',(-38.8744474110663,-70.7557881486592,
-217.585277143015));
#201152=CARTESIAN_POINT('Ctrl Pts',(-41.6504481618404,-72.7432453287128,
-214.439202637353));
#201153=CARTESIAN_POINT('Ctrl Pts',(-24.9744025307133,-60.8143487212353,
-233.322986925177));
#201154=CARTESIAN_POINT('Ctrl Pts',(-25.6670491804662,-61.3113173869818,
-232.536442059561));
#201155=CARTESIAN_POINT('Ctrl Pts',(-26.3596977749792,-61.8082844221729,
-231.749898382092));
#201156=CARTESIAN_POINT('Ctrl Pts',(-27.0523477402915,-62.3052500852752,
-230.96335555072));
#201157=CARTESIAN_POINT('Ctrl Pts',(-27.7449977056038,-62.8022157483775,
-230.176812719347));
#201158=CARTESIAN_POINT('Ctrl Pts',(-28.4376490490292,-63.2991800360968,
-229.390270738434));
#201159=CARTESIAN_POINT('Ctrl Pts',(-29.1303013990492,-63.7961431156999,
-228.603729386647));
#201160=CARTESIAN_POINT('Ctrl Pts',(-30.5156060990893,-64.7900692749063,
-227.030646683075));
#201161=CARTESIAN_POINT('Ctrl Pts',(-31.9009147636639,-65.7839906295158,
-225.45756645914));
#201162=CARTESIAN_POINT('Ctrl Pts',(-33.2862256991509,-66.777907941617,
-223.884487706564));
#201163=CARTESIAN_POINT('Ctrl Pts',(-36.0568475701252,-68.7657425658195,
-220.738330201412));
#201164=CARTESIAN_POINT('Ctrl Pts',(-38.827478307619,-70.7535611178629,
-217.592178452254));
#201165=CARTESIAN_POINT('Ctrl Pts',(-41.5981125175426,-72.7413660196969,
-214.446029255158));
#201166=CARTESIAN_POINT('Ctrl Pts',(-24.96452603429,-60.8123106330865,-233.326738316813));
#201167=CARTESIAN_POINT('Ctrl Pts',(-25.6564783942742,-61.3093307323952,
-232.540170136386));
#201168=CARTESIAN_POINT('Ctrl Pts',(-26.3484364151579,-61.8063476946002,
-231.753605361133));
#201169=CARTESIAN_POINT('Ctrl Pts',(-27.0403984599708,-62.3033622546844,
-230.967043014045));
#201170=CARTESIAN_POINT('Ctrl Pts',(-27.7323605047837,-62.8003768147686,
-230.180480666957));
#201171=CARTESIAN_POINT('Ctrl Pts',(-28.4243265937515,-63.2973889636564,
-229.393920760111));
#201172=CARTESIAN_POINT('Ctrl Pts',(-29.1162956595838,-63.794399180595,
-228.607362656609));
#201173=CARTESIAN_POINT('Ctrl Pts',(-30.5002337912484,-64.7884196144722,
-227.034246449605));
#201174=CARTESIAN_POINT('Ctrl Pts',(-31.8841836526759,-65.7824324003622,
-225.461137349913));
#201175=CARTESIAN_POINT('Ctrl Pts',(-33.2681403403832,-66.7764397401221,
-223.888032432174));
#201176=CARTESIAN_POINT('Ctrl Pts',(-36.0360537157978,-68.7644544196418,
-220.741822596696));
#201177=CARTESIAN_POINT('Ctrl Pts',(-38.8039937558954,-70.7524476024647,
-217.595629106873));
#201178=CARTESIAN_POINT('Ctrl Pts',(-41.5719446953938,-72.740426365189,
-214.449442564061));
#201179=CARTESIAN_POINT('Ctrl Pts',(-24.9541490838557,-60.8102778631162,
-233.330474075949));
#201180=CARTESIAN_POINT('Ctrl Pts',(-25.6454401441992,-61.307345800731,
-232.543880802852));
#201181=CARTESIAN_POINT('Ctrl Pts',(-26.3367401731056,-61.8044093273887,
-231.757292929005));
#201182=CARTESIAN_POINT('Ctrl Pts',(-27.0280467391398,-62.3014695196208,
-230.970708996412));
#201183=CARTESIAN_POINT('Ctrl Pts',(-27.719353305174,-62.7985297118529,
-230.18412506382));
#201184=CARTESIAN_POINT('Ctrl Pts',(-28.4106664345268,-63.2955865581015,
-229.397545088212));
#201185=CARTESIAN_POINT('Ctrl Pts',(-29.1019844928396,-63.7926407824983,
-228.610968089891));
#201186=CARTESIAN_POINT('Ctrl Pts',(-30.4846206094652,-64.7867492312918,
-227.037814093248));
#201187=CARTESIAN_POINT('Ctrl Pts',(-31.8672761708201,-65.7808473127859,
-225.464671843211));
#201188=CARTESIAN_POINT('Ctrl Pts',(-33.2499434120597,-66.7749384699927,
-223.891536687223));
#201189=CARTESIAN_POINT('Ctrl Pts',(-36.0152778945389,-68.7631207844063,
-220.745266375246));
#201190=CARTESIAN_POINT('Ctrl Pts',(-38.7806580129467,-70.7512758829813,
-217.599023790475));
#201191=CARTESIAN_POINT('Ctrl Pts',(-41.5460576771974,-72.7394153448676,
-214.45279331175));
#201192=CARTESIAN_POINT('Ctrl Pts',(-24.9431675857188,-60.8082654676189,
-233.334164524199));
#201193=CARTESIAN_POINT('Ctrl Pts',(-25.6338346604351,-61.3053771897629,
-232.547545996672));
#201194=CARTESIAN_POINT('Ctrl Pts',(-26.3245132764945,-61.8024835845448,
-231.760934436748));
#201195=CARTESIAN_POINT('Ctrl Pts',(-27.0152005013104,-62.2995859346266,
-230.97432807854));
#201196=CARTESIAN_POINT('Ctrl Pts',(-27.7058877261263,-62.7966882847084,
-230.187721720333));
#201197=CARTESIAN_POINT('Ctrl Pts',(-28.3965835877948,-63.2937865778419,
-229.401120580787));
#201198=CARTESIAN_POINT('Ctrl Pts',(-29.0872860637793,-63.7908816992324,
-228.614523442413));
#201199=CARTESIAN_POINT('Ctrl Pts',(-30.4686910157482,-64.7850719420134,
-227.041329165664));
#201200=CARTESIAN_POINT('Ctrl Pts',(-31.8501220936262,-65.7792496428099,
-225.468150694098));
#201201=CARTESIAN_POINT('Ctrl Pts',(-33.231569388313,-66.7734191417836,
-223.894982065188));
#201202=CARTESIAN_POINT('Ctrl Pts',(-35.9944639776866,-68.7617581397308,
-220.748644807367));
#201203=CARTESIAN_POINT('Ctrl Pts',(-38.7574219835962,-70.7500649666192,
-217.602346047653));
#201204=CARTESIAN_POINT('Ctrl Pts',(-41.5204085705364,-72.7383548951067,
-214.45606483788));
#201205=CARTESIAN_POINT('Ctrl Pts',(-24.9376768366503,-60.8072592698702,
-233.336009748324));
#201206=CARTESIAN_POINT('Ctrl Pts',(-25.6280319185531,-61.3043928842789,
-232.549378593582));
#201207=CARTESIAN_POINT('Ctrl Pts',(-26.318399828189,-61.8015207131228,
-231.762755190619));
#201208=CARTESIAN_POINT('Ctrl Pts',(-27.0087773823957,-62.2986441421295,
-230.976137619604));
#201209=CARTESIAN_POINT('Ctrl Pts',(-27.6991549366024,-62.7957675711362,
-230.189520048589));
#201210=CARTESIAN_POINT('Ctrl Pts',(-28.3895421644288,-63.2928865877122,
-229.402908327074));
#201211=CARTESIAN_POINT('Ctrl Pts',(-29.0799368492491,-63.7900021575995,
-228.616301118674));
#201212=CARTESIAN_POINT('Ctrl Pts',(-30.4607262188897,-64.7842332973742,
-227.043086701871));
#201213=CARTESIAN_POINT('Ctrl Pts',(-31.8415450550293,-65.778450807822,
-225.469890119541));
#201214=CARTESIAN_POINT('Ctrl Pts',(-33.2223823764397,-66.772659477679,
-223.89670475417));
#201215=CARTESIAN_POINT('Ctrl Pts',(-35.9840570192604,-68.7610768173931,
-220.750334023428));
#201216=CARTESIAN_POINT('Ctrl Pts',(-38.7458039689211,-70.7494595084382,
-217.604007176241));
#201217=CARTESIAN_POINT('Ctrl Pts',(-41.5075840172059,-72.7378246702262,
-214.457700600944));
#201218=CARTESIAN_POINT('Ctrl Pts',(-24.9320351560731,-60.8062580406183,
-233.337843753845));
#201219=CARTESIAN_POINT('Ctrl Pts',(-25.6220875425827,-61.3034125499849,
-232.551199913808));
#201220=CARTESIAN_POINT('Ctrl Pts',(-26.312153866782,-61.8005609014255,
-231.764564507522));
#201221=CARTESIAN_POINT('Ctrl Pts',(-27.0022307652976,-62.2977045512317,
-230.977935502733));
#201222=CARTESIAN_POINT('Ctrl Pts',(-27.6923076638132,-62.794848201038,
-230.191306497943));
#201223=CARTESIAN_POINT('Ctrl Pts',(-28.3823951656622,-63.2919871367077,
-229.404683912223));
#201224=CARTESIAN_POINT('Ctrl Pts',(-29.0724909030316,-63.7891223844269,
-228.618066315475));
#201225=CARTESIAN_POINT('Ctrl Pts',(-30.4526823777702,-64.7833928798651,
-227.044831121978));
#201226=CARTESIAN_POINT('Ctrl Pts',(-31.8329064109243,-65.7776487896842,
-225.471615652582));
#201227=CARTESIAN_POINT('Ctrl Pts',(-33.2131511215727,-66.7718952685571,
-223.898412735151));
#201228=CARTESIAN_POINT('Ctrl Pts',(-35.9736405428697,-68.7603882263028,
-220.752006900292));
#201229=CARTESIAN_POINT('Ctrl Pts',(-38.7342108749039,-70.7488442420639,
-217.605650187832));
#201230=CARTESIAN_POINT('Ctrl Pts',(-41.4948189193303,-72.737282086382,
-214.459316539654));
#201231=CARTESIAN_POINT('Ctrl Pts',(-24.9262307371789,-60.8052629613404,
-233.339663481057));
#201232=CARTESIAN_POINT('Ctrl Pts',(-25.6159901042832,-61.3024373924278,
-232.553007006783));
#201233=CARTESIAN_POINT('Ctrl Pts',(-26.3057643351287,-61.7996053791141,
-231.766359540212));
#201234=CARTESIAN_POINT('Ctrl Pts',(-26.9955499476215,-62.2967684208872,
-230.979718973407));
#201235=CARTESIAN_POINT('Ctrl Pts',(-27.6853355601145,-62.7939314626603,
-230.193078406603));
#201236=CARTESIAN_POINT('Ctrl Pts',(-28.3751325826488,-63.2910895473583,
-229.406444756795));
#201237=CARTESIAN_POINT('Ctrl Pts',(-29.0649385371855,-63.7882437431482,
-228.619816524538));
#201238=CARTESIAN_POINT('Ctrl Pts',(-30.4445504462589,-64.7825521347279,
-227.046560060024));
#201239=CARTESIAN_POINT('Ctrl Pts',(-31.8241976850135,-65.7768451422546,
-225.473325024605));
#201240=CARTESIAN_POINT('Ctrl Pts',(-33.2038676569546,-66.7711282018108,
-223.90010380027));
#201241=CARTESIAN_POINT('Ctrl Pts',(-35.9632076008367,-68.7596943209232,
-220.753661351601));
#201242=CARTESIAN_POINT('Ctrl Pts',(-38.7226365397166,-70.7482214856064,
-217.607272976111));
#201243=CARTESIAN_POINT('Ctrl Pts',(-41.4821077889028,-72.7367298763208,
-214.460910461991));
#201244=CARTESIAN_POINT('Ctrl Pts',(-24.9204263182847,-60.8042678820624,
-233.341483208271));
#201245=CARTESIAN_POINT('Ctrl Pts',(-25.6098926659838,-61.3014622348707,
-232.554814099759));
#201246=CARTESIAN_POINT('Ctrl Pts',(-26.2993748034754,-61.7986498568027,
-231.768154572902));
#201247=CARTESIAN_POINT('Ctrl Pts',(-26.9888691299455,-62.2958322905427,
-230.981502444082));
#201248=CARTESIAN_POINT('Ctrl Pts',(-27.6783634564157,-62.7930147242826,
-230.194850315263));
#201249=CARTESIAN_POINT('Ctrl Pts',(-28.3678699996353,-63.2901919580089,
-229.408205601368));
#201250=CARTESIAN_POINT('Ctrl Pts',(-29.0573861713395,-63.7873651018695,
-228.621566733601));
#201251=CARTESIAN_POINT('Ctrl Pts',(-30.4364185147476,-64.7817113895908,
-227.048288998068));
#201252=CARTESIAN_POINT('Ctrl Pts',(-31.8154889591027,-65.776041494825,
-225.475034396628));
#201253=CARTESIAN_POINT('Ctrl Pts',(-33.1945841923364,-66.7703611350645,
-223.901794865388));
#201254=CARTESIAN_POINT('Ctrl Pts',(-35.9527746588037,-68.7590004155436,
-220.755315802909));
#201255=CARTESIAN_POINT('Ctrl Pts',(-38.7110622045295,-70.7475987291489,
-217.608895764391));
#201256=CARTESIAN_POINT('Ctrl Pts',(-41.4693966584753,-72.7361776662597,
-214.462504384327));
#201257=CARTESIAN_POINT('Ctrl Pts',(-24.9106027465158,-60.8049715273879,
-233.340948124015));
#201258=CARTESIAN_POINT('Ctrl Pts',(-25.5998098315156,-61.3021744082037,
-232.554282687331));
#201259=CARTESIAN_POINT('Ctrl Pts',(-26.2890324103538,-61.7993707608737,
-231.767626642701));
#201260=CARTESIAN_POINT('Ctrl Pts',(-26.9782669268481,-62.2965621103122,
-230.980977835653));
#201261=CARTESIAN_POINT('Ctrl Pts',(-27.6675014433422,-62.7937534597507,
-230.194329028605));
#201262=CARTESIAN_POINT('Ctrl Pts',(-28.3567479253494,-63.2909397940828,
-229.407687476061));
#201263=CARTESIAN_POINT('Ctrl Pts',(-29.0460038234333,-63.7881222076912,
-228.621051634203));
#201264=CARTESIAN_POINT('Ctrl Pts',(-30.424515619601,-64.7824870349079,
-227.047779950486));
#201265=CARTESIAN_POINT('Ctrl Pts',(-31.8030646725822,-65.776836354002,
-225.474530862664));
#201266=CARTESIAN_POINT('Ctrl Pts',(-33.1816379091815,-66.771175783969,
-223.901296458627));
#201267=CARTESIAN_POINT('Ctrl Pts',(-35.9387843823801,-68.759854643903,
-220.754827650554));
#201268=CARTESIAN_POINT('Ctrl Pts',(-38.6960255585086,-70.7484948217514,
-217.608416348934));
#201269=CARTESIAN_POINT('Ctrl Pts',(-41.4533123673286,-72.737117447414,
-214.462032879015));
#201270=CARTESIAN_POINT('Ctrl Pts',(-24.9017054131522,-60.8052918727755,
-233.340945144186));
#201271=CARTESIAN_POINT('Ctrl Pts',(-25.5906443745351,-61.3025059726095,
-232.554279700873));
#201272=CARTESIAN_POINT('Ctrl Pts',(-26.2795988326832,-61.7997136258234,
-231.767623645885));
#201273=CARTESIAN_POINT('Ctrl Pts',(-26.9685652314336,-62.2969163567666,
-230.980974825615));
#201274=CARTESIAN_POINT('Ctrl Pts',(-27.6575316301841,-62.7941190877098,
-230.194326005343));
#201275=CARTESIAN_POINT('Ctrl Pts',(-28.346509997394,-63.2913168845119,
-229.407684436704));
#201276=CARTESIAN_POINT('Ctrl Pts',(-29.0354977836505,-63.7885108411498,
-228.621048576497));
#201277=CARTESIAN_POINT('Ctrl Pts',(-30.4134733561636,-64.7828987544258,
-227.047776856082));
#201278=CARTESIAN_POINT('Ctrl Pts',(-31.7914861973683,-65.7772714817533,
-225.474527722644));
#201279=CARTESIAN_POINT('Ctrl Pts',(-33.1695232342839,-66.7716346400439,
-223.90129326724));
#201280=CARTESIAN_POINT('Ctrl Pts',(-35.925597308115,-68.7603609566252,
-220.754824356431));
#201281=CARTESIAN_POINT('Ctrl Pts',(-38.6817661332381,-70.749049871159,
-217.608412929565));
#201282=CARTESIAN_POINT('Ctrl Pts',(-41.437980641355,-72.7377225056729,
-214.462029323759));
#201283=CARTESIAN_POINT('',(-26.5827141673278,-60.7444095340058,-232.85005));
#201284=CARTESIAN_POINT('',(-25.3523897646956,-61.114818041723,-232.850050017304));
#201285=CARTESIAN_POINT('Ctrl Pts',(-26.5827141673278,-60.7444095340058,
-232.85005));
#201286=CARTESIAN_POINT('Ctrl Pts',(-26.5523883211155,-60.7606145810421,
-232.85005));
#201287=CARTESIAN_POINT('Ctrl Pts',(-26.5182436214773,-60.7785813873836,
-232.85005));
#201288=CARTESIAN_POINT('Ctrl Pts',(-26.4690256747712,-60.8033306143011,
-232.85005));
#201289=CARTESIAN_POINT('Ctrl Pts',(-26.4527133286803,-60.8112699859099,
-232.850050000173));
#201290=CARTESIAN_POINT('Ctrl Pts',(-26.3977210282154,-60.8370309306803,
-232.850050000173));
#201291=CARTESIAN_POINT('Ctrl Pts',(-26.3580453525237,-60.8538506884452,
-232.85005));
#201292=CARTESIAN_POINT('Ctrl Pts',(-26.2130644838343,-60.9164277579278,
-232.85005));
#201293=CARTESIAN_POINT('Ctrl Pts',(-26.1545198953832,-60.9398574595328,
-232.85005));
#201294=CARTESIAN_POINT('Ctrl Pts',(-26.0680132927756,-60.971650599673,
-232.85005));
#201295=CARTESIAN_POINT('Ctrl Pts',(-26.0182912512482,-60.9885178579036,
-232.850050000019));
#201296=CARTESIAN_POINT('Ctrl Pts',(-25.9539874352103,-61.0096287447273,
-232.850050000019));
#201297=CARTESIAN_POINT('Ctrl Pts',(-25.9240201650144,-61.019154825783,
-232.85005));
#201298=CARTESIAN_POINT('Ctrl Pts',(-25.8612333031519,-61.0378499416973,
-232.85005));
#201299=CARTESIAN_POINT('Ctrl Pts',(-25.8258381809542,-61.047112084847,
-232.85005));
#201300=CARTESIAN_POINT('Ctrl Pts',(-25.7621933691786,-61.0617509830125,
-232.85005));
#201301=CARTESIAN_POINT('Ctrl Pts',(-25.7424556613749,-61.0661234399878,
-232.850049999971));
#201302=CARTESIAN_POINT('Ctrl Pts',(-25.6672523478798,-61.0820029852263,
-232.850049999971));
#201303=CARTESIAN_POINT('Ctrl Pts',(-25.6192423246462,-61.0902478978104,
-232.850050000018));
#201304=CARTESIAN_POINT('Ctrl Pts',(-25.528905053629,-61.1015857089327,
-232.850050000018));
#201305=CARTESIAN_POINT('Ctrl Pts',(-25.4898697688722,-61.1058736055181,
-232.85005));
#201306=CARTESIAN_POINT('Ctrl Pts',(-25.4126689239331,-61.1125397549223,
-232.85005));
#201307=CARTESIAN_POINT('Ctrl Pts',(-25.3781594362844,-61.1138848746439,
-232.85005));
#201308=CARTESIAN_POINT('Ctrl Pts',(-25.3523897698351,-61.1148181836303,
-232.85005));
#201309=CARTESIAN_POINT('',(-46.8664918972107,-70.8820281131858,-214.224994829282));
#201310=CARTESIAN_POINT('Ctrl Pts',(-26.5827166022082,-60.7444082350379,
-232.85005));
#201311=CARTESIAN_POINT('Ctrl Pts',(-27.4045094191061,-61.1514998298357,
-232.097461865351));
#201312=CARTESIAN_POINT('Ctrl Pts',(-28.2261252496076,-61.5588361613065,
-231.344818757035));
#201313=CARTESIAN_POINT('Ctrl Pts',(-29.9098798269229,-62.3943471342904,
-229.801945520923));
#201314=CARTESIAN_POINT('Ctrl Pts',(-30.7719992818189,-62.8225494262878,
-229.011709845571));
#201315=CARTESIAN_POINT('Ctrl Pts',(-33.3576883801732,-64.1081568139303,
-226.640829838263));
#201316=CARTESIAN_POINT('Ctrl Pts',(-35.0805895061186,-64.9665572155428,
-225.060010587065));
#201317=CARTESIAN_POINT('Ctrl Pts',(-40.1613675899462,-67.5043536465696,
-220.39488359422));
#201318=CARTESIAN_POINT('Ctrl Pts',(-43.5163811847326,-69.1882952855583,
-217.309957960225));
#201319=CARTESIAN_POINT('Ctrl Pts',(-46.8664918972107,-70.8820281131858,
-214.224994829282));
#201320=CARTESIAN_POINT('',(-41.8937014876592,-72.6456596144325,-214.55018589167));
#201321=CARTESIAN_POINT('Ctrl Pts',(-46.8664918907845,-70.8820281261857,
-214.224994454969));
#201322=CARTESIAN_POINT('Ctrl Pts',(-46.7744407826033,-70.9511131613608,
-214.228242207603));
#201323=CARTESIAN_POINT('Ctrl Pts',(-46.680727279368,-71.0186224423001,
-214.231828155425));
#201324=CARTESIAN_POINT('Ctrl Pts',(-46.5495229902255,-71.1092838966998,
-214.237663532247));
#201325=CARTESIAN_POINT('Ctrl Pts',(-46.5126373769831,-71.1343646694262,
-214.239393263808));
#201326=CARTESIAN_POINT('Ctrl Pts',(-46.3057923036224,-71.2726997131669,
-214.249757794819));
#201327=CARTESIAN_POINT('Ctrl Pts',(-46.1254151593501,-71.3847351190163,
-214.258939730943));
#201328=CARTESIAN_POINT('Ctrl Pts',(-45.7687595214659,-71.5880113826264,
-214.27689821422));
#201329=CARTESIAN_POINT('Ctrl Pts',(-45.5977961983387,-71.6781131955288,
-214.286477772573));
#201330=CARTESIAN_POINT('Ctrl Pts',(-45.3185014968499,-71.8138089272529,
-214.303180439003));
#201331=CARTESIAN_POINT('Ctrl Pts',(-45.2120152032011,-71.8629654501139,
-214.309490070308));
#201332=CARTESIAN_POINT('Ctrl Pts',(-45.046199455701,-71.935548692169,-214.319240105057));
#201333=CARTESIAN_POINT('Ctrl Pts',(-44.9874097476947,-71.9605279868894,
-214.322717043323));
#201334=CARTESIAN_POINT('Ctrl Pts',(-44.7920434623916,-72.0410490489618,
-214.334469550289));
#201335=CARTESIAN_POINT('Ctrl Pts',(-44.6545819295426,-72.0937224742825,
-214.343103618652));
#201336=CARTESIAN_POINT('Ctrl Pts',(-44.0770061022199,-72.298643730271,
-214.380774049869));
#201337=CARTESIAN_POINT('Ctrl Pts',(-43.6246516197569,-72.4199541122146,
-214.411162580962));
#201338=CARTESIAN_POINT('Ctrl Pts',(-43.0535644966474,-72.5255358982375,
-214.454758498776));
#201339=CARTESIAN_POINT('Ctrl Pts',(-42.9403769882396,-72.5441841202125,
-214.463730404288));
#201340=CARTESIAN_POINT('Ctrl Pts',(-42.7453484949782,-72.5724398999914,
-214.479262989124));
#201341=CARTESIAN_POINT('Ctrl Pts',(-42.663500340452,-72.5831344326424,
-214.485726488472));
#201342=CARTESIAN_POINT('Ctrl Pts',(-42.3528138938661,-72.6193128180556,
-214.510537926913));
#201343=CARTESIAN_POINT('Ctrl Pts',(-42.123906167336,-72.6369493090122,
-214.52972492121));
#201344=CARTESIAN_POINT('Ctrl Pts',(-41.8937014876739,-72.6456596144296,
-214.550185891837));
#201345=CARTESIAN_POINT('',(-41.3748964727292,-72.6655519634609,-214.574036901741));
#201346=CARTESIAN_POINT('Ctrl Pts',(-41.8937014876741,-72.6456596144277,
-214.55018589184));
#201347=CARTESIAN_POINT('Ctrl Pts',(-41.8073293516378,-72.6489276960371,
-214.557862789404));
#201348=CARTESIAN_POINT('Ctrl Pts',(-41.7213837775228,-72.6521985331045,
-214.563823000958));
#201349=CARTESIAN_POINT('Ctrl Pts',(-41.5899590748613,-72.6572360335019,
-214.569961528013));
#201350=CARTESIAN_POINT('Ctrl Pts',(-41.5458704327232,-72.6589321169506,
-214.571508890137));
#201351=CARTESIAN_POINT('Ctrl Pts',(-41.4802081830395,-72.6614677335481,
-214.573029139169));
#201352=CARTESIAN_POINT('Ctrl Pts',(-41.4590018913533,-72.6622881096249,
-214.573399452815));
#201353=CARTESIAN_POINT('Ctrl Pts',(-41.4169705066586,-72.6639170467841,
-214.573893334939));
#201354=CARTESIAN_POINT('Ctrl Pts',(-41.4044675732566,-72.6644020926304,
-214.574005833637));
#201355=CARTESIAN_POINT('Ctrl Pts',(-41.3748964708024,-72.6655518905447,
-214.574037743505));
#201356=CARTESIAN_POINT('Ctrl Pts',(-25.3523897720292,-61.114817956777,
-232.850049970045));
#201357=CARTESIAN_POINT('Ctrl Pts',(-30.6926995480076,-64.965287483333,
-226.757725855014));
#201358=CARTESIAN_POINT('Ctrl Pts',(-36.0337490039693,-68.8154400690564,
-220.665850944208));
#201359=CARTESIAN_POINT('Ctrl Pts',(-41.3748962564069,-72.665551761209,
-214.574036584249));
#201360=CARTESIAN_POINT('Ctrl Pts',(-27.4675166955088,36.501209334595,-233.2699618027));
#201361=CARTESIAN_POINT('Ctrl Pts',(-28.0986597880893,36.9344896240505,
-232.484645254214));
#201362=CARTESIAN_POINT('Ctrl Pts',(-28.7300030462673,37.3676977230337,
-231.69945191414));
#201363=CARTESIAN_POINT('Ctrl Pts',(-29.3615087464634,37.8008474937043,
-230.914358703846));
#201364=CARTESIAN_POINT('Ctrl Pts',(-29.9930144466596,38.2339972643749,
-230.129265493552));
#201365=CARTESIAN_POINT('Ctrl Pts',(-30.624682800611,38.6670886387032,-229.344272547955));
#201366=CARTESIAN_POINT('Ctrl Pts',(-31.2564852375126,39.1001323034766,
-228.559362491382));
#201367=CARTESIAN_POINT('Ctrl Pts',(-32.5200901113159,39.9662196330235,
-226.989542378236));
#201368=CARTESIAN_POINT('Ctrl Pts',(-33.7842270188127,40.8321176985828,
-225.420051188828));
#201369=CARTESIAN_POINT('Ctrl Pts',(-35.0487393284727,41.6978863030865,
-223.850794334856));
#201370=CARTESIAN_POINT('Ctrl Pts',(-37.5777639477929,43.429423512094,-220.712280626913));
#201371=CARTESIAN_POINT('Ctrl Pts',(-40.1082645173074,45.1604528702306,
-217.574688874121));
#201372=CARTESIAN_POINT('Ctrl Pts',(-42.6395909737856,46.8912293280373,
-214.437630225606));
#201373=CARTESIAN_POINT('Ctrl Pts',(-27.5495579756445,36.5028921654741,
-233.251051919951));
#201374=CARTESIAN_POINT('Ctrl Pts',(-28.1827688115622,36.9359521258547,
-232.465366213753));
#201375=CARTESIAN_POINT('Ctrl Pts',(-28.8164085091962,37.3688162618127,
-231.679931708896));
#201376=CARTESIAN_POINT('Ctrl Pts',(-29.45037829501,37.8015234896747,-230.894689344989));
#201377=CARTESIAN_POINT('Ctrl Pts',(-30.0843480808238,38.2342307175367,
-230.109446981082));
#201378=CARTESIAN_POINT('Ctrl Pts',(-30.7186486771531,38.6667807943463,
-229.324397213218));
#201379=CARTESIAN_POINT('Ctrl Pts',(-31.3532086585038,39.0992026045944,
-228.539497756859));
#201380=CARTESIAN_POINT('Ctrl Pts',(-32.6223286212052,39.9640462250905,
-226.96969884414));
#201381=CARTESIAN_POINT('Ctrl Pts',(-33.8924746608402,40.828381296436,-225.400494315711));
#201382=CARTESIAN_POINT('Ctrl Pts',(-35.1632781294504,41.6923616886714,
-223.831668727949));
#201383=CARTESIAN_POINT('Ctrl Pts',(-37.7048850666709,43.4203224731419,
-220.694017552425));
#201384=CARTESIAN_POINT('Ctrl Pts',(-40.2490633538194,45.1468896454712,
-217.55784834607));
#201385=CARTESIAN_POINT('Ctrl Pts',(-42.7944274621604,46.8726693939935,
-214.42236887553));
#201386=CARTESIAN_POINT('Ctrl Pts',(-27.6055780256448,36.5084909217888,
-233.228921976304));
#201387=CARTESIAN_POINT('Ctrl Pts',(-28.2423304860859,36.9411059500847,
-232.442898411838));
#201388=CARTESIAN_POINT('Ctrl Pts',(-28.8798608338247,37.3733283098348,
-231.657313855381));
#201389=CARTESIAN_POINT('Ctrl Pts',(-29.5179264655878,37.8052614858298,
-230.87202778373));
#201390=CARTESIAN_POINT('Ctrl Pts',(-30.1559920973509,38.2371946618249,
-230.08674171208));
#201391=CARTESIAN_POINT('Ctrl Pts',(-30.7945950027779,38.6688382551504,
-229.301755452856));
#201392=CARTESIAN_POINT('Ctrl Pts',(-31.433575412527,39.1002648835096,-228.516978390142));
#201393=CARTESIAN_POINT('Ctrl Pts',(-32.7115362320255,39.9631181402278,
-226.947424264716));
#201394=CARTESIAN_POINT('Ctrl Pts',(-33.9909784660999,40.82511685855,-225.378690793586));
#201395=CARTESIAN_POINT('Ctrl Pts',(-35.2712022810355,41.6865965771103,
-223.810389502773));
#201396=CARTESIAN_POINT('Ctrl Pts',(-37.8316499109069,43.4095560142309,
-220.673786921149));
#201397=CARTESIAN_POINT('Ctrl Pts',(-40.3951430863757,45.1304838440415,
-217.53887071552));
#201398=CARTESIAN_POINT('Ctrl Pts',(-42.9596694236649,46.8503990616624,
-214.404555343614));
#201399=CARTESIAN_POINT('Ctrl Pts',(-27.6544884050101,36.5134544997187,
-233.208489782041));
#201400=CARTESIAN_POINT('Ctrl Pts',(-28.2958883125488,36.9453045586868,
-232.422071262426));
#201401=CARTESIAN_POINT('Ctrl Pts',(-28.9385402233851,37.3764580517972,
-231.636337934604));
#201402=CARTESIAN_POINT('Ctrl Pts',(-29.5819207190053,37.8071775310161,
-230.850998973988));
#201403=CARTESIAN_POINT('Ctrl Pts',(-30.2253012146256,38.2378970102351,
-230.065660013372));
#201404=CARTESIAN_POINT('Ctrl Pts',(-30.8694237090864,38.6681763110842,
-229.280723186985));
#201405=CARTESIAN_POINT('Ctrl Pts',(-31.5140148312165,39.0981569518477,
-228.496039104459));
#201406=CARTESIAN_POINT('Ctrl Pts',(-32.8031970754766,39.9581182333748,
-226.926670939409));
#201407=CARTESIAN_POINT('Ctrl Pts',(-34.094212486763,40.8169068877022,-225.358291458816));
#201408=CARTESIAN_POINT('Ctrl Pts',(-35.3860663228485,41.675053386644,-223.79036645522));
#201409=CARTESIAN_POINT('Ctrl Pts',(-37.9697739950195,43.3913463845276,
-220.654516448028));
#201410=CARTESIAN_POINT('Ctrl Pts',(-40.5567806505099,45.1051056979372,
-217.520458021817));
#201411=CARTESIAN_POINT('Ctrl Pts',(-43.1447063347815,46.8176414904025,
-214.386944837765));
#201412=CARTESIAN_POINT('Ctrl Pts',(-27.7033987843753,36.5184180776487,
-233.188057587778));
#201413=CARTESIAN_POINT('Ctrl Pts',(-28.3494461390117,36.9495031672888,
-232.401244113014));
#201414=CARTESIAN_POINT('Ctrl Pts',(-28.9972196129455,37.3795877937595,
-231.615362013826));
#201415=CARTESIAN_POINT('Ctrl Pts',(-29.6459149724228,37.8090935762025,
-230.829970164246));
#201416=CARTESIAN_POINT('Ctrl Pts',(-30.2946103319002,38.2385993586454,
-230.044578314665));
#201417=CARTESIAN_POINT('Ctrl Pts',(-30.944252415395,38.6675143670179,-229.259690921114));
#201418=CARTESIAN_POINT('Ctrl Pts',(-31.5944542499059,39.0960490201859,
-228.475099818776));
#201419=CARTESIAN_POINT('Ctrl Pts',(-32.8948579189276,39.9531183265218,
-226.905917614101));
#201420=CARTESIAN_POINT('Ctrl Pts',(-34.1974465074261,40.8086969168544,
-225.337892124046));
#201421=CARTESIAN_POINT('Ctrl Pts',(-35.5009303646614,41.6635101961778,
-223.770343407667));
#201422=CARTESIAN_POINT('Ctrl Pts',(-38.1078980791321,43.3731367548243,
-220.635245974907));
#201423=CARTESIAN_POINT('Ctrl Pts',(-40.7184182146441,45.0797275518329,
-217.502045328114));
#201424=CARTESIAN_POINT('Ctrl Pts',(-43.329743245898,46.7848839191427,-214.369334331916));
#201425=CARTESIAN_POINT('Ctrl Pts',(-27.7467504913837,36.5219322799631,
-233.170032188139));
#201426=CARTESIAN_POINT('Ctrl Pts',(-28.3985217181101,36.9519116209705,
-232.382753952573));
#201427=CARTESIAN_POINT('Ctrl Pts',(-29.0525419525678,37.3805207587552,
-231.59666656708));
#201428=CARTESIAN_POINT('Ctrl Pts',(-29.707648099349,37.8084119595345,-230.811147097123));
#201429=CARTESIAN_POINT('Ctrl Pts',(-30.3627542461301,38.2363031603138,
-230.025627627167));
#201430=CARTESIAN_POINT('Ctrl Pts',(-31.0189916736704,38.6634523908632,
-229.240701082927));
#201431=CARTESIAN_POINT('Ctrl Pts',(-31.6758577488396,39.0901500013781,
-228.456102690314));
#201432=CARTESIAN_POINT('Ctrl Pts',(-32.9895898991783,39.9435452224079,
-226.886905905089));
#201433=CARTESIAN_POINT('Ctrl Pts',(-34.305776607248,40.7951703456425,-225.318990914817));
#201434=CARTESIAN_POINT('Ctrl Pts',(-35.6228886941575,41.6459326221272,
-223.751565966636));
#201435=CARTESIAN_POINT('Ctrl Pts',(-38.2571128679763,43.3474571750966,
-220.616716070273));
#201436=CARTESIAN_POINT('Ctrl Pts',(-40.8950551389346,45.0455299408185,
-217.483839750893));
#201437=CARTESIAN_POINT('Ctrl Pts',(-43.5337367396124,46.7419641904284,
-214.351434639915));
#201438=CARTESIAN_POINT('Ctrl Pts',(-27.8054264163448,36.5146074937637,
-233.160277704479));
#201439=CARTESIAN_POINT('Ctrl Pts',(-28.4608655062395,36.9445884335815,
-232.371247983632));
#201440=CARTESIAN_POINT('Ctrl Pts',(-29.1196314139931,37.372514313029,-231.584005383938));
#201441=CARTESIAN_POINT('Ctrl Pts',(-29.7799261927146,37.7994041715398,
-230.797562749801));
#201442=CARTESIAN_POINT('Ctrl Pts',(-30.4402209714361,38.2262940300507,
-230.011120115663));
#201443=CARTESIAN_POINT('Ctrl Pts',(-31.1021216515676,38.6521081108545,
-229.225521863909));
#201444=CARTESIAN_POINT('Ctrl Pts',(-31.7648888134181,39.0772864601489,
-228.440373573626));
#201445=CARTESIAN_POINT('Ctrl Pts',(-33.090423137119,39.9276431587379,-226.87007699306));
#201446=CARTESIAN_POINT('Ctrl Pts',(-34.4193423302246,40.7755094860917,
-225.301539303434));
#201447=CARTESIAN_POINT('Ctrl Pts',(-35.7494892631586,41.6222215800908,
-223.73364023664));
#201448=CARTESIAN_POINT('Ctrl Pts',(-38.4097831290267,43.3156457680889,
-220.597842103052));
#201449=CARTESIAN_POINT('Ctrl Pts',(-41.0750442414306,45.0044380406571,
-217.464638507897));
#201450=CARTESIAN_POINT('Ctrl Pts',(-43.7412542098013,46.69118281627,-214.332014574282));
#201451=CARTESIAN_POINT('Ctrl Pts',(-27.864102341306,36.5072827075644,-233.150523220819));
#201452=CARTESIAN_POINT('Ctrl Pts',(-28.523209294369,36.9372652461925,-232.359742014691));
#201453=CARTESIAN_POINT('Ctrl Pts',(-29.1867208754184,37.3645078673026,
-231.571344200798));
#201454=CARTESIAN_POINT('Ctrl Pts',(-29.8522042860804,37.7903963835451,
-230.783978402477));
#201455=CARTESIAN_POINT('Ctrl Pts',(-30.5176876967423,38.2162848997876,
-229.996612604157));
#201456=CARTESIAN_POINT('Ctrl Pts',(-31.1852516294648,38.6407638308456,
-229.210342644892));
#201457=CARTESIAN_POINT('Ctrl Pts',(-31.8539198779964,39.0644229189197,
-228.424644456938));
#201458=CARTESIAN_POINT('Ctrl Pts',(-33.1912563750597,39.9117410950679,
-226.853248081031));
#201459=CARTESIAN_POINT('Ctrl Pts',(-34.532908053201,40.7558486265409,-225.284087692051));
#201460=CARTESIAN_POINT('Ctrl Pts',(-35.8760898321597,41.5985105380543,
-223.715714506644));
#201461=CARTESIAN_POINT('Ctrl Pts',(-38.5624533900771,43.2838343610812,
-220.578968135829));
#201462=CARTESIAN_POINT('Ctrl Pts',(-41.2550333439266,44.9633461404957,
-217.4454372649));
#201463=CARTESIAN_POINT('Ctrl Pts',(-43.9487716799902,46.6404014421116,
-214.312594508648));
#201464=CARTESIAN_POINT('Ctrl Pts',(-27.9190830878262,36.5008900102226,
-233.139346077501));
#201465=CARTESIAN_POINT('Ctrl Pts',(-28.5832756511028,36.9299347713319,
-232.34736702198));
#201466=CARTESIAN_POINT('Ctrl Pts',(-29.2527286972829,37.3556305517945,
-231.558257704261));
#201467=CARTESIAN_POINT('Ctrl Pts',(-29.9244591932939,37.7797083909036,
-230.770340230532));
#201468=CARTESIAN_POINT('Ctrl Pts',(-30.5961896893049,38.2037862300127,
-229.982422756802));
#201469=CARTESIAN_POINT('Ctrl Pts',(-31.270338006197,38.626174417356,-229.195781239181));
#201470=CARTESIAN_POINT('Ctrl Pts',(-31.945743753703,39.0475951547582,-228.409789029494));
#201471=CARTESIAN_POINT('Ctrl Pts',(-33.2965552487149,39.8904366295628,
-226.837804610121));
#201472=CARTESIAN_POINT('Ctrl Pts',(-34.6522827270746,40.7294895383089,
-225.268361443424));
#201473=CARTESIAN_POINT('Ctrl Pts',(-36.0097034880497,41.5668741114757,
-223.699782360708));
#201474=CARTESIAN_POINT('Ctrl Pts',(-38.7245450099999,43.2416432578092,
-220.56262419528));
#201475=CARTESIAN_POINT('Ctrl Pts',(-41.4463029811519,44.9096878836177,
-217.429019852247));
#201476=CARTESIAN_POINT('Ctrl Pts',(-44.169290550113,46.5749498873242,-214.296143159535));
#201477=CARTESIAN_POINT('Ctrl Pts',(-27.9635611001738,36.4990952898012,
-233.124907406577));
#201478=CARTESIAN_POINT('Ctrl Pts',(-28.6335193341731,36.9265762879192,
-232.332215621801));
#201479=CARTESIAN_POINT('Ctrl Pts',(-29.3093382993415,37.3501779403658,
-231.542719800075));
#201480=CARTESIAN_POINT('Ctrl Pts',(-29.9876295989316,37.7719445682467,
-230.754510440041));
#201481=CARTESIAN_POINT('Ctrl Pts',(-30.6659208985218,38.1937111961276,
-229.966301080007));
#201482=CARTESIAN_POINT('Ctrl Pts',(-31.346850346985,38.6135550182896,-229.179478141202));
#201483=CARTESIAN_POINT('Ctrl Pts',(-32.0291309789057,39.032311940978,-228.393348201459));
#201484=CARTESIAN_POINT('Ctrl Pts',(-33.3936922427472,39.869825786355,-226.821088321973));
#201485=CARTESIAN_POINT('Ctrl Pts',(-34.7635386549114,40.7030825753783,
-225.251542754464));
#201486=CARTESIAN_POINT('Ctrl Pts',(-36.1351659076718,41.5344930728638,
-223.682897927105));
#201487=CARTESIAN_POINT('Ctrl Pts',(-38.8784204131928,43.1973140678347,
-220.545608272386));
#201488=CARTESIAN_POINT('Ctrl Pts',(-41.6289795635766,44.8526757118206,
-217.412042386738));
#201489=CARTESIAN_POINT('Ctrl Pts',(-44.3807833059246,46.5049749771785,
-214.279216302521));
#201490=CARTESIAN_POINT('Ctrl Pts',(-28.0080391125216,36.4973005693799,
-233.110468735653));
#201491=CARTESIAN_POINT('Ctrl Pts',(-28.6837630172434,36.9232178045066,
-232.317064221622));
#201492=CARTESIAN_POINT('Ctrl Pts',(-29.3659479014001,37.344725328937,-231.527181895889));
#201493=CARTESIAN_POINT('Ctrl Pts',(-30.0508000045693,37.7641807455897,
-230.73868064955));
#201494=CARTESIAN_POINT('Ctrl Pts',(-30.7356521077386,38.1836361622425,
-229.950179403211));
#201495=CARTESIAN_POINT('Ctrl Pts',(-31.423362687773,38.6009356192233,-229.163175043223));
#201496=CARTESIAN_POINT('Ctrl Pts',(-32.1125182041085,39.0170287271978,
-228.376907373423));
#201497=CARTESIAN_POINT('Ctrl Pts',(-33.4908292367796,39.849214943147,-226.804372033824));
#201498=CARTESIAN_POINT('Ctrl Pts',(-34.8747945827483,40.6766756124477,
-225.234724065505));
#201499=CARTESIAN_POINT('Ctrl Pts',(-36.2606283272941,41.5021120342519,
-223.666013493501));
#201500=CARTESIAN_POINT('Ctrl Pts',(-39.0322958163857,43.1529848778602,
-220.528592349493));
#201501=CARTESIAN_POINT('Ctrl Pts',(-41.8116561460013,44.7956635400236,
-217.395064921228));
#201502=CARTESIAN_POINT('Ctrl Pts',(-44.5922760617361,46.4350000670329,
-214.262289445508));
#201503=CARTESIAN_POINT('Ctrl Pts',(-28.0494437864605,36.495141074799,-233.096611018152));
#201504=CARTESIAN_POINT('Ctrl Pts',(-28.7308360120535,36.9193190689171,
-232.302532895241));
#201505=CARTESIAN_POINT('Ctrl Pts',(-29.4192203432693,37.3385601524366,
-231.512266925172));
#201506=CARTESIAN_POINT('Ctrl Pts',(-30.1104565561833,37.7555228770627,
-230.723470216585));
#201507=CARTESIAN_POINT('Ctrl Pts',(-30.8016927690973,38.1724856016888,
-229.934673507997));
#201508=CARTESIAN_POINT('Ctrl Pts',(-31.4959930724453,38.5870515082353,
-229.147475500813));
#201509=CARTESIAN_POINT('Ctrl Pts',(-32.1918313004172,39.0002838036336,
-228.361056572999));
#201510=CARTESIAN_POINT('Ctrl Pts',(-33.5835077563608,39.82674839443,-226.788218717371));
#201511=CARTESIAN_POINT('Ctrl Pts',(-34.981204076813,40.6479886792153,-225.218435880259));
#201512=CARTESIAN_POINT('Ctrl Pts',(-36.3808689058395,41.4670086872456,
-223.649631412145));
#201513=CARTESIAN_POINT('Ctrl Pts',(-39.1801985638925,43.1050487033063,
-220.512022475916));
#201514=CARTESIAN_POINT('Ctrl Pts',(-41.9876501636135,44.7340917680141,
-217.378490005261));
#201515=CARTESIAN_POINT('Ctrl Pts',(-44.7964013528814,46.3594930633657,
-214.245731113265));
#201516=CARTESIAN_POINT('Ctrl Pts',(-28.0986638608654,36.4864396316355,
-233.086219707902));
#201517=CARTESIAN_POINT('Ctrl Pts',(-28.7855090882708,36.908671912885,-232.291339757935));
#201518=CARTESIAN_POINT('Ctrl Pts',(-29.4797969634702,37.3255148395588,
-231.50054713919));
#201519=CARTESIAN_POINT('Ctrl Pts',(-30.1771392417705,37.7398414336408,
-230.711331015122));
#201520=CARTESIAN_POINT('Ctrl Pts',(-30.8744815200707,38.1541680277229,
-229.922114891055));
#201521=CARTESIAN_POINT('Ctrl Pts',(-31.5751008302705,38.565853402466,-229.134613456395));
#201522=CARTESIAN_POINT('Ctrl Pts',(-32.2773697651967,38.9760615626091,
-228.347946926293));
#201523=CARTESIAN_POINT('Ctrl Pts',(-33.6819076350491,39.7964778828953,
-226.77461386609));
#201524=CARTESIAN_POINT('Ctrl Pts',(-35.092901360331,40.6111090059392,-225.204554400508));
#201525=CARTESIAN_POINT('Ctrl Pts',(-36.506013012055,41.4232755079927,-223.635540355772));
#201526=CARTESIAN_POINT('Ctrl Pts',(-39.3322363155031,43.0476085120996,
-220.4975122663));
#201527=CARTESIAN_POINT('Ctrl Pts',(-42.1671908002668,44.6619661512638,
-217.363841724096));
#201528=CARTESIAN_POINT('Ctrl Pts',(-45.0035463653253,46.2723209746968,
-214.23099286058));
#201529=CARTESIAN_POINT('Ctrl Pts',(-28.1478839352704,36.477738188472,-233.075828397652));
#201530=CARTESIAN_POINT('Ctrl Pts',(-28.8401821644882,36.8980247568529,
-232.280146620628));
#201531=CARTESIAN_POINT('Ctrl Pts',(-29.5403735836712,37.3124695266811,
-231.488827353208));
#201532=CARTESIAN_POINT('Ctrl Pts',(-30.2438219273577,37.724159990219,-230.69919181366));
#201533=CARTESIAN_POINT('Ctrl Pts',(-30.9472702710442,38.1358504537568,
-229.909556274112));
#201534=CARTESIAN_POINT('Ctrl Pts',(-31.6542085880957,38.5446552966966,
-229.121751411976));
#201535=CARTESIAN_POINT('Ctrl Pts',(-32.3629082299762,38.9518393215846,
-228.334837279587));
#201536=CARTESIAN_POINT('Ctrl Pts',(-33.7803075137374,39.7662073713606,
-226.761009014808));
#201537=CARTESIAN_POINT('Ctrl Pts',(-35.204598643849,40.5742293326632,-225.190672920757));
#201538=CARTESIAN_POINT('Ctrl Pts',(-36.6311571182707,41.3795423287398,
-223.621449299399));
#201539=CARTESIAN_POINT('Ctrl Pts',(-39.4842740671139,42.9901683208929,
-220.483002056683));
#201540=CARTESIAN_POINT('Ctrl Pts',(-42.3467314369201,44.5898405345135,
-217.349193442931));
#201541=CARTESIAN_POINT('Ctrl Pts',(-45.2106913777692,46.1851488860278,
-214.216254607896));
#201542=CARTESIAN_POINT('Ctrl Pts',(-28.2012732840083,36.4651498400409,
-233.067037777728));
#201543=CARTESIAN_POINT('Ctrl Pts',(-28.8990579728149,36.8831408843765,
-232.270578628329));
#201544=CARTESIAN_POINT('Ctrl Pts',(-29.6051083171889,37.2948838670021,
-231.478729287174));
#201545=CARTESIAN_POINT('Ctrl Pts',(-30.3146028640688,37.7036388348153,
-230.688668141709));
#201546=CARTESIAN_POINT('Ctrl Pts',(-31.0240974109487,38.1123938026283,
-229.898606996244));
#201547=CARTESIAN_POINT('Ctrl Pts',(-31.7372746006804,38.5180264505524,
-229.110487353379));
#201548=CARTESIAN_POINT('Ctrl Pts',(-32.4523194990151,38.9218935751344,
-228.323313754114));
#201549=CARTESIAN_POINT('Ctrl Pts',(-33.8824092956843,39.7296278242987,
-226.748966555583));
#201550=CARTESIAN_POINT('Ctrl Pts',(-35.3198051784721,40.5304514518755,
-225.178327508987));
#201551=CARTESIAN_POINT('Ctrl Pts',(-36.7596189263893,41.3283116061093,
-223.608870010882));
#201552=CARTESIAN_POINT('Ctrl Pts',(-39.6392464222237,42.9240319145765,
-220.469955014674));
#201553=CARTESIAN_POINT('Ctrl Pts',(-42.5288205943682,44.5077862844145,
-217.335965063606));
#201554=CARTESIAN_POINT('Ctrl Pts',(-45.4200071428167,46.0868030777345,
-214.202896281505));
#201555=CARTESIAN_POINT('Ctrl Pts',(-28.2536248719719,36.45164456484,-233.058476234802));
#201556=CARTESIAN_POINT('Ctrl Pts',(-28.956246064681,36.8674691193729,-232.261151946464));
#201557=CARTESIAN_POINT('Ctrl Pts',(-29.6674872789167,37.2766580792002,
-231.468687139439));
#201558=CARTESIAN_POINT('Ctrl Pts',(-30.3823793991597,37.6826022896234,
-230.678128469586));
#201559=CARTESIAN_POINT('Ctrl Pts',(-31.0972715194027,38.0885465000466,
-229.887569799732));
#201560=CARTESIAN_POINT('Ctrl Pts',(-31.8160539135098,38.4911129154006,
-229.099074756418));
#201561=CARTESIAN_POINT('Ctrl Pts',(-32.5368266733684,38.8917474183737,
-228.311589632248));
#201562=CARTESIAN_POINT('Ctrl Pts',(-33.9783721930855,39.6930164243198,
-226.736619383908));
#201563=CARTESIAN_POINT('Ctrl Pts',(-35.4277003933768,40.4867262619234,
-225.16560579597));
#201564=CARTESIAN_POINT('Ctrl Pts',(-36.8796336124663,41.2771645198602,
-223.595856775541));
#201565=CARTESIAN_POINT('Ctrl Pts',(-39.7835000506455,42.8580410357338,
-220.456358734683));
#201566=CARTESIAN_POINT('Ctrl Pts',(-42.6980566108585,44.4257389283559,
-217.322125580858));
#201567=CARTESIAN_POINT('Ctrl Pts',(-45.6143789670139,45.9882588716253,
-214.18887606046));
#201568=CARTESIAN_POINT('Ctrl Pts',(-28.3059764599357,36.4381392896391,
-233.049914691876));
#201569=CARTESIAN_POINT('Ctrl Pts',(-29.0134341565471,36.8517973543695,
-232.2517252646));
#201570=CARTESIAN_POINT('Ctrl Pts',(-29.7298662406445,37.2584322913983,
-231.458644991706));
#201571=CARTESIAN_POINT('Ctrl Pts',(-30.4501559342506,37.6615657444315,
-230.667588797462));
#201572=CARTESIAN_POINT('Ctrl Pts',(-31.1704456278568,38.0646991974648,
-229.876532603218));
#201573=CARTESIAN_POINT('Ctrl Pts',(-31.8948332263391,38.464199380249,-229.087662159456));
#201574=CARTESIAN_POINT('Ctrl Pts',(-32.6213338477217,38.8616012616129,
-228.299865510382));
#201575=CARTESIAN_POINT('Ctrl Pts',(-34.0743350904866,39.6564050243409,
-226.724272212234));
#201576=CARTESIAN_POINT('Ctrl Pts',(-35.5355956082815,40.4430010719712,
-225.152884082953));
#201577=CARTESIAN_POINT('Ctrl Pts',(-36.9996482985433,41.2260174336112,
-223.582843540199));
#201578=CARTESIAN_POINT('Ctrl Pts',(-39.9277536790671,42.792050156891,-220.442762454692));
#201579=CARTESIAN_POINT('Ctrl Pts',(-42.8672926273489,44.3436915722972,
-217.308286098109));
#201580=CARTESIAN_POINT('Ctrl Pts',(-45.8087507912112,45.889714665516,-214.174855839415));
#201581=CARTESIAN_POINT('Ctrl Pts',(-28.3519546381049,36.428499297722,-233.038801999823));
#201582=CARTESIAN_POINT('Ctrl Pts',(-29.0685651860499,36.8359598776144,
-232.242286479252));
#201583=CARTESIAN_POINT('Ctrl Pts',(-29.7920661546429,37.237805899639,-231.449720689388));
#201584=CARTESIAN_POINT('Ctrl Pts',(-30.5189980352994,37.6364573834381,
-230.658986703413));
#201585=CARTESIAN_POINT('Ctrl Pts',(-31.2459299159559,38.0351088672372,
-229.868252717438));
#201586=CARTESIAN_POINT('Ctrl Pts',(-31.9764124958348,38.4305023582899,
-229.079433957463));
#201587=CARTESIAN_POINT('Ctrl Pts',(-32.7088796298207,38.8238619301343,
-228.291635917502));
#201588=CARTESIAN_POINT('Ctrl Pts',(-34.1738138977924,39.6105810738233,
-226.716039837583));
#201589=CARTESIAN_POINT('Ctrl Pts',(-35.6464836269217,40.3893479405787,
-225.144422997191));
#201590=CARTESIAN_POINT('Ctrl Pts',(-37.122025520744,41.1643408760019,-223.574201356819));
#201591=CARTESIAN_POINT('Ctrl Pts',(-40.0731093083885,42.7143267468484,
-220.433758076075));
#201592=CARTESIAN_POINT('Ctrl Pts',(-43.0357115526382,44.2493386577901,
-217.298984924306));
#201593=CARTESIAN_POINT('Ctrl Pts',(-46.0004325581354,45.7782515470524,
-214.165346999843));
#201594=CARTESIAN_POINT('Ctrl Pts',(-28.404523824249,36.4142111160726,-233.028222391732));
#201595=CARTESIAN_POINT('Ctrl Pts',(-29.1296788023777,36.8148442685854,
-232.23397055258));
#201596=CARTESIAN_POINT('Ctrl Pts',(-29.8595774687733,37.2115210846296,
-231.442464211111));
#201597=CARTESIAN_POINT('Ctrl Pts',(-30.5921210784794,37.6056911614944,
-230.652400010517));
#201598=CARTESIAN_POINT('Ctrl Pts',(-31.3246646881855,37.9998612383593,
-229.862335809922));
#201599=CARTESIAN_POINT('Ctrl Pts',(-32.0599114204536,38.3914951944436,
-229.073755169551));
#201600=CARTESIAN_POINT('Ctrl Pts',(-32.7968044445028,38.7814033859296,
-228.286041512615));
#201601=CARTESIAN_POINT('Ctrl Pts',(-34.2705904926014,39.5612197689016,
-226.710614198745));
#201602=CARTESIAN_POINT('Ctrl Pts',(-35.7508066075144,40.334264217189,-225.138570075993));
#201603=CARTESIAN_POINT('Ctrl Pts',(-37.2337704007868,41.1036371719424,
-223.567901121106));
#201604=CARTESIAN_POINT('Ctrl Pts',(-40.1996979873318,42.6423830814493,
-220.426563211331));
#201605=CARTESIAN_POINT('Ctrl Pts',(-43.1764747241572,44.166666266985,-217.290698996916));
#201606=CARTESIAN_POINT('Ctrl Pts',(-46.1558000266483,45.6842043061087,
-214.156194672008));
#201607=CARTESIAN_POINT('Ctrl Pts',(-28.4570930103932,36.3999229344231,
-233.01764278364));
#201608=CARTESIAN_POINT('Ctrl Pts',(-29.1907924187055,36.7937286595564,
-232.225654625907));
#201609=CARTESIAN_POINT('Ctrl Pts',(-29.9270887829037,37.1852362696201,
-231.435207732835));
#201610=CARTESIAN_POINT('Ctrl Pts',(-30.6652441216594,37.5749249395508,
-230.645813317621));
#201611=CARTESIAN_POINT('Ctrl Pts',(-31.403399460415,37.9646136094813,-229.856418902407));
#201612=CARTESIAN_POINT('Ctrl Pts',(-32.1434103450723,38.3524880305972,
-229.06807638164));
#201613=CARTESIAN_POINT('Ctrl Pts',(-32.884729259185,38.7389448417248,-228.280447107729));
#201614=CARTESIAN_POINT('Ctrl Pts',(-34.3673670874105,39.5118584639798,
-226.705188559907));
#201615=CARTESIAN_POINT('Ctrl Pts',(-35.8551295881073,40.2791804937992,
-225.132717154794));
#201616=CARTESIAN_POINT('Ctrl Pts',(-37.3455152808298,41.0429334678829,
-223.561600885392));
#201617=CARTESIAN_POINT('Ctrl Pts',(-40.3262866662749,42.5704394160502,
-220.419368346588));
#201618=CARTESIAN_POINT('Ctrl Pts',(-43.3172378956761,44.0839938761798,
-217.282413069526));
#201619=CARTESIAN_POINT('Ctrl Pts',(-46.3111674951612,45.590157065165,-214.147042344173));
#201620=CARTESIAN_POINT('Ctrl Pts',(-28.5214435153128,36.3758121500046,
-233.010309376466));
#201621=CARTESIAN_POINT('Ctrl Pts',(-29.2597711912192,36.7652926192596,
-232.219435748514));
#201622=CARTESIAN_POINT('Ctrl Pts',(-29.9999412300851,37.1531174751436,
-231.429684565593));
#201623=CARTESIAN_POINT('Ctrl Pts',(-30.741464839369,37.539582297854,-230.640726768058));
#201624=CARTESIAN_POINT('Ctrl Pts',(-31.482988448653,37.9260471205643,-229.851768970523));
#201625=CARTESIAN_POINT('Ctrl Pts',(-32.2258698218865,38.3111507874138,
-229.063608073021));
#201626=CARTESIAN_POINT('Ctrl Pts',(-32.9697681692284,38.6951211034311,
-228.276025525187));
#201627=CARTESIAN_POINT('Ctrl Pts',(-34.4575648639124,39.4630617354659,
-226.700860429518));
#201628=CARTESIAN_POINT('Ctrl Pts',(-35.9493723068607,40.2265053230493,
-225.12797096096));
#201629=CARTESIAN_POINT('Ctrl Pts',(-37.4435195048015,40.9866952819017,
-223.556350656432));
#201630=CARTESIAN_POINT('Ctrl Pts',(-40.4318139006829,42.5070751996064,
-220.413110047378));
#201631=CARTESIAN_POINT('Ctrl Pts',(-43.4292180728484,44.0146569196856,
-217.274809144726));
#201632=CARTESIAN_POINT('Ctrl Pts',(-46.4299697523172,45.5143458457586,
-214.138325398592));
#201633=CARTESIAN_POINT('Ctrl Pts',(-28.5917373044541,36.3459190971896,
-233.004412799005));
#201634=CARTESIAN_POINT('Ctrl Pts',(-29.3336456870839,36.7317236596899,
-232.214541575288));
#201635=CARTESIAN_POINT('Ctrl Pts',(-30.0768533355596,37.1163079376712,
-231.425484075423));
#201636=CARTESIAN_POINT('Ctrl Pts',(-30.8210649438641,37.4998384795814,
-230.63703601277));
#201637=CARTESIAN_POINT('Ctrl Pts',(-31.5652765521686,37.8833690214916,
-229.848587950118));
#201638=CARTESIAN_POINT('Ctrl Pts',(-32.3104940183536,38.2658454573702,
-229.060750983011));
#201639=CARTESIAN_POINT('Ctrl Pts',(-33.056499757863,38.6474031071304,-228.273381017246));
#201640=CARTESIAN_POINT('Ctrl Pts',(-34.5485112368819,39.4105184066505,
-226.698641085717));
#201641=CARTESIAN_POINT('Ctrl Pts',(-36.0436413480666,40.1699780267802,
-225.125745165631));
#201642=CARTESIAN_POINT('Ctrl Pts',(-37.5407436150405,40.9265749496157,
-223.553976309726));
#201643=CARTESIAN_POINT('Ctrl Pts',(-40.5349481489884,42.439768795287,-220.410438597917));
#201644=CARTESIAN_POINT('Ctrl Pts',(-43.536857304037,43.9416524034681,-217.271298591679));
#201645=CARTESIAN_POINT('Ctrl Pts',(-46.5420263558244,45.4357480033572,
-214.134039310084));
#201646=CARTESIAN_POINT('Ctrl Pts',(-28.6268841990247,36.3309725707821,
-233.001464510274));
#201647=CARTESIAN_POINT('Ctrl Pts',(-29.3705829350163,36.7149391799052,
-232.212094488675));
#201648=CARTESIAN_POINT('Ctrl Pts',(-30.1153093882969,37.097903168935,-231.423383830337));
#201649=CARTESIAN_POINT('Ctrl Pts',(-30.8608649961116,37.4799665704452,
-230.635190635126));
#201650=CARTESIAN_POINT('Ctrl Pts',(-31.6064206039263,37.8620299719552,
-229.846997439915));
#201651=CARTESIAN_POINT('Ctrl Pts',(-32.3528061165871,38.2431927923484,
-229.059322438005));
#201652=CARTESIAN_POINT('Ctrl Pts',(-33.0998655521803,38.6235441089799,
-228.272058763276));
#201653=CARTESIAN_POINT('Ctrl Pts',(-34.5939844233666,39.3842467422428,
-226.697531413816));
#201654=CARTESIAN_POINT('Ctrl Pts',(-36.0907758686695,40.1417143786457,
-225.124632267967));
#201655=CARTESIAN_POINT('Ctrl Pts',(-37.5893556701601,40.8965147834728,
-223.552789136373));
#201656=CARTESIAN_POINT('Ctrl Pts',(-40.5865152731412,42.4061155931272,
-220.409102873187));
#201657=CARTESIAN_POINT('Ctrl Pts',(-43.5906769196312,43.9051501453593,
-217.269543315155));
#201658=CARTESIAN_POINT('Ctrl Pts',(-46.598054657578,45.3964490821564,-214.13189626583));
#201659=CARTESIAN_POINT('Ctrl Pts',(-28.6518975580342,36.3261811548597,
-232.993056797812));
#201660=CARTESIAN_POINT('Ctrl Pts',(-29.398737821756,36.7070015779651,-232.205034899571));
#201661=CARTESIAN_POINT('Ctrl Pts',(-30.1460916201158,37.0872237185874,
-231.417368861425));
#201662=CARTESIAN_POINT('Ctrl Pts',(-30.8939024648147,37.4668637098655,
-230.6300135554));
#201663=CARTESIAN_POINT('Ctrl Pts',(-31.6417133095137,37.8465037011437,
-229.842658249374));
#201664=CARTESIAN_POINT('Ctrl Pts',(-32.3899812257617,38.225561587839,-229.055613721231));
#201665=CARTESIAN_POINT('Ctrl Pts',(-33.1386550153031,38.6040547581662,
-228.268840529801));
#201666=CARTESIAN_POINT('Ctrl Pts',(-34.6360025943859,39.3610410988206,
-226.69529414694));
#201667=CARTESIAN_POINT('Ctrl Pts',(-36.1349692411245,40.1157684838324,
-225.122828814917));
#201668=CARTESIAN_POINT('Ctrl Pts',(-37.6352027617429,40.8683822730397,
-223.551187160683));
#201669=CARTESIAN_POINT('Ctrl Pts',(-40.6356698029797,42.3736098514546,
-220.407903852216));
#201670=CARTESIAN_POINT('Ctrl Pts',(-43.6411528261178,43.8703944217154,
-217.267871204892));
#201671=CARTESIAN_POINT('Ctrl Pts',(-46.6495816719042,45.3598482038711,
-214.129724170691));
#201672=CARTESIAN_POINT('Ctrl Pts',(-28.6836693563314,36.3172916302978,
-232.984586371767));
#201673=CARTESIAN_POINT('Ctrl Pts',(-29.4328038186657,36.6955273714839,
-232.197666951892));
#201674=CARTESIAN_POINT('Ctrl Pts',(-30.1821597301324,37.0733995616469,
-231.410933917807));
#201675=CARTESIAN_POINT('Ctrl Pts',(-30.9317206554361,37.4509071831741,
-230.624372601034));
#201676=CARTESIAN_POINT('Ctrl Pts',(-31.6812815807397,37.8284148047014,
-229.83781128426));
#201677=CARTESIAN_POINT('Ctrl Pts',(-32.4310475185464,38.2055578694789,
-229.051421689267));
#201678=CARTESIAN_POINT('Ctrl Pts',(-33.1810027512314,38.5823363130566,
-228.265190292231));
#201679=CARTESIAN_POINT('Ctrl Pts',(-34.6809132166015,39.3358932002121,
-226.69272749816));
#201680=CARTESIAN_POINT('Ctrl Pts',(-36.1815801312299,40.0879909915779,
-225.120896504533));
#201681=CARTESIAN_POINT('Ctrl Pts',(-37.6828865095192,40.8386380933409,
-223.549601777981));
#201682=CARTESIAN_POINT('Ctrl Pts',(-40.6854992660978,42.3399322968669,
-220.407012324875));
#201683=CARTESIAN_POINT('Ctrl Pts',(-43.6906591856765,43.835419294533,-217.266555597716));
#201684=CARTESIAN_POINT('Ctrl Pts',(-46.6975653758367,45.3252553963054,
-214.127639057046));
#201685=CARTESIAN_POINT('Ctrl Pts',(-28.7154411546286,36.3084021057357,
-232.976115945722));
#201686=CARTESIAN_POINT('Ctrl Pts',(-29.4668698155753,36.6840531650027,
-232.190299004213));
#201687=CARTESIAN_POINT('Ctrl Pts',(-30.2182278401491,37.0595754047064,
-231.404498974189));
#201688=CARTESIAN_POINT('Ctrl Pts',(-30.9695388460574,37.4349506564828,
-230.618731646667));
#201689=CARTESIAN_POINT('Ctrl Pts',(-31.7208498519656,37.8103259082591,
-229.832964319146));
#201690=CARTESIAN_POINT('Ctrl Pts',(-32.4721138113312,38.1855541511188,
-229.047229657302));
#201691=CARTESIAN_POINT('Ctrl Pts',(-33.2233504871597,38.560617867947,-228.261540054661));
#201692=CARTESIAN_POINT('Ctrl Pts',(-34.7258238388169,39.3107453016035,
-226.690160849379));
#201693=CARTESIAN_POINT('Ctrl Pts',(-36.2281910213353,40.0602134993234,
-225.11896419415));
#201694=CARTESIAN_POINT('Ctrl Pts',(-37.7305702572955,40.808893913642,-223.548016395278));
#201695=CARTESIAN_POINT('Ctrl Pts',(-40.7353287292159,42.3062547422792,
-220.406120797533));
#201696=CARTESIAN_POINT('Ctrl Pts',(-43.7401655452353,43.8004441673505,
-217.265239990539));
#201697=CARTESIAN_POINT('Ctrl Pts',(-46.7455490797692,45.2906625887397,
-214.1255539434));
#201698=CARTESIAN_POINT('Ctrl Pts',(-28.7546828535794,36.2946048538794,
-232.967923270373));
#201699=CARTESIAN_POINT('Ctrl Pts',(-29.5075354964661,36.6682851435785,
-232.18296040294));
#201700=CARTESIAN_POINT('Ctrl Pts',(-30.260203356218,37.041928546648,-231.397949783602));
#201701=CARTESIAN_POINT('Ctrl Pts',(-31.012687072449,37.4155430678739,-230.612897000714));
#201702=CARTESIAN_POINT('Ctrl Pts',(-31.7651707886799,37.7891575890997,
-229.827844217825));
#201703=CARTESIAN_POINT('Ctrl Pts',(-32.5174703341753,38.1627432696007,
-229.042749264024));
#201704=CARTESIAN_POINT('Ctrl Pts',(-33.2695884278607,38.5363065970483,
-228.257619016064));
#201705=CARTESIAN_POINT('Ctrl Pts',(-34.7738246152316,39.2834332519434,
-226.687358520144));
#201706=CARTESIAN_POINT('Ctrl Pts',(-36.2773319082997,40.0304737792722,
-225.116955396868));
#201707=CARTESIAN_POINT('Ctrl Pts',(-37.7801639596043,40.7774501421753,
-223.546481445834));
#201708=CARTESIAN_POINT('Ctrl Pts',(-40.7858280622135,42.2714028679817,
-220.405533543764));
#201709=CARTESIAN_POINT('Ctrl Pts',(-43.788714991937,43.7652295475826,-217.264288793245));
#201710=CARTESIAN_POINT('Ctrl Pts',(-46.7899896154941,45.2580776239732,
-214.123556902107));
#201711=CARTESIAN_POINT('Ctrl Pts',(-28.811481324712,36.2672238003158,-232.961663720964));
#201712=CARTESIAN_POINT('Ctrl Pts',(-29.5645263655861,36.6399226415611,
-232.177270818232));
#201713=CARTESIAN_POINT('Ctrl Pts',(-30.3173414199567,37.0126142771829,
-231.392803581211));
#201714=CARTESIAN_POINT('Ctrl Pts',(-31.069911071871,37.385324556228,-230.608260371606));
#201715=CARTESIAN_POINT('Ctrl Pts',(-31.8224807237854,37.7580348352731,
-229.823717162));
#201716=CARTESIAN_POINT('Ctrl Pts',(-32.5748049718356,38.1307637318441,
-229.039097966911));
#201717=CARTESIAN_POINT('Ctrl Pts',(-33.326867581659,38.5035402264522,-228.254401763819));
#201718=CARTESIAN_POINT('Ctrl Pts',(-34.8309928013059,39.2490932156681,
-226.685009357635));
#201719=CARTESIAN_POINT('Ctrl Pts',(-36.3340721635766,39.9948325139069,
-225.115307761803));
#201720=CARTESIAN_POINT('Ctrl Pts',(-37.8359666905481,40.7410341111373,
-223.545299801334));
#201721=CARTESIAN_POINT('Ctrl Pts',(-40.8397557444911,42.233437305598,-220.405283880397));
#201722=CARTESIAN_POINT('Ctrl Pts',(-43.8388051696003,43.7275965705222,
-217.264000696622));
#201723=CARTESIAN_POINT('Ctrl Pts',(-46.8319258491792,45.2266492383781,
-214.121813627025));
#201724=CARTESIAN_POINT('',(-27.8050194937375,36.7328856011635,-232.85004997616));
#201725=CARTESIAN_POINT('',(-28.91863242939,36.3202559697984,-232.850049997099));
#201726=CARTESIAN_POINT('Ctrl Pts',(-27.8050195498509,36.7328855898013,
-232.85005));
#201727=CARTESIAN_POINT('Ctrl Pts',(-27.8949275165814,36.7209782096512,
-232.85005));
#201728=CARTESIAN_POINT('Ctrl Pts',(-27.9520459297408,36.7106005629156,
-232.850049999996));
#201729=CARTESIAN_POINT('Ctrl Pts',(-28.0460926671002,36.6880699552386,
-232.850049999996));
#201730=CARTESIAN_POINT('Ctrl Pts',(-28.0749971330459,36.6807536283026,
-232.85004999998));
#201731=CARTESIAN_POINT('Ctrl Pts',(-28.1941353499751,36.6493093982322,
-232.85004999998));
#201732=CARTESIAN_POINT('Ctrl Pts',(-28.2670565577019,36.626391907203,-232.85005000281));
#201733=CARTESIAN_POINT('Ctrl Pts',(-28.4092997003064,36.5718764626196,
-232.85005000281));
#201734=CARTESIAN_POINT('Ctrl Pts',(-28.4498501321219,36.5555397344433,
-232.850050000011));
#201735=CARTESIAN_POINT('Ctrl Pts',(-28.516992000843,36.5269407519737,-232.850050000011));
#201736=CARTESIAN_POINT('Ctrl Pts',(-28.5460646864076,36.5139050283581,
-232.850049999999));
#201737=CARTESIAN_POINT('Ctrl Pts',(-28.5974873610269,36.4900506389875,
-232.850049999999));
#201738=CARTESIAN_POINT('Ctrl Pts',(-28.6238785516589,36.4773923395039,
-232.85005));
#201739=CARTESIAN_POINT('Ctrl Pts',(-28.6914460343325,36.4443598397627,
-232.85005));
#201740=CARTESIAN_POINT('Ctrl Pts',(-28.7430990859246,36.4184125393908,
-232.850050000001));
#201741=CARTESIAN_POINT('Ctrl Pts',(-28.8244637237435,36.3756607678727,
-232.850050000001));
#201742=CARTESIAN_POINT('Ctrl Pts',(-28.8695136741866,36.3496498157912,
-232.85005));
#201743=CARTESIAN_POINT('Ctrl Pts',(-28.9186324246664,36.3202560005055,
-232.85005));
#201744=CARTESIAN_POINT('',(-42.5495440650111,46.8296601025756,-214.549225413994));
#201745=CARTESIAN_POINT('Ctrl Pts',(-27.8050194367111,36.7328856245227,
-232.850049943209));
#201746=CARTESIAN_POINT('Ctrl Pts',(-28.8113908504514,37.4236469909598,
-231.598047201307));
#201747=CARTESIAN_POINT('Ctrl Pts',(-29.8181679708266,38.1142366013137,
-230.346339471264));
#201748=CARTESIAN_POINT('Ctrl Pts',(-30.825311593422,38.8047002149063,-229.094849929364));
#201749=CARTESIAN_POINT('Ctrl Pts',(-32.0551345438968,39.647825246345,-227.566656207657));
#201750=CARTESIAN_POINT('Ctrl Pts',(-33.2855044821927,40.4907627392734,
-226.038787218309));
#201751=CARTESIAN_POINT('Ctrl Pts',(-34.5163077632667,41.3335669381032,
-224.511155775758));
#201752=CARTESIAN_POINT('Ctrl Pts',(-35.858766024936,42.2528279419423,-222.844941944213));
#201753=CARTESIAN_POINT('Ctrl Pts',(-37.2017438370567,43.1719331137164,
-221.179005741399));
#201754=CARTESIAN_POINT('Ctrl Pts',(-38.5450581953352,44.0909285309741,
-219.513278100248));
#201755=CARTESIAN_POINT('Ctrl Pts',(-39.87961658598,45.0039337687333,-217.858407975228));
#201756=CARTESIAN_POINT('Ctrl Pts',(-41.2145061144966,45.9168299735115,
-216.203744979336));
#201757=CARTESIAN_POINT('Ctrl Pts',(-42.5495440044243,46.8296601017195,
-214.549225420693));
#201758=CARTESIAN_POINT('',(-42.9717852817482,46.7498147039571,-214.534096350323));
#201759=CARTESIAN_POINT('Ctrl Pts',(-42.971785281757,46.7498147039532,-214.534096350459));
#201760=CARTESIAN_POINT('Ctrl Pts',(-42.9007346296511,46.763275910118,-214.539081896592));
#201761=CARTESIAN_POINT('Ctrl Pts',(-42.8299315204016,46.776675786459,-214.542916316407));
#201762=CARTESIAN_POINT('Ctrl Pts',(-42.6886800576438,46.8033850073215,
-214.547976621766));
#201763=CARTESIAN_POINT('Ctrl Pts',(-42.619734567264,46.8164109911115,-214.549201740479));
#201764=CARTESIAN_POINT('Ctrl Pts',(-42.5495441334904,46.8296600955011,
-214.549225427215));
#201765=CARTESIAN_POINT('',(-46.6391379650153,45.1301057079818,-214.324193082213));
#201766=CARTESIAN_POINT('Ctrl Pts',(-42.971785281757,46.749814703953,-214.534096350459));
#201767=CARTESIAN_POINT('Ctrl Pts',(-43.0986721931805,46.7257747996628,
-214.525192835446));
#201768=CARTESIAN_POINT('Ctrl Pts',(-43.2250603487763,46.698950689265,-214.516517597901));
#201769=CARTESIAN_POINT('Ctrl Pts',(-43.4873979542421,46.6372234999647,
-214.499052367715));
#201770=CARTESIAN_POINT('Ctrl Pts',(-43.6236733286717,46.60170761618,-214.490110644589));
#201771=CARTESIAN_POINT('Ctrl Pts',(-43.8528808069682,46.536136708902,-214.475014174647));
#201772=CARTESIAN_POINT('Ctrl Pts',(-43.9471502951446,46.5074540598357,
-214.468951067953));
#201773=CARTESIAN_POINT('Ctrl Pts',(-44.1657362375147,46.4369225437304,
-214.455376470205));
#201774=CARTESIAN_POINT('Ctrl Pts',(-44.2895719690723,46.3939046797032,
-214.44795935219));
#201775=CARTESIAN_POINT('Ctrl Pts',(-44.5758870683756,46.2872516658799,
-214.430838622384));
#201776=CARTESIAN_POINT('Ctrl Pts',(-44.7376694317707,46.2214844642399,
-214.421105848178));
#201777=CARTESIAN_POINT('Ctrl Pts',(-44.9968191999223,46.1070741801046,
-214.40608822588));
#201778=CARTESIAN_POINT('Ctrl Pts',(-45.0953309340452,46.061394556028,-214.400545485118));
#201779=CARTESIAN_POINT('Ctrl Pts',(-45.3586587291112,45.933337546142,-214.386175771088));
#201780=CARTESIAN_POINT('Ctrl Pts',(-45.5225973316144,45.847169815917,-214.377106637015));
#201781=CARTESIAN_POINT('Ctrl Pts',(-45.7910067952199,45.695231241578,-214.362880563465));
#201782=CARTESIAN_POINT('Ctrl Pts',(-45.8980961662255,45.6315653233674,
-214.357676228472));
#201783=CARTESIAN_POINT('Ctrl Pts',(-46.0677903916686,45.5257929940805,
-214.349632079152));
#201784=CARTESIAN_POINT('Ctrl Pts',(-46.1316130051584,45.4848666363269,
-214.346627166685));
#201785=CARTESIAN_POINT('Ctrl Pts',(-46.276213361064,45.3894937683197,-214.339569954199));
#201786=CARTESIAN_POINT('Ctrl Pts',(-46.3575523972629,45.3339263996382,
-214.335548815048));
#201787=CARTESIAN_POINT('Ctrl Pts',(-46.5062346419384,45.2285595756106,
-214.32924726228));
#201788=CARTESIAN_POINT('Ctrl Pts',(-46.5731746843278,45.1796922527548,
-214.326639483805));
#201789=CARTESIAN_POINT('Ctrl Pts',(-46.6391379870654,45.1301057439282,
-214.324192948162));
#201790=CARTESIAN_POINT('Ctrl Pts',(-28.9186324244905,36.3202560021114,
-232.85005));
#201791=CARTESIAN_POINT('Ctrl Pts',(-31.8738175305195,37.7828806767965,
-229.771729072198));
#201792=CARTESIAN_POINT('Ctrl Pts',(-34.8254630565706,39.2453536842348,
-226.692248678165));
#201793=CARTESIAN_POINT('Ctrl Pts',(-40.7330653074378,42.1803713539693,
-220.516897602703));
#201794=CARTESIAN_POINT('Ctrl Pts',(-43.6889686819812,43.6528974634763,
-217.42098942157));
#201795=CARTESIAN_POINT('Ctrl Pts',(-46.6391379591575,45.1301057601645,
-214.324193166304));
#201796=CARTESIAN_POINT('Ctrl Pts',(-46.9840049393815,18.6129810161854,
-232.962872244472));
#201797=CARTESIAN_POINT('Ctrl Pts',(-47.8808382771992,19.9304390734321,
-231.392237704844));
#201798=CARTESIAN_POINT('Ctrl Pts',(-48.7782728428765,21.247161929372,-229.821521522905));
#201799=CARTESIAN_POINT('Ctrl Pts',(-49.6764219919997,22.5630778387597,
-228.250728876356));
#201800=CARTESIAN_POINT('Ctrl Pts',(-50.5745711411229,23.8789937481474,
-226.679936229808));
#201801=CARTESIAN_POINT('Ctrl Pts',(-51.4734343837544,25.1941028059552,
-225.109066921118));
#201802=CARTESIAN_POINT('Ctrl Pts',(-52.3731538889575,26.508321667889,-223.538132682591));
#201803=CARTESIAN_POINT('Ctrl Pts',(-54.1725928993637,29.1367593917566,
-220.396264205537));
#201804=CARTESIAN_POINT('Ctrl Pts',(-55.9754067618462,31.7616502024816,
-217.254119255235));
#201805=CARTESIAN_POINT('Ctrl Pts',(-57.7832199428974,34.3821699572177,
-214.111935079921));
#201806=CARTESIAN_POINT('Ctrl Pts',(-46.9913120403997,18.6016320696042,
-232.962809737275));
#201807=CARTESIAN_POINT('Ctrl Pts',(-47.8881017068652,19.919347208754,-231.392174086571));
#201808=CARTESIAN_POINT('Ctrl Pts',(-48.7854927208081,21.2363283107576,
-229.821456748291));
#201809=CARTESIAN_POINT('Ctrl Pts',(-49.6835984491062,22.5525036430274,
-228.250662893886));
#201810=CARTESIAN_POINT('Ctrl Pts',(-50.5817041774044,23.8686789752972,
-226.679869039482));
#201811=CARTESIAN_POINT('Ctrl Pts',(-51.480524130202,25.1840486327538,-225.108998471456));
#201812=CARTESIAN_POINT('Ctrl Pts',(-52.3802004849816,26.4985292873713,
-223.538062914284));
#201813=CARTESIAN_POINT('Ctrl Pts',(-54.1795531945409,29.1274905966065,
-220.396191799938));
#201814=CARTESIAN_POINT('Ctrl Pts',(-55.9822813208348,31.7529097593695,
-217.254043978496));
#201815=CARTESIAN_POINT('Ctrl Pts',(-57.7900093367969,34.3739628192697,
-214.111856605281));
#201816=CARTESIAN_POINT('Ctrl Pts',(-46.9993592918125,18.5895020464233,
-232.962537246545));
#201817=CARTESIAN_POINT('Ctrl Pts',(-47.8960185439573,19.9075721396807,
-231.391930728925));
#201818=CARTESIAN_POINT('Ctrl Pts',(-48.7932866262407,21.2248997369702,
-229.821238456431));
#201819=CARTESIAN_POINT('Ctrl Pts',(-49.6912806705268,22.5414098682959,
-228.250464972721));
#201820=CARTESIAN_POINT('Ctrl Pts',(-50.5892747148128,23.8579199996217,
-226.679691489012));
#201821=CARTESIAN_POINT('Ctrl Pts',(-51.4879942010195,25.1736127697718,
-225.108836587826));
#201822=CARTESIAN_POINT('Ctrl Pts',(-52.3875865131366,26.4884007882765,
-223.537911482743));
#201823=CARTESIAN_POINT('Ctrl Pts',(-54.1867711373708,29.117976825286,-220.396061272575));
#201824=CARTESIAN_POINT('Ctrl Pts',(-55.9893940924071,31.7439488367061,
-217.25391286698));
#201825=CARTESIAN_POINT('Ctrl Pts',(-57.7971476360592,34.365448302035,-214.11170390739));
#201826=CARTESIAN_POINT('Ctrl Pts',(-47.0041643855294,18.580762838696,-232.963218170749));
#201827=CARTESIAN_POINT('Ctrl Pts',(-47.9010716022698,19.8987644772325,
-231.392505287657));
#201828=CARTESIAN_POINT('Ctrl Pts',(-48.7985636253896,21.2160564611115,
-229.821719884836));
#201829=CARTESIAN_POINT('Ctrl Pts',(-49.6967438426135,22.5325760511435,
-228.250869035074));
#201830=CARTESIAN_POINT('Ctrl Pts',(-50.5949240598375,23.8490956411754,
-226.680018185312));
#201831=CARTESIAN_POINT('Ctrl Pts',(-51.4937920916948,25.1648428846195,
-225.10910171349));
#201832=CARTESIAN_POINT('Ctrl Pts',(-52.3934756614324,26.4797462844595,
-223.53813309987));
#201833=CARTESIAN_POINT('Ctrl Pts',(-54.1928428009075,29.1095530841393,
-220.396195872632));
#201834=CARTESIAN_POINT('Ctrl Pts',(-55.9954317595172,31.7359937276413,
-217.254034998605));
#201835=CARTESIAN_POINT('Ctrl Pts',(-57.8026630300816,34.3583854144121,
-214.111890802731));
#201836=CARTESIAN_POINT('Ctrl Pts',(-47.0089694792463,18.5720236309689,
-232.963899094952));
#201837=CARTESIAN_POINT('Ctrl Pts',(-47.9061246605823,19.8899568147843,
-231.393079846389));
#201838=CARTESIAN_POINT('Ctrl Pts',(-48.8038406245385,21.2072131852528,
-229.822201313241));
#201839=CARTESIAN_POINT('Ctrl Pts',(-49.7022070147003,22.523742233991,-228.251273097427));
#201840=CARTESIAN_POINT('Ctrl Pts',(-50.6005734048621,23.8402712827293,
-226.680344881612));
#201841=CARTESIAN_POINT('Ctrl Pts',(-51.4995899823701,25.1560729994673,
-225.109366839153));
#201842=CARTESIAN_POINT('Ctrl Pts',(-52.3993648097282,26.4710917806424,
-223.538354716999));
#201843=CARTESIAN_POINT('Ctrl Pts',(-54.1989144644443,29.1011293429925,
-220.39633047269));
#201844=CARTESIAN_POINT('Ctrl Pts',(-56.0014694266273,31.7280386185765,
-217.25415713023));
#201845=CARTESIAN_POINT('Ctrl Pts',(-57.8081784241041,34.3513225267891,
-214.112077698071));
#201846=CARTESIAN_POINT('Ctrl Pts',(-47.0135037838248,18.5636186637907,
-232.964603901451));
#201847=CARTESIAN_POINT('Ctrl Pts',(-47.9109413268945,19.8814389765153,
-231.393671922464));
#201848=CARTESIAN_POINT('Ctrl Pts',(-48.8089116831402,21.1986202770561,
-229.822695902599));
#201849=CARTESIAN_POINT('Ctrl Pts',(-49.7074910913547,22.5151234922153,
-228.251687496631));
#201850=CARTESIAN_POINT('Ctrl Pts',(-50.6060704995693,23.8316267073747,
-226.680679090663));
#201851=CARTESIAN_POINT('Ctrl Pts',(-51.5052588130045,25.1474518025266,
-225.109638186271));
#201852=CARTESIAN_POINT('Ctrl Pts',(-52.4051458912763,26.4625572063643,
-223.538582055459));
#201853=CARTESIAN_POINT('Ctrl Pts',(-54.2049200478198,29.0927680140397,
-220.396469793837));
#201854=CARTESIAN_POINT('Ctrl Pts',(-56.0074702714946,31.7201003474161,
-217.254286107255));
#201855=CARTESIAN_POINT('Ctrl Pts',(-57.8137160680311,34.3442051333583,
-214.11226899193));
#201856=CARTESIAN_POINT('Ctrl Pts',(-47.0177828560111,18.5555300817996,
-232.96533252157));
#201857=CARTESIAN_POINT('Ctrl Pts',(-47.9155370349421,19.8731929180949,
-231.394280823516));
#201858=CARTESIAN_POINT('Ctrl Pts',(-48.8137913023007,21.1902606020353,
-229.823202807664));
#201859=CARTESIAN_POINT('Ctrl Pts',(-49.7126093236726,22.5067040125525,
-228.252111396185));
#201860=CARTESIAN_POINT('Ctrl Pts',(-50.6114273450444,23.8231474230696,
-226.681019984706));
#201861=CARTESIAN_POINT('Ctrl Pts',(-51.5108090328418,25.1389665178458,
-225.109915092335));
#201862=CARTESIAN_POINT('Ctrl Pts',(-52.4108279627846,26.4541313607334,
-223.538814574431));
#201863=CARTESIAN_POINT('Ctrl Pts',(-54.2108658226704,29.0844610465087,
-220.396613538622));
#201864=CARTESIAN_POINT('Ctrl Pts',(-56.0134397408495,31.7121723231175,
-217.254421501589));
#201865=CARTESIAN_POINT('Ctrl Pts',(-57.8192783928772,34.3370299914758,
-214.112464332901));
#201866=CARTESIAN_POINT('Ctrl Pts',(-47.0263410003839,18.5393529178172,
-232.966789761807));
#201867=CARTESIAN_POINT('Ctrl Pts',(-47.9247284510372,19.856700801254,-231.395498625619));
#201868=CARTESIAN_POINT('Ctrl Pts',(-48.8235505406218,21.1735412519938,
-229.824216617793));
#201869=CARTESIAN_POINT('Ctrl Pts',(-49.7228457883083,22.4898650532266,
-228.252959195293));
#201870=CARTESIAN_POINT('Ctrl Pts',(-50.6221410359948,23.8061888544594,
-226.681701772792));
#201871=CARTESIAN_POINT('Ctrl Pts',(-51.5219094725163,25.1219959484843,
-225.110468904466));
#201872=CARTESIAN_POINT('Ctrl Pts',(-52.4221921058014,26.4372796694717,
-223.539279612374));
#201873=CARTESIAN_POINT('Ctrl Pts',(-54.2227573723716,29.0678471114466,
-220.396901028191));
#201874=CARTESIAN_POINT('Ctrl Pts',(-56.0253786795592,31.6963162745203,
-217.254692290257));
#201875=CARTESIAN_POINT('Ctrl Pts',(-57.8304030425693,34.3226797077107,
-214.112855014843));
#201876=CARTESIAN_POINT('Ctrl Pts',(-47.0338760075754,18.5244437003147,
-232.968343063198));
#201877=CARTESIAN_POINT('Ctrl Pts',(-47.9330342637239,19.8412977645685,
-231.396784393101));
#201878=CARTESIAN_POINT('Ctrl Pts',(-48.8325426907541,21.1577563020188,
-229.825280180548));
#201879=CARTESIAN_POINT('Ctrl Pts',(-49.7324178666844,22.4738242520981,
-228.253845361594));
#201880=CARTESIAN_POINT('Ctrl Pts',(-50.6322930426146,23.7898922021775,
-226.682410542641));
#201881=CARTESIAN_POINT('Ctrl Pts',(-51.5325349868385,25.1055695505858,
-225.111045116373));
#201882=CARTESIAN_POINT('Ctrl Pts',(-52.4331598468605,26.4208632806089,
-223.539765492053));
#201883=CARTESIAN_POINT('Ctrl Pts',(-54.2344095669047,29.0514507406552,
-220.397206243413));
#201884=CARTESIAN_POINT('Ctrl Pts',(-56.0371921164241,31.6805012272399,
-217.254988767415));
#201885=CARTESIAN_POINT('Ctrl Pts',(-57.8416264681079,34.3080984038517,
-214.113261878824));
#201886=CARTESIAN_POINT('Ctrl Pts',(-47.0405353763693,18.5106352292473,
-232.969983979348));
#201887=CARTESIAN_POINT('Ctrl Pts',(-47.9405971515569,19.8268187140002,
-231.398125716493));
#201888=CARTESIAN_POINT('Ctrl Pts',(-48.8408986391317,21.1427526567519,
-229.826381496195));
#201889=CARTESIAN_POINT('Ctrl Pts',(-49.7414431123329,22.4584427038901,
-228.254759191353));
#201890=CARTESIAN_POINT('Ctrl Pts',(-50.6419875855342,23.7741327510283,
-226.683136886512));
#201891=CARTESIAN_POINT('Ctrl Pts',(-51.5427750540585,25.0895788993504,
-225.111636500013));
#201892=CARTESIAN_POINT('Ctrl Pts',(-52.443808131774,26.4047878990792,-223.540266455142));
#201893=CARTESIAN_POINT('Ctrl Pts',(-54.2458742872048,29.0352058985368,
-220.397526365399));
#201894=CARTESIAN_POINT('Ctrl Pts',(-56.0489238784563,31.6646741163143,
-217.255307216989));
#201895=CARTESIAN_POINT('Ctrl Pts',(-57.852967529916,34.2932604357928,-214.113682169595));
#201896=CARTESIAN_POINT('Ctrl Pts',(-47.0538541139573,18.4830182871128,
-232.973265811648));
#201897=CARTESIAN_POINT('Ctrl Pts',(-47.955722927223,19.7978606128634,-231.400808363276));
#201898=CARTESIAN_POINT('Ctrl Pts',(-48.8576105358869,21.1127453662178,
-229.828584127488));
#201899=CARTESIAN_POINT('Ctrl Pts',(-49.7594936036301,22.4276796074738,
-228.256586850871));
#201900=CARTESIAN_POINT('Ctrl Pts',(-50.6613766713732,23.7426138487298,
-226.684589574255));
#201901=CARTESIAN_POINT('Ctrl Pts',(-51.5632551884987,25.0575975968797,
-225.112819267293));
#201902=CARTESIAN_POINT('Ctrl Pts',(-52.4651047016009,26.3726371360198,
-223.541268381319));
#201903=CARTESIAN_POINT('Ctrl Pts',(-54.2688037278052,29.0027162143,-220.398166609371));
#201904=CARTESIAN_POINT('Ctrl Pts',(-56.0723874025208,31.6330198944631,
-217.255944116137));
#201905=CARTESIAN_POINT('Ctrl Pts',(-57.875649653532,34.2635844996751,-214.114522751136));
#201906=CARTESIAN_POINT('Ctrl Pts',(-47.0636230131447,18.4598625903094,
-232.976920051811));
#201907=CARTESIAN_POINT('Ctrl Pts',(-47.9678453495437,19.7726375200406,
-231.403727674415));
#201908=CARTESIAN_POINT('Ctrl Pts',(-48.8717566764505,21.0858891471629,
-229.830947114461));
#201909=CARTESIAN_POINT('Ctrl Pts',(-49.7753424176378,22.3995713001604,
-228.258531477614));
#201910=CARTESIAN_POINT('Ctrl Pts',(-50.6789281588252,23.713253453158,-226.686115840768));
#201911=CARTESIAN_POINT('Ctrl Pts',(-51.5821885259387,25.0273656345712,
-225.114064824849));
#201912=CARTESIAN_POINT('Ctrl Pts',(-52.4851199367133,26.3418548778766,
-223.54233208791));
#201913=CARTESIAN_POINT('Ctrl Pts',(-54.2909827582626,28.9708333644873,
-220.398866614033));
#201914=CARTESIAN_POINT('Ctrl Pts',(-56.0955252131014,31.6013169572485,
-217.256668942392));
#201915=CARTESIAN_POINT('Ctrl Pts',(-57.8988032731226,34.2328814256343,
-214.115416854107));
#201916=CARTESIAN_POINT('Ctrl Pts',(-47.07151283755,18.4392609475024,-232.980675631547));
#201917=CARTESIAN_POINT('Ctrl Pts',(-47.9784669049768,19.7494077885448,
-231.40663525448));
#201918=CARTESIAN_POINT('Ctrl Pts',(-48.8846403863511,21.0606622046162,
-229.833271513153));
#201919=CARTESIAN_POINT('Ctrl Pts',(-49.7901160730939,22.3727913382652,
-228.260434083043));
#201920=CARTESIAN_POINT('Ctrl Pts',(-50.6955917598367,23.6849204719142,
-226.687596652933));
#201921=CARTESIAN_POINT('Ctrl Pts',(-51.6003698589295,24.9979251551198,
-225.115286361312));
#201922=CARTESIAN_POINT('Ctrl Pts',(-52.5045272731894,26.3116209606581,
-223.543390841591));
#201923=CARTESIAN_POINT('Ctrl Pts',(-54.3128421017092,28.939012571735,-220.399599802148));
#201924=CARTESIAN_POINT('Ctrl Pts',(-56.1186826713171,31.569141738417,-217.257449700108));
#201925=CARTESIAN_POINT('Ctrl Pts',(-57.9225686339535,34.2009514305169,
-214.116344107367));
#201926=CARTESIAN_POINT('Ctrl Pts',(-47.0872924863604,18.3980576618883,
-232.988186791018));
#201927=CARTESIAN_POINT('Ctrl Pts',(-47.999710015843,19.7029483255535,-231.41245041461));
#201928=CARTESIAN_POINT('Ctrl Pts',(-48.9104078061524,21.0102083195229,
-229.837920310538));
#201929=CARTESIAN_POINT('Ctrl Pts',(-49.819663384006,22.3192314144748,-228.264239293901));
#201930=CARTESIAN_POINT('Ctrl Pts',(-50.7289189618596,23.6282545094267,
-226.690558277265));
#201931=CARTESIAN_POINT('Ctrl Pts',(-51.636732524911,24.9390441962169,-225.117729434238));
#201932=CARTESIAN_POINT('Ctrl Pts',(-52.5433419461414,26.2511531262214,
-223.545508348952));
#201933=CARTESIAN_POINT('Ctrl Pts',(-54.3565607886023,28.8753709862302,
-220.401066178378));
#201934=CARTESIAN_POINT('Ctrl Pts',(-56.1649975877485,31.5047913007538,
-217.259011215537));
#201935=CARTESIAN_POINT('Ctrl Pts',(-57.9700993556152,34.1370914402818,
-214.118198613889));
#201936=CARTESIAN_POINT('Ctrl Pts',(-47.0957039619647,18.3671243104028,
-232.996174969848));
#201937=CARTESIAN_POINT('Ctrl Pts',(-48.0152404739711,19.6642406239314,
-231.41815251762));
#201938=CARTESIAN_POINT('Ctrl Pts',(-48.9313836399292,20.966064710906,-229.842352705242));
#201939=CARTESIAN_POINT('Ctrl Pts',(-49.8451267410034,22.2708048165049,
-228.267820632962));
#201940=CARTESIAN_POINT('Ctrl Pts',(-50.7588698420775,23.575544922104,-226.693288560683));
#201941=CARTESIAN_POINT('Ctrl Pts',(-51.6702057869443,24.8832308760699,
-225.12004558303));
#201942=CARTESIAN_POINT('Ctrl Pts',(-52.5798100280734,26.1928111185938,
-223.547584934865));
#201943=CARTESIAN_POINT('Ctrl Pts',(-54.3990185103318,28.8119716036413,
-220.402663638535));
#201944=CARTESIAN_POINT('Ctrl Pts',(-56.2114230943841,31.438531247625,-217.260790636888));
#201945=CARTESIAN_POINT('Ctrl Pts',(-58.0200925469402,34.0683156133792,
-214.120181154191));
#201946=CARTESIAN_POINT('Ctrl Pts',(-47.1150642483994,18.3236858273299,
-232.999295710587));
#201947=CARTESIAN_POINT('Ctrl Pts',(-48.0392206238659,19.6158965079908,
-231.420362484156));
#201948=CARTESIAN_POINT('Ctrl Pts',(-48.9590100671071,20.9141580894346,
-229.844205156969));
#201949=CARTESIAN_POINT('Ctrl Pts',(-49.8759725739142,22.2158319633755,
-228.269472472139));
#201950=CARTESIAN_POINT('Ctrl Pts',(-50.7929350807213,23.5175058373164,
-226.694739787308));
#201951=CARTESIAN_POINT('Ctrl Pts',(-51.7070476323962,24.8226580511233,
-225.12147447558));
#201952=CARTESIAN_POINT('Ctrl Pts',(-52.6192352667853,26.1299128826243,
-223.549042364026));
#201953=CARTESIAN_POINT('Ctrl Pts',(-54.4436105355637,28.7444225456263,
-220.404178140919));
#201954=CARTESIAN_POINT('Ctrl Pts',(-56.2604448907417,31.367132192526,-217.262559371757));
#201955=CARTESIAN_POINT('Ctrl Pts',(-58.0734857403641,33.9931206393803,
-214.122173015364));
#201956=CARTESIAN_POINT('Ctrl Pts',(-47.1344245348341,18.280247344257,-233.002416451326));
#201957=CARTESIAN_POINT('Ctrl Pts',(-48.0632007737606,19.5675523920502,
-231.422572450694));
#201958=CARTESIAN_POINT('Ctrl Pts',(-48.9866364942849,20.8622514679632,
-229.846057608697));
#201959=CARTESIAN_POINT('Ctrl Pts',(-49.906818406825,22.1608591102461,-228.271124311316));
#201960=CARTESIAN_POINT('Ctrl Pts',(-50.8270003193651,23.459466752529,-226.696191013934));
#201961=CARTESIAN_POINT('Ctrl Pts',(-51.7438894778481,24.7620852261766,
-225.12290336813));
#201962=CARTESIAN_POINT('Ctrl Pts',(-52.6586605054972,26.0670146466549,
-223.550499793187));
#201963=CARTESIAN_POINT('Ctrl Pts',(-54.4882025607956,28.6768734876113,
-220.405692643303));
#201964=CARTESIAN_POINT('Ctrl Pts',(-56.3094666870994,31.2957331374271,
-217.264328106627));
#201965=CARTESIAN_POINT('Ctrl Pts',(-58.1268789337879,33.9179256653815,
-214.124164876537));
#201966=CARTESIAN_POINT('Ctrl Pts',(-47.1550475881779,18.2351214015296,
-233.004587184861));
#201967=CARTESIAN_POINT('Ctrl Pts',(-48.0879494927851,19.5179208547626,
-231.424215169804));
#201968=CARTESIAN_POINT('Ctrl Pts',(-49.0146228296911,20.8093049547191,
-229.847633981322));
#201969=CARTESIAN_POINT('Ctrl Pts',(-49.9377435309543,22.1049290587682,
-228.272719230379));
#201970=CARTESIAN_POINT('Ctrl Pts',(-50.8608642322175,23.4005531628173,
-226.697804479436));
#201971=CARTESIAN_POINT('Ctrl Pts',(-51.7803719924673,24.7005632099661,
-225.124644811749));
#201972=CARTESIAN_POINT('Ctrl Pts',(-52.6976719303263,26.0029791484965,
-223.55238064694));
#201973=CARTESIAN_POINT('Ctrl Pts',(-54.5322718060444,28.6078110255573,
-220.407852317323));
#201974=CARTESIAN_POINT('Ctrl Pts',(-56.3582589004816,31.2220093923588,
-217.266815267618));
#201975=CARTESIAN_POINT('Ctrl Pts',(-58.1805302372139,33.8394259727705,
-214.126915573344));
#201976=CARTESIAN_POINT('Ctrl Pts',(-47.1711020320382,18.1951169691784,
-233.008152197064));
#201977=CARTESIAN_POINT('Ctrl Pts',(-48.1091754301695,19.471620881615,-231.426873602798));
#201978=CARTESIAN_POINT('Ctrl Pts',(-49.0396359981975,20.7586423084589,
-229.850155627119));
#201979=CARTESIAN_POINT('Ctrl Pts',(-49.9662083070876,22.0502814645383,
-228.275198729438));
#201980=CARTESIAN_POINT('Ctrl Pts',(-50.8927806159777,23.3419206206176,
-226.700241831756));
#201981=CARTESIAN_POINT('Ctrl Pts',(-51.8153427493086,24.6384368291909,
-225.12719326289));
#201982=CARTESIAN_POINT('Ctrl Pts',(-52.7356127602431,25.9374582798656,
-223.555055698046));
#201983=CARTESIAN_POINT('Ctrl Pts',(-54.5761527821122,28.535501181215,-220.410780568357));
#201984=CARTESIAN_POINT('Ctrl Pts',(-56.4077512436301,31.1433164616566,
-217.270071905955));
#201985=CARTESIAN_POINT('Ctrl Pts',(-58.2358086912436,33.7542064961608,
-214.130435725157));
#201986=CARTESIAN_POINT('Ctrl Pts',(-47.1871564758985,18.1551125368272,
-233.011717209266));
#201987=CARTESIAN_POINT('Ctrl Pts',(-48.1304013675538,19.4253209084676,
-231.429532035792));
#201988=CARTESIAN_POINT('Ctrl Pts',(-49.0646491667038,20.7079796621986,
-229.852677272917));
#201989=CARTESIAN_POINT('Ctrl Pts',(-49.9946730832209,21.9956338703083,
-228.277678228496));
#201990=CARTESIAN_POINT('Ctrl Pts',(-50.924696999738,23.283288078418,-226.702679184075));
#201991=CARTESIAN_POINT('Ctrl Pts',(-51.8503135061499,24.5763104484158,
-225.129741714031));
#201992=CARTESIAN_POINT('Ctrl Pts',(-52.7735535901599,25.8719374112347,
-223.557730749151));
#201993=CARTESIAN_POINT('Ctrl Pts',(-54.62003375818,28.4631913368726,-220.413708819391));
#201994=CARTESIAN_POINT('Ctrl Pts',(-56.4572435867786,31.0646235309543,
-217.273328544292));
#201995=CARTESIAN_POINT('Ctrl Pts',(-58.2910871452732,33.6689870195509,
-214.133955876969));
#201996=CARTESIAN_POINT('Ctrl Pts',(-47.2003193864821,18.1182964298664,
-233.015989564334));
#201997=CARTESIAN_POINT('Ctrl Pts',(-48.1493988764852,19.3809230047756,
-231.432724300644));
#201998=CARTESIAN_POINT('Ctrl Pts',(-49.0877568643722,20.6584395224563,
-229.855761293683));
#201999=CARTESIAN_POINT('Ctrl Pts',(-50.0215848134126,21.9412987456968,
-228.28073090895));
#202000=CARTESIAN_POINT('Ctrl Pts',(-50.9554127624531,23.2241579689375,
-226.705700524218));
#202001=CARTESIAN_POINT('Ctrl Pts',(-51.8844304624717,24.5129032830703,
-225.132894527219));
#202002=CARTESIAN_POINT('Ctrl Pts',(-52.811027126582,25.8043188185571,-223.561022084209));
#202003=CARTESIAN_POINT('Ctrl Pts',(-54.6642204548024,28.3871498895308,
-220.417277198188));
#202004=CARTESIAN_POINT('Ctrl Pts',(-56.5079518327106,30.9804583526794,
-217.27722687764));
#202005=CARTESIAN_POINT('Ctrl Pts',(-58.3485555395427,33.5765033299539,
-214.138113904034));
#202006=CARTESIAN_POINT('Ctrl Pts',(-47.2098674957262,18.0858618424364,
-233.021306146667));
#202007=CARTESIAN_POINT('Ctrl Pts',(-48.1660577345037,19.3384804806313,
-231.436445859109));
#202008=CARTESIAN_POINT('Ctrl Pts',(-49.1090703108757,20.6096704873925,
-229.859386110464));
#202009=CARTESIAN_POINT('Ctrl Pts',(-50.0473336065433,21.8864233995054,
-228.284270940977));
#202010=CARTESIAN_POINT('Ctrl Pts',(-50.9855969022109,23.1631763116183,
-226.709155771488));
#202011=CARTESIAN_POINT('Ctrl Pts',(-51.9186177626333,24.4464108695765,
-225.136458640789));
#202012=CARTESIAN_POINT('Ctrl Pts',(-52.8491949026841,25.7323667348012,
-223.564699625624));
#202013=CARTESIAN_POINT('Ctrl Pts',(-54.7103491827856,28.3042784652506,
-220.421181595292));
#202014=CARTESIAN_POINT('Ctrl Pts',(-56.5618994916621,30.8869590362523,
-217.281419567094));
#202015=CARTESIAN_POINT('Ctrl Pts',(-58.4105543383496,33.4721882778783,
-214.142529225918));
#202016=CARTESIAN_POINT('Ctrl Pts',(-47.2289637142144,18.0209926675766,
-233.031939311332));
#202017=CARTESIAN_POINT('Ctrl Pts',(-48.1993754505405,19.2535954323428,
-231.443888976038));
#202018=CARTESIAN_POINT('Ctrl Pts',(-49.1516972038829,20.512132417265,-229.866635744028));
#202019=CARTESIAN_POINT('Ctrl Pts',(-50.0988311928047,21.7766727071225,
-228.291351005029));
#202020=CARTESIAN_POINT('Ctrl Pts',(-51.0459651817265,23.0412129969801,
-226.716066266029));
#202021=CARTESIAN_POINT('Ctrl Pts',(-51.9869923629565,24.3134260425889,
-225.14358686793));
#202022=CARTESIAN_POINT('Ctrl Pts',(-52.9255304548883,25.5884625672894,
-223.572054708453));
#202023=CARTESIAN_POINT('Ctrl Pts',(-54.802606638752,28.1385356166903,-220.4289903895));
#202024=CARTESIAN_POINT('Ctrl Pts',(-56.6697948095651,30.6999604033981,
-217.289804946001));
#202025=CARTESIAN_POINT('Ctrl Pts',(-58.5345519359632,33.2635581737269,
-214.151359869686));
#202026=CARTESIAN_POINT('Ctrl Pts',(-47.2430220815907,17.9624777113029,
-233.042540471425));
#202027=CARTESIAN_POINT('Ctrl Pts',(-48.2273551133025,19.1720899539984,
-231.451949485653));
#202028=CARTESIAN_POINT('Ctrl Pts',(-49.1896659714189,20.4147736143863,
-229.87503540962));
#202029=CARTESIAN_POINT('Ctrl Pts',(-50.1472740382399,21.6628174682499,
-228.299725265682));
#202030=CARTESIAN_POINT('Ctrl Pts',(-51.1048821050609,22.9108613221134,
-226.724415121745));
#202031=CARTESIAN_POINT('Ctrl Pts',(-52.0562292256746,24.1671081729364,
-225.152079490178));
#202032=CARTESIAN_POINT('Ctrl Pts',(-53.0052546893374,25.4261024980228,
-223.580661790924));
#202033=CARTESIAN_POINT('Ctrl Pts',(-54.9033056166631,27.9440911481955,
-220.437826392414));
#202034=CARTESIAN_POINT('Ctrl Pts',(-56.7919721995556,30.4733633447205,
-217.298842424047));
#202035=CARTESIAN_POINT('Ctrl Pts',(-58.6785207415017,33.0046199530293,
-214.16054151441));
#202036=CARTESIAN_POINT('Ctrl Pts',(-47.2636279462708,17.8918194961353,
-233.049292072559));
#202037=CARTESIAN_POINT('Ctrl Pts',(-48.2527927601426,19.0896993463335,
-231.461117845357));
#202038=CARTESIAN_POINT('Ctrl Pts',(-49.2222701184903,20.3177090530585,
-229.885189443365));
#202039=CARTESIAN_POINT('Ctrl Pts',(-50.1877928495361,21.5503879875109,
-228.310673435979));
#202040=CARTESIAN_POINT('Ctrl Pts',(-51.1533155805818,22.7830669219633,
-226.736157428594));
#202041=CARTESIAN_POINT('Ctrl Pts',(-52.1134152350247,24.0230769225979,
-225.164293315049));
#202042=CARTESIAN_POINT('Ctrl Pts',(-53.0715402305708,25.265515738592,-223.593249605752));
#202043=CARTESIAN_POINT('Ctrl Pts',(-54.9877902216631,27.75039337058,-220.451162187155));
#202044=CARTESIAN_POINT('Ctrl Pts',(-56.8960314270369,30.2452705785478,
-217.312517061756));
#202045=CARTESIAN_POINT('Ctrl Pts',(-58.8025041724956,32.7418818204746,
-214.174488273677));
#202046=CARTESIAN_POINT('Ctrl Pts',(-47.2842338109509,17.8211612809678,
-233.056043673691));
#202047=CARTESIAN_POINT('Ctrl Pts',(-48.2782304069827,19.0073087386684,
-231.47028620506));
#202048=CARTESIAN_POINT('Ctrl Pts',(-49.2548742655618,20.2206444917306,
-229.89534347711));
#202049=CARTESIAN_POINT('Ctrl Pts',(-50.2283116608323,21.437958506772,-228.321621606276));
#202050=CARTESIAN_POINT('Ctrl Pts',(-51.2017490561027,22.6552725218134,
-226.747899735443));
#202051=CARTESIAN_POINT('Ctrl Pts',(-52.1706012443748,23.8790456722595,
-225.176507139922));
#202052=CARTESIAN_POINT('Ctrl Pts',(-53.1378257718042,25.1049289791612,
-223.60583742058));
#202053=CARTESIAN_POINT('Ctrl Pts',(-55.072274826663,27.5566955929646,-220.464497981896));
#202054=CARTESIAN_POINT('Ctrl Pts',(-57.0000906545182,30.0171778123751,
-217.326191699464));
#202055=CARTESIAN_POINT('Ctrl Pts',(-58.9264876034895,32.47914368792,-214.188435032943));
#202056=CARTESIAN_POINT('Ctrl Pts',(-47.2994830625051,17.7544372214138,
-233.064985179967));
#202057=CARTESIAN_POINT('Ctrl Pts',(-48.2988763150662,18.9260864440995,
-231.481022299027));
#202058=CARTESIAN_POINT('Ctrl Pts',(-49.2831180301545,20.12226670526,-229.90673458038));
#202059=CARTESIAN_POINT('Ctrl Pts',(-50.264622038348,21.3220097502749,-228.333564088779));
#202060=CARTESIAN_POINT('Ctrl Pts',(-51.2461260465415,22.5217527952899,
-226.760393597177));
#202061=CARTESIAN_POINT('Ctrl Pts',(-52.2236675241889,23.7273082081328,
-225.189324740538));
#202062=CARTESIAN_POINT('Ctrl Pts',(-53.199809818472,24.9347623794372,-223.618913074665));
#202063=CARTESIAN_POINT('Ctrl Pts',(-55.1520944070382,27.3496707220463,
-220.478089742921));
#202064=CARTESIAN_POINT('Ctrl Pts',(-57.0986707756308,29.7724235792233,
-217.34001940174));
#202065=CARTESIAN_POINT('Ctrl Pts',(-59.0440358271753,32.1965198188522,
-214.20245343815));
#202066=CARTESIAN_POINT('Ctrl Pts',(-47.3068095033878,17.6967086574683,
-233.077497779098));
#202067=CARTESIAN_POINT('Ctrl Pts',(-48.3116549954781,18.8520796703188,
-231.494638672248));
#202068=CARTESIAN_POINT('Ctrl Pts',(-49.3030451918381,20.0301039514678,
-229.920713549775));
#202069=CARTESIAN_POINT('Ctrl Pts',(-50.2920112564435,21.2114530404761,
-228.347855989514));
#202070=CARTESIAN_POINT('Ctrl Pts',(-51.280977321049,22.3928021294844,-226.774998429254));
#202071=CARTESIAN_POINT('Ctrl Pts',(-52.2664287923936,23.5795439345552,
-225.204106117501));
#202072=CARTESIAN_POINT('Ctrl Pts',(-53.2506399867227,24.7680561731562,
-223.633834433041));
#202073=CARTESIAN_POINT('Ctrl Pts',(-55.2190623753812,27.1450806503585,
-220.493291064124));
#202074=CARTESIAN_POINT('Ctrl Pts',(-57.1824244494106,29.5294142243635,
-217.355341819955));
#202075=CARTESIAN_POINT('Ctrl Pts',(-59.1447159484551,31.9150218118753,
-214.217874373197));
#202076=CARTESIAN_POINT('Ctrl Pts',(-47.3141359442706,17.638980093523,-233.090010378228));
#202077=CARTESIAN_POINT('Ctrl Pts',(-48.32443367589,18.7780728965381,-231.50825504547));
#202078=CARTESIAN_POINT('Ctrl Pts',(-49.3229723535216,19.9379411976756,
-229.93469251917));
#202079=CARTESIAN_POINT('Ctrl Pts',(-50.3194004745391,21.1008963306773,
-228.36214789025));
#202080=CARTESIAN_POINT('Ctrl Pts',(-51.3158285955566,22.2638514636789,
-226.78960326133));
#202081=CARTESIAN_POINT('Ctrl Pts',(-52.3091900605982,23.4317796609776,
-225.218887494463));
#202082=CARTESIAN_POINT('Ctrl Pts',(-53.3014701549735,24.6013499668753,
-223.648755791418));
#202083=CARTESIAN_POINT('Ctrl Pts',(-55.2860303437241,26.9404905786706,
-220.508492385326));
#202084=CARTESIAN_POINT('Ctrl Pts',(-57.2661781231904,29.2864048695037,
-217.370664238171));
#202085=CARTESIAN_POINT('Ctrl Pts',(-59.2453960697349,31.6335238048983,
-214.233295308244));
#202086=CARTESIAN_POINT('Ctrl Pts',(-47.3205362764709,17.5794518606674,
-233.102169725448));
#202087=CARTESIAN_POINT('Ctrl Pts',(-48.3341251295478,18.7044081787822,
-231.522433893026));
#202088=CARTESIAN_POINT('Ctrl Pts',(-49.338165710491,19.8469474114891,-229.949581699504));
#202089=CARTESIAN_POINT('Ctrl Pts',(-50.3405072447859,20.99216003676,-228.377642387885));
#202090=CARTESIAN_POINT('Ctrl Pts',(-51.3428487790808,22.1373726620309,
-226.805703076266));
#202091=CARTESIAN_POINT('Ctrl Pts',(-52.3427094024845,23.2868368796911,
-225.235339740797));
#202092=CARTESIAN_POINT('Ctrl Pts',(-53.3416967030123,24.4377161128276,
-223.665489068171));
#202093=CARTESIAN_POINT('Ctrl Pts',(-55.3396713040681,26.7394745791004,
-220.525787722919));
#202094=CARTESIAN_POINT('Ctrl Pts',(-57.334081396471,29.0470612357366,-217.388215315384));
#202095=CARTESIAN_POINT('Ctrl Pts',(-59.3277447200742,31.3557006527919,
-214.251054208451));
#202096=CARTESIAN_POINT('Ctrl Pts',(-47.3285982419782,17.5118110061916,
-233.112766042078));
#202097=CARTESIAN_POINT('Ctrl Pts',(-48.3441007183216,18.6236888893903,
-231.535741196264));
#202098=CARTESIAN_POINT('Ctrl Pts',(-49.3524346981868,19.7490902161012,
-229.963964803722));
#202099=CARTESIAN_POINT('Ctrl Pts',(-50.3595015772335,20.8765891331594,
-228.392921090687));
#202100=CARTESIAN_POINT('Ctrl Pts',(-51.3665684562802,22.0040880502176,
-226.821877377652));
#202101=CARTESIAN_POINT('Ctrl Pts',(-52.3717783622527,23.1348854144855,
-225.252060380076));
#202102=CARTESIAN_POINT('Ctrl Pts',(-53.3763360684624,24.2667864286898,
-223.682648344784));
#202103=CARTESIAN_POINT('Ctrl Pts',(-55.3854514808819,26.5305884570984,
-220.5438242742));
#202104=CARTESIAN_POINT('Ctrl Pts',(-57.3919042457265,28.7989304812669,
-217.40667659104));
#202105=CARTESIAN_POINT('Ctrl Pts',(-59.397804330835,31.0680944254412,-214.269858953779));
#202106=CARTESIAN_POINT('Ctrl Pts',(-47.3366602074855,17.444170151716,-233.123362358707));
#202107=CARTESIAN_POINT('Ctrl Pts',(-48.3540763070954,18.5429695999985,
-231.549048499502));
#202108=CARTESIAN_POINT('Ctrl Pts',(-49.3667036858826,19.6512330207133,
-229.97834790794));
#202109=CARTESIAN_POINT('Ctrl Pts',(-50.378495909681,20.7610182295588,-228.40819979349));
#202110=CARTESIAN_POINT('Ctrl Pts',(-51.3902881334795,21.8708034384043,
-226.83805167904));
#202111=CARTESIAN_POINT('Ctrl Pts',(-52.4008473220208,22.9829339492799,
-225.268781019355));
#202112=CARTESIAN_POINT('Ctrl Pts',(-53.4109754339125,24.0958567445521,
-223.699807621397));
#202113=CARTESIAN_POINT('Ctrl Pts',(-55.4312316576958,26.3217023350964,
-220.561860825481));
#202114=CARTESIAN_POINT('Ctrl Pts',(-57.4497270949821,28.5507997267972,
-217.425137866697));
#202115=CARTESIAN_POINT('Ctrl Pts',(-59.4678639415957,30.7804881980906,
-214.288663699106));
#202116=CARTESIAN_POINT('Ctrl Pts',(-47.3394631111059,17.3809856982998,
-233.13701868782));
#202117=CARTESIAN_POINT('Ctrl Pts',(-48.3594374346572,18.4637008192816,
-231.564473009033));
#202118=CARTESIAN_POINT('Ctrl Pts',(-49.3763048521849,19.5528780490395,
-229.994408187512));
#202119=CARTESIAN_POINT('Ctrl Pts',(-50.3925482040264,20.6432779103424,
-228.424798520261));
#202120=CARTESIAN_POINT('Ctrl Pts',(-51.4087915558678,21.7336777716453,
-226.85518885301));
#202121=CARTESIAN_POINT('Ctrl Pts',(-52.4241774034375,22.8258062072129,
-225.286233875719));
#202122=CARTESIAN_POINT('Ctrl Pts',(-53.4392506767952,23.9185477700511,
-223.717512563418));
#202123=CARTESIAN_POINT('Ctrl Pts',(-55.4693972235108,26.1040308957274,
-220.580069938817));
#202124=CARTESIAN_POINT('Ctrl Pts',(-57.4982777107523,28.2920062253737,
-217.443579202073));
#202125=CARTESIAN_POINT('Ctrl Pts',(-59.526890391898,30.4804660465043,-214.307294206909));
#202126=CARTESIAN_POINT('Ctrl Pts',(-47.3388947489722,17.3172597414177,
-233.15277350217));
#202127=CARTESIAN_POINT('Ctrl Pts',(-48.3602977670814,18.3855423142397,
-231.582083581833));
#202128=CARTESIAN_POINT('Ctrl Pts',(-49.3799313248768,19.4576103826212,
-230.012850342708));
#202129=CARTESIAN_POINT('Ctrl Pts',(-50.3991818891466,20.5304657339301,
-228.443915670914));
#202130=CARTESIAN_POINT('Ctrl Pts',(-51.4184324534164,21.6033210852391,
-226.874980999121));
#202131=CARTESIAN_POINT('Ctrl Pts',(-52.4371748506907,22.6772399564986,
-225.306453273624));
#202132=CARTESIAN_POINT('Ctrl Pts',(-53.4557277384216,23.7515480681017,
-223.738076580824));
#202133=CARTESIAN_POINT('Ctrl Pts',(-55.4928335138835,25.9001642913079,
-220.601323195224));
#202134=CARTESIAN_POINT('Ctrl Pts',(-57.529175347697,28.050353188994,-217.465180895102));
#202135=CARTESIAN_POINT('Ctrl Pts',(-59.5653551090103,30.2008561303528,
-214.329177297802));
#202136=CARTESIAN_POINT('Ctrl Pts',(-47.3383263868385,17.2535337845356,
-233.16852831652));
#202137=CARTESIAN_POINT('Ctrl Pts',(-48.3611580995056,18.3073838091979,
-231.599694154632));
#202138=CARTESIAN_POINT('Ctrl Pts',(-49.3835577975687,19.3623427162029,
-230.031292497904));
#202139=CARTESIAN_POINT('Ctrl Pts',(-50.4058155742669,20.4176535575179,
-228.463032821567));
#202140=CARTESIAN_POINT('Ctrl Pts',(-51.4280733509651,21.4729643988329,
-226.894773145231));
#202141=CARTESIAN_POINT('Ctrl Pts',(-52.4501722979439,22.5286737057843,
-225.326672671531));
#202142=CARTESIAN_POINT('Ctrl Pts',(-53.472204800048,23.5845483661524,-223.75864059823));
#202143=CARTESIAN_POINT('Ctrl Pts',(-55.5162698042562,25.6962976868884,
-220.622576451631));
#202144=CARTESIAN_POINT('Ctrl Pts',(-57.5600729846415,27.8087001526143,
-217.486782588132));
#202145=CARTESIAN_POINT('Ctrl Pts',(-59.6038198261226,29.9212462142014,
-214.351060388696));
#202146=CARTESIAN_POINT('Ctrl Pts',(-47.3375387814793,17.1823623301207,
-233.18377696202));
#202147=CARTESIAN_POINT('Ctrl Pts',(-48.3615298096416,18.2217514970558,
-231.616266612933));
#202148=CARTESIAN_POINT('Ctrl Pts',(-49.3856802662736,19.2607945266738,
-230.048626531198));
#202149=CARTESIAN_POINT('Ctrl Pts',(-50.4098664093718,20.299771974626,-228.480964758552));
#202150=CARTESIAN_POINT('Ctrl Pts',(-51.43405255247,21.3387494225781,-226.913302985906));
#202151=CARTESIAN_POINT('Ctrl Pts',(-52.4582849722416,22.377636554534,-225.34560994901));
#202152=CARTESIAN_POINT('Ctrl Pts',(-53.4825352205651,23.4164945474948,
-223.777908916675));
#202153=CARTESIAN_POINT('Ctrl Pts',(-55.5310357172121,25.4942105334166,
-220.642506852006));
#202154=CARTESIAN_POINT('Ctrl Pts',(-57.5796085089827,27.5718067803009,
-217.507071482923));
#202155=CARTESIAN_POINT('Ctrl Pts',(-59.6282062333003,29.6493743968087,
-214.371636285096));
#202156=CARTESIAN_POINT('Ctrl Pts',(-47.3352334252266,17.1035049830549,
-233.199529035477));
#202157=CARTESIAN_POINT('Ctrl Pts',(-48.3600042849483,18.1301783396072,
-231.632852310436));
#202158=CARTESIAN_POINT('Ctrl Pts',(-49.3851454200133,19.1559450105208,
-230.065825712809));
#202159=CARTESIAN_POINT('Ctrl Pts',(-50.4104205557466,20.1813828669923,
-228.498672133956));
#202160=CARTESIAN_POINT('Ctrl Pts',(-51.4356956914798,21.2068207234638,
-226.931518555102));
#202161=CARTESIAN_POINT('Ctrl Pts',(-52.4611193627566,22.2318946684557,
-225.364224580397));
#202162=CARTESIAN_POINT('Ctrl Pts',(-53.4866146769212,23.2567945291104,
-223.79686392097));
#202163=CARTESIAN_POINT('Ctrl Pts',(-55.5376053052503,25.3065942504197,
-220.662142602115));
#202164=CARTESIAN_POINT('Ctrl Pts',(-57.5888779614229,27.3557092766758,
-217.527159175984));
#202165=CARTESIAN_POINT('Ctrl Pts',(-59.6402468289299,29.4046011172088,
-214.392093753442));
#202166=CARTESIAN_POINT('Ctrl Pts',(-47.3340807471002,17.0640763095221,
-233.207405072206));
#202167=CARTESIAN_POINT('Ctrl Pts',(-48.3592415226016,18.084391760883,-231.641145159187));
#202168=CARTESIAN_POINT('Ctrl Pts',(-49.3848779968831,19.1035202524442,
-230.074425303614));
#202169=CARTESIAN_POINT('Ctrl Pts',(-50.4106976289339,20.1221883131755,
-228.507525821657));
#202170=CARTESIAN_POINT('Ctrl Pts',(-51.4365172609848,21.1408563739068,
-226.9406263397));
#202171=CARTESIAN_POINT('Ctrl Pts',(-52.4625365580142,22.1590237254166,
-225.373531896091));
#202172=CARTESIAN_POINT('Ctrl Pts',(-53.4886544050993,23.1769445199182,
-223.806341423117));
#202173=CARTESIAN_POINT('Ctrl Pts',(-55.5408900992694,25.2127861089213,
-220.671960477169));
#202174=CARTESIAN_POINT('Ctrl Pts',(-57.593512687643,27.2476605248632,-217.537203022514));
#202175=CARTESIAN_POINT('Ctrl Pts',(-59.6462671267447,29.2822144774089,
-214.402322487616));
#202176=CARTESIAN_POINT('Ctrl Pts',(-47.3300959856285,17.0287621384219,
-233.217844880347));
#202177=CARTESIAN_POINT('Ctrl Pts',(-48.3560378107335,18.0419554383925,
-231.651416226232));
#202178=CARTESIAN_POINT('Ctrl Pts',(-49.3823066249335,19.0542905470043,
-230.08464943573));
#202179=CARTESIAN_POINT('Ctrl Pts',(-50.4087248511739,20.0662312984004,
-228.517726367742));
#202180=CARTESIAN_POINT('Ctrl Pts',(-51.4351430774143,21.0781720497965,
-226.950803299753));
#202181=CARTESIAN_POINT('Ctrl Pts',(-52.4617184722238,22.0896985728052,
-225.383716267118));
#202182=CARTESIAN_POINT('Ctrl Pts',(-53.4883790234851,23.1010010173179,
-223.816540379752));
#202183=CARTESIAN_POINT('Ctrl Pts',(-55.5417001260078,25.1236059063434,
-220.68218860502));
#202184=CARTESIAN_POINT('Ctrl Pts',(-57.5953541578395,27.1453352451054,
-217.54748972819));
#202185=CARTESIAN_POINT('Ctrl Pts',(-59.6491347229493,29.1667389675576,
-214.412662365356));
#202186=CARTESIAN_POINT('Ctrl Pts',(-47.3252263828413,16.9896223025012,
-233.229110072315));
#202187=CARTESIAN_POINT('Ctrl Pts',(-48.3518314896857,17.9964142568803,
-231.662398987523));
#202188=CARTESIAN_POINT('Ctrl Pts',(-49.3786544580299,19.0026193721543,
-230.095454289591));
#202189=CARTESIAN_POINT('Ctrl Pts',(-50.4055851760868,20.0085325545711,
-228.528392739382));
#202190=CARTESIAN_POINT('Ctrl Pts',(-51.4325158941438,21.0144457369877,
-226.961331189173));
#202191=CARTESIAN_POINT('Ctrl Pts',(-52.459558588544,22.0200559113108,-225.394148461867));
#202192=CARTESIAN_POINT('Ctrl Pts',(-53.4866652007083,23.0254932317529,
-223.826896445521));
#202193=CARTESIAN_POINT('Ctrl Pts',(-55.5408784250369,25.0363678726369,
-220.692392412828));
#202194=CARTESIAN_POINT('Ctrl Pts',(-57.5953414810798,27.046567195329,-217.557617709049));
#202195=CARTESIAN_POINT('Ctrl Pts',(-59.6499065909155,29.0564953668167,
-214.422734451764));
#202196=CARTESIAN_POINT('Ctrl Pts',(-47.3227915814476,16.9700523845408,
-233.234742668299));
#202197=CARTESIAN_POINT('Ctrl Pts',(-48.3497283291618,17.9736436661242,
-231.667890368169));
#202198=CARTESIAN_POINT('Ctrl Pts',(-49.3768283745781,18.9767837847294,
-230.100856716523));
#202199=CARTESIAN_POINT('Ctrl Pts',(-50.4040153385433,19.9796831826563,
-228.533725925203));
#202200=CARTESIAN_POINT('Ctrl Pts',(-51.4312023025085,20.9825825805833,
-226.966595133883));
#202201=CARTESIAN_POINT('Ctrl Pts',(-52.4584786467041,21.9852345805636,
-225.399364559241));
#202202=CARTESIAN_POINT('Ctrl Pts',(-53.4858082893199,22.9877393389703,
-223.832074478405));
#202203=CARTESIAN_POINT('Ctrl Pts',(-55.5404675745514,24.9927488557837,
-220.697494316732));
#202204=CARTESIAN_POINT('Ctrl Pts',(-57.5953351427,26.9971831704407,-217.562681699479));
#202205=CARTESIAN_POINT('Ctrl Pts',(-59.6502925248986,29.0013735664462,
-214.427770494967));
#202206=CARTESIAN_POINT('Ctrl Pts',(-47.3201275842246,16.9495165547055,
-233.240576377928));
#202207=CARTESIAN_POINT('Ctrl Pts',(-48.3473719504709,17.9500807957729,
-231.67355223474));
#202208=CARTESIAN_POINT('Ctrl Pts',(-49.3747299988842,18.9503241764231,
-230.106397960498));
#202209=CARTESIAN_POINT('Ctrl Pts',(-50.4021522240997,19.9503861234,-228.539169864665));
#202210=CARTESIAN_POINT('Ctrl Pts',(-51.4295744493152,20.9504480703769,
-226.97194176883));
#202211=CARTESIAN_POINT('Ctrl Pts',(-52.4570622538851,21.9503247000739,
-225.40463829887));
#202212=CARTESIAN_POINT('Ctrl Pts',(-53.4845908245458,22.9500863858554,
-223.837287994071));
#202213=CARTESIAN_POINT('Ctrl Pts',(-55.539647965867,24.9496097574185,-220.702587384473));
#202214=CARTESIAN_POINT('Ctrl Pts',(-57.5948645555888,26.9486836845843,
-217.56770364283));
#202215=CARTESIAN_POINT('Ctrl Pts',(-59.6501540472924,28.9475552769007,
-214.432737386764));
#202216=CARTESIAN_POINT('Ctrl Pts',(-47.317375174873,16.9271166732568,-233.246414795271));
#202217=CARTESIAN_POINT('Ctrl Pts',(-48.3448826696721,17.9249382396269,
-231.679221637881));
#202218=CARTESIAN_POINT('Ctrl Pts',(-49.3724670545446,18.9225395323645,
-230.111938592781));
#202219=CARTESIAN_POINT('Ctrl Pts',(-50.4000965635423,19.9200114073275,
-228.544602587596));
#202220=CARTESIAN_POINT('Ctrl Pts',(-51.42772607254,20.9174832822903,-226.977266582412));
#202221=CARTESIAN_POINT('Ctrl Pts',(-52.4554015221151,21.9148234426101,
-225.409876692422));
#202222=CARTESIAN_POINT('Ctrl Pts',(-53.4831063385788,22.9120795922463,
-223.842452376097));
#202223=CARTESIAN_POINT('Ctrl Pts',(-55.5385159715063,24.9065918915186,
-220.707603743446));
#202224=CARTESIAN_POINT('Ctrl Pts',(-57.5940405653775,26.9007754041514,
-217.572620374409));
#202225=CARTESIAN_POINT('Ctrl Pts',(-59.6496198849772,28.8948045789125,
-214.437573677779));
#202226=CARTESIAN_POINT('Ctrl Pts',(-47.3159989701972,16.9159167325326,
-233.249334003942));
#202227=CARTESIAN_POINT('Ctrl Pts',(-48.3436380292726,17.9123669615539,
-231.682056339452));
#202228=CARTESIAN_POINT('Ctrl Pts',(-49.3713355823747,18.9086472103352,
-230.114708908922));
#202229=CARTESIAN_POINT('Ctrl Pts',(-50.3990687332636,19.9048240492912,
-228.547318949062));
#202230=CARTESIAN_POINT('Ctrl Pts',(-51.4268018841524,20.9010008882471,
-226.979928989203));
#202231=CARTESIAN_POINT('Ctrl Pts',(-52.45457115623,21.8970728138782,-225.412495889199));
#202232=CARTESIAN_POINT('Ctrl Pts',(-53.4823640955953,22.8930761954416,
-223.84503456711));
#202233=CARTESIAN_POINT('Ctrl Pts',(-55.537949974326,24.8850829585685,-220.710111922933));
#202234=CARTESIAN_POINT('Ctrl Pts',(-57.5936285702719,26.8768212639349,
-217.575078740198));
#202235=CARTESIAN_POINT('Ctrl Pts',(-59.6493528038196,28.8684292299185,
-214.439991823286));
#202236=CARTESIAN_POINT('Ctrl Pts',(-47.3145992078122,16.9042529363287,
-233.252255026597));
#202237=CARTESIAN_POINT('Ctrl Pts',(-48.342359204181,17.8994019124442,-231.684893211564));
#202238=CARTESIAN_POINT('Ctrl Pts',(-49.3701622440295,18.8944243694381,
-230.117479224879));
#202239=CARTESIAN_POINT('Ctrl Pts',(-50.3979922061516,19.8893677455407,
-228.55003257268));
#202240=CARTESIAN_POINT('Ctrl Pts',(-51.4258221682736,20.8843111216433,
-226.982585920481));
#202241=CARTESIAN_POINT('Ctrl Pts',(-52.4536793921196,21.8791744293876,
-225.41510619931));
#202242=CARTESIAN_POINT('Ctrl Pts',(-53.4815548458549,22.8739843484231,
-223.847604402904));
#202243=CARTESIAN_POINT('Ctrl Pts',(-55.5373057533255,24.8636041864943,
-220.712600810094));
#202244=CARTESIAN_POINT('Ctrl Pts',(-57.5931281378066,26.8530147412008,
-217.577510678694));
#202245=CARTESIAN_POINT('Ctrl Pts',(-59.6489867620326,28.8423205147682,
-214.442377165073));
#202246=CARTESIAN_POINT('Ctrl Pts',(-47.3131850756779,16.8920273532507,
-233.255157881008));
#202247=CARTESIAN_POINT('Ctrl Pts',(-48.3410552958596,17.8859535740668,
-231.68771449894));
#202248=CARTESIAN_POINT('Ctrl Pts',(-49.3689559345468,18.8797895866585,
-230.120233792132));
#202249=CARTESIAN_POINT('Ctrl Pts',(-50.3968759670817,19.8735681235901,
-228.552729269786));
#202250=CARTESIAN_POINT('Ctrl Pts',(-51.4247959996165,20.8673466605217,
-226.98522474744));
#202251=CARTESIAN_POINT('Ctrl Pts',(-52.4527356437508,21.8610670819393,
-225.417696146955));
#202252=CARTESIAN_POINT('Ctrl Pts',(-53.4806885888443,22.8547481865589,
-223.850151240679));
#202253=CARTESIAN_POINT('Ctrl Pts',(-55.5365944790313,24.8421103957982,
-220.715061428126));
#202254=CARTESIAN_POINT('Ctrl Pts',(-57.5925525533974,26.8293183807281,
-217.579907651647));
#202255=CARTESIAN_POINT('Ctrl Pts',(-59.6485376230928,28.8164474339779,
-214.444721098757));
#202256=CARTESIAN_POINT('Ctrl Pts',(-47.3124780096108,16.8859145617117,
-233.256609308214));
#202257=CARTESIAN_POINT('Ctrl Pts',(-48.3404033416989,17.879229404878,-231.689125142628));
#202258=CARTESIAN_POINT('Ctrl Pts',(-49.3683527798054,18.8724721952687,
-230.121611075758));
#202259=CARTESIAN_POINT('Ctrl Pts',(-50.3963178475467,19.8656683126149,
-228.554077618338));
#202260=CARTESIAN_POINT('Ctrl Pts',(-51.424282915288,20.8588644299609,-226.986544160919));
#202261=CARTESIAN_POINT('Ctrl Pts',(-52.4522637695665,21.8520134082152,
-225.418991120778));
#202262=CARTESIAN_POINT('Ctrl Pts',(-53.480255460339,22.8451301056268,-223.851424659566));
#202263=CARTESIAN_POINT('Ctrl Pts',(-55.5362388418842,24.83136350045,-220.716291737142));
#202264=CARTESIAN_POINT('Ctrl Pts',(-57.5922647611927,26.8174702004918,
-217.581106138124));
#202265=CARTESIAN_POINT('Ctrl Pts',(-59.6483130536229,28.8035108935828,
-214.4458930656));
#202266=CARTESIAN_POINT('Ctrl Pts',(-47.3117672667176,16.8796614828891,
-233.258056246654));
#202267=CARTESIAN_POINT('Ctrl Pts',(-48.3397450538273,17.8723845217414,
-231.690531924442));
#202268=CARTESIAN_POINT('Ctrl Pts',(-49.3677413331199,18.8650518969515,
-230.122984445821));
#202269=CARTESIAN_POINT('Ctrl Pts',(-50.3957497606693,19.8576827301003,
-228.555421751598));
#202270=CARTESIAN_POINT('Ctrl Pts',(-51.4237581882186,20.8503135632492,
-226.987859057374));
#202271=CARTESIAN_POINT('Ctrl Pts',(-52.4517788757404,21.8429075199303,
-225.420281009185));
#202272=CARTESIAN_POINT('Ctrl Pts',(-53.4798080609562,22.835475963723,-223.852692331251));
#202273=CARTESIAN_POINT('Ctrl Pts',(-55.5358664313876,24.8206128513086,
-220.717514975384));
#202274=CARTESIAN_POINT('Ctrl Pts',(-57.5919581746568,26.8056495551953,
-217.582295877378));
#202275=CARTESIAN_POINT('Ctrl Pts',(-59.6480677075794,28.790633246673,-214.447054670791));
#202276=CARTESIAN_POINT('Ctrl Pts',(-47.3110535174895,16.873256830116,-233.259496526039));
#202277=CARTESIAN_POINT('Ctrl Pts',(-48.3390812029547,17.8654084135782,
-231.691932847844));
#202278=CARTESIAN_POINT('Ctrl Pts',(-49.3671224159146,18.8575190179354,
-230.124352092621));
#202279=CARTESIAN_POINT('Ctrl Pts',(-50.3951725945636,19.8496024611769,
-228.556760010403));
#202280=CARTESIAN_POINT('Ctrl Pts',(-51.4232227732125,20.8416859044184,
-226.989167928185));
#202281=CARTESIAN_POINT('Ctrl Pts',(-52.4512819949066,21.8337419536198,
-225.421564422348));
#202282=CARTESIAN_POINT('Ctrl Pts',(-53.4793475235956,22.8257789108232,
-223.853952950714));
#202283=CARTESIAN_POINT('Ctrl Pts',(-55.5354785809735,24.8098528252302,
-220.718730007446));
#202284=CARTESIAN_POINT('Ctrl Pts',(-57.5916344152767,26.7938517410564,
-217.583475771517));
#202285=CARTESIAN_POINT('Ctrl Pts',(-59.6478035550371,28.7778105309341,
-214.448204781494));
#202286=CARTESIAN_POINT('Ctrl Pts',(-47.3103397682614,16.8668521773429,
-233.260936805424));
#202287=CARTESIAN_POINT('Ctrl Pts',(-48.3384173520821,17.8584323054149,
-231.693333771247));
#202288=CARTESIAN_POINT('Ctrl Pts',(-49.3665034987094,18.8499861389194,
-230.125719739421));
#202289=CARTESIAN_POINT('Ctrl Pts',(-50.3945954284579,19.8415221922535,
-228.558098269208));
#202290=CARTESIAN_POINT('Ctrl Pts',(-51.4226873582065,20.8330582455877,
-226.990476798996));
#202291=CARTESIAN_POINT('Ctrl Pts',(-52.4507851140727,21.8245763873091,
-225.422847835511));
#202292=CARTESIAN_POINT('Ctrl Pts',(-53.4788869862349,22.8160818579234,
-223.855213570177));
#202293=CARTESIAN_POINT('Ctrl Pts',(-55.5350907305594,24.7990927991518,
-220.719945039509));
#202294=CARTESIAN_POINT('Ctrl Pts',(-57.5913106558967,26.7820539269176,
-217.584655665656));
#202295=CARTESIAN_POINT('Ctrl Pts',(-59.6475394024948,28.7649878151953,
-214.449354892196));
#202296=CARTESIAN_POINT('Ctrl Pts',(-47.3110520982437,16.8559465263517,
-233.26053824229));
#202297=CARTESIAN_POINT('Ctrl Pts',(-48.3391380137511,17.8470909658639,
-231.692946212383));
#202298=CARTESIAN_POINT('Ctrl Pts',(-49.3672339116285,18.8382047449221,
-230.125341393407));
#202299=CARTESIAN_POINT('Ctrl Pts',(-50.3953364602535,19.82929801124,-228.55772801405));
#202300=CARTESIAN_POINT('Ctrl Pts',(-51.4234390088786,20.8203912775578,
-226.990114634692));
#202301=CARTESIAN_POINT('Ctrl Pts',(-52.4515482625761,21.8114638664511,
-225.422492626496));
#202302=CARTESIAN_POINT('Ctrl Pts',(-53.4796622004807,22.8025219415151,
-223.854864559695));
#202303=CARTESIAN_POINT('Ctrl Pts',(-55.5358900762899,24.7846380916432,
-220.719608426093));
#202304=CARTESIAN_POINT('Ctrl Pts',(-57.5921363546469,26.7666972063695,
-217.58432848346));
#202305=CARTESIAN_POINT('Ctrl Pts',(-59.6483924596735,28.7487254799229,
-214.449035662994));
#202306=CARTESIAN_POINT('Ctrl Pts',(-47.3114554705886,16.8460380888807,
-233.260539515782));
#202307=CARTESIAN_POINT('Ctrl Pts',(-48.3395590816568,17.8367146054412,
-231.692947455239));
#202308=CARTESIAN_POINT('Ctrl Pts',(-49.3676726219367,18.8273604593628,
-230.125342611939));
#202309=CARTESIAN_POINT('Ctrl Pts',(-50.3957927612346,19.8179857984423,
-228.557729212486));
#202310=CARTESIAN_POINT('Ctrl Pts',(-51.4239129005325,20.8086111375217,
-226.990115813032));
#202311=CARTESIAN_POINT('Ctrl Pts',(-52.4520396931497,21.7992157970736,
-225.422493789));
#202312=CARTESIAN_POINT('Ctrl Pts',(-53.480171119088,22.7898059407486,-223.854865709355));
#202313=CARTESIAN_POINT('Ctrl Pts',(-55.5364339709647,24.7709862280985,
-220.719609550066));
#202314=CARTESIAN_POINT('Ctrl Pts',(-57.5927150219887,26.7521094718628,
-217.584329593504));
#202315=CARTESIAN_POINT('Ctrl Pts',(-59.6490056999632,28.7332018665566,
-214.449036765473));
#202316=CARTESIAN_POINT('',(-47.0649767742812,18.6816981840219,-232.850050031414));
#202317=CARTESIAN_POINT('',(-47.5797438888055,17.1282946860168,-232.850050025775));
#202318=CARTESIAN_POINT('Ctrl Pts',(-47.0649772746806,18.681698503234,-232.85005));
#202319=CARTESIAN_POINT('Ctrl Pts',(-47.0897739050568,18.6428271142161,
-232.85005));
#202320=CARTESIAN_POINT('Ctrl Pts',(-47.1311006982707,18.5775957466655,
-232.850050000004));
#202321=CARTESIAN_POINT('Ctrl Pts',(-47.194785050436,18.4616925010307,-232.850050000004));
#202322=CARTESIAN_POINT('Ctrl Pts',(-47.2287770053728,18.3950676863438,
-232.850049999972));
#202323=CARTESIAN_POINT('Ctrl Pts',(-47.294963678024,18.2630532098196,-232.850049999972));
#202324=CARTESIAN_POINT('Ctrl Pts',(-47.3298979480949,18.1874159971604,
-232.850050000077));
#202325=CARTESIAN_POINT('Ctrl Pts',(-47.3845235381683,18.0516462813532,
-232.850050000077));
#202326=CARTESIAN_POINT('Ctrl Pts',(-47.4068726947903,17.992614936778,-232.850050003188));
#202327=CARTESIAN_POINT('Ctrl Pts',(-47.4814502842607,17.7794293002805,
-232.850050003188));
#202328=CARTESIAN_POINT('Ctrl Pts',(-47.5068744752097,17.6686904849674,
-232.85005000024));
#202329=CARTESIAN_POINT('Ctrl Pts',(-47.5415713170795,17.4960000874156,
-232.85005000024));
#202330=CARTESIAN_POINT('Ctrl Pts',(-47.5519413173953,17.4283876884363,
-232.85005));
#202331=CARTESIAN_POINT('Ctrl Pts',(-47.5744439294891,17.2490905556932,
-232.85005));
#202332=CARTESIAN_POINT('Ctrl Pts',(-47.5778164032854,17.1751517854889,
-232.85005));
#202333=CARTESIAN_POINT('Ctrl Pts',(-47.5797441362696,17.1282946961977,
-232.85005));
#202334=CARTESIAN_POINT('',(-57.6802384504567,34.1916870210802,-214.317651768483));
#202335=CARTESIAN_POINT('Ctrl Pts',(-47.0649765291407,18.6816980387269,
-232.850049769526));
#202336=CARTESIAN_POINT('Ctrl Pts',(-48.8271545273793,21.2716434707432,
-229.763670058287));
#202337=CARTESIAN_POINT('Ctrl Pts',(-50.591632449928,23.8587524581056,-226.676983143055));
#202338=CARTESIAN_POINT('Ctrl Pts',(-52.3593744293695,26.4424372048812,
-223.590052929728));
#202339=CARTESIAN_POINT('Ctrl Pts',(-54.1292305723972,29.029211957027,-220.499430845344));
#202340=CARTESIAN_POINT('Ctrl Pts',(-55.9023386650238,31.6125563678527,
-217.408555364207));
#202341=CARTESIAN_POINT('Ctrl Pts',(-57.6802383718549,34.1916869226675,
-214.317651641153));
#202342=CARTESIAN_POINT('',(-59.5599473199192,29.0716011550534,-214.548757454512));
#202343=CARTESIAN_POINT('Ctrl Pts',(-57.6802384190918,34.1916870036612,
-214.317652095804));
#202344=CARTESIAN_POINT('Ctrl Pts',(-57.711076640637,34.1523839213935,-214.318515519703));
#202345=CARTESIAN_POINT('Ctrl Pts',(-57.7444787407025,34.1091244974209,
-214.319516304586));
#202346=CARTESIAN_POINT('Ctrl Pts',(-57.8155385849082,34.015034636639,-214.321768181642));
#202347=CARTESIAN_POINT('Ctrl Pts',(-57.8508234071904,33.9673227106125,
-214.32296093355));
#202348=CARTESIAN_POINT('Ctrl Pts',(-57.9661234018488,33.808083144089,-214.32727701056));
#202349=CARTESIAN_POINT('Ctrl Pts',(-58.0434074298098,33.6958767305163,
-214.331195699283));
#202350=CARTESIAN_POINT('Ctrl Pts',(-58.1756532244509,33.494224655047,-214.338033936497));
#202351=CARTESIAN_POINT('Ctrl Pts',(-58.232181736934,33.4045586829591,-214.340952245208));
#202352=CARTESIAN_POINT('Ctrl Pts',(-58.3756461184004,33.1676840614597,
-214.348689659445));
#202353=CARTESIAN_POINT('Ctrl Pts',(-58.4602479257778,33.0184255663356,
-214.353756590895));
#202354=CARTESIAN_POINT('Ctrl Pts',(-58.6568844792436,32.6464976653465,
-214.368544945655));
#202355=CARTESIAN_POINT('Ctrl Pts',(-58.7646217839408,32.4201536609433,
-214.377793138464));
#202356=CARTESIAN_POINT('Ctrl Pts',(-58.9195386091013,32.0554702583991,
-214.392846705456));
#202357=CARTESIAN_POINT('Ctrl Pts',(-58.9732785720301,31.9197057886375,
-214.398754579606));
#202358=CARTESIAN_POINT('Ctrl Pts',(-59.1078149579114,31.5535708296281,
-214.415391307452));
#202359=CARTESIAN_POINT('Ctrl Pts',(-59.1824588553433,31.3211191065939,
-214.426591762046));
#202360=CARTESIAN_POINT('Ctrl Pts',(-59.2717173594901,30.9979484732358,
-214.442018247786));
#202361=CARTESIAN_POINT('Ctrl Pts',(-59.2947355260442,30.9092561462526,
-214.446284061646));
#202362=CARTESIAN_POINT('Ctrl Pts',(-59.3544699104766,30.6634680433675,
-214.458293748765));
#202363=CARTESIAN_POINT('Ctrl Pts',(-59.3882196655572,30.5059342511556,
-214.466398394897));
#202364=CARTESIAN_POINT('Ctrl Pts',(-59.4590872539795,30.1244208307377,
-214.487274531048));
#202365=CARTESIAN_POINT('Ctrl Pts',(-59.492072393894,29.8990070152149,-214.499666866019));
#202366=CARTESIAN_POINT('Ctrl Pts',(-59.5376880887931,29.4727426572454,
-214.524039704186));
#202367=CARTESIAN_POINT('Ctrl Pts',(-59.5522340174229,29.2722643299,-214.536262708201));
#202368=CARTESIAN_POINT('Ctrl Pts',(-59.559947319918,29.0716011550592,-214.548757454604));
#202369=CARTESIAN_POINT('',(-59.5744430571196,28.6979747816093,-214.56059856522));
#202370=CARTESIAN_POINT('Ctrl Pts',(-59.5599473199158,29.0716011550593,
-214.548757454608));
#202371=CARTESIAN_POINT('Ctrl Pts',(-59.562335847696,29.0094631058835,-214.552626620787));
#202372=CARTESIAN_POINT('Ctrl Pts',(-59.5647394386419,28.9472090864927,
-214.555583575921));
#202373=CARTESIAN_POINT('Ctrl Pts',(-59.5683821822733,28.8533107884066,
-214.558574296067));
#202374=CARTESIAN_POINT('Ctrl Pts',(-59.5696089211159,28.8217653832972,
-214.559329741406));
#202375=CARTESIAN_POINT('Ctrl Pts',(-59.5720174159227,28.7599810676145,
-214.560318279807));
#202376=CARTESIAN_POINT('Ctrl Pts',(-59.5727190081475,28.7420025676919,
-214.5605526967));
#202377=CARTESIAN_POINT('Ctrl Pts',(-59.5744429767042,28.6979747794686,
-214.560599513176));
#202378=CARTESIAN_POINT('Ctrl Pts',(-59.5744427861971,28.6979745676234,
-214.560598252186));
#202379=CARTESIAN_POINT('Ctrl Pts',(-55.5761465166849,24.8416079159138,
-220.657162906121));
#202380=CARTESIAN_POINT('Ctrl Pts',(-51.5778799971753,20.9851500975526,
-226.753689417593));
#202381=CARTESIAN_POINT('Ctrl Pts',(-47.5797437329671,17.1282947147807,
-232.85004994177));
#202382=CARTESIAN_POINT('Origin',(-41.5452362233251,-63.7990866568863,-205.306318983907));
#202383=CARTESIAN_POINT('',(-47.2772325636527,-70.8123207858077,-202.84995));
#202384=CARTESIAN_POINT('',(-41.9017397792002,-72.8497297394107,-202.84995));
#202385=CARTESIAN_POINT('Origin',(-41.5452362233251,-63.7990866568863,-202.84995));
#202386=CARTESIAN_POINT('',(-41.9000522051254,-72.8068868830794,-205.306318983907));
#202387=CARTESIAN_POINT('',(-47.1516276096018,-70.6586401308143,-214.220867040027));
#202388=CARTESIAN_POINT('Ctrl Pts',(-47.1516276096073,-70.658640130818,
-214.220867039664));
#202389=CARTESIAN_POINT('Ctrl Pts',(-47.1049465298323,-70.69680049246,-214.220539579083));
#202390=CARTESIAN_POINT('Ctrl Pts',(-47.0581254645236,-70.7342797725851,
-214.220714572147));
#202391=CARTESIAN_POINT('Ctrl Pts',(-46.9626662222933,-70.8090665014231,
-214.222095580797));
#202392=CARTESIAN_POINT('Ctrl Pts',(-46.9147757072847,-70.8457911604741,
-214.22327290135));
#202393=CARTESIAN_POINT('Ctrl Pts',(-46.8664918175106,-70.8820283127247,
-214.224988432219));
#202394=CARTESIAN_POINT('',(-47.250099122033,-70.7791223733342,-205.306318983907));
#202395=CARTESIAN_POINT('Origin',(0.,-12.9675000200281,-205.306318983907));
#202396=CARTESIAN_POINT('Ctrl Pts',(-50.9302694868398,-67.3511117059353,
-214.24934096937));
#202397=CARTESIAN_POINT('Ctrl Pts',(-50.6301450874489,-67.632232782722,
-214.247062743179));
#202398=CARTESIAN_POINT('Ctrl Pts',(-50.3277270490238,-67.9108411525188,
-214.244646208669));
#202399=CARTESIAN_POINT('Ctrl Pts',(-49.7080810419159,-68.4722815054349,
-214.240153263143));
#202400=CARTESIAN_POINT('Ctrl Pts',(-49.3907687173044,-68.7548784334755,
-214.238095007483));
#202401=CARTESIAN_POINT('Ctrl Pts',(-48.4391587456012,-69.5878975441349,
-214.231198509907));
#202402=CARTESIAN_POINT('Ctrl Pts',(-47.7996962354631,-70.1288637578241,
-214.22541314119));
#202403=CARTESIAN_POINT('Ctrl Pts',(-47.1516276096073,-70.658640130818,
-214.220867039664));
#202404=CARTESIAN_POINT('',(-57.55661147574,-60.2824542804282,-214.249782619794));
#202405=CARTESIAN_POINT('Ctrl Pts',(-57.5566114760922,-60.2824542808246,
-214.249782589791));
#202406=CARTESIAN_POINT('Ctrl Pts',(-57.0250153197209,-60.929054875926,
-214.252086125668));
#202407=CARTESIAN_POINT('Ctrl Pts',(-56.4825490090204,-61.5666907434623,
-214.255305282271));
#202408=CARTESIAN_POINT('Ctrl Pts',(-55.3753515248431,-62.8244435222611,
-214.258374348072));
#202409=CARTESIAN_POINT('Ctrl Pts',(-54.8117226671775,-63.4434099521044,
-214.259195881147));
#202410=CARTESIAN_POINT('Ctrl Pts',(-54.2386983288856,-64.0517945375328,
-214.260116172733));
#202411=CARTESIAN_POINT('',(-57.7103246972002,-60.4088156810276,-202.84995));
#202412=CARTESIAN_POINT('',(-57.677203474973,-60.3815880685163,-205.306318983907));
#202413=CARTESIAN_POINT('Origin',(0.,-12.9675000200281,-202.84995));
#202414=CARTESIAN_POINT('Origin',(-50.7133971693864,-54.6569255427236,-205.306318983907));
#202415=CARTESIAN_POINT('',(-59.7639914300581,-55.014666400457,-202.84995));
#202416=CARTESIAN_POINT('Origin',(-50.7133971693864,-54.6569255427236,-202.84995));
#202417=CARTESIAN_POINT('Origin',(-53.6115278221397,-57.0237333927552,-218.549922256745));
#202418=CARTESIAN_POINT('',(-59.7211488048338,-55.0129729693901,-205.306318983907));
#202419=CARTESIAN_POINT('Origin',(-50.7133971693864,28.7219255026674,-205.306318983907));
#202420=CARTESIAN_POINT('',(-57.7103246972002,34.4738156409714,-202.84995));
#202421=CARTESIAN_POINT('',(-59.7639914300583,29.0796663604006,-202.84995));
#202422=CARTESIAN_POINT('Origin',(-50.7133971693864,28.7219255026674,-202.84995));
#202423=CARTESIAN_POINT('',(-59.7211488048339,29.0779729293336,-205.306318983907));
#202424=CARTESIAN_POINT('',(-57.555715349607,34.3467175710979,-214.316254908503));
#202425=CARTESIAN_POINT('Origin',(-53.918424535989,31.3368194791983,-218.660877916293));
#202426=CARTESIAN_POINT('',(-57.677203474973,34.44658802846,-205.306318983907));
#202427=CARTESIAN_POINT('Origin',(0.,-12.9675000200281,-205.306318983907));
#202428=CARTESIAN_POINT('',(-46.8872094279775,44.936516366183,-214.320099730218));
#202429=CARTESIAN_POINT('Ctrl Pts',(-46.8872094285464,44.9365163666477,
-214.32009968902));
#202430=CARTESIAN_POINT('Ctrl Pts',(-47.5890114515051,44.368165416605,-214.323378596591));
#202431=CARTESIAN_POINT('Ctrl Pts',(-48.2806521881363,43.7869284638981,
-214.327270067522));
#202432=CARTESIAN_POINT('Ctrl Pts',(-49.2784687584601,42.9168915640759,
-214.330851585581));
#202433=CARTESIAN_POINT('Ctrl Pts',(-49.5914691205952,42.6393040561203,
-214.331776628684));
#202434=CARTESIAN_POINT('Ctrl Pts',(-50.2053425551683,42.0855623761046,
-214.333899644539));
#202435=CARTESIAN_POINT('Ctrl Pts',(-50.506054266235,41.8097922959792,-214.335007679769));
#202436=CARTESIAN_POINT('Ctrl Pts',(-50.804536443953,41.5315226006458,-214.335913275952));
#202437=CARTESIAN_POINT('',(-47.0132029332902,45.0921138114136,-202.84995));
#202438=CARTESIAN_POINT('',(-46.9862210240714,45.0587921244845,-205.306318983907));
#202439=CARTESIAN_POINT('Origin',(0.,-12.9675000200281,-202.84995));
#202440=CARTESIAN_POINT('Ctrl Pts',(-54.1218033362461,38.2387592926023,
-214.333529894748));
#202441=CARTESIAN_POINT('Ctrl Pts',(-54.3992526046939,37.9455431189732,
-214.332337047462));
#202442=CARTESIAN_POINT('Ctrl Pts',(-54.6742923213544,37.6501031166571,
-214.331036263298));
#202443=CARTESIAN_POINT('Ctrl Pts',(-55.2277092285518,37.0458584843467,
-214.328741493667));
#202444=CARTESIAN_POINT('Ctrl Pts',(-55.5058839842676,36.7369811431027,
-214.327762901693));
#202445=CARTESIAN_POINT('Ctrl Pts',(-56.3870207183081,35.7419812347418,
-214.323805214881));
#202446=CARTESIAN_POINT('Ctrl Pts',(-56.9779401341808,35.0494690118534,
-214.319418635742));
#202447=CARTESIAN_POINT('Ctrl Pts',(-57.5557151719484,34.346717423436,-214.316255263493));
#202448=CARTESIAN_POINT('Origin',(-41.3132181298675,38.0528376956935,-205.306318983907));
#202449=CARTESIAN_POINT('',(-43.0099907914441,46.9501517582364,-202.84995));
#202450=CARTESIAN_POINT('Origin',(-41.3132181298675,38.0528376956935,-202.84995));
#202451=CARTESIAN_POINT('Origin',(-43.9075665164217,41.2822320849722,-218.664372653694));
#202452=CARTESIAN_POINT('',(-43.001958811097,46.9080347125589,-205.306318983907));
#202453=CARTESIAN_POINT('Origin',(1004.,-12.967500020028,-179.606318983907));
#202454=CARTESIAN_POINT('',(-62.6666822880186,29.1944003864053,-179.64995));
#202455=CARTESIAN_POINT('',(-62.6666822880186,-55.1294004264619,-179.64995));
#202456=CARTESIAN_POINT('Origin',(1004.,-12.967500020028,-179.64995));
#202457=CARTESIAN_POINT('',(-62.2620407574844,-55.1134062492798,-202.84995));
#202458=CARTESIAN_POINT('',(-62.6674432759983,-55.1294305058671,-179.606318983907));
#202459=CARTESIAN_POINT('',(-62.2620407574844,29.1784062092233,-202.84995));
#202460=CARTESIAN_POINT('Origin',(1004.,-12.967500020028,-202.84995));
#202461=CARTESIAN_POINT('',(-62.6674432759984,29.1944304658105,-179.606318983907));
#202462=CARTESIAN_POINT('Origin',(-50.7133971693864,28.7219255026673,-179.606318983907));
#202463=CARTESIAN_POINT('',(-59.9543671306402,36.3185518471891,-179.64995));
#202464=CARTESIAN_POINT('Origin',(-50.7133971693864,28.7219255026673,-179.64995));
#202465=CARTESIAN_POINT('',(-59.6415426483635,36.0613915368278,-202.84995));
#202466=CARTESIAN_POINT('Origin',(-50.7133971693864,28.7219255026674,-202.84995));
#202467=CARTESIAN_POINT('',(-59.9549554431411,36.3190354750184,-179.606318983907));
#202468=CARTESIAN_POINT('Origin',(0.,-12.9675000200281,-179.606318983907));
#202469=CARTESIAN_POINT('',(-48.8412921507357,47.3497382103492,-179.64995));
#202470=CARTESIAN_POINT('Origin',(0.,-12.9675000200281,-179.64995));
#202471=CARTESIAN_POINT('',(-48.5864524674565,47.0350203720195,-202.84995));
#202472=CARTESIAN_POINT('Origin',(0.,-12.9675000200281,-202.84995));
#202473=CARTESIAN_POINT('',(-48.8417714142841,47.3503300835849,-179.606318983907));
#202474=CARTESIAN_POINT('Origin',(-41.3132181298675,38.0528376956935,-179.606318983907));
#202475=CARTESIAN_POINT('',(-43.5541767698386,49.8036828575113,-179.64995));
#202476=CARTESIAN_POINT('Origin',(-41.3132181298675,38.0528376956935,-179.64995));
#202477=CARTESIAN_POINT('',(-43.478316039927,49.4058943061501,-202.84995));
#202478=CARTESIAN_POINT('Origin',(-41.3132181298675,38.0528376956935,-202.84995));
#202479=CARTESIAN_POINT('',(-43.5543194371113,49.8044309574546,-179.606318983907));
#202480=CARTESIAN_POINT('Origin',(-41.5452362233251,-63.7990866568863,-179.606318983907));
#202481=CARTESIAN_POINT('',(-49.1155884655664,-73.0615930440079,-179.64995));
#202482=CARTESIAN_POINT('',(-42.0160769799045,-75.7524362554308,-179.64995));
#202483=CARTESIAN_POINT('Origin',(-41.5452362233251,-63.7990866568863,-179.64995));
#202484=CARTESIAN_POINT('',(-42.0001381210477,-75.3477925421285,-202.84995));
#202485=CARTESIAN_POINT('',(-42.0161069552755,-75.7531972475156,-179.606318983907));
#202486=CARTESIAN_POINT('',(-48.8593175837476,-72.7480395125837,-202.84995));
#202487=CARTESIAN_POINT('Origin',(-41.5452362233251,-63.7990866568863,-202.84995));
#202488=CARTESIAN_POINT('',(-49.1160704206943,-73.0621827275931,-179.606318983907));
#202489=CARTESIAN_POINT('Origin',(0.,-12.9675000200281,-179.606318983907));
#202490=CARTESIAN_POINT('',(-59.9543671306402,-62.2535518872453,-179.64995));
#202491=CARTESIAN_POINT('Origin',(0.,-12.9675000200281,-179.64995));
#202492=CARTESIAN_POINT('',(-59.6415426483635,-61.9963915768841,-202.84995));
#202493=CARTESIAN_POINT('Origin',(0.,-12.9675000200281,-202.84995));
#202494=CARTESIAN_POINT('',(-59.9549554431411,-62.2540355150746,-179.606318983907));
#202495=CARTESIAN_POINT('Origin',(-50.7133971693864,-54.6569255427236,-179.606318983907));
#202496=CARTESIAN_POINT('Origin',(-50.7133971693864,-54.6569255427236,-179.64995));
#202497=CARTESIAN_POINT('Origin',(-50.7133971693864,-54.6569255427236,-202.84995));
#202498=CARTESIAN_POINT('Ctrl Pts',(-47.7724784290048,-32.4865586987341,
-232.970973990925));
#202499=CARTESIAN_POINT('Ctrl Pts',(-51.8616631458841,-35.9897429718971,
-226.798709657862));
#202500=CARTESIAN_POINT('Ctrl Pts',(-55.9509791745034,-39.4923578424338,
-220.626231304292));
#202501=CARTESIAN_POINT('Ctrl Pts',(-60.0403077603802,-42.9948148700989,
-214.453693714461));
#202502=CARTESIAN_POINT('Ctrl Pts',(-47.6970999179399,-35.0937046824551,
-232.967721023846));
#202503=CARTESIAN_POINT('Ctrl Pts',(-51.7757137841176,-39.0045377390498,
-226.795568831742));
#202504=CARTESIAN_POINT('Ctrl Pts',(-55.8544675412487,-42.9147019697459,
-220.623140932772));
#202505=CARTESIAN_POINT('Ctrl Pts',(-59.9332050840609,-46.8246892042479,
-214.450640245293));
#202506=CARTESIAN_POINT('Ctrl Pts',(-47.6083941910801,-37.6707809958978,
-232.96396511673));
#202507=CARTESIAN_POINT('Ctrl Pts',(-51.6738491177805,-42.0114382175837,
-226.791891649754));
#202508=CARTESIAN_POINT('Ctrl Pts',(-55.7393519427245,-46.3514436774691,
-220.61950573142));
#202509=CARTESIAN_POINT('Ctrl Pts',(-59.8047170999058,-50.6912943906935,
-214.447047813144));
#202510=CARTESIAN_POINT('Ctrl Pts',(-47.5079779560868,-40.2034134198457,
-232.959831751742));
#202511=CARTESIAN_POINT('Ctrl Pts',(-51.5558271984379,-45.0119998619165,
-226.787659137649));
#202512=CARTESIAN_POINT('Ctrl Pts',(-55.603839292235,-49.8201780781628,
-220.615275392699));
#202513=CARTESIAN_POINT('Ctrl Pts',(-59.6518858770376,-54.6282695245469,
-214.442846690034));
#202514=CARTESIAN_POINT('',(-47.8511644985019,-32.6020541825732,-232.850071652982));
#202515=CARTESIAN_POINT('Ctrl Pts',(-47.8511937435036,-32.6021335774055,
-232.85005));
#202516=CARTESIAN_POINT('Ctrl Pts',(-47.8129987256184,-33.8832172184026,
-232.85005));
#202517=CARTESIAN_POINT('Ctrl Pts',(-47.7712743196189,-35.1649732916811,
-232.850050000001));
#202518=CARTESIAN_POINT('Ctrl Pts',(-47.6808913011582,-37.7267114902632,
-232.850050000001));
#202519=CARTESIAN_POINT('Ctrl Pts',(-47.632174582744,-39.0083318774293,
-232.85005));
#202520=CARTESIAN_POINT('Ctrl Pts',(-47.5799752941153,-40.2889415902927,
-232.85005));
#202521=CARTESIAN_POINT('',(-59.8539584057532,-46.7516625814213,-214.560265665659));
#202522=CARTESIAN_POINT('Ctrl Pts',(-47.8511937435036,-32.6021335774055,
-232.85005));
#202523=CARTESIAN_POINT('Ctrl Pts',(-49.7758731964884,-34.8662384268529,
-229.917938361341));
#202524=CARTESIAN_POINT('Ctrl Pts',(-52.006472582506,-37.4944438055142,
-226.519199319976));
#202525=CARTESIAN_POINT('Ctrl Pts',(-55.7540093824077,-41.913096923482,
-220.808621189981));
#202526=CARTESIAN_POINT('Ctrl Pts',(-57.9042257962353,-44.4502782877339,
-217.531776051457));
#202527=CARTESIAN_POINT('Ctrl Pts',(-59.8539550780142,-46.7516786354062,
-214.560279194377));
#202528=CARTESIAN_POINT('Ctrl Pts',(-59.8539609358732,-46.7516610380903,
-214.560271423235));
#202529=CARTESIAN_POINT('Ctrl Pts',(-59.8127437126638,-48.0499861504054,
-214.559533037022));
#202530=CARTESIAN_POINT('Ctrl Pts',(-59.769150621426,-49.34823472919,-214.558748583908));
#202531=CARTESIAN_POINT('Ctrl Pts',(-59.6772124392589,-51.9445894630669,
-214.557078958964));
#202532=CARTESIAN_POINT('Ctrl Pts',(-59.6288676637842,-53.242684640561,
-214.556193992093));
#202533=CARTESIAN_POINT('Ctrl Pts',(-59.5781472511379,-54.5406860123126,
-214.555282751789));
#202534=CARTESIAN_POINT('Ctrl Pts',(-47.5077687575999,17.0588630313157,
-232.959797430566));
#202535=CARTESIAN_POINT('Ctrl Pts',(-51.5543587613359,20.962467251341,-226.789554159174));
#202536=CARTESIAN_POINT('Ctrl Pts',(-55.6010831372117,24.8656613676635,
-220.619139657106));
#202537=CARTESIAN_POINT('Ctrl Pts',(-59.6478359854379,28.7687682426261,
-214.448688656128));
#202538=CARTESIAN_POINT('Ctrl Pts',(-47.6093150514154,14.5106669763354,
-232.963237198889));
#202539=CARTESIAN_POINT('Ctrl Pts',(-51.673625611954,17.943733161272,-226.793068881834));
#202540=CARTESIAN_POINT('Ctrl Pts',(-55.7379386239558,21.3761434795959,
-220.622650915033));
#202541=CARTESIAN_POINT('Ctrl Pts',(-59.8021028749556,24.8083979649139,
-214.45217527183));
#202542=CARTESIAN_POINT('Ctrl Pts',(-47.6990097155228,11.9175493678758,
-232.966275794525));
#202543=CARTESIAN_POINT('Ctrl Pts',(-51.7765308861555,14.9186157818217,
-226.796020622489));
#202544=CARTESIAN_POINT('Ctrl Pts',(-55.8541462985605,17.9190127102163,
-220.625556640966));
#202545=CARTESIAN_POINT('Ctrl Pts',(-59.9317344440901,20.9192322601435,
-214.455037317351));
#202546=CARTESIAN_POINT('Ctrl Pts',(-47.7752156818158,9.29411691894321,
-232.968782926844));
#202547=CARTESIAN_POINT('Ctrl Pts',(-51.8633248967382,11.8855265874929,
-226.79842796189));
#202548=CARTESIAN_POINT('Ctrl Pts',(-55.9515262957967,14.4763668580276,
-220.627916411389));
#202549=CARTESIAN_POINT('Ctrl Pts',(-60.0397300597283,17.0670490879089,
-214.457361414306));
#202550=CARTESIAN_POINT('',(-59.8522817919913,20.8670659745804,-214.56462304469));
#202551=CARTESIAN_POINT('Ctrl Pts',(-59.5744430045609,28.6979747791781,
-214.56059791914));
#202552=CARTESIAN_POINT('Ctrl Pts',(-59.6255523742397,27.3929948773216,
-214.561350802779));
#202553=CARTESIAN_POINT('Ctrl Pts',(-59.6742602842767,26.0879255239807,
-214.562076913704));
#202554=CARTESIAN_POINT('Ctrl Pts',(-59.7668739992229,23.4776071864522,
-214.563426526416));
#202555=CARTESIAN_POINT('Ctrl Pts',(-59.8107792490354,22.1723754160636,
-214.56404982166));
#202556=CARTESIAN_POINT('Ctrl Pts',(-59.8522830098483,20.8670660146469,
-214.564626087537));
#202557=CARTESIAN_POINT('',(-47.8524647801522,9.39110652846791,-232.850060330937));
#202558=CARTESIAN_POINT('Ctrl Pts',(-59.8522792844971,20.8670810655101,
-214.564630881667));
#202559=CARTESIAN_POINT('Ctrl Pts',(-57.9231698177518,19.0197028269434,
-217.504721577749));
#202560=CARTESIAN_POINT('Ctrl Pts',(-55.7588762173457,16.9478029332325,
-220.803047120975));
#202561=CARTESIAN_POINT('Ctrl Pts',(-52.0105370781302,13.362350606817,-226.514897697653));
#202562=CARTESIAN_POINT('Ctrl Pts',(-49.7764856318141,11.2269580602607,
-229.918931539958));
#202563=CARTESIAN_POINT('Ctrl Pts',(-47.8524795676142,9.39114590592674,
-232.85005));
#202564=CARTESIAN_POINT('Ctrl Pts',(-47.5797436947461,17.1282946781069,
-232.85005));
#202565=CARTESIAN_POINT('Ctrl Pts',(-47.6322830986109,15.839317171622,-232.85005));
#202566=CARTESIAN_POINT('Ctrl Pts',(-47.6812964150147,14.5493107491118,
-232.850050000002));
#202567=CARTESIAN_POINT('Ctrl Pts',(-47.7721850391671,11.9708027192453,
-232.850050000002));
#202568=CARTESIAN_POINT('Ctrl Pts',(-47.8141193819828,10.6806307165552,
-232.85005));
#202569=CARTESIAN_POINT('Ctrl Pts',(-47.8524795676142,9.39114590592674,
-232.85005));
#202570=CARTESIAN_POINT('Origin',(1004.,-12.967500020028,-205.306318983907));
#202571=CARTESIAN_POINT('Ctrl Pts',(-59.852283684575,20.8670529899755,-214.564611171477));
#202572=CARTESIAN_POINT('Ctrl Pts',(-59.9408921983977,18.6616086582029,
-213.507172831477));
#202573=CARTESIAN_POINT('Ctrl Pts',(-60.0187430617361,16.1586269377748,
-213.171736592191));
#202574=CARTESIAN_POINT('Ctrl Pts',(-60.0783440471533,13.709584889334,-213.274710076528));
#202575=CARTESIAN_POINT('Ctrl Pts',(-60.0869371638556,13.3564883090716,
-213.289556528511));
#202576=CARTESIAN_POINT('Ctrl Pts',(-60.0951902283565,13.0034719450298,
-213.313678069836));
#202577=CARTESIAN_POINT('Ctrl Pts',(-60.1030981576493,12.6512459219475,
-213.346442200715));
#202578=CARTESIAN_POINT('Ctrl Pts',(-60.1182284170081,11.9773310594209,
-213.409129887912));
#202579=CARTESIAN_POINT('Ctrl Pts',(-60.1324253703542,11.283793184265,-213.510071155534));
#202580=CARTESIAN_POINT('Ctrl Pts',(-60.1429164546448,10.7356826748675,
-213.608457606495));
#202581=CARTESIAN_POINT('Ctrl Pts',(-60.1466440184685,10.5409347489484,
-213.643415077543));
#202582=CARTESIAN_POINT('Ctrl Pts',(-60.1500513021095,10.3579630053009,
-213.678691006502));
#202583=CARTESIAN_POINT('Ctrl Pts',(-60.1532641850396,10.1814317298332,
-213.714618736487));
#202584=CARTESIAN_POINT('Ctrl Pts',(-60.1571763074451,9.96648086699788,
-213.758365639348));
#202585=CARTESIAN_POINT('Ctrl Pts',(-60.1608006466485,9.76108925215573,
-213.803062347838));
#202586=CARTESIAN_POINT('Ctrl Pts',(-60.1643187438617,9.55589232998761,
-213.850313921784));
#202587=CARTESIAN_POINT('Ctrl Pts',(-60.1647663228057,9.52978679163152,
-213.856325355888));
#202588=CARTESIAN_POINT('Ctrl Pts',(-60.1652121278246,9.50368446580759,
-213.862379491625));
#202589=CARTESIAN_POINT('Ctrl Pts',(-60.1656564875316,9.47756602057091,
-213.868480820893));
#202590=CARTESIAN_POINT('Ctrl Pts',(-60.1660491443594,9.4544865520864,-213.873872238157));
#202591=CARTESIAN_POINT('Ctrl Pts',(-60.1664410470052,9.43139075002581,
-213.879283604594));
#202592=CARTESIAN_POINT('Ctrl Pts',(-60.1668339732077,9.40824978917481,
-213.884647521255));
#202593=CARTESIAN_POINT('Ctrl Pts',(-60.1675888932482,9.36378959540123,
-213.894953090485));
#202594=CARTESIAN_POINT('Ctrl Pts',(-60.1683459618837,9.3191789651964,-213.905157368098));
#202595=CARTESIAN_POINT('Ctrl Pts',(-60.1691067978077,9.27432300489259,
-213.91527730166));
#202596=CARTESIAN_POINT('Ctrl Pts',(-60.1705954940517,9.1865551990907,-213.935078557894));
#202597=CARTESIAN_POINT('Ctrl Pts',(-60.1720986097152,9.09784859398886,
-213.954559217709));
#202598=CARTESIAN_POINT('Ctrl Pts',(-60.1736282672258,9.00748926176064,
-213.973818634937));
#202599=CARTESIAN_POINT('Ctrl Pts',(-60.1792151276392,8.67746442109373,
-214.044160966443));
#202600=CARTESIAN_POINT('Ctrl Pts',(-60.1853553620157,8.31350519984393,
-214.113465883351));
#202601=CARTESIAN_POINT('Ctrl Pts',(-60.1914134093591,7.95361934628412,
-214.171719071268));
#202602=CARTESIAN_POINT('Ctrl Pts',(-60.2137472534458,6.62684950003347,
-214.386477646555));
#202603=CARTESIAN_POINT('Ctrl Pts',(-60.236418104203,5.27038456544881,-214.469588956065));
#202604=CARTESIAN_POINT('Ctrl Pts',(-60.2591685013589,3.93463693001197,
-214.381568911362));
#202605=CARTESIAN_POINT('Ctrl Pts',(-60.270567951341,3.26533923579523,-214.337465061652));
#202606=CARTESIAN_POINT('Ctrl Pts',(-60.2826202444475,2.56566381511999,
-214.241040503758));
#202607=CARTESIAN_POINT('Ctrl Pts',(-60.292057365503,2.02427812018546,-214.137294054647));
#202608=CARTESIAN_POINT('Ctrl Pts',(-60.2979421316394,1.68668276821483,
-214.072600215613));
#202609=CARTESIAN_POINT('Ctrl Pts',(-60.3031851011954,1.38822157870232,
-214.004609259433));
#202610=CARTESIAN_POINT('Ctrl Pts',(-60.3084747241416,1.08920916466888,
-213.927821213477));
#202611=CARTESIAN_POINT('Ctrl Pts',(-60.3091581982913,1.05057365935602,
-213.917899401477));
#202612=CARTESIAN_POINT('Ctrl Pts',(-60.3098424352801,1.01193290476609,
-213.907817486517));
#202613=CARTESIAN_POINT('Ctrl Pts',(-60.3105289330055,0.973203341285052,
-213.897551739282));
#202614=CARTESIAN_POINT('Ctrl Pts',(-60.3112345718811,0.933393907674668,
-213.886999759185));
#202615=CARTESIAN_POINT('Ctrl Pts',(-60.3119438877354,0.893513565114719,
-213.87616273221));
#202616=CARTESIAN_POINT('Ctrl Pts',(-60.3126540303503,0.853391001986712,
-213.865328893283));
#202617=CARTESIAN_POINT('Ctrl Pts',(-60.3142387111128,0.763857642627992,
-213.841153219592));
#202618=CARTESIAN_POINT('Ctrl Pts',(-60.3158218668931,0.673014957611186,
-213.817396808284));
#202619=CARTESIAN_POINT('Ctrl Pts',(-60.3174186631854,0.579830242826638,
-213.793870865919));
#202620=CARTESIAN_POINT('Ctrl Pts',(-60.3203923825932,0.406292017450701,
-213.750058419878));
#202621=CARTESIAN_POINT('Ctrl Pts',(-60.3234151563687,0.224650876049034,
-213.706988287318));
#202622=CARTESIAN_POINT('Ctrl Pts',(-60.3265631280972,0.0280980835395926,
-213.664136837394));
#202623=CARTESIAN_POINT('Ctrl Pts',(-60.3339383732068,-0.432396846778452,
-213.563742051876));
#202624=CARTESIAN_POINT('Ctrl Pts',(-60.3416644856382,-0.959964067856175,
-213.470756377755));
#202625=CARTESIAN_POINT('Ctrl Pts',(-60.3482721133978,-1.46527456786017,
-213.40505861675));
#202626=CARTESIAN_POINT('Ctrl Pts',(-60.3615553279344,-2.48109265317286,
-213.272987397582));
#202627=CARTESIAN_POINT('Ctrl Pts',(-60.3719858564929,-3.50919761377231,
-213.2277198046));
#202628=CARTESIAN_POINT('Ctrl Pts',(-60.3794425164094,-4.53314772643593,
-213.26537659776));
#202629=CARTESIAN_POINT('Ctrl Pts',(-60.3850857563185,-5.30807862114162,
-213.293875459232));
#202630=CARTESIAN_POINT('Ctrl Pts',(-60.389031621255,-6.08056089768348,
-213.369825212479));
#202631=CARTESIAN_POINT('Ctrl Pts',(-60.3913108160445,-6.84593414020724,
-213.491429597462));
#202632=CARTESIAN_POINT('Ctrl Pts',(-60.3924832204613,-7.23963764205741,
-213.553982179063));
#202633=CARTESIAN_POINT('Ctrl Pts',(-60.393210861424,-7.65045599543644,
-213.633390155679));
#202634=CARTESIAN_POINT('Ctrl Pts',(-60.3934920217241,-7.99285084597502,
-213.708959851915));
#202635=CARTESIAN_POINT('Ctrl Pts',(-60.3936603081493,-8.19778875984029,
-213.754191536544));
#202636=CARTESIAN_POINT('Ctrl Pts',(-60.3936984229566,-8.3833292016282,
-213.798440546674));
#202637=CARTESIAN_POINT('Ctrl Pts',(-60.3936519031611,-8.56176805395006,
-213.843419246262));
#202638=CARTESIAN_POINT('Ctrl Pts',(-60.3936457152461,-8.58550342183554,
-213.849402169644));
#202639=CARTESIAN_POINT('Ctrl Pts',(-60.3936379471922,-8.60911262131742,
-213.855400254366));
#202640=CARTESIAN_POINT('Ctrl Pts',(-60.3936286330974,-8.63262423355809,
-213.86141955001));
#202641=CARTESIAN_POINT('Ctrl Pts',(-60.3936240106306,-8.64429274776344,
-213.864406849902));
#202642=CARTESIAN_POINT('Ctrl Pts',(-60.3936189488047,-8.65593645131671,
-213.867402543179));
#202643=CARTESIAN_POINT('Ctrl Pts',(-60.3936136334464,-8.66756126923334,
-213.870397484014));
#202644=CARTESIAN_POINT('Ctrl Pts',(-60.3936089954616,-8.67770465498888,
-213.873010758511));
#202645=CARTESIAN_POINT('Ctrl Pts',(-60.3936043793879,-8.68783651798293,
-213.875611805623));
#202646=CARTESIAN_POINT('Ctrl Pts',(-60.3935997841399,-8.69795915571533,
-213.878201268307));
#202647=CARTESIAN_POINT('Ctrl Pts',(-60.3935813536365,-8.73855877228209,
-213.888587019024));
#202648=CARTESIAN_POINT('Ctrl Pts',(-60.3935632575531,-8.77901001068333,
-213.898786760883));
#202649=CARTESIAN_POINT('Ctrl Pts',(-60.3935454305536,-8.81946085570323,
-213.9088392194));
#202650=CARTESIAN_POINT('Ctrl Pts',(-60.3935099629075,-8.89993969675822,
-213.928839054034));
#202651=CARTESIAN_POINT('Ctrl Pts',(-60.3934755529649,-8.9804162770879,
-213.948259982409));
#202652=CARTESIAN_POINT('Ctrl Pts',(-60.3934417749187,-9.06205842258958,
-213.967356720238));
#202653=CARTESIAN_POINT('Ctrl Pts',(-60.3932972840641,-9.41129541870198,
-214.049045991312));
#202654=CARTESIAN_POINT('Ctrl Pts',(-60.3931553384559,-9.79419688676307,
-214.129239831576));
#202655=CARTESIAN_POINT('Ctrl Pts',(-60.3930255323827,-10.2663428839057,
-214.205320185781));
#202656=CARTESIAN_POINT('Ctrl Pts',(-60.3927844696473,-11.1431647675559,
-214.346608939443));
#202657=CARTESIAN_POINT('Ctrl Pts',(-60.3926875276504,-12.0266701068567,
-214.418412123761));
#202658=CARTESIAN_POINT('Ctrl Pts',(-60.3927142613204,-12.9140676164264,
-214.419432663803));
#202659=CARTESIAN_POINT('Ctrl Pts',(-60.392740601048,-13.7883885989459,
-214.420438165354));
#202660=CARTESIAN_POINT('Ctrl Pts',(-60.392886297565,-14.6625510241356,
-214.352549769935));
#202661=CARTESIAN_POINT('Ctrl Pts',(-60.3930924113226,-15.5293465961958,
-214.221220332185));
#202662=CARTESIAN_POINT('Ctrl Pts',(-60.3931958927294,-15.9645297022867,
-214.155285116912));
#202663=CARTESIAN_POINT('Ctrl Pts',(-60.3933106563195,-16.3866140396118,
-214.073965655162));
#202664=CARTESIAN_POINT('Ctrl Pts',(-60.3934060177548,-16.7332476949765,
-213.998244468936));
#202665=CARTESIAN_POINT('Ctrl Pts',(-60.3934150872653,-16.7662148746455,
-213.991042877537));
#202666=CARTESIAN_POINT('Ctrl Pts',(-60.3934240727474,-16.7988175394096,
-213.983832359438));
#202667=CARTESIAN_POINT('Ctrl Pts',(-60.393432985145,-16.8311197866803,
-213.976604381314));
#202668=CARTESIAN_POINT('Ctrl Pts',(-60.3934565432233,-16.9165040912771,
-213.95749871722));
#202669=CARTESIAN_POINT('Ctrl Pts',(-60.3934796365262,-16.9997898733479,
-213.938272995079));
#202670=CARTESIAN_POINT('Ctrl Pts',(-60.3935024947112,-17.0821483260315,
-213.918723916564));
#202671=CARTESIAN_POINT('Ctrl Pts',(-60.3935141968302,-17.1243112718211,
-213.908715875971));
#202672=CARTESIAN_POINT('Ctrl Pts',(-60.3935258376587,-17.1662309100974,
-213.898622064381));
#202673=CARTESIAN_POINT('Ctrl Pts',(-60.3935374491214,-17.2080633558844,
-213.888408909728));
#202674=CARTESIAN_POINT('Ctrl Pts',(-60.3935432880669,-17.2290992392795,
-213.883273117969));
#202675=CARTESIAN_POINT('Ctrl Pts',(-60.393549119591,-17.2501130687726,
-213.878107082029));
#202676=CARTESIAN_POINT('Ctrl Pts',(-60.393554947749,-17.2711246845471,
-213.872906131118));
#202677=CARTESIAN_POINT('Ctrl Pts',(-60.3935615224738,-17.294827815679,
-213.867038956371));
#202678=CARTESIAN_POINT('Ctrl Pts',(-60.3935675567514,-17.3185350501926,
-213.861156493035));
#202679=CARTESIAN_POINT('Ctrl Pts',(-60.3935716543076,-17.3422928483403,
-213.855327567938));
#202680=CARTESIAN_POINT('Ctrl Pts',(-60.3936041243251,-17.5305553343483,
-213.809137768578));
#202681=CARTESIAN_POINT('Ctrl Pts',(-60.3935458845432,-17.7216373314316,
-213.764774682049));
#202682=CARTESIAN_POINT('Ctrl Pts',(-60.3933602461435,-17.9298338823286,
-213.719802565618));
#202683=CARTESIAN_POINT('Ctrl Pts',(-60.39306103192,-18.2654076075664,-213.647315963041));
#202684=CARTESIAN_POINT('Ctrl Pts',(-60.3923553391732,-18.6775129550165,
-213.567607646049));
#202685=CARTESIAN_POINT('Ctrl Pts',(-60.3910564967462,-19.1075296034981,
-213.499906653704));
#202686=CARTESIAN_POINT('Ctrl Pts',(-60.3887092138914,-19.8846605974918,
-213.377556647813));
#202687=CARTESIAN_POINT('Ctrl Pts',(-60.3846983903846,-20.669134581579,
-213.299096394904));
#202688=CARTESIAN_POINT('Ctrl Pts',(-60.3789612071656,-21.4554845530463,
-213.268525469849));
#202689=CARTESIAN_POINT('Ctrl Pts',(-60.3679012957513,-22.971378449573,
-213.209592068205));
#202690=CARTESIAN_POINT('Ctrl Pts',(-60.3502984944823,-24.5000103406804,
-213.329130293887));
#202691=CARTESIAN_POINT('Ctrl Pts',(-60.3264857554363,-25.9796130521886,
-213.6570101885));
#202692=CARTESIAN_POINT('Ctrl Pts',(-60.3234504544024,-26.1682112487739,
-213.698803540418));
#202693=CARTESIAN_POINT('Ctrl Pts',(-60.32045653301,-26.3472746066239,-213.742037759623));
#202694=CARTESIAN_POINT('Ctrl Pts',(-60.3175367315418,-26.516649532719,
-213.78578065973));
#202695=CARTESIAN_POINT('Ctrl Pts',(-60.3159762978469,-26.6071688178869,
-213.809158240699));
#202696=CARTESIAN_POINT('Ctrl Pts',(-60.3144291687252,-26.6953838659087,
-213.832796220737));
#202697=CARTESIAN_POINT('Ctrl Pts',(-60.3128853379364,-26.7820351410227,
-213.856805411057));
#202698=CARTESIAN_POINT('Ctrl Pts',(-60.3124915944156,-26.8041349581721,
-213.862928791414));
#202699=CARTESIAN_POINT('Ctrl Pts',(-60.3120980566698,-26.8261330430226,
-213.86907659917));
#202700=CARTESIAN_POINT('Ctrl Pts',(-60.3117045402841,-26.8480416873385,
-213.875251256029));
#202701=CARTESIAN_POINT('Ctrl Pts',(-60.3115355397114,-26.857450630824,
-213.877903040255));
#202702=CARTESIAN_POINT('Ctrl Pts',(-60.3113666893836,-26.8668457943141,
-213.880549365385));
#202703=CARTESIAN_POINT('Ctrl Pts',(-60.311198146228,-26.8762313719384,
-213.883178158384));
#202704=CARTESIAN_POINT('Ctrl Pts',(-60.3110325273771,-26.8854541052786,
-213.88576134056));
#202705=CARTESIAN_POINT('Ctrl Pts',(-60.3108671528631,-26.8946666125183,
-213.888331312463));
#202706=CARTESIAN_POINT('Ctrl Pts',(-60.3107020058,-26.9038697912027,-213.890888412478));
#202707=CARTESIAN_POINT('Ctrl Pts',(-60.31003714784,-26.940920444689,-213.901182923738));
#202708=CARTESIAN_POINT('Ctrl Pts',(-60.3093759742382,-26.9778199604899,
-213.911268999765));
#202709=CARTESIAN_POINT('Ctrl Pts',(-60.3087174003261,-27.0146264313552,
-213.921167211129));
#202710=CARTESIAN_POINT('Ctrl Pts',(-60.3034328975208,-27.3099674628737,
-214.000592048282));
#202711=CARTESIAN_POINT('Ctrl Pts',(-60.2983146403094,-27.5991766863594,
-214.068573069903));
#202712=CARTESIAN_POINT('Ctrl Pts',(-60.2928256973099,-27.9124538529064,
-214.131004935625));
#202713=CARTESIAN_POINT('Ctrl Pts',(-60.2839179962429,-28.4208539858519,
-214.23232214678));
#202714=CARTESIAN_POINT('Ctrl Pts',(-60.2740350908591,-28.9922802878427,
-214.323849549146));
#202715=CARTESIAN_POINT('Ctrl Pts',(-60.2607587673068,-29.7735994708971,
-214.377595134823));
#202716=CARTESIAN_POINT('Ctrl Pts',(-60.2515599690423,-30.3149539744131,
-214.414833968173));
#202717=CARTESIAN_POINT('Ctrl Pts',(-60.2410136149577,-30.9417409026654,
-214.424736435113));
#202718=CARTESIAN_POINT('Ctrl Pts',(-60.2310558010096,-31.5353290509064,
-214.401902737164));
#202719=CARTESIAN_POINT('Ctrl Pts',(-60.2183577806209,-32.2922616917676,
-214.372785627362));
#202720=CARTESIAN_POINT('Ctrl Pts',(-60.2057261525619,-33.0473025715524,
-214.295280550927));
#202721=CARTESIAN_POINT('Ctrl Pts',(-60.1931159963307,-33.7953694742733,
-214.178967256063));
#202722=CARTESIAN_POINT('Ctrl Pts',(-60.1870407676876,-34.1557676637223,
-214.122930689379));
#202723=CARTESIAN_POINT('Ctrl Pts',(-60.1809699443646,-34.5145264949527,
-214.05797839233));
#202724=CARTESIAN_POINT('Ctrl Pts',(-60.1749016871998,-34.8710225250701,
-213.985271624848));
#202725=CARTESIAN_POINT('Ctrl Pts',(-60.1733510559208,-34.9621185152596,
-213.966692750421));
#202726=CARTESIAN_POINT('Ctrl Pts',(-60.1718496862813,-35.050193464265,
-213.948229706888));
#202727=CARTESIAN_POINT('Ctrl Pts',(-60.1702373704645,-35.1446172308779,
-213.927869919498));
#202728=CARTESIAN_POINT('Ctrl Pts',(-60.1694999096097,-35.1878059355493,
-213.918557509326));
#202729=CARTESIAN_POINT('Ctrl Pts',(-60.1687161169393,-35.23367491272,-213.908549231462));
#202730=CARTESIAN_POINT('Ctrl Pts',(-60.1678875012017,-35.2821213266033,
-213.897823414987));
#202731=CARTESIAN_POINT('Ctrl Pts',(-60.1675039091746,-35.3045486801587,
-213.892858100551));
#202732=CARTESIAN_POINT('Ctrl Pts',(-60.1671107108273,-35.3275283964073,
-213.887738985336));
#202733=CARTESIAN_POINT('Ctrl Pts',(-60.1667080521216,-35.3510503623432,
-213.882463780837));
#202734=CARTESIAN_POINT('Ctrl Pts',(-60.1665110501776,-35.3625585526502,
-213.879882871679));
#202735=CARTESIAN_POINT('Ctrl Pts',(-60.1663118308306,-35.3741960784184,
-213.877262456814));
#202736=CARTESIAN_POINT('Ctrl Pts',(-60.1661102633079,-35.385963215018,
-213.874608964427));
#202737=CARTESIAN_POINT('Ctrl Pts',(-60.1658814425207,-35.399321346446,
-213.871596702288));
#202738=CARTESIAN_POINT('Ctrl Pts',(-60.1656492765433,-35.4128496429709,
-213.868556305922));
#202739=CARTESIAN_POINT('Ctrl Pts',(-60.1654137561779,-35.4265466933703,
-213.865488895693));
#202740=CARTESIAN_POINT('Ctrl Pts',(-60.1622181589691,-35.6123915818273,
-213.82386953276));
#202741=CARTESIAN_POINT('Ctrl Pts',(-60.158406128703,-35.8293021918329,
-213.777246558444));
#202742=CARTESIAN_POINT('Ctrl Pts',(-60.1539472537289,-36.0737459393782,
-213.728630617293));
#202743=CARTESIAN_POINT('Ctrl Pts',(-60.1418239904498,-36.7383655857192,
-213.596448428388));
#202744=CARTESIAN_POINT('Ctrl Pts',(-60.1249235460772,-37.6062744383648,
-213.448897620045));
#202745=CARTESIAN_POINT('Ctrl Pts',(-60.1024025775609,-38.6088068260868,
-213.355157950907));
#202746=CARTESIAN_POINT('Ctrl Pts',(-60.0769094959091,-39.7436443442948,
-213.249047370555));
#202747=CARTESIAN_POINT('Ctrl Pts',(-60.0435573435545,-41.0613446239085,
-213.221088955402));
#202748=CARTESIAN_POINT('Ctrl Pts',(-60.0067973884015,-42.3155600514751,
-213.345100282712));
#202749=CARTESIAN_POINT('Ctrl Pts',(-59.9618223482237,-43.8500665276586,
-213.496825561076));
#202750=CARTESIAN_POINT('Ctrl Pts',(-59.9097381130811,-45.3772288239093,
-213.865683397748));
#202751=CARTESIAN_POINT('Ctrl Pts',(-59.8539617334923,-46.7516465274364,
-214.56025213694));
#202752=CARTESIAN_POINT('Origin',(1004.,-12.967500020028,-202.84995));
#202753=CARTESIAN_POINT('Ctrl Pts',(-21.8343359993853,37.3653585113446,
-232.959639066595));
#202754=CARTESIAN_POINT('Ctrl Pts',(-25.7068670980457,41.0171742382378,
-226.784363424386));
#202755=CARTESIAN_POINT('Ctrl Pts',(-29.5908265861273,44.7050007481411,
-220.612769983421));
#202756=CARTESIAN_POINT('Ctrl Pts',(-33.4823003440903,48.4301227180298,
-214.442258946369));
#202757=CARTESIAN_POINT('Ctrl Pts',(-23.8044899907809,37.1610589494743,
-232.959868581815));
#202758=CARTESIAN_POINT('Ctrl Pts',(-28.0381839166385,40.7424490125755,
-226.783608200302));
#202759=CARTESIAN_POINT('Ctrl Pts',(-32.283433258083,44.3482400615009,-220.611766381486));
#202760=CARTESIAN_POINT('Ctrl Pts',(-36.5352279127207,47.9802021638173,
-214.441141334719));
#202761=CARTESIAN_POINT('Ctrl Pts',(-25.7658626658342,36.9296719371149,
-232.9601933409));
#202762=CARTESIAN_POINT('Ctrl Pts',(-30.3639150200345,40.4303260414807,
-226.78272680046));
#202763=CARTESIAN_POINT('Ctrl Pts',(-34.9732667504195,43.9421267939794,
-220.610591760459));
#202764=CARTESIAN_POINT('Ctrl Pts',(-39.587510189865,47.4674439422847,-214.439830103812));
#202765=CARTESIAN_POINT('Ctrl Pts',(-27.7161624394018,36.671894066742,-232.960596901862));
#202766=CARTESIAN_POINT('Ctrl Pts',(-32.6826602701726,40.0809702013776,
-226.781662197074));
#202767=CARTESIAN_POINT('Ctrl Pts',(-37.6596812128995,43.4862512150987,
-220.609204852275));
#202768=CARTESIAN_POINT('Ctrl Pts',(-42.6390550299281,46.8908628802244,
-214.438294417841));
#202769=CARTESIAN_POINT('',(-23.9219380212091,37.2105892288189,-232.850059426121));
#202770=CARTESIAN_POINT('Origin',(-0.0818455390431216,-172.606491708452,
-232.85022953235));
#202771=CARTESIAN_POINT('',(-33.4675962034302,48.3558337693674,-214.551986533665));
#202772=CARTESIAN_POINT('Ctrl Pts',(-23.9219380212091,37.2105892288189,
-232.850059426121));
#202773=CARTESIAN_POINT('Ctrl Pts',(-24.1894337590953,37.5543763047846,
-232.280636433357));
#202774=CARTESIAN_POINT('Ctrl Pts',(-24.4678390241573,37.9086652249051,
-231.694544993519));
#202775=CARTESIAN_POINT('Ctrl Pts',(-24.7575586284418,38.2734572988675,
-231.091774329981));
#202776=CARTESIAN_POINT('Ctrl Pts',(-24.8338303793635,38.3694926716625,
-230.933088575782));
#202777=CARTESIAN_POINT('Ctrl Pts',(-24.910886561832,38.4662559972377,-230.773246849354));
#202778=CARTESIAN_POINT('Ctrl Pts',(-24.9887351655947,38.5637473465457,
-230.612248954828));
#202779=CARTESIAN_POINT('Ctrl Pts',(-25.1755142162996,38.7976544533602,
-230.225973126467));
#202780=CARTESIAN_POINT('Ctrl Pts',(-25.3668559491288,39.0357523185106,
-229.833042219166));
#202781=CARTESIAN_POINT('Ctrl Pts',(-25.5628869758507,39.2780421787683,
-229.433455789082));
#202782=CARTESIAN_POINT('Ctrl Pts',(-25.6609024892116,39.3991871088971,
-229.23366257404));
#202783=CARTESIAN_POINT('Ctrl Pts',(-25.7600905647287,39.521380045916,-229.032205503484));
#202784=CARTESIAN_POINT('Ctrl Pts',(-25.8604684704001,39.6446211959334,
-228.829084681626));
#202785=CARTESIAN_POINT('Ctrl Pts',(-25.9106574232357,39.706241770942,-228.727524270697));
#202786=CARTESIAN_POINT('Ctrl Pts',(-25.9611438336268,39.768124399285,-228.625547922004));
#202787=CARTESIAN_POINT('Ctrl Pts',(-26.0119299676247,39.8302691107557,
-228.523155661133));
#202788=CARTESIAN_POINT('Ctrl Pts',(-26.0373230346236,39.8613414664911,
-228.471959530698));
#202789=CARTESIAN_POINT('Ctrl Pts',(-26.0627910325259,39.8924793430169,
-228.420659422224));
#202790=CARTESIAN_POINT('Ctrl Pts',(-26.0883342475814,39.9236827441997,
-228.369255339306));
#202791=CARTESIAN_POINT('Ctrl Pts',(-26.1074916588731,39.9470852950868,
-228.330702277118));
#202792=CARTESIAN_POINT('Ctrl Pts',(-26.1266913798135,39.9705247035944,
-228.292090729306));
#202793=CARTESIAN_POINT('Ctrl Pts',(-26.1459335324298,39.9940009714088,
-228.253420697542));
#202794=CARTESIAN_POINT('Ctrl Pts',(-26.1523475833019,40.0018263940136,
-228.240530686954));
#202795=CARTESIAN_POINT('Ctrl Pts',(-26.159603988047,40.0106774358069,-228.225951592293));
#202796=CARTESIAN_POINT('Ctrl Pts',(-26.1651898335708,40.0174895257253,
-228.214731171203));
#202797=CARTESIAN_POINT('Ctrl Pts',(-26.4784456003041,40.3995134183188,
-227.585486843432));
#202798=CARTESIAN_POINT('Ctrl Pts',(-26.8042399378866,40.7928975113341,
-226.938117284709));
#202799=CARTESIAN_POINT('Ctrl Pts',(-27.1430237328783,41.1976515383687,
-226.272617727839));
#202800=CARTESIAN_POINT('Ctrl Pts',(-27.1908671777602,41.254811376795,-226.178635099866));
#202801=CARTESIAN_POINT('Ctrl Pts',(-27.2389697606827,41.3121979844456,
-226.084290897946));
#202802=CARTESIAN_POINT('Ctrl Pts',(-27.2873328347012,41.3698114029867,
-225.989585108865));
#202803=CARTESIAN_POINT('Ctrl Pts',(-27.4827460398511,41.6026010468474,
-225.60692205102));
#202804=CARTESIAN_POINT('Ctrl Pts',(-27.6824126124695,41.8390934527353,
-225.218356004158));
#202805=CARTESIAN_POINT('Ctrl Pts',(-27.8864313861877,42.0792915016639,
-224.823887988709));
#202806=CARTESIAN_POINT('Ctrl Pts',(-27.9884407730468,42.1993905261282,
-224.626653980985));
#202807=CARTESIAN_POINT('Ctrl Pts',(-28.0915382097496,42.3204159683605,
-224.427944485158));
#202808=CARTESIAN_POINT('Ctrl Pts',(-28.1957371229962,42.4423682592528,
-224.227759780574));
#202809=CARTESIAN_POINT('Ctrl Pts',(-28.2478365796194,42.5033444046989,
-224.127667428282));
#202810=CARTESIAN_POINT('Ctrl Pts',(-28.3002114053509,42.5645522628344,
-224.027206274105));
#202811=CARTESIAN_POINT('Ctrl Pts',(-28.3528633081307,42.6259918913164,
-223.926376358727));
#202812=CARTESIAN_POINT('Ctrl Pts',(-28.3791892595206,42.6567117055573,
-223.875961401039));
#202813=CARTESIAN_POINT('Ctrl Pts',(-28.4055844801704,42.6874894624216,
-223.825454253071));
#202814=CARTESIAN_POINT('Ctrl Pts',(-28.4320491872001,42.7183251694128,
-223.774854920477));
#202815=CARTESIAN_POINT('Ctrl Pts',(-28.4518977174724,42.7414519496563,
-223.736905421032));
#202816=CARTESIAN_POINT('Ctrl Pts',(-28.4717853338333,42.7646113268491,
-223.698904067736));
#202817=CARTESIAN_POINT('Ctrl Pts',(-28.4917121286658,42.7878033042288,
-223.660850863104));
#202818=CARTESIAN_POINT('Ctrl Pts',(-28.4983543936099,42.7955339633554,
-223.64816646156));
#202819=CARTESIAN_POINT('Ctrl Pts',(-28.5058234396025,42.8042250770556,
-223.633906381256));
#202820=CARTESIAN_POINT('Ctrl Pts',(-28.5116519864808,42.8110061484612,
-223.622780374796));
#202821=CARTESIAN_POINT('Ctrl Pts',(-28.8846789866944,43.2449947184182,
-222.910715961337));
#202822=CARTESIAN_POINT('Ctrl Pts',(-29.2740946136785,43.6935589406833,
-222.175300745994));
#202823=CARTESIAN_POINT('Ctrl Pts',(-29.6803694781413,44.1567272852874,
-221.416525967767));
#202824=CARTESIAN_POINT('Ctrl Pts',(-29.8835069103727,44.3883114575895,
-221.037138578654));
#202825=CARTESIAN_POINT('Ctrl Pts',(-30.0908607695619,44.6235468200016,
-220.65191152586));
#202826=CARTESIAN_POINT('Ctrl Pts',(-30.3024996229282,44.8624379324151,
-220.260845174858));
#202827=CARTESIAN_POINT('Ctrl Pts',(-30.4083190496114,44.9818834886218,
-220.065311999357));
#202828=CARTESIAN_POINT('Ctrl Pts',(-30.5152097241604,45.10224299076,-219.868319004086));
#202829=CARTESIAN_POINT('Ctrl Pts',(-30.6231809422163,45.2235170782419,
-219.669866346784));
#202830=CARTESIAN_POINT('Ctrl Pts',(-30.6771665512442,45.2841541219828,
-219.570640018133));
#202831=CARTESIAN_POINT('Ctrl Pts',(-30.7314222961001,45.3450198126418,
-219.471048774303));
#202832=CARTESIAN_POINT('Ctrl Pts',(-30.7859493585771,45.4061142340476,
-219.371092639537));
#202833=CARTESIAN_POINT('Ctrl Pts',(-30.8132128898157,45.4366614447505,
-219.321114572154));
#202834=CARTESIAN_POINT('Ctrl Pts',(-30.8405442504562,45.4672658381784,
-219.271045282059));
#202835=CARTESIAN_POINT('Ctrl Pts',(-30.8679435906687,45.4979274250916,
-219.220884772699));
#202836=CARTESIAN_POINT('Ctrl Pts',(-30.8884930958281,45.5209236152766,
-219.183264390679));
#202837=CARTESIAN_POINT('Ctrl Pts',(-30.9090808394965,45.5439519768002,
-219.145592697825));
#202838=CARTESIAN_POINT('Ctrl Pts',(-30.9297068855559,45.5670125142704,
-219.107869695687));
#202839=CARTESIAN_POINT('Ctrl Pts',(-30.9365822342424,45.5746993600938,
-219.095295361641));
#202840=CARTESIAN_POINT('Ctrl Pts',(-30.9443002873472,45.5833269031714,
-219.081182394694));
#202841=CARTESIAN_POINT('Ctrl Pts',(-30.9503457014926,45.5900837772301,
-219.070129590519));
#202842=CARTESIAN_POINT('Ctrl Pts',(-31.3783887818336,46.0685014862618,
-218.28754030354));
#202843=CARTESIAN_POINT('Ctrl Pts',(-31.826098659014,46.5643404167945,-217.477019211197));
#202844=CARTESIAN_POINT('Ctrl Pts',(-32.2939772733384,47.0776507896269,
-216.638564146678));
#202845=CARTESIAN_POINT('Ctrl Pts',(-32.6719260436299,47.4922989873653,
-215.96126655094));
#202846=CARTESIAN_POINT('Ctrl Pts',(-33.0630364837259,47.9183480882516,
-215.265741238066));
#202847=CARTESIAN_POINT('Ctrl Pts',(-33.4675962034302,48.3558337693674,
-214.551986533665));
#202848=CARTESIAN_POINT('Ctrl Pts',(-33.4676025732012,48.3558411518987,
-214.551991264071));
#202849=CARTESIAN_POINT('Ctrl Pts',(-34.986173088576,48.1318948779757,-214.551622026082));
#202850=CARTESIAN_POINT('Ctrl Pts',(-36.5024599607171,47.8927123635888,
-214.551192124683));
#202851=CARTESIAN_POINT('Ctrl Pts',(-39.5299978799685,47.3839481265764,
-214.550248248569));
#202852=CARTESIAN_POINT('Ctrl Pts',(-41.0411822924498,47.1143775777148,
-214.549734342702));
#202853=CARTESIAN_POINT('Ctrl Pts',(-42.5495440571184,46.8296601105062,
-214.549225394074));
#202854=CARTESIAN_POINT('Origin',(296.501483394397,-25.4138432731711,-232.85005));
#202855=CARTESIAN_POINT('',(-47.6963129660555,-31.8956500308477,-232.849931330248));
#202856=CARTESIAN_POINT('Origin',(636.934816028482,-11.5034818258361,-232.85005));
#202857=CARTESIAN_POINT('Ctrl Pts',(-47.696355285306,-31.8961636867541,
-232.85005));
#202858=CARTESIAN_POINT('Ctrl Pts',(-47.7198209970693,-32.0141643773229,
-232.85005));
#202859=CARTESIAN_POINT('Ctrl Pts',(-47.7444480612299,-32.1319277281148,
-232.850050000009));
#202860=CARTESIAN_POINT('Ctrl Pts',(-47.7960571707323,-32.367227820781,
-232.850050000009));
#202861=CARTESIAN_POINT('Ctrl Pts',(-47.8230417127441,-32.484751255595,
-232.85005));
#202862=CARTESIAN_POINT('Ctrl Pts',(-47.8511636801456,-32.6020082275457,
-232.85005));
#202863=CARTESIAN_POINT('Ctrl Pts',(-47.0825542034256,-41.7715518889728,
-232.85005));
#202864=CARTESIAN_POINT('Ctrl Pts',(-46.9318457802784,-42.0078889334137,
-232.85005));
#202865=CARTESIAN_POINT('Ctrl Pts',(-46.790407810866,-42.2260222196836,
-232.85005));
#202866=CARTESIAN_POINT('Ctrl Pts',(-46.4935676456938,-42.6770301149308,
-232.85005));
#202867=CARTESIAN_POINT('Ctrl Pts',(-46.3418104287299,-42.9039683374183,
-232.85005));
#202868=CARTESIAN_POINT('Ctrl Pts',(-45.8752836486906,-43.5906554858717,
-232.85005));
#202869=CARTESIAN_POINT('Ctrl Pts',(-45.5551891811036,-44.0469551839436,
-232.85005));
#202870=CARTESIAN_POINT('Ctrl Pts',(-44.5502158894675,-45.434541329739,
-232.85005));
#202871=CARTESIAN_POINT('Ctrl Pts',(-43.8423500925213,-46.3501756007727,
-232.85005));
#202872=CARTESIAN_POINT('Ctrl Pts',(-41.5657247068321,-49.1071648985542,
-232.85005));
#202873=CARTESIAN_POINT('Ctrl Pts',(-39.8686235209219,-50.9065939957953,
-232.85005));
#202874=CARTESIAN_POINT('Ctrl Pts',(-36.3067467607518,-54.2094198215295,
-232.85005));
#202875=CARTESIAN_POINT('Ctrl Pts',(-34.3620922232014,-55.779993285671,
-232.85005));
#202876=CARTESIAN_POINT('Ctrl Pts',(-29.6879673386845,-59.0721264532024,
-232.85005));
#202877=CARTESIAN_POINT('Ctrl Pts',(-27.4993617066061,-60.2539794127404,
-232.85005));
#202878=CARTESIAN_POINT('Ctrl Pts',(-26.5827048610815,-60.7443921296953,
-232.85005));
#202879=CARTESIAN_POINT('',(-21.0035766188647,-61.257476972142,-232.850047644298));
#202880=CARTESIAN_POINT('Origin',(-0.0517782018608104,643.799970559367,
-232.855108201462));
#202881=CARTESIAN_POINT('',(-20.3871357022546,-61.1221564407624,-232.850041788805));
#202882=CARTESIAN_POINT('Ctrl Pts',(-20.3871899403996,-61.1221588841743,
-232.85005));
#202883=CARTESIAN_POINT('Ctrl Pts',(-20.4903351182891,-61.1426979252124,
-232.85005));
#202884=CARTESIAN_POINT('Ctrl Pts',(-20.5932743876283,-61.1642481051797,
-232.850050000001));
#202885=CARTESIAN_POINT('Ctrl Pts',(-20.7987564077172,-61.2093548950234,
-232.850050000001));
#202886=CARTESIAN_POINT('Ctrl Pts',(-20.901290168981,-61.2329102063362,
-232.85005));
#202887=CARTESIAN_POINT('Ctrl Pts',(-21.0035920114341,-61.2574518715733,
-232.85005));
#202888=CARTESIAN_POINT('Origin',(-7.14692237356698E-14,623.509175991979,
-232.85005));
#202889=CARTESIAN_POINT('Ctrl Pts',(-25.2562521239792,-61.0455007230049,
-232.959725695103));
#202890=CARTESIAN_POINT('Ctrl Pts',(-30.6613188291079,-64.9426708583199,
-226.793511106062));
#202891=CARTESIAN_POINT('Ctrl Pts',(-36.0671479350067,-68.8395145916166,
-220.627759071707));
#202892=CARTESIAN_POINT('Ctrl Pts',(-41.4730739204624,-72.736318130574,
-214.462066626483));
#202893=CARTESIAN_POINT('Ctrl Pts',(-23.6900699183709,-61.1001919234539,
-232.961968408598));
#202894=CARTESIAN_POINT('Ctrl Pts',(-28.7297131786069,-65.012574288375,
-226.795902612053));
#202895=CARTESIAN_POINT('Ctrl Pts',(-33.7700272351411,-68.9255509631158,
-220.630194103463));
#202896=CARTESIAN_POINT('Ctrl Pts',(-38.8104606792061,-72.8393402290212,
-214.464534772546));
#202897=CARTESIAN_POINT('Ctrl Pts',(-22.115564575717,-61.1500631726904,
-232.964012351071));
#202898=CARTESIAN_POINT('Ctrl Pts',(-26.7965523266534,-65.0759017171342,
-226.798067164761));
#202899=CARTESIAN_POINT('Ctrl Pts',(-31.4781225651976,-69.0031581792391,
-220.632397171727));
#202900=CARTESIAN_POINT('Ctrl Pts',(-36.1598241774431,-72.9319991467586,
-214.466766784373));
#202901=CARTESIAN_POINT('Ctrl Pts',(-20.5341645416114,-61.1949426407512,
-232.965861592748));
#202902=CARTESIAN_POINT('Ctrl Pts',(-24.8619705593691,-65.1326290782542,
-226.800008788317));
#202903=CARTESIAN_POINT('Ctrl Pts',(-29.1902811104598,-69.0724625871147,
-220.634368994467));
#202904=CARTESIAN_POINT('Ctrl Pts',(-33.5187281767876,-73.0145710177392,
-214.468761046583));
#202905=CARTESIAN_POINT('',(-33.4888847838974,-72.9429804215028,-214.578390315157));
#202906=CARTESIAN_POINT('Ctrl Pts',(-21.0035766188647,-61.257476972142,
-232.850047644298));
#202907=CARTESIAN_POINT('Ctrl Pts',(-21.4855291169009,-61.7123302898789,
-232.13856112446));
#202908=CARTESIAN_POINT('Ctrl Pts',(-21.9854835224216,-62.1838047440078,
-231.401113733466));
#202909=CARTESIAN_POINT('Ctrl Pts',(-22.5035510757124,-62.6718647794899,
-230.637765485951));
#202910=CARTESIAN_POINT('Ctrl Pts',(-22.961623614274,-63.1034048325268,
-229.962817079465));
#202911=CARTESIAN_POINT('Ctrl Pts',(-23.4338577616424,-63.5479114810121,
-229.267619379724));
#202912=CARTESIAN_POINT('Ctrl Pts',(-23.9203643500785,-64.0053593573632,
-228.552213807771));
#202913=CARTESIAN_POINT('Ctrl Pts',(-24.4387307921192,-64.4927641196409,
-227.789958476056));
#202914=CARTESIAN_POINT('Ctrl Pts',(-24.9732848589469,-64.9948621266171,
-227.004760241598));
#202915=CARTESIAN_POINT('Ctrl Pts',(-25.5241023969115,-65.5116339688911,
-226.196655135222));
#202916=CARTESIAN_POINT('Ctrl Pts',(-25.7995111658937,-65.7700198900281,
-225.792602582035));
#202917=CARTESIAN_POINT('Ctrl Pts',(-26.078985368137,-66.03207440159,-225.38282313732));
#202918=CARTESIAN_POINT('Ctrl Pts',(-26.362531603249,-66.2977959631439,
-224.967320133644));
#202919=CARTESIAN_POINT('Ctrl Pts',(-26.504304720805,-66.4306567439208,
-224.759568631806));
#202920=CARTESIAN_POINT('Ctrl Pts',(-26.6470958466098,-66.5644342873659,
-224.550386240369));
#202921=CARTESIAN_POINT('Ctrl Pts',(-26.7909055674976,-66.699128475012,
-224.339773277289));
#202922=CARTESIAN_POINT('Ctrl Pts',(-26.8628104279415,-66.766475568835,
-224.234466795749));
#202923=CARTESIAN_POINT('Ctrl Pts',(-26.9349699371596,-66.8340518237192,
-224.128802671308));
#202924=CARTESIAN_POINT('Ctrl Pts',(-27.0073841607627,-66.9018572273527,
-224.022780940459));
#202925=CARTESIAN_POINT('Ctrl Pts',(-27.0435912725642,-66.9357599291695,
-223.969770075035));
#202926=CARTESIAN_POINT('Ctrl Pts',(-27.0798620629622,-66.9697199181742,
-223.916669808009));
#202927=CARTESIAN_POINT('Ctrl Pts',(-27.1161965393057,-67.0037371930959,
-223.863480143587));
#202928=CARTESIAN_POINT('Ctrl Pts',(-27.1502601108777,-67.0356283883349,
-223.813614833192));
#202929=CARTESIAN_POINT('Ctrl Pts',(-27.1843796564252,-67.0675699325244,
-223.763670950868));
#202930=CARTESIAN_POINT('Ctrl Pts',(-27.2185551816222,-67.0995618247377,
-223.71364849992));
#202931=CARTESIAN_POINT('Ctrl Pts',(-27.2208335499687,-67.1016946175519,
-223.710313669857));
#202932=CARTESIAN_POINT('Ctrl Pts',(-27.2236948361456,-67.1043730690699,
-223.706125650112));
#202933=CARTESIAN_POINT('Ctrl Pts',(-27.2253910330544,-67.1059608744884,
-223.703642962148));
#202934=CARTESIAN_POINT('Ctrl Pts',(-27.6762562132143,-67.5280145714332,
-223.043721021226));
#202935=CARTESIAN_POINT('Ctrl Pts',(-28.1506357027507,-67.9716482766551,
-222.350079919967));
#202936=CARTESIAN_POINT('Ctrl Pts',(-28.6486036964326,-68.4368359628475,
-221.622769209847));
#202937=CARTESIAN_POINT('Ctrl Pts',(-29.1347392918129,-68.8909701555265,
-220.912740393585));
#202938=CARTESIAN_POINT('Ctrl Pts',(-29.6433554842619,-69.365646209218,
-220.170623031685));
#202939=CARTESIAN_POINT('Ctrl Pts',(-30.1745694141053,-69.8608390978478,
-219.396463103265));
#202940=CARTESIAN_POINT('Ctrl Pts',(-30.6879409058229,-70.3393994247554,
-218.648305694445));
#202941=CARTESIAN_POINT('Ctrl Pts',(-31.2224175099817,-70.8371215031639,
-217.870222065641));
#202942=CARTESIAN_POINT('Ctrl Pts',(-31.7781526360163,-71.3539817960171,
-217.062253580961));
#202943=CARTESIAN_POINT('Ctrl Pts',(-32.3275541022051,-71.8649514817638,
-216.263493435486));
#202944=CARTESIAN_POINT('Ctrl Pts',(-32.8977320509018,-72.3946256494591,
-215.435525743744));
#202945=CARTESIAN_POINT('Ctrl Pts',(-33.4888847838974,-72.9429804215028,
-214.578390315157));
#202946=CARTESIAN_POINT('Ctrl Pts',(-41.3748964705093,-72.6655519150593,
-214.574036340781));
#202947=CARTESIAN_POINT('Ctrl Pts',(-40.0607372977895,-72.716660645803,
-214.574827132799));
#202948=CARTESIAN_POINT('Ctrl Pts',(-38.7464886157383,-72.7653339442144,
-214.575594614694));
#202949=CARTESIAN_POINT('Ctrl Pts',(-36.1178114852045,-72.8578102117473,
-214.577053530306));
#202950=CARTESIAN_POINT('Ctrl Pts',(-34.8033905902617,-72.9016129219457,
-214.577744931601));
#202951=CARTESIAN_POINT('Ctrl Pts',(-33.4888912371591,-72.9429802184569,
-214.578390311931));
#202952=CARTESIAN_POINT('Origin',(0.,-12.9675000200281,-215.85005));
#202953=CARTESIAN_POINT('',(-48.0827620446565,42.0414223951255,-215.85005));
#202954=CARTESIAN_POINT('Ctrl Pts',(-49.1680521502591,41.086535378401,-215.85005));
#202955=CARTESIAN_POINT('Ctrl Pts',(-48.9888707647949,41.2476479220656,
-215.85005));
#202956=CARTESIAN_POINT('Ctrl Pts',(-48.8088730843222,41.4077049862833,
-215.850050000001));
#202957=CARTESIAN_POINT('Ctrl Pts',(-48.4481130991412,41.725084481334,-215.850050000001));
#202958=CARTESIAN_POINT('Ctrl Pts',(-48.265340719459,41.8841953684814,-215.85005));
#202959=CARTESIAN_POINT('Ctrl Pts',(-48.0827620446564,42.0414223951254,
-215.85005));
#202960=CARTESIAN_POINT('',(-54.6458252041307,35.5078877047658,-215.85005));
#202961=CARTESIAN_POINT('Ctrl Pts',(-54.6458252041308,35.5078877047659,
-215.85005));
#202962=CARTESIAN_POINT('Ctrl Pts',(-54.4864708806764,35.6908450584155,
-215.85005));
#202963=CARTESIAN_POINT('Ctrl Pts',(-54.3265120584759,35.8725242596181,
-215.850050000225));
#202964=CARTESIAN_POINT('Ctrl Pts',(-54.0074980938231,36.2310904022842,
-215.850050000225));
#202965=CARTESIAN_POINT('Ctrl Pts',(-53.8465341367002,36.410205079622,-215.85005));
#202966=CARTESIAN_POINT('Ctrl Pts',(-53.6858060762413,36.5871897873468,
-215.85005));
#202967=CARTESIAN_POINT('Origin',(-48.892180948596,36.2913696007177,-215.85005));
#202968=CARTESIAN_POINT('Ctrl Pts',(-28.7632636728437,36.243359951239,-233.011888154992));
#202969=CARTESIAN_POINT('Ctrl Pts',(-31.7703631777874,37.7316226214323,
-229.879662179404));
#202970=CARTESIAN_POINT('Ctrl Pts',(-34.7738161809111,39.2196944596949,
-226.746236332649));
#202971=CARTESIAN_POINT('Ctrl Pts',(-37.7725662199917,40.7095348345317,
-223.611574672556));
#202972=CARTESIAN_POINT('Ctrl Pts',(-40.7713162590722,42.1993752093685,
-220.476913012461));
#202973=CARTESIAN_POINT('Ctrl Pts',(-43.7653510607838,43.6909491168262,
-217.340988222568));
#202974=CARTESIAN_POINT('Ctrl Pts',(-46.7534875501661,45.1873665995436,
-214.204156771482));
#202975=CARTESIAN_POINT('Ctrl Pts',(-28.818156654463,36.2102288606094,-233.012213872822));
#202976=CARTESIAN_POINT('Ctrl Pts',(-31.8223098653572,37.6990724529492,
-229.880007982271));
#202977=CARTESIAN_POINT('Ctrl Pts',(-34.8228081429799,39.18767633626,-226.746603037528));
#202978=CARTESIAN_POINT('Ctrl Pts',(-37.8185924512592,40.6780007601943,
-223.611963071785));
#202979=CARTESIAN_POINT('Ctrl Pts',(-40.8143767595385,42.1683251841286,
-220.477323106043));
#202980=CARTESIAN_POINT('Ctrl Pts',(-43.8054348260158,43.6603350812977,
-217.341420791685));
#202981=CARTESIAN_POINT('Ctrl Pts',(-46.7905804536569,45.1571425161278,
-214.2046126078));
#202982=CARTESIAN_POINT('Ctrl Pts',(-28.8701497243513,36.1801317847072,
-233.011182834863));
#202983=CARTESIAN_POINT('Ctrl Pts',(-31.871666643597,37.6692800952327,-229.879182435101));
#202984=CARTESIAN_POINT('Ctrl Pts',(-34.8695237116303,39.1581256922717,
-226.745980987327));
#202985=CARTESIAN_POINT('Ctrl Pts',(-37.8626041662257,40.6486877405231,
-223.611516219864));
#202986=CARTESIAN_POINT('Ctrl Pts',(-40.8556846208211,42.1392497887745,
-220.4770514524));
#202987=CARTESIAN_POINT('Ctrl Pts',(-43.8439779916275,43.6314868745012,
-217.341294913291));
#202988=CARTESIAN_POINT('Ctrl Pts',(-46.8261837881837,45.128675130066,-214.204570275934));
#202989=CARTESIAN_POINT('Ctrl Pts',(-28.9236494148868,36.1483017803918,
-233.01082974273));
#202990=CARTESIAN_POINT('Ctrl Pts',(-31.9223177157407,37.6379530768432,
-229.878939694123));
#202991=CARTESIAN_POINT('Ctrl Pts',(-34.9173208817124,39.1272459095225,
-226.745848865747));
#202992=CARTESIAN_POINT('Ctrl Pts',(-37.9075126656038,40.6182282999103,
-223.611482166239));
#202993=CARTESIAN_POINT('Ctrl Pts',(-40.8977044494953,42.109210690298,-220.477115466732));
#202994=CARTESIAN_POINT('Ctrl Pts',(-43.8830754570229,43.6018377843273,
-217.341443930439));
#202995=CARTESIAN_POINT('Ctrl Pts',(-46.8622654530928,45.0994691148216,
-214.204774369339));
#202996=CARTESIAN_POINT('Ctrl Pts',(-28.9771491054224,36.1164717760765,
-233.010476650599));
#202997=CARTESIAN_POINT('Ctrl Pts',(-31.9729687878842,37.6066260584536,
-229.878696953144));
#202998=CARTESIAN_POINT('Ctrl Pts',(-34.9651180517945,39.0963661267734,
-226.745716744168));
#202999=CARTESIAN_POINT('Ctrl Pts',(-37.952421164982,40.5877688592974,-223.611448112616));
#203000=CARTESIAN_POINT('Ctrl Pts',(-40.9397242781695,42.0791715918215,
-220.477179481064));
#203001=CARTESIAN_POINT('Ctrl Pts',(-43.9221729224182,43.5721886941534,
-217.341592947587));
#203002=CARTESIAN_POINT('Ctrl Pts',(-46.8983471180018,45.0702630995771,
-214.204978462744));
#203003=CARTESIAN_POINT('Ctrl Pts',(-29.030685932722,36.0844977879761,-233.010123307814));
#203004=CARTESIAN_POINT('Ctrl Pts',(-32.0236191310345,37.5751950097359,
-229.878452353611));
#203005=CARTESIAN_POINT('Ctrl Pts',(-35.012877532973,39.0654224083999,-226.745581710878));
#203006=CARTESIAN_POINT('Ctrl Pts',(-37.997256377555,40.5572850161139,-223.611410887796));
#203007=CARTESIAN_POINT('Ctrl Pts',(-40.9816352221372,42.0491476238279,
-220.477240064714));
#203008=CARTESIAN_POINT('Ctrl Pts',(-43.9611273848811,43.5425935498471,
-217.341739105347));
#203009=CARTESIAN_POINT('Ctrl Pts',(-46.934252483156,45.041149319151,-214.205180808032));
#203010=CARTESIAN_POINT('Ctrl Pts',(-29.0842579792521,36.0523797092374,
-233.009769824147));
#203011=CARTESIAN_POINT('Ctrl Pts',(-32.0742678787604,37.5436593534111,
-229.878206054095));
#203012=CARTESIAN_POINT('Ctrl Pts',(-35.0605994496261,39.0344137463011,
-226.745443927067));
#203013=CARTESIAN_POINT('Ctrl Pts',(-38.0420193927072,40.5267753480634,
-223.611370632498));
#203014=CARTESIAN_POINT('Ctrl Pts',(-41.0234393357883,42.0191369498257,
-220.477297337928));
#203015=CARTESIAN_POINT('Ctrl Pts',(-43.9999418407127,43.5130501216253,
-217.341882483075));
#203016=CARTESIAN_POINT('Ctrl Pts',(-46.9699855652835,45.0121250312964,
-214.205381478311));
#203017=CARTESIAN_POINT('Ctrl Pts',(-29.1914020723121,35.98814355176,-233.009062856813));
#203018=CARTESIAN_POINT('Ctrl Pts',(-32.1755653742122,37.4805880407614,
-229.877713455064));
#203019=CARTESIAN_POINT('Ctrl Pts',(-35.1560432829324,38.9723964221036,
-226.745168359446));
#203020=CARTESIAN_POINT('Ctrl Pts',(-38.1315454230114,40.4657560119625,
-223.611290121901));
#203021=CARTESIAN_POINT('Ctrl Pts',(-41.1070475630904,41.9591156018214,
-220.477411884356));
#203022=CARTESIAN_POINT('Ctrl Pts',(-44.0775707523758,43.4539632651818,
-217.342169238531));
#203023=CARTESIAN_POINT('Ctrl Pts',(-47.0414517295384,44.9540764555871,
-214.205782818867));
#203024=CARTESIAN_POINT('Ctrl Pts',(-29.2986870405764,35.9233310293129,
-233.008355328346));
#203025=CARTESIAN_POINT('Ctrl Pts',(-32.2768564887194,37.4170982945592,
-229.877214059559));
#203026=CARTESIAN_POINT('Ctrl Pts',(-35.2513368575648,38.9101193220809,
-226.744881791608));
#203027=CARTESIAN_POINT('Ctrl Pts',(-38.220782661284,40.4046333779168,-223.611197490097));
#203028=CARTESIAN_POINT('Ctrl Pts',(-41.1902284650032,41.8991474337527,
-220.477513188586));
#203029=CARTESIAN_POINT('Ctrl Pts',(-44.1546396323386,43.3950832783248,
-217.342444873235));
#203030=CARTESIAN_POINT('Ctrl Pts',(-47.1122287537746,44.8963858575329,
-214.206177460189));
#203031=CARTESIAN_POINT('Ctrl Pts',(-29.4060975644904,35.8579413159883,
-233.007648088092));
#203032=CARTESIAN_POINT('Ctrl Pts',(-32.3781342806196,37.3531855340767,
-229.87670909491));
#203033=CARTESIAN_POINT('Ctrl Pts',(-35.3464811752108,38.8475743913038,
-226.744585492565));
#203034=CARTESIAN_POINT('Ctrl Pts',(-38.3097398506307,40.3433960477796,
-223.611093856846));
#203035=CARTESIAN_POINT('Ctrl Pts',(-41.2729985260507,41.8392177042554,
-220.477602221127));
#203036=CARTESIAN_POINT('Ctrl Pts',(-44.231172512421,43.3363922589179,-217.342710032053));
#203037=CARTESIAN_POINT('Ctrl Pts',(-47.182348866173,44.8390312087872,-214.206565980874));
#203038=CARTESIAN_POINT('Ctrl Pts',(-29.6209186123181,35.727161889339,-233.006233607583));
#203039=CARTESIAN_POINT('Ctrl Pts',(-32.5806898644201,37.2253600131119,
-229.875699165609));
#203040=CARTESIAN_POINT('Ctrl Pts',(-35.5367698105028,38.7224845297496,
-226.743992894479));
#203041=CARTESIAN_POINT('Ctrl Pts',(-38.4876542293243,40.2209213875052,
-223.610886590344));
#203042=CARTESIAN_POINT('Ctrl Pts',(-41.4385386481458,41.7193582452608,
-220.477780286209));
#203043=CARTESIAN_POINT('Ctrl Pts',(-44.3842382725856,43.2190102201042,
-217.343240349689));
#203044=CARTESIAN_POINT('Ctrl Pts',(-47.3225890909698,44.7243219112958,
-214.207343022243));
#203045=CARTESIAN_POINT('Ctrl Pts',(-29.8362418555055,35.5940736601297,
-233.004820318005));
#203046=CARTESIAN_POINT('Ctrl Pts',(-32.7831921644516,37.0958423851614,
-229.874667015866));
#203047=CARTESIAN_POINT('Ctrl Pts',(-35.7264614073862,38.5963233250342,
-226.743361409764));
#203048=CARTESIAN_POINT('Ctrl Pts',(-38.664448374147,40.0979879599528,-223.610635340874));
#203049=CARTESIAN_POINT('Ctrl Pts',(-41.6024353409078,41.5996525948713,
-220.477909271983));
#203050=CARTESIAN_POINT('Ctrl Pts',(-44.5351599478724,43.1023841297568,
-217.343728766806));
#203051=CARTESIAN_POINT('Ctrl Pts',(-47.4602015413284,44.6109565161706,
-214.208095611128));
#203052=CARTESIAN_POINT('Ctrl Pts',(-30.0519450660363,35.4586704870703,
-233.00341455534));
#203053=CARTESIAN_POINT('Ctrl Pts',(-32.9855855312196,36.9645966036217,
-229.87362179639));
#203054=CARTESIAN_POINT('Ctrl Pts',(-35.9155640960709,38.4690265434296,
-226.742700788357));
#203055=CARTESIAN_POINT('Ctrl Pts',(-38.8401926838925,39.9745043257835,
-223.610348870589));
#203056=CARTESIAN_POINT('Ctrl Pts',(-41.7648212717142,41.4799821081373,
-220.477996952821));
#203057=CARTESIAN_POINT('Ctrl Pts',(-44.6841307999907,42.986369790773,-217.344180493823));
#203058=CARTESIAN_POINT('Ctrl Pts',(-47.5954455649975,44.4987574479709,
-214.208828131933));
#203059=CARTESIAN_POINT('Ctrl Pts',(-30.4833514870981,35.1878641409515,
-233.000603030011));
#203060=CARTESIAN_POINT('Ctrl Pts',(-33.3903722647552,36.7021050405422,
-229.871531357437));
#203061=CARTESIAN_POINT('Ctrl Pts',(-36.2937694734405,38.2144329802205,
-226.741379545545));
#203062=CARTESIAN_POINT('Ctrl Pts',(-39.1916813033838,39.727537057445,-223.60977593002));
#203063=CARTESIAN_POINT('Ctrl Pts',(-42.089593133327,41.2406411346694,-220.478172314495));
#203064=CARTESIAN_POINT('Ctrl Pts',(-44.9820725042275,42.7543411128055,
-217.345083947855));
#203065=CARTESIAN_POINT('Ctrl Pts',(-47.8659336123358,44.2743593115718,
-214.210293173543));
#203066=CARTESIAN_POINT('Ctrl Pts',(-30.916277333454,34.9077973812142,-232.997822214095));
#203067=CARTESIAN_POINT('Ctrl Pts',(-33.7947232111487,36.4327000734428,
-229.869389558127));
#203068=CARTESIAN_POINT('Ctrl Pts',(-36.6696189896331,37.9552966453494,
-226.739942596491));
#203069=CARTESIAN_POINT('Ctrl Pts',(-39.5389699559083,39.4783689999817,
-223.60906282344));
#203070=CARTESIAN_POINT('Ctrl Pts',(-42.4083209221835,41.001441354614,-220.47818305039));
#203071=CARTESIAN_POINT('Ctrl Pts',(-45.2722095136632,42.5247604673061,
-217.345841145671));
#203072=CARTESIAN_POINT('Ctrl Pts',(-48.1269460791978,44.0546275108218,
-214.211679022545));
#203073=CARTESIAN_POINT('Ctrl Pts',(-31.3497500510356,34.6184286458191,
-232.99511552399));
#203074=CARTESIAN_POINT('Ctrl Pts',(-34.1981927402684,36.1561028618858,
-229.86725871849));
#203075=CARTESIAN_POINT('Ctrl Pts',(-37.0431800113206,37.6911082882257,
-226.738459395528));
#203076=CARTESIAN_POINT('Ctrl Pts',(-39.8826292444588,39.2262665988641,
-223.608273410873));
#203077=CARTESIAN_POINT('Ctrl Pts',(-42.722078477597,40.7614249095024,-220.47808742622));
#203078=CARTESIAN_POINT('Ctrl Pts',(-45.5561045113048,42.2964603802716,
-217.34649079771));
#203079=CARTESIAN_POINT('Ctrl Pts',(-48.3805813576904,43.8381246360801,
-214.213011833879));
#203080=CARTESIAN_POINT('Ctrl Pts',(-32.216695486199,34.0396911750287,-232.98970214378));
#203081=CARTESIAN_POINT('Ctrl Pts',(-35.0051317985077,35.6029084387718,
-229.862997039215));
#203082=CARTESIAN_POINT('Ctrl Pts',(-37.7903020546954,37.1627315739784,
-226.7354929936));
#203083=CARTESIAN_POINT('Ctrl Pts',(-40.5699478215597,38.7220617966288,
-223.60669458574));
#203084=CARTESIAN_POINT('Ctrl Pts',(-43.3495935884239,40.2813920192791,
-220.477896177879));
#203085=CARTESIAN_POINT('Ctrl Pts',(-46.1238945065879,41.8398602062025,
-217.347790101788));
#203086=CARTESIAN_POINT('Ctrl Pts',(-48.8878519146755,43.4051188865968,
-214.215677456544));
#203087=CARTESIAN_POINT('Ctrl Pts',(-33.0858200844503,33.4237352208328,
-232.984594842862));
#203088=CARTESIAN_POINT('Ctrl Pts',(-35.8085395768491,35.0209330321244,
-229.858794403155));
#203089=CARTESIAN_POINT('Ctrl Pts',(-38.5282634124981,36.6141368109387,
-226.732360240482));
#203090=CARTESIAN_POINT('Ctrl Pts',(-41.2427386177898,38.2061131505809,
-223.604831267861));
#203091=CARTESIAN_POINT('Ctrl Pts',(-43.9572138230815,39.7980894902232,
-220.47730229524));
#203092=CARTESIAN_POINT('Ctrl Pts',(-46.6666957170646,41.3883883178512,
-217.348681905218));
#203093=CARTESIAN_POINT('Ctrl Pts',(-49.3656016298064,42.9850105281785,
-214.21816495405));
#203094=CARTESIAN_POINT('Ctrl Pts',(-33.949434877602,32.770352829909,-232.980025784665));
#203095=CARTESIAN_POINT('Ctrl Pts',(-36.6048862944054,34.4080943544835,
-229.854970428563));
#203096=CARTESIAN_POINT('Ctrl Pts',(-39.2576627597897,36.0413528393508,
-226.72942775857));
#203097=CARTESIAN_POINT('Ctrl Pts',(-41.9056884039802,37.6725825561817,
-223.603007266837));
#203098=CARTESIAN_POINT('Ctrl Pts',(-44.5537140481708,39.3038122730124,
-220.476586775106));
#203099=CARTESIAN_POINT('Ctrl Pts',(-47.1972705274053,40.9325619164058,
-217.349301164816));
#203100=CARTESIAN_POINT('Ctrl Pts',(-49.8308862116777,42.5662844245855,
-214.220385090245));
#203101=CARTESIAN_POINT('Ctrl Pts',(-35.6766644639054,31.4635880480613,
-232.97088766827));
#203102=CARTESIAN_POINT('Ctrl Pts',(-38.1975797295179,33.1824169992017,
-229.847322479379));
#203103=CARTESIAN_POINT('Ctrl Pts',(-40.7164614543727,34.8957848961753,
-226.723562794745));
#203104=CARTESIAN_POINT('Ctrl Pts',(-43.231587976361,36.605521367383,-223.599359264791));
#203105=CARTESIAN_POINT('Ctrl Pts',(-45.7467144983492,38.3152578385909,
-220.475155734837));
#203106=CARTESIAN_POINT('Ctrl Pts',(-48.2584201480868,40.0209091135152,
-217.350539684011));
#203107=CARTESIAN_POINT('Ctrl Pts',(-50.7614553754203,41.7288322173994,
-214.224825362635));
#203108=CARTESIAN_POINT('Ctrl Pts',(-37.3872308412151,30.0009912840992,
-232.96524155552));
#203109=CARTESIAN_POINT('Ctrl Pts',(-39.7663238105267,31.8283107595538,
-229.842276532991));
#203110=CARTESIAN_POINT('Ctrl Pts',(-42.1439828477997,33.6499110945716,
-226.719277469106));
#203111=CARTESIAN_POINT('Ctrl Pts',(-44.5191699020356,35.4667587805032,
-223.596189898099));
#203112=CARTESIAN_POINT('Ctrl Pts',(-46.8943569562715,37.2836064664347,
-220.473102327093));
#203113=CARTESIAN_POINT('Ctrl Pts',(-49.2672899419476,39.0954616111304,
-217.349938712546));
#203114=CARTESIAN_POINT('Ctrl Pts',(-51.6347775088331,40.905653234556,-214.226516638731));
#203115=CARTESIAN_POINT('Ctrl Pts',(-38.9866932910313,28.4456556381462,
-232.962790912271));
#203116=CARTESIAN_POINT('Ctrl Pts',(-41.2391357104746,30.3925039299732,
-229.839958591048));
#203117=CARTESIAN_POINT('Ctrl Pts',(-43.490849558744,32.3336071411576,-226.717133201801));
#203118=CARTESIAN_POINT('Ctrl Pts',(-45.7416073381742,34.2690638917383,
-223.59431099442));
#203119=CARTESIAN_POINT('Ctrl Pts',(-47.9923651176044,36.2045206423189,
-220.471488787039));
#203120=CARTESIAN_POINT('Ctrl Pts',(-50.2421837638693,38.1343124474224,
-217.348670714219));
#203121=CARTESIAN_POINT('Ctrl Pts',(-52.490668536736,40.0587201499459,-214.225843430884));
#203122=CARTESIAN_POINT('Ctrl Pts',(-40.5861557408476,26.890319992193,-232.960340269022));
#203123=CARTESIAN_POINT('Ctrl Pts',(-42.7119476104226,28.9566971003925,
-229.837640649106));
#203124=CARTESIAN_POINT('Ctrl Pts',(-44.8377162696882,31.0173031877438,
-226.714988934497));
#203125=CARTESIAN_POINT('Ctrl Pts',(-46.9640447743127,33.0713690029734,
-223.592432090741));
#203126=CARTESIAN_POINT('Ctrl Pts',(-49.0903732789372,35.1254348182031,
-220.469875246985));
#203127=CARTESIAN_POINT('Ctrl Pts',(-51.2170775857911,37.1731632837144,
-217.347402715892));
#203128=CARTESIAN_POINT('Ctrl Pts',(-53.3465595646389,39.2117870653358,
-214.225170223039));
#203129=CARTESIAN_POINT('Ctrl Pts',(-42.0829734536151,25.2333240584369,
-232.96163643903));
#203130=CARTESIAN_POINT('Ctrl Pts',(-44.0964019190368,27.4311852581839,
-229.838534751308));
#203131=CARTESIAN_POINT('Ctrl Pts',(-46.1104687275099,29.6236435023039,
-226.715389153373));
#203132=CARTESIAN_POINT('Ctrl Pts',(-48.1264950127556,31.8092762896688,
-223.592148794104));
#203133=CARTESIAN_POINT('Ctrl Pts',(-50.1425212980013,33.9949090770337,
-220.468908434835));
#203134=CARTESIAN_POINT('Ctrl Pts',(-52.1601585723181,36.1740231929721,
-217.345564448446));
#203135=CARTESIAN_POINT('Ctrl Pts',(-54.1842549207791,38.3419362669036,
-214.22207202995));
#203136=CARTESIAN_POINT('Ctrl Pts',(-43.422273991912,23.5661942096002,-232.965337149737));
#203137=CARTESIAN_POINT('Ctrl Pts',(-45.3530981989507,25.8862379834418,
-229.841157038659));
#203138=CARTESIAN_POINT('Ctrl Pts',(-47.2852714213136,28.2012404581192,
-226.716776130434));
#203139=CARTESIAN_POINT('Ctrl Pts',(-49.2205702668173,30.5094898312471,
-223.59207508571));
#203140=CARTESIAN_POINT('Ctrl Pts',(-51.155869112321,32.817739204375,-220.467374040986));
#203141=CARTESIAN_POINT('Ctrl Pts',(-53.0939569308302,35.1194950308581,
-217.342336617277));
#203142=CARTESIAN_POINT('Ctrl Pts',(-55.0403804700997,37.4099350168284,
-214.216875626567));
#203143=CARTESIAN_POINT('Ctrl Pts',(-44.7615745302087,21.8990643607635,
-232.969037860444));
#203144=CARTESIAN_POINT('Ctrl Pts',(-46.6097944788647,24.3412907086997,
-229.843779326009));
#203145=CARTESIAN_POINT('Ctrl Pts',(-48.4600741151173,26.7788374139345,
-226.718163107495));
#203146=CARTESIAN_POINT('Ctrl Pts',(-50.314645520879,29.2097033728254,-223.592001377317));
#203147=CARTESIAN_POINT('Ctrl Pts',(-52.1692169266407,31.6405693317163,
-220.465839647138));
#203148=CARTESIAN_POINT('Ctrl Pts',(-54.0277552893424,34.0649668687443,
-217.339108786108));
#203149=CARTESIAN_POINT('Ctrl Pts',(-55.8965060194204,36.4779337667532,
-214.211679223185));
#203150=CARTESIAN_POINT('Ctrl Pts',(-45.9478671932277,20.2170814818308,
-232.97487795833));
#203151=CARTESIAN_POINT('Ctrl Pts',(-47.742137018698,22.773387445697,-229.848036259254));
#203152=CARTESIAN_POINT('Ctrl Pts',(-49.5390933433176,25.3254669009981,
-226.72056760043));
#203153=CARTESIAN_POINT('Ctrl Pts',(-51.3405748716693,27.8719256903179,
-223.592376908212));
#203154=CARTESIAN_POINT('Ctrl Pts',(-53.1420564000211,30.4183844796377,
-220.464186215995));
#203155=CARTESIAN_POINT('Ctrl Pts',(-54.9479893176734,32.9592452374763,
-217.335250628456));
#203156=CARTESIAN_POINT('Ctrl Pts',(-56.7618317615675,35.4923074576668,
-214.205720218898));
#203157=CARTESIAN_POINT('Ctrl Pts',(-46.9910749481346,18.573078208412,-232.979487417878));
#203158=CARTESIAN_POINT('Ctrl Pts',(-48.777813963045,21.1992978212187,-229.849984990042));
#203159=CARTESIAN_POINT('Ctrl Pts',(-50.5669117785144,23.8226213730258,
-226.720151765023));
#203160=CARTESIAN_POINT('Ctrl Pts',(-52.3593746083135,26.4424369538029,
-223.59005292932));
#203161=CARTESIAN_POINT('Ctrl Pts',(-54.1518374381127,29.06225253458,-220.459954093617));
#203162=CARTESIAN_POINT('Ctrl Pts',(-55.9476448491922,31.678562291835,-217.329579884935));
#203163=CARTESIAN_POINT('Ctrl Pts',(-57.7483973817176,34.2905533170906,
-214.199162765268));
#203164=CARTESIAN_POINT('',(-46.7405472321667,30.7185439590785,-225.418940742796));
#203165=CARTESIAN_POINT('Ctrl Pts',(-54.6458252041307,35.5078877047659,
-215.85005));
#203166=CARTESIAN_POINT('Ctrl Pts',(-54.5943354599518,35.087122974679,-216.179655766524));
#203167=CARTESIAN_POINT('Ctrl Pts',(-54.4989704543799,34.6852639061865,
-216.528294351409));
#203168=CARTESIAN_POINT('Ctrl Pts',(-54.2127819561474,33.8548754265287,
-217.317195844329));
#203169=CARTESIAN_POINT('Ctrl Pts',(-54.0059798593604,33.4340164708342,
-217.764515858533));
#203170=CARTESIAN_POINT('Ctrl Pts',(-53.2992114913906,32.3315417127153,
-219.06879824846));
#203171=CARTESIAN_POINT('Ctrl Pts',(-52.6935858833432,31.7306722107994,
-219.957379377995));
#203172=CARTESIAN_POINT('Ctrl Pts',(-51.1420741771435,30.7313234767532,
-221.883755689445));
#203173=CARTESIAN_POINT('Ctrl Pts',(-50.1720763337667,30.4163412318132,
-222.887464054421));
#203174=CARTESIAN_POINT('Ctrl Pts',(-48.7953703137217,30.3299008816491,
-224.056790689196));
#203175=CARTESIAN_POINT('Ctrl Pts',(-48.3973293089683,30.3422930430152,
-224.368248807804));
#203176=CARTESIAN_POINT('Ctrl Pts',(-47.5822488325699,30.4570387032031,
-224.938952842351));
#203177=CARTESIAN_POINT('Ctrl Pts',(-47.1618710052275,30.5599614050353,
-225.200460248924));
#203178=CARTESIAN_POINT('Ctrl Pts',(-46.7405472321717,30.7185439590994,
-225.41894074279));
#203179=CARTESIAN_POINT('Ctrl Pts',(-28.918632420916,36.3202559369514,-232.85005));
#203180=CARTESIAN_POINT('Ctrl Pts',(-29.1405722429493,36.1874419307039,
-232.85005));
#203181=CARTESIAN_POINT('Ctrl Pts',(-29.3442027713454,36.0636271479823,
-232.85005));
#203182=CARTESIAN_POINT('Ctrl Pts',(-29.7663007847225,35.8033260589207,
-232.85005));
#203183=CARTESIAN_POINT('Ctrl Pts',(-29.9787466996519,35.6703265943611,
-232.85005));
#203184=CARTESIAN_POINT('Ctrl Pts',(-30.6209255013549,35.2622379995154,
-232.85005));
#203185=CARTESIAN_POINT('Ctrl Pts',(-31.0479818197497,34.98254405126,-232.85005));
#203186=CARTESIAN_POINT('Ctrl Pts',(-32.3437566649082,34.1080837663654,
-232.85005));
#203187=CARTESIAN_POINT('Ctrl Pts',(-33.2007785122789,33.4934899779856,
-232.85005));
#203188=CARTESIAN_POINT('Ctrl Pts',(-35.7754719960827,31.5304296840008,
-232.85005));
#203189=CARTESIAN_POINT('Ctrl Pts',(-37.4639373139644,30.0758667472214,
-232.85005));
#203190=CARTESIAN_POINT('Ctrl Pts',(-40.599089476002,27.0270783922592,-232.85005));
#203191=CARTESIAN_POINT('Ctrl Pts',(-42.1044452521513,25.3726646453487,
-232.85005));
#203192=CARTESIAN_POINT('Ctrl Pts',(-44.762707951181,22.0795000960731,-232.85005));
#203193=CARTESIAN_POINT('Ctrl Pts',(-45.9624973465495,20.4083241018545,
-232.85005));
#203194=CARTESIAN_POINT('Ctrl Pts',(-47.0649763530314,18.681697915047,-232.85005));
#203195=CARTESIAN_POINT('Ctrl Pts',(-48.0827620446564,42.0414223951255,
-215.85005));
#203196=CARTESIAN_POINT('Ctrl Pts',(-47.6918902578017,41.9918377458004,
-216.158510565779));
#203197=CARTESIAN_POINT('Ctrl Pts',(-47.3178589835132,41.9044704486574,
-216.48375532529));
#203198=CARTESIAN_POINT('Ctrl Pts',(-46.5278541133197,41.641234161018,-217.23269561852));
#203199=CARTESIAN_POINT('Ctrl Pts',(-46.1204261816762,41.4485202650992,
-217.663837570708));
#203200=CARTESIAN_POINT('Ctrl Pts',(-44.981799852587,40.7494982164702,-219.00027770574));
#203201=CARTESIAN_POINT('Ctrl Pts',(-44.3453100117826,40.1178561866307,
-219.946031814412));
#203202=CARTESIAN_POINT('Ctrl Pts',(-43.3187329856621,38.5182399992048,
-221.95430949443));
#203203=CARTESIAN_POINT('Ctrl Pts',(-43.002470525188,37.5284133107564,-222.985431129024));
#203204=CARTESIAN_POINT('Ctrl Pts',(-42.9307447595933,36.1378442916941,
-224.156404719787));
#203205=CARTESIAN_POINT('Ctrl Pts',(-42.9463038154314,35.7490409900809,
-224.457196959813));
#203206=CARTESIAN_POINT('Ctrl Pts',(-43.0642975219893,34.9494394058048,
-225.008393072148));
#203207=CARTESIAN_POINT('Ctrl Pts',(-43.1679394115819,34.535481911261,-225.260388542568));
#203208=CARTESIAN_POINT('Ctrl Pts',(-43.3259173910694,34.1204116753623,
-225.468974352254));
#203209=CARTESIAN_POINT('',(-45.7333210472294,31.2122413349066,-225.850044625489));
#203210=CARTESIAN_POINT('Ctrl Pts',(-45.7333215211538,31.2122476871429,
-225.850034142281));
#203211=CARTESIAN_POINT('Ctrl Pts',(-45.3380055594478,31.455444850938,-225.979526553824));
#203212=CARTESIAN_POINT('Ctrl Pts',(-44.9655439649494,31.7492431768137,
-226.049129920994));
#203213=CARTESIAN_POINT('Ctrl Pts',(-44.2903200744336,32.435009374361,-226.04918891067));
#203214=CARTESIAN_POINT('Ctrl Pts',(-44.0029189269882,32.8110299162004,
-225.979864418515));
#203215=CARTESIAN_POINT('Ctrl Pts',(-43.7661192040752,33.2092653547038,
-225.850049930202));
#203216=CARTESIAN_POINT('',(-46.4511396589728,30.4281656954993,-225.850049999692));
#203217=CARTESIAN_POINT('Ctrl Pts',(-46.4511396584396,30.4281656950206,
-225.85005));
#203218=CARTESIAN_POINT('Ctrl Pts',(-46.3327936013924,30.5600059653032,
-225.85005));
#203219=CARTESIAN_POINT('Ctrl Pts',(-46.2137942836441,30.6912801190928,
-225.85005));
#203220=CARTESIAN_POINT('Ctrl Pts',(-45.9745262548726,30.952635522043,-225.85005));
#203221=CARTESIAN_POINT('Ctrl Pts',(-45.8542372577667,31.0827388238805,
-225.85005));
#203222=CARTESIAN_POINT('Ctrl Pts',(-45.7333160870584,31.2122314463161,
-225.85005));
#203223=CARTESIAN_POINT('Ctrl Pts',(-46.4511396588545,30.4281656952996,
-225.850049999479));
#203224=CARTESIAN_POINT('Ctrl Pts',(-46.49937538757,30.476563209559,-225.778199404494));
#203225=CARTESIAN_POINT('Ctrl Pts',(-46.5476099273389,30.5249595308839,
-225.706349253907));
#203226=CARTESIAN_POINT('Ctrl Pts',(-46.6440796086263,30.6217527773017,
-225.562645429306));
#203227=CARTESIAN_POINT('Ctrl Pts',(-46.6923132700127,30.670148217298,-225.490793960134));
#203228=CARTESIAN_POINT('Ctrl Pts',(-46.7405472321751,30.7185439590791,
-225.418940742802));
#203229=CARTESIAN_POINT('Origin',(0.,-12.9675000200281,-215.85005));
#203230=CARTESIAN_POINT('',(-48.069978588367,-67.6025450148014,-215.850048907738));
#203231=CARTESIAN_POINT('Ctrl Pts',(-48.0699790801226,-67.6025411545956,
-215.85005));
#203232=CARTESIAN_POINT('Ctrl Pts',(-48.2216024642868,-67.4737675776872,
-215.85005));
#203233=CARTESIAN_POINT('Ctrl Pts',(-48.37313230858,-67.3439224269873,-215.850050000034));
#203234=CARTESIAN_POINT('Ctrl Pts',(-48.672769750555,-67.0849704871732,
-215.850050000034));
#203235=CARTESIAN_POINT('Ctrl Pts',(-48.8224593013279,-66.9544830612177,
-215.85005));
#203236=CARTESIAN_POINT('Ctrl Pts',(-48.9715866554311,-66.8233021636441,
-215.85005));
#203237=CARTESIAN_POINT('',(-53.9390346875574,-61.9113848028034,-215.85005));
#203238=CARTESIAN_POINT('Origin',(-48.1334350484927,-61.7961505568785,-215.85005));
#203239=CARTESIAN_POINT('Ctrl Pts',(-53.7300151844416,-62.1425230012532,
-215.85005));
#203240=CARTESIAN_POINT('Ctrl Pts',(-53.7649393991568,-62.1040873964405,
-215.85005));
#203241=CARTESIAN_POINT('Ctrl Pts',(-53.799816986159,-62.0656105112331,
-215.85005));
#203242=CARTESIAN_POINT('Ctrl Pts',(-53.8694902457089,-61.9885636960974,
-215.85005));
#203243=CARTESIAN_POINT('Ctrl Pts',(-53.9042848508542,-61.9499949024127,
-215.85005));
#203244=CARTESIAN_POINT('Ctrl Pts',(-53.9390346875574,-61.9113848028034,
-215.85005));
#203245=CARTESIAN_POINT('Ctrl Pts',(-46.9944270680642,-41.6193123752663,
-233.004519986905));
#203246=CARTESIAN_POINT('Ctrl Pts',(-48.7878616654988,-44.7175816808496,
-229.860902939557));
#203247=CARTESIAN_POINT('Ctrl Pts',(-50.5840414119712,-47.8137084153908,
-226.716710153573));
#203248=CARTESIAN_POINT('Ctrl Pts',(-52.3845374377678,-50.9067036630134,
-223.571849766529));
#203249=CARTESIAN_POINT('Ctrl Pts',(-54.1850334635645,-53.999698910636,
-220.426989379484));
#203250=CARTESIAN_POINT('Ctrl Pts',(-55.9897753069174,-57.0895865666151,
-217.281445207064));
#203251=CARTESIAN_POINT('Ctrl Pts',(-57.8017289442242,-60.1747340778167,
-214.135276372889));
#203252=CARTESIAN_POINT('Ctrl Pts',(-46.9566286849537,-41.6781739629451,
-233.004786483119));
#203253=CARTESIAN_POINT('Ctrl Pts',(-48.7510652266437,-44.7730579825931,
-229.861179418927));
#203254=CARTESIAN_POINT('Ctrl Pts',(-50.5482471004081,-47.8657963569279,
-226.716997721658));
#203255=CARTESIAN_POINT('Ctrl Pts',(-52.3497454436632,-50.9553990731154,
-223.572150029539));
#203256=CARTESIAN_POINT('Ctrl Pts',(-54.1512437869183,-54.045001789303,
-220.427302337419));
#203257=CARTESIAN_POINT('Ctrl Pts',(-55.9569880950718,-57.1314927928873,
-217.28177244287));
#203258=CARTESIAN_POINT('Ctrl Pts',(-57.7699448315789,-60.2132374154909,
-214.135620383829));
#203259=CARTESIAN_POINT('Ctrl Pts',(-46.9219121704599,-41.7340896317106,
-233.003924127997));
#203260=CARTESIAN_POINT('Ctrl Pts',(-48.7170243830511,-44.8259324838809,
-229.860501038468));
#203261=CARTESIAN_POINT('Ctrl Pts',(-50.5148833131725,-47.9156143059604,
-226.716492970748));
#203262=CARTESIAN_POINT('Ctrl Pts',(-52.3171186451179,-51.0020915740055,
-223.571790312035));
#203263=CARTESIAN_POINT('Ctrl Pts',(-54.1193539770633,-54.0885688420506,
-220.427087653323));
#203264=CARTESIAN_POINT('Ctrl Pts',(-55.9258862266926,-57.1718702110663,
-217.28167372519));
#203265=CARTESIAN_POINT('Ctrl Pts',(-57.7398613178177,-60.2502287004015,
-214.1355819053));
#203266=CARTESIAN_POINT('Ctrl Pts',(-46.8853928444761,-41.791544195152,
-233.003625168491));
#203267=CARTESIAN_POINT('Ctrl Pts',(-48.681427442577,-44.8800992987762,
-229.860296540463));
#203268=CARTESIAN_POINT('Ctrl Pts',(-50.4802079998591,-47.9664858608819,
-226.716379335157));
#203269=CARTESIAN_POINT('Ctrl Pts',(-52.2833924017896,-51.0496336439922,
-223.57175528194));
#203270=CARTESIAN_POINT('Ctrl Pts',(-54.0865768037201,-54.1327814271025,
-220.427131228723));
#203271=CARTESIAN_POINT('Ctrl Pts',(-55.8940807177617,-57.2127217368356,
-217.281783456688));
#203272=CARTESIAN_POINT('Ctrl Pts',(-57.7091409883845,-60.287618730288,
-214.135731970477));
#203273=CARTESIAN_POINT('Ctrl Pts',(-46.8488735184923,-41.8489987585935,
-233.003326208986));
#203274=CARTESIAN_POINT('Ctrl Pts',(-48.645830502103,-44.9342661136713,
-229.860092042457));
#203275=CARTESIAN_POINT('Ctrl Pts',(-50.4455326865456,-48.0173574158033,
-226.716265699565));
#203276=CARTESIAN_POINT('Ctrl Pts',(-52.2496661584613,-51.0971757139789,
-223.571720251843));
#203277=CARTESIAN_POINT('Ctrl Pts',(-54.053799630377,-54.1769940121544,
-220.427174804122));
#203278=CARTESIAN_POINT('Ctrl Pts',(-55.8622752088309,-57.2535732626049,
-217.281893188185));
#203279=CARTESIAN_POINT('Ctrl Pts',(-57.6784206589513,-60.3250087601744,
-214.135882035655));
#203280=CARTESIAN_POINT('Ctrl Pts',(-46.8121794637376,-41.9064965273971,
-233.003026620871));
#203281=CARTESIAN_POINT('Ctrl Pts',(-48.6101143190285,-44.9884269324132,
-229.859885255064));
#203282=CARTESIAN_POINT('Ctrl Pts',(-50.4107926169958,-48.0681748858937,
-226.716148772852));
#203283=CARTESIAN_POINT('Ctrl Pts',(-52.2159279111165,-51.1446171397359,
-223.571681746167));
#203284=CARTESIAN_POINT('Ctrl Pts',(-54.0210632052373,-54.221059393578,
-220.427214719482));
#203285=CARTESIAN_POINT('Ctrl Pts',(-55.8305612422911,-57.2942327369214,
-217.281999929988));
#203286=CARTESIAN_POINT('Ctrl Pts',(-57.6478412701604,-60.3621625545191,
-214.136030325987));
#203287=CARTESIAN_POINT('Ctrl Pts',(-46.7753102520778,-41.9640352485997,
-233.002726574857));
#203288=CARTESIAN_POINT('Ctrl Pts',(-48.5742777683907,-45.0425809377688,
-229.859676400769));
#203289=CARTESIAN_POINT('Ctrl Pts',(-50.3759860497308,-48.1189387987811,
-226.716028769071));
#203290=CARTESIAN_POINT('Ctrl Pts',(-52.1821753368859,-51.191959764097,
-223.571639944857));
#203291=CARTESIAN_POINT('Ctrl Pts',(-53.9883646240409,-54.264980729413,
-220.427251120643));
#203292=CARTESIAN_POINT('Ctrl Pts',(-55.7989353732621,-57.3347046065519,
-217.282103770803));
#203293=CARTESIAN_POINT('Ctrl Pts',(-57.6173986625019,-60.3990859831037,
-214.136176919604));
#203294=CARTESIAN_POINT('Ctrl Pts',(-46.7015718287581,-42.0791126910049,
-233.00212648283));
#203295=CARTESIAN_POINT('Ctrl Pts',(-48.5026046671152,-45.1508889484801,
-229.859258692179));
#203296=CARTESIAN_POINT('Ctrl Pts',(-50.3063729152009,-48.2204666245557,
-226.715788761507));
#203297=CARTESIAN_POINT('Ctrl Pts',(-52.1146701884246,-51.2866450128194,
-223.571556342237));
#203298=CARTESIAN_POINT('Ctrl Pts',(-53.9229674616482,-54.3528234010831,
-220.427323922968));
#203299=CARTESIAN_POINT('Ctrl Pts',(-55.7356836352042,-57.4156483458129,
-217.282311452432));
#203300=CARTESIAN_POINT('Ctrl Pts',(-57.5565134471849,-60.4729328402728,
-214.136470106837));
#203301=CARTESIAN_POINT('Ctrl Pts',(-46.6271327739678,-42.1943539415595,
-233.001524562797));
#203302=CARTESIAN_POINT('Ctrl Pts',(-48.4304500911505,-45.2591697072969,
-229.858832720452));
#203303=CARTESIAN_POINT('Ctrl Pts',(-50.2364937898458,-48.3217802201232,
-226.715536447315));
#203304=CARTESIAN_POINT('Ctrl Pts',(-52.0471077366989,-51.3809350513845,
-223.571459556911));
#203305=CARTESIAN_POINT('Ctrl Pts',(-53.857721683552,-54.4400898826458,
-220.427382666507));
#203306=CARTESIAN_POINT('Ctrl Pts',(-55.672784296813,-57.4958416576678,
-217.282507528118));
#203307=CARTESIAN_POINT('Ctrl Pts',(-57.4961753701015,-60.5458582201909,
-214.136756507531));
#203308=CARTESIAN_POINT('Ctrl Pts',(-46.5519897086414,-42.3097409936012,
-233.000922137489));
#203309=CARTESIAN_POINT('Ctrl Pts',(-48.3578050935127,-45.3674166545976,
-229.858400212826));
#203310=CARTESIAN_POINT('Ctrl Pts',(-50.166334738395,-48.4228838232303,
-226.715273522923));
#203311=CARTESIAN_POINT('Ctrl Pts',(-51.9794693444289,-51.4748446769843,
-223.571351034937));
#203312=CARTESIAN_POINT('Ctrl Pts',(-53.7926039504629,-54.5268055307383,
-220.427428546952));
#203313=CARTESIAN_POINT('Ctrl Pts',(-55.6102096831407,-57.5753202178,-217.28269273506));
#203314=CARTESIAN_POINT('Ctrl Pts',(-57.4363509894997,-60.6179092484165,
-214.137036747929));
#203315=CARTESIAN_POINT('Ctrl Pts',(-46.4017035779887,-42.5405150976846,
-232.999717286874));
#203316=CARTESIAN_POINT('Ctrl Pts',(-48.2125150982371,-45.5839105491989,
-229.857535197574));
#203317=CARTESIAN_POINT('Ctrl Pts',(-50.0260166354934,-48.6250910294446,
-226.714747674137));
#203318=CARTESIAN_POINT('Ctrl Pts',(-51.844192559889,-51.6626639281839,
-223.571133990991));
#203319=CARTESIAN_POINT('Ctrl Pts',(-53.6623684842846,-54.7002368269232,
-220.427520307844));
#203320=CARTESIAN_POINT('Ctrl Pts',(-55.4850604557961,-57.7342773380644,
-217.283063148945));
#203321=CARTESIAN_POINT('Ctrl Pts',(-57.3167022282962,-60.7620113048676,
-214.137597228726));
#203322=CARTESIAN_POINT('Ctrl Pts',(-46.2486013427642,-42.7718723828066,
-232.998510473058));
#203323=CARTESIAN_POINT('Ctrl Pts',(-48.0652633432344,-45.8002692151702,
-229.856644114599));
#203324=CARTESIAN_POINT('Ctrl Pts',(-49.8845788152544,-48.8264582428966,
-226.714179427834));
#203325=CARTESIAN_POINT('Ctrl Pts',(-51.708612066789,-51.848961452988,-223.570870018747));
#203326=CARTESIAN_POINT('Ctrl Pts',(-53.5326453183235,-54.8714646630795,
-220.427560609659));
#203327=CARTESIAN_POINT('Ctrl Pts',(-55.3612102766787,-57.8903753028513,
-217.283390075808));
#203328=CARTESIAN_POINT('Ctrl Pts',(-57.1991084585358,-60.9026157167782,
-214.13813310078));
#203329=CARTESIAN_POINT('Ctrl Pts',(-46.0926567139982,-43.0036690826345,
-232.997311586148));
#203330=CARTESIAN_POINT('Ctrl Pts',(-47.9159791152656,-46.0164399058077,
-229.855739900183));
#203331=CARTESIAN_POINT('Ctrl Pts',(-49.7419098599322,-49.0270196364001,
-226.713581949947));
#203332=CARTESIAN_POINT('Ctrl Pts',(-51.5725780231494,-52.0338565143131,
-223.570570609253));
#203333=CARTESIAN_POINT('Ctrl Pts',(-53.4032461863666,-55.0406933922261,
-220.427559268559));
#203334=CARTESIAN_POINT('Ctrl Pts',(-55.2384359222485,-58.0439012335412,
-217.283679691665));
#203335=CARTESIAN_POINT('Ctrl Pts',(-57.083299585097,-61.0401022731089,
-214.13864916931));
#203336=CARTESIAN_POINT('Ctrl Pts',(-45.7807674564663,-43.4672624822902,
-232.994913812328));
#203337=CARTESIAN_POINT('Ctrl Pts',(-47.617410659328,-46.4487812870827,
-229.853931471351));
#203338=CARTESIAN_POINT('Ctrl Pts',(-49.4565719492878,-49.4281424234071,
-226.71238699417));
#203339=CARTESIAN_POINT('Ctrl Pts',(-51.3005099358702,-52.4036466369632,
-223.569971790265));
#203340=CARTESIAN_POINT('Ctrl Pts',(-53.1444479224527,-55.3791508505193,
-220.427556586359));
#203341=CARTESIAN_POINT('Ctrl Pts',(-54.992887213388,-58.3509530949211,
-217.284258923378));
#203342=CARTESIAN_POINT('Ctrl Pts',(-56.8516818382195,-61.3150753857701,
-214.139681306367));
#203343=CARTESIAN_POINT('Ctrl Pts',(-45.457507604722,-43.9326130692061,
-232.99254867873));
#203344=CARTESIAN_POINT('Ctrl Pts',(-47.3107111022754,-46.8803707732786,
-229.852071833745));
#203345=CARTESIAN_POINT('Ctrl Pts',(-49.1663089215364,-49.8260415059931,
-226.711076271479));
#203346=CARTESIAN_POINT('Ctrl Pts',(-51.0266279973321,-52.7678256944002,
-223.569232172689));
#203347=CARTESIAN_POINT('Ctrl Pts',(-52.8869470731278,-55.7096098828074,
-220.427388073898));
#203348=CARTESIAN_POINT('Ctrl Pts',(-54.7516438900022,-58.6477142186619,
-217.284689472746));
#203349=CARTESIAN_POINT('Ctrl Pts',(-56.6272059226936,-61.5775733671438,
-214.14063576296));
#203350=CARTESIAN_POINT('Ctrl Pts',(-45.122678945944,-44.3985758751927,
-232.990284156912));
#203351=CARTESIAN_POINT('Ctrl Pts',(-46.9953289795326,-47.3107844763396,
-229.850249364904));
#203352=CARTESIAN_POINT('Ctrl Pts',(-48.8702338796761,-50.2209949619586,
-226.709744329754));
#203353=CARTESIAN_POINT('Ctrl Pts',(-50.7497258393681,-53.1273622037278,
-223.56843670589));
#203354=CARTESIAN_POINT('Ctrl Pts',(-52.62921779906,-56.033729445497,-220.427129082025));
#203355=CARTESIAN_POINT('Ctrl Pts',(-54.5128930537055,-58.9365113017985,
-217.285019110898));
#203356=CARTESIAN_POINT('Ctrl Pts',(-56.4076769323115,-61.8306798185293,
-214.141539423862));
#203357=CARTESIAN_POINT('Ctrl Pts',(-44.4530216283881,-45.330501487166,
-232.985755113274));
#203358=CARTESIAN_POINT('Ctrl Pts',(-46.364564734047,-48.1716118824616,
-229.846604427224));
#203359=CARTESIAN_POINT('Ctrl Pts',(-48.2780837959556,-51.0109018738896,
-226.707080446303));
#203360=CARTESIAN_POINT('Ctrl Pts',(-50.19592152344,-53.846435222383,-223.566845772292));
#203361=CARTESIAN_POINT('Ctrl Pts',(-52.1137592509244,-56.6819685708763,
-220.42661109828));
#203362=CARTESIAN_POINT('Ctrl Pts',(-54.0353913811122,-59.5141054680716,
-217.285678387203));
#203363=CARTESIAN_POINT('Ctrl Pts',(-55.9686189515471,-62.3368927213004,
-214.143346745665));
#203364=CARTESIAN_POINT('Ctrl Pts',(-43.7371085113763,-46.2648305947527,
-232.981637432207));
#203365=CARTESIAN_POINT('Ctrl Pts',(-45.6990794088443,-49.0277012666958,
-229.84312647621));
#203366=CARTESIAN_POINT('Ctrl Pts',(-47.6626881850455,-51.7889977645385,
-226.704357361211));
#203367=CARTESIAN_POINT('Ctrl Pts',(-49.6300299185432,-54.5469161187202,
-223.565063052865));
#203368=CARTESIAN_POINT('Ctrl Pts',(-51.5973716520409,-57.3048344729019,
-220.425768744518));
#203369=CARTESIAN_POINT('Ctrl Pts',(-53.5678464328781,-60.0598292382354,
-217.285973682359));
#203370=CARTESIAN_POINT('Ctrl Pts',(-55.5492457890124,-62.8055814665179,
-214.145012087778));
#203371=CARTESIAN_POINT('Ctrl Pts',(-42.9734424791526,-47.1926155685251,
-232.978313839575));
#203372=CARTESIAN_POINT('Ctrl Pts',(-44.9946071331279,-49.8757842370209,
-229.840273609375));
#203373=CARTESIAN_POINT('Ctrl Pts',(-47.0170439436796,-52.5576635978524,
-226.702063718992));
#203374=CARTESIAN_POINT('Ctrl Pts',(-49.0424058070309,-55.2367916852255,
-223.563495724472));
#203375=CARTESIAN_POINT('Ctrl Pts',(-51.0677676703821,-57.9159197725986,
-220.424927729951));
#203376=CARTESIAN_POINT('Ctrl Pts',(-53.0955326872786,-60.5927163347612,
-217.286025395512));
#203377=CARTESIAN_POINT('Ctrl Pts',(-55.1321416284158,-63.2617424152049,
-214.146274180285));
#203378=CARTESIAN_POINT('Ctrl Pts',(-41.4461104147051,-49.0481855160699,
-232.97166665431));
#203379=CARTESIAN_POINT('Ctrl Pts',(-43.5856625816949,-51.5719501776712,
-229.834567875703));
#203380=CARTESIAN_POINT('Ctrl Pts',(-45.725755460948,-54.09499526448,-226.697476434552));
#203381=CARTESIAN_POINT('Ctrl Pts',(-47.8671575840062,-56.616542818236,
-223.560361067685));
#203382=CARTESIAN_POINT('Ctrl Pts',(-50.0085597070645,-59.138090371992,
-220.423245700818));
#203383=CARTESIAN_POINT('Ctrl Pts',(-52.1509051960796,-61.6584905278127,
-217.286128821816));
#203384=CARTESIAN_POINT('Ctrl Pts',(-54.2979333072227,-64.1740643125789,
-214.148798365297));
#203385=CARTESIAN_POINT('Ctrl Pts',(-39.7224455239868,-50.8825869261812,
-232.968811623327));
#203386=CARTESIAN_POINT('Ctrl Pts',(-42.0166284209611,-53.2398821108309,
-229.831855736726));
#203387=CARTESIAN_POINT('Ctrl Pts',(-44.3107862632822,-55.5969218113776,
-226.694951854308));
#203388=CARTESIAN_POINT('Ctrl Pts',(-46.6046310902244,-57.9539261591375,
-223.55816686563));
#203389=CARTESIAN_POINT('Ctrl Pts',(-48.8984759171666,-60.3109305068973,
-220.421381876952));
#203390=CARTESIAN_POINT('Ctrl Pts',(-51.1921534761245,-62.6678044223395,
-217.284704907766));
#203391=CARTESIAN_POINT('Ctrl Pts',(-53.4842288420267,-65.0255514956176,
-214.148339440146));
#203392=CARTESIAN_POINT('Ctrl Pts',(-37.882123536986,-52.5752193780183,
-232.970806720566));
#203393=CARTESIAN_POINT('Ctrl Pts',(-40.3469003584876,-54.7858287675482,
-229.833381329414));
#203394=CARTESIAN_POINT('Ctrl Pts',(-42.8110087314114,-56.9968033268292,
-226.695906966754));
#203395=CARTESIAN_POINT('Ctrl Pts',(-45.2731441984033,-59.2095312210711,
-223.558332736904));
#203396=CARTESIAN_POINT('Ctrl Pts',(-47.7352796653952,-61.4222591153131,
-220.420758507053));
#203397=CARTESIAN_POINT('Ctrl Pts',(-50.1959790879104,-63.636130388643,
-217.283078469976));
#203398=CARTESIAN_POINT('Ctrl Pts',(-52.6494272678771,-65.857552778289,
-214.145217662806));
#203399=CARTESIAN_POINT('Ctrl Pts',(-36.0418015499852,-54.2678518298554,
-232.972801817804));
#203400=CARTESIAN_POINT('Ctrl Pts',(-38.677172296014,-56.3317754242655,
-229.834906922101));
#203401=CARTESIAN_POINT('Ctrl Pts',(-41.3112311995406,-58.3966848422808,
-226.696862079201));
#203402=CARTESIAN_POINT('Ctrl Pts',(-43.9416573065822,-60.4651362830048,
-223.558498608177));
#203403=CARTESIAN_POINT('Ctrl Pts',(-46.5720834136237,-62.5335877237288,
-220.420135137153));
#203404=CARTESIAN_POINT('Ctrl Pts',(-49.1998046996963,-64.6044563549465,
-217.281452032185));
#203405=CARTESIAN_POINT('Ctrl Pts',(-51.8146256937275,-66.6895540609604,
-214.142095885467));
#203406=CARTESIAN_POINT('Ctrl Pts',(-34.0754426298001,-55.8293718868815,
-232.978994680116));
#203407=CARTESIAN_POINT('Ctrl Pts',(-36.898122716604,-57.765479730986,-229.840093780616));
#203408=CARTESIAN_POINT('Ctrl Pts',(-39.7189124685042,-59.7032049990848,
-226.700797887619));
#203409=CARTESIAN_POINT('Ctrl Pts',(-42.5347347571142,-61.6462105210921,
-223.560608578979));
#203410=CARTESIAN_POINT('Ctrl Pts',(-45.3505570457242,-63.5892160430994,
-220.420419270338));
#203411=CARTESIAN_POINT('Ctrl Pts',(-48.1623968718184,-65.5360552707562,
-217.279358981544));
#203412=CARTESIAN_POINT('Ctrl Pts',(-50.9580697373535,-67.5028226458884,
-214.13623151235));
#203413=CARTESIAN_POINT('Ctrl Pts',(-32.1087006613968,-57.191646012686,
-232.989078118058));
#203414=CARTESIAN_POINT('Ctrl Pts',(-35.1076397475695,-59.0371491145894,
-229.847995786691));
#203415=CARTESIAN_POINT('Ctrl Pts',(-38.1040273439412,-60.8851347665649,
-226.706162642268));
#203416=CARTESIAN_POINT('Ctrl Pts',(-41.0945558666574,-62.7399255565489,
-223.562922655666));
#203417=CARTESIAN_POINT('Ctrl Pts',(-44.0850843893735,-64.5947163465329,
-220.419682669063));
#203418=CARTESIAN_POINT('Ctrl Pts',(-47.0704902905866,-66.4550539448948,
-217.275009748779));
#203419=CARTESIAN_POINT('Ctrl Pts',(-50.0397793224693,-68.3371871397263,
-214.127816818154));
#203420=CARTESIAN_POINT('Ctrl Pts',(-31.1253296771952,-57.8727830755883,
-232.994119837029));
#203421=CARTESIAN_POINT('Ctrl Pts',(-34.2123982630523,-59.6729838063912,
-229.851946789728));
#203422=CARTESIAN_POINT('Ctrl Pts',(-37.2965847816597,-61.4760996503049,
-226.708845019593));
#203423=CARTESIAN_POINT('Ctrl Pts',(-40.374466421429,-63.2867830742773,
-223.564079694009));
#203424=CARTESIAN_POINT('Ctrl Pts',(-43.4523480611983,-65.0974664982497,
-220.419314368426));
#203425=CARTESIAN_POINT('Ctrl Pts',(-46.5245369999706,-66.9145532819642,
-217.272835132396));
#203426=CARTESIAN_POINT('Ctrl Pts',(-49.5806341150271,-68.7543693866452,
-214.123609471056));
#203427=CARTESIAN_POINT('Ctrl Pts',(-30.1402892390281,-58.5059782041702,
-232.999787567079));
#203428=CARTESIAN_POINT('Ctrl Pts',(-33.312862968668,-60.2699670414456,
-229.856286548401));
#203429=CARTESIAN_POINT('Ctrl Pts',(-36.4822633143695,-62.0372971477581,
-226.711666225327));
#203430=CARTESIAN_POINT('Ctrl Pts',(-39.645238310907,-63.8126368978593,
-223.565198694695));
#203431=CARTESIAN_POINT('Ctrl Pts',(-42.8082133074446,-65.5879766479605,
-220.418731164063));
#203432=CARTESIAN_POINT('Ctrl Pts',(-45.9651478987472,-67.3704636405086,
-217.270335425737));
#203433=CARTESIAN_POINT('Ctrl Pts',(-49.1075700836515,-69.1744983835783,
-214.119318043209));
#203434=CARTESIAN_POINT('Ctrl Pts',(-29.1622830188973,-59.093703206177,
-233.005601149464));
#203435=CARTESIAN_POINT('Ctrl Pts',(-32.4119055964007,-60.8333256128672,
-229.860352517102));
#203436=CARTESIAN_POINT('Ctrl Pts',(-35.6582030143032,-62.5766317072687,
-226.713886241748));
#203437=CARTESIAN_POINT('Ctrl Pts',(-38.8983695571512,-64.3279278794606,
-223.565632722533));
#203438=CARTESIAN_POINT('Ctrl Pts',(-42.1385360999994,-66.0792240516524,
-220.417379203317));
#203439=CARTESIAN_POINT('Ctrl Pts',(-45.3727988408086,-67.8379178590787,
-217.267251393612));
#203440=CARTESIAN_POINT('Ctrl Pts',(-48.5947562955792,-69.6157591498535,
-214.114999659484));
#203441=CARTESIAN_POINT('Ctrl Pts',(-28.673279908832,-59.3875657071804,
-233.008507940657));
#203442=CARTESIAN_POINT('Ctrl Pts',(-31.9614269102671,-61.115004898578,
-229.862385501452));
#203443=CARTESIAN_POINT('Ctrl Pts',(-35.2461728642701,-62.846298987024,
-226.714996249958));
#203444=CARTESIAN_POINT('Ctrl Pts',(-38.5249351802734,-64.5855733702612,
-223.565849736452));
#203445=CARTESIAN_POINT('Ctrl Pts',(-41.8036974962768,-66.3248477534984,
-220.416703222945));
#203446=CARTESIAN_POINT('Ctrl Pts',(-45.0766243118393,-68.0716449683638,
-217.26570937755));
#203447=CARTESIAN_POINT('Ctrl Pts',(-48.338349401543,-69.8363895329911,
-214.112840467621));
#203448=CARTESIAN_POINT('Ctrl Pts',(-28.1860374776607,-59.6700652305358,
-233.011446770425));
#203449=CARTESIAN_POINT('Ctrl Pts',(-31.5105936078552,-61.3882833386183,
-229.864343520922));
#203450=CARTESIAN_POINT('Ctrl Pts',(-34.8317102236203,-63.1105042946341,
-226.715949123638));
#203451=CARTESIAN_POINT('Ctrl Pts',(-38.1470954909054,-64.8405791788429,
-223.565888981583));
#203452=CARTESIAN_POINT('Ctrl Pts',(-41.4624807581906,-66.5706540630517,
-220.415828839529));
#203453=CARTESIAN_POINT('Ctrl Pts',(-44.772220394414,-68.3082505831985,
-217.264016183284));
#203454=CARTESIAN_POINT('Ctrl Pts',(-48.0720115712419,-70.062309547184,
-214.110662164981));
#203455=CARTESIAN_POINT('Ctrl Pts',(-27.7016532108346,-59.9415372606891,
-233.014331652954));
#203456=CARTESIAN_POINT('Ctrl Pts',(-31.05976276075,-61.6538447557032,-229.866107695338));
#203457=CARTESIAN_POINT('Ctrl Pts',(-34.4144695478916,-63.3702479288391,
-226.716625256232));
#203458=CARTESIAN_POINT('Ctrl Pts',(-37.7638186351444,-65.0942396965474,
-223.565650201608));
#203459=CARTESIAN_POINT('Ctrl Pts',(-41.1131677223973,-66.8182314642556,
-220.414675146985));
#203460=CARTESIAN_POINT('Ctrl Pts',(-44.4572046958943,-68.5495754713907,
-217.262129974306));
#203461=CARTESIAN_POINT('Ctrl Pts',(-47.7925819070095,-70.295770952258,
-214.1084263508));
#203462=CARTESIAN_POINT('Ctrl Pts',(-27.4594610774215,-60.0772732757658,
-233.015774094218));
#203463=CARTESIAN_POINT('Ctrl Pts',(-30.8343473371973,-61.7866254642456,
-229.866989782546));
#203464=CARTESIAN_POINT('Ctrl Pts',(-34.2058492100272,-63.5001197459416,
-226.716963322528));
#203465=CARTESIAN_POINT('Ctrl Pts',(-37.5721802072639,-65.2210699553996,
-223.565530811621));
#203466=CARTESIAN_POINT('Ctrl Pts',(-40.9385112045005,-66.9420201648576,
-220.414098300713));
#203467=CARTESIAN_POINT('Ctrl Pts',(-44.2996968466345,-68.6702379154868,
-217.261186869816));
#203468=CARTESIAN_POINT('Ctrl Pts',(-47.6528670748933,-70.412501654795,
-214.107308443709));
#203469=CARTESIAN_POINT('Ctrl Pts',(-27.2179835587658,-60.2102526866361,
-233.017202782736));
#203470=CARTESIAN_POINT('Ctrl Pts',(-30.608932448567,-61.9174772218177,
-229.867823057804));
#203471=CARTESIAN_POINT('Ctrl Pts',(-33.9965344785202,-63.628876184999,
-226.717232037632));
#203472=CARTESIAN_POINT('Ctrl Pts',(-37.3791828237546,-65.3475636411034,
-223.565341878319));
#203473=CARTESIAN_POINT('Ctrl Pts',(-40.761831168989,-67.0662510972078,
-220.413451719006));
#203474=CARTESIAN_POINT('Ctrl Pts',(-44.1395366106154,-68.7920796018397,
-217.260195585412));
#203475=CARTESIAN_POINT('Ctrl Pts',(-47.509880204324,-70.5311169985697,
-214.10617593024));
#203476=CARTESIAN_POINT('Ctrl Pts',(-26.9773582084069,-60.3405190002037,
-233.018605415792));
#203477=CARTESIAN_POINT('Ctrl Pts',(-30.383562017878,-62.046487235826,-229.868590727832));
#203478=CARTESIAN_POINT('Ctrl Pts',(-33.786482884195,-63.7566420726074,
-226.717416049128));
#203479=CARTESIAN_POINT('Ctrl Pts',(-37.1846995203357,-65.4738805679581,
-223.56507131637));
#203480=CARTESIAN_POINT('Ctrl Pts',(-40.5829161564765,-67.1911190633088,
-220.412726583613));
#203481=CARTESIAN_POINT('Ctrl Pts',(-43.9764292691396,-68.9153271247727,
-217.259151804163));
#203482=CARTESIAN_POINT('Ctrl Pts',(-47.3632316759027,-70.6518934365393,
-214.105023471352));
#203483=CARTESIAN_POINT('Ctrl Pts',(-26.8570455332274,-60.4056521569874,
-233.019306732319));
#203484=CARTESIAN_POINT('Ctrl Pts',(-30.2708768025335,-62.1109922428301,
-229.868974562847));
#203485=CARTESIAN_POINT('Ctrl Pts',(-33.6814570870323,-63.8205250164116,
-226.717508054876));
#203486=CARTESIAN_POINT('Ctrl Pts',(-37.0874578686263,-65.5370390313854,
-223.564936035396));
#203487=CARTESIAN_POINT('Ctrl Pts',(-40.4934586502203,-67.2535530463592,
-220.412364015916));
#203488=CARTESIAN_POINT('Ctrl Pts',(-43.8948755984016,-68.9769508862391,
-217.258629913538));
#203489=CARTESIAN_POINT('Ctrl Pts',(-47.289907411692,-70.7122816555241,
-214.104447241908));
#203490=CARTESIAN_POINT('Ctrl Pts',(-26.7369459033605,-60.4701070554585,
-233.020001519128));
#203491=CARTESIAN_POINT('Ctrl Pts',(-30.1582026923428,-62.1750368311418,
-229.869341977822));
#203492=CARTESIAN_POINT('Ctrl Pts',(-33.5762470819994,-63.8841603164497,
-226.717578885404));
#203493=CARTESIAN_POINT('Ctrl Pts',(-36.9898447579513,-65.6001532805383,
-223.564780357348));
#203494=CARTESIAN_POINT('Ctrl Pts',(-40.4034424339031,-67.3161462446269,
-220.411981829292));
#203495=CARTESIAN_POINT('Ctrl Pts',(-43.8125851811644,-69.0389260700454,
-217.258094911949));
#203496=CARTESIAN_POINT('Ctrl Pts',(-47.2156677897142,-70.7732100898985,
-214.103866027175));
#203497=CARTESIAN_POINT('Ctrl Pts',(-26.6170765305167,-60.5338892284733,
-233.020688145171));
#203498=CARTESIAN_POINT('Ctrl Pts',(-30.045545113986,-62.238632000908,-229.869690768214));
#203499=CARTESIAN_POINT('Ctrl Pts',(-33.4708476093749,-63.9475635251553,
-226.717626646141));
#203500=CARTESIAN_POINT('Ctrl Pts',(-36.8918444428126,-65.6632431316632,
-223.564602851986));
#203501=CARTESIAN_POINT('Ctrl Pts',(-40.3128412762504,-67.378922738171,
-220.411579057831));
#203502=CARTESIAN_POINT('Ctrl Pts',(-43.7295213469238,-69.1012807810974,
-217.257546349595));
#203503=CARTESIAN_POINT('Ctrl Pts',(-47.140464436521,-70.8347129400802,
-214.103279186265));
#203504=CARTESIAN_POINT('Ctrl Pts',(-26.4972071576729,-60.5976714014882,
-233.021374771214));
#203505=CARTESIAN_POINT('Ctrl Pts',(-29.9328875356291,-62.3022271706743,
-229.870039558606));
#203506=CARTESIAN_POINT('Ctrl Pts',(-33.3654481367504,-64.010966733861,
-226.717674406878));
#203507=CARTESIAN_POINT('Ctrl Pts',(-36.793844127674,-65.7263329827881,
-223.564425346624));
#203508=CARTESIAN_POINT('Ctrl Pts',(-40.2222401185977,-67.4416992317152,
-220.411176286369));
#203509=CARTESIAN_POINT('Ctrl Pts',(-43.6464575126834,-69.1636354921494,
-217.256997787241));
#203510=CARTESIAN_POINT('Ctrl Pts',(-47.0652610833278,-70.8962157902618,
-214.102692345356));
#203511=CARTESIAN_POINT('Ctrl Pts',(-26.3772071408559,-60.6610527709189,
-233.021822686564));
#203512=CARTESIAN_POINT('Ctrl Pts',(-29.8198922647338,-62.3656430824214,
-229.870183157334));
#203513=CARTESIAN_POINT('Ctrl Pts',(-33.2595071470079,-64.0744068681985,
-226.717552132221));
#203514=CARTESIAN_POINT('Ctrl Pts',(-36.6950887844903,-65.7896831337175,
-223.564108323038));
#203515=CARTESIAN_POINT('Ctrl Pts',(-40.1306704219727,-67.5049593992365,
-220.410664513854));
#203516=CARTESIAN_POINT('Ctrl Pts',(-43.5622034605361,-69.2267005231895,
-217.256365654455));
#203517=CARTESIAN_POINT('Ctrl Pts',(-46.9885985225256,-70.9587167786769,
-214.102032318221));
#203518=CARTESIAN_POINT('Ctrl Pts',(-26.2545891898305,-60.7273783411365,
-233.020937743651));
#203519=CARTESIAN_POINT('Ctrl Pts',(-29.704767491125,-62.4315344808983,
-229.869275405273));
#203520=CARTESIAN_POINT('Ctrl Pts',(-33.1518809533354,-64.139871089189,
-226.716620552092));
#203521=CARTESIAN_POINT('Ctrl Pts',(-36.5949698446713,-65.8547248151706,
-223.563151715778));
#203522=CARTESIAN_POINT('Ctrl Pts',(-40.038058736007,-67.5695785411523,
-220.409682879464));
#203523=CARTESIAN_POINT('Ctrl Pts',(-43.4771077064633,-69.2909019608329,
-217.255357871467));
#203524=CARTESIAN_POINT('Ctrl Pts',(-46.911032093483,-71.0224993808136,
-214.10099631368));
#203525=CARTESIAN_POINT('',(-42.5905577899916,-59.5881438265759,-225.000659040692));
#203526=CARTESIAN_POINT('Ctrl Pts',(-48.0699773895611,-67.6025469094357,
-215.850046926336));
#203527=CARTESIAN_POINT('Ctrl Pts',(-47.7935023640231,-67.6024435896897,
-216.017223632964));
#203528=CARTESIAN_POINT('Ctrl Pts',(-47.5226056067636,-67.5828243379733,
-216.193667418601));
#203529=CARTESIAN_POINT('Ctrl Pts',(-46.9774368515139,-67.5066353739982,
-216.5734123135));
#203530=CARTESIAN_POINT('Ctrl Pts',(-46.7040353167265,-67.4475753903814,
-216.777867265658));
#203531=CARTESIAN_POINT('Ctrl Pts',(-45.9194030179567,-67.2207720759118,
-217.40470002861));
#203532=CARTESIAN_POINT('Ctrl Pts',(-45.4358292265386,-67.0029495672062,
-217.845716150046));
#203533=CARTESIAN_POINT('Ctrl Pts',(-44.3014622491111,-66.3069334262107,
-219.018073172344));
#203534=CARTESIAN_POINT('Ctrl Pts',(-43.7134054388051,-65.7467619648911,
-219.774958898609));
#203535=CARTESIAN_POINT('Ctrl Pts',(-42.6715909373129,-64.2628736064779,
-221.493288736712));
#203536=CARTESIAN_POINT('Ctrl Pts',(-42.3167080561632,-63.2947927751177,
-222.434026477107));
#203537=CARTESIAN_POINT('Ctrl Pts',(-42.1771404629454,-61.8708033766699,
-223.580484791686));
#203538=CARTESIAN_POINT('Ctrl Pts',(-42.180006878906,-61.4303388699728,
-223.906345139384));
#203539=CARTESIAN_POINT('Ctrl Pts',(-42.2949054529825,-60.5240489280129,
-224.504112439923));
#203540=CARTESIAN_POINT('Ctrl Pts',(-42.408777306242,-60.0550288947154,
-224.777157735648));
#203541=CARTESIAN_POINT('Ctrl Pts',(-42.5905622784972,-59.5881432109375,
-225.000654103808));
#203542=CARTESIAN_POINT('Ctrl Pts',(-53.9390346875573,-61.9113848028035,
-215.85005));
#203543=CARTESIAN_POINT('Ctrl Pts',(-53.9476622151261,-61.6293619830306,
-216.023587794996));
#203544=CARTESIAN_POINT('Ctrl Pts',(-53.9357969743604,-61.3527628870338,
-216.207117110883));
#203545=CARTESIAN_POINT('Ctrl Pts',(-53.8747173093831,-60.8022834426257,
-216.59757991481));
#203546=CARTESIAN_POINT('Ctrl Pts',(-53.8237963891831,-60.5287413941462,
-216.805449392086));
#203547=CARTESIAN_POINT('Ctrl Pts',(-53.6143973977264,-59.7162941773142,
-217.463133835212));
#203548=CARTESIAN_POINT('Ctrl Pts',(-53.3987000943071,-59.2066382206332,
-217.934268469262));
#203549=CARTESIAN_POINT('Ctrl Pts',(-52.7251467717684,-58.0641624039732,
-219.12859993374));
#203550=CARTESIAN_POINT('Ctrl Pts',(-52.1960061469933,-57.4802041226149,
-219.873917995722));
#203551=CARTESIAN_POINT('Ctrl Pts',(-50.7690642493973,-56.4143480280836,
-221.574539600558));
#203552=CARTESIAN_POINT('Ctrl Pts',(-49.8225109115708,-56.0319094103337,
-222.505508240576));
#203553=CARTESIAN_POINT('Ctrl Pts',(-48.3443436484928,-55.835956780535,
-223.691800920573));
#203554=CARTESIAN_POINT('Ctrl Pts',(-47.8286143703577,-55.8298643113913,
-224.064010045577));
#203555=CARTESIAN_POINT('Ctrl Pts',(-46.8826009388687,-55.9534328528004,
-224.650663983079));
#203556=CARTESIAN_POINT('Ctrl Pts',(-46.4559435829215,-56.0545281652879,
-224.882862691977));
#203557=CARTESIAN_POINT('Ctrl Pts',(-46.030027499011,-56.2113956008523,
-225.073027461904));
#203558=CARTESIAN_POINT('Ctrl Pts',(-41.9650124840222,-58.9506172433346,
-225.850033985948));
#203559=CARTESIAN_POINT('Ctrl Pts',(-42.1763950772714,-59.1660491934041,
-225.5629733364));
#203560=CARTESIAN_POINT('Ctrl Pts',(-42.3849068502055,-59.3785553348708,
-225.279850227117));
#203561=CARTESIAN_POINT('Ctrl Pts',(-42.590551250619,-59.5881391761779,
-225.000663880113));
#203562=CARTESIAN_POINT('Origin',(296.501483394397,-25.4138432731711,-232.85005));
#203563=CARTESIAN_POINT('',(-10.360380424878,38.165365484964,-232.850050038296));
#203564=CARTESIAN_POINT('',(-15.4720288026696,37.8533269327943,-232.85005));
#203565=CARTESIAN_POINT('Origin',(2.61456814389029E-14,-173.57701443073,
-232.85005));
#203566=CARTESIAN_POINT('Ctrl Pts',(-10.3603804210433,38.16536553404,-232.85005));
#203567=CARTESIAN_POINT('Ctrl Pts',(-11.2139414965945,38.2320615098657,
-232.85005));
#203568=CARTESIAN_POINT('Ctrl Pts',(-12.0722256690462,38.2392370527988,
-232.85005));
#203569=CARTESIAN_POINT('Ctrl Pts',(-13.7815229121495,38.1349615420106,
-232.85005));
#203570=CARTESIAN_POINT('Ctrl Pts',(-14.6332355233986,38.0230811620804,
-232.85005));
#203571=CARTESIAN_POINT('Ctrl Pts',(-15.4720288026693,37.853326932793,-232.85005));
#203572=CARTESIAN_POINT('Origin',(296.501483394397,-25.4138432731711,-232.85005));
#203573=CARTESIAN_POINT('Ctrl Pts',(-47.8524635552852,9.39108009191238,
-232.85005));
#203574=CARTESIAN_POINT('Ctrl Pts',(-47.8251207475469,9.27869452829718,
-232.85005));
#203575=CARTESIAN_POINT('Ctrl Pts',(-47.7988578503938,9.16605178669914,
-232.850050000002));
#203576=CARTESIAN_POINT('Ctrl Pts',(-47.7485452399956,8.9404131852861,-232.850050000002));
#203577=CARTESIAN_POINT('Ctrl Pts',(-47.7244950993554,8.82742853781365,
-232.85005));
#203578=CARTESIAN_POINT('Ctrl Pts',(-47.7015450634134,8.71421534318112,
-232.85005));
#203579=CARTESIAN_POINT('',(-23.1986392345853,37.1456077166894,-232.850148165968));
#203580=CARTESIAN_POINT('Origin',(2.61456814389029E-14,-173.57701443073,
-232.85005));
#203581=CARTESIAN_POINT('Ctrl Pts',(-23.1986880090039,37.1456674152139,
-232.85005));
#203582=CARTESIAN_POINT('Ctrl Pts',(-23.3194050754071,37.154620362199,-232.85005));
#203583=CARTESIAN_POINT('Ctrl Pts',(-23.4400518234764,37.164509338947,-232.85005));
#203584=CARTESIAN_POINT('Ctrl Pts',(-23.6811423763216,37.1861531096,-232.85005));
#203585=CARTESIAN_POINT('Ctrl Pts',(-23.8015842986948,37.1979071562942,
-232.85005));
#203586=CARTESIAN_POINT('Ctrl Pts',(-23.9219289938183,37.2105935013701,
-232.85005));
#203587=CARTESIAN_POINT('Origin',(296.501483394397,-25.4138432731711,-232.85005));
#203588=CARTESIAN_POINT('',(-47.8903177140771,0.753846963912779,-232.850053817009));
#203589=CARTESIAN_POINT('',(-47.9312868154534,-1.80167576439668,-232.850051862368));
#203590=CARTESIAN_POINT('Origin',(636.934816028482,-11.5034818258361,-232.85005));
#203591=CARTESIAN_POINT('Ctrl Pts',(-47.8903230579921,0.75384761155794,
-232.85005));
#203592=CARTESIAN_POINT('Ctrl Pts',(-47.9416808738277,0.330078821801721,
-232.85005));
#203593=CARTESIAN_POINT('Ctrl Pts',(-47.9708354565936,-0.095756747675781,
-232.850050000016));
#203594=CARTESIAN_POINT('Ctrl Pts',(-47.9845047846122,-0.949125474243279,
-232.850050000016));
#203595=CARTESIAN_POINT('Ctrl Pts',(-47.9690398565759,-1.37636912129171,
-232.85005));
#203596=CARTESIAN_POINT('Ctrl Pts',(-47.931289209931,-1.80167597693282,
-232.85005));
#203597=CARTESIAN_POINT('Origin',(296.501483394397,-25.4138432731711,-232.85005));
#203598=CARTESIAN_POINT('',(-47.9981322788631,-9.91532742253397,-232.850009339187));
#203599=CARTESIAN_POINT('',(-47.9977289503046,-13.2576712963443,-232.850013209406));
#203600=CARTESIAN_POINT('Origin',(636.934816028482,-11.5034818258361,-232.85005));
#203601=CARTESIAN_POINT('Ctrl Pts',(-47.9981596989451,-9.91572581758163,
-232.85005));
#203602=CARTESIAN_POINT('Ctrl Pts',(-48.0736753643642,-10.4692652745412,
-232.85005));
#203603=CARTESIAN_POINT('Ctrl Pts',(-48.111823774494,-11.0292275871121,
-232.85005));
#203604=CARTESIAN_POINT('Ctrl Pts',(-48.1115279552437,-12.1458824488847,
-232.85005));
#203605=CARTESIAN_POINT('Ctrl Pts',(-48.0732754984808,-12.7047197969431,
-232.85005));
#203606=CARTESIAN_POINT('Ctrl Pts',(-47.9977546165566,-13.2572998177748,
-232.85005));
#203607=CARTESIAN_POINT('Origin',(296.501483394397,-25.4138432731711,-232.85005));
#203608=CARTESIAN_POINT('',(-47.9291893708826,-21.3522304066337,-232.850051757442));
#203609=CARTESIAN_POINT('',(-47.8870567810509,-23.9416215055321,-232.850052596546));
#203610=CARTESIAN_POINT('Origin',(636.934816028482,-11.5034818258361,-232.85005));
#203611=CARTESIAN_POINT('Ctrl Pts',(-47.9291915823105,-21.3522302047528,
-232.85005));
#203612=CARTESIAN_POINT('Ctrl Pts',(-47.9685182384559,-21.783019276162,
-232.85005));
#203613=CARTESIAN_POINT('Ctrl Pts',(-47.9846715385196,-22.2158717780932,
-232.850050000023));
#203614=CARTESIAN_POINT('Ctrl Pts',(-47.9706154668234,-23.0806717086415,
-232.850050000023));
#203615=CARTESIAN_POINT('Ctrl Pts',(-47.9403670434338,-23.5122314437496,
-232.85005));
#203616=CARTESIAN_POINT('Ctrl Pts',(-47.8870605128751,-23.9416219688181,
-232.85005));
#203617=CARTESIAN_POINT('Origin',(296.501483394397,-25.4138432731711,-232.85005));
#203618=CARTESIAN_POINT('',(-10.1856061283707,-61.3499012171703,-232.85005));
#203619=CARTESIAN_POINT('',(-13.6391777675768,-61.2898273935359,-232.85005));
#203620=CARTESIAN_POINT('Ctrl Pts',(-10.1856061283708,-61.3499012171695,
-232.85005));
#203621=CARTESIAN_POINT('Ctrl Pts',(-10.7540331810879,-61.4387873155578,
-232.85005));
#203622=CARTESIAN_POINT('Ctrl Pts',(-11.3321672532956,-61.4795692677295,
-232.85005));
#203623=CARTESIAN_POINT('Ctrl Pts',(-12.4893568184743,-61.4603506900827,
-232.85005));
#203624=CARTESIAN_POINT('Ctrl Pts',(-13.0690230896359,-61.4003891839744,
-232.85005));
#203625=CARTESIAN_POINT('Ctrl Pts',(-13.6391777675768,-61.289827393536,
-232.85005));
#203626=CARTESIAN_POINT('Origin',(-7.14692237356698E-14,623.509175991979,
-232.85005));
#203627=CARTESIAN_POINT('Origin',(-0.128459562639233,-12.6359082483571,
-225.85005));
#203628=CARTESIAN_POINT('',(-46.7347424436738,30.7127197009669,-225.85005));
#203629=CARTESIAN_POINT('Origin',(-48.892180948596,36.2913696007177,-225.85005));
#203630=CARTESIAN_POINT('',(-53.8170476734233,37.8187794096849,-225.85005));
#203631=CARTESIAN_POINT('Origin',(636.934816028482,-11.5034818258361,-234.75005));
#203632=CARTESIAN_POINT('',(-47.9849429580539,-16.0452820755244,-232.250052142049));
#203633=CARTESIAN_POINT('Ctrl Pts',(-47.9849415007718,-16.0452825742631,
-232.250056396759));
#203634=CARTESIAN_POINT('Ctrl Pts',(-47.9880651131553,-15.5742306821108,
-232.306343147704));
#203635=CARTESIAN_POINT('Ctrl Pts',(-47.9906783186251,-15.1065446149179,
-232.390988202572));
#203636=CARTESIAN_POINT('Ctrl Pts',(-47.9942849350928,-14.3203139878749,
-232.579502138114));
#203637=CARTESIAN_POINT('Ctrl Pts',(-47.9949617724383,-14.1407707769958,
-232.636201143858));
#203638=CARTESIAN_POINT('Ctrl Pts',(-47.9965339240235,-13.6931733637722,
-232.756352689979));
#203639=CARTESIAN_POINT('Ctrl Pts',(-47.9971930434488,-13.4765686846904,
-232.80695441365));
#203640=CARTESIAN_POINT('Ctrl Pts',(-47.9977536577298,-13.257674236261,
-232.849976418813));
#203641=CARTESIAN_POINT('',(-47.9866836135147,-7.23226647128753,-232.25005191098));
#203642=CARTESIAN_POINT('Origin',(636.934816028482,-11.5034818258361,-232.25005));
#203643=CARTESIAN_POINT('Ctrl Pts',(-47.9866823371376,-7.23226600773662,
-232.250055704934));
#203644=CARTESIAN_POINT('Ctrl Pts',(-47.9895098141046,-7.68567315063931,
-232.306404893473));
#203645=CARTESIAN_POINT('Ctrl Pts',(-47.9918619737062,-8.13535273752287,
-232.390421945345));
#203646=CARTESIAN_POINT('Ctrl Pts',(-47.9951073324733,-8.89528528197956,
-232.579944924587));
#203647=CARTESIAN_POINT('Ctrl Pts',(-47.9956980243075,-9.06520173831264,
-232.636698278605));
#203648=CARTESIAN_POINT('Ctrl Pts',(-47.9971000734922,-9.4997170477986,
-232.757828881318));
#203649=CARTESIAN_POINT('Ctrl Pts',(-47.9976741114781,-9.70630394983337,
-232.80764645552));
#203650=CARTESIAN_POINT('Ctrl Pts',(-47.9981587676889,-9.91532413904543,
-232.849968678375));
#203651=CARTESIAN_POINT('Origin',(636.934816028482,-11.5034818258361,-234.75005));
#203652=CARTESIAN_POINT('',(-47.8275275119673,3.86645886896237,-232.25005));
#203653=CARTESIAN_POINT('',(-47.9644141218642,-4.51936149851664,-232.250085462751));
#203654=CARTESIAN_POINT('Origin',(636.934816028482,-11.5034818258361,-232.25005));
#203655=CARTESIAN_POINT('Ctrl Pts',(-47.8275275119675,3.86645886896245,
-232.250050000001));
#203656=CARTESIAN_POINT('Ctrl Pts',(-47.8393033810287,3.34181977921662,
-232.308606692494));
#203657=CARTESIAN_POINT('Ctrl Pts',(-47.8504216708136,2.81940125771536,
-232.399682736105));
#203658=CARTESIAN_POINT('Ctrl Pts',(-47.8640428170584,2.14390431815265,
-232.55505864472));
#203659=CARTESIAN_POINT('Ctrl Pts',(-47.8678682595301,1.94983002712662,
-232.604470061216));
#203660=CARTESIAN_POINT('Ctrl Pts',(-47.876573696563,1.50418121394012,-232.71811471315));
#203661=CARTESIAN_POINT('Ctrl Pts',(-47.8835694576846,1.13072531538302,
-232.794863478221));
#203662=CARTESIAN_POINT('Ctrl Pts',(-47.8903149889077,0.753848021453944,
-232.850061370667));
#203663=CARTESIAN_POINT('Ctrl Pts',(-47.9312856139398,-1.8016763710691,
-232.850055542859));
#203664=CARTESIAN_POINT('Ctrl Pts',(-47.9394982187954,-2.38141739948144,
-232.757175193341));
#203665=CARTESIAN_POINT('Ctrl Pts',(-47.9438448367589,-2.72209125824031,
-232.634139478145));
#203666=CARTESIAN_POINT('Ctrl Pts',(-47.954612172792,-3.60581024584066,
-232.397143115374));
#203667=CARTESIAN_POINT('Ctrl Pts',(-47.9597127879937,-4.06055719066972,
-232.308472253544));
#203668=CARTESIAN_POINT('Ctrl Pts',(-47.9643913372016,-4.51935998922945,
-232.250120925502));
#203669=CARTESIAN_POINT('Origin',(636.934816028482,-11.5034818258361,-234.75005));
#203670=CARTESIAN_POINT('',(-47.7599172087244,-29.6370001055566,-232.25005));
#203671=CARTESIAN_POINT('Origin',(636.934816028482,-11.5034818258361,-232.25005));
#203672=CARTESIAN_POINT('Ctrl Pts',(-47.7599172087244,-29.6370001055567,
-232.25005));
#203673=CARTESIAN_POINT('Ctrl Pts',(-47.7492894555136,-30.0382882911887,
-232.296444128103));
#203674=CARTESIAN_POINT('Ctrl Pts',(-47.7383552845378,-30.4376621737927,
-232.368907951216));
#203675=CARTESIAN_POINT('Ctrl Pts',(-47.7170269872741,-31.1933172306936,
-232.569380385358));
#203676=CARTESIAN_POINT('Ctrl Pts',(-47.7066212951508,-31.5515003035446,
-232.693743240766));
#203677=CARTESIAN_POINT('Ctrl Pts',(-47.6963708717086,-31.8956404071764,
-232.849812660495));
#203678=CARTESIAN_POINT('Origin',(636.934816028482,-11.5034818258361,-234.75005));
#203679=CARTESIAN_POINT('',(-47.9620917743623,-18.7116135613516,-232.250083778634));
#203680=CARTESIAN_POINT('',(-47.8203127443142,-27.1915604710334,-232.250049983782));
#203681=CARTESIAN_POINT('Origin',(636.934816028482,-11.5034818258361,-232.25005));
#203682=CARTESIAN_POINT('Ctrl Pts',(-47.9620703904922,-18.7116148410405,
-232.250117557268));
#203683=CARTESIAN_POINT('Ctrl Pts',(-47.9573554138762,-19.1596188938302,
-232.306669892292));
#203684=CARTESIAN_POINT('Ctrl Pts',(-47.952238347251,-19.6037872905696,
-232.393382749887));
#203685=CARTESIAN_POINT('Ctrl Pts',(-47.9411866433023,-20.4904993022867,
-232.635960657362));
#203686=CARTESIAN_POINT('Ctrl Pts',(-47.9372122530391,-20.794255996158,
-232.756243969881));
#203687=CARTESIAN_POINT('Ctrl Pts',(-47.9291882608127,-21.3522298073388,
-232.850055227));
#203688=CARTESIAN_POINT('Ctrl Pts',(-47.8870548777005,-23.9416222224618,
-232.850057734118));
#203689=CARTESIAN_POINT('Ctrl Pts',(-47.8808419217877,-24.283696516233,
-232.800020744851));
#203690=CARTESIAN_POINT('Ctrl Pts',(-47.8744102330401,-24.6236650946472,
-232.733213391971));
#203691=CARTESIAN_POINT('Ctrl Pts',(-47.8666304747006,-25.019568091157,
-232.639069109828));
#203692=CARTESIAN_POINT('Ctrl Pts',(-47.8654339475312,-25.0799470331636,
-232.62410827376));
#203693=CARTESIAN_POINT('Ctrl Pts',(-47.8619240948923,-25.2566749049581,
-232.580479584111));
#203694=CARTESIAN_POINT('Ctrl Pts',(-47.8588236469902,-25.4102068713,-232.54485449108));
#203695=CARTESIAN_POINT('Ctrl Pts',(-47.8446425337259,-26.1008593428905,
-232.395217345888));
#203696=CARTESIAN_POINT('Ctrl Pts',(-47.8328230396433,-26.6455101093022,
-232.305849122883));
#203697=CARTESIAN_POINT('Ctrl Pts',(-47.8203127558795,-27.1915604680009,
-232.250049951514));
#203698=CARTESIAN_POINT('Origin',(-7.14692237356698E-14,623.509175991979,
-234.75005));
#203699=CARTESIAN_POINT('Ctrl Pts',(-13.6391777675768,-61.2898273935359,
-232.85005));
#203700=CARTESIAN_POINT('Ctrl Pts',(-13.7679778538919,-61.2872620754425,
-232.820255967378));
#203701=CARTESIAN_POINT('Ctrl Pts',(-13.8962943913745,-61.2846700045451,
-232.78803439649));
#203702=CARTESIAN_POINT('Ctrl Pts',(-14.0579979559295,-61.2813584495498,
-232.744562636193));
#203703=CARTESIAN_POINT('Ctrl Pts',(-14.0841407462716,-61.2808208278262,
-232.737348171434));
#203704=CARTESIAN_POINT('Ctrl Pts',(-14.1136793535434,-61.280212286192,
-232.729268531082));
#203705=CARTESIAN_POINT('Ctrl Pts',(-14.1196218846364,-61.2800897833729,
-232.727647118086));
#203706=CARTESIAN_POINT('Ctrl Pts',(-14.1382345381682,-61.2797058487589,
-232.722581330731));
#203707=CARTESIAN_POINT('Ctrl Pts',(-14.1509054399916,-61.2794441266336,
-232.719151061211));
#203708=CARTESIAN_POINT('Ctrl Pts',(-14.3680771081964,-61.2749523320009,
-232.660673210664));
#203709=CARTESIAN_POINT('Ctrl Pts',(-14.5738916269567,-61.2706036848072,
-232.610036215289));
#203710=CARTESIAN_POINT('Ctrl Pts',(-15.5130869583053,-61.2503314811182,
-232.401689231682));
#203711=CARTESIAN_POINT('Ctrl Pts',(-16.2652400898949,-61.2328950900326,
-232.297341076771));
#203712=CARTESIAN_POINT('Ctrl Pts',(-17.557415570875,-61.2007887070211,
-232.254652621942));
#203713=CARTESIAN_POINT('Ctrl Pts',(-18.1075672345134,-61.1864563064708,
-232.27870892851));
#203714=CARTESIAN_POINT('Ctrl Pts',(-18.9473592849301,-61.1635855249242,
-232.402122405382));
#203715=CARTESIAN_POINT('Ctrl Pts',(-19.2463100795496,-61.1552436964942,
-232.463744244621));
#203716=CARTESIAN_POINT('Ctrl Pts',(-19.8287142284054,-61.1386226678951,
-232.626250777318));
#203717=CARTESIAN_POINT('Ctrl Pts',(-20.1129420846328,-61.1303255101954,
-232.726867615116));
#203718=CARTESIAN_POINT('Ctrl Pts',(-20.3871350980679,-61.1221605172865,
-232.850025366413));
#203719=CARTESIAN_POINT('',(-8.46314246790651,-61.3733482641917,-232.250044026154));
#203720=CARTESIAN_POINT('Ctrl Pts',(-10.1856061283711,-61.3499012171704,
-232.850049999999));
#203721=CARTESIAN_POINT('Ctrl Pts',(-9.82032687406902,-61.3553338539493,
-232.743373739408));
#203722=CARTESIAN_POINT('Ctrl Pts',(-9.6075193118261,-61.3583117635047,
-232.640308531627));
#203723=CARTESIAN_POINT('Ctrl Pts',(-9.04581817676723,-61.3659623843461,
-232.420098274593));
#203724=CARTESIAN_POINT('Ctrl Pts',(-8.75670787203841,-61.3697245641403,
-232.326864869098));
#203725=CARTESIAN_POINT('Ctrl Pts',(-8.46321410432377,-61.3733513183579,
-232.25005));
#203726=CARTESIAN_POINT('Origin',(-7.14692237356698E-14,623.509175991979,
-232.25005));
#203727=CARTESIAN_POINT('Origin',(-49.9798730220992,-67.1190133783941,-228.35005));
#203728=CARTESIAN_POINT('',(-42.5792116384512,-59.576583500476,-225.85005));
#203729=CARTESIAN_POINT('Origin',(-48.892180948596,36.2913696007177,-218.306418983907));
#203730=CARTESIAN_POINT('',(-46.7347424436738,30.7127197009669,-225.85005));
#203731=CARTESIAN_POINT('Origin',(-53.8170476734233,37.8187794096849,-228.35005));
#203732=CARTESIAN_POINT('Ctrl Pts',(-47.6396641907623,9.56951109638858,
-233.375524009166));
#203733=CARTESIAN_POINT('Ctrl Pts',(-49.8405355389308,11.6556158167396,
-230.003433166063));
#203734=CARTESIAN_POINT('Ctrl Pts',(-52.0418116007037,13.7520462993107,
-226.638133451275));
#203735=CARTESIAN_POINT('Ctrl Pts',(-54.2429855256817,15.8525357612388,
-223.275331821509));
#203736=CARTESIAN_POINT('Ctrl Pts',(-56.4441594506596,17.9530252231669,
-219.912530191744));
#203737=CARTESIAN_POINT('Ctrl Pts',(-58.6452885751193,20.0579121947712,
-216.552478218177));
#203738=CARTESIAN_POINT('Ctrl Pts',(-60.846321628963,22.164968605821,-213.193734192871));
#203739=CARTESIAN_POINT('Ctrl Pts',(-47.1914720210979,7.6140088721643,-233.185323795226));
#203740=CARTESIAN_POINT('Ctrl Pts',(-49.3672203068766,9.52128975296003,
-229.826228944008));
#203741=CARTESIAN_POINT('Ctrl Pts',(-51.5415920964213,11.4345056878504,
-226.469384191172));
#203742=CARTESIAN_POINT('Ctrl Pts',(-53.7154316537813,13.3500108047595,
-223.113404278841));
#203743=CARTESIAN_POINT('Ctrl Pts',(-55.8892712111413,15.2655159216685,
-219.757424366509));
#203744=CARTESIAN_POINT('Ctrl Pts',(-58.0625313135173,17.1835155618891,
-216.402388112408));
#203745=CARTESIAN_POINT('Ctrl Pts',(-60.2355063327765,19.10274141504,-213.047815750158));
#203746=CARTESIAN_POINT('Ctrl Pts',(-47.0946540619524,5.59941768418452,
-233.074415744431));
#203747=CARTESIAN_POINT('Ctrl Pts',(-49.2606104729176,7.3239784675775,-229.720965119143));
#203748=CARTESIAN_POINT('Ctrl Pts',(-51.4258904074922,9.05055026326663,
-226.367922363131));
#203749=CARTESIAN_POINT('Ctrl Pts',(-53.5909200701262,10.7779010963922,
-223.015045172743));
#203750=CARTESIAN_POINT('Ctrl Pts',(-55.7559497327601,12.5052519295177,
-219.662167982355));
#203751=CARTESIAN_POINT('Ctrl Pts',(-57.9207041285279,14.2334502664104,
-216.309468982699));
#203752=CARTESIAN_POINT('Ctrl Pts',(-60.0853267482839,15.9620648827344,
-212.956859706535));
#203753=CARTESIAN_POINT('Ctrl Pts',(-47.3220782931503,3.64213739520988,
-233.009326653747));
#203754=CARTESIAN_POINT('Ctrl Pts',(-49.5001561272747,5.17923014873171,
-229.65822098902));
#203755=CARTESIAN_POINT('Ctrl Pts',(-51.6785800990322,6.71512263630363,
-226.306791304678));
#203756=CARTESIAN_POINT('Ctrl Pts',(-53.8571359353927,8.25054831515734,
-222.955233810924));
#203757=CARTESIAN_POINT('Ctrl Pts',(-56.0356917717532,9.78597399401105,
-219.603676317171));
#203758=CARTESIAN_POINT('Ctrl Pts',(-58.2143916305598,11.3208922926972,
-216.251980359006));
#203759=CARTESIAN_POINT('Ctrl Pts',(-60.3931615898891,12.8555608031383,
-212.900215711346));
#203760=CARTESIAN_POINT('Ctrl Pts',(-47.3789343509497,3.15281732296621,
-232.993054381077));
#203761=CARTESIAN_POINT('Ctrl Pts',(-49.5600425408639,4.64304306902027,
-229.642534956489));
#203762=CARTESIAN_POINT('Ctrl Pts',(-51.7417525219173,6.13126572956288,
-226.291508540064));
#203763=CARTESIAN_POINT('Ctrl Pts',(-53.9236899017093,7.61871011984863,
-222.94028097047));
#203764=CARTESIAN_POINT('Ctrl Pts',(-56.1056272815015,9.10615451013438,
-219.589053400875));
#203765=CARTESIAN_POINT('Ctrl Pts',(-58.2878135060677,10.5927527992689,
-216.237608203082));
#203766=CARTESIAN_POINT('Ctrl Pts',(-60.4701203002903,12.0789347832393,
-212.886054712549));
#203767=CARTESIAN_POINT('Ctrl Pts',(-47.4559590230269,2.66718238323085,
-232.979818118251));
#203768=CARTESIAN_POINT('Ctrl Pts',(-49.6414718351808,4.11022346681344,
-229.629652968461));
#203769=CARTESIAN_POINT('Ctrl Pts',(-51.8278741302197,5.55050627061373,
-226.278876468708));
#203770=CARTESIAN_POINT('Ctrl Pts',(-54.0146079802632,6.98971963348256,
-222.927854342566));
#203771=CARTESIAN_POINT('Ctrl Pts',(-56.2013418303068,8.4289329963514,-219.576832216423));
#203772=CARTESIAN_POINT('Ctrl Pts',(-58.3884396888769,9.86698316181859,
-216.225545116483));
#203773=CARTESIAN_POINT('Ctrl Pts',(-60.5757125562048,11.3044617097837,
-212.874125306097));
#203774=CARTESIAN_POINT('Ctrl Pts',(-47.5526556810106,2.18649568630384,
-232.969248737689));
#203775=CARTESIAN_POINT('Ctrl Pts',(-49.7440252884103,3.58214069800097,
-229.619256142275));
#203776=CARTESIAN_POINT('Ctrl Pts',(-51.9366046755093,4.97428639343047,
-226.268610062602));
#203777=CARTESIAN_POINT('Ctrl Pts',(-54.129628172195,6.36508038888444,-222.917696367826));
#203778=CARTESIAN_POINT('Ctrl Pts',(-56.3226516688807,7.7558743843384,-219.56678267305));
#203779=CARTESIAN_POINT('Ctrl Pts',(-58.5161645712576,9.14519694298261,
-216.215581556974));
#203780=CARTESIAN_POINT('Ctrl Pts',(-60.7099107655409,10.5337979996055,
-212.864235131559));
#203781=CARTESIAN_POINT('Ctrl Pts',(-47.5768298455065,2.06632401207208,
-232.96660639255));
#203782=CARTESIAN_POINT('Ctrl Pts',(-49.7696636517176,3.45012000579785,
-229.616656935729));
#203783=CARTESIAN_POINT('Ctrl Pts',(-51.9637873118318,4.83023142413465,
-226.266043461076));
#203784=CARTESIAN_POINT('Ctrl Pts',(-54.158383220178,6.2089205777349,-222.915156874141));
#203785=CARTESIAN_POINT('Ctrl Pts',(-56.3529791285242,7.58760973133515,
-219.564270287207));
#203786=CARTESIAN_POINT('Ctrl Pts',(-58.5480957918528,8.96475038827362,
-216.213090667097));
#203787=CARTESIAN_POINT('Ctrl Pts',(-60.7434603178749,10.3411320720609,
-212.861762587924));
#203788=CARTESIAN_POINT('Ctrl Pts',(-47.602234241193,1.94646167456563,-232.964131776795));
#203789=CARTESIAN_POINT('Ctrl Pts',(-49.7966228589716,3.3183954301123,-229.614213917398));
#203790=CARTESIAN_POINT('Ctrl Pts',(-51.9923835106293,4.68646023480269,
-226.263625471024));
#203791=CARTESIAN_POINT('Ctrl Pts',(-54.1886450914894,6.05303276847634,
-222.912759842952));
#203792=CARTESIAN_POINT('Ctrl Pts',(-56.3849066723495,7.41960530214998,
-219.561894214879));
#203793=CARTESIAN_POINT('Ctrl Pts',(-58.5817210184137,8.78455283392743,
-216.210731524094));
#203794=CARTESIAN_POINT('Ctrl Pts',(-60.7787980463854,10.1487042615692,
-212.859417974186));
#203795=CARTESIAN_POINT('Ctrl Pts',(-47.628862493758,1.82692857762527,-232.96182118511));
#203796=CARTESIAN_POINT('Ctrl Pts',(-49.8248974717912,3.18698851762863,
-229.611923806209));
#203797=CARTESIAN_POINT('Ctrl Pts',(-52.0223889083793,4.54299549104381,
-226.26135312848));
#203798=CARTESIAN_POINT('Ctrl Pts',(-54.2204105268588,5.89744057105422,
-222.91050257153));
#203799=CARTESIAN_POINT('Ctrl Pts',(-56.4184321453384,7.25188565106463,
-219.559652014579));
#203800=CARTESIAN_POINT('Ctrl Pts',(-58.6170392389817,8.60462958153552,
-216.208501890991));
#203801=CARTESIAN_POINT('Ctrl Pts',(-60.8159240956269,9.95654052871553,
-212.857199226772));
#203802=CARTESIAN_POINT('Ctrl Pts',(-47.6321910253286,1.81198694050772,
-232.961532361149));
#203803=CARTESIAN_POINT('Ctrl Pts',(-49.8284317983937,3.17056265356817,
-229.61163754231));
#203804=CARTESIAN_POINT('Ctrl Pts',(-52.026139583098,4.52506239807395,-226.261069085663));
#203805=CARTESIAN_POINT('Ctrl Pts',(-54.22438120628,5.87799154637645,-222.910220412602));
#203806=CARTESIAN_POINT('Ctrl Pts',(-56.422622829462,7.23092069467897,-219.559371739542));
#203807=CARTESIAN_POINT('Ctrl Pts',(-58.6214540165528,8.58213917498653,
-216.208223186853));
#203808=CARTESIAN_POINT('Ctrl Pts',(-60.8205648517821,9.93252006210882,
-212.856921883345));
#203809=CARTESIAN_POINT('Ctrl Pts',(-47.6355386803079,1.79705044787909,
-232.961246101092));
#203810=CARTESIAN_POINT('Ctrl Pts',(-49.8319866787204,3.15414175308971,
-229.611353668433));
#203811=CARTESIAN_POINT('Ctrl Pts',(-52.0299122769924,4.5071340934001,-226.260787319329));
#203812=CARTESIAN_POINT('Ctrl Pts',(-54.2283753792766,5.85854714070898,
-222.90994043808));
#203813=CARTESIAN_POINT('Ctrl Pts',(-56.4268384815609,7.20996018801785,
-219.55909355683));
#203814=CARTESIAN_POINT('Ctrl Pts',(-58.6258952474512,8.55965305446516,
-216.207946506826));
#203815=CARTESIAN_POINT('Ctrl Pts',(-60.825233550716,9.90850372176869,-212.856646507051));
#203816=CARTESIAN_POINT('Ctrl Pts',(-47.6389054467951,1.78211913870348,
-232.960962398579));
#203817=CARTESIAN_POINT('Ctrl Pts',(-49.8355621025854,3.13772585835723,
-229.611072178893));
#203818=CARTESIAN_POINT('Ctrl Pts',(-52.033706981916,4.48921062136337,-226.260507824327));
#203819=CARTESIAN_POINT('Ctrl Pts',(-54.2323930398121,5.83910740022999,
-222.909662643248));
#203820=CARTESIAN_POINT('Ctrl Pts',(-56.4310790977081,7.18900417909662,
-219.558817462169));
#203821=CARTESIAN_POINT('Ctrl Pts',(-58.6303629299522,8.5371712694402,-216.207671846982));
#203822=CARTESIAN_POINT('Ctrl Pts',(-60.8299301929379,9.88449155844584,
-212.856373094261));
#203823=CARTESIAN_POINT('Ctrl Pts',(-47.6422722132824,1.76718782952786,
-232.960678696067));
#203824=CARTESIAN_POINT('Ctrl Pts',(-49.8391375264504,3.12130996362475,
-229.610790689353));
#203825=CARTESIAN_POINT('Ctrl Pts',(-52.0375016868396,4.47128714932663,
-226.260228329323));
#203826=CARTESIAN_POINT('Ctrl Pts',(-54.2364107003475,5.81966765975101,
-222.909384848415));
#203827=CARTESIAN_POINT('Ctrl Pts',(-56.4353197138554,7.16804817017539,
-219.558541367508));
#203828=CARTESIAN_POINT('Ctrl Pts',(-58.6348306124533,8.51468948441525,
-216.207397187139));
#203829=CARTESIAN_POINT('Ctrl Pts',(-60.8346268351599,9.86047939512299,
-212.856099681471));
#203830=CARTESIAN_POINT('Ctrl Pts',(-47.6439085847953,1.75733843295859,
-232.961288761302));
#203831=CARTESIAN_POINT('Ctrl Pts',(-49.8410717940384,3.10978994722575,
-229.611386840422));
#203832=CARTESIAN_POINT('Ctrl Pts',(-52.0397142106509,4.45813110010028,
-226.26081354148));
#203833=CARTESIAN_POINT('Ctrl Pts',(-54.2388940831247,5.80489015915614,
-222.909960879112));
#203834=CARTESIAN_POINT('Ctrl Pts',(-56.4380739555984,7.151649218212,-219.559108216744));
#203835=CARTESIAN_POINT('Ctrl Pts',(-58.6378476177344,8.49668463701677,
-216.207956614142));
#203836=CARTESIAN_POINT('Ctrl Pts',(-60.8379027023408,9.84087662291507,
-212.856652729236));
#203837=CARTESIAN_POINT('Ctrl Pts',(-47.6460194974834,1.74602297076459,
-232.961641432517));
#203838=CARTESIAN_POINT('Ctrl Pts',(-49.8434528457034,3.09685564489722,
-229.611730184141));
#203839=CARTESIAN_POINT('Ctrl Pts',(-52.042354516691,4.44359608350473,-226.26114964818));
#203840=CARTESIAN_POINT('Ctrl Pts',(-54.2417894607756,5.78876232686925,
-222.91029092321));
#203841=CARTESIAN_POINT('Ctrl Pts',(-56.4412244048602,7.13392857023377,
-219.559432198239));
#203842=CARTESIAN_POINT('Ctrl Pts',(-58.6412485837932,8.47737953915866,
-216.208275719059));
#203843=CARTESIAN_POINT('Ctrl Pts',(-60.8415519676109,9.81999143035988,
-212.856967648949));
#203844=CARTESIAN_POINT('Ctrl Pts',(-47.6502413228594,1.72339204637661,
-232.962346774948));
#203845=CARTESIAN_POINT('Ctrl Pts',(-49.8482149490333,3.07098704024018,
-229.612416871579));
#203846=CARTESIAN_POINT('Ctrl Pts',(-52.0476351287711,4.41452605031363,
-226.261821861581));
#203847=CARTESIAN_POINT('Ctrl Pts',(-54.2475802160774,5.75650666229548,
-222.910951011405));
#203848=CARTESIAN_POINT('Ctrl Pts',(-56.4475253033837,7.09848727427732,
-219.560080161228));
#203849=CARTESIAN_POINT('Ctrl Pts',(-58.6480505159108,8.43876934344246,
-216.208913928891));
#203850=CARTESIAN_POINT('Ctrl Pts',(-60.8488504981511,9.77822104524949,
-212.857597488374));
#203851=CARTESIAN_POINT('Ctrl Pts',(-47.6543975111204,1.70075790412697,
-232.963053249537));
#203852=CARTESIAN_POINT('Ctrl Pts',(-49.8529058064771,3.04510985941153,
-229.613104472738));
#203853=CARTESIAN_POINT('Ctrl Pts',(-52.0528389954907,4.38544246561079,
-226.262494888344));
#203854=CARTESIAN_POINT('Ctrl Pts',(-54.2532887985736,5.72423254074652,
-222.911611841699));
#203855=CARTESIAN_POINT('Ctrl Pts',(-56.4537386016565,7.06302261588225,
-219.560728795054));
#203856=CARTESIAN_POINT('Ctrl Pts',(-58.6547594906971,8.4001309754133,-216.209552773761));
#203857=CARTESIAN_POINT('Ctrl Pts',(-60.8560507563961,9.73641770115673,
-212.858227938596));
#203858=CARTESIAN_POINT('Ctrl Pts',(-47.6584881964675,1.67812063274807,
-232.963760828248));
#203859=CARTESIAN_POINT('Ctrl Pts',(-49.8575254560703,3.01922438781437,
-229.613792971254));
#203860=CARTESIAN_POINT('Ctrl Pts',(-52.0579660735326,4.35634578681776,
-226.263168720394));
#203861=CARTESIAN_POINT('Ctrl Pts',(-54.2589150870478,5.6919405831028,-222.912273412552));
#203862=CARTESIAN_POINT('Ctrl Pts',(-56.459864100563,7.02753537938784,-219.56137810471));
#203863=CARTESIAN_POINT('Ctrl Pts',(-58.6613752354701,8.36146537341484,
-216.210192263444));
#203864=CARTESIAN_POINT('Ctrl Pts',(-60.8631523975563,9.69458248633691,
-212.858859013292));
#203865=CARTESIAN_POINT('Ctrl Pts',(-47.6666695671617,1.63284608999026,
-232.96517598567));
#203866=CARTESIAN_POINT('Ctrl Pts',(-49.8667647552568,2.96745344462007,
-229.615169968288));
#203867=CARTESIAN_POINT('Ctrl Pts',(-52.0682202296165,4.29815242923168,
-226.264516384494));
#203868=CARTESIAN_POINT('Ctrl Pts',(-54.2701676639963,5.62735666781534,
-222.913596554258));
#203869=CARTESIAN_POINT('Ctrl Pts',(-56.4721150983761,6.956560906399,-219.562676724022));
#203870=CARTESIAN_POINT('Ctrl Pts',(-58.6746067250159,8.28413416941793,
-216.211471242811));
#203871=CARTESIAN_POINT('Ctrl Pts',(-60.8773556798765,9.61091205669726,
-212.860121162684));
#203872=CARTESIAN_POINT('Ctrl Pts',(-47.6745889282634,1.58755903151136,
-232.966595558784));
#203873=CARTESIAN_POINT('Ctrl Pts',(-49.8757192238467,2.91564933843912,
-229.616550553645));
#203874=CARTESIAN_POINT('Ctrl Pts',(-52.0781672310342,4.23990669526066,
-226.265867268572));
#203875=CARTESIAN_POINT('Ctrl Pts',(-54.281091064319,5.56270140804211,-222.914922656992));
#203876=CARTESIAN_POINT('Ctrl Pts',(-56.4840148976038,6.88549612082355,
-219.563978045413));
#203877=CARTESIAN_POINT('Ctrl Pts',(-58.6874652929996,8.20669402936436,
-216.212752800202));
#203878=CARTESIAN_POINT('Ctrl Pts',(-60.891164492042,9.52711414398385,-212.861385808758));
#203879=CARTESIAN_POINT('Ctrl Pts',(-47.6822473288034,1.54226015711989,
-232.968019332623));
#203880=CARTESIAN_POINT('Ctrl Pts',(-49.8843891563535,2.86381435135825,
-229.6179346096));
#203881=CARTESIAN_POINT('Ctrl Pts',(-52.0878067306158,4.18161224455118,
-226.267221321995));
#203882=CARTESIAN_POINT('Ctrl Pts',(-54.2916843246343,5.49797977211644,
-222.916251722872));
#203883=CARTESIAN_POINT('Ctrl Pts',(-56.4955619186529,6.81434729968171,
-219.565282123748));
#203884=CARTESIAN_POINT('Ctrl Pts',(-58.6999487759841,8.12915246217079,
-216.214037028638));
#203885=CARTESIAN_POINT('Ctrl Pts',(-60.9045760974657,9.44319745618915,
-212.862653075561));
#203886=CARTESIAN_POINT('Ctrl Pts',(-47.7128809309633,1.36106465955398,
-232.973714427979));
#203887=CARTESIAN_POINT('Ctrl Pts',(-49.9190688863809,2.65647440303478,
-229.623470833417));
#203888=CARTESIAN_POINT('Ctrl Pts',(-52.1263647289421,3.94843444171322,
-226.272637535688));
#203889=CARTESIAN_POINT('Ctrl Pts',(-54.3340573658958,5.23909322841377,
-222.921567986388));
#203890=CARTESIAN_POINT('Ctrl Pts',(-56.5417500028495,6.52975201511432,
-219.570498437088));
#203891=CARTESIAN_POINT('Ctrl Pts',(-58.7498827079224,7.81898619339649,
-216.219173942379));
#203892=CARTESIAN_POINT('Ctrl Pts',(-60.9582225191604,9.10753070501037,
-212.867722142776));
#203893=CARTESIAN_POINT('Ctrl Pts',(-47.7393398420482,1.17968029636359,
-232.979476459983));
#203894=CARTESIAN_POINT('Ctrl Pts',(-49.9491962843832,2.44864037742646,
-229.629062225071));
#203895=CARTESIAN_POINT('Ctrl Pts',(-52.1600026985195,3.71447716168251,
-226.278104081914));
#203896=CARTESIAN_POINT('Ctrl Pts',(-54.3711479805289,4.97914463445542,
-222.926931273635));
#203897=CARTESIAN_POINT('Ctrl Pts',(-56.5822932625382,6.24381210722835,
-219.575758465357));
#203898=CARTESIAN_POINT('Ctrl Pts',(-58.7938147846409,7.50719703392768,
-216.224353199397));
#203899=CARTESIAN_POINT('Ctrl Pts',(-61.0055130419957,8.76996349473516,
-212.872832752187));
#203900=CARTESIAN_POINT('Ctrl Pts',(-47.7616858294571,0.998150138415235,
-232.985293804272));
#203901=CARTESIAN_POINT('Ctrl Pts',(-49.9747881970607,2.24045815861694,
-229.634704119062));
#203902=CARTESIAN_POINT('Ctrl Pts',(-52.1886983731474,3.47997469249725,
-226.283620725365));
#203903=CARTESIAN_POINT('Ctrl Pts',(-54.4028959591866,4.71845222593428,
-222.932344808848));
#203904=CARTESIAN_POINT('Ctrl Pts',(-56.6170935452258,5.95692975937132,
-219.581068892331));
#203905=CARTESIAN_POINT('Ctrl Pts',(-58.8316104681301,7.19426601066472,
-216.229583902017));
#203906=CARTESIAN_POINT('Ctrl Pts',(-61.046277219474,8.43105358570855,-212.877995957148));
#203907=CARTESIAN_POINT('Ctrl Pts',(-47.8510697790929,0.272029506621824,
-233.008563181426));
#203908=CARTESIAN_POINT('Ctrl Pts',(-50.0771558477705,1.40772928337885,
-229.657271695028));
#203909=CARTESIAN_POINT('Ctrl Pts',(-52.3034810716587,2.54196481575621,
-226.305687299172));
#203910=CARTESIAN_POINT('Ctrl Pts',(-54.5298878738176,3.67568259184972,
-222.953998949698));
#203911=CARTESIAN_POINT('Ctrl Pts',(-56.7562946759763,4.80940036794322,
-219.602310600225));
#203912=CARTESIAN_POINT('Ctrl Pts',(-58.9827932020866,5.94254191761289,
-216.250506712501));
#203913=CARTESIAN_POINT('Ctrl Pts',(-61.2093339293867,7.07541394960212,
-212.898648776991));
#203914=CARTESIAN_POINT('Ctrl Pts',(-47.8748620676848,-0.456315238952961,
-233.032739707064));
#203915=CARTESIAN_POINT('Ctrl Pts',(-50.106976448607,0.569429995731811,
-229.68067062904));
#203916=CARTESIAN_POINT('Ctrl Pts',(-52.3389983552511,1.59514136085191,
-226.328577629014));
#203917=CARTESIAN_POINT('Ctrl Pts',(-54.5709908267102,2.62083609058904,
-222.976477458797));
#203918=CARTESIAN_POINT('Ctrl Pts',(-56.8029832981692,3.64653082032617,
-219.624377288579));
#203919=CARTESIAN_POINT('Ctrl Pts',(-59.0349420500259,4.672208415501,-216.272268764454));
#203920=CARTESIAN_POINT('Ctrl Pts',(-61.2668859324121,5.69787672746903,
-212.920156700729));
#203921=CARTESIAN_POINT('Ctrl Pts',(-47.8343566648447,-1.18129562201859,
-233.057735449668));
#203922=CARTESIAN_POINT('Ctrl Pts',(-50.0649792011103,-0.264693413707682,
-229.704700485746));
#203923=CARTESIAN_POINT('Ctrl Pts',(-52.2954559925465,0.653414022650932,
-226.351982116141));
#203924=CARTESIAN_POINT('Ctrl Pts',(-54.525876562459,1.57206651464896,-222.999376095285));
#203925=CARTESIAN_POINT('Ctrl Pts',(-56.7562971323714,2.49071900664698,
-219.646770074429));
#203926=CARTESIAN_POINT('Ctrl Pts',(-58.9866565003629,3.40997442959623,
-216.294288989989));
#203927=CARTESIAN_POINT('Ctrl Pts',(-61.2169859241647,4.32951560431301,
-212.941866493395));
#203928=CARTESIAN_POINT('Ctrl Pts',(-47.8141039634246,-1.54378581355141,
-233.070233320969));
#203929=CARTESIAN_POINT('Ctrl Pts',(-50.043980577362,-0.681755118427429,
-229.716715414099));
#203930=CARTESIAN_POINT('Ctrl Pts',(-52.2736848111942,0.182550353550442,
-226.363684359704));
#203931=CARTESIAN_POINT('Ctrl Pts',(-54.5033194303334,1.04768172667892,
-223.010825413529));
#203932=CARTESIAN_POINT('Ctrl Pts',(-56.7329540494726,1.91281309980739,
-219.657966467354));
#203933=CARTESIAN_POINT('Ctrl Pts',(-58.9625137255313,2.77885743664385,
-216.305299102755));
#203934=CARTESIAN_POINT('Ctrl Pts',(-61.192035920041,3.64533504273501,-212.952721389729));
#203935=CARTESIAN_POINT('Ctrl Pts',(-47.777753685031,-1.90560042502214,
-233.082905053984));
#203936=CARTESIAN_POINT('Ctrl Pts',(-50.0050281763432,-1.0977804796852,
-229.72888694318));
#203937=CARTESIAN_POINT('Ctrl Pts',(-52.2321769379993,-0.286940211741083,
-226.375533132468));
#203938=CARTESIAN_POINT('Ctrl Pts',(-54.4592660843647,0.525003723543879,
-223.022413310737));
#203939=CARTESIAN_POINT('Ctrl Pts',(-56.6863552307302,1.33694765882884,
-219.669293489006));
#203940=CARTESIAN_POINT('Ctrl Pts',(-58.9133824694609,2.15010954210964,
-216.316434370579));
#203941=CARTESIAN_POINT('Ctrl Pts',(-61.140376519071,2.96385127852703,-212.963696992235));
#203942=CARTESIAN_POINT('Ctrl Pts',(-47.725208148176,-2.26586793370592,
-233.095797498554));
#203943=CARTESIAN_POINT('Ctrl Pts',(-49.9481820104395,-1.51156427070571,
-229.741201508812));
#203944=CARTESIAN_POINT('Ctrl Pts',(-52.171153048358,-0.753464571140378,
-226.387470648604));
#203945=CARTESIAN_POINT('Ctrl Pts',(-54.3941000891112,0.00604443117689846,
-223.034045756));
#203946=CARTESIAN_POINT('Ctrl Pts',(-56.6170471298644,0.765553433494175,
-219.680620863394));
#203947=CARTESIAN_POINT('Ctrl Pts',(-58.8399741136204,1.52661141375358,
-216.32753645248));
#203948=CARTESIAN_POINT('Ctrl Pts',(-61.0628850955307,2.28841296751785,
-212.974611260487));
#203949=CARTESIAN_POINT('Ctrl Pts',(-47.6989353797486,-2.4460016880478,
-233.102243720839));
#203950=CARTESIAN_POINT('Ctrl Pts',(-49.9197589274877,-1.71845616621595,
-229.747358791629));
#203951=CARTESIAN_POINT('Ctrl Pts',(-52.1406411035373,-0.986726750840026,
-226.393439406672));
#203952=CARTESIAN_POINT('Ctrl Pts',(-54.3615170914844,-0.253435215006592,
-223.039861978631));
#203953=CARTESIAN_POINT('Ctrl Pts',(-56.5823930794315,0.479856320826842,
-219.686284550589));
#203954=CARTESIAN_POINT('Ctrl Pts',(-58.8032699357002,1.21486234957556,
-216.333087493431));
#203955=CARTESIAN_POINT('Ctrl Pts',(-61.0241393837606,1.95069381201327,
-212.980068394613));
#203956=CARTESIAN_POINT('Ctrl Pts',(-47.6686102280658,-2.62577030498296,
-233.108739309799));
#203957=CARTESIAN_POINT('Ctrl Pts',(-49.8868622268275,-1.92479179417762,
-229.753549805137));
#203958=CARTESIAN_POINT('Ctrl Pts',(-52.1052541434417,-1.21924080077849,
-226.399430730627));
#203959=CARTESIAN_POINT('Ctrl Pts',(-54.3236644404932,-0.511970286406943,
-223.045691665041));
#203960=CARTESIAN_POINT('Ctrl Pts',(-56.5420747375447,0.195300227964602,
-219.691952599455));
#203961=CARTESIAN_POINT('Ctrl Pts',(-58.7605144009039,0.904454604383199,
-216.338635936458));
#203962=CARTESIAN_POINT('Ctrl Pts',(-60.9789586636595,1.61451932982577,
-212.985517079921));
#203963=CARTESIAN_POINT('Ctrl Pts',(-47.6342055660403,-2.80514285302076,
-233.11527543729));
#203964=CARTESIAN_POINT('Ctrl Pts',(-49.8494963118054,-2.13043323572804,
-229.759772872591));
#203965=CARTESIAN_POINT('Ctrl Pts',(-52.0650271669924,-1.4507786685942,
-226.405446498001));
#203966=CARTESIAN_POINT('Ctrl Pts',(-54.2806082192958,-0.769247485060314,
-223.051539438634));
#203967=CARTESIAN_POINT('Ctrl Pts',(-56.4961892715991,-0.0877163015264225,
-219.697632379269));
#203968=CARTESIAN_POINT('Ctrl Pts',(-58.7118360495897,0.595866264290071,
-216.344190859432));
#203969=CARTESIAN_POINT('Ctrl Pts',(-60.9275031739158,1.28044489740776,
-212.990967740646));
#203970=CARTESIAN_POINT('Ctrl Pts',(-47.6299049832871,-2.82756442152549,
-233.116092453226));
#203971=CARTESIAN_POINT('Ctrl Pts',(-49.8448255724277,-2.15613841592184,
-229.760550756022));
#203972=CARTESIAN_POINT('Ctrl Pts',(-52.0599987949363,-1.47972090207117,
-226.406198468922));
#203973=CARTESIAN_POINT('Ctrl Pts',(-54.2752261916461,-0.801407134891986,
-223.052270410334));
#203974=CARTESIAN_POINT('Ctrl Pts',(-56.4904535883559,-0.123093367712802,
-219.698342351745));
#203975=CARTESIAN_POINT('Ctrl Pts',(-58.7057512556755,0.557292721778429,
-216.344885224803));
#203976=CARTESIAN_POINT('Ctrl Pts',(-60.9210712376979,1.23868559335551,
-212.991649073236));
#203977=CARTESIAN_POINT('Ctrl Pts',(-47.6255406457911,-2.84997980588785,
-233.116910107551));
#203978=CARTESIAN_POINT('Ctrl Pts',(-49.8400849976146,-2.18183275209659,
-229.761329146599));
#203979=CARTESIAN_POINT('Ctrl Pts',(-52.0548947978176,-1.50864788311527,
-226.406950828634));
#203980=CARTESIAN_POINT('Ctrl Pts',(-54.2697628615623,-0.83354712920943,
-223.053001671879));
#203981=CARTESIAN_POINT('Ctrl Pts',(-56.4846309253071,-0.158446375303592,
-219.699052515123));
#203982=CARTESIAN_POINT('Ctrl Pts',(-58.699573926166,0.518747611680667,
-216.345579699174));
#203983=CARTESIAN_POINT('Ctrl Pts',(-60.9145412680937,1.1969591078103,-212.992330444524));
#203984=CARTESIAN_POINT('Ctrl Pts',(-47.6211124898449,-2.8723889492326,
-233.117728387381));
#203985=CARTESIAN_POINT('Ctrl Pts',(-49.8352745925261,-2.20751597714286,
-229.762108046517));
#203986=CARTESIAN_POINT('Ctrl Pts',(-52.0497152441705,-1.53755916668926,
-226.407703586764));
#203987=CARTESIAN_POINT('Ctrl Pts',(-54.2642183610334,-0.865666855062723,
-223.053733238581));
#203988=CARTESIAN_POINT('Ctrl Pts',(-56.4787214778963,-0.193774543436184,
-219.699762890398));
#203989=CARTESIAN_POINT('Ctrl Pts',(-58.6933043194368,0.480231871349857,
-216.346274307009));
#203990=CARTESIAN_POINT('Ctrl Pts',(-60.9079135866709,1.15526652998651,
-212.993011881675));
#203991=CARTESIAN_POINT('Ctrl Pts',(-47.6166843338988,-2.89479809257736,
-233.118546667211));
#203992=CARTESIAN_POINT('Ctrl Pts',(-49.8304641874375,-2.23319920218914,
-229.762886946434));
#203993=CARTESIAN_POINT('Ctrl Pts',(-52.0445356905235,-1.56647045026326,
-226.408456344895));
#203994=CARTESIAN_POINT('Ctrl Pts',(-54.2586738605045,-0.897786580916013,
-223.054464805284));
#203995=CARTESIAN_POINT('Ctrl Pts',(-56.4728120304856,-0.229102711568775,
-219.700473265674));
#203996=CARTESIAN_POINT('Ctrl Pts',(-58.6870347127076,0.44171613101905,
-216.346968914843));
#203997=CARTESIAN_POINT('Ctrl Pts',(-60.9012859052481,1.11357395216271,
-212.993693318827));
#203998=CARTESIAN_POINT('Ctrl Pts',(-47.6122821058773,-2.91382681376045,
-233.120123741771));
#203999=CARTESIAN_POINT('Ctrl Pts',(-49.8256462366764,-2.25563426408762,
-229.764381027656));
#204000=CARTESIAN_POINT('Ctrl Pts',(-52.0393253463554,-1.59222179649422,
-226.409896055477));
#204001=CARTESIAN_POINT('Ctrl Pts',(-54.2530784318765,-0.926817341305142,
-223.05586052551));
#204002=CARTESIAN_POINT('Ctrl Pts',(-56.4668315173976,-0.261412886116064,
-219.701824995542));
#204003=CARTESIAN_POINT('Ctrl Pts',(-58.680677501921,0.406166125023995,
-216.348288119608));
#204004=CARTESIAN_POINT('Ctrl Pts',(-60.8945556035063,1.07480407935814,
-212.99498540692));
#204005=CARTESIAN_POINT('Ctrl Pts',(-47.6074726880044,-2.94429670427164,
-233.119124814901));
#204006=CARTESIAN_POINT('Ctrl Pts',(-49.8205052535735,-2.2890391191441,
-229.763446888111));
#204007=CARTESIAN_POINT('Ctrl Pts',(-52.0338426588191,-1.6286224591917,
-226.409003009738));
#204008=CARTESIAN_POINT('Ctrl Pts',(-54.2472513064603,-0.966235601713411,
-223.055000571257));
#204009=CARTESIAN_POINT('Ctrl Pts',(-56.4606599541014,-0.303848744235122,
-219.700998132776));
#204010=CARTESIAN_POINT('Ctrl Pts',(-58.6741582110175,0.36068851501233,
-216.347485336292));
#204011=CARTESIAN_POINT('Ctrl Pts',(-60.8876872878579,1.02627337962685,
-212.994202601728));
#204012=CARTESIAN_POINT('Ctrl Pts',(-47.5978538522586,-3.00523648529404,
-233.117126961161));
#204013=CARTESIAN_POINT('Ctrl Pts',(-49.8102232873676,-2.35584882925707,
-229.761578609019));
#204014=CARTESIAN_POINT('Ctrl Pts',(-52.0228772837467,-1.70142378458667,
-226.407216918259));
#204015=CARTESIAN_POINT('Ctrl Pts',(-54.2355970556278,-1.04507212252995,
-223.053280662751));
#204016=CARTESIAN_POINT('Ctrl Pts',(-56.448316827509,-0.388720460473239,
-219.699344407242));
#204017=CARTESIAN_POINT('Ctrl Pts',(-58.6611196292105,0.269733294988998,
-216.345879769661));
#204018=CARTESIAN_POINT('Ctrl Pts',(-60.873950656561,0.929211980164266,
-212.992636991345));
#204019=CARTESIAN_POINT('Ctrl Pts',(-47.5885508550713,-3.06624038087206,
-233.115176478235));
#204020=CARTESIAN_POINT('Ctrl Pts',(-49.8002794578931,-2.42271445147103,
-229.759753873753));
#204021=CARTESIAN_POINT('Ctrl Pts',(-52.0122734022483,-1.77427184016,-226.405472145231));
#204022=CARTESIAN_POINT('Ctrl Pts',(-54.2243279326664,-1.12394607107203,
-223.051600306617));
#204023=CARTESIAN_POINT('Ctrl Pts',(-56.4363824630845,-0.473620301984068,
-219.697728468003));
#204024=CARTESIAN_POINT('Ctrl Pts',(-58.6485137824127,0.178759449846657,
-216.344310765974));
#204025=CARTESIAN_POINT('Ctrl Pts',(-60.8606708677034,0.832141479427629,
-212.99110694513));
#204026=CARTESIAN_POINT('Ctrl Pts',(-47.5795644264693,-3.1273054400959,
-233.113272591666));
#204027=CARTESIAN_POINT('Ctrl Pts',(-49.7906742268616,-2.48963297721053,
-229.757972064269));
#204028=CARTESIAN_POINT('Ctrl Pts',(-52.0020311559296,-1.84716370589099,
-226.403768144263));
#204029=CARTESIAN_POINT('Ctrl Pts',(-54.2134437517945,-1.20285465735803,
-223.049959011375));
#204030=CARTESIAN_POINT('Ctrl Pts',(-56.4248563476593,-0.558545608825073,
-219.696149878487));
#204031=CARTESIAN_POINT('Ctrl Pts',(-58.6363398184349,0.0877694602078754,
-216.342777920879));
#204032=CARTESIAN_POINT('Ctrl Pts',(-60.8478467270347,0.735064158177848,
-212.989612083611));
#204033=CARTESIAN_POINT('Ctrl Pts',(-47.5615915692654,-3.24943555854357,
-233.109464818529));
#204034=CARTESIAN_POINT('Ctrl Pts',(-49.7714637647986,-2.62347002868952,
-229.7544084453));
#204035=CARTESIAN_POINT('Ctrl Pts',(-51.9815466632923,-1.99294743735296,
-226.40036014233));
#204036=CARTESIAN_POINT('Ctrl Pts',(-54.1916753900507,-1.36067182993002,
-223.046676420892));
#204037=CARTESIAN_POINT('Ctrl Pts',(-56.401804116809,-0.728396222507082,
-219.692992699454));
#204038=CARTESIAN_POINT('Ctrl Pts',(-58.6119918904791,-0.0942105190696879,
-216.339712230689));
#204039=CARTESIAN_POINT('Ctrl Pts',(-60.8221984456974,0.540909515678286,
-212.986622360574));
#204040=CARTESIAN_POINT('Ctrl Pts',(-47.5448849460372,-3.37181033218646,
-233.105843362456));
#204041=CARTESIAN_POINT('Ctrl Pts',(-49.7536076690841,-2.75751868949416,
-229.751016479375));
#204042=CARTESIAN_POINT('Ctrl Pts',(-51.9625086899236,-2.13890640284165,
-226.397115187946));
#204043=CARTESIAN_POINT('Ctrl Pts',(-54.1714467798668,-1.51862754547975,
-223.043550040683));
#204044=CARTESIAN_POINT('Ctrl Pts',(-56.38038486981,-0.898348688117847,
-219.68998489342));
#204045=CARTESIAN_POINT('Ctrl Pts',(-58.5893714844719,-0.276255066290686,
-216.336791153806));
#204046=CARTESIAN_POINT('Ctrl Pts',(-60.798372749993,0.346727601648124,
-212.983773359142));
#204047=CARTESIAN_POINT('Ctrl Pts',(-47.5294508970783,-3.49440615205346,
-233.102402864825));
#204048=CARTESIAN_POINT('Ctrl Pts',(-49.7371099711637,-2.89175495532409,
-229.747791831751));
#204049=CARTESIAN_POINT('Ctrl Pts',(-51.9449186325461,-2.28501732803231,
-226.3940294043));
#204050=CARTESIAN_POINT('Ctrl Pts',(-54.1527566412239,-1.67669958626741,
-223.040576342272));
#204051=CARTESIAN_POINT('Ctrl Pts',(-56.3605946499017,-1.0683818445025,
-219.687123280246));
#204052=CARTESIAN_POINT('Ctrl Pts',(-58.5684718967623,-0.458344461962341,
-216.334011708901));
#204053=CARTESIAN_POINT('Ctrl Pts',(-60.7763601725369,0.15253653159383,
-212.981062249621));
#204054=CARTESIAN_POINT('Ctrl Pts',(-47.4059785054068,-4.47517271098946,
-233.07487888378));
#204055=CARTESIAN_POINT('Ctrl Pts',(-49.6051283878,-3.96564508196357,-229.721994650771));
#204056=CARTESIAN_POINT('Ctrl Pts',(-51.8041981735258,-3.45390472955758,
-226.369343135129));
#204057=CARTESIAN_POINT('Ctrl Pts',(-54.0032355320804,-2.94127591256867,
-223.016786754993));
#204058=CARTESIAN_POINT('Ctrl Pts',(-56.202272890635,-2.42864709557977,
-219.664230374857));
#204059=CARTESIAN_POINT('Ctrl Pts',(-58.4012751950854,-1.91505962733557,
-216.311776149656));
#204060=CARTESIAN_POINT('Ctrl Pts',(-60.6002595528876,-1.40099202884052,
-212.959373373456));
#204061=CARTESIAN_POINT('Ctrl Pts',(-47.3643002300016,-5.47063877596875,
-233.058775431931));
#204062=CARTESIAN_POINT('Ctrl Pts',(-49.5603357959614,-5.05191240085809,
-229.706777484113));
#204063=CARTESIAN_POINT('Ctrl Pts',(-51.7562892676681,-4.63275255105671,
-226.354730416234));
#204064=CARTESIAN_POINT('Ctrl Pts',(-53.9522144422201,-4.21341447341654,
-223.002667034626));
#204065=CARTESIAN_POINT('Ctrl Pts',(-56.148139616772,-3.79407639577637,
-219.650603653018));
#204066=CARTESIAN_POINT('Ctrl Pts',(-58.3440331530531,-3.37454700228228,
-216.298521859654));
#204067=CARTESIAN_POINT('Ctrl Pts',(-60.5399122633319,-2.95492052264675,
-212.94643187892));
#204068=CARTESIAN_POINT('Ctrl Pts',(-47.4064137512828,-6.46376836204135,
-233.053237209745));
#204069=CARTESIAN_POINT('Ctrl Pts',(-49.6038760388037,-6.13507130643716,
-229.701318673814));
#204070=CARTESIAN_POINT('Ctrl Pts',(-51.8014392198341,-5.80767781765755,
-226.34934009846));
#204071=CARTESIAN_POINT('Ctrl Pts',(-53.999040049297,-5.48080969928608,
-222.997335349492));
#204072=CARTESIAN_POINT('Ctrl Pts',(-56.19664087876,-5.15394158091461,-219.645330600522));
#204073=CARTESIAN_POINT('Ctrl Pts',(-58.3942830138637,-4.82763991403419,
-216.293298098971));
#204074=CARTESIAN_POINT('Ctrl Pts',(-60.5919449770341,-4.50162265073271,
-212.941251066378));
#204075=CARTESIAN_POINT('Ctrl Pts',(-47.4274705119234,-6.96033315507766,
-233.050468098652));
#204076=CARTESIAN_POINT('Ctrl Pts',(-49.6256461602249,-6.6766507592267,
-229.698589268665));
#204077=CARTESIAN_POINT('Ctrl Pts',(-51.8240141959171,-6.39514045095797,
-226.346644939574));
#204078=CARTESIAN_POINT('Ctrl Pts',(-54.0224528528355,-6.11450731222085,
-222.994669506924));
#204079=CARTESIAN_POINT('Ctrl Pts',(-56.220891509754,-5.83387417348373,
-219.642694074275));
#204080=CARTESIAN_POINT('Ctrl Pts',(-58.419407944269,-5.55418636991015,
-216.29068621863));
#204081=CARTESIAN_POINT('Ctrl Pts',(-60.6179613338852,-5.27497371477569,
-212.938660660107));
#204082=CARTESIAN_POINT('Ctrl Pts',(-47.4693973645209,-7.45640759953517,
-233.050348887721));
#204083=CARTESIAN_POINT('Ctrl Pts',(-49.6694421105903,-7.21751150761842,
-229.698309141063));
#204084=CARTESIAN_POINT('Ctrl Pts',(-51.8698193135396,-6.98165879246334,
-226.346267078691));
#204085=CARTESIAN_POINT('Ctrl Pts',(-54.0703159902812,-6.74703873870746,
-222.994214128443));
#204086=CARTESIAN_POINT('Ctrl Pts',(-56.2708126670227,-6.51241868495157,
-219.642161178194));
#204087=CARTESIAN_POINT('Ctrl Pts',(-58.4714415769781,-6.27912620426164,
-216.290098836338));
#204088=CARTESIAN_POINT('Ctrl Pts',(-60.6721324487782,-6.0465020347434,
-212.938028751337));
#204089=CARTESIAN_POINT('Ctrl Pts',(-47.5320802669249,-7.94976361170966,
-233.052889623343));
#204090=CARTESIAN_POINT('Ctrl Pts',(-49.7351412982067,-7.7556448112324,
-229.700481632561));
#204091=CARTESIAN_POINT('Ctrl Pts',(-51.9387261626187,-7.5654468780096,
-226.348205936691));
#204092=CARTESIAN_POINT('Ctrl Pts',(-54.1424952790584,-7.37683668146129,
-222.995965483144));
#204093=CARTESIAN_POINT('Ctrl Pts',(-56.3462643954981,-7.18822648491298,
-219.643725029598));
#204094=CARTESIAN_POINT('Ctrl Pts',(-58.5502384998489,-7.00132626939384,
-216.291526839263));
#204095=CARTESIAN_POINT('Ctrl Pts',(-60.7543073371829,-6.81528655387943,
-212.939344378339));
#204096=CARTESIAN_POINT('Ctrl Pts',(-47.563421718127,-8.1964416177969,-233.054159991154));
#204097=CARTESIAN_POINT('Ctrl Pts',(-49.7679908920149,-8.02471146303938,
-229.70156787831));
#204098=CARTESIAN_POINT('Ctrl Pts',(-51.9731795871583,-7.85734092078273,
-226.34917536569));
#204099=CARTESIAN_POINT('Ctrl Pts',(-54.1785849234471,-7.6917356528382,
-222.996841160495));
#204100=CARTESIAN_POINT('Ctrl Pts',(-56.3839902597359,-7.52613038489368,
-219.644506955299));
#204101=CARTESIAN_POINT('Ctrl Pts',(-58.5896369612844,-7.36242630195994,
-216.292240840726));
#204102=CARTESIAN_POINT('Ctrl Pts',(-60.7953947813852,-7.19967881344745,
-212.94000219184));
#204103=CARTESIAN_POINT('Ctrl Pts',(-47.5999371411941,-8.4424144119742,
-233.056093784063));
#204104=CARTESIAN_POINT('Ctrl Pts',(-49.8063055502802,-8.29307945277301,
-229.703266385626));
#204105=CARTESIAN_POINT('Ctrl Pts',(-52.0134014665884,-8.14854160584086,
-226.350723520978));
#204106=CARTESIAN_POINT('Ctrl Pts',(-54.2207502118905,-8.00594532648383,
-222.998268420575));
#204107=CARTESIAN_POINT('Ctrl Pts',(-56.4280989571927,-7.8633490471268,
-219.645813320171));
#204108=CARTESIAN_POINT('Ctrl Pts',(-58.6357298166351,-7.72284397328174,
-216.293459199193));
#204109=CARTESIAN_POINT('Ctrl Pts',(-60.8434900309058,-7.58339072582217,
-212.941147613748));
#204110=CARTESIAN_POINT('Ctrl Pts',(-47.6415907958571,-8.68748728842518,
-233.058700763469));
#204111=CARTESIAN_POINT('Ctrl Pts',(-49.8500528218283,-8.56055336019126,
-229.705584368071));
#204112=CARTESIAN_POINT('Ctrl Pts',(-52.0593649584596,-8.43886161373385,
-226.352856624949));
#204113=CARTESIAN_POINT('Ctrl Pts',(-54.2689704157657,-8.31928937162988,
-223.000252784861));
#204114=CARTESIAN_POINT('Ctrl Pts',(-56.4785758730718,-8.19971712952592,
-219.647648944772));
#204115=CARTESIAN_POINT('Ctrl Pts',(-58.6885092193172,-8.08242819326595,
-216.295186431349));
#204116=CARTESIAN_POINT('Ctrl Pts',(-60.8985922273728,-7.96628687259449,
-212.942784965869));
#204117=CARTESIAN_POINT('Ctrl Pts',(-47.6624176231886,-8.81002372665067,
-233.060004253171));
#204118=CARTESIAN_POINT('Ctrl Pts',(-49.8719264576024,-8.69429031390039,
-229.706743359295));
#204119=CARTESIAN_POINT('Ctrl Pts',(-52.0823467043952,-8.58402161768034,
-226.353923176935));
#204120=CARTESIAN_POINT('Ctrl Pts',(-54.2930805177033,-8.47596139420291,
-223.001244967003));
#204121=CARTESIAN_POINT('Ctrl Pts',(-56.5038143310114,-8.36790117072548,
-219.648566757072));
#204122=CARTESIAN_POINT('Ctrl Pts',(-58.7148989206583,-8.26222030325806,
-216.296050047426));
#204123=CARTESIAN_POINT('Ctrl Pts',(-60.9261433256064,-8.15773494598065,
-212.943603641929));
#204124=CARTESIAN_POINT('Ctrl Pts',(-47.6845291479335,-8.93233516940169,
-233.061476300607));
#204125=CARTESIAN_POINT('Ctrl Pts',(-49.8951583401493,-8.82780373392919,
-229.708057415679));
#204126=CARTESIAN_POINT('Ctrl Pts',(-52.1067639241,-8.72896144063768,-226.355136126385));
#204127=CARTESIAN_POINT('Ctrl Pts',(-54.3187044016857,-8.63241699899096,
-223.002376557269));
#204128=CARTESIAN_POINT('Ctrl Pts',(-56.5306448792714,-8.53587255734424,
-219.649616988152));
#204129=CARTESIAN_POINT('Ctrl Pts',(-58.7429602838421,-8.44180404135816,
-216.297040966938));
#204130=CARTESIAN_POINT('Ctrl Pts',(-60.9554461772338,-8.34897906928816,
-212.944545370418));
#204131=CARTESIAN_POINT('Ctrl Pts',(-47.7079217613744,-9.05439718416747,
-233.063119714194));
#204132=CARTESIAN_POINT('Ctrl Pts',(-49.9197449843438,-8.96106910734242,
-229.709528628916));
#204133=CARTESIAN_POINT('Ctrl Pts',(-52.1326136936507,-8.87365758922025,
-226.356497221309));
#204134=CARTESIAN_POINT('Ctrl Pts',(-54.3458398007892,-8.78863407215474,
-223.003649044211));
#204135=CARTESIAN_POINT('Ctrl Pts',(-56.5590659079277,-8.70361055508924,
-219.650800867113));
#204136=CARTESIAN_POINT('Ctrl Pts',(-58.7726924798428,-8.62116045955843,
-216.298160266832));
#204137=CARTESIAN_POINT('Ctrl Pts',(-60.9865007760101,-8.54000225738003,
-212.945611112248));
#204138=CARTESIAN_POINT('Ctrl Pts',(-47.7108458380545,-9.0696549360132,
-233.063325140892));
#204139=CARTESIAN_POINT('Ctrl Pts',(-49.9228183148681,-8.97772727901907,
-229.709712530571));
#204140=CARTESIAN_POINT('Ctrl Pts',(-52.1358449148446,-8.89174460779308,
-226.356667358174));
#204141=CARTESIAN_POINT('Ctrl Pts',(-54.3492317256771,-8.80816120630022,
-223.003808105078));
#204142=CARTESIAN_POINT('Ctrl Pts',(-56.5626185365097,-8.72457780480736,
-219.650948851983));
#204143=CARTESIAN_POINT('Ctrl Pts',(-58.7764090043429,-8.64358001183346,
-216.29830017932));
#204144=CARTESIAN_POINT('Ctrl Pts',(-60.9903826008572,-8.56388015589151,
-212.945744329977));
#204145=CARTESIAN_POINT('Ctrl Pts',(-47.7137899325008,-9.08490879046653,
-233.063533246565));
#204146=CARTESIAN_POINT('Ctrl Pts',(-49.9259128140418,-8.99438157488791,
-229.709898888829));
#204147=CARTESIAN_POINT('Ctrl Pts',(-52.1390985200058,-8.90982781887923,
-226.356839810649));
#204148=CARTESIAN_POINT('Ctrl Pts',(-54.3526472682709,-8.82768461331957,
-223.003969368145));
#204149=CARTESIAN_POINT('Ctrl Pts',(-56.5661960165361,-8.74554140775991,
-219.65109892564));
#204150=CARTESIAN_POINT('Ctrl Pts',(-58.7801516357373,-8.66599601217575,
-216.29844209819));
#204151=CARTESIAN_POINT('Ctrl Pts',(-60.994291796841,-8.58775460223573,
-212.945879485775));
#204152=CARTESIAN_POINT('Ctrl Pts',(-47.716754038316,-9.10015869973864,
-233.063744037883));
#204153=CARTESIAN_POINT('Ctrl Pts',(-49.9290284754874,-9.01103194700285,
-229.71008770866));
#204154=CARTESIAN_POINT('Ctrl Pts',(-52.1423745037473,-8.92790717652798,
-226.357014582869));
#204155=CARTESIAN_POINT('Ctrl Pts',(-54.3560864243857,-8.84720424996069,
-223.004132836908));
#204156=CARTESIAN_POINT('Ctrl Pts',(-56.5697983450241,-8.7665013233934,
-219.651251090947));
#204157=CARTESIAN_POINT('Ctrl Pts',(-58.78392037252,-8.68840842352587,-216.298586025925));
#204158=CARTESIAN_POINT('Ctrl Pts',(-60.9982283640248,-8.61162556319128,
-212.946016581829));
#204159=CARTESIAN_POINT('Ctrl Pts',(-47.7182360912236,-9.10778365437469,
-233.063849433542));
#204160=CARTESIAN_POINT('Ctrl Pts',(-49.9305863062102,-9.01935713306031,
-229.710182118577));
#204161=CARTESIAN_POINT('Ctrl Pts',(-52.1440124956181,-8.93694685535236,
-226.357101968979));
#204162=CARTESIAN_POINT('Ctrl Pts',(-54.3578060024431,-8.85696406828125,
-223.004214571289));
#204163=CARTESIAN_POINT('Ctrl Pts',(-56.5715995092681,-8.77698128121015,
-219.6513271736));
#204164=CARTESIAN_POINT('Ctrl Pts',(-58.7858047409113,-8.69961462920092,
-216.298657989792));
#204165=CARTESIAN_POINT('Ctrl Pts',(-61.0001966476166,-8.62356104366905,
-212.946085129856));
#204166=CARTESIAN_POINT('Ctrl Pts',(-47.7199389533574,-9.11682055194411,
-233.06406871878));
#204167=CARTESIAN_POINT('Ctrl Pts',(-49.9323460073902,-9.02903001372169,
-229.710378872728));
#204168=CARTESIAN_POINT('Ctrl Pts',(-52.1458407050898,-8.94729076123427,
-226.357284562563));
#204169=CARTESIAN_POINT('Ctrl Pts',(-54.3597065585291,-8.86799272250201,
-223.004385813307));
#204170=CARTESIAN_POINT('Ctrl Pts',(-56.5735724119685,-8.78869468376974,
-219.651487064051));
#204171=CARTESIAN_POINT('Ctrl Pts',(-58.7878543357751,-8.71202766150863,
-216.298809692624));
#204172=CARTESIAN_POINT('Ctrl Pts',(-61.0023248619954,-8.63668103342285,
-212.946230067727));
#204173=CARTESIAN_POINT('Ctrl Pts',(-47.7211311423516,-9.12247799776195,
-233.064017991084));
#204174=CARTESIAN_POINT('Ctrl Pts',(-49.9336413200512,-9.03547708644307,
-229.710333027481));
#204175=CARTESIAN_POINT('Ctrl Pts',(-52.1472334449741,-8.95451285699648,
-226.357241499541));
#204176=CARTESIAN_POINT('Ctrl Pts',(-54.3611948094061,-8.87598426441826,
-223.004344929563));
#204177=CARTESIAN_POINT('Ctrl Pts',(-56.5751561738381,-8.79745567184005,
-219.651448359586));
#204178=CARTESIAN_POINT('Ctrl Pts',(-58.7895314509544,-8.72155201353807,
-216.298772458348));
#204179=CARTESIAN_POINT('Ctrl Pts',(-61.004094357101,-8.64696579840547,
-212.94619401758));
#204180=CARTESIAN_POINT('Ctrl Pts',(-47.7223233313458,-9.1281354435798,
-233.063967263389));
#204181=CARTESIAN_POINT('Ctrl Pts',(-49.9349366327123,-9.04192415916445,
-229.710287182234));
#204182=CARTESIAN_POINT('Ctrl Pts',(-52.1486261848584,-8.96173495275868,
-226.357198436518));
#204183=CARTESIAN_POINT('Ctrl Pts',(-54.362683060283,-8.88397580633452,
-223.004304045819));
#204184=CARTESIAN_POINT('Ctrl Pts',(-56.5767399357077,-8.80621665991036,
-219.651409655121));
#204185=CARTESIAN_POINT('Ctrl Pts',(-58.7912085661337,-8.73107636556752,
-216.298735224073));
#204186=CARTESIAN_POINT('Ctrl Pts',(-61.0058638522065,-8.6572505633881,
-212.946157967432));
#204187=CARTESIAN_POINT('Ctrl Pts',(-47.7235115705647,-9.13379405727712,
-233.063916532445));
#204188=CARTESIAN_POINT('Ctrl Pts',(-49.9362275889306,-9.04837227186877,
-229.710241325062));
#204189=CARTESIAN_POINT('Ctrl Pts',(-52.1500141863611,-8.96895796970056,
-226.357155358521));
#204190=CARTESIAN_POINT('Ctrl Pts',(-54.3641661982611,-8.89196815031558,
-223.004263144959));
#204191=CARTESIAN_POINT('Ctrl Pts',(-56.5783182101612,-8.8149783309306,
-219.651370931397));
#204192=CARTESIAN_POINT('Ctrl Pts',(-58.7928798280227,-8.740601282021,-216.298697969725));
#204193=CARTESIAN_POINT('Ctrl Pts',(-61.0076271318174,-8.66753577332984,
-212.946121896728));
#204194=CARTESIAN_POINT('Ctrl Pts',(-47.724695856798,-9.13945382791814,
-233.06386579822));
#204195=CARTESIAN_POINT('Ctrl Pts',(-49.9375141864838,-9.05482141596443,
-229.710195456012));
#204196=CARTESIAN_POINT('Ctrl Pts',(-52.1513974481024,-8.97618190118969,
-226.357112265619));
#204197=CARTESIAN_POINT('Ctrl Pts',(-54.3656442227822,-8.89996129157268,
-223.00422222707));
#204198=CARTESIAN_POINT('Ctrl Pts',(-56.579890997462,-8.82374068195567,
-219.651332188522));
#204199=CARTESIAN_POINT('Ctrl Pts',(-58.7945452376739,-8.75012676166283,
-216.298660695422));
#204200=CARTESIAN_POINT('Ctrl Pts',(-61.0093841977678,-8.67782142864838,
-212.946085805591));
#204201=CARTESIAN_POINT('Ctrl Pts',(-47.7294330017316,-9.16209291048223,
-233.063662861321));
#204202=CARTESIAN_POINT('Ctrl Pts',(-49.9426605766967,-9.08061799234707,
-229.710011979809));
#204203=CARTESIAN_POINT('Ctrl Pts',(-52.1569304950676,-9.0050776271462,
-226.356939894011));
#204204=CARTESIAN_POINT('Ctrl Pts',(-54.3715563208665,-8.93193385660108,
-223.004058555517));
#204205=CARTESIAN_POINT('Ctrl Pts',(-56.5861821466654,-8.85879008605595,
-219.651177217023));
#204206=CARTESIAN_POINT('Ctrl Pts',(-58.8012068762785,-8.78822868023012,
-216.29851159821));
#204207=CARTESIAN_POINT('Ctrl Pts',(-61.0164124615696,-8.71896404992253,
-212.945941441045));
#204208=CARTESIAN_POINT('Ctrl Pts',(-47.7341068986215,-9.18475050415316,
-233.063459871981));
#204209=CARTESIAN_POINT('Ctrl Pts',(-49.9477372281162,-9.10643107100621,
-229.709828313605));
#204210=CARTESIAN_POINT('Ctrl Pts',(-52.1623877057604,-9.03398798587052,
-226.356767284002));
#204211=CARTESIAN_POINT('Ctrl Pts',(-54.3773866035966,-8.96391917805846,
-223.003894611599));
#204212=CARTESIAN_POINT('Ctrl Pts',(-56.5923855014328,-8.89385037024639,
-219.651021939195));
#204213=CARTESIAN_POINT('Ctrl Pts',(-58.8077748791159,-8.8263396098254,
-216.298362181801));
#204214=CARTESIAN_POINT('Ctrl Pts',(-61.0233413068671,-8.76011379724005,
-212.945796749657));
#204215=CARTESIAN_POINT('Ctrl Pts',(-47.7387173442106,-9.207425908897,-233.06325682779));
#204216=CARTESIAN_POINT('Ctrl Pts',(-49.9527439997195,-9.13226010185821,
-229.709644459743));
#204217=CARTESIAN_POINT('Ctrl Pts',(-52.1677689925887,-9.06291255266274,
-226.356594439508));
#204218=CARTESIAN_POINT('Ctrl Pts',(-54.383135035575,-8.99591694925441,
-223.003730400442));
#204219=CARTESIAN_POINT('Ctrl Pts',(-56.5985010785614,-8.92892134584607,
-219.650866361376));
#204220=CARTESIAN_POINT('Ctrl Pts',(-58.8142493132399,-8.86445947120716,
-216.2982124531));
#204221=CARTESIAN_POINT('Ctrl Pts',(-61.030170850553,-8.80127069719074,
-212.945651738761));
#204222=CARTESIAN_POINT('Ctrl Pts',(-47.7479382353889,-9.25277671838467,
-233.062850739409));
#204223=CARTESIAN_POINT('Ctrl Pts',(-49.9627575429261,-9.18391816356222,
-229.70927675202));
#204224=CARTESIAN_POINT('Ctrl Pts',(-52.1785315662453,-9.12076168624719,
-226.356248750518));
#204225=CARTESIAN_POINT('Ctrl Pts',(-54.394631899532,-9.05991249164631,
-223.003401978127));
#204226=CARTESIAN_POINT('Ctrl Pts',(-56.6107322328186,-8.99906329704543,
-219.650555205738));
#204227=CARTESIAN_POINT('Ctrl Pts',(-58.827198181488,-8.9406991939707,-216.297912995698));
#204228=CARTESIAN_POINT('Ctrl Pts',(-61.0438299379249,-8.88358449709214,
-212.945361716967));
#204229=CARTESIAN_POINT('Ctrl Pts',(-47.7569053178599,-9.29819877221664,
-233.062444432209));
#204230=CARTESIAN_POINT('Ctrl Pts',(-49.9724915649241,-9.23564003421678,
-229.708908294511));
#204231=CARTESIAN_POINT('Ctrl Pts',(-52.1889904432917,-9.1786676522935,
-226.355902124491));
#204232=CARTESIAN_POINT('Ctrl Pts',(-54.4058013599478,-9.12395783319898,
-223.003072487813));
#204233=CARTESIAN_POINT('Ctrl Pts',(-56.6226122766038,-9.06924801410446,
-219.650242851134));
#204234=CARTESIAN_POINT('Ctrl Pts',(-58.8397727753602,-9.01697464410811,
-216.297612290131));
#204235=CARTESIAN_POINT('Ctrl Pts',(-61.0570918196413,-8.96592690776347,
-212.945070418141));
#204236=CARTESIAN_POINT('Ctrl Pts',(-47.7656170077038,-9.34368646884676,
-233.062037879842));
#204237=CARTESIAN_POINT('Ctrl Pts',(-49.9819449608238,-9.2874213104565,
-229.708539095772));
#204238=CARTESIAN_POINT('Ctrl Pts',(-52.1991449367821,-9.23662705053824,
-226.355554581771));
#204239=CARTESIAN_POINT('Ctrl Pts',(-54.4166431400134,-9.18805051768256,
-223.002741959001));
#204240=CARTESIAN_POINT('Ctrl Pts',(-56.6341413432447,-9.13947398482688,
-219.649929336231));
#204241=CARTESIAN_POINT('Ctrl Pts',(-58.8519736255103,-9.09328518499885,
-216.297310379527));
#204242=CARTESIAN_POINT('Ctrl Pts',(-61.069957421301,-9.04829813924799,
-212.94477788882));
#204243=CARTESIAN_POINT('Ctrl Pts',(-47.9050040452069,-10.0714896149287,
-233.055533041971));
#204244=CARTESIAN_POINT('Ctrl Pts',(-50.1331992952188,-10.115921730292,
-229.702631915958));
#204245=CARTESIAN_POINT('Ctrl Pts',(-52.3616168326291,-10.1639774224541,
-226.349993898252));
#204246=CARTESIAN_POINT('Ctrl Pts',(-54.5901116210639,-10.2135334694198,
-222.997453498015));
#204247=CARTESIAN_POINT('Ctrl Pts',(-56.8186064094987,-10.2630895163856,
-219.644913097779));
#204248=CARTESIAN_POINT('Ctrl Pts',(-59.0471872279132,-10.3142538392508,
-216.292479809858));
#204249=CARTESIAN_POINT('Ctrl Pts',(-61.2758070478567,-10.3662378430004,
-212.940097419686));
#204250=CARTESIAN_POINT('Ctrl Pts',(-47.9784204856001,-10.8160623601621,
-233.048965734498));
#204251=CARTESIAN_POINT('Ctrl Pts',(-50.2122149161821,-10.9596359714715,
-229.696533843322));
#204252=CARTESIAN_POINT('Ctrl Pts',(-52.4459513488164,-11.1050325676855,
-226.344195161346));
#204253=CARTESIAN_POINT('Ctrl Pts',(-54.6796638979776,-11.2511741221942,
-222.991894447348));
#204254=CARTESIAN_POINT('Ctrl Pts',(-56.9133764471387,-11.3973156767028,
-219.639593733351));
#204255=CARTESIAN_POINT('Ctrl Pts',(-59.1470633643947,-11.5442580388962,
-216.287333861831));
#204256=CARTESIAN_POINT('Ctrl Pts',(-61.3807372553903,-11.6916056255194,
-212.935094620098));
#204257=CARTESIAN_POINT('Ctrl Pts',(-47.9834035327445,-11.5593373188707,
-233.042545221464));
#204258=CARTESIAN_POINT('Ctrl Pts',(-50.2170610824398,-11.8031522322565,
-229.690412491071));
#204259=CARTESIAN_POINT('Ctrl Pts',(-52.4507177144441,-12.0469951332675,
-226.33828118561));
#204260=CARTESIAN_POINT('Ctrl Pts',(-54.684373970075,-12.2908494697823,
-222.986150461423));
#204261=CARTESIAN_POINT('Ctrl Pts',(-56.9180302257058,-12.5347038062971,
-219.634019737236));
#204262=CARTESIAN_POINT('Ctrl Pts',(-59.1516860770602,-12.7785704359954,
-216.281889638136));
#204263=CARTESIAN_POINT('Ctrl Pts',(-61.3853417234255,-13.0224432858052,
-212.92975985503));
#204264=CARTESIAN_POINT('Ctrl Pts',(-47.9883865798889,-12.3026122775794,
-233.036124708431));
#204265=CARTESIAN_POINT('Ctrl Pts',(-50.2219072486975,-12.6466684930416,
-229.684291138819));
#204266=CARTESIAN_POINT('Ctrl Pts',(-52.4554840800718,-12.9889576988494,
-226.332367209873));
#204267=CARTESIAN_POINT('Ctrl Pts',(-54.6890840421723,-13.3305248173704,
-222.980406475497));
#204268=CARTESIAN_POINT('Ctrl Pts',(-56.9226840042728,-13.6720919358914,
-219.628445741121));
#204269=CARTESIAN_POINT('Ctrl Pts',(-59.1563087897256,-14.0128828330946,
-216.276445414441));
#204270=CARTESIAN_POINT('Ctrl Pts',(-61.3899461914607,-14.353280946091,
-212.924425089962));
#204271=CARTESIAN_POINT('Ctrl Pts',(-47.9249646072757,-13.0488680722298,
-233.029820400472));
#204272=CARTESIAN_POINT('Ctrl Pts',(-50.1526004463906,-13.4919379593521,
-229.678126738255));
#204273=CARTESIAN_POINT('Ctrl Pts',(-52.3806853939039,-13.9314932517732,
-226.326331018504));
#204274=CARTESIAN_POINT('Ctrl Pts',(-54.6089422344929,-14.3695898632513,
-222.974482011522));
#204275=CARTESIAN_POINT('Ctrl Pts',(-56.8371990750819,-14.8076864747294,
-219.622633004539));
#204276=CARTESIAN_POINT('Ctrl Pts',(-59.0656432437958,-15.2442202432178,
-216.270729289381));
#204277=CARTESIAN_POINT('Ctrl Pts',(-61.2941782948235,-15.6799563776017,
-212.918794099076));
#204278=CARTESIAN_POINT('Ctrl Pts',(-47.794905416537,-13.7800486938334,
-233.0237330726));
#204279=CARTESIAN_POINT('Ctrl Pts',(-50.0104931205382,-14.3235088264801,
-229.67202163298));
#204280=CARTESIAN_POINT('Ctrl Pts',(-52.2272657548643,-14.8617096033744,
-226.320268783124));
#204281=CARTESIAN_POINT('Ctrl Pts',(-54.4444686924125,-15.3977680306514,
-222.968464399553));
#204282=CARTESIAN_POINT('Ctrl Pts',(-56.6616716299607,-15.9338264579286,
-219.616660015982));
#204283=CARTESIAN_POINT('Ctrl Pts',(-58.8793495680496,-16.4675807101401,
-216.264808277961));
#204284=CARTESIAN_POINT('Ctrl Pts',(-61.0972513955672,-17.0001720517288,
-212.912922153302));
#204285=CARTESIAN_POINT('Ctrl Pts',(-47.7867767171158,-13.8257474826836,
-233.023352614608));
#204286=CARTESIAN_POINT('Ctrl Pts',(-50.0016114126724,-14.3754820056756,
-229.6716400639));
#204287=CARTESIAN_POINT('Ctrl Pts',(-52.2176770274244,-14.9198481253495,
-226.319889893413));
#204288=CARTESIAN_POINT('Ctrl Pts',(-54.4341890960325,-15.4620291661139,
-222.968088298805));
#204289=CARTESIAN_POINT('Ctrl Pts',(-56.6507011646406,-16.0042102068785,
-219.616286704198));
#204290=CARTESIAN_POINT('Ctrl Pts',(-58.8677062133155,-16.5440407393228,
-216.264438214748));
#204291=CARTESIAN_POINT('Ctrl Pts',(-61.0849434643637,-17.0826855313617,
-212.912555156691));
#204292=CARTESIAN_POINT('Ctrl Pts',(-47.7783900662832,-13.8713871446584,
-233.022972933189));
#204293=CARTESIAN_POINT('Ctrl Pts',(-49.9924469184794,-14.4274016342853,
-229.671258688898));
#204294=CARTESIAN_POINT('Ctrl Pts',(-52.2077820506802,-14.9779386235856,
-226.319510892586));
#204295=CARTESIAN_POINT('Ctrl Pts',(-54.423580209151,-15.5262479876512,
-222.967711846576));
#204296=CARTESIAN_POINT('Ctrl Pts',(-56.6393783676217,-16.0745573517168,
-219.615912800565));
#204297=CARTESIAN_POINT('Ctrl Pts',(-58.8556879728042,-16.6204700248875,
-216.264067401558));
#204298=CARTESIAN_POINT('Ctrl Pts',(-61.0722383017368,-17.1651742681581,
-212.91218728226));
#204299=CARTESIAN_POINT('Ctrl Pts',(-47.7697469949171,-13.9169620127152,
-233.022593985349));
#204300=CARTESIAN_POINT('Ctrl Pts',(-49.983000674726,-14.4792632474105,
-229.670877481921));
#204301=CARTESIAN_POINT('Ctrl Pts',(-52.1975814320602,-15.0359776440825,
-226.319131772858));
#204302=CARTESIAN_POINT('Ctrl Pts',(-54.4126422197256,-15.5904219929251,
-222.967335049774));
#204303=CARTESIAN_POINT('Ctrl Pts',(-56.627703007391,-16.1448663417677,
-219.615538326691));
#204304=CARTESIAN_POINT('Ctrl Pts',(-58.8432942103714,-16.6968678996294,
-216.263695872058));
#204305=CARTESIAN_POINT('Ctrl Pts',(-61.0591348703587,-17.2476384491985,
-212.91181857376));
#204306=CARTESIAN_POINT('Ctrl Pts',(-47.7654254592341,-13.9397494467436,
-233.022404511428));
#204307=CARTESIAN_POINT('Ctrl Pts',(-49.9782775528494,-14.5051940539731,
-229.670686878432));
#204308=CARTESIAN_POINT('Ctrl Pts',(-52.1924811227502,-15.064997154331,
-226.318942212994));
#204309=CARTESIAN_POINT('Ctrl Pts',(-54.4071732250129,-15.6225089955621,
-222.967146651374));
#204310=CARTESIAN_POINT('Ctrl Pts',(-56.6218653272756,-16.1800208367931,
-219.615351089753));
#204311=CARTESIAN_POINT('Ctrl Pts',(-58.8370973291551,-16.7350668370003,
-216.263510107308));
#204312=CARTESIAN_POINT('Ctrl Pts',(-61.0525831546696,-17.2888705397188,
-212.911634219511));
#204313=CARTESIAN_POINT('Ctrl Pts',(-47.7610398192893,-13.962520682369,
-233.022215220766));
#204314=CARTESIAN_POINT('Ctrl Pts',(-49.973483994075,-14.5311103567258,
-229.670496316751));
#204315=CARTESIAN_POINT('Ctrl Pts',(-52.1873044032685,-15.0940037951854,
-226.318752623187));
#204316=CARTESIAN_POINT('Ctrl Pts',(-54.4016219548089,-15.6545847941602,
-222.9669581666));
#204317=CARTESIAN_POINT('Ctrl Pts',(-56.6159395063494,-16.2151657931349,
-219.615163710013));
#204318=CARTESIAN_POINT('Ctrl Pts',(-58.8308065673522,-16.7732579216688,
-216.263324163236));
#204319=CARTESIAN_POINT('Ctrl Pts',(-61.0459318716081,-17.3300964912969,
-212.911449656498));
#204320=CARTESIAN_POINT('Ctrl Pts',(-47.7565902716679,-13.9852750117499,
-233.022026107165));
#204321=CARTESIAN_POINT('Ctrl Pts',(-49.9686201309427,-14.5570115979937,
-229.670305792423));
#204322=CARTESIAN_POINT('Ctrl Pts',(-52.1820513513198,-15.1229971351898,
-226.318563001159));
#204323=CARTESIAN_POINT('Ctrl Pts',(-54.3959884334715,-15.6866490761195,
-222.966769594939));
#204324=CARTESIAN_POINT('Ctrl Pts',(-56.6099255156231,-16.2503010170492,
-219.614976188718));
#204325=CARTESIAN_POINT('Ctrl Pts',(-58.8244218448074,-16.8114410702517,
-216.26313804258));
#204326=CARTESIAN_POINT('Ctrl Pts',(-61.0391808904015,-17.371316327283,
-212.911264888718));
#204327=CARTESIAN_POINT('Ctrl Pts',(-47.7543654978573,-13.9966521764404,
-233.021931550365));
#204328=CARTESIAN_POINT('Ctrl Pts',(-49.9661881993766,-14.5699622186276,
-229.67021053026));
#204329=CARTESIAN_POINT('Ctrl Pts',(-52.1794248253455,-15.137493805192,
-226.318468190145));
#204330=CARTESIAN_POINT('Ctrl Pts',(-54.3931716728027,-15.7026812170992,
-222.966675309108));
#204331=CARTESIAN_POINT('Ctrl Pts',(-56.60691852026,-16.2678686290064,-219.614882428071));
#204332=CARTESIAN_POINT('Ctrl Pts',(-58.821229483535,-16.8305326445432,
-216.263044982252));
#204333=CARTESIAN_POINT('Ctrl Pts',(-61.0358053997983,-17.391926245276,
-212.911172504828));
#204334=CARTESIAN_POINT('Ctrl Pts',(-47.7521247471819,-14.008025114576,
-233.021837037822));
#204335=CARTESIAN_POINT('Ctrl Pts',(-49.9637386917516,-14.5829090738954,
-229.670115277422));
#204336=CARTESIAN_POINT('Ctrl Pts',(-52.1767792162729,-15.1519871499853,
-226.318373371061));
#204337=CARTESIAN_POINT('Ctrl Pts',(-54.3903343493595,-15.7187104789216,
-222.966581001541));
#204338=CARTESIAN_POINT('Ctrl Pts',(-56.6038894824462,-16.2854338078579,
-219.61478863202));
#204339=CARTESIAN_POINT('Ctrl Pts',(-58.8180136320704,-16.8496222348139,
-216.262951877763));
#204340=CARTESIAN_POINT('Ctrl Pts',(-61.0324049846472,-17.4125346343709,
-212.91108006973));
#204341=CARTESIAN_POINT('Ctrl Pts',(-47.7498680445413,-14.0193937377161,
-233.021742568709));
#204342=CARTESIAN_POINT('Ctrl Pts',(-49.9612716248183,-14.5958520941202,
-229.670020033279));
#204343=CARTESIAN_POINT('Ctrl Pts',(-52.1741145339256,-15.1664771156592,
-226.318278543544));
#204344=CARTESIAN_POINT('Ctrl Pts',(-54.3874764662403,-15.7347368225257,
-222.966486672088));
#204345=CARTESIAN_POINT('Ctrl Pts',(-56.600838398555,-16.3029965293923,
-219.614694800631));
#204346=CARTESIAN_POINT('Ctrl Pts',(-58.8147742803545,-16.8687098306404,
-216.262858729364));
#204347=CARTESIAN_POINT('Ctrl Pts',(-61.0289796285328,-17.4331414974815,
-212.910987583833));
#204348=CARTESIAN_POINT('Ctrl Pts',(-47.7476113419008,-14.0307623608562,
-233.021648099596));
#204349=CARTESIAN_POINT('Ctrl Pts',(-49.9588045578851,-14.6087951143449,
-229.669924789137));
#204350=CARTESIAN_POINT('Ctrl Pts',(-52.1714498515783,-15.180967081333,
-226.318183716026));
#204351=CARTESIAN_POINT('Ctrl Pts',(-54.3846185831211,-15.7507631661298,
-222.966392342634));
#204352=CARTESIAN_POINT('Ctrl Pts',(-56.5977873146637,-16.3205592509265,
-219.614600969242));
#204353=CARTESIAN_POINT('Ctrl Pts',(-58.8115349286387,-16.887797426467,
-216.262765580964));
#204354=CARTESIAN_POINT('Ctrl Pts',(-61.0255542724185,-17.4537483605921,
-212.910895097936));
#204355=CARTESIAN_POINT('Ctrl Pts',(-47.7442016228112,-14.0473500394083,
-233.021665980788));
#204356=CARTESIAN_POINT('Ctrl Pts',(-49.9552695851286,-14.62672636609,-229.669960086485));
#204357=CARTESIAN_POINT('Ctrl Pts',(-52.167771235297,-15.2002885297448,
-226.318229365726));
#204358=CARTESIAN_POINT('Ctrl Pts',(-54.3807900271312,-15.7714932773578,
-222.966446178071));
#204359=CARTESIAN_POINT('Ctrl Pts',(-56.5938088189654,-16.3426980249709,
-219.614662990416));
#204360=CARTESIAN_POINT('Ctrl Pts',(-58.8073994401649,-16.9113648377023,
-216.262833288602));
#204361=CARTESIAN_POINT('Ctrl Pts',(-61.0212585846625,-17.4787543086446,
-212.910967436579));
#204362=CARTESIAN_POINT('Ctrl Pts',(-47.7411284099535,-14.0625507697344,
-233.021657357818));
#204363=CARTESIAN_POINT('Ctrl Pts',(-49.9520501521893,-14.6433321699676,
-229.669963755451));
#204364=CARTESIAN_POINT('Ctrl Pts',(-52.164395575698,-15.2183262074345,
-226.318240561216));
#204365=CARTESIAN_POINT('Ctrl Pts',(-54.3772547239517,-15.7909735318649,
-222.966463366842));
#204366=CARTESIAN_POINT('Ctrl Pts',(-56.5901138722054,-16.3636208562953,
-219.614686172468));
#204367=CARTESIAN_POINT('Ctrl Pts',(-58.8035410200603,-16.9337418020372,
-216.262860718253));
#204368=CARTESIAN_POINT('Ctrl Pts',(-61.0172349543283,-17.5025911610169,
-212.910998351897));
#204369=CARTESIAN_POINT('Ctrl Pts',(-47.7165427070916,-14.1841566123428,
-233.021588374054));
#204370=CARTESIAN_POINT('Ctrl Pts',(-49.9262946886754,-14.7761786009886,
-229.669993107177));
#204371=CARTESIAN_POINT('Ctrl Pts',(-52.1373902989064,-15.3626276289524,
-226.318330125135));
#204372=CARTESIAN_POINT('Ctrl Pts',(-54.3489722985157,-15.9468155679217,
-222.966600877007));
#204373=CARTESIAN_POINT('Ctrl Pts',(-56.560554298125,-16.531003506891,-219.614871628879));
#204374=CARTESIAN_POINT('Ctrl Pts',(-58.7726736592232,-17.1127575167165,
-216.263080155467));
#204375=CARTESIAN_POINT('Ctrl Pts',(-60.9850459116547,-17.6932859799952,
-212.911245674445));
#204376=CARTESIAN_POINT('Ctrl Pts',(-47.6932284506644,-14.3060363961889,
-233.021682926744));
#204377=CARTESIAN_POINT('Ctrl Pts',(-49.901885438682,-14.9092956442213,
-229.670173308391));
#204378=CARTESIAN_POINT('Ctrl Pts',(-52.1118097264559,-15.507193974503,
-226.318562347407));
#204379=CARTESIAN_POINT('Ctrl Pts',(-54.3221941272102,-16.1029162862599,
-222.966874425379));
#204380=CARTESIAN_POINT('Ctrl Pts',(-56.5325785279645,-16.6986385980169,
-219.615186503351));
#204381=CARTESIAN_POINT('Ctrl Pts',(-58.7434709011157,-17.2920187463379,
-216.263424143813));
#204382=CARTESIAN_POINT('Ctrl Pts',(-60.9546027715979,-17.8842191820846,
-212.911613494952));
#204383=CARTESIAN_POINT('Ctrl Pts',(-47.6711899624377,-14.4281659124299,
-233.021940707592));
#204384=CARTESIAN_POINT('Ctrl Pts',(-49.8788265984679,-15.0426590253955,
-229.670504307963));
#204385=CARTESIAN_POINT('Ctrl Pts',(-52.0876575029478,-15.6520019918285,
-226.318937245156));
#204386=CARTESIAN_POINT('Ctrl Pts',(-54.296923205648,-16.259253814469,-222.967284070276));
#204387=CARTESIAN_POINT('Ctrl Pts',(-56.5061889083483,-16.8665056371095,
-219.615630895396));
#204388=CARTESIAN_POINT('Ctrl Pts',(-58.7159343195776,-17.4715067819979,
-216.263892782403));
#204389=CARTESIAN_POINT('Ctrl Pts',(-60.9259062922535,-18.0753740181923,
-212.912101903999));
#204390=CARTESIAN_POINT('Ctrl Pts',(-47.6271129859842,-14.672424944912,
-233.022456269286));
#204391=CARTESIAN_POINT('Ctrl Pts',(-49.8327089180398,-15.3093857877439,
-229.671166307109));
#204392=CARTESIAN_POINT('Ctrl Pts',(-52.0393530559316,-15.9416180264796,
-226.319687040658));
#204393=CARTESIAN_POINT('Ctrl Pts',(-54.2463813625237,-16.5719288708872,
-222.968103360071));
#204394=CARTESIAN_POINT('Ctrl Pts',(-56.4534096691157,-17.2022397152948,
-219.616519679485));
#204395=CARTESIAN_POINT('Ctrl Pts',(-58.6608611565012,-17.830482853318,
-216.264830059583));
#204396=CARTESIAN_POINT('Ctrl Pts',(-60.8685133335648,-18.4576836904079,
-212.913078722092));
#204397=CARTESIAN_POINT('Ctrl Pts',(-47.5881385453956,-14.9176828178641,
-233.023623696835));
#204398=CARTESIAN_POINT('Ctrl Pts',(-49.7919925129992,-15.5770978463543,
-229.672430710276));
#204399=CARTESIAN_POINT('Ctrl Pts',(-51.9967617280187,-16.2322007103616,
-226.321006893536));
#204400=CARTESIAN_POINT('Ctrl Pts',(-54.2018683085728,-16.8855511423113,
-222.96946650484));
#204401=CARTESIAN_POINT('Ctrl Pts',(-56.4069748891269,-17.538901574261,
-219.617926116144));
#204402=CARTESIAN_POINT('Ctrl Pts',(-58.6124525981959,-18.1903661459459,
-216.266265596097));
#204403=CARTESIAN_POINT('Ctrl Pts',(-60.8181069486676,-18.8408799020897,
-212.914537613908));
#204404=CARTESIAN_POINT('Ctrl Pts',(-47.554307632397,-15.1637468311187,
-233.025453073475));
#204405=CARTESIAN_POINT('Ctrl Pts',(-49.7567152646595,-15.8456016742832,
-229.674306559616));
#204406=CARTESIAN_POINT('Ctrl Pts',(-51.9599159483462,-16.5235645049904,
-226.322904658655));
#204407=CARTESIAN_POINT('Ctrl Pts',(-54.1634104836589,-17.1999459798668,
-222.971380331423));
#204408=CARTESIAN_POINT('Ctrl Pts',(-56.3669050189717,-17.8763274547433,
-219.619856004191));
#204409=CARTESIAN_POINT('Ctrl Pts',(-58.5707224241369,-18.5510070650469,
-216.268204278443));
#204410=CARTESIAN_POINT('Ctrl Pts',(-60.7746940090617,-19.2248286528632,
-212.916482666117));
#204411=CARTESIAN_POINT('Ctrl Pts',(-47.4866458063998,-15.6558748576279,
-233.029111826755));
#204412=CARTESIAN_POINT('Ctrl Pts',(-49.68616076798,-16.3826093301408,-229.678058258297));
#204413=CARTESIAN_POINT('Ctrl Pts',(-51.8862243890013,-17.1062920942477,
-226.326700188893));
#204414=CARTESIAN_POINT('Ctrl Pts',(-54.0864948338312,-17.8287356549779,
-222.97520798459));
#204415=CARTESIAN_POINT('Ctrl Pts',(-56.2867652786612,-18.551179215708,
-219.623715780286));
#204416=CARTESIAN_POINT('Ctrl Pts',(-58.4872620760191,-19.2722889032489,
-216.272081643134));
#204417=CARTESIAN_POINT('Ctrl Pts',(-60.6878681298499,-19.9927261544104,
-212.920372770536));
#204418=CARTESIAN_POINT('Ctrl Pts',(-47.4396210333615,-16.1511579441859,
-233.035417077088));
#204419=CARTESIAN_POINT('Ctrl Pts',(-49.6374078624443,-16.9227386754765,
-229.684254369749));
#204420=CARTESIAN_POINT('Ctrl Pts',(-51.835544167002,-17.6921151741007,
-226.332805980913));
#204421=CARTESIAN_POINT('Ctrl Pts',(-54.0338142213281,-18.4605999037604,
-222.98123698552));
#204422=CARTESIAN_POINT('Ctrl Pts',(-56.2320842756543,-19.2290846334201,
-219.629667990126));
#204423=CARTESIAN_POINT('Ctrl Pts',(-58.4305002120414,-19.9966086767195,
-216.277970249807));
#204424=CARTESIAN_POINT('Ctrl Pts',(-60.6289872337381,-20.7636493692889,
-212.926206211883));
#204425=CARTESIAN_POINT('Ctrl Pts',(-47.4134504259477,-16.6473487128058,
-233.044455194982));
#204426=CARTESIAN_POINT('Ctrl Pts',(-49.6106642054098,-17.4639704569693,
-229.692980964189));
#204427=CARTESIAN_POINT('Ctrl Pts',(-51.808075938482,-18.2792435060293,
-226.341309714209));
#204428=CARTESIAN_POINT('Ctrl Pts',(-54.0055642141686,-19.0939722550291,
-222.989556757961));
#204429=CARTESIAN_POINT('Ctrl Pts',(-56.2030524898552,-19.9087010040289,
-219.637803801712));
#204430=CARTESIAN_POINT('Ctrl Pts',(-58.4006240585482,-20.7228430676927,
-216.285963294552));
#204431=CARTESIAN_POINT('Ctrl Pts',(-60.5982364662104,-21.5366903458251,
-212.934078132851));
#204432=CARTESIAN_POINT('Ctrl Pts',(-47.3611092111201,-17.6397302500457,
-233.062531430769));
#204433=CARTESIAN_POINT('Ctrl Pts',(-49.5571768913406,-18.5464340199547,
-229.71043415307));
#204434=CARTESIAN_POINT('Ctrl Pts',(-51.753139481442,-19.4535001698865,
-226.358317180801));
#204435=CARTESIAN_POINT('Ctrl Pts',(-53.9490641998496,-20.3607169575665,
-223.006196302843));
#204436=CARTESIAN_POINT('Ctrl Pts',(-56.1449889182572,-21.2679337452465,
-219.654075424885));
#204437=CARTESIAN_POINT('Ctrl Pts',(-58.3408717515618,-22.175311849639,
-216.301949384044));
#204438=CARTESIAN_POINT('Ctrl Pts',(-60.5367349311551,-23.0827722988975,
-212.949821974785));
#204439=CARTESIAN_POINT('Ctrl Pts',(-47.3924301901722,-18.6362326223204,
-233.091564811217));
#204440=CARTESIAN_POINT('Ctrl Pts',(-49.5919089377565,-19.6336206651606,
-229.73800885476));
#204441=CARTESIAN_POINT('Ctrl Pts',(-51.7911544990196,-20.633178776548,
-226.384892671102));
#204442=CARTESIAN_POINT('Ctrl Pts',(-53.9903074147697,-21.6336083947046,
-223.031955741188));
#204443=CARTESIAN_POINT('Ctrl Pts',(-56.1894603305198,-22.6340380128611,
-219.679018811274));
#204444=CARTESIAN_POINT('Ctrl Pts',(-58.3885128958421,-23.6354079399365,
-216.326274549018));
#204445=CARTESIAN_POINT('Ctrl Pts',(-60.5875151336786,-24.637248848966,
-212.973627321642));
#204446=CARTESIAN_POINT('Ctrl Pts',(-47.5062945476757,-19.6195995248629,
-233.133241732319));
#204447=CARTESIAN_POINT('Ctrl Pts',(-49.7144600590333,-20.7098790140667,
-229.777291719128));
#204448=CARTESIAN_POINT('Ctrl Pts',(-51.9225250540634,-21.8042698865183,
-226.422628306549));
#204449=CARTESIAN_POINT('Ctrl Pts',(-54.1305210352282,-22.9002472192685,
-223.06844144768));
#204450=CARTESIAN_POINT('Ctrl Pts',(-56.3385170163929,-23.9962245520186,
-219.714254588812));
#204451=CARTESIAN_POINT('Ctrl Pts',(-58.5464456271153,-25.0939292676188,
-216.360591734734));
#204452=CARTESIAN_POINT('Ctrl Pts',(-60.7543325255676,-26.1924804157199,
-213.007179917814));
#204453=CARTESIAN_POINT('Ctrl Pts',(-47.5205275923637,-19.7425203876807,
-233.138451347457));
#204454=CARTESIAN_POINT('Ctrl Pts',(-49.7297789491929,-20.8444113076799,
-229.782202077174));
#204455=CARTESIAN_POINT('Ctrl Pts',(-51.9389463734439,-21.9506562752646,
-226.42734526098));
#204456=CARTESIAN_POINT('Ctrl Pts',(-54.1480477377855,-23.0585770723389,
-223.073002160992));
#204457=CARTESIAN_POINT('Ctrl Pts',(-56.3571491021271,-24.1664978694133,
-219.718659061004));
#204458=CARTESIAN_POINT('Ctrl Pts',(-58.5661872185244,-25.276244433579,
-216.364881382949));
#204459=CARTESIAN_POINT('Ctrl Pts',(-60.7751846995537,-26.3868843615641,
-213.011373992336));
#204460=CARTESIAN_POINT('Ctrl Pts',(-47.5360446986138,-19.8652437656123,
-233.143861532478));
#204461=CARTESIAN_POINT('Ctrl Pts',(-49.7464660141853,-20.9787779864532,
-229.787297715501));
#204462=CARTESIAN_POINT('Ctrl Pts',(-51.9568241644486,-22.0969116538416,
-226.432238588131));
#204463=CARTESIAN_POINT('Ctrl Pts',(-54.1671204241435,-23.2168106787515,
-223.077732193586));
#204464=CARTESIAN_POINT('Ctrl Pts',(-56.3774166838384,-24.3367097036616,
-219.723225799041));
#204465=CARTESIAN_POINT('Ctrl Pts',(-58.5876552513978,-25.4585332815125,
-216.369328422911));
#204466=CARTESIAN_POINT('Ctrl Pts',(-60.7978548655404,-26.5812970894946,
-213.015721487035));
#204467=CARTESIAN_POINT('Ctrl Pts',(-47.552840900575,-19.9877453892004,
-233.149480158731));
#204468=CARTESIAN_POINT('Ctrl Pts',(-49.764518524335,-21.1129544864435,
-229.792585026173));
#204469=CARTESIAN_POINT('Ctrl Pts',(-51.976158307113,-22.2430122546447,
-226.437313966284));
#204470=CARTESIAN_POINT('Ctrl Pts',(-54.1877416326195,-23.3749253815565,
-223.082636672215));
#204471=CARTESIAN_POINT('Ctrl Pts',(-56.399324958126,-24.5068385084684,
-219.727959378147));
#204472=CARTESIAN_POINT('Ctrl Pts',(-58.6108576613275,-25.6407757471239,
-216.373937091928));
#204473=CARTESIAN_POINT('Ctrl Pts',(-60.8223537175678,-26.7757001729515,
-213.02022637406));
#204474=CARTESIAN_POINT('Ctrl Pts',(-47.5612390015556,-20.0489962009945,
-233.152289471859));
#204475=CARTESIAN_POINT('Ctrl Pts',(-49.7735447794099,-21.1800427364387,
-229.795228681509));
#204476=CARTESIAN_POINT('Ctrl Pts',(-51.9858253784452,-22.3160625550462,
-226.43985165536));
#204477=CARTESIAN_POINT('Ctrl Pts',(-54.1980522368575,-23.453982732959,
-223.08508891153));
#204478=CARTESIAN_POINT('Ctrl Pts',(-56.4102790952697,-24.5919029108718,
-219.730326167701));
#204479=CARTESIAN_POINT('Ctrl Pts',(-58.6224588662923,-25.7318969799296,
-216.376241426438));
#204480=CARTESIAN_POINT('Ctrl Pts',(-60.8346031435815,-26.87290171468,-213.022478817573));
#204481=CARTESIAN_POINT('Ctrl Pts',(-47.5699568885701,-20.1101915733302,
-233.155150913204));
#204482=CARTESIAN_POINT('Ctrl Pts',(-49.7829124042595,-21.2470834394385,
-229.797920267832));
#204483=CARTESIAN_POINT('Ctrl Pts',(-51.9958565445205,-22.3890741581773,
-226.44243486757));
#204484=CARTESIAN_POINT('Ctrl Pts',(-54.2087499771628,-23.5330103552298,
-223.087584770755));
#204485=CARTESIAN_POINT('Ctrl Pts',(-56.421643409805,-24.6769465522823,
-219.732734673941));
#204486=CARTESIAN_POINT('Ctrl Pts',(-58.6344936689916,-25.8230066133188,
-216.378586173355));
#204487=CARTESIAN_POINT('Ctrl Pts',(-60.847309743967,-26.9701008413005,
-213.024770613288));
#204488=CARTESIAN_POINT('Ctrl Pts',(-47.5789940164766,-20.1713284656181,
-233.15806557645));
#204489=CARTESIAN_POINT('Ctrl Pts',(-49.7926211103158,-21.3140735095608,
-229.800660662664));
#204490=CARTESIAN_POINT('Ctrl Pts',(-52.0062518326129,-22.4620440746829,
-226.445064375697));
#204491=CARTESIAN_POINT('Ctrl Pts',(-54.2198352050027,-23.6120053955637,
-223.090124941524));
#204492=CARTESIAN_POINT('Ctrl Pts',(-56.4334185773924,-24.7619667164447,
-219.735185507351));
#204493=CARTESIAN_POINT('Ctrl Pts',(-58.6469630826069,-25.9141021151943,
-216.380971893111));
#204494=CARTESIAN_POINT('Ctrl Pts',(-60.8604748729077,-27.0672952246279,
-213.027102282233));
#204495=CARTESIAN_POINT('Ctrl Pts',(-47.5812532984532,-20.1866126886901,
-233.158794242262));
#204496=CARTESIAN_POINT('Ctrl Pts',(-49.7950482868299,-21.3308210270913,
-229.801345761373));
#204497=CARTESIAN_POINT('Ctrl Pts',(-52.0088506546361,-22.4802865538093,
-226.445721752729));
#204498=CARTESIAN_POINT('Ctrl Pts',(-54.2226065119627,-23.6317541556473,
-223.090759984216));
#204499=CARTESIAN_POINT('Ctrl Pts',(-56.4363623692893,-24.7832217574852,
-219.735798215704));
#204500=CARTESIAN_POINT('Ctrl Pts',(-58.6500804360107,-25.9368759906632,
-216.38156832305));
#204501=CARTESIAN_POINT('Ctrl Pts',(-60.8637661551428,-27.0915938204597,
-213.027685199469));
#204502=CARTESIAN_POINT('Ctrl Pts',(-47.5835325332411,-20.2018932567312,
-233.159526234808));
#204503=CARTESIAN_POINT('Ctrl Pts',(-49.7974967810963,-21.3475653800119,
-229.802033910872));
#204504=CARTESIAN_POINT('Ctrl Pts',(-52.011472234427,-22.4985264274573,
-226.446382023462));
#204505=CARTESIAN_POINT('Ctrl Pts',(-54.2254020370079,-23.6515008792884,
-223.091397796547));
#204506=CARTESIAN_POINT('Ctrl Pts',(-56.4393318395888,-24.8044753311196,
-219.73641356963));
#204507=CARTESIAN_POINT('Ctrl Pts',(-58.6532249526671,-25.9596489828307,
-216.382167313891));
#204508=CARTESIAN_POINT('Ctrl Pts',(-60.8670860954703,-27.1158921197517,
-213.028270608861));
#204509=CARTESIAN_POINT('Ctrl Pts',(-47.5858317128383,-20.2171701221733,
-233.160261571908));
#204510=CARTESIAN_POINT('Ctrl Pts',(-49.7999665889626,-21.3643065199923,
-229.802725125393));
#204511=CARTESIAN_POINT('Ctrl Pts',(-52.0141165726974,-22.5167636487862,
-226.447045200389));
#204512=CARTESIAN_POINT('Ctrl Pts',(-54.22822178586,-23.6712455217665,-223.092038389655));
#204513=CARTESIAN_POINT('Ctrl Pts',(-56.4423269990226,-24.8257273947467,
-219.737031578921));
#204514=CARTESIAN_POINT('Ctrl Pts',(-58.6563966485487,-25.9824210519681,
-216.382768874591));
#204515=CARTESIAN_POINT('Ctrl Pts',(-60.8704347151645,-27.140190085957,
-213.028858518708));
#204516=CARTESIAN_POINT('Ctrl Pts',(-47.5869813026369,-20.2248085548944,
-233.160629240458));
#204517=CARTESIAN_POINT('Ctrl Pts',(-49.8012014928958,-21.3726770899824,
-229.803070732654));
#204518=CARTESIAN_POINT('Ctrl Pts',(-52.0154387418326,-22.5258822594507,
-226.447376788852));
#204519=CARTESIAN_POINT('Ctrl Pts',(-54.2296316602861,-23.6811178430054,
-223.092358686209));
#204520=CARTESIAN_POINT('Ctrl Pts',(-56.4438245787395,-24.8363534265602,
-219.737340583566));
#204521=CARTESIAN_POINT('Ctrl Pts',(-58.6579824964894,-25.9938070865368,
-216.383069654941));
#204522=CARTESIAN_POINT('Ctrl Pts',(-60.8721090250117,-27.1523390690596,
-213.029152473631));
#204523=CARTESIAN_POINT('Ctrl Pts',(-47.5882003780178,-20.2289848114109,
-233.159841710208));
#204524=CARTESIAN_POINT('Ctrl Pts',(-49.8025239788324,-21.3777302901863,
-229.80232330561));
#204525=CARTESIAN_POINT('Ctrl Pts',(-52.016858339954,-22.5317814550976,
-226.446655795734));
#204526=CARTESIAN_POINT('Ctrl Pts',(-54.2311466126926,-23.6878505920434,
-223.091659114758));
#204527=CARTESIAN_POINT('Ctrl Pts',(-56.4454348854312,-24.8439197289892,
-219.736662433782));
#204528=CARTESIAN_POINT('Ctrl Pts',(-58.6596860711528,-26.0021935301855,
-216.382407404553));
#204529=CARTESIAN_POINT('Ctrl Pts',(-60.8739050401878,-27.1615389533073,
-213.028503498334));
#204530=CARTESIAN_POINT('Ctrl Pts',(-47.5893856011509,-20.2345630906963,
-233.159521876246));
#204531=CARTESIAN_POINT('Ctrl Pts',(-49.8038047411002,-21.384127338717,
-229.802018401381));
#204532=CARTESIAN_POINT('Ctrl Pts',(-52.0182317111982,-22.5389852621582,
-226.446360938398));
#204533=CARTESIAN_POINT('Ctrl Pts',(-54.2326117356213,-23.695856045427,
-223.091372426396));
#204534=CARTESIAN_POINT('Ctrl Pts',(-56.4469917600444,-24.8527268286958,
-219.736383914393));
#204535=CARTESIAN_POINT('Ctrl Pts',(-58.661333695373,-26.0117968360436,
-216.38213501004));
#204536=CARTESIAN_POINT('Ctrl Pts',(-60.8756430054541,-27.1719356700459,
-213.028236234081));
#204537=CARTESIAN_POINT('Ctrl Pts',(-47.590570824284,-20.2401413699817,
-233.159202042285));
#204538=CARTESIAN_POINT('Ctrl Pts',(-49.805085503368,-21.3905243872477,
-229.801713497152));
#204539=CARTESIAN_POINT('Ctrl Pts',(-52.0196050824424,-22.5461890692189,
-226.44606608106));
#204540=CARTESIAN_POINT('Ctrl Pts',(-54.23407685855,-23.7038614988106,-223.091085738033));
#204541=CARTESIAN_POINT('Ctrl Pts',(-56.4485486346576,-24.8615339284022,
-219.736105395004));
#204542=CARTESIAN_POINT('Ctrl Pts',(-58.6629813195933,-26.0214001419017,
-216.381862615529));
#204543=CARTESIAN_POINT('Ctrl Pts',(-60.8773809707203,-27.1823323867845,
-213.027968969829));
#204544=CARTESIAN_POINT('Ctrl Pts',(-47.5917520994765,-20.2457201234783,
-233.158882308471));
#204545=CARTESIAN_POINT('Ctrl Pts',(-49.8063619385521,-21.3969222170114,
-229.801408683416));
#204546=CARTESIAN_POINT('Ctrl Pts',(-52.0209737682581,-22.553393946814,
-226.445771304011));
#204547=CARTESIAN_POINT('Ctrl Pts',(-54.235536945469,-23.7118683113933,
-223.090799121214));
#204548=CARTESIAN_POINT('Ctrl Pts',(-56.4501001226798,-24.8703426759725,
-219.735826938416));
#204549=CARTESIAN_POINT('Ctrl Pts',(-58.6646232151106,-26.0310053820113,
-216.38159027621));
#204550=CARTESIAN_POINT('Ctrl Pts',(-60.8791128691258,-27.1927313248522,
-213.027701754131));
#204551=CARTESIAN_POINT('Ctrl Pts',(-47.592929427391,-20.2512993504693,
-233.15856267521));
#204552=CARTESIAN_POINT('Ctrl Pts',(-49.8076340463092,-21.4033208239495,
-229.801103960199));
#204553=CARTESIAN_POINT('Ctrl Pts',(-52.0223377673611,-22.5605998880764,
-226.445476607082));
#204554=CARTESIAN_POINT('Ctrl Pts',(-54.2369919941413,-23.7198764736633,
-223.090512575624));
#204555=CARTESIAN_POINT('Ctrl Pts',(-56.4516462209215,-24.8791530592503,
-219.735548544168));
#204556=CARTESIAN_POINT('Ctrl Pts',(-58.6662593777807,-26.0406125417595,
-216.381317991529));
#204557=CARTESIAN_POINT('Ctrl Pts',(-60.880838695562,-27.2031324672545,
-213.027434586363));
#204558=CARTESIAN_POINT('Ctrl Pts',(-47.5976387390489,-20.2736162584332,
-233.157284142165));
#204559=CARTESIAN_POINT('Ctrl Pts',(-49.8127224773379,-21.4289152517019,
-229.799885067328));
#204560=CARTESIAN_POINT('Ctrl Pts',(-52.0277937637733,-22.5894236531258,
-226.444297819366));
#204561=CARTESIAN_POINT('Ctrl Pts',(-54.2428121888309,-23.7519091227437,
-223.089366393269));
#204562=CARTESIAN_POINT('Ctrl Pts',(-56.4578306138885,-24.9143945923615,
-219.734434967173));
#204563=CARTESIAN_POINT('Ctrl Pts',(-58.6728040284611,-26.079041180752,
-216.380228852809));
#204564=CARTESIAN_POINT('Ctrl Pts',(-60.8877420013067,-27.2447370368634,
-213.02636591529));
#204565=CARTESIAN_POINT('Ctrl Pts',(-47.6022848944595,-20.2959407423872,
-233.156007217897));
#204566=CARTESIAN_POINT('Ctrl Pts',(-49.8177416695991,-21.4545221142991,
-229.798667622657));
#204567=CARTESIAN_POINT('Ctrl Pts',(-52.0331747727777,-22.6182644368655,
-226.443120313462));
#204568=CARTESIAN_POINT('Ctrl Pts',(-54.2485517715197,-23.7839633668058,
-223.088221350469));
#204569=CARTESIAN_POINT('Ctrl Pts',(-56.4639287702618,-24.949662296746,
-219.733322387475));
#204570=CARTESIAN_POINT('Ctrl Pts',(-58.6792569534495,-26.1175005338857,
-216.379140588177));
#204571=CARTESIAN_POINT('Ctrl Pts',(-60.8945481553838,-27.2863768757278,
-213.025298010954));
#204572=CARTESIAN_POINT('Ctrl Pts',(-47.6068679344032,-20.3182727557442,
-233.154731928786));
#204573=CARTESIAN_POINT('Ctrl Pts',(-49.8226916006283,-21.4801411515154,
-229.797451628545));
#204574=CARTESIAN_POINT('Ctrl Pts',(-52.0384807122269,-22.6471217996642,
-226.441944079533));
#204575=CARTESIAN_POINT('Ctrl Pts',(-54.254210599501,-23.8160385972306,
-223.087077428057));
#204576=CARTESIAN_POINT('Ctrl Pts',(-56.4699404867752,-24.984955394797,
-219.732210776581));
#204577=CARTESIAN_POINT('Ctrl Pts',(-58.6856178886063,-26.1559896665116,
-216.378053163374));
#204578=CARTESIAN_POINT('Ctrl Pts',(-60.9012568321316,-27.3280508969457,
-213.024230834597));
#204579=CARTESIAN_POINT('Ctrl Pts',(-47.6435322539531,-20.4969288626005,
-233.144529615889));
#204580=CARTESIAN_POINT('Ctrl Pts',(-49.8622910488621,-21.6850934492459,
-229.78772367565));
#204581=CARTESIAN_POINT('Ctrl Pts',(-52.0809282278205,-22.8779807020543,
-226.432534208105));
#204582=CARTESIAN_POINT('Ctrl Pts',(-54.2994812233516,-24.0726404406297,
-223.077926048768));
#204583=CARTESIAN_POINT('Ctrl Pts',(-56.5180342188827,-25.2673001792052,
-219.723317889431));
#204584=CARTESIAN_POINT('Ctrl Pts',(-58.7365053698609,-26.4639027275198,
-216.369353764958));
#204585=CARTESIAN_POINT('Ctrl Pts',(-60.9549262461142,-27.6614430666891,
-213.015693423744));
#204586=CARTESIAN_POINT('Ctrl Pts',(-47.6761580143262,-20.6760672828885,
-233.134431726961));
#204587=CARTESIAN_POINT('Ctrl Pts',(-49.8974580357697,-21.890825164949,
-229.77808818943));
#204588=CARTESIAN_POINT('Ctrl Pts',(-52.11857127794,-23.1099007208212,-226.423205300924));
#204589=CARTESIAN_POINT('Ctrl Pts',(-54.3395833259005,-24.3305853285644,
-223.068845880567));
#204590=CARTESIAN_POINT('Ctrl Pts',(-56.5605953738609,-25.5512699363075,
-219.714486460211));
#204591=CARTESIAN_POINT('Ctrl Pts',(-58.7815049542864,-26.7737213502237,
-216.36070754227));
#204592=CARTESIAN_POINT('Ctrl Pts',(-61.0023564697282,-27.9970224992499,
-213.007202010553));
#204593=CARTESIAN_POINT('Ctrl Pts',(-47.7047603197491,-20.8556613435138,
-233.124453388251));
#204594=CARTESIAN_POINT('Ctrl Pts',(-49.9281792692869,-22.0972013968281,
-229.768548954079));
#204595=CARTESIAN_POINT('Ctrl Pts',(-52.1513679132233,-23.3426563590316,
-226.413955402434));
#204596=CARTESIAN_POINT('Ctrl Pts',(-54.374445390284,-24.58956219214,-223.059830549548));
#204597=CARTESIAN_POINT('Ctrl Pts',(-56.5975228673448,-25.8364680252484,
-219.705705696663));
#204598=CARTESIAN_POINT('Ctrl Pts',(-58.8204852380101,-27.0849692159872,
-216.352100946617));
#204599=CARTESIAN_POINT('Ctrl Pts',(-61.0433852523227,-28.3342355002131,
-212.998740881412));
#204600=CARTESIAN_POINT('Ctrl Pts',(-47.761964930595,-21.2148494647643,
-233.104496710832));
#204601=CARTESIAN_POINT('Ctrl Pts',(-49.9896217363213,-22.5099538605863,
-229.749470483377));
#204602=CARTESIAN_POINT('Ctrl Pts',(-52.2169611837896,-23.8081676354522,
-226.395455605453));
#204603=CARTESIAN_POINT('Ctrl Pts',(-54.4441695190511,-25.1075159192911,
-223.041799887511));
#204604=CARTESIAN_POINT('Ctrl Pts',(-56.6713778543125,-26.4068642031302,
-219.688144169568));
#204605=CARTESIAN_POINT('Ctrl Pts',(-58.8984458054575,-27.7074649475142,
-216.33488775531));
#204606=CARTESIAN_POINT('Ctrl Pts',(-61.1254428175118,-29.0086615021396,
-212.981818623129));
#204607=CARTESIAN_POINT('Ctrl Pts',(-47.8030826102193,-21.5759569839245,
-233.085053373718));
#204608=CARTESIAN_POINT('Ctrl Pts',(-50.0332812842976,-22.9253020461421,
-229.730786405659));
#204609=CARTESIAN_POINT('Ctrl Pts',(-52.2631570285769,-24.2769902935286,
-226.377264845526));
#204610=CARTESIAN_POINT('Ctrl Pts',(-54.4929077000272,-25.6295283315933,
-223.024008347048));
#204611=CARTESIAN_POINT('Ctrl Pts',(-56.7226583714774,-26.9820663696581,
-219.67075184857));
#204612=CARTESIAN_POINT('Ctrl Pts',(-58.9522730259992,-28.3355440479673,
-216.317789947423));
#204613=CARTESIAN_POINT('Ctrl Pts',(-61.1818210021897,-29.6894673923576,
-212.964966336897));
#204614=CARTESIAN_POINT('Ctrl Pts',(-47.8281547001989,-21.9381226823642,
-233.066054879848));
#204615=CARTESIAN_POINT('Ctrl Pts',(-50.0590295861697,-23.3420565686501,
-229.712518150776));
#204616=CARTESIAN_POINT('Ctrl Pts',(-52.2896542767201,-24.7475525298228,
-226.359471317301));
#204617=CARTESIAN_POINT('Ctrl Pts',(-54.5201844975327,-26.1536136226082,
-223.006599089445));
#204618=CARTESIAN_POINT('Ctrl Pts',(-56.7507147183453,-27.5596747153937,
-219.653726861588));
#204619=CARTESIAN_POINT('Ctrl Pts',(-58.9811415508881,-28.9663610919618,
-216.301048580499));
#204620=CARTESIAN_POINT('Ctrl Pts',(-61.2115183316506,-30.3733436736124,
-212.948461459071));
#204621=CARTESIAN_POINT('Ctrl Pts',(-47.878298880158,-22.6624540792437,
-233.028057892109));
#204622=CARTESIAN_POINT('Ctrl Pts',(-50.1105261899139,-24.1755656136661,
-229.675981641008));
#204623=CARTESIAN_POINT('Ctrl Pts',(-52.3426487730065,-25.6886770024113,
-226.323884260853));
#204624=CARTESIAN_POINT('Ctrl Pts',(-54.5747380925437,-27.201784204638,
-222.971780574238));
#204625=CARTESIAN_POINT('Ctrl Pts',(-56.8068274120809,-28.7148914068648,
-219.619676887624));
#204626=CARTESIAN_POINT('Ctrl Pts',(-59.0388786006661,-30.2279951799507,
-216.267565846653));
#204627=CARTESIAN_POINT('Ctrl Pts',(-61.2709129905723,-31.7410962361218,
-212.915451703421));
#204628=CARTESIAN_POINT('Ctrl Pts',(-47.8643060007033,-23.3916852678342,
-232.992031101241));
#204629=CARTESIAN_POINT('Ctrl Pts',(-50.090369934904,-25.0147380524944,
-229.641119166754));
#204630=CARTESIAN_POINT('Ctrl Pts',(-52.3167608689203,-26.6363742930146,
-226.289781396988));
#204631=CARTESIAN_POINT('Ctrl Pts',(-54.5432642950053,-28.2575096926779,
-222.938292603557));
#204632=CARTESIAN_POINT('Ctrl Pts',(-56.7697677210903,-29.8786450923411,
-219.586803810126));
#204633=CARTESIAN_POINT('Ctrl Pts',(-58.9963973187644,-31.499223086313,
-216.235147117033));
#204634=CARTESIAN_POINT('Ctrl Pts',(-61.2230851874141,-33.1195404004377,
-212.883411876817));
#204635=CARTESIAN_POINT('Ctrl Pts',(-47.7843348584855,-24.1202237497555,
-232.95800139794));
#204636=CARTESIAN_POINT('Ctrl Pts',(-49.99728150262,-25.8497978524297,-229.608138122646));
#204637=CARTESIAN_POINT('Ctrl Pts',(-52.2112045262045,-27.5766829623168,
-226.257539270556));
#204638=CARTESIAN_POINT('Ctrl Pts',(-54.4254782083431,-29.3025655601605,
-222.906657351959));
#204639=CARTESIAN_POINT('Ctrl Pts',(-56.6397518904817,-31.0284481580042,
-219.555775433364));
#204640=CARTESIAN_POINT('Ctrl Pts',(-58.8544142415175,-32.7532300084283,
-216.204585123186));
#204641=CARTESIAN_POINT('Ctrl Pts',(-61.0692598838066,-34.4774822060492,
-212.853243959114));
#204642=CARTESIAN_POINT('Ctrl Pts',(-47.764342072931,-24.3023583702358,
-232.949493972115));
#204643=CARTESIAN_POINT('Ctrl Pts',(-49.974009394549,-26.0585628024136,
-229.599892861619));
#204644=CARTESIAN_POINT('Ctrl Pts',(-52.1848154405255,-27.8117601296424,
-226.249478738948));
#204645=CARTESIAN_POINT('Ctrl Pts',(-54.3960316866775,-29.5638295270311,
-222.898748539061));
#204646=CARTESIAN_POINT('Ctrl Pts',(-56.6072479328295,-31.3158989244199,
-219.548018339173));
#204647=CARTESIAN_POINT('Ctrl Pts',(-58.8189184722057,-33.0667317389572,
-216.196944624725));
#204648=CARTESIAN_POINT('Ctrl Pts',(-61.0308035579046,-34.8169676574521,
-212.845701979688));
#204649=CARTESIAN_POINT('Ctrl Pts',(-47.740213651375,-24.4844399226315,
-232.941108585445));
#204650=CARTESIAN_POINT('Ctrl Pts',(-49.9461781517511,-26.2670695016037,
-229.591763145452));
#204651=CARTESIAN_POINT('Ctrl Pts',(-52.1534586043331,-28.0463810912831,
-226.241533050557));
#204652=CARTESIAN_POINT('Ctrl Pts',(-54.3612152314905,-29.8244384178816,
-222.890954611672));
#204653=CARTESIAN_POINT('Ctrl Pts',(-56.5689718586478,-31.6024957444801,
-219.540376172787));
#204654=CARTESIAN_POINT('Ctrl Pts',(-58.7772552102583,-33.379180627117,
-216.189420287308));
#204655=CARTESIAN_POINT('Ctrl Pts',(-60.9857878512938,-35.1552003357181,
-212.838277543654));
#204656=CARTESIAN_POINT('Ctrl Pts',(-47.7118765658424,-24.6664222949089,
-232.932859181476));
#204657=CARTESIAN_POINT('Ctrl Pts',(-49.9137627052303,-26.4751698404963,
-229.583753063685));
#204658=CARTESIAN_POINT('Ctrl Pts',(-52.1171498878757,-28.280309601158,
-226.233700065929));
#204659=CARTESIAN_POINT('Ctrl Pts',(-54.321084090016,-30.084072222256,-222.883268552734));
#204660=CARTESIAN_POINT('Ctrl Pts',(-56.5250182921564,-31.887834843354,
-219.53283703954));
#204661=CARTESIAN_POINT('Ctrl Pts',(-58.7295564557497,-33.6900941117383,
-216.181996801466));
#204662=CARTESIAN_POINT('Ctrl Pts',(-60.9343814743951,-35.4916209740569,
-212.830952580145));
#204663=CARTESIAN_POINT('Ctrl Pts',(-47.7047922944592,-24.7119178879782,
-232.930796830484));
#204664=CARTESIAN_POINT('Ctrl Pts',(-49.9056588436001,-26.5271949252194,
-229.581750543243));
#204665=CARTESIAN_POINT('Ctrl Pts',(-52.1080727087613,-28.3387917286268,
-226.231741819771));
#204666=CARTESIAN_POINT('Ctrl Pts',(-54.3110513046474,-30.1489806733496,
-222.881347038));
#204667=CARTESIAN_POINT('Ctrl Pts',(-56.5140299005335,-31.9591696180724,
-219.530952256228));
#204668=CARTESIAN_POINT('Ctrl Pts',(-58.7176317671225,-33.7678224828936,
-216.180140930006));
#204669=CARTESIAN_POINT('Ctrl Pts',(-60.9215298801705,-35.5757261336416,
-212.829121339267));
#204670=CARTESIAN_POINT('Ctrl Pts',(-47.6974449417632,-24.7574072627311,
-232.928742990504));
#204671=CARTESIAN_POINT('Ctrl Pts',(-49.8972684550162,-26.5791946079747,
-229.579755520635));
#204672=CARTESIAN_POINT('Ctrl Pts',(-52.0986860379256,-28.3972305774635,
-226.229790640633));
#204673=CARTESIAN_POINT('Ctrl Pts',(-54.3006863636687,-30.2138281843841,
-222.879432289762));
#204674=CARTESIAN_POINT('Ctrl Pts',(-56.5026866894118,-32.0304257913048,
-219.529073938891));
#204675=CARTESIAN_POINT('Ctrl Pts',(-58.705329891559,-33.8454548987401,
-216.178291388644));
#204676=CARTESIAN_POINT('Ctrl Pts',(-60.9082789063849,-35.6597180491639,
-212.827296342558));
#204677=CARTESIAN_POINT('Ctrl Pts',(-47.6898332885707,-24.8028896565292,
-232.926697902178));
#204678=CARTESIAN_POINT('Ctrl Pts',(-49.8885911188174,-26.6311665651389,
-229.577768100455));
#204679=CARTESIAN_POINT('Ctrl Pts',(-52.0889901241519,-28.455622455455,
-226.227846540711));
#204680=CARTESIAN_POINT('Ctrl Pts',(-54.2899901539046,-30.2786097609959,
-222.877524247479));
#204681=CARTESIAN_POINT('Ctrl Pts',(-56.4909901836572,-32.1015970665369,
-219.527201954246));
#204682=CARTESIAN_POINT('Ctrl Pts',(-58.6926529531334,-33.9229838341469,
-216.176447991634));
#204683=CARTESIAN_POINT('Ctrl Pts',(-60.8946312627443,-35.7435879987355,
-212.825477361568));
#204684=CARTESIAN_POINT('Ctrl Pts',(-47.6860274619745,-24.8256308534282,
-232.925675358015));
#204685=CARTESIAN_POINT('Ctrl Pts',(-49.8842524507179,-26.657152543721,
-229.576774390365));
#204686=CARTESIAN_POINT('Ctrl Pts',(-52.0841421672651,-28.4848183944506,
-226.22687449075));
#204687=CARTESIAN_POINT('Ctrl Pts',(-54.2846420490225,-30.3110005493018,
-222.876570226337));
#204688=CARTESIAN_POINT('Ctrl Pts',(-56.4851419307799,-32.1371827041529,
-219.526265961925));
#204689=CARTESIAN_POINT('Ctrl Pts',(-58.6863144839206,-33.9617483018504,
-216.17552629313));
#204690=CARTESIAN_POINT('Ctrl Pts',(-60.887807440924,-35.7855229735214,
-212.824567871073));
#204691=CARTESIAN_POINT('Ctrl Pts',(-47.6821555597811,-24.8483703047961,
-232.924655001894));
#204692=CARTESIAN_POINT('Ctrl Pts',(-49.8798420455288,-26.6831315908415,
-229.575782581129));
#204693=CARTESIAN_POINT('Ctrl Pts',(-52.0792168996413,-28.5140025907287,
-226.225904210874));
#204694=CARTESIAN_POINT('Ctrl Pts',(-54.2792111270821,-30.3433748540391,
-222.875617881988));
#204695=CARTESIAN_POINT('Ctrl Pts',(-56.4792053545228,-32.1727471173495,
-219.525331553101));
#204696=CARTESIAN_POINT('Ctrl Pts',(-58.6798822493665,-34.0004868995374,
-216.174606131045));
#204697=CARTESIAN_POINT('Ctrl Pts',(-60.88088445209,-35.8274274569215,-212.823659884843));
#204698=CARTESIAN_POINT('Ctrl Pts',(-47.6782174267913,-24.8711079134889,
-232.92363686464));
#204699=CARTESIAN_POINT('Ctrl Pts',(-49.8753598495424,-26.7091034156505,
-229.574792687293));
#204700=CARTESIAN_POINT('Ctrl Pts',(-52.0742143523489,-28.5431745827215,
-226.224935704284));
#204701=CARTESIAN_POINT('Ctrl Pts',(-54.2736974997456,-30.3757320511356,
-222.874667208678));
#204702=CARTESIAN_POINT('Ctrl Pts',(-56.4731806471424,-32.2082895195496,
-219.524398713072));
#204703=CARTESIAN_POINT('Ctrl Pts',(-58.6733565172052,-34.0391986871267,
-216.173687484148));
#204704=CARTESIAN_POINT('Ctrl Pts',(-60.8738626376389,-35.8693003593042,
-212.822753376317));
#204705=CARTESIAN_POINT('Ctrl Pts',(-47.6762483602964,-24.8824767178353,
-232.923127796013));
#204706=CARTESIAN_POINT('Ctrl Pts',(-49.8731187515493,-26.722089328055,
-229.574297740375));
#204707=CARTESIAN_POINT('Ctrl Pts',(-52.0717130787027,-28.557760578718,
-226.224451450989));
#204708=CARTESIAN_POINT('Ctrl Pts',(-54.2709406860775,-30.3919106496837,
-222.874191872023));
#204709=CARTESIAN_POINT('Ctrl Pts',(-56.4701682934522,-32.2260607206496,
-219.523932293058));
#204710=CARTESIAN_POINT('Ctrl Pts',(-58.6700936511245,-34.0585545809213,
-216.173228160698));
#204711=CARTESIAN_POINT('Ctrl Pts',(-60.8703517304133,-35.8902368104956,
-212.822300122054));
#204712=CARTESIAN_POINT('Ctrl Pts',(-47.6742627360736,-24.8938450614933,
-232.922619282109));
#204713=CARTESIAN_POINT('Ctrl Pts',(-49.8708597058451,-26.7350734348772,
-229.573803272322));
#204714=CARTESIAN_POINT('Ctrl Pts',(-52.069192485139,-28.5723435236424,
-226.223967641033));
#204715=CARTESIAN_POINT('Ctrl Pts',(-54.2681631960686,-30.4080849713239,
-222.873716953146));
#204716=CARTESIAN_POINT('Ctrl Pts',(-56.4671339069982,-32.2438264190054,
-219.523466265261));
#204717=CARTESIAN_POINT('Ctrl Pts',(-58.666807410665,-34.0779037721973,
-216.172769216067));
#204718=CARTESIAN_POINT('Ctrl Pts',(-60.8668161168113,-35.9111653664389,
-212.821847237238));
#204719=CARTESIAN_POINT('Ctrl Pts',(-47.6722605345507,-24.9052129322023,
-232.922111326828));
#204720=CARTESIAN_POINT('Ctrl Pts',(-49.8685827056453,-26.7480556997355,
-229.573309285042));
#204721=CARTESIAN_POINT('Ctrl Pts',(-52.0666525755381,-28.5869233597964,
-226.223484274919));
#204722=CARTESIAN_POINT('Ctrl Pts',(-54.2653650437259,-30.4242549380612,
-222.873242451443));
#204723=CARTESIAN_POINT('Ctrl Pts',(-56.4640775119137,-32.2615865163259,
-219.523000627968));
#204724=CARTESIAN_POINT('Ctrl Pts',(-58.6634978294311,-34.0972461434794,
-216.172310647723));
#204725=CARTESIAN_POINT('Ctrl Pts',(-60.8632558396737,-35.9320858909674,
-212.821394718674));
#204726=CARTESIAN_POINT('Ctrl Pts',(-47.6712594337893,-24.9108968675569,
-232.921857349187));
#204727=CARTESIAN_POINT('Ctrl Pts',(-49.8674442055454,-26.7545468321646,
-229.573062291402));
#204728=CARTESIAN_POINT('Ctrl Pts',(-52.0653826207377,-28.5942132778735,
-226.223242591862));
#204729=CARTESIAN_POINT('Ctrl Pts',(-54.2639659675545,-30.4323399214299,
-222.873005200592));
#204730=CARTESIAN_POINT('Ctrl Pts',(-56.4625493143714,-32.2704665649863,
-219.522767809321));
#204731=CARTESIAN_POINT('Ctrl Pts',(-58.6618430388141,-34.1069173291204,
-216.172081363551));
#204732=CARTESIAN_POINT('Ctrl Pts',(-60.8614757011049,-35.9425461532316,
-212.821168459392));
#204733=CARTESIAN_POINT('Ctrl Pts',(-47.6708439427048,-24.9151766736244,
-232.921223878144));
#204734=CARTESIAN_POINT('Ctrl Pts',(-49.8668624993017,-26.7596833615473,
-229.572444432014));
#204735=CARTESIAN_POINT('Ctrl Pts',(-52.064650178125,-28.6001828109265,
-226.222636553605));
#204736=CARTESIAN_POINT('Ctrl Pts',(-54.2630886768694,-30.4391324823344,
-222.872409015864));
#204737=CARTESIAN_POINT('Ctrl Pts',(-56.4615271756139,-32.2780821537422,
-219.522181478123));
#204738=CARTESIAN_POINT('Ctrl Pts',(-58.6606824811278,-34.1153452969724,
-216.171502871612));
#204739=CARTESIAN_POINT('Ctrl Pts',(-60.8601798411379,-35.9517810490386,
-212.820596670274));
#204740=CARTESIAN_POINT('Ctrl Pts',(-47.6690974499491,-24.9226147901915,
-232.921444558725));
#204741=CARTESIAN_POINT('Ctrl Pts',(-49.8650134863522,-26.7678656673941,
-229.572661252457));
#204742=CARTESIAN_POINT('Ctrl Pts',(-52.0626926881854,-28.6091201074371,
-226.222850519243));
#204743=CARTESIAN_POINT('Ctrl Pts',(-54.261020613352,-30.4488288829175,
-222.87262061773));
#204744=CARTESIAN_POINT('Ctrl Pts',(-56.4593485385187,-32.2885376583978,
-219.522390716218));
#204745=CARTESIAN_POINT('Ctrl Pts',(-58.65839093571,-34.1265643975113,-216.171710253535));
#204746=CARTESIAN_POINT('Ctrl Pts',(-60.8577743014912,-35.9637659284024,
-212.820802473134));
#204747=CARTESIAN_POINT('Ctrl Pts',(-47.6673509571934,-24.9300529067585,
-232.921665239305));
#204748=CARTESIAN_POINT('Ctrl Pts',(-49.8631644734026,-26.7760479732408,
-229.5728780729));
#204749=CARTESIAN_POINT('Ctrl Pts',(-52.0607351982457,-28.6180574039478,
-226.223064484881));
#204750=CARTESIAN_POINT('Ctrl Pts',(-54.2589525498347,-30.4585252835005,
-222.872832219598));
#204751=CARTESIAN_POINT('Ctrl Pts',(-56.4571699014236,-32.2989931630532,
-219.522599954314));
#204752=CARTESIAN_POINT('Ctrl Pts',(-58.6560993902921,-34.1377834980502,
-216.171917635457));
#204753=CARTESIAN_POINT('Ctrl Pts',(-60.8553687618446,-35.9757508077661,
-212.821008275995));
#204754=CARTESIAN_POINT('Ctrl Pts',(-47.6656092026626,-24.9374924051846,
-232.921886594377));
#204755=CARTESIAN_POINT('Ctrl Pts',(-49.8613205610057,-26.7842316103463,
-229.573095523243));
#204756=CARTESIAN_POINT('Ctrl Pts',(-52.0587831785056,-28.6269959846611,
-226.223279050959));
#204757=CARTESIAN_POINT('Ctrl Pts',(-54.2568903279106,-30.468222923408,
-222.873044397953));
#204758=CARTESIAN_POINT('Ctrl Pts',(-56.4549974773155,-32.3094498621548,
-219.522809744947));
#204759=CARTESIAN_POINT('Ctrl Pts',(-58.6538144314378,-34.1490037503303,
-216.17212555206));
#204760=CARTESIAN_POINT('Ctrl Pts',(-60.8529701831065,-35.987736797489,
-212.821214598585));
#204761=CARTESIAN_POINT('Ctrl Pts',(-47.6638721879803,-24.9449332806664,
-232.922108625287));
#204762=CARTESIAN_POINT('Ctrl Pts',(-49.8594817505659,-26.7924165735007,
-229.57331360468));
#204763=CARTESIAN_POINT('Ctrl Pts',(-52.0568366301129,-28.6359358440905,
-226.223494218563));
#204764=CARTESIAN_POINT('Ctrl Pts',(-54.2548339484627,-30.4779217969194,
-222.873257153795));
#204765=CARTESIAN_POINT('Ctrl Pts',(-56.4528312668125,-32.3199077497483,
-219.523020089027));
#204766=CARTESIAN_POINT('Ctrl Pts',(-58.6515360594894,-34.1602251482123,
-216.172334004182));
#204767=CARTESIAN_POINT('Ctrl Pts',(-60.85057856534,-35.9997238912687,-212.821421441686));
#204768=CARTESIAN_POINT('Ctrl Pts',(-47.6360799530631,-25.0639872883753,
-232.925661119858));
#204769=CARTESIAN_POINT('Ctrl Pts',(-49.8300607835295,-26.9233759839715,
-229.576802907687));
#204770=CARTESIAN_POINT('Ctrl Pts',(-52.0256918558292,-28.7789735949605,
-226.226936900208));
#204771=CARTESIAN_POINT('Ctrl Pts',(-54.2219318772968,-30.6331037731025,
-222.876661247257));
#204772=CARTESIAN_POINT('Ctrl Pts',(-56.4181718987644,-32.4872339512444,
-219.526385594307));
#204773=CARTESIAN_POINT('Ctrl Pts',(-58.6150821083144,-34.339767514325,
-216.175669238136));
#204774=CARTESIAN_POINT('Ctrl Pts',(-60.8123126810755,-36.1915173917436,
-212.824730931321));
#204775=CARTESIAN_POINT('Ctrl Pts',(-47.6095010735459,-25.1833938131447,
-232.929386557426));
#204776=CARTESIAN_POINT('Ctrl Pts',(-49.8019458805959,-27.054674855399,
-229.58045371177));
#204777=CARTESIAN_POINT('Ctrl Pts',(-51.9959477143626,-28.9223386907395,
-226.230533520487));
#204778=CARTESIAN_POINT('Ctrl Pts',(-54.1905254516978,-30.7886015464719,
-222.88021313116));
#204779=CARTESIAN_POINT('Ctrl Pts',(-56.3851031890331,-32.6548644022043,
-219.529892741831));
#204780=CARTESIAN_POINT('Ctrl Pts',(-58.5803143829409,-34.5196031508285,
-216.179141529169));
#204781=CARTESIAN_POINT('Ctrl Pts',(-60.7758287854006,-36.3835935276752,
-212.828173639481));
#204782=CARTESIAN_POINT('Ctrl Pts',(-47.5841424907316,-25.3031332383162,
-232.93329091056));
#204783=CARTESIAN_POINT('Ctrl Pts',(-49.7751430286533,-27.1862918963392,
-229.584271284343));
#204784=CARTESIAN_POINT('Ctrl Pts',(-51.9676091114587,-29.0660086976874,
-226.234288856273));
#204785=CARTESIAN_POINT('Ctrl Pts',(-54.1606184685044,-30.9443917197372,
-222.883917182185));
#204786=CARTESIAN_POINT('Ctrl Pts',(-56.3536278255502,-32.822774741787,
-219.533545508098));
#204787=CARTESIAN_POINT('Ctrl Pts',(-58.5472344262499,-34.6997069346566,
-216.182754549711));
#204788=CARTESIAN_POINT('Ctrl Pts',(-60.7411272633344,-36.5759265044021,
-212.831752983035));
#204789=CARTESIAN_POINT('Ctrl Pts',(-47.4827081594745,-25.7820909390022,
-232.948908323096));
#204790=CARTESIAN_POINT('Ctrl Pts',(-49.667931620883,-27.7127600601,-229.599541574634));
#204791=CARTESIAN_POINT('Ctrl Pts',(-51.854254699843,-29.6406887254791,
-226.249310199414));
#204792=CARTESIAN_POINT('Ctrl Pts',(-54.0409905357308,-31.5675524127984,
-222.898733386289));
#204793=CARTESIAN_POINT('Ctrl Pts',(-56.2277263716187,-33.4944161001178,
-219.548156573164));
#204794=CARTESIAN_POINT('Ctrl Pts',(-58.4149145994856,-35.4201220699693,
-216.197206631876));
#204795=CARTESIAN_POINT('Ctrl Pts',(-60.6023211750695,-37.3452584113098,
-212.84607035725));
#204796=CARTESIAN_POINT('Ctrl Pts',(-47.4007849436546,-26.2663735290611,
-232.967369843972));
#204797=CARTESIAN_POINT('Ctrl Pts',(-49.5817020458226,-28.2443177299668,
-229.617464898372));
#204798=CARTESIAN_POINT('Ctrl Pts',(-51.7633793713291,-30.2202463681864,
-226.266857669841));
#204799=CARTESIAN_POINT('Ctrl Pts',(-53.9453452831587,-32.19539073454,-222.915972481834));
#204800=CARTESIAN_POINT('Ctrl Pts',(-56.1273111949884,-34.1705351008938,
-219.565087293826));
#204801=CARTESIAN_POINT('Ctrl Pts',(-58.3095925631572,-36.1448271352898,
-216.213901211887));
#204802=CARTESIAN_POINT('Ctrl Pts',(-60.4920271624846,-38.1186994663558,
-212.862565596074));
#204803=CARTESIAN_POINT('Ctrl Pts',(-47.338918326904,-26.7547399443242,
-232.989202284253));
#204804=CARTESIAN_POINT('Ctrl Pts',(-49.5169190710851,-28.779613867576,
-229.63849750905));
#204805=CARTESIAN_POINT('Ctrl Pts',(-51.6953679974136,-30.8032553785755,
-226.287341083189));
#204806=CARTESIAN_POINT('Ctrl Pts',(-53.8739882225852,-32.826417079771,
-222.936006744139));
#204807=CARTESIAN_POINT('Ctrl Pts',(-56.0526084477568,-34.8495787809666,
-219.584672405089));
#204808=CARTESIAN_POINT('Ctrl Pts',(-58.2314156201025,-36.8722190976995,
-216.233145260744));
#204809=CARTESIAN_POINT('Ctrl Pts',(-60.4103139494413,-38.8946025877681,
-212.88152253822));
#204810=CARTESIAN_POINT('Ctrl Pts',(-47.0914518599014,-28.7082056053768,
-233.076532045377));
#204811=CARTESIAN_POINT('Ctrl Pts',(-49.2577871721353,-30.9207984180132,
-229.722627951761));
#204812=CARTESIAN_POINT('Ctrl Pts',(-51.4233225017517,-33.1352914201321,
-226.36927473658));
#204813=CARTESIAN_POINT('Ctrl Pts',(-53.588559980291,-35.3505224606949,
-223.016143793358));
#204814=CARTESIAN_POINT('Ctrl Pts',(-55.7537974588302,-37.5657535012578,
-219.663012850137));
#204815=CARTESIAN_POINT('Ctrl Pts',(-57.9187078478837,-39.7817869473385,
-216.310121456173));
#204816=CARTESIAN_POINT('Ctrl Pts',(-60.0834610972678,-41.9982150734171,
-212.9573503068));
#204817=CARTESIAN_POINT('Ctrl Pts',(-47.1654872359782,-30.7268333335968,
-233.215238694904));
#204818=CARTESIAN_POINT('Ctrl Pts',(-49.3424661286879,-33.1216582244425,
-229.854296748355));
#204819=CARTESIAN_POINT('Ctrl Pts',(-51.5175746565146,-35.5225299367126,
-226.496223095384));
#204820=CARTESIAN_POINT('Ctrl Pts',(-53.691970049721,-37.9257105515243,
-223.139241204672));
#204821=CARTESIAN_POINT('Ctrl Pts',(-55.8663654429275,-40.3288911663362,
-219.782259313959));
#204822=CARTESIAN_POINT('Ctrl Pts',(-58.0399820141948,-42.7345941518082,
-216.426471773175));
#204823=CARTESIAN_POINT('Ctrl Pts',(-60.2132186858487,-45.1415311212291,
-213.071269036894));
#204824=CARTESIAN_POINT('Ctrl Pts',(-47.6009947863409,-32.6895605159758,
-233.446187702606));
#204825=CARTESIAN_POINT('Ctrl Pts',(-49.8025157165519,-35.2628848633458,
-230.069700789871));
#204826=CARTESIAN_POINT('Ctrl Pts',(-52.004194845104,-37.8467163541935,
-226.701486649479));
#204827=CARTESIAN_POINT('Ctrl Pts',(-54.2056301169259,-40.4346768564372,
-223.336322656971));
#204828=CARTESIAN_POINT('Ctrl Pts',(-56.4070653887478,-43.0226373586808,
-219.971158664462));
#204829=CARTESIAN_POINT('Ctrl Pts',(-58.6083138625641,-45.6150709680905,
-216.609349785985));
#204830=CARTESIAN_POINT('Ctrl Pts',(-60.8093841578956,-48.2097095522884,
-213.249138279223));
#204831=CARTESIAN_POINT('',(-47.7643893940416,6.45775162350445,-232.249941470498));
#204832=CARTESIAN_POINT('Ctrl Pts',(-47.7643209769699,6.45773201240538,
-232.25005));
#204833=CARTESIAN_POINT('Ctrl Pts',(-47.742487483556,6.0248506060618,-232.25005));
#204834=CARTESIAN_POINT('Ctrl Pts',(-47.7367469535682,5.59139851916973,
-232.250049999992));
#204835=CARTESIAN_POINT('Ctrl Pts',(-47.7578535444487,4.72659631822721,
-232.250049999992));
#204836=CARTESIAN_POINT('Ctrl Pts',(-47.7845553907336,4.29572876651442,
-232.25005));
#204837=CARTESIAN_POINT('Ctrl Pts',(-47.8275275119679,3.86645886896242,
-232.25005));
#204838=CARTESIAN_POINT('Ctrl Pts',(-47.7644582781562,6.45775343049303,
-232.249941470498));
#204839=CARTESIAN_POINT('Ctrl Pts',(-47.7644427531638,6.45834525788562,
-232.249977646999));
#204840=CARTESIAN_POINT('Ctrl Pts',(-47.7644272274041,6.45893708525808,
-232.2500138235));
#204841=CARTESIAN_POINT('Ctrl Pts',(-47.7644117008771,6.45952891261041,
-232.25005));
#204842=CARTESIAN_POINT('',(-47.7598796740376,-29.6330550718714,-232.249824579447));
#204843=CARTESIAN_POINT('Ctrl Pts',(-47.7600215784967,-29.6330588292648,
-232.249824579447));
#204844=CARTESIAN_POINT('Ctrl Pts',(-47.7599867923538,-29.6343725881289,
-232.249899719632));
#204845=CARTESIAN_POINT('Ctrl Pts',(-47.7599520024297,-29.6356863468928,
-232.249974859816));
#204846=CARTESIAN_POINT('Ctrl Pts',(-47.7599172087244,-29.6370001055566,
-232.25005));
#204847=CARTESIAN_POINT('Ctrl Pts',(-47.8203127214913,-27.1915604688604,
-232.25005));
#204848=CARTESIAN_POINT('Ctrl Pts',(-47.7818352998325,-27.5956825746322,
-232.25005));
#204849=CARTESIAN_POINT('Ctrl Pts',(-47.7575670812008,-28.0014343001242,
-232.250050000008));
#204850=CARTESIAN_POINT('Ctrl Pts',(-47.7373322719693,-28.8165134987483,
-232.250050000008));
#204851=CARTESIAN_POINT('Ctrl Pts',(-47.7414965389119,-29.2249682525368,
-232.25005));
#204852=CARTESIAN_POINT('Ctrl Pts',(-47.759738683675,-29.6330167920719,
-232.25005));
#204853=CARTESIAN_POINT('Ctrl Pts',(-47.9849458443842,-16.0452823276962,
-232.25005));
#204854=CARTESIAN_POINT('Ctrl Pts',(-47.9462873275331,-16.4877634160273,
-232.25005));
#204855=CARTESIAN_POINT('Ctrl Pts',(-47.9250450211594,-16.9313786818294,
-232.250050000001));
#204856=CARTESIAN_POINT('Ctrl Pts',(-47.9174315533184,-17.8216219782253,
-232.250050000001));
#204857=CARTESIAN_POINT('Ctrl Pts',(-47.9311272415885,-18.2671771560637,
-232.25005));
#204858=CARTESIAN_POINT('Ctrl Pts',(-47.9621131582323,-18.7116122816628,
-232.25005));
#204859=CARTESIAN_POINT('Ctrl Pts',(-47.9644369065268,-4.51936300780383,
-232.25005));
#204860=CARTESIAN_POINT('Ctrl Pts',(-47.9319477065125,-4.97119967391103,
-232.25005));
#204861=CARTESIAN_POINT('Ctrl Pts',(-47.9174771946989,-5.42425649476983,
-232.25005));
#204862=CARTESIAN_POINT('Ctrl Pts',(-47.9248943561099,-6.33010700446719,
-232.25005));
#204863=CARTESIAN_POINT('Ctrl Pts',(-47.9467635146194,-6.78180681201324,
-232.25005));
#204864=CARTESIAN_POINT('Ctrl Pts',(-47.9866861404267,-7.23226624733626,
-232.25005));
#204865=CARTESIAN_POINT('Origin',(-48.1334350484927,-61.7961505568785,-218.306418983907));
#204866=CARTESIAN_POINT('Origin',(-24.838300653577,28.3971299569735,-229.35005));
#204867=CARTESIAN_POINT('',(-24.960358769668,29.3896529120211,-229.35005));
#204868=CARTESIAN_POINT('',(-24.960358769668,29.3896529120211,-229.35005));
#204869=CARTESIAN_POINT('',(-25.366775135568,29.2460791438418,-229.35005));
#204870=CARTESIAN_POINT('Origin',(-24.838300653577,28.3971299569735,-229.35005));
#204871=CARTESIAN_POINT('',(-25.366775135568,29.2460791438418,-229.35005));
#204872=CARTESIAN_POINT('Origin',(6.29739814579425E-15,-11.5034818258363,
-229.35005));
#204873=CARTESIAN_POINT('',(-39.8203148590359,15.2984308769399,-229.35005));
#204874=CARTESIAN_POINT('Origin',(6.29739814579425E-15,-11.5034818258363,
-229.35005));
#204875=CARTESIAN_POINT('',(-39.8203148590359,15.2984308769399,-229.35005));
#204876=CARTESIAN_POINT('Origin',(-38.9907249661392,14.740057695632,-229.35005));
#204877=CARTESIAN_POINT('',(-39.989972084972,14.7788545447883,-229.35005));
#204878=CARTESIAN_POINT('Origin',(-38.9907249661392,14.740057695632,-229.35005));
#204879=CARTESIAN_POINT('',(-39.989972084972,14.7788545447883,-229.35005));
#204880=CARTESIAN_POINT('Origin',(636.934816028482,-11.5034818258361,-229.35005));
#204881=CARTESIAN_POINT('Origin',(636.934816028482,-11.5034818258361,-229.35005));
#204882=CARTESIAN_POINT('Origin',(-38.9907249661392,-37.7470213473046,-229.35005));
#204883=CARTESIAN_POINT('',(-39.989972084972,-37.7858181964606,-229.35005));
#204884=CARTESIAN_POINT('',(-39.989972084972,-37.7858181964606,-229.35005));
#204885=CARTESIAN_POINT('',(-39.8203148590358,-38.3053945286125,-229.35005));
#204886=CARTESIAN_POINT('Origin',(-38.9907249661392,-37.7470213473046,-229.35005));
#204887=CARTESIAN_POINT('',(-39.8203148590358,-38.3053945286125,-229.35005));
#204888=CARTESIAN_POINT('Origin',(6.29739814579425E-15,-11.5034818258363,
-229.35005));
#204889=CARTESIAN_POINT('Origin',(6.29739814579425E-15,-11.5034818258363,
-229.35005));
#204890=CARTESIAN_POINT('Origin',(-22.9178089794592,-52.5372975341153,-229.35005));
#204891=CARTESIAN_POINT('',(-23.4054219364689,-53.410357442802,-229.35005));
#204892=CARTESIAN_POINT('',(-23.4054219364689,-53.410357442802,-229.35005));
#204893=CARTESIAN_POINT('',(-22.9516892713016,-53.5367234322311,-229.35005));
#204894=CARTESIAN_POINT('Origin',(-22.9178089794592,-52.5372975341153,-229.35005));
#204895=CARTESIAN_POINT('',(-22.9516892713016,-53.5367234322311,-229.35005));
#204896=CARTESIAN_POINT('Origin',(-48.892180948596,36.2913696007177,-218.35005));
#204897=CARTESIAN_POINT('',(-48.892180948596,32.9413696007177,-218.35005));
#204898=CARTESIAN_POINT('Origin',(-48.892180948596,36.2913696007177,-218.35005));
#204899=CARTESIAN_POINT('Origin',(-48.892180948596,36.2913696007177,-218.35005));
#204900=CARTESIAN_POINT('',(-48.892180948596,32.7753941674559,-227.858776203219));
#204901=CARTESIAN_POINT('',(-48.892180948596,32.9413696007177,-218.35005));
#204902=CARTESIAN_POINT('Origin',(-48.892180948596,36.2913696007177,-227.858776203219));
#204903=CARTESIAN_POINT('Origin',(-48.892180948596,36.2913696007177,-227.858776203219));
#204904=CARTESIAN_POINT('Origin',(-48.1334350484927,-61.7961505568785,-218.35005));
#204905=CARTESIAN_POINT('',(-48.1334350484927,-65.1461505568793,-218.35005));
#204906=CARTESIAN_POINT('Origin',(-48.1334350484927,-61.7961505568785,-218.35005));
#204907=CARTESIAN_POINT('Origin',(-48.1334350484927,-61.7961505568785,-218.35005));
#204908=CARTESIAN_POINT('',(-48.1334350484927,-65.1461505568793,-218.35005));
#204909=CARTESIAN_POINT('Origin',(-0.127542579976414,-12.8706479699377,
-228.35005));
#204910=CARTESIAN_POINT('Origin',(-55.2047656166361,-61.9923285455256,-228.35005));
#204911=CARTESIAN_POINT('Origin',(-48.1954151687739,-68.8699303295103,-228.35005));
#204912=CARTESIAN_POINT('Origin',(-0.127542579976414,-12.8706479699377,
-228.35005));
#204913=CARTESIAN_POINT('Origin',(-0.128459562639233,-12.6359082483571,
-228.35005));
#204914=CARTESIAN_POINT('Origin',(-48.892180948596,36.2913696007177,-228.35005));
#204915=CARTESIAN_POINT('Origin',(-48.6323674899383,42.9861279943057,-228.35005));
#204916=CARTESIAN_POINT('Origin',(-55.5877717798047,36.0539745652106,-228.35005));
#204917=CARTESIAN_POINT('Origin',(-0.128459562639233,-12.6359082483571,
-228.35005));
#204918=CARTESIAN_POINT('Origin',(-51.397926952212,-43.6786252257833,-167.906149834141));
#204919=CARTESIAN_POINT('Origin',(-51.7304496786285,-70.1559157828803,-167.906149834141));
#204920=CARTESIAN_POINT('Origin',(0.,-12.9675000200281,-167.906149834141));
#204921=CARTESIAN_POINT('Origin',(-51.3278340104563,17.8606293780317,-167.906149834141));
#204922=CARTESIAN_POINT('Origin',(-51.6000409161409,44.3386087195339,-167.906149834141));
#204923=CARTESIAN_POINT('Origin',(0.,-12.9675000200281,-167.906149834141));
#204924=CARTESIAN_POINT('Ctrl Pts',(-48.9714493645238,-32.4976365372143,
-239.032601429863));
#204925=CARTESIAN_POINT('Ctrl Pts',(-68.1913744168868,-58.588595799019,
-211.730755606268));
#204926=CARTESIAN_POINT('Ctrl Pts',(-47.6504140161628,-30.9809716432943,
-239.032601429841));
#204927=CARTESIAN_POINT('Ctrl Pts',(-66.0438929094031,-54.9590042342752,
-211.730755606272));
#204928=CARTESIAN_POINT('Ctrl Pts',(-46.5919797891444,-28.6187972486599,
-239.032601429843));
#204929=CARTESIAN_POINT('Ctrl Pts',(-64.3781819143446,-49.9473558418611,
-211.730755606271));
#204930=CARTESIAN_POINT('Ctrl Pts',(-46.3023719972087,-25.6595919193811,
-239.032601429843));
#204931=CARTESIAN_POINT('Ctrl Pts',(-63.9692632136205,-43.762285990858,
-211.730755606272));
#204932=CARTESIAN_POINT('Ctrl Pts',(-46.3453291243135,-24.2216224913335,
-239.032601429843));
#204933=CARTESIAN_POINT('Ctrl Pts',(-64.0706036090694,-40.7439486410264,
-211.730755606272));
#204934=CARTESIAN_POINT('Ctrl Pts',(-46.4942182564745,-23.2800468285249,
-239.032601429843));
#204935=CARTESIAN_POINT('Ctrl Pts',(-64.3397924421248,-38.7400276918009,
-211.730755606272));
#204936=CARTESIAN_POINT('Ctrl Pts',(-46.6823308842909,-22.4376754428628,
-239.032601429843));
#204937=CARTESIAN_POINT('Ctrl Pts',(-64.6771567767455,-36.9265599675944,
-211.730755606272));
#204938=CARTESIAN_POINT('Ctrl Pts',(-46.8110566085946,-21.6771313665435,
-239.032601429843));
#204939=CARTESIAN_POINT('Ctrl Pts',(-64.9159602271999,-35.2663729129392,
-211.730755606272));
#204940=CARTESIAN_POINT('Ctrl Pts',(-46.8864232013851,-20.5344885406242,
-239.032601429843));
#204941=CARTESIAN_POINT('Ctrl Pts',(-65.0656320382587,-32.7370789599851,
-211.730755606271));
#204942=CARTESIAN_POINT('Ctrl Pts',(-46.845613352649,-19.389471894004,-239.032601429842));
#204943=CARTESIAN_POINT('Ctrl Pts',(-65.0024851991802,-30.205094760215,
-211.730755606272));
#204944=CARTESIAN_POINT('Ctrl Pts',(-46.739717205202,-18.6241517464968,
-239.032601429843));
#204945=CARTESIAN_POINT('Ctrl Pts',(-64.8208630220631,-28.539554521699,
-211.730755606272));
#204946=CARTESIAN_POINT('Ctrl Pts',(-46.5950583390951,-17.8704826264274,
-239.032601429843));
#204947=CARTESIAN_POINT('Ctrl Pts',(-64.5773028603203,-26.9236650389039,
-211.730755606272));
#204948=CARTESIAN_POINT('Ctrl Pts',(-46.4891834572756,-17.1171663742141,
-239.032601429843));
#204949=CARTESIAN_POINT('Ctrl Pts',(-64.4023778490554,-25.3332388913667,
-211.730755606272));
#204950=CARTESIAN_POINT('Ctrl Pts',(-46.4453565014347,-15.9661997524868,
-239.032601429843));
#204951=CARTESIAN_POINT('Ctrl Pts',(-64.3295185111446,-22.9500603856902,
-211.730755606271));
#204952=CARTESIAN_POINT('Ctrl Pts',(-46.5193900629931,-14.8111705824743,
-239.032601429843));
#204953=CARTESIAN_POINT('Ctrl Pts',(-64.443529180052,-20.5764219053293,
-211.730755606272));
#204954=CARTESIAN_POINT('Ctrl Pts',(-46.6471770799421,-14.0499533302827,
-239.032601429843));
#204955=CARTESIAN_POINT('Ctrl Pts',(-64.6432253119956,-19.0049914961272,
-211.730755606272));
#204956=CARTESIAN_POINT('Ctrl Pts',(-46.7740202606564,-13.4754604930206,
-239.032601429843));
#204957=CARTESIAN_POINT('Ctrl Pts',(-64.8432542225078,-17.8091893041105,
-211.730755606272));
#204958=CARTESIAN_POINT('Ctrl Pts',(-46.8513541209764,-13.0740155121622,
-239.032601429843));
#204959=CARTESIAN_POINT('Ctrl Pts',(-64.9641969010104,-16.980210969671,
-211.730755606271));
#204960=CARTESIAN_POINT('Ctrl Pts',(-46.9348053643729,-12.4640324698742,
-239.032601429843));
#204961=CARTESIAN_POINT('Ctrl Pts',(-65.0935448562552,-15.7339405894364,
-211.730755606272));
#204962=CARTESIAN_POINT('Ctrl Pts',(-46.9850328086675,-11.8494593400854,
-239.032601429843));
#204963=CARTESIAN_POINT('Ctrl Pts',(-65.171164912913,-14.4848476258101,
-211.730755606272));
#204964=CARTESIAN_POINT('Ctrl Pts',(-46.9961709729731,-11.4388750292095,
-239.032601429843));
#204965=CARTESIAN_POINT('Ctrl Pts',(-65.1884659210897,-13.6502250547399,
-211.730755606272));
#204966=CARTESIAN_POINT('Ctrl Pts',(-46.9961709729731,-11.0289590886771,
-239.032601429843));
#204967=CARTESIAN_POINT('Ctrl Pts',(-65.1884659210897,-12.8146289801201,
-211.730755606272));
#204968=CARTESIAN_POINT('Ctrl Pts',(-46.9850328086376,-10.6183760206315,
-239.032601429842));
#204969=CARTESIAN_POINT('Ctrl Pts',(-65.1711648319807,-11.980003483899,
-211.730755606272));
#204970=CARTESIAN_POINT('Ctrl Pts',(-46.9348056898163,-10.0038043022318,
-239.032601429843));
#204971=CARTESIAN_POINT('Ctrl Pts',(-65.093544987819,-10.7309166067835,
-211.730755606272));
#204972=CARTESIAN_POINT('Ctrl Pts',(-46.8513537675148,-9.39381595500219,
-239.032601429843));
#204973=CARTESIAN_POINT('Ctrl Pts',(-64.9641971936048,-9.48464435696854,
-211.730755606272));
#204974=CARTESIAN_POINT('Ctrl Pts',(-46.7740202606564,-8.99237362486574,
-239.032601429843));
#204975=CARTESIAN_POINT('Ctrl Pts',(-64.8432542225078,-8.65566473074882,
-211.730755606272));
#204976=CARTESIAN_POINT('Ctrl Pts',(-46.6471770799421,-8.41788078760364,
-239.032601429843));
#204977=CARTESIAN_POINT('Ctrl Pts',(-64.6432253119957,-7.45986253873205,
-211.730755606272));
#204978=CARTESIAN_POINT('Ctrl Pts',(-46.5193900629931,-7.65666353541205,
-239.032601429843));
#204979=CARTESIAN_POINT('Ctrl Pts',(-64.4435291800518,-5.88843212952995,
-211.730755606271));
#204980=CARTESIAN_POINT('Ctrl Pts',(-46.4453565014347,-6.50163436539958,
-239.032601429843));
#204981=CARTESIAN_POINT('Ctrl Pts',(-64.3295185111447,-3.51479364916907,
-211.730755606272));
#204982=CARTESIAN_POINT('Ctrl Pts',(-46.4891834572756,-5.35066774367227,
-239.032601429843));
#204983=CARTESIAN_POINT('Ctrl Pts',(-64.4023778490553,-1.13161514349255,
-211.730755606272));
#204984=CARTESIAN_POINT('Ctrl Pts',(-46.5950583390951,-4.59735149145896,
-239.032601429843));
#204985=CARTESIAN_POINT('Ctrl Pts',(-64.5773028603203,0.458811004044723,
-211.730755606272));
#204986=CARTESIAN_POINT('Ctrl Pts',(-46.739717205202,-3.84368237138963,
-239.032601429843));
#204987=CARTESIAN_POINT('Ctrl Pts',(-64.8208630220631,2.07470048683978,
-211.730755606272));
#204988=CARTESIAN_POINT('Ctrl Pts',(-46.8456133526491,-3.07836222388228,
-239.032601429843));
#204989=CARTESIAN_POINT('Ctrl Pts',(-65.0024851991801,3.74024072535572,
-211.730755606271));
#204990=CARTESIAN_POINT('Ctrl Pts',(-46.8864232013849,-1.93334557726219,
-239.032601429842));
#204991=CARTESIAN_POINT('Ctrl Pts',(-65.0656320382587,6.27222492512578,
-211.730755606272));
#204992=CARTESIAN_POINT('Ctrl Pts',(-46.8110566085948,-0.790702751342818,
-239.032601429843));
#204993=CARTESIAN_POINT('Ctrl Pts',(-64.9159602271998,8.80151887808002,
-211.730755606272));
#204994=CARTESIAN_POINT('Ctrl Pts',(-46.6823308842909,-0.0301586750235619,
-239.032601429843));
#204995=CARTESIAN_POINT('Ctrl Pts',(-64.6771567767455,10.4617059327352,
-211.730755606272));
#204996=CARTESIAN_POINT('Ctrl Pts',(-46.4942182564745,0.812212710638539,
-239.032601429843));
#204997=CARTESIAN_POINT('Ctrl Pts',(-64.3397924421248,12.2751736569417,
-211.730755606272));
#204998=CARTESIAN_POINT('Ctrl Pts',(-46.3453291243136,1.75378837344716,
-239.032601429843));
#204999=CARTESIAN_POINT('Ctrl Pts',(-64.0706036090695,14.2790946061672,
-211.730755606272));
#205000=CARTESIAN_POINT('Ctrl Pts',(-46.3023719972086,3.1917578014948,-239.032601429843));
#205001=CARTESIAN_POINT('Ctrl Pts',(-63.9692632136205,17.2974319559987,
-211.730755606272));
#205002=CARTESIAN_POINT('Ctrl Pts',(-46.5821989973795,6.05102323992199,
-239.032601429842));
#205003=CARTESIAN_POINT('Ctrl Pts',(-64.3643716897167,23.2736162661097,
-211.730755606271));
#205004=CARTESIAN_POINT('Ctrl Pts',(-47.566430740579,8.32255892669279,-239.032601429843));
#205005=CARTESIAN_POINT('Ctrl Pts',(-65.9117879843948,28.0899407880831,
-211.730755606275));
#205006=CARTESIAN_POINT('Ctrl Pts',(-48.7769866795674,9.7996450480234,-239.032601429843));
#205007=CARTESIAN_POINT('Ctrl Pts',(-67.8755806199084,31.5767606755659,
-211.730755606259));
#205008=CARTESIAN_POINT('Origin',(6.29739814579425E-15,-11.5034818258363,
-234.75005));
#205009=CARTESIAN_POINT('',(-42.9727564520429,17.4202489659096,-234.75005));
#205010=CARTESIAN_POINT('',(-42.9727564520429,17.4202489659097,-234.75005));
#205011=CARTESIAN_POINT('',(-27.3749781671338,32.4720860539414,-234.75005));
#205012=CARTESIAN_POINT('Origin',(6.29739814579425E-15,-11.5034818258363,
-234.75005));
#205013=CARTESIAN_POINT('',(-27.3749781671338,32.4720860539414,-234.75005));
#205014=CARTESIAN_POINT('Origin',(-38.9907249661392,14.740057695632,-234.75005));
#205015=CARTESIAN_POINT('',(-43.7871111365364,14.9262825715819,-234.75005));
#205016=CARTESIAN_POINT('',(-43.7871111365364,14.9262825715819,-234.75005));
#205017=CARTESIAN_POINT('Origin',(-38.9907249661392,14.740057695632,-234.75005));
#205018=CARTESIAN_POINT('Origin',(636.934816028482,-11.5034818258361,-234.75005));
#205019=CARTESIAN_POINT('',(-43.7871111365364,-37.9332462232544,-234.75005));
#205020=CARTESIAN_POINT('',(-43.7871111365364,-37.9332462232544,-234.75005));
#205021=CARTESIAN_POINT('Origin',(636.934816028482,-11.5034818258361,-234.75005));
#205022=CARTESIAN_POINT('Origin',(-38.9907249661392,-37.7470213473046,-234.75005));
#205023=CARTESIAN_POINT('',(-42.9727564520428,-40.4272126175822,-234.75005));
#205024=CARTESIAN_POINT('',(-42.9727564520428,-40.4272126175822,-234.75005));
#205025=CARTESIAN_POINT('Origin',(-38.9907249661392,-37.7470213473046,-234.75005));
#205026=CARTESIAN_POINT('Origin',(6.29739814579425E-15,-11.5034818258363,
-234.75005));
#205027=CARTESIAN_POINT('',(-25.258351173106,-56.7279850958119,-234.75005));
#205028=CARTESIAN_POINT('',(-25.258351173106,-56.7279850958119,-234.75005));
#205029=CARTESIAN_POINT('Origin',(6.29739814579425E-15,-11.5034818258363,
-234.75005));
#205030=CARTESIAN_POINT('Origin',(-22.9178089794592,-52.5372975341153,-234.75005));
#205031=CARTESIAN_POINT('',(-23.0804343803032,-57.3345418450714,-234.75005));
#205032=CARTESIAN_POINT('',(-23.0804343803032,-57.3345418450714,-234.75005));
#205033=CARTESIAN_POINT('Origin',(-22.9178089794592,-52.5372975341153,-234.75005));
#205034=CARTESIAN_POINT('Origin',(-24.838300653577,28.3971299569735,-234.75005));
#205035=CARTESIAN_POINT('',(-25.4241796108136,33.1612401412018,-234.75005));
#205036=CARTESIAN_POINT('Origin',(-24.838300653577,28.3971299569735,-234.75005));
#205037=CARTESIAN_POINT('',(-25.4241796108136,33.1612401412018,-234.75005));
#205038=CARTESIAN_POINT('Origin',(-22.9178089794592,-52.5372975341153,-234.75005));
#205039=CARTESIAN_POINT('',(-25.8434867215177,-57.775656986236,-234.75005));
#205040=CARTESIAN_POINT('',(-25.8434867215177,-57.775656986236,-234.75005));
#205041=CARTESIAN_POINT('',(-23.121090730514,-58.5338529228103,-234.75005));
#205042=CARTESIAN_POINT('Origin',(-22.9178089794592,-52.5372975341153,-234.75005));
#205043=CARTESIAN_POINT('',(-23.121090730514,-58.5338529228103,-234.75005));
#205044=CARTESIAN_POINT('Origin',(-24.838300653577,28.3971299569735,-234.75005));
#205045=CARTESIAN_POINT('',(-25.5706493501227,34.3522676872588,-234.75005));
#205046=CARTESIAN_POINT('',(-25.5706493501227,34.3522676872588,-234.75005));
#205047=CARTESIAN_POINT('',(-28.0091475455229,33.4908250781833,-234.75005));
#205048=CARTESIAN_POINT('Origin',(-24.838300653577,28.3971299569735,-234.75005));
#205049=CARTESIAN_POINT('',(-28.0091475455229,33.4908250781833,-234.75005));
#205050=CARTESIAN_POINT('Origin',(6.29739814579425E-15,-11.5034818258363,
-234.75005));
#205051=CARTESIAN_POINT('',(-43.9682643235187,18.0902967834791,-234.75005));
#205052=CARTESIAN_POINT('Origin',(6.29739814579425E-15,-11.5034818258363,
-234.75005));
#205053=CARTESIAN_POINT('',(-43.9682643235187,18.0902967834791,-234.75005));
#205054=CARTESIAN_POINT('Origin',(-38.9907249661392,14.740057695632,-234.75005));
#205055=CARTESIAN_POINT('',(-44.9862076791357,14.9728387905693,-234.75005));
#205056=CARTESIAN_POINT('Origin',(-38.9907249661392,14.740057695632,-234.75005));
#205057=CARTESIAN_POINT('',(-44.9862076791357,14.9728387905693,-234.75005));
#205058=CARTESIAN_POINT('Origin',(636.934816028482,-11.5034818258361,-234.75005));
#205059=CARTESIAN_POINT('',(-44.9862076791357,-37.9798024422418,-234.75005));
#205060=CARTESIAN_POINT('Origin',(636.934816028482,-11.5034818258361,-234.75005));
#205061=CARTESIAN_POINT('',(-44.9862076791357,-37.9798024422418,-234.75005));
#205062=CARTESIAN_POINT('Origin',(-38.9907249661392,-37.7470213473046,-234.75005));
#205063=CARTESIAN_POINT('',(-43.9682643235187,-41.0972604351516,-234.75005));
#205064=CARTESIAN_POINT('Origin',(-38.9907249661392,-37.7470213473046,-234.75005));
#205065=CARTESIAN_POINT('',(-43.9682643235187,-41.0972604351516,-234.75005));
#205066=CARTESIAN_POINT('Origin',(6.29739814579425E-15,-11.5034818258363,
-234.75005));
#205067=CARTESIAN_POINT('Origin',(6.29739814579425E-15,-11.5034818258363,
-234.75005));
#205068=CARTESIAN_POINT('Ctrl Pts',(-48.1560655127274,-41.999274229607,
-235.35005));
#205069=CARTESIAN_POINT('Ctrl Pts',(-51.9279919200935,-48.6191351285365,
-228.68335));
#205070=CARTESIAN_POINT('Ctrl Pts',(-55.7004001286368,-55.2387363218615,
-222.01665));
#205071=CARTESIAN_POINT('Ctrl Pts',(-59.4732891526772,-61.8580772083615,
-215.34995));
#205072=CARTESIAN_POINT('Ctrl Pts',(-59.5110180429176,-61.9242706172265,
-215.283283));
#205073=CARTESIAN_POINT('Ctrl Pts',(-59.548746933158,-61.9904640260915,
-215.216616));
#205074=CARTESIAN_POINT('Ctrl Pts',(-59.5864758233984,-62.0566574349565,
-215.149949));
#205075=CARTESIAN_POINT('Ctrl Pts',(-48.2756382252007,-41.8104563330539,
-235.35005));
#205076=CARTESIAN_POINT('Ctrl Pts',(-52.0407670149459,-48.4530353242655,
-228.68335));
#205077=CARTESIAN_POINT('Ctrl Pts',(-55.8063647406712,-55.0953754160451,
-222.01665));
#205078=CARTESIAN_POINT('Ctrl Pts',(-59.57243049321,-61.7374760219621,-215.34995));
#205079=CARTESIAN_POINT('Ctrl Pts',(-59.6100911507354,-61.8038970280213,
-215.283283));
#205080=CARTESIAN_POINT('Ctrl Pts',(-59.6477518082608,-61.8703180340805,
-215.216616));
#205081=CARTESIAN_POINT('Ctrl Pts',(-59.6854124657861,-61.9367390401396,
-215.149949));
#205082=CARTESIAN_POINT('Ctrl Pts',(-48.3910626922776,-41.5900298422911,
-235.35005));
#205083=CARTESIAN_POINT('Ctrl Pts',(-52.1903238662186,-48.2138133273298,
-228.68335));
#205084=CARTESIAN_POINT('Ctrl Pts',(-55.9900266043744,-54.8373975226491,
-222.01665));
#205085=CARTESIAN_POINT('Ctrl Pts',(-59.790170143516,-61.4607818737039,
-215.34995));
#205086=CARTESIAN_POINT('Ctrl Pts',(-59.8281715789074,-61.5270157172145,
-215.283283));
#205087=CARTESIAN_POINT('Ctrl Pts',(-59.8661730142988,-61.593249560725,
-215.216616));
#205088=CARTESIAN_POINT('Ctrl Pts',(-59.9041744496902,-61.6594834042356,
-215.149949));
#205089=CARTESIAN_POINT('Ctrl Pts',(-48.5387172079886,-41.2798109487642,
-235.35005));
#205090=CARTESIAN_POINT('Ctrl Pts',(-52.4230972161915,-47.8204177760876,
-228.68335));
#205091=CARTESIAN_POINT('Ctrl Pts',(-56.3078726256209,-54.3608781649969,
-222.01665));
#205092=CARTESIAN_POINT('Ctrl Pts',(-60.1930428686919,-60.9011916159786,
-215.34995));
#205093=CARTESIAN_POINT('Ctrl Pts',(-60.2318945711226,-60.9665947504884,
-215.283283000001));
#205094=CARTESIAN_POINT('Ctrl Pts',(-60.2707462735533,-61.0319978849983,
-215.216616));
#205095=CARTESIAN_POINT('Ctrl Pts',(-60.309597975984,-61.0974010195081,
-215.149949));
#205096=CARTESIAN_POINT('Ctrl Pts',(-48.6371642419829,-41.0193984169334,
-235.35005));
#205097=CARTESIAN_POINT('Ctrl Pts',(-52.6688606290506,-47.3486283864447,
-228.68335));
#205098=CARTESIAN_POINT('Ctrl Pts',(-56.7009009677878,-53.6777576502171,
-222.01665));
#205099=CARTESIAN_POINT('Ctrl Pts',(-60.7332848610003,-60.0067857712577,
-215.34995));
#205100=CARTESIAN_POINT('Ctrl Pts',(-60.7736086999325,-60.0700760524681,
-215.283283));
#205101=CARTESIAN_POINT('Ctrl Pts',(-60.8139325388646,-60.1333663336785,
-215.216616));
#205102=CARTESIAN_POINT('Ctrl Pts',(-60.8542563777967,-60.1966566148889,
-215.149949));
#205103=CARTESIAN_POINT('Ctrl Pts',(-48.7259447515556,-40.7557132274099,
-235.35005));
#205104=CARTESIAN_POINT('Ctrl Pts',(-52.8863489207853,-46.8366038296761,
-228.68335));
#205105=CARTESIAN_POINT('Ctrl Pts',(-57.0470401243311,-52.9174317848832,
-222.016650000001));
#205106=CARTESIAN_POINT('Ctrl Pts',(-61.2080181081436,-58.9981967263321,
-215.349950000001));
#205107=CARTESIAN_POINT('Ctrl Pts',(-61.2496278879817,-59.0590043757466,
-215.283283000001));
#205108=CARTESIAN_POINT('Ctrl Pts',(-61.2912376678198,-59.1198120251611,
-215.216616));
#205109=CARTESIAN_POINT('Ctrl Pts',(-61.332847447658,-59.1806196745756,
-215.149949000001));
#205110=CARTESIAN_POINT('Ctrl Pts',(-48.7945150938174,-40.4960542325497,
-235.35005));
#205111=CARTESIAN_POINT('Ctrl Pts',(-53.0535779259056,-46.3256171279293,
-228.68335));
#205112=CARTESIAN_POINT('Ctrl Pts',(-57.3128652259323,-52.1551472055685,
-222.01665));
#205113=CARTESIAN_POINT('Ctrl Pts',(-61.572376853754,-57.9846441771198,
-215.34995));
#205114=CARTESIAN_POINT('Ctrl Pts',(-61.6149719700322,-58.0429391468354,
-215.283283));
#205115=CARTESIAN_POINT('Ctrl Pts',(-61.6575670863105,-58.1012341165509,
-215.216616));
#205116=CARTESIAN_POINT('Ctrl Pts',(-61.7001622025887,-58.1595290862664,
-215.149949));
#205117=CARTESIAN_POINT('Ctrl Pts',(-48.8537891615446,-40.2227290210882,
-235.35005));
#205118=CARTESIAN_POINT('Ctrl Pts',(-53.184407479365,-45.7839380160283,
-228.68335));
#205119=CARTESIAN_POINT('Ctrl Pts',(-57.5151818684938,-51.3451352378197,
-222.01665));
#205120=CARTESIAN_POINT('Ctrl Pts',(-61.8461122714633,-56.9063204848096,
-215.349950000001));
#205121=CARTESIAN_POINT('Ctrl Pts',(-61.889421575493,-56.9619323372794,
-215.283283000001));
#205122=CARTESIAN_POINT('Ctrl Pts',(-61.9327308795227,-57.0175441897493,
-215.216616));
#205123=CARTESIAN_POINT('Ctrl Pts',(-61.9760401835524,-57.0731560422192,
-215.149949000001));
#205124=CARTESIAN_POINT('Ctrl Pts',(-48.8993219763807,-39.9191637201113,
-235.35005));
#205125=CARTESIAN_POINT('Ctrl Pts',(-53.2653672535676,-45.2450247261708,
-228.68335));
#205126=CARTESIAN_POINT('Ctrl Pts',(-57.631494193953,-50.5708856635808,
-222.01665));
#205127=CARTESIAN_POINT('Ctrl Pts',(-61.9977027895214,-55.8967464260103,
-215.34995));
#205128=CARTESIAN_POINT('Ctrl Pts',(-62.0413648754771,-55.9500050336346,
-215.283283));
#205129=CARTESIAN_POINT('Ctrl Pts',(-62.0850269614327,-56.0032636412589,
-215.216616));
#205130=CARTESIAN_POINT('Ctrl Pts',(-62.1286890473884,-56.0565222488832,
-215.149949));
#205131=CARTESIAN_POINT('Ctrl Pts',(-48.9214109907111,-39.6817730556917,
-235.35005));
#205132=CARTESIAN_POINT('Ctrl Pts',(-53.2924626390134,-44.9053881830262,
-228.68335));
#205133=CARTESIAN_POINT('Ctrl Pts',(-57.6635282520289,-50.1290038777392,
-222.01665));
#205134=CARTESIAN_POINT('Ctrl Pts',(-62.0346078304961,-55.3526201213579,
-215.34995));
#205135=CARTESIAN_POINT('Ctrl Pts',(-62.0783186262807,-55.4048562837941,
-215.283283));
#205136=CARTESIAN_POINT('Ctrl Pts',(-62.1220294220654,-55.4570924462303,
-215.216616));
#205137=CARTESIAN_POINT('Ctrl Pts',(-62.1657402178501,-55.5093286086665,
-215.149949));
#205138=CARTESIAN_POINT('Ctrl Pts',(-48.9276804568491,-39.5283381317121,
-235.35005));
#205139=CARTESIAN_POINT('Ctrl Pts',(-53.2999213760692,-44.7204933330714,
-228.68335));
#205140=CARTESIAN_POINT('Ctrl Pts',(-57.6721622952894,-49.9126485344307,
-222.01665));
#205141=CARTESIAN_POINT('Ctrl Pts',(-62.0444032145095,-55.1048037357899,
-215.34995));
#205142=CARTESIAN_POINT('Ctrl Pts',(-62.0881256237017,-55.1567252878035,
-215.283283));
#205143=CARTESIAN_POINT('Ctrl Pts',(-62.1318480328939,-55.2086468398171,
-215.216616));
#205144=CARTESIAN_POINT('Ctrl Pts',(-62.1755704420861,-55.2605683918307,
-215.149949));
#205145=CARTESIAN_POINT('Ctrl Pts',(-48.4015825627194,-42.4301635567086,
-234.916111528175));
#205146=CARTESIAN_POINT('Ctrl Pts',(-51.8161020106309,-48.4227195017014,
-228.881144730288));
#205147=CARTESIAN_POINT('Ctrl Pts',(-55.2310162579792,-54.4150626175587,
-222.846177932402));
#205148=CARTESIAN_POINT('Ctrl Pts',(-58.6463245735781,-60.4071924582901,
-216.811211134516));
#205149=CARTESIAN_POINT('',(-55.4860418356793,-47.316570933751,-225.35));
#205150=CARTESIAN_POINT('Ctrl Pts',(-24.4127870505286,-62.4913878448826,
-235.35005));
#205151=CARTESIAN_POINT('Ctrl Pts',(-30.252655437952,-66.705065059021,-228.68335));
#205152=CARTESIAN_POINT('Ctrl Pts',(-36.0925246020991,-70.9187639624533,
-222.01665));
#205153=CARTESIAN_POINT('Ctrl Pts',(-41.9323946221365,-75.1324845521997,
-215.34995));
#205154=CARTESIAN_POINT('Ctrl Pts',(-41.990793322337,-75.1746217580972,
-215.283283));
#205155=CARTESIAN_POINT('Ctrl Pts',(-42.0491920225373,-75.2167589639946,
-215.216616));
#205156=CARTESIAN_POINT('Ctrl Pts',(-42.1075907227377,-75.2588961698921,
-215.149949));
#205157=CARTESIAN_POINT('Ctrl Pts',(-24.4238355020022,-62.4909941277675,
-235.35005));
#205158=CARTESIAN_POINT('Ctrl Pts',(-30.2665958673131,-66.7045508406744,
-228.68335));
#205159=CARTESIAN_POINT('Ctrl Pts',(-36.1093567495128,-70.9181220131437,
-222.01665));
#205160=CARTESIAN_POINT('Ctrl Pts',(-41.9521182016317,-75.1317076431822,
-215.34995));
#205161=CARTESIAN_POINT('Ctrl Pts',(-42.0105458161529,-75.1738434994826,
-215.283283));
#205162=CARTESIAN_POINT('Ctrl Pts',(-42.0689734306741,-75.215979355783,
-215.216616));
#205163=CARTESIAN_POINT('Ctrl Pts',(-42.1274010451954,-75.2581152120834,
-215.149949));
#205164=CARTESIAN_POINT('Ctrl Pts',(-24.4348839534758,-62.4906004106524,
-235.35005));
#205165=CARTESIAN_POINT('Ctrl Pts',(-30.2805362966741,-66.7040366223279,
-228.68335));
#205166=CARTESIAN_POINT('Ctrl Pts',(-36.1261888969267,-70.9174800638341,
-222.01665));
#205167=CARTESIAN_POINT('Ctrl Pts',(-41.971841781127,-75.1309307341648,
-215.34995));
#205168=CARTESIAN_POINT('Ctrl Pts',(-42.030298309969,-75.1730652408681,
-215.283283));
#205169=CARTESIAN_POINT('Ctrl Pts',(-42.088754838811,-75.2151997475714,
-215.216616));
#205170=CARTESIAN_POINT('Ctrl Pts',(-42.147211367653,-75.2573342542747,
-215.149949));
#205171=CARTESIAN_POINT('Ctrl Pts',(-24.4459324049493,-62.4902066935372,
-235.35005));
#205172=CARTESIAN_POINT('Ctrl Pts',(-30.2944767260352,-66.7035224039813,
-228.68335));
#205173=CARTESIAN_POINT('Ctrl Pts',(-36.1430210443405,-70.9168381145244,
-222.01665));
#205174=CARTESIAN_POINT('Ctrl Pts',(-41.9915653606222,-75.1301538251473,
-215.34995));
#205175=CARTESIAN_POINT('Ctrl Pts',(-42.050050803785,-75.1722869822535,
-215.283283));
#205176=CARTESIAN_POINT('Ctrl Pts',(-42.1085362469478,-75.2144201393598,
-215.216616));
#205177=CARTESIAN_POINT('Ctrl Pts',(-42.1670216901106,-75.256553296466,
-215.149949));
#205178=CARTESIAN_POINT('Ctrl Pts',(-24.5840380483692,-62.4852852295981,
-235.35005));
#205179=CARTESIAN_POINT('Ctrl Pts',(-30.4687320930486,-66.6970946746494,
-228.68335));
#205180=CARTESIAN_POINT('Ctrl Pts',(-36.3534228870133,-70.9088137481542,
-222.01665));
#205181=CARTESIAN_POINT('Ctrl Pts',(-42.2381101043121,-75.120442462429,
-215.34995));
#205182=CARTESIAN_POINT('Ctrl Pts',(-42.2969569764852,-75.1625587495718,
-215.283283));
#205183=CARTESIAN_POINT('Ctrl Pts',(-42.3558038486582,-75.2046750367146,
-215.216616));
#205184=CARTESIAN_POINT('Ctrl Pts',(-42.4146507208312,-75.2467913238573,
-215.149949));
#205185=CARTESIAN_POINT('Ctrl Pts',(-24.7878826649652,-62.4682791689329,
-235.35005));
#205186=CARTESIAN_POINT('Ctrl Pts',(-30.7858798041607,-66.6737307701245,
-228.68335));
#205187=CARTESIAN_POINT('Ctrl Pts',(-36.7838683264116,-70.8789174633912,
-222.01665));
#205188=CARTESIAN_POINT('Ctrl Pts',(-42.781847274702,-75.0838392837,-215.34995));
#205189=CARTESIAN_POINT('Ctrl Pts',(-42.8418270641849,-75.1258885019031,
-215.283283));
#205190=CARTESIAN_POINT('Ctrl Pts',(-42.9018068536678,-75.1679377201062,
-215.216616));
#205191=CARTESIAN_POINT('Ctrl Pts',(-42.9617866431507,-75.2099869383093,
-215.149949));
#205192=CARTESIAN_POINT('Ctrl Pts',(-25.048207175495,-62.4347017437458,
-235.35005));
#205193=CARTESIAN_POINT('Ctrl Pts',(-31.2985071141138,-66.6007006042259,
-228.68335));
#205194=CARTESIAN_POINT('Ctrl Pts',(-37.5487936188611,-70.7661908933779,
-222.01665));
#205195=CARTESIAN_POINT('Ctrl Pts',(-43.7990648514606,-74.9311726743249,
-215.34995));
#205196=CARTESIAN_POINT('Ctrl Pts',(-43.8615675637866,-74.9728224921344,
-215.283283));
#205197=CARTESIAN_POINT('Ctrl Pts',(-43.9240702761126,-75.0144723099439,
-215.216616));
#205198=CARTESIAN_POINT('Ctrl Pts',(-43.9865729884385,-75.0561221277533,
-215.149949));
#205199=CARTESIAN_POINT('Ctrl Pts',(-25.2812199560259,-62.390732268219,
-235.35005));
#205200=CARTESIAN_POINT('Ctrl Pts',(-31.8143029221326,-66.4798048243852,
-228.68335));
#205201=CARTESIAN_POINT('Ctrl Pts',(-38.3473707133638,-70.5681428074098,
-222.01665));
#205202=CARTESIAN_POINT('Ctrl Pts',(-44.8804206737979,-74.6557463029982,
-215.34995));
#205203=CARTESIAN_POINT('Ctrl Pts',(-44.9457511734022,-74.6966223379541,
-215.283283));
#205204=CARTESIAN_POINT('Ctrl Pts',(-45.0110816730065,-74.73749837291,-215.216616));
#205205=CARTESIAN_POINT('Ctrl Pts',(-45.0764121726109,-74.7783744078659,
-215.149949));
#205206=CARTESIAN_POINT('Ctrl Pts',(-25.5015868365187,-62.3415392578964,
-235.35005));
#205207=CARTESIAN_POINT('Ctrl Pts',(-32.299209143815,-66.325492796133,-228.68335));
#205208=CARTESIAN_POINT('Ctrl Pts',(-39.0968174546589,-70.3085029414293,
-222.01665));
#205209=CARTESIAN_POINT('Ctrl Pts',(-45.8944083573785,-74.2905697967455,
-215.34995));
#205210=CARTESIAN_POINT('Ctrl Pts',(-45.9623842664057,-74.3303904652987,
-215.283283));
#205211=CARTESIAN_POINT('Ctrl Pts',(-46.0303601754329,-74.3702111338518,
-215.216616));
#205212=CARTESIAN_POINT('Ctrl Pts',(-46.0983360844601,-74.410031802405,
-215.149949));
#205213=CARTESIAN_POINT('Ctrl Pts',(-25.7300777644121,-62.275287851211,
-235.35005));
#205214=CARTESIAN_POINT('Ctrl Pts',(-32.7889564583827,-66.1223030781061,
-228.68335));
#205215=CARTESIAN_POINT('Ctrl Pts',(-39.8478250972557,-69.9681827947029,
-222.01665));
#205216=CARTESIAN_POINT('Ctrl Pts',(-46.906679573783,-73.8129271161338,
-215.34995));
#205217=CARTESIAN_POINT('Ctrl Pts',(-46.9772681185483,-73.8513745593482,
-215.283283));
#205218=CARTESIAN_POINT('Ctrl Pts',(-47.0478566633135,-73.8898220025625,
-215.216616));
#205219=CARTESIAN_POINT('Ctrl Pts',(-47.1184452080788,-73.9282694457768,
-215.149949));
#205220=CARTESIAN_POINT('Ctrl Pts',(-25.9496411726737,-62.2064433802863,
-235.35005));
#205221=CARTESIAN_POINT('Ctrl Pts',(-33.2328325215974,-65.8962682476017,
-228.68335));
#205222=CARTESIAN_POINT('Ctrl Pts',(-40.5160203632138,-69.5847817101261,
-222.01665));
#205223=CARTESIAN_POINT('Ctrl Pts',(-47.7991999531534,-73.2719838903286,
-215.34995));
#205224=CARTESIAN_POINT('Ctrl Pts',(-47.8720317490528,-73.3088559121307,
-215.283283));
#205225=CARTESIAN_POINT('Ctrl Pts',(-47.9448635449522,-73.3457279339327,
-215.216616));
#205226=CARTESIAN_POINT('Ctrl Pts',(-48.0176953408516,-73.3825999557347,
-215.149949));
#205227=CARTESIAN_POINT('Ctrl Pts',(-26.2296171960789,-62.0929811520229,
-235.35005));
#205228=CARTESIAN_POINT('Ctrl Pts',(-33.5992240749579,-65.6911775370676,
-228.68335));
#205229=CARTESIAN_POINT('Ctrl Pts',(-40.9688364442604,-69.2879023661194,
-222.01665));
#205230=CARTESIAN_POINT('Ctrl Pts',(-48.3384489792287,-72.8831557643943,
-215.34995));
#205231=CARTESIAN_POINT('Ctrl Pts',(-48.4121451045784,-72.919108298377,
-215.283283));
#205232=CARTESIAN_POINT('Ctrl Pts',(-48.485841229928,-72.9550608323598,
-215.216616));
#205233=CARTESIAN_POINT('Ctrl Pts',(-48.5595373552777,-72.9910133663425,
-215.149949));
#205234=CARTESIAN_POINT('Ctrl Pts',(-26.4137508499222,-62.0144582859218,
-235.35005));
#205235=CARTESIAN_POINT('Ctrl Pts',(-33.8110251833904,-65.5692400768433,
-228.68335));
#205236=CARTESIAN_POINT('Ctrl Pts',(-41.2083125347321,-69.1224537201152,
-222.01665));
#205237=CARTESIAN_POINT('Ctrl Pts',(-48.6056072289401,-72.6740993398878,
-215.34995));
#205238=CARTESIAN_POINT('Ctrl Pts',(-48.6795801758822,-72.7096157960855,
-215.283283));
#205239=CARTESIAN_POINT('Ctrl Pts',(-48.7535531228243,-72.7451322522832,
-215.216616));
#205240=CARTESIAN_POINT('Ctrl Pts',(-48.8275260697664,-72.780648708481,
-215.149949));
#205241=CARTESIAN_POINT('Ctrl Pts',(-26.60131676328,-61.915483833886,-235.35005));
#205242=CARTESIAN_POINT('Ctrl Pts',(-33.9746898504281,-65.4717344596898,
-228.68335));
#205243=CARTESIAN_POINT('Ctrl Pts',(-41.3480800753329,-69.0263711060389,
-222.01665));
#205244=CARTESIAN_POINT('Ctrl Pts',(-48.7214815967444,-72.5793938958684,
-215.34995));
#205245=CARTESIAN_POINT('Ctrl Pts',(-48.7952156119585,-72.6149241237667,
-215.283283));
#205246=CARTESIAN_POINT('Ctrl Pts',(-48.8689496271726,-72.6504543516649,
-215.216616));
#205247=CARTESIAN_POINT('Ctrl Pts',(-48.9426836423867,-72.6859845795632,
-215.149949));
#205248=CARTESIAN_POINT('',(-33.2187488845874,-68.8101802592752,-225.35));
#205249=CARTESIAN_POINT('Ctrl Pts',(-27.0930165135311,-62.1526330725429,
-234.905475377596));
#205250=CARTESIAN_POINT('Ctrl Pts',(-33.75885046978,-65.3675653924474,-228.878503713969));
#205251=CARTESIAN_POINT('Ctrl Pts',(-40.424698326436,-68.5811786244384,
-222.851532050343));
#205252=CARTESIAN_POINT('Ctrl Pts',(-47.0905557676078,-71.7934728593479,
-216.824560386716));
#205253=CARTESIAN_POINT('Ctrl Pts',(-29.0709882823152,37.525873057636,-235.35005));
#205254=CARTESIAN_POINT('Ctrl Pts',(-35.5332604733831,40.6579014073498,
-228.683350000001));
#205255=CARTESIAN_POINT('Ctrl Pts',(-41.9930962102693,43.771133049519,-222.01665));
#205256=CARTESIAN_POINT('Ctrl Pts',(-48.4493862544499,46.8657485296993,
-215.34995));
#205257=CARTESIAN_POINT('Ctrl Pts',(-48.5139491548917,46.8966946845011,
-215.283283));
#205258=CARTESIAN_POINT('Ctrl Pts',(-48.5785120553335,46.9276408393029,
-215.216616));
#205259=CARTESIAN_POINT('Ctrl Pts',(-48.6430749557753,46.9585869941047,
-215.149949));
#205260=CARTESIAN_POINT('Ctrl Pts',(-28.9262831839988,37.6116730896339,
-235.35005));
#205261=CARTESIAN_POINT('Ctrl Pts',(-35.404815368487,40.7403542996618,-228.683350000001));
#205262=CARTESIAN_POINT('Ctrl Pts',(-41.8809828830328,43.8508119821702,
-222.01665));
#205263=CARTESIAN_POINT('Ctrl Pts',(-48.3537103198215,46.9432211795102,
-215.34995));
#205264=CARTESIAN_POINT('Ctrl Pts',(-48.4184375941894,46.9741452714836,
-215.283283));
#205265=CARTESIAN_POINT('Ctrl Pts',(-48.4831648685572,47.005069363457,-215.216616));
#205266=CARTESIAN_POINT('Ctrl Pts',(-48.5478921429251,47.0359934554304,
-215.149949));
#205267=CARTESIAN_POINT('Ctrl Pts',(-28.7510590357854,37.7017381212741,
-235.35005));
#205268=CARTESIAN_POINT('Ctrl Pts',(-35.2153249135404,40.8559840579253,
-228.683350000001));
#205269=CARTESIAN_POINT('Ctrl Pts',(-41.67737658309,43.9932018113665,-222.01665));
#205270=CARTESIAN_POINT('Ctrl Pts',(-48.1362091874323,47.1135549465408,
-215.34995));
#205271=CARTESIAN_POINT('Ctrl Pts',(-48.2007975134757,47.1447584778926,
-215.283283));
#205272=CARTESIAN_POINT('Ctrl Pts',(-48.2653858395191,47.1759620092443,
-215.216616));
#205273=CARTESIAN_POINT('Ctrl Pts',(-48.3299741655626,47.207165540596,-215.149949));
#205274=CARTESIAN_POINT('Ctrl Pts',(-28.5095079111441,37.8154098604791,
-235.350050000001));
#205275=CARTESIAN_POINT('Ctrl Pts',(-34.9092271504532,41.0352703241457,
-228.683350000001));
#205276=CARTESIAN_POINT('Ctrl Pts',(-41.3069791618872,44.2400465335893,
-222.016650000001));
#205277=CARTESIAN_POINT('Ctrl Pts',(-47.7018738162952,47.429883386524,-215.34995));
#205278=CARTESIAN_POINT('Ctrl Pts',(-47.7658227628392,47.4617817550534,
-215.283283));
#205279=CARTESIAN_POINT('Ctrl Pts',(-47.8297717093833,47.4936801235827,
-215.216616));
#205280=CARTESIAN_POINT('Ctrl Pts',(-47.8937206559274,47.525578492112,-215.149949));
#205281=CARTESIAN_POINT('Ctrl Pts',(-28.3066649003232,37.8966208237621,
-235.35005));
#205282=CARTESIAN_POINT('Ctrl Pts',(-34.5530956045189,41.2282169831045,
-228.68335));
#205283=CARTESIAN_POINT('Ctrl Pts',(-40.7978279568429,44.5468276894782,
-222.01665));
#205284=CARTESIAN_POINT('Ctrl Pts',(-47.0400956910773,47.8525776841313,
-215.34995));
#205285=CARTESIAN_POINT('Ctrl Pts',(-47.1025183684196,47.8856351840778,
-215.283283));
#205286=CARTESIAN_POINT('Ctrl Pts',(-47.1649410457619,47.9186926840244,
-215.216616));
#205287=CARTESIAN_POINT('Ctrl Pts',(-47.2273637231043,47.9517501839709,
-215.149949));
#205288=CARTESIAN_POINT('Ctrl Pts',(-28.0997724400839,37.970731452037,-235.35005));
#205289=CARTESIAN_POINT('Ctrl Pts',(-34.1684829306694,41.4070992755122,
-228.683350000001));
#205290=CARTESIAN_POINT('Ctrl Pts',(-40.2357864490083,44.8327392792855,
-222.01665));
#205291=CARTESIAN_POINT('Ctrl Pts',(-46.3010499603476,48.2477545207809,
-215.34995));
#205292=CARTESIAN_POINT('Ctrl Pts',(-46.361702595461,48.2819046731959,-215.283283));
#205293=CARTESIAN_POINT('Ctrl Pts',(-46.4223552305744,48.3160548256108,
-215.216616));
#205294=CARTESIAN_POINT('Ctrl Pts',(-46.4830078656878,48.3502049780258,
-215.149949));
#205295=CARTESIAN_POINT('Ctrl Pts',(-27.9025329741163,38.0324522529201,
-235.35005));
#205296=CARTESIAN_POINT('Ctrl Pts',(-33.7896008939784,41.5559827385479,
-228.683350000001));
#205297=CARTESIAN_POINT('Ctrl Pts',(-39.6755763327887,45.0712058294971,
-222.01665));
#205298=CARTESIAN_POINT('Ctrl Pts',(-45.5599690892415,48.5782013338904,
-215.349950000001));
#205299=CARTESIAN_POINT('Ctrl Pts',(-45.618813016806,48.6132712889344,-215.283283000001));
#205300=CARTESIAN_POINT('Ctrl Pts',(-45.6776569443706,48.6483412439783,
-215.216616));
#205301=CARTESIAN_POINT('Ctrl Pts',(-45.7365008719351,48.6834111990222,
-215.149949000001));
#205302=CARTESIAN_POINT('Ctrl Pts',(-27.6836295517497,38.0888474954169,
-235.35005));
#205303=CARTESIAN_POINT('Ctrl Pts',(-33.3812146101381,41.6857034969331,
-228.68335));
#205304=CARTESIAN_POINT('Ctrl Pts',(-39.0780453981879,45.2768392802963,
-222.01665));
#205305=CARTESIAN_POINT('Ctrl Pts',(-44.773784383473,48.8623098007285,-215.34995));
#205306=CARTESIAN_POINT('Ctrl Pts',(-44.8307417733259,48.8981645059328,
-215.283283));
#205307=CARTESIAN_POINT('Ctrl Pts',(-44.8876991631787,48.9340192111371,
-215.216616));
#205308=CARTESIAN_POINT('Ctrl Pts',(-44.9446565530316,48.9698739163414,
-215.149949));
#205309=CARTESIAN_POINT('Ctrl Pts',(-27.4619512217085,38.1391172889764,
-235.35005));
#205310=CARTESIAN_POINT('Ctrl Pts',(-32.9867338744792,41.7852023290646,
-228.683350000001));
#205311=CARTESIAN_POINT('Ctrl Pts',(-38.511124795091,45.4283250387717,-222.016650000001));
#205312=CARTESIAN_POINT('Ctrl Pts',(-44.0349491888799,49.0685138787004,
-215.349950000001));
#205313=CARTESIAN_POINT('Ctrl Pts',(-44.0901874328179,49.1049157670997,
-215.283283000001));
#205314=CARTESIAN_POINT('Ctrl Pts',(-44.1454256767557,49.141317655499,-215.216616));
#205315=CARTESIAN_POINT('Ctrl Pts',(-44.2006639206936,49.1777195438983,
-215.149949000001));
#205316=CARTESIAN_POINT('Ctrl Pts',(-27.272251770635,38.1696450547512,-235.35005));
#205317=CARTESIAN_POINT('Ctrl Pts',(-32.7234828694691,41.832799228952,-228.68335));
#205318=CARTESIAN_POINT('Ctrl Pts',(-38.1745805518739,45.4949461119472,
-222.01665));
#205319=CARTESIAN_POINT('Ctrl Pts',(-43.625485383249,49.1560953813671,-215.34995));
#205320=CARTESIAN_POINT('Ctrl Pts',(-43.6799944315629,49.1927068740612,
-215.283283));
#205321=CARTESIAN_POINT('Ctrl Pts',(-43.7345034798766,49.2293183667554,
-215.216616));
#205322=CARTESIAN_POINT('Ctrl Pts',(-43.7890125281904,49.2659298594496,
-215.149949));
#205323=CARTESIAN_POINT('Ctrl Pts',(-27.1569075795172,38.1844371310006,
-235.35005));
#205324=CARTESIAN_POINT('Ctrl Pts',(-32.5837764342019,41.8536056393876,
-228.68335));
#205325=CARTESIAN_POINT('Ctrl Pts',(-38.0106452875494,45.5227741479461,
-222.01665));
#205326=CARTESIAN_POINT('Ctrl Pts',(-43.4375141409548,49.1919426564936,
-215.34995));
#205327=CARTESIAN_POINT('Ctrl Pts',(-43.4917828294889,49.2286343415791,
-215.283283));
#205328=CARTESIAN_POINT('Ctrl Pts',(-43.5460515180229,49.2653260266646,
-215.216616));
#205329=CARTESIAN_POINT('Ctrl Pts',(-43.600320206557,49.30201771175,-215.149949));
#205330=CARTESIAN_POINT('Ctrl Pts',(-29.5524353619882,37.7591803693089,
-234.853368133768));
#205331=CARTESIAN_POINT('Ctrl Pts',(-35.3897707041939,40.5875346064766,
-228.831260854445));
#205332=CARTESIAN_POINT('Ctrl Pts',(-41.225095491082,43.4005549188572,-222.809153575121));
#205333=CARTESIAN_POINT('Ctrl Pts',(-47.0575921287078,46.1983743823903,
-216.787046295788));
#205334=CARTESIAN_POINT('',(-35.2972108607157,43.6881898936869,-225.35));
#205335=CARTESIAN_POINT('Ctrl Pts',(-48.9291851287222,16.4845500982845,
-235.35005));
#205336=CARTESIAN_POINT('Ctrl Pts',(-53.3017114728827,20.6931427899333,
-228.68335));
#205337=CARTESIAN_POINT('Ctrl Pts',(-57.6742344655836,24.9017353436595,
-222.01665));
#205338=CARTESIAN_POINT('Ctrl Pts',(-62.0467541066728,29.1103277631972,
-215.34995));
#205339=CARTESIAN_POINT('Ctrl Pts',(-62.0904793030837,29.1524136873926,
-215.283283));
#205340=CARTESIAN_POINT('Ctrl Pts',(-62.1342044994946,29.194499611588,-215.216616));
#205341=CARTESIAN_POINT('Ctrl Pts',(-62.1779296959055,29.2365855357833,
-215.149949));
#205342=CARTESIAN_POINT('Ctrl Pts',(-48.9286835714312,16.4968248922029,
-235.35005));
#205343=CARTESIAN_POINT('Ctrl Pts',(-53.3011147739234,20.7079343778016,
-228.68335));
#205344=CARTESIAN_POINT('Ctrl Pts',(-57.6735437421284,24.9190437709811,
-222.01665));
#205345=CARTESIAN_POINT('Ctrl Pts',(-62.0459704759518,29.1301530740427,
-215.34995));
#205346=CARTESIAN_POINT('Ctrl Pts',(-62.08969474329,29.1722641670733,-215.283283));
#205347=CARTESIAN_POINT('Ctrl Pts',(-62.1334190106282,29.2143752601038,
-215.216616));
#205348=CARTESIAN_POINT('Ctrl Pts',(-62.1771432779665,29.2564863531345,
-215.149949));
#205349=CARTESIAN_POINT('Ctrl Pts',(-48.9281820141402,16.5090996861212,
-235.35005));
#205350=CARTESIAN_POINT('Ctrl Pts',(-53.3005180749641,20.72272596567,-228.68335));
#205351=CARTESIAN_POINT('Ctrl Pts',(-57.6728530186733,24.9363521983027,
-222.01665));
#205352=CARTESIAN_POINT('Ctrl Pts',(-62.0451868452307,29.1499783848881,
-215.34995));
#205353=CARTESIAN_POINT('Ctrl Pts',(-62.0889101834963,29.1921146467539,
-215.283283));
#205354=CARTESIAN_POINT('Ctrl Pts',(-62.1326335217618,29.2342509086198,
-215.216616));
#205355=CARTESIAN_POINT('Ctrl Pts',(-62.1763568600274,29.2763871704856,
-215.149949));
#205356=CARTESIAN_POINT('Ctrl Pts',(-48.9276804568491,16.5213744800396,
-235.35005));
#205357=CARTESIAN_POINT('Ctrl Pts',(-53.2999213760048,20.7375175535383,
-228.68335));
#205358=CARTESIAN_POINT('Ctrl Pts',(-57.6721622952182,24.9536606256242,
-222.01665));
#205359=CARTESIAN_POINT('Ctrl Pts',(-62.0444032145096,29.1698036957335,
-215.34995));
#205360=CARTESIAN_POINT('Ctrl Pts',(-62.0881256237025,29.2119651264346,
-215.283283));
#205361=CARTESIAN_POINT('Ctrl Pts',(-62.1318480328954,29.2541265571357,
-215.216616));
#205362=CARTESIAN_POINT('Ctrl Pts',(-62.1755704420884,29.2962879878368,
-215.149949));
#205363=CARTESIAN_POINT('Ctrl Pts',(-48.9214109907111,16.6748094040191,
-235.35005));
#205364=CARTESIAN_POINT('Ctrl Pts',(-53.2924626390134,20.9224124018924,
-228.68335));
#205365=CARTESIAN_POINT('Ctrl Pts',(-57.663528252029,25.170015967144,-222.01665));
#205366=CARTESIAN_POINT('Ctrl Pts',(-62.0346078304961,29.4176200813015,
-215.34995));
#205367=CARTESIAN_POINT('Ctrl Pts',(-62.0783186262808,29.4600961224431,
-215.283283));
#205368=CARTESIAN_POINT('Ctrl Pts',(-62.1220294220655,29.5025721635847,
-215.216616));
#205369=CARTESIAN_POINT('Ctrl Pts',(-62.1657402178502,29.5450482047262,
-215.149949));
#205370=CARTESIAN_POINT('Ctrl Pts',(-48.8992712925998,16.9131404133547,
-235.35005));
#205371=CARTESIAN_POINT('Ctrl Pts',(-53.2652870417935,21.2619501899207,
-228.68335));
#205372=CARTESIAN_POINT('Ctrl Pts',(-57.6313776897902,25.6107124643303,
-222.01665));
#205373=CARTESIAN_POINT('Ctrl Pts',(-61.9975402416511,29.9594276183431,
-215.34995));
#205374=CARTESIAN_POINT('Ctrl Pts',(-62.0412018671697,30.0029147698833,
-215.283283));
#205375=CARTESIAN_POINT('Ctrl Pts',(-62.0848634926883,30.0464019214233,
-215.216616));
#205376=CARTESIAN_POINT('Ctrl Pts',(-62.1285251182069,30.0898890729635,
-215.149949));
#205377=CARTESIAN_POINT('Ctrl Pts',(-48.8533444192211,17.2181014412188,
-235.35005));
#205378=CARTESIAN_POINT('Ctrl Pts',(-53.1855995667747,21.7941761255924,
-228.68335));
#205379=CARTESIAN_POINT('Ctrl Pts',(-57.5179747573295,26.3699864363254,
-222.01665));
#205380=CARTESIAN_POINT('Ctrl Pts',(-61.8504540244681,30.9455347714532,
-215.34995));
#205381=CARTESIAN_POINT('Ctrl Pts',(-61.8937788171395,30.9912902548045,
-215.283283));
#205382=CARTESIAN_POINT('Ctrl Pts',(-61.9371036098109,31.0370457381558,
-215.216616));
#205383=CARTESIAN_POINT('Ctrl Pts',(-61.9804284024823,31.082801221507,-215.149949));
#205384=CARTESIAN_POINT('Ctrl Pts',(-48.793774157437,17.4925774935122,-235.35005));
#205385=CARTESIAN_POINT('Ctrl Pts',(-53.0569741223029,22.3329163118503,
-228.68335));
#205386=CARTESIAN_POINT('Ctrl Pts',(-57.3203153214379,27.1726388120429,
-222.01665));
#205387=CARTESIAN_POINT('Ctrl Pts',(-61.5837608612094,32.0117507116806,
-215.34995));
#205388=CARTESIAN_POINT('Ctrl Pts',(-61.6263953166071,32.060141830677,-215.283283));
#205389=CARTESIAN_POINT('Ctrl Pts',(-61.6690297720048,32.1085329496734,
-215.216616));
#205390=CARTESIAN_POINT('Ctrl Pts',(-61.7116642274025,32.1569240686698,
-215.149949));
#205391=CARTESIAN_POINT('Ctrl Pts',(-48.7243271460874,17.7538206185435,
-235.35005));
#205392=CARTESIAN_POINT('Ctrl Pts',(-52.8915700395936,22.8426678835018,
-228.68335));
#205393=CARTESIAN_POINT('Ctrl Pts',(-57.0589527628024,27.9304206519508,
-222.01665));
#205394=CARTESIAN_POINT('Ctrl Pts',(-61.2264100602501,33.0170891792215,
-215.34995));
#205395=CARTESIAN_POINT('Ctrl Pts',(-61.2680846332245,33.0679558644942,
-215.283283));
#205396=CARTESIAN_POINT('Ctrl Pts',(-61.309759206199,33.1188225497669,-215.216616));
#205397=CARTESIAN_POINT('Ctrl Pts',(-61.3514337791735,33.1696892350396,
-215.149949));
#205398=CARTESIAN_POINT('Ctrl Pts',(-48.6354732464631,18.0177190827397,
-235.35005));
#205399=CARTESIAN_POINT('Ctrl Pts',(-52.6780922604543,23.3513726702934,
-228.68335));
#205400=CARTESIAN_POINT('Ctrl Pts',(-56.7208284608432,28.6833361882777,
-222.01665));
#205401=CARTESIAN_POINT('Ctrl Pts',(-60.7635813168395,34.0136255628538,
-215.34995));
#205402=CARTESIAN_POINT('Ctrl Pts',(-60.8040088453995,34.0669284565996,
-215.283283));
#205403=CARTESIAN_POINT('Ctrl Pts',(-60.8444363739595,34.1202313503453,
-215.216616));
#205404=CARTESIAN_POINT('Ctrl Pts',(-60.8848639025194,34.1735342440911,
-215.149949));
#205405=CARTESIAN_POINT('Ctrl Pts',(-48.5352774797299,18.2802794424427,
-235.35005));
#205406=CARTESIAN_POINT('Ctrl Pts',(-52.4343101169869,23.8247568642913,
-228.68335));
#205407=CARTESIAN_POINT('Ctrl Pts',(-56.3334174156944,29.3668400879758,
-222.016650000001));
#205408=CARTESIAN_POINT('Ctrl Pts',(-60.2324571773606,34.9065517584836,
-215.349950000001));
#205409=CARTESIAN_POINT('Ctrl Pts',(-60.2714475749772,34.9619488751887,
-215.283283000001));
#205410=CARTESIAN_POINT('Ctrl Pts',(-60.3104379725939,35.0173459918937,
-215.216616));
#205411=CARTESIAN_POINT('Ctrl Pts',(-60.3494283702106,35.0727431085988,
-215.149949000001));
#205412=CARTESIAN_POINT('Ctrl Pts',(-48.3890207412154,18.5878255918932,
-235.35005));
#205413=CARTESIAN_POINT('Ctrl Pts',(-52.1962991404372,24.228375758149,-228.68335));
#205414=CARTESIAN_POINT('Ctrl Pts',(-56.0035911516163,29.8657278812732,
-222.01665));
#205415=CARTESIAN_POINT('Ctrl Pts',(-59.810707037304,35.4999122879811,-215.34995));
#205416=CARTESIAN_POINT('Ctrl Pts',(-59.8487781961609,35.5562541320482,
-215.283283));
#205417=CARTESIAN_POINT('Ctrl Pts',(-59.8868493550178,35.6125959761153,
-215.216616));
#205418=CARTESIAN_POINT('Ctrl Pts',(-59.9249205138747,35.6689378201824,
-215.149949));
#205419=CARTESIAN_POINT('Ctrl Pts',(-48.2711217441656,18.8106246802399,
-235.35005));
#205420=CARTESIAN_POINT('Ctrl Pts',(-52.0406861996216,24.475501377336,-228.68335));
#205421=CARTESIAN_POINT('Ctrl Pts',(-55.8102121224059,30.1365835498488,
-222.01665));
#205422=CARTESIAN_POINT('Ctrl Pts',(-59.5794745156759,35.7939072308497,
-215.34995));
#205423=CARTESIAN_POINT('Ctrl Pts',(-59.6171671396086,35.8504804676597,
-215.283283));
#205424=CARTESIAN_POINT('Ctrl Pts',(-59.6548597635413,35.9070537044696,
-215.216616));
#205425=CARTESIAN_POINT('Ctrl Pts',(-59.692552387474,35.9636269412797,-215.149949));
#205426=CARTESIAN_POINT('Ctrl Pts',(-48.1560655143106,18.9923105754345,
-235.35005));
#205427=CARTESIAN_POINT('Ctrl Pts',(-51.9286217775904,24.6399928719346,
-228.68335));
#205428=CARTESIAN_POINT('Ctrl Pts',(-55.7011108008251,30.2835687301176,
-222.01665));
#205429=CARTESIAN_POINT('Ctrl Pts',(-59.4732891526392,35.9230771683515,
-215.34995));
#205430=CARTESIAN_POINT('Ctrl Pts',(-59.5110109361573,35.9794722527339,
-215.283283));
#205431=CARTESIAN_POINT('Ctrl Pts',(-59.5487327196755,36.0358673371162,
-215.216616));
#205432=CARTESIAN_POINT('Ctrl Pts',(-59.5864545031936,36.0922624214986,
-215.149949));
#205433=CARTESIAN_POINT('Ctrl Pts',(-48.1468610159222,19.00684544705,-235.35005));
#205434=CARTESIAN_POINT('Ctrl Pts',(-51.9196566238279,24.6531521915024,
-228.68335));
#205435=CARTESIAN_POINT('Ctrl Pts',(-55.6923826950986,30.2953275445391,
-222.01665));
#205436=CARTESIAN_POINT('Ctrl Pts',(-59.4647943235962,35.9334107633517,
-215.34995));
#205437=CARTESIAN_POINT('Ctrl Pts',(-59.5025184398812,35.9897915955398,
-215.283283));
#205438=CARTESIAN_POINT('Ctrl Pts',(-59.5402425561662,36.046172427728,-215.216616));
#205439=CARTESIAN_POINT('Ctrl Pts',(-59.5779666724512,36.102553259916,-215.149949));
#205440=CARTESIAN_POINT('Ctrl Pts',(-48.1376565175338,19.0213803186655,
-235.35005));
#205441=CARTESIAN_POINT('Ctrl Pts',(-51.9106914700654,24.6663115110703,
-228.68335));
#205442=CARTESIAN_POINT('Ctrl Pts',(-55.6836545893721,30.3070863589606,
-222.01665));
#205443=CARTESIAN_POINT('Ctrl Pts',(-59.4562994945533,35.9437443583519,
-215.34995));
#205444=CARTESIAN_POINT('Ctrl Pts',(-59.4940259436051,36.0001109383457,
-215.283283));
#205445=CARTESIAN_POINT('Ctrl Pts',(-59.5317523926569,36.0564775183397,
-215.216616));
#205446=CARTESIAN_POINT('Ctrl Pts',(-59.5694788417088,36.1128440983336,
-215.149949));
#205447=CARTESIAN_POINT('Ctrl Pts',(-48.1284520191454,19.0359151902811,
-235.35005));
#205448=CARTESIAN_POINT('Ctrl Pts',(-51.9017263163029,24.6794708306382,
-228.68335));
#205449=CARTESIAN_POINT('Ctrl Pts',(-55.6749264836457,30.3188451733821,
-222.01665));
#205450=CARTESIAN_POINT('Ctrl Pts',(-59.4478046655104,35.9540779533519,
-215.34995));
#205451=CARTESIAN_POINT('Ctrl Pts',(-59.485533447329,36.0104302811517,-215.283283));
#205452=CARTESIAN_POINT('Ctrl Pts',(-59.5232622291477,36.0667826089514,
-215.216616));
#205453=CARTESIAN_POINT('Ctrl Pts',(-59.5609910109663,36.1231349367511,
-215.149949));
#205454=CARTESIAN_POINT('',(-55.4860418356284,22.8455890891576,-225.35));
#205455=CARTESIAN_POINT('Ctrl Pts',(-48.4260896922586,19.3965417854656,
-234.872874618363));
#205456=CARTESIAN_POINT('Ctrl Pts',(-51.8397102119512,24.5067087698627,
-228.840465153427));
#205457=CARTESIAN_POINT('Ctrl Pts',(-55.2532709224339,29.6135143043896,
-222.808055688492));
#205458=CARTESIAN_POINT('Ctrl Pts',(-58.6665914736623,34.7169872964315,
-216.775646223556));
#205459=CARTESIAN_POINT('Origin',(-41.5452362233251,-63.7990866568863,-205.34995));
#205460=CARTESIAN_POINT('',(-48.8319431829163,-72.7145462807723,-205.34995));
#205461=CARTESIAN_POINT('',(-41.9984355604289,-75.3045692187324,-205.34995));
#205462=CARTESIAN_POINT('Origin',(0.,-12.9675000200281,-205.34995));
#205463=CARTESIAN_POINT('',(-59.6081272922882,-61.9689221688742,-205.34995));
#205464=CARTESIAN_POINT('Origin',(-50.7133971693864,-54.6569255427236,-205.34995));
#205465=CARTESIAN_POINT('',(-62.2188176672479,-55.1116977796555,-205.34995));
#205466=CARTESIAN_POINT('Origin',(-50.7133971693864,28.7219255026674,-205.34995));
#205467=CARTESIAN_POINT('',(-59.6081272922883,36.0339221288179,-205.34995));
#205468=CARTESIAN_POINT('',(-62.218817667248,29.176697739599,-205.34995));
#205469=CARTESIAN_POINT('Origin',(0.,-12.9675000200281,-205.34995));
#205470=CARTESIAN_POINT('',(-48.5592309447134,47.0014027710106,-205.34995));
#205471=CARTESIAN_POINT('Origin',(-41.3132181298675,38.0528376956935,-205.34995));
#205472=CARTESIAN_POINT('',(-43.4702127313761,49.3634032389879,-205.34995));
#205473=CARTESIAN_POINT('Origin',(1004.,-12.967500020028,-179.64995));
#205474=CARTESIAN_POINT('',(-65.1651121384123,-55.2281553161325,-179.64995));
#205475=CARTESIAN_POINT('',(-65.1651121384124,-55.2281553161325,-179.64995));
#205476=CARTESIAN_POINT('',(-65.1651121384124,29.2931552760762,-179.64995));
#205477=CARTESIAN_POINT('Origin',(1004.,-12.967500020028,-179.64995));
#205478=CARTESIAN_POINT('',(-65.1651121384125,29.293155276076,-179.64995));
#205479=CARTESIAN_POINT('Origin',(-50.7133971693864,28.7219255026673,-179.64995));
#205480=CARTESIAN_POINT('',(-61.8858792604563,37.9063695753764,-179.64995));
#205481=CARTESIAN_POINT('Origin',(-50.7133971693864,28.7219255026673,-179.64995));
#205482=CARTESIAN_POINT('',(-61.8858792604564,37.9063695753764,-179.64995));
#205483=CARTESIAN_POINT('Origin',(0.,-12.9675000200281,-179.64995));
#205484=CARTESIAN_POINT('',(-50.4147813349261,49.2929407301111,-179.64995));
#205485=CARTESIAN_POINT('Origin',(0.,-12.9675000200281,-179.64995));
#205486=CARTESIAN_POINT('',(-50.4147813349261,49.292940730111,-179.64995));
#205487=CARTESIAN_POINT('Origin',(-41.3132181298675,38.0528376956935,-179.64995));
#205488=CARTESIAN_POINT('',(-44.0225733573905,52.2597994838836,-179.64995));
#205489=CARTESIAN_POINT('Origin',(-41.3132181298675,38.0528376956935,-179.64995));
#205490=CARTESIAN_POINT('',(-44.0225733573905,52.2597994838836,-179.64995));
#205491=CARTESIAN_POINT('Origin',(-41.5452362233251,-63.7990866568863,-179.64995));
#205492=CARTESIAN_POINT('',(-42.1144903105792,-78.2508795831687,-179.64995));
#205493=CARTESIAN_POINT('',(-42.1144903105791,-78.2508795831687,-179.64995));
#205494=CARTESIAN_POINT('',(-50.6979144815776,-74.9976066350312,-179.64995));
#205495=CARTESIAN_POINT('Origin',(-41.5452362233251,-63.7990866568863,-179.64995));
#205496=CARTESIAN_POINT('',(-50.6979144815776,-74.9976066350312,-179.64995));
#205497=CARTESIAN_POINT('Origin',(0.,-12.9675000200281,-179.64995));
#205498=CARTESIAN_POINT('',(-61.8858792604563,-63.8413696154326,-179.64995));
#205499=CARTESIAN_POINT('Origin',(0.,-12.9675000200281,-179.64995));
#205500=CARTESIAN_POINT('',(-61.8858792604563,-63.8413696154326,-179.64995));
#205501=CARTESIAN_POINT('Origin',(-50.7133971693864,-54.6569255427236,-179.64995));
#205502=CARTESIAN_POINT('Origin',(-50.7133971693864,-54.6569255427236,-179.64995));
#205503=CARTESIAN_POINT('Ctrl Pts',(-48.9276804568491,-39.5283381317121,
-235.35005));
#205504=CARTESIAN_POINT('Ctrl Pts',(-53.2999213760692,-44.7204933330714,
-228.68335));
#205505=CARTESIAN_POINT('Ctrl Pts',(-57.6721622952894,-49.9126485344307,
-222.01665));
#205506=CARTESIAN_POINT('Ctrl Pts',(-62.0444032145095,-55.1048037357899,
-215.34995));
#205507=CARTESIAN_POINT('Ctrl Pts',(-49.0194233450359,-37.283081077169,
-235.35005));
#205508=CARTESIAN_POINT('Ctrl Pts',(-53.4090672042376,-42.0148742220589,
-228.683350000001));
#205509=CARTESIAN_POINT('Ctrl Pts',(-57.7985067146479,-46.7466590436653,
-222.016650000001));
#205510=CARTESIAN_POINT('Ctrl Pts',(-62.1877418657617,-51.4784358040522,
-215.34995));
#205511=CARTESIAN_POINT('Ctrl Pts',(-49.1841844420714,-32.7087365060477,
-235.35005));
#205512=CARTESIAN_POINT('Ctrl Pts',(-53.600359505658,-36.5883830285289,
-228.68335));
#205513=CARTESIAN_POINT('Ctrl Pts',(-58.0165345692446,-40.4680295510101,
-222.01665));
#205514=CARTESIAN_POINT('Ctrl Pts',(-62.4327096328312,-44.3476760734913,
-215.34995));
#205515=CARTESIAN_POINT('Ctrl Pts',(-49.3659986639477,-25.6715165814334,
-235.35005));
#205516=CARTESIAN_POINT('Ctrl Pts',(-53.8070961606803,-28.4006856868431,
-228.68335));
#205517=CARTESIAN_POINT('Ctrl Pts',(-58.2481936574129,-31.1298547922528,
-222.01665));
#205518=CARTESIAN_POINT('Ctrl Pts',(-62.6892911541455,-33.8590238976625,
-215.34995));
#205519=CARTESIAN_POINT('Ctrl Pts',(-49.4760453414413,-18.5583238061847,
-235.35005));
#205520=CARTESIAN_POINT('Ctrl Pts',(-53.9314601157808,-20.1883767671888,
-228.68335));
#205521=CARTESIAN_POINT('Ctrl Pts',(-58.3868748901203,-21.8184297281929,
-222.01665));
#205522=CARTESIAN_POINT('Ctrl Pts',(-62.8422896644598,-23.448482689197,
-215.34995));
#205523=CARTESIAN_POINT('Ctrl Pts',(-49.5,-13.8395357876534,-235.35005));
#205524=CARTESIAN_POINT('Ctrl Pts',(-53.9589513940208,-14.7196423822522,
-228.68335));
#205525=CARTESIAN_POINT('Ctrl Pts',(-58.4179027880416,-15.599748976851,
-222.01665));
#205526=CARTESIAN_POINT('Ctrl Pts',(-62.8768541820624,-16.4798555714498,
-215.34995));
#205527=CARTESIAN_POINT('Ctrl Pts',(-49.5,-11.5034818258362,-235.35005));
#205528=CARTESIAN_POINT('Ctrl Pts',(-53.9589513940208,-11.9914878905669,
-228.68335));
#205529=CARTESIAN_POINT('Ctrl Pts',(-58.4179027880416,-12.4794939552975,
-222.01665));
#205530=CARTESIAN_POINT('Ctrl Pts',(-62.8768541820624,-12.9675000200282,
-215.34995));
#205531=CARTESIAN_POINT('Ctrl Pts',(-49.5,-11.5034818258362,-235.35005));
#205532=CARTESIAN_POINT('Ctrl Pts',(-53.9589513940208,-11.9914878905669,
-228.68335));
#205533=CARTESIAN_POINT('Ctrl Pts',(-58.4179027880416,-12.4794939552975,
-222.01665));
#205534=CARTESIAN_POINT('Ctrl Pts',(-62.8768541820624,-12.9675000200282,
-215.34995));
#205535=CARTESIAN_POINT('Ctrl Pts',(-62.9214436960026,-12.9723800806755,
-215.283283));
#205536=CARTESIAN_POINT('Ctrl Pts',(-62.9660332099428,-12.9772601413228,
-215.216616));
#205537=CARTESIAN_POINT('Ctrl Pts',(-63.010622723883,-12.9821402019701,
-215.149949));
#205538=CARTESIAN_POINT('Ctrl Pts',(-49.5,-9.16742786401911,-235.35005));
#205539=CARTESIAN_POINT('Ctrl Pts',(-53.9589513940208,-9.26333339888158,
-228.68335));
#205540=CARTESIAN_POINT('Ctrl Pts',(-58.4179027880416,-9.35923893374405,
-222.01665));
#205541=CARTESIAN_POINT('Ctrl Pts',(-62.8768541820624,-9.45514446860653,
-215.34995));
#205542=CARTESIAN_POINT('Ctrl Pts',(-62.9214436960026,-9.45610352395515,
-215.283283));
#205543=CARTESIAN_POINT('Ctrl Pts',(-62.9660332099428,-9.45706257930377,
-215.216616));
#205544=CARTESIAN_POINT('Ctrl Pts',(-63.010622723883,-9.4580216346524,-215.149949));
#205545=CARTESIAN_POINT('Ctrl Pts',(-49.4760453034623,-4.44863709409477,
-235.35005));
#205546=CARTESIAN_POINT('Ctrl Pts',(-53.9314600904615,-3.79459717968296,
-228.68335));
#205547=CARTESIAN_POINT('Ctrl Pts',(-58.3868748774607,-3.14055726527114,
-222.01665));
#205548=CARTESIAN_POINT('Ctrl Pts',(-62.8422896644599,-2.48651735085932,
-215.34995));
#205549=CARTESIAN_POINT('Ctrl Pts',(-62.8868438123299,-2.47997695171521,
-215.283283));
#205550=CARTESIAN_POINT('Ctrl Pts',(-62.9313979601999,-2.47343655257108,
-215.216616));
#205551=CARTESIAN_POINT('Ctrl Pts',(-62.9759521080699,-2.46689615342696,
-215.149949));
#205552=CARTESIAN_POINT('Ctrl Pts',(-49.3659992921549,2.6645466712911,-235.350050000001));
#205553=CARTESIAN_POINT('Ctrl Pts',(-53.8070965794851,4.41770573339612,
-228.683350000001));
#205554=CARTESIAN_POINT('Ctrl Pts',(-58.2481938668153,6.17086479550113,
-222.016650000001));
#205555=CARTESIAN_POINT('Ctrl Pts',(-62.6892911541455,7.92402385760615,
-215.349950000001));
#205556=CARTESIAN_POINT('Ctrl Pts',(-62.7337021270188,7.9415554482272,-215.283283000001));
#205557=CARTESIAN_POINT('Ctrl Pts',(-62.7781130998921,7.95908703884825,
-215.216616));
#205558=CARTESIAN_POINT('Ctrl Pts',(-62.8225240727654,7.9766186294693,-215.149949000001));
#205559=CARTESIAN_POINT('Ctrl Pts',(-49.1841830823307,9.70178317521733,
-235.35005));
#205560=CARTESIAN_POINT('Ctrl Pts',(-53.6003585991642,12.6054141279565,
-228.68335));
#205561=CARTESIAN_POINT('Ctrl Pts',(-58.0165341159977,15.5090450806958,
-222.01665));
#205562=CARTESIAN_POINT('Ctrl Pts',(-62.4327096328312,18.412676033435,-215.34995));
#205563=CARTESIAN_POINT('Ctrl Pts',(-62.4768713879996,18.4417123429624,
-215.283283));
#205564=CARTESIAN_POINT('Ctrl Pts',(-62.5210331431679,18.4707486524898,
-215.216616));
#205565=CARTESIAN_POINT('Ctrl Pts',(-62.5651948983362,18.4997849620172,
-215.149949));
#205566=CARTESIAN_POINT('Ctrl Pts',(-49.0194233450359,14.2761174254963,
-235.35005));
#205567=CARTESIAN_POINT('Ctrl Pts',(-53.4090672042376,18.031898440925,-228.68335));
#205568=CARTESIAN_POINT('Ctrl Pts',(-57.7985067146477,21.7876711330703,
-222.01665));
#205569=CARTESIAN_POINT('Ctrl Pts',(-62.1877418657617,25.5434357639959,
-215.34995));
#205570=CARTESIAN_POINT('Ctrl Pts',(-62.2316342172729,25.5809934103052,
-215.283283));
#205571=CARTESIAN_POINT('Ctrl Pts',(-62.275526568784,25.6185510566144,-215.216616));
#205572=CARTESIAN_POINT('Ctrl Pts',(-62.3194189202952,25.6561087029237,
-215.149949));
#205573=CARTESIAN_POINT('Ctrl Pts',(-48.9276804568491,16.5213744800396,
-235.35005));
#205574=CARTESIAN_POINT('Ctrl Pts',(-53.2999213760048,20.7375175535383,
-228.68335));
#205575=CARTESIAN_POINT('Ctrl Pts',(-57.6721622952182,24.9536606256242,
-222.01665));
#205576=CARTESIAN_POINT('Ctrl Pts',(-62.0444032145096,29.1698036957335,
-215.34995));
#205577=CARTESIAN_POINT('Ctrl Pts',(-62.0881256237025,29.2119651264346,
-215.283283));
#205578=CARTESIAN_POINT('Ctrl Pts',(-62.1318480328954,29.2541265571357,
-215.216616));
#205579=CARTESIAN_POINT('Ctrl Pts',(-62.1755704420884,29.2962879878368,
-215.149949));
#205580=CARTESIAN_POINT('Origin',(1004.,-12.967500020028,-205.34995));
#205581=CARTESIAN_POINT('Ctrl Pts',(-27.1569075795172,38.1844371310006,
-235.35005));
#205582=CARTESIAN_POINT('Ctrl Pts',(-32.5837764342019,41.8536056393876,
-228.68335));
#205583=CARTESIAN_POINT('Ctrl Pts',(-38.0106452875494,45.5227741479461,
-222.01665));
#205584=CARTESIAN_POINT('Ctrl Pts',(-43.4375141409548,49.1919426564936,
-215.34995));
#205585=CARTESIAN_POINT('Ctrl Pts',(-43.4917828294889,49.2286343415791,
-215.283283));
#205586=CARTESIAN_POINT('Ctrl Pts',(-43.5460515180229,49.2653260266646,
-215.216616));
#205587=CARTESIAN_POINT('Ctrl Pts',(-43.600320206557,49.30201771175,-215.149949));
#205588=CARTESIAN_POINT('Ctrl Pts',(-22.7175376169318,38.7537549124104,
-235.35005));
#205589=CARTESIAN_POINT('Ctrl Pts',(-27.2067518411579,42.6544032575593,
-228.68335));
#205590=CARTESIAN_POINT('Ctrl Pts',(-31.7011009472754,46.5938202572852,
-222.01665));
#205591=CARTESIAN_POINT('Ctrl Pts',(-36.2028725106807,50.5716334315145,
-215.34995));
#205592=CARTESIAN_POINT('Ctrl Pts',(-36.2478902263148,50.6114115632568,
-215.283283));
#205593=CARTESIAN_POINT('Ctrl Pts',(-36.2929079419489,50.6511896949991,
-215.216616));
#205594=CARTESIAN_POINT('Ctrl Pts',(-36.3379256575829,50.6909678267414,
-215.149949));
#205595=CARTESIAN_POINT('Ctrl Pts',(-13.711356444076,39.6240660636921,-235.35005));
#205596=CARTESIAN_POINT('Ctrl Pts',(-16.3741503826813,43.8592570013518,
-228.68335));
#205597=CARTESIAN_POINT('Ctrl Pts',(-19.0446466451262,48.1913695751969,
-222.01665));
#205598=CARTESIAN_POINT('Ctrl Pts',(-21.7262765934597,52.6194725853171,
-215.34995));
#205599=CARTESIAN_POINT('Ctrl Pts',(-21.753092892943,52.6637536154183,-215.283283));
#205600=CARTESIAN_POINT('Ctrl Pts',(-21.7799091924264,52.7080346455195,
-215.216616));
#205601=CARTESIAN_POINT('Ctrl Pts',(-21.8067254919097,52.7523156756207,
-215.149949));
#205602=CARTESIAN_POINT('Ctrl Pts',(5.03069808033274E-14,40.0660654363212,
-235.350050000001));
#205603=CARTESIAN_POINT('Ctrl Pts',(2.50315176572591E-14,44.4636082157172,
-228.683350000001));
#205604=CARTESIAN_POINT('Ctrl Pts',(-3.67646180426256E-14,48.9871491221026,
-222.016650000001));
#205605=CARTESIAN_POINT('Ctrl Pts',(2.42861286636753E-14,53.6354775956494,
-215.34995));
#205606=CARTESIAN_POINT('Ctrl Pts',(2.48966361307383E-14,53.6819608803848,
-215.283283));
#205607=CARTESIAN_POINT('Ctrl Pts',(2.55071435978013E-14,53.7284441651203,
-215.216616));
#205608=CARTESIAN_POINT('Ctrl Pts',(2.61176510648644E-14,53.7749274498558,
-215.149949));
#205609=CARTESIAN_POINT('Ctrl Pts',(13.7113564440761,39.6240660636921,-235.35005));
#205610=CARTESIAN_POINT('Ctrl Pts',(16.3741503826814,43.8592570013518,-228.68335));
#205611=CARTESIAN_POINT('Ctrl Pts',(19.0446466451262,48.1913695751964,-222.01665));
#205612=CARTESIAN_POINT('Ctrl Pts',(21.7262765934598,52.619472585317,-215.34995));
#205613=CARTESIAN_POINT('Ctrl Pts',(21.7530928929431,52.6637536154182,-215.283283));
#205614=CARTESIAN_POINT('Ctrl Pts',(21.7799091924265,52.7080346455194,-215.216616));
#205615=CARTESIAN_POINT('Ctrl Pts',(21.8067254919098,52.7523156756206,-215.149949));
#205616=CARTESIAN_POINT('Ctrl Pts',(22.7175376169319,38.7537549124104,-235.350050000001));
#205617=CARTESIAN_POINT('Ctrl Pts',(27.206751841158,42.6544032575593,-228.68335));
#205618=CARTESIAN_POINT('Ctrl Pts',(31.7011009472754,46.5938202572849,-222.01665));
#205619=CARTESIAN_POINT('Ctrl Pts',(36.2028725106808,50.5716334315145,-215.34995));
#205620=CARTESIAN_POINT('Ctrl Pts',(36.2478902263149,50.6114115632568,-215.283283));
#205621=CARTESIAN_POINT('Ctrl Pts',(36.2929079419489,50.6511896949991,-215.216616));
#205622=CARTESIAN_POINT('Ctrl Pts',(36.337925657583,50.6909678267414,-215.149949));
#205623=CARTESIAN_POINT('Ctrl Pts',(27.1569075795173,38.1844371310006,-235.35005));
#205624=CARTESIAN_POINT('Ctrl Pts',(32.5837764342019,41.8536056393876,-228.68335));
#205625=CARTESIAN_POINT('Ctrl Pts',(38.0106452875494,45.5227741479461,-222.01665));
#205626=CARTESIAN_POINT('Ctrl Pts',(43.4375141409549,49.1919426564936,-215.34995));
#205627=CARTESIAN_POINT('Ctrl Pts',(43.491782829489,49.2286343415791,-215.283283));
#205628=CARTESIAN_POINT('Ctrl Pts',(43.546051518023,49.2653260266646,-215.216616));
#205629=CARTESIAN_POINT('Ctrl Pts',(43.6003202065571,49.30201771175,-215.149949));
#205630=CARTESIAN_POINT('Ctrl Pts',(24.4459324049495,-62.4902066935372,
-235.35005));
#205631=CARTESIAN_POINT('Ctrl Pts',(30.2944767260349,-66.7035224039814,
-228.68335));
#205632=CARTESIAN_POINT('Ctrl Pts',(36.1430210443398,-70.9168381145246,
-222.01665));
#205633=CARTESIAN_POINT('Ctrl Pts',(41.991565360621,-75.1301538251475,-215.34995));
#205634=CARTESIAN_POINT('Ctrl Pts',(42.0500508037838,-75.1722869822537,
-215.283283));
#205635=CARTESIAN_POINT('Ctrl Pts',(42.1085362469466,-75.21442013936,-215.216616));
#205636=CARTESIAN_POINT('Ctrl Pts',(42.1670216901095,-75.2565532964662,
-215.149949));
#205637=CARTESIAN_POINT('Ctrl Pts',(20.4621956228808,-62.6321691537996,
-235.35005));
#205638=CARTESIAN_POINT('Ctrl Pts',(25.267980358079,-66.8889339565476,-228.68335));
#205639=CARTESIAN_POINT('Ctrl Pts',(30.0738587790242,-71.1483055815339,
-222.01665));
#205640=CARTESIAN_POINT('Ctrl Pts',(34.8798403105591,-75.4102836728986,
-215.34995));
#205641=CARTESIAN_POINT('Ctrl Pts',(34.9279001258744,-75.4529034538122,
-215.283283));
#205642=CARTESIAN_POINT('Ctrl Pts',(34.9759599411898,-75.4955232347258,
-215.216616));
#205643=CARTESIAN_POINT('Ctrl Pts',(35.0240197565051,-75.5381430156395,
-215.149949));
#205644=CARTESIAN_POINT('Ctrl Pts',(12.3633338208145,-62.8510026026509,
-235.35005));
#205645=CARTESIAN_POINT('Ctrl Pts',(15.1854795229237,-67.1680657809434,
-228.68335));
#205646=CARTESIAN_POINT('Ctrl Pts',(18.0077657557388,-71.4916460146837,
-222.01665));
#205647=CARTESIAN_POINT('Ctrl Pts',(20.8302066559562,-75.8217424142497,
-215.34995));
#205648=CARTESIAN_POINT('Ctrl Pts',(20.8584310649584,-75.8650433782453,
-215.283283));
#205649=CARTESIAN_POINT('Ctrl Pts',(20.8866554739606,-75.908344342241,-215.216616));
#205650=CARTESIAN_POINT('Ctrl Pts',(20.9148798829627,-75.9516453062367,
-215.149949));
#205651=CARTESIAN_POINT('Ctrl Pts',(1.09287578986539E-13,-62.9629927582852,
-235.35005));
#205652=CARTESIAN_POINT('Ctrl Pts',(-1.49836951995733E-13,-67.3083190291539,
-228.683350000001));
#205653=CARTESIAN_POINT('Ctrl Pts',(-3.24284869790415E-13,-71.6621174720752,
-222.016650000001));
#205654=CARTESIAN_POINT('Ctrl Pts',(-5.36029554076834E-13,-76.0243869305461,
-215.349950000001));
#205655=CARTESIAN_POINT('Ctrl Pts',(-5.38147000919697E-13,-76.0680096251308,
-215.283283000001));
#205656=CARTESIAN_POINT('Ctrl Pts',(-5.40264447762562E-13,-76.1116323197155,
-215.216616000001));
#205657=CARTESIAN_POINT('Ctrl Pts',(-5.42381894605426E-13,-76.1552550143002,
-215.149949000001));
#205658=CARTESIAN_POINT('Ctrl Pts',(-12.3633338208143,-62.8510026026509,
-235.35005));
#205659=CARTESIAN_POINT('Ctrl Pts',(-15.185479522924,-67.1680657809432,
-228.68335));
#205660=CARTESIAN_POINT('Ctrl Pts',(-18.0077657557395,-71.4916460146835,
-222.01665));
#205661=CARTESIAN_POINT('Ctrl Pts',(-20.8302066559573,-75.8217424142497,
-215.34995));
#205662=CARTESIAN_POINT('Ctrl Pts',(-20.8584310649595,-75.8650433782453,
-215.283283));
#205663=CARTESIAN_POINT('Ctrl Pts',(-20.8866554739617,-75.908344342241,
-215.216616));
#205664=CARTESIAN_POINT('Ctrl Pts',(-20.9148798829638,-75.9516453062367,
-215.149949));
#205665=CARTESIAN_POINT('Ctrl Pts',(-20.4621956228805,-62.6321691537997,
-235.35005));
#205666=CARTESIAN_POINT('Ctrl Pts',(-25.2679803580793,-66.8889339565475,
-228.68335));
#205667=CARTESIAN_POINT('Ctrl Pts',(-30.0738587790249,-71.1483055815338,
-222.01665));
#205668=CARTESIAN_POINT('Ctrl Pts',(-34.8798403105602,-75.4102836728983,
-215.34995));
#205669=CARTESIAN_POINT('Ctrl Pts',(-34.9279001258756,-75.4529034538119,
-215.283283));
#205670=CARTESIAN_POINT('Ctrl Pts',(-34.975959941191,-75.4955232347256,
-215.216616));
#205671=CARTESIAN_POINT('Ctrl Pts',(-35.0240197565063,-75.5381430156392,
-215.149949));
#205672=CARTESIAN_POINT('Ctrl Pts',(-24.4459324049493,-62.4902066935372,
-235.35005));
#205673=CARTESIAN_POINT('Ctrl Pts',(-30.2944767260352,-66.7035224039813,
-228.68335));
#205674=CARTESIAN_POINT('Ctrl Pts',(-36.1430210443405,-70.9168381145244,
-222.01665));
#205675=CARTESIAN_POINT('Ctrl Pts',(-41.9915653606222,-75.1301538251473,
-215.34995));
#205676=CARTESIAN_POINT('Ctrl Pts',(-42.050050803785,-75.1722869822535,
-215.283283));
#205677=CARTESIAN_POINT('Ctrl Pts',(-42.1085362469478,-75.2144201393598,
-215.216616));
#205678=CARTESIAN_POINT('Ctrl Pts',(-42.1670216901106,-75.256553296466,
-215.149949));
#205679=CARTESIAN_POINT('Origin',(0.,-12.9675000200281,-218.35005));
#205680=CARTESIAN_POINT('Ctrl Pts',(-7312.83864083626,-22580.9607088348,
-376.75075701007));
#205681=CARTESIAN_POINT('Ctrl Pts',(-6830.77747415825,-19700.0678309805,
-349.81728900813));
#205682=CARTESIAN_POINT('Ctrl Pts',(-6348.71630748024,-16819.1749531262,
-322.88382100619));
#205683=CARTESIAN_POINT('Ctrl Pts',(-5866.65514080223,-13938.2820752719,
-295.95035300425));
#205684=CARTESIAN_POINT('Ctrl Pts',(-5625.62455746322,-12497.8356363448,
-282.483619003281));
#205685=CARTESIAN_POINT('Ctrl Pts',(-5384.59397412422,-11057.3891974177,
-269.01688500231));
#205686=CARTESIAN_POINT('Ctrl Pts',(-5143.56339078521,-9616.94275849054,
-255.55015100134));
#205687=CARTESIAN_POINT('Ctrl Pts',(-5023.0480991157,-8896.71953902697,
-248.816784000855));
#205688=CARTESIAN_POINT('Ctrl Pts',(-4902.5328074462,-8176.49631956341,
-242.083417000367));
#205689=CARTESIAN_POINT('Ctrl Pts',(-4782.0175157767,-7456.27310009984,
-235.350049999879));
#205690=CARTESIAN_POINT('Ctrl Pts',(-4662.69544481679,-6743.18080360126,
-228.683349999394));
#205691=CARTESIAN_POINT('Ctrl Pts',(-4544.55443977813,-6017.25926759624,
-222.01665));
#205692=CARTESIAN_POINT('Ctrl Pts',(-4428.35272571124,-5278.63127980493,
-215.34995));
#205693=CARTESIAN_POINT('Ctrl Pts',(-4427.19070857058,-5271.24499992702,
-215.283283));
#205694=CARTESIAN_POINT('Ctrl Pts',(-4426.02869142993,-5263.85872004911,
-215.216616));
#205695=CARTESIAN_POINT('Ctrl Pts',(-4424.86667428927,-5256.4724401712,
-215.149949));
#205696=CARTESIAN_POINT('Ctrl Pts',(-5678.44144856441,-17578.5062585325,
-376.75075700783));
#205697=CARTESIAN_POINT('Ctrl Pts',(-5307.04370444825,-15333.6138629625,
-349.817289006321));
#205698=CARTESIAN_POINT('Ctrl Pts',(-4935.64596033209,-13088.7214673926,
-322.883821004812));
#205699=CARTESIAN_POINT('Ctrl Pts',(-4564.24821621593,-10843.8290718226,
-295.950353003305));
#205700=CARTESIAN_POINT('Ctrl Pts',(-4378.54934415786,-9721.38287403765,
-282.48361900255));
#205701=CARTESIAN_POINT('Ctrl Pts',(-4192.85047209977,-8598.93667625267,
-269.016885001796));
#205702=CARTESIAN_POINT('Ctrl Pts',(-4007.1516000417,-7476.4904784677,-255.550151001042));
#205703=CARTESIAN_POINT('Ctrl Pts',(-3914.30216401265,-6915.26737957521,
-248.816784000665));
#205704=CARTESIAN_POINT('Ctrl Pts',(-3821.45272798362,-6354.04428068272,
-242.083417000286));
#205705=CARTESIAN_POINT('Ctrl Pts',(-3728.60329195457,-5792.82118179023,
-235.350049999906));
#205706=CARTESIAN_POINT('Ctrl Pts',(-3636.67315727236,-5237.15474724321,
-228.683349999529));
#205707=CARTESIAN_POINT('Ctrl Pts',(-3545.66125393428,-4671.51484522691,
-222.01665));
#205708=CARTESIAN_POINT('Ctrl Pts',(-3456.15702691661,-4095.9969311378,
-215.34995));
#205709=CARTESIAN_POINT('Ctrl Pts',(-3455.26198464644,-4090.24175199691,
-215.283283));
#205710=CARTESIAN_POINT('Ctrl Pts',(-3454.36694237628,-4084.48657285602,
-215.216616));
#205711=CARTESIAN_POINT('Ctrl Pts',(-3453.47190010611,-4078.73139371513,
-215.149949));
#205712=CARTESIAN_POINT('Ctrl Pts',(-4044.04425629255,-12576.0518082303,
-376.750757005589));
#205713=CARTESIAN_POINT('Ctrl Pts',(-3783.30993473824,-10967.1598949446,
-349.817289004512));
#205714=CARTESIAN_POINT('Ctrl Pts',(-3522.57561318394,-9358.26798165898,
-322.883821003436));
#205715=CARTESIAN_POINT('Ctrl Pts',(-3261.84129162964,-7749.37606837333,
-295.950353002358));
#205716=CARTESIAN_POINT('Ctrl Pts',(-3131.47413085249,-6944.9301117305,
-282.483619001821));
#205717=CARTESIAN_POINT('Ctrl Pts',(-3001.10697007533,-6140.48415508768,
-269.016885001282));
#205718=CARTESIAN_POINT('Ctrl Pts',(-2870.73980929818,-5336.03819844486,
-255.550151000744));
#205719=CARTESIAN_POINT('Ctrl Pts',(-2805.5562289096,-4933.81522012345,
-248.816784000475));
#205720=CARTESIAN_POINT('Ctrl Pts',(-2740.37264852102,-4531.59224180204,
-242.083417000204));
#205721=CARTESIAN_POINT('Ctrl Pts',(-2675.18906813245,-4129.36926348062,
-235.350049999933));
#205722=CARTESIAN_POINT('Ctrl Pts',(-2610.65086972792,-3731.12869088517,
-228.683349999664));
#205723=CARTESIAN_POINT('Ctrl Pts',(-2546.76806809043,-3325.77042285759,
-222.01665));
#205724=CARTESIAN_POINT('Ctrl Pts',(-2483.96132812197,-2913.36258247067,
-215.34995));
#205725=CARTESIAN_POINT('Ctrl Pts',(-2483.3332607223,-2909.2385040668,-215.283283));
#205726=CARTESIAN_POINT('Ctrl Pts',(-2482.70519332262,-2905.11442566293,
-215.216616));
#205727=CARTESIAN_POINT('Ctrl Pts',(-2482.07712592294,-2900.99034725906,
-215.149949));
#205728=CARTESIAN_POINT('Ctrl Pts',(-2409.6470640207,-7573.59735792804,
-376.750757003348));
#205729=CARTESIAN_POINT('Ctrl Pts',(-2259.57616502824,-6600.7059269267,
-349.817289002703));
#205730=CARTESIAN_POINT('Ctrl Pts',(-2109.5052660358,-5627.81449592536,
-322.883821002058));
#205731=CARTESIAN_POINT('Ctrl Pts',(-1959.43436704334,-4654.92306492402,
-295.950353001413));
#205732=CARTESIAN_POINT('Ctrl Pts',(-1884.39891754712,-4168.47734942335,
-282.483619001091));
#205733=CARTESIAN_POINT('Ctrl Pts',(-1809.36346805089,-3682.03163392268,
-269.016885000768));
#205734=CARTESIAN_POINT('Ctrl Pts',(-1734.32801855467,-3195.58591842202,
-255.550151000446));
#205735=CARTESIAN_POINT('Ctrl Pts',(-1696.81029380655,-2952.36306067169,
-248.816784000284));
#205736=CARTESIAN_POINT('Ctrl Pts',(-1659.29256905844,-2709.14020292135,
-242.083417000122));
#205737=CARTESIAN_POINT('Ctrl Pts',(-1621.77484431033,-2465.91734517101,
-235.35004999996));
#205738=CARTESIAN_POINT('Ctrl Pts',(-1584.62858218348,-2225.10263452712,
-228.683349999799));
#205739=CARTESIAN_POINT('Ctrl Pts',(-1547.87488224658,-1980.02600048826,
-222.01665));
#205740=CARTESIAN_POINT('Ctrl Pts',(-1511.76562932734,-1730.72823380353,
-215.34995));
#205741=CARTESIAN_POINT('Ctrl Pts',(-1511.40453679815,-1728.23525613669,
-215.283283));
#205742=CARTESIAN_POINT('Ctrl Pts',(-1511.04344426897,-1725.74227846985,
-215.216616));
#205743=CARTESIAN_POINT('Ctrl Pts',(-1510.68235173978,-1723.249300803,-215.149949));
#205744=CARTESIAN_POINT('Ctrl Pts',(-1864.84799993008,-5906.11254116062,
-376.750757002601));
#205745=CARTESIAN_POINT('Ctrl Pts',(-1751.66490845825,-5145.22127092072,
-349.8172890021));
#205746=CARTESIAN_POINT('Ctrl Pts',(-1638.48181698641,-4384.33000068082,
-322.883821001599));
#205747=CARTESIAN_POINT('Ctrl Pts',(-1525.29872551458,-3623.43873044092,
-295.950353001097));
#205748=CARTESIAN_POINT('Ctrl Pts',(-1468.70717977866,-3242.99309532097,
-282.483619000847));
#205749=CARTESIAN_POINT('Ctrl Pts',(-1412.11563404274,-2862.54746020102,
-269.016885000597));
#205750=CARTESIAN_POINT('Ctrl Pts',(-1355.52408830682,-2482.10182508107,
-255.550151000346));
#205751=CARTESIAN_POINT('Ctrl Pts',(-1327.22831543887,-2291.87900752109,
-248.816784000221));
#205752=CARTESIAN_POINT('Ctrl Pts',(-1298.93254257091,-2101.65618996112,
-242.083417000095));
#205753=CARTESIAN_POINT('Ctrl Pts',(-1270.63676970295,-1911.43337240115,
-235.350049999969));
#205754=CARTESIAN_POINT('Ctrl Pts',(-1242.621153002,-1723.09394907444,-228.683349999844));
#205755=CARTESIAN_POINT('Ctrl Pts',(-1214.91048696529,-1531.44452636515,
-222.01665));
#205756=CARTESIAN_POINT('Ctrl Pts',(-1187.70039639579,-1336.51678424783,
-215.34995));
#205757=CARTESIAN_POINT('Ctrl Pts',(-1187.4282954901,-1334.56750682665,
-215.283283));
#205758=CARTESIAN_POINT('Ctrl Pts',(-1187.15619458441,-1332.61822940548,
-215.216616));
#205759=CARTESIAN_POINT('Ctrl Pts',(-1186.88409367872,-1330.66895198431,
-215.149949));
#205760=CARTESIAN_POINT('Ctrl Pts',(-1320.04893583946,-4238.62772439321,
-376.750757001854));
#205761=CARTESIAN_POINT('Ctrl Pts',(-1243.75365188824,-3689.73661491475,
-349.817289001497));
#205762=CARTESIAN_POINT('Ctrl Pts',(-1167.45836793703,-3140.84550543629,
-322.883821001139));
#205763=CARTESIAN_POINT('Ctrl Pts',(-1091.16308398581,-2591.95439595782,
-295.950353000782));
#205764=CARTESIAN_POINT('Ctrl Pts',(-1053.0154420102,-2317.50884121858,
-282.483619000604));
#205765=CARTESIAN_POINT('Ctrl Pts',(-1014.86780003459,-2043.06328647936,
-269.016885000425));
#205766=CARTESIAN_POINT('Ctrl Pts',(-976.720158058986,-1768.61773174013,
-255.550151000247));
#205767=CARTESIAN_POINT('Ctrl Pts',(-957.646337071182,-1631.39495437051,
-248.816784000158));
#205768=CARTESIAN_POINT('Ctrl Pts',(-938.572516083378,-1494.17217700089,
-242.083417000068));
#205769=CARTESIAN_POINT('Ctrl Pts',(-919.498695095574,-1356.94939963128,
-235.350049999978));
#205770=CARTESIAN_POINT('Ctrl Pts',(-900.61372382052,-1221.08526362176,
-228.683349999889));
#205771=CARTESIAN_POINT('Ctrl Pts',(-881.946091684011,-1082.86305224204,
-222.01665));
#205772=CARTESIAN_POINT('Ctrl Pts',(-863.635163464249,-942.305334692116,
-215.34995));
#205773=CARTESIAN_POINT('Ctrl Pts',(-863.452054182054,-940.899757516616,
-215.283283));
#205774=CARTESIAN_POINT('Ctrl Pts',(-863.268944899859,-939.494180341118,
-215.216616));
#205775=CARTESIAN_POINT('Ctrl Pts',(-863.085835617665,-938.088603165619,
-215.149949));
#205776=CARTESIAN_POINT('Ctrl Pts',(-775.24987174884,-2571.1429076258,-376.750757001107));
#205777=CARTESIAN_POINT('Ctrl Pts',(-735.842395318242,-2234.25195890877,
-349.817289000894));
#205778=CARTESIAN_POINT('Ctrl Pts',(-696.434918887644,-1897.36101019174,
-322.883821000681));
#205779=CARTESIAN_POINT('Ctrl Pts',(-657.027442457046,-1560.47006147472,
-295.950353000467));
#205780=CARTESIAN_POINT('Ctrl Pts',(-637.323704241746,-1392.0245871162,
-282.483619000361));
#205781=CARTESIAN_POINT('Ctrl Pts',(-617.619966026447,-1223.57911275769,
-269.016885000254));
#205782=CARTESIAN_POINT('Ctrl Pts',(-597.916227811148,-1055.13363839918,
-255.550151000147));
#205783=CARTESIAN_POINT('Ctrl Pts',(-588.064358703498,-970.910901219922,
-248.816784000094));
#205784=CARTESIAN_POINT('Ctrl Pts',(-578.212489595849,-886.688164040665,
-242.083417000041));
#205785=CARTESIAN_POINT('Ctrl Pts',(-568.360620488199,-802.465426861409,
-235.350049999987));
#205786=CARTESIAN_POINT('Ctrl Pts',(-558.606294639041,-719.076578169076,
-228.683349999934));
#205787=CARTESIAN_POINT('Ctrl Pts',(-548.981696402727,-634.281578118933,
-222.01665));
#205788=CARTESIAN_POINT('Ctrl Pts',(-539.569930532705,-548.093885136405,
-215.34995));
#205789=CARTESIAN_POINT('Ctrl Pts',(-539.475812874006,-547.23200820658,
-215.283283));
#205790=CARTESIAN_POINT('Ctrl Pts',(-539.381695215308,-546.370131276755,
-215.216616));
#205791=CARTESIAN_POINT('Ctrl Pts',(-539.287577556609,-545.50825434693,
-215.149949));
#205792=CARTESIAN_POINT('Ctrl Pts',(-593.650183718634,-2015.31463536999,
-376.750757000858));
#205793=CARTESIAN_POINT('Ctrl Pts',(-566.538643128242,-1749.09040690678,
-349.817289000693));
#205794=CARTESIAN_POINT('Ctrl Pts',(-539.427102537849,-1482.86617844356,
-322.883821000528));
#205795=CARTESIAN_POINT('Ctrl Pts',(-512.315561947457,-1216.64194998035,
-295.950353000362));
#205796=CARTESIAN_POINT('Ctrl Pts',(-498.759791652261,-1083.52983574874,
-282.48361900028));
#205797=CARTESIAN_POINT('Ctrl Pts',(-485.204021357065,-950.417721517136,
-269.016885000197));
#205798=CARTESIAN_POINT('Ctrl Pts',(-471.648251061869,-817.305607285529,
-255.550151000114));
#205799=CARTESIAN_POINT('Ctrl Pts',(-464.87036591427,-750.749550169726,
-248.816784000073));
#205800=CARTESIAN_POINT('Ctrl Pts',(-458.092480766672,-684.193493053923,
-242.083417000031));
#205801=CARTESIAN_POINT('Ctrl Pts',(-451.314595619074,-617.637435938119,
-235.35004999999));
#205802=CARTESIAN_POINT('Ctrl Pts',(-444.603818245215,-551.740349684848,
-228.683349999949));
#205803=CARTESIAN_POINT('Ctrl Pts',(-437.993564642299,-484.754420077896,
-222.01665));
#205804=CARTESIAN_POINT('Ctrl Pts',(-431.54818622219,-416.690068617835,
-215.34995));
#205805=CARTESIAN_POINT('Ctrl Pts',(-431.48373243799,-416.009425103234,
-215.283283));
#205806=CARTESIAN_POINT('Ctrl Pts',(-431.419278653791,-415.328781588633,
-215.216616));
#205807=CARTESIAN_POINT('Ctrl Pts',(-431.354824869591,-414.648138074033,
-215.149949));
#205808=CARTESIAN_POINT('Ctrl Pts',(-412.050495688428,-1459.48636311419,
-376.750757000609));
#205809=CARTESIAN_POINT('Ctrl Pts',(-397.234890938242,-1263.92885490479,
-349.817289000492));
#205810=CARTESIAN_POINT('Ctrl Pts',(-382.419286188055,-1068.37134669538,
-322.883821000374));
#205811=CARTESIAN_POINT('Ctrl Pts',(-367.603681437869,-872.813838485983,
-295.950353000257));
#205812=CARTESIAN_POINT('Ctrl Pts',(-360.195879062775,-775.035084381282,
-282.483619000199));
#205813=CARTESIAN_POINT('Ctrl Pts',(-352.788076687683,-677.256330276581,
-269.016885000139));
#205814=CARTESIAN_POINT('Ctrl Pts',(-345.380274312589,-579.477576171881,
-255.550151000081));
#205815=CARTESIAN_POINT('Ctrl Pts',(-341.676373125042,-530.58819911953,
-248.816784000052));
#205816=CARTESIAN_POINT('Ctrl Pts',(-337.972471937496,-481.69882206718,
-242.083417000022));
#205817=CARTESIAN_POINT('Ctrl Pts',(-334.26857074995,-432.80944501483,-235.350049999993));
#205818=CARTESIAN_POINT('Ctrl Pts',(-330.601341851388,-384.404121200621,
-228.683349999963));
#205819=CARTESIAN_POINT('Ctrl Pts',(-327.005432881871,-335.22726203686,
-222.01665));
#205820=CARTESIAN_POINT('Ctrl Pts',(-323.526441911676,-285.286252099265,
-215.34995));
#205821=CARTESIAN_POINT('Ctrl Pts',(-323.491652001974,-284.786841999889,
-215.283283));
#205822=CARTESIAN_POINT('Ctrl Pts',(-323.456862092273,-284.287431900513,
-215.216616));
#205823=CARTESIAN_POINT('Ctrl Pts',(-323.422072182572,-283.788021801137,
-215.149949));
#205824=CARTESIAN_POINT('Ctrl Pts',(-230.450807658222,-903.658090858384,
-376.75075700036));
#205825=CARTESIAN_POINT('Ctrl Pts',(-227.931138748241,-778.767302902795,
-349.817289000291));
#205826=CARTESIAN_POINT('Ctrl Pts',(-225.411469838261,-653.876514947205,
-322.883821000222));
#205827=CARTESIAN_POINT('Ctrl Pts',(-222.891800928281,-528.985726991616,
-295.950353000152));
#205828=CARTESIAN_POINT('Ctrl Pts',(-221.63196647329,-466.540333013821,
-282.483619000117));
#205829=CARTESIAN_POINT('Ctrl Pts',(-220.3721320183,-404.094939036027,-269.016885000082));
#205830=CARTESIAN_POINT('Ctrl Pts',(-219.11229756331,-341.649545058231,
-255.550151000048));
#205831=CARTESIAN_POINT('Ctrl Pts',(-218.482380335815,-310.426848069334,
-248.816784000031));
#205832=CARTESIAN_POINT('Ctrl Pts',(-217.85246310832,-279.204151080437,
-242.083417000013));
#205833=CARTESIAN_POINT('Ctrl Pts',(-217.222545880824,-247.981454091539,
-235.350049999996));
#205834=CARTESIAN_POINT('Ctrl Pts',(-216.598865457562,-217.067892716394,
-228.683349999979));
#205835=CARTESIAN_POINT('Ctrl Pts',(-216.017301121443,-185.700103995824,
-222.01665));
#205836=CARTESIAN_POINT('Ctrl Pts',(-215.504697601161,-153.882435580695,
-215.34995));
#205837=CARTESIAN_POINT('Ctrl Pts',(-215.499571565958,-153.564258896543,
-215.283283));
#205838=CARTESIAN_POINT('Ctrl Pts',(-215.494445530756,-153.246082212392,
-215.216616));
#205839=CARTESIAN_POINT('Ctrl Pts',(-215.489319495554,-152.92790552824,
-215.149949));
#205840=CARTESIAN_POINT('Ctrl Pts',(-169.91757831482,-718.38200010645,-376.750757000277));
#205841=CARTESIAN_POINT('Ctrl Pts',(-171.496554684908,-617.046785568798,
-349.817289000224));
#205842=CARTESIAN_POINT('Ctrl Pts',(-173.075531054996,-515.711571031146,
-322.883821000171));
#205843=CARTESIAN_POINT('Ctrl Pts',(-174.654507425084,-414.376356493494,
-295.950353000117));
#205844=CARTESIAN_POINT('Ctrl Pts',(-175.443995610129,-363.708749224667,
-282.48361900009));
#205845=CARTESIAN_POINT('Ctrl Pts',(-176.233483795173,-313.041141955842,
-269.016885000063));
#205846=CARTESIAN_POINT('Ctrl Pts',(-177.022971980217,-262.373534687016,
-255.550151000037));
#205847=CARTESIAN_POINT('Ctrl Pts',(-177.417716072739,-237.039731052603,
-248.816784000024));
#205848=CARTESIAN_POINT('Ctrl Pts',(-177.812460165261,-211.70592741819,
-242.08341700001));
#205849=CARTESIAN_POINT('Ctrl Pts',(-178.207204257783,-186.372123783777,
-235.350049999997));
#205850=CARTESIAN_POINT('Ctrl Pts',(-178.598039992953,-161.289149888318,
-228.683349999984));
#205851=CARTESIAN_POINT('Ctrl Pts',(-179.021257201301,-135.857717982145,
-222.01665));
#205852=CARTESIAN_POINT('Ctrl Pts',(-179.497449497656,-110.081163407838,
-215.34995));
#205853=CARTESIAN_POINT('Ctrl Pts',(-179.50221142062,-109.823397862094,
-215.283283));
#205854=CARTESIAN_POINT('Ctrl Pts',(-179.506973343583,-109.565632316351,
-215.216616));
#205855=CARTESIAN_POINT('Ctrl Pts',(-179.511735266547,-109.307866770608,
-215.149949));
#205856=CARTESIAN_POINT('Ctrl Pts',(-109.384348971418,-533.105909354515,
-376.750757000194));
#205857=CARTESIAN_POINT('Ctrl Pts',(-115.061970621574,-455.3262682348,-349.817289000156));
#205858=CARTESIAN_POINT('Ctrl Pts',(-120.739592271731,-377.546627115086,
-322.883821000119));
#205859=CARTESIAN_POINT('Ctrl Pts',(-126.417213921888,-299.766985995371,
-295.950353000081));
#205860=CARTESIAN_POINT('Ctrl Pts',(-129.256024746967,-260.877165435514,
-282.483619000063));
#205861=CARTESIAN_POINT('Ctrl Pts',(-132.094835572045,-221.987344875657,
-269.016885000044));
#205862=CARTESIAN_POINT('Ctrl Pts',(-134.933646397123,-183.097524315799,
-255.550151000025));
#205863=CARTESIAN_POINT('Ctrl Pts',(-136.353051809663,-163.652614035871,
-248.816784000016));
#205864=CARTESIAN_POINT('Ctrl Pts',(-137.772457222202,-144.207703755942,
-242.083417000007));
#205865=CARTESIAN_POINT('Ctrl Pts',(-139.191862634741,-124.762793476013,
-235.350049999998));
#205866=CARTESIAN_POINT('Ctrl Pts',(-140.597214528344,-105.510407060242,
-228.683349999989));
#205867=CARTESIAN_POINT('Ctrl Pts',(-142.025213281158,-86.0153319684663,
-222.01665));
#205868=CARTESIAN_POINT('Ctrl Pts',(-143.490201394151,-66.2798912349809,
-215.34995));
#205869=CARTESIAN_POINT('Ctrl Pts',(-143.504851275281,-66.082536827646,
-215.283283));
#205870=CARTESIAN_POINT('Ctrl Pts',(-143.519501156411,-65.8851824203112,
-215.216616));
#205871=CARTESIAN_POINT('Ctrl Pts',(-143.534151037541,-65.6878280129763,
-215.149949));
#205872=CARTESIAN_POINT('Ctrl Pts',(-48.8511196280154,-347.82981860258,
-376.750757000109));
#205873=CARTESIAN_POINT('Ctrl Pts',(-58.6273865582409,-293.605750900803,
-349.817289000088));
#205874=CARTESIAN_POINT('Ctrl Pts',(-68.4036534884664,-239.381683199026,
-322.883821000067));
#205875=CARTESIAN_POINT('Ctrl Pts',(-78.179920418692,-185.157615497249,
-295.950353000046));
#205876=CARTESIAN_POINT('Ctrl Pts',(-83.0680538838047,-158.04558164636,
-282.483619000036));
#205877=CARTESIAN_POINT('Ctrl Pts',(-87.9561873489175,-130.933547795471,
-269.016885000025));
#205878=CARTESIAN_POINT('Ctrl Pts',(-92.8443208140303,-103.821513944583,
-255.550151000015));
#205879=CARTESIAN_POINT('Ctrl Pts',(-95.2883875465867,-90.2654970191385,
-248.816784000009));
#205880=CARTESIAN_POINT('Ctrl Pts',(-97.7324542791431,-76.7094800936942,
-242.083417000004));
#205881=CARTESIAN_POINT('Ctrl Pts',(-100.176521011699,-63.1534631682499,
-235.350049999999));
#205882=CARTESIAN_POINT('Ctrl Pts',(-102.596389063735,-49.7316642321664,
-228.683349999994));
#205883=CARTESIAN_POINT('Ctrl Pts',(-105.029169361015,-36.1729459547875,
-222.01665));
#205884=CARTESIAN_POINT('Ctrl Pts',(-107.482953290646,-22.4786190621241,
-215.34995));
#205885=CARTESIAN_POINT('Ctrl Pts',(-107.507491129942,-22.3416757931975,
-215.283283));
#205886=CARTESIAN_POINT('Ctrl Pts',(-107.532028969239,-22.2047325242709,
-215.216616));
#205887=CARTESIAN_POINT('Ctrl Pts',(-107.556566808535,-22.0677892553443,
-215.149949));
#205888=CARTESIAN_POINT('Ctrl Pts',(-28.673376513548,-286.071121685269,
-376.750757000082));
#205889=CARTESIAN_POINT('Ctrl Pts',(-39.8158585371298,-239.698911789471,
-349.817289000066));
#205890=CARTESIAN_POINT('Ctrl Pts',(-50.9583405607115,-193.326701893672,
-322.88382100005));
#205891=CARTESIAN_POINT('Ctrl Pts',(-62.1008225842933,-146.954491997874,
-295.950353000034));
#205892=CARTESIAN_POINT('Ctrl Pts',(-67.6720635960841,-123.768387049975,
-282.483619000027));
#205893=CARTESIAN_POINT('Ctrl Pts',(-73.243304607875,-100.582282102076,
-269.016885000018));
#205894=CARTESIAN_POINT('Ctrl Pts',(-78.8145456196659,-77.3961771541774,
-255.550151000011));
#205895=CARTESIAN_POINT('Ctrl Pts',(-81.6001661255613,-65.8031246802278,
-248.816784000007));
#205896=CARTESIAN_POINT('Ctrl Pts',(-84.3857866314568,-54.2100722062783,
-242.083417000003));
#205897=CARTESIAN_POINT('Ctrl Pts',(-87.1714071373522,-42.6170197323288,
-235.350049999999));
#205898=CARTESIAN_POINT('Ctrl Pts',(-89.9294472421992,-31.1387499561412,
-228.683349999995));
#205899=CARTESIAN_POINT('Ctrl Pts',(-92.6971547209677,-19.5588172835613,
-222.01665));
#205900=CARTESIAN_POINT('Ctrl Pts',(-95.4805372561441,-7.8781950045052,
-215.34995));
#205901=CARTESIAN_POINT('Ctrl Pts',(-95.508371081496,-7.76138878171465,
-215.283283));
#205902=CARTESIAN_POINT('Ctrl Pts',(-95.5362049068479,-7.64458255892409,
-215.216616));
#205903=CARTESIAN_POINT('Ctrl Pts',(-95.5640387321998,-7.52777633613354,
-215.149949));
#205904=CARTESIAN_POINT('Ctrl Pts',(-8.49563339908065,-224.312424767957,
-376.750757000054));
#205905=CARTESIAN_POINT('Ctrl Pts',(-21.0043305160186,-185.792072678138,
-349.817289000044));
#205906=CARTESIAN_POINT('Ctrl Pts',(-33.5130276329566,-147.271720588319,
-322.883821000033));
#205907=CARTESIAN_POINT('Ctrl Pts',(-46.0217247498946,-108.7513684985,-295.950353000022));
#205908=CARTESIAN_POINT('Ctrl Pts',(-52.2760733083635,-89.4911924535907,
-282.483619000017));
#205909=CARTESIAN_POINT('Ctrl Pts',(-58.5304218668325,-70.2310164086813,
-269.016885000012));
#205910=CARTESIAN_POINT('Ctrl Pts',(-64.7847704253015,-50.9708403637719,
-255.550151000007));
#205911=CARTESIAN_POINT('Ctrl Pts',(-67.911944704536,-41.3407523413171,
-248.816784000005));
#205912=CARTESIAN_POINT('Ctrl Pts',(-71.0391189837705,-31.7106643188625,
-242.083417000002));
#205913=CARTESIAN_POINT('Ctrl Pts',(-74.166293263005,-22.0805762964077,
-235.35005));
#205914=CARTESIAN_POINT('Ctrl Pts',(-77.2625054206629,-12.5458356801159,
-228.683349999997));
#205915=CARTESIAN_POINT('Ctrl Pts',(-80.3651400809202,-2.94468861233498,
-222.01665));
#205916=CARTESIAN_POINT('Ctrl Pts',(-83.4781212216425,6.72222905311371,
-215.34995));
#205917=CARTESIAN_POINT('Ctrl Pts',(-83.5092510330498,6.81889822976819,
-215.283283));
#205918=CARTESIAN_POINT('Ctrl Pts',(-83.5403808444571,6.91556740642268,
-215.216616));
#205919=CARTESIAN_POINT('Ctrl Pts',(-83.5715106558644,7.01223658307716,
-215.149949));
#205920=CARTESIAN_POINT('Ctrl Pts',(11.6821097153867,-162.553727850645,
-376.750757000025));
#205921=CARTESIAN_POINT('Ctrl Pts',(-2.1928024949075,-131.885233566805,
-349.81728900002));
#205922=CARTESIAN_POINT('Ctrl Pts',(-16.0677147052017,-101.216739282966,
-322.883821000016));
#205923=CARTESIAN_POINT('Ctrl Pts',(-29.9426269154959,-70.548244999126,
-295.95035300001));
#205924=CARTESIAN_POINT('Ctrl Pts',(-36.880083020643,-55.2139978572062,
-282.483619000008));
#205925=CARTESIAN_POINT('Ctrl Pts',(-43.81753912579,-39.8797507152863,-269.016885000005));
#205926=CARTESIAN_POINT('Ctrl Pts',(-50.7549952309371,-24.5455035733664,
-255.550151000003));
#205927=CARTESIAN_POINT('Ctrl Pts',(-54.2237232835107,-16.8783800024065,
-248.816784000002));
#205928=CARTESIAN_POINT('Ctrl Pts',(-57.6924513360842,-9.21125643144658,
-242.083417000001));
#205929=CARTESIAN_POINT('Ctrl Pts',(-61.1611793886578,-1.54413286048666,
-235.35005));
#205930=CARTESIAN_POINT('Ctrl Pts',(-64.5955635991267,6.04707859590932,
-228.683349999999));
#205931=CARTESIAN_POINT('Ctrl Pts',(-68.0331254408726,13.6694400588913,
-222.01665));
#205932=CARTESIAN_POINT('Ctrl Pts',(-71.4757051871408,21.3226531107326,
-215.34995));
#205933=CARTESIAN_POINT('Ctrl Pts',(-71.5101309846035,21.3991852412511,
-215.283283));
#205934=CARTESIAN_POINT('Ctrl Pts',(-71.5445567820663,21.4757173717695,
-215.216616));
#205935=CARTESIAN_POINT('Ctrl Pts',(-71.578982579529,21.5522495022879,-215.149949));
#205936=CARTESIAN_POINT('Ctrl Pts',(18.4080240868758,-141.967495544875,
-376.750757000016));
#205937=CARTESIAN_POINT('Ctrl Pts',(4.07770684546288,-113.916287196361,
-349.817289000013));
#205938=CARTESIAN_POINT('Ctrl Pts',(-10.25261039595,-85.865078847848,-322.88382100001));
#205939=CARTESIAN_POINT('Ctrl Pts',(-24.582927637363,-57.8138704993346,
-295.950353000006));
#205940=CARTESIAN_POINT('Ctrl Pts',(-31.7480862580694,-43.7882663250779,
-282.483619000005));
#205941=CARTESIAN_POINT('Ctrl Pts',(-38.9132448787759,-29.7626621508213,
-269.016885000003));
#205942=CARTESIAN_POINT('Ctrl Pts',(-46.0784034994824,-15.7370579765646,
-255.550151000002));
#205943=CARTESIAN_POINT('Ctrl Pts',(-49.6609828098356,-8.72425588943629,
-248.816784000002));
#205944=CARTESIAN_POINT('Ctrl Pts',(-53.2435621201888,-1.71145380230796,
-242.083417000001));
#205945=CARTESIAN_POINT('Ctrl Pts',(-56.826141430542,5.30134828482038,-235.35005));
#205946=CARTESIAN_POINT('Ctrl Pts',(-60.3732496586146,12.2447166879177,
-228.683349999999));
#205947=CARTESIAN_POINT('Ctrl Pts',(-63.9224538941901,19.2074829493001,
-222.01665));
#205948=CARTESIAN_POINT('Ctrl Pts',(-67.4748998423069,26.1894611299389,
-215.34995));
#205949=CARTESIAN_POINT('Ctrl Pts',(-67.5104243017881,26.2592809117453,
-215.283283));
#205950=CARTESIAN_POINT('Ctrl Pts',(-67.5459487612693,26.3291006935517,
-215.216616));
#205951=CARTESIAN_POINT('Ctrl Pts',(-67.5814732207505,26.3989204753581,
-215.149949));
#205952=CARTESIAN_POINT('Ctrl Pts',(25.1339384583649,-121.381263239104,
-376.750757000007));
#205953=CARTESIAN_POINT('Ctrl Pts',(10.3482161858333,-95.9473408259171,
-349.817289000005));
#205954=CARTESIAN_POINT('Ctrl Pts',(-4.4375060866984,-70.5134184127302,
-322.883821000004));
#205955=CARTESIAN_POINT('Ctrl Pts',(-19.22322835923,-45.0794959995432,-295.950353000003));
#205956=CARTESIAN_POINT('Ctrl Pts',(-26.6160894954959,-32.3625347929498,
-282.483619000002));
#205957=CARTESIAN_POINT('Ctrl Pts',(-34.0089506317617,-19.6455735863562,
-269.016885000001));
#205958=CARTESIAN_POINT('Ctrl Pts',(-41.4018117680275,-6.9286123797628,
-255.550151000001));
#205959=CARTESIAN_POINT('Ctrl Pts',(-45.0982423361605,-0.570131776466063,
-248.816784000001));
#205960=CARTESIAN_POINT('Ctrl Pts',(-48.7946729042934,5.78834882683067,
-242.083417));
#205961=CARTESIAN_POINT('Ctrl Pts',(-52.4911034724263,12.1468294301274,
-235.35005));
#205962=CARTESIAN_POINT('Ctrl Pts',(-56.1509357181025,18.4423547799261,
-228.68335));
#205963=CARTESIAN_POINT('Ctrl Pts',(-59.8117823475076,24.7455258397088,
-222.01665));
#205964=CARTESIAN_POINT('Ctrl Pts',(-63.4740944974731,31.0562691491453,
-215.34995));
#205965=CARTESIAN_POINT('Ctrl Pts',(-63.5107176189727,31.1193765822396,
-215.283283));
#205966=CARTESIAN_POINT('Ctrl Pts',(-63.5473407404724,31.1824840153339,
-215.216616));
#205967=CARTESIAN_POINT('Ctrl Pts',(-63.5839638619721,31.2455914484283,
-215.149949));
#205968=CARTESIAN_POINT('Ctrl Pts',(31.859852829854,-100.795030933333,-376.750756999998));
#205969=CARTESIAN_POINT('Ctrl Pts',(16.6187255262036,-77.9783944554729,
-349.817288999998));
#205970=CARTESIAN_POINT('Ctrl Pts',(1.37759822255324,-55.1617579776124,
-322.883820999999));
#205971=CARTESIAN_POINT('Ctrl Pts',(-13.8635290810972,-32.3451214997519,
-295.950352999999));
#205972=CARTESIAN_POINT('Ctrl Pts',(-21.4840927329223,-20.9368032608216,
-282.483618999999));
#205973=CARTESIAN_POINT('Ctrl Pts',(-29.1046563847475,-9.52848502189127,
-269.016885));
#205974=CARTESIAN_POINT('Ctrl Pts',(-36.7252200365728,1.87983321703902,
-255.550151));
#205975=CARTESIAN_POINT('Ctrl Pts',(-40.5355018624854,7.58399233650416,
-248.816784));
#205976=CARTESIAN_POINT('Ctrl Pts',(-44.345783688398,13.2881514559693,-242.083417));
#205977=CARTESIAN_POINT('Ctrl Pts',(-48.1560655143106,18.9923105754345,
-235.35005));
#205978=CARTESIAN_POINT('Ctrl Pts',(-51.9286217775904,24.6399928719346,
-228.68335));
#205979=CARTESIAN_POINT('Ctrl Pts',(-55.7011108008251,30.2835687301176,
-222.01665));
#205980=CARTESIAN_POINT('Ctrl Pts',(-59.4732891526392,35.9230771683515,
-215.34995));
#205981=CARTESIAN_POINT('Ctrl Pts',(-59.5110109361573,35.9794722527339,
-215.283283));
#205982=CARTESIAN_POINT('Ctrl Pts',(-59.5487327196755,36.0358673371162,
-215.216616));
#205983=CARTESIAN_POINT('Ctrl Pts',(-59.5864545031936,36.0922624214986,
-215.149949));
#205984=CARTESIAN_POINT('Ctrl Pts',(33.5413314227263,-95.6484728568909,
-376.750756999995));
#205985=CARTESIAN_POINT('Ctrl Pts',(18.1863528612963,-73.4861578628619,
-349.817288999997));
#205986=CARTESIAN_POINT('Ctrl Pts',(2.83137429986615,-51.3238428688329,
-322.883820999997));
#205987=CARTESIAN_POINT('Ctrl Pts',(-12.5236042615639,-29.161527874804,
-295.950352999998));
#205988=CARTESIAN_POINT('Ctrl Pts',(-20.201093542279,-18.0803703777895,
-282.483618999998));
#205989=CARTESIAN_POINT('Ctrl Pts',(-27.878582822994,-6.99921288077501,
-269.016884999999));
#205990=CARTESIAN_POINT('Ctrl Pts',(-35.556072103709,4.08194461623947,-255.550151));
#205991=CARTESIAN_POINT('Ctrl Pts',(-39.3948167440666,9.62252336474671,
-248.816784));
#205992=CARTESIAN_POINT('Ctrl Pts',(-43.2335613844241,15.163102113254,-242.083417));
#205993=CARTESIAN_POINT('Ctrl Pts',(-47.0723060247816,20.7036808617612,
-235.35005));
#205994=CARTESIAN_POINT('Ctrl Pts',(-50.8730432924624,26.1894023949367,
-228.683350000001));
#205995=CARTESIAN_POINT('Ctrl Pts',(-54.6734429141545,31.6680794527198,
-222.01665));
#205996=CARTESIAN_POINT('Ctrl Pts',(-58.4730878164307,37.1397791731531,
-215.34995));
#205997=CARTESIAN_POINT('Ctrl Pts',(-58.5110842654535,37.1944961703575,
-215.283283));
#205998=CARTESIAN_POINT('Ctrl Pts',(-58.5490807144762,37.2492131675618,
-215.216616));
#205999=CARTESIAN_POINT('Ctrl Pts',(-58.587077163499,37.3039301647661,-215.149949));
#206000=CARTESIAN_POINT('Ctrl Pts',(41.2301579830855,-81.5182387771612,
-376.750756999989));
#206001=CARTESIAN_POINT('Ctrl Pts',(24.8836555508694,-61.3775485896441,
-349.817288999991));
#206002=CARTESIAN_POINT('Ctrl Pts',(8.53715311865333,-41.2368584021269,
-322.883820999993));
#206003=CARTESIAN_POINT('Ctrl Pts',(-7.80934931356275,-21.0961682146096,
-295.950352999996));
#206004=CARTESIAN_POINT('Ctrl Pts',(-15.9826005296708,-11.025823120851,
-282.483618999996));
#206005=CARTESIAN_POINT('Ctrl Pts',(-24.1558517457789,-0.955478027092413,
-269.016884999998));
#206006=CARTESIAN_POINT('Ctrl Pts',(-32.3291029618869,9.1148670666662,-255.550150999998));
#206007=CARTESIAN_POINT('Ctrl Pts',(-36.4157285699409,14.1500396135455,
-248.816783999999));
#206008=CARTESIAN_POINT('Ctrl Pts',(-40.5023541779949,19.1852121604248,
-242.083416999999));
#206009=CARTESIAN_POINT('Ctrl Pts',(-44.588979786049,24.2203847073041,-235.35005));
#206010=CARTESIAN_POINT('Ctrl Pts',(-48.6351437544193,29.2057040606499,
-228.683350000001));
#206011=CARTESIAN_POINT('Ctrl Pts',(-52.6799616741893,34.1756765917424,
-222.01665));
#206012=CARTESIAN_POINT('Ctrl Pts',(-56.7225263698862,39.1304491224114,
-215.34995));
#206013=CARTESIAN_POINT('Ctrl Pts',(-56.7629520168432,39.1799968477181,
-215.283283));
#206014=CARTESIAN_POINT('Ctrl Pts',(-56.8033776638002,39.2295445730248,
-215.216616));
#206015=CARTESIAN_POINT('Ctrl Pts',(-56.8438033107571,39.2790922983315,
-215.149949));
#206016=CARTESIAN_POINT('Ctrl Pts',(61.5202391452974,-58.1759617860395,
-376.750756999982));
#206017=CARTESIAN_POINT('Ctrl Pts',(42.2054487986876,-41.4892341751692,
-349.817288999985));
#206018=CARTESIAN_POINT('Ctrl Pts',(22.8906584520777,-24.8025065642989,
-322.883820999989));
#206019=CARTESIAN_POINT('Ctrl Pts',(3.5758681054679,-8.11577895342853,-295.950352999993));
#206020=CARTESIAN_POINT('Ctrl Pts',(-6.08152706783702,0.227584852006628,
-282.483618999994));
#206021=CARTESIAN_POINT('Ctrl Pts',(-15.738922241142,8.57094865744179,-269.016884999996));
#206022=CARTESIAN_POINT('Ctrl Pts',(-25.3963174144469,16.9143124628769,
-255.550150999997));
#206023=CARTESIAN_POINT('Ctrl Pts',(-30.2250150010993,21.0859943655945,
-248.816783999999));
#206024=CARTESIAN_POINT('Ctrl Pts',(-35.0537125877518,25.2576762683121,
-242.083416999999));
#206025=CARTESIAN_POINT('Ctrl Pts',(-39.8824101744042,29.4293581710297,
-235.35005));
#206026=CARTESIAN_POINT('Ctrl Pts',(-44.6632988740601,33.5597362925323,
-228.683350000001));
#206027=CARTESIAN_POINT('Ctrl Pts',(-49.4410603210161,37.6624224459266,
-222.01665));
#206028=CARTESIAN_POINT('Ctrl Pts',(-54.214059251162,41.7376821955923,-215.34995));
#206029=CARTESIAN_POINT('Ctrl Pts',(-54.2617892404634,41.778434793089,-215.283283));
#206030=CARTESIAN_POINT('Ctrl Pts',(-54.3095192297649,41.8191873905857,
-215.216616));
#206031=CARTESIAN_POINT('Ctrl Pts',(-54.3572492190663,41.8599399880823,
-215.149949));
#206032=CARTESIAN_POINT('Ctrl Pts',(86.4308715045652,-38.5465561709931,
-376.75075699998));
#206033=CARTESIAN_POINT('Ctrl Pts',(63.394599877538,-24.7210691437011,-349.817288999984));
#206034=CARTESIAN_POINT('Ctrl Pts',(40.3583282505107,-10.8955821164091,
-322.883820999988));
#206035=CARTESIAN_POINT('Ctrl Pts',(17.3220566234834,2.92990491088294,-295.950352999991));
#206036=CARTESIAN_POINT('Ctrl Pts',(5.80392080996978,9.84264842452895,-282.483618999993));
#206037=CARTESIAN_POINT('Ctrl Pts',(-5.71421500354386,16.755391938175,-269.016884999996));
#206038=CARTESIAN_POINT('Ctrl Pts',(-17.2323508170575,23.668135451821,-255.550150999997));
#206039=CARTESIAN_POINT('Ctrl Pts',(-22.9914187238143,27.1245072086439,
-248.816783999998));
#206040=CARTESIAN_POINT('Ctrl Pts',(-28.7504866305711,30.580878965467,-242.083416999999));
#206041=CARTESIAN_POINT('Ctrl Pts',(-34.509554537328,34.03725072229,-235.35005));
#206042=CARTESIAN_POINT('Ctrl Pts',(-40.2116019697604,37.4594009765702,
-228.683350000001));
#206043=CARTESIAN_POINT('Ctrl Pts',(-45.9096065172025,40.8490096838924,
-222.01665));
#206044=CARTESIAN_POINT('Ctrl Pts',(-51.6016474095961,44.2063892516083,
-215.34995));
#206045=CARTESIAN_POINT('Ctrl Pts',(-51.65856781852,44.2399630472854,-215.283283));
#206046=CARTESIAN_POINT('Ctrl Pts',(-51.715488227444,44.2735368429626,-215.216616));
#206047=CARTESIAN_POINT('Ctrl Pts',(-51.7724086363679,44.3071106386397,
-215.149949));
#206048=CARTESIAN_POINT('Ctrl Pts',(101.966904434915,-30.8346247983327,
-376.750756999984));
#206049=CARTESIAN_POINT('Ctrl Pts',(76.6679969066201,-18.0147641121609,
-349.817288999987));
#206050=CARTESIAN_POINT('Ctrl Pts',(51.3690893783256,-5.19490342598898,
-322.88382099999));
#206051=CARTESIAN_POINT('Ctrl Pts',(26.070181850031,7.62495726018286,-295.950352999994));
#206052=CARTESIAN_POINT('Ctrl Pts',(13.4207280858838,14.0348876032688,-282.483618999995));
#206053=CARTESIAN_POINT('Ctrl Pts',(0.771274321736487,20.4448179463547,
-269.016884999996));
#206054=CARTESIAN_POINT('Ctrl Pts',(-11.8781794424108,26.8547482894406,
-255.550150999998));
#206055=CARTESIAN_POINT('Ctrl Pts',(-18.2029063244844,30.0597134609836,
-248.816783999999));
#206056=CARTESIAN_POINT('Ctrl Pts',(-24.5276332065581,33.2646786325266,
-242.083416999999));
#206057=CARTESIAN_POINT('Ctrl Pts',(-30.8523600886317,36.4696438040695,
-235.35005));
#206058=CARTESIAN_POINT('Ctrl Pts',(-37.1144659124669,39.6428766471814,
-228.683350000001));
#206059=CARTESIAN_POINT('Ctrl Pts',(-43.3732515923186,42.7902567304839,
-222.01665));
#206060=CARTESIAN_POINT('Ctrl Pts',(-49.6271914214616,45.9120323459617,
-215.34995));
#206061=CARTESIAN_POINT('Ctrl Pts',(-49.6897308197531,45.9432501021165,
-215.283283));
#206062=CARTESIAN_POINT('Ctrl Pts',(-49.7522702180445,45.9744678582713,
-215.216616));
#206063=CARTESIAN_POINT('Ctrl Pts',(-49.8148096163359,46.005685614426,-215.149949));
#206064=CARTESIAN_POINT('Ctrl Pts',(107.993804890233,-28.9044482397935,
-376.750756999988));
#206065=CARTESIAN_POINT('Ctrl Pts',(81.8862252383193,-16.2510537069498,
-349.81728899999));
#206066=CARTESIAN_POINT('Ctrl Pts',(55.7786455864053,-3.5976591741061,-322.883820999992));
#206067=CARTESIAN_POINT('Ctrl Pts',(29.6710659344913,9.05573535873763,-295.950352999994));
#206068=CARTESIAN_POINT('Ctrl Pts',(16.6172761085343,15.3824326251595,-282.483618999996));
#206069=CARTESIAN_POINT('Ctrl Pts',(3.5634862825773,21.7091298915814,-269.016884999997));
#206070=CARTESIAN_POINT('Ctrl Pts',(-9.49030354337971,28.0358271580032,
-255.550150999998));
#206071=CARTESIAN_POINT('Ctrl Pts',(-16.0171984563582,31.1991757912142,
-248.816783999999));
#206072=CARTESIAN_POINT('Ctrl Pts',(-22.5440933693367,34.3625244244251,
-242.083416999999));
#206073=CARTESIAN_POINT('Ctrl Pts',(-29.0709882823152,37.525873057636,-235.35005));
#206074=CARTESIAN_POINT('Ctrl Pts',(-35.5332604733831,40.6579014073498,
-228.683350000001));
#206075=CARTESIAN_POINT('Ctrl Pts',(-41.9930962102693,43.771133049519,-222.01665));
#206076=CARTESIAN_POINT('Ctrl Pts',(-48.4493862544499,46.8657485296993,
-215.34995));
#206077=CARTESIAN_POINT('Ctrl Pts',(-48.5139491548917,46.8966946845011,
-215.283283));
#206078=CARTESIAN_POINT('Ctrl Pts',(-48.5785120553335,46.9276408393029,
-215.216616));
#206079=CARTESIAN_POINT('Ctrl Pts',(-48.6430749557753,46.9585869941047,
-215.149949));
#206080=CARTESIAN_POINT('Ctrl Pts',(132.101406711508,-21.1837420056372,
-376.750756999997));
#206081=CARTESIAN_POINT('Ctrl Pts',(102.759138565116,-9.1962120861059,-349.817288999997));
#206082=CARTESIAN_POINT('Ctrl Pts',(73.4168704187245,2.79131783342537,-322.883820999998));
#206083=CARTESIAN_POINT('Ctrl Pts',(44.0746022723325,14.7788477529567,-295.950352999998));
#206084=CARTESIAN_POINT('Ctrl Pts',(29.4034681991366,20.7726127127223,-282.483618999999));
#206085=CARTESIAN_POINT('Ctrl Pts',(14.7323341259406,26.766377672488,-269.016884999999));
#206086=CARTESIAN_POINT('Ctrl Pts',(0.0612000527446133,32.7601426322536,
-255.550151));
#206087=CARTESIAN_POINT('Ctrl Pts',(-7.27436698385337,35.7570251121364,
-248.816784));
#206088=CARTESIAN_POINT('Ctrl Pts',(-14.6099340204513,38.7539075920192,
-242.083417));
#206089=CARTESIAN_POINT('Ctrl Pts',(-21.9455010570494,41.7507900719021,
-235.35005));
#206090=CARTESIAN_POINT('Ctrl Pts',(-29.2084387170473,44.7180004480236,
-228.68335));
#206091=CARTESIAN_POINT('Ctrl Pts',(-36.4724746820719,47.694638325659,-222.016650000001));
#206092=CARTESIAN_POINT('Ctrl Pts',(-43.7381655864028,50.6806132646498,
-215.34995));
#206093=CARTESIAN_POINT('Ctrl Pts',(-43.810822495446,50.7104730140397,-215.283283));
#206094=CARTESIAN_POINT('Ctrl Pts',(-43.8834794044894,50.7403327634296,
-215.216616));
#206095=CARTESIAN_POINT('Ctrl Pts',(-43.9561363135327,50.7701925128195,
-215.149949));
#206096=CARTESIAN_POINT('Ctrl Pts',(156.209008532784,-13.4630357714808,
-376.750757000006));
#206097=CARTESIAN_POINT('Ctrl Pts',(123.632051891913,-2.14137046526198,
-349.817289000005));
#206098=CARTESIAN_POINT('Ctrl Pts',(91.0550952510435,9.18029484095685,-322.883821000004));
#206099=CARTESIAN_POINT('Ctrl Pts',(58.4781386101737,20.5019601471757,-295.950353000003));
#206100=CARTESIAN_POINT('Ctrl Pts',(42.1896602897388,26.1627928002851,-282.483619000002));
#206101=CARTESIAN_POINT('Ctrl Pts',(25.9011819693039,31.8236254533946,-269.016885000001));
#206102=CARTESIAN_POINT('Ctrl Pts',(9.61270364886893,37.484458106504,-255.550151000001));
#206103=CARTESIAN_POINT('Ctrl Pts',(1.46846448865147,40.3148744330587,-248.816784000001));
#206104=CARTESIAN_POINT('Ctrl Pts',(-6.67577467156599,43.1452907596133,
-242.083417));
#206105=CARTESIAN_POINT('Ctrl Pts',(-14.8200138317834,45.9757070861681,
-235.35005));
#206106=CARTESIAN_POINT('Ctrl Pts',(-22.8836169607117,48.7780994886975,
-228.68335));
#206107=CARTESIAN_POINT('Ctrl Pts',(-30.9518531538746,51.6181436017991,
-222.016650000001));
#206108=CARTESIAN_POINT('Ctrl Pts',(-39.0269449183556,54.4954779996004,
-215.349950000001));
#206109=CARTESIAN_POINT('Ctrl Pts',(-39.1076958360005,54.5242513435783,
-215.283283000001));
#206110=CARTESIAN_POINT('Ctrl Pts',(-39.1884467536454,54.5530246875563,
-215.216616));
#206111=CARTESIAN_POINT('Ctrl Pts',(-39.2691976712902,54.5817980315343,
-215.149949000001));
#206112=CARTESIAN_POINT('Ctrl Pts',(180.316610354058,-5.74232953732446,
-376.750757000015));
#206113=CARTESIAN_POINT('Ctrl Pts',(144.50496521871,4.91347115558193,-349.817289000013));
#206114=CARTESIAN_POINT('Ctrl Pts',(108.693320083363,15.5692718484884,-322.88382100001));
#206115=CARTESIAN_POINT('Ctrl Pts',(72.8816749480149,26.2250725413947,-295.950353000006));
#206116=CARTESIAN_POINT('Ctrl Pts',(54.975852380341,31.5529728878479,-282.483619000005));
#206117=CARTESIAN_POINT('Ctrl Pts',(37.0700298126672,36.8808732343011,-269.016885000003));
#206118=CARTESIAN_POINT('Ctrl Pts',(19.1642072449932,42.2087735807543,-255.550151000002));
#206119=CARTESIAN_POINT('Ctrl Pts',(10.2112959611563,44.8727237539809,-248.816784000002));
#206120=CARTESIAN_POINT('Ctrl Pts',(1.25838467731937,47.5366739272075,-242.083417000001));
#206121=CARTESIAN_POINT('Ctrl Pts',(-7.69452660651757,50.2006241004341,
-235.35005));
#206122=CARTESIAN_POINT('Ctrl Pts',(-16.558795204376,52.8381985293713,-228.68335));
#206123=CARTESIAN_POINT('Ctrl Pts',(-25.4312316256772,55.5416488779391,
-222.016650000001));
#206124=CARTESIAN_POINT('Ctrl Pts',(-34.3157242503085,58.3103427345509,
-215.349950000001));
#206125=CARTESIAN_POINT('Ctrl Pts',(-34.4045691765549,58.3380296731169,
-215.283283000001));
#206126=CARTESIAN_POINT('Ctrl Pts',(-34.4934141028013,58.365716611683,-215.216616));
#206127=CARTESIAN_POINT('Ctrl Pts',(-34.5822590290476,58.3934035502491,
-215.149949000001));
#206128=CARTESIAN_POINT('Ctrl Pts',(252.639415817883,17.4197891651448,-376.750757000044));
#206129=CARTESIAN_POINT('Ctrl Pts',(207.123705199102,26.0779960181138,-349.817289000036));
#206130=CARTESIAN_POINT('Ctrl Pts',(161.60799458032,34.7362028710828,-322.883821000027));
#206131=CARTESIAN_POINT('Ctrl Pts',(116.092283961538,43.3944097240518,-295.950353000018));
#206132=CARTESIAN_POINT('Ctrl Pts',(93.3344286521477,47.7235131505364,-282.483619000015));
#206133=CARTESIAN_POINT('Ctrl Pts',(70.576573342757,52.0526165770209,-269.01688500001));
#206134=CARTESIAN_POINT('Ctrl Pts',(47.8187180333662,56.3817200035054,-255.550151000006));
#206135=CARTESIAN_POINT('Ctrl Pts',(36.4397903786708,58.5462717167477,-248.816784000004));
#206136=CARTESIAN_POINT('Ctrl Pts',(25.0608627239755,60.7108234299899,-242.083417000002));
#206137=CARTESIAN_POINT('Ctrl Pts',(13.6819350692801,62.8753751432322,-235.35005));
#206138=CARTESIAN_POINT('Ctrl Pts',(2.41567006463117,65.0184956513928,-228.683349999998));
#206139=CARTESIAN_POINT('Ctrl Pts',(-8.86936704108513,67.3121647063593,
-222.016650000002));
#206140=CARTESIAN_POINT('Ctrl Pts',(-20.1820622461672,69.7549369394024,
-215.349950000001));
#206141=CARTESIAN_POINT('Ctrl Pts',(-20.2951891982182,69.7793646617328,
-215.283283000001));
#206142=CARTESIAN_POINT('Ctrl Pts',(-20.4083161502691,69.8037923840631,
-215.216616));
#206143=CARTESIAN_POINT('Ctrl Pts',(-20.5214431023201,69.8282201063935,
-215.149949000001));
#206144=CARTESIAN_POINT('Ctrl Pts',(324.962221281708,40.581907867614,-376.750757000072));
#206145=CARTESIAN_POINT('Ctrl Pts',(269.742445179492,47.2425208806457,-349.817289000059));
#206146=CARTESIAN_POINT('Ctrl Pts',(214.522669077277,53.9031338936774,-322.883821000045));
#206147=CARTESIAN_POINT('Ctrl Pts',(159.302892975062,60.563746906709,-295.950353000031));
#206148=CARTESIAN_POINT('Ctrl Pts',(131.693004923954,63.8940534132249,-282.483619000024));
#206149=CARTESIAN_POINT('Ctrl Pts',(104.083116872847,67.2243599197407,-269.016885000017));
#206150=CARTESIAN_POINT('Ctrl Pts',(76.4732288217392,70.5546664262565,-255.55015100001));
#206151=CARTESIAN_POINT('Ctrl Pts',(62.6682847961853,72.2198196795144,-248.816784000007));
#206152=CARTESIAN_POINT('Ctrl Pts',(48.8633407706315,73.8849729327724,-242.083417000003));
#206153=CARTESIAN_POINT('Ctrl Pts',(35.0583967450777,75.5501261860303,-235.35005));
#206154=CARTESIAN_POINT('Ctrl Pts',(21.3901353336382,77.1987927734144,-228.683349999997));
#206155=CARTESIAN_POINT('Ctrl Pts',(7.69249754350693,79.0826805347794,-222.016650000002));
#206156=CARTESIAN_POINT('Ctrl Pts',(-6.0484002420259,81.199531144254,-215.349950000001));
#206157=CARTESIAN_POINT('Ctrl Pts',(-6.18580921988141,81.2206996503486,
-215.283283000001));
#206158=CARTESIAN_POINT('Ctrl Pts',(-6.32321819773692,81.2418681564432,
-215.216616000001));
#206159=CARTESIAN_POINT('Ctrl Pts',(-6.46062717559243,81.2630366625378,
-215.149949000001));
#206160=CARTESIAN_POINT('Ctrl Pts',(397.285026745533,63.7440265700833,-376.750757000099));
#206161=CARTESIAN_POINT('Ctrl Pts',(332.361185159884,68.4070457431775,-349.81728900008));
#206162=CARTESIAN_POINT('Ctrl Pts',(267.437343574235,73.0700649162719,-322.883821000062));
#206163=CARTESIAN_POINT('Ctrl Pts',(202.513501988586,77.7330840893662,-295.950353000043));
#206164=CARTESIAN_POINT('Ctrl Pts',(170.051581195761,80.0645936759133,-282.483619000033));
#206165=CARTESIAN_POINT('Ctrl Pts',(137.589660402937,82.3961032624605,-269.016885000024));
#206166=CARTESIAN_POINT('Ctrl Pts',(105.127739610112,84.7276128490076,-255.550151000015));
#206167=CARTESIAN_POINT('Ctrl Pts',(88.8967792136999,85.8933676422812,-248.81678400001));
#206168=CARTESIAN_POINT('Ctrl Pts',(72.6658188172876,87.0591224355548,-242.083417000005));
#206169=CARTESIAN_POINT('Ctrl Pts',(56.4348584208753,88.2248772288284,-235.35005));
#206170=CARTESIAN_POINT('Ctrl Pts',(40.3646006026454,89.3790898954359,-228.683349999995));
#206171=CARTESIAN_POINT('Ctrl Pts',(24.254362128099,90.8531963631996,-222.016650000002));
#206172=CARTESIAN_POINT('Ctrl Pts',(8.08526176211542,92.6441253491055,-215.349950000002));
#206173=CARTESIAN_POINT('Ctrl Pts',(7.92357075845534,92.6620346389644,-215.283283000002));
#206174=CARTESIAN_POINT('Ctrl Pts',(7.76187975479526,92.6799439288233,-215.216616000002));
#206175=CARTESIAN_POINT('Ctrl Pts',(7.60018875113518,92.6978532186822,-215.149949000001));
#206176=CARTESIAN_POINT('Ctrl Pts',(614.253443137008,133.230382677491,-376.750757000185));
#206177=CARTESIAN_POINT('Ctrl Pts',(520.217405101058,131.900620330773,-349.81728900015));
#206178=CARTESIAN_POINT('Ctrl Pts',(426.181367065107,130.570857984055,-322.883821000115));
#206179=CARTESIAN_POINT('Ctrl Pts',(332.145329029157,129.241095637338,-295.950353000079));
#206180=CARTESIAN_POINT('Ctrl Pts',(285.127310011182,128.576214463979,-282.483619000062));
#206181=CARTESIAN_POINT('Ctrl Pts',(238.109290993206,127.91133329062,-269.016885000044));
#206182=CARTESIAN_POINT('Ctrl Pts',(191.091271975231,127.246452117261,-255.550151000026));
#206183=CARTESIAN_POINT('Ctrl Pts',(167.582262466243,126.914011530581,-248.816784000018));
#206184=CARTESIAN_POINT('Ctrl Pts',(144.073252957256,126.581570943902,-242.083417000009));
#206185=CARTESIAN_POINT('Ctrl Pts',(120.564243448268,126.249130357223,-235.35005));
#206186=CARTESIAN_POINT('Ctrl Pts',(97.2879964096667,125.9199812615,-228.683349999992));
#206187=CARTESIAN_POINT('Ctrl Pts',(73.9399558818752,126.16474384846,-222.016650000005));
#206188=CARTESIAN_POINT('Ctrl Pts',(50.4862477745394,126.97790796366,-215.349950000003));
#206189=CARTESIAN_POINT('Ctrl Pts',(50.2517106934656,126.986039604812,-215.283283000003));
#206190=CARTESIAN_POINT('Ctrl Pts',(50.0171736123918,126.994171245964,-215.216616000002));
#206191=CARTESIAN_POINT('Ctrl Pts',(49.782636531318,127.002302887115,-215.149949000002));
#206192=CARTESIAN_POINT('Ctrl Pts',(831.221859528483,202.716738784898,-376.75075700027));
#206193=CARTESIAN_POINT('Ctrl Pts',(708.073625042231,195.394194918369,-349.817289000218));
#206194=CARTESIAN_POINT('Ctrl Pts',(584.92539055598,188.071651051839,-322.883821000167));
#206195=CARTESIAN_POINT('Ctrl Pts',(461.777156069728,180.749107185309,-295.950353000116));
#206196=CARTESIAN_POINT('Ctrl Pts',(400.203038826602,177.087835252044,-282.48361900009));
#206197=CARTESIAN_POINT('Ctrl Pts',(338.628921583476,173.426563318779,-269.016885000064));
#206198=CARTESIAN_POINT('Ctrl Pts',(277.05480434035,169.765291385514,-255.550151000039));
#206199=CARTESIAN_POINT('Ctrl Pts',(246.267745718787,167.934655418882,-248.816784000026));
#206200=CARTESIAN_POINT('Ctrl Pts',(215.480687097224,166.10401945225,-242.083417000013));
#206201=CARTESIAN_POINT('Ctrl Pts',(184.693628475661,164.273383485617,-235.35005));
#206202=CARTESIAN_POINT('Ctrl Pts',(154.211392216688,162.460872627565,-228.683349999988));
#206203=CARTESIAN_POINT('Ctrl Pts',(123.625549635651,161.47629133372,-222.016650000007));
#206204=CARTESIAN_POINT('Ctrl Pts',(92.8872337869633,161.311690578215,-215.349950000004));
#206205=CARTESIAN_POINT('Ctrl Pts',(92.5798506284758,161.31004457066,-215.283283000004));
#206206=CARTESIAN_POINT('Ctrl Pts',(92.2724674699883,161.308398563104,-215.216616000004));
#206207=CARTESIAN_POINT('Ctrl Pts',(91.9650843115009,161.306752555549,-215.149949000004));
#206208=CARTESIAN_POINT('Ctrl Pts',(1048.19027591996,272.203094892306,-376.750757000354));
#206209=CARTESIAN_POINT('Ctrl Pts',(895.929844983404,258.887769505964,-349.817289000287));
#206210=CARTESIAN_POINT('Ctrl Pts',(743.669414046851,245.572444119622,-322.883821000219));
#206211=CARTESIAN_POINT('Ctrl Pts',(591.408983110298,232.257118733281,-295.950353000152));
#206212=CARTESIAN_POINT('Ctrl Pts',(515.278767642022,225.59945604011,-282.483619000118));
#206213=CARTESIAN_POINT('Ctrl Pts',(439.148552173745,218.941793346939,-269.016885000084));
#206214=CARTESIAN_POINT('Ctrl Pts',(363.018336705469,212.284130653768,-255.550151000051));
#206215=CARTESIAN_POINT('Ctrl Pts',(324.953228971331,208.955299307182,-248.816784000034));
#206216=CARTESIAN_POINT('Ctrl Pts',(286.888121237192,205.626467960597,-242.083417000017));
#206217=CARTESIAN_POINT('Ctrl Pts',(248.823013503054,202.297636614011,-235.35005));
#206218=CARTESIAN_POINT('Ctrl Pts',(211.134788023709,199.001763993629,-228.683349999984));
#206219=CARTESIAN_POINT('Ctrl Pts',(173.311143389428,196.787838818981,-222.016650000008));
#206220=CARTESIAN_POINT('Ctrl Pts',(135.288219799387,195.64547319277,-215.349950000004));
#206221=CARTESIAN_POINT('Ctrl Pts',(134.907990563486,195.634049536507,-215.283283000005));
#206222=CARTESIAN_POINT('Ctrl Pts',(134.527761327585,195.622625880244,-215.216616000005));
#206223=CARTESIAN_POINT('Ctrl Pts',(134.147532091684,195.611202223982,-215.149949000005));
#206224=CARTESIAN_POINT('Ctrl Pts',(1699.09552509438,480.662163214529,-376.75075700061));
#206225=CARTESIAN_POINT('Ctrl Pts',(1459.49850480692,449.368493268751,-349.817289000493));
#206226=CARTESIAN_POINT('Ctrl Pts',(1219.90148451947,418.074823322972,-322.883821000378));
#206227=CARTESIAN_POINT('Ctrl Pts',(980.30446423201,386.781153377194,-295.950353000261));
#206228=CARTESIAN_POINT('Ctrl Pts',(860.505954088282,371.134318404306,-282.483619000203));
#206229=CARTESIAN_POINT('Ctrl Pts',(740.707443944553,355.487483431416,-269.016885000145));
#206230=CARTESIAN_POINT('Ctrl Pts',(620.908933800825,339.840648458528,-255.550151000087));
#206231=CARTESIAN_POINT('Ctrl Pts',(561.009678728961,332.017230972083,-248.816784000058));
#206232=CARTESIAN_POINT('Ctrl Pts',(501.110423657097,324.193813485639,-242.083417000029));
#206233=CARTESIAN_POINT('Ctrl Pts',(441.211168585233,316.370395999194,-235.35005));
#206234=CARTESIAN_POINT('Ctrl Pts',(381.904975444773,308.624438091823,-228.683349999972));
#206235=CARTESIAN_POINT('Ctrl Pts',(322.367924650756,302.722481274762,-222.016650000015));
#206236=CARTESIAN_POINT('Ctrl Pts',(262.491177836659,298.646821036434,-215.349950000008));
#206237=CARTESIAN_POINT('Ctrl Pts',(261.892410368517,298.60606443405,-215.283283000008));
#206238=CARTESIAN_POINT('Ctrl Pts',(261.293642900374,298.565307831665,-215.216616000008));
#206239=CARTESIAN_POINT('Ctrl Pts',(260.694875432232,298.524551229281,-215.149949000007));
#206240=CARTESIAN_POINT('Ctrl Pts',(2350.0007742688,689.121231536752,-376.750757000865));
#206241=CARTESIAN_POINT('Ctrl Pts',(2023.06716463044,639.849217031537,-349.8172890007));
#206242=CARTESIAN_POINT('Ctrl Pts',(1696.13355499208,590.577202526323,-322.883821000536));
#206243=CARTESIAN_POINT('Ctrl Pts',(1369.19994535372,541.305188021109,-295.95035300037));
#206244=CARTESIAN_POINT('Ctrl Pts',(1205.73314053454,516.669180768502,-282.483619000288));
#206245=CARTESIAN_POINT('Ctrl Pts',(1042.26633571536,492.033173515894,-269.016885000205));
#206246=CARTESIAN_POINT('Ctrl Pts',(878.799530896182,467.397166263287,-255.550151000123));
#206247=CARTESIAN_POINT('Ctrl Pts',(797.066128486591,455.079162636984,-248.816784000082));
#206248=CARTESIAN_POINT('Ctrl Pts',(715.332726077001,442.76115901068,-242.083417000041));
#206249=CARTESIAN_POINT('Ctrl Pts',(633.599323667412,430.443155384376,-235.35005));
#206250=CARTESIAN_POINT('Ctrl Pts',(552.675162865837,418.247112190016,-228.68334999996));
#206251=CARTESIAN_POINT('Ctrl Pts',(471.424705912085,408.657123730544,-222.016650000021));
#206252=CARTESIAN_POINT('Ctrl Pts',(389.694135873931,401.648168880098,-215.34995000001));
#206253=CARTESIAN_POINT('Ctrl Pts',(388.876830173548,401.578079331591,-215.28328300001));
#206254=CARTESIAN_POINT('Ctrl Pts',(388.059524473164,401.507989783086,-215.216616000011));
#206255=CARTESIAN_POINT('Ctrl Pts',(387.242218772781,401.43790023458,-215.149949000011));
#206256=CARTESIAN_POINT('Ctrl Pts',(3000.90602344323,897.580299858975,-376.75075700112));
#206257=CARTESIAN_POINT('Ctrl Pts',(2586.63582445396,830.329940794324,-349.817289000906));
#206258=CARTESIAN_POINT('Ctrl Pts',(2172.36562546469,763.079581729674,-322.883821000693));
#206259=CARTESIAN_POINT('Ctrl Pts',(1758.09542647544,695.829222665023,-295.95035300048));
#206260=CARTESIAN_POINT('Ctrl Pts',(1550.9603269808,662.204043132698,-282.483619000373));
#206261=CARTESIAN_POINT('Ctrl Pts',(1343.82522748617,628.578863600373,-269.016885000266));
#206262=CARTESIAN_POINT('Ctrl Pts',(1136.69012799154,594.953684068047,-255.55015100016));
#206263=CARTESIAN_POINT('Ctrl Pts',(1033.12257824422,578.141094301885,-248.816784000106));
#206264=CARTESIAN_POINT('Ctrl Pts',(929.555028496906,561.328504535722,-242.083417000053));
#206265=CARTESIAN_POINT('Ctrl Pts',(825.98747874959,544.515914769559,-235.35005));
#206266=CARTESIAN_POINT('Ctrl Pts',(723.445350286901,527.86978628821,-228.683349999948));
#206267=CARTESIAN_POINT('Ctrl Pts',(620.481487173413,514.591766186325,-222.016650000027));
#206268=CARTESIAN_POINT('Ctrl Pts',(516.897093911203,504.649516723762,-215.349950000014));
#206269=CARTESIAN_POINT('Ctrl Pts',(515.861249978578,504.550094229134,-215.283283000013));
#206270=CARTESIAN_POINT('Ctrl Pts',(514.825406045954,504.450671734507,-215.216616000014));
#206271=CARTESIAN_POINT('Ctrl Pts',(513.789562113329,504.351249239879,-215.149949000014));
#206272=CARTESIAN_POINT('Ctrl Pts',(4953.62177096649,1522.95750482565,-376.750757001886));
#206273=CARTESIAN_POINT('Ctrl Pts',(4277.34180392452,1401.77211208268,-349.817289001526));
#206274=CARTESIAN_POINT('Ctrl Pts',(3601.06183688254,1280.58671933972,-322.883821001167));
#206275=CARTESIAN_POINT('Ctrl Pts',(2924.78186984057,1159.40132659677,-295.950353000808));
#206276=CARTESIAN_POINT('Ctrl Pts',(2586.64188631958,1098.80863022529,-282.483619000628));
#206277=CARTESIAN_POINT('Ctrl Pts',(2248.50190279859,1038.21593385381,-269.016885000448));
#206278=CARTESIAN_POINT('Ctrl Pts',(1910.36191927761,977.623237482327,-255.550151000268));
#206279=CARTESIAN_POINT('Ctrl Pts',(1741.29192751712,947.326889296587,-248.816784000179));
#206280=CARTESIAN_POINT('Ctrl Pts',(1572.22193575662,917.030541110847,-242.08341700009));
#206281=CARTESIAN_POINT('Ctrl Pts',(1403.15194399613,886.734192925108,-235.35005));
#206282=CARTESIAN_POINT('Ctrl Pts',(1235.75591255009,856.737808582791,-228.683349999911));
#206283=CARTESIAN_POINT('Ctrl Pts',(1067.6518309574,832.395693553669,-222.016650000045));
#206284=CARTESIAN_POINT('Ctrl Pts',(898.505968023019,813.653560254753,-215.349950000023));
#206285=CARTESIAN_POINT('Ctrl Pts',(896.814509393671,813.466138921761,-215.283283000022));
#206286=CARTESIAN_POINT('Ctrl Pts',(895.123050764323,813.278717588769,-215.216616000022));
#206287=CARTESIAN_POINT('Ctrl Pts',(893.431592134975,813.091296255777,-215.149949000023));
#206288=CARTESIAN_POINT('Ctrl Pts',(6906.33751848976,2148.33470979231,-376.750757002651));
#206289=CARTESIAN_POINT('Ctrl Pts',(5968.04778339507,1973.21428337105,-349.817289002145));
#206290=CARTESIAN_POINT('Ctrl Pts',(5029.75804830038,1798.09385694977,-322.883821001641));
#206291=CARTESIAN_POINT('Ctrl Pts',(4091.4683132057,1622.97343052851,-295.950353001135));
#206292=CARTESIAN_POINT('Ctrl Pts',(3622.32344565836,1535.41321731788,-282.483619000883));
#206293=CARTESIAN_POINT('Ctrl Pts',(3153.17857811102,1447.85300410724,-269.01688500063));
#206294=CARTESIAN_POINT('Ctrl Pts',(2684.03371056368,1360.29279089661,-255.550151000377));
#206295=CARTESIAN_POINT('Ctrl Pts',(2449.46127679,1316.51268429129,-248.816784000251));
#206296=CARTESIAN_POINT('Ctrl Pts',(2214.88884301634,1272.73257768597,-242.083417000126));
#206297=CARTESIAN_POINT('Ctrl Pts',(1980.31640924266,1228.95247108066,-235.35005));
#206298=CARTESIAN_POINT('Ctrl Pts',(1748.06647481329,1185.60583087737,-228.683349999876));
#206299=CARTESIAN_POINT('Ctrl Pts',(1514.82217474138,1150.19962092101,-222.016650000063));
#206300=CARTESIAN_POINT('Ctrl Pts',(1280.11484213483,1122.65760378574,-215.349950000032));
#206301=CARTESIAN_POINT('Ctrl Pts',(1277.76776880876,1122.38218361439,-215.283283000032));
#206302=CARTESIAN_POINT('Ctrl Pts',(1275.42069548269,1122.10676344303,-215.216616000032));
#206303=CARTESIAN_POINT('Ctrl Pts',(1273.07362215662,1121.83134327167,-215.149949000032));
#206304=CARTESIAN_POINT('Ctrl Pts',(8859.05326601302,2773.71191475898,-376.750757003417));
#206305=CARTESIAN_POINT('Ctrl Pts',(7658.75376286563,2544.6564546594,-349.817289002765));
#206306=CARTESIAN_POINT('Ctrl Pts',(6458.45425971823,2315.60099455983,-322.883821002114));
#206307=CARTESIAN_POINT('Ctrl Pts',(5258.15475657084,2086.54553446025,-295.950353001463));
#206308=CARTESIAN_POINT('Ctrl Pts',(4658.00500499714,1972.01780441047,-282.483619001138));
#206309=CARTESIAN_POINT('Ctrl Pts',(4057.85525342344,1857.49007436067,-269.016885000812));
#206310=CARTESIAN_POINT('Ctrl Pts',(3457.70550184975,1742.96234431089,-255.550151000486));
#206311=CARTESIAN_POINT('Ctrl Pts',(3157.6306260629,1685.69847928599,-248.816784000324));
#206312=CARTESIAN_POINT('Ctrl Pts',(2857.55575027604,1628.4346142611,-242.083417000162));
#206313=CARTESIAN_POINT('Ctrl Pts',(2557.4808744892,1571.17074923621,-235.35005));
#206314=CARTESIAN_POINT('Ctrl Pts',(2260.37703707648,1514.47385317195,-228.683349999839));
#206315=CARTESIAN_POINT('Ctrl Pts',(1961.99251852537,1468.00354828836,-222.01665000008));
#206316=CARTESIAN_POINT('Ctrl Pts',(1661.72371624665,1431.66164731674,-215.349950000041));
#206317=CARTESIAN_POINT('Ctrl Pts',(1658.72102822386,1431.29822830702,-215.28328300004));
#206318=CARTESIAN_POINT('Ctrl Pts',(1655.71834020106,1430.93480929729,-215.216616000041));
#206319=CARTESIAN_POINT('Ctrl Pts',(1652.71565217826,1430.57139028757,-215.149949000041));
#206320=CARTESIAN_POINT('Ctrl Pts',(14717.2005085828,4649.84352965899,-376.750757005713));
#206321=CARTESIAN_POINT('Ctrl Pts',(12730.8717012773,4258.98296852449,-349.817289004623));
#206322=CARTESIAN_POINT('Ctrl Pts',(10744.5428939718,3868.12240738999,-322.883821003535));
#206323=CARTESIAN_POINT('Ctrl Pts',(8758.21408666624,3477.26184625548,-295.950353002446));
#206324=CARTESIAN_POINT('Ctrl Pts',(7765.04968301347,3281.83156568823,-282.483619001902));
#206325=CARTESIAN_POINT('Ctrl Pts',(6771.88527936071,3086.40128512098,-269.016885001358));
#206326=CARTESIAN_POINT('Ctrl Pts',(5778.72087570795,2890.97100455373,-255.550151000813));
#206327=CARTESIAN_POINT('Ctrl Pts',(5282.13867388157,2793.2558642701,-248.816784000541));
#206328=CARTESIAN_POINT('Ctrl Pts',(4785.55647205519,2695.54072398648,-242.083417000271));
#206329=CARTESIAN_POINT('Ctrl Pts',(4288.9742702288,2597.82558370285,-235.35005));
#206330=CARTESIAN_POINT('Ctrl Pts',(3797.30872386605,2501.0779200557,-228.683349999731));
#206331=CARTESIAN_POINT('Ctrl Pts',(3303.50354987733,2421.41533039039,-222.016650000135));
#206332=CARTESIAN_POINT('Ctrl Pts',(2806.55033858209,2358.67377790971,-215.349950000068));
#206333=CARTESIAN_POINT('Ctrl Pts',(2801.58080646913,2358.0463623849,-215.283283000067));
#206334=CARTESIAN_POINT('Ctrl Pts',(2796.61127435617,2357.41894686008,-215.216616000068));
#206335=CARTESIAN_POINT('Ctrl Pts',(2791.64174224321,2356.79153133527,-215.149949000068));
#206336=CARTESIAN_POINT('Ctrl Pts',(20575.3477511526,6525.97514455899,-376.750757008008));
#206337=CARTESIAN_POINT('Ctrl Pts',(17802.9896396889,5973.30948238956,-349.817289006482));
#206338=CARTESIAN_POINT('Ctrl Pts',(15030.6315282253,5420.64382022014,-322.883821004956));
#206339=CARTESIAN_POINT('Ctrl Pts',(12258.2734167616,4867.97815805071,-295.950353003429));
#206340=CARTESIAN_POINT('Ctrl Pts',(10872.0943610298,4591.645326966,-282.483619002666));
#206341=CARTESIAN_POINT('Ctrl Pts',(9485.91530529798,4315.31249588128,-269.016885001903));
#206342=CARTESIAN_POINT('Ctrl Pts',(8099.73624956616,4038.97966479657,-255.55015100114));
#206343=CARTESIAN_POINT('Ctrl Pts',(7406.64672170025,3900.81324925421,-248.816784000758));
#206344=CARTESIAN_POINT('Ctrl Pts',(6713.55719383433,3762.64683371185,-242.083417000379));
#206345=CARTESIAN_POINT('Ctrl Pts',(6020.46766596842,3624.4804181695,-235.35005));
#206346=CARTESIAN_POINT('Ctrl Pts',(5334.24041065563,3487.68198693944,-228.683349999624));
#206347=CARTESIAN_POINT('Ctrl Pts',(4645.01458122929,3374.82711249242,-222.016650000188));
#206348=CARTESIAN_POINT('Ctrl Pts',(3951.37696091755,3285.68590850268,-215.349950000095));
#206349=CARTESIAN_POINT('Ctrl Pts',(3944.44058471441,3284.79449646278,-215.283283000095));
#206350=CARTESIAN_POINT('Ctrl Pts',(3937.50420851128,3283.90308442287,-215.216616000095));
#206351=CARTESIAN_POINT('Ctrl Pts',(3930.56783230814,3283.01167238296,-215.149949000095));
#206352=CARTESIAN_POINT('Ctrl Pts',(26433.4949937224,8402.106759459,-376.750757010304));
#206353=CARTESIAN_POINT('Ctrl Pts',(22875.1075781007,7687.63599625465,-349.81728900834));
#206354=CARTESIAN_POINT('Ctrl Pts',(19316.7201624788,6973.16523305029,-322.883821006377));
#206355=CARTESIAN_POINT('Ctrl Pts',(15758.332746857,6258.69446984594,-295.950353004413));
#206356=CARTESIAN_POINT('Ctrl Pts',(13979.1390390461,5901.45908824376,-282.48361900343));
#206357=CARTESIAN_POINT('Ctrl Pts',(12199.9453312353,5544.22370664158,-269.016885002448));
#206358=CARTESIAN_POINT('Ctrl Pts',(10420.7516234244,5186.98832503941,-255.550151001467));
#206359=CARTESIAN_POINT('Ctrl Pts',(9531.15476951892,5008.37063423832,-248.816784000976));
#206360=CARTESIAN_POINT('Ctrl Pts',(8641.55791561347,4829.75294343723,-242.083417000487));
#206361=CARTESIAN_POINT('Ctrl Pts',(7751.96106170802,4651.13525263614,-235.35005));
#206362=CARTESIAN_POINT('Ctrl Pts',(6871.1720974452,4474.28605382318,-228.683349999516));
#206363=CARTESIAN_POINT('Ctrl Pts',(5986.52561258124,4328.23889459445,-222.016650000243));
#206364=CARTESIAN_POINT('Ctrl Pts',(5096.20358325299,4212.69803909567,-215.349950000122));
#206365=CARTESIAN_POINT('Ctrl Pts',(5087.30036295968,4211.54263054066,-215.283283000121));
#206366=CARTESIAN_POINT('Ctrl Pts',(5078.39714266638,4210.38722198566,-215.216616000122));
#206367=CARTESIAN_POINT('Ctrl Pts',(5069.49392237307,4209.23181343066,-215.149949000122));
#206368=CARTESIAN_POINT('Origin',(0.,-12.9675000200281,-218.35005));
#206369=CARTESIAN_POINT('Ctrl Pts',(10765.646428189,-1979.29526939781,-376.750757000846));
#206370=CARTESIAN_POINT('Ctrl Pts',(9257.10677574949,-1902.78686830728,
-349.817289000686));
#206371=CARTESIAN_POINT('Ctrl Pts',(7748.56712330994,-1826.27846721676,
-322.883821000524));
#206372=CARTESIAN_POINT('Ctrl Pts',(6240.0274708704,-1749.77006612623,-295.950353000363));
#206373=CARTESIAN_POINT('Ctrl Pts',(5485.75764465062,-1711.51586558096,
-282.483619000282));
#206374=CARTESIAN_POINT('Ctrl Pts',(4731.48781843085,-1673.2616650357,-269.016885000202));
#206375=CARTESIAN_POINT('Ctrl Pts',(3977.21799221108,-1635.00746449044,
-255.550151000121));
#206376=CARTESIAN_POINT('Ctrl Pts',(3600.08307910119,-1615.8803642178,-248.816784000081));
#206377=CARTESIAN_POINT('Ctrl Pts',(3222.9481659913,-1596.75326394517,-242.083417000041));
#206378=CARTESIAN_POINT('Ctrl Pts',(2845.81325288141,-1577.62616367254,
-235.35005));
#206379=CARTESIAN_POINT('Ctrl Pts',(2472.41234881222,-1558.68844063033,
-228.68334999996));
#206380=CARTESIAN_POINT('Ctrl Pts',(2099.07452015968,-1540.45097924114,
-222.01665));
#206381=CARTESIAN_POINT('Ctrl Pts',(1725.79722689738,-1522.91379824522,
-215.34994999996));
#206382=CARTESIAN_POINT('Ctrl Pts',(1722.06445396475,-1522.73842643524,
-215.28328299996));
#206383=CARTESIAN_POINT('Ctrl Pts',(1718.33168103213,-1522.56305462527,
-215.21661599996));
#206384=CARTESIAN_POINT('Ctrl Pts',(1714.5989080995,-1522.3876828153,-215.14994899996));
#206385=CARTESIAN_POINT('Ctrl Pts',(8392.35568812379,-1534.61913504983,
-376.750757000658));
#206386=CARTESIAN_POINT('Ctrl Pts',(7213.78531733318,-1478.38877237011,
-349.817289000532));
#206387=CARTESIAN_POINT('Ctrl Pts',(6035.21494654257,-1422.15840969038,
-322.883821000408));
#206388=CARTESIAN_POINT('Ctrl Pts',(4856.64457575196,-1365.92804701065,
-295.950353000282));
#206389=CARTESIAN_POINT('Ctrl Pts',(4267.35939035666,-1337.81286567079,
-282.48361900022));
#206390=CARTESIAN_POINT('Ctrl Pts',(3678.07420496136,-1309.69768433093,
-269.016885000157));
#206391=CARTESIAN_POINT('Ctrl Pts',(3088.78901956605,-1281.58250299106,
-255.550151000094));
#206392=CARTESIAN_POINT('Ctrl Pts',(2794.1464268684,-1267.52491232113,-248.816784000063));
#206393=CARTESIAN_POINT('Ctrl Pts',(2499.50383417074,-1253.4673216512,-242.083417000031));
#206394=CARTESIAN_POINT('Ctrl Pts',(2204.8612414731,-1239.40973098127,-235.35005));
#206395=CARTESIAN_POINT('Ctrl Pts',(1913.13590216849,-1225.49132437738,
-228.683349999968));
#206396=CARTESIAN_POINT('Ctrl Pts',(1621.45955977666,-1212.11656254984,
-222.01665));
#206397=CARTESIAN_POINT('Ctrl Pts',(1329.83024235737,-1199.28546008462,
-215.349949999969));
#206398=CARTESIAN_POINT('Ctrl Pts',(1326.91394918317,-1199.15714905996,
-215.283282999969));
#206399=CARTESIAN_POINT('Ctrl Pts',(1323.99765600898,-1199.02883803529,
-215.216615999969));
#206400=CARTESIAN_POINT('Ctrl Pts',(1321.08136283478,-1198.90052701063,
-215.149948999969));
#206401=CARTESIAN_POINT('Ctrl Pts',(6019.06494805854,-1089.94300070186,
-376.750757000469));
#206402=CARTESIAN_POINT('Ctrl Pts',(5170.46385891687,-1053.99067643293,
-349.817289000379));
#206403=CARTESIAN_POINT('Ctrl Pts',(4321.8627697752,-1018.03835216401,-322.88382100029));
#206404=CARTESIAN_POINT('Ctrl Pts',(3473.26168063352,-982.086027895082,
-295.950353000201));
#206405=CARTESIAN_POINT('Ctrl Pts',(3048.96113606269,-964.10986576062,-282.483619000157));
#206406=CARTESIAN_POINT('Ctrl Pts',(2624.66059149186,-946.133703626157,
-269.016885000112));
#206407=CARTESIAN_POINT('Ctrl Pts',(2200.36004692103,-928.157541491694,
-255.550151000067));
#206408=CARTESIAN_POINT('Ctrl Pts',(1988.2097746356,-919.169460424462,-248.816784000044));
#206409=CARTESIAN_POINT('Ctrl Pts',(1776.05950235019,-910.181379357231,
-242.083417000023));
#206410=CARTESIAN_POINT('Ctrl Pts',(1563.90923006478,-901.19329829,-235.35005));
#206411=CARTESIAN_POINT('Ctrl Pts',(1353.85945552476,-892.294208124424,
-228.683349999978));
#206412=CARTESIAN_POINT('Ctrl Pts',(1143.84459939364,-883.782145858533,
-222.01665));
#206413=CARTESIAN_POINT('Ctrl Pts',(933.863257817356,-875.657121924021,
-215.349949999977));
#206414=CARTESIAN_POINT('Ctrl Pts',(931.763444401592,-875.575871684668,
-215.283282999978));
#206415=CARTESIAN_POINT('Ctrl Pts',(929.663630985828,-875.494621445315,
-215.216615999977));
#206416=CARTESIAN_POINT('Ctrl Pts',(927.563817570064,-875.413371205962,
-215.149948999978));
#206417=CARTESIAN_POINT('Ctrl Pts',(3645.77420799329,-645.266866353884,
-376.75075700028));
#206418=CARTESIAN_POINT('Ctrl Pts',(3127.14240050056,-629.592580495759,
-349.817289000227));
#206419=CARTESIAN_POINT('Ctrl Pts',(2608.51059300782,-613.918294637635,
-322.883821000173));
#206420=CARTESIAN_POINT('Ctrl Pts',(2089.87878551509,-598.24400877951,-295.95035300012));
#206421=CARTESIAN_POINT('Ctrl Pts',(1830.56288176873,-590.406865850448,
-282.483619000093));
#206422=CARTESIAN_POINT('Ctrl Pts',(1571.24697802237,-582.569722921386,
-269.016885000067));
#206423=CARTESIAN_POINT('Ctrl Pts',(1311.931074276,-574.732579992324,-255.55015100004));
#206424=CARTESIAN_POINT('Ctrl Pts',(1182.27312240282,-570.814008527792,
-248.816784000027));
#206425=CARTESIAN_POINT('Ctrl Pts',(1052.61517052964,-566.895437063261,
-242.083417000014));
#206426=CARTESIAN_POINT('Ctrl Pts',(922.957218656454,-562.97686559873,-235.35005));
#206427=CARTESIAN_POINT('Ctrl Pts',(794.583008881026,-559.097091871471,
-228.683349999987));
#206428=CARTESIAN_POINT('Ctrl Pts',(666.229639010622,-555.447729167229,
-222.01665));
#206429=CARTESIAN_POINT('Ctrl Pts',(537.896273277345,-552.028783763422,
-215.349949999987));
#206430=CARTESIAN_POINT('Ctrl Pts',(536.612939620012,-551.994594309379,
-215.283282999987));
#206431=CARTESIAN_POINT('Ctrl Pts',(535.329605962679,-551.960404855337,
-215.216615999987));
#206432=CARTESIAN_POINT('Ctrl Pts',(534.046272305346,-551.926215401294,
-215.149948999987));
#206433=CARTESIAN_POINT('Ctrl Pts',(2854.6772946382,-497.041488237892,-376.750757000217));
#206434=CARTESIAN_POINT('Ctrl Pts',(2446.03524769512,-488.126548516702,
-349.817289000176));
#206435=CARTESIAN_POINT('Ctrl Pts',(2037.39320075203,-479.211608795511,
-322.883821000135));
#206436=CARTESIAN_POINT('Ctrl Pts',(1628.75115380895,-470.29666907432,-295.950353000093));
#206437=CARTESIAN_POINT('Ctrl Pts',(1424.43013033741,-465.839199213724,
-282.483619000073));
#206438=CARTESIAN_POINT('Ctrl Pts',(1220.10910686587,-461.381729353129,
-269.016885000052));
#206439=CARTESIAN_POINT('Ctrl Pts',(1015.78808339432,-456.924259492534,
-255.550151000031));
#206440=CARTESIAN_POINT('Ctrl Pts',(913.627571658554,-454.695524562236,
-248.816784000021));
#206441=CARTESIAN_POINT('Ctrl Pts',(811.467059922784,-452.466789631938,
-242.083417000011));
#206442=CARTESIAN_POINT('Ctrl Pts',(709.306548187014,-450.23805470164,-235.35005));
#206443=CARTESIAN_POINT('Ctrl Pts',(608.157526666449,-448.03138645382,-228.68334999999));
#206444=CARTESIAN_POINT('Ctrl Pts',(507.024652216282,-446.002923603462,
-222.01665));
#206445=CARTESIAN_POINT('Ctrl Pts',(405.907278430675,-444.152671043223,
-215.34994999999));
#206446=CARTESIAN_POINT('Ctrl Pts',(404.896104692818,-444.134168517617,
-215.283282999989));
#206447=CARTESIAN_POINT('Ctrl Pts',(403.884930954962,-444.115665992011,
-215.21661599999));
#206448=CARTESIAN_POINT('Ctrl Pts',(402.873757217106,-444.097163466405,
-215.14994899999));
#206449=CARTESIAN_POINT('Ctrl Pts',(2063.58038128312,-348.816110121901,
-376.750757000154));
#206450=CARTESIAN_POINT('Ctrl Pts',(1764.92809488968,-346.660516537644,
-349.817289000125));
#206451=CARTESIAN_POINT('Ctrl Pts',(1466.27580849624,-344.504922953386,
-322.883821000096));
#206452=CARTESIAN_POINT('Ctrl Pts',(1167.6235221028,-342.349329369129,-295.950353000066));
#206453=CARTESIAN_POINT('Ctrl Pts',(1018.29737890609,-341.271532577001,
-282.483619000052));
#206454=CARTESIAN_POINT('Ctrl Pts',(868.971235709368,-340.193735784872,
-269.016885000037));
#206455=CARTESIAN_POINT('Ctrl Pts',(719.64509251265,-339.115938992743,-255.550151000022));
#206456=CARTESIAN_POINT('Ctrl Pts',(644.982020914291,-338.577040596679,
-248.816784000015));
#206457=CARTESIAN_POINT('Ctrl Pts',(570.318949315933,-338.038142200615,
-242.083417000008));
#206458=CARTESIAN_POINT('Ctrl Pts',(495.655877717574,-337.49924380455,-235.35005));
#206459=CARTESIAN_POINT('Ctrl Pts',(421.732044451872,-336.96568103617,-228.683349999993));
#206460=CARTESIAN_POINT('Ctrl Pts',(347.819665421942,-336.558118039694,
-222.01665));
#206461=CARTESIAN_POINT('Ctrl Pts',(273.918283584005,-336.276558323023,
-215.349949999993));
#206462=CARTESIAN_POINT('Ctrl Pts',(273.179269765626,-336.273742725853,
-215.283282999993));
#206463=CARTESIAN_POINT('Ctrl Pts',(272.440255947246,-336.270927128685,
-215.216615999993));
#206464=CARTESIAN_POINT('Ctrl Pts',(271.701242128866,-336.268111531515,
-215.149948999993));
#206465=CARTESIAN_POINT('Ctrl Pts',(1272.48346792803,-200.59073200591,-376.750757000092));
#206466=CARTESIAN_POINT('Ctrl Pts',(1083.82094208424,-205.194484558586,
-349.817289000074));
#206467=CARTESIAN_POINT('Ctrl Pts',(895.15841624045,-209.798237111262,-322.883821000057));
#206468=CARTESIAN_POINT('Ctrl Pts',(706.49589039666,-214.401989663939,-295.950353000039));
#206469=CARTESIAN_POINT('Ctrl Pts',(612.164627474765,-216.703865940277,
-282.483619000031));
#206470=CARTESIAN_POINT('Ctrl Pts',(517.83336455287,-219.005742216615,-269.016885000022));
#206471=CARTESIAN_POINT('Ctrl Pts',(423.502101630976,-221.307618492953,
-255.550151000013));
#206472=CARTESIAN_POINT('Ctrl Pts',(376.336470170028,-222.458556631122,
-248.816784000009));
#206473=CARTESIAN_POINT('Ctrl Pts',(329.170838709081,-223.609494769291,
-242.083417000004));
#206474=CARTESIAN_POINT('Ctrl Pts',(282.005207248134,-224.760432907461,
-235.35005));
#206475=CARTESIAN_POINT('Ctrl Pts',(235.306562237295,-225.899975618519,
-228.683349999995));
#206476=CARTESIAN_POINT('Ctrl Pts',(188.614678627603,-227.113312475926,
-222.01665));
#206477=CARTESIAN_POINT('Ctrl Pts',(141.929288737335,-228.400445602824,
-215.349949999996));
#206478=CARTESIAN_POINT('Ctrl Pts',(141.462434838432,-228.413316934091,
-215.283282999995));
#206479=CARTESIAN_POINT('Ctrl Pts',(140.995580939529,-228.426188265358,
-215.216615999995));
#206480=CARTESIAN_POINT('Ctrl Pts',(140.528727040626,-228.439059596626,
-215.149948999996));
#206481=CARTESIAN_POINT('Ctrl Pts',(1008.78449680967,-151.182272633913,
-376.750757000071));
#206482=CARTESIAN_POINT('Ctrl Pts',(856.785224482427,-158.039140565566,
-349.817289000057));
#206483=CARTESIAN_POINT('Ctrl Pts',(704.785952155186,-164.896008497221,
-322.883821000044));
#206484=CARTESIAN_POINT('Ctrl Pts',(552.786679827945,-171.752876428875,
-295.95035300003));
#206485=CARTESIAN_POINT('Ctrl Pts',(476.787043664325,-175.181310394702,
-282.483619000024));
#206486=CARTESIAN_POINT('Ctrl Pts',(400.787407500704,-178.609744360529,
-269.016885000016));
#206487=CARTESIAN_POINT('Ctrl Pts',(324.787771337084,-182.038178326357,
-255.55015100001));
#206488=CARTESIAN_POINT('Ctrl Pts',(286.787953255274,-183.75239530927,-248.816784000007));
#206489=CARTESIAN_POINT('Ctrl Pts',(248.788135173463,-185.466612292184,
-242.083417000003));
#206490=CARTESIAN_POINT('Ctrl Pts',(210.788317091653,-187.180829275097,
-235.35005));
#206491=CARTESIAN_POINT('Ctrl Pts',(173.164734832436,-188.878073812635,
-228.683349999997));
#206492=CARTESIAN_POINT('Ctrl Pts',(135.546349696156,-190.631710621336,
-222.01665));
#206493=CARTESIAN_POINT('Ctrl Pts',(97.932957121778,-192.441741362757,-215.349949999997));
#206494=CARTESIAN_POINT('Ctrl Pts',(97.5568231960341,-192.45984167017,-215.283282999997));
#206495=CARTESIAN_POINT('Ctrl Pts',(97.1806892702902,-192.477941977583,
-215.216615999996));
#206496=CARTESIAN_POINT('Ctrl Pts',(96.8045553445463,-192.496042284996,
-215.149948999996));
#206497=CARTESIAN_POINT('Ctrl Pts',(745.085525691306,-101.773813261915,
-376.75075700005));
#206498=CARTESIAN_POINT('Ctrl Pts',(629.749506880614,-110.883796572547,
-349.81728900004));
#206499=CARTESIAN_POINT('Ctrl Pts',(514.413488069922,-119.993779883179,
-322.88382100003));
#206500=CARTESIAN_POINT('Ctrl Pts',(399.07746925923,-129.103763193811,-295.950353000021));
#206501=CARTESIAN_POINT('Ctrl Pts',(341.409459853884,-133.658754849127,
-282.483619000017));
#206502=CARTESIAN_POINT('Ctrl Pts',(283.741450448538,-138.213746504444,
-269.016885000012));
#206503=CARTESIAN_POINT('Ctrl Pts',(226.073441043192,-142.76873815976,-255.550151000007));
#206504=CARTESIAN_POINT('Ctrl Pts',(197.239436340519,-145.046233987418,
-248.816784000005));
#206505=CARTESIAN_POINT('Ctrl Pts',(168.405431637847,-147.323729815076,
-242.083417000002));
#206506=CARTESIAN_POINT('Ctrl Pts',(139.571426935173,-149.601225642734,
-235.35005));
#206507=CARTESIAN_POINT('Ctrl Pts',(111.022907427576,-151.856172006752,
-228.683349999998));
#206508=CARTESIAN_POINT('Ctrl Pts',(82.4780207647092,-154.150108766748,
-222.01665));
#206509=CARTESIAN_POINT('Ctrl Pts',(53.9366255062213,-156.48303712269,-215.349949999998));
#206510=CARTESIAN_POINT('Ctrl Pts',(53.6512115536363,-156.506366406249,
-215.283282999997));
#206511=CARTESIAN_POINT('Ctrl Pts',(53.3657976010514,-156.529695689807,
-215.216615999998));
#206512=CARTESIAN_POINT('Ctrl Pts',(53.0803836484664,-156.553024973366,
-215.149948999998));
#206513=CARTESIAN_POINT('Ctrl Pts',(481.386554572944,-52.3653538899179,
-376.750757000028));
#206514=CARTESIAN_POINT('Ctrl Pts',(402.713789278801,-63.7284525795279,
-349.817289000023));
#206515=CARTESIAN_POINT('Ctrl Pts',(324.041023984658,-75.0915512691379,
-322.883821000018));
#206516=CARTESIAN_POINT('Ctrl Pts',(245.368258690515,-86.4546499587479,
-295.950353000012));
#206517=CARTESIAN_POINT('Ctrl Pts',(206.031876043444,-92.1361993035529,
-282.48361900001));
#206518=CARTESIAN_POINT('Ctrl Pts',(166.695493396372,-97.8177486483579,
-269.016885000007));
#206519=CARTESIAN_POINT('Ctrl Pts',(127.359110749301,-103.499297993163,
-255.550151000004));
#206520=CARTESIAN_POINT('Ctrl Pts',(107.690919425765,-106.340072665565,
-248.816784000003));
#206521=CARTESIAN_POINT('Ctrl Pts',(88.0227281022291,-109.180847337968,
-242.083417000002));
#206522=CARTESIAN_POINT('Ctrl Pts',(68.3545367786933,-112.02162201037,-235.35005));
#206523=CARTESIAN_POINT('Ctrl Pts',(48.8810800227174,-114.834270200868,
-228.683349999999));
#206524=CARTESIAN_POINT('Ctrl Pts',(29.4096918332626,-117.668506912158,
-222.01665));
#206525=CARTESIAN_POINT('Ctrl Pts',(9.94029389066457,-120.524332882624,
-215.349949999999));
#206526=CARTESIAN_POINT('Ctrl Pts',(9.74559991123855,-120.552891142328,
-215.283282999999));
#206527=CARTESIAN_POINT('Ctrl Pts',(9.55090593181253,-120.581449402032,
-215.216615999999));
#206528=CARTESIAN_POINT('Ctrl Pts',(9.3562119523865,-120.610007661736,-215.149948999999));
#206529=CARTESIAN_POINT('Ctrl Pts',(393.48689753349,-35.8958674325856,-376.750757000021));
#206530=CARTESIAN_POINT('Ctrl Pts',(327.035216744864,-48.0100045818548,
-349.817289000017));
#206531=CARTESIAN_POINT('Ctrl Pts',(260.583535956237,-60.1241417311241,
-322.883821000013));
#206532=CARTESIAN_POINT('Ctrl Pts',(194.13185516761,-72.2382788803934,-295.950353000009));
#206533=CARTESIAN_POINT('Ctrl Pts',(160.906014773297,-78.2953474550281,
-282.483619000007));
#206534=CARTESIAN_POINT('Ctrl Pts',(127.680174378983,-84.3524160296627,
-269.016885000005));
#206535=CARTESIAN_POINT('Ctrl Pts',(94.45433398467,-90.4094846042973,-255.550151000003));
#206536=CARTESIAN_POINT('Ctrl Pts',(77.8414137875133,-93.4380188916147,
-248.816784000002));
#206537=CARTESIAN_POINT('Ctrl Pts',(61.2284935903567,-96.466553178932,-242.083417000001));
#206538=CARTESIAN_POINT('Ctrl Pts',(44.6155733932,-99.4950874662493,-235.35005));
#206539=CARTESIAN_POINT('Ctrl Pts',(28.167137554431,-102.493636265573,-228.683349999999));
#206540=CARTESIAN_POINT('Ctrl Pts',(11.7202488561137,-105.507972960628,
-222.01665));
#206541=CARTESIAN_POINT('Ctrl Pts',(-4.72514998118767,-108.538098135935,
-215.349949999999));
#206542=CARTESIAN_POINT('Ctrl Pts',(-4.88960396956071,-108.568399387688,
-215.283282999999));
#206543=CARTESIAN_POINT('Ctrl Pts',(-5.05405795793375,-108.59870063944,
-215.216615999999));
#206544=CARTESIAN_POINT('Ctrl Pts',(-5.2185119463068,-108.629001891193,
-215.149948999999));
#206545=CARTESIAN_POINT('Ctrl Pts',(305.587240494037,-19.4263809752531,
-376.750757000014));
#206546=CARTESIAN_POINT('Ctrl Pts',(251.356644210927,-32.2915565841817,
-349.817289000011));
#206547=CARTESIAN_POINT('Ctrl Pts',(197.126047927816,-45.1567321931103,
-322.883821000009));
#206548=CARTESIAN_POINT('Ctrl Pts',(142.895451644705,-58.0219078020389,
-295.950353000006));
#206549=CARTESIAN_POINT('Ctrl Pts',(115.78015350315,-64.4544956065032,-282.483619000005));
#206550=CARTESIAN_POINT('Ctrl Pts',(88.6648553615948,-70.8870834109675,
-269.016885000003));
#206551=CARTESIAN_POINT('Ctrl Pts',(61.5495572200395,-77.3196712154318,
-255.550151000002));
#206552=CARTESIAN_POINT('Ctrl Pts',(47.9919081492619,-80.5359651176639,
-248.816784000002));
#206553=CARTESIAN_POINT('Ctrl Pts',(34.4342590784842,-83.7522590198961,
-242.083417000001));
#206554=CARTESIAN_POINT('Ctrl Pts',(20.8766100077067,-86.9685529221282,
-235.35005));
#206555=CARTESIAN_POINT('Ctrl Pts',(7.45319508614462,-90.1530023302789,
-228.68335));
#206556=CARTESIAN_POINT('Ctrl Pts',(-5.96919412103514,-93.3474390090985,
-222.01665));
#206557=CARTESIAN_POINT('Ctrl Pts',(-19.3905938530399,-96.5518633892461,
-215.34995));
#206558=CARTESIAN_POINT('Ctrl Pts',(-19.52480785036,-96.5839076330473,-215.283283));
#206559=CARTESIAN_POINT('Ctrl Pts',(-19.6590218476801,-96.6159518768485,
-215.216616));
#206560=CARTESIAN_POINT('Ctrl Pts',(-19.7932358450001,-96.6479961206498,
-215.149949));
#206561=CARTESIAN_POINT('Ctrl Pts',(217.687583454584,-2.9568945179205,-376.750757000007));
#206562=CARTESIAN_POINT('Ctrl Pts',(175.67807167699,-16.5731085865084,-349.817289000006));
#206563=CARTESIAN_POINT('Ctrl Pts',(133.668559899395,-30.1893226550964,
-322.883821000005));
#206564=CARTESIAN_POINT('Ctrl Pts',(91.6590481218006,-43.8055367236842,
-295.950353000003));
#206565=CARTESIAN_POINT('Ctrl Pts',(70.6542922330034,-50.6136437579782,
-282.483619000003));
#206566=CARTESIAN_POINT('Ctrl Pts',(49.6495363442062,-57.4217507922722,
-269.016885000001));
#206567=CARTESIAN_POINT('Ctrl Pts',(28.644780455409,-64.2298578265662,-255.550151000001));
#206568=CARTESIAN_POINT('Ctrl Pts',(18.1424025110104,-67.6339113437132,
-248.816784000001));
#206569=CARTESIAN_POINT('Ctrl Pts',(7.64002456661188,-71.0379648608601,
-242.083417000001));
#206570=CARTESIAN_POINT('Ctrl Pts',(-2.8623533777867,-74.4420183780071,
-235.35005));
#206571=CARTESIAN_POINT('Ctrl Pts',(-13.2607473821417,-77.8123683949843,
-228.68335));
#206572=CARTESIAN_POINT('Ctrl Pts',(-23.658637098184,-81.1869050575687,
-222.01665));
#206573=CARTESIAN_POINT('Ctrl Pts',(-34.0560377248921,-84.5656286425572,
-215.34995));
#206574=CARTESIAN_POINT('Ctrl Pts',(-34.1600117311593,-84.599415878407,
-215.283283));
#206575=CARTESIAN_POINT('Ctrl Pts',(-34.2639857374263,-84.6332031142567,
-215.216616));
#206576=CARTESIAN_POINT('Ctrl Pts',(-34.3679597436934,-84.6669903501065,
-215.149949));
#206577=CARTESIAN_POINT('Ctrl Pts',(188.387697774766,2.53293430119023,-376.750757000005));
#206578=CARTESIAN_POINT('Ctrl Pts',(150.451880832343,-11.3336259206174,
-349.817289000004));
#206579=CARTESIAN_POINT('Ctrl Pts',(112.516063889921,-25.2001861424251,
-322.883821000003));
#206580=CARTESIAN_POINT('Ctrl Pts',(74.580246947499,-39.0667463642328,-295.950353000002));
#206581=CARTESIAN_POINT('Ctrl Pts',(55.6123384762878,-46.0000264751366,
-282.483619000002));
#206582=CARTESIAN_POINT('Ctrl Pts',(36.6444300050767,-52.9333065860405,
-269.016885000001));
#206583=CARTESIAN_POINT('Ctrl Pts',(17.6765215338656,-59.8665866969443,
-255.550151000001));
#206584=CARTESIAN_POINT('Ctrl Pts',(8.19256729825999,-63.3332267523963,
-248.816784000001));
#206585=CARTESIAN_POINT('Ctrl Pts',(-1.29138693734558,-66.7998668078482,
-242.083417));
#206586=CARTESIAN_POINT('Ctrl Pts',(-10.7753411729511,-70.2665068633001,
-235.35005));
#206587=CARTESIAN_POINT('Ctrl Pts',(-20.1653948715705,-73.6988237498861,
-228.68335));
#206588=CARTESIAN_POINT('Ctrl Pts',(-29.5551180905669,-77.1333937403921,
-222.01665));
#206589=CARTESIAN_POINT('Ctrl Pts',(-38.9445190155095,-80.5702170603276,
-215.34995));
#206590=CARTESIAN_POINT('Ctrl Pts',(-39.038413024759,-80.6045852935269,
-215.283283));
#206591=CARTESIAN_POINT('Ctrl Pts',(-39.1323070340084,-80.6389535267262,
-215.216616));
#206592=CARTESIAN_POINT('Ctrl Pts',(-39.2262010432579,-80.6733217599254,
-215.149949));
#206593=CARTESIAN_POINT('Ctrl Pts',(159.087812094948,8.022763120301,-376.750757000003));
#206594=CARTESIAN_POINT('Ctrl Pts',(125.225689987698,-6.09414325472644,
-349.817289000002));
#206595=CARTESIAN_POINT('Ctrl Pts',(91.3635678804476,-20.2110496297539,
-322.883821000001));
#206596=CARTESIAN_POINT('Ctrl Pts',(57.5014457731974,-34.3279560047813,
-295.950353000001));
#206597=CARTESIAN_POINT('Ctrl Pts',(40.5703847195723,-41.386409192295,-282.483619000001));
#206598=CARTESIAN_POINT('Ctrl Pts',(23.6393236659472,-48.4448623798088,
-269.016885));
#206599=CARTESIAN_POINT('Ctrl Pts',(6.70826261232206,-55.5033155673225,
-255.550151000001));
#206600=CARTESIAN_POINT('Ctrl Pts',(-1.75726791449049,-59.0325421610793,
-248.816784));
#206601=CARTESIAN_POINT('Ctrl Pts',(-10.222798441303,-62.5617687548362,
-242.083417));
#206602=CARTESIAN_POINT('Ctrl Pts',(-18.6883289681156,-66.090995348593,
-235.35005));
#206603=CARTESIAN_POINT('Ctrl Pts',(-27.0700423609993,-69.585279104788,
-228.68335));
#206604=CARTESIAN_POINT('Ctrl Pts',(-35.4515990829499,-73.0798824232155,
-222.01665));
#206605=CARTESIAN_POINT('Ctrl Pts',(-43.833000306127,-76.574805478098,-215.34995));
#206606=CARTESIAN_POINT('Ctrl Pts',(-43.9168143183588,-76.6097547086468,
-215.283283));
#206607=CARTESIAN_POINT('Ctrl Pts',(-44.0006283305905,-76.6447039391955,
-215.216616));
#206608=CARTESIAN_POINT('Ctrl Pts',(-44.0844423428223,-76.6796531697443,
-215.149949));
#206609=CARTESIAN_POINT('Ctrl Pts',(129.78792641513,13.512591939412,-376.750757));
#206610=CARTESIAN_POINT('Ctrl Pts',(99.9994991430521,-0.854660588835203,
-349.817289000001));
#206611=CARTESIAN_POINT('Ctrl Pts',(70.211071870974,-15.2219131170825,-322.883821));
#206612=CARTESIAN_POINT('Ctrl Pts',(40.4226445988958,-29.5891656453297,
-295.950353));
#206613=CARTESIAN_POINT('Ctrl Pts',(25.5284309628568,-36.7727919094533,
-282.483619));
#206614=CARTESIAN_POINT('Ctrl Pts',(10.6342173268177,-43.9564181735769,
-269.016885));
#206615=CARTESIAN_POINT('Ctrl Pts',(-4.25999630922143,-51.1400444377006,
-255.550151));
#206616=CARTESIAN_POINT('Ctrl Pts',(-11.707103127241,-54.7318575697624,
-248.816784));
#206617=CARTESIAN_POINT('Ctrl Pts',(-19.1542099452605,-58.3236707018242,
-242.083417));
#206618=CARTESIAN_POINT('Ctrl Pts',(-26.60131676328,-61.915483833886,-235.35005));
#206619=CARTESIAN_POINT('Ctrl Pts',(-33.9746898504281,-65.4717344596898,
-228.68335));
#206620=CARTESIAN_POINT('Ctrl Pts',(-41.3480800753329,-69.0263711060389,
-222.01665));
#206621=CARTESIAN_POINT('Ctrl Pts',(-48.7214815967444,-72.5793938958684,
-215.34995));
#206622=CARTESIAN_POINT('Ctrl Pts',(-48.7952156119585,-72.6149241237667,
-215.283283));
#206623=CARTESIAN_POINT('Ctrl Pts',(-48.8689496271726,-72.6504543516649,
-215.216616));
#206624=CARTESIAN_POINT('Ctrl Pts',(-48.9426836423867,-72.6859845795632,
-215.149949));
#206625=CARTESIAN_POINT('Ctrl Pts',(122.462954995176,14.8850491441897,-376.750756999999));
#206626=CARTESIAN_POINT('Ctrl Pts',(93.6929514318907,0.455210077637512,
-349.817289));
#206627=CARTESIAN_POINT('Ctrl Pts',(64.9229478686056,-13.9746289889147,
-322.883821));
#206628=CARTESIAN_POINT('Ctrl Pts',(36.1529443053205,-28.4044680554669,
-295.950353));
#206629=CARTESIAN_POINT('Ctrl Pts',(21.7679425236779,-35.619387588743,-282.483619));
#206630=CARTESIAN_POINT('Ctrl Pts',(7.38294074203528,-42.834307122019,-269.016885));
#206631=CARTESIAN_POINT('Ctrl Pts',(-7.00206103960729,-50.0492266552951,
-255.550151));
#206632=CARTESIAN_POINT('Ctrl Pts',(-14.1945619304286,-53.6566864219332,
-248.816784));
#206633=CARTESIAN_POINT('Ctrl Pts',(-21.3870628212499,-57.2641461885712,
-242.083417));
#206634=CARTESIAN_POINT('Ctrl Pts',(-28.5795637120712,-60.8716059552093,
-235.35005));
#206635=CARTESIAN_POINT('Ctrl Pts',(-35.7008517227853,-64.4433482984152,
-228.68335));
#206636=CARTESIAN_POINT('Ctrl Pts',(-42.8222003234286,-68.0129932767448,
-222.01665));
#206637=CARTESIAN_POINT('Ctrl Pts',(-49.9436019193987,-71.5805410003109,
-215.34995));
#206638=CARTESIAN_POINT('Ctrl Pts',(-50.0148159353584,-71.6162164775466,
-215.283283));
#206639=CARTESIAN_POINT('Ctrl Pts',(-50.0860299513181,-71.6518919547823,
-215.216616));
#206640=CARTESIAN_POINT('Ctrl Pts',(-50.1572439672778,-71.687567432018,
-215.149949));
#206641=CARTESIAN_POINT('Ctrl Pts',(103.0219124536,22.8222305961756,-376.750757000007));
#206642=CARTESIAN_POINT('Ctrl Pts',(77.174697282254,7.34909250165779,-349.817289000007));
#206643=CARTESIAN_POINT('Ctrl Pts',(51.3274821109085,-8.12404559286004,
-322.883821000005));
#206644=CARTESIAN_POINT('Ctrl Pts',(25.480266939563,-23.5971836873778,-295.950353000003));
#206645=CARTESIAN_POINT('Ctrl Pts',(12.5566593538902,-31.3337527346368,
-282.483619000003));
#206646=CARTESIAN_POINT('Ctrl Pts',(-0.366948231782582,-39.0703217818957,
-269.016885000003));
#206647=CARTESIAN_POINT('Ctrl Pts',(-13.2905558174553,-46.8068908291546,
-255.550151000002));
#206648=CARTESIAN_POINT('Ctrl Pts',(-19.7523596102917,-50.6751753527841,
-248.816784000002));
#206649=CARTESIAN_POINT('Ctrl Pts',(-26.2141634031281,-54.5434598764135,
-242.083417000001));
#206650=CARTESIAN_POINT('Ctrl Pts',(-32.6759671959645,-58.411744400043,
-235.350050000001));
#206651=CARTESIAN_POINT('Ctrl Pts',(-39.0737927334262,-62.2417290769038,
-228.683350000001));
#206652=CARTESIAN_POINT('Ctrl Pts',(-45.4718450018044,-66.0691978041651,
-222.01665));
#206653=CARTESIAN_POINT('Ctrl Pts',(-51.8701148758579,-69.894150514329,
-215.34995));
#206654=CARTESIAN_POINT('Ctrl Pts',(-51.9340975745985,-69.9324000414307,
-215.283283));
#206655=CARTESIAN_POINT('Ctrl Pts',(-51.998080273339,-69.9706495685323,
-215.216616));
#206656=CARTESIAN_POINT('Ctrl Pts',(-52.0620629720796,-70.0088990956339,
-215.149949));
#206657=CARTESIAN_POINT('Ctrl Pts',(71.4332298554826,45.3676034181815,-376.750756999996));
#206658=CARTESIAN_POINT('Ctrl Pts',(50.4371334176971,26.5324811107851,-349.817288999997));
#206659=CARTESIAN_POINT('Ctrl Pts',(29.4410369799117,7.69735880338874,-322.883820999997));
#206660=CARTESIAN_POINT('Ctrl Pts',(8.44494054212614,-11.1377635040076,
-295.950352999998));
#206661=CARTESIAN_POINT('Ctrl Pts',(-2.05310767676661,-20.5553246577058,
-282.483618999998));
#206662=CARTESIAN_POINT('Ctrl Pts',(-12.5511558956594,-29.972885811404,
-269.016884999999));
#206663=CARTESIAN_POINT('Ctrl Pts',(-23.0492041145521,-39.3904469651022,
-255.550150999999));
#206664=CARTESIAN_POINT('Ctrl Pts',(-28.2982282239985,-44.0992275419513,
-248.816783999999));
#206665=CARTESIAN_POINT('Ctrl Pts',(-33.5472523334448,-48.8080081188004,
-242.083416999999));
#206666=CARTESIAN_POINT('Ctrl Pts',(-38.7962764428913,-53.5167886956495,
-235.35005));
#206667=CARTESIAN_POINT('Ctrl Pts',(-43.9933300166005,-58.1789476826288,
-228.68335));
#206668=CARTESIAN_POINT('Ctrl Pts',(-49.1909136386903,-62.839044754287,
-222.01665));
#206669=CARTESIAN_POINT('Ctrl Pts',(-54.3890197977427,-67.4970794092701,
-215.34995));
#206670=CARTESIAN_POINT('Ctrl Pts',(-54.4410008593333,-67.5436597558199,
-215.283283));
#206671=CARTESIAN_POINT('Ctrl Pts',(-54.4929819209238,-67.5902401023698,
-215.216616));
#206672=CARTESIAN_POINT('Ctrl Pts',(-54.5449629825143,-67.6368204489196,
-215.149949));
#206673=CARTESIAN_POINT('Ctrl Pts',(45.0390725903934,73.7599134480721,-376.750757000003));
#206674=CARTESIAN_POINT('Ctrl Pts',(28.0469137085574,50.6061693294573,-349.817289000002));
#206675=CARTESIAN_POINT('Ctrl Pts',(11.0547548267215,27.4524252108426,-322.883821000002));
#206676=CARTESIAN_POINT('Ctrl Pts',(-5.93740405511448,4.29868109222778,
-295.950353000001));
#206677=CARTESIAN_POINT('Ctrl Pts',(-14.4334834960324,-7.2781909670796,
-282.483619000001));
#206678=CARTESIAN_POINT('Ctrl Pts',(-22.9295629369504,-18.855063026387,
-269.016885000001));
#206679=CARTESIAN_POINT('Ctrl Pts',(-31.4256423778684,-30.4319350856944,
-255.550151000001));
#206680=CARTESIAN_POINT('Ctrl Pts',(-35.6736820983274,-36.2203711153481,
-248.816784000001));
#206681=CARTESIAN_POINT('Ctrl Pts',(-39.9217218187864,-42.0088071450018,
-242.083417000001));
#206682=CARTESIAN_POINT('Ctrl Pts',(-44.1697615392454,-47.7972431746554,
-235.35005));
#206683=CARTESIAN_POINT('Ctrl Pts',(-48.3757414604919,-53.5283679564908,
-228.68335));
#206684=CARTESIAN_POINT('Ctrl Pts',(-52.582425249623,-59.2584041216488,
-222.01665));
#206685=CARTESIAN_POINT('Ctrl Pts',(-56.7898089004066,-64.9873508559399,
-215.34995));
#206686=CARTESIAN_POINT('Ctrl Pts',(-56.8318827369145,-65.0446403232828,
-215.283283));
#206687=CARTESIAN_POINT('Ctrl Pts',(-56.8739565734223,-65.1019297906258,
-215.216616));
#206688=CARTESIAN_POINT('Ctrl Pts',(-56.9160304099302,-65.1592192579687,
-215.149949));
#206689=CARTESIAN_POINT('Ctrl Pts',(34.4954719600033,91.6721063226136,-376.750757));
#206690=CARTESIAN_POINT('Ctrl Pts',(18.9810705532065,65.8496728858911,-349.817289000001));
#206691=CARTESIAN_POINT('Ctrl Pts',(3.46666914640964,40.0272394491684,-322.883821));
#206692=CARTESIAN_POINT('Ctrl Pts',(-12.0477322603872,14.2048060124459,
-295.950353));
#206693=CARTESIAN_POINT('Ctrl Pts',(-19.8049329637856,1.2935892940846,-282.483619));
#206694=CARTESIAN_POINT('Ctrl Pts',(-27.562133667184,-11.6176274242767,
-269.016885));
#206695=CARTESIAN_POINT('Ctrl Pts',(-35.3193343705824,-24.528844142638,
-255.550151));
#206696=CARTESIAN_POINT('Ctrl Pts',(-39.1979347222817,-30.9844525018186,
-248.816784));
#206697=CARTESIAN_POINT('Ctrl Pts',(-43.0765350739809,-37.4400608609993,
-242.083417));
#206698=CARTESIAN_POINT('Ctrl Pts',(-46.9551354256801,-43.8956692201799,
-235.35005));
#206699=CARTESIAN_POINT('Ctrl Pts',(-50.7953337936991,-50.2873606649132,
-228.68335));
#206700=CARTESIAN_POINT('Ctrl Pts',(-54.6361431746697,-56.6785834369767,
-222.01665));
#206701=CARTESIAN_POINT('Ctrl Pts',(-58.477561814447,-63.069336786611,-215.34995));
#206702=CARTESIAN_POINT('Ctrl Pts',(-58.5159760008448,-63.1332443201074,
-215.283283));
#206703=CARTESIAN_POINT('Ctrl Pts',(-58.5543901872426,-63.1971518536037,
-215.216616));
#206704=CARTESIAN_POINT('Ctrl Pts',(-58.5928043736403,-63.2610593871,-215.149949));
#206705=CARTESIAN_POINT('Ctrl Pts',(31.8464935875069,98.4079754366887,-376.750756999999));
#206706=CARTESIAN_POINT('Ctrl Pts',(16.6079109017479,71.6637374050134,-349.817289));
#206707=CARTESIAN_POINT('Ctrl Pts',(1.36932821598904,44.919499373338,-322.883821));
#206708=CARTESIAN_POINT('Ctrl Pts',(-13.8692544697699,18.1752613416626,
-295.950353));
#206709=CARTESIAN_POINT('Ctrl Pts',(-21.4885458126493,4.80314232582491,
-282.483619));
#206710=CARTESIAN_POINT('Ctrl Pts',(-29.1078371555287,-8.56897669001278,
-269.016885));
#206711=CARTESIAN_POINT('Ctrl Pts',(-36.7271284984082,-21.9410957058504,
-255.550151));
#206712=CARTESIAN_POINT('Ctrl Pts',(-40.5367741698479,-28.6271552137693,
-248.816784));
#206713=CARTESIAN_POINT('Ctrl Pts',(-44.3464198412877,-35.3132147216881,
-242.083417));
#206714=CARTESIAN_POINT('Ctrl Pts',(-48.1560655127274,-41.999274229607,
-235.35005));
#206715=CARTESIAN_POINT('Ctrl Pts',(-51.9279919200935,-48.6191351285365,
-228.68335));
#206716=CARTESIAN_POINT('Ctrl Pts',(-55.7004001286368,-55.2387363218615,
-222.01665));
#206717=CARTESIAN_POINT('Ctrl Pts',(-59.4732891526772,-61.8580772083615,
-215.34995));
#206718=CARTESIAN_POINT('Ctrl Pts',(-59.5110180429176,-61.9242706172265,
-215.283283));
#206719=CARTESIAN_POINT('Ctrl Pts',(-59.548746933158,-61.9904640260915,
-215.216616));
#206720=CARTESIAN_POINT('Ctrl Pts',(-59.5864758233984,-62.0566574349565,
-215.149949));
#206721=CARTESIAN_POINT('Ctrl Pts',(21.2505800975213,125.351451892989,-376.750756999997));
#206722=CARTESIAN_POINT('Ctrl Pts',(7.11527229591406,94.9199954815027,-349.817288999997));
#206723=CARTESIAN_POINT('Ctrl Pts',(-7.02003550569317,64.4885390700161,
-322.883820999998));
#206724=CARTESIAN_POINT('Ctrl Pts',(-21.1553433073004,34.0570826585295,
-295.950352999998));
#206725=CARTESIAN_POINT('Ctrl Pts',(-28.222997208104,18.8413544527863,-282.483618999999));
#206726=CARTESIAN_POINT('Ctrl Pts',(-35.2906511089077,3.62562624704296,
-269.016884999999));
#206727=CARTESIAN_POINT('Ctrl Pts',(-42.3583050097113,-11.5901019587003,
-255.550151));
#206728=CARTESIAN_POINT('Ctrl Pts',(-45.8921319601131,-19.197966061572,
-248.816784));
#206729=CARTESIAN_POINT('Ctrl Pts',(-49.4259589105149,-26.8058301644436,
-242.083417));
#206730=CARTESIAN_POINT('Ctrl Pts',(-52.9597858609167,-34.4136942673153,
-235.35005));
#206731=CARTESIAN_POINT('Ctrl Pts',(-56.458624425671,-41.9462329830297,
-228.68335));
#206732=CARTESIAN_POINT('Ctrl Pts',(-59.957427944505,-49.4793478614006,
-222.01665));
#206733=CARTESIAN_POINT('Ctrl Pts',(-63.4561985055979,-57.0130388953633,
-215.34995));
#206734=CARTESIAN_POINT('Ctrl Pts',(-63.4911862112088,-57.0883758057029,
-215.283283));
#206735=CARTESIAN_POINT('Ctrl Pts',(-63.5261739168198,-57.1637127160426,
-215.216616));
#206736=CARTESIAN_POINT('Ctrl Pts',(-63.5611616224307,-57.2390496263822,
-215.149949));
#206737=CARTESIAN_POINT('Ctrl Pts',(10.6546666075359,152.29492834929,-376.750756999995));
#206738=CARTESIAN_POINT('Ctrl Pts',(-2.37736630991967,118.176253557992,
-349.817288999995));
#206739=CARTESIAN_POINT('Ctrl Pts',(-15.4093992273753,84.0575787666943,
-322.883820999996));
#206740=CARTESIAN_POINT('Ctrl Pts',(-28.4414321448309,49.9389039753965,
-295.950352999998));
#206741=CARTESIAN_POINT('Ctrl Pts',(-34.9574486035587,32.8795665797476,
-282.483618999998));
#206742=CARTESIAN_POINT('Ctrl Pts',(-41.4734650622865,15.8202291840987,
-269.016884999999));
#206743=CARTESIAN_POINT('Ctrl Pts',(-47.9894815210143,-1.2391082115502,
-255.550151));
#206744=CARTESIAN_POINT('Ctrl Pts',(-51.2474897503782,-9.76877690937465,
-248.816784));
#206745=CARTESIAN_POINT('Ctrl Pts',(-54.5054979797421,-18.2984456071991,
-242.083417));
#206746=CARTESIAN_POINT('Ctrl Pts',(-57.763506209106,-26.8281143050236,
-235.35005));
#206747=CARTESIAN_POINT('Ctrl Pts',(-60.9892569312485,-35.273330837523,
-228.683350000001));
#206748=CARTESIAN_POINT('Ctrl Pts',(-64.2144557603733,-43.7199594009398,
-222.016650000001));
#206749=CARTESIAN_POINT('Ctrl Pts',(-67.4391078585187,-52.1680005823651,
-215.349950000001));
#206750=CARTESIAN_POINT('Ctrl Pts',(-67.4713543795001,-52.2524809941794,
-215.283283000001));
#206751=CARTESIAN_POINT('Ctrl Pts',(-67.5036009004816,-52.3369614059937,
-215.216616));
#206752=CARTESIAN_POINT('Ctrl Pts',(-67.535847421463,-52.4214418178079,
-215.149949000001));
#206753=CARTESIAN_POINT('Ctrl Pts',(0.0587531175507312,179.238404805591,
-376.750756999993));
#206754=CARTESIAN_POINT('Ctrl Pts',(-11.8700049157533,141.432511634481,
-349.817288999993));
#206755=CARTESIAN_POINT('Ctrl Pts',(-23.7987629490573,103.626618463372,
-322.883820999995));
#206756=CARTESIAN_POINT('Ctrl Pts',(-35.7275209823613,65.8207252922634,
-295.950352999997));
#206757=CARTESIAN_POINT('Ctrl Pts',(-41.6918999990133,46.9177787067089,
-282.483618999997));
#206758=CARTESIAN_POINT('Ctrl Pts',(-47.6562790156653,28.0148321211544,
-269.016884999998));
#206759=CARTESIAN_POINT('Ctrl Pts',(-53.6206580323173,9.11188553559992,
-255.550150999999));
#206760=CARTESIAN_POINT('Ctrl Pts',(-56.6028475406433,-0.339587757177323,
-248.816784));
#206761=CARTESIAN_POINT('Ctrl Pts',(-59.5850370489693,-9.79106104995457,
-242.083416999999));
#206762=CARTESIAN_POINT('Ctrl Pts',(-62.5672265572953,-19.2425343427318,
-235.35005));
#206763=CARTESIAN_POINT('Ctrl Pts',(-65.519889436826,-28.6004286920162,
-228.683350000001));
#206764=CARTESIAN_POINT('Ctrl Pts',(-68.4714835762416,-37.9605709404789,
-222.016650000001));
#206765=CARTESIAN_POINT('Ctrl Pts',(-71.4220172114394,-47.322962269367,
-215.349950000001));
#206766=CARTESIAN_POINT('Ctrl Pts',(-71.4515225477914,-47.4165861826559,
-215.283283000001));
#206767=CARTESIAN_POINT('Ctrl Pts',(-71.4810278841433,-47.5102100959448,
-215.216616));
#206768=CARTESIAN_POINT('Ctrl Pts',(-71.5105332204953,-47.6038340092336,
-215.149949000001));
#206769=CARTESIAN_POINT('Ctrl Pts',(-31.728987352405,260.068834174492,-376.750756999986));
#206770=CARTESIAN_POINT('Ctrl Pts',(-40.3479207332542,211.20128586395,-349.817288999988));
#206771=CARTESIAN_POINT('Ctrl Pts',(-48.9668541141034,162.333737553407,
-322.883820999991));
#206772=CARTESIAN_POINT('Ctrl Pts',(-57.5857874949526,113.466189242864,
-295.950352999994));
#206773=CARTESIAN_POINT('Ctrl Pts',(-61.8952541853772,89.0324150875929,
-282.483618999995));
#206774=CARTESIAN_POINT('Ctrl Pts',(-66.2047208758018,64.5986409323216,
-269.016884999996));
#206775=CARTESIAN_POINT('Ctrl Pts',(-70.5141875662264,40.1648667770503,
-255.550150999998));
#206776=CARTESIAN_POINT('Ctrl Pts',(-72.6689209114386,27.9479796994146,
-248.816783999999));
#206777=CARTESIAN_POINT('Ctrl Pts',(-74.8236542566509,15.731092621779,-242.083416999999));
#206778=CARTESIAN_POINT('Ctrl Pts',(-76.9783876018632,3.51420554414337,
-235.35005));
#206779=CARTESIAN_POINT('Ctrl Pts',(-79.1117869535586,-8.58172225549588,
-228.683350000001));
#206780=CARTESIAN_POINT('Ctrl Pts',(-81.2425670238464,-20.6824055590965,
-222.016650000001));
#206781=CARTESIAN_POINT('Ctrl Pts',(-83.3707452702016,-32.7878473303725,
-215.349950000001));
#206782=CARTESIAN_POINT('Ctrl Pts',(-83.3920270526652,-32.9089017480852,
-215.283283000001));
#206783=CARTESIAN_POINT('Ctrl Pts',(-83.4133088351287,-33.0299561657981,
-215.216616));
#206784=CARTESIAN_POINT('Ctrl Pts',(-83.4345906175922,-33.1510105835108,
-215.149949000001));
#206785=CARTESIAN_POINT('Ctrl Pts',(-63.5167278223608,340.899263543393,
-376.750756999979));
#206786=CARTESIAN_POINT('Ctrl Pts',(-68.8258365507552,280.970060093418,
-349.817288999983));
#206787=CARTESIAN_POINT('Ctrl Pts',(-74.1349452791495,221.040856643441,
-322.883820999986));
#206788=CARTESIAN_POINT('Ctrl Pts',(-79.4440540075439,161.111653193465,
-295.950352999991));
#206789=CARTESIAN_POINT('Ctrl Pts',(-82.098608371741,131.147051468477,-282.483618999993));
#206790=CARTESIAN_POINT('Ctrl Pts',(-84.7531627359382,101.182449743489,
-269.016884999995));
#206791=CARTESIAN_POINT('Ctrl Pts',(-87.4077171001354,71.2178480185007,
-255.550150999997));
#206792=CARTESIAN_POINT('Ctrl Pts',(-88.734994282234,56.2355471560066,-248.816783999998));
#206793=CARTESIAN_POINT('Ctrl Pts',(-90.0622714643326,41.2532462935126,
-242.083416999999));
#206794=CARTESIAN_POINT('Ctrl Pts',(-91.3895486464312,26.2709454310185,
-235.35005));
#206795=CARTESIAN_POINT('Ctrl Pts',(-92.7036844702911,11.4369841810244,
-228.683350000001));
#206796=CARTESIAN_POINT('Ctrl Pts',(-94.0136504714512,-3.40424017771396,
-222.016650000001));
#206797=CARTESIAN_POINT('Ctrl Pts',(-95.3194733289638,-18.252732391378,
-215.349950000001));
#206798=CARTESIAN_POINT('Ctrl Pts',(-95.3325315575389,-18.4012173135146,
-215.283283000001));
#206799=CARTESIAN_POINT('Ctrl Pts',(-95.345589786114,-18.5497022356513,
-215.216616000001));
#206800=CARTESIAN_POINT('Ctrl Pts',(-95.3586480146891,-18.698187157788,
-215.149949000001));
#206801=CARTESIAN_POINT('Ctrl Pts',(-95.3044682923166,421.729692912295,
-376.750756999971));
#206802=CARTESIAN_POINT('Ctrl Pts',(-97.3037523682561,350.738834322885,
-349.817288999976));
#206803=CARTESIAN_POINT('Ctrl Pts',(-99.3030364441956,279.747975733475,
-322.883820999982));
#206804=CARTESIAN_POINT('Ctrl Pts',(-101.302320520135,208.757117144065,
-295.950352999988));
#206805=CARTESIAN_POINT('Ctrl Pts',(-102.301962558105,173.261687849361,
-282.48361899999));
#206806=CARTESIAN_POINT('Ctrl Pts',(-103.301604596075,137.766258554656,
-269.016884999993));
#206807=CARTESIAN_POINT('Ctrl Pts',(-104.301246634044,102.270829259951,
-255.550150999996));
#206808=CARTESIAN_POINT('Ctrl Pts',(-104.801067653029,84.5231146125986,
-248.816783999998));
#206809=CARTESIAN_POINT('Ctrl Pts',(-105.300888672014,66.7753999652462,
-242.083416999998));
#206810=CARTESIAN_POINT('Ctrl Pts',(-105.800709690999,49.0276853178937,
-235.35005));
#206811=CARTESIAN_POINT('Ctrl Pts',(-106.295581987024,31.4556906175448,
-228.683350000001));
#206812=CARTESIAN_POINT('Ctrl Pts',(-106.784733919056,13.8739252036685,
-222.016650000002));
#206813=CARTESIAN_POINT('Ctrl Pts',(-107.268201387726,-3.71761745238349,
-215.349950000002));
#206814=CARTESIAN_POINT('Ctrl Pts',(-107.273036062413,-3.89353287894403,
-215.283283000002));
#206815=CARTESIAN_POINT('Ctrl Pts',(-107.277870737099,-4.06944830550458,
-215.216616000002));
#206816=CARTESIAN_POINT('Ctrl Pts',(-107.282705411786,-4.24536373206513,
-215.149949000001));
#206817=CARTESIAN_POINT('Ctrl Pts',(-190.667689702184,664.220981018999,
-376.750756999951));
#206818=CARTESIAN_POINT('Ctrl Pts',(-182.737499820759,560.045157011288,
-349.81728899996));
#206819=CARTESIAN_POINT('Ctrl Pts',(-174.807309939334,455.869333003578,
-322.883820999969));
#206820=CARTESIAN_POINT('Ctrl Pts',(-166.877120057909,351.693508995868,
-295.950352999979));
#206821=CARTESIAN_POINT('Ctrl Pts',(-162.912025117196,299.605596992013,
-282.483618999983));
#206822=CARTESIAN_POINT('Ctrl Pts',(-158.946930176484,247.517684988157,
-269.016884999988));
#206823=CARTESIAN_POINT('Ctrl Pts',(-154.981835235771,195.429772984302,
-255.550150999993));
#206824=CARTESIAN_POINT('Ctrl Pts',(-152.999287765415,169.385816982375,
-248.816783999995));
#206825=CARTESIAN_POINT('Ctrl Pts',(-151.016740295059,143.341860980447,
-242.083416999997));
#206826=CARTESIAN_POINT('Ctrl Pts',(-149.034192824703,117.297904978519,
-235.35005));
#206827=CARTESIAN_POINT('Ctrl Pts',(-147.071274537221,91.5118099271058,
-228.683350000003));
#206828=CARTESIAN_POINT('Ctrl Pts',(-145.09798426187,65.708421347816,-222.016650000002));
#206829=CARTESIAN_POINT('Ctrl Pts',(-143.114385564013,39.8877273646,-215.349950000003));
#206830=CARTESIAN_POINT('Ctrl Pts',(-143.094549577034,39.6295204247678,
-215.283283000003));
#206831=CARTESIAN_POINT('Ctrl Pts',(-143.074713590055,39.3713134849356,
-215.216616000002));
#206832=CARTESIAN_POINT('Ctrl Pts',(-143.054877603077,39.1131065451034,
-215.149949000002));
#206833=CARTESIAN_POINT('Ctrl Pts',(-286.030911112051,906.712269125702,
-376.750756999929));
#206834=CARTESIAN_POINT('Ctrl Pts',(-268.171247273262,769.351479699691,
-349.817288999943));
#206835=CARTESIAN_POINT('Ctrl Pts',(-250.311583434473,631.990690273681,
-322.883820999956));
#206836=CARTESIAN_POINT('Ctrl Pts',(-232.451919595683,494.62990084767,-295.95035299997));
#206837=CARTESIAN_POINT('Ctrl Pts',(-223.522087676288,425.949506134664,
-282.483618999976));
#206838=CARTESIAN_POINT('Ctrl Pts',(-214.592255756894,357.269111421658,
-269.016884999983));
#206839=CARTESIAN_POINT('Ctrl Pts',(-205.662423837499,288.588716708654,
-255.55015099999));
#206840=CARTESIAN_POINT('Ctrl Pts',(-201.197507877801,254.24851935215,-248.816783999994));
#206841=CARTESIAN_POINT('Ctrl Pts',(-196.732591918104,219.908321995647,
-242.083416999997));
#206842=CARTESIAN_POINT('Ctrl Pts',(-192.267675958407,185.568124639145,
-235.35005));
#206843=CARTESIAN_POINT('Ctrl Pts',(-187.846967087419,151.567929236667,
-228.683350000004));
#206844=CARTESIAN_POINT('Ctrl Pts',(-183.411234604685,117.542917491964,
-222.016650000003));
#206845=CARTESIAN_POINT('Ctrl Pts',(-178.960569740299,83.4930721815835,
-215.349950000004));
#206846=CARTESIAN_POINT('Ctrl Pts',(-178.916063091656,83.1525737284796,
-215.283283000004));
#206847=CARTESIAN_POINT('Ctrl Pts',(-178.871556443012,82.8120752753758,
-215.216616000004));
#206848=CARTESIAN_POINT('Ctrl Pts',(-178.827049794367,82.4715768222719,
-215.149949000004));
#206849=CARTESIAN_POINT('Ctrl Pts',(-381.394132521918,1149.20355723241,
-376.750756999909));
#206850=CARTESIAN_POINT('Ctrl Pts',(-353.604994725765,978.657802388094,
-349.817288999926));
#206851=CARTESIAN_POINT('Ctrl Pts',(-325.815856929611,808.112047543783,
-322.883820999944));
#206852=CARTESIAN_POINT('Ctrl Pts',(-298.026719133457,637.566292699472,
-295.950352999961));
#206853=CARTESIAN_POINT('Ctrl Pts',(-284.13215023538,552.293415277316,-282.48361899997));
#206854=CARTESIAN_POINT('Ctrl Pts',(-270.237581337303,467.02053785516,-269.016884999978));
#206855=CARTESIAN_POINT('Ctrl Pts',(-256.343012439226,381.747660433005,
-255.550150999987));
#206856=CARTESIAN_POINT('Ctrl Pts',(-249.395727990188,339.111221721927,
-248.816783999992));
#206857=CARTESIAN_POINT('Ctrl Pts',(-242.448443541149,296.474783010849,
-242.083416999996));
#206858=CARTESIAN_POINT('Ctrl Pts',(-235.501159092111,253.83834429977,-235.35005));
#206859=CARTESIAN_POINT('Ctrl Pts',(-228.622659637617,211.624048546228,
-228.683350000005));
#206860=CARTESIAN_POINT('Ctrl Pts',(-221.724484947499,169.377413636111,
-222.016650000005));
#206861=CARTESIAN_POINT('Ctrl Pts',(-214.806753916586,127.098416998567,
-215.349950000004));
#206862=CARTESIAN_POINT('Ctrl Pts',(-214.737576606277,126.675627032191,
-215.283283000005));
#206863=CARTESIAN_POINT('Ctrl Pts',(-214.668399295968,126.252837065816,
-215.216616000005));
#206864=CARTESIAN_POINT('Ctrl Pts',(-214.599221985659,125.83004709944,-215.149949000005));
#206865=CARTESIAN_POINT('Ctrl Pts',(-667.483796751521,1876.67742155251,
-376.750756999846));
#206866=CARTESIAN_POINT('Ctrl Pts',(-609.906237083273,1606.57677045331,
-349.817288999875));
#206867=CARTESIAN_POINT('Ctrl Pts',(-552.328677415026,1336.47611935409,
-322.883820999905));
#206868=CARTESIAN_POINT('Ctrl Pts',(-494.751117746779,1066.37546825488,
-295.950352999934));
#206869=CARTESIAN_POINT('Ctrl Pts',(-465.962337912655,931.325142705271,
-282.483618999949));
#206870=CARTESIAN_POINT('Ctrl Pts',(-437.173558078531,796.274817155664,
-269.016884999963));
#206871=CARTESIAN_POINT('Ctrl Pts',(-408.384778244408,661.224491606058,
-255.550150999978));
#206872=CARTESIAN_POINT('Ctrl Pts',(-393.990388327346,593.699328831254,
-248.816783999986));
#206873=CARTESIAN_POINT('Ctrl Pts',(-379.595998410284,526.174166056451,
-242.083416999993));
#206874=CARTESIAN_POINT('Ctrl Pts',(-365.201608493222,458.649003281647,
-235.35005));
#206875=CARTESIAN_POINT('Ctrl Pts',(-350.94973728821,391.792406474911,-228.683350000008));
#206876=CARTESIAN_POINT('Ctrl Pts',(-336.664235975943,324.880902068554,
-222.016650000008));
#206877=CARTESIAN_POINT('Ctrl Pts',(-322.345306445446,257.914451449517,
-215.349950000008));
#206878=CARTESIAN_POINT('Ctrl Pts',(-322.202117150141,257.244786943327,
-215.283283000008));
#206879=CARTESIAN_POINT('Ctrl Pts',(-322.058927854835,256.575122437136,
-215.216616000008));
#206880=CARTESIAN_POINT('Ctrl Pts',(-321.91573855953,255.905457930946,-215.149949000007));
#206881=CARTESIAN_POINT('Ctrl Pts',(-953.573460981123,2604.15128587263,
-376.750756999783));
#206882=CARTESIAN_POINT('Ctrl Pts',(-866.207479440782,2234.49573851851,
-349.817288999824));
#206883=CARTESIAN_POINT('Ctrl Pts',(-778.841497900441,1864.8401911644,-322.883820999866));
#206884=CARTESIAN_POINT('Ctrl Pts',(-691.4755163601,1495.18464381028,-295.950352999906));
#206885=CARTESIAN_POINT('Ctrl Pts',(-647.79252558993,1310.35687013323,-282.483618999927));
#206886=CARTESIAN_POINT('Ctrl Pts',(-604.109534819759,1125.52909645617,
-269.016884999948));
#206887=CARTESIAN_POINT('Ctrl Pts',(-560.426544049589,940.701322779111,
-255.550150999969));
#206888=CARTESIAN_POINT('Ctrl Pts',(-538.585048664503,848.287435940582,
-248.81678399998));
#206889=CARTESIAN_POINT('Ctrl Pts',(-516.743553279418,755.873549102053,
-242.08341699999));
#206890=CARTESIAN_POINT('Ctrl Pts',(-494.902057894333,663.459662263524,
-235.35005));
#206891=CARTESIAN_POINT('Ctrl Pts',(-473.276814938803,571.960764403594,
-228.683350000011));
#206892=CARTESIAN_POINT('Ctrl Pts',(-451.603987004386,480.384390500996,
-222.016650000011));
#206893=CARTESIAN_POINT('Ctrl Pts',(-429.883858974306,388.730485900468,
-215.34995000001));
#206894=CARTESIAN_POINT('Ctrl Pts',(-429.666657694005,387.813946854463,
-215.28328300001));
#206895=CARTESIAN_POINT('Ctrl Pts',(-429.449456413704,386.897407808457,
-215.216616000011));
#206896=CARTESIAN_POINT('Ctrl Pts',(-429.232255133403,385.980868762451,
-215.149949000011));
#206897=CARTESIAN_POINT('Ctrl Pts',(-1239.66312521072,3331.62515019274,
-376.750756999719));
#206898=CARTESIAN_POINT('Ctrl Pts',(-1122.50872179829,2862.41470658373,
-349.817288999773));
#206899=CARTESIAN_POINT('Ctrl Pts',(-1005.35431838586,2393.20426297471,
-322.883820999826));
#206900=CARTESIAN_POINT('Ctrl Pts',(-888.199914973422,1923.99381936569,
-295.95035299988));
#206901=CARTESIAN_POINT('Ctrl Pts',(-829.622713267204,1689.38859756118,
-282.483618999906));
#206902=CARTESIAN_POINT('Ctrl Pts',(-771.045511560987,1454.78337575667,
-269.016884999933));
#206903=CARTESIAN_POINT('Ctrl Pts',(-712.46830985477,1220.17815395216,-255.55015099996));
#206904=CARTESIAN_POINT('Ctrl Pts',(-683.179709001661,1102.87554304991,
-248.816783999974));
#206905=CARTESIAN_POINT('Ctrl Pts',(-653.891108148553,985.572932147655,
-242.083416999987));
#206906=CARTESIAN_POINT('Ctrl Pts',(-624.602507295445,868.2703212454,-235.35005));
#206907=CARTESIAN_POINT('Ctrl Pts',(-595.603892589396,752.129122332277,
-228.683350000014));
#206908=CARTESIAN_POINT('Ctrl Pts',(-566.54373803283,635.887878933439,-222.016650000014));
#206909=CARTESIAN_POINT('Ctrl Pts',(-537.422411503166,519.546520351418,
-215.349950000014));
#206910=CARTESIAN_POINT('Ctrl Pts',(-537.131198237869,518.383106765598,
-215.283283000013));
#206911=CARTESIAN_POINT('Ctrl Pts',(-536.839984972572,517.219693179777,
-215.216616000014));
#206912=CARTESIAN_POINT('Ctrl Pts',(-536.548771707275,516.056279593957,
-215.149949000014));
#206913=CARTESIAN_POINT('Ctrl Pts',(-2097.93211789953,5514.04674315307,
-376.750756999531));
#206914=CARTESIAN_POINT('Ctrl Pts',(-1891.41244887082,4746.17161077935,
-349.81728899962));
#206915=CARTESIAN_POINT('Ctrl Pts',(-1684.8927798421,3978.29647840563,-322.88382099971));
#206916=CARTESIAN_POINT('Ctrl Pts',(-1478.37311081339,3210.42134603191,
-295.950352999799));
#206917=CARTESIAN_POINT('Ctrl Pts',(-1375.11327629903,2826.48377984504,
-282.483618999843));
#206918=CARTESIAN_POINT('Ctrl Pts',(-1271.85344178467,2442.54621365819,
-269.016884999889));
#206919=CARTESIAN_POINT('Ctrl Pts',(-1168.59360727031,2058.60864747133,
-255.550150999933));
#206920=CARTESIAN_POINT('Ctrl Pts',(-1116.96369001313,1866.6398643779,-248.816783999956));
#206921=CARTESIAN_POINT('Ctrl Pts',(-1065.33377275596,1674.67108128446,
-242.083416999977));
#206922=CARTESIAN_POINT('Ctrl Pts',(-1013.70385549878,1482.70229819103,
-235.35005));
#206923=CARTESIAN_POINT('Ctrl Pts',(-962.585125541175,1292.63419611833,
-228.683350000023));
#206924=CARTESIAN_POINT('Ctrl Pts',(-911.362991118159,1102.39834423077,
-222.016650000023));
#206925=CARTESIAN_POINT('Ctrl Pts',(-860.038069089746,911.99462370427,-215.349950000023));
#206926=CARTESIAN_POINT('Ctrl Pts',(-859.524819869462,910.090586499004,
-215.283283000022));
#206927=CARTESIAN_POINT('Ctrl Pts',(-859.011570649176,908.186549293739,
-215.216616000022));
#206928=CARTESIAN_POINT('Ctrl Pts',(-858.498321428892,906.282512088474,
-215.149949000023));
#206929=CARTESIAN_POINT('Ctrl Pts',(-2956.20111058834,7696.4683361134,-376.750756999341));
#206930=CARTESIAN_POINT('Ctrl Pts',(-2660.31617594335,6629.92851497498,
-349.817288999467));
#206931=CARTESIAN_POINT('Ctrl Pts',(-2364.43124129834,5563.38869383655,
-322.883820999593));
#206932=CARTESIAN_POINT('Ctrl Pts',(-2068.54630665335,4496.84887269812,
-295.950352999718));
#206933=CARTESIAN_POINT('Ctrl Pts',(-1920.60383933086,3963.57896212891,
-282.48361899978));
#206934=CARTESIAN_POINT('Ctrl Pts',(-1772.66137200836,3430.3090515597,-269.016884999844));
#206935=CARTESIAN_POINT('Ctrl Pts',(-1624.71890468586,2897.03914099049,
-255.550150999906));
#206936=CARTESIAN_POINT('Ctrl Pts',(-1550.74767102461,2630.40418570588,
-248.816783999938));
#206937=CARTESIAN_POINT('Ctrl Pts',(-1476.77643736336,2363.76923042127,
-242.083416999969));
#206938=CARTESIAN_POINT('Ctrl Pts',(-1402.80520370211,2097.13427513666,
-235.35005));
#206939=CARTESIAN_POINT('Ctrl Pts',(-1329.56635849295,1833.13926990437,
-228.683350000032));
#206940=CARTESIAN_POINT('Ctrl Pts',(-1256.18224420349,1568.9088095281,-222.016650000032));
#206941=CARTESIAN_POINT('Ctrl Pts',(-1182.65372667633,1304.44272705712,
-215.349950000032));
#206942=CARTESIAN_POINT('Ctrl Pts',(-1181.91844150105,1301.79806623241,
-215.283283000032));
#206943=CARTESIAN_POINT('Ctrl Pts',(-1181.18315632578,1299.1534054077,-215.216616000032));
#206944=CARTESIAN_POINT('Ctrl Pts',(-1180.44787115051,1296.50874458299,
-215.149949000032));
#206945=CARTESIAN_POINT('Ctrl Pts',(-3814.47010327714,9878.88992907374,
-376.750756999153));
#206946=CARTESIAN_POINT('Ctrl Pts',(-3429.21990301587,8513.68541917061,
-349.817288999315));
#206947=CARTESIAN_POINT('Ctrl Pts',(-3043.96970275459,7148.48090926748,
-322.883820999476));
#206948=CARTESIAN_POINT('Ctrl Pts',(-2658.71950249332,5783.27639936434,
-295.950352999637));
#206949=CARTESIAN_POINT('Ctrl Pts',(-2466.09440236268,5100.67414441278,
-282.483618999717));
#206950=CARTESIAN_POINT('Ctrl Pts',(-2273.46930223204,4418.07188946121,
-269.016884999799));
#206951=CARTESIAN_POINT('Ctrl Pts',(-2080.84420210141,3735.46963450965,
-255.550150999879));
#206952=CARTESIAN_POINT('Ctrl Pts',(-1984.53165203609,3394.16850703386,
-248.81678399992));
#206953=CARTESIAN_POINT('Ctrl Pts',(-1888.21910197076,3052.86737955808,
-242.08341699996));
#206954=CARTESIAN_POINT('Ctrl Pts',(-1791.90655190545,2711.56625208229,
-235.35005));
#206955=CARTESIAN_POINT('Ctrl Pts',(-1696.54759144473,2373.64434369042,
-228.683350000041));
#206956=CARTESIAN_POINT('Ctrl Pts',(-1601.00149728882,2035.41927482542,
-222.016650000041));
#206957=CARTESIAN_POINT('Ctrl Pts',(-1505.26938426291,1696.89083040998,
-215.349950000041));
#206958=CARTESIAN_POINT('Ctrl Pts',(-1504.31206313264,1693.50554596582,
-215.28328300004));
#206959=CARTESIAN_POINT('Ctrl Pts',(-1503.35474200239,1690.12026152166,
-215.216616000041));
#206960=CARTESIAN_POINT('Ctrl Pts',(-1502.39742087213,1686.7349770775,-215.149949000041));
#206961=CARTESIAN_POINT('Origin',(636.934816028482,-11.5034818258361,-229.35005));
#206962=CARTESIAN_POINT('Origin',(636.934816028482,-11.5034818258361,-229.35005));
#206963=CARTESIAN_POINT('Origin',(636.934816028482,-11.5034818258361,-229.35005));
#206964=CARTESIAN_POINT('Origin',(636.934816028482,-11.5034818258361,-229.35005));
#206965=CARTESIAN_POINT('Origin',(636.934816028482,-11.5034818258361,-229.35005));
#206966=CARTESIAN_POINT('Origin',(636.934816028482,-11.5034818258361,-229.35005));
#206967=CARTESIAN_POINT('Origin',(636.934816028482,-11.5034818258361,-229.35005));
#206968=CARTESIAN_POINT('Origin',(636.934816028482,-11.5034818258361,-229.35005));
#206969=CARTESIAN_POINT('Origin',(636.934816028482,-11.5034818258361,-229.35005));
#206970=CARTESIAN_POINT('Origin',(636.934816028482,-11.5034818258361,-229.35005));
#206971=CARTESIAN_POINT('Origin',(0.,-32.21456093117,-229.35005));
#206972=CARTESIAN_POINT('',(0.,-32.21456093117,-229.35005));
#206973=CARTESIAN_POINT('Origin',(0.,-33.21456093117,-229.35005));
#206974=CARTESIAN_POINT('',(0.,-33.21456093117,-229.35005));
#206975=CARTESIAN_POINT('Origin',(2.22174260618994E-13,-11.0034818258363,
-229.35005));
#206976=CARTESIAN_POINT('',(2.22174260618994E-13,-11.0034818258363,-229.35005));
#206977=CARTESIAN_POINT('Origin',(2.22174260618994E-13,-12.0034818258363,
-229.35005));
#206978=CARTESIAN_POINT('',(2.22174260618994E-13,-12.0034818258363,-229.35005));
#206979=CARTESIAN_POINT('Origin',(1.54373336646987E-15,-42.8201004838369,
-229.35005));
#206980=CARTESIAN_POINT('',(1.54373336646987E-15,-42.8201004838369,-229.35005));
#206981=CARTESIAN_POINT('Origin',(1.23757166668304E-15,-43.8201004838368,
-229.35005));
#206982=CARTESIAN_POINT('',(1.23757166668304E-15,-43.8201004838368,-229.35005));
#206983=CARTESIAN_POINT('Origin',(2.8425373731103E-15,9.20759727949731,
-229.35005));
#206984=CARTESIAN_POINT('',(2.8425373731103E-15,9.20759727949731,-229.35005));
#206985=CARTESIAN_POINT('Origin',(2.53637567332344E-15,10.2075972794973,
-229.35005));
#206986=CARTESIAN_POINT('',(2.53637567332344E-15,10.2075972794973,-229.35005));
#206987=CARTESIAN_POINT('Origin',(1.54373336646988E-15,19.8131368321642,
-229.35005));
#206988=CARTESIAN_POINT('',(1.54373336646988E-15,19.8131368321642,-229.35005));
#206989=CARTESIAN_POINT('Origin',(1.23757166668304E-15,20.8131368321642,
-229.35005));
#206990=CARTESIAN_POINT('',(1.23757166668304E-15,20.8131368321642,-229.35005));
#206991=CARTESIAN_POINT('Origin',(2.61456814389029E-14,-173.57701443073,
-229.35005));
#206992=CARTESIAN_POINT('Origin',(2.61456814389029E-14,-173.57701443073,
-229.35005));
#206993=CARTESIAN_POINT('Origin',(-7.14692237356698E-14,623.509175991979,
-229.35005));
#206994=CARTESIAN_POINT('Origin',(-7.14692237356698E-14,623.509175991979,
-229.35005));
#206995=CARTESIAN_POINT('Origin',(2.61456814389029E-14,-173.57701443073,
-229.35005));
#206996=CARTESIAN_POINT('Origin',(2.61456814389029E-14,-173.57701443073,
-232.25005));
#206997=CARTESIAN_POINT('Origin',(2.61456814389029E-14,-173.57701443073,
-229.35005));
#206998=CARTESIAN_POINT('Origin',(0.,-32.21456093117,-229.35005));
#206999=CARTESIAN_POINT('',(0.,-32.21456093117,-229.35005));
#207000=CARTESIAN_POINT('Origin',(0.,-33.21456093117,-229.35005));
#207001=CARTESIAN_POINT('',(0.,-33.21456093117,-229.35005));
#207002=CARTESIAN_POINT('Origin',(3.33261390928491E-13,-21.6090213785032,
-229.35005));
#207003=CARTESIAN_POINT('',(3.33261390928491E-13,-21.6090213785032,-229.35005));
#207004=CARTESIAN_POINT('Origin',(3.33261390928491E-13,-22.6090213785032,
-229.35005));
#207005=CARTESIAN_POINT('',(3.33261390928491E-13,-22.6090213785032,-229.35005));
#207006=CARTESIAN_POINT('Origin',(2.22174260618994E-13,-11.0034818258363,
-229.35005));
#207007=CARTESIAN_POINT('',(2.22174260618994E-13,-11.0034818258363,-229.35005));
#207008=CARTESIAN_POINT('Origin',(2.22174260618994E-13,-12.0034818258363,
-229.35005));
#207009=CARTESIAN_POINT('',(2.22174260618994E-13,-12.0034818258363,-229.35005));
#207010=CARTESIAN_POINT('Origin',(1.11087130309497E-13,-0.397942273169518,
-229.35005));
#207011=CARTESIAN_POINT('',(1.11087130309497E-13,-0.397942273169518,-229.35005));
#207012=CARTESIAN_POINT('Origin',(1.11087130309497E-13,-1.3979422731695,
-229.35005));
#207013=CARTESIAN_POINT('',(1.11087130309497E-13,-1.3979422731695,-229.35005));
#207014=CARTESIAN_POINT('Origin',(1.54373336646987E-15,-42.8201004838369,
-229.35005));
#207015=CARTESIAN_POINT('',(1.54373336646987E-15,-42.8201004838369,-229.35005));
#207016=CARTESIAN_POINT('Origin',(1.23757166668304E-15,-43.8201004838368,
-229.35005));
#207017=CARTESIAN_POINT('',(1.23757166668304E-15,-43.8201004838368,-229.35005));
#207018=CARTESIAN_POINT('Origin',(2.8425373731103E-15,9.20759727949731,
-229.35005));
#207019=CARTESIAN_POINT('',(2.8425373731103E-15,9.20759727949731,-229.35005));
#207020=CARTESIAN_POINT('Origin',(2.53637567332344E-15,10.2075972794973,
-229.35005));
#207021=CARTESIAN_POINT('',(2.53637567332344E-15,10.2075972794973,-229.35005));
#207022=CARTESIAN_POINT('Origin',(1.54373336646988E-15,19.8131368321642,
-229.35005));
#207023=CARTESIAN_POINT('',(1.54373336646988E-15,19.8131368321642,-229.35005));
#207024=CARTESIAN_POINT('Origin',(1.23757166668304E-15,20.8131368321642,
-229.35005));
#207025=CARTESIAN_POINT('',(1.23757166668304E-15,20.8131368321642,-229.35005));
#207026=CARTESIAN_POINT('Origin',(2.61456814389029E-14,-173.57701443073,
-229.35005));
#207027=CARTESIAN_POINT('Origin',(2.61456814389029E-14,-173.57701443073,
-229.35005));
#207028=CARTESIAN_POINT('Origin',(2.61456814389029E-14,-173.57701443073,
-229.35005));
#207029=CARTESIAN_POINT('Origin',(2.61456814389029E-14,-173.57701443073,
-229.35005));
#207030=CARTESIAN_POINT('Origin',(-7.14692237356698E-14,623.509175991979,
-229.35005));
#207031=CARTESIAN_POINT('Origin',(-7.14692237356698E-14,623.509175991979,
-229.35005));
#207032=CARTESIAN_POINT('Origin',(-7.14692237356698E-14,623.509175991979,
-229.35005));
#207033=CARTESIAN_POINT('Origin',(-7.14692237356698E-14,623.509175991979,
-229.35005));
#207034=CARTESIAN_POINT('Origin',(6.29739814579425E-15,-11.5034818258363,
-229.35005));
#207035=CARTESIAN_POINT('Origin',(6.29739814579425E-15,-11.5034818258363,
-229.35005));
#207036=CARTESIAN_POINT('Origin',(6.29739814579425E-15,-11.5034818258363,
-229.35005));
#207037=CARTESIAN_POINT('Origin',(6.29739814579425E-15,-11.5034818258363,
-229.35005));
#207038=CARTESIAN_POINT('Origin',(6.29739814579425E-15,-11.5034818258363,
-229.35005));
#207039=CARTESIAN_POINT('Origin',(6.29739814579425E-15,-11.5034818258363,
-229.35005));
#207040=CARTESIAN_POINT('Origin',(6.29739814579425E-15,-11.5034818258363,
-229.35005));
#207041=CARTESIAN_POINT('Origin',(6.29739814579425E-15,-11.5034818258363,
-229.35005));
#207042=CARTESIAN_POINT('Origin',(0.,-32.21456093117,-229.35005));
#207043=CARTESIAN_POINT('',(0.,-32.21456093117,-229.35005));
#207044=CARTESIAN_POINT('Origin',(0.,-32.21456093117,-229.35005));
#207045=CARTESIAN_POINT('',(0.,-32.21456093117,-229.35005));
#207046=CARTESIAN_POINT('Origin',(0.,-33.21456093117,-229.35005));
#207047=CARTESIAN_POINT('',(0.,-33.21456093117,-229.35005));
#207048=CARTESIAN_POINT('Origin',(0.,-33.21456093117,-229.35005));
#207049=CARTESIAN_POINT('',(0.,-33.21456093117,-229.35005));
#207050=CARTESIAN_POINT('Origin',(3.33261390928491E-13,-21.6090213785032,
-229.35005));
#207051=CARTESIAN_POINT('',(3.33261390928491E-13,-21.6090213785032,-229.35005));
#207052=CARTESIAN_POINT('Origin',(3.33261390928491E-13,-21.6090213785032,
-229.35005));
#207053=CARTESIAN_POINT('',(3.33261390928491E-13,-21.6090213785032,-229.35005));
#207054=CARTESIAN_POINT('Origin',(3.33261390928491E-13,-22.6090213785032,
-229.35005));
#207055=CARTESIAN_POINT('',(3.33261390928491E-13,-22.6090213785032,-229.35005));
#207056=CARTESIAN_POINT('Origin',(3.33261390928491E-13,-22.6090213785032,
-229.35005));
#207057=CARTESIAN_POINT('',(3.33261390928491E-13,-22.6090213785032,-229.35005));
#207058=CARTESIAN_POINT('Origin',(2.22174260618994E-13,-11.0034818258363,
-229.35005));
#207059=CARTESIAN_POINT('',(2.22174260618994E-13,-11.0034818258363,-229.35005));
#207060=CARTESIAN_POINT('Origin',(2.22174260618994E-13,-11.0034818258363,
-229.35005));
#207061=CARTESIAN_POINT('',(2.22174260618994E-13,-11.0034818258363,-229.35005));
#207062=CARTESIAN_POINT('Origin',(2.22174260618994E-13,-12.0034818258363,
-229.35005));
#207063=CARTESIAN_POINT('',(2.22174260618994E-13,-12.0034818258363,-229.35005));
#207064=CARTESIAN_POINT('Origin',(2.22174260618994E-13,-12.0034818258363,
-229.35005));
#207065=CARTESIAN_POINT('',(2.22174260618994E-13,-12.0034818258363,-229.35005));
#207066=CARTESIAN_POINT('Origin',(1.11087130309497E-13,-0.397942273169518,
-229.35005));
#207067=CARTESIAN_POINT('',(1.11087130309497E-13,-0.397942273169518,-229.35005));
#207068=CARTESIAN_POINT('Origin',(1.11087130309497E-13,-0.397942273169518,
-229.35005));
#207069=CARTESIAN_POINT('',(1.11087130309497E-13,-0.397942273169518,-229.35005));
#207070=CARTESIAN_POINT('Origin',(1.11087130309497E-13,-1.3979422731695,
-229.35005));
#207071=CARTESIAN_POINT('',(1.11087130309497E-13,-1.3979422731695,-229.35005));
#207072=CARTESIAN_POINT('Origin',(1.11087130309497E-13,-1.3979422731695,
-229.35005));
#207073=CARTESIAN_POINT('',(1.11087130309497E-13,-1.3979422731695,-229.35005));
#207074=CARTESIAN_POINT('Origin',(1.54373336646987E-15,-42.8201004838369,
-229.35005));
#207075=CARTESIAN_POINT('',(1.54373336646987E-15,-42.8201004838369,-229.35005));
#207076=CARTESIAN_POINT('Origin',(1.54373336646987E-15,-42.8201004838369,
-229.35005));
#207077=CARTESIAN_POINT('',(1.54373336646987E-15,-42.8201004838369,-229.35005));
#207078=CARTESIAN_POINT('Origin',(1.23757166668304E-15,-43.8201004838368,
-229.35005));
#207079=CARTESIAN_POINT('',(1.23757166668304E-15,-43.8201004838368,-229.35005));
#207080=CARTESIAN_POINT('Origin',(1.23757166668304E-15,-43.8201004838368,
-229.35005));
#207081=CARTESIAN_POINT('',(1.23757166668304E-15,-43.8201004838368,-229.35005));
#207082=CARTESIAN_POINT('Origin',(2.8425373731103E-15,9.20759727949731,
-229.35005));
#207083=CARTESIAN_POINT('',(2.8425373731103E-15,9.20759727949731,-229.35005));
#207084=CARTESIAN_POINT('Origin',(2.8425373731103E-15,9.20759727949731,
-229.35005));
#207085=CARTESIAN_POINT('',(2.8425373731103E-15,9.20759727949731,-229.35005));
#207086=CARTESIAN_POINT('Origin',(2.53637567332344E-15,10.2075972794973,
-229.35005));
#207087=CARTESIAN_POINT('',(2.53637567332344E-15,10.2075972794973,-229.35005));
#207088=CARTESIAN_POINT('Origin',(2.53637567332344E-15,10.2075972794973,
-229.35005));
#207089=CARTESIAN_POINT('',(2.53637567332344E-15,10.2075972794973,-229.35005));
#207090=CARTESIAN_POINT('Origin',(1.54373336646988E-15,19.8131368321642,
-229.35005));
#207091=CARTESIAN_POINT('',(1.54373336646988E-15,19.8131368321642,-229.35005));
#207092=CARTESIAN_POINT('Origin',(1.54373336646988E-15,19.8131368321642,
-229.35005));
#207093=CARTESIAN_POINT('',(1.54373336646988E-15,19.8131368321642,-229.35005));
#207094=CARTESIAN_POINT('Origin',(1.23757166668304E-15,20.8131368321642,
-229.35005));
#207095=CARTESIAN_POINT('',(1.23757166668304E-15,20.8131368321642,-229.35005));
#207096=CARTESIAN_POINT('Origin',(1.23757166668304E-15,20.8131368321642,
-229.35005));
#207097=CARTESIAN_POINT('',(1.23757166668304E-15,20.8131368321642,-229.35005));
#207098=CARTESIAN_POINT('Ctrl Pts',(51.7233397168138,38.3762252975093,-227.858776203219));
#207099=CARTESIAN_POINT('Ctrl Pts',(51.7302447133037,38.3813101134616,-228.35005));
#207100=CARTESIAN_POINT('Ctrl Pts',(52.1258919562643,38.67266339879,-228.35005));
#207101=CARTESIAN_POINT('Ctrl Pts',(51.6174495896917,38.5200202664566,-227.858776175692));
#207102=CARTESIAN_POINT('Ctrl Pts',(51.6128088111955,38.5425689461205,-228.410692739194));
#207103=CARTESIAN_POINT('Ctrl Pts',(52.0466039743291,38.878041220954,-228.35005));
#207104=CARTESIAN_POINT('Ctrl Pts',(51.5002798258237,38.6559630716119,-227.854887707304));
#207105=CARTESIAN_POINT('Ctrl Pts',(51.5043449566927,38.6663650434491,-228.441452922891));
#207106=CARTESIAN_POINT('Ctrl Pts',(51.9333069568917,39.0542288907298,-228.338384512236));
#207107=CARTESIAN_POINT('Ctrl Pts',(51.247332174135,38.9079983209904,-227.854896823446));
#207108=CARTESIAN_POINT('Ctrl Pts',(51.2577525408945,38.9120667908531,-228.441337182113));
#207109=CARTESIAN_POINT('Ctrl Pts',(51.6439737530735,39.342374196026,-228.3384118607));
#207110=CARTESIAN_POINT('Ctrl Pts',(51.1119650116918,39.023887086559,-227.858776175352));
#207111=CARTESIAN_POINT('Ctrl Pts',(51.1344983277446,39.0193462915006,-228.410782960183));
#207112=CARTESIAN_POINT('Ctrl Pts',(51.4685984426326,39.4543128793957,-228.35005));
#207113=CARTESIAN_POINT('Ctrl Pts',(50.9675450051224,39.1294935022024,-227.858776203219));
#207114=CARTESIAN_POINT('Ctrl Pts',(50.9726066716339,39.136415486161,-228.35005));
#207115=CARTESIAN_POINT('Ctrl Pts',(51.2626335243565,39.533036088795,-228.35005));
#207116=CARTESIAN_POINT('',(52.1258919562641,38.6726633987897,-228.35005));
#207117=CARTESIAN_POINT('',(51.7233397168138,38.3762252975093,-227.858776203219));
#207118=CARTESIAN_POINT('Origin',(52.1258919562641,38.6726633987897,-227.85005));
#207119=CARTESIAN_POINT('',(50.9675450051224,39.1294935022024,-227.858776203219));
#207120=CARTESIAN_POINT('Ctrl Pts',(50.9675450051224,39.1294935022024,-227.858776203219));
#207121=CARTESIAN_POINT('Ctrl Pts',(50.9830880714985,39.1181277118405,-227.858776203219));
#207122=CARTESIAN_POINT('Ctrl Pts',(51.0010148380594,39.1048281103116,-227.858730357654));
#207123=CARTESIAN_POINT('Ctrl Pts',(51.0212177237975,39.0894556321685,-227.85860987035));
#207124=CARTESIAN_POINT('Ctrl Pts',(51.0407951016109,39.0745591061753,-227.858493113492));
#207125=CARTESIAN_POINT('Ctrl Pts',(51.0625096818472,39.0577159016543,-227.858305190088));
#207126=CARTESIAN_POINT('Ctrl Pts',(51.0862346209097,39.0387664781746,-227.858039584716));
#207127=CARTESIAN_POINT('Ctrl Pts',(51.108501017397,39.0209820119935,-227.857790308017));
#207128=CARTESIAN_POINT('Ctrl Pts',(51.1325379340948,39.0013420490696,-227.857471813149));
#207129=CARTESIAN_POINT('Ctrl Pts',(51.1582177288737,38.9796886779462,-227.857109298627));
#207130=CARTESIAN_POINT('Ctrl Pts',(51.164515737183,38.9743781560967,-227.857020391395));
#207131=CARTESIAN_POINT('Ctrl Pts',(51.1709124581292,38.968946412574,-227.8569290201));
#207132=CARTESIAN_POINT('Ctrl Pts',(51.1774058068761,38.9633908868785,-227.85683594779));
#207133=CARTESIAN_POINT('Ctrl Pts',(51.2041328930996,38.9405239471736,-227.856452855527));
#207134=CARTESIAN_POINT('Ctrl Pts',(51.2285321441227,38.9189559026779,-227.856101868042));
#207135=CARTESIAN_POINT('Ctrl Pts',(51.2507490067655,38.8988503544204,-227.85581896922));
#207136=CARTESIAN_POINT('Ctrl Pts',(51.2739503915884,38.8778538451608,-227.855523533967));
#207137=CARTESIAN_POINT('Ctrl Pts',(51.2947718475604,38.8584525160497,-227.855301345718));
#207138=CARTESIAN_POINT('Ctrl Pts',(51.3133513197527,38.8408013282161,-227.855152877392));
#207139=CARTESIAN_POINT('Ctrl Pts',(51.3327688896871,38.8223539164361,-227.854997711837));
#207140=CARTESIAN_POINT('Ctrl Pts',(51.3497378512431,38.8058183365427,-227.854921938072));
#207141=CARTESIAN_POINT('Ctrl Pts',(51.3643831288794,38.7913345616423,-227.854899769182));
#207142=CARTESIAN_POINT('Ctrl Pts',(51.3676380035395,38.788115580543,-227.854894842204));
#207143=CARTESIAN_POINT('Ctrl Pts',(51.370777973267,38.7849977994569,-227.854892502014));
#207144=CARTESIAN_POINT('Ctrl Pts',(51.3738041885888,38.7819825040676,-227.854892383582));
#207145=CARTESIAN_POINT('Ctrl Pts',(51.3738047928673,38.7819819019696,-227.854892383558));
#207146=CARTESIAN_POINT('Ctrl Pts',(51.37380539715,38.7819812998671,-227.854892383534));
#207147=CARTESIAN_POINT('Ctrl Pts',(51.3738060014367,38.78198069776,-227.854892383511));
#207148=CARTESIAN_POINT('Ctrl Pts',(51.3873290404909,38.7685064364501,-227.854891858251));
#207149=CARTESIAN_POINT('Ctrl Pts',(51.4029131555694,38.7527647227732,-227.854936775985));
#207150=CARTESIAN_POINT('Ctrl Pts',(51.4204379639646,38.734631047722,-227.855055719537));
#207151=CARTESIAN_POINT('Ctrl Pts',(51.4373488622628,38.7171326119248,-227.855170496387));
#207152=CARTESIAN_POINT('Ctrl Pts',(51.4560669428818,38.6974064333121,-227.855355226822));
#207153=CARTESIAN_POINT('Ctrl Pts',(51.4764468776254,38.6753178021015,-227.855616531962));
#207154=CARTESIAN_POINT('Ctrl Pts',(51.4954944831492,38.6546732053866,-227.855860754393));
#207155=CARTESIAN_POINT('Ctrl Pts',(51.515993657152,38.6319645100545,-227.856172586645));
#207156=CARTESIAN_POINT('Ctrl Pts',(51.5377932005687,38.6070676878515,-227.856528479526));
#207157=CARTESIAN_POINT('Ctrl Pts',(51.5438321409979,38.600170734861,-227.856627069477));
#207158=CARTESIAN_POINT('Ctrl Pts',(51.5499706739712,38.593105796085,-227.856728824965));
#207159=CARTESIAN_POINT('Ctrl Pts',(51.556205114735,38.58587009375,-227.856832699314));
#207160=CARTESIAN_POINT('Ctrl Pts',(51.5791743717403,38.5592119358101,-227.857215398697));
#207161=CARTESIAN_POINT('Ctrl Pts',(51.6000534221824,38.5341766143175,-227.857566058089));
#207162=CARTESIAN_POINT('Ctrl Pts',(51.6189965727127,38.5109146691511,-227.857848834773));
#207163=CARTESIAN_POINT('Ctrl Pts',(51.6388353321281,38.486552927795,-227.858144980791));
#207164=CARTESIAN_POINT('Ctrl Pts',(51.6565512897508,38.4641361492409,-227.858367658238));
#207165=CARTESIAN_POINT('Ctrl Pts',(51.6723014335466,38.4438000309361,-227.858516309415));
#207166=CARTESIAN_POINT('Ctrl Pts',(51.6888025129355,38.4224943268766,-227.858672047985));
#207167=CARTESIAN_POINT('Ctrl Pts',(51.703146422698,38.4034723566256,-227.858747661482));
#207168=CARTESIAN_POINT('Ctrl Pts',(51.7154836737872,38.3868512424513,-227.858769253939));
#207169=CARTESIAN_POINT('Ctrl Pts',(51.7181992444909,38.3831927442666,-227.858774006687));
#207170=CARTESIAN_POINT('Ctrl Pts',(51.7208174652636,38.3796504240554,-227.858776203219));
#207171=CARTESIAN_POINT('Ctrl Pts',(51.7233397168138,38.3762252975093,-227.858776203219));
#207172=CARTESIAN_POINT('',(51.2626335243563,39.5330360887948,-228.35005));
#207173=CARTESIAN_POINT('Origin',(51.2626335243564,39.5330360887949,-227.85005));
#207174=CARTESIAN_POINT('Ctrl Pts',(52.1258919562641,38.6726633987898,-228.35005));
#207175=CARTESIAN_POINT('Ctrl Pts',(52.101394940538,38.7361174509243,-228.35005));
#207176=CARTESIAN_POINT('Ctrl Pts',(52.0737422806294,38.7965600493266,-228.348939269426));
#207177=CARTESIAN_POINT('Ctrl Pts',(52.04303112011,38.8540344509297,-228.347412323243));
#207178=CARTESIAN_POINT('Ctrl Pts',(52.0113965235525,38.9132370169139,-228.345839464202));
#207179=CARTESIAN_POINT('Ctrl Pts',(51.9765167444005,38.9692904956714,-228.343823772569));
#207180=CARTESIAN_POINT('Ctrl Pts',(51.938458912692,39.0222114372786,-228.342098890823));
#207181=CARTESIAN_POINT('Ctrl Pts',(51.9116888594152,39.0594362701891,-228.340885601097));
#207182=CARTESIAN_POINT('Ctrl Pts',(51.8833455488624,39.0951105484446,-228.339815631152));
#207183=CARTESIAN_POINT('Ctrl Pts',(51.8534413111295,39.1292301746532,-228.339142200799));
#207184=CARTESIAN_POINT('Ctrl Pts',(51.8340942469303,39.1513044573889,-228.338706513376));
#207185=CARTESIAN_POINT('Ctrl Pts',(51.8140936482124,39.1727278475187,-228.338436787019));
#207186=CARTESIAN_POINT('Ctrl Pts',(51.7934409172728,39.1934973238057,-228.338402007334));
#207187=CARTESIAN_POINT('Ctrl Pts',(51.7918446266259,39.1951026379326,-228.338399319143));
#207188=CARTESIAN_POINT('Ctrl Pts',(51.7902444453824,39.1967040387988,-228.338398034845));
#207189=CARTESIAN_POINT('Ctrl Pts',(51.7886403549826,39.1983015433779,-228.338398186468));
#207190=CARTESIAN_POINT('Ctrl Pts',(51.724379729213,39.2622983380304,-228.338404260535));
#207191=CARTESIAN_POINT('Ctrl Pts',(51.6539261706324,39.3200860120821,-228.340708253783));
#207192=CARTESIAN_POINT('Ctrl Pts',(51.5772375424492,39.3714801303097,-228.343273660827));
#207193=CARTESIAN_POINT('Ctrl Pts',(51.4964326560892,39.425632825192,-228.345976765962));
#207194=CARTESIAN_POINT('Ctrl Pts',(51.4087052720494,39.4726870394319,-228.348969753843));
#207195=CARTESIAN_POINT('Ctrl Pts',(51.3140209355321,39.512440028451,-228.349816254427));
#207196=CARTESIAN_POINT('Ctrl Pts',(51.2971136329727,39.5195385184199,-228.34996740975));
#207197=CARTESIAN_POINT('Ctrl Pts',(51.2799845442189,39.5264042410929,-228.35005));
#207198=CARTESIAN_POINT('Ctrl Pts',(51.2626335243564,39.5330360887947,-228.35005));
#207199=CARTESIAN_POINT('Origin',(48.892180948596,36.2913696007177,-227.85005));
#207200=CARTESIAN_POINT('Origin',(48.892180948596,36.2913696007177,-228.35005));
#207201=CARTESIAN_POINT('',(48.892180948596,32.7753941674559,-227.858776203219));
#207202=CARTESIAN_POINT('Origin',(48.892180948596,36.2913696007177,-227.858776203219));
#207203=CARTESIAN_POINT('Origin',(48.892180948596,36.2913696007177,-227.858776203219));
#207204=CARTESIAN_POINT('Origin',(48.1334350484927,-61.7961505568785,-227.85005));
#207205=CARTESIAN_POINT('',(48.1334350484927,-57.7802512760377,-228.35005));
#207206=CARTESIAN_POINT('Origin',(48.1334350484927,-61.7961505568785,-228.35005));
#207207=CARTESIAN_POINT('',(48.1334350484927,-58.2801751236159,-227.858776203219));
#207208=CARTESIAN_POINT('Origin',(48.1334350484927,-57.7802512760377,-227.85005));
#207209=CARTESIAN_POINT('',(48.1334350484927,-65.3121259901411,-227.858776203219));
#207210=CARTESIAN_POINT('Origin',(48.1334350484927,-61.7961505568785,-227.858776203219));
#207211=CARTESIAN_POINT('Origin',(48.1334350484927,-61.7961505568785,-227.858776203219));
#207212=CARTESIAN_POINT('Ctrl Pts',(54.2123842387114,-60.9809369188682,
-220.34872120014));
#207213=CARTESIAN_POINT('Ctrl Pts',(53.9849086976504,-60.7491038125482,
-220.006959754302));
#207214=CARTESIAN_POINT('Ctrl Pts',(54.3075179287798,-60.4058635314347,
-219.986910060041));
#207215=CARTESIAN_POINT('Ctrl Pts',(54.2905773520916,-61.0606279145824,
-220.207250076519));
#207216=CARTESIAN_POINT('Ctrl Pts',(54.0902539551932,-60.8227589927709,
-219.884871134182));
#207217=CARTESIAN_POINT('Ctrl Pts',(54.4118428785764,-60.5120824447637,
-219.845412347007));
#207218=CARTESIAN_POINT('Ctrl Pts',(54.359483942211,-61.1484321661822,-220.068048613768));
#207219=CARTESIAN_POINT('Ctrl Pts',(54.1883692315684,-60.9105945733191,
-219.759116870628));
#207220=CARTESIAN_POINT('Ctrl Pts',(54.5038491541938,-60.6290451815934,
-219.706184350974));
#207221=CARTESIAN_POINT('Ctrl Pts',(54.4780017311477,-61.3407746536632,
-219.794316977736));
#207222=CARTESIAN_POINT('Ctrl Pts',(54.3601921871582,-61.1113013655168,
-219.509518223974));
#207223=CARTESIAN_POINT('Ctrl Pts',(54.6622597796057,-60.8851359437949,
-219.432400986523));
#207224=CARTESIAN_POINT('Ctrl Pts',(54.527958659632,-61.4464128888113,-219.65854206581));
#207225=CARTESIAN_POINT('Ctrl Pts',(54.4358335264181,-61.2248747082977,
-219.383842189249));
#207226=CARTESIAN_POINT('Ctrl Pts',(54.7291280292789,-61.0257268060029,
-219.29660115324));
#207227=CARTESIAN_POINT('Ctrl Pts',(54.602542940236,-61.6709815877632,-219.399995666978));
#207228=CARTESIAN_POINT('Ctrl Pts',(54.5543689314799,-61.4719546649753,
-219.143398711153));
#207229=CARTESIAN_POINT('Ctrl Pts',(54.8292130354721,-61.324481551372,-219.038012931781));
#207230=CARTESIAN_POINT('Ctrl Pts',(54.6275380455227,-61.7897249373771,
-219.277032330241));
#207231=CARTESIAN_POINT('Ctrl Pts',(54.5990060222776,-61.6050459038175,
-219.027646728975));
#207232=CARTESIAN_POINT('Ctrl Pts',(54.8629184699323,-61.4823979173559,
-218.915032638408));
#207233=CARTESIAN_POINT('Ctrl Pts',(54.647034139304,-62.043025557965,-219.046408327258));
#207234=CARTESIAN_POINT('Ctrl Pts',(54.6493563799739,-61.8922244718436,
-218.810400243037));
#207235=CARTESIAN_POINT('Ctrl Pts',(54.8898067560441,-61.8191471195123,
-218.684386523562));
#207236=CARTESIAN_POINT('Ctrl Pts',(54.641064245613,-62.1766218791842,-218.939992225721));
#207237=CARTESIAN_POINT('Ctrl Pts',(54.6555291975715,-62.0456431176211,
-218.709001772433));
#207238=CARTESIAN_POINT('Ctrl Pts',(54.8823609599701,-61.9966926518151,
-218.577969748941));
#207239=CARTESIAN_POINT('Ctrl Pts',(54.6151554910244,-62.3124799546862,
-218.850050000001));
#207240=CARTESIAN_POINT('Ctrl Pts',(54.6359260398381,-62.2035651560494,
-218.622717457036));
#207241=CARTESIAN_POINT('Ctrl Pts',(54.848380895554,-62.1772035872432,-218.488025452359));
#207242=CARTESIAN_POINT('',(54.8483808955536,-62.1772035872456,-218.488025452358));
#207243=CARTESIAN_POINT('',(54.615155491024,-62.3124799546881,-218.85005));
#207244=CARTESIAN_POINT('Origin',(55.1063041457817,-62.4061442430845,-218.85005));
#207245=CARTESIAN_POINT('',(54.2123842387114,-60.9809369188682,-220.34872120014));
#207246=CARTESIAN_POINT('Ctrl Pts',(54.2123842387114,-60.9809369188682,
-220.34872120014));
#207247=CARTESIAN_POINT('Ctrl Pts',(54.2537240469357,-61.0230686404178,
-220.273927028716));
#207248=CARTESIAN_POINT('Ctrl Pts',(54.2896597958659,-61.0646008231263,
-220.204851872225));
#207249=CARTESIAN_POINT('Ctrl Pts',(54.3210095713433,-61.1044816969448,
-220.141567685847));
#207250=CARTESIAN_POINT('Ctrl Pts',(54.3238457271854,-61.1080896453766,
-220.135842483284));
#207251=CARTESIAN_POINT('Ctrl Pts',(54.3266443240743,-61.1116841049447,
-220.130164684514));
#207252=CARTESIAN_POINT('Ctrl Pts',(54.3294059505124,-61.115264314403,-220.124534347917));
#207253=CARTESIAN_POINT('Ctrl Pts',(54.3510792439722,-61.1433618619816,
-220.080347366046));
#207254=CARTESIAN_POINT('Ctrl Pts',(54.370479895722,-61.1705828148596,-220.039078356947));
#207255=CARTESIAN_POINT('Ctrl Pts',(54.3879023892055,-61.1966031534464,
-220.00071034299));
#207256=CARTESIAN_POINT('Ctrl Pts',(54.3955663297739,-61.2080491803131,
-219.983832725617));
#207257=CARTESIAN_POINT('Ctrl Pts',(54.4028473735161,-61.2192634874255,
-219.967516092357));
#207258=CARTESIAN_POINT('Ctrl Pts',(54.4097697233646,-61.2302215008038,
-219.951757419607));
#207259=CARTESIAN_POINT('Ctrl Pts',(54.4111288373526,-61.2323729652038,
-219.948663407742));
#207260=CARTESIAN_POINT('Ctrl Pts',(54.4120182448729,-61.2337858808344,
-219.946634534833));
#207261=CARTESIAN_POINT('Ctrl Pts',(54.4136687028363,-61.2364267554626,
-219.942853784503));
#207262=CARTESIAN_POINT('Ctrl Pts',(54.4138526602173,-61.2367211030867,
-219.942432388173));
#207263=CARTESIAN_POINT('Ctrl Pts',(54.4140460332135,-61.2370307393494,
-219.941989237738));
#207264=CARTESIAN_POINT('Ctrl Pts',(54.4142504910173,-61.2373584174968,
-219.9415204411));
#207265=CARTESIAN_POINT('Ctrl Pts',(54.4157577062355,-61.2397739843335,
-219.938064581681));
#207266=CARTESIAN_POINT('Ctrl Pts',(54.4172550982855,-61.2421889601547,
-219.934618672845));
#207267=CARTESIAN_POINT('Ctrl Pts',(54.4187427686362,-61.2446032994954,
-219.931182653013));
#207268=CARTESIAN_POINT('Ctrl Pts',(54.4361365177009,-61.2728316046632,
-219.891008923185));
#207269=CARTESIAN_POINT('Ctrl Pts',(54.4522303236627,-61.3010643287227,
-219.852083180668));
#207270=CARTESIAN_POINT('Ctrl Pts',(54.4671094261737,-61.3291558492811,
-219.814439928106));
#207271=CARTESIAN_POINT('Ctrl Pts',(54.4785012271342,-61.3506633972424,
-219.785619342968));
#207272=CARTESIAN_POINT('Ctrl Pts',(54.4891812458271,-61.3720890889861,
-219.757549559389));
#207273=CARTESIAN_POINT('Ctrl Pts',(54.4991903161083,-61.3933821403281,
-219.730231992184));
#207274=CARTESIAN_POINT('Ctrl Pts',(54.5158763994284,-61.4288797059211,
-219.684690978917));
#207275=CARTESIAN_POINT('Ctrl Pts',(54.5307001536245,-61.4640120265341,
-219.641236079515));
#207276=CARTESIAN_POINT('Ctrl Pts',(54.5438437305745,-61.4985738453453,
-219.599859124708));
#207277=CARTESIAN_POINT('Ctrl Pts',(54.5449970207671,-61.5016064906308,
-219.596228481667));
#207278=CARTESIAN_POINT('Ctrl Pts',(54.5461373724362,-61.5046347625141,
-219.592613825135));
#207279=CARTESIAN_POINT('Ctrl Pts',(54.5472649091519,-61.5076585370498,
-219.589015137637));
#207280=CARTESIAN_POINT('Ctrl Pts',(54.5495945111213,-61.5139059532228,
-219.581579894628));
#207281=CARTESIAN_POINT('Ctrl Pts',(54.5518694025075,-61.5201341524938,
-219.574212841306));
#207282=CARTESIAN_POINT('Ctrl Pts',(54.554090649916,-61.5263419968953,-219.566913836884));
#207283=CARTESIAN_POINT('Ctrl Pts',(54.5555526235454,-61.5304278563884,
-219.562109801122));
#207284=CARTESIAN_POINT('Ctrl Pts',(54.5567753187678,-61.5338904711071,
-219.558053827738));
#207285=CARTESIAN_POINT('Ctrl Pts',(54.5581873646019,-61.5379417398871,
-219.553326108062));
#207286=CARTESIAN_POINT('Ctrl Pts',(54.5589207084565,-61.5400457601614,
-219.550870774044));
#207287=CARTESIAN_POINT('Ctrl Pts',(54.5597045823261,-61.5423088586908,
-219.548234516646));
#207288=CARTESIAN_POINT('Ctrl Pts',(54.5605944954227,-61.5449032557025,
-219.545220712212));
#207289=CARTESIAN_POINT('Ctrl Pts',(54.5621719558726,-61.549502085288,-219.539878440797));
#207290=CARTESIAN_POINT('Ctrl Pts',(54.5637240141203,-61.5541001818136,
-219.534560962645));
#207291=CARTESIAN_POINT('Ctrl Pts',(54.5652507364924,-61.5586970472681,
-219.529268620771));
#207292=CARTESIAN_POINT('Ctrl Pts',(54.5780112412408,-61.5971181279658,
-219.485034675651));
#207293=CARTESIAN_POINT('Ctrl Pts',(54.5890413035181,-61.6354331544369,
-219.442535875386));
#207294=CARTESIAN_POINT('Ctrl Pts',(54.5984153252178,-61.6735157296616,
-219.401798240125));
#207295=CARTESIAN_POINT('Ctrl Pts',(54.6027277343643,-61.6910351733947,
-219.383057367046));
#207296=CARTESIAN_POINT('Ctrl Pts',(54.6066902752954,-61.7085051178258,
-219.364688932253));
#207297=CARTESIAN_POINT('Ctrl Pts',(54.6103132286145,-61.7259117389287,
-219.346694043013));
#207298=CARTESIAN_POINT('Ctrl Pts',(54.6183417653991,-61.7644851583222,
-219.306817009699));
#207299=CARTESIAN_POINT('Ctrl Pts',(54.6246998913435,-61.8027476831842,
-219.268776760042));
#207300=CARTESIAN_POINT('Ctrl Pts',(54.6295318825711,-61.8405436932965,
-219.232560832877));
#207301=CARTESIAN_POINT('Ctrl Pts',(54.6312513254441,-61.8539932376264,
-219.21967355413));
#207302=CARTESIAN_POINT('Ctrl Pts',(54.6327779097984,-61.8673837179251,
-219.20701693033));
#207303=CARTESIAN_POINT('Ctrl Pts',(54.6341193240819,-61.8807082423834,
-219.194589255187));
#207304=CARTESIAN_POINT('Ctrl Pts',(54.6345726244288,-61.8852109613671,
-219.190389605964));
#207305=CARTESIAN_POINT('Ctrl Pts',(54.6349450981342,-61.8890796851728,
-219.186797222501));
#207306=CARTESIAN_POINT('Ctrl Pts',(54.6353505020694,-61.8934796155092,
-219.182728343179));
#207307=CARTESIAN_POINT('Ctrl Pts',(54.6355981015012,-61.8961668618742,
-219.180243285387));
#207308=CARTESIAN_POINT('Ctrl Pts',(54.6358573830125,-61.8990525672118,
-219.177580791167));
#207309=CARTESIAN_POINT('Ctrl Pts',(54.6361464827514,-61.9024062219641,
-219.174497870032));
#207310=CARTESIAN_POINT('Ctrl Pts',(54.6365480120771,-61.9070640979499,
-219.170216014747));
#207311=CARTESIAN_POINT('Ctrl Pts',(54.6369277824627,-61.9117200028051,
-219.1659562532));
#207312=CARTESIAN_POINT('Ctrl Pts',(54.6372859911519,-61.9163739319722,
-219.161718390579));
#207313=CARTESIAN_POINT('Ctrl Pts',(54.6402489447282,-61.9548693020932,
-219.126664550208));
#207314=CARTESIAN_POINT('Ctrl Pts',(54.6416927844994,-61.9931370662252,
-219.093227206538));
#207315=CARTESIAN_POINT('Ctrl Pts',(54.6417016572482,-62.0310368381492,
-219.061436133771));
#207316=CARTESIAN_POINT('Ctrl Pts',(54.6417109462764,-62.0707147391475,
-219.028153531427));
#207317=CARTESIAN_POINT('Ctrl Pts',(54.6401477866251,-62.1099895493046,
-218.996674810712));
#207318=CARTESIAN_POINT('Ctrl Pts',(54.6371107038755,-62.1487460190625,
-218.966996442013));
#207319=CARTESIAN_POINT('Ctrl Pts',(54.6338463359794,-62.1904028937909,
-218.935097043157));
#207320=CARTESIAN_POINT('Ctrl Pts',(54.6288796078067,-62.231461062838,-218.905277062178));
#207321=CARTESIAN_POINT('Ctrl Pts',(54.6223290653762,-62.2718265419444,
-218.87749714131));
#207322=CARTESIAN_POINT('Ctrl Pts',(54.6201170830798,-62.2854571269101,
-218.868116438291));
#207323=CARTESIAN_POINT('Ctrl Pts',(54.6177244432035,-62.2990091065251,
-218.858968114652));
#207324=CARTESIAN_POINT('Ctrl Pts',(54.6151554910244,-62.3124799546862,
-218.850050000001));
#207325=CARTESIAN_POINT('',(54.3075179287798,-60.4058635314347,-219.986910060041));
#207326=CARTESIAN_POINT('Origin',(54.5692758093764,-60.630753528645,-220.34872120014));
#207327=CARTESIAN_POINT('Ctrl Pts',(54.848380895554,-62.1772035872432,-218.488025452359));
#207328=CARTESIAN_POINT('Ctrl Pts',(54.8595780951736,-62.1177211521084,
-218.517664132001));
#207329=CARTESIAN_POINT('Ctrl Pts',(54.8678564354363,-62.0587810759542,
-218.548979038982));
#207330=CARTESIAN_POINT('Ctrl Pts',(54.8734777099421,-62.0004951204819,
-218.581727253286));
#207331=CARTESIAN_POINT('Ctrl Pts',(54.8794967639772,-61.9380846626563,
-218.616792836944));
#207332=CARTESIAN_POINT('Ctrl Pts',(54.8824693653225,-61.8764235092185,
-218.653502177699));
#207333=CARTESIAN_POINT('Ctrl Pts',(54.8826645527079,-61.8156518061647,
-218.691591283606));
#207334=CARTESIAN_POINT('Ctrl Pts',(54.8828436018189,-61.7599047640072,
-218.726531146832));
#207335=CARTESIAN_POINT('Ctrl Pts',(54.8806845561729,-61.7049057977467,
-218.762632937219));
#207336=CARTESIAN_POINT('Ctrl Pts',(54.8763620068724,-61.6507727587228,
-218.799709864555));
#207337=CARTESIAN_POINT('Ctrl Pts',(54.8763424593426,-61.6505279570742,
-218.799877534671));
#207338=CARTESIAN_POINT('Ctrl Pts',(54.8763228688496,-61.6502831758785,
-218.800045222107));
#207339=CARTESIAN_POINT('Ctrl Pts',(54.8763032354031,-61.6500384151223,
-218.800212926867));
#207340=CARTESIAN_POINT('Ctrl Pts',(54.8628119724682,-61.4818493143656,
-218.915452449409));
#207341=CARTESIAN_POINT('Ctrl Pts',(54.8291146403181,-61.3241894585149,
-219.038266143607));
#207342=CARTESIAN_POINT('Ctrl Pts',(54.7791703042592,-61.175104320049,-219.167307118481));
#207343=CARTESIAN_POINT('Ctrl Pts',(54.7790856375891,-61.174851587843,-219.167525871407));
#207344=CARTESIAN_POINT('Ctrl Pts',(54.7790009228209,-61.1745988809922,
-219.167744642781));
#207345=CARTESIAN_POINT('Ctrl Pts',(54.7789161599765,-61.1743461995148,
-219.167963432577));
#207346=CARTESIAN_POINT('Ctrl Pts',(54.7321821205352,-61.0350301322992,
-219.288593303123));
#207347=CARTESIAN_POINT('Ctrl Pts',(54.6708383586244,-60.9034276348827,
-219.414819509759));
#207348=CARTESIAN_POINT('Ctrl Pts',(54.5985281980209,-60.7825291610854,
-219.542285535957));
#207349=CARTESIAN_POINT('Ctrl Pts',(54.5934244554191,-60.7739959938782,
-219.55128224932));
#207350=CARTESIAN_POINT('Ctrl Pts',(54.58826606349,-60.7655161570842,-219.560285148006));
#207351=CARTESIAN_POINT('Ctrl Pts',(54.5830542956885,-60.757090705388,-219.569292703597));
#207352=CARTESIAN_POINT('Ctrl Pts',(54.5829701683847,-60.7569547034476,
-219.569438101741));
#207353=CARTESIAN_POINT('Ctrl Pts',(54.5828860266501,-60.7568187140274,
-219.569583502503));
#207354=CARTESIAN_POINT('Ctrl Pts',(54.5828018704853,-60.7566827371269,
-219.569728905881));
#207355=CARTESIAN_POINT('Ctrl Pts',(54.5036381576416,-60.6287724845599,
-219.706506423312));
#207356=CARTESIAN_POINT('Ctrl Pts',(54.4117181269148,-60.5119554283026,
-219.845581549818));
#207357=CARTESIAN_POINT('Ctrl Pts',(54.3075179287798,-60.4058635314347,
-219.986910060041));
#207358=CARTESIAN_POINT('Ctrl Pts',(54.3075179287798,-60.4058635314347,
-219.986910060041));
#207359=CARTESIAN_POINT('Ctrl Pts',(53.9849086976503,-60.7491038125481,
-220.006959754301));
#207360=CARTESIAN_POINT('Ctrl Pts',(54.2123842387114,-60.9809369188682,
-220.34872120014));
#207361=CARTESIAN_POINT('Ctrl Pts',(52.5270340116508,-58.593055911284,-222.401810820094));
#207362=CARTESIAN_POINT('Ctrl Pts',(52.2079291156962,-58.9380840675622,
-222.419842682816));
#207363=CARTESIAN_POINT('Ctrl Pts',(52.433041068884,-59.1675083087135,-222.763182656182));
#207364=CARTESIAN_POINT('Ctrl Pts',(50.7503363279055,-56.7819842883116,
-224.820210504335));
#207365=CARTESIAN_POINT('Ctrl Pts',(50.428037288823,-57.124096290766,-224.842059161051));
#207366=CARTESIAN_POINT('Ctrl Pts',(50.6562579911382,-57.3566888322572,
-225.181485677498));
#207367=CARTESIAN_POINT('Ctrl Pts',(48.9740484537045,-54.9709070690089,
-227.238815650979));
#207368=CARTESIAN_POINT('Ctrl Pts',(48.6520074870279,-55.3140445196239,
-227.259140997287));
#207369=CARTESIAN_POINT('Ctrl Pts',(48.8796513269547,-55.5460491487752,
-227.60005));
#207370=CARTESIAN_POINT('',(48.8796513269546,-55.5460491487752,-227.60005));
#207371=CARTESIAN_POINT('',(48.9740484537045,-54.9709070690089,-227.238815650979));
#207372=CARTESIAN_POINT('Origin',(49.2365428976196,-55.195865758552,-227.60005));
#207373=CARTESIAN_POINT('Ctrl Pts',(54.3075179287798,-60.4058635314347,
-219.986910060041));
#207374=CARTESIAN_POINT('Ctrl Pts',(53.8875633330448,-59.9782848917578,
-220.556501654024));
#207375=CARTESIAN_POINT('Ctrl Pts',(53.4552664659625,-59.5380214346079,
-221.143316453006));
#207376=CARTESIAN_POINT('Ctrl Pts',(53.0105815049601,-59.0850311267164,
-221.747382788392));
#207377=CARTESIAN_POINT('Ctrl Pts',(52.6770677842083,-58.7452883957977,
-222.200432539931));
#207378=CARTESIAN_POINT('Ctrl Pts',(52.3365853899896,-58.3983865617056,
-222.663186174999));
#207379=CARTESIAN_POINT('Ctrl Pts',(51.9891084328353,-58.044304097751,-223.135650875041));
#207380=CARTESIAN_POINT('Ctrl Pts',(51.9239565033689,-57.9779136357595,
-223.224238006299));
#207381=CARTESIAN_POINT('Ctrl Pts',(51.8585586551558,-57.9112707208977,
-223.313166528186));
#207382=CARTESIAN_POINT('Ctrl Pts',(51.7929146954598,-57.8443751995069,
-223.402436467273));
#207383=CARTESIAN_POINT('Ctrl Pts',(51.7621440893522,-57.8130179238549,
-223.44428175122));
#207384=CARTESIAN_POINT('Ctrl Pts',(51.731319405913,-57.7816051437855,-223.486202053495));
#207385=CARTESIAN_POINT('Ctrl Pts',(51.7004406247366,-57.7501368431761,
-223.528197376319));
#207386=CARTESIAN_POINT('Ctrl Pts',(51.6929621699204,-57.7425156141222,
-223.538368118565));
#207387=CARTESIAN_POINT('Ctrl Pts',(51.6854805420115,-57.7348911285222,
-223.548543261124));
#207388=CARTESIAN_POINT('Ctrl Pts',(51.6779957407168,-57.7272633861453,
-223.558722804025));
#207389=CARTESIAN_POINT('Ctrl Pts',(51.6741238780136,-57.7233175804979,
-223.563988647557));
#207390=CARTESIAN_POINT('Ctrl Pts',(51.6702511661257,-57.7193709033506,
-223.569255668603));
#207391=CARTESIAN_POINT('Ctrl Pts',(51.6663776050122,-57.7154233546713,
-223.574523867165));
#207392=CARTESIAN_POINT('Ctrl Pts',(51.6653057221808,-57.7143309981726,
-223.575981670831));
#207393=CARTESIAN_POINT('Ctrl Pts',(51.664233774322,-57.7132385749384,-223.577439564662));
#207394=CARTESIAN_POINT('Ctrl Pts',(51.6631617614348,-57.712146084968,-223.57889754866));
#207395=CARTESIAN_POINT('Ctrl Pts',(51.6625551133699,-57.7115278489986,
-223.579722616325));
#207396=CARTESIAN_POINT('Ctrl Pts',(51.6619484444804,-57.7109095916577,
-223.580547712866));
#207397=CARTESIAN_POINT('Ctrl Pts',(51.6613417547661,-57.7102913129452,
-223.581372838281));
#207398=CARTESIAN_POINT('Ctrl Pts',(51.660743488977,-57.7096816190717,-223.582186506777));
#207399=CARTESIAN_POINT('Ctrl Pts',(51.6601403769267,-57.7090669862187,
-223.583006766944));
#207400=CARTESIAN_POINT('Ctrl Pts',(51.6595329670214,-57.7084479732613,
-223.58383287295));
#207401=CARTESIAN_POINT('Ctrl Pts',(51.6557850761697,-57.704628488298,-223.588930180572));
#207402=CARTESIAN_POINT('Ctrl Pts',(51.6518829388499,-57.7006518043736,
-223.594237292841));
#207403=CARTESIAN_POINT('Ctrl Pts',(51.6481312278776,-57.6968284147854,
-223.599339838672));
#207404=CARTESIAN_POINT('Ctrl Pts',(51.646262699952,-57.6949241875491,-223.601881145677));
#207405=CARTESIAN_POINT('Ctrl Pts',(51.6444314852871,-57.693057985038,-223.604371709749));
#207406=CARTESIAN_POINT('Ctrl Pts',(51.6426752228762,-57.6912681656368,
-223.606760338636));
#207407=CARTESIAN_POINT('Ctrl Pts',(51.6416597675426,-57.6902333079493,
-223.608141422652));
#207408=CARTESIAN_POINT('Ctrl Pts',(51.6406693691138,-57.6892239855127,
-223.609488429222));
#207409=CARTESIAN_POINT('Ctrl Pts',(51.6397113028646,-57.6882476126825,
-223.610791463244));
#207410=CARTESIAN_POINT('Ctrl Pts',(51.6393123131538,-57.6878409991384,
-223.611334115872));
#207411=CARTESIAN_POINT('Ctrl Pts',(51.6389191572805,-57.6874403308405,
-223.611868834326));
#207412=CARTESIAN_POINT('Ctrl Pts',(51.6385241006106,-57.6870377253632,
-223.612406138221));
#207413=CARTESIAN_POINT('Ctrl Pts',(51.1416290490366,-57.1806479219664,
-224.2882171474));
#207414=CARTESIAN_POINT('Ctrl Pts',(50.6267656464817,-56.6558456527314,
-224.988840225086));
#207415=CARTESIAN_POINT('Ctrl Pts',(50.0938544585926,-56.1125730789731,
-225.714254827363));
#207416=CARTESIAN_POINT('Ctrl Pts',(49.7290551815088,-55.7406810138965,
-226.210830482952));
#207417=CARTESIAN_POINT('Ctrl Pts',(49.3557981786686,-55.3601335228959,
-226.719022737376));
#207418=CARTESIAN_POINT('Ctrl Pts',(48.9740484537045,-54.9709070690089,
-227.238815650979));
#207419=CARTESIAN_POINT('Ctrl Pts',(48.8796513269547,-55.5460491487752,
-227.60005));
#207420=CARTESIAN_POINT('Ctrl Pts',(50.6562583519279,-57.3566891999582,
-225.181485185797));
#207421=CARTESIAN_POINT('Ctrl Pts',(52.4330406746144,-59.1675079068912,
-222.763183190988));
#207422=CARTESIAN_POINT('Ctrl Pts',(54.2123842387114,-60.9809369188682,
-220.34872120014));
#207423=CARTESIAN_POINT('Origin',(55.1063041457817,-62.4061442430845,-218.85005));
#207424=CARTESIAN_POINT('',(55.1063041458243,-62.4061442430364,-218.35005));
#207425=CARTESIAN_POINT('Origin',(55.1063041458054,-62.4061442430575,-218.85005));
#207426=CARTESIAN_POINT('Origin',(55.1063041457932,-62.4061442430715,-218.85005));
#207427=CARTESIAN_POINT('Ctrl Pts',(47.4613130320155,-55.2424342950265,
-228.348304885641));
#207428=CARTESIAN_POINT('Ctrl Pts',(47.3021046372418,-55.1176952304439,
-228.346450927386));
#207429=CARTESIAN_POINT('Ctrl Pts',(47.1811427047561,-55.0343199344272,
-228.485631153611));
#207430=CARTESIAN_POINT('Ctrl Pts',(47.5376722342335,-55.1241814098811,
-228.358006905805));
#207431=CARTESIAN_POINT('Ctrl Pts',(47.406151448781,-54.9745809391036,-228.36408944129));
#207432=CARTESIAN_POINT('Ctrl Pts',(47.3217648821301,-54.8530430703057,
-228.501869875666));
#207433=CARTESIAN_POINT('Ctrl Pts',(47.6631621977863,-55.0560571955665,
-228.326632472374));
#207434=CARTESIAN_POINT('Ctrl Pts',(47.5601436638269,-54.8771403537813,
-228.316192700349));
#207435=CARTESIAN_POINT('Ctrl Pts',(47.5116824699239,-54.7217215905284,
-228.449649225183));
#207436=CARTESIAN_POINT('Ctrl Pts',(47.9275209649132,-55.0225868309807,
-228.21963517134));
#207437=CARTESIAN_POINT('Ctrl Pts',(47.850416577859,-54.802837775062,-228.155623333054));
#207438=CARTESIAN_POINT('Ctrl Pts',(47.8754805878992,-54.5907583268247,
-228.271417688637));
#207439=CARTESIAN_POINT('Ctrl Pts',(48.0593323270884,-55.0436861910913,
-228.152274449338));
#207440=CARTESIAN_POINT('Ctrl Pts',(47.9863428228055,-54.8113544609062,
-228.052661933177));
#207441=CARTESIAN_POINT('Ctrl Pts',(48.0444656792804,-54.5754212470967,
-228.159184370623));
#207442=CARTESIAN_POINT('Ctrl Pts',(48.3135352870045,-55.1294371299156,
-228.006090181985));
#207443=CARTESIAN_POINT('Ctrl Pts',(48.2286493510528,-54.8812191556274,
-227.834617170415));
#207444=CARTESIAN_POINT('Ctrl Pts',(48.3555740327057,-54.6054209473356,
-227.915582350477));
#207445=CARTESIAN_POINT('Ctrl Pts',(48.4368943091309,-55.1940478275634,
-227.92683964474));
#207446=CARTESIAN_POINT('Ctrl Pts',(48.3369447816902,-54.944944352671,-227.716654532444));
#207447=CARTESIAN_POINT('Ctrl Pts',(48.49900012063,-54.6503832012681,-227.783505557683));
#207448=CARTESIAN_POINT('Ctrl Pts',(48.6860658100372,-55.3621740854522,
-227.753484899464));
#207449=CARTESIAN_POINT('Ctrl Pts',(48.5353337959282,-55.1181513278107,
-227.465234070536));
#207450=CARTESIAN_POINT('Ctrl Pts',(48.7763611981979,-54.7909405035185,
-227.49457033784));
#207451=CARTESIAN_POINT('Ctrl Pts',(48.808149438057,-55.468371606431,-227.660133432125));
#207452=CARTESIAN_POINT('Ctrl Pts',(48.6175640550392,-55.2345767175589,
-227.333089928053));
#207453=CARTESIAN_POINT('Ctrl Pts',(48.9044383729524,-54.8912970631231,
-227.33896894949));
#207454=CARTESIAN_POINT('Ctrl Pts',(48.9209614213312,-55.5892183382082,
-227.56593431681));
#207455=CARTESIAN_POINT('Ctrl Pts',(48.6743407164146,-55.3608255688747,
-227.213117273111));
#207456=CARTESIAN_POINT('Ctrl Pts',(49.0153493238984,-55.0140778973635,
-227.181921047664));
#207457=CARTESIAN_POINT('',(47.4910910659473,-55.2017568268661,-228.35005));
#207458=CARTESIAN_POINT('',(47.2343490658922,-54.9709330687352,-228.488381729218));
#207459=CARTESIAN_POINT('Origin',(47.4910910659474,-55.2017568268662,-228.85005));
#207460=CARTESIAN_POINT('Ctrl Pts',(48.9740484537045,-54.9709070690089,
-227.238815650979));
#207461=CARTESIAN_POINT('Ctrl Pts',(48.9229565323117,-54.9188144908534,
-227.30838274414));
#207462=CARTESIAN_POINT('Ctrl Pts',(48.8416414398881,-54.8479207863561,
-227.411623042946));
#207463=CARTESIAN_POINT('Ctrl Pts',(48.738379705309,-54.7781024203753,-227.530126961583));
#207464=CARTESIAN_POINT('Ctrl Pts',(48.6923014503903,-54.7509634238684,
-227.580497977433));
#207465=CARTESIAN_POINT('Ctrl Pts',(48.6611746664914,-54.7334914992703,
-227.613986126256));
#207466=CARTESIAN_POINT('Ctrl Pts',(48.6464955257704,-54.7256187239374,
-227.629549471375));
#207467=CARTESIAN_POINT('Ctrl Pts',(48.5611906556844,-54.6822841007737,
-227.718479526806));
#207468=CARTESIAN_POINT('Ctrl Pts',(48.4914725151753,-54.6544212751007,
-227.786430965697));
#207469=CARTESIAN_POINT('Ctrl Pts',(48.3845686321144,-54.6228948487552,
-227.883569215853));
#207470=CARTESIAN_POINT('Ctrl Pts',(48.3305350506504,-54.6096981433835,
-227.930941113887));
#207471=CARTESIAN_POINT('Ctrl Pts',(48.2664530938673,-54.5988018476774,
-227.98411318093));
#207472=CARTESIAN_POINT('Ctrl Pts',(48.2387632988875,-54.5950968611026,
-228.006452249522));
#207473=CARTESIAN_POINT('Ctrl Pts',(48.2202528979549,-54.5928413400655,
-228.021245192995));
#207474=CARTESIAN_POINT('Ctrl Pts',(48.212327822807,-54.5919538315903,-228.027529021694));
#207475=CARTESIAN_POINT('Ctrl Pts',(48.1163763146568,-54.582537302858,-228.10276417424));
#207476=CARTESIAN_POINT('Ctrl Pts',(48.0325110079193,-54.5834648765834,
-228.162697419324));
#207477=CARTESIAN_POINT('Ctrl Pts',(47.9088313425645,-54.5986997083007,
-228.242183617849));
#207478=CARTESIAN_POINT('Ctrl Pts',(47.8475214607299,-54.6097772709699,
-228.279323299837));
#207479=CARTESIAN_POINT('Ctrl Pts',(47.7870065001217,-54.6260191079529,
-228.312557855911));
#207480=CARTESIAN_POINT('Ctrl Pts',(47.7468401025145,-54.6379912724447,
-228.333846420869));
#207481=CARTESIAN_POINT('Ctrl Pts',(47.7287456377893,-54.6438689926409,
-228.34312351292));
#207482=CARTESIAN_POINT('Ctrl Pts',(47.6633263561034,-54.6672964949944,
-228.375252805728));
#207483=CARTESIAN_POINT('Ctrl Pts',(47.6206907845702,-54.6856607265798,
-228.394188721727));
#207484=CARTESIAN_POINT('Ctrl Pts',(47.5373966142101,-54.7278310248293,
-228.427093328645));
#207485=CARTESIAN_POINT('Ctrl Pts',(47.4983789032494,-54.7505406095228,
-228.440586801717));
#207486=CARTESIAN_POINT('Ctrl Pts',(47.3744847769716,-54.8333295171273,
-228.476467690392));
#207487=CARTESIAN_POINT('Ctrl Pts',(47.3001594386793,-54.8976848030761,
-228.488412567484));
#207488=CARTESIAN_POINT('Ctrl Pts',(47.2343490658922,-54.9709330687352,
-228.488381729218));
#207489=CARTESIAN_POINT('Ctrl Pts',(47.4910910659473,-55.2017568268661,
-228.35005));
#207490=CARTESIAN_POINT('Ctrl Pts',(47.5339427387703,-55.1499211321669,
-228.35005));
#207491=CARTESIAN_POINT('Ctrl Pts',(47.5881950341781,-55.1087905244168,
-228.341044977978));
#207492=CARTESIAN_POINT('Ctrl Pts',(47.6839946527033,-55.0657816325896,
-228.31377766011));
#207493=CARTESIAN_POINT('Ctrl Pts',(47.7183291272714,-55.054562056961,-228.302405862635));
#207494=CARTESIAN_POINT('Ctrl Pts',(47.7730862638229,-55.0427477414354,
-228.281993305555));
#207495=CARTESIAN_POINT('Ctrl Pts',(47.801278640751,-55.0380943922812,-228.270949402552));
#207496=CARTESIAN_POINT('Ctrl Pts',(47.8355181611567,-55.0349339773232,
-228.256625838884));
#207497=CARTESIAN_POINT('Ctrl Pts',(47.8504731154847,-55.0340735392657,
-228.250182443202));
#207498=CARTESIAN_POINT('Ctrl Pts',(47.8605046077288,-55.0336105743244,
-228.245819553912));
#207499=CARTESIAN_POINT('Ctrl Pts',(47.8671616032058,-55.0333962334904,
-228.242891178549));
#207500=CARTESIAN_POINT('Ctrl Pts',(47.9260892897782,-55.0319989091495,
-228.216792199271));
#207501=CARTESIAN_POINT('Ctrl Pts',(47.9863251637679,-55.0372942416347,
-228.187704506116));
#207502=CARTESIAN_POINT('Ctrl Pts',(48.0825738653862,-55.0563960118545,
-228.137219522214));
#207503=CARTESIAN_POINT('Ctrl Pts',(48.1156375092139,-55.0646247696504,
-228.119253305707));
#207504=CARTESIAN_POINT('Ctrl Pts',(48.1665329703472,-55.0799280610835,
-228.090632666823));
#207505=CARTESIAN_POINT('Ctrl Pts',(48.1923055907121,-55.0883198524848,
-228.075905015572));
#207506=CARTESIAN_POINT('Ctrl Pts',(48.2229038264921,-55.0994431878277,
-228.058005688231));
#207507=CARTESIAN_POINT('Ctrl Pts',(48.2361268097716,-55.1045000334963,
-228.050182680758));
#207508=CARTESIAN_POINT('Ctrl Pts',(48.244965992782,-55.1079360956767,-228.044933803818));
#207509=CARTESIAN_POINT('Ctrl Pts',(48.2506824272076,-55.1102021852281,
-228.041523979641));
#207510=CARTESIAN_POINT('Ctrl Pts',(48.3043736715184,-55.1317487878865,
-228.009406678981));
#207511=CARTESIAN_POINT('Ctrl Pts',(48.3580533109924,-55.1569140229942,
-227.976053422806));
#207512=CARTESIAN_POINT('Ctrl Pts',(48.4422450190772,-55.2030191070475,
-227.921281485012));
#207513=CARTESIAN_POINT('Ctrl Pts',(48.470919305374,-55.2197819670126,-227.902237232472));
#207514=CARTESIAN_POINT('Ctrl Pts',(48.5147023734957,-55.2471592361541,
-227.872519388519));
#207515=CARTESIAN_POINT('Ctrl Pts',(48.5367866985082,-55.2614062320095,
-227.857373013928));
#207516=CARTESIAN_POINT('Ctrl Pts',(48.5628565451969,-55.279036830306,-227.839210184702));
#207517=CARTESIAN_POINT('Ctrl Pts',(48.5740911026579,-55.286812519136,-227.83132216892));
#207518=CARTESIAN_POINT('Ctrl Pts',(48.5815941382064,-55.2920455257207,
-227.826040568224));
#207519=CARTESIAN_POINT('Ctrl Pts',(48.586626808195,-55.2955891551262,-227.822486557596));
#207520=CARTESIAN_POINT('Ctrl Pts',(48.668802202713,-55.3537811062054,-227.764344353453));
#207521=CARTESIAN_POINT('Ctrl Pts',(48.7690559004533,-55.4333351349916,
-227.690384734712));
#207522=CARTESIAN_POINT('Ctrl Pts',(48.8796513269546,-55.5460491487752,
-227.60005));
#207523=CARTESIAN_POINT('Origin',(53.1417095267163,-62.031487089538,-218.85005));
#207524=CARTESIAN_POINT('',(54.6082148364463,-63.3913996516292,-218.35005));
#207525=CARTESIAN_POINT('',(54.2415885090138,-63.0514215111064,-218.85005));
#207526=CARTESIAN_POINT('Origin',(54.6082148364463,-63.3913996516292,-218.85005));
#207527=CARTESIAN_POINT('Origin',(53.1417095267163,-62.031487089538,-218.85005));
#207528=CARTESIAN_POINT('Origin',(53.1417095267163,-62.031487089538,-218.35005));
#207529=CARTESIAN_POINT('Ctrl Pts',(47.2343490658922,-54.9709330687353,
-228.488381729218));
#207530=CARTESIAN_POINT('Ctrl Pts',(47.3421114593162,-55.0678167910323,
-228.35005));
#207531=CARTESIAN_POINT('Ctrl Pts',(47.4910910659474,-55.2017568268662,
-228.35005));
#207532=CARTESIAN_POINT('Ctrl Pts',(46.3105395613661,-55.9991515869664,
-228.487948838892));
#207533=CARTESIAN_POINT('Ctrl Pts',(46.4160092042075,-56.0984512122452,
-228.350050000212));
#207534=CARTESIAN_POINT('Ctrl Pts',(46.5610878289829,-56.2361862677858,
-228.35005));
#207535=CARTESIAN_POINT('Ctrl Pts',(45.350506384691,-56.9893433179289,-228.48772415168));
#207536=CARTESIAN_POINT('Ctrl Pts',(45.4531166269507,-57.091545569762,-228.350050000038));
#207537=CARTESIAN_POINT('Ctrl Pts',(45.5947854895852,-57.2325158021754,
-228.35005));
#207538=CARTESIAN_POINT('Ctrl Pts',(43.3550620161755,-58.8891661040005,
-228.487824007409));
#207539=CARTESIAN_POINT('Ctrl Pts',(43.4520711334389,-58.9967304277239,
-228.350049999962));
#207540=CARTESIAN_POINT('Ctrl Pts',(43.5860475125547,-59.145141081541,-228.35005));
#207541=CARTESIAN_POINT('Ctrl Pts',(42.3185849747264,-59.7984761650306,
-228.488134585451));
#207542=CARTESIAN_POINT('Ctrl Pts',(42.4124726432155,-59.9088386926303,
-228.35005000027));
#207543=CARTESIAN_POINT('Ctrl Pts',(42.5429028274419,-60.0607223439083,
-228.35005));
#207544=CARTESIAN_POINT('Ctrl Pts',(41.2456587371609,-60.6702615191614,
-228.488620962447));
#207545=CARTESIAN_POINT('Ctrl Pts',(41.3371131727634,-60.7827319875555,
-228.35005));
#207546=CARTESIAN_POINT('Ctrl Pts',(41.4636310035132,-60.9383233439605,
-228.35005));
#207547=CARTESIAN_POINT('',(41.4636310035131,-60.9383233439604,-228.35005));
#207548=CARTESIAN_POINT('',(41.2456587371609,-60.6702615191614,-228.488620962447));
#207549=CARTESIAN_POINT('Origin',(41.4636310035131,-60.9383233439605,-228.85005));
#207550=CARTESIAN_POINT('Ctrl Pts',(47.2343490658922,-54.9709330687353,
-228.488381729218));
#207551=CARTESIAN_POINT('Ctrl Pts',(46.9328032818251,-55.3065595781188,
-228.48824042704));
#207552=CARTESIAN_POINT('Ctrl Pts',(46.6244555698817,-55.6414031174716,
-228.488119930198));
#207553=CARTESIAN_POINT('Ctrl Pts',(46.3094873419398,-55.9746757314993,
-228.48802406009));
#207554=CARTESIAN_POINT('Ctrl Pts',(46.0030015393239,-56.2989729638508,
-228.487930771864));
#207555=CARTESIAN_POINT('Ctrl Pts',(45.6902469778881,-56.6217826575224,
-228.48786080601));
#207556=CARTESIAN_POINT('Ctrl Pts',(45.3714253331597,-56.9424129887812,
-228.487817653494));
#207557=CARTESIAN_POINT('Ctrl Pts',(45.0526036884314,-57.2630433200401,
-228.487774500978));
#207558=CARTESIAN_POINT('Ctrl Pts',(44.7277147844279,-57.5814940621824,
-228.487758166213));
#207559=CARTESIAN_POINT('Ctrl Pts',(44.3969971042378,-57.8971105887381,
-228.487772045555));
#207560=CARTESIAN_POINT('Ctrl Pts',(44.3822709262308,-57.9111643434371,
-228.487772663573));
#207561=CARTESIAN_POINT('Ctrl Pts',(44.3675332810124,-57.9252124055014,
-228.487773341473));
#207562=CARTESIAN_POINT('Ctrl Pts',(44.3527842004334,-57.9392547109648,
-228.487774079544));
#207563=CARTESIAN_POINT('Ctrl Pts',(44.0592830129135,-58.2186913380103,
-228.487788766885));
#207564=CARTESIAN_POINT('Ctrl Pts',(43.7611582389086,-58.4958173950288,
-228.487826099836));
#207565=CARTESIAN_POINT('Ctrl Pts',(43.458773346099,-58.7702839246494,-228.487884322887));
#207566=CARTESIAN_POINT('Ctrl Pts',(43.1544170933402,-59.0465398039921,
-228.487942925516));
#207567=CARTESIAN_POINT('Ctrl Pts',(42.8457450210993,-59.3201014229422,
-228.488022688327));
#207568=CARTESIAN_POINT('Ctrl Pts',(42.5331641521048,-59.5906515496429,
-228.488121528093));
#207569=CARTESIAN_POINT('Ctrl Pts',(42.2168635114787,-59.8644212741694,
-228.48822154407));
#207570=CARTESIAN_POINT('Ctrl Pts',(41.8965605056513,-60.1351074534593,
-228.488341090339));
#207571=CARTESIAN_POINT('Ctrl Pts',(41.5727137355554,-60.4024200399638,
-228.488477758894));
#207572=CARTESIAN_POINT('Ctrl Pts',(41.464087735809,-60.4920831140937,-228.488523600816));
#207573=CARTESIAN_POINT('Ctrl Pts',(41.3550633321572,-60.5813669426097,
-228.488571367329));
#207574=CARTESIAN_POINT('Ctrl Pts',(41.2456587371609,-60.6702615191614,
-228.488620962447));
#207575=CARTESIAN_POINT('Ctrl Pts',(41.4636310035131,-60.9383233439604,
-228.35005));
#207576=CARTESIAN_POINT('Ctrl Pts',(42.5429085052274,-60.0607177270638,
-228.35005));
#207577=CARTESIAN_POINT('Ctrl Pts',(43.5860475125577,-59.1451410815382,
-228.35005));
#207578=CARTESIAN_POINT('Ctrl Pts',(44.5904165010271,-58.1888284418133,
-228.35005));
#207579=CARTESIAN_POINT('Ctrl Pts',(45.5947854894966,-57.2325158020884,
-228.35005));
#207580=CARTESIAN_POINT('Ctrl Pts',(46.5610786115705,-56.2361965201832,
-228.35005));
#207581=CARTESIAN_POINT('Ctrl Pts',(47.4910910659473,-55.2017568268661,
-228.35005));
#207582=CARTESIAN_POINT('Origin',(0.127542579976414,-12.8706479699377,-218.85005));
#207583=CARTESIAN_POINT('',(49.6055526500885,-68.3000311480131,-218.35005));
#207584=CARTESIAN_POINT('',(49.2725916132775,-67.9270204940557,-218.85005));
#207585=CARTESIAN_POINT('Origin',(49.6055526500885,-68.3000311480131,-218.85005));
#207586=CARTESIAN_POINT('Origin',(0.127542579976414,-12.8706479699377,-218.85005));
#207587=CARTESIAN_POINT('Origin',(0.127542579976414,-12.8706479699377,-218.35005));
#207588=CARTESIAN_POINT('Ctrl Pts',(41.8829757794224,-62.4277604346488,
-227.501386391297));
#207589=CARTESIAN_POINT('Ctrl Pts',(41.6736215736677,-62.1444346782205,
-227.135070658787));
#207590=CARTESIAN_POINT('Ctrl Pts',(41.3169485390188,-62.5017525488842,
-227.074161006169));
#207591=CARTESIAN_POINT('Ctrl Pts',(41.7287883985619,-62.2910497761554,
-227.617062287714));
#207592=CARTESIAN_POINT('Ctrl Pts',(41.5115567796579,-62.083269453487,-227.276647215301));
#207593=CARTESIAN_POINT('Ctrl Pts',(41.1560049633125,-62.3716221357762,
-227.267023357385));
#207594=CARTESIAN_POINT('Ctrl Pts',(41.5970941915982,-62.142277885216,-227.731465467726));
#207595=CARTESIAN_POINT('Ctrl Pts',(41.3631012191682,-61.9849776212493,
-227.438037521325));
#207596=CARTESIAN_POINT('Ctrl Pts',(41.029038944944,-62.2181773292512,-227.457737962389));
#207597=CARTESIAN_POINT('Ctrl Pts',(41.4165235670895,-61.863351898693,-227.924583312038));
#207598=CARTESIAN_POINT('Ctrl Pts',(41.1742388084123,-61.7588443268157,
-227.719355887922));
#207599=CARTESIAN_POINT('Ctrl Pts',(40.8795052413903,-61.9086867290362,
-227.779669319348));
#207600=CARTESIAN_POINT('Ctrl Pts',(41.3544951862324,-61.7387982044088,
-228.004831636089));
#207601=CARTESIAN_POINT('Ctrl Pts',(41.1128065542583,-61.64889903365,-227.838230834733));
#207602=CARTESIAN_POINT('Ctrl Pts',(40.83755717967,-61.7643747830512,-227.9134383294));
#207603=CARTESIAN_POINT('Ctrl Pts',(41.2769460700564,-61.4864549806276,
-228.15152387739));
#207604=CARTESIAN_POINT('Ctrl Pts',(41.0509213652705,-61.4074771774304,
-228.055852077472));
#207605=CARTESIAN_POINT('Ctrl Pts',(40.8167874720303,-61.4561982274081,
-228.157939415417));
#207606=CARTESIAN_POINT('Ctrl Pts',(41.26069413732,-61.3563209527895,-228.219337533727));
#207607=CARTESIAN_POINT('Ctrl Pts',(41.047419886702,-61.2728349773798,-228.158786517575));
#207608=CARTESIAN_POINT('Ctrl Pts',(40.8377574579081,-61.2894729474476,
-228.270955921442));
#207609=CARTESIAN_POINT('Ctrl Pts',(41.3125718827386,-61.0669017530136,
-228.340235822512));
#207610=CARTESIAN_POINT('Ctrl Pts',(41.1455858541625,-60.9545637033621,
-228.337710180632));
#207611=CARTESIAN_POINT('Ctrl Pts',(41.001859551751,-60.8897708053934,-228.472378638455));
#207612=CARTESIAN_POINT('Ctrl Pts',(41.4201040030741,-60.9266188466363,
-228.370752133428));
#207613=CARTESIAN_POINT('Ctrl Pts',(41.2921211277785,-60.7745213841431,
-228.383736779337));
#207614=CARTESIAN_POINT('Ctrl Pts',(41.1915219835725,-60.6688302795368,
-228.523150593268));
#207615=CARTESIAN_POINT('Ctrl Pts',(41.6001886489201,-60.8718793597729,
-228.335060161219));
#207616=CARTESIAN_POINT('Ctrl Pts',(41.5006043490813,-60.6869018002498,
-228.322259765032));
#207617=CARTESIAN_POINT('Ctrl Pts',(41.4493760764998,-60.5376437416971,
-228.463541011146));
#207618=CARTESIAN_POINT('',(41.7563078823353,-62.3074742642099,-227.60005));
#207619=CARTESIAN_POINT('',(41.1874522920715,-62.3844144545142,-227.238927571877));
#207620=CARTESIAN_POINT('Origin',(41.3994163116703,-62.6576576544332,-227.60005));
#207621=CARTESIAN_POINT('Ctrl Pts',(41.2456587371608,-60.6702615191613,
-228.488620962446));
#207622=CARTESIAN_POINT('Ctrl Pts',(41.2197244417364,-60.6913339308266,
-228.488632715863));
#207623=CARTESIAN_POINT('Ctrl Pts',(41.1947961167656,-60.7134311818696,
-228.48724613514));
#207624=CARTESIAN_POINT('Ctrl Pts',(41.1708632827344,-60.7365186965675,
-228.484495167239));
#207625=CARTESIAN_POINT('Ctrl Pts',(41.1596112218472,-60.7473733291938,
-228.483201795201));
#207626=CARTESIAN_POINT('Ctrl Pts',(41.1485791592349,-60.7584475828374,
-228.481606311605));
#207627=CARTESIAN_POINT('Ctrl Pts',(41.1377675402693,-60.7697403512738,
-228.479709419403));
#207628=CARTESIAN_POINT('Ctrl Pts',(41.1258039235476,-60.7822363848215,
-228.477610409871));
#207629=CARTESIAN_POINT('Ctrl Pts',(41.1139760163711,-60.7951667696545,
-228.475098941214));
#207630=CARTESIAN_POINT('Ctrl Pts',(41.1024394739555,-60.8083607221593,
-228.472208416089));
#207631=CARTESIAN_POINT('Ctrl Pts',(41.0976756225717,-60.8138089775059,
-228.471014814781));
#207632=CARTESIAN_POINT('Ctrl Pts',(41.0929610512213,-60.8193019557174,
-228.469756992603));
#207633=CARTESIAN_POINT('Ctrl Pts',(41.0883049776624,-60.8248267792451,
-228.468439019492));
#207634=CARTESIAN_POINT('Ctrl Pts',(41.0803391715892,-60.8342788792288,
-228.466184175773));
#207635=CARTESIAN_POINT('Ctrl Pts',(41.0725424991094,-60.8438221898664,
-228.463756003074));
#207636=CARTESIAN_POINT('Ctrl Pts',(41.0649629951811,-60.8533924384031,
-228.461173742144));
#207637=CARTESIAN_POINT('Ctrl Pts',(41.0573834912528,-60.8629626869397,
-228.458591481213));
#207638=CARTESIAN_POINT('Ctrl Pts',(41.0500211562498,-60.8725598738205,
-228.45585513266));
#207639=CARTESIAN_POINT('Ctrl Pts',(41.0429240799344,-60.8821197945625,
-228.452984028281));
#207640=CARTESIAN_POINT('Ctrl Pts',(41.0247366592379,-60.9066186575638,
-228.445626352967));
#207641=CARTESIAN_POINT('Ctrl Pts',(41.0076807313764,-60.9315713204337,
-228.437229166001));
#207642=CARTESIAN_POINT('Ctrl Pts',(40.9917410517639,-60.9569680117623,
-228.427810778945));
#207643=CARTESIAN_POINT('Ctrl Pts',(40.9828008708308,-60.9712124019319,
-228.422528233347));
#207644=CARTESIAN_POINT('Ctrl Pts',(40.9742125859198,-60.9855966398325,
-228.41692385506));
#207645=CARTESIAN_POINT('Ctrl Pts',(40.965979388266,-61.0001195637171,-228.410996850065));
#207646=CARTESIAN_POINT('Ctrl Pts',(40.9545231990119,-61.0203276738028,
-228.402749642383));
#207647=CARTESIAN_POINT('Ctrl Pts',(40.9437436672703,-61.0408032710641,
-228.393885042642));
#207648=CARTESIAN_POINT('Ctrl Pts',(40.9336502467295,-61.0615476677132,
-228.384396871472));
#207649=CARTESIAN_POINT('Ctrl Pts',(40.929608662109,-61.0698540920934,-228.380597639436));
#207650=CARTESIAN_POINT('Ctrl Pts',(40.92553780094,-61.0784981103401,-228.3765612754));
#207651=CARTESIAN_POINT('Ctrl Pts',(40.9216159438804,-61.0871276381461,
-228.372444588586));
#207652=CARTESIAN_POINT('Ctrl Pts',(40.9176158482466,-61.0959293195877,
-228.368245776466));
#207653=CARTESIAN_POINT('Ctrl Pts',(40.9137709112863,-61.1047157126402,
-228.363963477019));
#207654=CARTESIAN_POINT('Ctrl Pts',(40.9102260118624,-61.1131057492398,
-228.359796853342));
#207655=CARTESIAN_POINT('Ctrl Pts',(40.908812233677,-61.1164518669433,-228.358135118844));
#207656=CARTESIAN_POINT('Ctrl Pts',(40.907445684125,-61.1197348779016,-228.35649213395));
#207657=CARTESIAN_POINT('Ctrl Pts',(40.9061336970849,-61.1229304187023,
-228.354881812122));
#207658=CARTESIAN_POINT('Ctrl Pts',(40.9059057765971,-61.1234855531631,
-228.354602064437));
#207659=CARTESIAN_POINT('Ctrl Pts',(40.9056794946264,-61.1240379804454,
-228.354323359087));
#207660=CARTESIAN_POINT('Ctrl Pts',(40.9054548859916,-61.1245875752137,
-228.354045769407));
#207661=CARTESIAN_POINT('Ctrl Pts',(40.8895791691886,-61.163433859588,-228.334425263015));
#207662=CARTESIAN_POINT('Ctrl Pts',(40.8760959108351,-61.202729232473,-228.313004683474));
#207663=CARTESIAN_POINT('Ctrl Pts',(40.864938821336,-61.2424592911638,-228.289840584947));
#207664=CARTESIAN_POINT('Ctrl Pts',(40.8551443466649,-61.2773371196117,
-228.269505516709));
#207665=CARTESIAN_POINT('Ctrl Pts',(40.8471421184351,-61.3125510851886,
-228.247826182382));
#207666=CARTESIAN_POINT('Ctrl Pts',(40.8409152666239,-61.348111079235,-228.224809686116));
#207667=CARTESIAN_POINT('Ctrl Pts',(40.8348327040824,-61.3828470733333,
-228.202326530539));
#207668=CARTESIAN_POINT('Ctrl Pts',(40.8304445378103,-61.4179102691019,
-228.178569468885));
#207669=CARTESIAN_POINT('Ctrl Pts',(40.8277690023158,-61.4533105529692,
-228.153524940798));
#207670=CARTESIAN_POINT('Ctrl Pts',(40.8249932163602,-61.4900372609432,
-228.127542011598));
#207671=CARTESIAN_POINT('Ctrl Pts',(40.8240607946239,-61.5271238425471,
-228.100175491165));
#207672=CARTESIAN_POINT('Ctrl Pts',(40.8250357033287,-61.5645566624456,
-228.071404099149));
#207673=CARTESIAN_POINT('Ctrl Pts',(40.8251726188277,-61.5698137015823,
-228.067363464908));
#207674=CARTESIAN_POINT('Ctrl Pts',(40.8253472277531,-61.5750775224125,
-228.063295116071));
#207675=CARTESIAN_POINT('Ctrl Pts',(40.8255597807069,-61.5803480206386,
-228.059199003225));
#207676=CARTESIAN_POINT('Ctrl Pts',(40.825799634981,-61.5862954869228,-228.054576766009));
#207677=CARTESIAN_POINT('Ctrl Pts',(40.8261100272156,-61.5926975688732,
-228.049569932398));
#207678=CARTESIAN_POINT('Ctrl Pts',(40.8264578487316,-61.5987977399614,
-228.044768050139));
#207679=CARTESIAN_POINT('Ctrl Pts',(40.8266877729433,-61.6028302019118,
-228.041593810069));
#207680=CARTESIAN_POINT('Ctrl Pts',(40.8269329257887,-61.6067311348939,
-228.038509504216));
#207681=CARTESIAN_POINT('Ctrl Pts',(40.8271725319483,-61.6102864365788,
-228.035688802337));
#207682=CARTESIAN_POINT('Ctrl Pts',(40.8272131709247,-61.6108894420335,
-228.035210390441));
#207683=CARTESIAN_POINT('Ctrl Pts',(40.8272536360648,-61.6114825561387,
-228.034739531352));
#207684=CARTESIAN_POINT('Ctrl Pts',(40.8272938061133,-61.6120647388012,
-228.034277080873));
#207685=CARTESIAN_POINT('Ctrl Pts',(40.8298349940696,-61.6488940587812,
-228.00502211024));
#207686=CARTESIAN_POINT('Ctrl Pts',(40.8341898410855,-61.6853715561985,
-227.974947206424));
#207687=CARTESIAN_POINT('Ctrl Pts',(40.840294556687,-61.7215236844399,-227.944074086286));
#207688=CARTESIAN_POINT('Ctrl Pts',(40.8466081307678,-61.7589126726802,
-227.912144714988));
#207689=CARTESIAN_POINT('Ctrl Pts',(40.854793122881,-61.7959550152558,-227.879360657465));
#207690=CARTESIAN_POINT('Ctrl Pts',(40.86482559579,-61.8326735860296,-227.845723429335));
#207691=CARTESIAN_POINT('Ctrl Pts',(40.8745653337792,-61.8683207551688,
-227.813067693144));
#207692=CARTESIAN_POINT('Ctrl Pts',(40.8860468086191,-61.9036640700498,
-227.779606546507));
#207693=CARTESIAN_POINT('Ctrl Pts',(40.8992893740948,-61.9387038113221,
-227.745333169578));
#207694=CARTESIAN_POINT('Ctrl Pts',(40.9053795738278,-61.9548184398155,
-227.729570988798));
#207695=CARTESIAN_POINT('Ctrl Pts',(40.9118428318196,-61.9708685867213,
-227.713636893048));
#207696=CARTESIAN_POINT('Ctrl Pts',(40.9186838005535,-61.9868520978782,
-227.697530300764));
#207697=CARTESIAN_POINT('Ctrl Pts',(40.9224514188616,-61.9956549109891,
-227.688659701537));
#207698=CARTESIAN_POINT('Ctrl Pts',(40.9264807276567,-62.0047698498522,
-227.679399004713));
#207699=CARTESIAN_POINT('Ctrl Pts',(40.9305535053323,-62.013685526149,-227.67026325364));
#207700=CARTESIAN_POINT('Ctrl Pts',(40.9343385705297,-62.0219713739782,
-227.661772877737));
#207701=CARTESIAN_POINT('Ctrl Pts',(40.9381604199117,-62.0300854268991,
-227.653390637984));
#207702=CARTESIAN_POINT('Ctrl Pts',(40.9418110223868,-62.0376411022744,
-227.645531244992));
#207703=CARTESIAN_POINT('Ctrl Pts',(40.9419554686057,-62.0379400635409,
-227.645220266295));
#207704=CARTESIAN_POINT('Ctrl Pts',(40.9420996426571,-62.038238161741,-227.644910100089));
#207705=CARTESIAN_POINT('Ctrl Pts',(40.9422435309139,-62.0385353735754,
-227.644600772006));
#207706=CARTESIAN_POINT('Ctrl Pts',(41.0037900116267,-62.1656641806455,
-227.512289384515));
#207707=CARTESIAN_POINT('Ctrl Pts',(41.0857394019224,-62.2807520250138,
-227.377065009777));
#207708=CARTESIAN_POINT('Ctrl Pts',(41.1874522920715,-62.3844144545142,
-227.238927571877));
#207709=CARTESIAN_POINT('Ctrl Pts',(41.7563078823353,-62.3074742642099,
-227.60005));
#207710=CARTESIAN_POINT('Ctrl Pts',(41.7026267238965,-62.2527647791652,
-227.643792731266));
#207711=CARTESIAN_POINT('Ctrl Pts',(41.6565415403856,-62.200359156799,-227.684086045573));
#207712=CARTESIAN_POINT('Ctrl Pts',(41.5970055355346,-62.1269748350088,
-227.738766339681));
#207713=CARTESIAN_POINT('Ctrl Pts',(41.5787613895645,-62.1033815672565,
-227.756041513266));
#207714=CARTESIAN_POINT('Ctrl Pts',(41.5535989156551,-62.0694882409635,
-227.780515268765));
#207715=CARTESIAN_POINT('Ctrl Pts',(41.5415689308369,-62.0529154117129,
-227.792392926535));
#207716=CARTESIAN_POINT('Ctrl Pts',(41.5284587659491,-62.0342737779368,
-227.805623935743));
#207717=CARTESIAN_POINT('Ctrl Pts',(41.5230342538352,-62.0264370469646,
-227.811160687378));
#207718=CARTESIAN_POINT('Ctrl Pts',(41.5194606092816,-62.0212468923819,
-227.814822210717));
#207719=CARTESIAN_POINT('Ctrl Pts',(41.5185130669224,-62.0198696273061,
-227.815793580791));
#207720=CARTESIAN_POINT('Ctrl Pts',(41.4749543623288,-61.955929657224,-227.860770813693));
#207721=CARTESIAN_POINT('Ctrl Pts',(41.4402071580976,-61.8974857906177,
-227.900311593228));
#207722=CARTESIAN_POINT('Ctrl Pts',(41.3963536552126,-61.8135081173075,
-227.95506194786));
#207723=CARTESIAN_POINT('Ctrl Pts',(41.3831145126627,-61.7861294546533,
-227.97255652996));
#207724=CARTESIAN_POINT('Ctrl Pts',(41.3651951560785,-61.7461085650297,
-227.997655201073));
#207725=CARTESIAN_POINT('Ctrl Pts',(41.3567204361325,-61.7263597795088,
-228.009919084671));
#207726=CARTESIAN_POINT('Ctrl Pts',(41.3476551381641,-61.7038037315272,
-228.023728678121));
#207727=CARTESIAN_POINT('Ctrl Pts',(41.343943347233,-61.6942433384729,-228.029540639883));
#207728=CARTESIAN_POINT('Ctrl Pts',(41.3415070331292,-61.6878937067045,
-228.033391670802));
#207729=CARTESIAN_POINT('Ctrl Pts',(41.3407858071833,-61.6860066029679,
-228.034535283631));
#207730=CARTESIAN_POINT('Ctrl Pts',(41.3126011552024,-61.6107572390613,
-228.079959711279));
#207731=CARTESIAN_POINT('Ctrl Pts',(41.2945210437306,-61.5431299204009,
-228.118474409734));
#207732=CARTESIAN_POINT('Ctrl Pts',(41.2787043693704,-61.4478231136571,
-228.169410280855));
#207733=CARTESIAN_POINT('Ctrl Pts',(41.2753166770858,-61.4170759345204,
-228.185255180313));
#207734=CARTESIAN_POINT('Ctrl Pts',(41.2729000846091,-61.372646611079,-228.207308552331));
#207735=CARTESIAN_POINT('Ctrl Pts',(41.2723581451704,-61.3508546926235,
-228.2179071948));
#207736=CARTESIAN_POINT('Ctrl Pts',(41.2728580181042,-61.3262039384022,
-228.229524784819));
#207737=CARTESIAN_POINT('Ctrl Pts',(41.27331130909,-61.3158084787955,-228.234344013731));
#207738=CARTESIAN_POINT('Ctrl Pts',(41.2736662371782,-61.308916144085,-228.237521390818));
#207739=CARTESIAN_POINT('Ctrl Pts',(41.2737659913982,-61.307031081556,-228.238389501627));
#207740=CARTESIAN_POINT('Ctrl Pts',(41.2847906540784,-61.1436769906793,
-228.312841875131));
#207741=CARTESIAN_POINT('Ctrl Pts',(41.3528351981069,-61.0176483773379,
-228.35005));
#207742=CARTESIAN_POINT('Ctrl Pts',(41.4636310035131,-60.9383233439604,
-228.35005));
#207743=CARTESIAN_POINT('Origin',(48.2737085028446,-66.8079885321834,-218.85005));
#207744=CARTESIAN_POINT('',(49.0417551583074,-68.6546353135231,-218.35005));
#207745=CARTESIAN_POINT('',(48.8497434944417,-68.1929736181882,-218.85005));
#207746=CARTESIAN_POINT('Origin',(49.0417551583074,-68.6546353135231,-218.85005));
#207747=CARTESIAN_POINT('Origin',(48.2737085028446,-66.8079885321834,-218.85005));
#207748=CARTESIAN_POINT('Origin',(48.2737085028446,-66.8079885321834,-218.35005));
#207749=CARTESIAN_POINT('Ctrl Pts',(41.1874522920715,-62.3844144545142,
-227.238927571877));
#207750=CARTESIAN_POINT('Ctrl Pts',(41.533590072875,-62.0804900295131,-227.265723268608));
#207751=CARTESIAN_POINT('Ctrl Pts',(41.7563078823354,-62.3074742642099,
-227.60005));
#207752=CARTESIAN_POINT('Ctrl Pts',(42.9977586927641,-64.2294190860942,
-224.780329817623));
#207753=CARTESIAN_POINT('Ctrl Pts',(43.3439332486946,-63.9255124877361,
-224.807072796208));
#207754=CARTESIAN_POINT('Ctrl Pts',(43.5663090949841,-64.1521482085568,
-225.141881592783));
#207755=CARTESIAN_POINT('Ctrl Pts',(44.8096404055398,-66.0773673148437,
-222.324535970207));
#207756=CARTESIAN_POINT('Ctrl Pts',(45.1633560000594,-65.7797884513162,
-222.341036594742));
#207757=CARTESIAN_POINT('Ctrl Pts',(45.3784193710744,-65.9989716179707,
-222.686835360681));
#207758=CARTESIAN_POINT('Ctrl Pts',(46.6323854374629,-67.9411854921914,
-219.886423382228));
#207759=CARTESIAN_POINT('Ctrl Pts',(46.9799636370447,-67.6311953742356,
-219.91012892279));
#207760=CARTESIAN_POINT('Ctrl Pts',(47.2030337908495,-67.8585387028531,
-220.250747695207));
#207761=CARTESIAN_POINT('',(47.2030337908494,-67.858538702853,-220.250747695207));
#207762=CARTESIAN_POINT('',(46.6323854374629,-67.9411854921913,-219.886423382228));
#207763=CARTESIAN_POINT('Origin',(46.8461422201844,-68.2087220930763,-220.250747695207));
#207764=CARTESIAN_POINT('Ctrl Pts',(41.1874522920715,-62.3844144545142,
-227.238927571877));
#207765=CARTESIAN_POINT('Ctrl Pts',(41.6650043735109,-62.8711197999119,
-226.59035864759));
#207766=CARTESIAN_POINT('Ctrl Pts',(42.1301866064175,-63.3454119978617,
-225.959062309233));
#207767=CARTESIAN_POINT('Ctrl Pts',(42.8097176035461,-64.0383310888314,
-225.038026680594));
#207768=CARTESIAN_POINT('Ctrl Pts',(43.1449188366604,-64.3801644733344,
-224.583986085998));
#207769=CARTESIAN_POINT('Ctrl Pts',(43.528027568592,-64.7709351764863,-224.065607193486));
#207770=CARTESIAN_POINT('Ctrl Pts',(43.717592476361,-64.9643223419007,-223.809251530859));
#207771=CARTESIAN_POINT('Ctrl Pts',(43.8118775094903,-65.0605177877102,
-223.681782145453));
#207772=CARTESIAN_POINT('Ctrl Pts',(43.8588955882238,-65.1084912135109,
-223.618224564227));
#207773=CARTESIAN_POINT('Ctrl Pts',(43.8790195202237,-65.1290246426943,
-223.591023553304));
#207774=CARTESIAN_POINT('Ctrl Pts',(43.8924295465235,-65.1427076848833,
-223.572897979902));
#207775=CARTESIAN_POINT('Ctrl Pts',(43.8984888898217,-65.1488904466342,
-223.564708078702));
#207776=CARTESIAN_POINT('Ctrl Pts',(44.8455797929338,-66.1152831054553,
-222.284638320274));
#207777=CARTESIAN_POINT('Ctrl Pts',(45.753629864441,-67.0426283261149,-221.061851095243));
#207778=CARTESIAN_POINT('Ctrl Pts',(46.6323854374629,-67.9411854921913,
-219.886423382228));
#207779=CARTESIAN_POINT('Ctrl Pts',(47.2030337908494,-67.858538702853,-220.250747695207));
#207780=CARTESIAN_POINT('Ctrl Pts',(45.378411470404,-65.9989635659536,-222.68684590906));
#207781=CARTESIAN_POINT('Ctrl Pts',(43.5663164045416,-64.1521556581376,
-225.14187166565));
#207782=CARTESIAN_POINT('Ctrl Pts',(41.7563078823354,-62.3074742642099,
-227.60005));
#207783=CARTESIAN_POINT('Ctrl Pts',(48.8497434944417,-68.1929736181882,
-218.85005));
#207784=CARTESIAN_POINT('Ctrl Pts',(48.8497434944417,-68.1929736181882,
-218.35005));
#207785=CARTESIAN_POINT('Ctrl Pts',(49.0417551583074,-68.6546353135231,
-218.35005));
#207786=CARTESIAN_POINT('Ctrl Pts',(48.7287312757308,-68.2433043207298,
-218.85004996112));
#207787=CARTESIAN_POINT('Ctrl Pts',(48.7557592223196,-68.232063046543,-218.382837715704));
#207788=CARTESIAN_POINT('Ctrl Pts',(48.8914370751605,-68.6805168842225,
-218.35005));
#207789=CARTESIAN_POINT('Ctrl Pts',(48.6040131804169,-68.2768832027127,
-218.836912439222));
#207790=CARTESIAN_POINT('Ctrl Pts',(48.6402644556944,-68.2689304282727,
-218.402170544444));
#207791=CARTESIAN_POINT('Ctrl Pts',(48.7342750095003,-68.6918682705249,
-218.342169793108));
#207792=CARTESIAN_POINT('Ctrl Pts',(48.4757604447939,-68.2943179077776,
-218.82266550408));
#207793=CARTESIAN_POINT('Ctrl Pts',(48.5093251395215,-68.2897551158004,
-218.412348259396));
#207794=CARTESIAN_POINT('Ctrl Pts',(48.5701931618903,-68.6892604152372,
-218.333619302448));
#207795=CARTESIAN_POINT('',(48.5701931618903,-68.6892604152372,-218.333619302448));
#207796=CARTESIAN_POINT('',(48.4757604447939,-68.2943179077777,-218.82266550408));
#207797=CARTESIAN_POINT('Origin',(48.5431110921104,-68.7897610329756,-218.82266550408));
#207798=CARTESIAN_POINT('Ctrl Pts',(48.8497434944417,-68.1929736181882,
-218.85005));
#207799=CARTESIAN_POINT('Ctrl Pts',(48.8253786724137,-68.2031072941346,
-218.850049992172));
#207800=CARTESIAN_POINT('Ctrl Pts',(48.7996420667697,-68.213071276654,-218.849493836655));
#207801=CARTESIAN_POINT('Ctrl Pts',(48.7724981693848,-68.2226546374388,
-218.848378544969));
#207802=CARTESIAN_POINT('Ctrl Pts',(48.7693432105752,-68.2237685198008,
-218.848248913646));
#207803=CARTESIAN_POINT('Ctrl Pts',(48.7661692323878,-68.2248772454103,
-218.848111784651));
#207804=CARTESIAN_POINT('Ctrl Pts',(48.7629761734588,-68.225980471413,-218.84796719926));
#207805=CARTESIAN_POINT('Ctrl Pts',(48.7476437968494,-68.2312779234595,
-218.847272931563));
#207806=CARTESIAN_POINT('Ctrl Pts',(48.7318720892122,-68.2364484273792,
-218.846405096242));
#207807=CARTESIAN_POINT('Ctrl Pts',(48.7156578079315,-68.2414522477113,
-218.845363694404));
#207808=CARTESIAN_POINT('Ctrl Pts',(48.7075506672912,-68.2439541578774,
-218.844842993486));
#207809=CARTESIAN_POINT('Ctrl Pts',(48.6993328825448,-68.2464143815189,
-218.844278900983));
#207810=CARTESIAN_POINT('Ctrl Pts',(48.6910043184336,-68.2488278002158,
-218.843671417198));
#207811=CARTESIAN_POINT('Ctrl Pts',(48.686840036378,-68.2500345095643,-218.843367675305));
#207812=CARTESIAN_POINT('Ctrl Pts',(48.6826480594132,-68.2512295172066,
-218.843053085484));
#207813=CARTESIAN_POINT('Ctrl Pts',(48.6784283853964,-68.252412176893,-218.842727562152));
#207814=CARTESIAN_POINT('Ctrl Pts',(48.6751994187233,-68.2533171682971,
-218.842478466135));
#207815=CARTESIAN_POINT('Ctrl Pts',(48.6711530911778,-68.2544347700194,
-218.842158889697));
#207816=CARTESIAN_POINT('Ctrl Pts',(48.6681283537951,-68.2552591312216,
-218.841915521378));
#207817=CARTESIAN_POINT('Ctrl Pts',(48.6672003078158,-68.2555120606506,
-218.841840851427));
#207818=CARTESIAN_POINT('Ctrl Pts',(48.666368517125,-68.2557377718834,-218.841773526889));
#207819=CARTESIAN_POINT('Ctrl Pts',(48.6656862746315,-68.255922463752,-218.841718135008));
#207820=CARTESIAN_POINT('Ctrl Pts',(48.649737121747,-68.2602401057584,-218.840423208958));
#207821=CARTESIAN_POINT('Ctrl Pts',(48.6318323557602,-68.2648053884177,
-218.838855344496));
#207822=CARTESIAN_POINT('Ctrl Pts',(48.6119507030164,-68.2694009179544,
-218.836970612394));
#207823=CARTESIAN_POINT('Ctrl Pts',(48.5929129470642,-68.2738013856076,
-218.835165879645));
#207824=CARTESIAN_POINT('Ctrl Pts',(48.5720624686907,-68.2782291657522,
-218.833069427729));
#207825=CARTESIAN_POINT('Ctrl Pts',(48.5493736675765,-68.2824612289884,
-218.830677796369));
#207826=CARTESIAN_POINT('Ctrl Pts',(48.5285405771963,-68.2863471529494,
-218.828481775872));
#207827=CARTESIAN_POINT('Ctrl Pts',(48.5061574779594,-68.2900676146866,
-218.826036371646));
#207828=CARTESIAN_POINT('Ctrl Pts',(48.4821999960562,-68.2934285274618,
-218.82338018019));
#207829=CARTESIAN_POINT('Ctrl Pts',(48.4800659796662,-68.2937279012849,
-218.823143579527));
#207830=CARTESIAN_POINT('Ctrl Pts',(48.4779194688382,-68.2940244095746,
-218.822905338518));
#207831=CARTESIAN_POINT('Ctrl Pts',(48.4757604447939,-68.2943179077776,
-218.82266550408));
#207832=CARTESIAN_POINT('Ctrl Pts',(48.5701931618903,-68.6892604152372,
-218.333619302448));
#207833=CARTESIAN_POINT('Ctrl Pts',(48.7359603200225,-68.6918950616687,
-218.342257615425));
#207834=CARTESIAN_POINT('Ctrl Pts',(48.8931846693406,-68.6802159916351,
-218.35005));
#207835=CARTESIAN_POINT('Ctrl Pts',(49.0417551583074,-68.6546353135231,
-218.35005));
#207836=CARTESIAN_POINT('Ctrl Pts',(48.4757604447937,-68.2943179077776,
-218.82266550408));
#207837=CARTESIAN_POINT('Ctrl Pts',(48.3620909039911,-68.309770170134,-218.591540694519));
#207838=CARTESIAN_POINT('Ctrl Pts',(48.3245605310988,-68.5271120961852,
-218.457629631481));
#207839=CARTESIAN_POINT('Ctrl Pts',(48.2145031263758,-68.3298332850564,
-218.997150144364));
#207840=CARTESIAN_POINT('Ctrl Pts',(48.0565790003986,-68.3305373905487,
-218.760296345904));
#207841=CARTESIAN_POINT('Ctrl Pts',(47.9776226084149,-68.5733796207043,
-218.632054575151));
#207842=CARTESIAN_POINT('Ctrl Pts',(47.9672522644602,-68.2939398715798,
-219.226769248345));
#207843=CARTESIAN_POINT('Ctrl Pts',(47.7753561891483,-68.2571865053622,
-218.980775448776));
#207844=CARTESIAN_POINT('Ctrl Pts',(47.6490670814862,-68.5245197011494,
-218.861741583456));
#207845=CARTESIAN_POINT('Ctrl Pts',(47.539630313305,-68.1358047923417,-219.716553805522));
#207846=CARTESIAN_POINT('Ctrl Pts',(47.3075378575116,-68.013479625276,-219.436238572541));
#207847=CARTESIAN_POINT('Ctrl Pts',(47.0804817541883,-68.3120180317949,
-219.351800153131));
#207848=CARTESIAN_POINT('Ctrl Pts',(47.354847997338,-68.013261091513,-219.980493179131));
#207849=CARTESIAN_POINT('Ctrl Pts',(47.1165089694488,-67.8332337800358,
-219.681063518939));
#207850=CARTESIAN_POINT('Ctrl Pts',(46.8345979831258,-68.1479546277615,
-219.615942902681));
#207851=CARTESIAN_POINT('Ctrl Pts',(47.2030337908474,-67.858538702855,-220.250747695207));
#207852=CARTESIAN_POINT('Ctrl Pts',(46.9799636370427,-67.6311953742376,
-219.91012892279));
#207853=CARTESIAN_POINT('Ctrl Pts',(46.6323854374609,-67.9411854921933,
-219.886423382227));
#207854=CARTESIAN_POINT('',(48.3245605310987,-68.5271120961857,-218.45762963148));
#207855=CARTESIAN_POINT('Origin',(48.5431110921103,-68.7897610329758,-218.82266550408));
#207856=CARTESIAN_POINT('Ctrl Pts',(46.632385437463,-67.9411854921914,-219.886423382228));
#207857=CARTESIAN_POINT('Ctrl Pts',(46.6789349826013,-67.9887839692199,
-219.824158485406));
#207858=CARTESIAN_POINT('Ctrl Pts',(46.7272112617812,-68.0335239722974,
-219.763011130579));
#207859=CARTESIAN_POINT('Ctrl Pts',(46.7770922567545,-68.0754781330116,
-219.702981480643));
#207860=CARTESIAN_POINT('Ctrl Pts',(46.8296502730403,-68.1196838964142,
-219.639730149737));
#207861=CARTESIAN_POINT('Ctrl Pts',(46.8839897850005,-68.160797451316,-219.577719302768));
#207862=CARTESIAN_POINT('Ctrl Pts',(46.9400226203996,-68.1988812889257,
-219.516936401576));
#207863=CARTESIAN_POINT('Ctrl Pts',(46.9985251342596,-68.2386436929114,
-219.453474460125));
#207864=CARTESIAN_POINT('Ctrl Pts',(47.0588761815705,-68.2751048341591,
-219.391348551543));
#207865=CARTESIAN_POINT('Ctrl Pts',(47.1210077877848,-68.3082886731283,
-219.330562267133));
#207866=CARTESIAN_POINT('Ctrl Pts',(47.1831393939991,-68.3414725120975,
-219.269775982722));
#207867=CARTESIAN_POINT('Ctrl Pts',(47.2470552838015,-68.3713804372138,
-219.210326169212));
#207868=CARTESIAN_POINT('Ctrl Pts',(47.3127122895345,-68.3979939965537,
-219.152234411495));
#207869=CARTESIAN_POINT('Ctrl Pts',(47.3221962661813,-68.4018382531178,
-219.143843214434));
#207870=CARTESIAN_POINT('Ctrl Pts',(47.3312777219034,-68.4054398649159,
-219.135865758659));
#207871=CARTESIAN_POINT('Ctrl Pts',(47.3406919758767,-68.409094347228,-219.127653243753));
#207872=CARTESIAN_POINT('Ctrl Pts',(47.3480787307764,-68.4119617826299,
-219.121209415608));
#207873=CARTESIAN_POINT('Ctrl Pts',(47.3556708314958,-68.4148611232482,
-219.114621070859));
#207874=CARTESIAN_POINT('Ctrl Pts',(47.3638354720275,-68.4179171786934,
-219.107580695432));
#207875=CARTESIAN_POINT('Ctrl Pts',(47.364148530177,-68.418034357528,-219.107310745163));
#207876=CARTESIAN_POINT('Ctrl Pts',(47.3644616002814,-68.4181514532561,
-219.107040847959));
#207877=CARTESIAN_POINT('Ctrl Pts',(47.3647746823481,-68.4182684659211,
-219.10677100378));
#207878=CARTESIAN_POINT('Ctrl Pts',(47.4110307172631,-68.4355563993204,
-219.066903112672));
#207879=CARTESIAN_POINT('Ctrl Pts',(47.4576985949707,-68.4510436336742,
-219.028094295378));
#207880=CARTESIAN_POINT('Ctrl Pts',(47.5047241972111,-68.4647642254001,
-218.990341332514));
#207881=CARTESIAN_POINT('Ctrl Pts',(47.5329030678403,-68.4729859335927,
-218.967718850169));
#207882=CARTESIAN_POINT('Ctrl Pts',(47.5612113910329,-68.4805730273755,
-218.945475130944));
#207883=CARTESIAN_POINT('Ctrl Pts',(47.5896454632259,-68.4875294857434,
-218.923607470301));
#207884=CARTESIAN_POINT('Ctrl Pts',(47.6277488305346,-68.4968515584511,
-218.894303489499));
#207885=CARTESIAN_POINT('Ctrl Pts',(47.6660759138159,-68.5050408980252,
-218.865676249708));
#207886=CARTESIAN_POINT('Ctrl Pts',(47.7046218854028,-68.5120873419134,
-218.837731470339));
#207887=CARTESIAN_POINT('Ctrl Pts',(47.7238948711963,-68.5156105638575,
-218.823759080654));
#207888=CARTESIAN_POINT('Ctrl Pts',(47.7432236774575,-68.5188456333958,
-218.809958418662));
#207889=CARTESIAN_POINT('Ctrl Pts',(47.7626047403424,-68.5217969580725,
-218.796327863849));
#207890=CARTESIAN_POINT('Ctrl Pts',(47.7729855113983,-68.5233777292595,
-218.789027146147));
#207891=CARTESIAN_POINT('Ctrl Pts',(47.7829426565521,-68.524813935548,-218.782081134656));
#207892=CARTESIAN_POINT('Ctrl Pts',(47.7931789075124,-68.5262114580297,
-218.774996323705));
#207893=CARTESIAN_POINT('Ctrl Pts',(47.8020538981449,-68.527423132009,-218.768853681144));
#207894=CARTESIAN_POINT('Ctrl Pts',(47.8111389551874,-68.5286052992481,
-218.762606853945));
#207895=CARTESIAN_POINT('Ctrl Pts',(47.8209032985487,-68.5298001944143,
-218.755946475681));
#207896=CARTESIAN_POINT('Ctrl Pts',(47.8790078311355,-68.5369106392807,
-218.716312661959));
#207897=CARTESIAN_POINT('Ctrl Pts',(47.9371237250222,-68.5414328500945,
-218.678502918883));
#207898=CARTESIAN_POINT('Ctrl Pts',(47.9951858050162,-68.5434012407283,
-218.642520231142));
#207899=CARTESIAN_POINT('Ctrl Pts',(48.0542593885108,-68.5454039228311,
-218.605910686516));
#207900=CARTESIAN_POINT('Ctrl Pts',(48.1132779188672,-68.5447637771468,
-218.571191543065));
#207901=CARTESIAN_POINT('Ctrl Pts',(48.1722176288345,-68.5414882566244,
-218.538361397313));
#207902=CARTESIAN_POINT('Ctrl Pts',(48.2230544566548,-68.538663046373,-218.510044656906));
#207903=CARTESIAN_POINT('Ctrl Pts',(48.2738336083459,-68.5338770215185,
-218.483132870144));
#207904=CARTESIAN_POINT('Ctrl Pts',(48.3245605310988,-68.5271120961852,
-218.457629631481));
#207905=CARTESIAN_POINT('',(48.2736913638528,-68.3080354249668,-218.970411512989));
#207906=CARTESIAN_POINT('Ctrl Pts',(48.2736913638528,-68.3080354249668,
-218.970411512989));
#207907=CARTESIAN_POINT('Ctrl Pts',(48.2352706160841,-68.3080419600251,
-219.000929763438));
#207908=CARTESIAN_POINT('Ctrl Pts',(48.1961538364747,-68.3065666156675,
-219.033386630441));
#207909=CARTESIAN_POINT('Ctrl Pts',(48.1564716235175,-68.3034518671295,
-219.067833966359));
#207910=CARTESIAN_POINT('Ctrl Pts',(48.1190450812612,-68.3005141713942,
-219.100323199627));
#207911=CARTESIAN_POINT('Ctrl Pts',(48.0811155483893,-68.2961179360676,
-219.134583250583));
#207912=CARTESIAN_POINT('Ctrl Pts',(48.0428230551683,-68.2901435429112,
-219.170624127822));
#207913=CARTESIAN_POINT('Ctrl Pts',(48.0120582244176,-68.2853436153318,
-219.199579972561));
#207914=CARTESIAN_POINT('Ctrl Pts',(47.9810624393644,-68.2795258339341,
-219.229681930507));
#207915=CARTESIAN_POINT('Ctrl Pts',(47.9499142999773,-68.2726338250037,
-219.260926465793));
#207916=CARTESIAN_POINT('Ctrl Pts',(47.9173884187917,-68.2654369693324,
-219.293553006651));
#207917=CARTESIAN_POINT('Ctrl Pts',(47.884690621732,-68.2570677822824,-219.327430912405));
#207918=CARTESIAN_POINT('Ctrl Pts',(47.8519122600643,-68.2474620614157,
-219.362556430075));
#207919=CARTESIAN_POINT('Ctrl Pts',(47.831598938395,-68.2415092288792,-219.384324325203));
#207920=CARTESIAN_POINT('Ctrl Pts',(47.811255962524,-68.2350819225415,-219.406569983772));
#207921=CARTESIAN_POINT('Ctrl Pts',(47.7909033810425,-68.2281634706586,
-219.429295593734));
#207922=CARTESIAN_POINT('Ctrl Pts',(47.7784142497046,-68.2239180409426,
-219.443240907147));
#207923=CARTESIAN_POINT('Ctrl Pts',(47.7659232461178,-68.2194881738068,
-219.457365090839));
#207924=CARTESIAN_POINT('Ctrl Pts',(47.7534412888826,-68.2148723319607,
-219.471661526933));
#207925=CARTESIAN_POINT('Ctrl Pts',(47.7408887066471,-68.21023037291,-219.486038854652));
#207926=CARTESIAN_POINT('Ctrl Pts',(47.7283302837597,-68.2053993054349,
-219.500603213225));
#207927=CARTESIAN_POINT('Ctrl Pts',(47.7157811377292,-68.2003778392676,
-219.515344195403));
#207928=CARTESIAN_POINT('Ctrl Pts',(47.7069924423551,-68.1968610950709,
-219.525667925922));
#207929=CARTESIAN_POINT('Ctrl Pts',(47.6982072159195,-68.1932505778963,
-219.536079512527));
#207930=CARTESIAN_POINT('Ctrl Pts',(47.6894276522935,-68.1895447985078,
-219.546578761834));
#207931=CARTESIAN_POINT('Ctrl Pts',(47.6850378704804,-68.1876919088135,
-219.551828386488));
#207932=CARTESIAN_POINT('Ctrl Pts',(47.6806495046123,-68.1858152041822,
-219.557099926126));
#207933=CARTESIAN_POINT('Ctrl Pts',(47.6762628309838,-68.1839145024519,
-219.562393351676));
#207934=CARTESIAN_POINT('Ctrl Pts',(47.6751661625767,-68.1834393270193,
-219.563716708063));
#207935=CARTESIAN_POINT('Ctrl Pts',(47.6740695999485,-68.1829626517843,
-219.565041432296));
#207936=CARTESIAN_POINT('Ctrl Pts',(47.6729731474406,-68.1824844739318,
-219.566367523873));
#207937=CARTESIAN_POINT('Ctrl Pts',(47.6727519650219,-68.1823880132704,
-219.566635030345));
#207938=CARTESIAN_POINT('Ctrl Pts',(47.6725293350301,-68.1822908590618,
-219.566904347797));
#207939=CARTESIAN_POINT('Ctrl Pts',(47.6723008586559,-68.182191085278,-219.567180803719));
#207940=CARTESIAN_POINT('Ctrl Pts',(47.6694450526422,-68.1809439779004,
-219.570636322859));
#207941=CARTESIAN_POINT('Ctrl Pts',(47.6659219370643,-68.1793899298261,
-219.574914316411));
#207942=CARTESIAN_POINT('Ctrl Pts',(47.6637661869299,-68.1784326234025,
-219.577538166137));
#207943=CARTESIAN_POINT('Ctrl Pts',(47.663529499819,-68.1783275174869,-219.577826247488));
#207944=CARTESIAN_POINT('Ctrl Pts',(47.6633092672032,-68.1782296454147,
-219.5780943722));
#207945=CARTESIAN_POINT('Ctrl Pts',(47.6631081652735,-68.1781402268487,
-219.578339252732));
#207946=CARTESIAN_POINT('Ctrl Pts',(47.6312267100201,-68.1639643608312,
-219.617161096537));
#207947=CARTESIAN_POINT('Ctrl Pts',(47.5979339811122,-68.1478376530234,
-219.65898213675));
#207948=CARTESIAN_POINT('Ctrl Pts',(47.5635841092145,-68.1294106324221,
-219.703868909107));
#207949=CARTESIAN_POINT('Ctrl Pts',(47.5312117306429,-68.1120444399476,
-219.746171587613));
#207950=CARTESIAN_POINT('Ctrl Pts',(47.4979006949716,-68.092634432448,-219.791197643804));
#207951=CARTESIAN_POINT('Ctrl Pts',(47.4639844702321,-68.07088947511,-219.838976427383));
#207952=CARTESIAN_POINT('Ctrl Pts',(47.4313133363501,-68.0499427919839,
-219.885001214842));
#207953=CARTESIAN_POINT('Ctrl Pts',(47.398080746371,-68.0268288922644,-219.933580747127));
#207954=CARTESIAN_POINT('Ctrl Pts',(47.3646176674441,-68.0012979457342,
-219.984709699179));
#207955=CARTESIAN_POINT('Ctrl Pts',(47.3328901754178,-67.9770911802948,
-220.033186810986));
#207956=CARTESIAN_POINT('Ctrl Pts',(47.3009556582199,-67.9507112332735,
-220.083955944682));
#207957=CARTESIAN_POINT('Ctrl Pts',(47.269124158351,-67.9219610284792,-220.136979491753));
#207958=CARTESIAN_POINT('Ctrl Pts',(47.2470063865729,-67.9019842610999,
-220.173822327241));
#207959=CARTESIAN_POINT('Ctrl Pts',(47.2249389168298,-67.8808634476479,
-220.211752930696));
#207960=CARTESIAN_POINT('Ctrl Pts',(47.2030337908474,-67.858538702855,-220.250747695207));
#207961=CARTESIAN_POINT('Origin',(48.3024486247851,-65.8934766456585,-221.196305192212));
#207962=CARTESIAN_POINT('Origin',(48.5431110921103,-68.7897610329758,-218.82266550408));
#207963=CARTESIAN_POINT('Origin',(48.5431110921103,-68.7897610329758,-218.82266550408));
#207964=CARTESIAN_POINT('Ctrl Pts',(49.9129432931154,30.3691563923977,-227.499480149477));
#207965=CARTESIAN_POINT('Ctrl Pts',(49.6184756168536,30.1420169376964,-227.148453859162));
#207966=CARTESIAN_POINT('Ctrl Pts',(49.9837284343871,29.7888486466285,-227.087470733639));
#207967=CARTESIAN_POINT('Ctrl Pts',(49.7890584560673,30.2238721235565,-227.617517102611));
#207968=CARTESIAN_POINT('Ctrl Pts',(49.5695507897331,29.9909534013765,-227.289688948551));
#207969=CARTESIAN_POINT('Ctrl Pts',(49.8665188865492,29.6366170163525,-227.284491638227));
#207970=CARTESIAN_POINT('Ctrl Pts',(49.6516701724817,30.1008771252358,-227.734473228363));
#207971=CARTESIAN_POINT('Ctrl Pts',(49.4836503780786,29.8530854215471,-227.451963630924));
#207972=CARTESIAN_POINT('Ctrl Pts',(49.7240534002376,29.5185044777796,-227.479632631849));
#207973=CARTESIAN_POINT('Ctrl Pts',(49.3886607896581,29.9360305472667,-227.932360963694));
#207974=CARTESIAN_POINT('Ctrl Pts',(49.2742353859129,29.682693950235,-227.736609390718));
#207975=CARTESIAN_POINT('Ctrl Pts',(49.4281098110363,29.3861258524904,-227.809829648684));
#207976=CARTESIAN_POINT('Ctrl Pts',(49.2735716953388,29.882741984255,-228.012019018908));
#207977=CARTESIAN_POINT('Ctrl Pts',(49.1732865590743,29.6308954154206,-227.853520161143));
#207978=CARTESIAN_POINT('Ctrl Pts',(49.2924069787687,29.3532300095823,-227.942750035685));
#207979=CARTESIAN_POINT('Ctrl Pts',(49.0943862810714,29.8358745178422,-228.122462272144));
#207980=CARTESIAN_POINT('Ctrl Pts',(49.0001873355215,29.5964093801985,-228.017396499293));
#207981=CARTESIAN_POINT('Ctrl Pts',(49.0692583324707,29.3499433053121,-228.127035773479));
#207982=CARTESIAN_POINT('Ctrl Pts',(49.0341585258203,29.8261040960875,-228.157331139179));
#207983=CARTESIAN_POINT('Ctrl Pts',(48.9401951728418,29.592107178363,-228.069035448677));
#207984=CARTESIAN_POINT('Ctrl Pts',(48.9922826040891,29.356783950037,-228.185219179292));
#207985=CARTESIAN_POINT('Ctrl Pts',(48.9155060353659,29.8208605820001,-228.220674964975));
#207986=CARTESIAN_POINT('Ctrl Pts',(48.8177391420467,29.6007095174117,-228.162636460521));
#207987=CARTESIAN_POINT('Ctrl Pts',(48.8360255565098,29.3888574699875,-228.290916415101));
#207988=CARTESIAN_POINT('Ctrl Pts',(48.8558606667612,29.8254987747837,-228.249737935875));
#207989=CARTESIAN_POINT('Ctrl Pts',(48.7537342504269,29.6136686499989,-228.205811972947));
#207990=CARTESIAN_POINT('Ctrl Pts',(48.7550839596696,29.4146403264887,-228.339409706525));
#207991=CARTESIAN_POINT('Ctrl Pts',(48.6420919128915,29.8753757465965,-228.341028197144));
#207992=CARTESIAN_POINT('Ctrl Pts',(48.5186265173263,29.6983851148206,-228.339000179185));
#207993=CARTESIAN_POINT('Ctrl Pts',(48.4540259802448,29.5512136888258,-228.491735739523));
#207994=CARTESIAN_POINT('Ctrl Pts',(48.5064500994514,29.983068024979,-228.369467059033));
#207995=CARTESIAN_POINT('Ctrl Pts',(48.3448350811457,29.8430513441803,-228.381209650087));
#207996=CARTESIAN_POINT('Ctrl Pts',(48.2378026611094,29.7390715475708,-228.539159295418));
#207997=CARTESIAN_POINT('Ctrl Pts',(48.4475474979323,30.1465475641224,-228.335963042699));
#207998=CARTESIAN_POINT('Ctrl Pts',(48.2552013856293,30.0316164665649,-228.324119572824));
#207999=CARTESIAN_POINT('Ctrl Pts',(48.1059399365173,29.9750822258506,-228.483236405913));
#208000=CARTESIAN_POINT('',(48.2384287873563,29.7860380279371,-228.505869818703));
#208001=CARTESIAN_POINT('',(48.515339402069,30.020261242545,-228.35005));
#208002=CARTESIAN_POINT('Origin',(48.515339402069,30.020261242545,-228.85005));
#208003=CARTESIAN_POINT('',(49.8031531494471,30.2499539750197,-227.60005));
#208004=CARTESIAN_POINT('Ctrl Pts',(49.8031531494471,30.2499539750197,-227.60005));
#208005=CARTESIAN_POINT('Ctrl Pts',(49.7527362723413,30.1993679966667,-227.644974522657));
#208006=CARTESIAN_POINT('Ctrl Pts',(49.7041257946578,30.1562841819435,-227.686309984401));
#208007=CARTESIAN_POINT('Ctrl Pts',(49.6358287764031,30.1010089879944,-227.742300319835));
#208008=CARTESIAN_POINT('Ctrl Pts',(49.6138301469231,30.0841450753157,-227.759970768332));
#208009=CARTESIAN_POINT('Ctrl Pts',(49.5821921102083,30.0609822914565,-227.784975491548));
#208010=CARTESIAN_POINT('Ctrl Pts',(49.566712728017,30.0499345103878,-227.797103193557));
#208011=CARTESIAN_POINT('Ctrl Pts',(49.549289886841,30.0379373173742,-227.810599354216));
#208012=CARTESIAN_POINT('Ctrl Pts',(49.5419635975734,30.0329825325858,-227.816244118858));
#208013=CARTESIAN_POINT('Ctrl Pts',(49.5371111255115,30.0297204039543,-227.819976409313));
#208014=CARTESIAN_POINT('Ctrl Pts',(49.5358192723333,30.0288527682603,-227.820969727432));
#208015=CARTESIAN_POINT('Ctrl Pts',(49.4761015676757,29.9891895263879,-227.866745295705));
#208016=CARTESIAN_POINT('Ctrl Pts',(49.4212428073257,29.9579805853916,-227.906937128057));
#208017=CARTESIAN_POINT('Ctrl Pts',(49.3421216382348,29.919204999993,-227.962493464653));
#208018=CARTESIAN_POINT('Ctrl Pts',(49.3162749091124,29.9076202744173,-227.980228558398));
#208019=CARTESIAN_POINT('Ctrl Pts',(49.2784287290678,29.8921209136238,-228.005645523579));
#208020=CARTESIAN_POINT('Ctrl Pts',(49.2597364927902,29.8848407893681,-228.018057957077));
#208021=CARTESIAN_POINT('Ctrl Pts',(49.2383606512453,29.8771413537661,-228.0320224667));
#208022=CARTESIAN_POINT('Ctrl Pts',(49.2292949767161,29.8740088784577,-228.03789690835));
#208023=CARTESIAN_POINT('Ctrl Pts',(49.2232727107977,29.8719574195942,-228.041788726452));
#208024=CARTESIAN_POINT('Ctrl Pts',(49.2214396993231,29.8713363276065,-228.042972081044));
#208025=CARTESIAN_POINT('Ctrl Pts',(49.1507737414336,29.8479572973245,-228.088392226472));
#208026=CARTESIAN_POINT('Ctrl Pts',(49.0869264206795,29.8340568928808,-228.126800162686));
#208027=CARTESIAN_POINT('Ctrl Pts',(48.9965302726213,29.8239838805917,-228.17740626585));
#208028=CARTESIAN_POINT('Ctrl Pts',(48.9672934413079,29.8224230610671,-228.193113085777));
#208029=CARTESIAN_POINT('Ctrl Pts',(48.924945017721,29.8226136605282,-228.214916183171));
#208030=CARTESIAN_POINT('Ctrl Pts',(48.9041473927209,29.8233420361004,-228.225378910074));
#208031=CARTESIAN_POINT('Ctrl Pts',(48.8805769903507,29.8252653389655,-228.236818978745));
#208032=CARTESIAN_POINT('Ctrl Pts',(48.8706275872652,29.8263160738771,-228.241558062775));
#208033=CARTESIAN_POINT('Ctrl Pts',(48.8640288696302,29.8270664940945,-228.244681106617));
#208034=CARTESIAN_POINT('Ctrl Pts',(48.8619974565436,29.8273038682259,-228.245640131405));
#208035=CARTESIAN_POINT('Ctrl Pts',(48.7129766922957,29.8466994525346,-228.315254631247));
#208036=CARTESIAN_POINT('Ctrl Pts',(48.5945826105962,29.9151547892192,-228.35005));
#208037=CARTESIAN_POINT('Ctrl Pts',(48.515339402069,30.020261242545,-228.35005));
#208038=CARTESIAN_POINT('',(49.8755750290351,29.6684593880862,-227.255950349386));
#208039=CARTESIAN_POINT('Origin',(50.1572979707234,29.8969930061248,-227.60005));
#208040=CARTESIAN_POINT('Ctrl Pts',(48.2384287873563,29.7860380279371,-228.505869818703));
#208041=CARTESIAN_POINT('Ctrl Pts',(48.3005627733003,29.7125636424197,-228.505880994607));
#208042=CARTESIAN_POINT('Ctrl Pts',(48.3682975812994,29.6477646817255,-228.495224421534));
#208043=CARTESIAN_POINT('Ctrl Pts',(48.4781251048924,29.5638843894103,-228.463237938458));
#208044=CARTESIAN_POINT('Ctrl Pts',(48.5350955562029,29.5252734538315,-228.443244291053));
#208045=CARTESIAN_POINT('Ctrl Pts',(48.6051255375809,29.4861167483495,-228.412917658814));
#208046=CARTESIAN_POINT('Ctrl Pts',(48.6358987065498,29.4706038724335,-228.398420378511));
#208047=CARTESIAN_POINT('Ctrl Pts',(48.6565827304486,29.4605445821547,-228.38842215782));
#208048=CARTESIAN_POINT('Ctrl Pts',(48.6680836436967,29.4551709393352,-228.382711156425));
#208049=CARTESIAN_POINT('Ctrl Pts',(48.7530057377613,29.4168188138147,-228.339625726171));
#208050=CARTESIAN_POINT('Ctrl Pts',(48.8296829433926,29.3915172223634,-228.294286688015));
#208051=CARTESIAN_POINT('Ctrl Pts',(48.9465146046185,29.3668671949067,-228.215716813884));
#208052=CARTESIAN_POINT('Ctrl Pts',(49.0053847104949,29.3578670652606,-228.173791547594));
#208053=CARTESIAN_POINT('Ctrl Pts',(49.0748703494029,29.3532047319551,-228.120258160781));
#208054=CARTESIAN_POINT('Ctrl Pts',(49.1048232381759,29.3524592107239,-228.096325157259));
#208055=CARTESIAN_POINT('Ctrl Pts',(49.1248304708793,29.3522407306626,-228.080149794142));
#208056=CARTESIAN_POINT('Ctrl Pts',(49.1360275453979,29.3522905620935,-228.070980769437));
#208057=CARTESIAN_POINT('Ctrl Pts',(49.2158411714096,29.353636723251,-228.004953353353));
#208058=CARTESIAN_POINT('Ctrl Pts',(49.2851376328763,29.3618147939751,-227.942889930398));
#208059=CARTESIAN_POINT('Ctrl Pts',(49.3867128239049,29.3845233081293,-227.844736216309));
#208060=CARTESIAN_POINT('Ctrl Pts',(49.4369079545403,29.3984875351963,-227.794394714351));
#208061=CARTESIAN_POINT('Ctrl Pts',(49.4862331273773,29.4163574712173,-227.742156245023));
#208062=CARTESIAN_POINT('Ctrl Pts',(49.5189252866697,29.4291374288087,-227.706909050499));
#208063=CARTESIAN_POINT('Ctrl Pts',(49.5362231832806,29.4364311931001,-227.687904724522));
#208064=CARTESIAN_POINT('Ctrl Pts',(49.6721982976717,29.4975011599834,-227.53602800549));
#208065=CARTESIAN_POINT('Ctrl Pts',(49.7801088316737,29.572761994563,-227.397668277446));
#208066=CARTESIAN_POINT('Ctrl Pts',(49.8755750290351,29.6684593880862,-227.255950349386));
#208067=CARTESIAN_POINT('Ctrl Pts',(49.8755750290351,29.6684593880862,-227.255950349386));
#208068=CARTESIAN_POINT('Ctrl Pts',(49.566578371721,30.0125857112181,-227.280382264872));
#208069=CARTESIAN_POINT('Ctrl Pts',(49.8031531494471,30.2499539750196,-227.60005));
#208070=CARTESIAN_POINT('Ctrl Pts',(51.4695961402316,31.2663408349186,-224.889653425376));
#208071=CARTESIAN_POINT('Ctrl Pts',(51.160952124674,31.6123070902132,-224.911157102841));
#208072=CARTESIAN_POINT('Ctrl Pts',(51.3963758794861,31.8485204702035,-225.233951755693));
#208073=CARTESIAN_POINT('Ctrl Pts',(53.0649609053862,32.864644901729,-222.524371622939));
#208074=CARTESIAN_POINT('Ctrl Pts',(52.757248450643,33.2139574900831,-222.540616273922));
#208075=CARTESIAN_POINT('Ctrl Pts',(52.9904440332794,33.4479352247441,-222.868995945589));
#208076=CARTESIAN_POINT('Ctrl Pts',(54.6643562096698,34.4651804296883,-220.162900223157));
#208077=CARTESIAN_POINT('Ctrl Pts',(54.3487296401403,34.8107766034666,-220.183958003048));
#208078=CARTESIAN_POINT('Ctrl Pts',(54.5875190481085,35.0503669255136,-220.508112862707));
#208079=CARTESIAN_POINT('',(54.5875190481084,35.0503669255136,-220.508112862707));
#208080=CARTESIAN_POINT('',(54.6643562096698,34.4651804296884,-220.162900223157));
#208081=CARTESIAN_POINT('Origin',(54.9416638693848,34.6974059566189,-220.508112862707));
#208082=CARTESIAN_POINT('Ctrl Pts',(49.8755750290351,29.6684593880862,-227.255950349386));
#208083=CARTESIAN_POINT('Ctrl Pts',(51.5864044294278,31.383432005677,-224.716253529058));
#208084=CARTESIAN_POINT('Ctrl Pts',(53.1817714358015,32.9815387074691,-222.351903486981));
#208085=CARTESIAN_POINT('Ctrl Pts',(54.6643562096698,34.4651804296884,-220.162900223157));
#208086=CARTESIAN_POINT('Ctrl Pts',(54.5875190481084,35.0503669255136,-220.508112862707));
#208087=CARTESIAN_POINT('Ctrl Pts',(52.990443779671,33.4479349702851,-222.86899632084));
#208088=CARTESIAN_POINT('Ctrl Pts',(51.3963761190905,31.8485207106117,-225.233951400128));
#208089=CARTESIAN_POINT('Ctrl Pts',(49.8031531494471,30.2499539750197,-227.60005));
#208090=CARTESIAN_POINT('Ctrl Pts',(42.4431629103415,35.679860391633,-228.507034483728));
#208091=CARTESIAN_POINT('Ctrl Pts',(42.5405392130025,35.7913421132894,-228.35005));
#208092=CARTESIAN_POINT('Ctrl Pts',(42.6824807550636,35.9538445605081,-228.35005));
#208093=CARTESIAN_POINT('Ctrl Pts',(43.4842614434386,34.7712285271383,-228.506443516651));
#208094=CARTESIAN_POINT('Ctrl Pts',(43.5839578161182,34.8805832623425,-228.350049999846));
#208095=CARTESIAN_POINT('Ctrl Pts',(43.7299304472252,35.0389252651105,-228.35005));
#208096=CARTESIAN_POINT('Ctrl Pts',(44.4876418177359,33.826550002353,-228.506035020985));
#208097=CARTESIAN_POINT('Ctrl Pts',(44.590423195572,33.9329609873047,-228.350049999904));
#208098=CARTESIAN_POINT('Ctrl Pts',(44.7400658047431,34.0873590008399,-228.35005));
#208099=CARTESIAN_POINT('Ctrl Pts',(46.4180861418825,31.8610058543969,-228.505671567324));
#208100=CARTESIAN_POINT('Ctrl Pts',(46.5261142282933,31.9620046547715,-228.350050000096));
#208101=CARTESIAN_POINT('Ctrl Pts',(46.6832166107726,32.108381759188,-228.35005));
#208102=CARTESIAN_POINT('Ctrl Pts',(47.3461759565219,30.8411406013281,-228.505709331207));
#208103=CARTESIAN_POINT('Ctrl Pts',(47.4568224915956,30.9392657163356,-228.350050000173));
#208104=CARTESIAN_POINT('Ctrl Pts',(47.617275666974,31.0819979338032,-228.35005));
#208105=CARTESIAN_POINT('Ctrl Pts',(48.2384287873563,29.7860380279371,-228.505869818703));
#208106=CARTESIAN_POINT('Ctrl Pts',(48.3513278433713,29.8815330303712,-228.35005));
#208107=CARTESIAN_POINT('Ctrl Pts',(48.515339402069,30.020261242545,-228.35005));
#208108=CARTESIAN_POINT('',(42.4431629103415,35.679860391633,-228.507034483728));
#208109=CARTESIAN_POINT('',(42.6824807550636,35.9538445605081,-228.35005));
#208110=CARTESIAN_POINT('Origin',(42.6824807550636,35.9538445605081,-228.85005));
#208111=CARTESIAN_POINT('Ctrl Pts',(48.515339402069,30.020261242545,-228.35005));
#208112=CARTESIAN_POINT('Ctrl Pts',(47.6172684110892,31.0820065120798,-228.35005));
#208113=CARTESIAN_POINT('Ctrl Pts',(46.6832166107701,32.1083817591879,-228.35005));
#208114=CARTESIAN_POINT('Ctrl Pts',(45.7116412077571,33.0978703800133,-228.35005));
#208115=CARTESIAN_POINT('Ctrl Pts',(44.7400658047442,34.0873590008387,-228.35005));
#208116=CARTESIAN_POINT('Ctrl Pts',(43.7299213057923,35.0389332497409,-228.35005));
#208117=CARTESIAN_POINT('Ctrl Pts',(42.6824807550636,35.9538445605081,-228.35005));
#208118=CARTESIAN_POINT('Ctrl Pts',(42.4431629103415,35.679860391633,-228.507034483728));
#208119=CARTESIAN_POINT('Ctrl Pts',(42.783732660266,35.3826238505884,-228.5068411634));
#208120=CARTESIAN_POINT('Ctrl Pts',(43.1251178195728,35.0772901594386,-228.506664609947));
#208121=CARTESIAN_POINT('Ctrl Pts',(43.4664349615021,34.7639460185337,-228.506508376881));
#208122=CARTESIAN_POINT('Ctrl Pts',(43.7986630315905,34.4589460451426,-228.506356304208));
#208123=CARTESIAN_POINT('Ctrl Pts',(44.1308266151257,34.1463564072806,-228.506223487408));
#208124=CARTESIAN_POINT('Ctrl Pts',(44.4621498940903,33.8262865256091,-228.506113215303));
#208125=CARTESIAN_POINT('Ctrl Pts',(44.7934731730549,33.5062166439377,-228.506002943198));
#208126=CARTESIAN_POINT('Ctrl Pts',(45.1239551433519,33.1786670679477,-228.50591521934));
#208127=CARTESIAN_POINT('Ctrl Pts',(45.4528639798093,32.8437779283751,-228.505853294154));
#208128=CARTESIAN_POINT('Ctrl Pts',(45.7418215590338,32.5495664498336,-228.505798890776));
#208129=CARTESIAN_POINT('Ctrl Pts',(46.0296572151249,32.2497783732728,-228.505763776886));
#208130=CARTESIAN_POINT('Ctrl Pts',(46.3158895995213,31.9447181809263,-228.505746122221));
#208131=CARTESIAN_POINT('Ctrl Pts',(46.6021152411152,31.6396651749107,-228.505728467972));
#208132=CARTESIAN_POINT('Ctrl Pts',(46.8867376705897,31.3293403107133,-228.505728268231));
#208133=CARTESIAN_POINT('Ctrl Pts',(47.1693119506508,31.0140854067816,-228.505743316248));
#208134=CARTESIAN_POINT('Ctrl Pts',(47.4524717478086,30.6981772688189,-228.505758395446));
#208135=CARTESIAN_POINT('Ctrl Pts',(47.7335748895764,30.3773186565972,-228.505788781456));
#208136=CARTESIAN_POINT('Ctrl Pts',(48.0122104039763,30.0518908485059,-228.505831936305));
#208137=CARTESIAN_POINT('Ctrl Pts',(48.0878005118504,29.9636066139142,-228.505843643641));
#208138=CARTESIAN_POINT('Ctrl Pts',(48.1632092196792,29.8749863133239,-228.505856289123));
#208139=CARTESIAN_POINT('Ctrl Pts',(48.2384287873563,29.7860380279371,-228.505869818703));
#208140=CARTESIAN_POINT('Ctrl Pts',(54.9968660030027,36.3988348033229,-218.849954951747));
#208141=CARTESIAN_POINT('Ctrl Pts',(55.018269151756,36.2900558272771,-218.637811171833));
#208142=CARTESIAN_POINT('Ctrl Pts',(55.2146353748417,36.257836765148,-218.504776656654));
#208143=CARTESIAN_POINT('Ctrl Pts',(55.052102137237,36.1181036738987,-219.049315831028));
#208144=CARTESIAN_POINT('Ctrl Pts',(55.0614326261139,35.9588010119692,-218.832425369541));
#208145=CARTESIAN_POINT('Ctrl Pts',(55.2870795674735,35.8851781565784,-218.70395400533));
#208146=CARTESIAN_POINT('Ctrl Pts',(55.0225064544189,35.8553343499292,-219.318743015247));
#208147=CARTESIAN_POINT('Ctrl Pts',(54.9920018852822,35.6566773356544,-219.093930954085));
#208148=CARTESIAN_POINT('Ctrl Pts',(55.2466620625239,35.5359310914396,-218.973388048174));
#208149=CARTESIAN_POINT('Ctrl Pts',(54.8701701172632,35.4039199531589,-219.888552047874));
#208150=CARTESIAN_POINT('Ctrl Pts',(54.7478058041725,35.1574653296587,-219.629072060686));
#208151=CARTESIAN_POINT('Ctrl Pts',(55.04206217923,34.9357811050907,-219.543206859615));
#208152=CARTESIAN_POINT('Ctrl Pts',(54.745550854066,35.2089287796815,-220.196631257494));
#208153=CARTESIAN_POINT('Ctrl Pts',(54.5592271140423,34.9538518370357,-219.918109540734));
#208154=CARTESIAN_POINT('Ctrl Pts',(54.8753705653342,34.6763452196017,-219.851342245783));
#208155=CARTESIAN_POINT('Ctrl Pts',(54.5875190481085,35.0503669255137,-220.508112862707));
#208156=CARTESIAN_POINT('Ctrl Pts',(54.3487296401403,34.8107766034666,-220.183958003048));
#208157=CARTESIAN_POINT('Ctrl Pts',(54.6643562096698,34.4651804296883,-220.162900223157));
#208158=CARTESIAN_POINT('',(54.9968660030035,36.3988348033192,-218.84995495175));
#208159=CARTESIAN_POINT('',(55.2146353748417,36.257836765148,-218.504776656654));
#208160=CARTESIAN_POINT('Origin',(55.4874598092474,36.4953631270242,-218.849954951747));
#208161=CARTESIAN_POINT('Ctrl Pts',(54.6643562096698,34.4651804296883,-220.162900223157));
#208162=CARTESIAN_POINT('Ctrl Pts',(54.7074039308287,34.508258839999,-220.099341225512));
#208163=CARTESIAN_POINT('Ctrl Pts',(54.7480314614451,34.5527651846987,-220.036777704785));
#208164=CARTESIAN_POINT('Ctrl Pts',(54.7863060742582,34.5985925935165,-219.975215224127));
#208165=CARTESIAN_POINT('Ctrl Pts',(54.8273110867564,34.6476891965443,-219.909261054947));
#208166=CARTESIAN_POINT('Ctrl Pts',(54.8656162789774,34.69830187121,-219.844455384552));
#208167=CARTESIAN_POINT('Ctrl Pts',(54.9012839494488,34.7503560715278,-219.780785198212));
#208168=CARTESIAN_POINT('Ctrl Pts',(54.9313207276235,34.7941924210102,-219.727166690522));
#208169=CARTESIAN_POINT('Ctrl Pts',(54.959488169708,34.8390547171882,-219.674350124633));
#208170=CARTESIAN_POINT('Ctrl Pts',(54.9858017155598,34.8849169151779,-219.622333509997));
#208171=CARTESIAN_POINT('Ctrl Pts',(55.0178834325347,34.9408325285293,-219.558914375301));
#208172=CARTESIAN_POINT('Ctrl Pts',(55.0472095907453,34.998232325381,-219.496685631604));
#208173=CARTESIAN_POINT('Ctrl Pts',(55.0737733419852,35.0570995269978,-219.435651937387));
#208174=CARTESIAN_POINT('Ctrl Pts',(55.0959985739645,35.1063522549011,-219.384586558846));
#208175=CARTESIAN_POINT('Ctrl Pts',(55.1162888777561,35.1566323285765,-219.334358625518));
#208176=CARTESIAN_POINT('Ctrl Pts',(55.1346165986468,35.2079360988119,-219.284985901448));
#208177=CARTESIAN_POINT('Ctrl Pts',(55.1370365296852,35.2147100772414,-219.278466891903));
#208178=CARTESIAN_POINT('Ctrl Pts',(55.1392598915153,35.221036410009,-219.272407652944));
#208179=CARTESIAN_POINT('Ctrl Pts',(55.1416546709122,35.2279680296668,-219.265801317888));
#208180=CARTESIAN_POINT('Ctrl Pts',(55.1424346005327,35.2302255133815,-219.263649772573));
#208181=CARTESIAN_POINT('Ctrl Pts',(55.1432323949011,35.2325473997641,-219.261440311746));
#208182=CARTESIAN_POINT('Ctrl Pts',(55.1440597796072,35.2349706839286,-219.259138509777));
#208183=CARTESIAN_POINT('Ctrl Pts',(55.1441605630477,35.2352658633217,-219.258858128087));
#208184=CARTESIAN_POINT('Ctrl Pts',(55.1442612725152,35.2355610486931,-219.25857780077));
#208185=CARTESIAN_POINT('Ctrl Pts',(55.1443619080441,35.2358562400493,-219.258297527793));
#208186=CARTESIAN_POINT('Ctrl Pts',(55.1603383653164,35.2827195311766,-219.213802613465));
#208187=CARTESIAN_POINT('Ctrl Pts',(55.1745132525297,35.3299375330594,-219.170490352343));
#208188=CARTESIAN_POINT('Ctrl Pts',(55.1868961950868,35.377471738341,-219.128368907279));
#208189=CARTESIAN_POINT('Ctrl Pts',(55.1952874349737,35.4096830578649,-219.099825517992));
#208190=CARTESIAN_POINT('Ctrl Pts',(55.2028557096548,35.4420407056901,-219.071828315238));
#208191=CARTESIAN_POINT('Ctrl Pts',(55.2096002183572,35.4745446654207,-219.044375123623));
#208192=CARTESIAN_POINT('Ctrl Pts',(55.2179802508663,35.5149307411503,-219.010264612634));
#208193=CARTESIAN_POINT('Ctrl Pts',(55.2250915055409,35.5555371343618,-218.976995360291));
#208194=CARTESIAN_POINT('Ctrl Pts',(55.2309378807329,35.5963523838428,-218.944567088419));
#208195=CARTESIAN_POINT('Ctrl Pts',(55.233861068329,35.6167600085833,-218.928352952483));
#208196=CARTESIAN_POINT('Ctrl Pts',(55.2364680386656,35.6372198496141,-218.91234906497));
#208197=CARTESIAN_POINT('Ctrl Pts',(55.2387592664335,35.6577305151278,-218.896555409356));
#208198=CARTESIAN_POINT('Ctrl Pts',(55.2399048803175,35.6679858478847,-218.888658581548));
#208199=CARTESIAN_POINT('Ctrl Pts',(55.2409715586851,35.678253886869,-218.880814311874));
#208200=CARTESIAN_POINT('Ctrl Pts',(55.241959358827,35.688534461645,-218.873022599437));
#208201=CARTESIAN_POINT('Ctrl Pts',(55.2426458899188,35.6956795651188,-218.867607280467));
#208202=CARTESIAN_POINT('Ctrl Pts',(55.2432514894495,35.7023487309182,-218.862579958581));
#208203=CARTESIAN_POINT('Ctrl Pts',(55.2438669137039,35.7095462696188,-218.8571838814));
#208204=CARTESIAN_POINT('Ctrl Pts',(55.2441369790844,35.7127047509656,-218.854815931767));
#208205=CARTESIAN_POINT('Ctrl Pts',(55.2444084132222,35.7159652044752,-218.852377223766));
#208206=CARTESIAN_POINT('Ctrl Pts',(55.2446861814473,35.7194136243086,-218.849805133612));
#208207=CARTESIAN_POINT('Ctrl Pts',(55.2483291642508,35.7646403025828,-218.816071684817));
#208208=CARTESIAN_POINT('Ctrl Pts',(55.2504339246697,35.8097873894187,-218.783583104913));
#208209=CARTESIAN_POINT('Ctrl Pts',(55.2510014461176,35.8548473662421,-218.752339591324));
#208210=CARTESIAN_POINT('Ctrl Pts',(55.251799183524,35.9181859927769,-218.708422097834));
#208211=CARTESIAN_POINT('Ctrl Pts',(55.2495512973704,35.9813642859329,-218.666963136053));
#208212=CARTESIAN_POINT('Ctrl Pts',(55.2442764911647,36.0443389392307,-218.627967205458));
#208213=CARTESIAN_POINT('Ctrl Pts',(55.2389089241922,36.1084210412002,-218.588285507031));
#208214=CARTESIAN_POINT('Ctrl Pts',(55.2304080556554,36.1722930120072,-218.551152986505));
#208215=CARTESIAN_POINT('Ctrl Pts',(55.2187640677965,36.2359515925339,-218.516569914905));
#208216=CARTESIAN_POINT('Ctrl Pts',(55.2174292017159,36.2432494084467,-218.512605313619));
#208217=CARTESIAN_POINT('Ctrl Pts',(55.2160529867808,36.2505444581524,-218.508674224936));
#208218=CARTESIAN_POINT('Ctrl Pts',(55.2146353748417,36.257836765148,-218.504776656654));
#208219=CARTESIAN_POINT('Ctrl Pts',(54.9968660030034,36.3988348033192,-218.84995495175));
#208220=CARTESIAN_POINT('Ctrl Pts',(55.0040920464924,36.362109290608,-218.876035526304));
#208221=CARTESIAN_POINT('Ctrl Pts',(55.0100902040703,36.3245420184541,-218.904133384402));
#208222=CARTESIAN_POINT('Ctrl Pts',(55.0146816372595,36.2862590986273,-218.934320638599));
#208223=CARTESIAN_POINT('Ctrl Pts',(55.0175341077067,36.26247547967,-218.953074750208));
#208224=CARTESIAN_POINT('Ctrl Pts',(55.0198440529379,36.2384160209788,-218.972634555083));
#208225=CARTESIAN_POINT('Ctrl Pts',(55.0215733928243,36.2141149072774,-218.99300918415));
#208226=CARTESIAN_POINT('Ctrl Pts',(55.0248772919048,36.1676876966138,-219.031934856756));
#208227=CARTESIAN_POINT('Ctrl Pts',(55.0260595476318,36.1203762301498,-219.073838887151));
#208228=CARTESIAN_POINT('Ctrl Pts',(55.0248935219138,36.0724066660917,-219.118759345035));
#208229=CARTESIAN_POINT('Ctrl Pts',(55.0240041749923,36.0358194935617,-219.153020914324));
#208230=CARTESIAN_POINT('Ctrl Pts',(55.0217494012894,35.9988459801408,-219.189039842437));
#208231=CARTESIAN_POINT('Ctrl Pts',(55.0180465606492,35.961603893522,-219.226800636546));
#208232=CARTESIAN_POINT('Ctrl Pts',(55.0143234843304,35.9241582823743,-219.264767789873));
#208233=CARTESIAN_POINT('Ctrl Pts',(55.0091362504138,35.8864343633192,-219.304502287204));
#208234=CARTESIAN_POINT('Ctrl Pts',(55.0024125558477,35.8485468343893,-219.345982968744));
#208235=CARTESIAN_POINT('Ctrl Pts',(54.9959666612172,35.8122246878533,-219.385749811182));
#208236=CARTESIAN_POINT('Ctrl Pts',(54.9881101007026,35.7757565885262,-219.427115973757));
#208237=CARTESIAN_POINT('Ctrl Pts',(54.978783579186,35.7392359043793,-219.47006753094));
#208238=CARTESIAN_POINT('Ctrl Pts',(54.9737864840352,35.7196683374868,-219.493080721627));
#208239=CARTESIAN_POINT('Ctrl Pts',(54.9683676566711,35.700086635794,-219.516547938461));
#208240=CARTESIAN_POINT('Ctrl Pts',(54.962518087953,35.6805061616403,-219.540466343658));
#208241=CARTESIAN_POINT('Ctrl Pts',(54.9584722404756,35.6669633492073,-219.557009481108));
#208242=CARTESIAN_POINT('Ctrl Pts',(54.9542204118081,35.6534213830759,-219.573768146966));
#208243=CARTESIAN_POINT('Ctrl Pts',(54.9497594430271,35.6398852506478,-219.590741752706));
#208244=CARTESIAN_POINT('Ctrl Pts',(54.9486324135337,35.6364654507742,-219.595030003806));
#208245=CARTESIAN_POINT('Ctrl Pts',(54.9474919474504,35.6330457676747,-219.599332298452));
#208246=CARTESIAN_POINT('Ctrl Pts',(54.9463382858411,35.629627151544,-219.60364753156));
#208247=CARTESIAN_POINT('Ctrl Pts',(54.9461922858206,35.6291945133935,-219.60419363981));
#208248=CARTESIAN_POINT('Ctrl Pts',(54.9460460675899,35.6287618689978,-219.604739983546));
#208249=CARTESIAN_POINT('Ctrl Pts',(54.9458996314877,35.6283292201355,-219.605286560807));
#208250=CARTESIAN_POINT('Ctrl Pts',(54.9457655873106,35.6279331835038,-219.605786884826));
#208251=CARTESIAN_POINT('Ctrl Pts',(54.945631966464,35.6275389212305,-219.606285153914));
#208252=CARTESIAN_POINT('Ctrl Pts',(54.9454942839764,35.6271332403158,-219.606798055818));
#208253=CARTESIAN_POINT('Ctrl Pts',(54.9447134539827,35.6248325277747,-219.609706843985));
#208254=CARTESIAN_POINT('Ctrl Pts',(54.9438343666549,35.6222630584633,-219.612962841538));
#208255=CARTESIAN_POINT('Ctrl Pts',(54.9430286280765,35.6199273297219,-219.615929620851));
#208256=CARTESIAN_POINT('Ctrl Pts',(54.9426383484526,35.6187959611129,-219.617366654581));
#208257=CARTESIAN_POINT('Ctrl Pts',(54.9422654235513,35.6177193398141,-219.618735762759));
#208258=CARTESIAN_POINT('Ctrl Pts',(54.9419300749024,35.6167541113451,-219.619964278477));
#208259=CARTESIAN_POINT('Ctrl Pts',(54.941747008926,35.6162271955734,-219.62063492209));
#208260=CARTESIAN_POINT('Ctrl Pts',(54.941575148176,35.6157334705899,-219.621263665118));
#208261=CARTESIAN_POINT('Ctrl Pts',(54.9414178205515,35.6152821267846,-219.621838668181));
#208262=CARTESIAN_POINT('Ctrl Pts',(54.9413537204437,35.6150982354517,-219.622072942094));
#208263=CARTESIAN_POINT('Ctrl Pts',(54.9412924648862,35.6149226137709,-219.622296720729));
#208264=CARTESIAN_POINT('Ctrl Pts',(54.9412304034246,35.6147447846829,-219.622523349969));
#208265=CARTESIAN_POINT('Ctrl Pts',(54.9281435230044,35.5772460221848,-219.670312584787));
#208266=CARTESIAN_POINT('Ctrl Pts',(54.9131804711756,35.5390861037303,-219.720677924238));
#208267=CARTESIAN_POINT('Ctrl Pts',(54.8960963824159,35.500529589748,-219.773644865139));
#208268=CARTESIAN_POINT('Ctrl Pts',(54.8905118862791,35.4879261254128,-219.790958851328));
#208269=CARTESIAN_POINT('Ctrl Pts',(54.8847008768019,35.4752805096263,-219.808550513932));
#208270=CARTESIAN_POINT('Ctrl Pts',(54.8786552093599,35.4626026527875,-219.826419782291));
#208271=CARTESIAN_POINT('Ctrl Pts',(54.8663596694719,35.4368187181017,-219.862761890748));
#208272=CARTESIAN_POINT('Ctrl Pts',(54.8530933057166,35.410900869322,-219.900253099045));
#208273=CARTESIAN_POINT('Ctrl Pts',(54.8387867552026,35.3849304106352,-219.938883517151));
#208274=CARTESIAN_POINT('Ctrl Pts',(54.8316334799456,35.3719451812918,-219.958198726204));
#208275=CARTESIAN_POINT('Ctrl Pts',(54.8242199501464,35.3589465132715,-219.977798384425));
#208276=CARTESIAN_POINT('Ctrl Pts',(54.8165395696195,35.3459480790558,-219.997684076851));
#208277=CARTESIAN_POINT('Ctrl Pts',(54.8126993793561,35.339448861948,-220.007626923063));
#208278=CARTESIAN_POINT('Ctrl Pts',(54.8087924839424,35.3329497025708,-220.01764127887));
#208279=CARTESIAN_POINT('Ctrl Pts',(54.8048180095845,35.3264521669541,-220.027727144102));
#208280=CARTESIAN_POINT('Ctrl Pts',(54.8028307724055,35.3232033991458,-220.032770076718));
#208281=CARTESIAN_POINT('Ctrl Pts',(54.800826640669,35.3199550371977,-220.037830886689));
#208282=CARTESIAN_POINT('Ctrl Pts',(54.7988055087113,35.3167072803064,-220.042909573995));
#208283=CARTESIAN_POINT('Ctrl Pts',(54.797056869173,35.3138973914768,-220.047303544113));
#208284=CARTESIAN_POINT('Ctrl Pts',(54.7948825822304,35.310433149772,-220.052740770874));
#208285=CARTESIAN_POINT('Ctrl Pts',(54.7933541298033,35.3080144248348,-220.056548243653));
#208286=CARTESIAN_POINT('Ctrl Pts',(54.7931159493833,35.3076375122719,-220.057141566317));
#208287=CARTESIAN_POINT('Ctrl Pts',(54.7928935324271,35.307285921985,-220.0576952873));
#208288=CARTESIAN_POINT('Ctrl Pts',(54.7926910080452,35.3069660248027,-220.058199267894));
#208289=CARTESIAN_POINT('Ctrl Pts',(54.7778673199726,35.2835512833232,-220.095087918257));
#208290=CARTESIAN_POINT('Ctrl Pts',(54.761373636425,35.2589411193526,-220.134834364075));
#208291=CARTESIAN_POINT('Ctrl Pts',(54.7429690732774,35.2333793116411,-220.177477225497));
#208292=CARTESIAN_POINT('Ctrl Pts',(54.7251831383047,35.2086767068525,-220.218686742626));
#208293=CARTESIAN_POINT('Ctrl Pts',(54.7056120315136,35.1830853552272,-220.262601832834));
#208294=CARTESIAN_POINT('Ctrl Pts',(54.6840331800314,35.1568641348512,-220.30923021939));
#208295=CARTESIAN_POINT('Ctrl Pts',(54.6636061794762,35.1320425689946,-220.353369643532));
#208296=CARTESIAN_POINT('Ctrl Pts',(54.6413795825545,35.1066567034407,-220.399940802683));
#208297=CARTESIAN_POINT('Ctrl Pts',(54.6171673998294,35.0809605126591,-220.448918846524));
#208298=CARTESIAN_POINT('Ctrl Pts',(54.6075983865104,35.0708049973705,-220.468275695065));
#208299=CARTESIAN_POINT('Ctrl Pts',(54.5977193044027,35.0606013940828,-220.48800809843));
#208300=CARTESIAN_POINT('Ctrl Pts',(54.5875190481085,35.0503669255137,-220.508112862707));
#208301=CARTESIAN_POINT('Ctrl Pts',(42.6824807550636,35.9538445605081,-228.35005));
#208302=CARTESIAN_POINT('Ctrl Pts',(42.5404167002247,35.791201853955,-228.35005));
#208303=CARTESIAN_POINT('Ctrl Pts',(42.443021269923,35.6796982339285,-228.50726297195));
#208304=CARTESIAN_POINT('Ctrl Pts',(42.5913145600393,36.0267272443623,-228.35005));
#208305=CARTESIAN_POINT('Ctrl Pts',(42.4282834326699,35.8863211720346,-228.352241313908));
#208306=CARTESIAN_POINT('Ctrl Pts',(42.2979928747684,35.806276985376,-228.507342686565));
#208307=CARTESIAN_POINT('Ctrl Pts',(42.5313139073579,36.1299188273931,-228.321794566394));
#208308=CARTESIAN_POINT('Ctrl Pts',(42.3443085102026,36.0112714706978,-228.310299465652));
#208309=CARTESIAN_POINT('Ctrl Pts',(42.1843277826865,35.9629604673028,-228.460330590341));
#208310=CARTESIAN_POINT('Ctrl Pts',(42.4814079540288,36.3579978037835,-228.225751005231));
#208311=CARTESIAN_POINT('Ctrl Pts',(42.2569704879925,36.2630116503163,-228.16819510465));
#208312=CARTESIAN_POINT('Ctrl Pts',(42.0432088071097,36.2819979616018,-228.300386998121));
#208313=CARTESIAN_POINT('Ctrl Pts',(42.4898483164371,36.4810484712422,-228.159605024773));
#208314=CARTESIAN_POINT('Ctrl Pts',(42.2522549527837,36.3904916192652,-228.068484337662));
#208315=CARTESIAN_POINT('Ctrl Pts',(42.0140892672452,36.4425131983365,-228.190195527837));
#208316=CARTESIAN_POINT('Ctrl Pts',(42.5520089174244,36.7203516154467,-228.012906367619));
#208317=CARTESIAN_POINT('Ctrl Pts',(42.2976224084343,36.6185146335635,-227.852954061751));
#208318=CARTESIAN_POINT('Ctrl Pts',(42.0182756482514,36.7396699246603,-227.945762342978));
#208319=CARTESIAN_POINT('Ctrl Pts',(42.6046949644287,36.835724973434,-227.933213206321));
#208320=CARTESIAN_POINT('Ctrl Pts',(42.3488315361518,36.7193728341531,-227.736107069137));
#208321=CARTESIAN_POINT('Ctrl Pts',(42.0504918440331,36.8754822200752,-227.812957113271));
#208322=CARTESIAN_POINT('Ctrl Pts',(42.7406007705538,37.0550530398967,-227.767956190477));
#208323=CARTESIAN_POINT('Ctrl Pts',(42.4877694298107,36.8912905811231,-227.501601704626));
#208324=CARTESIAN_POINT('Ctrl Pts',(42.1592600405123,37.1219402239383,-227.537528223444));
#208325=CARTESIAN_POINT('Ctrl Pts',(42.8221296650751,37.1564022812852,-227.68437936815));
#208326=CARTESIAN_POINT('Ctrl Pts',(42.5766199121254,36.9595585654922,-227.385429649693));
#208327=CARTESIAN_POINT('Ctrl Pts',(42.2344115671227,37.22968036859,-227.398223401081));
#208328=CARTESIAN_POINT('Ctrl Pts',(42.9157357330403,37.2503223096489,-227.60005));
#208329=CARTESIAN_POINT('Ctrl Pts',(42.6749497694503,37.0087287354121,-227.278243940858));
#208330=CARTESIAN_POINT('Ctrl Pts',(42.3280651351011,37.3236108350448,-227.257633534302));
#208331=CARTESIAN_POINT('',(42.3284659498332,37.323247286775,-227.257657541791));
#208332=CARTESIAN_POINT('',(42.9157357330403,37.2503223096489,-227.60005));
#208333=CARTESIAN_POINT('Origin',(42.561590911764,37.6032832785437,-227.60005));
#208334=CARTESIAN_POINT('Ctrl Pts',(42.6824807550636,35.9538445605081,-228.35005));
#208335=CARTESIAN_POINT('Ctrl Pts',(42.6316328790924,35.9944948069838,-228.35005));
#208336=CARTESIAN_POINT('Ctrl Pts',(42.5896593585113,36.0448083850312,-228.34162603267));
#208337=CARTESIAN_POINT('Ctrl Pts',(42.5424025219209,36.1323898340594,-228.316179318494));
#208338=CARTESIAN_POINT('Ctrl Pts',(42.5292691936361,36.1636004599124,-228.305571179723));
#208339=CARTESIAN_POINT('Ctrl Pts',(42.5138046839852,36.2131355824937,-228.286535124351));
#208340=CARTESIAN_POINT('Ctrl Pts',(42.5071313240516,36.2385829156178,-228.276237069799));
#208341=CARTESIAN_POINT('Ctrl Pts',(42.5012657853535,36.2693943137178,-228.262881841837));
#208342=CARTESIAN_POINT('Ctrl Pts',(42.4991705525361,36.2828327009754,-228.256874092392));
#208343=CARTESIAN_POINT('Ctrl Pts',(42.4978675356399,36.2918427283243,-228.252806174876));
#208344=CARTESIAN_POINT('Ctrl Pts',(42.4971073002351,36.2976454866849,-228.250155383563));
#208345=CARTESIAN_POINT('Ctrl Pts',(42.4902787436054,36.3534654942239,-228.224467376528));
#208346=CARTESIAN_POINT('Ctrl Pts',(42.4900043444909,36.4104109333233,-228.195635420535));
#208347=CARTESIAN_POINT('Ctrl Pts',(42.500106112153,36.5011621787222,-228.145358810264));
#208348=CARTESIAN_POINT('Ctrl Pts',(42.5052272864443,36.5322997566167,-228.127432972543));
#208349=CARTESIAN_POINT('Ctrl Pts',(42.5157127222045,36.5801646485169,-228.098833017281));
#208350=CARTESIAN_POINT('Ctrl Pts',(42.5216564611549,36.6043866235847,-228.08410574718));
#208351=CARTESIAN_POINT('Ctrl Pts',(42.5298562807234,36.6331137291362,-228.066190354362));
#208352=CARTESIAN_POINT('Ctrl Pts',(42.5336458407521,36.6455214921606,-228.058357028594));
#208353=CARTESIAN_POINT('Ctrl Pts',(42.5362338683169,36.6538142366302,-228.053100521665));
#208354=CARTESIAN_POINT('Ctrl Pts',(42.537938728552,36.6591389606888,-228.049708921276));
#208355=CARTESIAN_POINT('Ctrl Pts',(42.5545287108761,36.7101243781582,-228.017133053639));
#208356=CARTESIAN_POINT('Ctrl Pts',(42.5747596787098,36.7609669156392,-227.98326264424));
#208357=CARTESIAN_POINT('Ctrl Pts',(42.6131000308354,36.8404500872112,-227.927602813803));
#208358=CARTESIAN_POINT('Ctrl Pts',(42.6272141217683,36.8674793873369,-227.908244075784));
#208359=CARTESIAN_POINT('Ctrl Pts',(42.6505325971428,36.9086798126113,-227.878030386003));
#208360=CARTESIAN_POINT('Ctrl Pts',(42.6627287854389,36.929444028542,-227.862630076912));
#208361=CARTESIAN_POINT('Ctrl Pts',(42.6779304132337,36.9539229855824,-227.844161463063));
#208362=CARTESIAN_POINT('Ctrl Pts',(42.6846574393355,36.9644648178459,-227.836140473796));
#208363=CARTESIAN_POINT('Ctrl Pts',(42.6891896446285,36.9715036068993,-227.830769810322));
#208364=CARTESIAN_POINT('Ctrl Pts',(42.6922398709184,36.9761885029208,-227.827182725376));
#208365=CARTESIAN_POINT('Ctrl Pts',(42.7435040992353,37.0543999679727,-227.767172645826));
#208366=CARTESIAN_POINT('Ctrl Pts',(42.8141078943411,37.1483536050482,-227.691606152183));
#208367=CARTESIAN_POINT('Ctrl Pts',(42.9157357330403,37.2503223096489,-227.60005));
#208368=CARTESIAN_POINT('Ctrl Pts',(42.3284659498332,37.323247286775,-227.257657541791));
#208369=CARTESIAN_POINT('Ctrl Pts',(42.2811180628148,37.2757753423908,-227.328721687048));
#208370=CARTESIAN_POINT('Ctrl Pts',(42.2176885536698,37.1997647460476,-227.434077804087));
#208371=CARTESIAN_POINT('Ctrl Pts',(42.1571641943227,37.102490126336,-227.554823097481));
#208372=CARTESIAN_POINT('Ctrl Pts',(42.1341311988921,37.0589366221338,-227.606106042546));
#208373=CARTESIAN_POINT('Ctrl Pts',(42.1194236021323,37.0294840880552,-227.640191330852));
#208374=CARTESIAN_POINT('Ctrl Pts',(42.1128271528602,37.015528461262,-227.656087200987));
#208375=CARTESIAN_POINT('Ctrl Pts',(42.0771342094186,36.9349109661749,-227.746259228812));
#208376=CARTESIAN_POINT('Ctrl Pts',(42.0554154181983,36.8688204128193,-227.815014008253));
#208377=CARTESIAN_POINT('Ctrl Pts',(42.0331267124034,36.767193592861,-227.913071913187));
#208378=CARTESIAN_POINT('Ctrl Pts',(42.0245542841569,36.7157574583335,-227.960832299597));
#208379=CARTESIAN_POINT('Ctrl Pts',(42.0190571196657,36.6546381121702,-228.01433275981));
#208380=CARTESIAN_POINT('Ctrl Pts',(42.0176663611937,36.6282039350124,-228.036785816201));
#208381=CARTESIAN_POINT('Ctrl Pts',(42.0169536651772,36.6105275347935,-228.051648806624));
#208382=CARTESIAN_POINT('Ctrl Pts',(42.0167229576871,36.6028158122403,-228.058077290188));
#208383=CARTESIAN_POINT('Ctrl Pts',(42.0152804436434,36.5124088085728,-228.132560715103));
#208384=CARTESIAN_POINT('Ctrl Pts',(42.0227620917502,36.4331676079849,-228.191748775822));
#208385=CARTESIAN_POINT('Ctrl Pts',(42.0470046923612,36.3159899802422,-228.270001724761));
#208386=CARTESIAN_POINT('Ctrl Pts',(42.0623804322714,36.2578224973236,-228.306495913695));
#208387=CARTESIAN_POINT('Ctrl Pts',(42.0826088707734,36.2002903559472,-228.339041674326));
#208388=CARTESIAN_POINT('Ctrl Pts',(42.0971692804965,36.1620773525,-228.359861419569));
#208389=CARTESIAN_POINT('Ctrl Pts',(42.1043788617509,36.1444221549774,-228.369138705036));
#208390=CARTESIAN_POINT('Ctrl Pts',(42.1312624500863,36.0833875270383,-228.399817656059));
#208391=CARTESIAN_POINT('Ctrl Pts',(42.1516074709484,36.0435243978327,-228.41787768135));
#208392=CARTESIAN_POINT('Ctrl Pts',(42.1970961458717,35.9654732242671,-228.449212514483));
#208393=CARTESIAN_POINT('Ctrl Pts',(42.2213297257763,35.9285200210562,-228.46212743063));
#208394=CARTESIAN_POINT('Ctrl Pts',(42.3066148061692,35.8127999962566,-228.495853703076));
#208395=CARTESIAN_POINT('Ctrl Pts',(42.3711567239947,35.7427046981823,-228.50707535717));
#208396=CARTESIAN_POINT('Ctrl Pts',(42.4431629103415,35.679860391633,-228.507034483728));
#208397=CARTESIAN_POINT('Origin',(55.4874598092496,36.4953631270247,-218.849954951747));
#208398=CARTESIAN_POINT('',(55.4814981831708,36.4969369346298,-218.349992971048));
#208399=CARTESIAN_POINT('Origin',(55.4874598092437,36.4953631270311,-218.849954951747));
#208400=CARTESIAN_POINT('Origin',(55.4874598092496,36.4953631270247,-218.849954951747));
#208401=CARTESIAN_POINT('Ctrl Pts',(47.045128487469,42.0562187287015,-220.184138377616));
#208402=CARTESIAN_POINT('Ctrl Pts',(47.3919300806126,41.7415300830818,-220.204915325333));
#208403=CARTESIAN_POINT('Ctrl Pts',(47.632114758242,41.9825203546087,-220.52735443572));
#208404=CARTESIAN_POINT('Ctrl Pts',(45.4710211549778,40.4746337203406,-222.538908637374));
#208405=CARTESIAN_POINT('Ctrl Pts',(45.8197306764781,40.1640574272761,-222.557165671255));
#208406=CARTESIAN_POINT('Ctrl Pts',(46.0573262334548,40.4024498941129,-222.881354490551));
#208407=CARTESIAN_POINT('Ctrl Pts',(43.9001479472544,38.8990472866343,-224.898729936232));
#208408=CARTESIAN_POINT('Ctrl Pts',(44.2455143968232,38.5845611308926,-224.921907632466));
#208409=CARTESIAN_POINT('Ctrl Pts',(44.4868142732993,38.8266703421046,-225.241085046204));
#208410=CARTESIAN_POINT('Ctrl Pts',(42.3284659498332,37.3232472867751,-227.257657541791));
#208411=CARTESIAN_POINT('Ctrl Pts',(42.6752110219232,37.0089908641416,-227.278593100034));
#208412=CARTESIAN_POINT('Ctrl Pts',(42.9157357330403,37.2503223096489,-227.60005));
#208413=CARTESIAN_POINT('',(47.045128487469,42.0562187287015,-220.184138377616));
#208414=CARTESIAN_POINT('',(47.632114758242,41.9825203546087,-220.52735443572));
#208415=CARTESIAN_POINT('Origin',(47.2779699369656,42.3354813235036,-220.52735443572));
#208416=CARTESIAN_POINT('Ctrl Pts',(42.9157357330403,37.2503223096489,-227.60005));
#208417=CARTESIAN_POINT('Ctrl Pts',(44.486815106976,38.8266711785776,-225.241083793951));
#208418=CARTESIAN_POINT('Ctrl Pts',(46.0573252848254,40.4024489423018,-222.881355908373));
#208419=CARTESIAN_POINT('Ctrl Pts',(47.632114758242,41.9825203546087,-220.52735443572));
#208420=CARTESIAN_POINT('Ctrl Pts',(47.045128487469,42.0562187287015,-220.184138377616));
#208421=CARTESIAN_POINT('Ctrl Pts',(46.6671603770723,41.6764551098387,-220.74955602554));
#208422=CARTESIAN_POINT('Ctrl Pts',(46.2816417972639,41.2893651286945,-221.326854599969));
#208423=CARTESIAN_POINT('Ctrl Pts',(45.6919698908576,40.6973563649584,-222.210623851371));
#208424=CARTESIAN_POINT('Ctrl Pts',(45.4935115980833,40.4981264890257,-222.508183833464));
#208425=CARTESIAN_POINT('Ctrl Pts',(45.1929349926702,40.1964208373708,-222.958979154044));
#208426=CARTESIAN_POINT('Ctrl Pts',(45.0419240224792,40.0448531632896,-223.185490651193));
#208427=CARTESIAN_POINT('Ctrl Pts',(44.8644692412467,39.8667714265379,-223.451703279039));
#208428=CARTESIAN_POINT('Ctrl Pts',(44.775421562876,39.7774172976856,-223.585296896588));
#208429=CARTESIAN_POINT('Ctrl Pts',(44.7371894799003,39.7390555405282,-223.642655726315));
#208430=CARTESIAN_POINT('Ctrl Pts',(44.7116861193944,39.713466117932,-223.680918151067));
#208431=CARTESIAN_POINT('Ctrl Pts',(44.6978670848006,39.6996007071365,-223.701650844387));
#208432=CARTESIAN_POINT('Ctrl Pts',(43.9368930555956,38.9360854584715,-224.843345868572));
#208433=CARTESIAN_POINT('Ctrl Pts',(43.1511964037071,38.1481333969899,-226.022826588096));
#208434=CARTESIAN_POINT('Ctrl Pts',(42.3284659498332,37.323247286775,-227.257657541791));
#208435=CARTESIAN_POINT('Ctrl Pts',(54.9916284043978,36.4242882801268,-218.85005));
#208436=CARTESIAN_POINT('Ctrl Pts',(54.9916284043978,36.4242882801267,-218.35005));
#208437=CARTESIAN_POINT('Ctrl Pts',(55.4804763444372,36.5293010961029,-218.35005));
#208438=CARTESIAN_POINT('Ctrl Pts',(54.9934502776071,36.4158072299129,-218.850049997976));
#208439=CARTESIAN_POINT('Ctrl Pts',(54.9932481939215,36.4167479617736,-218.351913756624));
#208440=CARTESIAN_POINT('Ctrl Pts',(55.4808808567138,36.5185275155889,-218.35005));
#208441=CARTESIAN_POINT('Ctrl Pts',(54.9951959309483,36.4073227473215,-218.85001713104));
#208442=CARTESIAN_POINT('Ctrl Pts',(54.9948238206649,36.4091341749127,-218.353722457588));
#208443=CARTESIAN_POINT('Ctrl Pts',(55.4812212937741,36.5077394466269,-218.350030277458));
#208444=CARTESIAN_POINT('Ctrl Pts',(54.9968660030035,36.3988348033192,-218.849954951747));
#208445=CARTESIAN_POINT('Ctrl Pts',(54.9963513974766,36.4014502251401,-218.35547736011));
#208446=CARTESIAN_POINT('Ctrl Pts',(55.4814981831709,36.4969369346252,-218.349992971048));
#208447=CARTESIAN_POINT('',(54.9916284043978,36.4242882801268,-218.85005));
#208448=CARTESIAN_POINT('',(55.4804763444372,36.529301096103,-218.35005));
#208449=CARTESIAN_POINT('Origin',(55.4804763444372,36.529301096103,-218.85005));
#208450=CARTESIAN_POINT('Ctrl Pts',(55.4814981831708,36.4969369346298,-218.349992971048));
#208451=CARTESIAN_POINT('Ctrl Pts',(55.4812216183662,36.507726772777,-218.350030233692));
#208452=CARTESIAN_POINT('Ctrl Pts',(55.4808813172563,36.5185152497272,-218.35005));
#208453=CARTESIAN_POINT('Ctrl Pts',(55.4804763444372,36.5293010961029,-218.35005));
#208454=CARTESIAN_POINT('Ctrl Pts',(54.9916284043978,36.4242882801268,-218.85005));
#208455=CARTESIAN_POINT('Ctrl Pts',(54.9934477121007,36.4158191726697,-218.850049997978));
#208456=CARTESIAN_POINT('Ctrl Pts',(54.9951937291456,36.4073339377235,-218.850017211078));
#208457=CARTESIAN_POINT('Ctrl Pts',(54.9968660030035,36.3988348033193,-218.849954951747));
#208458=CARTESIAN_POINT('Ctrl Pts',(47.6321147582419,41.9825203546088,-220.52735443572));
#208459=CARTESIAN_POINT('Ctrl Pts',(47.3919300806125,41.7415300830818,-220.204915325333));
#208460=CARTESIAN_POINT('Ctrl Pts',(47.0451284874689,42.0562187287016,-220.184138377616));
#208461=CARTESIAN_POINT('Ctrl Pts',(47.7902484566451,42.1411844429755,-220.212182607147));
#208462=CARTESIAN_POINT('Ctrl Pts',(47.5344785649843,41.9530961111727,-219.935794482803));
#208463=CARTESIAN_POINT('Ctrl Pts',(47.255889523814,42.2679809657455,-219.868852497358));
#208464=CARTESIAN_POINT('Ctrl Pts',(47.979916006804,42.2643583982894,-219.907394043497));
#208465=CARTESIAN_POINT('Ctrl Pts',(47.7321494909123,42.1394451765273,-219.649704637013));
#208466=CARTESIAN_POINT('Ctrl Pts',(47.5083824724237,42.4326649364373,-219.563965012339));
#208467=CARTESIAN_POINT('Ctrl Pts',(48.3223344522033,42.3817233472697,-219.469720269686));
#208468=CARTESIAN_POINT('Ctrl Pts',(48.1175959253334,42.3304889669946,-219.231029546912));
#208469=CARTESIAN_POINT('Ctrl Pts',(47.9638307571195,42.5902413709234,-219.126165729975));
#208470=CARTESIAN_POINT('Ctrl Pts',(48.4441285568109,42.4082510978142,-219.330335434312));
#208471=CARTESIAN_POINT('Ctrl Pts',(48.2547747023757,42.3779588184084,-219.098571457423));
#208472=CARTESIAN_POINT('Ctrl Pts',(48.1257697081393,42.6260372470741,-218.986746587154));
#208473=CARTESIAN_POINT('Ctrl Pts',(48.7024187673651,42.4292025475747,-219.071888450679));
#208474=CARTESIAN_POINT('Ctrl Pts',(48.5489925463845,42.4312682822061,-218.853050886544));
#208475=CARTESIAN_POINT('Ctrl Pts',(48.4690711499939,42.6549505391914,-218.728256059428));
#208476=CARTESIAN_POINT('Ctrl Pts',(48.8408569866003,42.4234942721779,-218.951187879954));
#208477=CARTESIAN_POINT('Ctrl Pts',(48.7086549671031,42.4384217702358,-218.737132750757));
#208478=CARTESIAN_POINT('Ctrl Pts',(48.653008232647,42.6479010052335,-218.607549287092));
#208479=CARTESIAN_POINT('Ctrl Pts',(48.9829866058019,42.3956441991541,-218.850009606915));
#208480=CARTESIAN_POINT('Ctrl Pts',(48.874649979175,42.4168725889835,-218.639304842979));
#208481=CARTESIAN_POINT('Ctrl Pts',(48.841793010828,42.6113834075459,-218.506376562157));
#208482=CARTESIAN_POINT('',(48.8417930108281,42.6113834075459,-218.506376562157));
#208483=CARTESIAN_POINT('',(48.9829866058019,42.3956441991541,-218.850009606915));
#208484=CARTESIAN_POINT('Origin',(49.0791324003789,42.8863131162308,-218.850009606915));
#208485=CARTESIAN_POINT('Ctrl Pts',(47.6321147582419,41.9825203546088,-220.527354435719));
#208486=CARTESIAN_POINT('Ctrl Pts',(47.6671476766846,42.0176707755733,-220.45753131079));
#208487=CARTESIAN_POINT('Ctrl Pts',(47.702587917472,42.0499288628698,-220.390497026025));
#208488=CARTESIAN_POINT('Ctrl Pts',(47.7381227903546,42.0794845162404,-220.326313799903));
#208489=CARTESIAN_POINT('Ctrl Pts',(47.7765285867267,42.1114280216736,-220.256945100567));
#208490=CARTESIAN_POINT('Ctrl Pts',(47.8150447748923,42.1402149076497,-220.190906713326));
#208491=CARTESIAN_POINT('Ctrl Pts',(47.8532392505425,42.1661345339121,-220.128263389041));
#208492=CARTESIAN_POINT('Ctrl Pts',(47.8771525096411,42.1823626068991,-220.089042899195));
#208493=CARTESIAN_POINT('Ctrl Pts',(47.9009389144252,42.1974677336501,-220.051152968164));
#208494=CARTESIAN_POINT('Ctrl Pts',(47.9244865778018,42.2115289122536,-220.014607284998));
#208495=CARTESIAN_POINT('Ctrl Pts',(47.9717155479152,42.2397310728417,-219.941308505817));
#208496=CARTESIAN_POINT('Ctrl Pts',(48.0179957113527,42.2637421484083,-219.873396984484));
#208497=CARTESIAN_POINT('Ctrl Pts',(48.0625242392206,42.2842897519008,-219.810804136404));
#208498=CARTESIAN_POINT('Ctrl Pts',(48.0965454910983,42.2999887931083,-219.762981152977));
#208499=CARTESIAN_POINT('Ctrl Pts',(48.1295446337251,42.3136683515992,-219.718260357638));
#208500=CARTESIAN_POINT('Ctrl Pts',(48.161211549205,42.3256611217467,-219.67656254218));
#208501=CARTESIAN_POINT('Ctrl Pts',(48.1709917013847,42.3293650226578,-219.663684401869));
#208502=CARTESIAN_POINT('Ctrl Pts',(48.1806451362829,42.3329079837966,-219.651094352271));
#208503=CARTESIAN_POINT('Ctrl Pts',(48.1901636764875,42.3362995838709,-219.638789476176));
#208504=CARTESIAN_POINT('Ctrl Pts',(48.1914442602548,42.3367558752671,-219.637134030673));
#208505=CARTESIAN_POINT('Ctrl Pts',(48.1918676801253,42.3369073614638,-219.636586003471));
#208506=CARTESIAN_POINT('Ctrl Pts',(48.1939977635784,42.337660147459,-219.633838241004));
#208507=CARTESIAN_POINT('Ctrl Pts',(48.1987254711478,42.3393309515031,-219.627739598532));
#208508=CARTESIAN_POINT('Ctrl Pts',(48.2034571415651,42.3409777836824,-219.621663132572));
#208509=CARTESIAN_POINT('Ctrl Pts',(48.2081925863628,42.3426008804874,-219.615608748564));
#208510=CARTESIAN_POINT('Ctrl Pts',(48.2505195271242,42.357108645914,-219.561492701556));
#208511=CARTESIAN_POINT('Ctrl Pts',(48.2928719490673,42.3695301859433,-219.509592142788));
#208512=CARTESIAN_POINT('Ctrl Pts',(48.3351019107294,42.3799619787972,-219.459922348728));
#208513=CARTESIAN_POINT('Ctrl Pts',(48.3798530128249,42.3910165525801,-219.407287254176));
#208514=CARTESIAN_POINT('Ctrl Pts',(48.4244665059068,42.3998369007734,-219.357157107164));
#208515=CARTESIAN_POINT('Ctrl Pts',(48.4687832982745,42.4065723067832,-219.30950325958));
#208516=CARTESIAN_POINT('Ctrl Pts',(48.5038177012274,42.4118969459458,-219.271830765491));
#208517=CARTESIAN_POINT('Ctrl Pts',(48.5386670314813,42.4159193551787,-219.235704827783));
#208518=CARTESIAN_POINT('Ctrl Pts',(48.5732599550489,42.4187257113642,-219.201093557407));
#208519=CARTESIAN_POINT('Ctrl Pts',(48.6064110596672,42.4214150997681,-219.167924870669));
#208520=CARTESIAN_POINT('Ctrl Pts',(48.6394527787534,42.4229783080772,-219.136041680009));
#208521=CARTESIAN_POINT('Ctrl Pts',(48.6722329973828,42.4234626745377,-219.105527001474));
#208522=CARTESIAN_POINT('Ctrl Pts',(48.7065599782558,42.4239698962379,-219.073572462115));
#208523=CARTESIAN_POINT('Ctrl Pts',(48.740600205348,42.4232941558778,-219.043118528264));
#208524=CARTESIAN_POINT('Ctrl Pts',(48.7742098510797,42.4215075438899,-219.014215586192));
#208525=CARTESIAN_POINT('Ctrl Pts',(48.8101746554899,42.4195957370468,-218.983287302483));
#208526=CARTESIAN_POINT('Ctrl Pts',(48.8456463337473,42.416411997341,-218.954134987967));
#208527=CARTESIAN_POINT('Ctrl Pts',(48.8804839718521,42.4120632042333,-218.926770715568));
#208528=CARTESIAN_POINT('Ctrl Pts',(48.9153216099568,42.4077144111257,-218.899406443168));
#208529=CARTESIAN_POINT('Ctrl Pts',(48.9495255120609,42.4022008472995,-218.873829660666));
#208530=CARTESIAN_POINT('Ctrl Pts',(48.9829866058019,42.3956441991541,-218.850009606915));
#208531=CARTESIAN_POINT('Ctrl Pts',(48.841793010828,42.6113834075459,-218.506376562157));
#208532=CARTESIAN_POINT('Ctrl Pts',(48.7921389548229,42.6209882435831,-218.532986949914));
#208533=CARTESIAN_POINT('Ctrl Pts',(48.7423679185265,42.6286450457463,-218.561188681117));
#208534=CARTESIAN_POINT('Ctrl Pts',(48.6924667173058,42.634401307697,-218.59095945731));
#208535=CARTESIAN_POINT('Ctrl Pts',(48.6430231770834,42.640104776999,-218.620457195524));
#208536=CARTESIAN_POINT('Ctrl Pts',(48.5934540403996,42.6439416775049,-218.651494363475));
#208537=CARTESIAN_POINT('Ctrl Pts',(48.543772185369,42.6459227720059,-218.6840600903));
#208538=CARTESIAN_POINT('Ctrl Pts',(48.4932286959486,42.6479382247078,-218.717190605821));
#208539=CARTESIAN_POINT('Ctrl Pts',(48.4425606545126,42.6480337331324,-218.751907906809));
#208540=CARTESIAN_POINT('Ctrl Pts',(48.3917898255881,42.6461829344346,-218.788225803387));
#208541=CARTESIAN_POINT('Ctrl Pts',(48.3715210860928,42.6454440582441,-218.80272464062));
#208542=CARTESIAN_POINT('Ctrl Pts',(48.3512361589158,42.6443945431748,-218.817478808531));
#208543=CARTESIAN_POINT('Ctrl Pts',(48.3309376355839,42.6430308843516,-218.832489881455));
#208544=CARTESIAN_POINT('Ctrl Pts',(48.3233495728856,42.6425211167946,-218.838101371544));
#208545=CARTESIAN_POINT('Ctrl Pts',(48.3152632055342,42.6419301470072,-218.844118980124));
#208546=CARTESIAN_POINT('Ctrl Pts',(48.3076677770069,42.6413300633137,-218.849806740241));
#208547=CARTESIAN_POINT('Ctrl Pts',(48.3041115100809,42.6410490972321,-218.852469814894));
#208548=CARTESIAN_POINT('Ctrl Pts',(48.3006625067958,42.6407667959799,-218.85506030479));
#208549=CARTESIAN_POINT('Ctrl Pts',(48.2974204929156,42.6404937520387,-218.857501393121));
#208550=CARTESIAN_POINT('Ctrl Pts',(48.2971497386314,42.6404709489849,-218.857705258727));
#208551=CARTESIAN_POINT('Ctrl Pts',(48.296880421018,42.6404482119113,-218.857908086002));
#208552=CARTESIAN_POINT('Ctrl Pts',(48.2966125980265,42.6404255474864,-218.858109829903));
#208553=CARTESIAN_POINT('Ctrl Pts',(48.2228468677989,42.6341831489165,-218.913675582879));
#208554=CARTESIAN_POINT('Ctrl Pts',(48.1497074685359,42.6239015850986,-218.971998779091));
#208555=CARTESIAN_POINT('Ctrl Pts',(48.0772565138272,42.609556511184,-219.033078804808));
#208556=CARTESIAN_POINT('Ctrl Pts',(48.0685873731365,42.6078400470672,-219.040387353584));
#208557=CARTESIAN_POINT('Ctrl Pts',(48.0599281431717,42.6060654018618,-219.047735343152));
#208558=CARTESIAN_POINT('Ctrl Pts',(48.0512789750459,42.6042325345101,-219.05512274593));
#208559=CARTESIAN_POINT('Ctrl Pts',(48.0108123723846,42.5956571531817,-219.089685965027));
#208560=CARTESIAN_POINT('Ctrl Pts',(47.9705646754492,42.5858071104717,-219.1251129597));
#208561=CARTESIAN_POINT('Ctrl Pts',(47.9305490404132,42.5746767894346,-219.161403956555));
#208562=CARTESIAN_POINT('Ctrl Pts',(47.9105412228952,42.5691116289161,-219.179549454982));
#208563=CARTESIAN_POINT('Ctrl Pts',(47.8905914347185,42.5632263822981,-219.197910966478));
#208564=CARTESIAN_POINT('Ctrl Pts',(47.8707014981217,42.5570201524988,-219.216488612424));
#208565=CARTESIAN_POINT('Ctrl Pts',(47.8607565298232,42.5539170375991,-219.225777435397));
#208566=CARTESIAN_POINT('Ctrl Pts',(47.8508265142323,42.5507336940937,-219.235120285671));
#208567=CARTESIAN_POINT('Ctrl Pts',(47.8409116461696,42.5474700662204,-219.244517159201));
#208568=CARTESIAN_POINT('Ctrl Pts',(47.8337212795827,42.5451032489654,-219.251331870706));
#208569=CARTESIAN_POINT('Ctrl Pts',(47.8260625557433,42.5425331118276,-219.258629887513));
#208570=CARTESIAN_POINT('Ctrl Pts',(47.8189725322148,42.5401089729406,-219.265421986316));
#208571=CARTESIAN_POINT('Ctrl Pts',(47.8165753157007,42.5392893443809,-219.267718471138));
#208572=CARTESIAN_POINT('Ctrl Pts',(47.8142428881523,42.5384867810019,-219.269956972505));
#208573=CARTESIAN_POINT('Ctrl Pts',(47.8120146859391,42.5377158576958,-219.272098836301));
#208574=CARTESIAN_POINT('Ctrl Pts',(47.8117458163428,42.5376228329978,-219.272357287733));
#208575=CARTESIAN_POINT('Ctrl Pts',(47.8114784723229,42.5375302752592,-219.272614321647));
#208576=CARTESIAN_POINT('Ctrl Pts',(47.8112127226038,42.537438210317,-219.272869870324));
#208577=CARTESIAN_POINT('Ctrl Pts',(47.731812238609,42.5099311220856,-219.349222495541));
#208578=CARTESIAN_POINT('Ctrl Pts',(47.6546767982,42.4779131198223,-219.427655041056));
#208579=CARTESIAN_POINT('Ctrl Pts',(47.5799714073587,42.4412550793883,-219.508179149439));
#208580=CARTESIAN_POINT('Ctrl Pts',(47.5061288943132,42.4050204543033,-219.587773171461));
#208581=CARTESIAN_POINT('Ctrl Pts',(47.4346606908892,42.3642522713035,-219.669410737826));
#208582=CARTESIAN_POINT('Ctrl Pts',(47.3656965554581,42.3188657023054,-219.753094765277));
#208583=CARTESIAN_POINT('Ctrl Pts',(47.2978184355232,42.2741938601279,-219.835460975139));
#208584=CARTESIAN_POINT('Ctrl Pts',(47.2323661737487,42.2250479023035,-219.919809709308));
#208585=CARTESIAN_POINT('Ctrl Pts',(47.169433903332,42.1713867096496,-220.006135435357));
#208586=CARTESIAN_POINT('Ctrl Pts',(47.1268378225816,42.1350658129092,-220.064565515398));
#208587=CARTESIAN_POINT('Ctrl Pts',(47.0853956260421,42.0966771525707,-220.123901151368));
#208588=CARTESIAN_POINT('Ctrl Pts',(47.0451284874691,42.0562187287014,-220.184138377616));
#208589=CARTESIAN_POINT('Origin',(53.5250845842796,36.1092498321983,-218.85005));
#208590=CARTESIAN_POINT('',(54.6328983814091,37.1205601658197,-218.85005));
#208591=CARTESIAN_POINT('',(55.0021696471189,37.4576636103602,-218.35005));
#208592=CARTESIAN_POINT('Origin',(55.0021696471189,37.4576636103602,-218.85005));
#208593=CARTESIAN_POINT('Origin',(53.5250845842796,36.1092498321983,-218.35005));
#208594=CARTESIAN_POINT('Origin',(53.5250845842796,36.1092498321983,-218.85005));
#208595=CARTESIAN_POINT('Origin',(49.0791324003789,42.8863131162308,-218.850009606915));
#208596=CARTESIAN_POINT('',(49.0801870931398,42.8824343798319,-218.350025764149));
#208597=CARTESIAN_POINT('Origin',(49.0791324003789,42.8863131162308,-218.850009606915));
#208598=CARTESIAN_POINT('Origin',(49.0791324003789,42.8863131162308,-218.850009606915));
#208599=CARTESIAN_POINT('Origin',(0.128459562639233,-12.6359082483571,-218.85005));
#208600=CARTESIAN_POINT('',(49.7021444432209,42.0348313420379,-218.85005));
#208601=CARTESIAN_POINT('',(50.0380095169376,42.4052293067426,-218.35005));
#208602=CARTESIAN_POINT('Origin',(50.0380095169376,42.4052293067426,-218.85005));
#208603=CARTESIAN_POINT('Origin',(0.128459562639233,-12.6359082483571,-218.35005));
#208604=CARTESIAN_POINT('Origin',(0.128459562639233,-12.6359082483571,-218.85005));
#208605=CARTESIAN_POINT('Ctrl Pts',(49.1011166787324,42.8818771940186,-218.35005));
#208606=CARTESIAN_POINT('Ctrl Pts',(48.9994748145671,42.3923172574951,-218.35005));
#208607=CARTESIAN_POINT('Ctrl Pts',(48.999474814567,42.392317257495,-218.85005));
#208608=CARTESIAN_POINT('Ctrl Pts',(49.09414603136,42.8820897398471,-218.35005));
#208609=CARTESIAN_POINT('Ctrl Pts',(48.994587444257,42.3933319685669,-218.351257450515));
#208610=CARTESIAN_POINT('Ctrl Pts',(48.9939799633645,42.3934580921056,-218.85004999869));
#208611=CARTESIAN_POINT('Ctrl Pts',(49.0871694989175,42.882275419924,-218.350041726378));
#208612=CARTESIAN_POINT('Ctrl Pts',(48.9896694475663,42.3943279693454,-218.352441808199));
#208613=CARTESIAN_POINT('Ctrl Pts',(48.9884838968603,42.394567013707,-218.850036211906));
#208614=CARTESIAN_POINT('Ctrl Pts',(49.0801870931398,42.8824343798319,-218.350025764149));
#208615=CARTESIAN_POINT('Ctrl Pts',(48.9847217242793,42.3953042054457,-218.353603405568));
#208616=CARTESIAN_POINT('Ctrl Pts',(48.9829866058019,42.3956441991541,-218.850009606915));
#208617=CARTESIAN_POINT('',(49.1011166787325,42.8818771940186,-218.35005));
#208618=CARTESIAN_POINT('',(48.999474814567,42.392317257495,-218.85005));
#208619=CARTESIAN_POINT('Origin',(49.1011166787325,42.8818771940186,-218.85005));
#208620=CARTESIAN_POINT('Ctrl Pts',(48.9829866058019,42.3956441991541,-218.850009606915));
#208621=CARTESIAN_POINT('Ctrl Pts',(48.9884887606911,42.3945660606471,-218.85003623417));
#208622=CARTESIAN_POINT('Ctrl Pts',(48.993985033412,42.3934570394682,-218.850049998691));
#208623=CARTESIAN_POINT('Ctrl Pts',(48.999474814567,42.392317257495,-218.85005));
#208624=CARTESIAN_POINT('Ctrl Pts',(49.1011166787325,42.8818771940186,-218.35005));
#208625=CARTESIAN_POINT('Ctrl Pts',(49.0941409157939,42.8820898960309,-218.35005));
#208626=CARTESIAN_POINT('Ctrl Pts',(49.0871642720694,42.8822755387356,-218.35004171443));
#208627=CARTESIAN_POINT('Ctrl Pts',(49.0801870931398,42.8824343798319,-218.350025764149));
#208628=CARTESIAN_POINT('Origin',(48.6945492220708,40.9236374479242,-218.85005));
#208629=CARTESIAN_POINT('Origin',(48.6945492220708,40.9236374479242,-218.85005));
#208630=CARTESIAN_POINT('Origin',(48.6945492220708,40.9236374479242,-218.35005));
#208631=CARTESIAN_POINT('Origin',(0.,-178.58000002,-205.84995));
#208632=CARTESIAN_POINT('',(43.4686063353067,49.3549798298524,-205.841223796781));
#208633=CARTESIAN_POINT('Origin',(0.,-178.58000002,-205.841223796781));
#208634=CARTESIAN_POINT('',(43.5622571193626,49.8460535351382,-205.34995));
#208635=CARTESIAN_POINT('Origin',(0.,-178.58000002,-205.34995));
#208636=CARTESIAN_POINT('Origin',(43.5622571193626,49.8460535351382,-205.84995));
#208637=CARTESIAN_POINT('Origin',(41.3132181298675,38.0528376956935,-205.84995));
#208638=CARTESIAN_POINT('',(48.8684365469981,47.38326056293,-205.34995));
#208639=CARTESIAN_POINT('',(48.5538345628697,46.9947384336248,-205.841223796781));
#208640=CARTESIAN_POINT('Origin',(48.8684365469981,47.38326056293,-205.84995));
#208641=CARTESIAN_POINT('Origin',(41.3132181298675,38.0528376956935,-205.841223796781));
#208642=CARTESIAN_POINT('Origin',(41.3132181298675,38.0528376956935,-205.34995));
#208643=CARTESIAN_POINT('Origin',(0.,-12.9675000200281,-205.84995));
#208644=CARTESIAN_POINT('',(59.9876878113059,36.3459434263872,-205.34995));
#208645=CARTESIAN_POINT('',(59.6015030478428,36.0284766063157,-205.841223796781));
#208646=CARTESIAN_POINT('Origin',(59.9876878113059,36.3459434263873,-205.84995));
#208647=CARTESIAN_POINT('Origin',(0.,-12.9675000200281,-205.841223796781));
#208648=CARTESIAN_POINT('Origin',(0.,-12.9675000200281,-205.34995));
#208649=CARTESIAN_POINT('Origin',(50.7133971693864,28.7219255026674,-205.84995));
#208650=CARTESIAN_POINT('',(62.7097829146859,29.1961040154388,-205.34995));
#208651=CARTESIAN_POINT('',(62.2102491422031,29.1763590533857,-205.841223796781));
#208652=CARTESIAN_POINT('Origin',(62.709782914686,29.1961040154388,-205.84995));
#208653=CARTESIAN_POINT('Origin',(50.7133971693864,28.7219255026674,-205.841223796781));
#208654=CARTESIAN_POINT('Origin',(50.7133971693864,28.7219255026674,-205.34995));
#208655=CARTESIAN_POINT('Origin',(-1004.,-12.967500020028,-205.84995));
#208656=CARTESIAN_POINT('',(62.7097829146858,-55.1311040554952,-205.34995));
#208657=CARTESIAN_POINT('',(62.210249142203,-55.1113590934421,-205.841223796781));
#208658=CARTESIAN_POINT('Origin',(62.7097829146858,-55.1311040554952,-205.84995));
#208659=CARTESIAN_POINT('Origin',(-1004.,-12.967500020028,-205.841223796781));
#208660=CARTESIAN_POINT('Origin',(-1004.,-12.967500020028,-205.34995));
#208661=CARTESIAN_POINT('Origin',(50.7133971693864,-54.6569255427236,-205.84995));
#208662=CARTESIAN_POINT('',(59.9876878113058,-62.2809434664435,-205.34995));
#208663=CARTESIAN_POINT('',(59.6015030478428,-61.963476646372,-205.841223796781));
#208664=CARTESIAN_POINT('Origin',(59.9876878113059,-62.2809434664436,-205.84995));
#208665=CARTESIAN_POINT('Origin',(50.7133971693864,-54.6569255427236,-205.841223796781));
#208666=CARTESIAN_POINT('Origin',(50.7133971693864,-54.6569255427236,-205.34995));
#208667=CARTESIAN_POINT('Origin',(0.,-12.9675000200281,-205.84995));
#208668=CARTESIAN_POINT('',(49.142885306769,-73.0949913797652,-205.34995));
#208669=CARTESIAN_POINT('',(48.8265164945923,-72.7079065982776,-205.841223796781));
#208670=CARTESIAN_POINT('Origin',(49.142885306769,-73.0949913797652,-205.84995));
#208671=CARTESIAN_POINT('Origin',(0.,-12.9675000200281,-205.841223796781));
#208672=CARTESIAN_POINT('Origin',(0.,-12.9675000200281,-205.34995));
#208673=CARTESIAN_POINT('Origin',(41.5452362233251,-63.7990866568863,-205.84995));
#208674=CARTESIAN_POINT('',(42.0177747166746,-75.7955371145968,-205.34995));
#208675=CARTESIAN_POINT('',(41.998098045614,-75.2960006474661,-205.841223796781));
#208676=CARTESIAN_POINT('Origin',(42.0177747166746,-75.7955371145968,-205.84995));
#208677=CARTESIAN_POINT('Origin',(41.5452362233251,-63.7990866568863,-205.841223796781));
#208678=CARTESIAN_POINT('Origin',(41.5452362233251,-63.7990866568863,-205.34995));
#208679=CARTESIAN_POINT('Origin',(0.,990.91999998,-205.84995));
#208680=CARTESIAN_POINT('Origin',(0.,990.91999998,-205.34995));
#208681=CARTESIAN_POINT('Origin',(0.,990.91999998,-205.841223796781));
#208682=CARTESIAN_POINT('Ctrl Pts',(55.1063041457933,-62.4061442430715,
-218.35005));
#208683=CARTESIAN_POINT('Ctrl Pts',(54.9567009523894,-62.2733518205981,
-218.35005));
#208684=CARTESIAN_POINT('Ctrl Pts',(54.8483808955536,-62.1772035872457,
-218.488025452358));
#208685=CARTESIAN_POINT('Ctrl Pts',(55.189518743021,-62.3123951476979,-218.35005));
#208686=CARTESIAN_POINT('Ctrl Pts',(55.0396688463657,-62.1798977449584,
-218.35005000001));
#208687=CARTESIAN_POINT('Ctrl Pts',(54.9311672479814,-62.0839582776323,
-218.48801196499));
#208688=CARTESIAN_POINT('Ctrl Pts',(55.2724546450001,-62.2184167144346,
-218.35005));
#208689=CARTESIAN_POINT('Ctrl Pts',(55.1223583736958,-62.0862177900441,
-218.350049999979));
#208690=CARTESIAN_POINT('Ctrl Pts',(55.0136740740194,-61.9904901268701,
-218.487996778695));
#208691=CARTESIAN_POINT('Ctrl Pts',(55.3551085347194,-62.1242062049499,
-218.35005));
#208692=CARTESIAN_POINT('Ctrl Pts',(55.204767621478,-61.9923073188158,-218.35005));
#208693=CARTESIAN_POINT('Ctrl Pts',(55.0958998011493,-61.8967941020366,
-218.487980161586));
#208694=CARTESIAN_POINT('',(55.3551085347089,-62.1242062049619,-218.35005));
#208695=CARTESIAN_POINT('Origin',(6.53661563613523,-19.2936643109222,-218.35005));
#208696=CARTESIAN_POINT('',(55.0958998011388,-61.8967941020485,-218.487980161586));
#208697=CARTESIAN_POINT('Origin',(6.32111438748812,-19.0925318432536,-218.204998012194));
#208698=CARTESIAN_POINT('Origin',(55.3551085347089,-62.1242062049619,-218.85005));
#208699=CARTESIAN_POINT('Ctrl Pts',(55.2339673727997,-61.7389489519143,
-218.487950878256));
#208700=CARTESIAN_POINT('Ctrl Pts',(55.3431423575669,-61.8341015991581,
-218.35005));
#208701=CARTESIAN_POINT('Ctrl Pts',(55.4938952567199,-61.9654919306031,
-218.35005));
#208702=CARTESIAN_POINT('Ctrl Pts',(55.1880309233148,-61.7916386130721,
-218.487961072495));
#208703=CARTESIAN_POINT('Ctrl Pts',(55.2971033694472,-61.8869121544979,
-218.350049999996));
#208704=CARTESIAN_POINT('Ctrl Pts',(55.4477195716702,-62.0184723768345,
-218.35005));
#208705=CARTESIAN_POINT('Ctrl Pts',(55.14200840849,-61.8442534512036,-218.487970843436));
#208706=CARTESIAN_POINT('Ctrl Pts',(55.2509784443238,-61.9396472076622,
-218.350050000013));
#208707=CARTESIAN_POINT('Ctrl Pts',(55.4014572374666,-62.0713770530022,
-218.35005));
#208708=CARTESIAN_POINT('Ctrl Pts',(55.0958998011388,-61.8967941020486,
-218.487980161586));
#208709=CARTESIAN_POINT('Ctrl Pts',(55.2047676214677,-61.9923073188278,
-218.35005));
#208710=CARTESIAN_POINT('Ctrl Pts',(55.3551085347089,-62.1242062049619,
-218.35005));
#208711=CARTESIAN_POINT('',(55.2339673727996,-61.7389489519143,-218.487950878256));
#208712=CARTESIAN_POINT('',(55.4938952567199,-61.9654919306031,-218.35005));
#208713=CARTESIAN_POINT('Origin',(55.4938952567198,-61.9654919306031,-218.85005));
#208714=CARTESIAN_POINT('Ctrl Pts',(55.3551085347089,-62.1242062049619,
-218.35005));
#208715=CARTESIAN_POINT('Ctrl Pts',(55.4014571755248,-62.0713771235952,
-218.35005));
#208716=CARTESIAN_POINT('Ctrl Pts',(55.4477196335097,-62.0184723058819,
-218.35005));
#208717=CARTESIAN_POINT('Ctrl Pts',(55.4938952567199,-61.9654919306031,
-218.35005));
#208718=CARTESIAN_POINT('Origin',(7.62393634648824,-43.3515330069781,-218.305892816451));
#208719=CARTESIAN_POINT('Ctrl Pts',(49.4570218871579,-69.5396831399799,
-217.525618242158));
#208720=CARTESIAN_POINT('Ctrl Pts',(49.2592415957564,-69.455430883311,-217.233755494175));
#208721=CARTESIAN_POINT('Ctrl Pts',(49.1082596796586,-69.7601043330141,
-217.107989577217));
#208722=CARTESIAN_POINT('Ctrl Pts',(49.2622754448157,-69.4954973356379,
-217.612334261911));
#208723=CARTESIAN_POINT('Ctrl Pts',(49.0757606270564,-69.4511605712625,
-217.34710501445));
#208724=CARTESIAN_POINT('Ctrl Pts',(48.912676519449,-69.7205296868298,-217.252740911407));
#208725=CARTESIAN_POINT('Ctrl Pts',(49.0788953913437,-69.440810795047,-217.70194766018));
#208726=CARTESIAN_POINT('Ctrl Pts',(48.8940785173341,-69.4269663422441,
-217.47286760646));
#208727=CARTESIAN_POINT('Ctrl Pts',(48.7307698712856,-69.6620794550121,
-217.402284510414));
#208728=CARTESIAN_POINT('Ctrl Pts',(48.7966565591402,-69.3194187518267,
-217.863510508004));
#208729=CARTESIAN_POINT('Ctrl Pts',(48.6179833119651,-69.3347292882382,
-217.703261160372));
#208730=CARTESIAN_POINT('Ctrl Pts',(48.4568130848015,-69.5116847789954,
-217.67207172234));
#208731=CARTESIAN_POINT('Ctrl Pts',(48.6861912261675,-69.2595360633236,
-217.934600613269));
#208732=CARTESIAN_POINT('Ctrl Pts',(48.5105553232489,-69.2816866454383,
-217.805049640232));
#208733=CARTESIAN_POINT('Ctrl Pts',(48.3516107950449,-69.4327456757647,
-217.790813441481));
#208734=CARTESIAN_POINT('Ctrl Pts',(48.5120925091425,-69.1176128201212,
-218.077169784276));
#208735=CARTESIAN_POINT('Ctrl Pts',(48.346506115558,-69.1351464133951,-218.00756927047));
#208736=CARTESIAN_POINT('Ctrl Pts',(48.1935846999847,-69.2311811089996,
-218.029011852183));
#208737=CARTESIAN_POINT('Ctrl Pts',(48.44853190302,-69.0341658346798,-218.149562838542));
#208738=CARTESIAN_POINT('Ctrl Pts',(48.2881462840732,-69.0394916099964,
-218.110930665774));
#208739=CARTESIAN_POINT('Ctrl Pts',(48.141063563618,-69.1062596209728,-218.149999563001));
#208740=CARTESIAN_POINT('Ctrl Pts',(48.4345085199297,-68.8996986141391,
-218.239932923561));
#208741=CARTESIAN_POINT('Ctrl Pts',(48.2846281886007,-68.8713617818855,
-218.233863811861));
#208742=CARTESIAN_POINT('Ctrl Pts',(48.1484532516179,-68.8904009633176,
-218.301080288388));
#208743=CARTESIAN_POINT('Ctrl Pts',(48.4438278731385,-68.8541286362714,
-218.266363445181));
#208744=CARTESIAN_POINT('Ctrl Pts',(48.2975896440283,-68.8120721221255,
-218.268779191712));
#208745=CARTESIAN_POINT('Ctrl Pts',(48.1656057057525,-68.8149306500085,
-218.345277024483));
#208746=CARTESIAN_POINT('Ctrl Pts',(48.507784321035,-68.732929092821,-218.324806358094));
#208747=CARTESIAN_POINT('Ctrl Pts',(48.3709960733748,-68.6498345611464,
-218.341572514799));
#208748=CARTESIAN_POINT('Ctrl Pts',(48.2519986346533,-68.6077656957913,
-218.443032871038));
#208749=CARTESIAN_POINT('Ctrl Pts',(48.5915006514379,-68.6628850039255,
-218.344419445302));
#208750=CARTESIAN_POINT('Ctrl Pts',(48.4608840740975,-68.5494670324552,
-218.359917285752));
#208751=CARTESIAN_POINT('Ctrl Pts',(48.3506511305266,-68.4802802531201,
-218.475898114176));
#208752=CARTESIAN_POINT('Ctrl Pts',(48.6940335790739,-68.6081147401982,
-218.348150004632));
#208753=CARTESIAN_POINT('Ctrl Pts',(48.5650271218342,-68.4711538784475,
-218.353348100088));
#208754=CARTESIAN_POINT('Ctrl Pts',(48.4661517708994,-68.3748018054678,
-218.482144505478));
#208755=CARTESIAN_POINT('',(48.9443109379934,-69.7210624363875,-217.233400031701));
#208756=CARTESIAN_POINT('Ctrl Pts',(48.3245605310987,-68.5271120961857,
-218.45762963148));
#208757=CARTESIAN_POINT('Ctrl Pts',(48.2969090264087,-68.5624400955583,
-218.448765818759));
#208758=CARTESIAN_POINT('Ctrl Pts',(48.272373979724,-68.5979809825957,-218.437849245981));
#208759=CARTESIAN_POINT('Ctrl Pts',(48.2296118037038,-68.6694696560977,
-218.411910580311));
#208760=CARTESIAN_POINT('Ctrl Pts',(48.2118419283057,-68.7043185904572,
-218.39740761229));
#208761=CARTESIAN_POINT('Ctrl Pts',(48.1808487368591,-68.7788024321227,
-218.362219656654));
#208762=CARTESIAN_POINT('Ctrl Pts',(48.1629168738174,-68.8344186687614,
-218.332820537156));
#208763=CARTESIAN_POINT('Ctrl Pts',(48.1530254853042,-68.8896516378129,
-218.2989091885));
#208764=CARTESIAN_POINT('Ctrl Pts',(48.1482245464656,-68.9263872954923,
-218.275298905138));
#208765=CARTESIAN_POINT('Ctrl Pts',(48.1466843549373,-68.9458148942746,
-218.262219668185));
#208766=CARTESIAN_POINT('Ctrl Pts',(48.1449816941239,-68.997348945024,-218.226114299801));
#208767=CARTESIAN_POINT('Ctrl Pts',(48.1481130692551,-69.0481950185523,
-218.18764191845));
#208768=CARTESIAN_POINT('Ctrl Pts',(48.1585276426128,-69.0980066943639,
-218.145619017648));
#208769=CARTESIAN_POINT('Ctrl Pts',(48.1670914404119,-69.1309846393012,
-218.116814746125));
#208770=CARTESIAN_POINT('Ctrl Pts',(48.172730617193,-69.1488647385631,-218.100610979771));
#208771=CARTESIAN_POINT('Ctrl Pts',(48.1888010654547,-69.1931241036076,
-218.059258944812));
#208772=CARTESIAN_POINT('Ctrl Pts',(48.2086778269923,-69.2362855894174,
-218.016459214628));
#208773=CARTESIAN_POINT('Ctrl Pts',(48.2385256773599,-69.2847267297988,
-217.963992729438));
#208774=CARTESIAN_POINT('Ctrl Pts',(48.252743015283,-69.3050781343457,-217.940964207218));
#208775=CARTESIAN_POINT('Ctrl Pts',(48.2625378116414,-69.3185549550489,
-217.925491217803));
#208776=CARTESIAN_POINT('Ctrl Pts',(48.2682837752384,-69.3261280787323,
-217.916654176065));
#208777=CARTESIAN_POINT('Ctrl Pts',(48.3089960702895,-69.378036374536,-217.855301989849));
#208778=CARTESIAN_POINT('Ctrl Pts',(48.3519830933143,-69.4212627364945,
-217.798872847759));
#208779=CARTESIAN_POINT('Ctrl Pts',(48.426557326924,-69.4817802610263,-217.711388336444));
#208780=CARTESIAN_POINT('Ctrl Pts',(48.4663669961376,-69.5109587572413,
-217.666935881241));
#208781=CARTESIAN_POINT('Ctrl Pts',(48.5171938223511,-69.5431236077837,
-217.613831834301));
#208782=CARTESIAN_POINT('Ctrl Pts',(48.5399117039659,-69.5565080736488,
-217.590806632211));
#208783=CARTESIAN_POINT('Ctrl Pts',(48.5552642540727,-69.5653422517974,
-217.575397314189));
#208784=CARTESIAN_POINT('Ctrl Pts',(48.5641005162855,-69.5702949293905,
-217.566622736532));
#208785=CARTESIAN_POINT('Ctrl Pts',(48.6801593526136,-69.6340177431732,
-217.452322976306));
#208786=CARTESIAN_POINT('Ctrl Pts',(48.8048901567373,-69.6829147138422,
-217.343489913132));
#208787=CARTESIAN_POINT('Ctrl Pts',(48.9443109379934,-69.7210624363875,
-217.233400031701));
#208788=CARTESIAN_POINT('',(49.2925903552098,-69.4989817480832,-217.60005));
#208789=CARTESIAN_POINT('Ctrl Pts',(49.2925903552098,-69.4989817480832,
-217.60005));
#208790=CARTESIAN_POINT('Ctrl Pts',(49.1484673907459,-69.4601446914727,
-217.668076900971));
#208791=CARTESIAN_POINT('Ctrl Pts',(49.0242599947267,-69.4170675539365,
-217.732996299125));
#208792=CARTESIAN_POINT('Ctrl Pts',(48.8668072751,-69.3498582752364,-217.822902511881));
#208793=CARTESIAN_POINT('Ctrl Pts',(48.8191318230071,-69.3270264133442,
-217.851645777573));
#208794=CARTESIAN_POINT('Ctrl Pts',(48.7547036967668,-69.2926109521484,
-217.892735727221));
#208795=CARTESIAN_POINT('Ctrl Pts',(48.7242609407847,-69.2753611405731,
-217.91277605223));
#208796=CARTESIAN_POINT('Ctrl Pts',(48.6918169106576,-69.2552639129,-217.935248183673));
#208797=CARTESIAN_POINT('Ctrl Pts',(48.6763596974272,-69.2452345365248,
-217.946255129638));
#208798=CARTESIAN_POINT('Ctrl Pts',(48.669898709807,-69.2409416675107,-217.950923096411));
#208799=CARTESIAN_POINT('Ctrl Pts',(48.6656276861863,-69.2380811075938,
-217.954024100342));
#208800=CARTESIAN_POINT('Ctrl Pts',(48.6650074713428,-69.2376705467468,
-217.954471148243));
#208801=CARTESIAN_POINT('Ctrl Pts',(48.6038690780288,-69.1960562874253,
-217.999308408621));
#208802=CARTESIAN_POINT('Ctrl Pts',(48.5576057289715,-69.1560179545467,
-218.03878501502));
#208803=CARTESIAN_POINT('Ctrl Pts',(48.5048358437187,-69.0957393063493,
-218.093132674187));
#208804=CARTESIAN_POINT('Ctrl Pts',(48.4826068126659,-69.0655460792566,
-218.119094170054));
#208805=CARTESIAN_POINT('Ctrl Pts',(48.4638790662549,-69.0304739208104,
-218.147136413011));
#208806=CARTESIAN_POINT('Ctrl Pts',(48.4573898341797,-69.0155026490939,
-218.158662749366));
#208807=CARTESIAN_POINT('Ctrl Pts',(48.4534044218793,-69.0055380297188,
-218.166236605228));
#208808=CARTESIAN_POINT('Ctrl Pts',(48.4521313177971,-69.002214019677,-218.168746457979));
#208809=CARTESIAN_POINT('Ctrl Pts',(48.4147042004739,-68.8897627549664,
-218.252011243573));
#208810=CARTESIAN_POINT('Ctrl Pts',(48.4558803503785,-68.7836110335151,
-218.307899599653));
#208811=CARTESIAN_POINT('Ctrl Pts',(48.5701931618903,-68.6892604152372,
-218.333619302448));
#208812=CARTESIAN_POINT('Origin',(49.1624951782473,-69.9817604188332,-217.60005));
#208813=CARTESIAN_POINT('Ctrl Pts',(55.4237479323138,-62.1328188643259,
-218.341144661975));
#208814=CARTESIAN_POINT('Ctrl Pts',(55.2405234564513,-62.0021381064316,
-218.318170442032));
#208815=CARTESIAN_POINT('Ctrl Pts',(55.0928795124925,-61.9237973298156,
-218.473054790165));
#208816=CARTESIAN_POINT('Ctrl Pts',(55.494632995213,-61.9315980237713,-218.361192001577));
#208817=CARTESIAN_POINT('Ctrl Pts',(55.3400279587498,-61.8078970750489,
-218.369232738601));
#208818=CARTESIAN_POINT('Ctrl Pts',(55.2399321713626,-61.7035864993853,
-218.506552167714));
#208819=CARTESIAN_POINT('Ctrl Pts',(55.6064180550928,-61.7413047615639,
-218.350163543339));
#208820=CARTESIAN_POINT('Ctrl Pts',(55.5091017198289,-61.6043114926627,
-218.374336100872));
#208821=CARTESIAN_POINT('Ctrl Pts',(55.4522604695358,-61.4873000226074,
-218.488185460704));
#208822=CARTESIAN_POINT('Ctrl Pts',(55.7967381055322,-61.6583804609248,
-218.254186826194));
#208823=CARTESIAN_POINT('Ctrl Pts',(55.7613184164348,-61.5067436997404,
-218.252944363189));
#208824=CARTESIAN_POINT('Ctrl Pts',(55.774129320809,-61.3703224231151,-218.328019869095));
#208825=CARTESIAN_POINT('Ctrl Pts',(55.8477306234162,-61.6541946099495,
-218.22271673907));
#208826=CARTESIAN_POINT('Ctrl Pts',(55.8266978017486,-61.4985748755131,
-218.210789756319));
#208827=CARTESIAN_POINT('Ctrl Pts',(55.8574329037833,-61.3577410974567,
-218.275498156808));
#208828=CARTESIAN_POINT('Ctrl Pts',(55.9478060913509,-61.6785900219245,
-218.1506974888));
#208829=CARTESIAN_POINT('Ctrl Pts',(55.9489905260305,-61.5152696674129,
-218.112160517346));
#208830=CARTESIAN_POINT('Ctrl Pts',(56.0156028250703,-61.3669778003364,
-218.155301834069));
#208831=CARTESIAN_POINT('Ctrl Pts',(55.9954662711786,-61.7067706426262,
-218.111190879857));
#208832=CARTESIAN_POINT('Ctrl Pts',(56.0045190211886,-61.5400305154986,
-218.056751473387));
#208833=CARTESIAN_POINT('Ctrl Pts',(56.0882300869458,-61.3886089876927,
-218.089366319566));
#208834=CARTESIAN_POINT('Ctrl Pts',(56.1267636112953,-61.8218463607312,
-217.990670505791));
#208835=CARTESIAN_POINT('Ctrl Pts',(56.1502648139586,-61.6460669288342,
-217.886016299921));
#208836=CARTESIAN_POINT('Ctrl Pts',(56.2821971389062,-61.4871566064044,
-217.888227119225));
#208837=CARTESIAN_POINT('Ctrl Pts',(56.1994729047277,-61.9375893837876,
-217.907702178034));
#208838=CARTESIAN_POINT('Ctrl Pts',(56.2191388000639,-61.7583243798369,
-217.767022200493));
#208839=CARTESIAN_POINT('Ctrl Pts',(56.3811156518498,-61.5958538338606,
-217.749769988996));
#208840=CARTESIAN_POINT('Ctrl Pts',(56.3439578714798,-62.2446096393604,
-217.718697327292));
#208841=CARTESIAN_POINT('Ctrl Pts',(56.3359782479612,-62.0576869907416,
-217.49766835849));
#208842=CARTESIAN_POINT('Ctrl Pts',(56.5650907006514,-61.8919890523586,
-217.43440812177));
#208843=CARTESIAN_POINT('Ctrl Pts',(56.4064091508865,-62.4540207436425,
-217.612944268375));
#208844=CARTESIAN_POINT('Ctrl Pts',(56.3631474716341,-62.2659851591403,
-217.349074894179));
#208845=CARTESIAN_POINT('Ctrl Pts',(56.6320495252993,-62.09974891787,-217.258041794045));
#208846=CARTESIAN_POINT('Ctrl Pts',(56.4532198574233,-62.6711239243471,
-217.514416680063));
#208847=CARTESIAN_POINT('Ctrl Pts',(56.363816920114,-62.4684902652751,-217.222377953599));
#208848=CARTESIAN_POINT('Ctrl Pts',(56.6724481617213,-62.3181880639774,
-217.093652670756));
#208849=CARTESIAN_POINT('',(56.6309943627598,-62.1341374253209,-217.237388612086));
#208850=CARTESIAN_POINT('',(56.4090189474477,-62.4870630585556,-217.60005));
#208851=CARTESIAN_POINT('Origin',(56.8921651292037,-62.3583394513399,-217.60005));
#208852=CARTESIAN_POINT('Ctrl Pts',(55.4938952567199,-61.9654919306031,
-218.35005));
#208853=CARTESIAN_POINT('Ctrl Pts',(55.57896365653,-61.7965571013242,-218.35005));
#208854=CARTESIAN_POINT('Ctrl Pts',(55.6778758905696,-61.6964283653063,
-218.318350028606));
#208855=CARTESIAN_POINT('Ctrl Pts',(55.8312897454811,-61.6535904959217,
-218.233316266271));
#208856=CARTESIAN_POINT('Ctrl Pts',(55.8841740643655,-61.6572520033479,
-218.198283210441));
#208857=CARTESIAN_POINT('Ctrl Pts',(55.9636629054506,-61.6903101237091,
-218.136750461095));
#208858=CARTESIAN_POINT('Ctrl Pts',(55.990187345622,-61.7059235141358,-218.114749592215));
#208859=CARTESIAN_POINT('Ctrl Pts',(56.0297268316923,-61.7363117331637,
-218.079709596312));
#208860=CARTESIAN_POINT('Ctrl Pts',(56.0494350297545,-61.7532478097978,
-218.061680601021));
#208861=CARTESIAN_POINT('Ctrl Pts',(56.0722599880634,-61.7760710568074,
-218.039806012764));
#208862=CARTESIAN_POINT('Ctrl Pts',(56.0836232219663,-61.7882507374176,
-218.028665294619));
#208863=CARTESIAN_POINT('Ctrl Pts',(56.0884818569286,-61.7936353893167,
-218.023847847065));
#208864=CARTESIAN_POINT('Ctrl Pts',(56.0917183460573,-61.7972617995588,
-218.020626775486));
#208865=CARTESIAN_POINT('Ctrl Pts',(56.0940933660921,-61.7999613204208,
-218.018251410963));
#208866=CARTESIAN_POINT('Ctrl Pts',(56.2047141650995,-61.9266217894036,
-217.90733398084));
#208867=CARTESIAN_POINT('Ctrl Pts',(56.319891141774,-62.1525342185782,-217.762647327886));
#208868=CARTESIAN_POINT('Ctrl Pts',(56.4090189474477,-62.4870630585556,
-217.60005));
#208869=CARTESIAN_POINT('Ctrl Pts',(56.6309943627598,-62.1341374253209,
-217.237388612085));
#208870=CARTESIAN_POINT('Ctrl Pts',(56.6169100679614,-62.0818886112393,
-217.279832325573));
#208871=CARTESIAN_POINT('Ctrl Pts',(56.6012339430048,-62.0318061452899,
-217.32206232518));
#208872=CARTESIAN_POINT('Ctrl Pts',(56.5839430146363,-61.983949822002,-217.364070353647));
#208873=CARTESIAN_POINT('Ctrl Pts',(56.5749805387295,-61.9591442629644,
-217.385844542691));
#208874=CARTESIAN_POINT('Ctrl Pts',(56.565584111166,-61.9349359769846,-217.407559629734));
#208875=CARTESIAN_POINT('Ctrl Pts',(56.555749303194,-61.9113292073645,-217.429217603718));
#208876=CARTESIAN_POINT('Ctrl Pts',(56.5413449582148,-61.8767540479494,
-217.460938500528));
#208877=CARTESIAN_POINT('Ctrl Pts',(56.5260014871927,-61.8434724446632,
-217.492534008143));
#208878=CARTESIAN_POINT('Ctrl Pts',(56.5097077166323,-61.8115034765981,
-217.524004303589));
#208879=CARTESIAN_POINT('Ctrl Pts',(56.5015608313522,-61.7955189925656,
-217.539739451313));
#208880=CARTESIAN_POINT('Ctrl Pts',(56.4931762425887,-61.7798627597669,
-217.555443322554));
#208881=CARTESIAN_POINT('Ctrl Pts',(56.484552572944,-61.7645370401173,-217.571115950688));
#208882=CARTESIAN_POINT('Ctrl Pts',(56.4802407381216,-61.7568741802925,
-217.578952264755));
#208883=CARTESIAN_POINT('Ctrl Pts',(56.4758692047043,-61.7492938920849,
-217.586780750714));
#208884=CARTESIAN_POINT('Ctrl Pts',(56.4714378241961,-61.7417964317611,
-217.594601409107));
#208885=CARTESIAN_POINT('Ctrl Pts',(56.4688298172435,-61.7373839403005,
-217.599204112807));
#208886=CARTESIAN_POINT('Ctrl Pts',(56.4664773451866,-61.7334599236759,
-217.603321244088));
#208887=CARTESIAN_POINT('Ctrl Pts',(56.4638952029632,-61.7292104003187,
-217.607804843996));
#208888=CARTESIAN_POINT('Ctrl Pts',(56.4620899125892,-61.7262393696988,
-217.610939527935));
#208889=CARTESIAN_POINT('Ctrl Pts',(56.4601717903347,-61.7231097076094,
-217.614253458791));
#208890=CARTESIAN_POINT('Ctrl Pts',(56.4579637271793,-61.719553010382,-217.618039957184));
#208891=CARTESIAN_POINT('Ctrl Pts',(56.4578997107073,-61.7194498941248,
-217.618149735869));
#208892=CARTESIAN_POINT('Ctrl Pts',(56.4578356866977,-61.7193468013413,
-217.61825950554));
#208893=CARTESIAN_POINT('Ctrl Pts',(56.4577716551528,-61.7192437320224,
-217.618369266201));
#208894=CARTESIAN_POINT('Ctrl Pts',(56.4421392669783,-61.6940808282613,
-217.64516576577));
#208895=CARTESIAN_POINT('Ctrl Pts',(56.4259894997883,-61.6701881268128,
-217.671554538388));
#208896=CARTESIAN_POINT('Ctrl Pts',(56.4093342638972,-61.6475961080088,
-217.697509113608));
#208897=CARTESIAN_POINT('Ctrl Pts',(56.3906581150786,-61.6222628189425,
-217.726612964943));
#208898=CARTESIAN_POINT('Ctrl Pts',(56.371347168254,-61.5985638219521,-217.755171020173));
#208899=CARTESIAN_POINT('Ctrl Pts',(56.3513931964498,-61.5764978346059,
-217.783190968782));
#208900=CARTESIAN_POINT('Ctrl Pts',(56.3403344621818,-61.5642685955942,
-217.798719965661));
#208901=CARTESIAN_POINT('Ctrl Pts',(56.3290777206293,-61.5525403034329,
-217.814084430147));
#208902=CARTESIAN_POINT('Ctrl Pts',(56.317617496657,-61.5413100898162,-217.829290220593));
#208903=CARTESIAN_POINT('Ctrl Pts',(56.2843115039728,-61.5086725590434,
-217.873481673272));
#208904=CARTESIAN_POINT('Ctrl Pts',(56.2493216160993,-61.4802753388256,
-217.916287262279));
#208905=CARTESIAN_POINT('Ctrl Pts',(56.2126168425407,-61.4561551423685,
-217.957709313443));
#208906=CARTESIAN_POINT('Ctrl Pts',(56.2074534717953,-61.4527620818838,
-217.963536277798));
#208907=CARTESIAN_POINT('Ctrl Pts',(56.2022561580052,-61.4494536957759,
-217.969335844824));
#208908=CARTESIAN_POINT('Ctrl Pts',(56.1970247680347,-61.4462301002552,
-217.975108045127));
#208909=CARTESIAN_POINT('Ctrl Pts',(56.189954819578,-61.4418735804193,-217.982908870311));
#208910=CARTESIAN_POINT('Ctrl Pts',(56.1828226665242,-61.4376719457195,
-217.990659675144));
#208911=CARTESIAN_POINT('Ctrl Pts',(56.1756278034111,-61.4336259639,-217.998360366589));
#208912=CARTESIAN_POINT('Ctrl Pts',(56.1719130982625,-61.4315370249918,
-218.002336230718));
#208913=CARTESIAN_POINT('Ctrl Pts',(56.1685141252281,-61.4296717765924,
-218.005945833167));
#208914=CARTESIAN_POINT('Ctrl Pts',(56.164919310722,-61.427743320513,-218.009736234828));
#208915=CARTESIAN_POINT('Ctrl Pts',(56.1615514734821,-61.4259366275144,
-218.013287309813));
#208916=CARTESIAN_POINT('Ctrl Pts',(56.1580118462168,-61.4240742515902,
-218.0169971257));
#208917=CARTESIAN_POINT('Ctrl Pts',(56.1538562118344,-61.4219533837318,
-218.021312277383));
#208918=CARTESIAN_POINT('Ctrl Pts',(56.1535326322412,-61.4217882417833,
-218.021648277834));
#208919=CARTESIAN_POINT('Ctrl Pts',(56.1532089858838,-61.4216234325919,
-218.021984122385));
#208920=CARTESIAN_POINT('Ctrl Pts',(56.152885272635,-61.4214589557602,-218.022319811373));
#208921=CARTESIAN_POINT('Ctrl Pts',(56.1326266942832,-61.4111656891305,
-218.04332785384));
#208922=CARTESIAN_POINT('Ctrl Pts',(56.1120734784841,-61.4022192130818,
-218.063722287668));
#208923=CARTESIAN_POINT('Ctrl Pts',(56.0912527901401,-61.3945894700681,
-218.083499993318));
#208924=CARTESIAN_POINT('Ctrl Pts',(56.0770726973867,-61.3893931738732,
-218.096969754544));
#208925=CARTESIAN_POINT('Ctrl Pts',(56.0627674817464,-61.3848077257068,
-218.110154174073));
#208926=CARTESIAN_POINT('Ctrl Pts',(56.0483341812414,-61.3808286563396,
-218.123057646765));
#208927=CARTESIAN_POINT('Ctrl Pts',(56.0303519758079,-61.3758712009903,
-218.139133865552));
#208928=CARTESIAN_POINT('Ctrl Pts',(56.0121738273229,-61.3718554913409,
-218.15477159619));
#208929=CARTESIAN_POINT('Ctrl Pts',(55.9937942323692,-61.3687879496844,
-218.169970023791));
#208930=CARTESIAN_POINT('Ctrl Pts',(55.9862609286416,-61.3675306465146,
-218.176199452219));
#208931=CARTESIAN_POINT('Ctrl Pts',(55.9789241937587,-61.3664673725087,
-218.182166842088));
#208932=CARTESIAN_POINT('Ctrl Pts',(55.9715043320131,-61.3655468829179,
-218.188106246611));
#208933=CARTESIAN_POINT('Ctrl Pts',(55.9643409032318,-61.3646582057628,
-218.193840383278));
#208934=CARTESIAN_POINT('Ctrl Pts',(55.9570998422772,-61.3639025843755,
-218.199548566063));
#208935=CARTESIAN_POINT('Ctrl Pts',(55.9495121619786,-61.3632758832898,
-218.205428014337));
#208936=CARTESIAN_POINT('Ctrl Pts',(55.9457841879237,-61.3629679729278,
-218.208316700966));
#208937=CARTESIAN_POINT('Ctrl Pts',(55.9419722879021,-61.362691833393,-218.211246512342));
#208938=CARTESIAN_POINT('Ctrl Pts',(55.9380430218637,-61.3624511630172,
-218.214239363226));
#208939=CARTESIAN_POINT('Ctrl Pts',(55.9375347347342,-61.3624200300643,
-218.214626516341));
#208940=CARTESIAN_POINT('Ctrl Pts',(55.9370262986849,-61.3623896074125,
-218.215013338391));
#208941=CARTESIAN_POINT('Ctrl Pts',(55.9365177134434,-61.3623598955499,
-218.21539982926));
#208942=CARTESIAN_POINT('Ctrl Pts',(55.9168041387,-61.3612082163902,-218.230380831454));
#208943=CARTESIAN_POINT('Ctrl Pts',(55.8970064047387,-61.3611339147912,
-218.244756879731));
#208944=CARTESIAN_POINT('Ctrl Pts',(55.8771158279607,-61.3621037947684,
-218.258552765903));
#208945=CARTESIAN_POINT('Ctrl Pts',(55.8615464471865,-61.3628629698712,
-218.26935151786));
#208946=CARTESIAN_POINT('Ctrl Pts',(55.8459239121599,-61.3642624475839,
-218.27979178035));
#208947=CARTESIAN_POINT('Ctrl Pts',(55.8302484900842,-61.366294962689,-218.289876937764));
#208948=CARTESIAN_POINT('Ctrl Pts',(55.8257068705157,-61.3668838406363,
-218.292798897252));
#208949=CARTESIAN_POINT('Ctrl Pts',(55.8211607962849,-61.3675259035511,
-218.29569103093));
#208950=CARTESIAN_POINT('Ctrl Pts',(55.8166102389797,-61.3682210877797,
-218.298553376832));
#208951=CARTESIAN_POINT('Ctrl Pts',(55.8128092045475,-61.3688017681255,
-218.300944265376));
#208952=CARTESIAN_POINT('Ctrl Pts',(55.8089983934449,-61.3694205155333,
-218.303318560299));
#208953=CARTESIAN_POINT('Ctrl Pts',(55.8051757780505,-61.3700780867166,
-218.30567724614));
#208954=CARTESIAN_POINT('Ctrl Pts',(55.7983202521378,-61.3712573830416,
-218.309907342614));
#208955=CARTESIAN_POINT('Ctrl Pts',(55.7914313802385,-61.3725609532495,
-218.314084260537));
#208956=CARTESIAN_POINT('Ctrl Pts',(55.7845238850248,-61.3739877414227,
-218.318197921959));
#208957=CARTESIAN_POINT('Ctrl Pts',(55.7688812052958,-61.3772188389109,
-218.327513699409));
#208958=CARTESIAN_POINT('Ctrl Pts',(55.7531422004866,-61.3810931503088,
-218.336498652793));
#208959=CARTESIAN_POINT('Ctrl Pts',(55.7374922209247,-61.3855480998269,
-218.345056637219));
#208960=CARTESIAN_POINT('Ctrl Pts',(55.7335797260343,-61.3866618372065,
-218.347196133325));
#208961=CARTESIAN_POINT('Ctrl Pts',(55.7296728414405,-61.3878108496662,
-218.349309539776));
#208962=CARTESIAN_POINT('Ctrl Pts',(55.7257744241213,-61.3889940773438,
-218.351395437214));
#208963=CARTESIAN_POINT('Ctrl Pts',(55.7140791721637,-61.3925437603767,
-218.357653129527));
#208964=CARTESIAN_POINT('Ctrl Pts',(55.7024601151168,-61.396401379636,-218.3636632402));
#208965=CARTESIAN_POINT('Ctrl Pts',(55.6909944590457,-61.4005387214182,
-218.369387227857));
#208966=CARTESIAN_POINT('Ctrl Pts',(55.6904721203629,-61.4007272055,-218.369647994459));
#208967=CARTESIAN_POINT('Ctrl Pts',(55.6899496363347,-61.400916414908,-218.369908412714));
#208968=CARTESIAN_POINT('Ctrl Pts',(55.6894270067505,-61.4011063509032,
-218.370168481955));
#208969=CARTESIAN_POINT('Ctrl Pts',(55.6619133365653,-61.4111054716716,
-218.383859745449));
#208970=CARTESIAN_POINT('Ctrl Pts',(55.6344763347929,-61.4229456905876,
-218.396340222171));
#208971=CARTESIAN_POINT('Ctrl Pts',(55.6070891104916,-61.4365888112143,
-218.407649991647));
#208972=CARTESIAN_POINT('Ctrl Pts',(55.5943945396522,-61.4429126927205,
-218.412892314425));
#208973=CARTESIAN_POINT('Ctrl Pts',(55.5817109693076,-61.4496244068266,
-218.417882581383));
#208974=CARTESIAN_POINT('Ctrl Pts',(55.5690375149754,-61.456722141651,-218.422622187911));
#208975=CARTESIAN_POINT('Ctrl Pts',(55.5487702728249,-61.4680727574056,
-218.430201712062));
#208976=CARTESIAN_POINT('Ctrl Pts',(55.5285322537927,-61.4804082518478,
-218.437139243937));
#208977=CARTESIAN_POINT('Ctrl Pts',(55.5083252248452,-61.4937253997328,
-218.443433751089));
#208978=CARTESIAN_POINT('Ctrl Pts',(55.5005249296046,-61.498866070612,-218.445863549864));
#208979=CARTESIAN_POINT('Ctrl Pts',(55.4924700861797,-61.5043278139308,
-218.448275734037));
#208980=CARTESIAN_POINT('Ctrl Pts',(55.4844646831107,-61.5099172845121,
-218.450571066518));
#208981=CARTESIAN_POINT('Ctrl Pts',(55.4761777049345,-61.5157033542859,
-218.452947133034));
#208982=CARTESIAN_POINT('Ctrl Pts',(55.4679439040137,-61.5216261860161,
-218.455197900852));
#208983=CARTESIAN_POINT('Ctrl Pts',(55.460084220559,-61.5274306880095,-218.457250847136));
#208984=CARTESIAN_POINT('Ctrl Pts',(55.4558674763759,-61.5305448210606,
-218.458352259089));
#208985=CARTESIAN_POINT('Ctrl Pts',(55.4517581179666,-61.5336242111068,
-218.45939738176));
#208986=CARTESIAN_POINT('Ctrl Pts',(55.447803718,-61.5366253992586,-218.46037904842));
#208987=CARTESIAN_POINT('Ctrl Pts',(55.4234882934493,-61.555079567953,-218.466415271821));
#208988=CARTESIAN_POINT('Ctrl Pts',(55.3994642092221,-61.5747880095429,
-218.471443614322));
#208989=CARTESIAN_POINT('Ctrl Pts',(55.3756994679743,-61.5957362573536,
-218.475492346442));
#208990=CARTESIAN_POINT('Ctrl Pts',(55.3515266265266,-61.6170442391092,
-218.479610605446));
#208991=CARTESIAN_POINT('Ctrl Pts',(55.3276213481284,-61.6396363978418,
-218.482715013696));
#208992=CARTESIAN_POINT('Ctrl Pts',(55.3039893611285,-61.6635080810643,
-218.48479891848));
#208993=CARTESIAN_POINT('Ctrl Pts',(55.2819264708097,-61.6857947524588,
-218.486744457917));
#208994=CARTESIAN_POINT('Ctrl Pts',(55.2601016111223,-61.7091979209098,
-218.487799869925));
#208995=CARTESIAN_POINT('Ctrl Pts',(55.2385592394913,-61.7337037475461,
-218.487935855327));
#208996=CARTESIAN_POINT('Ctrl Pts',(55.23702716172,-61.7354465840777,-218.487945526509));
#208997=CARTESIAN_POINT('Ctrl Pts',(55.2354965312477,-61.737194988746,-218.487950538905));
#208998=CARTESIAN_POINT('Ctrl Pts',(55.2339673727997,-61.7389489519143,
-218.487950878257));
#208999=CARTESIAN_POINT('Ctrl Pts',(48.9443109379934,-69.7210624363875,
-217.233400031701));
#209000=CARTESIAN_POINT('Ctrl Pts',(49.0991171386076,-69.4468461963775,
-217.336253844649));
#209001=CARTESIAN_POINT('Ctrl Pts',(49.2925903552098,-69.4989817480832,
-217.60005));
#209002=CARTESIAN_POINT('Ctrl Pts',(49.130620489061,-69.7720396651474,-217.086285690494));
#209003=CARTESIAN_POINT('Ctrl Pts',(49.2856293770243,-69.4971059616069,
-217.188797196021));
#209004=CARTESIAN_POINT('Ctrl Pts',(49.479508186842,-69.5493508092223,-217.453006109745));
#209005=CARTESIAN_POINT('Ctrl Pts',(49.3167847015304,-69.8229858522605,
-216.938985563531));
#209006=CARTESIAN_POINT('Ctrl Pts',(49.4718979894171,-69.5473000765824,
-217.041226996676));
#209007=CARTESIAN_POINT('Ctrl Pts',(49.6662875276291,-69.5996825510014,
-217.305773775928));
#209008=CARTESIAN_POINT('Ctrl Pts',(49.502798597092,-69.8738997057058,-216.791493525167));
#209009=CARTESIAN_POINT('Ctrl Pts',(49.6579114178628,-69.5974254266744,
-216.893543128263));
#209010=CARTESIAN_POINT('Ctrl Pts',(49.8529236261983,-69.6499756930601,
-217.158346534073));
#209011=CARTESIAN_POINT('',(49.8529236261983,-69.6499756930601,-217.158346534073));
#209012=CARTESIAN_POINT('',(49.5029673643273,-69.8740806799455,-216.790758026401));
#209013=CARTESIAN_POINT('Origin',(49.7228284492359,-70.13275436381,-217.158346534073));
#209014=CARTESIAN_POINT('Origin',(-167.970418940429,-23.6135530814242,73.4534718919959));
#209015=CARTESIAN_POINT('Origin',(-165.63543440526,-11.5819668880935,75.4526175248521));
#209016=CARTESIAN_POINT('Ctrl Pts',(56.7788252534563,-62.6825329319095,
-216.79113809033));
#209017=CARTESIAN_POINT('Ctrl Pts',(56.5025836743465,-62.8382452661243,
-216.892152466627));
#209018=CARTESIAN_POINT('Ctrl Pts',(56.5555093174817,-63.0368943169927,
-217.153871927429));
#209019=CARTESIAN_POINT('Ctrl Pts',(56.7295803718938,-62.4998572980931,
-216.940045714159));
#209020=CARTESIAN_POINT('Ctrl Pts',(56.4539126170321,-62.6555652121921,
-217.041204177849));
#209021=CARTESIAN_POINT('Ctrl Pts',(56.5067115045409,-62.8537385034605,
-217.302758005793));
#209022=CARTESIAN_POINT('Ctrl Pts',(56.680302877991,-62.3170582944071,-217.088794981881));
#209023=CARTESIAN_POINT('Ctrl Pts',(56.4051889499832,-62.4726876949562,
-217.190156301151));
#209024=CARTESIAN_POINT('Ctrl Pts',(56.4578811804683,-62.6704606639105,
-217.451483035533));
#209025=CARTESIAN_POINT('Ctrl Pts',(56.6309943627598,-62.1341374253209,
-217.237388612086));
#209026=CARTESIAN_POINT('Ctrl Pts',(56.3564132949791,-62.2896150482124,
-217.339009989763));
#209027=CARTESIAN_POINT('Ctrl Pts',(56.4090189474476,-62.4870630585555,
-217.60005));
#209028=CARTESIAN_POINT('',(56.7789323645482,-62.6826309921534,-216.790388211429));
#209029=CARTESIAN_POINT('',(56.5555093174817,-63.0368943169928,-217.153871927429));
#209030=CARTESIAN_POINT('Origin',(57.0386554992377,-62.9081707097771,-217.153871927429));
#209031=CARTESIAN_POINT('Origin',(-11.7909588194732,193.492081547376,120.824020637011));
#209032=CARTESIAN_POINT('Origin',(-10.1481943050527,195.398995247496,121.950798030302));
#209033=CARTESIAN_POINT('Ctrl Pts',(49.502798597092,-69.8738997057057,-216.791493525167));
#209034=CARTESIAN_POINT('Ctrl Pts',(49.6579114178629,-69.5974254266743,
-216.893543128263));
#209035=CARTESIAN_POINT('Ctrl Pts',(49.8529236261983,-69.6499756930601,
-217.158346534073));
#209036=CARTESIAN_POINT('Ctrl Pts',(49.8904699761689,-69.961109459285,-216.497441344741));
#209037=CARTESIAN_POINT('Ctrl Pts',(50.0485994592274,-69.7027047875172,
-216.601129210477));
#209038=CARTESIAN_POINT('Ctrl Pts',(50.2627282054337,-69.7604064193654,
-216.834634459542));
#209039=CARTESIAN_POINT('Ctrl Pts',(50.234208458361,-70.0386649773616,-216.158971875201));
#209040=CARTESIAN_POINT('Ctrl Pts',(50.4024671800086,-69.798062114882,-216.256560731386));
#209041=CARTESIAN_POINT('Ctrl Pts',(50.6264190422318,-69.8584107982651,
-216.462106475915));
#209042=CARTESIAN_POINT('Ctrl Pts',(50.5261810352842,-70.1046957156775,
-215.770277860521));
#209043=CARTESIAN_POINT('Ctrl Pts',(50.704122433655,-69.8793496612891,-215.854989245265));
#209044=CARTESIAN_POINT('Ctrl Pts',(50.9355365677156,-69.9417092155658,
-216.034373717099));
#209045=CARTESIAN_POINT('',(50.9355365677156,-69.9417092155658,-216.034373717099));
#209046=CARTESIAN_POINT('',(50.5260891840881,-70.1045902648202,-215.770190216137));
#209047=CARTESIAN_POINT('Origin',(50.8054413907531,-70.4244878863158,-216.034373717099));
#209048=CARTESIAN_POINT('Ctrl Pts',(49.503005485031,-69.8741215579355,-216.790591893854));
#209049=CARTESIAN_POINT('Ctrl Pts',(49.5036598824408,-69.8736705791977,
-216.790517784408));
#209050=CARTESIAN_POINT('Ctrl Pts',(49.507504324357,-69.8740966385711,-216.787917197217));
#209051=CARTESIAN_POINT('Ctrl Pts',(49.5145301680683,-69.8753873628897,
-216.7827677998));
#209052=CARTESIAN_POINT('Ctrl Pts',(49.5215382096988,-69.8766748167714,
-216.777631449924));
#209053=CARTESIAN_POINT('Ctrl Pts',(49.5317116207978,-69.8788226274945,
-216.769959125464));
#209054=CARTESIAN_POINT('Ctrl Pts',(49.5450246500239,-69.8817948135687,
-216.759685963983));
#209055=CARTESIAN_POINT('Ctrl Pts',(49.5540742065074,-69.8838151626043,
-216.752702763277));
#209056=CARTESIAN_POINT('Ctrl Pts',(49.5645741163918,-69.8862159430578,
-216.744516923557));
#209057=CARTESIAN_POINT('Ctrl Pts',(49.5765113792548,-69.888979213311,-216.735097065284));
#209058=CARTESIAN_POINT('Ctrl Pts',(49.5939391216258,-69.8930134347759,
-216.721344594134));
#209059=CARTESIAN_POINT('Ctrl Pts',(49.6144315139314,-69.8978215885242,
-216.704963518013));
#209060=CARTESIAN_POINT('Ctrl Pts',(49.6379310279013,-69.9033253866201,
-216.685823358771));
#209061=CARTESIAN_POINT('Ctrl Pts',(49.6461891503198,-69.9052595133642,
-216.679097186548));
#209062=CARTESIAN_POINT('Ctrl Pts',(49.6548184385922,-69.907279295187,-216.672029942124));
#209063=CARTESIAN_POINT('Ctrl Pts',(49.6638157326524,-69.9093804828061,
-216.664614872801));
#209064=CARTESIAN_POINT('Ctrl Pts',(49.6811158390666,-69.9134206719079,
-216.650357087349));
#209065=CARTESIAN_POINT('Ctrl Pts',(49.699776875429,-69.9177622530644,-216.634813749881));
#209066=CARTESIAN_POINT('Ctrl Pts',(49.7197723867992,-69.9223700050012,
-216.617931309463));
#209067=CARTESIAN_POINT('Ctrl Pts',(49.7297701424842,-69.9246738809696,
-216.609490089255));
#209068=CARTESIAN_POINT('Ctrl Pts',(49.7401014354786,-69.9270442043552,
-216.600713971417));
#209069=CARTESIAN_POINT('Ctrl Pts',(49.750762420894,-69.9294759003914,-216.59159562903));
#209070=CARTESIAN_POINT('Ctrl Pts',(49.7560929136017,-69.9306917484095,
-216.587036457837));
#209071=CARTESIAN_POINT('Ctrl Pts',(49.7615058242863,-69.9319229335857,
-216.582391722711));
#209072=CARTESIAN_POINT('Ctrl Pts',(49.7670006367179,-69.9331687794098,
-216.577660468699));
#209073=CARTESIAN_POINT('Ctrl Pts',(49.7697480429336,-69.9337917023218,
-216.575294841692));
#209074=CARTESIAN_POINT('Ctrl Pts',(49.772515924257,-69.9344182900113,-216.572907584482));
#209075=CARTESIAN_POINT('Ctrl Pts',(49.7753042138934,-69.9350484551439,
-216.570498575359));
#209076=CARTESIAN_POINT('Ctrl Pts',(49.7780925035297,-69.9356786202765,
-216.568089566236));
#209077=CARTESIAN_POINT('Ctrl Pts',(49.7822817015456,-69.9366233157115,
-216.564461979738));
#209078=CARTESIAN_POINT('Ctrl Pts',(49.7837302395077,-69.9369495938251,
-216.563206168813));
#209079=CARTESIAN_POINT('Ctrl Pts',(49.8300834542953,-69.9473904934593,
-216.523020219228));
#209080=CARTESIAN_POINT('Ctrl Pts',(49.8753773599085,-69.9575976012502,
-216.482374323618));
#209081=CARTESIAN_POINT('Ctrl Pts',(49.9195996591217,-69.9675665793152,
-216.441323275821));
#209082=CARTESIAN_POINT('Ctrl Pts',(49.9417108087283,-69.9725510683477,
-216.420797751923));
#209083=CARTESIAN_POINT('Ctrl Pts',(49.9635540819862,-69.9774760543192,
-216.400170973799));
#209084=CARTESIAN_POINT('Ctrl Pts',(49.9851282539123,-69.98234128434,-216.379449755809));
#209085=CARTESIAN_POINT('Ctrl Pts',(49.9994083221236,-69.9855616080122,
-216.365734262703));
#209086=CARTESIAN_POINT('Ctrl Pts',(50.0131165140574,-69.9886508257923,
-216.352422200884));
#209087=CARTESIAN_POINT('Ctrl Pts',(50.0271549209438,-69.9918184673918,
-216.33863391884));
#209088=CARTESIAN_POINT('Ctrl Pts',(50.0343255866789,-69.9934364643101,
-216.331591014157));
#209089=CARTESIAN_POINT('Ctrl Pts',(50.0415820727045,-69.9950744894472,
-216.324423275089));
#209090=CARTESIAN_POINT('Ctrl Pts',(50.0490423476813,-69.99675757341,-216.317009695042));
#209091=CARTESIAN_POINT('Ctrl Pts',(50.1373050109276,-70.0166701736136,
-216.229299480458));
#209092=CARTESIAN_POINT('Ctrl Pts',(50.221254127075,-70.0356392133376,-216.139590511556));
#209093=CARTESIAN_POINT('Ctrl Pts',(50.3007842172754,-70.0536146832101,
-216.048306803414));
#209094=CARTESIAN_POINT('Ctrl Pts',(50.3803143074759,-70.0715901530826,
-215.957023095271));
#209095=CARTESIAN_POINT('Ctrl Pts',(50.4554254383405,-70.0885721436241,
-215.864165404149));
#209096=CARTESIAN_POINT('Ctrl Pts',(50.5260568509089,-70.1045534073734,
-215.770160360609));
#209097=CARTESIAN_POINT('Ctrl Pts',(50.9355365677156,-69.9417092155658,
-216.034373717099));
#209098=CARTESIAN_POINT('Ctrl Pts',(50.8116343558521,-69.9083210790241,
-216.205819948822));
#209099=CARTESIAN_POINT('Ctrl Pts',(50.679045627584,-69.8725921723587,-216.368291840782));
#209100=CARTESIAN_POINT('Ctrl Pts',(50.5382668565233,-69.8346562811454,
-216.522302092548));
#209101=CARTESIAN_POINT('Ctrl Pts',(50.3916404967015,-69.7951446303951,
-216.682709534817));
#209102=CARTESIAN_POINT('Ctrl Pts',(50.2361294127338,-69.7532387981491,
-216.833937733262));
#209103=CARTESIAN_POINT('Ctrl Pts',(50.0722553986623,-69.7090793931218,
-216.976525935758));
#209104=CARTESIAN_POINT('Ctrl Pts',(50.0007248884674,-69.6898039467406,
-217.03876525375));
#209105=CARTESIAN_POINT('Ctrl Pts',(49.9276005183839,-69.6700990002659,
-217.099357901494));
#209106=CARTESIAN_POINT('Ctrl Pts',(49.8529236261983,-69.6499756930601,
-217.158346534073));
#209107=CARTESIAN_POINT('Ctrl Pts',(56.9946437140725,-63.654341638523,-215.806005173342));
#209108=CARTESIAN_POINT('Ctrl Pts',(56.7673159108321,-63.8318809481279,
-215.890327243741));
#209109=CARTESIAN_POINT('Ctrl Pts',(56.8293274051384,-64.0646324794683,
-216.070020447202));
#209110=CARTESIAN_POINT('Ctrl Pts',(56.932619322676,-63.3755293978699,-216.178019997802));
#209111=CARTESIAN_POINT('Ctrl Pts',(56.6905874263868,-63.5438912383415,
-216.274438039323));
#209112=CARTESIAN_POINT('Ctrl Pts',(56.7507244929534,-63.769607365439,-216.47928372567));
#209113=CARTESIAN_POINT('Ctrl Pts',(56.860146560067,-63.0493377881462,-216.504716595751));
#209114=CARTESIAN_POINT('Ctrl Pts',(56.6011588045338,-63.2082333266141,
-216.606979895655));
#209115=CARTESIAN_POINT('Ctrl Pts',(56.6588023342389,-63.4245903094199,
-216.83871657078));
#209116=CARTESIAN_POINT('Ctrl Pts',(56.7788252534563,-62.6825329319096,
-216.79113809033));
#209117=CARTESIAN_POINT('Ctrl Pts',(56.5025836743465,-62.8382452661242,
-216.892152466627));
#209118=CARTESIAN_POINT('Ctrl Pts',(56.5555093174817,-63.0368943169927,
-217.153871927429));
#209119=CARTESIAN_POINT('',(56.9945465422419,-63.6542557031434,-215.80592400831));
#209120=CARTESIAN_POINT('',(56.8293274051384,-64.0646324794683,-216.070020447202));
#209121=CARTESIAN_POINT('Origin',(57.3124735868944,-63.9359088722526,-216.070020447202));
#209122=CARTESIAN_POINT('Ctrl Pts',(56.5555093174817,-63.0368943169928,
-217.153871927428));
#209123=CARTESIAN_POINT('Ctrl Pts',(56.6017653589551,-63.2105099443389,
-217.012740999606));
#209124=CARTESIAN_POINT('Ctrl Pts',(56.6457145720425,-63.3754672117248,
-216.862817131852));
#209125=CARTESIAN_POINT('Ctrl Pts',(56.6872100613026,-63.5312147675134,
-216.70354056544));
#209126=CARTESIAN_POINT('Ctrl Pts',(56.7270307212971,-63.6806760842641,
-216.550692675001));
#209127=CARTESIAN_POINT('Ctrl Pts',(56.7645917777123,-63.8216562928075,
-216.389231897198));
#209128=CARTESIAN_POINT('Ctrl Pts',(56.7997545451807,-63.953634856878,-216.218629552566));
#209129=CARTESIAN_POINT('Ctrl Pts',(56.8098094620337,-63.9913745907972,
-216.169845212944));
#209130=CARTESIAN_POINT('Ctrl Pts',(56.8196682125205,-64.0283780415051,
-216.120313149194));
#209131=CARTESIAN_POINT('Ctrl Pts',(56.8293274051384,-64.0646324794683,
-216.070020447202));
#209132=CARTESIAN_POINT('Ctrl Pts',(56.9944699555807,-63.6541878226818,
-215.805860862997));
#209133=CARTESIAN_POINT('Ctrl Pts',(56.9794459967772,-63.5866902802209,
-215.895894129132));
#209134=CARTESIAN_POINT('Ctrl Pts',(56.9635084836788,-63.5150703368537,
-215.984953436998));
#209135=CARTESIAN_POINT('Ctrl Pts',(56.9466685708699,-63.4393805477762,
-216.072641385784));
#209136=CARTESIAN_POINT('Ctrl Pts',(56.9382486144655,-63.4015356532375,
-216.116485360177));
#209137=CARTESIAN_POINT('Ctrl Pts',(56.9296030730276,-63.3626733585993,
-216.159987654482));
#209138=CARTESIAN_POINT('Ctrl Pts',(56.9207359629282,-63.3228030795314,
-216.20310039353));
#209139=CARTESIAN_POINT('Ctrl Pts',(56.9163024078785,-63.3028679399975,
-216.224656763054));
#209140=CARTESIAN_POINT('Ctrl Pts',(56.91181348634,-63.2826808269247,-216.246115770319));
#209141=CARTESIAN_POINT('Ctrl Pts',(56.9072699345539,-63.2622431718491,
-216.267471425441));
#209142=CARTESIAN_POINT('Ctrl Pts',(56.9042193408906,-63.2485210918547,
-216.281809861373));
#209143=CARTESIAN_POINT('Ctrl Pts',(56.9010480846113,-63.2342431449902,
-216.296555148204));
#209144=CARTESIAN_POINT('Ctrl Pts',(56.897948704089,-63.2203010182936,-216.310790655394));
#209145=CARTESIAN_POINT('Ctrl Pts',(56.8964318697161,-63.2134777525306,
-216.317757501337));
#209146=CARTESIAN_POINT('Ctrl Pts',(56.8949327040015,-63.2067352855026,
-216.324602831575));
#209147=CARTESIAN_POINT('Ctrl Pts',(56.8934762334649,-63.2001801107107,
-216.331222459184));
#209148=CARTESIAN_POINT('Ctrl Pts',(56.8846112168146,-63.1602810999074,
-216.371513771297));
#209149=CARTESIAN_POINT('Ctrl Pts',(56.8755237821599,-63.1193619943915,
-216.411526369275));
#209150=CARTESIAN_POINT('Ctrl Pts',(56.8662137807326,-63.077429139806,-216.45120864926));
#209151=CARTESIAN_POINT('Ctrl Pts',(56.861558780019,-63.0564627125132,-216.471049789252));
#209152=CARTESIAN_POINT('Ctrl Pts',(56.8568481595931,-63.0352428671797,
-216.490808375499));
#209153=CARTESIAN_POINT('Ctrl Pts',(56.8520821602383,-63.0137706793198,
-216.510477896976));
#209154=CARTESIAN_POINT('Ctrl Pts',(56.8496991605609,-63.0030345853899,
-216.520312657714));
#209155=CARTESIAN_POINT('Ctrl Pts',(56.8473023177016,-62.9922354071859,
-216.530125154026));
#209156=CARTESIAN_POINT('Ctrl Pts',(56.8448916738711,-62.9813732913107,
-216.539914577476));
#209157=CARTESIAN_POINT('Ctrl Pts',(56.8436863519558,-62.9759422333731,
-216.5448092892));
#209158=CARTESIAN_POINT('Ctrl Pts',(56.8424775798923,-62.9704954411003,
-216.549698232825));
#209159=CARTESIAN_POINT('Ctrl Pts',(56.8412653639348,-62.9650329338615,
-216.55458130727));
#209160=CARTESIAN_POINT('Ctrl Pts',(56.8403562019666,-62.9609360534324,
-216.558243613104));
#209161=CARTESIAN_POINT('Ctrl Pts',(56.839445102816,-62.9568303333417,-216.561902617535));
#209162=CARTESIAN_POINT('Ctrl Pts',(56.8385320693501,-62.9527157820021,
-216.56555827794));
#209163=CARTESIAN_POINT('Ctrl Pts',(56.8382277248615,-62.9513442648889,
-216.566776831409));
#209164=CARTESIAN_POINT('Ctrl Pts',(56.8382152206193,-62.9512879268144,
-216.566828027));
#209165=CARTESIAN_POINT('Ctrl Pts',(56.8376183912324,-62.94859828724,-216.569212822087));
#209166=CARTESIAN_POINT('Ctrl Pts',(56.8305025760161,-62.9165305328181,
-216.597646008419));
#209167=CARTESIAN_POINT('Ctrl Pts',(56.8238616028387,-62.8872265401915,
-216.623070944351));
#209168=CARTESIAN_POINT('Ctrl Pts',(56.8178173128131,-62.8607818805868,
-216.645667973915));
#209169=CARTESIAN_POINT('Ctrl Pts',(56.8117204483761,-62.8341072001847,
-216.668461556843));
#209170=CARTESIAN_POINT('Ctrl Pts',(56.8062304512243,-62.8103415608514,
-216.688378132289));
#209171=CARTESIAN_POINT('Ctrl Pts',(56.8014409140339,-62.7895571321941,
-216.705568966566));
#209172=CARTESIAN_POINT('Ctrl Pts',(56.7966107261207,-62.7685962977551,
-216.722905706347));
#209173=CARTESIAN_POINT('Ctrl Pts',(56.7924927406286,-62.750667289575,-216.737470473255));
#209174=CARTESIAN_POINT('Ctrl Pts',(56.7891544483765,-62.7358213501912,
-216.749380072365));
#209175=CARTESIAN_POINT('Ctrl Pts',(56.7858060768922,-62.7209305867902,
-216.761325629864));
#209176=CARTESIAN_POINT('Ctrl Pts',(56.7832419532595,-62.709141376279,-216.770600095729));
#209177=CARTESIAN_POINT('Ctrl Pts',(56.7815043823577,-62.7004854065422,
-216.777280214984));
#209178=CARTESIAN_POINT('Ctrl Pts',(56.7797629254889,-62.6918100782785,
-216.783975273901));
#209179=CARTESIAN_POINT('Ctrl Pts',(56.7788516311555,-62.6862819290349,
-216.788064444018));
#209180=CARTESIAN_POINT('Ctrl Pts',(56.7787891208614,-62.6839146946666,
-216.789582191217));
#209181=CARTESIAN_POINT('Ctrl Pts',(56.7787708428251,-62.6832225143423,
-216.790025981136));
#209182=CARTESIAN_POINT('Ctrl Pts',(56.7788249825049,-62.6828004720904,
-216.79024963763));
#209183=CARTESIAN_POINT('Ctrl Pts',(56.7789516318532,-62.6826486313781,
-216.79025332208));
#209184=CARTESIAN_POINT('Ctrl Pts',(51.9620199839905,-69.8524482833038,
-212.903250403248));
#209185=CARTESIAN_POINT('Ctrl Pts',(51.8928715700308,-69.8849735800753,
-212.914037308895));
#209186=CARTESIAN_POINT('Ctrl Pts',(51.8371967923162,-69.9365578441711,
-212.924798774573));
#209187=CARTESIAN_POINT('Ctrl Pts',(52.0023737441193,-69.8310690362166,
-213.304505435696));
#209188=CARTESIAN_POINT('Ctrl Pts',(51.941700685795,-69.8615494218525,-213.296380663458));
#209189=CARTESIAN_POINT('Ctrl Pts',(51.8900804694045,-69.9070006930946,
-213.289619354923));
#209190=CARTESIAN_POINT('Ctrl Pts',(51.9342823138335,-69.8685686407292,
-213.657783042067));
#209191=CARTESIAN_POINT('Ctrl Pts',(51.8593850051349,-69.9028934810734,
-213.636762861553));
#209192=CARTESIAN_POINT('Ctrl Pts',(51.8014625992089,-69.9580400304186,
-213.610486438733));
#209193=CARTESIAN_POINT('Ctrl Pts',(51.7621689112058,-69.9305269210584,
-214.242088767328));
#209194=CARTESIAN_POINT('Ctrl Pts',(51.6558225747516,-69.9634677621137,
-214.190398126914));
#209195=CARTESIAN_POINT('Ctrl Pts',(51.5789777052583,-70.0457813460658,
-214.141301452941));
#209196=CARTESIAN_POINT('Ctrl Pts',(51.6732637051828,-69.9557792147167,
-214.478511967556));
#209197=CARTESIAN_POINT('Ctrl Pts',(51.5497057881375,-69.985967309418,-214.415265918991));
#209198=CARTESIAN_POINT('Ctrl Pts',(51.4643785947433,-70.0826136343188,
-214.356059518454));
#209199=CARTESIAN_POINT('Ctrl Pts',(51.3492289962179,-70.0110328842746,
-215.2590218875));
#209200=CARTESIAN_POINT('Ctrl Pts',(51.1618526758825,-70.0201965830603,
-215.162496083505));
#209201=CARTESIAN_POINT('Ctrl Pts',(51.0486202117362,-70.1704592965568,
-215.065022277779));
#209202=CARTESIAN_POINT('Ctrl Pts',(51.0782728947073,-70.0027462486926,
-215.78151451348));
#209203=CARTESIAN_POINT('Ctrl Pts',(50.8352661021995,-69.9666501783504,
-215.659256381595));
#209204=CARTESIAN_POINT('Ctrl Pts',(50.7036055976657,-70.1752051070453,
-215.539933768453));
#209205=CARTESIAN_POINT('Ctrl Pts',(50.79511229761,-69.8965255868172,-216.289741858889));
#209206=CARTESIAN_POINT('Ctrl Pts',(50.5508501997346,-69.8033231077245,
-216.081892433387));
#209207=CARTESIAN_POINT('Ctrl Pts',(50.3485321404655,-70.0571221488448,
-216.001649432013));
#209208=CARTESIAN_POINT('',(51.9718267086745,-69.8471376007524,-213.236262748316));
#209209=CARTESIAN_POINT('',(51.8506357968709,-69.9286975784453,-213.227536544931));
#209210=CARTESIAN_POINT('Origin',(52.1871615786983,-70.2983923998978,-213.236262748316));
#209211=CARTESIAN_POINT('Ctrl Pts',(50.526181157749,-70.1046957431703,-215.770277696984));
#209212=CARTESIAN_POINT('Ctrl Pts',(50.5900491822617,-70.1190337938543,
-215.684989847738));
#209213=CARTESIAN_POINT('Ctrl Pts',(50.6579835771245,-70.130651334725,-215.593317406618));
#209214=CARTESIAN_POINT('Ctrl Pts',(50.7646990473915,-70.1424896494519,
-215.44560740904));
#209215=CARTESIAN_POINT('Ctrl Pts',(50.8192571781922,-70.1470086832376,
-215.36920511009));
#209216=CARTESIAN_POINT('Ctrl Pts',(50.8847365884144,-70.149516553765,-215.275553310463));
#209217=CARTESIAN_POINT('Ctrl Pts',(50.9178970323605,-70.1500380291522,
-215.227594876075));
#209218=CARTESIAN_POINT('Ctrl Pts',(50.9357693297152,-70.1501156065902,
-215.201599164668));
#209219=CARTESIAN_POINT('Ctrl Pts',(50.9441383948169,-70.1500961107514,
-215.189385131094));
#209220=CARTESIAN_POINT('Ctrl Pts',(50.9489276109694,-70.1500711879545,
-215.182385426043));
#209221=CARTESIAN_POINT('Ctrl Pts',(50.9507973949068,-70.150059025442,-215.179650830219));
#209222=CARTESIAN_POINT('Ctrl Pts',(50.9850227491289,-70.1498153761691,
-215.129579963741));
#209223=CARTESIAN_POINT('Ctrl Pts',(51.0361537920302,-70.1483467098581,
-215.05498416666));
#209224=CARTESIAN_POINT('Ctrl Pts',(51.1351942660711,-70.1398574995953,
-214.903171554453));
#209225=CARTESIAN_POINT('Ctrl Pts',(51.1719033536906,-70.135947513949,-214.84590539025));
#209226=CARTESIAN_POINT('Ctrl Pts',(51.2317676039139,-70.1276087918756,
-214.749763328443));
#209227=CARTESIAN_POINT('Ctrl Pts',(51.2628970020121,-70.1228178480742,
-214.699132199145));
#209228=CARTESIAN_POINT('Ctrl Pts',(51.3011167631323,-70.1159211083316,
-214.635539753149));
#209229=CARTESIAN_POINT('Ctrl Pts',(51.3178816154838,-70.1126596506502,
-214.607313326825));
#209230=CARTESIAN_POINT('Ctrl Pts',(51.3291411614471,-70.1104145156853,
-214.588279274963));
#209231=CARTESIAN_POINT('Ctrl Pts',(51.3354355945575,-70.1091261688492,
-214.577592011259));
#209232=CARTESIAN_POINT('Ctrl Pts',(51.4219363715995,-70.0910297574046,
-214.430175036717));
#209233=CARTESIAN_POINT('Ctrl Pts',(51.4883839419626,-70.0723789788218,
-214.306593959656));
#209234=CARTESIAN_POINT('Ctrl Pts',(51.569496385825,-70.0464887061108,-214.145707845131));
#209235=CARTESIAN_POINT('Ctrl Pts',(51.5934318573064,-70.038194487785,-214.096142505444));
#209236=CARTESIAN_POINT('Ctrl Pts',(51.6250789004642,-70.0267088171666,
-214.027984609541));
#209237=CARTESIAN_POINT('Ctrl Pts',(51.6398373799156,-70.0212036779678,
-213.995452202307));
#209238=CARTESIAN_POINT('Ctrl Pts',(51.6552677865945,-70.0152828821744,
-213.960216179522));
#209239=CARTESIAN_POINT('Ctrl Pts',(51.6625447127538,-70.012457719356,-213.943278765729));
#209240=CARTESIAN_POINT('Ctrl Pts',(51.6655703886093,-70.0112769379038,
-213.936165814877));
#209241=CARTESIAN_POINT('Ctrl Pts',(51.667566936517,-70.0104965286416,-213.931456288653));
#209242=CARTESIAN_POINT('Ctrl Pts',(51.6678426662331,-70.0103889860098,
-213.930809474077));
#209243=CARTESIAN_POINT('Ctrl Pts',(51.7236131045389,-69.9885217372769,
-213.798345974757));
#209244=CARTESIAN_POINT('Ctrl Pts',(51.7641862310625,-69.9702533041814,
-213.680412346262));
#209245=CARTESIAN_POINT('Ctrl Pts',(51.8000752575117,-69.9534191577125,
-213.546566643314));
#209246=CARTESIAN_POINT('Ctrl Pts',(51.8065101620132,-69.9503504498528,
-213.520473763259));
#209247=CARTESIAN_POINT('Ctrl Pts',(51.815081994581,-69.9462323856597,-213.482350651028));
#209248=CARTESIAN_POINT('Ctrl Pts',(51.8177782617349,-69.9449337383462,
-213.469834026062));
#209249=CARTESIAN_POINT('Ctrl Pts',(51.8240538444693,-69.9418920320008,
-213.438561955842));
#209250=CARTESIAN_POINT('Ctrl Pts',(51.8385687686859,-69.934807758839,-213.360902677902));
#209251=CARTESIAN_POINT('Ctrl Pts',(51.8472684687624,-69.9303859558978,
-213.285865302574));
#209252=CARTESIAN_POINT('Ctrl Pts',(51.8506358032439,-69.9286975854465,
-213.227536545096));
#209253=CARTESIAN_POINT('Ctrl Pts',(51.9718267086745,-69.8471376007524,
-213.236262748316));
#209254=CARTESIAN_POINT('Ctrl Pts',(51.9712180886111,-69.8474280289595,
-213.25115219161));
#209255=CARTESIAN_POINT('Ctrl Pts',(51.9704619947239,-69.8477893139844,
-213.266128674664));
#209256=CARTESIAN_POINT('Ctrl Pts',(51.9695578201616,-69.8482201770776,
-213.281192197065));
#209257=CARTESIAN_POINT('Ctrl Pts',(51.9668452964747,-69.849512766357,-213.326382764268));
#209258=CARTESIAN_POINT('Ctrl Pts',(51.9628004574897,-69.8514324567245,
-213.372356687621));
#209259=CARTESIAN_POINT('Ctrl Pts',(51.957403416313,-69.8539366328684,-213.419113967205));
#209260=CARTESIAN_POINT('Ctrl Pts',(51.953805388862,-69.8556060836309,-213.450285486928));
#209261=CARTESIAN_POINT('Ctrl Pts',(51.9496063062332,-69.857535073295,-213.481805164329));
#209262=CARTESIAN_POINT('Ctrl Pts',(51.9447991135993,-69.859707575833,-213.513672998779));
#209263=CARTESIAN_POINT('Ctrl Pts',(51.9423955172823,-69.8607938271019,
-213.529606916005));
#209264=CARTESIAN_POINT('Ctrl Pts',(51.9398398741415,-69.8619409124089,
-213.545627872515));
#209265=CARTESIAN_POINT('Ctrl Pts',(51.9371312039438,-69.8631465120197,
-213.561735868497));
#209266=CARTESIAN_POINT('Ctrl Pts',(51.9357768688449,-69.863749311825,-213.569789866489));
#209267=CARTESIAN_POINT('Ctrl Pts',(51.9343842753551,-69.8643667368211,
-213.577865624349));
#209268=CARTESIAN_POINT('Ctrl Pts',(51.9329532930758,-69.8649984740466,
-213.585963142108));
#209269=CARTESIAN_POINT('Ctrl Pts',(51.9318040898334,-69.8655058139895,
-213.59246615322));
#209270=CARTESIAN_POINT('Ctrl Pts',(51.9304882819738,-69.8660846575816,
-213.599761180333));
#209271=CARTESIAN_POINT('Ctrl Pts',(51.9293469843985,-69.8665849976042,
-213.605973625865));
#209272=CARTESIAN_POINT('Ctrl Pts',(51.9290671437927,-69.8667076785404,
-213.607496887247));
#209273=CARTESIAN_POINT('Ctrl Pts',(51.9287980217135,-69.8668255599709,
-213.608955159132));
#209274=CARTESIAN_POINT('Ctrl Pts',(51.9285450430171,-69.8669362930855,
-213.6103209751));
#209275=CARTESIAN_POINT('Ctrl Pts',(51.9259755968611,-69.8680609837394,
-213.624193252248));
#209276=CARTESIAN_POINT('Ctrl Pts',(51.9232746503919,-69.8692348882112,
-213.638224440989));
#209277=CARTESIAN_POINT('Ctrl Pts',(51.9204413918511,-69.8704558726239,
-213.652414541545));
#209278=CARTESIAN_POINT('Ctrl Pts',(51.9130092672967,-69.8736587247825,
-213.689637616408));
#209279=CARTESIAN_POINT('Ctrl Pts',(51.9046682050277,-69.8771859654199,
-213.727954683684));
#209280=CARTESIAN_POINT('Ctrl Pts',(51.8953968498963,-69.8809927158852,
-213.767364302023));
#209281=CARTESIAN_POINT('Ctrl Pts',(51.8940649868285,-69.8815395690993,
-213.773025633558));
#209282=CARTESIAN_POINT('Ctrl Pts',(51.8927139885145,-69.8820921380719,
-213.778709544735));
#209283=CARTESIAN_POINT('Ctrl Pts',(51.8913438570338,-69.8826502356811,
-213.784416065952));
#209284=CARTESIAN_POINT('Ctrl Pts',(51.8840719367677,-69.8856123173298,
-213.81470320837));
#209285=CARTESIAN_POINT('Ctrl Pts',(51.8762586474763,-69.8887317234872,
-213.845625996737));
#209286=CARTESIAN_POINT('Ctrl Pts',(51.8678939860897,-69.8919803770025,
-213.877184429624));
#209287=CARTESIAN_POINT('Ctrl Pts',(51.8637116553965,-69.8936047037601,
-213.892963646068));
#209288=CARTESIAN_POINT('Ctrl Pts',(51.8593914425586,-69.8952612418583,
-213.908901773702));
#209289=CARTESIAN_POINT('Ctrl Pts',(51.8549319444312,-69.8969457262148,
-213.924998812825));
#209290=CARTESIAN_POINT('Ctrl Pts',(51.8527021953674,-69.897787968393,-213.933047332387));
#209291=CARTESIAN_POINT('Ctrl Pts',(51.8504376220739,-69.898637188788,-213.941135579829));
#209292=CARTESIAN_POINT('Ctrl Pts',(51.8481380362862,-69.8994927979795,
-213.949263555208));
#209293=CARTESIAN_POINT('Ctrl Pts',(51.8461958706252,-69.9002154215058,
-213.956128215252));
#209294=CARTESIAN_POINT('Ctrl Pts',(51.8438732407178,-69.9010733451928,
-213.964258553209));
#209295=CARTESIAN_POINT('Ctrl Pts',(51.842070356574,-69.9017349392692,-213.970519352044));
#209296=CARTESIAN_POINT('Ctrl Pts',(51.8417385686673,-69.9018566935785,
-213.97167153775));
#209297=CARTESIAN_POINT('Ctrl Pts',(51.841424522012,-69.9019717967303,-213.972760460356));
#209298=CARTESIAN_POINT('Ctrl Pts',(51.8411339883627,-69.9020781818389,
-213.973766641235));
#209299=CARTESIAN_POINT('Ctrl Pts',(51.8387541055504,-69.902949626824,-213.982008690256));
#209300=CARTESIAN_POINT('Ctrl Pts',(51.8363363641231,-69.903827736172,-213.990295341577));
#209301=CARTESIAN_POINT('Ctrl Pts',(51.8338819984518,-69.9047112698955,
-213.998627680016));
#209302=CARTESIAN_POINT('Ctrl Pts',(51.8324808638191,-69.9052156567168,
-214.003384399072));
#209303=CARTESIAN_POINT('Ctrl Pts',(51.8310675260514,-69.9057218589305,
-214.008155744382));
#209304=CARTESIAN_POINT('Ctrl Pts',(51.8296420981419,-69.9062297402504,
-214.012941827738));
#209305=CARTESIAN_POINT('Ctrl Pts',(51.8153492654977,-69.9113222901152,
-214.060932110502));
#209306=CARTESIAN_POINT('Ctrl Pts',(51.7998409444251,-69.916585345507,-214.11040028011));
#209307=CARTESIAN_POINT('Ctrl Pts',(51.7830759342136,-69.9219270924958,
-214.161345223105));
#209308=CARTESIAN_POINT('Ctrl Pts',(51.7676354711688,-69.9268468059905,
-214.208265177207));
#209309=CARTESIAN_POINT('Ctrl Pts',(51.7511288569624,-69.9318331635702,
-214.256437733182));
#209310=CARTESIAN_POINT('Ctrl Pts',(51.7335529865694,-69.9367881584781,
-214.305864031718));
#209311=CARTESIAN_POINT('Ctrl Pts',(51.715411255478,-69.941902681012,-214.356881625546));
#209312=CARTESIAN_POINT('Ctrl Pts',(51.6961231833034,-69.9469868554723,
-214.409234130947));
#209313=CARTESIAN_POINT('Ctrl Pts',(51.6756673953278,-69.9519113844906,
-214.462922288982));
#209314=CARTESIAN_POINT('Ctrl Pts',(51.6725028704175,-69.952673212623,-214.471227885115));
#209315=CARTESIAN_POINT('Ctrl Pts',(51.6693104576324,-69.9534311389829,
-214.479565427316));
#209316=CARTESIAN_POINT('Ctrl Pts',(51.666090144668,-69.9541845926543,-214.487934896969));
#209317=CARTESIAN_POINT('Ctrl Pts',(51.6540717845718,-69.9569965173456,
-214.519170153049));
#209318=CARTESIAN_POINT('Ctrl Pts',(51.6416637393713,-69.9597467973301,
-214.550850462129));
#209319=CARTESIAN_POINT('Ctrl Pts',(51.6288629772096,-69.9624031668261,
-214.582975828909));
#209320=CARTESIAN_POINT('Ctrl Pts',(51.6224625961287,-69.9637313515741,
-214.599038512299));
#209321=CARTESIAN_POINT('Ctrl Pts',(51.6159640247811,-69.9650359813243,
-214.615212460306));
#209322=CARTESIAN_POINT('Ctrl Pts',(51.6093669926804,-69.9663124743072,
-214.631497673968));
#209323=CARTESIAN_POINT('Ctrl Pts',(51.6060684766301,-69.9669507207987,
-214.639640280798));
#209324=CARTESIAN_POINT('Ctrl Pts',(51.6027453449678,-69.967581927318,-214.647810704043));
#209325=CARTESIAN_POINT('Ctrl Pts',(51.5993975681366,-69.9682054833559,
-214.656008943773));
#209326=CARTESIAN_POINT('Ctrl Pts',(51.5960497913055,-69.9688290393938,
-214.664207183504));
#209327=CARTESIAN_POINT('Ctrl Pts',(51.5922089524539,-69.9695287310569,
-214.673571360434));
#209328=CARTESIAN_POINT('Ctrl Pts',(51.5892787609849,-69.97005283305,-214.680686254955));
#209329=CARTESIAN_POINT('Ctrl Pts',(51.5855178612913,-69.9707255177692,
-214.689818219507));
#209330=CARTESIAN_POINT('Ctrl Pts',(51.5817432158244,-69.9713850932742,
-214.698946551937));
#209331=CARTESIAN_POINT('Ctrl Pts',(51.577955362358,-69.9720309789322,-214.70807142067));
#209332=CARTESIAN_POINT('Ctrl Pts',(51.5407516159422,-69.9783747740254,
-214.797694555628));
#209333=CARTESIAN_POINT('Ctrl Pts',(51.5021322457915,-69.983522563863,-214.887276965874));
#209334=CARTESIAN_POINT('Ctrl Pts',(51.4620858828276,-69.9871863037332,
-214.977038137691));
#209335=CARTESIAN_POINT('Ctrl Pts',(51.4553825953226,-69.987799570454,-214.992063096188));
#209336=CARTESIAN_POINT('Ctrl Pts',(51.4486393137466,-69.9883711391208,
-215.007093047948));
#209337=CARTESIAN_POINT('Ctrl Pts',(51.4418559736239,-69.9888995124673,
-215.022129004877));
#209338=CARTESIAN_POINT('Ctrl Pts',(51.4054244374199,-69.9917372667819,
-215.102883176025));
#209339=CARTESIAN_POINT('Ctrl Pts',(51.3678140905141,-69.9933348295019,
-215.183840248426));
#209340=CARTESIAN_POINT('Ctrl Pts',(51.3289922766921,-69.9934293097912,
-215.265239689279));
#209341=CARTESIAN_POINT('Ctrl Pts',(51.3130055938261,-69.9934682164335,
-215.29875968534));
#209342=CARTESIAN_POINT('Ctrl Pts',(51.2968134974982,-69.9932516514847,
-215.332354687047));
#209343=CARTESIAN_POINT('Ctrl Pts',(51.2804138736011,-69.9927586351109,
-215.366041430998));
#209344=CARTESIAN_POINT('Ctrl Pts',(51.2322113007033,-69.991309537385,-215.465055148702));
#209345=CARTESIAN_POINT('Ctrl Pts',(51.1833271215805,-69.9875001826157,
-215.562558563164));
#209346=CARTESIAN_POINT('Ctrl Pts',(51.1340474348521,-69.9811339312681,
-215.658556370273));
#209347=CARTESIAN_POINT('Ctrl Pts',(51.0857566979389,-69.9748954385065,
-215.752627683529));
#209348=CARTESIAN_POINT('Ctrl Pts',(51.0370862445689,-69.9662015861898,
-215.845253336452));
#209349=CARTESIAN_POINT('Ctrl Pts',(50.988291150118,-69.9549150808236,-215.936431165693));
#209350=CARTESIAN_POINT('Ctrl Pts',(50.9707187829144,-69.9508505202571,
-215.969266644634));
#209351=CARTESIAN_POINT('Ctrl Pts',(50.9531301111087,-69.9464501771695,
-216.001914282774));
#209352=CARTESIAN_POINT('Ctrl Pts',(50.9355365677156,-69.9417092155658,
-216.034373717099));
#209353=CARTESIAN_POINT('Ctrl Pts',(56.7848125695504,-63.9246781901443,
-216.32517479574));
#209354=CARTESIAN_POINT('Ctrl Pts',(56.6914248998238,-63.6774027044323,
-216.115752570451));
#209355=CARTESIAN_POINT('Ctrl Pts',(56.9501445726978,-63.4755122787923,
-216.036568692573));
#209356=CARTESIAN_POINT('Ctrl Pts',(56.8894862224836,-64.207100718668,-215.816976621421));
#209357=CARTESIAN_POINT('Ctrl Pts',(56.8535591097954,-63.9616332231967,
-215.693685144435));
#209358=CARTESIAN_POINT('Ctrl Pts',(57.0658653622442,-63.8303542975169,
-215.574406016486));
#209359=CARTESIAN_POINT('Ctrl Pts',(56.8975641679252,-64.4758958672083,
-215.297354439506));
#209360=CARTESIAN_POINT('Ctrl Pts',(56.9070622928758,-64.2861767382064,
-215.200133915087));
#209361=CARTESIAN_POINT('Ctrl Pts',(57.0603127501189,-64.1729106578878,
-215.102057245562));
#209362=CARTESIAN_POINT('Ctrl Pts',(56.8418253372028,-64.8002473979207,
-214.513441216471));
#209363=CARTESIAN_POINT('Ctrl Pts',(56.8725452070173,-64.6752546110846,
-214.449672310422));
#209364=CARTESIAN_POINT('Ctrl Pts',(56.9710064262051,-64.589603741335,-214.390090855151));
#209365=CARTESIAN_POINT('Ctrl Pts',(56.8164834138299,-64.8889909543264,
-214.276550655991));
#209366=CARTESIAN_POINT('Ctrl Pts',(56.8499614295511,-64.7813997862752,
-214.224386280783));
#209367=CARTESIAN_POINT('Ctrl Pts',(56.9338189208405,-64.7041705810812,
-214.174927340598));
#209368=CARTESIAN_POINT('Ctrl Pts',(56.7542865190199,-65.0610681985444,
-213.691334443373));
#209369=CARTESIAN_POINT('Ctrl Pts',(56.7891152509752,-64.9853348405543,
-213.67002187732));
#209370=CARTESIAN_POINT('Ctrl Pts',(56.845223212725,-64.9270476219534,-213.643352384884));
#209371=CARTESIAN_POINT('Ctrl Pts',(56.715855751278,-65.1308968640445,-213.329423714843));
#209372=CARTESIAN_POINT('Ctrl Pts',(56.7467138871531,-65.0699208185081,
-213.321468010001));
#209373=CARTESIAN_POINT('Ctrl Pts',(56.7926294083244,-65.0181571456724,
-213.314757534777));
#209374=CARTESIAN_POINT('Ctrl Pts',(56.7379487726703,-65.0891150537523,
-212.933426638013));
#209375=CARTESIAN_POINT('Ctrl Pts',(56.7708234918149,-65.0194823467915,
-212.944141985026));
#209376=CARTESIAN_POINT('Ctrl Pts',(56.8230504447964,-64.9635917011068,
-212.954964540018));
#209377=CARTESIAN_POINT('',(56.8144552895507,-64.9781463989707,-213.256094899005));
#209378=CARTESIAN_POINT('',(56.7323722878851,-65.0994854859682,-213.264821102391));
#209379=CARTESIAN_POINT('Origin',(57.1832000972235,-65.315712880919,-213.264821102391));
#209380=CARTESIAN_POINT('Ctrl Pts',(56.8293274051384,-64.0646324794683,
-216.070020447203));
#209381=CARTESIAN_POINT('Ctrl Pts',(56.84326082334,-64.1169296295291,-215.973290586946));
#209382=CARTESIAN_POINT('Ctrl Pts',(56.8540807904868,-64.1687301223484,
-215.875753618678));
#209383=CARTESIAN_POINT('Ctrl Pts',(56.8620665015112,-64.2197520230989,
-215.777434450787));
#209384=CARTESIAN_POINT('Ctrl Pts',(56.8704637792726,-64.2734034852173,
-215.674048119936));
#209385=CARTESIAN_POINT('Ctrl Pts',(56.8757276601601,-64.3261933988336,
-215.569796347129));
#209386=CARTESIAN_POINT('Ctrl Pts',(56.8782372726827,-64.3778064713355,
-215.464718636094));
#209387=CARTESIAN_POINT('Ctrl Pts',(56.8787179510732,-64.3876921761587,
-215.444592586928));
#209388=CARTESIAN_POINT('Ctrl Pts',(56.8790977254115,-64.3975347599611,
-215.424436281727));
#209389=CARTESIAN_POINT('Ctrl Pts',(56.8793794439324,-64.4073320876536,
-215.404250065956));
#209390=CARTESIAN_POINT('Ctrl Pts',(56.8809734983155,-64.462768532161,-215.290029937206));
#209391=CARTESIAN_POINT('Ctrl Pts',(56.8794264385425,-64.516761707439,-215.174834553312));
#209392=CARTESIAN_POINT('Ctrl Pts',(56.8752707176649,-64.5689845407945,
-215.058643815246));
#209393=CARTESIAN_POINT('Ctrl Pts',(56.8717243682961,-64.6135497119317,
-214.959490632745));
#209394=CARTESIAN_POINT('Ctrl Pts',(56.8662794381607,-64.6568268726743,
-214.859611308838));
#209395=CARTESIAN_POINT('Ctrl Pts',(56.8592726682421,-64.6986417564396,
-214.758976432767));
#209396=CARTESIAN_POINT('Ctrl Pts',(56.8589144900082,-64.7007792864842,
-214.753832090567));
#209397=CARTESIAN_POINT('Ctrl Pts',(56.858569077902,-64.7028133839436,-214.748925881222));
#209398=CARTESIAN_POINT('Ctrl Pts',(56.858219143076,-64.7048497019118,-214.744003822932));
#209399=CARTESIAN_POINT('Ctrl Pts',(56.857577925288,-64.708581034737,-214.734984682525));
#209400=CARTESIAN_POINT('Ctrl Pts',(56.8569216476466,-64.7123212263355,
-214.725912519824));
#209401=CARTESIAN_POINT('Ctrl Pts',(56.856129531978,-64.7167079167791,-214.715214173572));
#209402=CARTESIAN_POINT('Ctrl Pts',(56.8521198803907,-64.7389131337681,
-214.661059657083));
#209403=CARTESIAN_POINT('Ctrl Pts',(56.8477627871993,-64.7600622131556,
-214.608091953219));
#209404=CARTESIAN_POINT('Ctrl Pts',(56.8432140576396,-64.780169866364,-214.556312554883));
#209405=CARTESIAN_POINT('Ctrl Pts',(56.8422067256955,-64.784622775936,-214.544845827459));
#209406=CARTESIAN_POINT('Ctrl Pts',(56.8411898176111,-64.7890246987895,
-214.533437326435));
#209407=CARTESIAN_POINT('Ctrl Pts',(56.8401647355452,-64.7933759337862,
-214.522086984327));
#209408=CARTESIAN_POINT('Ctrl Pts',(56.8352240963379,-64.8143477983232,
-214.467381173837));
#209409=CARTESIAN_POINT('Ctrl Pts',(56.8300966765821,-64.8341405916693,
-214.414027988426));
#209410=CARTESIAN_POINT('Ctrl Pts',(56.8249223102875,-64.8527646839859,
-214.362027845373));
#209411=CARTESIAN_POINT('Ctrl Pts',(56.8241752397253,-64.8554536144417,
-214.354520109372));
#209412=CARTESIAN_POINT('Ctrl Pts',(56.8234271210218,-64.8581182365231,
-214.347040568721));
#209413=CARTESIAN_POINT('Ctrl Pts',(56.8226783067622,-64.8607586336227,
-214.339589215315));
#209414=CARTESIAN_POINT('Ctrl Pts',(56.8172799740449,-64.8797937172462,
-214.28587110783));
#209415=CARTESIAN_POINT('Ctrl Pts',(56.8118472574457,-64.8975712685443,
-214.233618613337));
#209416=CARTESIAN_POINT('Ctrl Pts',(56.8064985328116,-64.9141125012779,
-214.182831658659));
#209417=CARTESIAN_POINT('Ctrl Pts',(56.8059665418472,-64.9157577133529,
-214.177780323463));
#209418=CARTESIAN_POINT('Ctrl Pts',(56.8054353518806,-64.9173907247201,
-214.172743487259));
#209419=CARTESIAN_POINT('Ctrl Pts',(56.8049050600144,-64.9190115751451,
-214.167721150608));
#209420=CARTESIAN_POINT('Ctrl Pts',(56.8019740932707,-64.9279701487072,
-214.139962283016));
#209421=CARTESIAN_POINT('Ctrl Pts',(56.7990710543229,-64.9365561442558,
-214.112646317844));
#209422=CARTESIAN_POINT('Ctrl Pts',(56.7962122881473,-64.9447733636485,
-214.085773252415));
#209423=CARTESIAN_POINT('Ctrl Pts',(56.7947829050594,-64.9488819733448,
-214.0723367197));
#209424=CARTESIAN_POINT('Ctrl Pts',(56.793364567285,-64.9528983769426,-214.059010911378));
#209425=CARTESIAN_POINT('Ctrl Pts',(56.7919591967795,-64.9568229761714,
-214.04579579105));
#209426=CARTESIAN_POINT('Ctrl Pts',(56.7914940574196,-64.9581219116236,
-214.041421946155));
#209427=CARTESIAN_POINT('Ctrl Pts',(56.7910303191845,-64.9594108420278,
-214.0370598135));
#209428=CARTESIAN_POINT('Ctrl Pts',(56.7905681137647,-64.9606896047482,
-214.032710478153));
#209429=CARTESIAN_POINT('Ctrl Pts',(56.7903320662302,-64.9613426667301,
-214.030489279869));
#209430=CARTESIAN_POINT('Ctrl Pts',(56.7900963750574,-64.9619931979646,
-214.028271126613));
#209431=CARTESIAN_POINT('Ctrl Pts',(56.7898610688874,-64.9626411620832,
-214.026056163046));
#209432=CARTESIAN_POINT('Ctrl Pts',(56.7892594651863,-64.9642978020765,
-214.02039319943));
#209433=CARTESIAN_POINT('Ctrl Pts',(56.7887964162145,-64.9655667092386,
-214.016032247683));
#209434=CARTESIAN_POINT('Ctrl Pts',(56.7881197951723,-64.9674090172119,
-214.009650980091));
#209435=CARTESIAN_POINT('Ctrl Pts',(56.7880135606757,-64.9676982731583,
-214.00864907399));
#209436=CARTESIAN_POINT('Ctrl Pts',(56.7879020590799,-64.9680015799114,
-214.007597310036));
#209437=CARTESIAN_POINT('Ctrl Pts',(56.7877839260599,-64.9683225474116,
-214.006482759224));
#209438=CARTESIAN_POINT('Ctrl Pts',(56.7831823982202,-64.9808249018571,
-213.963068677471));
#209439=CARTESIAN_POINT('Ctrl Pts',(56.7787367570231,-64.9923644894355,
-213.920682639109));
#209440=CARTESIAN_POINT('Ctrl Pts',(56.7745322143122,-65.0029589631916,
-213.879327038137));
#209441=CARTESIAN_POINT('Ctrl Pts',(56.7723732859695,-65.0083989625544,
-213.858091963313));
#209442=CARTESIAN_POINT('Ctrl Pts',(56.7702771925501,-65.0135903115608,
-213.837128418878));
#209443=CARTESIAN_POINT('Ctrl Pts',(56.7682513586567,-65.0185384446053,
-213.81643577243));
#209444=CARTESIAN_POINT('Ctrl Pts',(56.7652657719922,-65.0258307897876,
-213.785939842091));
#209445=CARTESIAN_POINT('Ctrl Pts',(56.7624343578982,-65.0325914981013,
-213.756033196312));
#209446=CARTESIAN_POINT('Ctrl Pts',(56.7597790035186,-65.0388290000784,
-213.726715837373));
#209447=CARTESIAN_POINT('Ctrl Pts',(56.7584513263288,-65.0419477510669,
-213.712057157904));
#209448=CARTESIAN_POINT('Ctrl Pts',(56.7571675863838,-65.0449356659555,
-213.697545800093));
#209449=CARTESIAN_POINT('Ctrl Pts',(56.7559300838455,-65.0477936839908,
-213.683181763961));
#209450=CARTESIAN_POINT('Ctrl Pts',(56.7553113325763,-65.0492226930084,
-213.675999745895));
#209451=CARTESIAN_POINT('Ctrl Pts',(56.7547041368897,-65.0506192261019,
-213.668854558246));
#209452=CARTESIAN_POINT('Ctrl Pts',(56.7541087628032,-65.0519833917363,
-213.661746201));
#209453=CARTESIAN_POINT('Ctrl Pts',(56.7536173495646,-65.0531093545007,
-213.655879064802));
#209454=CARTESIAN_POINT('Ctrl Pts',(56.7532003342218,-65.054062025313,-213.650845260365));
#209455=CARTESIAN_POINT('Ctrl Pts',(56.7526934344304,-65.0552163784068,
-213.644643633688));
#209456=CARTESIAN_POINT('Ctrl Pts',(56.7525861973272,-65.0554605873883,
-213.643331649562));
#209457=CARTESIAN_POINT('Ctrl Pts',(56.7524749911325,-65.0557136672505,
-213.641967333306));
#209458=CARTESIAN_POINT('Ctrl Pts',(56.7523583579841,-65.0559788895194,
-213.640531620456));
#209459=CARTESIAN_POINT('Ctrl Pts',(56.7484892101348,-65.0647772816159,
-213.592903777379));
#209460=CARTESIAN_POINT('Ctrl Pts',(56.7450977176229,-65.0722727884523,
-213.546104049185));
#209461=CARTESIAN_POINT('Ctrl Pts',(56.7422442798078,-65.0784822788702,
-213.500132498924));
#209462=CARTESIAN_POINT('Ctrl Pts',(56.7411569104229,-65.0808485507898,
-213.482613961788));
#209463=CARTESIAN_POINT('Ctrl Pts',(56.7401472913062,-65.0830284776309,
-213.465215688936));
#209464=CARTESIAN_POINT('Ctrl Pts',(56.739217431577,-65.0850244019591,-213.447937667528));
#209465=CARTESIAN_POINT('Ctrl Pts',(56.7375324485498,-65.0886411825456,
-213.416628458296));
#209466=CARTESIAN_POINT('Ctrl Pts',(56.7361109105069,-65.0916508059742,
-213.385714140014));
#209467=CARTESIAN_POINT('Ctrl Pts',(56.7349660432972,-65.0940592063371,
-213.355194712262));
#209468=CARTESIAN_POINT('Ctrl Pts',(56.7343936096924,-65.0952634065186,
-213.339934998386));
#209469=CARTESIAN_POINT('Ctrl Pts',(56.7338903052853,-65.0963172819309,
-213.324774007188));
#209470=CARTESIAN_POINT('Ctrl Pts',(56.7334575601726,-65.0972214635079,
-213.309711738833));
#209471=CARTESIAN_POINT('Ctrl Pts',(56.7330248150599,-65.0981256450848,
-213.294649470477));
#209472=CARTESIAN_POINT('Ctrl Pts',(56.7326626297635,-65.0988801316234,
-213.279685924923));
#209473=CARTESIAN_POINT('Ctrl Pts',(56.7323722878852,-65.0994854859681,
-213.264821102391));
#209474=CARTESIAN_POINT('Ctrl Pts',(56.8144552965909,-64.9781464054155,
-213.256094899172));
#209475=CARTESIAN_POINT('Ctrl Pts',(56.8173698192824,-64.9724082471664,
-213.354908067617));
#209476=CARTESIAN_POINT('Ctrl Pts',(56.826589953151,-64.9552496135495,-213.462936231746));
#209477=CARTESIAN_POINT('Ctrl Pts',(56.8478208203418,-64.9105102551182,
-213.638651304624));
#209478=CARTESIAN_POINT('Ctrl Pts',(56.8561265977695,-64.8924262632227,
-213.699497248996));
#209479=CARTESIAN_POINT('Ctrl Pts',(56.8701310542426,-64.8602769803466,
-213.794107197711));
#209480=CARTESIAN_POINT('Ctrl Pts',(56.877519322744,-64.8429461914106,-213.842246804829));
#209481=CARTESIAN_POINT('Ctrl Pts',(56.8867453394759,-64.8204671022411,
-213.899847655935));
#209482=CARTESIAN_POINT('Ctrl Pts',(56.891500998712,-64.8086546888112,-213.929004149363));
#209483=CARTESIAN_POINT('Ctrl Pts',(56.8935687422973,-64.8034686168898,
-213.941575706016));
#209484=CARTESIAN_POINT('Ctrl Pts',(56.894953708788,-64.7999836718063,-213.94997356981));
#209485=CARTESIAN_POINT('Ctrl Pts',(56.8959660672666,-64.7974254727206,
-213.956090873043));
#209486=CARTESIAN_POINT('Ctrl Pts',(56.9085806509794,-64.7654768744261,
-214.032181519627));
#209487=CARTESIAN_POINT('Ctrl Pts',(56.9245208634359,-64.7239387163797,
-214.123129670428));
#209488=CARTESIAN_POINT('Ctrl Pts',(56.9506552785366,-64.6428094702132,
-214.284669744791));
#209489=CARTESIAN_POINT('Ctrl Pts',(56.9597238315858,-64.6126176262786,
-214.342694808236));
#209490=CARTESIAN_POINT('Ctrl Pts',(56.9733270105072,-64.5621346734833,
-214.435816572145));
#209491=CARTESIAN_POINT('Ctrl Pts',(56.9801274940962,-64.5355934286946,
-214.483897125758));
#209492=CARTESIAN_POINT('Ctrl Pts',(56.9868156677765,-64.5070058705281,
-214.534208560028));
#209493=CARTESIAN_POINT('Ctrl Pts',(56.9912365333911,-64.4874815157085,
-214.568238727438));
#209494=CARTESIAN_POINT('Ctrl Pts',(56.9932850709852,-64.4781618507159,
-214.584343321439));
#209495=CARTESIAN_POINT('Ctrl Pts',(57.0140657811359,-64.3799782829966,
-214.752247756963));
#209496=CARTESIAN_POINT('Ctrl Pts',(57.0241767490285,-64.3015299352387,
-214.877176173881));
#209497=CARTESIAN_POINT('Ctrl Pts',(57.0331607991196,-64.2027589295951,
-215.029558796027));
#209498=CARTESIAN_POINT('Ctrl Pts',(57.0351000718181,-64.1729616787377,
-215.07453124402));
#209499=CARTESIAN_POINT('Ctrl Pts',(57.0369954878965,-64.1334541081786,
-215.13349269937));
#209500=CARTESIAN_POINT('Ctrl Pts',(57.0376874847421,-64.1149952719801,
-215.160849123836));
#209501=CARTESIAN_POINT('Ctrl Pts',(57.03814759071,-64.0958133018828,-215.189096154017));
#209502=CARTESIAN_POINT('Ctrl Pts',(57.0383015913884,-64.0868199657608,
-215.202308125432));
#209503=CARTESIAN_POINT('Ctrl Pts',(57.038352406177,-64.0830947089198,-215.207775655625));
#209504=CARTESIAN_POINT('Ctrl Pts',(57.0383830268799,-64.0806399804401,
-215.211377463292));
#209505=CARTESIAN_POINT('Ctrl Pts',(57.0383846983023,-64.080615480532,-215.211413793855));
#209506=CARTESIAN_POINT('Ctrl Pts',(57.0399527711531,-63.9254596265941,
-215.438958594151));
#209507=CARTESIAN_POINT('Ctrl Pts',(57.022928908771,-63.7820296637233,-215.635331946852));
#209508=CARTESIAN_POINT('Ctrl Pts',(56.9946437346772,-63.6543417315389,
-215.806005049013));
#209509=CARTESIAN_POINT('Ctrl Pts',(51.822850344383,-69.9419965866856,-213.735470748631));
#209510=CARTESIAN_POINT('Ctrl Pts',(51.8804433982798,-69.889324596863,-213.7397430898));
#209511=CARTESIAN_POINT('Ctrl Pts',(51.9513667677563,-69.856765622058,-213.744232219612));
#209512=CARTESIAN_POINT('Ctrl Pts',(51.8765276514687,-69.9171366797839,
-212.719415019637));
#209513=CARTESIAN_POINT('Ctrl Pts',(51.9284789001597,-69.8695011096846,
-212.726011510236));
#209514=CARTESIAN_POINT('Ctrl Pts',(51.991780071228,-69.8379778346573,-212.728235356937));
#209515=CARTESIAN_POINT('Ctrl Pts',(51.9334544096015,-69.8892734758678,
-211.703692143478));
#209516=CARTESIAN_POINT('Ctrl Pts',(51.9794687356772,-69.8470038946564,
-211.710263762613));
#209517=CARTESIAN_POINT('Ctrl Pts',(52.0346456619607,-69.816925009228,-211.71249177384));
#209518=CARTESIAN_POINT('Ctrl Pts',(52.0385712075059,-69.8271258445134,
-210.267504272468));
#209519=CARTESIAN_POINT('Ctrl Pts',(52.0734597321493,-69.7950116391773,
-210.272241986443));
#209520=CARTESIAN_POINT('Ctrl Pts',(52.1138191538044,-69.7700067918124,
-210.276283653453));
#209521=CARTESIAN_POINT('Ctrl Pts',(52.072185388712,-69.806348038251,-209.845388043713));
#209522=CARTESIAN_POINT('Ctrl Pts',(52.1034382988763,-69.7775433560357,
-209.850130119974));
#209523=CARTESIAN_POINT('Ctrl Pts',(52.1391384959575,-69.7543237267294,
-209.854167521602));
#209524=CARTESIAN_POINT('Ctrl Pts',(52.1354652353079,-69.763262836332,-209.213638050098));
#209525=CARTESIAN_POINT('Ctrl Pts',(52.1597481032177,-69.7408313624291,
-209.21810272547));
#209526=CARTESIAN_POINT('Ctrl Pts',(52.1868109938527,-69.7218145199576,
-209.222414495584));
#209527=CARTESIAN_POINT('Ctrl Pts',(52.1584910060187,-69.747112810802,-209.003150816985));
#209528=CARTESIAN_POINT('Ctrl Pts',(52.1802056110658,-69.7270298301124,
-209.007617928732));
#209529=CARTESIAN_POINT('Ctrl Pts',(52.2041584674497,-69.7096301545639,
-209.011927312326));
#209530=CARTESIAN_POINT('Ctrl Pts',(52.2022638893192,-69.7142992552832,
-208.689605786204));
#209531=CARTESIAN_POINT('Ctrl Pts',(52.2190101918288,-69.6987724358089,
-208.694007820048));
#209532=CARTESIAN_POINT('Ctrl Pts',(52.2371408246248,-69.6848794419398,
-208.698381586053));
#209533=CARTESIAN_POINT('Ctrl Pts',(52.2182336078506,-69.7020812266945,
-208.585328566142));
#209534=CARTESIAN_POINT('Ctrl Pts',(52.2331514504351,-69.6882319207143,
-208.589731796556));
#209535=CARTESIAN_POINT('Ctrl Pts',(52.249174245292,-69.6756642254024,-208.594104390417));
#209536=CARTESIAN_POINT('Ctrl Pts',(52.2489412320905,-69.6774578274061,
-208.431136608511));
#209537=CARTESIAN_POINT('Ctrl Pts',(52.2602903339986,-69.6668890135686,
-208.435525620945));
#209538=CARTESIAN_POINT('Ctrl Pts',(52.2723150773139,-69.6570951860835,
-208.439912289689));
#209539=CARTESIAN_POINT('Ctrl Pts',(52.2601800097299,-69.6683161240625,
-208.380021453291));
#209540=CARTESIAN_POINT('Ctrl Pts',(52.270214924355,-69.658955894537,-208.384411029018));
#209541=CARTESIAN_POINT('Ctrl Pts',(52.2807846875617,-69.6502015352889,
-208.388797146169));
#209542=CARTESIAN_POINT('Ctrl Pts',(52.281999678196,-69.6499593019998,-208.305729941084));
#209543=CARTESIAN_POINT('Ctrl Pts',(52.2894520983595,-69.6429772988716,
-208.310116951883));
#209544=CARTESIAN_POINT('Ctrl Pts',(52.2972292893049,-69.6363602565428,
-208.314505613017));
#209545=CARTESIAN_POINT('Ctrl Pts',(52.2900513245554,-69.6431141725604,
-208.281238728998));
#209546=CARTESIAN_POINT('Ctrl Pts',(52.2965464863421,-69.6370140514492,
-208.285625985819));
#209547=CARTESIAN_POINT('Ctrl Pts',(52.3032976103578,-69.6311990926332,
-208.290014406272));
#209548=CARTESIAN_POINT('Ctrl Pts',(52.3055109262683,-69.6296515882696,
-208.24731365204));
#209549=CARTESIAN_POINT('Ctrl Pts',(52.3101508205055,-69.6252622995574,
-208.251700725001));
#209550=CARTESIAN_POINT('Ctrl Pts',(52.3149497431651,-69.6210491476294,
-208.256089330814));
#209551=CARTESIAN_POINT('Ctrl Pts',(52.3112700002316,-69.624596121335,-208.236328897454));
#209552=CARTESIAN_POINT('Ctrl Pts',(52.31521638535,-69.6208465529984,-208.24071608881));
#209553=CARTESIAN_POINT('Ctrl Pts',(52.3192905030199,-69.6172377131638,
-208.245104578722));
#209554=CARTESIAN_POINT('Ctrl Pts',(52.4157911999455,-69.5313285632376,
-208.09911365756));
#209555=CARTESIAN_POINT('Ctrl Pts',(52.4070413724992,-69.5392973207822,
-208.103538654047));
#209556=CARTESIAN_POINT('Ctrl Pts',(52.3980737175552,-69.546924914442,-208.107889777235));
#209557=CARTESIAN_POINT('Ctrl Pts',(52.8039539674273,-69.1685749088719,
-208.261113958564));
#209558=CARTESIAN_POINT('Ctrl Pts',(52.7473775130206,-69.2207759621712,
-208.265385690945));
#209559=CARTESIAN_POINT('Ctrl Pts',(52.6906841717837,-69.273483049227,-208.269888341076));
#209560=CARTESIAN_POINT('Ctrl Pts',(53.3726051882046,-68.2329805102008,
-225.06502763524));
#209561=CARTESIAN_POINT('Ctrl Pts',(53.252682904108,-68.3309162879933,-225.681318331171));
#209562=CARTESIAN_POINT('Ctrl Pts',(53.1203834433686,-68.5685596498648,
-225.080427005024));
#209563=CARTESIAN_POINT('',(52.3440043138885,-69.594874440935,-208.218811515427));
#209564=CARTESIAN_POINT('',(52.3440560052495,-69.5949303622595,-208.210085312208));
#209565=CARTESIAN_POINT('Origin',(52.6833983856504,-69.9620415201413,-208.218811515427));
#209566=CARTESIAN_POINT('Ctrl Pts',(51.8506358032439,-69.9286975854465,
-213.227536545096));
#209567=CARTESIAN_POINT('Ctrl Pts',(51.8965359306666,-69.9068955059224,
-212.381067577369));
#209568=CARTESIAN_POINT('Ctrl Pts',(51.9463091177219,-69.8815088904097,
-211.535021517202));
#209569=CARTESIAN_POINT('Ctrl Pts',(52.0389353307874,-69.8267824525318,
-210.267914982609));
#209570=CARTESIAN_POINT('Ctrl Pts',(52.0725035102325,-69.806045505995,-209.8458402758));
#209571=CARTESIAN_POINT('Ctrl Pts',(52.1356910661391,-69.7630436587203,
-209.214130441658));
#209572=CARTESIAN_POINT('Ctrl Pts',(52.1586824184498,-69.7469248062077,
-209.003656181328));
#209573=CARTESIAN_POINT('Ctrl Pts',(52.2023855392512,-69.7141755312691,
-208.690099641439));
#209574=CARTESIAN_POINT('Ctrl Pts',(52.2183291852341,-69.7019815954277,
-208.585816112664));
#209575=CARTESIAN_POINT('Ctrl Pts',(52.2489833267826,-69.6774084341258,
-208.431581516949));
#209576=CARTESIAN_POINT('Ctrl Pts',(52.2602021616247,-69.6682855321809,
-208.380448072074));
#209577=CARTESIAN_POINT('Ctrl Pts',(52.2819812944307,-69.6499675527577,
-208.306095531171));
#209578=CARTESIAN_POINT('Ctrl Pts',(52.2900177211888,-69.6431370963428,
-208.281577994998));
#209579=CARTESIAN_POINT('Ctrl Pts',(52.3054538148208,-69.6296980513237,
-208.247576563664));
#209580=CARTESIAN_POINT('Ctrl Pts',(52.3112042959167,-69.6246512725098,
-208.236560595082));
#209581=CARTESIAN_POINT('Ctrl Pts',(52.3253253083163,-69.6120530454534,
-208.217923065672));
#209582=CARTESIAN_POINT('Ctrl Pts',(52.3341567138414,-69.6040808580668,
-208.210085312176));
#209583=CARTESIAN_POINT('Ctrl Pts',(52.3440560052495,-69.5949303622595,
-208.210085312208));
#209584=CARTESIAN_POINT('Ctrl Pts',(52.3440043138833,-69.5948744409406,
-208.218811515393));
#209585=CARTESIAN_POINT('Ctrl Pts',(52.3424820359817,-69.5962815717119,
-208.218811515395));
#209586=CARTESIAN_POINT('Ctrl Pts',(52.3408547147374,-69.5977800490423,
-208.219125748933));
#209587=CARTESIAN_POINT('Ctrl Pts',(52.3391512870202,-69.5993409672496,
-208.21987200544));
#209588=CARTESIAN_POINT('Ctrl Pts',(52.3376186249417,-69.6007454061464,
-208.220543451042));
#209589=CARTESIAN_POINT('Ctrl Pts',(52.3360244145561,-69.6022003180093,
-208.221565577745));
#209590=CARTESIAN_POINT('Ctrl Pts',(52.3343938226836,-69.6036815434254,
-208.222987281035));
#209591=CARTESIAN_POINT('Ctrl Pts',(52.3328814720798,-69.6050553587805,
-208.224305890471));
#209592=CARTESIAN_POINT('Ctrl Pts',(52.3313378567263,-69.6064517683912,
-208.225968890555));
#209593=CARTESIAN_POINT('Ctrl Pts',(52.3297861601934,-69.6078494379871,
-208.227971012618));
#209594=CARTESIAN_POINT('Ctrl Pts',(52.3283529596706,-69.6091403739099,
-208.229820241721));
#209595=CARTESIAN_POINT('Ctrl Pts',(52.3269128910609,-69.6104323547897,
-208.2319590992));
#209596=CARTESIAN_POINT('Ctrl Pts',(52.3254865791142,-69.6117072283637,
-208.234337728021));
#209597=CARTESIAN_POINT('Ctrl Pts',(52.3251941318254,-69.6119686251227,
-208.234825435883));
#209598=CARTESIAN_POINT('Ctrl Pts',(52.3249022706465,-69.6122292986765,
-208.23532305026));
#209599=CARTESIAN_POINT('Ctrl Pts',(52.3246111854786,-69.612489086511,-208.235829859775));
#209600=CARTESIAN_POINT('Ctrl Pts',(52.3226799130822,-69.6142127094541,
-208.239192405634));
#209601=CARTESIAN_POINT('Ctrl Pts',(52.3207618818214,-69.6159161659265,
-208.242988126939));
#209602=CARTESIAN_POINT('Ctrl Pts',(52.3188715230813,-69.6175861945551,
-208.247212540653));
#209603=CARTESIAN_POINT('Ctrl Pts',(52.3171376894694,-69.6191179417879,
-208.25108716526));
#209604=CARTESIAN_POINT('Ctrl Pts',(52.3154272482004,-69.6206214591213,
-208.25532266912));
#209605=CARTESIAN_POINT('Ctrl Pts',(52.313737915979,-69.6220996391995,-208.259876064165));
#209606=CARTESIAN_POINT('Ctrl Pts',(52.312839974451,-69.6228853456825,-208.26229635927));
#209607=CARTESIAN_POINT('Ctrl Pts',(52.3119477536723,-69.6236641313598,
-208.264805759652));
#209608=CARTESIAN_POINT('Ctrl Pts',(52.3110589927009,-69.6244383044097,
-208.267392287932));
#209609=CARTESIAN_POINT('Ctrl Pts',(52.3085864708634,-69.6265920440916,
-208.274587977059));
#209610=CARTESIAN_POINT('Ctrl Pts',(52.3061287484059,-69.6287200926668,
-208.282439487147));
#209611=CARTESIAN_POINT('Ctrl Pts',(52.3037047421696,-69.6308048212131,
-208.290954531357));
#209612=CARTESIAN_POINT('Ctrl Pts',(52.3015089296444,-69.6326932953372,
-208.29866797716));
#209613=CARTESIAN_POINT('Ctrl Pts',(52.2993409311851,-69.634546082569,-208.3069260843));
#209614=CARTESIAN_POINT('Ctrl Pts',(52.2971949154258,-69.6363690309351,
-208.315703747231));
#209615=CARTESIAN_POINT('Ctrl Pts',(52.295364326622,-69.637924037628,-208.323191246527));
#209616=CARTESIAN_POINT('Ctrl Pts',(52.2935495863094,-69.6394574727516,
-208.331056549212));
#209617=CARTESIAN_POINT('Ctrl Pts',(52.2917323870528,-69.6409869521274,
-208.339261708216));
#209618=CARTESIAN_POINT('Ctrl Pts',(52.2884850180848,-69.6437201603016,
-208.353924480407));
#209619=CARTESIAN_POINT('Ctrl Pts',(52.2852408400929,-69.6464298179871,
-208.369711727464));
#209620=CARTESIAN_POINT('Ctrl Pts',(52.2820272057473,-69.6490902832157,
-208.38664308245));
#209621=CARTESIAN_POINT('Ctrl Pts',(52.2790795380118,-69.6515305631829,
-208.402173165666));
#209622=CARTESIAN_POINT('Ctrl Pts',(52.2761578716336,-69.6539291711863,
-208.418666029657));
#209623=CARTESIAN_POINT('Ctrl Pts',(52.2732561995377,-69.6562917771648,
-208.436115348614));
#209624=CARTESIAN_POINT('Ctrl Pts',(52.2705180528767,-69.658521237096,-208.452581300955));
#209625=CARTESIAN_POINT('Ctrl Pts',(52.2677979993281,-69.6607183676128,
-208.469899152139));
#209626=CARTESIAN_POINT('Ctrl Pts',(52.2650615521283,-69.6629155667661,
-208.488040589413));
#209627=CARTESIAN_POINT('Ctrl Pts',(52.2648981281873,-69.6630467861606,
-208.489124018019));
#209628=CARTESIAN_POINT('Ctrl Pts',(52.2647346358121,-69.6631780151523,
-208.490210376304));
#209629=CARTESIAN_POINT('Ctrl Pts',(52.2645710637428,-69.6633092643157,
-208.491299655199));
#209630=CARTESIAN_POINT('Ctrl Pts',(52.260313528908,-69.6667254825471,-208.519651945799));
#209631=CARTESIAN_POINT('Ctrl Pts',(52.2560326046515,-69.6701265640873,
-208.550011208226));
#209632=CARTESIAN_POINT('Ctrl Pts',(52.2517649403206,-69.6734780506684,
-208.582409808769));
#209633=CARTESIAN_POINT('Ctrl Pts',(52.2477984711022,-69.6765930023912,
-208.61252184238));
#209634=CARTESIAN_POINT('Ctrl Pts',(52.2438438954802,-69.6796647025151,
-208.644395735144));
#209635=CARTESIAN_POINT('Ctrl Pts',(52.2399006765453,-69.6826934930627,
-208.678040517083));
#209636=CARTESIAN_POINT('Ctrl Pts',(52.2362593492553,-69.685490400325,-208.709109464727));
#209637=CARTESIAN_POINT('Ctrl Pts',(52.2326279198868,-69.688250517501,-208.741688626789));
#209638=CARTESIAN_POINT('Ctrl Pts',(52.2289751792274,-69.6910028859806,
-208.775768002304));
#209639=CARTESIAN_POINT('Ctrl Pts',(52.2280173563656,-69.6917246129522,
-208.784704307404));
#209640=CARTESIAN_POINT('Ctrl Pts',(52.2270578831674,-69.6924459799922,
-208.793743664294));
#209641=CARTESIAN_POINT('Ctrl Pts',(52.2260957795316,-69.6931679007633,
-208.802885662675));
#209642=CARTESIAN_POINT('Ctrl Pts',(52.2204632758245,-69.6973942868489,
-208.856406237649));
#209643=CARTESIAN_POINT('Ctrl Pts',(52.2147742585669,-69.7016079333847,
-208.913478699865));
#209644=CARTESIAN_POINT('Ctrl Pts',(52.2090738657013,-69.705766109449,-208.9741602494));
#209645=CARTESIAN_POINT('Ctrl Pts',(52.2037779171684,-69.7096292618573,
-209.030536427466));
#209646=CARTESIAN_POINT('Ctrl Pts',(52.1984726040311,-69.7134441130084,
-209.090027907352));
#209647=CARTESIAN_POINT('Ctrl Pts',(52.1931642068981,-69.7172043138646,
-209.152666203404));
#209648=CARTESIAN_POINT('Ctrl Pts',(52.1882858395736,-69.7206599032885,
-209.210230211722));
#209649=CARTESIAN_POINT('Ctrl Pts',(52.1834050653669,-69.7240691542093,
-209.270451914207));
#209650=CARTESIAN_POINT('Ctrl Pts',(52.1784963359389,-69.7274555197984,
-209.333341603547));
#209651=CARTESIAN_POINT('Ctrl Pts',(52.1759593382091,-69.7292057083019,
-209.365845126387));
#209652=CARTESIAN_POINT('Ctrl Pts',(52.1734143426905,-69.730950278557,-209.39906106946));
#209653=CARTESIAN_POINT('Ctrl Pts',(52.1708539451181,-69.7326960847145,
-209.432989076637));
#209654=CARTESIAN_POINT('Ctrl Pts',(52.1632697473111,-69.7378673672427,
-209.533487811832));
#209655=CARTESIAN_POINT('Ctrl Pts',(52.1555870040426,-69.7430150975709,
-209.640265501971));
#209656=CARTESIAN_POINT('Ctrl Pts',(52.1478593423169,-69.7480875585307,
-209.75344383926));
#209657=CARTESIAN_POINT('Ctrl Pts',(52.1406857719123,-69.7527963122406,
-209.858507026501));
#209658=CARTESIAN_POINT('Ctrl Pts',(52.1334739691835,-69.7574397630151,
-209.969085955311));
#209659=CARTESIAN_POINT('Ctrl Pts',(52.1262360091054,-69.762005099994,-210.085273463446));
#209660=CARTESIAN_POINT('Ctrl Pts',(52.1196204051817,-69.7661778863737,
-210.191470586172));
#209661=CARTESIAN_POINT('Ctrl Pts',(52.1129831293641,-69.7702852473543,
-210.302353273817));
#209662=CARTESIAN_POINT('Ctrl Pts',(52.1063025138116,-69.7743460201426,
-210.417987894064));
#209663=CARTESIAN_POINT('Ctrl Pts',(52.1010659831097,-69.7775290144658,
-210.508626882994));
#209664=CARTESIAN_POINT('Ctrl Pts',(52.0958023524557,-69.7806838219579,
-210.602185411385));
#209665=CARTESIAN_POINT('Ctrl Pts',(52.0904846874294,-69.7838348020659,
-210.698693024827));
#209666=CARTESIAN_POINT('Ctrl Pts',(52.080225495559,-69.7899138817652,-210.884881910058));
#209667=CARTESIAN_POINT('Ctrl Pts',(52.0698067521628,-69.7959401628047,
-211.082055011306));
#209668=CARTESIAN_POINT('Ctrl Pts',(52.0592899423143,-69.8018521875684,
-211.290461140744));
#209669=CARTESIAN_POINT('Ctrl Pts',(52.0495256953229,-69.8073411591142,
-211.483954124991));
#209670=CARTESIAN_POINT('Ctrl Pts',(52.0396773891904,-69.8127312015491,
-211.687130103457));
#209671=CARTESIAN_POINT('Ctrl Pts',(52.0297642950147,-69.81800077633,-211.900183231084));
#209672=CARTESIAN_POINT('Ctrl Pts',(52.0202586260742,-69.8230537731479,
-212.104479938256));
#209673=CARTESIAN_POINT('Ctrl Pts',(52.0106939094361,-69.8279955156581,
-212.317858666779));
#209674=CARTESIAN_POINT('Ctrl Pts',(52.0010513321796,-69.832840099181,-212.540484705824));
#209675=CARTESIAN_POINT('Ctrl Pts',(51.9922011668754,-69.8372865623895,
-212.744815684374));
#209676=CARTESIAN_POINT('Ctrl Pts',(51.9832855225751,-69.8416510762705,
-212.956936580511));
#209677=CARTESIAN_POINT('Ctrl Pts',(51.9742552168064,-69.8459765591321,
-213.176969516857));
#209678=CARTESIAN_POINT('Ctrl Pts',(51.9734466757251,-69.8463638473015,
-213.196670474147));
#209679=CARTESIAN_POINT('Ctrl Pts',(51.9726371899477,-69.8467508461296,
-213.216434856257));
#209680=CARTESIAN_POINT('Ctrl Pts',(51.9718267086745,-69.8471376007524,
-213.236262748315));
#209681=CARTESIAN_POINT('Ctrl Pts',(56.4785498900846,-65.4721614184049,
-208.210085312209));
#209682=CARTESIAN_POINT('Ctrl Pts',(56.4784941157842,-65.4721095684412,
-208.214448081532));
#209683=CARTESIAN_POINT('Ctrl Pts',(56.478494115784,-65.4721095684411,-208.218811515427));
#209684=CARTESIAN_POINT('Ctrl Pts',(56.4880093612199,-65.4619859436241,
-208.210087277606));
#209685=CARTESIAN_POINT('Ctrl Pts',(56.4867940706151,-65.4631813685704,
-208.214450046893));
#209686=CARTESIAN_POINT('Ctrl Pts',(56.4856347339016,-65.464428502687,-208.218813480809));
#209687=CARTESIAN_POINT('Ctrl Pts',(56.4960155064695,-65.4531598633657,
-208.218220200296));
#209688=CARTESIAN_POINT('Ctrl Pts',(56.4938064756652,-65.455425583918,-208.222583010898));
#209689=CARTESIAN_POINT('Ctrl Pts',(56.4916787645948,-65.4577664915776,
-208.226946403507));
#209690=CARTESIAN_POINT('Ctrl Pts',(56.5087297972239,-65.4389829337676,
-208.237237256758));
#209691=CARTESIAN_POINT('Ctrl Pts',(56.5049328760549,-65.4429598777431,
-208.241599714584));
#209692=CARTESIAN_POINT('Ctrl Pts',(56.5012774655679,-65.4470659442998,
-208.245963459985));
#209693=CARTESIAN_POINT('Ctrl Pts',(56.5138509238801,-65.4331773923495,
-208.248518783163));
#209694=CARTESIAN_POINT('Ctrl Pts',(56.5094087292744,-65.4378503136699,
-208.25288112094));
#209695=CARTESIAN_POINT('Ctrl Pts',(56.5051439252244,-65.4426842233343,
-208.257244986379));
#209696=CARTESIAN_POINT('Ctrl Pts',(56.5273807159321,-65.4177153790657,
-208.283038207423));
#209697=CARTESIAN_POINT('Ctrl Pts',(56.5212265334526,-65.4242355589788,
-208.287400749103));
#209698=CARTESIAN_POINT('Ctrl Pts',(56.5153591918106,-65.4310145177164,
-208.291764410647));
#209699=CARTESIAN_POINT('Ctrl Pts',(56.5341593626729,-65.4097792264604,
-208.307533252362));
#209700=CARTESIAN_POINT('Ctrl Pts',(56.5271357114541,-65.4172387338904,
-208.311895535072));
#209701=CARTESIAN_POINT('Ctrl Pts',(56.5204776688227,-65.4250252363654,
-208.316259455579));
#209702=CARTESIAN_POINT('Ctrl Pts',(56.5525209588637,-65.3880602085305,
-208.38232400629));
#209703=CARTESIAN_POINT('Ctrl Pts',(56.5431294167638,-65.3980791094533,
-208.386688866059));
#209704=CARTESIAN_POINT('Ctrl Pts',(56.5343427956335,-65.4086346803882,
-208.391050209511));
#209705=CARTESIAN_POINT('Ctrl Pts',(56.5617269524415,-65.3767978707557,
-208.434001333226));
#209706=CARTESIAN_POINT('Ctrl Pts',(56.5511242891442,-65.3881281081246,
-208.438365624418));
#209707=CARTESIAN_POINT('Ctrl Pts',(56.5412952751588,-65.4001361493426,
-208.442727536444));
#209708=CARTESIAN_POINT('Ctrl Pts',(56.5863764886281,-65.3462052619613,
-208.588987026056));
#209709=CARTESIAN_POINT('Ctrl Pts',(56.5725061054701,-65.3610757695375,
-208.59336548035));
#209710=CARTESIAN_POINT('Ctrl Pts',(56.5599119337509,-65.3770518735271,
-208.597713229276));
#209711=CARTESIAN_POINT('Ctrl Pts',(56.5986098697023,-65.3302929526477,
-208.693634753733));
#209712=CARTESIAN_POINT('Ctrl Pts',(56.5830688742296,-65.3469778303877,
-208.698012046015));
#209713=CARTESIAN_POINT('Ctrl Pts',(56.5691529780988,-65.365046299052,-208.702360956951));
#209714=CARTESIAN_POINT('Ctrl Pts',(56.6315194173109,-65.2866023733443,
-209.008772950752));
#209715=CARTESIAN_POINT('Ctrl Pts',(56.6114339742289,-65.3082260137793,
-209.013214961635));
#209716=CARTESIAN_POINT('Ctrl Pts',(56.594014810857,-65.3320840644752,-209.017499153971));
#209717=CARTESIAN_POINT('Ctrl Pts',(56.6477298291647,-65.2635998038976,
-209.220340888184));
#209718=CARTESIAN_POINT('Ctrl Pts',(56.6253012100655,-65.2877789793426,
-209.224780476847));
#209719=CARTESIAN_POINT('Ctrl Pts',(56.6062646503943,-65.3147324550994,
-209.229067091402));
#209720=CARTESIAN_POINT('Ctrl Pts',(56.6909645146964,-65.2003964473429,
-209.855114420997));
#209721=CARTESIAN_POINT('Ctrl Pts',(56.6621798760702,-65.2315103701136,
-209.859829541482));
#209722=CARTESIAN_POINT('Ctrl Pts',(56.6389405444651,-65.2670590859439,
-209.863840624216));
#209723=CARTESIAN_POINT('Ctrl Pts',(56.7118396592687,-65.1667799745591,
-210.279514012908));
#209724=CARTESIAN_POINT('Ctrl Pts',(56.6797528213393,-65.2015162456806,
-210.284225552072));
#209725=CARTESIAN_POINT('Ctrl Pts',(56.6547249564177,-65.2417076178786,
-210.288240216126));
#209726=CARTESIAN_POINT('Ctrl Pts',(56.7669337250065,-65.0740063908786,
-211.553866504694));
#209727=CARTESIAN_POINT('Ctrl Pts',(56.7258904584642,-65.1185576981398,
-211.559720606721));
#209728=CARTESIAN_POINT('Ctrl Pts',(56.6963931899382,-65.1717493422662,
-211.562592707913));
#209729=CARTESIAN_POINT('Ctrl Pts',(56.7925037337705,-65.0241267882654,
-212.404990365038));
#209730=CARTESIAN_POINT('Ctrl Pts',(56.7467526277092,-65.0738827156515,
-212.410853939053));
#209731=CARTESIAN_POINT('Ctrl Pts',(56.7157486990471,-65.1341451836486,
-212.413730817787));
#209732=CARTESIAN_POINT('Ctrl Pts',(56.8144552965912,-64.9781464054152,
-213.256094899172));
#209733=CARTESIAN_POINT('Ctrl Pts',(56.7643939904929,-65.0327211703679,
-213.2603619646));
#209734=CARTESIAN_POINT('Ctrl Pts',(56.7323722878852,-65.0994854859681,
-213.264821102391));
#209735=CARTESIAN_POINT('',(56.4785498900846,-65.4721614184049,-208.210085312208));
#209736=CARTESIAN_POINT('',(56.478494115784,-65.4721095684411,-208.218811515426));
#209737=CARTESIAN_POINT('Origin',(56.8446958677552,-65.8125449908831,-208.218811515427));
#209738=CARTESIAN_POINT('Ctrl Pts',(56.7323722878852,-65.0994854859681,
-213.264821102391));
#209739=CARTESIAN_POINT('Ctrl Pts',(56.7280331299638,-65.1085325036252,
-213.0426659958));
#209740=CARTESIAN_POINT('Ctrl Pts',(56.7236600161187,-65.1174598023183,
-212.828408289229));
#209741=CARTESIAN_POINT('Ctrl Pts',(56.7192071520268,-65.1263191176805,
-212.621942418159));
#209742=CARTESIAN_POINT('Ctrl Pts',(56.7143712859647,-65.1359404449006,
-212.397717901465));
#209743=CARTESIAN_POINT('Ctrl Pts',(56.7094414942533,-65.1454814483888,
-212.182683232543));
#209744=CARTESIAN_POINT('Ctrl Pts',(56.7044007704901,-65.1549636966398,
-211.976689932902));
#209745=CARTESIAN_POINT('Ctrl Pts',(56.6990509914586,-65.16502731751,-211.758066836935));
#209746=CARTESIAN_POINT('Ctrl Pts',(56.6935766980629,-65.1750242887845,
-211.549627667317));
#209747=CARTESIAN_POINT('Ctrl Pts',(56.6879977785627,-65.1849372191661,
-211.351181755465));
#209748=CARTESIAN_POINT('Ctrl Pts',(56.6816574551575,-65.1962030537977,
-211.125652195569));
#209749=CARTESIAN_POINT('Ctrl Pts',(56.6751822988107,-65.207360021443,-210.913029724019));
#209750=CARTESIAN_POINT('Ctrl Pts',(56.6686464737588,-65.2183342962373,
-210.713019035319));
#209751=CARTESIAN_POINT('Ctrl Pts',(56.6645436973053,-65.2252232499444,
-210.587465009999));
#209752=CARTESIAN_POINT('Ctrl Pts',(56.6604331251529,-65.2320228858102,
-210.466880293573));
#209753=CARTESIAN_POINT('Ctrl Pts',(56.6562668550037,-65.2387859569443,
-210.351202386143));
#209754=CARTESIAN_POINT('Ctrl Pts',(56.6519002114437,-65.2458742925433,
-210.229961042825));
#209755=CARTESIAN_POINT('Ctrl Pts',(56.6474728117744,-65.2529220025824,
-210.114109749179));
#209756=CARTESIAN_POINT('Ctrl Pts',(56.6429718362471,-65.2599444300887,
-210.003567964623));
#209757=CARTESIAN_POINT('Ctrl Pts',(56.6379688409285,-65.2677501094857,
-209.880696816514));
#209758=CARTESIAN_POINT('Ctrl Pts',(56.6328751836196,-65.2755242926631,
-209.764385579971));
#209759=CARTESIAN_POINT('Ctrl Pts',(56.6277194341623,-65.2832385350797,
-209.654514291435));
#209760=CARTESIAN_POINT('Ctrl Pts',(56.624236911128,-65.2884492279441,-209.580300193892));
#209761=CARTESIAN_POINT('Ctrl Pts',(56.6207270390862,-65.2936315211658,
-209.509024134166));
#209762=CARTESIAN_POINT('Ctrl Pts',(56.617207440978,-65.2987671927539,-209.440647356452));
#209763=CARTESIAN_POINT('Ctrl Pts',(56.613775609728,-65.303774798084,-209.373975664024));
#209764=CARTESIAN_POINT('Ctrl Pts',(56.6103458753721,-65.3087263946004,
-209.310034156505));
#209765=CARTESIAN_POINT('Ctrl Pts',(56.6068764958621,-65.313666809265,-209.2488250452));
#209766=CARTESIAN_POINT('Ctrl Pts',(56.6032170825836,-65.3188778330151,
-209.184263231186));
#209767=CARTESIAN_POINT('Ctrl Pts',(56.5995139374616,-65.3240760159455,
-209.122741170297));
#209768=CARTESIAN_POINT('Ctrl Pts',(56.5957575695313,-65.329271895427,-209.064240357975));
#209769=CARTESIAN_POINT('Ctrl Pts',(56.5915999777325,-65.3350227553855,
-208.999490977178));
#209770=CARTESIAN_POINT('Ctrl Pts',(56.587377473491,-65.3407704865255,-208.938442616069));
#209771=CARTESIAN_POINT('Ctrl Pts',(56.5831193370057,-65.3464844948962,
-208.881047056792));
#209772=CARTESIAN_POINT('Ctrl Pts',(56.581245602093,-65.3489988663853,-208.855790923359));
#209773=CARTESIAN_POINT('Ctrl Pts',(56.5793654496022,-65.3515061949731,
-208.831241819825));
#209774=CARTESIAN_POINT('Ctrl Pts',(56.5774833115673,-65.3540018120632,
-208.807394533789));
#209775=CARTESIAN_POINT('Ctrl Pts',(56.5746535978651,-65.3577538651775,
-208.771541163416));
#209776=CARTESIAN_POINT('Ctrl Pts',(56.5718312042982,-65.3614666511509,
-208.737278831632));
#209777=CARTESIAN_POINT('Ctrl Pts',(56.5689753515512,-65.3651839879222,
-208.704609317259));
#209778=CARTESIAN_POINT('Ctrl Pts',(56.5659574293187,-65.3691122833498,
-208.670085809751));
#209779=CARTESIAN_POINT('Ctrl Pts',(56.5629025346554,-65.3730452421391,
-208.637340870275));
#209780=CARTESIAN_POINT('Ctrl Pts',(56.5598023265609,-65.3769921095606,
-208.606359994172));
#209781=CARTESIAN_POINT('Ctrl Pts',(56.5563780436769,-65.3813515558121,
-208.572140586786));
#209782=CARTESIAN_POINT('Ctrl Pts',(56.5528988257772,-65.3857275999304,
-208.540073180714));
#209783=CARTESIAN_POINT('Ctrl Pts',(56.5493950389307,-65.390088291123,-208.510120866391));
#209784=CARTESIAN_POINT('Ctrl Pts',(56.5487734136095,-65.3908619443679,
-208.504806868186));
#209785=CARTESIAN_POINT('Ctrl Pts',(56.5481511020616,-65.3916350213848,
-208.499559408636));
#209786=CARTESIAN_POINT('Ctrl Pts',(56.5475283779876,-65.3924072326121,
-208.494378238166));
#209787=CARTESIAN_POINT('Ctrl Pts',(56.5453287383415,-65.3951349036653,
-208.476076861271));
#209788=CARTESIAN_POINT('Ctrl Pts',(56.5431272051926,-65.3978490668695,
-208.45856228272));
#209789=CARTESIAN_POINT('Ctrl Pts',(56.5408939522005,-65.4005806848653,
-208.441891167501));
#209790=CARTESIAN_POINT('Ctrl Pts',(56.5385406282808,-65.4034591684012,
-208.424323729171));
#209791=CARTESIAN_POINT('Ctrl Pts',(56.5361523910466,-65.4063567084215,
-208.407692546603));
#209792=CARTESIAN_POINT('Ctrl Pts',(56.5337249489466,-65.4092773915755,
-208.392024350581));
#209793=CARTESIAN_POINT('Ctrl Pts',(56.5310690780669,-65.4124729188087,
-208.374881735499));
#209794=CARTESIAN_POINT('Ctrl Pts',(56.5283665728401,-65.4156958368807,
-208.358891580038));
#209795=CARTESIAN_POINT('Ctrl Pts',(56.5256428710774,-65.4189189062079,
-208.344047558516));
#209796=CARTESIAN_POINT('Ctrl Pts',(56.5254666684109,-65.4191274141355,
-208.343087263886));
#209797=CARTESIAN_POINT('Ctrl Pts',(56.5252903858615,-65.4193359134402,
-208.342131753863));
#209798=CARTESIAN_POINT('Ctrl Pts',(56.5251140337793,-65.4195443931164,
-208.341181021962));
#209799=CARTESIAN_POINT('Ctrl Pts',(56.5232954613085,-65.4216942707653,
-208.331376913944));
#209800=CARTESIAN_POINT('Ctrl Pts',(56.5214784629796,-65.4238324204977,
-208.322080413569));
#209801=CARTESIAN_POINT('Ctrl Pts',(56.5196276349714,-65.4259963733911,
-208.313319636639));
#209802=CARTESIAN_POINT('Ctrl Pts',(56.5175968875829,-65.4283706846008,
-208.303707222741));
#209803=CARTESIAN_POINT('Ctrl Pts',(56.5155255808571,-65.4307758824906,
-208.294739604155));
#209804=CARTESIAN_POINT('Ctrl Pts',(56.5134060791767,-65.4332201265201,
-208.286419651956));
#209805=CARTESIAN_POINT('Ctrl Pts',(56.5118129578226,-65.4350573401415,
-208.280165968067));
#209806=CARTESIAN_POINT('Ctrl Pts',(56.5101935109831,-65.4369156575986,
-208.274277409077));
#209807=CARTESIAN_POINT('Ctrl Pts',(56.5085556806693,-65.438786705909,-208.268745398167));
#209808=CARTESIAN_POINT('Ctrl Pts',(56.507131055958,-65.4404141893159,-208.263933520294));
#209809=CARTESIAN_POINT('Ctrl Pts',(56.5056850988358,-65.442059709221,-208.259369841015));
#209810=CARTESIAN_POINT('Ctrl Pts',(56.504210950984,-65.4437291528628,-208.255130145768));
#209811=CARTESIAN_POINT('Ctrl Pts',(56.5026151415113,-65.4455363759132,
-208.250540547902));
#209812=CARTESIAN_POINT('Ctrl Pts',(56.5009863989148,-65.4473715290094,
-208.246330361089));
#209813=CARTESIAN_POINT('Ctrl Pts',(56.4993319052539,-65.4492261566959,
-208.242536805959));
#209814=CARTESIAN_POINT('Ctrl Pts',(56.4983885522403,-65.4502836213804,
-208.240373810869));
#209815=CARTESIAN_POINT('Ctrl Pts',(56.4974371021737,-65.4513471421316,
-208.238345233095));
#209816=CARTESIAN_POINT('Ctrl Pts',(56.4964806846606,-65.4524133534391,
-208.236451053781));
#209817=CARTESIAN_POINT('Ctrl Pts',(56.4952333113097,-65.4538039214214,
-208.233980638125));
#209818=CARTESIAN_POINT('Ctrl Pts',(56.493956861388,-65.4552217028158,-208.231715946767));
#209819=CARTESIAN_POINT('Ctrl Pts',(56.4926742013412,-65.4566408027887,
-208.229722706621));
#209820=CARTESIAN_POINT('Ctrl Pts',(56.4912629399021,-65.4582021838225,
-208.227529621271));
#209821=CARTESIAN_POINT('Ctrl Pts',(56.4898441983158,-65.4597651242878,
-208.225664960423));
#209822=CARTESIAN_POINT('Ctrl Pts',(56.4884441179479,-65.4613010606549,
-208.224151229051));
#209823=CARTESIAN_POINT('Ctrl Pts',(56.4869391839692,-65.4629520250432,
-208.222524132615));
#209824=CARTESIAN_POINT('Ctrl Pts',(56.4854558349875,-65.4645717792676,
-208.221301691147));
#209825=CARTESIAN_POINT('Ctrl Pts',(56.4840212932626,-65.4661317407865,
-208.220448513651));
#209826=CARTESIAN_POINT('Ctrl Pts',(56.4823555603527,-65.4679431061828,
-208.219457837807));
#209827=CARTESIAN_POINT('Ctrl Pts',(56.4807557628038,-65.469673732465,-208.218964148661));
#209828=CARTESIAN_POINT('Ctrl Pts',(56.4792563268586,-65.4712890580059,
-208.218842434544));
#209829=CARTESIAN_POINT('Ctrl Pts',(56.4789992766148,-65.4715659753529,
-208.218821568935));
#209830=CARTESIAN_POINT('Ctrl Pts',(56.4787451563535,-65.4718395275162,
-208.218811515426));
#209831=CARTESIAN_POINT('Ctrl Pts',(56.478494115784,-65.4721095684411,-208.218811515426));
#209832=CARTESIAN_POINT('Ctrl Pts',(56.4785498900846,-65.4721614184049,
-208.210085312209));
#209833=CARTESIAN_POINT('Ctrl Pts',(56.4880134607985,-65.4619815336005,
-208.210087283952));
#209834=CARTESIAN_POINT('Ctrl Pts',(56.4960210114868,-65.4531537245717,
-208.218228453105));
#209835=CARTESIAN_POINT('Ctrl Pts',(56.5023726430475,-65.4460714077127,
-208.227728741309));
#209836=CARTESIAN_POINT('Ctrl Pts',(56.5087366507261,-65.4389752909997,
-208.23724754077));
#209837=CARTESIAN_POINT('Ctrl Pts',(56.513854727351,-65.433173044492,-208.248528534057));
#209838=CARTESIAN_POINT('Ctrl Pts',(56.5183608448225,-65.4280233981992,
-208.260025266392));
#209839=CARTESIAN_POINT('Ctrl Pts',(56.527384064744,-65.4177115518456,-208.283046757708));
#209840=CARTESIAN_POINT('Ctrl Pts',(56.5341620389057,-65.4097760673606,
-208.307543894395));
#209841=CARTESIAN_POINT('Ctrl Pts',(56.5402792876314,-65.4025401997578,
-208.332463842479));
#209842=CARTESIAN_POINT('Ctrl Pts',(56.5525225633485,-65.3880580810659,
-208.382339498829));
#209843=CARTESIAN_POINT('Ctrl Pts',(56.5617281325892,-65.3767964110653,
-208.434008552021));
#209844=CARTESIAN_POINT('Ctrl Pts',(56.5699429720804,-65.3666008613971,
-208.485663414341));
#209845=CARTESIAN_POINT('Ctrl Pts',(56.5863768923929,-65.346204498088,-208.588999808438));
#209846=CARTESIAN_POINT('Ctrl Pts',(56.5986107835984,-65.3302917454577,
-208.693643261059));
#209847=CARTESIAN_POINT('Ctrl Pts',(56.6095793668545,-65.3157298046138,
-208.79868090921));
#209848=CARTESIAN_POINT('Ctrl Pts',(56.6315196526886,-65.2866017817001,
-209.008786076848));
#209849=CARTESIAN_POINT('Ctrl Pts',(56.6477302855814,-65.2635991432574,
-209.220347327344));
#209850=CARTESIAN_POINT('Ctrl Pts',(56.6621411615825,-65.2425322660162,
-209.431932106333));
#209851=CARTESIAN_POINT('Ctrl Pts',(56.6909646006573,-65.200396045247,-209.855126434415));
#209852=CARTESIAN_POINT('Ctrl Pts',(56.7118400320305,-65.1667793523224,
-210.279522418803));
#209853=CARTESIAN_POINT('Ctrl Pts',(56.7302042319515,-65.1358555723291,
-210.704298191088));
#209854=CARTESIAN_POINT('Ctrl Pts',(56.7669339286709,-65.0740058285095,
-211.553879733265));
#209855=CARTESIAN_POINT('Ctrl Pts',(56.7925011773325,-65.0241321427268,
-212.404891259688));
#209856=CARTESIAN_POINT('Ctrl Pts',(56.8144552965909,-64.9781464054155,
-213.256094899172));
#209857=CARTESIAN_POINT('Origin',(0.,-12.9675000200281,-208.218811515427));
#209858=CARTESIAN_POINT('Origin',(0.,-12.9675000200281,-208.218811515427));
#209859=CARTESIAN_POINT('Origin',(0.,-12.9675000200281,-208.210085312208));
#209860=CARTESIAN_POINT('Ctrl Pts',(56.7131249770401,39.136390603742,-213.924107582134));
#209861=CARTESIAN_POINT('Ctrl Pts',(56.6591708158967,39.1947585157316,-213.928380187744));
#209862=CARTESIAN_POINT('Ctrl Pts',(56.6260312186758,39.26699791474,-213.932877779247));
#209863=CARTESIAN_POINT('Ctrl Pts',(56.6878438485494,39.1909973438446,-212.873680972192));
#209864=CARTESIAN_POINT('Ctrl Pts',(56.6390541381501,39.2436411705138,-212.880445101553));
#209865=CARTESIAN_POINT('Ctrl Pts',(56.6069323298669,39.308101280162,-212.882516880404));
#209866=CARTESIAN_POINT('Ctrl Pts',(56.6594850052376,39.248900569515,-211.823591080281));
#209867=CARTESIAN_POINT('Ctrl Pts',(56.6161967667701,39.2955248737877,-211.830328584023));
#209868=CARTESIAN_POINT('Ctrl Pts',(56.5855128843193,39.3516918804354,-211.83240628728));
#209869=CARTESIAN_POINT('Ctrl Pts',(56.5961170971406,39.3557075607436,-210.338665903179));
#209870=CARTESIAN_POINT('Ctrl Pts',(56.5632284029528,39.3910644172893,-210.343434951173));
#209871=CARTESIAN_POINT('Ctrl Pts',(56.5376887518409,39.4321195627096,-210.347455422068));
#209872=CARTESIAN_POINT('Ctrl Pts',(56.5749226987295,39.3898533622913,-209.90220762928));
#209873=CARTESIAN_POINT('Ctrl Pts',(56.5454235880735,39.4215267027753,-209.906981158345));
#209874=CARTESIAN_POINT('Ctrl Pts',(56.5216963051399,39.4578331766847,-209.910997266658));
#209875=CARTESIAN_POINT('Ctrl Pts',(56.5309467959293,39.4540847109595,-209.24891615073));
#209876=CARTESIAN_POINT('Ctrl Pts',(56.5079716151444,39.4786993973283,-209.253391637796));
#209877=CARTESIAN_POINT('Ctrl Pts',(56.4885248990568,39.506210827646,-209.257701934938));
#209878=CARTESIAN_POINT('Ctrl Pts',(56.5144681134185,39.4774389991119,-209.031360415952));
#209879=CARTESIAN_POINT('Ctrl Pts',(56.4938957981811,39.4994537797928,-209.035838362477));
#209880=CARTESIAN_POINT('Ctrl Pts',(56.4760962345234,39.5238015154724,-209.040146260381));
#209881=CARTESIAN_POINT('Ctrl Pts',(56.4809774462897,39.5218092152179,-208.707139552256));
#209882=CARTESIAN_POINT('Ctrl Pts',(56.4650653119284,39.5387956857416,-208.711547487502));
#209883=CARTESIAN_POINT('Ctrl Pts',(56.4508419233835,39.557225742165,-208.715924510879));
#209884=CARTESIAN_POINT('Ctrl Pts',(56.4685043569935,39.5379957558533,-208.599289345334));
#209885=CARTESIAN_POINT('Ctrl Pts',(56.4543082678724,39.5531313413699,-208.603698519052));
#209886=CARTESIAN_POINT('Ctrl Pts',(56.4414369686318,39.5694195255203,-208.60807433386));
#209887=CARTESIAN_POINT('Ctrl Pts',(56.4433791076362,39.5690861270511,-208.439774659198));
#209888=CARTESIAN_POINT('Ctrl Pts',(56.4325361263003,39.5806119265652,-208.444168467643));
#209889=CARTESIAN_POINT('Ctrl Pts',(56.4224946430317,39.5928429539091,-208.448559464111));
#209890=CARTESIAN_POINT('Ctrl Pts',(56.434042377723,39.5804730986549,-208.386840352034));
#209891=CARTESIAN_POINT('Ctrl Pts',(56.4244358024192,39.5906684103489,-208.391234746251));
#209892=CARTESIAN_POINT('Ctrl Pts',(56.4154558353936,39.6014220979252,-208.395625171312));
#209893=CARTESIAN_POINT('Ctrl Pts',(56.4153197235611,39.602540640524,-208.309894071191));
#209894=CARTESIAN_POINT('Ctrl Pts',(56.4081423174308,39.6101253887744,-208.314285655015));
#209895=CARTESIAN_POINT('Ctrl Pts',(56.4013424744876,39.6180493256973,-208.318678862813));
#209896=CARTESIAN_POINT('Ctrl Pts',(56.4083623316493,39.6106555249509,-208.284557461711));
#209897=CARTESIAN_POINT('Ctrl Pts',(56.4020826208256,39.6172758938669,-208.288949312307));
#209898=CARTESIAN_POINT('Ctrl Pts',(56.3960980548982,39.6241637622927,-208.293342260033));
#209899=CARTESIAN_POINT('Ctrl Pts',(56.3945592936364,39.6263652686867,-208.249138326507));
#209900=CARTESIAN_POINT('Ctrl Pts',(56.3900359410543,39.6311005791763,-208.253529947332));
#209901=CARTESIAN_POINT('Ctrl Pts',(56.3856941549037,39.6360014284045,-208.257923126188));
#209902=CARTESIAN_POINT('Ctrl Pts',(56.3894732411015,39.6321076620074,-208.237848616086));
#209903=CARTESIAN_POINT('Ctrl Pts',(56.3855943263936,39.6361515194816,-208.24224035659));
#209904=CARTESIAN_POINT('Ctrl Pts',(56.3818606603298,39.6403285142035,-208.246633418771));
#209905=CARTESIAN_POINT('Ctrl Pts',(56.2937742808158,39.7383680155035,-208.093554903205));
#209906=CARTESIAN_POINT('Ctrl Pts',(56.3019347808255,39.7295012949887,-208.097988441706));
#209907=CARTESIAN_POINT('Ctrl Pts',(56.3097336024218,39.7204021456198,-208.102340277927));
#209908=CARTESIAN_POINT('Ctrl Pts',(55.901541357958,40.1547597432569,-208.230910731216));
#209909=CARTESIAN_POINT('Ctrl Pts',(55.957654116832,40.0945682331347,-208.235168290733));
#209910=CARTESIAN_POINT('Ctrl Pts',(56.0141418475234,40.0342093581467,-208.239693755738));
#209911=CARTESIAN_POINT('Ctrl Pts',(55.1111144719458,40.5151527971883,-226.746035420514));
#209912=CARTESIAN_POINT('Ctrl Pts',(55.1914520133701,40.4117219444719,-227.50020914733));
#209913=CARTESIAN_POINT('Ctrl Pts',(55.4188282852024,40.3069503931471,-226.764375983926));
#209914=CARTESIAN_POINT('',(56.699489854167,39.164766900886,-213.398999668926));
#209915=CARTESIAN_POINT('',(56.6162420139465,39.2878063792742,-213.407725872324));
#209916=CARTESIAN_POINT('Origin',(57.0675004159511,39.5031336989999,-213.407725872324));
#209917=CARTESIAN_POINT('',(56.3587426896623,39.6656306474361,-208.218811515434));
#209918=CARTESIAN_POINT('Ctrl Pts',(56.3587426896624,39.665630647436,-208.218811515434));
#209919=CARTESIAN_POINT('Ctrl Pts',(56.3601495832745,39.6641241675047,-208.218811515434));
#209920=CARTESIAN_POINT('Ctrl Pts',(56.3616493238422,39.6625121262006,-208.219123491817));
#209921=CARTESIAN_POINT('Ctrl Pts',(56.3632133291857,39.6608228164564,-208.219864826396));
#209922=CARTESIAN_POINT('Ctrl Pts',(56.3646224181208,39.6593008346561,-208.22053273099));
#209923=CARTESIAN_POINT('Ctrl Pts',(56.3660836031149,39.6577161880681,-208.221550081639));
#209924=CARTESIAN_POINT('Ctrl Pts',(56.3675724084783,39.6560941073193,-208.222966468907));
#209925=CARTESIAN_POINT('Ctrl Pts',(56.3689541239424,39.6545887029798,-208.224280975315));
#209926=CARTESIAN_POINT('Ctrl Pts',(56.3703595934114,39.6530510813804,-208.225939838963));
#209927=CARTESIAN_POINT('Ctrl Pts',(56.3717666744691,39.6515050309337,-208.227939015451));
#209928=CARTESIAN_POINT('Ctrl Pts',(56.3730638621233,39.6500797274366,-208.229782055725));
#209929=CARTESIAN_POINT('Ctrl Pts',(56.3743623913668,39.6486472843762,-208.231914630948));
#209930=CARTESIAN_POINT('Ctrl Pts',(56.3756430732668,39.6472291934253,-208.234288738312));
#209931=CARTESIAN_POINT('Ctrl Pts',(56.376094096522,39.6467297782334,-208.235124837918));
#209932=CARTESIAN_POINT('Ctrl Pts',(56.3765428903921,39.6462321689465,-208.235990441946));
#209933=CARTESIAN_POINT('Ctrl Pts',(56.3769885653368,39.6457373905793,-208.236881866521));
#209934=CARTESIAN_POINT('Ctrl Pts',(56.37881285369,39.6437121064042,-208.24053074894));
#209935=CARTESIAN_POINT('Ctrl Pts',(56.3806052038614,39.6417121634959,-208.244629681269));
#209936=CARTESIAN_POINT('Ctrl Pts',(56.3823572094279,39.6397463121279,-208.249191218014));
#209937=CARTESIAN_POINT('Ctrl Pts',(56.3839571735553,39.6379510600302,-208.253356898361));
#209938=CARTESIAN_POINT('Ctrl Pts',(56.3855233415072,39.6361843954567,-208.257908600676));
#209939=CARTESIAN_POINT('Ctrl Pts',(56.3870701495925,39.6344312926996,-208.262824066145));
#209940=CARTESIAN_POINT('Ctrl Pts',(56.3877712828556,39.6336366507085,-208.265052135921));
#209941=CARTESIAN_POINT('Ctrl Pts',(56.388468749925,39.6328444709097,-208.267354469389));
#209942=CARTESIAN_POINT('Ctrl Pts',(56.3891656252778,39.6320515532012,-208.269726355525));
#209943=CARTESIAN_POINT('Ctrl Pts',(56.3913816577841,39.6295301102924,-208.277268847532));
#209944=CARTESIAN_POINT('Ctrl Pts',(56.3935673157433,39.6270280076159,-208.285480742852));
#209945=CARTESIAN_POINT('Ctrl Pts',(56.3957051192765,39.6245637499415,-208.294372756304));
#209946=CARTESIAN_POINT('Ctrl Pts',(56.3976391821956,39.6223343451728,-208.302417327858));
#209947=CARTESIAN_POINT('Ctrl Pts',(56.3995339263727,39.6201360741756,-208.311018721799));
#209948=CARTESIAN_POINT('Ctrl Pts',(56.4013976801705,39.6179604017859,-208.320157411357));
#209949=CARTESIAN_POINT('Ctrl Pts',(56.4029651061584,39.6161306507486,-208.327843093621));
#209950=CARTESIAN_POINT('Ctrl Pts',(56.4045108040343,39.6143166839342,-208.335908542756));
#209951=CARTESIAN_POINT('Ctrl Pts',(56.4060546455774,39.6124978246064,-208.344323125453));
#209952=CARTESIAN_POINT('Ctrl Pts',(56.4088227595351,39.6092366026791,-208.35941050532));
#209953=CARTESIAN_POINT('Ctrl Pts',(56.4115687404984,39.6059763732055,-208.375650545353));
#209954=CARTESIAN_POINT('Ctrl Pts',(56.414266332437,39.6027448960211,-208.393061304987));
#209955=CARTESIAN_POINT('Ctrl Pts',(56.4167639475216,39.5997529734676,-208.409181376846));
#209956=CARTESIAN_POINT('Ctrl Pts',(56.4192197492829,39.5967860493275,-208.426305292677));
#209957=CARTESIAN_POINT('Ctrl Pts',(56.4216387710761,39.5938389153697,-208.444423890791));
#209958=CARTESIAN_POINT('Ctrl Pts',(56.4239005683569,39.5910833306161,-208.461364869191));
#209959=CARTESIAN_POINT('Ctrl Pts',(56.4261299837435,39.5883452872419,-208.479175614652));
#209960=CARTESIAN_POINT('Ctrl Pts',(56.4283584828494,39.5855917216612,-208.49782421793));
#209961=CARTESIAN_POINT('Ctrl Pts',(56.4285133927028,39.585400312816,-208.499120539922));
#209962=CARTESIAN_POINT('Ctrl Pts',(56.428668310598,39.5852088158322,-208.500420899441));
#209963=CARTESIAN_POINT('Ctrl Pts',(56.4288232528699,39.5850172135307,-208.501725280663));
#209964=CARTESIAN_POINT('Ctrl Pts',(56.432293438562,39.580725966494,-208.530939032316));
#209965=CARTESIAN_POINT('Ctrl Pts',(56.4357490676031,39.5764097172179,-208.562213621881));
#209966=CARTESIAN_POINT('Ctrl Pts',(56.4391551317323,39.5721053282918,-208.595581146484));
#209967=CARTESIAN_POINT('Ctrl Pts',(56.4423216937235,39.5681036084618,-208.626602387169));
#209968=CARTESIAN_POINT('Ctrl Pts',(56.4454450058205,39.5641125747319,-208.659432798495));
#209969=CARTESIAN_POINT('Ctrl Pts',(56.4485249814543,39.5601321607569,-208.694080862067));
#209970=CARTESIAN_POINT('Ctrl Pts',(56.451369297175,39.5564563024417,-208.726077878807));
#209971=CARTESIAN_POINT('Ctrl Pts',(56.4541764558065,39.5527897115675,-208.759625141864));
#209972=CARTESIAN_POINT('Ctrl Pts',(56.4569751886937,39.5491018419698,-208.794711891478));
#209973=CARTESIAN_POINT('Ctrl Pts',(56.4577444522914,39.5480881890244,-208.804355884073));
#209974=CARTESIAN_POINT('Ctrl Pts',(56.4585132677862,39.5470727289412,-208.814116069679));
#209975=CARTESIAN_POINT('Ctrl Pts',(56.4592826862095,39.5460543462138,-208.823991952248));
#209976=CARTESIAN_POINT('Ctrl Pts',(56.4635914453566,39.5403513817942,-208.879297099709));
#209977=CARTESIAN_POINT('Ctrl Pts',(56.4678871861578,39.5345902747531,-208.938264807565));
#209978=CARTESIAN_POINT('Ctrl Pts',(56.4721263985457,39.5288164538003,-209.000955538769));
#209979=CARTESIAN_POINT('Ctrl Pts',(56.4760642649888,39.523453066997,-209.059189876687));
#209980=CARTESIAN_POINT('Ctrl Pts',(56.4799529250891,39.5180791658712,-209.120636905201));
#209981=CARTESIAN_POINT('Ctrl Pts',(56.4837859987149,39.5127008938574,-209.185332844094));
#209982=CARTESIAN_POINT('Ctrl Pts',(56.4873081739301,39.5077588504122,-209.244781332365));
#209983=CARTESIAN_POINT('Ctrl Pts',(56.4907832286359,39.5028133138086,-209.306973134386));
#209984=CARTESIAN_POINT('Ctrl Pts',(56.4942351443273,39.4978383106628,-209.37192419101));
#209985=CARTESIAN_POINT('Ctrl Pts',(56.4960297197263,39.4952519154396,-209.405690823447));
#209986=CARTESIAN_POINT('Ctrl Pts',(56.4978185487061,39.4926570170179,-209.440202996464));
#209987=CARTESIAN_POINT('Ctrl Pts',(56.4996087590354,39.4900459724346,-209.475461388355));
#209988=CARTESIAN_POINT('Ctrl Pts',(56.5048651761802,39.4823794210307,-209.578987109661));
#209989=CARTESIAN_POINT('Ctrl Pts',(56.5100972729331,39.4746123732906,-209.688950789672));
#209990=CARTESIAN_POINT('Ctrl Pts',(56.5152526591312,39.4667985899322,-209.805474420592));
#209991=CARTESIAN_POINT('Ctrl Pts',(56.5200402606557,39.4595422410028,-209.913685268741));
#209992=CARTESIAN_POINT('Ctrl Pts',(56.5247612649405,39.4522460582652,-210.02755354853));
#209993=CARTESIAN_POINT('Ctrl Pts',(56.5294024349243,39.4449224211257,-210.147172612983));
#209994=CARTESIAN_POINT('Ctrl Pts',(56.5336452006572,39.4382274548126,-210.256523416644));
#209995=CARTESIAN_POINT('Ctrl Pts',(56.5378210834422,39.431509723132,-210.370680096185));
#209996=CARTESIAN_POINT('Ctrl Pts',(56.5419487316549,39.4247479639329,-210.489709612087));
#209997=CARTESIAN_POINT('Ctrl Pts',(56.5452447224076,39.4193485949355,-210.584756516158));
#209998=CARTESIAN_POINT('Ctrl Pts',(56.5485103637142,39.4139207189296,-210.682910410159));
#209999=CARTESIAN_POINT('Ctrl Pts',(56.5517715302822,39.4084360149103,-210.784202905567));
#210000=CARTESIAN_POINT('Ctrl Pts',(56.5579467539937,39.398050383387,-210.97600660722));
#210001=CARTESIAN_POINT('Ctrl Pts',(56.5640670191006,39.3875025211926,-211.179071278287));
#210002=CARTESIAN_POINT('Ctrl Pts',(56.5700699283836,39.3768543172624,-211.393646924193));
#210003=CARTESIAN_POINT('Ctrl Pts',(56.5756452528862,39.3669645805561,-211.592938434341));
#210004=CARTESIAN_POINT('Ctrl Pts',(56.5811189037804,39.3569887584367,-211.802159549538));
#210005=CARTESIAN_POINT('Ctrl Pts',(56.5864687201405,39.3469466599906,-212.021505773689));
#210006=CARTESIAN_POINT('Ctrl Pts',(56.5916371677434,39.3372450074199,-212.233415751551));
#210007=CARTESIAN_POINT('Ctrl Pts',(56.5966894928584,39.3274820752966,-212.454776044889));
#210008=CARTESIAN_POINT('Ctrl Pts',(56.6016398763514,39.3176391858333,-212.685757113719));
#210009=CARTESIAN_POINT('Ctrl Pts',(56.6061501516399,39.3086713672439,-212.896203073781));
#210010=CARTESIAN_POINT('Ctrl Pts',(56.6105757435957,39.2996372422124,-213.114635211445));
#210011=CARTESIAN_POINT('Ctrl Pts',(56.614959710428,39.290488109814,-213.341176963337));
#210012=CARTESIAN_POINT('Ctrl Pts',(56.6153874935782,39.289595346518,-213.363282683563));
#210013=CARTESIAN_POINT('Ctrl Pts',(56.6158149084831,39.2887014581205,-213.385465616055));
#210014=CARTESIAN_POINT('Ctrl Pts',(56.6162420139465,39.2878063792742,-213.407725872324));
#210015=CARTESIAN_POINT('',(56.3587983457046,39.6656826243185,-208.210085312216));
#210016=CARTESIAN_POINT('Origin',(56.7241679835722,40.0068993898824,-208.218811515434));
#210017=CARTESIAN_POINT('Ctrl Pts',(56.6994898617306,39.1647669078403,-213.398999669105));
#210018=CARTESIAN_POINT('Ctrl Pts',(56.6773193211235,39.2114480278548,-212.523894235562));
#210019=CARTESIAN_POINT('Ctrl Pts',(56.651479770637,39.2620537363991,-211.649203631226));
#210020=CARTESIAN_POINT('Ctrl Pts',(56.5956975036787,39.3561498317412,-210.339090933364));
#210021=CARTESIAN_POINT('Ctrl Pts',(56.5745517354038,39.3902416134919,-209.902674994602));
#210022=CARTESIAN_POINT('Ctrl Pts',(56.5306742644768,39.4543652326716,-209.24942443662));
#210023=CARTESIAN_POINT('Ctrl Pts',(56.5142321837007,39.4776795989311,-209.03188052566));
#210024=CARTESIAN_POINT('Ctrl Pts',(56.480816494081,39.5219692158454,-208.70764780547));
#210025=CARTESIAN_POINT('Ctrl Pts',(56.4683713984661,39.5381257486172,-208.599790912822));
#210026=CARTESIAN_POINT('Ctrl Pts',(56.4433041343981,39.569154837062,-208.440233728844));
#210027=CARTESIAN_POINT('Ctrl Pts',(56.4339894177057,39.5805185781009,-208.387282545977));
#210028=CARTESIAN_POINT('Ctrl Pts',(56.4153107858428,39.6025404853857,-208.310273287259));
#210029=CARTESIAN_POINT('Ctrl Pts',(56.4083698728123,39.6106383616431,-208.284910555051));
#210030=CARTESIAN_POINT('Ctrl Pts',(56.394596442102,39.6263182576719,-208.249418094709));
#210031=CARTESIAN_POINT('Ctrl Pts',(56.3895186643059,39.6320526747255,-208.238093899573));
#210032=CARTESIAN_POINT('Ctrl Pts',(56.3765990499463,39.6464010040802,-208.218501926116));
#210033=CARTESIAN_POINT('Ctrl Pts',(56.3682899804801,39.6555191285273,-208.210085312216));
#210034=CARTESIAN_POINT('Ctrl Pts',(56.3587983457046,39.6656826243185,-208.210085312216));
#210035=CARTESIAN_POINT('Origin',(0.,-12.9675000200281,-208.218811515434));
#210036=CARTESIAN_POINT('',(52.2148720050704,43.7789665035542,-208.218811515434));
#210037=CARTESIAN_POINT('',(52.2149235689092,43.779022542486,-208.210085312216));
#210038=CARTESIAN_POINT('Origin',(52.5534287939255,44.1469057658247,-208.218811515435));
#210039=CARTESIAN_POINT('Origin',(0.,-12.9675000200281,-208.210085312216));
#210040=CARTESIAN_POINT('Origin',(0.,-12.9675000200281,-208.218811515434));
#210041=CARTESIAN_POINT('Ctrl Pts',(56.6214560695998,39.2782015364689,-213.075568750364));
#210042=CARTESIAN_POINT('Ctrl Pts',(56.654483236613,39.2080032797481,-213.086332264511));
#210043=CARTESIAN_POINT('Ctrl Pts',(56.7071198771834,39.1517102271814,-213.09704916438));
#210044=CARTESIAN_POINT('Ctrl Pts',(56.6004809601567,39.3177369985946,-213.475440414112));
#210045=CARTESIAN_POINT('Ctrl Pts',(56.6315613449632,39.2557964829605,-213.467329046301));
#210046=CARTESIAN_POINT('Ctrl Pts',(56.6782189205445,39.2033836493307,-213.460581076327));
#210047=CARTESIAN_POINT('Ctrl Pts',(56.6372034409747,39.2511121778754,-213.828824822694));
#210048=CARTESIAN_POINT('Ctrl Pts',(56.6720387769172,39.1751400320608,-213.807827408045));
#210049=CARTESIAN_POINT('Ctrl Pts',(56.7283118338796,39.116606690349,-213.781595977465));
#210050=CARTESIAN_POINT('Ctrl Pts',(56.6987085996655,39.0810160666721,-214.413338469428));
#210051=CARTESIAN_POINT('Ctrl Pts',(56.7321412993442,38.9737779499193,-214.361684674043));
#210052=CARTESIAN_POINT('Ctrl Pts',(56.8155652495982,38.8966330687837,-214.312698211001));
#210053=CARTESIAN_POINT('Ctrl Pts',(56.7239630070022,38.9928957520747,-214.64988909805));
#210054=CARTESIAN_POINT('Ctrl Pts',(56.7546676004383,38.8685060470322,-214.586687956946));
#210055=CARTESIAN_POINT('Ctrl Pts',(56.8524370552797,38.7830099878374,-214.527620279871));
#210056=CARTESIAN_POINT('Ctrl Pts',(56.7797859812607,38.6711930024679,-215.430608964657));
#210057=CARTESIAN_POINT('Ctrl Pts',(56.7896319635179,38.4831137119568,-215.334185599672));
#210058=CARTESIAN_POINT('Ctrl Pts',(56.9411099182686,38.3701449194622,-215.236934347207));
#210059=CARTESIAN_POINT('Ctrl Pts',(56.7727925783854,38.4015216091642,-215.952884479091));
#210060=CARTESIAN_POINT('Ctrl Pts',(56.7377496633354,38.1576856081976,-215.83078434059));
#210061=CARTESIAN_POINT('Ctrl Pts',(56.9475441086433,38.0266995615636,-215.711762130513));
#210062=CARTESIAN_POINT('Ctrl Pts',(56.6685131435906,38.118834322735,-216.461270781929));
#210063=CARTESIAN_POINT('Ctrl Pts',(56.576365951004,37.8732757014601,-216.253572790495));
#210064=CARTESIAN_POINT('Ctrl Pts',(56.8319648105423,37.6721636895405,-216.173673746282));
#210065=CARTESIAN_POINT('',(56.8784089882814,37.8494074227593,-215.942195856527));
#210066=CARTESIAN_POINT('',(56.7127812850717,38.2589564044561,-216.205851068199));
#210067=CARTESIAN_POINT('Origin',(57.1962194441171,38.1313337325768,-216.205851068199));
#210068=CARTESIAN_POINT('Ctrl Pts',(56.6162420139465,39.2878063792742,-213.407725872324));
#210069=CARTESIAN_POINT('Ctrl Pts',(56.6165277343106,39.2872075991701,-213.422617255017));
#210070=CARTESIAN_POINT('Ctrl Pts',(56.6168832113971,39.2864637908029,-213.437594243781));
#210071=CARTESIAN_POINT('Ctrl Pts',(56.6173071902525,39.2855743587294,-213.452656838247));
#210072=CARTESIAN_POINT('Ctrl Pts',(56.6185791268188,39.282906062509,-213.497844621643));
#210073=CARTESIAN_POINT('Ctrl Pts',(56.6204684474054,39.2789275478084,-213.543802858157));
#210074=CARTESIAN_POINT('Ctrl Pts',(56.6229334705114,39.2736193407654,-213.590531548545));
#210075=CARTESIAN_POINT('Ctrl Pts',(56.6245768192488,39.27008053607,-213.621684008803));
#210076=CARTESIAN_POINT('Ctrl Pts',(56.626475810809,39.2659506824126,-213.653178892369));
#210077=CARTESIAN_POINT('Ctrl Pts',(56.6286148188683,39.2612228888315,-213.68501619841));
#210078=CARTESIAN_POINT('Ctrl Pts',(56.6296843228979,39.258858992041,-213.700934851431));
#210079=CARTESIAN_POINT('Ctrl Pts',(56.6308137885021,39.2563455917412,-213.716939110088));
#210080=CARTESIAN_POINT('Ctrl Pts',(56.6320009587241,39.2536817324465,-213.733028974519));
#210081=CARTESIAN_POINT('Ctrl Pts',(56.6325945438351,39.2523498027992,-213.741073906734));
#210082=CARTESIAN_POINT('Ctrl Pts',(56.6332025518579,39.2509802568528,-213.749140240395));
#210083=CARTESIAN_POINT('Ctrl Pts',(56.6338246786909,39.2495729676807,-213.757227975525));
#210084=CARTESIAN_POINT('Ctrl Pts',(56.6343290486238,39.2484320518617,-213.763784854618));
#210085=CARTESIAN_POINT('Ctrl Pts',(56.6349037212799,39.2471275146199,-213.771128572755));
#210086=CARTESIAN_POINT('Ctrl Pts',(56.6354002884089,39.2459963926713,-213.777379412664));
#210087=CARTESIAN_POINT('Ctrl Pts',(56.6355162235629,39.2457323059252,-213.778838816731));
#210088=CARTESIAN_POINT('Ctrl Pts',(56.6356278283714,39.2454778780714,-213.780238734505));
#210089=CARTESIAN_POINT('Ctrl Pts',(56.6357330959044,39.2452377374264,-213.781555385346));
#210090=CARTESIAN_POINT('Ctrl Pts',(56.636845383284,39.2427003415081,-213.795467501181));
#210091=CARTESIAN_POINT('Ctrl Pts',(56.6380061653357,39.2400336252933,-213.809533615601));
#210092=CARTESIAN_POINT('Ctrl Pts',(56.6392133653724,39.2372367967664,-213.823753728813));
#210093=CARTESIAN_POINT('Ctrl Pts',(56.6424287823681,39.2297873520133,-213.861629467972));
#210094=CARTESIAN_POINT('Ctrl Pts',(56.6459740125889,39.2214162094164,-213.900598182719));
#210095=CARTESIAN_POINT('Ctrl Pts',(56.6498032020704,39.2121020323048,-213.940658617166));
#210096=CARTESIAN_POINT('Ctrl Pts',(56.6502869191469,39.2109254317358,-213.945719196259));
#210097=CARTESIAN_POINT('Ctrl Pts',(56.6507751265893,39.2097338312328,-213.950797222392));
#210098=CARTESIAN_POINT('Ctrl Pts',(56.6512676955233,39.2085272315157,-213.955892716039));
#210099=CARTESIAN_POINT('Ctrl Pts',(56.6541955830412,39.2013550612736,-213.986180927933));
#210100=CARTESIAN_POINT('Ctrl Pts',(56.6572790751068,39.1936506663972,-214.017085134124));
#210101=CARTESIAN_POINT('Ctrl Pts',(56.6604911051498,39.1854043760091,-214.048605333297));
#210102=CARTESIAN_POINT('Ctrl Pts',(56.6620971201713,39.181281230815,-214.064365432883));
#210103=CARTESIAN_POINT('Ctrl Pts',(56.6637351748836,39.1770225746252,-214.08027953076));
#210104=CARTESIAN_POINT('Ctrl Pts',(56.6654011751468,39.1726270545194,-214.096347627154));
#210105=CARTESIAN_POINT('Ctrl Pts',(56.6662341752783,39.1704292944666,-214.104381675351));
#210106=CARTESIAN_POINT('Ctrl Pts',(56.6670741539691,39.1681973156772,-214.112454223184));
#210107=CARTESIAN_POINT('Ctrl Pts',(56.6679205467032,39.1659309368603,-214.120565270699));
#210108=CARTESIAN_POINT('Ctrl Pts',(56.6686382008055,39.1640092804117,-214.127442605876));
#210109=CARTESIAN_POINT('Ctrl Pts',(56.6694887205913,39.1617155181499,-214.135571608633));
#210110=CARTESIAN_POINT('Ctrl Pts',(56.6701455208158,39.1599327774048,-214.141838684002));
#210111=CARTESIAN_POINT('Ctrl Pts',(56.6702633429838,39.1596129748655,-214.142962922971));
#210112=CARTESIAN_POINT('Ctrl Pts',(56.6703749277195,39.1593097487773,-214.14402729556));
#210113=CARTESIAN_POINT('Ctrl Pts',(56.6704783877725,39.159028345972,-214.145013884847));
#210114=CARTESIAN_POINT('Ctrl Pts',(56.6713398659602,39.156685196402,-214.153228892734));
#210115=CARTESIAN_POINT('Ctrl Pts',(56.6722080330432,39.1543049369045,-214.161487512375));
#210116=CARTESIAN_POINT('Ctrl Pts',(56.6730817428456,39.1518886370445,-214.169790761554));
#210117=CARTESIAN_POINT('Ctrl Pts',(56.6735877457118,39.1504892540327,-214.17459952972));
#210118=CARTESIAN_POINT('Ctrl Pts',(56.6740956287835,39.1490775454481,-214.179423011065));
#210119=CARTESIAN_POINT('Ctrl Pts',(56.6746052615809,39.1476536047955,-214.18426131276));
#210120=CARTESIAN_POINT('Ctrl Pts',(56.6796915033885,39.1334423795473,-214.232548574649));
#210121=CARTESIAN_POINT('Ctrl Pts',(56.684953508893,39.1180134548084,-214.282308281078));
#210122=CARTESIAN_POINT('Ctrl Pts',(56.6902997298246,39.1013256022754,-214.333539572759));
#210123=CARTESIAN_POINT('Ctrl Pts',(56.6951779830848,39.0860984779072,-214.380286465352));
#210124=CARTESIAN_POINT('Ctrl Pts',(56.7001262124787,39.0698230353042,-214.428258560292));
#210125=CARTESIAN_POINT('Ctrl Pts',(56.7050492608573,39.052496006805,-214.477456751543));
#210126=CARTESIAN_POINT('Ctrl Pts',(56.7101720338601,39.0344660328969,-214.52865087895));
#210127=CARTESIAN_POINT('Ctrl Pts',(56.7152706315545,39.0152903364839,-214.581171861781));
#210128=CARTESIAN_POINT('Ctrl Pts',(56.7202164165074,38.9949472473483,-214.635020459656));
#210129=CARTESIAN_POINT('Ctrl Pts',(56.720963128566,38.9918758582537,-214.643150493161));
#210130=CARTESIAN_POINT('Ctrl Pts',(56.7217062798833,38.9887779139132,-214.651310770207));
#210131=CARTESIAN_POINT('Ctrl Pts',(56.7224453422406,38.9856534013085,-214.659501272636));
#210132=CARTESIAN_POINT('Ctrl Pts',(56.7252624323166,38.9737436708722,-214.690721078222));
#210133=CARTESIAN_POINT('Ctrl Pts',(56.7280207596582,38.9614468560358,-214.722380406985));
#210134=CARTESIAN_POINT('Ctrl Pts',(56.7306885429869,38.9487598472382,-214.75447926351));
#210135=CARTESIAN_POINT('Ctrl Pts',(56.7320224346512,38.9424163428394,-214.770528691772));
#210136=CARTESIAN_POINT('Ctrl Pts',(56.7333336141141,38.9359752788485,-214.786688002162));
#210137=CARTESIAN_POINT('Ctrl Pts',(56.7346175684232,38.9294363703326,-214.802957195691));
#210138=CARTESIAN_POINT('Ctrl Pts',(56.7352595455777,38.9261669160747,-214.811091792455));
#210139=CARTESIAN_POINT('Ctrl Pts',(56.7358947107526,38.9228730002466,-214.819253860003));
#210140=CARTESIAN_POINT('Ctrl Pts',(56.7365224626186,38.919554591232,-214.827443398408));
#210141=CARTESIAN_POINT('Ctrl Pts',(56.7371502144845,38.9162361822173,-214.835632936812));
#210142=CARTESIAN_POINT('Ctrl Pts',(56.7378546750073,38.9124306555081,-214.844982606075));
#210143=CARTESIAN_POINT('Ctrl Pts',(56.7383831203994,38.9095243687999,-214.852093589858));
#210144=CARTESIAN_POINT('Ctrl Pts',(56.7390624730686,38.9057881386,-214.861235245527));
#210145=CARTESIAN_POINT('Ctrl Pts',(56.7397290362713,38.9020376117849,-214.870374141699));
#210146=CARTESIAN_POINT('Ctrl Pts',(56.7403822137486,38.8982733493814,-214.879510354443));
#210147=CARTESIAN_POINT('Ctrl Pts',(56.7470703821133,38.8597294289335,-214.973060011575));
#210148=CARTESIAN_POINT('Ctrl Pts',(56.7524888154197,38.8195967151214,-215.066647774888));
#210149=CARTESIAN_POINT('Ctrl Pts',(56.75629923383,38.7778906329865,-215.160439317411));
#210150=CARTESIAN_POINT('Ctrl Pts',(56.7567481817338,38.7729767741574,-215.171489945418));
#210151=CARTESIAN_POINT('Ctrl Pts',(56.7571747476926,38.7680410765947,-215.18254339977));
#210152=CARTESIAN_POINT('Ctrl Pts',(56.757578329166,38.7630835681807,-215.193599949725));
#210153=CARTESIAN_POINT('Ctrl Pts',(56.7606513461903,38.7253352849747,-215.277788567095));
#210154=CARTESIAN_POINT('Ctrl Pts',(56.7623974702021,38.686301527375,-215.362190731822));
#210155=CARTESIAN_POINT('Ctrl Pts',(56.762521509791,38.6459704543063,-215.447017807587));
#210156=CARTESIAN_POINT('Ctrl Pts',(56.7625655254613,38.6316589008054,-215.477118847326));
#210157=CARTESIAN_POINT('Ctrl Pts',(56.7624048272067,38.6171840356244,-215.507273405936));
#210158=CARTESIAN_POINT('Ctrl Pts',(56.7620246220546,38.6025455154463,-215.537491003004));
#210159=CARTESIAN_POINT('Ctrl Pts',(56.7607704964948,38.5542596302855,-215.637165246309));
#210160=CARTESIAN_POINT('Ctrl Pts',(56.7571502586175,38.5052402567317,-215.735351647595));
#210161=CARTESIAN_POINT('Ctrl Pts',(56.7509534925747,38.4557760674619,-215.832054892088));
#210162=CARTESIAN_POINT('Ctrl Pts',(56.7448960684165,38.4074241411545,-215.926583645525));
#210163=CARTESIAN_POINT('Ctrl Pts',(56.7363766210372,38.3586472645085,-216.019695331112));
#210164=CARTESIAN_POINT('Ctrl Pts',(56.7252464812199,38.3097021723518,-216.11138771604));
#210165=CARTESIAN_POINT('Ctrl Pts',(56.7214037584742,38.2928036947039,-216.143044857724));
#210166=CARTESIAN_POINT('Ctrl Pts',(56.7172502712356,38.2758850458335,-216.174532750333));
#210167=CARTESIAN_POINT('Ctrl Pts',(56.7127812850717,38.2589564044561,-216.205851068199));
#210168=CARTESIAN_POINT('Ctrl Pts',(56.8784089882814,37.8494074227593,-215.942195856527));
#210169=CARTESIAN_POINT('Ctrl Pts',(56.8923194163109,37.9131111636755,-215.85684824432));
#210170=CARTESIAN_POINT('Ctrl Pts',(56.9035288072913,37.9808416687619,-215.765163207208));
#210171=CARTESIAN_POINT('Ctrl Pts',(56.914779818816,38.0871684291001,-215.617449341681));
#210172=CARTESIAN_POINT('Ctrl Pts',(56.9190114191349,38.1415114743169,-215.541048698008));
#210173=CARTESIAN_POINT('Ctrl Pts',(56.9212013859612,38.2067058130031,-215.447397971083));
#210174=CARTESIAN_POINT('Ctrl Pts',(56.9215690259601,38.2397154101224,-215.399438830714));
#210175=CARTESIAN_POINT('Ctrl Pts',(56.9215656600791,38.257504698105,-215.373442266851));
#210176=CARTESIAN_POINT('Ctrl Pts',(56.9215088034732,38.265834430532,-215.361227686592));
#210177=CARTESIAN_POINT('Ctrl Pts',(56.9214626351149,38.2706010257896,-215.354227629012));
#210178=CARTESIAN_POINT('Ctrl Pts',(56.9214422193595,38.272460437043,-215.351495124754));
#210179=CARTESIAN_POINT('Ctrl Pts',(56.9210462352772,38.3066224801052,-215.301276190226));
#210180=CARTESIAN_POINT('Ctrl Pts',(56.9193511735892,38.3575254740986,-215.226640355385));
#210181=CARTESIAN_POINT('Ctrl Pts',(56.910501986457,38.4560022236843,-215.074830340481));
#210182=CARTESIAN_POINT('Ctrl Pts',(56.9064692885258,38.4924866873854,-215.017574749515));
#210183=CARTESIAN_POINT('Ctrl Pts',(56.897957870777,38.5519627451836,-214.921443048506));
#210184=CARTESIAN_POINT('Ctrl Pts',(56.8930834404498,38.5828852244691,-214.870815628649));
#210185=CARTESIAN_POINT('Ctrl Pts',(56.8860976844991,38.6208417602848,-214.807219480818));
#210186=CARTESIAN_POINT('Ctrl Pts',(56.8828002197628,38.6374891685479,-214.77898909186));
#210187=CARTESIAN_POINT('Ctrl Pts',(56.8805315935286,38.6486693924329,-214.759951795426));
#210188=CARTESIAN_POINT('Ctrl Pts',(56.8792297676071,38.6549228173467,-214.74925617217));
#210189=CARTESIAN_POINT('Ctrl Pts',(56.8609765545196,38.7407461211646,-214.601910135731));
#210190=CARTESIAN_POINT('Ctrl Pts',(56.8422826729904,38.806650416647,-214.478282783532));
#210191=CARTESIAN_POINT('Ctrl Pts',(56.816389824676,38.8870611879215,-214.317263299172));
#210192=CARTESIAN_POINT('Ctrl Pts',(56.8081057773634,38.9107819956799,-214.267642766951));
#210193=CARTESIAN_POINT('Ctrl Pts',(56.7966451030072,38.9421347884435,-214.199397507333));
#210194=CARTESIAN_POINT('Ctrl Pts',(56.7911549400794,38.956753098342,-214.166820249596));
#210195=CARTESIAN_POINT('Ctrl Pts',(56.7852548655275,38.9720320741206,-214.131532088428));
#210196=CARTESIAN_POINT('Ctrl Pts',(56.7824407647108,38.9792363102246,-214.114568907703));
#210197=CARTESIAN_POINT('Ctrl Pts',(56.7812648629523,38.9822314816374,-214.107445005404));
#210198=CARTESIAN_POINT('Ctrl Pts',(56.78048773646,38.9842078373838,-214.10272820146));
#210199=CARTESIAN_POINT('Ctrl Pts',(56.7804066536062,38.9844148179716,-214.102238950507));
#210200=CARTESIAN_POINT('Ctrl Pts',(56.7358311456287,39.0974359385773,-213.830613670394));
#210201=CARTESIAN_POINT('Ctrl Pts',(56.7051832112126,39.1534726566657,-213.596834029539));
#210202=CARTESIAN_POINT('Ctrl Pts',(56.6994898617306,39.1647669078403,-213.398999669105));
#210203=CARTESIAN_POINT('Ctrl Pts',(52.2149235689092,43.779022542486,-208.210085312216));
#210204=CARTESIAN_POINT('Ctrl Pts',(52.2148720050705,43.7789665035542,-208.214448081539));
#210205=CARTESIAN_POINT('Ctrl Pts',(52.2148720050704,43.7789665035542,-208.218811515435));
#210206=CARTESIAN_POINT('Ctrl Pts',(52.2043847769924,43.7887196915372,-208.210087338187));
#210207=CARTESIAN_POINT('Ctrl Pts',(52.2056250202409,43.7874750042174,-208.214450107462));
#210208=CARTESIAN_POINT('Ctrl Pts',(52.2069166839655,43.7862865377113,-208.21881354139));
#210209=CARTESIAN_POINT('Ctrl Pts',(52.195333723769,43.7968389605576,-208.218672616477));
#210210=CARTESIAN_POINT('Ctrl Pts',(52.1976712649932,43.7945859134348,-208.223035434656));
#210211=CARTESIAN_POINT('Ctrl Pts',(52.2000848734438,43.7924159898367,-208.227398819688));
#210212=CARTESIAN_POINT('Ctrl Pts',(52.1808472399183,43.8096868118422,-208.238463951946));
#210213=CARTESIAN_POINT('Ctrl Pts',(52.1849330344943,43.8058281558383,-208.242826402981));
#210214=CARTESIAN_POINT('Ctrl Pts',(52.1891506941446,43.8021155648562,-208.247190155172));
#210215=CARTESIAN_POINT('Ctrl Pts',(52.1749286143212,43.8148481482676,-208.250157029773));
#210216=CARTESIAN_POINT('Ctrl Pts',(52.1797237791601,43.8103385591305,-208.254519356384));
#210217=CARTESIAN_POINT('Ctrl Pts',(52.1846836299068,43.8060124062017,-208.258883232989));
#210218=CARTESIAN_POINT('Ctrl Pts',(52.1591833603872,43.828467493664,-208.285836176959));
#210219=CARTESIAN_POINT('Ctrl Pts',(52.1658591933782,43.8222328676652,-208.290198743649));
#210220=CARTESIAN_POINT('Ctrl Pts',(52.1728001724479,43.8162953562062,-208.294562380182));
#210221=CARTESIAN_POINT('Ctrl Pts',(52.1510964156406,43.8352931366209,-208.311120909483));
#210222=CARTESIAN_POINT('Ctrl Pts',(52.1587292093287,43.8281818395797,-208.315483211337));
#210223=CARTESIAN_POINT('Ctrl Pts',(52.1666971009815,43.8214493653102,-208.3198471127));
#210224=CARTESIAN_POINT('Ctrl Pts',(52.1289643871997,43.8537790486242,-208.388298939608));
#210225=CARTESIAN_POINT('Ctrl Pts',(52.1392045981911,43.8442802812313,-208.392664031458));
#210226=CARTESIAN_POINT('Ctrl Pts',(52.1499948920096,43.8354085050508,-208.397025142829));
#210227=CARTESIAN_POINT('Ctrl Pts',(52.1174992362576,43.8630330920583,-208.441520592514));
#210228=CARTESIAN_POINT('Ctrl Pts',(52.1290740876191,43.852314411835,-208.445885091517));
#210229=CARTESIAN_POINT('Ctrl Pts',(52.141343336723,43.8423973674724,-208.450246795732));
#210230=CARTESIAN_POINT('Ctrl Pts',(52.0863347270061,43.8878226116337,-208.601175288826));
#210231=CARTESIAN_POINT('Ctrl Pts',(52.1015151102266,43.8738103589885,-208.605554907233));
#210232=CARTESIAN_POINT('Ctrl Pts',(52.1178275724807,43.8611200325978,-208.609901492046));
#210233=CARTESIAN_POINT('Ctrl Pts',(52.0701168476483,43.9001220002185,-208.708951634353));
#210234=CARTESIAN_POINT('Ctrl Pts',(52.0871460895594,43.884425032588,-208.713330067135));
#210235=CARTESIAN_POINT('Ctrl Pts',(52.1055914799472,43.8704111305645,-208.717677837571));
#210236=CARTESIAN_POINT('Ctrl Pts',(52.0255864626054,43.9331969723227,-209.0334926008));
#210237=CARTESIAN_POINT('Ctrl Pts',(52.0476481597434,43.9129173610403,-209.037939859074));
#210238=CARTESIAN_POINT('Ctrl Pts',(52.071995743712,43.8953985191085,-209.042218804019));
#210239=CARTESIAN_POINT('Ctrl Pts',(52.0021445297993,43.949466653783,-209.251266491716));
#210240=CARTESIAN_POINT('Ctrl Pts',(52.0268103251713,43.9268242456044,-209.255711234979));
#210241=CARTESIAN_POINT('Ctrl Pts',(52.0543127614129,43.9076935513658,-209.259992694935));
#210242=CARTESIAN_POINT('Ctrl Pts',(51.937720029348,43.9928431481926,-209.90473928415));
#210243=CARTESIAN_POINT('Ctrl Pts',(51.9694532568106,43.9637905045621,-209.909476451697));
#210244=CARTESIAN_POINT('Ctrl Pts',(52.0057184578615,43.940477854794,-209.913465487369));
#210245=CARTESIAN_POINT('Ctrl Pts',(51.9034482509577,44.0137474304281,-210.34162185738));
#210246=CARTESIAN_POINT('Ctrl Pts',(51.9388750336111,43.9813630646936,-210.346355470779));
#210247=CARTESIAN_POINT('Ctrl Pts',(51.9798728970522,43.9562851731636,-210.350348060599));
#210248=CARTESIAN_POINT('Ctrl Pts',(51.8088683580654,44.0688586918087,-211.653440509504));
#210249=CARTESIAN_POINT('Ctrl Pts',(51.8543012271538,44.0274385666118,-211.659386088869));
#210250=CARTESIAN_POINT('Ctrl Pts',(51.9085528218201,43.9979691256788,-211.662166712722));
#210251=CARTESIAN_POINT('Ctrl Pts',(51.7580215322863,44.0943375071556,-212.529490943221));
#210252=CARTESIAN_POINT('Ctrl Pts',(51.8087639397327,44.0481656078252,-212.535446734955));
#210253=CARTESIAN_POINT('Ctrl Pts',(51.870219684202,44.0172576131423,-212.538231376868));
#210254=CARTESIAN_POINT('Ctrl Pts',(51.7111509881033,44.1161634878026,-213.405556127478));
#210255=CARTESIAN_POINT('Ctrl Pts',(51.7668122505506,44.0656404359961,-213.409820292477));
#210256=CARTESIAN_POINT('Ctrl Pts',(51.8348891643276,44.0337882456516,-213.414282330697));
#210257=CARTESIAN_POINT('',(51.8348891643276,44.0337882456516,-213.414282330697));
#210258=CARTESIAN_POINT('',(51.7111509810702,44.1161634800382,-213.405556127296));
#210259=CARTESIAN_POINT('Origin',(52.0467850062684,44.4866680886213,-213.414282330697));
#210260=CARTESIAN_POINT('Ctrl Pts',(52.2149235689092,43.779022542486,-208.210085312216));
#210261=CARTESIAN_POINT('Ctrl Pts',(52.2043801934833,43.7887239088728,-208.210087344463));
#210262=CARTESIAN_POINT('Ctrl Pts',(52.1953274288659,43.796844542981,-208.218681234754));
#210263=CARTESIAN_POINT('Ctrl Pts',(52.1880904910527,43.8032628774376,-208.228568296719));
#210264=CARTESIAN_POINT('Ctrl Pts',(52.1808394389761,43.8096937296283,-208.238474641509));
#210265=CARTESIAN_POINT('Ctrl Pts',(52.1749242234792,43.8148519452172,-208.250167023561));
#210266=CARTESIAN_POINT('Ctrl Pts',(52.1696802065441,43.8193879205004,-208.262050087041));
#210267=CARTESIAN_POINT('Ctrl Pts',(52.1591795680454,43.8284707738317,-208.28584477638));
#210268=CARTESIAN_POINT('Ctrl Pts',(52.1510932946611,43.8352957489707,-208.311131552955));
#210269=CARTESIAN_POINT('Ctrl Pts',(52.1437197227052,43.8414545028842,-208.336847252802));
#210270=CARTESIAN_POINT('Ctrl Pts',(52.1289623042575,43.8537805924866,-208.38831448545));
#210271=CARTESIAN_POINT('Ctrl Pts',(52.117497806034,43.8630342337481,-208.441527742187));
#210272=CARTESIAN_POINT('Ctrl Pts',(52.1071115904079,43.871295780733,-208.494739003265));
#210273=CARTESIAN_POINT('Ctrl Pts',(52.0863339472228,43.8878230204506,-208.601188227497));
#210274=CARTESIAN_POINT('Ctrl Pts',(52.0701156440688,43.9001228988017,-208.708960203697));
#210275=CARTESIAN_POINT('Ctrl Pts',(52.0552737632954,43.9111466435138,-208.817132044246));
#210276=CARTESIAN_POINT('Ctrl Pts',(52.0255859242023,43.9331971615186,-209.033505443658));
#210277=CARTESIAN_POINT('Ctrl Pts',(52.0021438786448,43.9494670967064,-209.251272899507));
#210278=CARTESIAN_POINT('Ctrl Pts',(51.980669942658,43.9639252593981,-209.469090795394));
#210279=CARTESIAN_POINT('Ctrl Pts',(51.9377196179987,43.9928432361475,-209.904751465645));
#210280=CARTESIAN_POINT('Ctrl Pts',(51.9034476265843,44.0137477974947,-210.34163037533));
#210281=CARTESIAN_POINT('Ctrl Pts',(51.8719217450993,44.032117736709,-210.778894755328));
#210282=CARTESIAN_POINT('Ctrl Pts',(51.8088678222893,44.0688588736632,-211.653453472328));
#210283=CARTESIAN_POINT('Ctrl Pts',(51.7580264403492,44.0943352215171,-212.529399211082));
#210284=CARTESIAN_POINT('Ctrl Pts',(51.7111509881036,44.1161634878024,-213.405556127478));
#210285=CARTESIAN_POINT('Ctrl Pts',(51.8348891643276,44.0337882456516,-213.414282330697));
#210286=CARTESIAN_POINT('Ctrl Pts',(51.8440852954194,44.0294855106755,-213.18625626589));
#210287=CARTESIAN_POINT('Ctrl Pts',(51.8531604919734,44.0251462166332,-212.96630637642));
#210288=CARTESIAN_POINT('Ctrl Pts',(51.8621671183822,44.0207245304424,-212.754324487476));
#210289=CARTESIAN_POINT('Ctrl Pts',(51.871945121168,44.0159241470436,-212.524187318841));
#210290=CARTESIAN_POINT('Ctrl Pts',(51.8816421638536,44.0110267854007,-212.303441420756));
#210291=CARTESIAN_POINT('Ctrl Pts',(51.8912802016416,44.0060153259421,-212.091936017557));
#210292=CARTESIAN_POINT('Ctrl Pts',(51.9015055904708,44.0006984634549,-211.867541277181));
#210293=CARTESIAN_POINT('Ctrl Pts',(51.9116640949647,43.9952536058705,-211.653547491765));
#210294=CARTESIAN_POINT('Ctrl Pts',(51.9217383966445,43.9897004291075,-211.449762344375));
#210295=CARTESIAN_POINT('Ctrl Pts',(51.933310516654,43.9833216219229,-211.215679004733));
#210296=CARTESIAN_POINT('Ctrl Pts',(51.9447712866266,43.976800121988,-210.995065528174));
#210297=CARTESIAN_POINT('Ctrl Pts',(51.9560438134912,43.9702123981561,-210.787615525048));
#210298=CARTESIAN_POINT('Ctrl Pts',(51.9630659686827,43.9661086138261,-210.658385749514));
#210299=CARTESIAN_POINT('Ctrl Pts',(51.9699973687366,43.9619953951688,-210.534265420326));
#210300=CARTESIAN_POINT('Ctrl Pts',(51.9768916294888,43.9578245559274,-210.415191219797));
#210301=CARTESIAN_POINT('Ctrl Pts',(51.9840937110015,43.953467493543,-210.290800494079));
#210302=CARTESIAN_POINT('Ctrl Pts',(51.9912547789145,43.9490479969219,-210.171916472859));
#210303=CARTESIAN_POINT('Ctrl Pts',(51.9983902835959,43.944553289385,-210.058458378852));
#210304=CARTESIAN_POINT('Ctrl Pts',(52.0063183623385,43.9395593335446,-209.932397960781));
#210305=CARTESIAN_POINT('Ctrl Pts',(52.0142146268005,43.9344727678281,-209.81303573055));
#210306=CARTESIAN_POINT('Ctrl Pts',(52.0220505221564,43.9293219842294,-209.700251538583));
#210307=CARTESIAN_POINT('Ctrl Pts',(52.0274154131935,43.9257954704734,-209.6230331898));
#210308=CARTESIAN_POINT('Ctrl Pts',(52.0327509345153,43.9222398433349,-209.548898118242));
#210309=CARTESIAN_POINT('Ctrl Pts',(52.0380379633556,43.9186734067761,-209.477805892547));
#210310=CARTESIAN_POINT('Ctrl Pts',(52.0431331684242,43.9152363675277,-209.40929303218));
#210311=CARTESIAN_POINT('Ctrl Pts',(52.0481711845886,43.9118009093687,-209.343582163061));
#210312=CARTESIAN_POINT('Ctrl Pts',(52.053197688286,43.9083249915534,-209.280672317176));
#210313=CARTESIAN_POINT('Ctrl Pts',(52.0584989082176,43.9046591025156,-209.214324225347));
#210314=CARTESIAN_POINT('Ctrl Pts',(52.0637869189831,43.9009485849322,-209.151091534621));
#210315=CARTESIAN_POINT('Ctrl Pts',(52.0690726236707,43.8971837489602,-209.090953530795));
#210316=CARTESIAN_POINT('Ctrl Pts',(52.0749226987908,43.8930169302381,-209.024394413184));
#210317=CARTESIAN_POINT('Ctrl Pts',(52.080769641772,43.8887838588144,-208.96162602192));
#210318=CARTESIAN_POINT('Ctrl Pts',(52.0865826447208,43.8845137395771,-208.902598818566));
#210319=CARTESIAN_POINT('Ctrl Pts',(52.0891752874545,43.8826092345029,-208.876272244984));
#210320=CARTESIAN_POINT('Ctrl Pts',(52.0917606452554,43.8806978553632,-208.850689622922));
#210321=CARTESIAN_POINT('Ctrl Pts',(52.0943337930903,43.8787842296859,-208.825845487606));
#210322=CARTESIAN_POINT('Ctrl Pts',(52.0981470647389,43.8759483356722,-208.789027767476));
#210323=CARTESIAN_POINT('Ctrl Pts',(52.1019204343215,43.8731194191416,-208.753839003036));
#210324=CARTESIAN_POINT('Ctrl Pts',(52.1056979659228,43.8702568909374,-208.720280928359));
#210325=CARTESIAN_POINT('Ctrl Pts',(52.1096891458759,43.8672324648333,-208.684824887469));
#210326=CARTESIAN_POINT('Ctrl Pts',(52.1136845529443,43.8641709060281,-208.651189045429));
#210327=CARTESIAN_POINT('Ctrl Pts',(52.1176934819693,43.8610639150675,-208.619358840089));
#210328=CARTESIAN_POINT('Ctrl Pts',(52.1221209898717,43.8576325180672,-208.584205190623));
#210329=CARTESIAN_POINT('Ctrl Pts',(52.1265646218548,43.8541460483929,-208.551253778001));
#210330=CARTESIAN_POINT('Ctrl Pts',(52.1309922302586,43.8506347478063,-208.520467603443));
#210331=CARTESIAN_POINT('Ctrl Pts',(52.1318186983157,43.849979319975,-208.514720981893));
#210332=CARTESIAN_POINT('Ctrl Pts',(52.1326445047111,43.8493231228087,-208.509049763197));
#210333=CARTESIAN_POINT('Ctrl Pts',(52.1334693091333,43.8486664746894,-208.50345365565));
#210334=CARTESIAN_POINT('Ctrl Pts',(52.1362477509627,43.8464544853346,-208.484602569417));
#210335=CARTESIAN_POINT('Ctrl Pts',(52.1390115559275,43.8442411033876,-208.466564424385));
#210336=CARTESIAN_POINT('Ctrl Pts',(52.141792873597,43.8419957546331,-208.449393395525));
#210337=CARTESIAN_POINT('Ctrl Pts',(52.1447241951854,43.8396293082002,-208.431296287042));
#210338=CARTESIAN_POINT('Ctrl Pts',(52.1476746346871,43.8372276679482,-208.414162016015));
#210339=CARTESIAN_POINT('Ctrl Pts',(52.1506486851097,43.834786239038,-208.398015691187));
#210340=CARTESIAN_POINT('Ctrl Pts',(52.1539039947587,43.8321139215049,-208.380342390623));
#210341=CARTESIAN_POINT('Ctrl Pts',(52.1571872713604,43.82939423425,-208.36385244999));
#210342=CARTESIAN_POINT('Ctrl Pts',(52.1604707470427,43.8266528564292,-208.34853874569));
#210343=CARTESIAN_POINT('Ctrl Pts',(52.1606844005896,43.8264744768242,-208.347542293285));
#210344=CARTESIAN_POINT('Ctrl Pts',(52.1608980453075,43.8262960144973,-208.346550809251));
#210345=CARTESIAN_POINT('Ctrl Pts',(52.1611116697293,43.8261174801212,-208.345564286924));
#210346=CARTESIAN_POINT('Ctrl Pts',(52.1632956867302,43.8242922107564,-208.33547844787));
#210347=CARTESIAN_POINT('Ctrl Pts',(52.1654674542167,43.822468685508,-208.325913484142));
#210348=CARTESIAN_POINT('Ctrl Pts',(52.1676645419426,43.8206118261382,-208.316897375615));
#210349=CARTESIAN_POINT('Ctrl Pts',(52.1700759527451,43.8185738325294,-208.30700175732));
#210350=CARTESIAN_POINT('Ctrl Pts',(52.1725176882122,43.8164958491871,-208.297767152186));
#210351=CARTESIAN_POINT('Ctrl Pts',(52.1749977315457,43.8143704840783,-208.289196225522));
#210352=CARTESIAN_POINT('Ctrl Pts',(52.1768850775668,43.812753052912,-208.28267363613));
#210353=CARTESIAN_POINT('Ctrl Pts',(52.1787936398816,43.8111090875315,-208.276534612158));
#210354=CARTESIAN_POINT('Ctrl Pts',(52.1807145176352,43.8094469441326,-208.270770100534));
#210355=CARTESIAN_POINT('Ctrl Pts',(52.1823557293411,43.8080267969119,-208.26584486053));
#210356=CARTESIAN_POINT('Ctrl Pts',(52.1840153685614,43.8065851661576,-208.261166956059));
#210357=CARTESIAN_POINT('Ctrl Pts',(52.1856993914338,43.80511516462,-208.256813689259));
#210358=CARTESIAN_POINT('Ctrl Pts',(52.187522563892,43.8035236979238,-208.252100715187));
#210359=CARTESIAN_POINT('Ctrl Pts',(52.1893742116152,43.8018990789262,-208.247767994534));
#210360=CARTESIAN_POINT('Ctrl Pts',(52.1912458864848,43.8002483732425,-208.243854523133));
#210361=CARTESIAN_POINT('Ctrl Pts',(52.1923633055812,43.7992628761973,-208.241518119654));
#210362=CARTESIAN_POINT('Ctrl Pts',(52.1934875690653,43.798268371482,-208.239330052569));
#210363=CARTESIAN_POINT('Ctrl Pts',(52.1946147722137,43.7972684489249,-208.237290523636));
#210364=CARTESIAN_POINT('Ctrl Pts',(52.1960055218434,43.7960347388096,-208.234774141286));
#210365=CARTESIAN_POINT('Ctrl Pts',(52.1974238413554,43.7947720316984,-208.23245629745));
#210366=CARTESIAN_POINT('Ctrl Pts',(52.1988449817247,43.7935018380268,-208.230406082707));
#210367=CARTESIAN_POINT('Ctrl Pts',(52.200408453943,43.7921044303109,-208.228150532263));
#210368=CARTESIAN_POINT('Ctrl Pts',(52.2019753026815,43.7906979991141,-208.226218733228));
#210369=CARTESIAN_POINT('Ctrl Pts',(52.2035177395458,43.7893076301571,-208.22463719045));
#210370=CARTESIAN_POINT('Ctrl Pts',(52.2051740594693,43.7878146058021,-208.222938877298));
#210371=CARTESIAN_POINT('Ctrl Pts',(52.2068022133339,43.7863401325541,-208.221643660656));
#210372=CARTESIAN_POINT('Ctrl Pts',(52.2083738943961,43.7849108267,-208.220720401459));
#210373=CARTESIAN_POINT('Ctrl Pts',(52.2102017346834,43.7832485665343,-208.219646665573));
#210374=CARTESIAN_POINT('Ctrl Pts',(52.2119530649539,43.7816475301323,-208.219075197685));
#210375=CARTESIAN_POINT('Ctrl Pts',(52.2135926537553,43.7801423382395,-208.218885518605));
#210376=CARTESIAN_POINT('Ctrl Pts',(52.2140270829265,43.7797435191783,-208.218835260806));
#210377=CARTESIAN_POINT('Ctrl Pts',(52.2144537171266,43.7793513883371,-208.218811515434));
#210378=CARTESIAN_POINT('Ctrl Pts',(52.2148720050704,43.7789665035542,-208.218811515434));
#210379=CARTESIAN_POINT('Ctrl Pts',(56.7089132278424,37.0787382657864,-216.762440352386));
#210380=CARTESIAN_POINT('Ctrl Pts',(56.4432500919345,37.2379648996087,-216.862162585544));
#210381=CARTESIAN_POINT('Ctrl Pts',(56.4975419847624,37.4436240691992,-217.108396707512));
#210382=CARTESIAN_POINT('Ctrl Pts',(56.7718148744283,37.3652096903236,-216.516505964954));
#210383=CARTESIAN_POINT('Ctrl Pts',(56.5198175013863,37.5280043332472,-216.615579405895));
#210384=CARTESIAN_POINT('Ctrl Pts',(56.5775101129868,37.7465455181985,-216.837759178115));
#210385=CARTESIAN_POINT('Ctrl Pts',(56.8285940470758,37.6233003639439,-216.244019387511));
#210386=CARTESIAN_POINT('Ctrl Pts',(56.5898249632591,37.7931945066467,-216.337771859736));
#210387=CARTESIAN_POINT('Ctrl Pts',(56.6495991956979,38.0196209280746,-216.537932548464));
#210388=CARTESIAN_POINT('Ctrl Pts',(56.8784089512595,37.8494072532151,-215.942196083675));
#210389=CARTESIAN_POINT('Ctrl Pts',(56.6513917750255,38.0264112674188,-216.026572725176));
#210390=CARTESIAN_POINT('Ctrl Pts',(56.7127812850717,38.2589564044561,-216.205851068199));
#210391=CARTESIAN_POINT('',(56.7089758625812,37.0787996208419,-216.761769944484));
#210392=CARTESIAN_POINT('',(56.4975419847624,37.4436240691992,-217.108396707512));
#210393=CARTESIAN_POINT('Origin',(56.9809801438088,37.3160013973188,-217.108396707512));
#210394=CARTESIAN_POINT('Ctrl Pts',(56.7127812850717,38.2589564044561,-216.205851068199));
#210395=CARTESIAN_POINT('Ctrl Pts',(56.675820350007,38.1189473751743,-216.400115647765));
#210396=CARTESIAN_POINT('Ctrl Pts',(56.6358255784857,37.9674460907173,-216.583274967065));
#210397=CARTESIAN_POINT('Ctrl Pts',(56.5929883959844,37.8051776760066,-216.756029715358));
#210398=CARTESIAN_POINT('Ctrl Pts',(56.5625833082106,37.6900023749221,-216.878648033801));
#210399=CARTESIAN_POINT('Ctrl Pts',(56.5307460013724,37.5694017889912,-216.996023775216));
#210400=CARTESIAN_POINT('Ctrl Pts',(56.4975419847624,37.4436240691992,-217.108396707512));
#210401=CARTESIAN_POINT('Ctrl Pts',(56.7089871854281,37.0788107123531,-216.761648750938));
#210402=CARTESIAN_POINT('Ctrl Pts',(56.708661470963,37.0793030031369,-216.761567481551));
#210403=CARTESIAN_POINT('Ctrl Pts',(56.7091315247285,37.0828254646993,-216.758788759137));
#210404=CARTESIAN_POINT('Ctrl Pts',(56.7103842705187,37.0893682154781,-216.753291228247));
#210405=CARTESIAN_POINT('Ctrl Pts',(56.7116344616361,37.0958976238959,-216.747804908245));
#210406=CARTESIAN_POINT('Ctrl Pts',(56.7136642224785,37.1054350836466,-216.739610788918));
#210407=CARTESIAN_POINT('Ctrl Pts',(56.7164352191511,37.1179511891652,-216.728646837421));
#210408=CARTESIAN_POINT('Ctrl Pts',(56.7174682169894,37.1226170590566,-216.724559593901));
#210409=CARTESIAN_POINT('Ctrl Pts',(56.7186039669403,37.1276966754221,-216.720087019819));
#210410=CARTESIAN_POINT('Ctrl Pts',(56.7198395388826,37.1331877755253,-216.715224484388));
#210411=CARTESIAN_POINT('Ctrl Pts',(56.7231360303223,37.14783796615,-216.702251296932));
#210412=CARTESIAN_POINT('Ctrl Pts',(56.7271451237326,37.1654188113094,-216.686504936086));
#210413=CARTESIAN_POINT('Ctrl Pts',(56.7317921133979,37.1858721625638,-216.667871599096));
#210414=CARTESIAN_POINT('Ctrl Pts',(56.7326930081959,37.1898373785583,-216.664259222574));
#210415=CARTESIAN_POINT('Ctrl Pts',(56.7336177907719,37.1939104852922,-216.660538231029));
#210416=CARTESIAN_POINT('Ctrl Pts',(56.7345657887601,37.1980909556426,-216.656707638063));
#210417=CARTESIAN_POINT('Ctrl Pts',(56.737484766271,37.2109630282513,-216.644912871764));
#210418=CARTESIAN_POINT('Ctrl Pts',(56.7406241476852,37.2248532466774,-216.6320793121));
#210419=CARTESIAN_POINT('Ctrl Pts',(56.7439616646172,37.2397440600632,-216.618175276465));
#210420=CARTESIAN_POINT('Ctrl Pts',(56.7456304230831,37.2471894667561,-216.611223258648));
#210421=CARTESIAN_POINT('Ctrl Pts',(56.7473486557363,37.2548849699725,-216.604003551846));
#210422=CARTESIAN_POINT('Ctrl Pts',(56.749113183206,37.2628280516737,-216.596511808696));
#210423=CARTESIAN_POINT('Ctrl Pts',(56.7499954469408,37.2667995925243,-216.592765937121));
#210424=CARTESIAN_POINT('Ctrl Pts',(56.7508892806168,37.2708330247062,-216.588952051994));
#210425=CARTESIAN_POINT('Ctrl Pts',(56.7517942616762,37.2749280118441,-216.585069586494));
#210426=CARTESIAN_POINT('Ctrl Pts',(56.7522467522059,37.2769755054131,-216.583128353743));
#210427=CARTESIAN_POINT('Ctrl Pts',(56.7527020293418,37.2790383875113,-216.581169975623));
#210428=CARTESIAN_POINT('Ctrl Pts',(56.7531600386458,37.2811166147432,-216.579194379838));
#210429=CARTESIAN_POINT('Ctrl Pts',(56.7536180479497,37.2831948419751,-216.577218784053));
#210430=CARTESIAN_POINT('Ctrl Pts',(56.7543059888436,37.286322328817,-216.574240479364));
#210431=CARTESIAN_POINT('Ctrl Pts',(56.7545422075944,37.2873972875617,-216.573215866174));
#210432=CARTESIAN_POINT('Ctrl Pts',(56.7621012076203,37.3217959673925,-216.540428244085));
#210433=CARTESIAN_POINT('Ctrl Pts',(56.7695178549811,37.355535319443,-216.507387750391));
#210434=CARTESIAN_POINT('Ctrl Pts',(56.7767905876617,37.3886103535824,-216.474120942766));
#210435=CARTESIAN_POINT('Ctrl Pts',(56.7809009568357,37.4073035472863,-216.455319363418));
#210436=CARTESIAN_POINT('Ctrl Pts',(56.7848762867467,37.4253986755092,-216.436844242353));
#210437=CARTESIAN_POINT('Ctrl Pts',(56.78886986911,37.4435511814868,-216.418027355469));
#210438=CARTESIAN_POINT('Ctrl Pts',(56.7919423812352,37.4575170371138,-216.40355035015));
#210439=CARTESIAN_POINT('Ctrl Pts',(56.795025195344,37.4715164619458,-216.388870306284));
#210440=CARTESIAN_POINT('Ctrl Pts',(56.7981765486193,37.4858386382505,-216.373668133342));
#210441=CARTESIAN_POINT('Ctrl Pts',(56.8159359101986,37.5665508546774,-216.287996720946));
#210442=CARTESIAN_POINT('Ctrl Pts',(56.832854077496,37.6433264560983,-216.200613606556));
#210443=CARTESIAN_POINT('Ctrl Pts',(56.8488877595288,37.7160793736129,-216.111889150275));
#210444=CARTESIAN_POINT('Ctrl Pts',(56.8590267960587,37.7620853058016,-216.055783478384));
#210445=CARTESIAN_POINT('Ctrl Pts',(56.8688128764962,37.8064834155413,-215.999141637438));
#210446=CARTESIAN_POINT('Ctrl Pts',(56.8782424684847,37.8492596800295,-215.942057996927));
#210447=CARTESIAN_POINT('Ctrl Pts',(50.6668571239968,44.0777189530043,-216.468046015339));
#210448=CARTESIAN_POINT('Ctrl Pts',(50.4202954871045,43.9828326938916,-216.258996421318));
#210449=CARTESIAN_POINT('Ctrl Pts',(50.2169391861068,44.2398739469141,-216.179548839231));
#210450=CARTESIAN_POINT('Ctrl Pts',(50.9477024065591,44.1832652290949,-215.960963622776));
#210451=CARTESIAN_POINT('Ctrl Pts',(50.702607269904,44.1457324009489,-215.837685287199));
#210452=CARTESIAN_POINT('Ctrl Pts',(50.5697429859293,44.3569399972268,-215.718609917522));
#210453=CARTESIAN_POINT('Ctrl Pts',(51.2153988083273,44.192734708103,-215.442665058708));
#210454=CARTESIAN_POINT('Ctrl Pts',(51.0255093994164,44.2008217405635,-215.345450727964));
#210455=CARTESIAN_POINT('Ctrl Pts',(50.9110336349312,44.3534119066666,-215.247525543514));
#210456=CARTESIAN_POINT('Ctrl Pts',(51.5381992078581,44.1395055735188,-214.660447877432));
#210457=CARTESIAN_POINT('Ctrl Pts',(51.4124712437483,44.1693327463343,-214.59669191525));
#210458=CARTESIAN_POINT('Ctrl Pts',(51.3258123082479,44.2676079799153,-214.537190176925));
#210459=CARTESIAN_POINT('Ctrl Pts',(51.6264957021156,44.1149795137312,-214.423951342294));
#210460=CARTESIAN_POINT('Ctrl Pts',(51.5180263342635,44.1477293653001,-214.371802696835));
#210461=CARTESIAN_POINT('Ctrl Pts',(51.4398111504988,44.2315500222654,-214.322416627157));
#210462=CARTESIAN_POINT('Ctrl Pts',(51.7972884149161,44.0548047396562,-213.839739291795));
#210463=CARTESIAN_POINT('Ctrl Pts',(51.7203476126764,44.089286352992,-213.818433091759));
#210464=CARTESIAN_POINT('Ctrl Pts',(51.6610101464785,44.1457350486596,-213.79183067467));
#210465=CARTESIAN_POINT('Ctrl Pts',(51.8659565316503,44.0178105340169,-213.478656833619));
#210466=CARTESIAN_POINT('Ctrl Pts',(51.8035205704321,44.0485969165887,-213.470699334602));
#210467=CARTESIAN_POINT('Ctrl Pts',(51.7505801429124,44.0950938200302,-213.464005878851));
#210468=CARTESIAN_POINT('Ctrl Pts',(51.8248396661196,44.0390948051906,-213.083798271317));
#210469=CARTESIAN_POINT('Ctrl Pts',(51.753836136243,44.0717738930276,-213.094488712702));
#210470=CARTESIAN_POINT('Ctrl Pts',(51.6968104056281,44.1244887290081,-213.105265698142));
#210471=CARTESIAN_POINT('',(50.8056178277775,44.122591905242,-216.213154850206));
#210472=CARTESIAN_POINT('',(50.3946587200443,44.285292057478,-215.949493832057));
#210473=CARTESIAN_POINT('Origin',(50.6744232242015,44.605072968075,-216.213154850206));
#210474=CARTESIAN_POINT('Ctrl Pts',(51.7111509881036,44.1161634878024,-213.405556127478));
#210475=CARTESIAN_POINT('Ctrl Pts',(51.7054714071276,44.1189759500224,-213.50459109405));
#210476=CARTESIAN_POINT('Ctrl Pts',(51.6884734636492,44.1278965425,-213.612607039845));
#210477=CARTESIAN_POINT('Ctrl Pts',(51.6441850919576,44.1484194974503,-213.787927031532));
#210478=CARTESIAN_POINT('Ctrl Pts',(51.6262866883493,44.1564463989509,-213.848578573237));
#210479=CARTESIAN_POINT('Ctrl Pts',(51.5944783226475,44.1699746414804,-213.942800966704));
#210480=CARTESIAN_POINT('Ctrl Pts',(51.5773336536473,44.1771103462579,-213.990722826982));
#210481=CARTESIAN_POINT('Ctrl Pts',(51.5551015148144,44.1860180080322,-214.048027515802));
#210482=CARTESIAN_POINT('Ctrl Pts',(51.5434203512994,44.190608779469,-214.077025395749));
#210483=CARTESIAN_POINT('Ctrl Pts',(51.5382922303731,44.1926046564484,-214.089526718781));
#210484=CARTESIAN_POINT('Ctrl Pts',(51.5348463012418,44.1939414477291,-214.097877258856));
#210485=CARTESIAN_POINT('Ctrl Pts',(51.5323282966788,44.1949141285707,-214.10393220042));
#210486=CARTESIAN_POINT('Ctrl Pts',(51.5003597777846,44.2072352608624,-214.180494287));
#210487=CARTESIAN_POINT('Ctrl Pts',(51.4589236498728,44.2227433939912,-214.271580524568));
#210488=CARTESIAN_POINT('Ctrl Pts',(51.3782047880098,44.2480465259769,-214.432816691758));
#210489=CARTESIAN_POINT('Ctrl Pts',(51.3481932423834,44.2568079154406,-214.490655269819));
#210490=CARTESIAN_POINT('Ctrl Pts',(51.2980611938582,44.2699144304708,-214.583366808615));
#210491=CARTESIAN_POINT('Ctrl Pts',(51.2717155778434,44.2764576509972,-214.631209651118));
#210492=CARTESIAN_POINT('Ctrl Pts',(51.2433573264094,44.2828773330698,-214.68123429109));
#210493=CARTESIAN_POINT('Ctrl Pts',(51.2239937443592,44.2871169811656,-214.7150623647));
#210494=CARTESIAN_POINT('Ctrl Pts',(51.214934183901,44.2890428011384,-214.730756571201));
#210495=CARTESIAN_POINT('Ctrl Pts',(51.1159651889466,44.3092682329707,-214.900388603229));
#210496=CARTESIAN_POINT('Ctrl Pts',(51.0372325599885,44.3187739897739,-215.025889321681));
#210497=CARTESIAN_POINT('Ctrl Pts',(50.9388506155471,44.3269983741609,-215.177851437473));
#210498=CARTESIAN_POINT('Ctrl Pts',(50.9093170633681,44.3287067824773,-215.222470642592));
#210499=CARTESIAN_POINT('Ctrl Pts',(50.870415210797,44.3303090954864,-215.280598871226));
#210500=CARTESIAN_POINT('Ctrl Pts',(50.8523116339892,44.3308676436715,-215.307462753606));
#210501=CARTESIAN_POINT('Ctrl Pts',(50.8336364266536,44.3311973019426,-215.335004734123));
#210502=CARTESIAN_POINT('Ctrl Pts',(50.8249195217816,44.3312925367348,-215.347831789202));
#210503=CARTESIAN_POINT('Ctrl Pts',(50.8213176701548,44.3313195626524,-215.353127434398));
#210504=CARTESIAN_POINT('Ctrl Pts',(50.8189463076488,44.3313346354746,-215.356613116074));
#210505=CARTESIAN_POINT('Ctrl Pts',(50.8189998321179,44.3313357734173,-215.356534797611));
#210506=CARTESIAN_POINT('Ctrl Pts',(50.6642979760868,44.3319582986941,-215.583833929845));
#210507=CARTESIAN_POINT('Ctrl Pts',(50.5215412302473,44.3141675772679,-215.779647760799));
#210508=CARTESIAN_POINT('Ctrl Pts',(50.3946839049651,44.2853208635448,-215.949517779663));
#210509=CARTESIAN_POINT('',(51.1992015578549,44.1752017469644,-215.438515904958));
#210510=CARTESIAN_POINT('Ctrl Pts',(51.1992016446529,44.1751487167426,-215.438515947409));
#210511=CARTESIAN_POINT('Ctrl Pts',(51.281838384943,44.1751487164063,-215.264092918614));
#210512=CARTESIAN_POINT('Ctrl Pts',(51.3570498862049,44.1683672671663,-215.096663697119));
#210513=CARTESIAN_POINT('Ctrl Pts',(51.4578268909383,44.153075442267,-214.856010573837));
#210514=CARTESIAN_POINT('Ctrl Pts',(51.4894281386649,44.1471157811946,-214.777541316661));
#210515=CARTESIAN_POINT('Ctrl Pts',(51.52643960228,44.1390383023429,-214.681640310082));
#210516=CARTESIAN_POINT('Ctrl Pts',(51.5330243552575,44.1375598470366,-214.664428060081));
#210517=CARTESIAN_POINT('Ctrl Pts',(51.5508612596177,44.1333734700322,-214.617109216616));
#210518=CARTESIAN_POINT('Ctrl Pts',(51.5769304234794,44.1269962078744,-214.546969728427));
#210519=CARTESIAN_POINT('Ctrl Pts',(51.600952481436,44.1204320662154,-214.479346571265));
#210520=CARTESIAN_POINT('Ctrl Pts',(51.6463079576364,44.1073102787278,-214.347455364974));
#210521=CARTESIAN_POINT('Ctrl Pts',(51.6729591850628,44.0985806227172,-214.264001371494));
#210522=CARTESIAN_POINT('Ctrl Pts',(51.7077592081449,44.0863610853566,-214.145530597343));
#210523=CARTESIAN_POINT('Ctrl Pts',(51.7184967630461,44.082431327535,-214.107158708638));
#210524=CARTESIAN_POINT('Ctrl Pts',(51.7382817589645,44.0749717043864,-214.032651669918));
#210525=CARTESIAN_POINT('Ctrl Pts',(51.7513941925948,44.06985843768,-213.980342118648));
#210526=CARTESIAN_POINT('Ctrl Pts',(51.8046067014177,44.0483179959303,-213.745999527886));
#210527=CARTESIAN_POINT('Ctrl Pts',(51.8284907824184,44.0367819547839,-213.572935771286));
#210528=CARTESIAN_POINT('Ctrl Pts',(51.8348891643276,44.0337882456516,-213.414282330697));
#210529=CARTESIAN_POINT('Ctrl Pts',(50.8056178277775,44.122591905242,-216.213154850207));
#210530=CARTESIAN_POINT('Ctrl Pts',(50.8518843754316,44.1351725469415,-216.127353743724));
#210531=CARTESIAN_POINT('Ctrl Pts',(50.898240202651,44.1454320264489,-216.039922027355));
#210532=CARTESIAN_POINT('Ctrl Pts',(50.9444825680174,44.1534284763442,-215.950864727423));
#210533=CARTESIAN_POINT('Ctrl Pts',(50.9642454094214,44.1568459609349,-215.912803843633));
#210534=CARTESIAN_POINT('Ctrl Pts',(50.9839873245558,44.1598506393414,-215.874445742745));
#210535=CARTESIAN_POINT('Ctrl Pts',(51.0036914984811,44.1624494574738,-215.835789521075));
#210536=CARTESIAN_POINT('Ctrl Pts',(51.03659613116,44.1667893073132,-215.771236255374));
#210537=CARTESIAN_POINT('Ctrl Pts',(51.0693950134981,44.1699966689994,-215.705853474845));
#210538=CARTESIAN_POINT('Ctrl Pts',(51.1020070264693,44.1721130516932,-215.639641199155));
#210539=CARTESIAN_POINT('Ctrl Pts',(51.1346190394405,44.174229434387,-215.573428923466));
#210540=CARTESIAN_POINT('Ctrl Pts',(51.1670439525282,44.175254960468,-215.506387152935));
#210541=CARTESIAN_POINT('Ctrl Pts',(51.1992014925245,44.1752416613785,-215.438515873006));
#210542=CARTESIAN_POINT('Ctrl Pts',(56.5618180211198,36.5289367340068,-217.254048694966));
#210543=CARTESIAN_POINT('Ctrl Pts',(56.2980271921268,36.6878565975336,-217.354444173088));
#210544=CARTESIAN_POINT('Ctrl Pts',(56.351930605989,36.892044198215,-217.60005));
#210545=CARTESIAN_POINT('Ctrl Pts',(56.6108961448827,36.7123872459292,-217.09039277187));
#210546=CARTESIAN_POINT('Ctrl Pts',(56.3465050213663,36.8714919357672,-217.190493004533));
#210547=CARTESIAN_POINT('Ctrl Pts',(56.4005154364319,37.0760848599628,-217.436382427969));
#210548=CARTESIAN_POINT('Ctrl Pts',(56.6599284966586,36.8956552674856,-216.926524548004));
#210549=CARTESIAN_POINT('Ctrl Pts',(56.394913005841,37.054862700115,-217.026399523816));
#210550=CARTESIAN_POINT('Ctrl Pts',(56.4490528535666,37.2599459188071,-217.272499319579));
#210551=CARTESIAN_POINT('Ctrl Pts',(56.7089132278424,37.0787382657863,-216.762440352386));
#210552=CARTESIAN_POINT('Ctrl Pts',(56.4432500919346,37.2379648996087,-216.862162585543));
#210553=CARTESIAN_POINT('Ctrl Pts',(56.4975419847625,37.4436240691992,-217.108396707512));
#210554=CARTESIAN_POINT('',(56.5618180211198,36.5289367340069,-217.254048694966));
#210555=CARTESIAN_POINT('',(56.351930605989,36.892044198215,-217.60005));
#210556=CARTESIAN_POINT('Origin',(56.8353687650353,36.7644215263347,-217.60005));
#210557=CARTESIAN_POINT('Origin',(1.5713232372253,-170.618389538147,32.0043824444259));
#210558=CARTESIAN_POINT('Origin',(3.60305208601888,-172.041642880457,32.426831165629));
#210559=CARTESIAN_POINT('Ctrl Pts',(50.3946838675078,44.2853208550272,-215.949517829821));
#210560=CARTESIAN_POINT('Ctrl Pts',(50.5733927277608,44.0594460487845,-216.033846066216));
#210561=CARTESIAN_POINT('Ctrl Pts',(50.8056178277775,44.122591905242,-216.213154850206));
#210562=CARTESIAN_POINT('Ctrl Pts',(50.1727811095107,44.2347300586007,-216.246332930804));
#210563=CARTESIAN_POINT('Ctrl Pts',(50.3446120279677,43.9972367818614,-216.339838795389));
#210564=CARTESIAN_POINT('Ctrl Pts',(50.5708296219181,44.0587490977934,-216.539715105359));
#210565=CARTESIAN_POINT('Ctrl Pts',(49.9199744021421,44.177167823471,-216.514858553214));
#210566=CARTESIAN_POINT('Ctrl Pts',(50.0849672365085,43.9266350565256,-216.613616901689));
#210567=CARTESIAN_POINT('Ctrl Pts',(50.3034496116678,43.9860440381524,-216.835170188754));
#210568=CARTESIAN_POINT('Ctrl Pts',(49.6396803417508,44.1134564636836,-216.757742122242));
#210569=CARTESIAN_POINT('Ctrl Pts',(49.8012110043667,43.8494770305304,-216.857236779929));
#210570=CARTESIAN_POINT('Ctrl Pts',(50.0071669705522,43.9054798737905,-217.102435280211));
#210571=CARTESIAN_POINT('',(50.0071669705522,43.9054798737905,-217.102435280211));
#210572=CARTESIAN_POINT('',(49.6397984855093,44.1135871370302,-216.757171052664));
#210573=CARTESIAN_POINT('Origin',(49.8759723669763,44.3879609366236,-217.102435280211));
#210574=CARTESIAN_POINT('Ctrl Pts',(50.3945871449586,44.285210229431,-215.949426636219));
#210575=CARTESIAN_POINT('Ctrl Pts',(50.3403778185267,44.2728463269777,-216.021921068329));
#210576=CARTESIAN_POINT('Ctrl Pts',(50.28355971832,44.2598869737324,-216.093705509569));
#210577=CARTESIAN_POINT('Ctrl Pts',(50.2241655077576,44.2463440207748,-216.164581859815));
#210578=CARTESIAN_POINT('Ctrl Pts',(50.1944684024764,44.239572544296,-216.200020034938));
#210579=CARTESIAN_POINT('Ctrl Pts',(50.1641272315725,44.2326551146929,-216.235231809947));
#210580=CARTESIAN_POINT('Ctrl Pts',(50.133147084301,44.2255941671355,-216.270193455524));
#210581=CARTESIAN_POINT('Ctrl Pts',(50.1156219255874,44.2215998598934,-216.289970907912));
#210582=CARTESIAN_POINT('Ctrl Pts',(50.0975181940928,44.2174787265865,-216.310078664585));
#210583=CARTESIAN_POINT('Ctrl Pts',(50.0794698516225,44.213366172549,-216.329813053606));
#210584=CARTESIAN_POINT('Ctrl Pts',(50.0656131873037,44.2102087479332,-216.344964184778));
#210585=CARTESIAN_POINT('Ctrl Pts',(50.051789719492,44.2070570535312,-216.35989596509));
#210586=CARTESIAN_POINT('Ctrl Pts',(50.0382957503063,44.203984129756,-216.374304437988));
#210587=CARTESIAN_POINT('Ctrl Pts',(50.0072258500349,44.1969087145151,-216.40747998551));
#210588=CARTESIAN_POINT('Ctrl Pts',(49.9754962336944,44.1896861667369,-216.440479352724));
#210589=CARTESIAN_POINT('Ctrl Pts',(49.943109870758,44.1823161715401,-216.473276174347));
#210590=CARTESIAN_POINT('Ctrl Pts',(49.9269166892898,44.1786311739417,-216.489674585158));
#210591=CARTESIAN_POINT('Ctrl Pts',(49.9105593293605,44.1749093239475,-216.506022369873));
#210592=CARTESIAN_POINT('Ctrl Pts',(49.8940382741992,44.1711506884566,-216.522316205284));
#210593=CARTESIAN_POINT('Ctrl Pts',(49.8857777466186,44.1692713707111,-216.53046312299));
#210594=CARTESIAN_POINT('Ctrl Pts',(49.8774762957926,44.1673828572408,-216.53859655406));
#210595=CARTESIAN_POINT('Ctrl Pts',(49.8691339870412,44.1654851614539,-216.54671608504));
#210596=CARTESIAN_POINT('Ctrl Pts',(49.8649628326655,44.1645363135605,-216.550775850529));
#210597=CARTESIAN_POINT('Ctrl Pts',(49.8607814638429,44.1635851701277,-216.554832141041));
#210598=CARTESIAN_POINT('Ctrl Pts',(49.8565898891525,44.162631733232,-216.558884904864));
#210599=CARTESIAN_POINT('Ctrl Pts',(49.8534462081347,44.1619166555603,-216.561924477731));
#210600=CARTESIAN_POINT('Ctrl Pts',(49.8502967863191,44.161200287819,-216.564962066839));
#210601=CARTESIAN_POINT('Ctrl Pts',(49.8471416274209,44.160482630978,-216.567997650376));
#210602=CARTESIAN_POINT('Ctrl Pts',(49.8460899077882,44.1602434120311,-216.569009511555));
#210603=CARTESIAN_POINT('Ctrl Pts',(49.846052776601,44.1602349647155,-216.569046012336));
#210604=CARTESIAN_POINT('Ctrl Pts',(49.8439845563056,44.1597645444787,-216.571032564579));
#210605=CARTESIAN_POINT('Ctrl Pts',(49.8163330530824,44.1534751628673,-216.597592189719));
#210606=CARTESIAN_POINT('Ctrl Pts',(49.7913737799107,44.1476814359235,-216.621099989597));
#210607=CARTESIAN_POINT('Ctrl Pts',(49.7691963068403,44.1424976436824,-216.641712338298));
#210608=CARTESIAN_POINT('Ctrl Pts',(49.7468039447084,44.1372636229844,-216.662524410758));
#210609=CARTESIAN_POINT('Ctrl Pts',(49.7272473454039,44.1326512141046,-216.680384949048));
#210610=CARTESIAN_POINT('Ctrl Pts',(49.7105929590235,44.1287463153261,-216.695420899773));
#210611=CARTESIAN_POINT('Ctrl Pts',(49.693882897516,44.1248283625851,-216.710507115242));
#210612=CARTESIAN_POINT('Ctrl Pts',(49.6800943060718,44.1216224781896,-216.722750012389));
#210613=CARTESIAN_POINT('Ctrl Pts',(49.6692714766647,44.1191865642665,-216.73224013285));
#210614=CARTESIAN_POINT('Ctrl Pts',(49.6584179235548,44.1167437353038,-216.741757193737));
#210615=CARTESIAN_POINT('Ctrl Pts',(49.6505468786249,44.1150751379176,-216.748505942923));
#210616=CARTESIAN_POINT('Ctrl Pts',(49.6456823274345,44.1142124382665,-216.752537603844));
#210617=CARTESIAN_POINT('Ctrl Pts',(49.6420995619744,44.1135770558044,-216.755506941596));
#210618=CARTESIAN_POINT('Ctrl Pts',(49.6401472140672,44.1133782759279,-216.757001588688));
#210619=CARTESIAN_POINT('Ctrl Pts',(49.6398281339281,44.1136199297753,-216.757027741579));
#210620=CARTESIAN_POINT('Ctrl Pts',(50.0071669705522,43.9054798737905,-217.102435280211));
#210621=CARTESIAN_POINT('Ctrl Pts',(50.1847337846587,43.9537632357284,-216.942259136119));
#210622=CARTESIAN_POINT('Ctrl Pts',(50.3518605126507,43.999207765089,-216.772016153339));
#210623=CARTESIAN_POINT('Ctrl Pts',(50.5078320264026,44.0416190066736,-216.591016782892));
#210624=CARTESIAN_POINT('Ctrl Pts',(50.612160077052,44.069987534065,-216.469947806684));
#210625=CARTESIAN_POINT('Ctrl Pts',(50.7114964522455,44.0969987421063,-216.344065601437));
#210626=CARTESIAN_POINT('Ctrl Pts',(50.8056178277775,44.1225919052419,-216.213154850207));
#210627=CARTESIAN_POINT('Ctrl Pts',(56.3926362809384,37.06446862304,-217.512497927056));
#210628=CARTESIAN_POINT('Ctrl Pts',(56.3025297216358,36.8538919311899,-217.234982111681));
#210629=CARTESIAN_POINT('Ctrl Pts',(56.6014172235551,36.7002760622361,-217.106014442417));
#210630=CARTESIAN_POINT('Ctrl Pts',(56.3494657971762,36.8595412342349,-217.614210849647));
#210631=CARTESIAN_POINT('Ctrl Pts',(56.3042743964622,36.6629877513575,-217.365043032676));
#210632=CARTESIAN_POINT('Ctrl Pts',(56.5644478950071,36.4938829304004,-217.276020812814));
#210633=CARTESIAN_POINT('Ctrl Pts',(56.2928585179201,36.6687695948746,-217.720014138817));
#210634=CARTESIAN_POINT('Ctrl Pts',(56.2815005063899,36.4738999535249,-217.512326327457));
#210635=CARTESIAN_POINT('Ctrl Pts',(56.5034547435963,36.3047735443712,-217.452585270555));
#210636=CARTESIAN_POINT('Ctrl Pts',(56.1826979052857,36.4485237337307,-217.873731285031));
#210637=CARTESIAN_POINT('Ctrl Pts',(56.1903893360325,36.2585417753414,-217.731401553872));
#210638=CARTESIAN_POINT('Ctrl Pts',(56.360210366167,36.0935380424276,-217.709357506335));
#210639=CARTESIAN_POINT('Ctrl Pts',(56.1505723352367,36.3946362936106,-217.914986052151));
#210640=CARTESIAN_POINT('Ctrl Pts',(56.1614999948485,36.2069207362181,-217.789469422921));
#210641=CARTESIAN_POINT('Ctrl Pts',(56.316755943097,36.0426866473361,-217.778283977819));
#210642=CARTESIAN_POINT('Ctrl Pts',(56.0799766262647,36.300874136992,-217.997168943781));
#210643=CARTESIAN_POINT('Ctrl Pts',(56.0918994632683,36.1185322173306,-217.904857915558));
#210644=CARTESIAN_POINT('Ctrl Pts',(56.2172639412631,35.9565745816487,-217.915612680145));
#210645=CARTESIAN_POINT('Ctrl Pts',(56.0407806740724,36.2602422377127,-218.038872206682));
#210646=CARTESIAN_POINT('Ctrl Pts',(56.0504566435121,36.0806895467743,-217.963493085148));
#210647=CARTESIAN_POINT('Ctrl Pts',(56.1601699153834,35.9206448721989,-217.98530951335));
#210648=CARTESIAN_POINT('Ctrl Pts',(55.9568722227823,36.2011920617794,-218.118554011763));
#210649=CARTESIAN_POINT('Ctrl Pts',(55.9559190189864,36.0280927685888,-218.074319363236));
#210650=CARTESIAN_POINT('Ctrl Pts',(56.0334146789495,35.8727684150699,-218.118501095087));
#210651=CARTESIAN_POINT('Ctrl Pts',(55.9109933553098,36.1822589517139,-218.15753647007));
#210652=CARTESIAN_POINT('Ctrl Pts',(55.9013096891468,36.012582278575,-218.128229973778));
#210653=CARTESIAN_POINT('Ctrl Pts',(55.9619426599398,35.8604753878485,-218.183672765375));
#210654=CARTESIAN_POINT('Ctrl Pts',(55.8172819109955,36.1744746994185,-218.226480768326));
#210655=CARTESIAN_POINT('Ctrl Pts',(55.7847759578152,36.0120234844064,-218.22108863219));
#210656=CARTESIAN_POINT('Ctrl Pts',(55.8109478702867,35.8674781880438,-218.298960241952));
#210657=CARTESIAN_POINT('Ctrl Pts',(55.7685414980389,36.1858554246731,-218.257001059377));
#210658=CARTESIAN_POINT('Ctrl Pts',(55.7213420795204,36.0271858039415,-218.261086960987));
#210659=CARTESIAN_POINT('Ctrl Pts',(55.7299143791894,35.8871614634557,-218.350008528068));
#210660=CARTESIAN_POINT('Ctrl Pts',(55.593234661827,36.2832559111648,-218.346964015346));
#210661=CARTESIAN_POINT('Ctrl Pts',(55.4860097606963,36.1376664348096,-218.372159308156));
#210662=CARTESIAN_POINT('Ctrl Pts',(55.4293178179656,36.0166622041161,-218.500532672009));
#210663=CARTESIAN_POINT('Ctrl Pts',(55.4818780387848,36.4672944339616,-218.361109888845));
#210664=CARTESIAN_POINT('Ctrl Pts',(55.3185434642075,36.3337248928643,-218.370180569382));
#210665=CARTESIAN_POINT('Ctrl Pts',(55.2179523418132,36.2266656323018,-218.52434896282));
#210666=CARTESIAN_POINT('Ctrl Pts',(55.4133688931145,36.6545388584683,-218.342531698738));
#210667=CARTESIAN_POINT('Ctrl Pts',(55.2229303298313,36.5126576021272,-218.321336607546));
#210668=CARTESIAN_POINT('Ctrl Pts',(55.0778128694631,36.4307605489773,-218.493419988678));
#210669=CARTESIAN_POINT('Ctrl Pts',(55.2146353748417,36.257836765148,-218.504776656654));
#210670=CARTESIAN_POINT('Ctrl Pts',(55.2853252387498,36.178323141292,-218.503619746298));
#210671=CARTESIAN_POINT('Ctrl Pts',(55.3572048505888,36.110335848808,-218.493333122548));
#210672=CARTESIAN_POINT('Ctrl Pts',(55.4666504076737,36.0261193376424,-218.464208616831));
#210673=CARTESIAN_POINT('Ctrl Pts',(55.5217803745163,35.9884509426223,-218.446222721449));
#210674=CARTESIAN_POINT('Ctrl Pts',(55.5774971758583,35.9575194484196,-218.423101362283));
#210675=CARTESIAN_POINT('Ctrl Pts',(55.6147698445988,35.9384032334131,-218.406545908665));
#210676=CARTESIAN_POINT('Ctrl Pts',(55.6324611397065,35.9300304583408,-218.398204123294));
#210677=CARTESIAN_POINT('Ctrl Pts',(55.7313233794382,35.8876181643618,-218.34857667575));
#210678=CARTESIAN_POINT('Ctrl Pts',(55.8079534193385,35.8685625899143,-218.300602301064));
#210679=CARTESIAN_POINT('Ctrl Pts',(55.9191591973471,35.8626148725108,-218.216232114058));
#210680=CARTESIAN_POINT('Ctrl Pts',(55.9738280789745,35.8652970767159,-218.17094486431));
#210681=CARTESIAN_POINT('Ctrl Pts',(56.0359726937985,35.8783633914484,-218.112680966177));
#210682=CARTESIAN_POINT('Ctrl Pts',(56.062256145949,35.8860946120971,-218.086547415529));
#210683=CARTESIAN_POINT('Ctrl Pts',(56.0797007647607,35.8917225550678,-218.068866535409));
#210684=CARTESIAN_POINT('Ctrl Pts',(56.089754223533,35.895294478457,-218.058454853419));
#210685=CARTESIAN_POINT('Ctrl Pts',(56.1552263829685,35.9201954539469,-217.989542144483));
#210686=CARTESIAN_POINT('Ctrl Pts',(56.2092799448895,35.952330746872,-217.924827472252));
#210687=CARTESIAN_POINT('Ctrl Pts',(56.284215107907,36.015451914569,-217.822567067476));
#210688=CARTESIAN_POINT('Ctrl Pts',(56.3201469433926,36.050740243414,-217.77013976598));
#210689=CARTESIAN_POINT('Ctrl Pts',(56.3594019560273,36.0983953590986,-217.706704657463));
#210690=CARTESIAN_POINT('Ctrl Pts',(56.375657213717,36.1202032964773,-217.679031770219));
#210691=CARTESIAN_POINT('Ctrl Pts',(56.3863680913675,36.1350489083464,-217.660475087131));
#210692=CARTESIAN_POINT('Ctrl Pts',(56.3924751485261,36.14382919598,-217.649680615388));
#210693=CARTESIAN_POINT('Ctrl Pts',(56.4675309888385,36.2547622702157,-217.514966686909));
#210694=CARTESIAN_POINT('Ctrl Pts',(56.5223283895667,36.3813273192802,-217.38573082968));
#210695=CARTESIAN_POINT('Ctrl Pts',(56.5618180211198,36.5289367340069,-217.254048694966));
#210696=CARTESIAN_POINT('Ctrl Pts',(56.351930605989,36.892044198215,-217.60005));
#210697=CARTESIAN_POINT('Ctrl Pts',(56.3106341552242,36.73561211731,-217.683519137624));
#210698=CARTESIAN_POINT('Ctrl Pts',(56.2620376674877,36.6063567109475,-217.763138346979));
#210699=CARTESIAN_POINT('Ctrl Pts',(56.1841151753959,36.4516751886226,-217.871613557135));
#210700=CARTESIAN_POINT('Ctrl Pts',(56.1573135581897,36.4066455053365,-217.905983993627));
#210701=CARTESIAN_POINT('Ctrl Pts',(56.1166432440885,36.3486930756933,-217.95452292113));
#210702=CARTESIAN_POINT('Ctrl Pts',(56.0961909694752,36.3221149231009,-217.978041235787));
#210703=CARTESIAN_POINT('Ctrl Pts',(56.0722901467882,36.2952600973141,-218.004121560642));
#210704=CARTESIAN_POINT('Ctrl Pts',(56.0603499093352,36.2828656242958,-218.01681895322));
#210705=CARTESIAN_POINT('Ctrl Pts',(56.0543848280906,36.2769259643628,-218.023081587245));
#210706=CARTESIAN_POINT('Ctrl Pts',(56.0518297096401,36.2744355207168,-218.025747097373));
#210707=CARTESIAN_POINT('Ctrl Pts',(56.0501266256028,36.2727874671719,-218.027519994919));
#210708=CARTESIAN_POINT('Ctrl Pts',(56.0499682211993,36.2726304501984,-218.027686065033));
#210709=CARTESIAN_POINT('Ctrl Pts',(55.9990105266362,36.2240321053245,-218.080507909176));
#210710=CARTESIAN_POINT('Ctrl Pts',(55.947907222693,36.1948194705703,-218.126920434258));
#210711=CARTESIAN_POINT('Ctrl Pts',(55.870874722202,36.1773006083812,-218.187476759461));
#210712=CARTESIAN_POINT('Ctrl Pts',(55.8451383675446,36.1758432616423,-218.206158299427));
#210713=CARTESIAN_POINT('Ctrl Pts',(55.8067444797832,36.1801517391582,-218.231754361591));
#210714=CARTESIAN_POINT('Ctrl Pts',(55.7939817881794,36.1826702714089,-218.239882441288));
#210715=CARTESIAN_POINT('Ctrl Pts',(55.7685784254658,36.189858492269,-218.25530756497));
#210716=CARTESIAN_POINT('Ctrl Pts',(55.7547799188749,36.1950574432706,-218.263238404901));
#210717=CARTESIAN_POINT('Ctrl Pts',(55.6522189990078,36.2419393110166,-218.319379639693));
#210718=CARTESIAN_POINT('Ctrl Pts',(55.5615769900803,36.3417129235347,-218.348549476024));
#210719=CARTESIAN_POINT('Ctrl Pts',(55.4814981831708,36.4969369346298,-218.349992971048));
#210720=CARTESIAN_POINT('Ctrl Pts',(49.6396803417518,44.1134564636829,-216.757742122242));
#210721=CARTESIAN_POINT('Ctrl Pts',(49.8012110043674,43.8494770305306,-216.85723677993));
#210722=CARTESIAN_POINT('Ctrl Pts',(50.0071669705522,43.9054798737905,-217.102435280211));
#210723=CARTESIAN_POINT('Ctrl Pts',(49.4561530329476,44.062897140813,-216.9238167844));
#210724=CARTESIAN_POINT('Ctrl Pts',(49.6176813002303,43.7995722598871,-217.023443915385));
#210725=CARTESIAN_POINT('Ctrl Pts',(49.8231124216493,43.8554323891537,-217.268463758512));
#210726=CARTESIAN_POINT('Ctrl Pts',(49.2724911599438,44.0123032282188,-217.089736149786));
#210727=CARTESIAN_POINT('Ctrl Pts',(49.4339330913007,43.7496080741896,-217.18956917487));
#210728=CARTESIAN_POINT('Ctrl Pts',(49.6389254121935,43.8053488862956,-217.43433427542));
#210729=CARTESIAN_POINT('Ctrl Pts',(49.0886970638134,43.9616759445554,-217.255503157469));
#210730=CARTESIAN_POINT('Ctrl Pts',(49.249970603928,43.6995856225942,-217.355612986355));
#210731=CARTESIAN_POINT('Ctrl Pts',(49.4546085996559,43.7552300878266,-217.60005));
#210732=CARTESIAN_POINT('',(49.4546085996559,43.7552300878266,-217.60005));
#210733=CARTESIAN_POINT('',(49.0886970638134,43.9616759445554,-217.255503157469));
#210734=CARTESIAN_POINT('Origin',(49.3234139960799,44.2377111506597,-217.60005));
#210735=CARTESIAN_POINT('Origin',(-245.875985088577,-31.0780147762713,132.706328537592));
#210736=CARTESIAN_POINT('Origin',(-243.323155334121,-35.8559000200963,132.120548472853));
#210737=CARTESIAN_POINT('Ctrl Pts',(49.2392068969802,42.8144262318624,-218.342424126527));
#210738=CARTESIAN_POINT('Ctrl Pts',(49.0981352490002,42.6214993839962,-218.320536202568));
#210739=CARTESIAN_POINT('Ctrl Pts',(49.0177848955319,42.4743719985975,-218.493933115956));
#210740=CARTESIAN_POINT('Ctrl Pts',(49.0491457939108,42.8840876677029,-218.360683589143));
#210741=CARTESIAN_POINT('Ctrl Pts',(48.9156261565165,42.7194999188607,-218.369201842649));
#210742=CARTESIAN_POINT('Ctrl Pts',(48.8090073140709,42.6180259879625,-218.524438151629));
#210743=CARTESIAN_POINT('Ctrl Pts',(48.8672534647879,42.9910417045365,-218.348178740586));
#210744=CARTESIAN_POINT('Ctrl Pts',(48.7219544884179,42.8806403242223,-218.373299555436));
#210745=CARTESIAN_POINT('Ctrl Pts',(48.6015262175029,42.8217286940762,-218.503553799908));
#210746=CARTESIAN_POINT('Ctrl Pts',(48.7646928214946,43.1655096926852,-218.259342211925));
#210747=CARTESIAN_POINT('Ctrl Pts',(48.6060096790964,43.1152569501545,-218.264332467645));
#210748=CARTESIAN_POINT('Ctrl Pts',(48.4659622753937,43.1213501679656,-218.355161400681));
#210749=CARTESIAN_POINT('Ctrl Pts',(48.7517775386604,43.2137285664805,-218.229368151499));
#210750=CARTESIAN_POINT('Ctrl Pts',(48.5892675478649,43.1781221617649,-218.225243782383));
#210751=CARTESIAN_POINT('Ctrl Pts',(48.4445750481121,43.2016010011096,-218.305092323547));
#210752=CARTESIAN_POINT('Ctrl Pts',(48.7563271074926,43.3078462492642,-218.160564679312));
#210753=CARTESIAN_POINT('Ctrl Pts',(48.5864539575163,43.2953660943901,-218.132916872251));
#210754=CARTESIAN_POINT('Ctrl Pts',(48.4338397167942,43.3533018519225,-218.190166022795));
#210755=CARTESIAN_POINT('Ctrl Pts',(48.7735288446776,43.353809900952,-218.121783538057));
#210756=CARTESIAN_POINT('Ctrl Pts',(48.600190391689,43.3502145581132,-218.079437137287));
#210757=CARTESIAN_POINT('Ctrl Pts',(48.4442068501562,43.4249009945937,-218.125389059377));
#210758=CARTESIAN_POINT('Ctrl Pts',(48.8590039851191,43.4820375499056,-218.000750329661));
#210759=CARTESIAN_POINT('Ctrl Pts',(48.6761884264651,43.4957516216008,-217.91062368486));
#210760=CARTESIAN_POINT('Ctrl Pts',(48.5121910139739,43.6184164248186,-217.923237587047));
#210761=CARTESIAN_POINT('Ctrl Pts',(48.9577162497748,43.553347797655,-217.915924150638));
#210762=CARTESIAN_POINT('Ctrl Pts',(48.7711504507846,43.5651821516904,-217.790160547008));
#210763=CARTESIAN_POINT('Ctrl Pts',(48.6033294989531,43.717527334291,-217.781577327593));
#210764=CARTESIAN_POINT('Ctrl Pts',(49.2312854327744,43.6941863378053,-217.721426214149));
#210765=CARTESIAN_POINT('Ctrl Pts',(49.036202633002,43.6813887518905,-217.516069552265));
#210766=CARTESIAN_POINT('Ctrl Pts',(48.8652456863714,43.9001875035932,-217.456834233708));
#210767=CARTESIAN_POINT('Ctrl Pts',(49.4219022397322,43.7527128881036,-217.614176933529));
#210768=CARTESIAN_POINT('Ctrl Pts',(49.2255719813905,43.7062052444277,-217.366811601907));
#210769=CARTESIAN_POINT('Ctrl Pts',(49.0541586904782,43.9632581572301,-217.27791260876));
#210770=CARTESIAN_POINT('Ctrl Pts',(49.6270070524957,43.7971127295262,-217.511593584289));
#210771=CARTESIAN_POINT('Ctrl Pts',(49.4168888445486,43.7053026630152,-217.236018678808));
#210772=CARTESIAN_POINT('Ctrl Pts',(49.2608016511118,44.0011146440645,-217.106570340894));
#210773=CARTESIAN_POINT('Ctrl Pts',(49.0801870931398,42.8824343798319,-218.350025764149));
#210774=CARTESIAN_POINT('Ctrl Pts',(49.0027571269435,42.9216296157716,-218.349558363419));
#210775=CARTESIAN_POINT('Ctrl Pts',(48.9387927753833,42.9635850473862,-218.342311230351));
#210776=CARTESIAN_POINT('Ctrl Pts',(48.8636071075648,43.0285900688282,-218.322357133335));
#210777=CARTESIAN_POINT('Ctrl Pts',(48.842004191093,43.0506080260999,-218.314196680044));
#210778=CARTESIAN_POINT('Ctrl Pts',(48.8148473949678,43.0839419698545,-218.299864963562));
#210779=CARTESIAN_POINT('Ctrl Pts',(48.8066696449585,43.0951047505369,-218.294739439232));
#210780=CARTESIAN_POINT('Ctrl Pts',(48.7920720413194,43.1175006398046,-218.283822966434));
#210781=CARTESIAN_POINT('Ctrl Pts',(48.7863005322459,43.1274160298958,-218.278747184425));
#210782=CARTESIAN_POINT('Ctrl Pts',(48.7553747751317,43.1902706205099,-218.244634347041));
#210783=CARTESIAN_POINT('Ctrl Pts',(48.7477937598005,43.2420701216404,-218.21038868015));
#210784=CARTESIAN_POINT('Ctrl Pts',(48.7628376713814,43.3195568794426,-218.149810572131));
#210785=CARTESIAN_POINT('Ctrl Pts',(48.7722543376512,43.3453523812971,-218.128090157083));
#210786=CARTESIAN_POINT('Ctrl Pts',(48.7930599541517,43.3837102238485,-218.093434197843));
#210787=CARTESIAN_POINT('Ctrl Pts',(48.8051328278828,43.4028056191118,-218.075588028891));
#210788=CARTESIAN_POINT('Ctrl Pts',(48.8221563815815,43.4248788632682,-218.053914616086));
#210789=CARTESIAN_POINT('Ctrl Pts',(48.8314046938857,43.4358573117923,-218.04287191288));
#210790=CARTESIAN_POINT('Ctrl Pts',(48.8355262866093,43.4405491551657,-218.038095968273));
#210791=CARTESIAN_POINT('Ctrl Pts',(48.8383091550492,43.4436740347655,-218.034902458652));
#210792=CARTESIAN_POINT('Ctrl Pts',(48.8403571964181,43.4459334904679,-218.032581409616));
#210793=CARTESIAN_POINT('Ctrl Pts',(48.9419508914772,43.5569843544506,-217.91819246589));
#210794=CARTESIAN_POINT('Ctrl Pts',(49.1434923162074,43.6706324100787,-217.767881223762));
#210795=CARTESIAN_POINT('Ctrl Pts',(49.4546085996559,43.7552300878266,-217.60005));
#210796=CARTESIAN_POINT('Ctrl Pts',(49.0886970638134,43.9616759445554,-217.255503157469));
#210797=CARTESIAN_POINT('Ctrl Pts',(49.0151399287483,43.9414141514911,-217.321845583205));
#210798=CARTESIAN_POINT('Ctrl Pts',(48.946963488087,43.9173173047126,-217.387552824715));
#210799=CARTESIAN_POINT('Ctrl Pts',(48.8529836892348,43.8753202935614,-217.485160910641));
#210800=CARTESIAN_POINT('Ctrl Pts',(48.8080643548638,43.8528590646516,-217.533726759519));
#210801=CARTESIAN_POINT('Ctrl Pts',(48.7593218903077,43.8240748429766,-217.589970076895));
#210802=CARTESIAN_POINT('Ctrl Pts',(48.7392211301387,43.8111840065362,-217.613985032988));
#210803=CARTESIAN_POINT('Ctrl Pts',(48.7259963435662,43.802466619305,-217.62997515421));
#210804=CARTESIAN_POINT('Ctrl Pts',(48.720651615937,43.7988677824946,-217.636498434306));
#210805=CARTESIAN_POINT('Ctrl Pts',(48.6521051529089,43.7511326433927,-217.721432036098));
#210806=CARTESIAN_POINT('Ctrl Pts',(48.6011058466663,43.7046963796237,-217.793420116029));
#210807=CARTESIAN_POINT('Ctrl Pts',(48.5396829829941,43.6289232846257,-217.896139553435));
#210808=CARTESIAN_POINT('Ctrl Pts',(48.5127389007901,43.5895075224444,-217.946183601514));
#210809=CARTESIAN_POINT('Ctrl Pts',(48.4879192797322,43.5408261485385,-218.002265900684));
#210810=CARTESIAN_POINT('Ctrl Pts',(48.4787011809696,43.51938296299,-218.025807795273));
#210811=CARTESIAN_POINT('Ctrl Pts',(48.4728712136029,43.5049584605067,-218.041392752447));
#210812=CARTESIAN_POINT('Ctrl Pts',(48.4704899065757,43.4987434520148,-218.048019264419));
#210813=CARTESIAN_POINT('Ctrl Pts',(48.4556126179059,43.4567276111961,-218.091989196291));
#210814=CARTESIAN_POINT('Ctrl Pts',(48.447318636186,43.4223097123662,-218.125369094889));
#210815=CARTESIAN_POINT('Ctrl Pts',(48.4379355955513,43.351853178451,-218.188536798286));
#210816=CARTESIAN_POINT('Ctrl Pts',(48.4367425363059,43.3173465388334,-218.217160970929));
#210817=CARTESIAN_POINT('Ctrl Pts',(48.4419528191108,43.2405774742888,-218.275471751038));
#210818=CARTESIAN_POINT('Ctrl Pts',(48.4484251786589,43.2018063387531,-218.302297507464));
#210819=CARTESIAN_POINT('Ctrl Pts',(48.4690551947459,43.1234942327623,-218.351289753058));
#210820=CARTESIAN_POINT('Ctrl Pts',(48.4840362288625,43.0821239108137,-218.374365224399));
#210821=CARTESIAN_POINT('Ctrl Pts',(48.5183278546908,43.0059380338195,-218.412220971132));
#210822=CARTESIAN_POINT('Ctrl Pts',(48.5490891293158,42.9488251961246,-218.437102070953));
#210823=CARTESIAN_POINT('Ctrl Pts',(48.5873397829352,42.8917692531179,-218.456717105432));
#210824=CARTESIAN_POINT('Ctrl Pts',(48.6144952712976,42.8537469019519,-218.468623558342));
#210825=CARTESIAN_POINT('Ctrl Pts',(48.6300405465755,42.8333212305513,-218.474349716168));
#210826=CARTESIAN_POINT('Ctrl Pts',(48.700481295165,42.745455745346,-218.496474416014));
#210827=CARTESIAN_POINT('Ctrl Pts',(48.7664496150731,42.6773021397737,-218.505675051354));
#210828=CARTESIAN_POINT('Ctrl Pts',(48.8417930108281,42.6113834075459,-218.506376562157));
#210829=CARTESIAN_POINT('Origin',(-2.81802535037841,-9.69927298715315,-227.60005));
#210830=CARTESIAN_POINT('',(48.1633319901564,41.4530789012665,-228.35005));
#210831=CARTESIAN_POINT('',(48.1633319901564,41.4530789012665,-228.35005));
#210832=CARTESIAN_POINT('',(47.632114758242,41.9825203546087,-227.60005));
#210833=CARTESIAN_POINT('',(41.9598150400404,36.2911954009805,-227.60005));
#210834=CARTESIAN_POINT('Origin',(48.1633319901564,41.4530789012665,-227.60005));
#210835=CARTESIAN_POINT('Ctrl Pts',(47.6321147582419,41.9825203546088,-227.60005));
#210836=CARTESIAN_POINT('Ctrl Pts',(48.6421799545279,42.9959733704936,-227.60005));
#210837=CARTESIAN_POINT('Ctrl Pts',(49.7021444432209,42.0348313420379,-227.60005));
#210838=CARTESIAN_POINT('Ctrl Pts',(47.6321147582419,41.9825203546088,-228.35005));
#210839=CARTESIAN_POINT('Ctrl Pts',(48.6421799545279,42.9959733704936,-228.35005));
#210840=CARTESIAN_POINT('Ctrl Pts',(49.7021444432209,42.0348313420379,-228.35005));
#210841=CARTESIAN_POINT('Ctrl Pts',(48.1633319901564,41.4530789012665,-228.35005));
#210842=CARTESIAN_POINT('Ctrl Pts',(48.6683645882994,41.9598054092088,-228.35005));
#210843=CARTESIAN_POINT('Ctrl Pts',(49.1983468326458,41.479234394981,-228.35005));
#210844=CARTESIAN_POINT('',(49.7021444432209,42.0348313420379,-227.60005));
#210845=CARTESIAN_POINT('Origin',(48.6945492220708,40.9236374479242,-227.60005));
#210846=CARTESIAN_POINT('',(49.1983468326459,41.4792343949811,-228.35005));
#210847=CARTESIAN_POINT('Origin',(49.1983468326459,41.4792343949811,-227.60005));
#210848=CARTESIAN_POINT('Origin',(48.6945492220708,40.9236374479242,-228.35005));
#210849=CARTESIAN_POINT('Origin',(0.128459562639233,-12.6359082483571,-227.60005));
#210850=CARTESIAN_POINT('',(54.0789914828443,36.6149049990089,-228.35005));
#210851=CARTESIAN_POINT('Origin',(0.128459562639233,-12.6359082483571,-228.35005));
#210852=CARTESIAN_POINT('Origin',(0.128459562639233,-12.6359082483571,-228.35005));
#210853=CARTESIAN_POINT('',(54.6328983814091,37.1205601658197,-227.60005));
#210854=CARTESIAN_POINT('Origin',(0.128459562639233,-12.6359082483571,-227.60005));
#210855=CARTESIAN_POINT('Origin',(54.0789914828443,36.6149049990089,-227.60005));
#210856=CARTESIAN_POINT('Ctrl Pts',(54.6328983814091,37.1205601658197,-227.60005));
#210857=CARTESIAN_POINT('Ctrl Pts',(55.5975842443944,36.0638199413983,-227.60005));
#210858=CARTESIAN_POINT('Ctrl Pts',(54.5875190481084,35.0503669255137,-227.60005));
#210859=CARTESIAN_POINT('Ctrl Pts',(54.6328983814091,37.1205601658197,-228.35005));
#210860=CARTESIAN_POINT('Ctrl Pts',(55.5975842443944,36.0638199413983,-228.35005));
#210861=CARTESIAN_POINT('Ctrl Pts',(54.5875190481084,35.0503669255137,-228.35005));
#210862=CARTESIAN_POINT('Ctrl Pts',(54.0789914828443,36.614904999009,-228.35005));
#210863=CARTESIAN_POINT('Ctrl Pts',(54.5613344143369,36.0865348867983,-228.35005));
#210864=CARTESIAN_POINT('Ctrl Pts',(54.056301816194,35.579808378856,-228.35005));
#210865=CARTESIAN_POINT('',(54.5875190481084,35.0503669255136,-227.60005));
#210866=CARTESIAN_POINT('',(54.056301816194,35.579808378856,-228.35005));
#210867=CARTESIAN_POINT('Origin',(54.056301816194,35.579808378856,-227.60005));
#210868=CARTESIAN_POINT('Origin',(53.5250845842796,36.1092498321983,-228.35005));
#210869=CARTESIAN_POINT('Origin',(53.5250845842796,36.1092498321983,-227.60005));
#210870=CARTESIAN_POINT('Origin',(3.07494447565784,-15.5725435095623,-227.60005));
#210871=CARTESIAN_POINT('',(54.5875190481084,35.0503669255136,-227.60005));
#210872=CARTESIAN_POINT('',(48.3142830765682,29.8185305620001,-228.35005));
#210873=CARTESIAN_POINT('Origin',(-10.7603008067452,26.6045648983079,-217.60005));
#210874=CARTESIAN_POINT('',(51.0024097331414,43.3988703109923,-218.35005));
#210875=CARTESIAN_POINT('',(-10.7603008067452,26.6045648983079,-218.35005));
#210876=CARTESIAN_POINT('',(50.8056178277775,44.122591905242,-217.60005));
#210877=CARTESIAN_POINT('',(51.6000409161409,44.3386087195339,-217.60005));
#210878=CARTESIAN_POINT('Origin',(51.0024097331414,43.3988703109923,-217.60005));
#210879=CARTESIAN_POINT('Ctrl Pts',(50.8056178277775,44.1225919052419,-217.60005));
#210880=CARTESIAN_POINT('Ctrl Pts',(51.6051500510689,44.3399979780626,-217.60005));
#210881=CARTESIAN_POINT('Ctrl Pts',(52.2148720050704,43.7789665035542,-217.60005));
#210882=CARTESIAN_POINT('Ctrl Pts',(50.8056178277775,44.1225919052419,-218.35005));
#210883=CARTESIAN_POINT('Ctrl Pts',(51.6051500510689,44.3399979780626,-218.35005));
#210884=CARTESIAN_POINT('Ctrl Pts',(52.2148720050704,43.7789665035542,-218.35005));
#210885=CARTESIAN_POINT('Ctrl Pts',(51.0024097331414,43.3988703109923,-218.35005));
#210886=CARTESIAN_POINT('Ctrl Pts',(51.4021758447871,43.5075733474026,-218.35005));
#210887=CARTESIAN_POINT('Ctrl Pts',(51.7070368217878,43.2270576101484,-218.35005));
#210888=CARTESIAN_POINT('',(52.2148720050704,43.7789665035542,-217.60005));
#210889=CARTESIAN_POINT('Origin',(51.1992016385053,42.6751487167426,-217.60005));
#210890=CARTESIAN_POINT('',(51.7070368217878,43.2270576101484,-218.35005));
#210891=CARTESIAN_POINT('Origin',(51.7070368217878,43.2270576101484,-217.60005));
#210892=CARTESIAN_POINT('Origin',(51.1992016385053,42.6751487167426,-218.35005));
#210893=CARTESIAN_POINT('Origin',(0.,-12.9675000200281,-217.60005));
#210894=CARTESIAN_POINT('',(56.3587426896623,39.6656306474361,-217.60005));
#210895=CARTESIAN_POINT('',(55.8106047487975,39.1537275337666,-218.35005));
#210896=CARTESIAN_POINT('Origin',(55.8106047487975,39.1537275337666,-217.60005));
#210897=CARTESIAN_POINT('Origin',(0.,-12.9675000200281,-218.35005));
#210898=CARTESIAN_POINT('Origin',(0.,-12.9675000200281,-217.60005));
#210899=CARTESIAN_POINT('Ctrl Pts',(56.3587426896623,39.6656306474361,-217.60005));
#210900=CARTESIAN_POINT('Ctrl Pts',(56.9242682147177,39.0600746573811,-217.60005));
#210901=CARTESIAN_POINT('Ctrl Pts',(56.7127812850717,38.2589564044561,-217.60005));
#210902=CARTESIAN_POINT('Ctrl Pts',(56.3587426896623,39.6656306474361,-218.35005));
#210903=CARTESIAN_POINT('Ctrl Pts',(56.9242682147177,39.0600746573811,-218.35005));
#210904=CARTESIAN_POINT('Ctrl Pts',(56.7127812850717,38.2589564044561,-218.35005));
#210905=CARTESIAN_POINT('Ctrl Pts',(55.8106047487975,39.1537275337666,-218.35005));
#210906=CARTESIAN_POINT('Ctrl Pts',(56.0933675113252,38.8509495387392,-218.35005));
#210907=CARTESIAN_POINT('Ctrl Pts',(55.9876240465022,38.4503904122767,-218.35005));
#210908=CARTESIAN_POINT('',(56.7127812850717,38.2589564044561,-217.60005));
#210909=CARTESIAN_POINT('',(55.9876240465022,38.4503904122767,-218.35005));
#210910=CARTESIAN_POINT('Origin',(55.9876240465022,38.4503904122767,-217.60005));
#210911=CARTESIAN_POINT('Origin',(55.2624668079327,38.6418244200972,-218.35005));
#210912=CARTESIAN_POINT('Origin',(55.2624668079327,38.6418244200972,-217.60005));
#210913=CARTESIAN_POINT('Origin',(39.6505639028577,-23.4348386281926,-217.60005));
#210914=CARTESIAN_POINT('',(39.6505639028577,-23.4348386281926,-218.35005));
#210915=CARTESIAN_POINT('',(51.3278340104563,17.8606293780317,-217.60005));
#210916=CARTESIAN_POINT('Origin',(39.6266165499379,-2.40986505017056,-217.60005));
#210917=CARTESIAN_POINT('',(56.1046081325044,-64.2577178902918,-218.35005));
#210918=CARTESIAN_POINT('',(56.1046081325044,-64.2577178902918,-218.35005));
#210919=CARTESIAN_POINT('',(56.8293274051384,-64.0646324794683,-217.60005));
#210920=CARTESIAN_POINT('',(56.0236521904458,-61.0406424582598,-217.60005));
#210921=CARTESIAN_POINT('Origin',(56.1046081325044,-64.2577178902918,-217.60005));
#210922=CARTESIAN_POINT('Ctrl Pts',(55.9291914878272,-64.9614564347782,
-218.35005));
#210923=CARTESIAN_POINT('Ctrl Pts',(56.2112637919648,-64.658035095081,-218.35005));
#210924=CARTESIAN_POINT('Ctrl Pts',(56.1046081325044,-64.2577178902918,
-218.35005));
#210925=CARTESIAN_POINT('Ctrl Pts',(56.478494115784,-65.4721095684411,-218.35005));
#210926=CARTESIAN_POINT('Ctrl Pts',(57.0426387240591,-64.8652668890467,
-218.35005));
#210927=CARTESIAN_POINT('Ctrl Pts',(56.8293274051384,-64.0646324794683,
-218.35005));
#210928=CARTESIAN_POINT('Ctrl Pts',(56.478494115784,-65.4721095684411,-217.60005));
#210929=CARTESIAN_POINT('Ctrl Pts',(57.0426387240591,-64.8652668890467,
-217.60005));
#210930=CARTESIAN_POINT('Ctrl Pts',(56.8293274051384,-64.0646324794683,
-217.60005));
#210931=CARTESIAN_POINT('',(56.478494115784,-65.4721095684411,-217.60005));
#210932=CARTESIAN_POINT('',(55.9291914878272,-64.9614564347782,-218.35005));
#210933=CARTESIAN_POINT('Origin',(55.9291914878272,-64.9614564347782,-217.60005));
#210934=CARTESIAN_POINT('Origin',(55.3798888598704,-64.4508033011153,-218.35005));
#210935=CARTESIAN_POINT('Origin',(55.3798888598704,-64.4508033011153,-217.60005));
#210936=CARTESIAN_POINT('Origin',(0.,-12.9675000200281,-217.60005));
#210937=CARTESIAN_POINT('',(52.3440043138885,-69.594874440935,-217.60005));
#210938=CARTESIAN_POINT('',(51.8349132062458,-69.0441238221254,-218.35005));
#210939=CARTESIAN_POINT('Origin',(51.8349132062458,-69.0441238221255,-217.60005));
#210940=CARTESIAN_POINT('Origin',(0.,-12.9675000200281,-218.35005));
#210941=CARTESIAN_POINT('Origin',(0.,-12.9675000200281,-217.60005));
#210942=CARTESIAN_POINT('Ctrl Pts',(51.1306793331593,-69.2175412094409,
-218.35005));
#210943=CARTESIAN_POINT('Ctrl Pts',(51.5306920318089,-69.3253333012854,
-218.35005));
#210944=CARTESIAN_POINT('Ctrl Pts',(51.8349132062458,-69.0441238221254,
-218.35005));
#210945=CARTESIAN_POINT('Ctrl Pts',(50.9355365677156,-69.9417092155658,
-218.35005));
#210946=CARTESIAN_POINT('Ctrl Pts',(51.7355619650149,-70.1572933992548,
-218.35005));
#210947=CARTESIAN_POINT('Ctrl Pts',(52.3440043138886,-69.5948744409349,
-218.35005));
#210948=CARTESIAN_POINT('Ctrl Pts',(50.9355365677156,-69.9417092155658,
-217.60005));
#210949=CARTESIAN_POINT('Ctrl Pts',(51.7355619650149,-70.1572933992548,
-217.60005));
#210950=CARTESIAN_POINT('Ctrl Pts',(52.3440043138886,-69.5948744409349,
-217.60005));
#210951=CARTESIAN_POINT('',(51.1306793331593,-69.2175412094409,-218.35005));
#210952=CARTESIAN_POINT('Origin',(51.325822098603,-68.4933732033159,-218.35005));
#210953=CARTESIAN_POINT('',(50.9355365677156,-69.9417092155658,-217.60005));
#210954=CARTESIAN_POINT('Origin',(51.325822098603,-68.4933732033159,-217.60005));
#210955=CARTESIAN_POINT('Origin',(51.1306793331593,-69.2175412094409,-217.60005));
#210956=CARTESIAN_POINT('Origin',(-10.6701281871898,-52.5639741032288,-217.60005));
#210957=CARTESIAN_POINT('',(48.0054978778587,-68.3753933286417,-218.35005));
#210958=CARTESIAN_POINT('',(50.9355365677156,-69.9417092155658,-217.60005));
#210959=CARTESIAN_POINT('Origin',(3.09688044790867,-9.95712216328114,-227.60005));
#210960=CARTESIAN_POINT('',(53.6770468827139,-61.5062120042031,-228.35005));
#210961=CARTESIAN_POINT('',(3.09688044790867,-9.95712216328114,-228.35005));
#210962=CARTESIAN_POINT('',(54.2123842387114,-60.9809369188682,-227.60005));
#210963=CARTESIAN_POINT('',(55.2047656166361,-61.9923285455256,-227.60005));
#210964=CARTESIAN_POINT('Origin',(53.6770468827139,-61.5062120042031,-227.60005));
#210965=CARTESIAN_POINT('Ctrl Pts',(53.6916490178651,-62.5414543003222,
-228.35005));
#210966=CARTESIAN_POINT('Ctrl Pts',(54.1781051950386,-62.0168686860244,
-228.35005));
#210967=CARTESIAN_POINT('Ctrl Pts',(53.6770468827138,-61.5062120042031,
-228.35005));
#210968=CARTESIAN_POINT('Ctrl Pts',(54.2415885090139,-63.0514215111064,
-228.35005));
#210969=CARTESIAN_POINT('Ctrl Pts',(55.2145008633609,-62.0022502825108,
-228.35005));
#210970=CARTESIAN_POINT('Ctrl Pts',(54.2123842387114,-60.9809369188682,
-228.35005));
#210971=CARTESIAN_POINT('Ctrl Pts',(54.2415885090139,-63.0514215111064,
-227.60005));
#210972=CARTESIAN_POINT('Ctrl Pts',(55.2145008633609,-62.0022502825108,
-227.60005));
#210973=CARTESIAN_POINT('Ctrl Pts',(54.2123842387114,-60.9809369188682,
-227.60005));
#210974=CARTESIAN_POINT('',(54.2415885090138,-63.0514215111064,-227.60005));
#210975=CARTESIAN_POINT('',(53.6916490178651,-62.5414543003222,-228.35005));
#210976=CARTESIAN_POINT('Origin',(53.6916490178651,-62.5414543003222,-227.60005));
#210977=CARTESIAN_POINT('Origin',(53.1417095267163,-62.031487089538,-228.35005));
#210978=CARTESIAN_POINT('Origin',(53.1417095267163,-62.031487089538,-227.60005));
#210979=CARTESIAN_POINT('Origin',(0.127542579976414,-12.8706479699377,-227.60005));
#210980=CARTESIAN_POINT('',(49.2725916132775,-67.9270204940557,-227.60005));
#210981=CARTESIAN_POINT('',(48.7731500580611,-67.3675045131195,-228.35005));
#210982=CARTESIAN_POINT('Origin',(48.7731500580611,-67.3675045131195,-227.60005));
#210983=CARTESIAN_POINT('Origin',(0.127542579976414,-12.8706479699377,-228.35005));
#210984=CARTESIAN_POINT('Origin',(0.127542579976414,-12.8706479699377,-227.60005));
#210985=CARTESIAN_POINT('Ctrl Pts',(47.738371146847,-67.3332636175182,-228.35005));
#210986=CARTESIAN_POINT('Ctrl Pts',(48.2394294591717,-67.8439202993396,
-228.35005));
#210987=CARTESIAN_POINT('Ctrl Pts',(48.7731500580611,-67.3675045131195,
-228.35005));
#210988=CARTESIAN_POINT('Ctrl Pts',(47.2030337908494,-67.858538702853,-228.35005));
#210989=CARTESIAN_POINT('Ctrl Pts',(48.2051504154989,-68.8798520664959,
-228.35005));
#210990=CARTESIAN_POINT('Ctrl Pts',(49.2725916132776,-67.9270204940556,
-228.35005));
#210991=CARTESIAN_POINT('Ctrl Pts',(47.2030337908494,-67.858538702853,-227.60005));
#210992=CARTESIAN_POINT('Ctrl Pts',(48.2051504154989,-68.8798520664959,
-227.60005));
#210993=CARTESIAN_POINT('Ctrl Pts',(49.2725916132776,-67.9270204940556,
-227.60005));
#210994=CARTESIAN_POINT('',(47.738371146847,-67.3332636175182,-228.35005));
#210995=CARTESIAN_POINT('Origin',(48.2737085028446,-66.8079885321834,-228.35005));
#210996=CARTESIAN_POINT('',(47.2030337908494,-67.858538702853,-227.60005));
#210997=CARTESIAN_POINT('Origin',(48.2737085028446,-66.8079885321834,-227.60005));
#210998=CARTESIAN_POINT('Origin',(47.738371146847,-67.3332636175182,-227.60005));
#210999=CARTESIAN_POINT('Origin',(-2.84179528795572,-15.7841737765938,-227.60005));
#211000=CARTESIAN_POINT('',(48.1954151687739,-68.8699303295103,-227.60005));
#211001=CARTESIAN_POINT('',(-2.84179528795573,-15.7841737765938,-228.35005));
#211002=CARTESIAN_POINT('Origin',(55.2624668079327,38.6418244200972,-167.906149834141));
#211003=CARTESIAN_POINT('',(56.3587426896623,39.6656306474361,-167.906149834141));
#211004=CARTESIAN_POINT('',(56.7127812850717,38.2589564044561,-167.906149834141));
#211005=CARTESIAN_POINT('Origin',(51.1992016385053,42.6751487167426,-167.906149834141));
#211006=CARTESIAN_POINT('',(52.2148720050704,43.7789665035542,-167.906149834141));
#211007=CARTESIAN_POINT('',(50.8056178277775,44.1225919052419,-167.906149834141));
#211008=CARTESIAN_POINT('Origin',(53.5250845842796,36.1092498321983,-228.35005));
#211009=CARTESIAN_POINT('',(54.6328983814091,37.1205601658197,-228.35005));
#211010=CARTESIAN_POINT('',(54.5875190481084,35.0503669255136,-228.35005));
#211011=CARTESIAN_POINT('Origin',(48.6945492220708,40.9236374479242,-228.35005));
#211012=CARTESIAN_POINT('',(47.632114758242,41.9825203546087,-228.35005));
#211013=CARTESIAN_POINT('',(49.7021444432209,42.0348313420379,-228.35005));
#211014=CARTESIAN_POINT('Origin',(53.1417095267163,-62.031487089538,-228.35005));
#211015=CARTESIAN_POINT('',(54.2123842387114,-60.9809369188682,-228.35005));
#211016=CARTESIAN_POINT('',(54.2415885090138,-63.0514215111064,-228.35005));
#211017=CARTESIAN_POINT('Origin',(48.2737085028446,-66.8079885321834,-228.35005));
#211018=CARTESIAN_POINT('',(49.2725916132775,-67.9270204940557,-228.35005));
#211019=CARTESIAN_POINT('',(47.2030337908494,-67.858538702853,-228.35005));
#211020=CARTESIAN_POINT('Origin',(51.325822098603,-68.4933732033159,-167.906149834141));
#211021=CARTESIAN_POINT('',(50.9355365677156,-69.9417092155658,-167.906149834141));
#211022=CARTESIAN_POINT('',(52.3440043138885,-69.594874440935,-167.906149834141));
#211023=CARTESIAN_POINT('Origin',(55.3798888598704,-64.4508033011153,-167.906149834141));
#211024=CARTESIAN_POINT('',(56.478494115784,-65.4721095684411,-167.906149834141));
#211025=CARTESIAN_POINT('',(56.8293274051384,-64.0646324794683,-167.906149834141));
#211026=CARTESIAN_POINT('Origin',(21.5,29.0311209585238,-234.90005));
#211027=CARTESIAN_POINT('',(21.6266284449832,30.2244211038859,-235.35005));
#211028=CARTESIAN_POINT('',(20.3,29.0311209585238,-235.35005));
#211029=CARTESIAN_POINT('Origin',(21.5,29.0311209585238,-235.35005));
#211030=CARTESIAN_POINT('',(21.5791427781145,29.7769335493751,-234.90005));
#211031=CARTESIAN_POINT('Origin',(21.6266284449832,30.2244211038859,-234.90005));
#211032=CARTESIAN_POINT('',(20.75,29.0311209585238,-234.90005));
#211033=CARTESIAN_POINT('Origin',(21.5,29.0311209585238,-234.90005));
#211034=CARTESIAN_POINT('Origin',(20.3,29.0311209585238,-234.90005));
#211035=CARTESIAN_POINT('Origin',(20.3,-25.4138432731711,-234.90005));
#211036=CARTESIAN_POINT('',(20.75,21.5631368321642,-234.90005));
#211037=CARTESIAN_POINT('',(20.3,21.5631368321642,-235.35005));
#211038=CARTESIAN_POINT('Origin',(20.3,21.5631368321642,-234.90005));
#211039=CARTESIAN_POINT('',(20.3,21.5631368321642,-235.35005));
#211040=CARTESIAN_POINT('',(20.75,29.0311209585238,-234.90005));
#211041=CARTESIAN_POINT('Origin',(-2.61456814389029E-14,-173.57701443073,
-234.90005));
#211042=CARTESIAN_POINT('',(25.0152849219089,29.8362882417925,-235.35005));
#211043=CARTESIAN_POINT('',(24.960358769668,29.3896529120211,-234.90005));
#211044=CARTESIAN_POINT('Origin',(25.0152849219089,29.8362882417925,-234.90005));
#211045=CARTESIAN_POINT('Origin',(-2.61456814389029E-14,-173.57701443073,
-234.90005));
#211046=CARTESIAN_POINT('Origin',(-2.61456814389029E-14,-173.57701443073,
-235.35005));
#211047=CARTESIAN_POINT('Origin',(21.5,21.5631368321642,-234.90005));
#211048=CARTESIAN_POINT('',(21.5,20.8131368321642,-234.90005));
#211049=CARTESIAN_POINT('',(21.5,20.3631368321642,-235.35005));
#211050=CARTESIAN_POINT('Origin',(21.5,20.3631368321642,-234.90005));
#211051=CARTESIAN_POINT('Origin',(21.5,21.5631368321642,-235.35005));
#211052=CARTESIAN_POINT('Origin',(21.5,21.5631368321642,-234.90005));
#211053=CARTESIAN_POINT('Origin',(24.838300653577,28.3971299569735,-234.90005));
#211054=CARTESIAN_POINT('',(25.604588652464,29.6281062779325,-235.35005));
#211055=CARTESIAN_POINT('',(25.366775135568,29.2460791438418,-234.90005));
#211056=CARTESIAN_POINT('Origin',(25.604588652464,29.6281062779325,-234.90005));
#211057=CARTESIAN_POINT('Origin',(24.838300653577,28.3971299569735,-234.90005));
#211058=CARTESIAN_POINT('Origin',(24.838300653577,28.3971299569735,-235.35005));
#211059=CARTESIAN_POINT('Origin',(-296.501483394397,20.3631368321642,-234.90005));
#211060=CARTESIAN_POINT('',(29.125,20.8131368321642,-234.90005));
#211061=CARTESIAN_POINT('',(29.125,20.3631368321642,-235.35005));
#211062=CARTESIAN_POINT('Origin',(29.125,20.3631368321642,-234.90005));
#211063=CARTESIAN_POINT('',(-296.501483394397,20.3631368321642,-235.35005));
#211064=CARTESIAN_POINT('',(-1.23757166668304E-15,20.8131368321642,-234.90005));
#211065=CARTESIAN_POINT('Origin',(-6.29739814579425E-15,-11.5034818258363,
-234.90005));
#211066=CARTESIAN_POINT('',(29.8646825396825,26.6475763089516,-235.35005));
#211067=CARTESIAN_POINT('',(29.5873015873016,26.2932321157492,-234.90005));
#211068=CARTESIAN_POINT('Origin',(29.8646825396825,26.6475763089516,-234.90005));
#211069=CARTESIAN_POINT('Origin',(-6.29739814579425E-15,-11.5034818258363,
-234.90005));
#211070=CARTESIAN_POINT('Origin',(-6.29739814579425E-15,-11.5034818258363,
-235.35005));
#211071=CARTESIAN_POINT('Origin',(29.125,21.5631368321642,-234.90005));
#211072=CARTESIAN_POINT('',(29.875,21.5631368321642,-234.90005));
#211073=CARTESIAN_POINT('',(30.325,21.5631368321642,-235.35005));
#211074=CARTESIAN_POINT('Origin',(30.325,21.5631368321642,-234.90005));
#211075=CARTESIAN_POINT('Origin',(29.125,21.5631368321642,-235.35005));
#211076=CARTESIAN_POINT('Origin',(29.125,21.5631368321642,-234.90005));
#211077=CARTESIAN_POINT('Origin',(29.125,25.702658460412,-234.90005));
#211078=CARTESIAN_POINT('',(30.325,25.702658460412,-235.35005));
#211079=CARTESIAN_POINT('',(29.875,25.702658460412,-234.90005));
#211080=CARTESIAN_POINT('Origin',(30.325,25.702658460412,-234.90005));
#211081=CARTESIAN_POINT('Origin',(29.125,25.702658460412,-234.90005));
#211082=CARTESIAN_POINT('Origin',(29.125,25.702658460412,-235.35005));
#211083=CARTESIAN_POINT('Origin',(30.325,-25.4138432731711,-234.90005));
#211084=CARTESIAN_POINT('',(29.875,21.5631368321642,-234.90005));
#211085=CARTESIAN_POINT('',(30.325,25.702658460412,-235.35005));
#211086=CARTESIAN_POINT('Origin',(11.3749999999999,29.8508988479304,-234.90005));
#211087=CARTESIAN_POINT('',(11.4419952819386,31.0490272351235,-235.35005));
#211088=CARTESIAN_POINT('',(10.1749999999999,29.8508988479304,-235.35005));
#211089=CARTESIAN_POINT('Origin',(11.3749999999999,29.8508988479304,-235.35005));
#211090=CARTESIAN_POINT('',(11.4168720512116,30.5997290899261,-234.90005));
#211091=CARTESIAN_POINT('Origin',(11.4419952819386,31.0490272351235,-234.90005));
#211092=CARTESIAN_POINT('',(10.6249999999999,29.8508988479304,-234.90005));
#211093=CARTESIAN_POINT('Origin',(11.3749999999999,29.8508988479304,-234.90005));
#211094=CARTESIAN_POINT('Origin',(10.1749999999999,29.8508988479304,-234.90005));
#211095=CARTESIAN_POINT('Origin',(10.1749999999999,-25.4138432731711,-234.90005));
#211096=CARTESIAN_POINT('',(10.6249999999999,21.5631368321642,-234.90005));
#211097=CARTESIAN_POINT('',(10.1749999999999,21.5631368321642,-235.35005));
#211098=CARTESIAN_POINT('Origin',(10.1749999999999,21.5631368321642,-234.90005));
#211099=CARTESIAN_POINT('',(10.1749999999999,21.5631368321642,-235.35005));
#211100=CARTESIAN_POINT('',(10.6249999999999,29.8508988479304,-234.90005));
#211101=CARTESIAN_POINT('Origin',(-2.61456814389029E-14,-173.57701443073,
-234.90005));
#211102=CARTESIAN_POINT('',(19.1119042071944,30.4756045219376,-235.35005));
#211103=CARTESIAN_POINT('',(19.0699401294965,30.0275654430807,-234.90005));
#211104=CARTESIAN_POINT('Origin',(19.1119042071944,30.4756045219376,-234.90005));
#211105=CARTESIAN_POINT('Origin',(-2.61456814389029E-14,-173.57701443073,
-234.90005));
#211106=CARTESIAN_POINT('Origin',(-2.61456814389029E-14,-173.57701443073,
-235.35005));
#211107=CARTESIAN_POINT('Origin',(11.3749999999999,21.5631368321642,-234.90005));
#211108=CARTESIAN_POINT('',(11.3749999999999,20.8131368321642,-234.90005));
#211109=CARTESIAN_POINT('',(11.3749999999999,20.3631368321642,-235.35005));
#211110=CARTESIAN_POINT('Origin',(11.3749999999999,20.3631368321642,-234.90005));
#211111=CARTESIAN_POINT('Origin',(11.3749999999999,21.5631368321642,-235.35005));
#211112=CARTESIAN_POINT('Origin',(11.3749999999999,21.5631368321642,-234.90005));
#211113=CARTESIAN_POINT('Origin',(19.,29.2808336449858,-234.90005));
#211114=CARTESIAN_POINT('',(20.2,29.2808336449858,-235.35005));
#211115=CARTESIAN_POINT('',(19.75,29.2808336449858,-234.90005));
#211116=CARTESIAN_POINT('Origin',(20.2,29.2808336449858,-234.90005));
#211117=CARTESIAN_POINT('Origin',(19.,29.2808336449858,-234.90005));
#211118=CARTESIAN_POINT('Origin',(19.,29.2808336449858,-235.35005));
#211119=CARTESIAN_POINT('Origin',(-296.501483394397,20.3631368321642,-234.90005));
#211120=CARTESIAN_POINT('',(19.,20.8131368321642,-234.90005));
#211121=CARTESIAN_POINT('',(19.,20.3631368321642,-235.35005));
#211122=CARTESIAN_POINT('Origin',(19.,20.3631368321642,-234.90005));
#211123=CARTESIAN_POINT('',(-296.501483394397,20.3631368321642,-235.35005));
#211124=CARTESIAN_POINT('',(-1.23757166668304E-15,20.8131368321642,-234.90005));
#211125=CARTESIAN_POINT('Origin',(20.2,-25.4138432731711,-234.90005));
#211126=CARTESIAN_POINT('',(20.2,21.5631368321642,-235.35005));
#211127=CARTESIAN_POINT('',(19.75,21.5631368321642,-234.90005));
#211128=CARTESIAN_POINT('Origin',(20.2,21.5631368321642,-234.90005));
#211129=CARTESIAN_POINT('',(19.75,21.5631368321642,-234.90005));
#211130=CARTESIAN_POINT('',(20.2,29.2808336449858,-235.35005));
#211131=CARTESIAN_POINT('Origin',(19.,21.5631368321642,-234.90005));
#211132=CARTESIAN_POINT('Origin',(19.,21.5631368321642,-234.90005));
#211133=CARTESIAN_POINT('Origin',(19.,21.5631368321642,-235.35005));
#211134=CARTESIAN_POINT('Origin',(1.25,30.1648419118246,-234.90005));
#211135=CARTESIAN_POINT('',(1.25736211889437,31.3648193279477,-235.35005));
#211136=CARTESIAN_POINT('',(0.0499999999999979,30.1648419118246,-235.35005));
#211137=CARTESIAN_POINT('Origin',(1.25,30.1648419118246,-235.35005));
#211138=CARTESIAN_POINT('',(1.25460132430898,30.9148277969016,-234.90005));
#211139=CARTESIAN_POINT('Origin',(1.25736211889437,31.3648193279477,-234.90005));
#211140=CARTESIAN_POINT('',(0.5,30.1648419118246,-234.90005));
#211141=CARTESIAN_POINT('Origin',(1.25,30.1648419118246,-234.90005));
#211142=CARTESIAN_POINT('Origin',(0.05,30.1648419118246,-234.90005));
#211143=CARTESIAN_POINT('Origin',(0.0499999999999945,-25.4138432731711,
-234.90005));
#211144=CARTESIAN_POINT('',(0.5,21.5631368321642,-234.90005));
#211145=CARTESIAN_POINT('',(0.0499999999999974,21.5631368321642,-235.35005));
#211146=CARTESIAN_POINT('Origin',(0.05,21.5631368321642,-234.90005));
#211147=CARTESIAN_POINT('',(0.0499999999999974,21.5631368321642,-235.35005));
#211148=CARTESIAN_POINT('',(0.5,30.1648419118246,-234.90005));
#211149=CARTESIAN_POINT('Origin',(-2.61456814389029E-14,-173.57701443073,
-234.90005));
#211150=CARTESIAN_POINT('',(8.9272710441499,31.1741516601419,-235.35005));
#211151=CARTESIAN_POINT('',(8.90766940259363,30.7245787787886,-234.90005));
#211152=CARTESIAN_POINT('Origin',(8.9272710441499,31.1741516601419,-234.90005));
#211153=CARTESIAN_POINT('Origin',(-2.61456814389029E-14,-173.57701443073,
-234.90005));
#211154=CARTESIAN_POINT('Origin',(-2.61456814389029E-14,-173.57701443073,
-235.35005));
#211155=CARTESIAN_POINT('Origin',(1.25,21.5631368321642,-234.90005));
#211156=CARTESIAN_POINT('',(1.25,20.8131368321642,-234.90005));
#211157=CARTESIAN_POINT('',(1.25,20.3631368321642,-235.35005));
#211158=CARTESIAN_POINT('Origin',(1.25,20.3631368321642,-234.90005));
#211159=CARTESIAN_POINT('Origin',(1.25,21.5631368321642,-235.35005));
#211160=CARTESIAN_POINT('Origin',(1.25,21.5631368321642,-234.90005));
#211161=CARTESIAN_POINT('Origin',(8.87499999999986,29.9752906431998,-234.90005));
#211162=CARTESIAN_POINT('',(10.075,29.9752906431998,-235.35005));
#211163=CARTESIAN_POINT('',(9.62499999999986,29.9752906431998,-234.90005));
#211164=CARTESIAN_POINT('Origin',(10.075,29.9752906431998,-234.90005));
#211165=CARTESIAN_POINT('Origin',(8.87499999999986,29.9752906431998,-234.90005));
#211166=CARTESIAN_POINT('Origin',(8.87499999999986,29.9752906431998,-235.35005));
#211167=CARTESIAN_POINT('Origin',(-296.501483394397,20.3631368321642,-234.90005));
#211168=CARTESIAN_POINT('',(8.87499999999986,20.8131368321642,-234.90005));
#211169=CARTESIAN_POINT('',(8.87499999999986,20.3631368321642,-235.35005));
#211170=CARTESIAN_POINT('Origin',(8.87499999999986,20.3631368321642,-234.90005));
#211171=CARTESIAN_POINT('',(-296.501483394397,20.3631368321642,-235.35005));
#211172=CARTESIAN_POINT('',(-1.23757166668304E-15,20.8131368321642,-234.90005));
#211173=CARTESIAN_POINT('Origin',(10.075,-25.4138432731712,-234.90005));
#211174=CARTESIAN_POINT('',(10.0749999999999,21.5631368321642,-235.35005));
#211175=CARTESIAN_POINT('',(9.62499999999986,21.5631368321642,-234.90005));
#211176=CARTESIAN_POINT('Origin',(10.0749999999999,21.5631368321642,-234.90005));
#211177=CARTESIAN_POINT('',(9.62499999999986,21.5631368321642,-234.90005));
#211178=CARTESIAN_POINT('',(10.075,29.9752906431998,-235.35005));
#211179=CARTESIAN_POINT('Origin',(8.87499999999986,21.5631368321642,-234.90005));
#211180=CARTESIAN_POINT('Origin',(8.87499999999986,21.5631368321642,-234.90005));
#211181=CARTESIAN_POINT('Origin',(8.87499999999986,21.5631368321642,-235.35005));
#211182=CARTESIAN_POINT('Origin',(1.25,19.0631368321642,-234.90005));
#211183=CARTESIAN_POINT('',(1.25,20.2631368321642,-235.35005));
#211184=CARTESIAN_POINT('',(1.25,19.8131368321642,-234.90005));
#211185=CARTESIAN_POINT('Origin',(1.25,20.2631368321642,-234.90005));
#211186=CARTESIAN_POINT('',(0.5,19.0631368321642,-234.90005));
#211187=CARTESIAN_POINT('Origin',(1.25,19.0631368321642,-234.90005));
#211188=CARTESIAN_POINT('',(0.0499999999999972,19.0631368321642,-235.35005));
#211189=CARTESIAN_POINT('Origin',(0.0499999999999994,19.0631368321642,-234.90005));
#211190=CARTESIAN_POINT('Origin',(1.25,19.0631368321642,-235.35005));
#211191=CARTESIAN_POINT('Origin',(0.0499999999999945,-25.4138432731711,
-234.90005));
#211192=CARTESIAN_POINT('',(0.5,10.9575972794973,-234.90005));
#211193=CARTESIAN_POINT('',(0.0499999999999967,10.9575972794973,-235.35005));
#211194=CARTESIAN_POINT('Origin',(0.0499999999999989,10.9575972794973,-234.90005));
#211195=CARTESIAN_POINT('',(0.0499999999999967,10.9575972794973,-235.35005));
#211196=CARTESIAN_POINT('',(0.5,19.0631368321642,-234.90005));
#211197=CARTESIAN_POINT('Origin',(-296.501483394397,20.2631368321643,-234.90005));
#211198=CARTESIAN_POINT('',(8.87499999999986,20.2631368321642,-235.35005));
#211199=CARTESIAN_POINT('',(8.87499999999986,19.8131368321642,-234.90005));
#211200=CARTESIAN_POINT('Origin',(8.87499999999986,20.2631368321642,-234.90005));
#211201=CARTESIAN_POINT('',(-1.54373336646988E-15,19.8131368321642,-234.90005));
#211202=CARTESIAN_POINT('',(-296.501483394397,20.2631368321643,-235.35005));
#211203=CARTESIAN_POINT('Origin',(1.25,10.9575972794973,-234.90005));
#211204=CARTESIAN_POINT('',(1.25,10.2075972794973,-234.90005));
#211205=CARTESIAN_POINT('',(1.25,9.75759727949733,-235.35005));
#211206=CARTESIAN_POINT('Origin',(1.25,9.75759727949733,-234.90005));
#211207=CARTESIAN_POINT('Origin',(1.25,10.9575972794973,-235.35005));
#211208=CARTESIAN_POINT('Origin',(1.25,10.9575972794973,-234.90005));
#211209=CARTESIAN_POINT('Origin',(8.87499999999986,19.0631368321642,-234.90005));
#211210=CARTESIAN_POINT('',(10.075,19.0631368321642,-235.35005));
#211211=CARTESIAN_POINT('',(9.62499999999986,19.0631368321642,-234.90005));
#211212=CARTESIAN_POINT('Origin',(10.075,19.0631368321642,-234.90005));
#211213=CARTESIAN_POINT('Origin',(8.87499999999986,19.0631368321642,-234.90005));
#211214=CARTESIAN_POINT('Origin',(8.87499999999986,19.0631368321642,-235.35005));
#211215=CARTESIAN_POINT('Origin',(-296.501483394397,9.75759727949737,-234.90005));
#211216=CARTESIAN_POINT('',(8.87499999999986,10.2075972794973,-234.90005));
#211217=CARTESIAN_POINT('',(8.87499999999986,9.75759727949733,-235.35005));
#211218=CARTESIAN_POINT('Origin',(8.87499999999986,9.75759727949733,-234.90005));
#211219=CARTESIAN_POINT('',(-296.501483394397,9.75759727949736,-235.35005));
#211220=CARTESIAN_POINT('',(-2.53637567332344E-15,10.2075972794973,-234.90005));
#211221=CARTESIAN_POINT('Origin',(10.075,-25.4138432731712,-234.90005));
#211222=CARTESIAN_POINT('',(10.0749999999998,10.9575972794973,-235.35005));
#211223=CARTESIAN_POINT('',(9.62499999999986,10.9575972794973,-234.90005));
#211224=CARTESIAN_POINT('Origin',(10.0749999999998,10.9575972794973,-234.90005));
#211225=CARTESIAN_POINT('',(9.62499999999986,10.9575972794973,-234.90005));
#211226=CARTESIAN_POINT('',(10.075,19.0631368321642,-235.35005));
#211227=CARTESIAN_POINT('Origin',(8.87499999999986,10.9575972794973,-234.90005));
#211228=CARTESIAN_POINT('Origin',(8.87499999999986,10.9575972794973,-234.90005));
#211229=CARTESIAN_POINT('Origin',(8.87499999999986,10.9575972794973,-235.35005));
#211230=CARTESIAN_POINT('Origin',(1.25,8.45759727949731,-234.90005));
#211231=CARTESIAN_POINT('',(1.25,9.65759727949731,-235.35005));
#211232=CARTESIAN_POINT('',(1.25,9.20759727949731,-234.90005));
#211233=CARTESIAN_POINT('Origin',(1.25,9.65759727949731,-234.90005));
#211234=CARTESIAN_POINT('',(0.5,8.45759727949731,-234.90005));
#211235=CARTESIAN_POINT('Origin',(1.25,8.45759727949731,-234.90005));
#211236=CARTESIAN_POINT('',(0.0499999999999966,8.45759727949731,-235.35005));
#211237=CARTESIAN_POINT('Origin',(0.0499999999999987,8.45759727949731,-234.90005));
#211238=CARTESIAN_POINT('Origin',(1.25,8.45759727949731,-235.35005));
#211239=CARTESIAN_POINT('Origin',(0.0499999999999945,-25.4138432731711,
-234.90005));
#211240=CARTESIAN_POINT('',(0.5,2.29555713691451,-234.90005));
#211241=CARTESIAN_POINT('',(0.0499999999999962,2.29555713691451,-235.35005));
#211242=CARTESIAN_POINT('Origin',(0.0499999999999985,2.29555713691451,-234.90005));
#211243=CARTESIAN_POINT('',(0.0499999999999962,2.29555713691451,-235.35005));
#211244=CARTESIAN_POINT('',(0.5,8.45759727949731,-234.90005));
#211245=CARTESIAN_POINT('Origin',(-296.501483394397,9.65759727949727,-234.90005));
#211246=CARTESIAN_POINT('',(8.87499999999986,9.65759727949731,-235.35005));
#211247=CARTESIAN_POINT('',(8.87499999999986,9.20759727949731,-234.90005));
#211248=CARTESIAN_POINT('Origin',(8.87499999999986,9.65759727949731,-234.90005));
#211249=CARTESIAN_POINT('',(-2.8425373731103E-15,9.20759727949731,-234.90005));
#211250=CARTESIAN_POINT('',(-296.501483394397,9.65759727949727,-235.35005));
#211251=CARTESIAN_POINT('Origin',(1.25,2.29555713691451,-234.90005));
#211252=CARTESIAN_POINT('',(1.18233753211584,1.54861551239502,-234.90005));
#211253=CARTESIAN_POINT('',(1.14174005138535,1.10045053768332,-235.35005));
#211254=CARTESIAN_POINT('Origin',(1.14174005138535,1.10045053768332,-234.90005));
#211255=CARTESIAN_POINT('Origin',(1.25,2.29555713691451,-235.35005));
#211256=CARTESIAN_POINT('Origin',(1.25,2.29555713691451,-234.90005));
#211257=CARTESIAN_POINT('Origin',(8.87499999999986,8.45759727949731,-234.90005));
#211258=CARTESIAN_POINT('',(10.075,8.45759727949731,-235.35005));
#211259=CARTESIAN_POINT('',(9.62499999999986,8.45759727949731,-234.90005));
#211260=CARTESIAN_POINT('Origin',(10.075,8.45759727949731,-234.90005));
#211261=CARTESIAN_POINT('Origin',(8.87499999999986,8.45759727949731,-234.90005));
#211262=CARTESIAN_POINT('Origin',(8.87499999999986,8.45759727949731,-235.35005));
#211263=CARTESIAN_POINT('Origin',(0.,-11.5034818258363,-234.90005));
#211264=CARTESIAN_POINT('',(5.33358654455957,0.46765101689032,-234.90005));
#211265=CARTESIAN_POINT('',(5.1504491822704,0.0566027149430096,-235.35005));
#211266=CARTESIAN_POINT('Origin',(5.1504491822704,0.0566027149430111,-234.90005));
#211267=CARTESIAN_POINT('Origin',(0.,-11.5034818258363,-235.35005));
#211268=CARTESIAN_POINT('Origin',(0.,-11.5034818258363,-234.90005));
#211269=CARTESIAN_POINT('Origin',(10.075,-25.4138432731712,-234.90005));
#211270=CARTESIAN_POINT('',(10.0749999999998,0.367156910880383,-235.35005));
#211271=CARTESIAN_POINT('',(9.62499999999985,0.367156910880383,-234.90005));
#211272=CARTESIAN_POINT('Origin',(10.0749999999998,0.367156910880383,-234.90005));
#211273=CARTESIAN_POINT('',(9.62499999999985,0.367156910880385,-234.90005));
#211274=CARTESIAN_POINT('',(10.075,8.45759727949732,-235.35005));
#211275=CARTESIAN_POINT('Origin',(9.40330570654115,9.60205772683049,-234.90005));
#211276=CARTESIAN_POINT('',(8.83216440217218,-0.38161883095341,-234.90005));
#211277=CARTESIAN_POINT('',(8.80646304347558,-0.830884276053686,-235.35005));
#211278=CARTESIAN_POINT('Origin',(8.80646304347558,-0.830884276053684,-234.90005));
#211279=CARTESIAN_POINT('Origin',(9.40330570654115,9.60205772683049,-235.35005));
#211280=CARTESIAN_POINT('Origin',(9.40330570654115,9.60205772683049,-234.90005));
#211281=CARTESIAN_POINT('Origin',(8.87499999999985,0.367156910880384,-234.90005));
#211282=CARTESIAN_POINT('Origin',(8.87499999999985,0.367156910880384,-235.35005));
#211283=CARTESIAN_POINT('Origin',(8.87499999999985,0.367156910880384,-234.90005));
#211284=CARTESIAN_POINT('Origin',(11.3749999999999,8.45759727949731,-234.90005));
#211285=CARTESIAN_POINT('',(11.3749999999999,9.65759727949731,-235.35005));
#211286=CARTESIAN_POINT('',(11.3749999999999,9.20759727949731,-234.90005));
#211287=CARTESIAN_POINT('Origin',(11.3749999999999,9.65759727949731,-234.90005));
#211288=CARTESIAN_POINT('',(10.6249999999999,8.45759727949731,-234.90005));
#211289=CARTESIAN_POINT('Origin',(11.3749999999999,8.45759727949731,-234.90005));
#211290=CARTESIAN_POINT('',(10.1749999999999,8.45759727949731,-235.35005));
#211291=CARTESIAN_POINT('Origin',(10.1749999999999,8.45759727949731,-234.90005));
#211292=CARTESIAN_POINT('Origin',(11.3749999999999,8.45759727949731,-235.35005));
#211293=CARTESIAN_POINT('Origin',(10.1749999999999,-25.4138432731711,-234.90005));
#211294=CARTESIAN_POINT('',(10.6249999999999,0.352057726830487,-234.90005));
#211295=CARTESIAN_POINT('',(10.1749999999999,0.352057726830488,-235.35005));
#211296=CARTESIAN_POINT('Origin',(10.1749999999999,0.352057726830487,-234.90005));
#211297=CARTESIAN_POINT('',(10.1749999999999,0.352057726830487,-235.35005));
#211298=CARTESIAN_POINT('',(10.6249999999999,8.45759727949731,-234.90005));
#211299=CARTESIAN_POINT('Origin',(-296.501483394397,9.65759727949727,-234.90005));
#211300=CARTESIAN_POINT('',(19.,9.65759727949731,-235.35005));
#211301=CARTESIAN_POINT('',(19.,9.20759727949731,-234.90005));
#211302=CARTESIAN_POINT('Origin',(19.,9.65759727949731,-234.90005));
#211303=CARTESIAN_POINT('',(-2.8425373731103E-15,9.20759727949731,-234.90005));
#211304=CARTESIAN_POINT('',(-296.501483394397,9.65759727949727,-235.35005));
#211305=CARTESIAN_POINT('Origin',(11.3749999999999,0.352057726830487,-234.90005));
#211306=CARTESIAN_POINT('',(11.3749999999999,-0.397942273169513,-234.90005));
#211307=CARTESIAN_POINT('',(11.3749999999999,-0.847942273169513,-235.35005));
#211308=CARTESIAN_POINT('Origin',(11.3749999999999,-0.847942273169513,-234.90005));
#211309=CARTESIAN_POINT('Origin',(11.3749999999999,0.352057726830487,-235.35005));
#211310=CARTESIAN_POINT('Origin',(11.3749999999999,0.352057726830487,-234.90005));
#211311=CARTESIAN_POINT('Origin',(19.,8.45759727949731,-234.90005));
#211312=CARTESIAN_POINT('',(20.2,8.45759727949731,-235.35005));
#211313=CARTESIAN_POINT('',(19.75,8.45759727949731,-234.90005));
#211314=CARTESIAN_POINT('Origin',(20.2,8.45759727949731,-234.90005));
#211315=CARTESIAN_POINT('Origin',(19.,8.45759727949731,-234.90005));
#211316=CARTESIAN_POINT('Origin',(19.,8.45759727949731,-235.35005));
#211317=CARTESIAN_POINT('Origin',(-296.501483394397,-0.84794227316963,-234.90005));
#211318=CARTESIAN_POINT('',(19.,-0.39794227316951,-234.90005));
#211319=CARTESIAN_POINT('',(19.,-0.847942273169513,-235.35005));
#211320=CARTESIAN_POINT('Origin',(19.,-0.84794227316951,-234.90005));
#211321=CARTESIAN_POINT('',(-296.501483394397,-0.84794227316963,-235.35005));
#211322=CARTESIAN_POINT('',(-1.11087130309497E-13,-0.397942273169517,-234.90005));
#211323=CARTESIAN_POINT('Origin',(20.2,-25.4138432731711,-234.90005));
#211324=CARTESIAN_POINT('',(20.2,0.352057726830487,-235.35005));
#211325=CARTESIAN_POINT('',(19.75,0.352057726830487,-234.90005));
#211326=CARTESIAN_POINT('Origin',(20.2,0.352057726830487,-234.90005));
#211327=CARTESIAN_POINT('',(19.75,0.352057726830487,-234.90005));
#211328=CARTESIAN_POINT('',(20.2,8.45759727949731,-235.35005));
#211329=CARTESIAN_POINT('Origin',(19.,0.35205772683049,-234.90005));
#211330=CARTESIAN_POINT('Origin',(19.,0.35205772683049,-234.90005));
#211331=CARTESIAN_POINT('Origin',(19.,0.35205772683049,-235.35005));
#211332=CARTESIAN_POINT('Origin',(11.3749999999999,19.0631368321642,-234.90005));
#211333=CARTESIAN_POINT('',(11.3749999999999,20.2631368321642,-235.35005));
#211334=CARTESIAN_POINT('',(11.3749999999999,19.8131368321642,-234.90005));
#211335=CARTESIAN_POINT('Origin',(11.3749999999999,20.2631368321642,-234.90005));
#211336=CARTESIAN_POINT('',(10.6249999999999,19.0631368321642,-234.90005));
#211337=CARTESIAN_POINT('Origin',(11.3749999999999,19.0631368321642,-234.90005));
#211338=CARTESIAN_POINT('',(10.1749999999999,19.0631368321642,-235.35005));
#211339=CARTESIAN_POINT('Origin',(10.1749999999999,19.0631368321642,-234.90005));
#211340=CARTESIAN_POINT('Origin',(11.3749999999999,19.0631368321642,-235.35005));
#211341=CARTESIAN_POINT('Origin',(10.1749999999999,-25.4138432731711,-234.90005));
#211342=CARTESIAN_POINT('',(10.6249999999999,10.9575972794973,-234.90005));
#211343=CARTESIAN_POINT('',(10.1749999999999,10.9575972794973,-235.35005));
#211344=CARTESIAN_POINT('Origin',(10.1749999999999,10.9575972794973,-234.90005));
#211345=CARTESIAN_POINT('',(10.1749999999999,10.9575972794973,-235.35005));
#211346=CARTESIAN_POINT('',(10.6249999999999,19.0631368321642,-234.90005));
#211347=CARTESIAN_POINT('Origin',(-296.501483394397,20.2631368321643,-234.90005));
#211348=CARTESIAN_POINT('',(19.,20.2631368321642,-235.35005));
#211349=CARTESIAN_POINT('',(19.,19.8131368321642,-234.90005));
#211350=CARTESIAN_POINT('Origin',(19.,20.2631368321642,-234.90005));
#211351=CARTESIAN_POINT('',(-1.54373336646988E-15,19.8131368321642,-234.90005));
#211352=CARTESIAN_POINT('',(-296.501483394397,20.2631368321643,-235.35005));
#211353=CARTESIAN_POINT('Origin',(11.3749999999999,10.9575972794973,-234.90005));
#211354=CARTESIAN_POINT('',(11.3749999999999,10.2075972794973,-234.90005));
#211355=CARTESIAN_POINT('',(11.3749999999999,9.75759727949733,-235.35005));
#211356=CARTESIAN_POINT('Origin',(11.3749999999999,9.75759727949733,-234.90005));
#211357=CARTESIAN_POINT('Origin',(11.3749999999999,10.9575972794973,-235.35005));
#211358=CARTESIAN_POINT('Origin',(11.3749999999999,10.9575972794973,-234.90005));
#211359=CARTESIAN_POINT('Origin',(19.,19.0631368321642,-234.90005));
#211360=CARTESIAN_POINT('',(20.2,19.0631368321642,-235.35005));
#211361=CARTESIAN_POINT('',(19.75,19.0631368321642,-234.90005));
#211362=CARTESIAN_POINT('Origin',(20.2,19.0631368321642,-234.90005));
#211363=CARTESIAN_POINT('Origin',(19.,19.0631368321642,-234.90005));
#211364=CARTESIAN_POINT('Origin',(19.,19.0631368321642,-235.35005));
#211365=CARTESIAN_POINT('Origin',(-296.501483394397,9.75759727949737,-234.90005));
#211366=CARTESIAN_POINT('',(19.,10.2075972794973,-234.90005));
#211367=CARTESIAN_POINT('',(19.,9.75759727949733,-235.35005));
#211368=CARTESIAN_POINT('Origin',(19.,9.75759727949733,-234.90005));
#211369=CARTESIAN_POINT('',(-296.501483394397,9.75759727949737,-235.35005));
#211370=CARTESIAN_POINT('',(-2.53637567332344E-15,10.2075972794973,-234.90005));
#211371=CARTESIAN_POINT('Origin',(20.2,-25.4138432731711,-234.90005));
#211372=CARTESIAN_POINT('',(20.2,10.9575972794973,-235.35005));
#211373=CARTESIAN_POINT('',(19.75,10.9575972794973,-234.90005));
#211374=CARTESIAN_POINT('Origin',(20.2,10.9575972794973,-234.90005));
#211375=CARTESIAN_POINT('',(19.75,10.9575972794973,-234.90005));
#211376=CARTESIAN_POINT('',(20.2,19.0631368321642,-235.35005));
#211377=CARTESIAN_POINT('Origin',(19.,10.9575972794973,-234.90005));
#211378=CARTESIAN_POINT('Origin',(19.,10.9575972794973,-234.90005));
#211379=CARTESIAN_POINT('Origin',(19.,10.9575972794973,-235.35005));
#211380=CARTESIAN_POINT('Origin',(21.5,19.0631368321642,-234.90005));
#211381=CARTESIAN_POINT('',(21.5,20.2631368321642,-235.35005));
#211382=CARTESIAN_POINT('',(21.5,19.8131368321642,-234.90005));
#211383=CARTESIAN_POINT('Origin',(21.5,20.2631368321642,-234.90005));
#211384=CARTESIAN_POINT('',(20.75,19.0631368321642,-234.90005));
#211385=CARTESIAN_POINT('Origin',(21.5,19.0631368321642,-234.90005));
#211386=CARTESIAN_POINT('',(20.3,19.0631368321642,-235.35005));
#211387=CARTESIAN_POINT('Origin',(20.3,19.0631368321642,-234.90005));
#211388=CARTESIAN_POINT('Origin',(21.5,19.0631368321642,-235.35005));
#211389=CARTESIAN_POINT('Origin',(20.3,-25.4138432731711,-234.90005));
#211390=CARTESIAN_POINT('',(20.75,10.9575972794973,-234.90005));
#211391=CARTESIAN_POINT('',(20.3,10.9575972794973,-235.35005));
#211392=CARTESIAN_POINT('Origin',(20.3,10.9575972794973,-234.90005));
#211393=CARTESIAN_POINT('',(20.3,10.9575972794973,-235.35005));
#211394=CARTESIAN_POINT('',(20.75,19.0631368321642,-234.90005));
#211395=CARTESIAN_POINT('Origin',(-296.501483394397,20.2631368321643,-234.90005));
#211396=CARTESIAN_POINT('',(29.125,20.2631368321642,-235.35005));
#211397=CARTESIAN_POINT('',(29.125,19.8131368321642,-234.90005));
#211398=CARTESIAN_POINT('Origin',(29.125,20.2631368321642,-234.90005));
#211399=CARTESIAN_POINT('',(-1.54373336646988E-15,19.8131368321642,-234.90005));
#211400=CARTESIAN_POINT('',(-296.501483394397,20.2631368321643,-235.35005));
#211401=CARTESIAN_POINT('Origin',(21.5,10.9575972794973,-234.90005));
#211402=CARTESIAN_POINT('',(21.5,10.2075972794973,-234.90005));
#211403=CARTESIAN_POINT('',(21.5,9.75759727949733,-235.35005));
#211404=CARTESIAN_POINT('Origin',(21.5,9.75759727949733,-234.90005));
#211405=CARTESIAN_POINT('Origin',(21.5,10.9575972794973,-235.35005));
#211406=CARTESIAN_POINT('Origin',(21.5,10.9575972794973,-234.90005));
#211407=CARTESIAN_POINT('Origin',(29.125,19.0631368321642,-234.90005));
#211408=CARTESIAN_POINT('',(30.325,19.0631368321642,-235.35005));
#211409=CARTESIAN_POINT('',(29.875,19.0631368321642,-234.90005));
#211410=CARTESIAN_POINT('Origin',(30.325,19.0631368321642,-234.90005));
#211411=CARTESIAN_POINT('Origin',(29.125,19.0631368321642,-234.90005));
#211412=CARTESIAN_POINT('Origin',(29.125,19.0631368321642,-235.35005));
#211413=CARTESIAN_POINT('Origin',(-296.501483394397,9.75759727949737,-234.90005));
#211414=CARTESIAN_POINT('',(29.125,10.2075972794973,-234.90005));
#211415=CARTESIAN_POINT('',(29.125,9.75759727949733,-235.35005));
#211416=CARTESIAN_POINT('Origin',(29.125,9.75759727949733,-234.90005));
#211417=CARTESIAN_POINT('',(-296.501483394397,9.75759727949737,-235.35005));
#211418=CARTESIAN_POINT('',(-2.53637567332344E-15,10.2075972794973,-234.90005));
#211419=CARTESIAN_POINT('Origin',(30.325,-25.4138432731711,-234.90005));
#211420=CARTESIAN_POINT('',(30.325,10.9575972794973,-235.35005));
#211421=CARTESIAN_POINT('',(29.875,10.9575972794973,-234.90005));
#211422=CARTESIAN_POINT('Origin',(30.325,10.9575972794973,-234.90005));
#211423=CARTESIAN_POINT('',(29.875,10.9575972794973,-234.90005));
#211424=CARTESIAN_POINT('',(30.325,19.0631368321642,-235.35005));
#211425=CARTESIAN_POINT('Origin',(29.125,10.9575972794973,-234.90005));
#211426=CARTESIAN_POINT('Origin',(29.125,10.9575972794973,-234.90005));
#211427=CARTESIAN_POINT('Origin',(29.125,10.9575972794973,-235.35005));
#211428=CARTESIAN_POINT('Origin',(21.5,8.45759727949731,-234.90005));
#211429=CARTESIAN_POINT('',(21.5,9.65759727949731,-235.35005));
#211430=CARTESIAN_POINT('',(21.5,9.20759727949731,-234.90005));
#211431=CARTESIAN_POINT('Origin',(21.5,9.65759727949731,-234.90005));
#211432=CARTESIAN_POINT('',(20.75,8.45759727949731,-234.90005));
#211433=CARTESIAN_POINT('Origin',(21.5,8.45759727949731,-234.90005));
#211434=CARTESIAN_POINT('',(20.3,8.45759727949731,-235.35005));
#211435=CARTESIAN_POINT('Origin',(20.3,8.45759727949731,-234.90005));
#211436=CARTESIAN_POINT('Origin',(21.5,8.45759727949731,-235.35005));
#211437=CARTESIAN_POINT('Origin',(20.3,-25.4138432731711,-234.90005));
#211438=CARTESIAN_POINT('',(20.75,0.352057726830487,-234.90005));
#211439=CARTESIAN_POINT('',(20.3,0.352057726830486,-235.35005));
#211440=CARTESIAN_POINT('Origin',(20.3,0.352057726830486,-234.90005));
#211441=CARTESIAN_POINT('',(20.3,0.352057726830487,-235.35005));
#211442=CARTESIAN_POINT('',(20.75,8.45759727949731,-234.90005));
#211443=CARTESIAN_POINT('Origin',(-296.501483394397,9.65759727949727,-234.90005));
#211444=CARTESIAN_POINT('',(29.125,9.65759727949731,-235.35005));
#211445=CARTESIAN_POINT('',(29.125,9.20759727949731,-234.90005));
#211446=CARTESIAN_POINT('Origin',(29.125,9.65759727949731,-234.90005));
#211447=CARTESIAN_POINT('',(-2.8425373731103E-15,9.20759727949731,-234.90005));
#211448=CARTESIAN_POINT('',(-296.501483394397,9.65759727949727,-235.35005));
#211449=CARTESIAN_POINT('Origin',(21.5,0.352057726830491,-234.90005));
#211450=CARTESIAN_POINT('',(21.5,-0.397942273169509,-234.90005));
#211451=CARTESIAN_POINT('',(21.5,-0.847942273169509,-235.35005));
#211452=CARTESIAN_POINT('Origin',(21.5,-0.847942273169509,-234.90005));
#211453=CARTESIAN_POINT('Origin',(21.5,0.352057726830491,-235.35005));
#211454=CARTESIAN_POINT('Origin',(21.5,0.352057726830491,-234.90005));
#211455=CARTESIAN_POINT('Origin',(29.125,8.45759727949731,-234.90005));
#211456=CARTESIAN_POINT('',(30.325,8.45759727949731,-235.35005));
#211457=CARTESIAN_POINT('',(29.875,8.45759727949731,-234.90005));
#211458=CARTESIAN_POINT('Origin',(30.325,8.45759727949731,-234.90005));
#211459=CARTESIAN_POINT('Origin',(29.125,8.45759727949731,-234.90005));
#211460=CARTESIAN_POINT('Origin',(29.125,8.45759727949731,-235.35005));
#211461=CARTESIAN_POINT('Origin',(-296.501483394397,-0.84794227316963,-234.90005));
#211462=CARTESIAN_POINT('',(29.125,-0.397942273169507,-234.90005));
#211463=CARTESIAN_POINT('',(29.125,-0.847942273169509,-235.35005));
#211464=CARTESIAN_POINT('Origin',(29.125,-0.847942273169506,-234.90005));
#211465=CARTESIAN_POINT('',(-296.501483394397,-0.84794227316963,-235.35005));
#211466=CARTESIAN_POINT('',(-1.11087130309497E-13,-0.397942273169517,-234.90005));
#211467=CARTESIAN_POINT('Origin',(30.325,-25.4138432731711,-234.90005));
#211468=CARTESIAN_POINT('',(30.325,0.352057726830494,-235.35005));
#211469=CARTESIAN_POINT('',(29.875,0.352057726830494,-234.90005));
#211470=CARTESIAN_POINT('Origin',(30.325,0.352057726830494,-234.90005));
#211471=CARTESIAN_POINT('',(29.875,0.352057726830494,-234.90005));
#211472=CARTESIAN_POINT('',(30.325,8.45759727949732,-235.35005));
#211473=CARTESIAN_POINT('Origin',(29.125,0.352057726830494,-234.90005));
#211474=CARTESIAN_POINT('Origin',(29.125,0.352057726830494,-234.90005));
#211475=CARTESIAN_POINT('Origin',(29.125,0.352057726830494,-235.35005));
#211476=CARTESIAN_POINT('Origin',(31.625,8.45759727949731,-234.90005));
#211477=CARTESIAN_POINT('',(31.625,9.65759727949731,-235.35005));
#211478=CARTESIAN_POINT('',(31.625,9.20759727949731,-234.90005));
#211479=CARTESIAN_POINT('Origin',(31.625,9.65759727949731,-234.90005));
#211480=CARTESIAN_POINT('',(30.875,8.45759727949731,-234.90005));
#211481=CARTESIAN_POINT('Origin',(31.625,8.45759727949731,-234.90005));
#211482=CARTESIAN_POINT('',(30.425,8.45759727949731,-235.35005));
#211483=CARTESIAN_POINT('Origin',(30.425,8.45759727949731,-234.90005));
#211484=CARTESIAN_POINT('Origin',(31.625,8.45759727949731,-235.35005));
#211485=CARTESIAN_POINT('Origin',(30.425,-25.4138432731711,-234.90005));
#211486=CARTESIAN_POINT('',(30.875,0.352057726830494,-234.90005));
#211487=CARTESIAN_POINT('',(30.425,0.352057726830494,-235.35005));
#211488=CARTESIAN_POINT('Origin',(30.425,0.352057726830494,-234.90005));
#211489=CARTESIAN_POINT('',(30.425,0.352057726830494,-235.35005));
#211490=CARTESIAN_POINT('',(30.875,8.45759727949732,-234.90005));
#211491=CARTESIAN_POINT('Origin',(-296.501483394397,9.65759727949727,-234.90005));
#211492=CARTESIAN_POINT('',(39.4555265729267,9.65759727949731,-235.35005));
#211493=CARTESIAN_POINT('',(39.4555265729267,9.20759727949731,-234.90005));
#211494=CARTESIAN_POINT('Origin',(39.4555265729267,9.65759727949731,-234.90005));
#211495=CARTESIAN_POINT('',(-2.8425373731103E-15,9.20759727949731,-234.90005));
#211496=CARTESIAN_POINT('',(-296.501483394397,9.65759727949727,-235.35005));
#211497=CARTESIAN_POINT('Origin',(31.625,0.352057726830494,-234.90005));
#211498=CARTESIAN_POINT('',(31.625,-0.397942273169506,-234.90005));
#211499=CARTESIAN_POINT('',(31.625,-0.847942273169506,-235.35005));
#211500=CARTESIAN_POINT('Origin',(31.625,-0.847942273169505,-234.90005));
#211501=CARTESIAN_POINT('Origin',(31.625,0.352057726830495,-235.35005));
#211502=CARTESIAN_POINT('Origin',(31.625,0.352057726830494,-234.90005));
#211503=CARTESIAN_POINT('Origin',(39.4555265729267,8.45759727949731,-234.90005));
#211504=CARTESIAN_POINT('',(40.6550043680477,8.49299528808125,-235.35005));
#211505=CARTESIAN_POINT('',(40.2052001948774,8.47972103486227,-234.90005));
#211506=CARTESIAN_POINT('Origin',(40.6550043680477,8.49299528808125,-234.90005));
#211507=CARTESIAN_POINT('Origin',(39.4555265729267,8.45759727949731,-234.90005));
#211508=CARTESIAN_POINT('Origin',(39.4555265729267,8.45759727949731,-235.35005));
#211509=CARTESIAN_POINT('Origin',(-296.501483394397,-0.84794227316963,-234.90005));
#211510=CARTESIAN_POINT('',(39.6461373136998,-0.397942273169503,-234.90005));
#211511=CARTESIAN_POINT('',(39.6461373136998,-0.847942273169505,-235.35005));
#211512=CARTESIAN_POINT('Origin',(39.6461373136998,-0.847942273169502,-234.90005));
#211513=CARTESIAN_POINT('',(-296.501483394397,-0.84794227316963,-235.35005));
#211514=CARTESIAN_POINT('',(-1.11087130309497E-13,-0.397942273169517,-234.90005));
#211515=CARTESIAN_POINT('Origin',(-636.934816028482,-11.5034818258361,-234.90005));
#211516=CARTESIAN_POINT('',(40.8459531286544,0.37308176509206,-235.35005));
#211517=CARTESIAN_POINT('',(40.3960221980464,0.365197750743974,-234.90005));
#211518=CARTESIAN_POINT('Origin',(40.8459531286544,0.37308176509206,-234.90005));
#211519=CARTESIAN_POINT('Origin',(-636.934816028482,-11.5034818258361,-234.90005));
#211520=CARTESIAN_POINT('Origin',(-636.934816028482,-11.5034818258361,-235.35005));
#211521=CARTESIAN_POINT('Origin',(39.6461373136998,0.352057726830498,-234.90005));
#211522=CARTESIAN_POINT('Origin',(39.6461373136998,0.352057726830498,-234.90005));
#211523=CARTESIAN_POINT('Origin',(39.6461373136998,0.352057726830498,-235.35005));
#211524=CARTESIAN_POINT('Origin',(31.625,19.0631368321642,-234.90005));
#211525=CARTESIAN_POINT('',(31.625,20.2631368321642,-235.35005));
#211526=CARTESIAN_POINT('',(31.625,19.8131368321642,-234.90005));
#211527=CARTESIAN_POINT('Origin',(31.625,20.2631368321642,-234.90005));
#211528=CARTESIAN_POINT('',(30.875,19.0631368321642,-234.90005));
#211529=CARTESIAN_POINT('Origin',(31.625,19.0631368321642,-234.90005));
#211530=CARTESIAN_POINT('',(30.425,19.0631368321642,-235.35005));
#211531=CARTESIAN_POINT('Origin',(30.425,19.0631368321642,-234.90005));
#211532=CARTESIAN_POINT('Origin',(31.625,19.0631368321642,-235.35005));
#211533=CARTESIAN_POINT('Origin',(30.425,-25.4138432731711,-234.90005));
#211534=CARTESIAN_POINT('',(30.875,10.9575972794973,-234.90005));
#211535=CARTESIAN_POINT('',(30.425,10.9575972794973,-235.35005));
#211536=CARTESIAN_POINT('Origin',(30.425,10.9575972794973,-234.90005));
#211537=CARTESIAN_POINT('',(30.425,10.9575972794973,-235.35005));
#211538=CARTESIAN_POINT('',(30.875,19.0631368321642,-234.90005));
#211539=CARTESIAN_POINT('Origin',(-296.501483394397,20.2631368321643,-234.90005));
#211540=CARTESIAN_POINT('',(36.0311576807679,20.2631368321642,-235.35005));
#211541=CARTESIAN_POINT('',(36.0311576807679,19.8131368321642,-234.90005));
#211542=CARTESIAN_POINT('Origin',(36.0311576807679,20.2631368321642,-234.90005));
#211543=CARTESIAN_POINT('',(-1.54373336646988E-15,19.8131368321642,-234.90005));
#211544=CARTESIAN_POINT('',(-296.501483394397,20.2631368321643,-235.35005));
#211545=CARTESIAN_POINT('Origin',(31.625,10.9575972794973,-234.90005));
#211546=CARTESIAN_POINT('',(31.625,10.2075972794973,-234.90005));
#211547=CARTESIAN_POINT('',(31.625,9.75759727949733,-235.35005));
#211548=CARTESIAN_POINT('Origin',(31.625,9.75759727949733,-234.90005));
#211549=CARTESIAN_POINT('Origin',(31.625,10.9575972794973,-235.35005));
#211550=CARTESIAN_POINT('Origin',(31.625,10.9575972794973,-234.90005));
#211551=CARTESIAN_POINT('Origin',(36.0311576807679,19.0631368321642,-234.90005));
#211552=CARTESIAN_POINT('',(36.9462347012319,19.8394319091927,-235.35005));
#211553=CARTESIAN_POINT('',(36.6030808185579,19.548321255307,-234.90005));
#211554=CARTESIAN_POINT('Origin',(36.9462347012319,19.8394319091927,-234.90005));
#211555=CARTESIAN_POINT('Origin',(36.0311576807679,19.0631368321642,-234.90005));
#211556=CARTESIAN_POINT('Origin',(36.0311576807679,19.0631368321642,-235.35005));
#211557=CARTESIAN_POINT('Origin',(-296.501483394397,9.75759727949737,-234.90005));
#211558=CARTESIAN_POINT('',(39.3771239584772,10.2075972794973,-234.90005));
#211559=CARTESIAN_POINT('',(39.3771239584772,9.75759727949732,-235.35005));
#211560=CARTESIAN_POINT('Origin',(39.3771239584772,9.75759727949733,-234.90005));
#211561=CARTESIAN_POINT('',(-296.501483394397,9.75759727949737,-235.35005));
#211562=CARTESIAN_POINT('',(-2.53637567332344E-15,10.2075972794973,-234.90005));
#211563=CARTESIAN_POINT('Origin',(-6.29739814579425E-15,-11.5034818258363,
-234.90005));
#211564=CARTESIAN_POINT('',(40.1936303108393,15.5496988085284,-235.35005));
#211565=CARTESIAN_POINT('',(39.8203148590359,15.2984308769399,-234.90005));
#211566=CARTESIAN_POINT('Origin',(40.1936303108393,15.5496988085284,-234.90005));
#211567=CARTESIAN_POINT('Origin',(-6.29739814579425E-15,-11.5034818258363,
-234.90005));
#211568=CARTESIAN_POINT('Origin',(-6.29739814579425E-15,-11.5034818258363,
-235.35005));
#211569=CARTESIAN_POINT('Origin',(39.3771239584772,10.9575972794973,-234.90005));
#211570=CARTESIAN_POINT('',(40.1267106833092,10.9824918965036,-234.90005));
#211571=CARTESIAN_POINT('',(40.5764627182082,10.9974286667074,-235.35005));
#211572=CARTESIAN_POINT('Origin',(40.5764627182083,10.9974286667074,-234.90005));
#211573=CARTESIAN_POINT('Origin',(39.3771239584772,10.9575972794973,-235.35005));
#211574=CARTESIAN_POINT('Origin',(39.3771239584772,10.9575972794973,-234.90005));
#211575=CARTESIAN_POINT('Origin',(38.9907249661392,14.740057695632,-234.90005));
#211576=CARTESIAN_POINT('',(40.4396332884467,14.7963131269086,-235.35005));
#211577=CARTESIAN_POINT('',(39.989972084972,14.7788545447883,-234.90005));
#211578=CARTESIAN_POINT('Origin',(40.4396332884467,14.7963131269086,-234.90005));
#211579=CARTESIAN_POINT('Origin',(38.9907249661392,14.740057695632,-234.90005));
#211580=CARTESIAN_POINT('Origin',(38.9907249661392,14.740057695632,-235.35005));
#211581=CARTESIAN_POINT('Origin',(-636.934816028482,-11.5034818258361,-234.90005));
#211582=CARTESIAN_POINT('Origin',(-636.934816028482,-11.5034818258361,-234.90005));
#211583=CARTESIAN_POINT('Origin',(-636.934816028482,-11.5034818258361,-235.35005));
#211584=CARTESIAN_POINT('Origin',(31.625,-2.14794227316952,-234.90005));
#211585=CARTESIAN_POINT('',(31.625,-0.947942273169512,-235.35005));
#211586=CARTESIAN_POINT('',(31.625,-1.39794227316951,-234.90005));
#211587=CARTESIAN_POINT('Origin',(31.625,-0.947942273169512,-234.90005));
#211588=CARTESIAN_POINT('',(30.875,-2.14794227316951,-234.90005));
#211589=CARTESIAN_POINT('Origin',(31.625,-2.14794227316952,-234.90005));
#211590=CARTESIAN_POINT('',(30.425,-2.14794227316951,-235.35005));
#211591=CARTESIAN_POINT('Origin',(30.425,-2.14794227316951,-234.90005));
#211592=CARTESIAN_POINT('Origin',(31.625,-2.14794227316952,-235.35005));
#211593=CARTESIAN_POINT('Origin',(30.425,-25.4138432731711,-234.90005));
#211594=CARTESIAN_POINT('',(30.875,-10.2534818258363,-234.90005));
#211595=CARTESIAN_POINT('',(30.425,-10.2534818258363,-235.35005));
#211596=CARTESIAN_POINT('Origin',(30.425,-10.2534818258363,-234.90005));
#211597=CARTESIAN_POINT('',(30.425,-10.2534818258363,-235.35005));
#211598=CARTESIAN_POINT('',(30.875,-2.14794227316951,-234.90005));
#211599=CARTESIAN_POINT('Origin',(-296.501483394397,-0.94794227316939,-234.90005));
#211600=CARTESIAN_POINT('',(39.6853241707135,-0.947942273169515,-235.35005));
#211601=CARTESIAN_POINT('',(39.6853241707135,-1.39794227316951,-234.90005));
#211602=CARTESIAN_POINT('Origin',(39.6853241707135,-0.947942273169515,-234.90005));
#211603=CARTESIAN_POINT('',(-1.11087130309497E-13,-1.3979422731695,-234.90005));
#211604=CARTESIAN_POINT('',(-296.501483394397,-0.94794227316939,-235.35005));
#211605=CARTESIAN_POINT('Origin',(31.625,-10.2534818258363,-234.90005));
#211606=CARTESIAN_POINT('',(31.625,-11.0034818258363,-234.90005));
#211607=CARTESIAN_POINT('',(31.625,-11.4534818258363,-235.35005));
#211608=CARTESIAN_POINT('Origin',(31.625,-11.4534818258363,-234.90005));
#211609=CARTESIAN_POINT('Origin',(31.625,-10.2534818258363,-235.35005));
#211610=CARTESIAN_POINT('Origin',(31.625,-10.2534818258363,-234.90005));
#211611=CARTESIAN_POINT('Origin',(39.6853241707135,-2.14794227316952,-234.90005));
#211612=CARTESIAN_POINT('',(40.8852094777378,-2.13135161353407,-235.35005));
#211613=CARTESIAN_POINT('',(40.4352524876037,-2.13757311089736,-234.90005));
#211614=CARTESIAN_POINT('Origin',(40.8852094777378,-2.13135161353407,-234.90005));
#211615=CARTESIAN_POINT('Origin',(39.6853241707135,-2.14794227316952,-234.90005));
#211616=CARTESIAN_POINT('Origin',(39.6853241707135,-2.14794227316952,-235.35005));
#211617=CARTESIAN_POINT('Origin',(-296.501483394397,-11.4534818258365,-234.90005));
#211618=CARTESIAN_POINT('',(39.7488454733312,-11.0034818258363,-234.90005));
#211619=CARTESIAN_POINT('',(39.7488454733312,-11.4534818258363,-235.35005));
#211620=CARTESIAN_POINT('Origin',(39.7488454733312,-11.4534818258363,-234.90005));
#211621=CARTESIAN_POINT('',(-296.501483394397,-11.4534818258365,-235.35005));
#211622=CARTESIAN_POINT('',(-2.22174260618994E-13,-11.0034818258363,-234.90005));
#211623=CARTESIAN_POINT('Origin',(-636.934816028482,-11.5034818258361,-234.90005));
#211624=CARTESIAN_POINT('',(40.9488434259496,-10.2512651365233,-235.35005));
#211625=CARTESIAN_POINT('',(40.4988441937178,-10.2520963950157,-234.90005));
#211626=CARTESIAN_POINT('Origin',(40.9488434259496,-10.2512651365233,-234.90005));
#211627=CARTESIAN_POINT('Origin',(-636.934816028482,-11.5034818258361,-234.90005));
#211628=CARTESIAN_POINT('Origin',(-636.934816028482,-11.5034818258361,-235.35005));
#211629=CARTESIAN_POINT('Origin',(39.7488454733312,-10.2534818258363,-234.90005));
#211630=CARTESIAN_POINT('Origin',(39.7488454733312,-10.2534818258363,-234.90005));
#211631=CARTESIAN_POINT('Origin',(39.7488454733312,-10.2534818258363,-235.35005));
#211632=CARTESIAN_POINT('Origin',(21.5,-2.14794227316951,-234.90005));
#211633=CARTESIAN_POINT('',(21.5,-0.947942273169508,-235.35005));
#211634=CARTESIAN_POINT('',(21.5,-1.39794227316951,-234.90005));
#211635=CARTESIAN_POINT('Origin',(21.5,-0.947942273169508,-234.90005));
#211636=CARTESIAN_POINT('',(20.75,-2.14794227316951,-234.90005));
#211637=CARTESIAN_POINT('Origin',(21.5,-2.14794227316951,-234.90005));
#211638=CARTESIAN_POINT('',(20.3,-2.14794227316951,-235.35005));
#211639=CARTESIAN_POINT('Origin',(20.3,-2.14794227316951,-234.90005));
#211640=CARTESIAN_POINT('Origin',(21.5,-2.14794227316951,-235.35005));
#211641=CARTESIAN_POINT('Origin',(20.3,-25.4138432731711,-234.90005));
#211642=CARTESIAN_POINT('',(20.75,-10.2534818258363,-234.90005));
#211643=CARTESIAN_POINT('',(20.3,-10.2534818258363,-235.35005));
#211644=CARTESIAN_POINT('Origin',(20.3,-10.2534818258363,-234.90005));
#211645=CARTESIAN_POINT('',(20.3,-10.2534818258363,-235.35005));
#211646=CARTESIAN_POINT('',(20.75,-2.14794227316951,-234.90005));
#211647=CARTESIAN_POINT('Origin',(-296.501483394397,-0.94794227316939,-234.90005));
#211648=CARTESIAN_POINT('',(29.125,-0.947942273169511,-235.35005));
#211649=CARTESIAN_POINT('',(29.125,-1.39794227316951,-234.90005));
#211650=CARTESIAN_POINT('Origin',(29.125,-0.947942273169511,-234.90005));
#211651=CARTESIAN_POINT('',(-1.11087130309497E-13,-1.3979422731695,-234.90005));
#211652=CARTESIAN_POINT('',(-296.501483394397,-0.94794227316939,-235.35005));
#211653=CARTESIAN_POINT('Origin',(21.5,-10.2534818258363,-234.90005));
#211654=CARTESIAN_POINT('',(21.5,-11.0034818258363,-234.90005));
#211655=CARTESIAN_POINT('',(21.5,-11.4534818258363,-235.35005));
#211656=CARTESIAN_POINT('Origin',(21.5,-11.4534818258363,-234.90005));
#211657=CARTESIAN_POINT('Origin',(21.5,-10.2534818258363,-235.35005));
#211658=CARTESIAN_POINT('Origin',(21.5,-10.2534818258363,-234.90005));
#211659=CARTESIAN_POINT('Origin',(29.125,-2.14794227316951,-234.90005));
#211660=CARTESIAN_POINT('',(30.325,-2.14794227316951,-235.35005));
#211661=CARTESIAN_POINT('',(29.875,-2.14794227316951,-234.90005));
#211662=CARTESIAN_POINT('Origin',(30.325,-2.14794227316951,-234.90005));
#211663=CARTESIAN_POINT('Origin',(29.125,-2.14794227316951,-234.90005));
#211664=CARTESIAN_POINT('Origin',(29.125,-2.14794227316951,-235.35005));
#211665=CARTESIAN_POINT('Origin',(-296.501483394397,-11.4534818258365,-234.90005));
#211666=CARTESIAN_POINT('',(29.125,-11.0034818258363,-234.90005));
#211667=CARTESIAN_POINT('',(29.125,-11.4534818258363,-235.35005));
#211668=CARTESIAN_POINT('Origin',(29.125,-11.4534818258363,-234.90005));
#211669=CARTESIAN_POINT('',(-296.501483394397,-11.4534818258365,-235.35005));
#211670=CARTESIAN_POINT('',(-2.22174260618994E-13,-11.0034818258363,-234.90005));
#211671=CARTESIAN_POINT('Origin',(30.325,-25.4138432731711,-234.90005));
#211672=CARTESIAN_POINT('',(30.325,-10.2534818258363,-235.35005));
#211673=CARTESIAN_POINT('',(29.875,-10.2534818258363,-234.90005));
#211674=CARTESIAN_POINT('Origin',(30.325,-10.2534818258363,-234.90005));
#211675=CARTESIAN_POINT('',(29.875,-10.2534818258363,-234.90005));
#211676=CARTESIAN_POINT('',(30.325,-2.14794227316951,-235.35005));
#211677=CARTESIAN_POINT('Origin',(29.125,-10.2534818258363,-234.90005));
#211678=CARTESIAN_POINT('Origin',(29.125,-10.2534818258363,-234.90005));
#211679=CARTESIAN_POINT('Origin',(29.125,-10.2534818258363,-235.35005));
#211680=CARTESIAN_POINT('Origin',(12.7946237611812,-10.2534818258363,-234.90005));
#211681=CARTESIAN_POINT('',(11.6003099441285,-10.370163042821,-235.35005));
#211682=CARTESIAN_POINT('',(12.0481776255232,-10.3264075864518,-234.90005));
#211683=CARTESIAN_POINT('Origin',(11.6003099441285,-10.370163042821,-234.90005));
#211684=CARTESIAN_POINT('',(12.7946237611812,-11.0034818258363,-234.90005));
#211685=CARTESIAN_POINT('Origin',(12.7946237611812,-10.2534818258363,-234.90005));
#211686=CARTESIAN_POINT('',(12.7946237611812,-11.4534818258363,-235.35005));
#211687=CARTESIAN_POINT('Origin',(12.7946237611812,-11.4534818258363,-234.90005));
#211688=CARTESIAN_POINT('Origin',(12.7946237611812,-10.2534818258363,-235.35005));
#211689=CARTESIAN_POINT('Origin',(-296.501483394397,-11.4534818258365,-234.90005));
#211690=CARTESIAN_POINT('',(19.,-11.0034818258363,-234.90005));
#211691=CARTESIAN_POINT('',(19.,-11.4534818258363,-235.35005));
#211692=CARTESIAN_POINT('Origin',(19.,-11.4534818258363,-234.90005));
#211693=CARTESIAN_POINT('',(-296.501483394397,-11.4534818258365,-235.35005));
#211694=CARTESIAN_POINT('',(-2.22174260618994E-13,-11.0034818258363,-234.90005));
#211695=CARTESIAN_POINT('Origin',(0.,-11.5034818258363,-234.90005));
#211696=CARTESIAN_POINT('',(10.8748986968178,-7.30965533947201,-235.35005));
#211697=CARTESIAN_POINT('',(11.294759518486,-7.14773903260897,-234.90005));
#211698=CARTESIAN_POINT('Origin',(10.8748986968178,-7.30965533947201,-234.90005));
#211699=CARTESIAN_POINT('Origin',(0.,-11.5034818258363,-234.90005));
#211700=CARTESIAN_POINT('Origin',(0.,-11.5034818258363,-235.35005));
#211701=CARTESIAN_POINT('Origin',(19.,-10.2534818258363,-234.90005));
#211702=CARTESIAN_POINT('',(19.75,-10.2534818258363,-234.90005));
#211703=CARTESIAN_POINT('',(20.2,-10.2534818258363,-235.35005));
#211704=CARTESIAN_POINT('Origin',(20.2,-10.2534818258363,-234.90005));
#211705=CARTESIAN_POINT('Origin',(19.,-10.2534818258363,-235.35005));
#211706=CARTESIAN_POINT('Origin',(19.,-10.2534818258363,-234.90005));
#211707=CARTESIAN_POINT('Origin',(20.625,-3.54959888009691,-234.90005));
#211708=CARTESIAN_POINT('',(10.1749999999999,-3.54959888009691,-235.35005));
#211709=CARTESIAN_POINT('',(10.6249999999999,-3.54959888009691,-234.90005));
#211710=CARTESIAN_POINT('Origin',(10.1749999999999,-3.54959888009691,-234.90005));
#211711=CARTESIAN_POINT('Origin',(20.625,-3.54959888009691,-234.90005));
#211712=CARTESIAN_POINT('Origin',(20.625,-3.54959888009691,-235.35005));
#211713=CARTESIAN_POINT('Origin',(20.2,-25.4138432731711,-234.90005));
#211714=CARTESIAN_POINT('',(19.75,-2.14794227316951,-234.90005));
#211715=CARTESIAN_POINT('',(20.2,-2.14794227316951,-235.35005));
#211716=CARTESIAN_POINT('Origin',(20.2,-2.14794227316951,-234.90005));
#211717=CARTESIAN_POINT('',(20.2,-2.14794227316951,-235.35005));
#211718=CARTESIAN_POINT('',(19.75,-10.2534818258363,-234.90005));
#211719=CARTESIAN_POINT('Origin',(10.1749999999999,-25.4138432731711,-234.90005));
#211720=CARTESIAN_POINT('',(10.1749999999999,-2.14794227316951,-235.35005));
#211721=CARTESIAN_POINT('',(10.6249999999999,-2.14794227316951,-234.90005));
#211722=CARTESIAN_POINT('Origin',(10.1749999999999,-2.14794227316951,-234.90005));
#211723=CARTESIAN_POINT('',(10.6249999999999,-2.14794227316951,-234.90005));
#211724=CARTESIAN_POINT('',(10.1749999999999,-3.54959888009691,-235.35005));
#211725=CARTESIAN_POINT('Origin',(19.,-2.14794227316951,-234.90005));
#211726=CARTESIAN_POINT('',(19.,-1.39794227316951,-234.90005));
#211727=CARTESIAN_POINT('',(19.,-0.947942273169507,-235.35005));
#211728=CARTESIAN_POINT('Origin',(19.,-0.947942273169508,-234.90005));
#211729=CARTESIAN_POINT('Origin',(19.,-2.14794227316951,-235.35005));
#211730=CARTESIAN_POINT('Origin',(19.,-2.14794227316951,-234.90005));
#211731=CARTESIAN_POINT('Origin',(11.3749999999999,-2.14794227316951,-234.90005));
#211732=CARTESIAN_POINT('',(11.3749999999999,-0.947942273169504,-235.35005));
#211733=CARTESIAN_POINT('',(11.3749999999999,-1.3979422731695,-234.90005));
#211734=CARTESIAN_POINT('Origin',(11.3749999999999,-0.947942273169504,-234.90005));
#211735=CARTESIAN_POINT('Origin',(11.3749999999999,-2.14794227316951,-234.90005));
#211736=CARTESIAN_POINT('Origin',(11.3749999999999,-2.14794227316951,-235.35005));
#211737=CARTESIAN_POINT('Origin',(-296.501483394397,-0.94794227316939,-234.90005));
#211738=CARTESIAN_POINT('',(-1.11087130309497E-13,-1.3979422731695,-234.90005));
#211739=CARTESIAN_POINT('',(-296.501483394397,-0.94794227316939,-235.35005));
#211740=CARTESIAN_POINT('Origin',(11.3749999999999,-20.8590213785032,-234.90005));
#211741=CARTESIAN_POINT('',(10.1749999999999,-20.8590213785032,-235.35005));
#211742=CARTESIAN_POINT('',(10.6249999999999,-20.8590213785032,-234.90005));
#211743=CARTESIAN_POINT('Origin',(10.1749999999999,-20.8590213785032,-234.90005));
#211744=CARTESIAN_POINT('',(11.3749999999999,-21.6090213785032,-234.90005));
#211745=CARTESIAN_POINT('Origin',(11.3749999999999,-20.8590213785032,-234.90005));
#211746=CARTESIAN_POINT('',(11.3749999999999,-22.0590213785032,-235.35005));
#211747=CARTESIAN_POINT('Origin',(11.3749999999999,-22.0590213785032,-234.90005));
#211748=CARTESIAN_POINT('Origin',(11.3749999999999,-20.8590213785032,-235.35005));
#211749=CARTESIAN_POINT('Origin',(-296.501483394397,-22.0590213785033,-234.90005));
#211750=CARTESIAN_POINT('',(19.,-21.6090213785031,-234.90005));
#211751=CARTESIAN_POINT('',(19.,-22.0590213785031,-235.35005));
#211752=CARTESIAN_POINT('Origin',(19.,-22.0590213785031,-234.90005));
#211753=CARTESIAN_POINT('',(-296.501483394397,-22.0590213785033,-235.35005));
#211754=CARTESIAN_POINT('',(-3.33261390928491E-13,-21.6090213785032,-234.90005));
#211755=CARTESIAN_POINT('Origin',(10.1749999999999,-25.4138432731711,-234.90005));
#211756=CARTESIAN_POINT('',(10.1749999999999,-19.4573647715757,-235.35005));
#211757=CARTESIAN_POINT('',(10.6249999999999,-19.4573647715757,-234.90005));
#211758=CARTESIAN_POINT('Origin',(10.1749999999999,-19.4573647715757,-234.90005));
#211759=CARTESIAN_POINT('',(10.6249999999999,-19.4573647715757,-234.90005));
#211760=CARTESIAN_POINT('',(10.1749999999999,-20.8590213785032,-235.35005));
#211761=CARTESIAN_POINT('Origin',(19.,-20.8590213785032,-234.90005));
#211762=CARTESIAN_POINT('',(19.75,-20.8590213785032,-234.90005));
#211763=CARTESIAN_POINT('',(20.2,-20.8590213785032,-235.35005));
#211764=CARTESIAN_POINT('Origin',(20.2,-20.8590213785032,-234.90005));
#211765=CARTESIAN_POINT('Origin',(19.,-20.8590213785032,-235.35005));
#211766=CARTESIAN_POINT('Origin',(19.,-20.8590213785032,-234.90005));
#211767=CARTESIAN_POINT('Origin',(20.625,-19.4573647715757,-234.90005));
#211768=CARTESIAN_POINT('',(10.8748986968178,-15.6973083122006,-235.35005));
#211769=CARTESIAN_POINT('',(11.294759518486,-15.8592246190636,-234.90005));
#211770=CARTESIAN_POINT('Origin',(10.8748986968178,-15.6973083122006,-234.90005));
#211771=CARTESIAN_POINT('Origin',(20.625,-19.4573647715757,-234.90005));
#211772=CARTESIAN_POINT('Origin',(20.625,-19.4573647715757,-235.35005));
#211773=CARTESIAN_POINT('Origin',(20.2,-25.4138432731711,-234.90005));
#211774=CARTESIAN_POINT('',(19.75,-12.7534818258363,-234.90005));
#211775=CARTESIAN_POINT('',(20.2,-12.7534818258363,-235.35005));
#211776=CARTESIAN_POINT('Origin',(20.2,-12.7534818258363,-234.90005));
#211777=CARTESIAN_POINT('',(20.2,-12.7534818258363,-235.35005));
#211778=CARTESIAN_POINT('',(19.75,-20.8590213785032,-234.90005));
#211779=CARTESIAN_POINT('Origin',(0.,-11.5034818258363,-234.90005));
#211780=CARTESIAN_POINT('',(11.6003099441285,-12.6368006088516,-235.35005));
#211781=CARTESIAN_POINT('',(12.0481776255232,-12.6805560652209,-234.90005));
#211782=CARTESIAN_POINT('Origin',(11.6003099441285,-12.6368006088516,-234.90005));
#211783=CARTESIAN_POINT('Origin',(0.,-11.5034818258363,-234.90005));
#211784=CARTESIAN_POINT('Origin',(0.,-11.5034818258363,-235.35005));
#211785=CARTESIAN_POINT('Origin',(19.,-12.7534818258363,-234.90005));
#211786=CARTESIAN_POINT('',(19.,-12.0034818258363,-234.90005));
#211787=CARTESIAN_POINT('',(19.,-11.5534818258363,-235.35005));
#211788=CARTESIAN_POINT('Origin',(19.,-11.5534818258363,-234.90005));
#211789=CARTESIAN_POINT('Origin',(19.,-12.7534818258363,-235.35005));
#211790=CARTESIAN_POINT('Origin',(19.,-12.7534818258363,-234.90005));
#211791=CARTESIAN_POINT('Origin',(12.7946237611812,-12.7534818258363,-234.90005));
#211792=CARTESIAN_POINT('',(12.7946237611812,-11.5534818258363,-235.35005));
#211793=CARTESIAN_POINT('',(12.7946237611812,-12.0034818258363,-234.90005));
#211794=CARTESIAN_POINT('Origin',(12.7946237611812,-11.5534818258363,-234.90005));
#211795=CARTESIAN_POINT('Origin',(12.7946237611812,-12.7534818258363,-234.90005));
#211796=CARTESIAN_POINT('Origin',(12.7946237611812,-12.7534818258363,-235.35005));
#211797=CARTESIAN_POINT('Origin',(-296.501483394397,-11.5534818258362,-234.90005));
#211798=CARTESIAN_POINT('',(-2.22174260618994E-13,-12.0034818258363,-234.90005));
#211799=CARTESIAN_POINT('',(-296.501483394397,-11.5534818258362,-235.35005));
#211800=CARTESIAN_POINT('Origin',(21.5,-20.8590213785032,-234.90005));
#211801=CARTESIAN_POINT('',(20.3,-20.8590213785032,-235.35005));
#211802=CARTESIAN_POINT('',(20.75,-20.8590213785032,-234.90005));
#211803=CARTESIAN_POINT('Origin',(20.3,-20.8590213785032,-234.90005));
#211804=CARTESIAN_POINT('',(21.5,-21.6090213785031,-234.90005));
#211805=CARTESIAN_POINT('Origin',(21.5,-20.8590213785032,-234.90005));
#211806=CARTESIAN_POINT('',(21.5,-22.0590213785031,-235.35005));
#211807=CARTESIAN_POINT('Origin',(21.5,-22.0590213785031,-234.90005));
#211808=CARTESIAN_POINT('Origin',(21.5,-20.8590213785032,-235.35005));
#211809=CARTESIAN_POINT('Origin',(-296.501483394397,-22.0590213785033,-234.90005));
#211810=CARTESIAN_POINT('',(29.125,-21.6090213785031,-234.90005));
#211811=CARTESIAN_POINT('',(29.125,-22.0590213785031,-235.35005));
#211812=CARTESIAN_POINT('Origin',(29.125,-22.0590213785031,-234.90005));
#211813=CARTESIAN_POINT('',(-296.501483394397,-22.0590213785033,-235.35005));
#211814=CARTESIAN_POINT('',(-3.33261390928491E-13,-21.6090213785032,-234.90005));
#211815=CARTESIAN_POINT('Origin',(20.3,-25.4138432731711,-234.90005));
#211816=CARTESIAN_POINT('',(20.3,-12.7534818258363,-235.35005));
#211817=CARTESIAN_POINT('',(20.75,-12.7534818258363,-234.90005));
#211818=CARTESIAN_POINT('Origin',(20.3,-12.7534818258363,-234.90005));
#211819=CARTESIAN_POINT('',(20.75,-12.7534818258363,-234.90005));
#211820=CARTESIAN_POINT('',(20.3,-20.8590213785032,-235.35005));
#211821=CARTESIAN_POINT('Origin',(29.125,-20.8590213785032,-234.90005));
#211822=CARTESIAN_POINT('',(29.875,-20.8590213785032,-234.90005));
#211823=CARTESIAN_POINT('',(30.325,-20.8590213785032,-235.35005));
#211824=CARTESIAN_POINT('Origin',(30.325,-20.8590213785032,-234.90005));
#211825=CARTESIAN_POINT('Origin',(29.125,-20.8590213785032,-235.35005));
#211826=CARTESIAN_POINT('Origin',(29.125,-20.8590213785032,-234.90005));
#211827=CARTESIAN_POINT('Origin',(21.5,-12.7534818258363,-234.90005));
#211828=CARTESIAN_POINT('',(21.5,-11.5534818258363,-235.35005));
#211829=CARTESIAN_POINT('',(21.5,-12.0034818258363,-234.90005));
#211830=CARTESIAN_POINT('Origin',(21.5,-11.5534818258363,-234.90005));
#211831=CARTESIAN_POINT('Origin',(21.5,-12.7534818258363,-234.90005));
#211832=CARTESIAN_POINT('Origin',(21.5,-12.7534818258363,-235.35005));
#211833=CARTESIAN_POINT('Origin',(30.325,-25.4138432731711,-234.90005));
#211834=CARTESIAN_POINT('',(29.875,-12.7534818258363,-234.90005));
#211835=CARTESIAN_POINT('',(30.325,-12.7534818258363,-235.35005));
#211836=CARTESIAN_POINT('Origin',(30.325,-12.7534818258363,-234.90005));
#211837=CARTESIAN_POINT('',(30.325,-12.7534818258363,-235.35005));
#211838=CARTESIAN_POINT('',(29.875,-20.8590213785032,-234.90005));
#211839=CARTESIAN_POINT('Origin',(-296.501483394397,-11.5534818258362,-234.90005));
#211840=CARTESIAN_POINT('',(29.125,-11.5534818258363,-235.35005));
#211841=CARTESIAN_POINT('',(29.125,-12.0034818258363,-234.90005));
#211842=CARTESIAN_POINT('Origin',(29.125,-11.5534818258363,-234.90005));
#211843=CARTESIAN_POINT('',(-2.22174260618994E-13,-12.0034818258363,-234.90005));
#211844=CARTESIAN_POINT('',(-296.501483394397,-11.5534818258362,-235.35005));
#211845=CARTESIAN_POINT('Origin',(29.125,-12.7534818258363,-234.90005));
#211846=CARTESIAN_POINT('Origin',(29.125,-12.7534818258363,-234.90005));
#211847=CARTESIAN_POINT('Origin',(29.125,-12.7534818258363,-235.35005));
#211848=CARTESIAN_POINT('Origin',(31.625,-20.8590213785032,-234.90005));
#211849=CARTESIAN_POINT('',(30.425,-20.8590213785032,-235.35005));
#211850=CARTESIAN_POINT('',(30.875,-20.8590213785032,-234.90005));
#211851=CARTESIAN_POINT('Origin',(30.425,-20.8590213785032,-234.90005));
#211852=CARTESIAN_POINT('',(31.625,-21.6090213785031,-234.90005));
#211853=CARTESIAN_POINT('Origin',(31.625,-20.8590213785032,-234.90005));
#211854=CARTESIAN_POINT('',(31.625,-22.0590213785031,-235.35005));
#211855=CARTESIAN_POINT('Origin',(31.625,-22.0590213785031,-234.90005));
#211856=CARTESIAN_POINT('Origin',(31.625,-20.8590213785032,-235.35005));
#211857=CARTESIAN_POINT('Origin',(-296.501483394397,-22.0590213785033,-234.90005));
#211858=CARTESIAN_POINT('',(39.6853241707135,-21.6090213785031,-234.90005));
#211859=CARTESIAN_POINT('',(39.6853241707135,-22.0590213785031,-235.35005));
#211860=CARTESIAN_POINT('Origin',(39.6853241707135,-22.0590213785031,-234.90005));
#211861=CARTESIAN_POINT('',(-296.501483394397,-22.0590213785033,-235.35005));
#211862=CARTESIAN_POINT('',(-3.33261390928491E-13,-21.6090213785032,-234.90005));
#211863=CARTESIAN_POINT('Origin',(30.425,-25.4138432731711,-234.90005));
#211864=CARTESIAN_POINT('',(30.425,-12.7534818258363,-235.35005));
#211865=CARTESIAN_POINT('',(30.875,-12.7534818258363,-234.90005));
#211866=CARTESIAN_POINT('Origin',(30.425,-12.7534818258363,-234.90005));
#211867=CARTESIAN_POINT('',(30.875,-12.7534818258363,-234.90005));
#211868=CARTESIAN_POINT('',(30.425,-20.8590213785032,-235.35005));
#211869=CARTESIAN_POINT('Origin',(39.6853241707135,-20.8590213785032,-234.90005));
#211870=CARTESIAN_POINT('',(40.4352524876037,-20.8693905407753,-234.90005));
#211871=CARTESIAN_POINT('',(40.8852094777378,-20.8756120381386,-235.35005));
#211872=CARTESIAN_POINT('Origin',(40.8852094777378,-20.8756120381386,-234.90005));
#211873=CARTESIAN_POINT('Origin',(39.6853241707135,-20.8590213785032,-235.35005));
#211874=CARTESIAN_POINT('Origin',(39.6853241707135,-20.8590213785032,-234.90005));
#211875=CARTESIAN_POINT('Origin',(31.625,-12.7534818258363,-234.90005));
#211876=CARTESIAN_POINT('',(31.625,-11.5534818258363,-235.35005));
#211877=CARTESIAN_POINT('',(31.625,-12.0034818258363,-234.90005));
#211878=CARTESIAN_POINT('Origin',(31.625,-11.5534818258363,-234.90005));
#211879=CARTESIAN_POINT('Origin',(31.625,-12.7534818258363,-234.90005));
#211880=CARTESIAN_POINT('Origin',(31.625,-12.7534818258363,-235.35005));
#211881=CARTESIAN_POINT('Origin',(-636.934816028482,-11.5034818258361,-234.90005));
#211882=CARTESIAN_POINT('',(40.4988441937178,-12.754867256657,-234.90005));
#211883=CARTESIAN_POINT('',(40.9488434259496,-12.7556985151494,-235.35005));
#211884=CARTESIAN_POINT('Origin',(40.9488434259496,-12.7556985151494,-234.90005));
#211885=CARTESIAN_POINT('Origin',(-636.934816028482,-11.5034818258361,-235.35005));
#211886=CARTESIAN_POINT('Origin',(-636.934816028482,-11.5034818258361,-234.90005));
#211887=CARTESIAN_POINT('Origin',(-296.501483394397,-11.5534818258362,-234.90005));
#211888=CARTESIAN_POINT('',(39.7488454733312,-11.5534818258363,-235.35005));
#211889=CARTESIAN_POINT('',(39.7488454733312,-12.0034818258363,-234.90005));
#211890=CARTESIAN_POINT('Origin',(39.7488454733312,-11.5534818258363,-234.90005));
#211891=CARTESIAN_POINT('',(-2.22174260618994E-13,-12.0034818258363,-234.90005));
#211892=CARTESIAN_POINT('',(-296.501483394397,-11.5534818258362,-235.35005));
#211893=CARTESIAN_POINT('Origin',(39.7488454733312,-12.7534818258363,-234.90005));
#211894=CARTESIAN_POINT('Origin',(39.7488454733312,-12.7534818258363,-234.90005));
#211895=CARTESIAN_POINT('Origin',(39.7488454733312,-12.7534818258363,-235.35005));
#211896=CARTESIAN_POINT('Origin',(29.125,-23.3590213785032,-234.90005));
#211897=CARTESIAN_POINT('',(30.325,-23.3590213785032,-235.35005));
#211898=CARTESIAN_POINT('',(29.875,-23.3590213785032,-234.90005));
#211899=CARTESIAN_POINT('Origin',(30.325,-23.3590213785032,-234.90005));
#211900=CARTESIAN_POINT('',(29.125,-22.6090213785032,-234.90005));
#211901=CARTESIAN_POINT('Origin',(29.125,-23.3590213785032,-234.90005));
#211902=CARTESIAN_POINT('',(29.125,-22.1590213785032,-235.35005));
#211903=CARTESIAN_POINT('Origin',(29.125,-22.1590213785032,-234.90005));
#211904=CARTESIAN_POINT('Origin',(29.125,-23.3590213785032,-235.35005));
#211905=CARTESIAN_POINT('Origin',(-296.501483394397,-22.1590213785031,-234.90005));
#211906=CARTESIAN_POINT('',(21.5,-22.6090213785032,-234.90005));
#211907=CARTESIAN_POINT('',(21.5,-22.1590213785032,-235.35005));
#211908=CARTESIAN_POINT('Origin',(21.5,-22.1590213785032,-234.90005));
#211909=CARTESIAN_POINT('',(-296.501483394397,-22.1590213785031,-235.35005));
#211910=CARTESIAN_POINT('',(-3.33261390928491E-13,-22.6090213785032,-234.90005));
#211911=CARTESIAN_POINT('Origin',(30.325,-25.4138432731711,-234.90005));
#211912=CARTESIAN_POINT('',(30.325,-31.46456093117,-235.35005));
#211913=CARTESIAN_POINT('',(29.875,-31.46456093117,-234.90005));
#211914=CARTESIAN_POINT('Origin',(30.325,-31.46456093117,-234.90005));
#211915=CARTESIAN_POINT('',(29.875,-31.46456093117,-234.90005));
#211916=CARTESIAN_POINT('',(30.325,-23.3590213785032,-235.35005));
#211917=CARTESIAN_POINT('Origin',(21.5,-23.3590213785032,-234.90005));
#211918=CARTESIAN_POINT('',(20.75,-23.3590213785032,-234.90005));
#211919=CARTESIAN_POINT('',(20.3,-23.3590213785032,-235.35005));
#211920=CARTESIAN_POINT('Origin',(20.3,-23.3590213785032,-234.90005));
#211921=CARTESIAN_POINT('Origin',(21.5,-23.3590213785032,-235.35005));
#211922=CARTESIAN_POINT('Origin',(21.5,-23.3590213785032,-234.90005));
#211923=CARTESIAN_POINT('Origin',(29.125,-31.46456093117,-234.90005));
#211924=CARTESIAN_POINT('',(29.125,-32.66456093117,-235.35005));
#211925=CARTESIAN_POINT('',(29.125,-32.21456093117,-234.90005));
#211926=CARTESIAN_POINT('Origin',(29.125,-32.66456093117,-234.90005));
#211927=CARTESIAN_POINT('Origin',(29.125,-31.46456093117,-234.90005));
#211928=CARTESIAN_POINT('Origin',(29.125,-31.46456093117,-235.35005));
#211929=CARTESIAN_POINT('Origin',(20.3,-25.4138432731711,-234.90005));
#211930=CARTESIAN_POINT('',(20.75,-31.46456093117,-234.90005));
#211931=CARTESIAN_POINT('',(20.3,-31.46456093117,-235.35005));
#211932=CARTESIAN_POINT('Origin',(20.3,-31.46456093117,-234.90005));
#211933=CARTESIAN_POINT('',(20.3,-31.46456093117,-235.35005));
#211934=CARTESIAN_POINT('',(20.75,-23.3590213785032,-234.90005));
#211935=CARTESIAN_POINT('Origin',(-296.501483394397,-32.6645609311701,-234.90005));
#211936=CARTESIAN_POINT('',(21.5,-32.66456093117,-235.35005));
#211937=CARTESIAN_POINT('',(21.5,-32.21456093117,-234.90005));
#211938=CARTESIAN_POINT('Origin',(21.5,-32.66456093117,-234.90005));
#211939=CARTESIAN_POINT('',(0.,-32.21456093117,-234.90005));
#211940=CARTESIAN_POINT('',(-296.501483394397,-32.6645609311701,-235.35005));
#211941=CARTESIAN_POINT('Origin',(21.5,-31.46456093117,-234.90005));
#211942=CARTESIAN_POINT('Origin',(21.5,-31.46456093117,-234.90005));
#211943=CARTESIAN_POINT('Origin',(21.5,-31.46456093117,-235.35005));
#211944=CARTESIAN_POINT('Origin',(19.,-23.3590213785032,-234.90005));
#211945=CARTESIAN_POINT('',(20.2,-23.3590213785032,-235.35005));
#211946=CARTESIAN_POINT('',(19.75,-23.3590213785032,-234.90005));
#211947=CARTESIAN_POINT('Origin',(20.2,-23.3590213785032,-234.90005));
#211948=CARTESIAN_POINT('',(19.,-22.6090213785032,-234.90005));
#211949=CARTESIAN_POINT('Origin',(19.,-23.3590213785032,-234.90005));
#211950=CARTESIAN_POINT('',(19.,-22.1590213785032,-235.35005));
#211951=CARTESIAN_POINT('Origin',(19.,-22.1590213785032,-234.90005));
#211952=CARTESIAN_POINT('Origin',(19.,-23.3590213785032,-235.35005));
#211953=CARTESIAN_POINT('Origin',(-296.501483394397,-22.1590213785031,-234.90005));
#211954=CARTESIAN_POINT('',(11.3749999999999,-22.6090213785032,-234.90005));
#211955=CARTESIAN_POINT('',(11.3749999999999,-22.1590213785032,-235.35005));
#211956=CARTESIAN_POINT('Origin',(11.3749999999999,-22.1590213785032,-234.90005));
#211957=CARTESIAN_POINT('',(-296.501483394397,-22.1590213785031,-235.35005));
#211958=CARTESIAN_POINT('',(-3.33261390928491E-13,-22.6090213785032,-234.90005));
#211959=CARTESIAN_POINT('Origin',(20.2,-25.4138432731711,-234.90005));
#211960=CARTESIAN_POINT('',(20.2,-31.46456093117,-235.35005));
#211961=CARTESIAN_POINT('',(19.75,-31.46456093117,-234.90005));
#211962=CARTESIAN_POINT('Origin',(20.2,-31.46456093117,-234.90005));
#211963=CARTESIAN_POINT('',(19.75,-31.46456093117,-234.90005));
#211964=CARTESIAN_POINT('',(20.2,-23.3590213785032,-235.35005));
#211965=CARTESIAN_POINT('Origin',(11.3749999999999,-23.3590213785032,-234.90005));
#211966=CARTESIAN_POINT('',(10.6249999999999,-23.3590213785032,-234.90005));
#211967=CARTESIAN_POINT('',(10.1749999999999,-23.3590213785032,-235.35005));
#211968=CARTESIAN_POINT('Origin',(10.1749999999999,-23.3590213785032,-234.90005));
#211969=CARTESIAN_POINT('Origin',(11.3749999999999,-23.3590213785032,-235.35005));
#211970=CARTESIAN_POINT('Origin',(11.3749999999999,-23.3590213785032,-234.90005));
#211971=CARTESIAN_POINT('Origin',(19.,-31.46456093117,-234.90005));
#211972=CARTESIAN_POINT('',(19.,-32.66456093117,-235.35005));
#211973=CARTESIAN_POINT('',(19.,-32.21456093117,-234.90005));
#211974=CARTESIAN_POINT('Origin',(19.,-32.66456093117,-234.90005));
#211975=CARTESIAN_POINT('Origin',(19.,-31.46456093117,-234.90005));
#211976=CARTESIAN_POINT('Origin',(19.,-31.46456093117,-235.35005));
#211977=CARTESIAN_POINT('Origin',(10.1749999999999,-25.4138432731711,-234.90005));
#211978=CARTESIAN_POINT('',(10.6249999999999,-31.46456093117,-234.90005));
#211979=CARTESIAN_POINT('',(10.1749999999999,-31.46456093117,-235.35005));
#211980=CARTESIAN_POINT('Origin',(10.1749999999999,-31.46456093117,-234.90005));
#211981=CARTESIAN_POINT('',(10.1749999999999,-31.46456093117,-235.35005));
#211982=CARTESIAN_POINT('',(10.6249999999999,-23.3590213785032,-234.90005));
#211983=CARTESIAN_POINT('Origin',(-296.501483394397,-32.6645609311701,-234.90005));
#211984=CARTESIAN_POINT('',(11.3749999999999,-32.66456093117,-235.35005));
#211985=CARTESIAN_POINT('',(11.3749999999999,-32.21456093117,-234.90005));
#211986=CARTESIAN_POINT('Origin',(11.3749999999999,-32.66456093117,-234.90005));
#211987=CARTESIAN_POINT('',(0.,-32.21456093117,-234.90005));
#211988=CARTESIAN_POINT('',(-296.501483394397,-32.6645609311701,-235.35005));
#211989=CARTESIAN_POINT('Origin',(11.3749999999999,-31.46456093117,-234.90005));
#211990=CARTESIAN_POINT('Origin',(11.3749999999999,-31.46456093117,-234.90005));
#211991=CARTESIAN_POINT('Origin',(11.3749999999999,-31.46456093117,-235.35005));
#211992=CARTESIAN_POINT('Origin',(1.25,-31.46456093117,-234.90005));
#211993=CARTESIAN_POINT('',(0.0499999999999941,-31.46456093117,-235.35005));
#211994=CARTESIAN_POINT('',(0.5,-31.46456093117,-234.90005));
#211995=CARTESIAN_POINT('Origin',(0.0499999999999941,-31.46456093117,-234.90005));
#211996=CARTESIAN_POINT('',(1.25,-32.21456093117,-234.90005));
#211997=CARTESIAN_POINT('Origin',(1.25,-31.46456093117,-234.90005));
#211998=CARTESIAN_POINT('',(1.25,-32.66456093117,-235.35005));
#211999=CARTESIAN_POINT('Origin',(1.25,-32.66456093117,-234.90005));
#212000=CARTESIAN_POINT('Origin',(1.25,-31.46456093117,-235.35005));
#212001=CARTESIAN_POINT('Origin',(-296.501483394397,-32.6645609311701,-234.90005));
#212002=CARTESIAN_POINT('',(8.87499999999984,-32.21456093117,-234.90005));
#212003=CARTESIAN_POINT('',(8.87499999999984,-32.66456093117,-235.35005));
#212004=CARTESIAN_POINT('Origin',(8.87499999999984,-32.66456093117,-234.90005));
#212005=CARTESIAN_POINT('',(-296.501483394397,-32.6645609311701,-235.35005));
#212006=CARTESIAN_POINT('',(0.,-32.21456093117,-234.90005));
#212007=CARTESIAN_POINT('Origin',(0.0499999999999945,-25.4138432731711,
-234.90005));
#212008=CARTESIAN_POINT('',(0.0499999999999967,-25.3025207885872,-235.35005));
#212009=CARTESIAN_POINT('',(0.5,-25.3025207885872,-234.90005));
#212010=CARTESIAN_POINT('Origin',(0.0499999999999967,-25.3025207885872,
-234.90005));
#212011=CARTESIAN_POINT('',(0.5,-25.3025207885872,-234.90005));
#212012=CARTESIAN_POINT('',(0.0499999999999941,-31.46456093117,-235.35005));
#212013=CARTESIAN_POINT('Origin',(8.87499999999984,-31.46456093117,-234.90005));
#212014=CARTESIAN_POINT('',(9.62499999999984,-31.46456093117,-234.90005));
#212015=CARTESIAN_POINT('',(10.0749999999998,-31.46456093117,-235.35005));
#212016=CARTESIAN_POINT('Origin',(10.0749999999998,-31.46456093117,-234.90005));
#212017=CARTESIAN_POINT('Origin',(8.87499999999984,-31.46456093117,-235.35005));
#212018=CARTESIAN_POINT('Origin',(8.87499999999984,-31.46456093117,-234.90005));
#212019=CARTESIAN_POINT('Origin',(1.25,-25.3025207885872,-234.90005));
#212020=CARTESIAN_POINT('',(1.14174005138534,-24.107414189356,-235.35005));
#212021=CARTESIAN_POINT('',(1.18233753211584,-24.5555791640676,-234.90005));
#212022=CARTESIAN_POINT('Origin',(1.14174005138534,-24.107414189356,-234.90005));
#212023=CARTESIAN_POINT('Origin',(1.25,-25.3025207885872,-234.90005));
#212024=CARTESIAN_POINT('Origin',(1.25,-25.3025207885872,-235.35005));
#212025=CARTESIAN_POINT('Origin',(10.075,-25.4138432731712,-234.90005));
#212026=CARTESIAN_POINT('',(9.62499999999985,-23.3741205625531,-234.90005));
#212027=CARTESIAN_POINT('',(10.075,-23.3741205625531,-235.35005));
#212028=CARTESIAN_POINT('Origin',(10.0749999999998,-23.3741205625531,-234.90005));
#212029=CARTESIAN_POINT('',(10.075,-23.3741205625531,-235.35005));
#212030=CARTESIAN_POINT('',(9.62499999999984,-31.46456093117,-234.90005));
#212031=CARTESIAN_POINT('Origin',(0.,-11.5034818258363,-234.90005));
#212032=CARTESIAN_POINT('',(5.15044918227034,-23.0635663666157,-235.35005));
#212033=CARTESIAN_POINT('',(5.33358654455951,-23.474614668563,-234.90005));
#212034=CARTESIAN_POINT('Origin',(5.15044918227034,-23.0635663666157,-234.90005));
#212035=CARTESIAN_POINT('Origin',(0.,-11.5034818258363,-234.90005));
#212036=CARTESIAN_POINT('Origin',(0.,-11.5034818258363,-235.35005));
#212037=CARTESIAN_POINT('Origin',(8.87499999999985,-23.3741205625531,-234.90005));
#212038=CARTESIAN_POINT('',(8.80646304347558,-22.176079375619,-235.35005));
#212039=CARTESIAN_POINT('Origin',(8.87499999999985,-23.3741205625531,-235.35005));
#212040=CARTESIAN_POINT('',(8.83216440217218,-22.6253448207192,-234.90005));
#212041=CARTESIAN_POINT('Origin',(8.87499999999985,-23.3741205625531,-234.90005));
#212042=CARTESIAN_POINT('Origin',(8.80646304347558,-22.176079375619,-234.90005));
#212043=CARTESIAN_POINT('Origin',(9.40330570654103,-32.6090213785032,-234.90005));
#212044=CARTESIAN_POINT('Origin',(9.40330570654103,-32.6090213785032,-235.35005));
#212045=CARTESIAN_POINT('Origin',(9.40330570654103,-32.6090213785032,-234.90005));
#212046=CARTESIAN_POINT('Origin',(31.625,-31.46456093117,-234.90005));
#212047=CARTESIAN_POINT('',(30.425,-31.46456093117,-235.35005));
#212048=CARTESIAN_POINT('',(30.875,-31.46456093117,-234.90005));
#212049=CARTESIAN_POINT('Origin',(30.425,-31.46456093117,-234.90005));
#212050=CARTESIAN_POINT('',(31.625,-32.21456093117,-234.90005));
#212051=CARTESIAN_POINT('Origin',(31.625,-31.46456093117,-234.90005));
#212052=CARTESIAN_POINT('',(31.625,-32.66456093117,-235.35005));
#212053=CARTESIAN_POINT('Origin',(31.625,-32.66456093117,-234.90005));
#212054=CARTESIAN_POINT('Origin',(31.625,-31.46456093117,-235.35005));
#212055=CARTESIAN_POINT('Origin',(-296.501483394397,-32.6645609311701,-234.90005));
#212056=CARTESIAN_POINT('',(39.4555265729267,-32.21456093117,-234.90005));
#212057=CARTESIAN_POINT('',(39.4555265729267,-32.66456093117,-235.35005));
#212058=CARTESIAN_POINT('Origin',(39.4555265729267,-32.66456093117,-234.90005));
#212059=CARTESIAN_POINT('',(-296.501483394397,-32.6645609311701,-235.35005));
#212060=CARTESIAN_POINT('',(0.,-32.21456093117,-234.90005));
#212061=CARTESIAN_POINT('Origin',(30.425,-25.4138432731711,-234.90005));
#212062=CARTESIAN_POINT('',(30.425,-23.3590213785032,-235.35005));
#212063=CARTESIAN_POINT('',(30.875,-23.3590213785032,-234.90005));
#212064=CARTESIAN_POINT('Origin',(30.425,-23.3590213785032,-234.90005));
#212065=CARTESIAN_POINT('',(30.875,-23.3590213785032,-234.90005));
#212066=CARTESIAN_POINT('',(30.425,-31.46456093117,-235.35005));
#212067=CARTESIAN_POINT('Origin',(39.4555265729267,-31.46456093117,-234.90005));
#212068=CARTESIAN_POINT('',(40.2052001948774,-31.486684686535,-234.90005));
#212069=CARTESIAN_POINT('',(40.6550043680477,-31.499958939754,-235.35005));
#212070=CARTESIAN_POINT('Origin',(40.6550043680476,-31.499958939754,-234.90005));
#212071=CARTESIAN_POINT('Origin',(39.4555265729267,-31.46456093117,-235.35005));
#212072=CARTESIAN_POINT('Origin',(39.4555265729267,-31.46456093117,-234.90005));
#212073=CARTESIAN_POINT('Origin',(31.625,-23.3590213785032,-234.90005));
#212074=CARTESIAN_POINT('',(31.625,-22.1590213785032,-235.35005));
#212075=CARTESIAN_POINT('',(31.625,-22.6090213785032,-234.90005));
#212076=CARTESIAN_POINT('Origin',(31.625,-22.1590213785032,-234.90005));
#212077=CARTESIAN_POINT('Origin',(31.625,-23.3590213785032,-234.90005));
#212078=CARTESIAN_POINT('Origin',(31.625,-23.3590213785032,-235.35005));
#212079=CARTESIAN_POINT('Origin',(-636.934816028482,-11.5034818258361,-234.90005));
#212080=CARTESIAN_POINT('',(40.3960221980465,-23.3721614024167,-234.90005));
#212081=CARTESIAN_POINT('',(40.8459531286544,-23.3800454167648,-235.35005));
#212082=CARTESIAN_POINT('Origin',(40.8459531286544,-23.3800454167648,-234.90005));
#212083=CARTESIAN_POINT('Origin',(-636.934816028482,-11.5034818258361,-235.35005));
#212084=CARTESIAN_POINT('Origin',(-636.934816028482,-11.5034818258361,-234.90005));
#212085=CARTESIAN_POINT('Origin',(-296.501483394397,-22.1590213785031,-234.90005));
#212086=CARTESIAN_POINT('',(39.6461373136998,-22.1590213785032,-235.35005));
#212087=CARTESIAN_POINT('',(39.6461373136998,-22.6090213785032,-234.90005));
#212088=CARTESIAN_POINT('Origin',(39.6461373136998,-22.1590213785032,-234.90005));
#212089=CARTESIAN_POINT('',(-3.33261390928491E-13,-22.6090213785032,-234.90005));
#212090=CARTESIAN_POINT('',(-296.501483394397,-22.1590213785031,-235.35005));
#212091=CARTESIAN_POINT('Origin',(39.6461373136998,-23.3590213785032,-234.90005));
#212092=CARTESIAN_POINT('Origin',(39.6461373136998,-23.3590213785032,-234.90005));
#212093=CARTESIAN_POINT('Origin',(39.6461373136998,-23.3590213785032,-235.35005));
#212094=CARTESIAN_POINT('Origin',(31.625,-42.0701004838368,-234.90005));
#212095=CARTESIAN_POINT('',(30.425,-42.0701004838368,-235.35005));
#212096=CARTESIAN_POINT('',(30.875,-42.0701004838368,-234.90005));
#212097=CARTESIAN_POINT('Origin',(30.425,-42.0701004838368,-234.90005));
#212098=CARTESIAN_POINT('',(31.625,-42.8201004838368,-234.90005));
#212099=CARTESIAN_POINT('Origin',(31.625,-42.0701004838368,-234.90005));
#212100=CARTESIAN_POINT('',(31.625,-43.2701004838368,-235.35005));
#212101=CARTESIAN_POINT('Origin',(31.625,-43.2701004838368,-234.90005));
#212102=CARTESIAN_POINT('Origin',(31.625,-42.0701004838368,-235.35005));
#212103=CARTESIAN_POINT('Origin',(-296.501483394397,-43.270100483837,-234.90005));
#212104=CARTESIAN_POINT('',(36.0311576807678,-42.8201004838368,-234.90005));
#212105=CARTESIAN_POINT('',(36.0311576807678,-43.2701004838368,-235.35005));
#212106=CARTESIAN_POINT('Origin',(36.0311576807678,-43.2701004838368,-234.90005));
#212107=CARTESIAN_POINT('',(-296.501483394397,-43.270100483837,-235.35005));
#212108=CARTESIAN_POINT('',(-1.54373336646987E-15,-42.8201004838369,-234.90005));
#212109=CARTESIAN_POINT('Origin',(30.425,-25.4138432731711,-234.90005));
#212110=CARTESIAN_POINT('',(30.425,-33.96456093117,-235.35005));
#212111=CARTESIAN_POINT('',(30.875,-33.96456093117,-234.90005));
#212112=CARTESIAN_POINT('Origin',(30.425,-33.96456093117,-234.90005));
#212113=CARTESIAN_POINT('',(30.875,-33.96456093117,-234.90005));
#212114=CARTESIAN_POINT('',(30.425,-42.0701004838368,-235.35005));
#212115=CARTESIAN_POINT('Origin',(36.0311576807678,-42.0701004838368,-234.90005));
#212116=CARTESIAN_POINT('',(36.6030808185578,-42.5552849069797,-234.90005));
#212117=CARTESIAN_POINT('',(36.9462347012318,-42.8463955608654,-235.35005));
#212118=CARTESIAN_POINT('Origin',(36.9462347012318,-42.8463955608654,-234.90005));
#212119=CARTESIAN_POINT('Origin',(36.0311576807678,-42.0701004838368,-235.35005));
#212120=CARTESIAN_POINT('Origin',(36.0311576807678,-42.0701004838368,-234.90005));
#212121=CARTESIAN_POINT('Origin',(31.625,-33.96456093117,-234.90005));
#212122=CARTESIAN_POINT('',(31.625,-32.76456093117,-235.35005));
#212123=CARTESIAN_POINT('',(31.625,-33.21456093117,-234.90005));
#212124=CARTESIAN_POINT('Origin',(31.625,-32.76456093117,-234.90005));
#212125=CARTESIAN_POINT('Origin',(31.625,-33.96456093117,-234.90005));
#212126=CARTESIAN_POINT('Origin',(31.625,-33.96456093117,-235.35005));
#212127=CARTESIAN_POINT('Origin',(-6.29739814579425E-15,-11.5034818258363,
-234.90005));
#212128=CARTESIAN_POINT('',(39.8203148590358,-38.3053945286125,-234.90005));
#212129=CARTESIAN_POINT('',(40.1936303108393,-38.5566624602009,-235.35005));
#212130=CARTESIAN_POINT('Origin',(40.1936303108393,-38.5566624602009,-234.90005));
#212131=CARTESIAN_POINT('Origin',(-6.29739814579425E-15,-11.5034818258363,
-235.35005));
#212132=CARTESIAN_POINT('Origin',(-6.29739814579425E-15,-11.5034818258363,
-234.90005));
#212133=CARTESIAN_POINT('Origin',(-296.501483394397,-32.7645609311699,-234.90005));
#212134=CARTESIAN_POINT('',(39.3771239584772,-32.76456093117,-235.35005));
#212135=CARTESIAN_POINT('',(39.3771239584772,-33.21456093117,-234.90005));
#212136=CARTESIAN_POINT('Origin',(39.3771239584772,-32.76456093117,-234.90005));
#212137=CARTESIAN_POINT('',(0.,-33.21456093117,-234.90005));
#212138=CARTESIAN_POINT('',(-296.501483394397,-32.7645609311699,-235.35005));
#212139=CARTESIAN_POINT('Origin',(38.9907249661392,-37.7470213473046,-234.90005));
#212140=CARTESIAN_POINT('',(39.989972084972,-37.7858181964606,-234.90005));
#212141=CARTESIAN_POINT('',(40.4396332884467,-37.8032767785809,-235.35005));
#212142=CARTESIAN_POINT('Origin',(40.4396332884467,-37.8032767785809,-234.90005));
#212143=CARTESIAN_POINT('Origin',(38.9907249661392,-37.7470213473046,-235.35005));
#212144=CARTESIAN_POINT('Origin',(38.9907249661392,-37.7470213473046,-234.90005));
#212145=CARTESIAN_POINT('Origin',(39.3771239584772,-33.96456093117,-234.90005));
#212146=CARTESIAN_POINT('',(40.5764627182082,-34.0043923183801,-235.35005));
#212147=CARTESIAN_POINT('',(40.1267106833092,-33.9894555481763,-234.90005));
#212148=CARTESIAN_POINT('Origin',(40.5764627182082,-34.0043923183801,-234.90005));
#212149=CARTESIAN_POINT('Origin',(39.3771239584772,-33.96456093117,-234.90005));
#212150=CARTESIAN_POINT('Origin',(39.3771239584772,-33.96456093117,-235.35005));
#212151=CARTESIAN_POINT('Origin',(-636.934816028482,-11.5034818258361,-234.90005));
#212152=CARTESIAN_POINT('Origin',(-636.934816028482,-11.5034818258361,-234.90005));
#212153=CARTESIAN_POINT('Origin',(-636.934816028482,-11.5034818258361,-235.35005));
#212154=CARTESIAN_POINT('Origin',(21.5,-42.0701004838368,-234.90005));
#212155=CARTESIAN_POINT('',(20.3,-42.0701004838368,-235.35005));
#212156=CARTESIAN_POINT('',(20.75,-42.0701004838368,-234.90005));
#212157=CARTESIAN_POINT('Origin',(20.3,-42.0701004838368,-234.90005));
#212158=CARTESIAN_POINT('',(21.5,-42.8201004838368,-234.90005));
#212159=CARTESIAN_POINT('Origin',(21.5,-42.0701004838368,-234.90005));
#212160=CARTESIAN_POINT('',(21.5,-43.2701004838368,-235.35005));
#212161=CARTESIAN_POINT('Origin',(21.5,-43.2701004838368,-234.90005));
#212162=CARTESIAN_POINT('Origin',(21.5,-42.0701004838368,-235.35005));
#212163=CARTESIAN_POINT('Origin',(-296.501483394397,-43.270100483837,-234.90005));
#212164=CARTESIAN_POINT('',(29.125,-42.8201004838368,-234.90005));
#212165=CARTESIAN_POINT('',(29.125,-43.2701004838368,-235.35005));
#212166=CARTESIAN_POINT('Origin',(29.125,-43.2701004838368,-234.90005));
#212167=CARTESIAN_POINT('',(-296.501483394397,-43.270100483837,-235.35005));
#212168=CARTESIAN_POINT('',(-1.54373336646987E-15,-42.8201004838369,-234.90005));
#212169=CARTESIAN_POINT('Origin',(20.3,-25.4138432731711,-234.90005));
#212170=CARTESIAN_POINT('',(20.3,-33.96456093117,-235.35005));
#212171=CARTESIAN_POINT('',(20.75,-33.96456093117,-234.90005));
#212172=CARTESIAN_POINT('Origin',(20.3,-33.96456093117,-234.90005));
#212173=CARTESIAN_POINT('',(20.75,-33.96456093117,-234.90005));
#212174=CARTESIAN_POINT('',(20.3,-42.0701004838368,-235.35005));
#212175=CARTESIAN_POINT('Origin',(29.125,-42.0701004838368,-234.90005));
#212176=CARTESIAN_POINT('',(29.875,-42.0701004838368,-234.90005));
#212177=CARTESIAN_POINT('',(30.325,-42.0701004838368,-235.35005));
#212178=CARTESIAN_POINT('Origin',(30.325,-42.0701004838368,-234.90005));
#212179=CARTESIAN_POINT('Origin',(29.125,-42.0701004838368,-235.35005));
#212180=CARTESIAN_POINT('Origin',(29.125,-42.0701004838368,-234.90005));
#212181=CARTESIAN_POINT('Origin',(21.5,-33.96456093117,-234.90005));
#212182=CARTESIAN_POINT('',(21.5,-32.76456093117,-235.35005));
#212183=CARTESIAN_POINT('',(21.5,-33.21456093117,-234.90005));
#212184=CARTESIAN_POINT('Origin',(21.5,-32.76456093117,-234.90005));
#212185=CARTESIAN_POINT('Origin',(21.5,-33.96456093117,-234.90005));
#212186=CARTESIAN_POINT('Origin',(21.5,-33.96456093117,-235.35005));
#212187=CARTESIAN_POINT('Origin',(30.325,-25.4138432731711,-234.90005));
#212188=CARTESIAN_POINT('',(29.875,-33.96456093117,-234.90005));
#212189=CARTESIAN_POINT('',(30.325,-33.96456093117,-235.35005));
#212190=CARTESIAN_POINT('Origin',(30.325,-33.96456093117,-234.90005));
#212191=CARTESIAN_POINT('',(30.325,-33.96456093117,-235.35005));
#212192=CARTESIAN_POINT('',(29.875,-42.0701004838368,-234.90005));
#212193=CARTESIAN_POINT('Origin',(-296.501483394397,-32.7645609311699,-234.90005));
#212194=CARTESIAN_POINT('',(29.125,-32.76456093117,-235.35005));
#212195=CARTESIAN_POINT('',(29.125,-33.21456093117,-234.90005));
#212196=CARTESIAN_POINT('Origin',(29.125,-32.76456093117,-234.90005));
#212197=CARTESIAN_POINT('',(0.,-33.21456093117,-234.90005));
#212198=CARTESIAN_POINT('',(-296.501483394397,-32.7645609311699,-235.35005));
#212199=CARTESIAN_POINT('Origin',(29.125,-33.96456093117,-234.90005));
#212200=CARTESIAN_POINT('Origin',(29.125,-33.96456093117,-234.90005));
#212201=CARTESIAN_POINT('Origin',(29.125,-33.96456093117,-235.35005));
#212202=CARTESIAN_POINT('Origin',(29.125,-44.5701004838368,-234.90005));
#212203=CARTESIAN_POINT('',(30.325,-44.5701004838368,-235.35005));
#212204=CARTESIAN_POINT('',(29.875,-44.5701004838368,-234.90005));
#212205=CARTESIAN_POINT('Origin',(30.325,-44.5701004838368,-234.90005));
#212206=CARTESIAN_POINT('',(29.125,-43.8201004838368,-234.90005));
#212207=CARTESIAN_POINT('Origin',(29.125,-44.5701004838368,-234.90005));
#212208=CARTESIAN_POINT('',(29.125,-43.3701004838369,-235.35005));
#212209=CARTESIAN_POINT('Origin',(29.125,-43.3701004838369,-234.90005));
#212210=CARTESIAN_POINT('Origin',(29.125,-44.5701004838368,-235.35005));
#212211=CARTESIAN_POINT('Origin',(-296.501483394397,-43.3701004838369,-234.90005));
#212212=CARTESIAN_POINT('',(21.5,-43.8201004838368,-234.90005));
#212213=CARTESIAN_POINT('',(21.5,-43.3701004838369,-235.35005));
#212214=CARTESIAN_POINT('Origin',(21.5,-43.3701004838369,-234.90005));
#212215=CARTESIAN_POINT('',(-296.501483394397,-43.3701004838369,-235.35005));
#212216=CARTESIAN_POINT('',(-1.23757166668304E-15,-43.8201004838368,-234.90005));
#212217=CARTESIAN_POINT('Origin',(30.325,-25.4138432731711,-234.90005));
#212218=CARTESIAN_POINT('',(30.325,-48.7096221120845,-235.35005));
#212219=CARTESIAN_POINT('',(29.875,-48.7096221120845,-234.90005));
#212220=CARTESIAN_POINT('Origin',(30.325,-48.7096221120845,-234.90005));
#212221=CARTESIAN_POINT('',(29.875,-48.7096221120845,-234.90005));
#212222=CARTESIAN_POINT('',(30.325,-44.5701004838368,-235.35005));
#212223=CARTESIAN_POINT('Origin',(21.5,-44.5701004838368,-234.90005));
#212224=CARTESIAN_POINT('',(20.75,-44.5701004838368,-234.90005));
#212225=CARTESIAN_POINT('',(20.3,-44.5701004838368,-235.35005));
#212226=CARTESIAN_POINT('Origin',(20.3,-44.5701004838368,-234.90005));
#212227=CARTESIAN_POINT('Origin',(21.5,-44.5701004838368,-235.35005));
#212228=CARTESIAN_POINT('Origin',(21.5,-44.5701004838368,-234.90005));
#212229=CARTESIAN_POINT('Origin',(29.125,-48.7096221120845,-234.90005));
#212230=CARTESIAN_POINT('',(29.8646825396825,-49.6545399606241,-235.35005));
#212231=CARTESIAN_POINT('',(29.5873015873016,-49.3001957674217,-234.90005));
#212232=CARTESIAN_POINT('Origin',(29.8646825396825,-49.6545399606241,-234.90005));
#212233=CARTESIAN_POINT('Origin',(29.125,-48.7096221120845,-234.90005));
#212234=CARTESIAN_POINT('Origin',(29.125,-48.7096221120845,-235.35005));
#212235=CARTESIAN_POINT('Origin',(20.3,-25.4138432731711,-234.90005));
#212236=CARTESIAN_POINT('',(20.75,-52.8339989151841,-234.90005));
#212237=CARTESIAN_POINT('',(20.3,-52.8339989151841,-235.35005));
#212238=CARTESIAN_POINT('Origin',(20.3,-52.8339989151841,-234.90005));
#212239=CARTESIAN_POINT('',(20.3,-52.8339989151841,-235.35005));
#212240=CARTESIAN_POINT('',(20.75,-44.5701004838368,-234.90005));
#212241=CARTESIAN_POINT('Origin',(-6.29739814579425E-15,-11.5034818258363,
-234.90005));
#212242=CARTESIAN_POINT('',(23.6248477671233,-53.8032344017111,-235.35005));
#212243=CARTESIAN_POINT('',(23.4054219364689,-53.410357442802,-234.90005));
#212244=CARTESIAN_POINT('Origin',(23.6248477671233,-53.8032344017111,-234.90005));
#212245=CARTESIAN_POINT('Origin',(-6.29739814579425E-15,-11.5034818258363,
-234.90005));
#212246=CARTESIAN_POINT('Origin',(-6.29739814579425E-15,-11.5034818258363,
-235.35005));
#212247=CARTESIAN_POINT('Origin',(21.5,-52.8339989151841,-234.90005));
#212248=CARTESIAN_POINT('',(21.5238294101154,-53.5836202590729,-234.90005));
#212249=CARTESIAN_POINT('',(21.5381270561845,-54.0333930654061,-235.35005));
#212250=CARTESIAN_POINT('Origin',(21.5381270561845,-54.0333930654061,-234.90005));
#212251=CARTESIAN_POINT('Origin',(21.5,-52.8339989151841,-235.35005));
#212252=CARTESIAN_POINT('Origin',(21.5,-52.8339989151841,-234.90005));
#212253=CARTESIAN_POINT('Origin',(22.9178089794592,-52.5372975341153,-234.90005));
#212254=CARTESIAN_POINT('',(22.9669354026308,-53.9864650863833,-235.35005));
#212255=CARTESIAN_POINT('',(22.9516892713016,-53.5367234322311,-234.90005));
#212256=CARTESIAN_POINT('Origin',(22.9669354026308,-53.9864650863833,-234.90005));
#212257=CARTESIAN_POINT('Origin',(22.9178089794592,-52.5372975341153,-234.90005));
#212258=CARTESIAN_POINT('Origin',(22.9178089794592,-52.5372975341153,-235.35005));
#212259=CARTESIAN_POINT('Origin',(7.14692237356698E-14,623.509175991979,
-234.90005));
#212260=CARTESIAN_POINT('Origin',(7.14692237356698E-14,623.509175991979,
-234.90005));
#212261=CARTESIAN_POINT('Origin',(7.14692237356698E-14,623.509175991979,
-235.35005));
#212262=CARTESIAN_POINT('Origin',(19.,-44.5701004838368,-234.90005));
#212263=CARTESIAN_POINT('',(20.2,-44.5701004838368,-235.35005));
#212264=CARTESIAN_POINT('',(19.75,-44.5701004838368,-234.90005));
#212265=CARTESIAN_POINT('Origin',(20.2,-44.5701004838368,-234.90005));
#212266=CARTESIAN_POINT('',(19.,-43.8201004838368,-234.90005));
#212267=CARTESIAN_POINT('Origin',(19.,-44.5701004838368,-234.90005));
#212268=CARTESIAN_POINT('',(19.,-43.3701004838369,-235.35005));
#212269=CARTESIAN_POINT('Origin',(19.,-43.3701004838369,-234.90005));
#212270=CARTESIAN_POINT('Origin',(19.,-44.5701004838368,-235.35005));
#212271=CARTESIAN_POINT('Origin',(-296.501483394397,-43.3701004838369,-234.90005));
#212272=CARTESIAN_POINT('',(11.3749999999999,-43.8201004838368,-234.90005));
#212273=CARTESIAN_POINT('',(11.3749999999999,-43.3701004838369,-235.35005));
#212274=CARTESIAN_POINT('Origin',(11.3749999999999,-43.3701004838369,-234.90005));
#212275=CARTESIAN_POINT('',(-296.501483394397,-43.3701004838369,-235.35005));
#212276=CARTESIAN_POINT('',(-1.23757166668304E-15,-43.8201004838368,-234.90005));
#212277=CARTESIAN_POINT('Origin',(20.2,-25.4138432731711,-234.90005));
#212278=CARTESIAN_POINT('',(20.2,-52.9088458284789,-235.35005));
#212279=CARTESIAN_POINT('',(19.75,-52.9088458284789,-234.90005));
#212280=CARTESIAN_POINT('Origin',(20.2,-52.9088458284789,-234.90005));
#212281=CARTESIAN_POINT('',(19.75,-52.9088458284789,-234.90005));
#212282=CARTESIAN_POINT('',(20.2,-44.5701004838368,-235.35005));
#212283=CARTESIAN_POINT('Origin',(11.3749999999999,-44.5701004838369,-234.90005));
#212284=CARTESIAN_POINT('',(10.6249999999999,-44.5701004838369,-234.90005));
#212285=CARTESIAN_POINT('',(10.1749999999999,-44.5701004838369,-235.35005));
#212286=CARTESIAN_POINT('Origin',(10.1749999999999,-44.5701004838369,-234.90005));
#212287=CARTESIAN_POINT('Origin',(11.3749999999999,-44.5701004838369,-235.35005));
#212288=CARTESIAN_POINT('Origin',(11.3749999999999,-44.5701004838369,-234.90005));
#212289=CARTESIAN_POINT('Origin',(19.,-52.9088458284789,-234.90005));
#212290=CARTESIAN_POINT('',(19.0336936775584,-54.1083727085831,-235.35005));
#212291=CARTESIAN_POINT('',(19.021058548474,-53.6585501285442,-234.90005));
#212292=CARTESIAN_POINT('Origin',(19.0336936775584,-54.1083727085831,-234.90005));
#212293=CARTESIAN_POINT('Origin',(19.,-52.9088458284789,-234.90005));
#212294=CARTESIAN_POINT('Origin',(19.,-52.9088458284789,-235.35005));
#212295=CARTESIAN_POINT('Origin',(10.1749999999999,-25.4138432731711,-234.90005));
#212296=CARTESIAN_POINT('',(10.6249999999999,-53.08002700974,-234.90005));
#212297=CARTESIAN_POINT('',(10.1749999999999,-53.08002700974,-235.35005));
#212298=CARTESIAN_POINT('Origin',(10.1749999999999,-53.08002700974,-234.90005));
#212299=CARTESIAN_POINT('',(10.1749999999999,-53.08002700974,-235.35005));
#212300=CARTESIAN_POINT('',(10.6249999999999,-44.5701004838369,-234.90005));
#212301=CARTESIAN_POINT('Origin',(7.14692237356698E-14,623.509175991979,
-234.90005));
#212302=CARTESIAN_POINT('',(11.3951718727487,-54.2798574542403,-235.35005));
#212303=CARTESIAN_POINT('',(11.3876074204679,-53.8299210375529,-234.90005));
#212304=CARTESIAN_POINT('Origin',(11.3951718727487,-54.2798574542403,-234.90005));
#212305=CARTESIAN_POINT('Origin',(7.14692237356698E-14,623.509175991979,
-234.90005));
#212306=CARTESIAN_POINT('Origin',(7.14692237356698E-14,623.509175991979,
-235.35005));
#212307=CARTESIAN_POINT('Origin',(11.3749999999999,-53.08002700974,-234.90005));
#212308=CARTESIAN_POINT('Origin',(11.3749999999999,-53.08002700974,-234.90005));
#212309=CARTESIAN_POINT('Origin',(11.3749999999999,-53.08002700974,-235.35005));
#212310=CARTESIAN_POINT('Origin',(11.3749999999999,-42.0701004838369,-234.90005));
#212311=CARTESIAN_POINT('',(10.1749999999999,-42.0701004838368,-235.35005));
#212312=CARTESIAN_POINT('',(10.6249999999999,-42.0701004838368,-234.90005));
#212313=CARTESIAN_POINT('Origin',(10.1749999999999,-42.0701004838368,-234.90005));
#212314=CARTESIAN_POINT('',(11.3749999999999,-42.8201004838369,-234.90005));
#212315=CARTESIAN_POINT('Origin',(11.3749999999999,-42.0701004838369,-234.90005));
#212316=CARTESIAN_POINT('',(11.3749999999999,-43.2701004838368,-235.35005));
#212317=CARTESIAN_POINT('Origin',(11.3749999999999,-43.2701004838368,-234.90005));
#212318=CARTESIAN_POINT('Origin',(11.3749999999999,-42.0701004838369,-235.35005));
#212319=CARTESIAN_POINT('Origin',(-296.501483394397,-43.270100483837,-234.90005));
#212320=CARTESIAN_POINT('',(19.,-42.8201004838368,-234.90005));
#212321=CARTESIAN_POINT('',(19.,-43.2701004838368,-235.35005));
#212322=CARTESIAN_POINT('Origin',(19.,-43.2701004838368,-234.90005));
#212323=CARTESIAN_POINT('',(-296.501483394397,-43.270100483837,-235.35005));
#212324=CARTESIAN_POINT('',(-1.54373336646987E-15,-42.8201004838369,-234.90005));
#212325=CARTESIAN_POINT('Origin',(10.1749999999999,-25.4138432731711,-234.90005));
#212326=CARTESIAN_POINT('',(10.1749999999999,-33.96456093117,-235.35005));
#212327=CARTESIAN_POINT('',(10.6249999999999,-33.96456093117,-234.90005));
#212328=CARTESIAN_POINT('Origin',(10.1749999999999,-33.96456093117,-234.90005));
#212329=CARTESIAN_POINT('',(10.6249999999999,-33.96456093117,-234.90005));
#212330=CARTESIAN_POINT('',(10.1749999999999,-42.0701004838368,-235.35005));
#212331=CARTESIAN_POINT('Origin',(19.,-42.0701004838368,-234.90005));
#212332=CARTESIAN_POINT('',(19.75,-42.0701004838368,-234.90005));
#212333=CARTESIAN_POINT('',(20.2,-42.0701004838368,-235.35005));
#212334=CARTESIAN_POINT('Origin',(20.2,-42.0701004838368,-234.90005));
#212335=CARTESIAN_POINT('Origin',(19.,-42.0701004838368,-235.35005));
#212336=CARTESIAN_POINT('Origin',(19.,-42.0701004838368,-234.90005));
#212337=CARTESIAN_POINT('Origin',(11.3749999999999,-33.96456093117,-234.90005));
#212338=CARTESIAN_POINT('',(11.3749999999999,-32.76456093117,-235.35005));
#212339=CARTESIAN_POINT('',(11.3749999999999,-33.21456093117,-234.90005));
#212340=CARTESIAN_POINT('Origin',(11.3749999999999,-32.76456093117,-234.90005));
#212341=CARTESIAN_POINT('Origin',(11.3749999999999,-33.96456093117,-234.90005));
#212342=CARTESIAN_POINT('Origin',(11.3749999999999,-33.96456093117,-235.35005));
#212343=CARTESIAN_POINT('Origin',(20.2,-25.4138432731711,-234.90005));
#212344=CARTESIAN_POINT('',(19.75,-33.96456093117,-234.90005));
#212345=CARTESIAN_POINT('',(20.2,-33.96456093117,-235.35005));
#212346=CARTESIAN_POINT('Origin',(20.2,-33.96456093117,-234.90005));
#212347=CARTESIAN_POINT('',(20.2,-33.96456093117,-235.35005));
#212348=CARTESIAN_POINT('',(19.75,-42.0701004838368,-234.90005));
#212349=CARTESIAN_POINT('Origin',(-296.501483394397,-32.7645609311699,-234.90005));
#212350=CARTESIAN_POINT('',(19.,-32.76456093117,-235.35005));
#212351=CARTESIAN_POINT('',(19.,-33.21456093117,-234.90005));
#212352=CARTESIAN_POINT('Origin',(19.,-32.76456093117,-234.90005));
#212353=CARTESIAN_POINT('',(0.,-33.21456093117,-234.90005));
#212354=CARTESIAN_POINT('',(-296.501483394397,-32.7645609311699,-235.35005));
#212355=CARTESIAN_POINT('Origin',(19.,-33.96456093117,-234.90005));
#212356=CARTESIAN_POINT('Origin',(19.,-33.96456093117,-234.90005));
#212357=CARTESIAN_POINT('Origin',(19.,-33.96456093117,-235.35005));
#212358=CARTESIAN_POINT('Origin',(8.87499999999984,-44.5701004838369,-234.90005));
#212359=CARTESIAN_POINT('',(10.075,-44.5701004838369,-235.35005));
#212360=CARTESIAN_POINT('',(9.62499999999984,-44.5701004838369,-234.90005));
#212361=CARTESIAN_POINT('Origin',(10.075,-44.5701004838369,-234.90005));
#212362=CARTESIAN_POINT('',(8.87499999999984,-43.8201004838368,-234.90005));
#212363=CARTESIAN_POINT('Origin',(8.87499999999984,-44.5701004838369,-234.90005));
#212364=CARTESIAN_POINT('',(8.87499999999984,-43.3701004838369,-235.35005));
#212365=CARTESIAN_POINT('Origin',(8.87499999999984,-43.3701004838369,-234.90005));
#212366=CARTESIAN_POINT('Origin',(8.87499999999984,-44.5701004838369,-235.35005));
#212367=CARTESIAN_POINT('Origin',(-296.501483394397,-43.3701004838369,-234.90005));
#212368=CARTESIAN_POINT('',(1.25,-43.8201004838368,-234.90005));
#212369=CARTESIAN_POINT('',(1.25,-43.3701004838369,-235.35005));
#212370=CARTESIAN_POINT('Origin',(1.25,-43.3701004838369,-234.90005));
#212371=CARTESIAN_POINT('',(-296.501483394397,-43.3701004838369,-235.35005));
#212372=CARTESIAN_POINT('',(-1.23757166668304E-15,-43.8201004838368,-234.90005));
#212373=CARTESIAN_POINT('Origin',(10.075,-25.4138432731712,-234.90005));
#212374=CARTESIAN_POINT('',(10.0749999999998,-53.1174378937751,-235.35005));
#212375=CARTESIAN_POINT('',(9.62499999999984,-53.1174378937751,-234.90005));
#212376=CARTESIAN_POINT('Origin',(10.0749999999998,-53.1174378937751,-234.90005));
#212377=CARTESIAN_POINT('',(9.62499999999984,-53.1174378937751,-234.90005));
#212378=CARTESIAN_POINT('',(10.075,-44.5701004838369,-235.35005));
#212379=CARTESIAN_POINT('Origin',(1.25,-44.5701004838369,-234.90005));
#212380=CARTESIAN_POINT('',(0.5,-44.5701004838369,-234.90005));
#212381=CARTESIAN_POINT('',(0.0499999999999953,-44.5701004838369,-235.35005));
#212382=CARTESIAN_POINT('Origin',(0.0499999999999955,-44.5701004838369,
-234.90005));
#212383=CARTESIAN_POINT('Origin',(1.25,-44.5701004838369,-235.35005));
#212384=CARTESIAN_POINT('Origin',(1.25,-44.5701004838369,-234.90005));
#212385=CARTESIAN_POINT('Origin',(8.87499999999984,-53.1174378937751,-234.90005));
#212386=CARTESIAN_POINT('',(8.89073849412256,-54.3173346809209,-235.35005));
#212387=CARTESIAN_POINT('',(8.88483655882654,-53.8673733857413,-234.90005));
#212388=CARTESIAN_POINT('Origin',(8.89073849412256,-54.3173346809209,-234.90005));
#212389=CARTESIAN_POINT('Origin',(8.87499999999984,-53.1174378937751,-234.90005));
#212390=CARTESIAN_POINT('Origin',(8.87499999999984,-53.1174378937751,-235.35005));
#212391=CARTESIAN_POINT('Origin',(0.0499999999999945,-25.4138432731711,
-234.90005));
#212392=CARTESIAN_POINT('',(0.5,-53.1744855098348,-234.90005));
#212393=CARTESIAN_POINT('',(0.0499999999999928,-53.1744855098348,-235.35005));
#212394=CARTESIAN_POINT('Origin',(0.049999999999995,-53.1744855098348,-234.90005));
#212395=CARTESIAN_POINT('',(0.0499999999999928,-53.1744855098348,-235.35005));
#212396=CARTESIAN_POINT('',(0.5,-44.5701004838369,-234.90005));
#212397=CARTESIAN_POINT('Origin',(7.14692237356698E-14,623.509175991979,
-234.90005));
#212398=CARTESIAN_POINT('',(1.25221668931305,-54.3744834624533,-235.35005));
#212399=CARTESIAN_POINT('',(1.25138543082066,-53.9244842302215,-234.90005));
#212400=CARTESIAN_POINT('Origin',(1.25221668931305,-54.3744834624533,-234.90005));
#212401=CARTESIAN_POINT('Origin',(7.14692237356698E-14,623.509175991979,
-234.90005));
#212402=CARTESIAN_POINT('Origin',(7.14692237356698E-14,623.509175991979,
-235.35005));
#212403=CARTESIAN_POINT('Origin',(1.25,-53.1744855098348,-234.90005));
#212404=CARTESIAN_POINT('Origin',(1.25,-53.1744855098348,-234.90005));
#212405=CARTESIAN_POINT('Origin',(1.25,-53.1744855098348,-235.35005));
#212406=CARTESIAN_POINT('Origin',(1.25,-42.0701004838369,-234.90005));
#212407=CARTESIAN_POINT('',(0.0499999999999935,-42.0701004838369,-235.35005));
#212408=CARTESIAN_POINT('',(0.5,-42.0701004838369,-234.90005));
#212409=CARTESIAN_POINT('Origin',(0.0499999999999935,-42.0701004838369,
-234.90005));
#212410=CARTESIAN_POINT('',(1.25,-42.8201004838369,-234.90005));
#212411=CARTESIAN_POINT('Origin',(1.25,-42.0701004838369,-234.90005));
#212412=CARTESIAN_POINT('',(1.25,-43.2701004838368,-235.35005));
#212413=CARTESIAN_POINT('Origin',(1.25,-43.2701004838368,-234.90005));
#212414=CARTESIAN_POINT('Origin',(1.25,-42.0701004838369,-235.35005));
#212415=CARTESIAN_POINT('Origin',(-296.501483394397,-43.270100483837,-234.90005));
#212416=CARTESIAN_POINT('',(8.87499999999984,-42.8201004838369,-234.90005));
#212417=CARTESIAN_POINT('',(8.87499999999984,-43.2701004838368,-235.35005));
#212418=CARTESIAN_POINT('Origin',(8.87499999999984,-43.2701004838368,-234.90005));
#212419=CARTESIAN_POINT('',(-296.501483394397,-43.270100483837,-235.35005));
#212420=CARTESIAN_POINT('',(-1.54373336646987E-15,-42.8201004838369,-234.90005));
#212421=CARTESIAN_POINT('Origin',(0.0499999999999945,-25.4138432731711,
-234.90005));
#212422=CARTESIAN_POINT('',(0.0499999999999959,-33.96456093117,-235.35005));
#212423=CARTESIAN_POINT('',(0.5,-33.96456093117,-234.90005));
#212424=CARTESIAN_POINT('Origin',(0.0499999999999959,-33.96456093117,-234.90005));
#212425=CARTESIAN_POINT('',(0.5,-33.96456093117,-234.90005));
#212426=CARTESIAN_POINT('',(0.0499999999999935,-42.0701004838369,-235.35005));
#212427=CARTESIAN_POINT('Origin',(8.87499999999984,-42.0701004838369,-234.90005));
#212428=CARTESIAN_POINT('',(9.62499999999984,-42.0701004838368,-234.90005));
#212429=CARTESIAN_POINT('',(10.0749999999998,-42.0701004838368,-235.35005));
#212430=CARTESIAN_POINT('Origin',(10.0749999999998,-42.0701004838368,-234.90005));
#212431=CARTESIAN_POINT('Origin',(8.87499999999984,-42.0701004838369,-235.35005));
#212432=CARTESIAN_POINT('Origin',(8.87499999999984,-42.0701004838369,-234.90005));
#212433=CARTESIAN_POINT('Origin',(1.25,-33.96456093117,-234.90005));
#212434=CARTESIAN_POINT('',(1.25,-32.76456093117,-235.35005));
#212435=CARTESIAN_POINT('',(1.25,-33.21456093117,-234.90005));
#212436=CARTESIAN_POINT('Origin',(1.25,-32.76456093117,-234.90005));
#212437=CARTESIAN_POINT('Origin',(1.25,-33.96456093117,-234.90005));
#212438=CARTESIAN_POINT('Origin',(1.25,-33.96456093117,-235.35005));
#212439=CARTESIAN_POINT('Origin',(10.075,-25.4138432731712,-234.90005));
#212440=CARTESIAN_POINT('',(9.62499999999984,-33.96456093117,-234.90005));
#212441=CARTESIAN_POINT('',(10.075,-33.96456093117,-235.35005));
#212442=CARTESIAN_POINT('Origin',(10.0749999999998,-33.96456093117,-234.90005));
#212443=CARTESIAN_POINT('',(10.075,-33.96456093117,-235.35005));
#212444=CARTESIAN_POINT('',(9.62499999999984,-42.0701004838368,-234.90005));
#212445=CARTESIAN_POINT('Origin',(-296.501483394397,-32.7645609311699,-234.90005));
#212446=CARTESIAN_POINT('',(8.87499999999984,-32.76456093117,-235.35005));
#212447=CARTESIAN_POINT('',(8.87499999999984,-33.21456093117,-234.90005));
#212448=CARTESIAN_POINT('Origin',(8.87499999999984,-32.76456093117,-234.90005));
#212449=CARTESIAN_POINT('',(0.,-33.21456093117,-234.90005));
#212450=CARTESIAN_POINT('',(-296.501483394397,-32.7645609311699,-235.35005));
#212451=CARTESIAN_POINT('Origin',(8.87499999999984,-33.96456093117,-234.90005));
#212452=CARTESIAN_POINT('Origin',(8.87499999999984,-33.96456093117,-234.90005));
#212453=CARTESIAN_POINT('Origin',(8.87499999999984,-33.96456093117,-235.35005));
#212454=CARTESIAN_POINT('Origin',(33.7514626427707,-44.5701004838368,-234.90005));
#212455=CARTESIAN_POINT('',(34.6086426463967,-45.4098876243575,-235.35005));
#212456=CARTESIAN_POINT('',(34.2872001450369,-45.0949674466622,-234.90005));
#212457=CARTESIAN_POINT('Origin',(34.6086426463967,-45.4098876243575,-234.90005));
#212458=CARTESIAN_POINT('',(33.7514626427707,-43.8201004838368,-234.90005));
#212459=CARTESIAN_POINT('Origin',(33.7514626427707,-44.5701004838368,-234.90005));
#212460=CARTESIAN_POINT('',(33.7514626427707,-43.3701004838369,-235.35005));
#212461=CARTESIAN_POINT('Origin',(33.7514626427707,-43.3701004838369,-234.90005));
#212462=CARTESIAN_POINT('Origin',(33.7514626427707,-44.5701004838368,-235.35005));
#212463=CARTESIAN_POINT('Origin',(-296.501483394397,-43.3701004838369,-234.90005));
#212464=CARTESIAN_POINT('',(31.625,-43.8201004838368,-234.90005));
#212465=CARTESIAN_POINT('',(31.625,-43.3701004838369,-235.35005));
#212466=CARTESIAN_POINT('Origin',(31.625,-43.3701004838369,-234.90005));
#212467=CARTESIAN_POINT('',(-296.501483394397,-43.3701004838369,-235.35005));
#212468=CARTESIAN_POINT('',(-1.23757166668304E-15,-43.8201004838368,-234.90005));
#212469=CARTESIAN_POINT('Origin',(-6.29739814579425E-15,-11.5034818258363,
-234.90005));
#212470=CARTESIAN_POINT('',(32.4281746031746,-47.5009260671432,-235.35005));
#212471=CARTESIAN_POINT('',(32.1269841269841,-47.1665844797626,-234.90005));
#212472=CARTESIAN_POINT('Origin',(32.4281746031746,-47.5009260671432,-234.90005));
#212473=CARTESIAN_POINT('Origin',(-6.29739814579425E-15,-11.5034818258363,
-234.90005));
#212474=CARTESIAN_POINT('Origin',(-6.29739814579425E-15,-11.5034818258363,
-235.35005));
#212475=CARTESIAN_POINT('Origin',(31.625,-44.5701004838368,-234.90005));
#212476=CARTESIAN_POINT('',(30.875,-44.5701004838368,-234.90005));
#212477=CARTESIAN_POINT('',(30.425,-44.5701004838368,-235.35005));
#212478=CARTESIAN_POINT('Origin',(30.425,-44.5701004838368,-234.90005));
#212479=CARTESIAN_POINT('Origin',(31.625,-44.5701004838368,-235.35005));
#212480=CARTESIAN_POINT('Origin',(31.625,-44.5701004838368,-234.90005));
#212481=CARTESIAN_POINT('Origin',(31.625,-46.609348500795,-234.90005));
#212482=CARTESIAN_POINT('',(30.425,-46.609348500795,-235.35005));
#212483=CARTESIAN_POINT('',(30.875,-46.609348500795,-234.90005));
#212484=CARTESIAN_POINT('Origin',(30.425,-46.609348500795,-234.90005));
#212485=CARTESIAN_POINT('Origin',(31.625,-46.609348500795,-234.90005));
#212486=CARTESIAN_POINT('Origin',(31.625,-46.609348500795,-235.35005));
#212487=CARTESIAN_POINT('Origin',(30.425,-25.4138432731711,-234.90005));
#212488=CARTESIAN_POINT('',(30.875,-44.5701004838368,-234.90005));
#212489=CARTESIAN_POINT('',(30.425,-46.609348500795,-235.35005));
#212490=CARTESIAN_POINT('Origin',(31.625,23.6023848491226,-234.90005));
#212491=CARTESIAN_POINT('',(32.4281746031746,24.4939624154707,-235.35005));
#212492=CARTESIAN_POINT('',(30.425,23.6023848491226,-235.35005));
#212493=CARTESIAN_POINT('Origin',(31.625,23.6023848491226,-235.35005));
#212494=CARTESIAN_POINT('',(32.1269841269841,24.1596208280901,-234.90005));
#212495=CARTESIAN_POINT('Origin',(32.4281746031746,24.4939624154707,-234.90005));
#212496=CARTESIAN_POINT('',(30.875,23.6023848491226,-234.90005));
#212497=CARTESIAN_POINT('Origin',(31.625,23.6023848491226,-234.90005));
#212498=CARTESIAN_POINT('Origin',(30.425,23.6023848491226,-234.90005));
#212499=CARTESIAN_POINT('Origin',(30.425,-25.4138432731711,-234.90005));
#212500=CARTESIAN_POINT('',(30.875,21.5631368321642,-234.90005));
#212501=CARTESIAN_POINT('',(30.425,21.5631368321642,-235.35005));
#212502=CARTESIAN_POINT('Origin',(30.425,21.5631368321642,-234.90005));
#212503=CARTESIAN_POINT('',(30.425,21.5631368321642,-235.35005));
#212504=CARTESIAN_POINT('',(30.875,23.6023848491225,-234.90005));
#212505=CARTESIAN_POINT('Origin',(-6.29739814579425E-15,-11.5034818258363,
-234.90005));
#212506=CARTESIAN_POINT('',(34.6086426463969,22.4029239726848,-235.35005));
#212507=CARTESIAN_POINT('',(34.2872001450371,22.0880037949896,-234.90005));
#212508=CARTESIAN_POINT('Origin',(34.6086426463969,22.4029239726848,-234.90005));
#212509=CARTESIAN_POINT('Origin',(-6.29739814579425E-15,-11.5034818258363,
-234.90005));
#212510=CARTESIAN_POINT('Origin',(-6.29739814579425E-15,-11.5034818258363,
-235.35005));
#212511=CARTESIAN_POINT('Origin',(31.625,21.5631368321642,-234.90005));
#212512=CARTESIAN_POINT('',(31.625,20.8131368321642,-234.90005));
#212513=CARTESIAN_POINT('',(31.625,20.3631368321642,-235.35005));
#212514=CARTESIAN_POINT('Origin',(31.625,20.3631368321642,-234.90005));
#212515=CARTESIAN_POINT('Origin',(31.625,21.5631368321642,-235.35005));
#212516=CARTESIAN_POINT('Origin',(31.625,21.5631368321642,-234.90005));
#212517=CARTESIAN_POINT('Origin',(33.751462642771,21.5631368321642,-234.90005));
#212518=CARTESIAN_POINT('',(33.751462642771,20.3631368321642,-235.35005));
#212519=CARTESIAN_POINT('',(33.751462642771,20.8131368321642,-234.90005));
#212520=CARTESIAN_POINT('Origin',(33.751462642771,20.3631368321642,-234.90005));
#212521=CARTESIAN_POINT('Origin',(33.751462642771,21.5631368321642,-234.90005));
#212522=CARTESIAN_POINT('Origin',(33.751462642771,21.5631368321642,-235.35005));
#212523=CARTESIAN_POINT('Origin',(-296.501483394397,20.3631368321642,-234.90005));
#212524=CARTESIAN_POINT('',(-1.23757166668304E-15,20.8131368321642,-234.90005));
#212525=CARTESIAN_POINT('',(-296.501483394397,20.3631368321642,-235.35005));
#212526=CARTESIAN_POINT('Origin',(0.,-11.5034818258363,-235.65005));
#212527=CARTESIAN_POINT('',(-9.37533200891943E-16,-19.1590213785032,-236.10005));
#212528=CARTESIAN_POINT('Origin',(0.,-11.5034818258363,-236.10005));
#212529=CARTESIAN_POINT('',(-9.92642306853574E-16,-19.6090213785032,-235.65005));
#212530=CARTESIAN_POINT('Origin',(-9.37533200891943E-16,-19.1590213785032,
-235.65005));
#212531=CARTESIAN_POINT('Origin',(0.,-11.5034818258363,-235.65005));
#212532=CARTESIAN_POINT('Origin',(0.,-11.5034818258363,-235.65005));
#212533=CARTESIAN_POINT('',(-5.66442007243621E-16,-16.1288318258363,-235.65005));
#212534=CARTESIAN_POINT('Origin',(0.,-11.5034818258363,-235.65005));
#212535=CARTESIAN_POINT('',(-6.21551113205252E-16,-16.5788318258363,-236.10005));
#212536=CARTESIAN_POINT('Origin',(-6.21551113205252E-16,-16.5788318258363,
-235.65005));
#212537=CARTESIAN_POINT('Origin',(0.,-11.5034818258363,-236.10005));
#212538=CARTESIAN_POINT('Origin',(7.14692237356698E-14,623.509175991979,
-234.90005));
#212539=CARTESIAN_POINT('',(23.121090730514,-58.5338529228103,-234.90005));
#212540=CARTESIAN_POINT('',(23.1363368618431,-58.9835945769624,-235.35005));
#212541=CARTESIAN_POINT('Origin',(23.1363368618431,-58.9835945769624,-234.90005));
#212542=CARTESIAN_POINT('Origin',(7.14692237356698E-14,623.509175991979,
-235.35005));
#212543=CARTESIAN_POINT('Origin',(7.14692237356698E-14,623.509175991979,
-234.90005));
#212544=CARTESIAN_POINT('Origin',(22.9178089794592,-52.5372975341153,-234.90005));
#212545=CARTESIAN_POINT('',(25.8434867215177,-57.775656986236,-234.90005));
#212546=CARTESIAN_POINT('',(26.0629125521721,-58.168533945145,-235.35005));
#212547=CARTESIAN_POINT('Origin',(26.0629125521721,-58.168533945145,-234.90005));
#212548=CARTESIAN_POINT('Origin',(22.9178089794592,-52.5372975341153,-235.35005));
#212549=CARTESIAN_POINT('Origin',(22.9178089794592,-52.5372975341153,-234.90005));
#212550=CARTESIAN_POINT('Origin',(-6.29739814579425E-15,-11.5034818258363,
-234.90005));
#212551=CARTESIAN_POINT('',(43.9682643235187,-41.0972604351516,-234.90005));
#212552=CARTESIAN_POINT('',(44.3415797753222,-41.3485283667401,-235.35005));
#212553=CARTESIAN_POINT('Origin',(44.3415797753222,-41.3485283667401,-234.90005));
#212554=CARTESIAN_POINT('Origin',(-6.29739814579425E-15,-11.5034818258363,
-235.35005));
#212555=CARTESIAN_POINT('Origin',(-6.29739814579425E-15,-11.5034818258363,
-234.90005));
#212556=CARTESIAN_POINT('Origin',(38.9907249661392,-37.7470213473046,-234.90005));
#212557=CARTESIAN_POINT('',(44.9862076791357,-37.9798024422418,-234.90005));
#212558=CARTESIAN_POINT('',(45.4358688826104,-37.9972610243621,-235.35005));
#212559=CARTESIAN_POINT('Origin',(45.4358688826105,-37.9972610243621,-234.90005));
#212560=CARTESIAN_POINT('Origin',(38.9907249661392,-37.7470213473046,-235.35005));
#212561=CARTESIAN_POINT('Origin',(38.9907249661392,-37.7470213473046,-234.90005));
#212562=CARTESIAN_POINT('Origin',(-636.934816028482,-11.5034818258361,-234.90005));
#212563=CARTESIAN_POINT('',(44.9862076791357,14.9728387905693,-234.90005));
#212564=CARTESIAN_POINT('',(45.4358688826104,14.9902973726896,-235.35005));
#212565=CARTESIAN_POINT('Origin',(45.4358688826104,14.9902973726896,-234.90005));
#212566=CARTESIAN_POINT('Origin',(-636.934816028482,-11.5034818258361,-235.35005));
#212567=CARTESIAN_POINT('Origin',(-636.934816028482,-11.5034818258361,-234.90005));
#212568=CARTESIAN_POINT('Origin',(38.9907249661392,14.740057695632,-234.90005));
#212569=CARTESIAN_POINT('',(43.9682643235187,18.0902967834791,-234.90005));
#212570=CARTESIAN_POINT('',(44.3415797753222,18.3415647150676,-235.35005));
#212571=CARTESIAN_POINT('Origin',(44.3415797753222,18.3415647150676,-234.90005));
#212572=CARTESIAN_POINT('Origin',(38.9907249661392,14.740057695632,-235.35005));
#212573=CARTESIAN_POINT('Origin',(38.9907249661392,14.740057695632,-234.90005));
#212574=CARTESIAN_POINT('Origin',(-6.29739814579425E-15,-11.5034818258363,
-234.90005));
#212575=CARTESIAN_POINT('',(28.0091475455229,33.4908250781833,-234.90005));
#212576=CARTESIAN_POINT('',(28.2469610624189,33.872852212274,-235.35005));
#212577=CARTESIAN_POINT('Origin',(28.2469610624189,33.872852212274,-234.90005));
#212578=CARTESIAN_POINT('Origin',(-6.29739814579425E-15,-11.5034818258363,
-235.35005));
#212579=CARTESIAN_POINT('Origin',(-6.29739814579425E-15,-11.5034818258363,
-234.90005));
#212580=CARTESIAN_POINT('Origin',(24.838300653577,28.3971299569735,-234.90005));
#212581=CARTESIAN_POINT('',(25.5706493501227,34.3522676872588,-234.90005));
#212582=CARTESIAN_POINT('',(25.6255755023637,34.7989030170302,-235.35005));
#212583=CARTESIAN_POINT('Origin',(25.6255755023637,34.7989030170302,-234.90005));
#212584=CARTESIAN_POINT('Origin',(24.838300653577,28.3971299569735,-235.35005));
#212585=CARTESIAN_POINT('Origin',(24.838300653577,28.3971299569735,-234.90005));
#212586=CARTESIAN_POINT('Origin',(-2.61456814389029E-14,-173.57701443073,
-234.90005));
#212587=CARTESIAN_POINT('Origin',(-2.61456814389029E-14,-173.57701443073,
-235.35005));
#212588=CARTESIAN_POINT('Origin',(-2.61456814389029E-14,-173.57701443073,
-234.90005));
#212589=CARTESIAN_POINT('Origin',(7.14692237356698E-14,623.509175991979,
-234.90005));
#212590=CARTESIAN_POINT('',(23.0651882489741,-56.8848001909192,-235.35005));
#212591=CARTESIAN_POINT('',(23.0804343803032,-57.3345418450714,-234.90005));
#212592=CARTESIAN_POINT('Origin',(23.0651882489741,-56.8848001909192,-234.90005));
#212593=CARTESIAN_POINT('Origin',(7.14692237356698E-14,623.509175991979,
-234.90005));
#212594=CARTESIAN_POINT('Origin',(7.14692237356698E-14,623.509175991979,
-235.35005));
#212595=CARTESIAN_POINT('Origin',(22.9178089794592,-52.5372975341153,-234.90005));
#212596=CARTESIAN_POINT('',(25.0389253424516,-56.3351081369028,-235.35005));
#212597=CARTESIAN_POINT('',(25.258351173106,-56.7279850958119,-234.90005));
#212598=CARTESIAN_POINT('Origin',(25.0389253424516,-56.3351081369028,-234.90005));
#212599=CARTESIAN_POINT('Origin',(22.9178089794592,-52.5372975341153,-234.90005));
#212600=CARTESIAN_POINT('Origin',(22.9178089794592,-52.5372975341153,-235.35005));
#212601=CARTESIAN_POINT('Origin',(-6.29739814579425E-15,-11.5034818258363,
-234.90005));
#212602=CARTESIAN_POINT('',(42.5994410002394,-40.1759446859937,-235.35005));
#212603=CARTESIAN_POINT('',(42.9727564520428,-40.4272126175822,-234.90005));
#212604=CARTESIAN_POINT('Origin',(42.5994410002394,-40.1759446859937,-234.90005));
#212605=CARTESIAN_POINT('Origin',(-6.29739814579425E-15,-11.5034818258363,
-234.90005));
#212606=CARTESIAN_POINT('Origin',(-6.29739814579425E-15,-11.5034818258363,
-235.35005));
#212607=CARTESIAN_POINT('Origin',(38.9907249661392,-37.7470213473046,-234.90005));
#212608=CARTESIAN_POINT('',(43.3374499330618,-37.915787641134,-235.35005));
#212609=CARTESIAN_POINT('',(43.7871111365364,-37.9332462232544,-234.90005));
#212610=CARTESIAN_POINT('Origin',(43.3374499330618,-37.915787641134,-234.90005));
#212611=CARTESIAN_POINT('Origin',(38.9907249661392,-37.7470213473046,-234.90005));
#212612=CARTESIAN_POINT('Origin',(38.9907249661392,-37.7470213473046,-235.35005));
#212613=CARTESIAN_POINT('Origin',(-636.934816028482,-11.5034818258361,-234.90005));
#212614=CARTESIAN_POINT('',(43.3374499330618,14.9088239894616,-235.35005));
#212615=CARTESIAN_POINT('',(43.7871111365364,14.9262825715819,-234.90005));
#212616=CARTESIAN_POINT('Origin',(43.3374499330618,14.9088239894616,-234.90005));
#212617=CARTESIAN_POINT('Origin',(-636.934816028482,-11.5034818258361,-234.90005));
#212618=CARTESIAN_POINT('Origin',(-636.934816028482,-11.5034818258361,-235.35005));
#212619=CARTESIAN_POINT('Origin',(38.9907249661392,14.740057695632,-234.90005));
#212620=CARTESIAN_POINT('',(42.5994410002394,17.1689810343211,-235.35005));
#212621=CARTESIAN_POINT('',(42.9727564520429,17.4202489659097,-234.90005));
#212622=CARTESIAN_POINT('Origin',(42.5994410002394,17.1689810343211,-234.90005));
#212623=CARTESIAN_POINT('Origin',(38.9907249661392,14.740057695632,-234.90005));
#212624=CARTESIAN_POINT('Origin',(38.9907249661392,14.740057695632,-235.35005));
#212625=CARTESIAN_POINT('Origin',(-6.29739814579425E-15,-11.5034818258363,
-234.90005));
#212626=CARTESIAN_POINT('',(27.1371646502378,32.0900589198506,-235.35005));
#212627=CARTESIAN_POINT('',(27.3749781671338,32.4720860539414,-234.90005));
#212628=CARTESIAN_POINT('Origin',(27.1371646502378,32.0900589198506,-234.90005));
#212629=CARTESIAN_POINT('Origin',(-6.29739814579425E-15,-11.5034818258363,
-234.90005));
#212630=CARTESIAN_POINT('Origin',(-6.29739814579425E-15,-11.5034818258363,
-235.35005));
#212631=CARTESIAN_POINT('Origin',(24.838300653577,28.3971299569735,-234.90005));
#212632=CARTESIAN_POINT('',(25.3692534585727,32.7146048114303,-235.35005));
#212633=CARTESIAN_POINT('',(25.4241796108136,33.1612401412018,-234.90005));
#212634=CARTESIAN_POINT('Origin',(25.3692534585727,32.7146048114303,-234.90005));
#212635=CARTESIAN_POINT('Origin',(24.838300653577,28.3971299569735,-234.90005));
#212636=CARTESIAN_POINT('Origin',(24.838300653577,28.3971299569735,-235.35005));
#212637=CARTESIAN_POINT('Origin',(-2.61456814389029E-14,-173.57701443073,
-234.90005));
#212638=CARTESIAN_POINT('Origin',(-2.61456814389029E-14,-173.57701443073,
-234.90005));
#212639=CARTESIAN_POINT('Origin',(-2.61456814389029E-14,-173.57701443073,
-235.35005));
#212640=CARTESIAN_POINT('Origin',(6.95148506756697,-6.01736880073005,-234.90005));
#212641=CARTESIAN_POINT('',(6.08254860609655,-5.18975208634635,-235.35005));
#212642=CARTESIAN_POINT('',(6.40839977914796,-5.50010835424024,-234.90005));
#212643=CARTESIAN_POINT('Origin',(6.08254860609655,-5.18975208634635,-234.90005));
#212644=CARTESIAN_POINT('',(6.36274467860838,-6.48200280121742,-234.90005));
#212645=CARTESIAN_POINT('Origin',(6.95148506756697,-6.01736880073005,-234.90005));
#212646=CARTESIAN_POINT('',(5.76949205973895,-5.81026368383122,-235.35005));
#212647=CARTESIAN_POINT('Ctrl Pts',(5.76949205973895,-5.81026368383121,
-235.35005));
#212648=CARTESIAN_POINT('Ctrl Pts',(5.82092507341363,-5.86238576252255,
-235.35005));
#212649=CARTESIAN_POINT('Ctrl Pts',(5.87146206806168,-5.91503600112616,
-235.33821291833));
#212650=CARTESIAN_POINT('Ctrl Pts',(6.00423457196882,-6.05699737629993,
-235.282379503985));
#212651=CARTESIAN_POINT('Ctrl Pts',(6.07889780142463,-6.14101690884923,
-235.222495970419));
#212652=CARTESIAN_POINT('Ctrl Pts',(6.22023885093968,-6.30512731290958,
-235.083822800187));
#212653=CARTESIAN_POINT('Ctrl Pts',(6.29326617328539,-6.39403176703485,
-234.990808270705));
#212654=CARTESIAN_POINT('Ctrl Pts',(6.36151501319033,-6.48044497931282,
-234.901656863128));
#212655=CARTESIAN_POINT('Ctrl Pts',(6.36212991841606,-6.48122383507554,
-234.900853430267));
#212656=CARTESIAN_POINT('Ctrl Pts',(6.36274467860838,-6.48200280121742,
-234.90005));
#212657=CARTESIAN_POINT('Origin',(6.95148506756697,-6.01736880073005,-235.35005));
#212658=CARTESIAN_POINT('Origin',(-147.944423723881,-166.906703884593,-234.90005));
#212659=CARTESIAN_POINT('',(7.1259980697973,-4.09420716929315,-235.35005));
#212660=CARTESIAN_POINT('',(7.45184924284871,-4.40456343718705,-234.90005));
#212661=CARTESIAN_POINT('Origin',(7.1259980697973,-4.09420716929315,-234.90005));
#212662=CARTESIAN_POINT('',(6.10697827817035,-5.81657868152891,-234.90005));
#212663=CARTESIAN_POINT('',(-147.944423723881,-166.906703884593,-235.35005));
#212664=CARTESIAN_POINT('Origin',(7.99493453126772,-4.92182388367686,-234.90005));
#212665=CARTESIAN_POINT('',(8.92138760391815,-4.15914131263135,-235.35005));
#212666=CARTESIAN_POINT('Origin',(7.99493453126772,-4.92182388367686,-235.35005));
#212667=CARTESIAN_POINT('',(8.57396770167424,-4.44514727677342,-234.90005));
#212668=CARTESIAN_POINT('Origin',(8.92138760391815,-4.15914131263135,-234.90005));
#212669=CARTESIAN_POINT('Origin',(7.99493453126772,-4.92182388367686,-234.90005));
#212670=CARTESIAN_POINT('Origin',(0.,-11.5034818258363,-234.90005));
#212671=CARTESIAN_POINT('',(11.4710456282303,-10.1086318165856,-235.35005));
#212672=CARTESIAN_POINT('',(11.0243360211906,-10.1629505700546,-234.90005));
#212673=CARTESIAN_POINT('Origin',(11.4710456282303,-10.1086318165856,-234.90005));
#212674=CARTESIAN_POINT('Origin',(0.,-11.5034818258363,-234.90005));
#212675=CARTESIAN_POINT('Origin',(0.,-11.5034818258363,-235.35005));
#212676=CARTESIAN_POINT('Origin',(10.2798200094577,-10.2534818258363,-234.90005));
#212677=CARTESIAN_POINT('',(10.2798200094577,-11.4534818258363,-235.35005));
#212678=CARTESIAN_POINT('',(10.2798200094577,-11.0034818258363,-234.90005));
#212679=CARTESIAN_POINT('Origin',(10.2798200094577,-11.4534818258363,-234.90005));
#212680=CARTESIAN_POINT('Origin',(10.2798200094577,-10.2534818258363,-234.90005));
#212681=CARTESIAN_POINT('Origin',(10.2798200094577,-10.2534818258363,-235.35005));
#212682=CARTESIAN_POINT('Origin',(-296.501483394397,-11.4534818258365,-234.90005));
#212683=CARTESIAN_POINT('',(8.76687405914145,-11.4534818258363,-235.35005));
#212684=CARTESIAN_POINT('',(8.76687405914145,-11.0034818258363,-234.90005));
#212685=CARTESIAN_POINT('Origin',(8.76687405914145,-11.4534818258363,-234.90005));
#212686=CARTESIAN_POINT('',(-2.22174260618994E-13,-11.0034818258363,-234.90005));
#212687=CARTESIAN_POINT('',(-296.501483394397,-11.4534818258365,-235.35005));
#212688=CARTESIAN_POINT('Origin',(8.76687405914145,-10.2534818258363,-234.90005));
#212689=CARTESIAN_POINT('',(8.02438338364376,-10.3593477636964,-234.90005));
#212690=CARTESIAN_POINT('',(8.1016440740309,-11.2522155575736,-235.35005));
#212691=CARTESIAN_POINT('Ctrl Pts',(8.02438338364377,-10.3593477636964,
-234.90005));
#212692=CARTESIAN_POINT('Ctrl Pts',(8.02452345554005,-10.3603301578355,
-234.900853430281));
#212693=CARTESIAN_POINT('Ctrl Pts',(8.02466334747473,-10.3613125808142,
-234.901656863113));
#212694=CARTESIAN_POINT('Ctrl Pts',(8.04016643948375,-10.4703300185997,
-234.990808271414));
#212695=CARTESIAN_POINT('Ctrl Pts',(8.05417784702261,-10.5845257804583,
-235.083822800183));
#212696=CARTESIAN_POINT('Ctrl Pts',(8.07553226267948,-10.8000565344901,
-235.222495970419));
#212697=CARTESIAN_POINT('Ctrl Pts',(8.08487817822972,-10.9120678443883,
-235.282379503985));
#212698=CARTESIAN_POINT('Ctrl Pts',(8.09610373786709,-11.1061182415686,
-235.33821291833));
#212699=CARTESIAN_POINT('Ctrl Pts',(8.09937411333572,-11.1790246205581,
-235.35005));
#212700=CARTESIAN_POINT('Ctrl Pts',(8.10164407403091,-11.2522155575736,
-235.35005));
#212701=CARTESIAN_POINT('Origin',(8.76687405914145,-10.2534818258363,-234.90005));
#212702=CARTESIAN_POINT('Origin',(8.76687405914145,-10.2534818258363,-235.35005));
#212703=CARTESIAN_POINT('Origin',(8.76687405914144,-12.7534818258363,-234.90005));
#212704=CARTESIAN_POINT('',(8.76687405914144,-11.5534818258363,-235.35005));
#212705=CARTESIAN_POINT('',(8.76687405914144,-12.0034818258363,-234.90005));
#212706=CARTESIAN_POINT('Origin',(8.76687405914144,-11.5534818258363,-234.90005));
#212707=CARTESIAN_POINT('',(8.02438338364376,-12.6476158879763,-234.90005));
#212708=CARTESIAN_POINT('Origin',(8.76687405914144,-12.7534818258363,-234.90005));
#212709=CARTESIAN_POINT('',(8.1016440740309,-11.7547480940991,-235.35005));
#212710=CARTESIAN_POINT('Ctrl Pts',(8.10164407403091,-11.7547480940991,
-235.35005));
#212711=CARTESIAN_POINT('Ctrl Pts',(8.09937411333572,-11.8279390311146,
-235.35005));
#212712=CARTESIAN_POINT('Ctrl Pts',(8.09610373786709,-11.9008454101041,
-235.33821291833));
#212713=CARTESIAN_POINT('Ctrl Pts',(8.08487817822972,-12.0948958072844,
-235.282379503985));
#212714=CARTESIAN_POINT('Ctrl Pts',(8.07553226267947,-12.2069071171825,
-235.222495970419));
#212715=CARTESIAN_POINT('Ctrl Pts',(8.05417784702484,-12.4224378711919,
-235.083822800197));
#212716=CARTESIAN_POINT('Ctrl Pts',(8.04016643880974,-12.5366336378126,
-234.990808267567));
#212717=CARTESIAN_POINT('Ctrl Pts',(8.02466334748842,-12.6456510707622,
-234.90165686319));
#212718=CARTESIAN_POINT('Ctrl Pts',(8.0245234555264,-12.6466334939328,-234.900853430203));
#212719=CARTESIAN_POINT('Ctrl Pts',(8.02438338364376,-12.6476158879763,
-234.90005));
#212720=CARTESIAN_POINT('Origin',(8.76687405914144,-12.7534818258363,-235.35005));
#212721=CARTESIAN_POINT('Origin',(-296.501483394397,-11.5534818258362,-234.90005));
#212722=CARTESIAN_POINT('',(10.2798200094577,-11.5534818258363,-235.35005));
#212723=CARTESIAN_POINT('',(10.2798200094577,-12.0034818258363,-234.90005));
#212724=CARTESIAN_POINT('Origin',(10.2798200094577,-11.5534818258363,-234.90005));
#212725=CARTESIAN_POINT('',(-2.22174260618994E-13,-12.0034818258363,-234.90005));
#212726=CARTESIAN_POINT('',(-296.501483394397,-11.5534818258362,-235.35005));
#212727=CARTESIAN_POINT('Origin',(10.2798200094577,-12.7534818258363,-234.90005));
#212728=CARTESIAN_POINT('',(11.4710456282303,-12.8983318350871,-235.35005));
#212729=CARTESIAN_POINT('',(11.0243360211906,-12.844013081618,-234.90005));
#212730=CARTESIAN_POINT('Origin',(11.4710456282303,-12.8983318350871,-234.90005));
#212731=CARTESIAN_POINT('Origin',(10.2798200094577,-12.7534818258363,-234.90005));
#212732=CARTESIAN_POINT('Origin',(10.2798200094577,-12.7534818258363,-235.35005));
#212733=CARTESIAN_POINT('Origin',(0.,-11.5034818258363,-234.90005));
#212734=CARTESIAN_POINT('',(8.92138760391814,-18.8478223390413,-235.35005));
#212735=CARTESIAN_POINT('',(8.57396770167423,-18.5618163748993,-234.90005));
#212736=CARTESIAN_POINT('Origin',(8.92138760391814,-18.8478223390413,-234.90005));
#212737=CARTESIAN_POINT('Origin',(0.,-11.5034818258363,-234.90005));
#212738=CARTESIAN_POINT('Origin',(0.,-11.5034818258363,-235.35005));
#212739=CARTESIAN_POINT('Origin',(7.99493453126771,-18.0851397679958,-234.90005));
#212740=CARTESIAN_POINT('',(7.1259980697973,-18.9127564823795,-235.35005));
#212741=CARTESIAN_POINT('',(7.4518492428487,-18.6024002144856,-234.90005));
#212742=CARTESIAN_POINT('Origin',(7.12599806979729,-18.9127564823795,-234.90005));
#212743=CARTESIAN_POINT('Origin',(7.99493453126771,-18.0851397679958,-234.90005));
#212744=CARTESIAN_POINT('Origin',(7.99493453126771,-18.0851397679958,-235.35005));
#212745=CARTESIAN_POINT('Origin',(-5.70871573332976,-5.43725435410305,-234.90005));
#212746=CARTESIAN_POINT('',(6.08254860609655,-17.8172115653263,-235.35005));
#212747=CARTESIAN_POINT('',(6.40839977914795,-17.5068552974324,-234.90005));
#212748=CARTESIAN_POINT('Origin',(6.08254860609655,-17.8172115653263,-234.90005));
#212749=CARTESIAN_POINT('',(6.40839977914795,-17.5068552974324,-234.90005));
#212750=CARTESIAN_POINT('',(7.1259980697973,-18.9127564823795,-235.35005));
#212751=CARTESIAN_POINT('Origin',(6.95148506756696,-16.9895948509426,-234.90005));
#212752=CARTESIAN_POINT('',(6.36274467860837,-16.5249608504553,-234.90005));
#212753=CARTESIAN_POINT('',(5.76949205973894,-17.1966999678414,-235.35005));
#212754=CARTESIAN_POINT('Ctrl Pts',(6.36274467860837,-16.5249608504552,
-234.90005));
#212755=CARTESIAN_POINT('Ctrl Pts',(6.36212991839126,-16.5257398166285,
-234.900853430299));
#212756=CARTESIAN_POINT('Ctrl Pts',(6.36151501321541,-16.5265186723281,
-234.901656863095));
#212757=CARTESIAN_POINT('Ctrl Pts',(6.2932661720145,-16.6129318862469,-234.990808272352));
#212758=CARTESIAN_POINT('Ctrl Pts',(6.22023885094755,-16.7018363387539,
-235.083822800179));
#212759=CARTESIAN_POINT('Ctrl Pts',(6.0788978014246,-16.8659467428234,-235.222495970419));
#212760=CARTESIAN_POINT('Ctrl Pts',(6.0042345719688,-16.9499662753727,-235.282379503985));
#212761=CARTESIAN_POINT('Ctrl Pts',(5.87146206806167,-17.0919276505465,
-235.33821291833));
#212762=CARTESIAN_POINT('Ctrl Pts',(5.82092507341363,-17.1445778891501,
-235.35005));
#212763=CARTESIAN_POINT('Ctrl Pts',(5.76949205973896,-17.1966999678414,
-235.35005));
#212764=CARTESIAN_POINT('Origin',(6.95148506756696,-16.9895948509426,-234.90005));
#212765=CARTESIAN_POINT('Origin',(6.95148506756696,-16.9895948509426,-235.35005));
#212766=CARTESIAN_POINT('Origin',(1.25,-2.73660776669487,-234.90005));
#212767=CARTESIAN_POINT('',(0.0499999999999959,-2.73660776669487,-235.35005));
#212768=CARTESIAN_POINT('',(0.5,-2.73660776669487,-234.90005));
#212769=CARTESIAN_POINT('Origin',(0.0499999999999959,-2.73660776669487,
-234.90005));
#212770=CARTESIAN_POINT('',(1.14413406213993,-3.47909844219256,-234.90005));
#212771=CARTESIAN_POINT('Origin',(1.25,-2.73660776669487,-234.90005));
#212772=CARTESIAN_POINT('',(0.251266268262739,-3.40183775180542,-235.35005));
#212773=CARTESIAN_POINT('Ctrl Pts',(0.251266268262739,-3.40183775180541,
-235.35005));
#212774=CARTESIAN_POINT('Ctrl Pts',(0.32445720527824,-3.4041077125006,-235.35005));
#212775=CARTESIAN_POINT('Ctrl Pts',(0.397363584267788,-3.40737808796923,
-235.33821291833));
#212776=CARTESIAN_POINT('Ctrl Pts',(0.591413981447983,-3.4186036476066,
-235.282379503985));
#212777=CARTESIAN_POINT('Ctrl Pts',(0.703425291346113,-3.42794956315684,
-235.222495970419));
#212778=CARTESIAN_POINT('Ctrl Pts',(0.918956045360102,-3.44930397881193,
-235.083822800194));
#212779=CARTESIAN_POINT('Ctrl Pts',(1.03315181082866,-3.46331538686338,
-234.990808268499));
#212780=CARTESIAN_POINT('Ctrl Pts',(1.14216924494769,-3.47881847835101,
-234.901656863173));
#212781=CARTESIAN_POINT('Ctrl Pts',(1.14315166807461,-3.4789583703068,-234.900853430221));
#212782=CARTESIAN_POINT('Ctrl Pts',(1.14413406213993,-3.47909844219256,
-234.90005));
#212783=CARTESIAN_POINT('Origin',(1.25,-2.73660776669487,-235.35005));
#212784=CARTESIAN_POINT('Origin',(0.0499999999999945,-25.4138432731711,
-234.90005));
#212785=CARTESIAN_POINT('',(0.0499999999999981,-1.22366181637858,-235.35005));
#212786=CARTESIAN_POINT('',(0.5,-1.22366181637858,-234.90005));
#212787=CARTESIAN_POINT('Origin',(0.0499999999999981,-1.22366181637858,
-234.90005));
#212788=CARTESIAN_POINT('',(0.5,-1.22366181637858,-234.90005));
#212789=CARTESIAN_POINT('',(0.0499999999999959,-2.73660776669487,-235.35005));
#212790=CARTESIAN_POINT('Origin',(1.25,-1.22366181637858,-234.90005));
#212791=CARTESIAN_POINT('',(1.39485000925072,-0.0324361976060192,-235.35005));
#212792=CARTESIAN_POINT('Origin',(1.25,-1.22366181637858,-235.35005));
#212793=CARTESIAN_POINT('',(1.3405312557817,-0.479145804645727,-234.90005));
#212794=CARTESIAN_POINT('Origin',(1.39485000925072,-0.0324361976060193,
-234.90005));
#212795=CARTESIAN_POINT('Origin',(1.25,-1.22366181637858,-234.90005));
#212796=CARTESIAN_POINT('Origin',(0.,-11.5034818258363,-234.90005));
#212797=CARTESIAN_POINT('',(6.90132755171766,-2.23513934310776,-235.35005));
#212798=CARTESIAN_POINT('',(6.63257355852517,-2.59607048770891,-234.90005));
#212799=CARTESIAN_POINT('Origin',(6.90132755171766,-2.23513934310776,-234.90005));
#212800=CARTESIAN_POINT('Origin',(0.,-11.5034818258363,-234.90005));
#212801=CARTESIAN_POINT('Origin',(0.,-11.5034818258363,-235.35005));
#212802=CARTESIAN_POINT('Origin',(6.18465023653769,-3.19762239537748,-234.90005));
#212803=CARTESIAN_POINT('',(7.05358669800811,-4.02523910976119,-235.35005));
#212804=CARTESIAN_POINT('',(6.7277355249567,-3.7148828418673,-234.90005));
#212805=CARTESIAN_POINT('Origin',(7.05358669800812,-4.0252391097612,-234.90005));
#212806=CARTESIAN_POINT('Origin',(6.18465023653769,-3.19762239537748,-234.90005));
#212807=CARTESIAN_POINT('Origin',(6.18465023653769,-3.19762239537748,-235.35005));
#212808=CARTESIAN_POINT('Origin',(-148.016835095671,-166.837735825062,-234.90005));
#212809=CARTESIAN_POINT('',(6.01013723430737,-5.12078402681439,-235.35005));
#212810=CARTESIAN_POINT('',(5.68428606125595,-4.81042775892049,-234.90005));
#212811=CARTESIAN_POINT('Origin',(6.01013723430736,-5.12078402681438,-234.90005));
#212812=CARTESIAN_POINT('',(5.38286456027834,-5.12689808620916,-234.90005));
#212813=CARTESIAN_POINT('',(-148.016835095671,-166.837735825062,-235.35005));
#212814=CARTESIAN_POINT('Origin',(5.14120077283694,-4.29316731243068,-234.90005));
#212815=CARTESIAN_POINT('',(4.70577833960231,-4.90382867901287,-234.90005));
#212816=CARTESIAN_POINT('',(5.40560135635379,-5.46367674487279,-235.35005));
#212817=CARTESIAN_POINT('Ctrl Pts',(4.70577833960231,-4.90382867901288,
-234.90005));
#212818=CARTESIAN_POINT('Ctrl Pts',(4.70658630944744,-4.9044047891374,-234.900853430186));
#212819=CARTESIAN_POINT('Ctrl Pts',(4.70739417634903,-4.90498104967104,
-234.901656863208));
#212820=CARTESIAN_POINT('Ctrl Pts',(4.79702737541902,-4.96894225601165,
-234.990808266726));
#212821=CARTESIAN_POINT('Ctrl Pts',(4.88938149377006,-5.03755500803373,
-235.083822800201));
#212822=CARTESIAN_POINT('Ctrl Pts',(5.0601779954728,-5.17073936145207,-235.222495970419));
#212823=CARTESIAN_POINT('Ctrl Pts',(5.14773261812957,-5.24122388268896,
-235.282379503985));
#212824=CARTESIAN_POINT('Ctrl Pts',(5.29598922334359,-5.36692809441377,
-235.33821291833));
#212825=CARTESIAN_POINT('Ctrl Pts',(5.35103724699188,-5.41484208553839,
-235.35005));
#212826=CARTESIAN_POINT('Ctrl Pts',(5.40560135635379,-5.46367674487279,
-235.35005));
#212827=CARTESIAN_POINT('Origin',(5.14120077283694,-4.29316731243068,-234.90005));
#212828=CARTESIAN_POINT('Origin',(5.14120077283694,-4.29316731243068,-235.35005));
#212829=CARTESIAN_POINT('Origin',(5.14120077283693,-18.713796339242,-234.90005));
#212830=CARTESIAN_POINT('',(5.40560135635378,-17.5432869067998,-235.35005));
#212831=CARTESIAN_POINT('',(4.7057783396023,-18.1031349726598,-234.90005));
#212832=CARTESIAN_POINT('Ctrl Pts',(5.40560135635379,-17.5432869067999,
-235.35005));
#212833=CARTESIAN_POINT('Ctrl Pts',(5.35103724699192,-17.5921215661342,
-235.35005));
#212834=CARTESIAN_POINT('Ctrl Pts',(5.29598922334368,-17.6400355572588,
-235.33821291833));
#212835=CARTESIAN_POINT('Ctrl Pts',(5.14773261813006,-17.7657397689833,
-235.282379503985));
#212836=CARTESIAN_POINT('Ctrl Pts',(5.06017799547341,-17.8362242902201,
-235.222495970419));
#212837=CARTESIAN_POINT('Ctrl Pts',(4.88938149380987,-17.9694086436079,
-235.083822800233));
#212838=CARTESIAN_POINT('Ctrl Pts',(4.79702736710125,-18.0380214015964,
-234.990808258517));
#212839=CARTESIAN_POINT('Ctrl Pts',(4.70739417651803,-18.101982601881,-234.901656863374));
#212840=CARTESIAN_POINT('Ctrl Pts',(4.70658630927984,-18.1025588626547,
-234.900853430019));
#212841=CARTESIAN_POINT('Ctrl Pts',(4.7057783396023,-18.1031349726598,-234.90005));
#212842=CARTESIAN_POINT('',(6.01013723430735,-17.8861796248583,-235.35005));
#212843=CARTESIAN_POINT('Origin',(5.14120077283693,-18.713796339242,-235.35005));
#212844=CARTESIAN_POINT('',(5.68428606125594,-18.1965358927522,-234.90005));
#212845=CARTESIAN_POINT('Origin',(6.01013723430735,-17.8861796248583,-234.90005));
#212846=CARTESIAN_POINT('Origin',(5.14120077283693,-18.713796339242,-234.90005));
#212847=CARTESIAN_POINT('Origin',(-5.78112710511895,-5.50622241363502,-234.90005));
#212848=CARTESIAN_POINT('',(7.0535866980081,-18.9817245419115,-235.35005));
#212849=CARTESIAN_POINT('',(6.72773552495669,-19.2920808098054,-234.90005));
#212850=CARTESIAN_POINT('Origin',(7.0535866980081,-18.9817245419115,-234.90005));
#212851=CARTESIAN_POINT('',(6.7277355249567,-19.2920808098054,-234.90005));
#212852=CARTESIAN_POINT('',(6.01013723430735,-17.8861796248583,-235.35005));
#212853=CARTESIAN_POINT('Origin',(6.18465023653768,-19.8093412562951,-234.90005));
#212854=CARTESIAN_POINT('',(6.90132755171765,-20.7718243085649,-235.35005));
#212855=CARTESIAN_POINT('',(6.63257355852516,-20.4108931639637,-234.90005));
#212856=CARTESIAN_POINT('Origin',(6.90132755171765,-20.7718243085649,-234.90005));
#212857=CARTESIAN_POINT('Origin',(6.18465023653768,-19.8093412562951,-234.90005));
#212858=CARTESIAN_POINT('Origin',(6.18465023653768,-19.8093412562951,-235.35005));
#212859=CARTESIAN_POINT('Origin',(0.,-11.5034818258363,-234.90005));
#212860=CARTESIAN_POINT('',(1.39485000925072,-22.9745274540666,-235.35005));
#212861=CARTESIAN_POINT('',(1.3405312557817,-22.5278178470269,-234.90005));
#212862=CARTESIAN_POINT('Origin',(1.39485000925072,-22.9745274540666,-234.90005));
#212863=CARTESIAN_POINT('Origin',(0.,-11.5034818258363,-234.90005));
#212864=CARTESIAN_POINT('Origin',(0.,-11.5034818258363,-235.35005));
#212865=CARTESIAN_POINT('Origin',(1.25,-21.7833018352941,-234.90005));
#212866=CARTESIAN_POINT('',(0.0499999999999969,-21.7833018352941,-235.35005));
#212867=CARTESIAN_POINT('',(0.5,-21.7833018352941,-234.90005));
#212868=CARTESIAN_POINT('Origin',(0.0499999999999947,-21.7833018352941,
-234.90005));
#212869=CARTESIAN_POINT('Origin',(1.25,-21.7833018352941,-234.90005));
#212870=CARTESIAN_POINT('Origin',(1.25,-21.7833018352941,-235.35005));
#212871=CARTESIAN_POINT('Origin',(0.0499999999999945,-25.4138432731711,
-234.90005));
#212872=CARTESIAN_POINT('',(0.0499999999999948,-20.2703558849778,-235.35005));
#212873=CARTESIAN_POINT('',(0.5,-20.2703558849778,-234.90005));
#212874=CARTESIAN_POINT('Origin',(0.049999999999997,-20.2703558849778,-234.90005));
#212875=CARTESIAN_POINT('',(0.5,-20.2703558849778,-234.90005));
#212876=CARTESIAN_POINT('',(0.0499999999999947,-21.7833018352941,-235.35005));
#212877=CARTESIAN_POINT('Origin',(1.25,-20.2703558849778,-234.90005));
#212878=CARTESIAN_POINT('',(1.14413406213993,-19.5278652094801,-234.90005));
#212879=CARTESIAN_POINT('',(0.251266268262739,-19.6051258998672,-235.35005));
#212880=CARTESIAN_POINT('Ctrl Pts',(1.14413406213993,-19.5278652094801,
-234.90005));
#212881=CARTESIAN_POINT('Ctrl Pts',(1.14315166831933,-19.5280052813309,
-234.900853430021));
#212882=CARTESIAN_POINT('Ctrl Pts',(1.14216924470093,-19.5281451733567,
-234.901656863372));
#212883=CARTESIAN_POINT('Ctrl Pts',(1.03315182300962,-19.543648263077,-234.990808258614));
#212884=CARTESIAN_POINT('Ctrl Pts',(0.918956045300628,-19.5576596728666,
-235.083822800233));
#212885=CARTESIAN_POINT('Ctrl Pts',(0.703425291345192,-19.5790140885159,
-235.222495970419));
#212886=CARTESIAN_POINT('Ctrl Pts',(0.591413981447227,-19.5883600040661,
-235.282379503985));
#212887=CARTESIAN_POINT('Ctrl Pts',(0.397363584267675,-19.5995855637034,
-235.33821291833));
#212888=CARTESIAN_POINT('Ctrl Pts',(0.324457205278181,-19.602855939172,
-235.35005));
#212889=CARTESIAN_POINT('Ctrl Pts',(0.25126626826274,-19.6051258998672,
-235.35005));
#212890=CARTESIAN_POINT('Origin',(1.25,-20.2703558849778,-234.90005));
#212891=CARTESIAN_POINT('Origin',(1.25,-20.2703558849778,-235.35005));
#212892=CARTESIAN_POINT('Origin',(0.,-178.58000002,-203.84995));
#212893=CARTESIAN_POINT('',(43.6624048158998,50.3711948984507,-205.34995));
#212894=CARTESIAN_POINT('Origin',(0.,-178.58000002,-205.34995));
#212895=CARTESIAN_POINT('',(43.9433571680673,51.844416014308,-203.876128609656));
#212896=CARTESIAN_POINT('Origin',(0.,-178.58000002,-203.876128609656));
#212897=CARTESIAN_POINT('Origin',(43.6624048158998,50.3711948984507,-203.84995));
#212898=CARTESIAN_POINT('Origin',(41.3132181298675,38.0528376956935,-203.84995));
#212899=CARTESIAN_POINT('',(50.148669624411,48.964302343774,-203.876128609656));
#212900=CARTESIAN_POINT('',(49.2048636720257,47.7987359558583,-205.34995));
#212901=CARTESIAN_POINT('Origin',(49.2048636720257,47.7987359558583,-203.84995));
#212902=CARTESIAN_POINT('Origin',(41.3132181298675,38.0528376956935,-205.34995));
#212903=CARTESIAN_POINT('Origin',(41.3132181298675,38.0528376956935,-203.876128609656));
#212904=CARTESIAN_POINT('Origin',(0.,-12.9675000200281,-203.84995));
#212905=CARTESIAN_POINT('',(61.5592179767879,37.6378345921813,-203.876128609656));
#212906=CARTESIAN_POINT('',(60.4006636863987,36.6854341319664,-205.34995));
#212907=CARTESIAN_POINT('Origin',(60.4006636863987,36.6854341319665,-203.84995));
#212908=CARTESIAN_POINT('Origin',(0.,-12.9675000200281,-205.34995));
#212909=CARTESIAN_POINT('Origin',(0.,-12.9675000200281,-203.876128609656));
#212910=CARTESIAN_POINT('Origin',(50.7133971693864,28.7219255026674,-203.84995));
#212911=CARTESIAN_POINT('',(64.7425725698088,29.2764536470619,-203.876128609656));
#212912=CARTESIAN_POINT('',(63.2439712523603,29.2172187609027,-205.34995));
#212913=CARTESIAN_POINT('Origin',(63.2439712523603,29.2172187609027,-203.84995));
#212914=CARTESIAN_POINT('Origin',(50.7133971693864,28.7219255026674,-205.34995));
#212915=CARTESIAN_POINT('Origin',(50.7133971693864,28.7219255026673,-203.876128609656));
#212916=CARTESIAN_POINT('Origin',(-1004.,-12.967500020028,-203.84995));
#212917=CARTESIAN_POINT('',(64.7425725698087,-55.2114536871185,-203.876128609656));
#212918=CARTESIAN_POINT('',(63.2439712523603,-55.1522188009592,-205.34995));
#212919=CARTESIAN_POINT('Origin',(63.2439712523603,-55.1522188009592,-203.84995));
#212920=CARTESIAN_POINT('Origin',(-1004.,-12.967500020028,-205.34995));
#212921=CARTESIAN_POINT('Origin',(-1004.,-12.967500020028,-203.87612860965));
#212922=CARTESIAN_POINT('Origin',(50.7133971693864,-54.6569255427236,-203.84995));
#212923=CARTESIAN_POINT('',(61.5592179767879,-63.5728346322375,-203.876128609656));
#212924=CARTESIAN_POINT('',(60.4006636863987,-62.6204341720228,-205.34995));
#212925=CARTESIAN_POINT('Origin',(60.4006636863987,-62.6204341720228,-203.84995));
#212926=CARTESIAN_POINT('Origin',(50.7133971693864,-54.6569255427236,-205.34995));
#212927=CARTESIAN_POINT('Origin',(50.7133971693864,-54.6569255427236,-203.876128609656));
#212928=CARTESIAN_POINT('Origin',(0.,-12.9675000200281,-203.84995));
#212929=CARTESIAN_POINT('',(50.4303082679829,-74.6701840550325,-203.876128609656));
#212930=CARTESIAN_POINT('',(49.481201831453,-73.5089297105696,-205.34995));
#212931=CARTESIAN_POINT('Origin',(49.481201831453,-73.5089297105696,-203.84995));
#212932=CARTESIAN_POINT('Origin',(0.,-12.9675000200281,-205.34995));
#212933=CARTESIAN_POINT('Origin',(0.,-12.9675000200281,-203.876128609656));
#212934=CARTESIAN_POINT('Origin',(41.5452362233251,-63.7990866568863,-203.84995));
#212935=CARTESIAN_POINT('',(42.0978464467214,-77.8283377352489,-203.876128609656));
#212936=CARTESIAN_POINT('',(42.0388164335396,-76.329728333857,-205.34995));
#212937=CARTESIAN_POINT('Origin',(42.0388164335396,-76.329728333857,-203.84995));
#212938=CARTESIAN_POINT('Origin',(41.5452362233251,-63.7990866568863,-205.34995));
#212939=CARTESIAN_POINT('Origin',(41.5452362233251,-63.7990866568863,-203.876128609656));
#212940=CARTESIAN_POINT('Origin',(0.,990.91999998,-203.84995));
#212941=CARTESIAN_POINT('Origin',(0.,990.91999998,-205.34995));
#212942=CARTESIAN_POINT('Origin',(0.,990.91999998,-203.876128609658));
#212943=CARTESIAN_POINT('Ctrl Pts',(23.5337713018193,37.7635770079652,-235.35005));
#212944=CARTESIAN_POINT('Ctrl Pts',(23.4412215482423,38.6445258986454,-235.35005));
#212945=CARTESIAN_POINT('Ctrl Pts',(23.3965311730095,39.0699180251918,-234.574369193282));
#212946=CARTESIAN_POINT('Ctrl Pts',(21.544967758244,37.5546394871334,-235.35005));
#212947=CARTESIAN_POINT('Ctrl Pts',(21.5595156328412,38.4042872399864,-235.350049999891));
#212948=CARTESIAN_POINT('Ctrl Pts',(21.528579903829,38.8428303292096,-234.630002261341));
#212949=CARTESIAN_POINT('Ctrl Pts',(19.5728087816907,37.6143598891719,-235.35005));
#212950=CARTESIAN_POINT('Ctrl Pts',(19.6460924738843,38.4272076002415,-235.350050000083));
#212951=CARTESIAN_POINT('Ctrl Pts',(19.6686531904506,38.8735235122781,-234.667980547948));
#212952=CARTESIAN_POINT('Ctrl Pts',(17.1293181155885,38.0221098575109,-235.35005));
#212953=CARTESIAN_POINT('Ctrl Pts',(17.2775595203712,38.7968938489773,-235.350049999979));
#212954=CARTESIAN_POINT('Ctrl Pts',(17.3605038451651,39.2363169917258,-234.700408624977));
#212955=CARTESIAN_POINT('Ctrl Pts',(16.6417036619234,38.1205664043706,-235.35005));
#212956=CARTESIAN_POINT('Ctrl Pts',(16.8064715779446,38.8874549017434,-235.350049999965));
#212957=CARTESIAN_POINT('Ctrl Pts',(16.8996732382546,39.3253279225055,-234.706109493926));
#212958=CARTESIAN_POINT('Ctrl Pts',(16.1400046127821,38.2400981929685,-235.35005));
#212959=CARTESIAN_POINT('Ctrl Pts',(16.321379078743,38.9989389430008,-235.350050000001));
#212960=CARTESIAN_POINT('Ctrl Pts',(16.42550941929,39.4346066602602,-234.71123368766));
#212961=CARTESIAN_POINT('Ctrl Pts',(16.1248016477258,38.2437210061727,-235.35005));
#212962=CARTESIAN_POINT('Ctrl Pts',(16.3049839983191,39.0030520275993,-235.350049999999));
#212963=CARTESIAN_POINT('Ctrl Pts',(16.4084002183571,39.4388699450819,-234.710975012385));
#212964=CARTESIAN_POINT('Ctrl Pts',(16.0943932017804,38.2509106189313,-235.35005));
#212965=CARTESIAN_POINT('Ctrl Pts',(16.2733843150407,39.0107061360713,-235.350050000001));
#212966=CARTESIAN_POINT('Ctrl Pts',(16.3760894567153,39.446674478502,-234.710745663099));
#212967=CARTESIAN_POINT('Ctrl Pts',(16.0791881134232,38.2544860973495,-235.35005));
#212968=CARTESIAN_POINT('Ctrl Pts',(16.2575832784277,39.014513360759,-235.350050000001));
#212969=CARTESIAN_POINT('Ctrl Pts',(16.3599327990296,39.4505564386636,-234.710630718465));
#212970=CARTESIAN_POINT('Ctrl Pts',(16.0335702546769,38.2651546047763,-235.35005));
#212971=CARTESIAN_POINT('Ctrl Pts',(16.2101754559538,39.0258758721752,-235.350049999999));
#212972=CARTESIAN_POINT('Ctrl Pts',(16.3114590264843,39.4621414418891,-234.710285080473));
#212973=CARTESIAN_POINT('Ctrl Pts',(16.0031548906349,38.2721897058173,-235.35005));
#212974=CARTESIAN_POINT('Ctrl Pts',(16.1785662488632,39.0333714350269,-235.350049999998));
#212975=CARTESIAN_POINT('Ctrl Pts',(16.2791381120791,39.4697836074978,-234.710053583084));
#212976=CARTESIAN_POINT('Ctrl Pts',(15.9118984440295,38.2930637479782,-235.35005));
#212977=CARTESIAN_POINT('Ctrl Pts',(16.0837198987913,39.0556218358223,-235.350050000004));
#212978=CARTESIAN_POINT('Ctrl Pts',(16.1821604215077,39.492466940349,-234.709355920323));
#212979=CARTESIAN_POINT('Ctrl Pts',(15.8510470069393,38.306671426842,-235.35005));
#212980=CARTESIAN_POINT('Ctrl Pts',(16.0204731962087,39.0701381365939,-235.35005));
#212981=CARTESIAN_POINT('Ctrl Pts',(16.1174886972092,39.5072649406307,-234.70888658509));
#212982=CARTESIAN_POINT('Ctrl Pts',(15.6684514409702,38.3465730643765,-235.35005));
#212983=CARTESIAN_POINT('Ctrl Pts',(15.8306591723873,39.1127448736401,-235.350049999999));
#212984=CARTESIAN_POINT('Ctrl Pts',(15.9234157668579,39.5506891483394,-234.707466239024));
#212985=CARTESIAN_POINT('Ctrl Pts',(15.5466660565693,38.3719456052131,-235.35005));
#212986=CARTESIAN_POINT('Ctrl Pts',(15.7040546546833,39.1398840785044,-235.350049999993));
#212987=CARTESIAN_POINT('Ctrl Pts',(15.7939567942534,39.5783455145344,-234.706502899802));
#212988=CARTESIAN_POINT('Ctrl Pts',(15.1811462193431,38.4444074431018,-235.35005));
#212989=CARTESIAN_POINT('Ctrl Pts',(15.3239537913802,39.2175582578027,-235.350050000014));
#212990=CARTESIAN_POINT('Ctrl Pts',(15.4053654748198,39.6574599908674,-234.703565858339));
#212991=CARTESIAN_POINT('Ctrl Pts',(14.9372480700734,38.4878406765044,-235.35005));
#212992=CARTESIAN_POINT('Ctrl Pts',(15.0703175067835,39.264312526642,-235.350050000014));
#212993=CARTESIAN_POINT('Ctrl Pts',(15.1460186735935,39.7050627091706,-234.701545340841));
#212994=CARTESIAN_POINT('Ctrl Pts',(13.7166846422703,38.6810491434111,-235.35005));
#212995=CARTESIAN_POINT('Ctrl Pts',(13.7992132146591,39.4736856374966,-235.350049999945));
#212996=CARTESIAN_POINT('Ctrl Pts',(13.8480833935374,39.9177504037689,-234.691149086225));
#212997=CARTESIAN_POINT('Ctrl Pts',(12.7368211879873,38.7593950182532,-235.35005));
#212998=CARTESIAN_POINT('Ctrl Pts',(12.7786543368479,39.5623177727158,-235.350049999973));
#212999=CARTESIAN_POINT('Ctrl Pts',(12.8051741258232,40.0075424243875,-234.681773511397));
#213000=CARTESIAN_POINT('Ctrl Pts',(11.2619727856902,38.7640531506662,-235.35005));
#213001=CARTESIAN_POINT('Ctrl Pts',(11.2431521551635,39.57939042452,-235.350050000013));
#213002=CARTESIAN_POINT('Ctrl Pts',(11.2337432072715,40.0228717807706,-234.665927297908));
#213003=CARTESIAN_POINT('Ctrl Pts',(10.7695125981793,38.7467544284527,-235.35005));
#213004=CARTESIAN_POINT('Ctrl Pts',(10.7295261233112,39.565608825609,-235.350049999918));
#213005=CARTESIAN_POINT('Ctrl Pts',(10.7088554256347,40.0080380899104,-234.660361333187));
#213006=CARTESIAN_POINT('Ctrl Pts',(10.0295286262227,38.6919125335409,-235.35005));
#213007=CARTESIAN_POINT('Ctrl Pts',(9.95766155311817,39.5152528143172,-235.350050000041));
#213008=CARTESIAN_POINT('Ctrl Pts',(9.91949508966786,39.9551826764288,-234.651499451358));
#213009=CARTESIAN_POINT('Ctrl Pts',(9.78265126231073,38.6688067779309,-235.35005));
#213010=CARTESIAN_POINT('Ctrl Pts',(9.69988287916204,39.4934693700283,-235.350049999959));
#213011=CARTESIAN_POINT('Ctrl Pts',(9.65607177918342,39.9324493818079,-234.648467075417));
#213012=CARTESIAN_POINT('Ctrl Pts',(9.52011153127327,38.6390634523758,-235.35005));
#213013=CARTESIAN_POINT('Ctrl Pts',(9.42586446285605,39.4649843060134,-235.350050000003));
#213014=CARTESIAN_POINT('Ctrl Pts',(9.37590715791402,39.9027865695414,-234.645166403075));
#213015=CARTESIAN_POINT('Ctrl Pts',(9.5046684949403,38.6373245042148,-235.35005));
#213016=CARTESIAN_POINT('Ctrl Pts',(9.41214667413609,39.4630372950313,-235.350049999998));
#213017=CARTESIAN_POINT('Ctrl Pts',(9.36306987593997,39.901015111022,-234.645686067046));
#213018=CARTESIAN_POINT('Ctrl Pts',(9.473784192795,38.6338861513583,-235.35005));
#213019=CARTESIAN_POINT('Ctrl Pts',(9.38247113793461,39.4594435790343,-235.350050000003));
#213020=CARTESIAN_POINT('Ctrl Pts',(9.33401274020438,39.8975447405836,-234.646059912476));
#213021=CARTESIAN_POINT('Ctrl Pts',(9.45834279379069,38.6321837719653,-235.35005));
#213022=CARTESIAN_POINT('Ctrl Pts',(9.36763359512751,39.4576634928911,-235.350049999998));
#213023=CARTESIAN_POINT('Ctrl Pts',(9.31948440605278,39.8958258095482,-234.646245966055));
#213024=CARTESIAN_POINT('Ctrl Pts',(9.41202084990189,38.6271269560786,-235.35005));
#213025=CARTESIAN_POINT('Ctrl Pts',(9.32312351171904,39.4523737016179,-235.350050000003));
#213026=CARTESIAN_POINT('Ctrl Pts',(9.27590015565431,39.8907177155567,-234.646801541337));
#213027=CARTESIAN_POINT('Ctrl Pts',(9.38114255812013,38.623822841143,-235.35005));
#213028=CARTESIAN_POINT('Ctrl Pts',(9.29344985904992,39.4489140122088,-235.35005));
#213029=CARTESIAN_POINT('Ctrl Pts',(9.24684499153364,39.8873772510059,-234.647168477753));
#213030=CARTESIAN_POINT('Ctrl Pts',(9.28851667185603,38.6141112621716,-235.35005));
#213031=CARTESIAN_POINT('Ctrl Pts',(9.20443932951169,39.4387362251899,-235.350049999998));
#213032=CARTESIAN_POINT('Ctrl Pts',(9.15968291091601,39.8775501712904,-234.648259112741));
#213033=CARTESIAN_POINT('Ctrl Pts',(9.22677806590085,38.6079045516347,-235.35005));
#213034=CARTESIAN_POINT('Ctrl Pts',(9.14509826755899,39.4322176005077,-235.350050000002));
#213035=CARTESIAN_POINT('Ctrl Pts',(9.10157940753183,39.8712578585209,-234.648972640385));
#213036=CARTESIAN_POINT('Ctrl Pts',(9.04159803643428,38.590083732581,-235.35005));
#213037=CARTESIAN_POINT('Ctrl Pts',(8.96711873611221,39.413462618403,-235.350049999995));
#213038=CARTESIAN_POINT('Ctrl Pts',(8.92728571898841,39.8531547209574,-234.65107374629));
#213039=CARTESIAN_POINT('Ctrl Pts',(8.9181923928208,38.5792687467551,-235.35005));
#213040=CARTESIAN_POINT('Ctrl Pts',(8.8484656438594,39.4020198774485,-235.350049999991));
#213041=CARTESIAN_POINT('Ctrl Pts',(8.8111123738377,39.8421175196046,-234.652421897231));
#213042=CARTESIAN_POINT('Ctrl Pts',(7.80796793746822,38.4914558622135,-235.35005));
#213043=CARTESIAN_POINT('Ctrl Pts',(7.78295663156236,39.308723576629,-235.350050000068));
#213044=CARTESIAN_POINT('Ctrl Pts',(7.76582808828186,39.7520042646446,-234.664105356254));
#213045=CARTESIAN_POINT('Ctrl Pts',(6.82559161716421,38.4810313542882,-235.35005));
#213046=CARTESIAN_POINT('Ctrl Pts',(6.83602241994642,39.2928501093446,-235.350049999919));
#213047=CARTESIAN_POINT('Ctrl Pts',(6.84026733134357,39.7374178092291,-234.671316797028));
#213048=CARTESIAN_POINT('Ctrl Pts',(5.35870346950635,38.5640529810103,-235.35005));
#213049=CARTESIAN_POINT('Ctrl Pts',(5.42261292444301,39.3678039902082,-235.350050000041));
#213050=CARTESIAN_POINT('Ctrl Pts',(5.45751451406658,39.8113778773929,-234.67782855951));
#213051=CARTESIAN_POINT('Ctrl Pts',(4.87084782996001,38.6081920655742,-235.35005));
#213052=CARTESIAN_POINT('Ctrl Pts',(4.95261115944054,39.4091800619321,-235.350049999987));
#213053=CARTESIAN_POINT('Ctrl Pts',(4.99768588356049,39.8520037968002,-234.679290572784));
#213054=CARTESIAN_POINT('Ctrl Pts',(4.14073989483365,38.6993202534944,-235.35005));
#213055=CARTESIAN_POINT('Ctrl Pts',(4.24935061898658,39.496080258275,-235.350050000007));
#213056=CARTESIAN_POINT('Ctrl Pts',(4.30944352059924,39.9371527903924,-234.680416520121));
#213057=CARTESIAN_POINT('Ctrl Pts',(3.8976491789597,38.7338397862931,-235.35005));
#213058=CARTESIAN_POINT('Ctrl Pts',(4.01519167481988,39.5291751697216,-235.350050000021));
#213059=CARTESIAN_POINT('Ctrl Pts',(4.08027426577388,39.9695612765499,-234.680616205795));
#213060=CARTESIAN_POINT('Ctrl Pts',(3.59413684714098,38.7822104560078,-235.35005));
#213061=CARTESIAN_POINT('Ctrl Pts',(3.72290333740421,39.5757342399723,-235.350049999995));
#213062=CARTESIAN_POINT('Ctrl Pts',(3.79420511631547,40.0151323858563,-234.680645380834));
#213063=CARTESIAN_POINT('Ctrl Pts',(3.53345194963507,38.7921458861338,-235.35005));
#213064=CARTESIAN_POINT('Ctrl Pts',(3.664465108349,39.5853059524361,-235.350049999998));
#213065=CARTESIAN_POINT('Ctrl Pts',(3.73701094502127,40.0244998494229,-234.68064014219));
#213066=CARTESIAN_POINT('Ctrl Pts',(3.41211742684046,38.8125413395452,-235.35005));
#213067=CARTESIAN_POINT('Ctrl Pts',(3.54762995410732,39.6049708499852,-235.350050000001));
#213068=CARTESIAN_POINT('Ctrl Pts',(3.62266424283369,40.0437428586239,-234.680607281213));
#213069=CARTESIAN_POINT('Ctrl Pts',(3.35147728959859,38.8231424752753,-235.35005));
#213070=CARTESIAN_POINT('Ctrl Pts',(3.49161331287685,39.6148541672734,-235.350050000006));
#213071=CARTESIAN_POINT('Ctrl Pts',(3.56919466402218,40.053171477784,-234.680497918826));
#213072=CARTESIAN_POINT('Ctrl Pts',(3.16954343825523,38.8547460002398,-235.35005));
#213073=CARTESIAN_POINT('Ctrl Pts',(3.30204310810083,39.6474891097825,-235.350049999988));
#213074=CARTESIAN_POINT('Ctrl Pts',(3.37542267175575,40.086577519758,-234.680874073307));
#213075=CARTESIAN_POINT('Ctrl Pts',(3.0481745839355,38.874630850895,-235.35005));
#213076=CARTESIAN_POINT('Ctrl Pts',(3.17556784923895,39.6680247489009,-235.350050000003));
#213077=CARTESIAN_POINT('Ctrl Pts',(3.24614026037888,40.107598873827,-234.681111548481));
#213078=CARTESIAN_POINT('Ctrl Pts',(1.95514022520376,39.0429654437216,-235.35005));
#213079=CARTESIAN_POINT('Ctrl Pts',(2.03697150224516,39.8418002800282,-235.350049999973));
#213080=CARTESIAN_POINT('Ctrl Pts',(2.08186324421676,40.2855474949375,-234.683127215883));
#213081=CARTESIAN_POINT('Ctrl Pts',(0.976538623334591,39.1173940813018,
-235.35005));
#213082=CARTESIAN_POINT('Ctrl Pts',(1.01727193036948,39.9186763854274,-235.350050000014));
#213083=CARTESIAN_POINT('Ctrl Pts',(1.03992075359521,40.3641796537732,-234.684031855599));
#213084=CARTESIAN_POINT('Ctrl Pts',(-1.46378262333123E-9,39.1173940795976,
-235.35005));
#213085=CARTESIAN_POINT('Ctrl Pts',(-2.52664204734146E-9,39.9186763848311,
-235.350050000001));
#213086=CARTESIAN_POINT('Ctrl Pts',(-3.11757902950382E-9,40.3641796532955,
-234.68403185425));
#213087=CARTESIAN_POINT('',(16.4332020134251,39.4328341554683,-234.711149933649));
#213088=CARTESIAN_POINT('',(9.39019403218236,39.9042967860601,-234.645338670229));
#213089=CARTESIAN_POINT('Ctrl Pts',(16.4332020134251,39.4328341554683,-234.711149933649));
#213090=CARTESIAN_POINT('Ctrl Pts',(16.4203687735928,39.4358646816662,-234.711186834089));
#213091=CARTESIAN_POINT('Ctrl Pts',(16.4059605185975,39.4394389786432,-234.71098583394));
#213092=CARTESIAN_POINT('Ctrl Pts',(16.3922402656679,39.4427528750883,-234.710888692203));
#213093=CARTESIAN_POINT('Ctrl Pts',(16.3760847365541,39.4466549715566,-234.710774308294));
#213094=CARTESIAN_POINT('Ctrl Pts',(16.3599280157032,39.4505367406652,-234.710659655018));
#213095=CARTESIAN_POINT('Ctrl Pts',(16.3437702132482,39.4543981737023,-234.710544734921));
#213096=CARTESIAN_POINT('Ctrl Pts',(16.3114533027793,39.4621213517823,-234.71031488544));
#213097=CARTESIAN_POINT('Ctrl Pts',(16.2791320654287,39.46976317781,-234.710083968637));
#213098=CARTESIAN_POINT('Ctrl Pts',(16.2468073837233,39.4773235962622,-234.709852004547));
#213099=CARTESIAN_POINT('Ctrl Pts',(16.1821472083185,39.4924469619834,-234.709387998781));
#213100=CARTESIAN_POINT('Ctrl Pts',(16.1174732492397,39.5072445696182,-234.708919803019));
#213101=CARTESIAN_POINT('Ctrl Pts',(16.0527925905293,39.5217162013998,-234.708447571674));
#213102=CARTESIAN_POINT('Ctrl Pts',(15.9233431638038,39.5506791785132,-234.707502465699));
#213103=CARTESIAN_POINT('Ctrl Pts',(15.7938668812152,39.578336176396,-234.706541204651));
#213104=CARTESIAN_POINT('Ctrl Pts',(15.664420813873,39.6046890583072,-234.70556492186));
#213105=CARTESIAN_POINT('Ctrl Pts',(15.4048133770445,39.65754044473,-234.703606961467));
#213106=CARTESIAN_POINT('Ctrl Pts',(15.1453273024862,39.705141822975,-234.701588751043));
#213107=CARTESIAN_POINT('Ctrl Pts',(14.8864260905022,39.7475653316504,-234.699517541149));
#213108=CARTESIAN_POINT('Ctrl Pts',(14.6384733849316,39.7881948199223,-234.697533919315));
#213109=CARTESIAN_POINT('Ctrl Pts',(14.391016124878,39.8241145499751,-234.695494894259));
#213110=CARTESIAN_POINT('Ctrl Pts',(14.1444226316741,39.8553859752978,-234.693402565929));
#213111=CARTESIAN_POINT('Ctrl Pts',(13.8954781303716,39.8869555405806,-234.691290289463));
#213112=CARTESIAN_POINT('Ctrl Pts',(13.6474139403796,39.9137877658293,-234.689123685087));
#213113=CARTESIAN_POINT('Ctrl Pts',(13.4006121728291,39.9359991936509,-234.686905722618));
#213114=CARTESIAN_POINT('Ctrl Pts',(13.2154735814038,39.9526611183254,-234.685241915865));
#213115=CARTESIAN_POINT('Ctrl Pts',(13.0310454540037,39.9667239118459,-234.683549225146));
#213116=CARTESIAN_POINT('Ctrl Pts',(12.8474902542086,39.9782559564172,-234.681829214244));
#213117=CARTESIAN_POINT('Ctrl Pts',(12.6339027438901,39.9916748118439,-234.679827784446));
#213118=CARTESIAN_POINT('Ctrl Pts',(12.421738466853,40.0015717217697,-234.677921264933));
#213119=CARTESIAN_POINT('Ctrl Pts',(12.2106113431622,40.0081508386869,-234.676039453921));
#213120=CARTESIAN_POINT('Ctrl Pts',(12.0591061036169,40.012872025937,-234.674689062634));
#213121=CARTESIAN_POINT('Ctrl Pts',(11.9081347609518,40.0158836098002,-234.673351340136));
#213122=CARTESIAN_POINT('Ctrl Pts',(11.7575518798804,40.0172447761073,-234.671999478744));
#213123=CARTESIAN_POINT('Ctrl Pts',(11.5451205475199,40.0191650101347,-234.670092371411));
#213124=CARTESIAN_POINT('Ctrl Pts',(11.3334790960771,40.0177944242705,-234.668159423378));
#213125=CARTESIAN_POINT('Ctrl Pts',(11.1221945383988,40.0132178609341,-234.666120035305));
#213126=CARTESIAN_POINT('Ctrl Pts',(10.9127324535587,40.0086807735653,-234.664098238339));
#213127=CARTESIAN_POINT('Ctrl Pts',(10.7036211597665,40.0009927930571,-234.661971856266));
#213128=CARTESIAN_POINT('Ctrl Pts',(10.4944307492036,39.9901862402078,-234.659659267466));
#213129=CARTESIAN_POINT('Ctrl Pts',(10.3905549522781,39.9848201276492,-234.658510926087));
#213130=CARTESIAN_POINT('Ctrl Pts',(10.2866595198607,39.9786842761451,-234.657316620765));
#213131=CARTESIAN_POINT('Ctrl Pts',(10.1826910350602,39.9717779243169,-234.656066034813));
#213132=CARTESIAN_POINT('Ctrl Pts',(9.97674280585096,39.9580973274317,-234.653588784491));
#213133=CARTESIAN_POINT('Ctrl Pts',(9.77052974306509,39.9413880055303,-234.650895256858));
#213134=CARTESIAN_POINT('Ctrl Pts',(9.56366756941837,39.9216004287237,-234.647908051821));
#213135=CARTESIAN_POINT('Ctrl Pts',(9.50662648274058,39.9161441151606,-234.647084346749));
#213136=CARTESIAN_POINT('Ctrl Pts',(9.44953599881491,39.9104534465954,-234.646238289762));
#213137=CARTESIAN_POINT('Ctrl Pts',(9.39238796798789,39.9045266899386,-234.645368206131));
#213138=CARTESIAN_POINT('Ctrl Pts',(9.39164951275459,39.9044501055943,-234.645356963087));
#213139=CARTESIAN_POINT('Ctrl Pts',(9.39091836077164,39.9043734691061,-234.645347149113));
#213140=CARTESIAN_POINT('Ctrl Pts',(9.39019403294204,39.9042967861422,-234.645338670235));
#213141=CARTESIAN_POINT('',(23.3965312474468,39.0699178884317,-234.574369311842));
#213142=CARTESIAN_POINT('Ctrl Pts',(23.3965311730095,39.0699180251917,-234.574369193282));
#213143=CARTESIAN_POINT('Ctrl Pts',(23.0945668978142,39.0332080891435,-234.583362575255));
#213144=CARTESIAN_POINT('Ctrl Pts',(22.7892825654022,39.0028096619222,-234.591999161059));
#213145=CARTESIAN_POINT('Ctrl Pts',(22.4810560648072,38.9792191234299,-234.600263558775));
#213146=CARTESIAN_POINT('Ctrl Pts',(22.1762733075222,38.955892156561,-234.608435620289));
#213147=CARTESIAN_POINT('Ctrl Pts',(21.8686137925994,38.9392219216893,-234.616243787899));
#213148=CARTESIAN_POINT('Ctrl Pts',(21.5584440197407,38.9296383570326,-234.623679503494));
#213149=CARTESIAN_POINT('Ctrl Pts',(21.2528094397991,38.9201949198749,-234.631006496681));
#213150=CARTESIAN_POINT('Ctrl Pts',(20.9447375071085,38.9176324870007,-234.637971880429));
#213151=CARTESIAN_POINT('Ctrl Pts',(20.6345794911481,38.9223123543167,-234.644573233207));
#213152=CARTESIAN_POINT('Ctrl Pts',(20.4201142239214,38.9255483467557,-234.649137877081));
#213153=CARTESIAN_POINT('Ctrl Pts',(20.2046515464032,38.9322460806201,-234.653528585768));
#213154=CARTESIAN_POINT('Ctrl Pts',(19.9883076390171,38.942510467933,-234.65774609101));
#213155=CARTESIAN_POINT('Ctrl Pts',(19.7072288045135,38.9558461890895,-234.66322556798));
#213156=CARTESIAN_POINT('Ctrl Pts',(19.4246735316766,38.9752044123415,-234.668412293426));
#213157=CARTESIAN_POINT('Ctrl Pts',(19.1409896021326,39.0007703112355,-234.67330953877));
#213158=CARTESIAN_POINT('Ctrl Pts',(18.8605201760056,39.0260465156463,-234.678151292031));
#213159=CARTESIAN_POINT('Ctrl Pts',(18.5789475541907,39.0573905103833,-234.682710118246));
#213160=CARTESIAN_POINT('Ctrl Pts',(18.2966065606005,39.0949307879218,-234.686992959889));
#213161=CARTESIAN_POINT('Ctrl Pts',(18.13867089569,39.1159300364496,-234.689388692205));
#213162=CARTESIAN_POINT('Ctrl Pts',(17.9804935567509,39.1388673942171,-234.691698151296));
#213163=CARTESIAN_POINT('Ctrl Pts',(17.8221337142222,39.1637582958363,-234.693923009571));
#213164=CARTESIAN_POINT('Ctrl Pts',(17.6071594454973,39.1975478177759,-234.696943265674));
#213165=CARTESIAN_POINT('Ctrl Pts',(17.3918441418382,39.234987417972,-234.699800486487));
#213166=CARTESIAN_POINT('Ctrl Pts',(17.1763463091445,39.276150383324,-234.702496183025));
#213167=CARTESIAN_POINT('Ctrl Pts',(16.9311343525973,39.3229891433482,-234.705563578247));
#213168=CARTESIAN_POINT('Ctrl Pts',(16.685681217613,39.3746501130852,-234.708421884368));
#213169=CARTESIAN_POINT('Ctrl Pts',(16.4401979186951,39.4312214602623,-234.711074951862));
#213170=CARTESIAN_POINT('Ctrl Pts',(16.4400911575267,39.4312460632522,-234.711076105687));
#213171=CARTESIAN_POINT('Ctrl Pts',(16.4399845215119,39.4312706239838,-234.711077278024));
#213172=CARTESIAN_POINT('Ctrl Pts',(16.4398780101602,39.4312951426272,-234.711078468791));
#213173=CARTESIAN_POINT('Ctrl Pts',(16.4376580748706,39.4318061661087,-234.711103287052));
#213174=CARTESIAN_POINT('Ctrl Pts',(16.4354272908939,39.4323210756196,-234.711126313563));
#213175=CARTESIAN_POINT('Ctrl Pts',(16.4332020134251,39.4328341554683,-234.711149933648));
#213176=CARTESIAN_POINT('',(23.5337713018193,37.7635770079652,-235.35005));
#213177=CARTESIAN_POINT('Origin',(23.5337713018193,37.7635770079652,-233.85005));
#213178=CARTESIAN_POINT('Ctrl Pts',(1.77635683940026E-15,39.1173940795976,
-235.35005));
#213179=CARTESIAN_POINT('Ctrl Pts',(0.356337369905621,39.1173940801923,
-235.35005));
#213180=CARTESIAN_POINT('Ctrl Pts',(0.71242141794696,39.1074881618969,-235.35005));
#213181=CARTESIAN_POINT('Ctrl Pts',(1.06804673827445,39.0877008656221,-235.35005));
#213182=CARTESIAN_POINT('Ctrl Pts',(1.42342108500666,39.0679275337324,-235.35005));
#213183=CARTESIAN_POINT('Ctrl Pts',(1.7783377368663,39.0382867784318,-235.35005));
#213184=CARTESIAN_POINT('Ctrl Pts',(2.13259518028593,38.9987512744367,-235.35005));
#213185=CARTESIAN_POINT('Ctrl Pts',(2.39770300797321,38.9691649615014,-235.35005));
#213186=CARTESIAN_POINT('Ctrl Pts',(2.66244176764352,38.9340362860626,-235.35005));
#213187=CARTESIAN_POINT('Ctrl Pts',(2.92672632283112,38.8933347008859,-235.35005));
#213188=CARTESIAN_POINT('Ctrl Pts',(2.92737060497439,38.8932354771363,-235.35005));
#213189=CARTESIAN_POINT('Ctrl Pts',(2.92801488526773,38.8931362200903,-235.35005));
#213190=CARTESIAN_POINT('Ctrl Pts',(2.92865916371251,38.8930369297473,-235.35005));
#213191=CARTESIAN_POINT('Ctrl Pts',(3.04946230489496,38.8744198466836,-235.35005));
#213192=CARTESIAN_POINT('Ctrl Pts',(3.17018687790291,38.8546342347918,-235.35005));
#213193=CARTESIAN_POINT('Ctrl Pts',(3.29083267335743,38.8336769886241,-235.35005));
#213194=CARTESIAN_POINT('Ctrl Pts',(3.35147729051483,38.8231424800179,-235.35005));
#213195=CARTESIAN_POINT('Ctrl Pts',(3.41211742776757,38.8125413442761,-235.35005));
#213196=CARTESIAN_POINT('Ctrl Pts',(3.47278468915089,38.8023436182718,-235.35005));
#213197=CARTESIAN_POINT('Ctrl Pts',(3.53345195083837,38.7921458922164,-235.35005));
#213198=CARTESIAN_POINT('Ctrl Pts',(3.5941368485939,38.7822104634589,-235.35005));
#213199=CARTESIAN_POINT('Ctrl Pts',(3.65483931509605,38.77253633205,-235.35005));
#213200=CARTESIAN_POINT('Ctrl Pts',(3.65546036588309,38.7724373553976,-235.35005));
#213201=CARTESIAN_POINT('Ctrl Pts',(3.65608141850748,38.772338406072,-235.35005));
#213202=CARTESIAN_POINT('Ctrl Pts',(3.6567024729692,38.7722394840726,-235.35005));
#213203=CARTESIAN_POINT('Ctrl Pts',(3.89889272031259,38.7336632480438,-235.35005));
#213204=CARTESIAN_POINT('Ctrl Pts',(4.14136237871588,38.6992425872422,-235.35005));
#213205=CARTESIAN_POINT('Ctrl Pts',(4.38410920892073,38.6689442099089,-235.35005));
#213206=CARTESIAN_POINT('Ctrl Pts',(4.38470863575882,38.6688693926167,-235.35005));
#213207=CARTESIAN_POINT('Ctrl Pts',(4.385308064291,38.6687946005203,-235.35005));
#213208=CARTESIAN_POINT('Ctrl Pts',(4.38590749451727,38.6687198336194,-235.35005));
#213209=CARTESIAN_POINT('Ctrl Pts',(4.87204943935151,38.6080833741744,-235.35005));
#213210=CARTESIAN_POINT('Ctrl Pts',(5.35930565181913,38.5640188991232,-235.35005));
#213211=CARTESIAN_POINT('Ctrl Pts',(5.84766618924905,38.5363791735804,-235.35005));
#213212=CARTESIAN_POINT('Ctrl Pts',(5.84822203464059,38.5363477144167,-235.35005));
#213213=CARTESIAN_POINT('Ctrl Pts',(5.84877788147003,38.5363162765022,-235.35005));
#213214=CARTESIAN_POINT('Ctrl Pts',(5.8493337297374,38.5362848598371,-235.35005));
#213215=CARTESIAN_POINT('Ctrl Pts',(6.82670834760912,38.4810434337187,-235.35005));
#213216=CARTESIAN_POINT('Ctrl Pts',(7.80852886296661,38.4915002286307,-235.35005));
#213217=CARTESIAN_POINT('Ctrl Pts',(8.79483411976782,38.569511762568,-235.35005));
#213218=CARTESIAN_POINT('Ctrl Pts',(8.79530155914491,38.5695487345527,-235.35005));
#213219=CARTESIAN_POINT('Ctrl Pts',(8.79576899920217,38.5695857217288,-235.35005));
#213220=CARTESIAN_POINT('Ctrl Pts',(8.79623643993962,38.5696227240969,-235.35005));
#213221=CARTESIAN_POINT('Ctrl Pts',(8.91912763117963,38.5793507275117,-235.35005));
#213222=CARTESIAN_POINT('Ctrl Pts',(9.04206583597103,38.5901287539636,-235.35005));
#213223=CARTESIAN_POINT('Ctrl Pts',(9.16505138923101,38.6019642804975,-235.35005));
#213224=CARTESIAN_POINT('Ctrl Pts',(9.22677806574757,38.6079045531424,-235.35005));
#213225=CARTESIAN_POINT('Ctrl Pts',(9.28851667172624,38.6141112633048,-235.35005));
#213226=CARTESIAN_POINT('Ctrl Pts',(9.35026726260429,38.6205856490536,-235.35005));
#213227=CARTESIAN_POINT('Ctrl Pts',(9.38114255802925,38.6238228419266,-235.35005));
#213228=CARTESIAN_POINT('Ctrl Pts',(9.41202084981748,38.6271269567803,-235.35005));
#213229=CARTESIAN_POINT('Ctrl Pts',(9.44290214575424,38.6304981673432,-235.35005));
#213230=CARTESIAN_POINT('Ctrl Pts',(9.4583427937156,38.6321837726239,-235.35005));
#213231=CARTESIAN_POINT('Ctrl Pts',(9.47378419271945,38.6338861520155,-235.35005));
#213232=CARTESIAN_POINT('Ctrl Pts',(9.4892263437929,38.635605328458,-235.35005));
#213233=CARTESIAN_POINT('Ctrl Pts',(9.50466849486033,38.6373245048999,-235.35005));
#213234=CARTESIAN_POINT('Ctrl Pts',(9.52011153118833,38.6390634530903,-235.35005));
#213235=CARTESIAN_POINT('Ctrl Pts',(9.53555504477742,38.6408130605231,-235.35005));
#213236=CARTESIAN_POINT('Ctrl Pts',(9.53599979556026,38.6408634466785,-235.35005));
#213237=CARTESIAN_POINT('Ctrl Pts',(9.53644454563409,38.6409138169984,-235.35005));
#213238=CARTESIAN_POINT('Ctrl Pts',(9.53688929499893,38.6409641714834,-235.35005));
#213239=CARTESIAN_POINT('Ctrl Pts',(9.78353997539554,38.6688899403824,-235.35005));
#213240=CARTESIAN_POINT('Ctrl Pts',(10.0299725953353,38.6919454677066,-235.35005));
#213241=CARTESIAN_POINT('Ctrl Pts',(10.2761899486978,38.7101931855589,-235.35005));
#213242=CARTESIAN_POINT('Ctrl Pts',(10.2766105499729,38.7102243572586,-235.35005));
#213243=CARTESIAN_POINT('Ctrl Pts',(10.2770311506211,38.710255514956,-235.35005));
#213244=CARTESIAN_POINT('Ctrl Pts',(10.2774517506423,38.7102866586516,-235.35005));
#213245=CARTESIAN_POINT('Ctrl Pts',(10.7703523227059,38.7467839115651,-235.35005));
#213246=CARTESIAN_POINT('Ctrl Pts',(11.2623919364771,38.7640519886161,-235.35005));
#213247=CARTESIAN_POINT('Ctrl Pts',(11.7535889201299,38.762500547725,-235.35005));
#213248=CARTESIAN_POINT('Ctrl Pts',(11.7539614946379,38.7624993709521,-235.35005));
#213249=CARTESIAN_POINT('Ctrl Pts',(11.7543340686623,38.7624981833755,-235.35005));
#213250=CARTESIAN_POINT('Ctrl Pts',(11.7547066422029,38.7624969849952,-235.35005));
#213251=CARTESIAN_POINT('Ctrl Pts',(12.7375637754513,38.759335631593,-235.35005));
#213252=CARTESIAN_POINT('Ctrl Pts',(13.7170546474298,38.6809905736403,-235.35005));
#213253=CARTESIAN_POINT('Ctrl Pts',(14.6931353846985,38.5264823710594,-235.35005));
#213254=CARTESIAN_POINT('Ctrl Pts',(14.6934128882961,38.5264384437689,-235.35005));
#213255=CARTESIAN_POINT('Ctrl Pts',(14.6936903916164,38.5263945102864,-235.35005));
#213256=CARTESIAN_POINT('Ctrl Pts',(14.6939678946594,38.5263505706118,-235.35005));
#213257=CARTESIAN_POINT('Ctrl Pts',(14.9378025763861,38.4877419252588,-235.35005));
#213258=CARTESIAN_POINT('Ctrl Pts',(15.1814232310733,38.4443525286098,-235.35005));
#213259=CARTESIAN_POINT('Ctrl Pts',(15.4248261113785,38.3960995539571,-235.35005));
#213260=CARTESIAN_POINT('Ctrl Pts',(15.5466660621667,38.3719456078342,-235.35005));
#213261=CARTESIAN_POINT('Ctrl Pts',(15.6684514484779,38.3465730678228,-235.35005));
#213262=CARTESIAN_POINT('Ctrl Pts',(15.7901818197943,38.3199719796031,-235.35005));
#213263=CARTESIAN_POINT('Ctrl Pts',(15.8510470109318,38.3066714342958,-235.35005));
#213264=CARTESIAN_POINT('Ctrl Pts',(15.9118984485245,38.2930637565816,-235.35005));
#213265=CARTESIAN_POINT('Ctrl Pts',(15.9727360775264,38.2791477304796,-235.35005));
#213266=CARTESIAN_POINT('Ctrl Pts',(16.0031548939305,38.2721897169932,-235.35005));
#213267=CARTESIAN_POINT('Ctrl Pts',(16.0335702581983,38.2651546167241,-235.35005));
#213268=CARTESIAN_POINT('Ctrl Pts',(16.0639821635381,38.258042279449,-235.35005));
#213269=CARTESIAN_POINT('Ctrl Pts',(16.0791881167504,38.2544861106846,-235.35005));
#213270=CARTESIAN_POINT('Ctrl Pts',(16.0943932052251,38.2509106327023,-235.35005));
#213271=CARTESIAN_POINT('Ctrl Pts',(16.1095974281268,38.2473158268211,-235.35005));
#213272=CARTESIAN_POINT('Ctrl Pts',(16.1248016514155,38.2437210208484,-235.35005));
#213273=CARTESIAN_POINT('Ctrl Pts',(16.140004616612,38.2400982081071,-235.35005));
#213274=CARTESIAN_POINT('Ctrl Pts',(16.1552076180073,38.2364760332375,-235.35005));
#213275=CARTESIAN_POINT('Ctrl Pts',(16.1554380518469,38.236421131469,-235.35005));
#213276=CARTESIAN_POINT('Ctrl Pts',(16.1556684859374,38.2363662336162,-235.35005));
#213277=CARTESIAN_POINT('Ctrl Pts',(16.1558989202787,38.2363113396791,-235.35005));
#213278=CARTESIAN_POINT('Ctrl Pts',(16.6421654924883,38.1204731945768,-235.35005));
#213279=CARTESIAN_POINT('Ctrl Pts',(17.1295496308336,38.0220712232916,-235.35005));
#213280=CARTESIAN_POINT('Ctrl Pts',(17.6180162768063,37.9405600316208,-235.35005));
#213281=CARTESIAN_POINT('Ctrl Pts',(17.6182014583502,37.9405291300875,-235.35005));
#213282=CARTESIAN_POINT('Ctrl Pts',(17.6183866400499,37.9404982309457,-235.35005));
#213283=CARTESIAN_POINT('Ctrl Pts',(17.6185718219055,37.9404673341953,-235.35005));
#213284=CARTESIAN_POINT('Ctrl Pts',(18.5958771217087,37.7774083899181,-235.35005));
#213285=CARTESIAN_POINT('Ctrl Pts',(19.5774518164961,37.6809633951712,-235.35005));
#213286=CARTESIAN_POINT('Ctrl Pts',(20.563312329756,37.6513870472214,-235.35005));
#213287=CARTESIAN_POINT('Ctrl Pts',(21.5491728430159,37.6218106992716,-235.35005));
#213288=CARTESIAN_POINT('Ctrl Pts',(22.5393191900798,37.6591029589904,-235.35005));
#213289=CARTESIAN_POINT('Ctrl Pts',(23.5337713018193,37.7635770079652,-235.35005));
#213290=CARTESIAN_POINT('Ctrl Pts',(9.39019403218236,39.9042967860601,-234.645338670229));
#213291=CARTESIAN_POINT('Ctrl Pts',(9.37475363168684,39.9026279307258,-234.645212295458));
#213292=CARTESIAN_POINT('Ctrl Pts',(9.36241909261664,39.9009373862515,-234.645694439942));
#213293=CARTESIAN_POINT('Ctrl Pts',(9.34854130807218,39.8992799258028,-234.645872989761));
#213294=CARTESIAN_POINT('Ctrl Pts',(9.33401289064803,39.8975447585514,-234.64605991054));
#213295=CARTESIAN_POINT('Ctrl Pts',(9.3194845954082,39.8958258317407,-234.646245963641));
#213296=CARTESIAN_POINT('Ctrl Pts',(9.30495632258662,39.894123111551,-234.646431157816));
#213297=CARTESIAN_POINT('Ctrl Pts',(9.27590137992507,39.8907178590417,-234.646801525732));
#213298=CARTESIAN_POINT('Ctrl Pts',(9.24684652697401,39.887377424119,-234.64716845854));
#213299=CARTESIAN_POINT('Ctrl Pts',(9.21779096466109,39.8841015577674,-234.647532022749));
#213300=CARTESIAN_POINT('Ctrl Pts',(9.15969278284146,39.8775512842996,-234.648258989216));
#213301=CARTESIAN_POINT('Ctrl Pts',(9.10159176571151,39.871259142112,-234.648972491407));
#213302=CARTESIAN_POINT('Ctrl Pts',(9.04348151135069,39.8652234793331,-234.64967300902));
#213303=CARTESIAN_POINT('Ctrl Pts',(8.92736484808448,39.8531629397571,-234.65107279239));
#213304=CARTESIAN_POINT('Ctrl Pts',(8.81121130823973,39.8421260486728,-234.652420791411));
#213305=CARTESIAN_POINT('Ctrl Pts',(8.69496967544261,39.8321049357202,-234.653720059344));
#213306=CARTESIAN_POINT('Ctrl Pts',(8.46608431126897,39.8123728824755,-234.656278380377));
#213307=CARTESIAN_POINT('Ctrl Pts',(8.23695543614247,39.7965715522408,-234.658649489037));
#213308=CARTESIAN_POINT('Ctrl Pts',(8.00713518629142,39.7847168766851,-234.660839220159));
#213309=CARTESIAN_POINT('Ctrl Pts',(7.83476999890313,39.7758258700182,-234.662481518501));
#213310=CARTESIAN_POINT('Ctrl Pts',(7.66201598405601,39.7691561378415,-234.664021730675));
#213311=CARTESIAN_POINT('Ctrl Pts',(7.48868554439324,39.7647375575943,-234.66546127314));
#213312=CARTESIAN_POINT('Ctrl Pts',(7.35868771464617,39.761423622409,-234.666540929989));
#213313=CARTESIAN_POINT('Ctrl Pts',(7.2283656693242,39.7593763654488,-234.667563941682));
#213314=CARTESIAN_POINT('Ctrl Pts',(7.09764070666038,39.758615755376,-234.668530586038));
#213315=CARTESIAN_POINT('Ctrl Pts',(7.06314672882331,39.7584150556285,-234.668785651393));
#213316=CARTESIAN_POINT('Ctrl Pts',(7.02862017588322,39.758304000414,-234.669036821695));
#213317=CARTESIAN_POINT('Ctrl Pts',(6.99409009464001,39.7582829607004,-234.669283884834));
#213318=CARTESIAN_POINT('Ctrl Pts',(6.75867700422119,39.7581395198566,-234.670968268276));
#213319=CARTESIAN_POINT('Ctrl Pts',(6.52286201588005,39.762181854609,-234.672463355194));
#213320=CARTESIAN_POINT('Ctrl Pts',(6.28701389358818,39.7704255684024,-234.673769643912));
#213321=CARTESIAN_POINT('Ctrl Pts',(6.16414506741507,39.7747202620691,-234.674450175773));
#213322=CARTESIAN_POINT('Ctrl Pts',(6.04126720097618,39.7801543731084,-234.67507950791));
#213323=CARTESIAN_POINT('Ctrl Pts',(5.91843211982557,39.7867245213383,-234.675657972016));
#213324=CARTESIAN_POINT('Ctrl Pts',(5.89988148264417,39.7877167495755,-234.675745332057));
#213325=CARTESIAN_POINT('Ctrl Pts',(5.88133207614076,39.7887348794358,-234.675831546829));
#213326=CARTESIAN_POINT('Ctrl Pts',(5.8627840714653,39.7897789158681,-234.675916615161));
#213327=CARTESIAN_POINT('Ctrl Pts',(5.66502610646588,39.8009103838531,-234.676823609769));
#213328=CARTESIAN_POINT('Ctrl Pts',(5.46740597226592,39.8149903643949,-234.677600277792));
#213329=CARTESIAN_POINT('Ctrl Pts',(5.27014966576015,39.8320105075238,-234.678245806341));
#213330=CARTESIAN_POINT('Ctrl Pts',(5.17152151250727,39.8405205790883,-234.678568570616));
#213331=CARTESIAN_POINT('Ctrl Pts',(5.07298423927242,39.8497646508467,-234.678859485214));
#213332=CARTESIAN_POINT('Ctrl Pts',(4.97456616129474,39.8597402211668,-234.679116775072));
#213333=CARTESIAN_POINT('Ctrl Pts',(4.9253571223059,39.8647280063269,-234.67924542));
#213334=CARTESIAN_POINT('Ctrl Pts',(4.87617787852371,39.8698986474593,-234.679365646105));
#213335=CARTESIAN_POINT('Ctrl Pts',(4.82703162371335,39.875251446779,-234.679477627772));
#213336=CARTESIAN_POINT('Ctrl Pts',(4.80245849630817,39.8779278464388,-234.679533618606));
#213337=CARTESIAN_POINT('Ctrl Pts',(4.77789361616645,39.8806497845711,-234.67958754763));
#213338=CARTESIAN_POINT('Ctrl Pts',(4.75333738875916,39.8834171708839,-234.679639426256));
#213339=CARTESIAN_POINT('Ctrl Pts',(4.73148831986303,39.8858794715136,-234.679685585614));
#213340=CARTESIAN_POINT('Ctrl Pts',(4.70816077797056,39.8885496195412,-234.679733064146));
#213341=CARTESIAN_POINT('Ctrl Pts',(4.68731978273058,39.8909689272488,-234.679774062183));
#213342=CARTESIAN_POINT('Ctrl Pts',(4.68473752726179,39.8912686859929,-234.679779141951));
#213343=CARTESIAN_POINT('Ctrl Pts',(4.68219344082424,39.8915645279947,-234.679784125136));
#213344=CARTESIAN_POINT('Ctrl Pts',(4.67969506209335,39.8918555273409,-234.679788999259));
#213345=CARTESIAN_POINT('Ctrl Pts',(4.63296703344735,39.8972981872607,-234.679880161636));
#213346=CARTESIAN_POINT('Ctrl Pts',(4.58600312877882,39.9029307496431,-234.679973381372));
#213347=CARTESIAN_POINT('Ctrl Pts',(4.53885549843968,39.9087526218986,-234.680067252505));
#213348=CARTESIAN_POINT('Ctrl Pts',(4.424673154427,39.9228520584111,-234.680294590038));
#213349=CARTESIAN_POINT('Ctrl Pts',(4.30941205520417,39.9380630127427,-234.680526134682));
#213350=CARTESIAN_POINT('Ctrl Pts',(4.19382133831405,39.9543414584605,-234.680743553396));
#213351=CARTESIAN_POINT('Ctrl Pts',(4.07974483468867,39.9704066600778,-234.680958123972));
#213352=CARTESIAN_POINT('Ctrl Pts',(3.96534735932018,39.9875115413643,-234.681158940829));
#213353=CARTESIAN_POINT('Ctrl Pts',(3.85134657577325,40.0055640599005,-234.681330634686));
#213354=CARTESIAN_POINT('Ctrl Pts',(3.79401158722453,40.0146433040193,-234.681416985542));
#213355=CARTESIAN_POINT('Ctrl Pts',(3.73677693279445,40.0239616791513,-234.681495952715));
#213356=CARTESIAN_POINT('Ctrl Pts',(3.67973367637223,40.0335031384469,-234.681565687655));
#213357=CARTESIAN_POINT('Ctrl Pts',(3.64924621527456,40.0386026872338,-234.68160295834));
#213358=CARTESIAN_POINT('Ctrl Pts',(3.61985573216485,40.0436394880348,-234.681614478861));
#213359=CARTESIAN_POINT('Ctrl Pts',(3.58934324812148,40.0488965317388,-234.681649314366));
#213360=CARTESIAN_POINT('Ctrl Pts',(3.58443348443461,40.0497424426204,-234.681654919747));
#213361=CARTESIAN_POINT('Ctrl Pts',(3.57949477874549,40.0505940414076,-234.681661126376));
#213362=CARTESIAN_POINT('Ctrl Pts',(3.57451801904532,40.0514524893135,-234.681668135715));
#213363=CARTESIAN_POINT('Ctrl Pts',(3.55480123180177,40.0548534641928,-234.681695905116));
#213364=CARTESIAN_POINT('Ctrl Pts',(3.53463540183366,40.0583388372962,-234.681732190185));
#213365=CARTESIAN_POINT('Ctrl Pts',(3.51349260734251,40.0619750592967,-234.681788699843));
#213366=CARTESIAN_POINT('Ctrl Pts',(3.51050442728484,40.0624889784038,-234.681796686538));
#213367=CARTESIAN_POINT('Ctrl Pts',(3.50749681626456,40.0630059003384,-234.681805075349));
#213368=CARTESIAN_POINT('Ctrl Pts',(3.50446836416328,40.0635260027774,-234.681813897546));
#213369=CARTESIAN_POINT('Ctrl Pts',(3.42074441322775,40.0779046456038,-234.682057794152));
#213370=CARTESIAN_POINT('Ctrl Pts',(3.33972206686012,40.0913287970994,-234.682233612489));
#213371=CARTESIAN_POINT('Ctrl Pts',(3.26040169897432,40.1040349279776,-234.682363606509));
#213372=CARTESIAN_POINT('Ctrl Pts',(3.211926012102,40.1118001267308,-234.682443050787));
#213373=CARTESIAN_POINT('Ctrl Pts',(3.16408589205622,40.1192960752724,-234.682505367319));
#213374=CARTESIAN_POINT('Ctrl Pts',(3.11665238015447,40.126567293819,-234.682555524582));
#213375=CARTESIAN_POINT('Ctrl Pts',(3.03672015498941,40.1388203329636,-234.682640046716));
#213376=CARTESIAN_POINT('Ctrl Pts',(2.95793206930389,40.1504404103641,-234.68268994071));
#213377=CARTESIAN_POINT('Ctrl Pts',(2.87918968065051,40.1615981162924,-234.682728533227));
#213378=CARTESIAN_POINT('Ctrl Pts',(2.8008095715495,40.1727044876248,-234.682766948186));
#213379=CARTESIAN_POINT('Ctrl Pts',(2.72247466309021,40.1833526657526,-234.682794164161));
#213380=CARTESIAN_POINT('Ctrl Pts',(2.64309811212022,40.193659954308,-234.682832586117));
#213381=CARTESIAN_POINT('Ctrl Pts',(2.57411475280095,40.2026176550564,-234.682865977282));
#213382=CARTESIAN_POINT('Ctrl Pts',(2.50434458908083,40.2113172116199,-234.682907824178));
#213383=CARTESIAN_POINT('Ctrl Pts',(2.43307271489723,40.21980369842,-234.682972457297));
#213384=CARTESIAN_POINT('Ctrl Pts',(2.21676521285307,40.2455598719722,-234.683168616421));
#213385=CARTESIAN_POINT('Ctrl Pts',(1.99806321819614,40.2681244085811,-234.683337166398));
#213386=CARTESIAN_POINT('Ctrl Pts',(1.77667857288155,40.2873136365197,-234.683478702563));
#213387=CARTESIAN_POINT('Ctrl Pts',(1.55768037275675,40.306296011627,-234.68361871302));
#213388=CARTESIAN_POINT('Ctrl Pts',(1.33605684155172,40.3219755131914,-234.683732289647));
#213389=CARTESIAN_POINT('Ctrl Pts',(1.11153890722954,40.3341248594886,-234.683819419986));
#213390=CARTESIAN_POINT('Ctrl Pts',(0.891158232169992,40.3460503261405,
-234.683904944748));
#213391=CARTESIAN_POINT('Ctrl Pts',(0.667988651385312,40.354574546182,-234.68396498895));
#213392=CARTESIAN_POINT('Ctrl Pts',(0.441788148323699,40.3594342654747,
-234.68399896599));
#213393=CARTESIAN_POINT('Ctrl Pts',(0.295808050543585,40.3625705197621,
-234.684020893315));
#213394=CARTESIAN_POINT('Ctrl Pts',(0.14856587322869,40.3641795877876,-234.684031952444));
#213395=CARTESIAN_POINT('Ctrl Pts',(2.66453525910038E-15,40.3641796532955,
-234.68403185425));
#213396=CARTESIAN_POINT('Ctrl Pts',(23.3814806446219,39.0698185248112,-234.571621167217));
#213397=CARTESIAN_POINT('Ctrl Pts',(23.4282937951356,38.6452631234932,-235.35005));
#213398=CARTESIAN_POINT('Ctrl Pts',(23.525610634336,37.7626986794242,-235.35005));
#213399=CARTESIAN_POINT('Ctrl Pts',(23.5896364911122,39.0717917430095,-234.609597560408));
#213400=CARTESIAN_POINT('Ctrl Pts',(23.6056657686035,38.6356324734982,-235.35005));
#213401=CARTESIAN_POINT('Ctrl Pts',(23.6385084238607,37.775139906398,-235.35005));
#213402=CARTESIAN_POINT('Ctrl Pts',(23.7999845563376,39.0524591845457,-234.643035391158));
#213403=CARTESIAN_POINT('Ctrl Pts',(23.7829033814932,38.6107706130362,-235.35005));
#213404=CARTESIAN_POINT('Ctrl Pts',(23.7514657535404,37.7755620251222,-235.35005));
#213405=CARTESIAN_POINT('Ctrl Pts',(24.0125934783339,39.0086422970752,-234.671185933941));
#213406=CARTESIAN_POINT('Ctrl Pts',(23.9601413389653,38.5676758646721,-235.35005));
#213407=CARTESIAN_POINT('Ctrl Pts',(23.8643244195193,37.7621460828182,-235.35005));
#213408=CARTESIAN_POINT('',(23.9972286459191,39.0117604146193,-234.669151583121));
#213409=CARTESIAN_POINT('',(23.8561664752437,37.7630917536256,-235.35005));
#213410=CARTESIAN_POINT('Origin',(23.8561664752439,37.7630917536255,-233.85005));
#213411=CARTESIAN_POINT('Ctrl Pts',(23.5337713018193,37.7635770079652,-235.35005));
#213412=CARTESIAN_POINT('Ctrl Pts',(23.6412535989187,37.7748687641791,-235.35005));
#213413=CARTESIAN_POINT('Ctrl Pts',(23.7487194439798,37.7752300509467,-235.35005));
#213414=CARTESIAN_POINT('Ctrl Pts',(23.8561664752437,37.7630917536256,-235.35005));
#213415=CARTESIAN_POINT('Origin',(23.3783761769639,36.3745931076819,-233.942512591795));
#213416=CARTESIAN_POINT('Ctrl Pts',(23.9972286658434,39.0117605909834,-234.669151698811));
#213417=CARTESIAN_POINT('Ctrl Pts',(23.9474058055448,38.5707334611872,-235.35005));
#213418=CARTESIAN_POINT('Ctrl Pts',(23.8561664752439,37.7630917536255,-235.35005));
#213419=CARTESIAN_POINT('Ctrl Pts',(25.2366484173464,38.8718330388058,-234.669014852156));
#213420=CARTESIAN_POINT('Ctrl Pts',(25.1842887597299,38.431109053993,-235.350049999742));
#213421=CARTESIAN_POINT('Ctrl Pts',(25.0882853750842,37.6238992104159,-235.35005));
#213422=CARTESIAN_POINT('Ctrl Pts',(26.4747606339603,38.7210799284767,-234.668852342857));
#213423=CARTESIAN_POINT('Ctrl Pts',(26.4198403391809,38.280686857661,-235.35005000043));
#213424=CARTESIAN_POINT('Ctrl Pts',(26.319091123968,37.47392953931,-235.35005));
#213425=CARTESIAN_POINT('Ctrl Pts',(27.711570814231,38.5594513301076,-234.668667513818));
#213426=CARTESIAN_POINT('Ctrl Pts',(27.654024085186,38.1194242486926,-235.35005));
#213427=CARTESIAN_POINT('Ctrl Pts',(27.5485779004777,37.3131372941855,-235.35005));
#213428=CARTESIAN_POINT('',(27.7115708142298,38.5594513301044,-234.66866751382));
#213429=CARTESIAN_POINT('',(27.5485779004777,37.3131372941855,-235.35005));
#213430=CARTESIAN_POINT('Origin',(27.5485779004728,37.3131372941843,-233.850050000003));
#213431=CARTESIAN_POINT('Origin',(0.0633608499796878,-172.860463397757,
-235.350049999539));
#213432=CARTESIAN_POINT('Origin',(0.0438186590672052,-173.169156331663,
-234.199437903576));
#213433=CARTESIAN_POINT('Ctrl Pts',(27.6870869834027,38.5647076063785,-234.665458925605));
#213434=CARTESIAN_POINT('Ctrl Pts',(27.6312386219367,38.1248642240496,-235.350050000001));
#213435=CARTESIAN_POINT('Ctrl Pts',(27.5285055536634,37.315722493921,-235.35005));
#213436=CARTESIAN_POINT('Ctrl Pts',(27.7719185087418,38.5485509850084,-234.673701202518));
#213437=CARTESIAN_POINT('Ctrl Pts',(27.710388063005,38.1083834979961,-235.350049999996));
#213438=CARTESIAN_POINT('Ctrl Pts',(27.5986154970304,37.3068273115645,-235.35005));
#213439=CARTESIAN_POINT('Ctrl Pts',(27.8660265843471,38.5268314825978,-234.686074077228));
#213440=CARTESIAN_POINT('Ctrl Pts',(27.7951602584987,38.0865442976545,-235.350049999997));
#213441=CARTESIAN_POINT('Ctrl Pts',(27.6684770389457,37.2966022256818,-235.35005));
#213442=CARTESIAN_POINT('Ctrl Pts',(28.0107486443927,38.4840136200808,-234.708383241074));
#213443=CARTESIAN_POINT('Ctrl Pts',(27.9227914578621,38.0449642852773,-235.350050000001));
#213444=CARTESIAN_POINT('Ctrl Pts',(27.7691733848276,37.2776980879525,-235.35005));
#213445=CARTESIAN_POINT('Ctrl Pts',(28.056519267283,38.4693001007684,-234.715635823842));
#213446=CARTESIAN_POINT('Ctrl Pts',(27.9627817556189,38.0309145591475,-235.350049999995));
#213447=CARTESIAN_POINT('Ctrl Pts',(27.8004215724929,37.2712202551586,-235.35005));
#213448=CARTESIAN_POINT('Ctrl Pts',(28.1424207276373,38.4415180788525,-234.727204794551));
#213449=CARTESIAN_POINT('Ctrl Pts',(28.0391835813355,38.0045168186177,-235.350050000004));
#213450=CARTESIAN_POINT('Ctrl Pts',(27.8627200032187,37.2572093770216,-235.35005));
#213451=CARTESIAN_POINT('Ctrl Pts',(28.1818076781825,38.4289988027469,-234.731157474203));
#213452=CARTESIAN_POINT('Ctrl Pts',(28.0752081342426,37.9926116568254,-235.350050000001));
#213453=CARTESIAN_POINT('Ctrl Pts',(27.8937776977631,37.249697476023,-235.35005));
#213454=CARTESIAN_POINT('Ctrl Pts',(28.2939062760355,38.3943578402229,-234.739890329309));
#213455=CARTESIAN_POINT('Ctrl Pts',(28.1794856739151,37.959489646501,-235.350049999998));
#213456=CARTESIAN_POINT('Ctrl Pts',(27.9867858054616,37.226404790223,-235.35005));
#213457=CARTESIAN_POINT('Ctrl Pts',(28.3725698489465,38.3676355099575,-234.747582193031));
#213458=CARTESIAN_POINT('Ctrl Pts',(28.2511672609651,37.9342399780936,-235.35004999998));
#213459=CARTESIAN_POINT('Ctrl Pts',(28.0485551598146,37.2098945175254,-235.35005));
#213460=CARTESIAN_POINT('Ctrl Pts',(28.499560264286,38.3162258363163,-234.763633757846));
#213461=CARTESIAN_POINT('Ctrl Pts',(28.3635285899708,37.8869011682613,-235.35005000001));
#213462=CARTESIAN_POINT('Ctrl Pts',(28.1402497418155,37.1819908028498,-235.35005));
#213463=CARTESIAN_POINT('Ctrl Pts',(28.5414369654236,38.2984968797705,-234.768759787037));
#213464=CARTESIAN_POINT('Ctrl Pts',(28.4005824927214,37.8706765859433,-235.350049999998));
#213465=CARTESIAN_POINT('Ctrl Pts',(28.1706617267493,37.1721527193585,-235.35005));
#213466=CARTESIAN_POINT('Ctrl Pts',(28.6210886692051,38.2646056135699,-234.777052100967));
#213467=CARTESIAN_POINT('Ctrl Pts',(28.4721423102288,37.8394910733453,-235.350050000002));
#213468=CARTESIAN_POINT('Ctrl Pts',(28.2311847426228,37.1515938768492,-235.35005));
#213469=CARTESIAN_POINT('Ctrl Pts',(28.6588366351122,38.2485358813461,-234.78021126702));
#213470=CARTESIAN_POINT('Ctrl Pts',(28.5066596950528,37.8245853061929,-235.350049999988));
#213471=CARTESIAN_POINT('Ctrl Pts',(28.2612972505945,37.1409013962204,-235.35005));
#213472=CARTESIAN_POINT('Ctrl Pts',(28.7710344960755,38.1996667667751,-234.789253190342));
#213473=CARTESIAN_POINT('Ctrl Pts',(28.6093471685584,37.7792838182322,-235.350050000025));
#213474=CARTESIAN_POINT('Ctrl Pts',(28.3512820909987,37.1078462406674,-235.35005));
#213475=CARTESIAN_POINT('Ctrl Pts',(28.8428008206516,38.1677622719788,-234.793805028219));
#213476=CARTESIAN_POINT('Ctrl Pts',(28.6759158482819,37.7494700953236,-235.350049999991));
#213477=CARTESIAN_POINT('Ctrl Pts',(28.4108519482495,37.0845842971443,-235.35005));
#213478=CARTESIAN_POINT('Ctrl Pts',(28.9948913431262,38.0914060325279,-234.807859220985));
#213479=CARTESIAN_POINT('Ctrl Pts',(28.8130624304243,37.6798186719204,-235.350050000009));
#213480=CARTESIAN_POINT('Ctrl Pts',(28.5284852992461,37.0351888006413,-235.35005));
#213481=CARTESIAN_POINT('Ctrl Pts',(29.0707345298403,38.0497116584053,-234.815474578403));
#213482=CARTESIAN_POINT('Ctrl Pts',(28.8810490621556,37.6420974921894,-235.350050000012));
#213483=CARTESIAN_POINT('Ctrl Pts',(28.5864462918562,37.0087322113245,-235.35005));
#213484=CARTESIAN_POINT('Ctrl Pts',(29.1729198726625,37.994577684537,-234.821977012417));
#213485=CARTESIAN_POINT('Ctrl Pts',(28.9761856145916,37.590712775769,-235.350049999993));
#213486=CARTESIAN_POINT('Ctrl Pts',(28.6725892746692,36.9674060120273,-235.35005));
#213487=CARTESIAN_POINT('Ctrl Pts',(29.2059516364469,37.9766885523724,-234.82374012897));
#213488=CARTESIAN_POINT('Ctrl Pts',(29.0072562987579,37.573898403251,-235.350049999995));
#213489=CARTESIAN_POINT('Ctrl Pts',(28.7011808463655,36.9533782896452,-235.35005));
#213490=CARTESIAN_POINT('Ctrl Pts',(29.2546260372023,37.9501878862571,-234.826062930886));
#213491=CARTESIAN_POINT('Ctrl Pts',(29.0533143455601,37.5488533460758,-235.350050000003));
#213492=CARTESIAN_POINT('Ctrl Pts',(28.7439306930081,36.9320540547938,-235.35005));
#213493=CARTESIAN_POINT('Ctrl Pts',(29.2703961112124,37.941727494487,-234.826631844201));
#213494=CARTESIAN_POINT('Ctrl Pts',(29.0684051119755,37.5407696411564,-235.350050000002));
#213495=CARTESIAN_POINT('Ctrl Pts',(28.7581616928441,36.9249070270844,-235.35005));
#213496=CARTESIAN_POINT('Ctrl Pts',(29.3050706121592,37.9214977173636,-234.829332507218));
#213497=CARTESIAN_POINT('Ctrl Pts',(29.1002611313985,37.5221587047774,-235.350049999998));
#213498=CARTESIAN_POINT('Ctrl Pts',(28.7865561585441,36.9104741568002,-235.35005));
#213499=CARTESIAN_POINT('Ctrl Pts',(29.3237188905298,37.9099446994752,-234.831343174629));
#213500=CARTESIAN_POINT('Ctrl Pts',(29.1168776732614,37.5117934675614,-235.350049999998));
#213501=CARTESIAN_POINT('Ctrl Pts',(28.8007140683774,36.9031768938705,-235.35005));
#213502=CARTESIAN_POINT('Ctrl Pts',(29.4267902669213,37.8438444640261,-234.843360679698));
#213503=CARTESIAN_POINT('Ctrl Pts',(29.2077156164998,37.4530850279629,-235.350050000008));
#213504=CARTESIAN_POINT('Ctrl Pts',(28.8771404183119,36.8629106275395,-235.35005));
#213505=CARTESIAN_POINT('Ctrl Pts',(29.5070851154047,37.7891356470415,-234.850802470886));
#213506=CARTESIAN_POINT('Ctrl Pts',(29.2794078069932,37.4043310205184,-235.350050000069));
#213507=CARTESIAN_POINT('Ctrl Pts',(28.938176463821,36.8274085232238,-235.35005));
#213508=CARTESIAN_POINT('Ctrl Pts',(29.57158663008,37.7472855488698,-234.853784838128));
#213509=CARTESIAN_POINT('Ctrl Pts',(29.3419504108669,37.3639149821511,-235.350049999978));
#213510=CARTESIAN_POINT('Ctrl Pts',(28.9987888521635,36.7910354495401,-235.35005));
#213511=CARTESIAN_POINT('',(29.5524353619882,37.7591803693089,-234.853368133768));
#213512=CARTESIAN_POINT('',(28.9814172171126,36.8014272692484,-235.35005));
#213513=CARTESIAN_POINT('Origin',(28.9814172171126,36.8014272692485,-233.85005));
#213514=CARTESIAN_POINT('Ctrl Pts',(27.5485779004777,37.3131372941856,-235.35005));
#213515=CARTESIAN_POINT('Ctrl Pts',(27.6119497053713,37.3048495466029,-235.35005));
#213516=CARTESIAN_POINT('Ctrl Pts',(27.6750965458531,37.2953595193401,-235.35005));
#213517=CARTESIAN_POINT('Ctrl Pts',(27.7378143932095,37.2835852418792,-235.35005));
#213518=CARTESIAN_POINT('Ctrl Pts',(27.7691734109443,37.2776980854911,-235.35005));
#213519=CARTESIAN_POINT('Ctrl Pts',(27.8004215957617,37.2712202529943,-235.35005));
#213520=CARTESIAN_POINT('Ctrl Pts',(27.8315707886446,37.2642148195972,-235.35005));
#213521=CARTESIAN_POINT('Ctrl Pts',(27.8627200211639,37.257209377286,-235.35005));
#213522=CARTESIAN_POINT('Ctrl Pts',(27.8937777129896,37.2496974771633,-235.35005));
#213523=CARTESIAN_POINT('Ctrl Pts',(27.9247804016332,37.2419332526298,-235.35005));
#213524=CARTESIAN_POINT('Ctrl Pts',(27.9867858296455,37.2264047908593,-235.35005));
#213525=CARTESIAN_POINT('Ctrl Pts',(28.0485551618066,37.2098945246507,-235.35005));
#213526=CARTESIAN_POINT('Ctrl Pts',(28.1096848833639,37.191292048355,-235.35005));
#213527=CARTESIAN_POINT('Ctrl Pts',(28.1402497358115,37.1819908127424,-235.35005));
#213528=CARTESIAN_POINT('Ctrl Pts',(28.1706617181455,37.1721527303683,-235.35005));
#213529=CARTESIAN_POINT('Ctrl Pts',(28.2009232370621,37.1618733050988,-235.35005));
#213530=CARTESIAN_POINT('Ctrl Pts',(28.2311847284776,37.151593889171,-235.35005));
#213531=CARTESIAN_POINT('Ctrl Pts',(28.2612972337604,37.1409014094734,-235.35005));
#213532=CARTESIAN_POINT('Ctrl Pts',(28.2912921994266,37.129883016559,-235.35005));
#213533=CARTESIAN_POINT('Ctrl Pts',(28.3512820882545,37.1078462463438,-235.35005));
#213534=CARTESIAN_POINT('Ctrl Pts',(28.4108519466395,37.0845843013711,-235.35005));
#213535=CARTESIAN_POINT('Ctrl Pts',(28.4696686246939,37.0598865511459,-235.35005));
#213536=CARTESIAN_POINT('Ctrl Pts',(28.5284852999082,37.0351888021132,-235.35005));
#213537=CARTESIAN_POINT('Ctrl Pts',(28.5864462936913,37.0087322116309,-235.35005));
#213538=CARTESIAN_POINT('Ctrl Pts',(28.6438749473726,36.9811814124344,-235.35005));
#213539=CARTESIAN_POINT('Ctrl Pts',(28.6725892757669,36.9674060120908,-235.35005));
#213540=CARTESIAN_POINT('Ctrl Pts',(28.7011808475711,36.9533782894892,-235.35005));
#213541=CARTESIAN_POINT('Ctrl Pts',(28.7296807442605,36.9391621333448,-235.35005));
#213542=CARTESIAN_POINT('Ctrl Pts',(28.7439306934412,36.9320540548556,-235.35005));
#213543=CARTESIAN_POINT('Ctrl Pts',(28.7581616932791,36.9249070270955,-235.35005));
#213544=CARTESIAN_POINT('Ctrl Pts',(28.7723589257722,36.9176905920959,-235.35005));
#213545=CARTESIAN_POINT('Ctrl Pts',(28.7865561589916,36.9104741567272,-235.35005));
#213546=CARTESIAN_POINT('Ctrl Pts',(28.8007140688312,36.9031768937556,-235.350049999999));
#213547=CARTESIAN_POINT('Ctrl Pts',(28.8148092348245,36.8957506630084,-235.350049999999));
#213548=CARTESIAN_POINT('Ctrl Pts',(28.8711899085552,36.8660457348789,-235.35005));
#213549=CARTESIAN_POINT('Ctrl Pts',(28.9265109173313,36.834162754371,-235.35005));
#213550=CARTESIAN_POINT('Ctrl Pts',(28.9814172171126,36.8014272692486,-235.35005));
#213551=CARTESIAN_POINT('Ctrl Pts',(29.5524353619882,37.7591803693089,-234.853368133768));
#213552=CARTESIAN_POINT('Ctrl Pts',(29.5491926324494,37.7613057727392,-234.853184787816));
#213553=CARTESIAN_POINT('Ctrl Pts',(29.5240197950341,37.7782295017975,-234.851479445173));
#213554=CARTESIAN_POINT('Ctrl Pts',(29.4656769295574,37.8169869705738,-234.846638436175));
#213555=CARTESIAN_POINT('Ctrl Pts',(29.4430292295003,37.8319697079636,-234.844644267336));
#213556=CARTESIAN_POINT('Ctrl Pts',(29.4064983288726,37.8559033707158,-234.841082265319));
#213557=CARTESIAN_POINT('Ctrl Pts',(29.393891920648,37.8641262032719,-234.839799806521));
#213558=CARTESIAN_POINT('Ctrl Pts',(29.3745220620691,37.8766873104466,-234.837733431133));
#213559=CARTESIAN_POINT('Ctrl Pts',(29.364720492403,37.8830256448728,-234.836664571642));
#213560=CARTESIAN_POINT('Ctrl Pts',(29.3547602107045,37.889436685229,-234.835542204454));
#213561=CARTESIAN_POINT('Ctrl Pts',(29.3480849681094,37.8937264029729,-234.834782069063));
#213562=CARTESIAN_POINT('Ctrl Pts',(29.3431599492174,37.896884697379,-234.834213609395));
#213563=CARTESIAN_POINT('Ctrl Pts',(29.3269344760838,37.9072780544614,-234.832328004808));
#213564=CARTESIAN_POINT('Ctrl Pts',(29.3106731982457,37.9172298129869,-234.830768462726));
#213565=CARTESIAN_POINT('Ctrl Pts',(29.2835927346762,37.9331272185667,-234.828603975926));
#213566=CARTESIAN_POINT('Ctrl Pts',(29.2741105557623,37.9385928841534,-234.827911618046));
#213567=CARTESIAN_POINT('Ctrl Pts',(29.2541227809703,37.949925161019,-234.826585177729));
#213568=CARTESIAN_POINT('Ctrl Pts',(29.2420295816336,37.9566673222368,-234.825864724755));
#213569=CARTESIAN_POINT('Ctrl Pts',(29.2136736977047,37.9722710985875,-234.824309002214));
#213570=CARTESIAN_POINT('Ctrl Pts',(29.1855684322557,37.9875854621943,-234.822771960206));
#213571=CARTESIAN_POINT('Ctrl Pts',(29.1532951346241,38.00489189903,-234.821011435464));
#213572=CARTESIAN_POINT('Ctrl Pts',(29.1372971866779,38.0133983224047,-234.820139345825));
#213573=CARTESIAN_POINT('Ctrl Pts',(29.1304716785934,38.0170117572164,-234.819767344423));
#213574=CARTESIAN_POINT('Ctrl Pts',(29.1259282891305,38.0194134838505,-234.819519732666));
#213575=CARTESIAN_POINT('Ctrl Pts',(29.1224601838887,38.021243126175,-234.8193307323));
#213576=CARTESIAN_POINT('Ctrl Pts',(29.112876957114,38.0262939218943,-234.818808483686));
#213577=CARTESIAN_POINT('Ctrl Pts',(29.099091972616,38.0337742454385,-234.817813387705));
#213578=CARTESIAN_POINT('Ctrl Pts',(29.0617166158013,38.0540345686262,-234.814761445759));
#213579=CARTESIAN_POINT('Ctrl Pts',(29.0401123377758,38.065758808627,-234.812888384745));
#213580=CARTESIAN_POINT('Ctrl Pts',(28.9806261264644,38.0973901660411,-234.807345372931));
#213581=CARTESIAN_POINT('Ctrl Pts',(28.9568964003388,38.1096526154491,-234.8050823928));
#213582=CARTESIAN_POINT('Ctrl Pts',(28.9290986853599,38.1238356761779,-234.802450711269));
#213583=CARTESIAN_POINT('Ctrl Pts',(28.9211478514516,38.1278509098975,-234.801700615536));
#213584=CARTESIAN_POINT('Ctrl Pts',(28.9111398006015,38.1328722652928,-234.800766169102));
#213585=CARTESIAN_POINT('Ctrl Pts',(28.9066160197033,38.1351319973066,-234.800346620177));
#213586=CARTESIAN_POINT('Ctrl Pts',(28.9028073007853,38.137023509385,-234.799998582689));
#213587=CARTESIAN_POINT('Ctrl Pts',(28.9004267038557,38.1382033549997,-234.799782449127));
#213588=CARTESIAN_POINT('Ctrl Pts',(28.9006519492602,38.138093475601,-234.799801689135));
#213589=CARTESIAN_POINT('Ctrl Pts',(28.8603923905194,38.1579548763275,-234.796205569945));
#213590=CARTESIAN_POINT('Ctrl Pts',(28.8225168056264,38.1758599748975,-234.793009488469));
#213591=CARTESIAN_POINT('Ctrl Pts',(28.764802173272,38.2020805237224,-234.788498118192));
#213592=CARTESIAN_POINT('Ctrl Pts',(28.7358063284038,38.2149869383765,-234.786313121037));
#213593=CARTESIAN_POINT('Ctrl Pts',(28.7018880369674,38.2296247093678,-234.783887661662));
#213594=CARTESIAN_POINT('Ctrl Pts',(28.6873487976685,38.2358013396985,-234.782874687066));
#213595=CARTESIAN_POINT('Ctrl Pts',(28.6776571681367,38.2398968528113,-234.782205261335));
#213596=CARTESIAN_POINT('Ctrl Pts',(28.6713086966326,38.2425619960944,-234.781771443078));
#213597=CARTESIAN_POINT('Ctrl Pts',(28.6412446469546,38.2551316958537,-234.77973049979));
#213598=CARTESIAN_POINT('Ctrl Pts',(28.6086604316154,38.2692123122386,-234.776707683702));
#213599=CARTESIAN_POINT('Ctrl Pts',(28.5510250123839,38.2938456778358,-234.770360493156));
#213600=CARTESIAN_POINT('Ctrl Pts',(28.5303190038827,38.3026476050971,-234.767942601905));
#213601=CARTESIAN_POINT('Ctrl Pts',(28.4966982222806,38.316676932562,-234.763862523424));
#213602=CARTESIAN_POINT('Ctrl Pts',(28.4792436754406,38.3238987297857,-234.761709173783));
#213603=CARTESIAN_POINT('Ctrl Pts',(28.4576361932315,38.3326807579169,-234.758998639333));
#213604=CARTESIAN_POINT('Ctrl Pts',(28.4480932800145,38.3365208563917,-234.757794490312));
#213605=CARTESIAN_POINT('Ctrl Pts',(28.4416666436022,38.3390979108861,-234.756982281764));
#213606=CARTESIAN_POINT('Ctrl Pts',(28.4365548603845,38.3411379275027,-234.756334962636));
#213607=CARTESIAN_POINT('Ctrl Pts',(28.4125359635179,38.3507010239759,-234.753291057889));
#213608=CARTESIAN_POINT('Ctrl Pts',(28.3816986646669,38.3623133318808,-234.74992258177));
#213609=CARTESIAN_POINT('Ctrl Pts',(28.322073080104,38.3831376740941,-234.7441144307));
#213610=CARTESIAN_POINT('Ctrl Pts',(28.2999760393941,38.3906429251353,-234.742052474195));
#213611=CARTESIAN_POINT('Ctrl Pts',(28.263501193126,38.4026421762831,-234.738770680216));
#213612=CARTESIAN_POINT('Ctrl Pts',(28.2444334747144,38.4088266683947,-234.73708256842));
#213613=CARTESIAN_POINT('Ctrl Pts',(28.2207628641438,38.4163370068423,-234.735030478749));
#213614=CARTESIAN_POINT('Ctrl Pts',(28.2103182751279,38.4196155083141,-234.734133306195));
#213615=CARTESIAN_POINT('Ctrl Pts',(28.203288896498,38.421814079242,-234.733531256592));
#213616=CARTESIAN_POINT('Ctrl Pts',(28.1980412534931,38.4234473771363,-234.733083597214));
#213617=CARTESIAN_POINT('Ctrl Pts',(28.1660285620671,38.433384328389,-234.730358631913));
#213618=CARTESIAN_POINT('Ctrl Pts',(28.1321616178479,38.4444861390464,-234.726389507244));
#213619=CARTESIAN_POINT('Ctrl Pts',(28.0734215990991,38.4634880588082,-234.718329143074));
#213620=CARTESIAN_POINT('Ctrl Pts',(28.0524938758821,38.4702132584191,-234.715291242156));
#213621=CARTESIAN_POINT('Ctrl Pts',(28.0071718419697,38.4843984690794,-234.708513214599));
#213622=CARTESIAN_POINT('Ctrl Pts',(27.9846241143607,38.4913191645377,-234.705055551881));
#213623=CARTESIAN_POINT('Ctrl Pts',(27.8419926047998,38.5330360338839,-234.683187034774));
#213624=CARTESIAN_POINT('Ctrl Pts',(27.7485282251975,38.5520905058658,-234.672515589894));
#213625=CARTESIAN_POINT('Ctrl Pts',(27.7115708142298,38.5594513301044,-234.66866751382));
#213626=CARTESIAN_POINT('Ctrl Pts',(29.5524353619883,37.7591803693089,-234.853368133768));
#213627=CARTESIAN_POINT('Ctrl Pts',(29.3235739752807,37.3753174315541,-235.35005));
#213628=CARTESIAN_POINT('Ctrl Pts',(28.9814172171125,36.8014272692485,-235.35005));
#213629=CARTESIAN_POINT('Ctrl Pts',(31.4648905505278,36.611137072351,-234.860838757985));
#213630=CARTESIAN_POINT('Ctrl Pts',(31.2186416313246,36.2384660822587,-235.350049999758));
#213631=CARTESIAN_POINT('Ctrl Pts',(30.8601181894623,35.6813344771098,-235.35005));
#213632=CARTESIAN_POINT('Ctrl Pts',(33.2921480182203,35.3641827858728,-234.867835939374));
#213633=CARTESIAN_POINT('Ctrl Pts',(33.0331144993804,35.001495733651,-235.35004999988));
#213634=CARTESIAN_POINT('Ctrl Pts',(32.655766056176,34.4636022590608,-235.35005));
#213635=CARTESIAN_POINT('Ctrl Pts',(36.7811408986291,32.6755312616936,-234.878440733198));
#213636=CARTESIAN_POINT('Ctrl Pts',(36.4951099976157,32.3351522367808,-235.35005000012));
#213637=CARTESIAN_POINT('Ctrl Pts',(36.0822840599884,31.8353365675869,-235.35005));
#213638=CARTESIAN_POINT('Ctrl Pts',(38.4421442470284,31.2387599869711,-234.881588663467));
#213639=CARTESIAN_POINT('Ctrl Pts',(38.1454280191491,30.9083681195947,-235.35004999988));
#213640=CARTESIAN_POINT('Ctrl Pts',(37.7150530376205,30.426874953249,-235.35005));
#213641=CARTESIAN_POINT('Ctrl Pts',(40.8137176069411,28.9351791157808,-234.88379235176));
#213642=CARTESIAN_POINT('Ctrl Pts',(40.4984745671759,28.6231683352463,-235.35005000006));
#213643=CARTESIAN_POINT('Ctrl Pts',(40.0413171754775,28.170164696784,-235.35005));
#213644=CARTESIAN_POINT('Ctrl Pts',(41.5826620989581,28.1429897152722,-234.884007663936));
#213645=CARTESIAN_POINT('Ctrl Pts',(41.2615827441429,27.8370429556774,-235.35005));
#213646=CARTESIAN_POINT('Ctrl Pts',(40.7957050001434,27.3932780662659,-235.35005));
#213647=CARTESIAN_POINT('Ctrl Pts',(43.0792410059956,26.5108878965485,-234.883573054699));
#213648=CARTESIAN_POINT('Ctrl Pts',(42.7465875350161,26.217481845266,-235.35005));
#213649=CARTESIAN_POINT('Ctrl Pts',(42.2637158381442,25.7917312522435,-235.35005));
#213650=CARTESIAN_POINT('Ctrl Pts',(43.8083339671196,25.6692406662039,-234.882926062436));
#213651=CARTESIAN_POINT('Ctrl Pts',(43.4701616566366,25.3820633016541,-235.35005));
#213652=CARTESIAN_POINT('Ctrl Pts',(42.9787004139624,24.9654368934267,-235.35005));
#213653=CARTESIAN_POINT('Ctrl Pts',(45.9226558299789,23.0793988618607,-234.879757408134));
#213654=CARTESIAN_POINT('Ctrl Pts',(45.5679898267064,22.8118032008958,-235.35005));
#213655=CARTESIAN_POINT('Ctrl Pts',(45.0499412762525,22.4237082823892,-235.35005));
#213656=CARTESIAN_POINT('Ctrl Pts',(47.2266045706789,21.2758301574159,-234.876040016386));
#213657=CARTESIAN_POINT('Ctrl Pts',(46.8615872941006,21.0215780313956,-235.350049999181));
#213658=CARTESIAN_POINT('Ctrl Pts',(46.326104449877,20.6527388844884,-235.350050000001));
#213659=CARTESIAN_POINT('Ctrl Pts',(48.4260896922586,19.3965417854656,-234.872874618363));
#213660=CARTESIAN_POINT('Ctrl Pts',(48.0508084453091,19.1577111488603,-235.35005));
#213661=CARTESIAN_POINT('Ctrl Pts',(47.500448334379,18.8074595529597,-235.350050000001));
#213662=CARTESIAN_POINT('',(48.4260896922586,19.3965417854656,-234.872874618363));
#213663=CARTESIAN_POINT('',(47.5004483343782,18.8074595529612,-235.35005));
#213664=CARTESIAN_POINT('Origin',(47.5004483343794,18.8074595529594,-233.85005));
#213665=CARTESIAN_POINT('Ctrl Pts',(28.9814172171126,36.8014272692485,-235.35005));
#213666=CARTESIAN_POINT('Ctrl Pts',(30.4445221387459,35.9291153361866,-235.35005));
#213667=CARTESIAN_POINT('Ctrl Pts',(31.8571523563316,34.997650520712,-235.35005));
#213668=CARTESIAN_POINT('Ctrl Pts',(33.219749332275,34.0075501952443,-235.35005));
#213669=CARTESIAN_POINT('Ctrl Pts',(33.6068768507225,33.7262527252077,-235.35005));
#213670=CARTESIAN_POINT('Ctrl Pts',(33.9899655501622,33.4402220370432,-235.35005));
#213671=CARTESIAN_POINT('Ctrl Pts',(34.3690250580976,33.1494694133448,-235.35005));
#213672=CARTESIAN_POINT('Ctrl Pts',(36.0822840600053,31.8353365675737,-235.35005));
#213673=CARTESIAN_POINT('Ctrl Pts',(37.7150530376344,30.4268749532356,-235.35005));
#213674=CARTESIAN_POINT('Ctrl Pts',(39.2658957962434,28.9224014489936,-235.35005));
#213675=CARTESIAN_POINT('Ctrl Pts',(40.0413171755479,28.1701646968727,-235.35005));
#213676=CARTESIAN_POINT('Ctrl Pts',(40.7957050001266,27.3932780662842,-235.35005));
#213677=CARTESIAN_POINT('Ctrl Pts',(41.52971041916,26.5925046592713,-235.35005));
#213678=CARTESIAN_POINT('Ctrl Pts',(42.2637158381934,25.7917312522584,-235.35005));
#213679=CARTESIAN_POINT('Ctrl Pts',(42.9787004139405,24.9654368934535,-235.35005));
#213680=CARTESIAN_POINT('Ctrl Pts',(43.669114034758,24.1181940231093,-235.35005));
#213681=CARTESIAN_POINT('Ctrl Pts',(45.0499412763931,22.423708282421,-235.35005));
#213682=CARTESIAN_POINT('Ctrl Pts',(46.3260905825898,20.6527606745438,-235.350050000001));
#213683=CARTESIAN_POINT('Ctrl Pts',(47.5004483343782,18.8074595529612,-235.350050000001));
#213684=CARTESIAN_POINT('Ctrl Pts',(48.4260896922586,19.3965417854656,-234.872874618363));
#213685=CARTESIAN_POINT('Ctrl Pts',(48.1436564566979,19.8390426530017,-234.873620088043));
#213686=CARTESIAN_POINT('Ctrl Pts',(47.8509659213957,20.2843345271102,-234.874408251377));
#213687=CARTESIAN_POINT('Ctrl Pts',(47.5478312881813,20.7314567814701,-234.875210279537));
#213688=CARTESIAN_POINT('Ctrl Pts',(47.2446966549669,21.17857903583,-234.876012307697));
#213689=CARTESIAN_POINT('Ctrl Pts',(46.9311176254783,21.6275314483713,-234.876828174927));
#213690=CARTESIAN_POINT('Ctrl Pts',(46.6069504587922,22.077383516232,-234.877623828772));
#213691=CARTESIAN_POINT('Ctrl Pts',(46.2853158480958,22.5237211148126,-234.878413266572));
#213692=CARTESIAN_POINT('Ctrl Pts',(45.9532587493137,22.9709428450799,-234.879182696605));
#213693=CARTESIAN_POINT('Ctrl Pts',(45.6106846858941,23.4181728809532,-234.879894109809));
#213694=CARTESIAN_POINT('Ctrl Pts',(45.438886706838,23.6424549400482,-234.880250877479));
#213695=CARTESIAN_POINT('Ctrl Pts',(45.2644444625615,23.8667396990142,-234.880592984785));
#213696=CARTESIAN_POINT('Ctrl Pts',(45.0873500700682,24.0909207476239,-234.880915242521));
#213697=CARTESIAN_POINT('Ctrl Pts',(44.9562263439977,24.256908241605,-234.881153847676));
#213698=CARTESIAN_POINT('Ctrl Pts',(44.8236483565289,24.4228393854534,-234.881381566083));
#213699=CARTESIAN_POINT('Ctrl Pts',(44.6896149039642,24.5886707122256,-234.881596204268));
#213700=CARTESIAN_POINT('Ctrl Pts',(44.6437008912031,24.6454772892997,-234.881669729945));
#213701=CARTESIAN_POINT('Ctrl Pts',(44.5976160952632,24.7022721553739,-234.881741720083));
#213702=CARTESIAN_POINT('Ctrl Pts',(44.5513620989383,24.7590516304435,-234.881812082364));
#213703=CARTESIAN_POINT('Ctrl Pts',(44.545635411938,24.7660814723512,-234.881820793888));
#213704=CARTESIAN_POINT('Ctrl Pts',(44.5389068663795,24.7743365414615,-234.881830990484));
#213705=CARTESIAN_POINT('Ctrl Pts',(44.5341724311188,24.7801389607782,-234.881840625232));
#213706=CARTESIAN_POINT('Ctrl Pts',(44.5271568104213,24.7887371505964,-234.881854902274));
#213707=CARTESIAN_POINT('Ctrl Pts',(44.5201320288114,24.7973415118698,-234.881869112118));
#213708=CARTESIAN_POINT('Ctrl Pts',(44.5130980691041,24.8059520361687,-234.881883254527));
#213709=CARTESIAN_POINT('Ctrl Pts',(44.3158466991869,25.0474145671404,-234.882279846158));
#213710=CARTESIAN_POINT('Ctrl Pts',(44.1115390894415,25.2935411331283,-234.882622828519));
#213711=CARTESIAN_POINT('Ctrl Pts',(43.8999455772027,25.5440099170768,-234.882911996411));
#213712=CARTESIAN_POINT('Ctrl Pts',(43.6836301225591,25.8000681879592,-234.883207617403));
#213713=CARTESIAN_POINT('Ctrl Pts',(43.4596994985199,26.0606651779403,-234.883446999152));
#213714=CARTESIAN_POINT('Ctrl Pts',(43.2279311288734,26.3254037209598,-234.883629298961));
#213715=CARTESIAN_POINT('Ctrl Pts',(43.0126714435026,26.5712851393899,-234.883798613693));
#213716=CARTESIAN_POINT('Ctrl Pts',(42.7906507648766,26.8207388317917,-234.883918683362));
#213717=CARTESIAN_POINT('Ctrl Pts',(42.5617130696684,27.0734008284491,-234.883988328101));
#213718=CARTESIAN_POINT('Ctrl Pts',(42.5441553921939,27.0927779687813,-234.883993669291));
#213719=CARTESIAN_POINT('Ctrl Pts',(42.5265570430006,27.1121739565691,-234.883998713658));
#213720=CARTESIAN_POINT('Ctrl Pts',(42.5089179577211,27.1315886162052,-234.88400346055));
#213721=CARTESIAN_POINT('Ctrl Pts',(42.4499887161555,27.1964497555151,-234.884019319121));
#213722=CARTESIAN_POINT('Ctrl Pts',(42.3906068528995,27.2615162095477,-234.884032443793));
#213723=CARTESIAN_POINT('Ctrl Pts',(42.3307745648553,27.3267765754063,-234.884042740597));
#213724=CARTESIAN_POINT('Ctrl Pts',(42.0118162244203,27.674671310354,-234.884097631552));
#213725=CARTESIAN_POINT('Ctrl Pts',(41.6797936742668,28.0283910413513,-234.884071798873));
#213726=CARTESIAN_POINT('Ctrl Pts',(41.3345347980372,28.3865291569703,-234.883944724371));
#213727=CARTESIAN_POINT('Ctrl Pts',(41.1295224027873,28.5991891578229,-234.883869268387));
#213728=CARTESIAN_POINT('Ctrl Pts',(40.9198276686865,28.813423315708,-234.883757772487));
#213729=CARTESIAN_POINT('Ctrl Pts',(40.7054078632846,29.0289348621045,-234.883611946477));
#213730=CARTESIAN_POINT('Ctrl Pts',(40.5981979605837,29.1366906353028,-234.883539033472));
#213731=CARTESIAN_POINT('Ctrl Pts',(40.4898070746579,29.2447653313473,-234.883457642229));
#213732=CARTESIAN_POINT('Ctrl Pts',(40.3802316765946,29.353119299156,-234.883368704201));
#213733=CARTESIAN_POINT('Ctrl Pts',(40.325443977563,29.4072962830604,-234.883324235188));
#213734=CARTESIAN_POINT('Ctrl Pts',(40.2703601511891,29.4615430861951,-234.883277880788));
#213735=CARTESIAN_POINT('Ctrl Pts',(40.2149798991556,29.5158545609305,-234.883229817462));
#213736=CARTESIAN_POINT('Ctrl Pts',(40.1872897731388,29.5430102982982,-234.883205785799));
#213737=CARTESIAN_POINT('Ctrl Pts',(40.1595255407743,29.5701822037018,-234.883181327038));
#213738=CARTESIAN_POINT('Ctrl Pts',(40.1316871684786,29.5973696282592,-234.883156466412));
#213739=CARTESIAN_POINT('Ctrl Pts',(40.1177679823308,29.6109633405379,-234.883144036099));
#213740=CARTESIAN_POINT('Ctrl Pts',(40.1038302612033,29.6245609326156,-234.883131505329));
#213741=CARTESIAN_POINT('Ctrl Pts',(40.0898740052607,29.63816232471,-234.883118873174));
#213742=CARTESIAN_POINT('Ctrl Pts',(40.0828958772893,29.6449630207572,-234.883112557097));
#213743=CARTESIAN_POINT('Ctrl Pts',(40.0759131156145,29.6517646668093,-234.883106215674));
#213744=CARTESIAN_POINT('Ctrl Pts',(40.0689257220724,29.6585672537589,-234.883099846813));
#213745=CARTESIAN_POINT('Ctrl Pts',(40.0654320253014,29.6619685472337,-234.883096662382));
#213746=CARTESIAN_POINT('Ctrl Pts',(40.0619371705636,29.6653700759328,-234.883093471092));
#213747=CARTESIAN_POINT('Ctrl Pts',(40.0584411579672,29.6687718386519,-234.88309027282));
#213748=CARTESIAN_POINT('Ctrl Pts',(40.0549451453709,29.672173601371,-234.883087074548));
#213749=CARTESIAN_POINT('Ctrl Pts',(40.0502325503488,29.6767576351331,-234.88308275321));
#213750=CARTESIAN_POINT('Ctrl Pts',(40.0479496434506,29.6789778242853,-234.883080661882));
#213751=CARTESIAN_POINT('Ctrl Pts',(40.0397122613223,29.6869889028178,-234.883073115772));
#213752=CARTESIAN_POINT('Ctrl Pts',(40.0314600881385,29.6950094293739,-234.88306551114));
#213753=CARTESIAN_POINT('Ctrl Pts',(40.0231931152336,29.7030393665907,-234.883057847064));
#213754=CARTESIAN_POINT('Ctrl Pts',(39.7340648184162,29.9838776005799,-234.882789804435));
#213755=CARTESIAN_POINT('Ctrl Pts',(39.4270515363959,30.2761740869847,-234.882462612569));
#213756=CARTESIAN_POINT('Ctrl Pts',(39.101843125911,30.5783620144702,-234.882040882582));
#213757=CARTESIAN_POINT('Ctrl Pts',(38.7766347154261,30.8805499419557,-234.881619152595));
#213758=CARTESIAN_POINT('Ctrl Pts',(38.4332306415388,31.1926281065363,-234.881102902623));
#213759=CARTESIAN_POINT('Ctrl Pts',(38.0712682413355,31.513016787025,-234.880453655042));
#213760=CARTESIAN_POINT('Ctrl Pts',(37.7729361607464,31.7770835011195,-234.879918540395));
#213761=CARTESIAN_POINT('Ctrl Pts',(37.4619590556278,32.0468022993597,-234.87930828589));
#213762=CARTESIAN_POINT('Ctrl Pts',(37.1385945228072,32.320888272906,-234.878607331997));
#213763=CARTESIAN_POINT('Ctrl Pts',(36.8341596152557,32.5789293675489,-234.877947411653));
#213764=CARTESIAN_POINT('Ctrl Pts',(36.5187448436518,32.8408411776355,-234.877207085432));
#213765=CARTESIAN_POINT('Ctrl Pts',(36.1925832819071,33.105593930084,-234.876373009221));
#213766=CARTESIAN_POINT('Ctrl Pts',(36.0125010781191,33.2517707476859,-234.87591249425));
#213767=CARTESIAN_POINT('Ctrl Pts',(35.8291431433675,33.3988143820157,-234.875423394975));
#213768=CARTESIAN_POINT('Ctrl Pts',(35.6425517526153,33.5465577186068,-234.874903437951));
#213769=CARTESIAN_POINT('Ctrl Pts',(35.4441641375414,33.7036413228997,-234.874350609477));
#213770=CARTESIAN_POINT('Ctrl Pts',(35.2421697499994,33.8614772542077,-234.873763030408));
#213771=CARTESIAN_POINT('Ctrl Pts',(35.0366444584247,34.0198570237832,-234.873138336286));
#213772=CARTESIAN_POINT('Ctrl Pts',(34.7129239504967,34.2693191656913,-234.872154387806));
#213773=CARTESIAN_POINT('Ctrl Pts',(34.380467076446,34.519959127306,-234.871093998833));
#213774=CARTESIAN_POINT('Ctrl Pts',(34.0396050005138,34.7709265774286,-234.869961744777));
#213775=CARTESIAN_POINT('Ctrl Pts',(33.7084194077682,35.0147694968892,-234.86886163345));
#213776=CARTESIAN_POINT('Ctrl Pts',(33.3692989638713,35.258921486016,-234.86769369779));
#213777=CARTESIAN_POINT('Ctrl Pts',(33.0225787895569,35.5026409891713,-234.866464203128));
#213778=CARTESIAN_POINT('Ctrl Pts',(32.9437420428357,35.5580575878139,-234.866184642357));
#213779=CARTESIAN_POINT('Ctrl Pts',(32.8645125168478,35.6134519903396,-234.865901906941));
#213780=CARTESIAN_POINT('Ctrl Pts',(32.7848943935183,35.668815773732,-234.865616084469));
#213781=CARTESIAN_POINT('Ctrl Pts',(32.4766529029193,35.8831566097681,-234.864509523031));
#213782=CARTESIAN_POINT('Ctrl Pts',(32.1625673629801,36.0970471664988,-234.863356567381));
#213783=CARTESIAN_POINT('Ctrl Pts',(31.8430678702853,36.3099026177018,-234.862163622325));
#213784=CARTESIAN_POINT('Ctrl Pts',(31.526926929929,36.5205205499423,-234.86098321741));
#213785=CARTESIAN_POINT('Ctrl Pts',(31.2054851825615,36.7301249484346,-234.85976367324));
#213786=CARTESIAN_POINT('Ctrl Pts',(30.8791919628904,36.9381880666467,-234.858512247707));
#213787=CARTESIAN_POINT('Ctrl Pts',(30.556834934552,37.1437412453529,-234.857275918566));
#213788=CARTESIAN_POINT('Ctrl Pts',(30.2297427352299,37.347790071322,-234.856008487168));
#213789=CARTESIAN_POINT('Ctrl Pts',(29.898381554584,37.549864558993,-234.854717774197));
#213790=CARTESIAN_POINT('Ctrl Pts',(29.7835715652017,37.6198793076691,-234.854270568094));
#213791=CARTESIAN_POINT('Ctrl Pts',(29.6682493871885,37.689657388203,-234.853820573372));
#213792=CARTESIAN_POINT('Ctrl Pts',(29.5524353619883,37.7591803693088,-234.853368133768));
#213793=CARTESIAN_POINT('Ctrl Pts',(48.4267513656518,19.3969628773257,-234.872032644088));
#213794=CARTESIAN_POINT('Ctrl Pts',(48.051385728879,19.1580785346661,-235.35005));
#213795=CARTESIAN_POINT('Ctrl Pts',(47.5004483343777,18.8074595529617,-235.35005));
#213796=CARTESIAN_POINT('Ctrl Pts',(48.4549570879676,19.355316987603,-234.870489902149));
#213797=CARTESIAN_POINT('Ctrl Pts',(48.077778833099,19.1189416686644,-235.350049999978));
#213798=CARTESIAN_POINT('Ctrl Pts',(47.5233281555475,18.7715078669293,-235.35005));
#213799=CARTESIAN_POINT('Ctrl Pts',(48.4839707017497,19.3121694435219,-234.86855017653));
#213800=CARTESIAN_POINT('Ctrl Pts',(48.1045857201146,19.0788852177624,-235.350050000005));
#213801=CARTESIAN_POINT('Ctrl Pts',(47.5458232280531,18.7353573183218,-235.35005));
#213802=CARTESIAN_POINT('Ctrl Pts',(48.5451033552256,19.2200302642562,-234.863016541227));
#213803=CARTESIAN_POINT('Ctrl Pts',(48.1599244780088,18.99523376352,-235.350049999995));
#213804=CARTESIAN_POINT('Ctrl Pts',(47.5895300323829,18.6623978031499,-235.35005));
#213805=CARTESIAN_POINT('Ctrl Pts',(48.5781288595687,19.1699035489294,-234.859044174147));
#213806=CARTESIAN_POINT('Ctrl Pts',(48.1890852791867,18.9509743482895,-235.350050000003));
#213807=CARTESIAN_POINT('Ctrl Pts',(47.6106972731343,18.625565406903,-235.35005));
#213808=CARTESIAN_POINT('Ctrl Pts',(48.6248763884555,19.0947802943512,-234.853271204071));
#213809=CARTESIAN_POINT('Ctrl Pts',(48.2306061221348,18.8843051626248,-235.350049999998));
#213810=CARTESIAN_POINT('Ctrl Pts',(47.6410934853577,18.569620618322,-235.35005));
#213811=CARTESIAN_POINT('Ctrl Pts',(48.6396028929279,19.0702227963992,-234.851536427768));
#213812=CARTESIAN_POINT('Ctrl Pts',(48.2438148297685,18.8622892880126,-235.350049999998));
#213813=CARTESIAN_POINT('Ctrl Pts',(47.6510095952452,18.550861366784,-235.35005));
#213814=CARTESIAN_POINT('Ctrl Pts',(48.6656509039339,19.0245062658543,-234.849261045971));
#213815=CARTESIAN_POINT('Ctrl Pts',(48.267810580405,18.8200790514748,-235.350050000002));
#213816=CARTESIAN_POINT('Ctrl Pts',(47.6705745922183,18.513205530003,-235.35005));
#213817=CARTESIAN_POINT('Ctrl Pts',(48.6767455877554,19.0036730196651,-234.848826976569));
#213818=CARTESIAN_POINT('Ctrl Pts',(48.2784387534682,18.8000789112269,-235.350050000001));
#213819=CARTESIAN_POINT('Ctrl Pts',(47.6802441619202,18.4943195741576,-235.35005));
#213820=CARTESIAN_POINT('Ctrl Pts',(48.7115701984993,18.9389677368683,-234.84683711776));
#213821=CARTESIAN_POINT('Ctrl Pts',(48.3113401572838,18.738781310839,-235.350049999999));
#213822=CARTESIAN_POINT('Ctrl Pts',(47.7090490788398,18.4375569718045,-235.35005));
#213823=CARTESIAN_POINT('Ctrl Pts',(48.7350953123161,18.8948187861069,-234.845248112377));
#213824=CARTESIAN_POINT('Ctrl Pts',(48.3333974993269,18.6972683757834,-235.350050000006));
#213825=CARTESIAN_POINT('Ctrl Pts',(47.7279282401082,18.3995486637502,-235.35005));
#213826=CARTESIAN_POINT('Ctrl Pts',(48.7834587614873,18.8028811954349,-234.841054202938));
#213827=CARTESIAN_POINT('Ctrl Pts',(48.3781881568565,18.6119741954475,-235.350049999994));
#213828=CARTESIAN_POINT('Ctrl Pts',(47.7647487546851,18.3230500802882,-235.35005));
#213829=CARTESIAN_POINT('Ctrl Pts',(48.8085457779383,18.754824580439,-234.838353991562));
#213830=CARTESIAN_POINT('Ctrl Pts',(48.4011086067165,18.5680238025553,-235.350050000015));
#213831=CARTESIAN_POINT('Ctrl Pts',(47.7827001660699,18.2845649741211,-235.35005));
#213832=CARTESIAN_POINT('Ctrl Pts',(48.8608504474587,18.6521989438873,-234.831101974325));
#213833=CARTESIAN_POINT('Ctrl Pts',(48.4481394235988,18.4760651492002,-235.350049999984));
#213834=CARTESIAN_POINT('Ctrl Pts',(47.81709615277,18.2068203539689,-235.35005));
#213835=CARTESIAN_POINT('Ctrl Pts',(48.8859768835832,18.6002207271149,-234.827451251642));
#213836=CARTESIAN_POINT('Ctrl Pts',(48.4707622377245,18.4294985425077,-235.350049999999));
#213837=CARTESIAN_POINT('Ctrl Pts',(47.8335233281929,18.1675458631259,-235.35005));
#213838=CARTESIAN_POINT('Ctrl Pts',(48.9317590979678,18.4991718431838,-234.821404066159));
#213839=CARTESIAN_POINT('Ctrl Pts',(48.5125008275188,18.3376757598027,-235.350050000001));
#213840=CARTESIAN_POINT('Ctrl Pts',(47.8650504941538,18.0883394728593,-235.35005));
#213841=CARTESIAN_POINT('Ctrl Pts',(48.9515891654281,18.4514986637869,-234.819445110721));
#213842=CARTESIAN_POINT('Ctrl Pts',(48.5309876753933,18.2932822237603,-235.350050000003));
#213843=CARTESIAN_POINT('Ctrl Pts',(47.8801543850424,18.0485058523287,-235.35005));
#213844=CARTESIAN_POINT('Ctrl Pts',(48.9911458371249,18.3546372294721,-234.814928550212));
#213845=CARTESIAN_POINT('Ctrl Pts',(48.5677267083794,18.2034775571371,-235.350049999996));
#213846=CARTESIAN_POINT('Ctrl Pts',(47.9094666156693,17.9685258021276,-235.35005));
#213847=CARTESIAN_POINT('Ctrl Pts',(49.0112209584123,18.3047581611111,-234.812156424171));
#213848=CARTESIAN_POINT('Ctrl Pts',(48.5862296950314,18.1576503455933,-235.350050000007));
#213849=CARTESIAN_POINT('Ctrl Pts',(47.9236194657386,17.9283599903447,-235.35005));
#213850=CARTESIAN_POINT('Ctrl Pts',(49.0522465206321,18.2003746116001,-234.805011039778));
#213851=CARTESIAN_POINT('Ctrl Pts',(48.6236963620426,18.0631017745501,-235.350049999994));
#213852=CARTESIAN_POINT('Ctrl Pts',(47.9505381729848,17.8475439007782,-235.35005));
#213853=CARTESIAN_POINT('Ctrl Pts',(49.0738330944827,18.1446322248529,-234.800204572025));
#213854=CARTESIAN_POINT('Ctrl Pts',(48.6431636354573,18.013619351879,-235.350050000009));
#213855=CARTESIAN_POINT('Ctrl Pts',(47.9632560597789,17.8068666429648,-235.35005));
#213856=CARTESIAN_POINT('Ctrl Pts',(49.1128299645569,18.0356471582971,-234.79145959571));
#213857=CARTESIAN_POINT('Ctrl Pts',(48.6787156361984,17.9158184822153,-235.350049999991));
#213858=CARTESIAN_POINT('Ctrl Pts',(47.9870034052699,17.7249653914156,-235.35005));
#213859=CARTESIAN_POINT('Ctrl Pts',(49.1305989485082,17.9820590712204,-234.787374959526));
#213860=CARTESIAN_POINT('Ctrl Pts',(48.695062620387,17.8673394303137,-235.35005000001));
#213861=CARTESIAN_POINT('Ctrl Pts',(47.9980630400304,17.6838206475214,-235.35005));
#213862=CARTESIAN_POINT('Ctrl Pts',(49.1628022975924,17.8778595100161,-234.780195549906));
#213863=CARTESIAN_POINT('Ctrl Pts',(48.7249821608991,17.7719530069924,-235.35004999999));
#213864=CARTESIAN_POINT('Ctrl Pts',(48.0189197776842,17.6012300921137,-235.35005));
#213865=CARTESIAN_POINT('Ctrl Pts',(49.1780152194113,17.8259868345273,-234.776643381592));
#213866=CARTESIAN_POINT('Ctrl Pts',(48.7391768429728,17.7243103604292,-235.350049999995));
#213867=CARTESIAN_POINT('Ctrl Pts',(48.0287613458656,17.5597948840364,-235.35005));
#213868=CARTESIAN_POINT('Ctrl Pts',(49.2088831316691,17.7175974214052,-234.76777083952));
#213869=CARTESIAN_POINT('Ctrl Pts',(48.7678666087892,17.6260826000281,-235.350050000005));
#213870=CARTESIAN_POINT('Ctrl Pts',(48.0470227250193,17.4765854309817,-235.35005));
#213871=CARTESIAN_POINT('Ctrl Pts',(49.2241633474364,17.6616758881998,-234.762670691852));
#213872=CARTESIAN_POINT('Ctrl Pts',(48.7820703212585,17.575815576902,-235.350050000005));
#213873=CARTESIAN_POINT('Ctrl Pts',(48.0554329780656,17.4347916601489,-235.35005));
#213874=CARTESIAN_POINT('Ctrl Pts',(49.252818588968,17.5488204678451,-234.751966143146));
#213875=CARTESIAN_POINT('Ctrl Pts',(48.8088973471943,17.474458441837,-235.350049999995));
#213876=CARTESIAN_POINT('Ctrl Pts',(48.0705953135359,17.3508835165529,-235.35005));
#213877=CARTESIAN_POINT('Ctrl Pts',(49.2656967371983,17.493038371525,-234.746774003745));
#213878=CARTESIAN_POINT('Ctrl Pts',(48.8210830469464,17.4240853616799,-235.35005));
#213879=CARTESIAN_POINT('Ctrl Pts',(48.0773499548877,17.3088369763077,-235.350050000001));
#213880=CARTESIAN_POINT('Ctrl Pts',(49.2886686943366,17.3835528691795,-234.737089395268));
#213881=CARTESIAN_POINT('Ctrl Pts',(48.8430358085064,17.3244453325067,-235.35005));
#213882=CARTESIAN_POINT('Ctrl Pts',(48.0894592880343,17.2245872750773,-235.350050000001));
#213883=CARTESIAN_POINT('Ctrl Pts',(49.2982406085014,17.331247813801,-234.733146358298));
#213884=CARTESIAN_POINT('Ctrl Pts',(48.8522983790287,17.2760488789422,-235.350050000014));
#213885=CARTESIAN_POINT('Ctrl Pts',(48.094834615712,17.1823864227582,-235.35005));
#213886=CARTESIAN_POINT('Ctrl Pts',(49.3275288703794,17.1670149718797,-234.71835081978));
#213887=CARTESIAN_POINT('Ctrl Pts',(48.8808279281815,17.1260157446175,-235.350049999972));
#213888=CARTESIAN_POINT('Ctrl Pts',(48.1091464500575,17.0555809060241,-235.35005));
#213889=CARTESIAN_POINT('Ctrl Pts',(49.3473085304738,17.0432902293076,-234.703208934491));
#213890=CARTESIAN_POINT('Ctrl Pts',(48.9006204915337,17.0169034054434,-235.35004999989));
#213891=CARTESIAN_POINT('Ctrl Pts',(48.1154436500424,16.9706923807857,-235.350050000001));
#213892=CARTESIAN_POINT('Ctrl Pts',(49.3584215990167,16.9360371933353,-234.693305891908));
#213893=CARTESIAN_POINT('Ctrl Pts',(48.9123686178224,16.9178382234301,-235.350050000001));
#213894=CARTESIAN_POINT('Ctrl Pts',(48.1189208895433,16.8854655414009,-235.350050000001));
#213895=CARTESIAN_POINT('',(49.3576635057812,16.9360062631145,-234.694420988467));
#213896=CARTESIAN_POINT('',(48.1189208895436,16.8854655414,-235.35005));
#213897=CARTESIAN_POINT('Origin',(48.1189208895436,16.8854655414,-233.85005));
#213898=CARTESIAN_POINT('Ctrl Pts',(47.5004483343782,18.8074595529612,-235.35005));
#213899=CARTESIAN_POINT('Ctrl Pts',(47.523328218883,18.7715077674088,-235.35005));
#213900=CARTESIAN_POINT('Ctrl Pts',(47.5458232845143,18.7353572240715,-235.35005));
#213901=CARTESIAN_POINT('Ctrl Pts',(47.5676766302509,18.6988775607556,-235.35005));
#213902=CARTESIAN_POINT('Ctrl Pts',(47.5895300808456,18.6623977224007,-235.35005));
#213903=CARTESIAN_POINT('Ctrl Pts',(47.6106973144047,18.6255653312655,-235.35005));
#213904=CARTESIAN_POINT('Ctrl Pts',(47.6309614148883,18.58826888133,-235.35005));
#213905=CARTESIAN_POINT('Ctrl Pts',(47.6410934945813,18.5696206021569,-235.35005));
#213906=CARTESIAN_POINT('Ctrl Pts',(47.6510096037987,18.5508613513732,-235.35005));
#213907=CARTESIAN_POINT('Ctrl Pts',(47.6607920942703,18.5320334486734,-235.35005));
#213908=CARTESIAN_POINT('Ctrl Pts',(47.6705746000884,18.513205516437,-235.35005));
#213909=CARTESIAN_POINT('Ctrl Pts',(47.6802441693448,18.4943195614609,-235.35005));
#213910=CARTESIAN_POINT('Ctrl Pts',(47.6898458018307,18.4753987071822,-235.35005));
#213911=CARTESIAN_POINT('Ctrl Pts',(47.70904910136,18.4375569305264,-235.35005));
#213912=CARTESIAN_POINT('Ctrl Pts',(47.7279282587774,18.3995486292809,-235.35005));
#213913=CARTESIAN_POINT('Ctrl Pts',(47.7463384996528,18.3612993731052,-235.35005));
#213914=CARTESIAN_POINT('Ctrl Pts',(47.7647487677154,18.323050060445,-235.35005));
#213915=CARTESIAN_POINT('Ctrl Pts',(47.7827001759863,18.2845649614141,-235.35005));
#213916=CARTESIAN_POINT('Ctrl Pts',(47.7998981639292,18.24569266604,-235.35005));
#213917=CARTESIAN_POINT('Ctrl Pts',(47.8170961582275,18.2068203563009,-235.35005));
#213918=CARTESIAN_POINT('Ctrl Pts',(47.8335233318918,18.1675458731571,-235.35005));
#213919=CARTESIAN_POINT('Ctrl Pts',(47.8492869191686,18.127942671175,-235.35005));
#213920=CARTESIAN_POINT('Ctrl Pts',(47.8650504948173,18.0883394984066,-235.35005));
#213921=CARTESIAN_POINT('Ctrl Pts',(47.8801543852333,18.0485058859946,-235.35005));
#213922=CARTESIAN_POINT('Ctrl Pts',(47.8948105132744,18.0085158319627,-235.35005));
#213923=CARTESIAN_POINT('Ctrl Pts',(47.909466614277,17.9685258517065,-235.35005));
#213924=CARTESIAN_POINT('Ctrl Pts',(47.9236194654021,17.9283600484622,-235.35005));
#213925=CARTESIAN_POINT('Ctrl Pts',(47.9370788390041,17.887951952103,-235.35005));
#213926=CARTESIAN_POINT('Ctrl Pts',(47.9505379989423,17.847544497211,-235.35005));
#213927=CARTESIAN_POINT('Ctrl Pts',(47.9632559353684,17.8068671621608,-235.35005));
#213928=CARTESIAN_POINT('Ctrl Pts',(47.9751297575526,17.7659160244471,-235.35005));
#213929=CARTESIAN_POINT('Ctrl Pts',(47.9870033323709,17.7249657398638,-235.35005));
#213930=CARTESIAN_POINT('Ctrl Pts',(47.9980630011651,17.6838209125432,-235.35005));
#213931=CARTESIAN_POINT('Ctrl Pts',(48.0084914348375,17.6425253763784,-235.35005));
#213932=CARTESIAN_POINT('Ctrl Pts',(48.0189197816014,17.6012301843623,-235.35005));
#213933=CARTESIAN_POINT('Ctrl Pts',(48.0287613705984,17.5597948897797,-235.35005));
#213934=CARTESIAN_POINT('Ctrl Pts',(48.0378920589035,17.5181901626578,-235.35005));
#213935=CARTESIAN_POINT('Ctrl Pts',(48.0470227852353,17.4765852622638,-235.35005));
#213936=CARTESIAN_POINT('Ctrl Pts',(48.0554330459596,17.4347914019545,-235.35005));
#213937=CARTESIAN_POINT('Ctrl Pts',(48.063014164453,17.3928375917214,-235.35005));
#213938=CARTESIAN_POINT('Ctrl Pts',(48.0705954092764,17.3508830823798,-235.35005));
#213939=CARTESIAN_POINT('Ctrl Pts',(48.0773500452528,17.3088364520712,-235.350050000001));
#213940=CARTESIAN_POINT('Ctrl Pts',(48.0834046340598,17.2667121275033,-235.350050000001));
#213941=CARTESIAN_POINT('Ctrl Pts',(48.0894593994455,17.2245865744039,-235.350050000001));
#213942=CARTESIAN_POINT('Ctrl Pts',(48.0948347135637,17.1823856312802,-235.35005));
#213943=CARTESIAN_POINT('Ctrl Pts',(48.0996052337066,17.140117917919,-235.35005));
#213944=CARTESIAN_POINT('Ctrl Pts',(48.1091469299998,17.0555766788456,-235.35005));
#213945=CARTESIAN_POINT('Ctrl Pts',(48.115443852909,16.9706874085479,-235.350050000001));
#213946=CARTESIAN_POINT('Ctrl Pts',(48.1189208895436,16.885465541401,-235.350050000001));
#213947=CARTESIAN_POINT('Ctrl Pts',(49.3576635057812,16.9360062631145,-234.694420988467));
#213948=CARTESIAN_POINT('Ctrl Pts',(49.3471263105466,17.0376600850593,-234.703795085131));
#213949=CARTESIAN_POINT('Ctrl Pts',(49.3364864909818,17.1066695044026,-234.711288975797));
#213950=CARTESIAN_POINT('Ctrl Pts',(49.3237382757546,17.184198787297,-234.719709502799));
#213951=CARTESIAN_POINT('Ctrl Pts',(49.3199917485045,17.2054352035257,-234.722046293634));
#213952=CARTESIAN_POINT('Ctrl Pts',(49.3153257977579,17.231486737478,-234.724846402637));
#213953=CARTESIAN_POINT('Ctrl Pts',(49.3139282901745,17.2391949265268,-234.72566225943));
#213954=CARTESIAN_POINT('Ctrl Pts',(49.3120847413681,17.2493712815277,-234.726709775306));
#213955=CARTESIAN_POINT('Ctrl Pts',(49.3112260642013,17.2541124666259,-234.727189465917));
#213956=CARTESIAN_POINT('Ctrl Pts',(49.3103374053008,17.2590488483845,-234.727671987138));
#213957=CARTESIAN_POINT('Ctrl Pts',(49.3099810386723,17.2610379965402,-234.727862256699));
#213958=CARTESIAN_POINT('Ctrl Pts',(49.3097489286637,17.2623361089118,-234.727985430796));
#213959=CARTESIAN_POINT('Ctrl Pts',(49.309846238275,17.2617880108445,-234.727934861414));
#213960=CARTESIAN_POINT('Ctrl Pts',(49.2992464648262,17.3213294243835,-234.733486618467));
#213961=CARTESIAN_POINT('Ctrl Pts',(49.2884703228539,17.3767076195097,-234.738564343094));
#213962=CARTESIAN_POINT('Ctrl Pts',(49.2716034836387,17.4576229182381,-234.745722233989));
#213963=CARTESIAN_POINT('Ctrl Pts',(49.2658594168752,17.4841982801646,-234.74803174828));
#213964=CARTESIAN_POINT('Ctrl Pts',(49.2541192293622,17.536662236027,-234.75249787818));
#213965=CARTESIAN_POINT('Ctrl Pts',(49.2486124761573,17.5605060465331,-234.754488334413));
#213966=CARTESIAN_POINT('Ctrl Pts',(49.2287650942653,17.6434371614011,-234.761227311344));
#213967=CARTESIAN_POINT('Ctrl Pts',(49.2145175041624,17.6969874216763,-234.765957475731));
#213968=CARTESIAN_POINT('Ctrl Pts',(49.1974893808914,17.7556761004413,-234.771546112902));
#213969=CARTESIAN_POINT('Ctrl Pts',(49.1955835644542,17.7621753990853,-234.77217078373));
#213970=CARTESIAN_POINT('Ctrl Pts',(49.1917448889839,17.7751320132382,-234.77342754767));
#213971=CARTESIAN_POINT('Ctrl Pts',(49.1922453722157,17.7734577366325,-234.773256809092));
#213972=CARTESIAN_POINT('Ctrl Pts',(49.1903887257174,17.7799422846575,-234.773791614339));
#213973=CARTESIAN_POINT('Ctrl Pts',(49.1884660325305,17.7867464598314,-234.774315162155));
#213974=CARTESIAN_POINT('Ctrl Pts',(49.1805664619759,17.8144826479086,-234.776386838561));
#213975=CARTESIAN_POINT('Ctrl Pts',(49.1724695390079,17.8427478887243,-234.778436000106));
#213976=CARTESIAN_POINT('Ctrl Pts',(49.1555043287524,17.8989903998451,-234.782511808337));
#213977=CARTESIAN_POINT('Ctrl Pts',(49.1490482401721,17.9200399629343,-234.784037422065));
#213978=CARTESIAN_POINT('Ctrl Pts',(49.139870853538,17.949153615481,-234.786153202958));
#213979=CARTESIAN_POINT('Ctrl Pts',(49.1382049819289,17.9543986428311,-234.786534456923));
#213980=CARTESIAN_POINT('Ctrl Pts',(49.1360928848702,17.9610269698035,-234.787017684095));
#213981=CARTESIAN_POINT('Ctrl Pts',(49.1329147871453,17.97096000841,-234.787743929867));
#213982=CARTESIAN_POINT('Ctrl Pts',(49.1211497879488,18.0072816681923,-234.790422286177));
#213983=CARTESIAN_POINT('Ctrl Pts',(49.1012598894988,18.0662235069236,-234.794889351849));
#213984=CARTESIAN_POINT('Ctrl Pts',(49.0825174881958,18.1181924771152,-234.798979971364));
#213985=CARTESIAN_POINT('Ctrl Pts',(49.0680042665894,18.1571143825403,-234.802092896427));
#213986=CARTESIAN_POINT('Ctrl Pts',(49.0630898685875,18.1700799530162,-234.803138031519));
#213987=CARTESIAN_POINT('Ctrl Pts',(49.0555990686584,18.1895248967006,-234.804716974264));
#213988=CARTESIAN_POINT('Ctrl Pts',(49.0518243968624,18.1992458491427,-234.805509255663));
#213989=CARTESIAN_POINT('Ctrl Pts',(49.0480071657046,18.2089635528941,-234.806305752102));
#213990=CARTESIAN_POINT('Ctrl Pts',(49.0454530370347,18.215441192851,-234.806837686404));
#213991=CARTESIAN_POINT('Ctrl Pts',(49.0436037898865,18.2201082125008,-234.807221882863));
#213992=CARTESIAN_POINT('Ctrl Pts',(49.0371348733642,18.236392118303,-234.808564168568));
#213993=CARTESIAN_POINT('Ctrl Pts',(49.02932205209,18.2565451559845,-234.809914794572));
#213994=CARTESIAN_POINT('Ctrl Pts',(49.0141489881303,18.2952634232637,-234.812176958313));
#213995=CARTESIAN_POINT('Ctrl Pts',(49.00569672982,18.3167439603432,-234.813367096367));
#213996=CARTESIAN_POINT('Ctrl Pts',(48.9958664941424,18.3413881453924,-234.814645818696));
#213997=CARTESIAN_POINT('Ctrl Pts',(48.9889979076846,18.3585171481307,-234.815517985643));
#213998=CARTESIAN_POINT('Ctrl Pts',(48.9858598222626,18.3663118599993,-234.815908817181));
#213999=CARTESIAN_POINT('Ctrl Pts',(48.9648229823787,18.4182202217313,-234.818463134686));
#214000=CARTESIAN_POINT('Ctrl Pts',(48.9507413163091,18.4516566711652,-234.820134628404));
#214001=CARTESIAN_POINT('Ctrl Pts',(48.9343809176692,18.4899400549726,-234.822083928554));
#214002=CARTESIAN_POINT('Ctrl Pts',(48.9297104857026,18.5007288856637,-234.822640705199));
#214003=CARTESIAN_POINT('Ctrl Pts',(48.923937278621,18.5139601119533,-234.82333638506));
#214004=CARTESIAN_POINT('Ctrl Pts',(48.9213588397062,18.5198371515105,-234.823649353714));
#214005=CARTESIAN_POINT('Ctrl Pts',(48.9192525948475,18.5246043300423,-234.823910015452));
#214006=CARTESIAN_POINT('Ctrl Pts',(48.9179543035251,18.52753551139,-234.824072166185));
#214007=CARTESIAN_POINT('Ctrl Pts',(48.9181500023951,18.5271000257874,-234.824046111913));
#214008=CARTESIAN_POINT('Ctrl Pts',(48.8954594683543,18.5780343181537,-234.826949191156));
#214009=CARTESIAN_POINT('Ctrl Pts',(48.8729488554902,18.6261902513722,-234.829886574551));
#214010=CARTESIAN_POINT('Ctrl Pts',(48.8363463911418,18.7002781537299,-234.834600259925));
#214011=CARTESIAN_POINT('Ctrl Pts',(48.8236560944642,18.7253040017816,-234.836222756763));
#214012=CARTESIAN_POINT('Ctrl Pts',(48.8038443429534,18.7634090756344,-234.83873340459));
#214013=CARTESIAN_POINT('Ctrl Pts',(48.7937510442086,18.7825948905538,-234.840007954146));
#214014=CARTESIAN_POINT('Ctrl Pts',(48.7807985548326,18.8068120782162,-234.841637189171));
#214015=CARTESIAN_POINT('Ctrl Pts',(48.7746647465271,18.8181753396998,-234.842407311938));
#214016=CARTESIAN_POINT('Ctrl Pts',(48.7711382294178,18.8246834174458,-234.842849785296));
#214017=CARTESIAN_POINT('Ctrl Pts',(48.7694150713952,18.8278574582801,-234.843065921241));
#214018=CARTESIAN_POINT('Ctrl Pts',(48.7686422398806,18.8292800854102,-234.843162847327));
#214019=CARTESIAN_POINT('Ctrl Pts',(48.7622006952152,18.8418648134774,-234.843660628641));
#214020=CARTESIAN_POINT('Ctrl Pts',(48.7432200186877,18.8782325404045,-234.845017135759));
#214021=CARTESIAN_POINT('Ctrl Pts',(48.7353260165666,18.8932819489295,-234.845570943989));
#214022=CARTESIAN_POINT('Ctrl Pts',(48.7209372066814,18.9204072865677,-234.846554115121));
#214023=CARTESIAN_POINT('Ctrl Pts',(48.7131049616897,18.9351084395387,-234.847083815383));
#214024=CARTESIAN_POINT('Ctrl Pts',(48.7028006926672,18.9542924498671,-234.847768499741));
#214025=CARTESIAN_POINT('Ctrl Pts',(48.6981288815276,18.9629542167293,-234.848076228906));
#214026=CARTESIAN_POINT('Ctrl Pts',(48.694956886559,18.9688270098263,-234.848284557907));
#214027=CARTESIAN_POINT('Ctrl Pts',(48.6926764803002,18.9730416096279,-234.848433780606));
#214028=CARTESIAN_POINT('Ctrl Pts',(48.6760489926829,19.0037412762689,-234.849519581485));
#214029=CARTESIAN_POINT('Ctrl Pts',(48.6614284555105,19.0299997531886,-234.850656844783));
#214030=CARTESIAN_POINT('Ctrl Pts',(48.6408431073285,19.065833411723,-234.852535739319));
#214031=CARTESIAN_POINT('Ctrl Pts',(48.6341892896175,19.077205959928,-234.853190870762));
#214032=CARTESIAN_POINT('Ctrl Pts',(48.6245121798185,19.0934316734949,-234.854216817824));
#214033=CARTESIAN_POINT('Ctrl Pts',(48.6197504107073,19.1013350867889,-234.85474060383));
#214034=CARTESIAN_POINT('Ctrl Pts',(48.6151090556708,19.1089199751746,-234.855280608546));
#214035=CARTESIAN_POINT('Ctrl Pts',(48.6120425369725,19.1139047949247,-234.855644215849));
#214036=CARTESIAN_POINT('Ctrl Pts',(48.6117051735357,19.1144605947675,-234.855682204168));
#214037=CARTESIAN_POINT('Ctrl Pts',(48.5230305908126,19.2570495990898,-234.866606036447));
#214038=CARTESIAN_POINT('Ctrl Pts',(48.4379564955549,19.37902047629,-234.872226499439));
#214039=CARTESIAN_POINT('Ctrl Pts',(48.4260896922586,19.3965417854656,-234.872874618363));
#214040=CARTESIAN_POINT('Ctrl Pts',(49.357663505782,16.9360062631151,-234.694420988466));
#214041=CARTESIAN_POINT('Ctrl Pts',(48.9115061644421,16.9178030353144,-235.35005));
#214042=CARTESIAN_POINT('Ctrl Pts',(48.1189208895436,16.8854655414,-235.35005));
#214043=CARTESIAN_POINT('Ctrl Pts',(49.4635649335608,14.3752531202943,-234.692333873014));
#214044=CARTESIAN_POINT('Ctrl Pts',(49.0175817386228,14.3575637238871,-235.350050000391));
#214045=CARTESIAN_POINT('Ctrl Pts',(48.2232158057592,14.3292187542857,-235.35005));
#214046=CARTESIAN_POINT('Ctrl Pts',(49.5551530156078,11.8140213189959,-234.690527234957));
#214047=CARTESIAN_POINT('Ctrl Pts',(49.1092649251398,11.7982892962054,-235.350049999822));
#214048=CARTESIAN_POINT('Ctrl Pts',(48.3134219778347,11.7724738102799,-235.35005));
#214049=CARTESIAN_POINT('Ctrl Pts',(49.6324230235364,9.25223577675678,-234.689044294154));
#214050=CARTESIAN_POINT('Ctrl Pts',(49.1866080561977,9.23896306516062,-235.35005));
#214051=CARTESIAN_POINT('Ctrl Pts',(48.3895556141632,9.21523338364434,-235.35005));
#214052=CARTESIAN_POINT('',(49.6324231701066,9.25223524236281,-234.689044137434));
#214053=CARTESIAN_POINT('',(48.3895556141631,9.21523338364434,-235.35005));
#214054=CARTESIAN_POINT('Origin',(48.3895556141631,9.21523338364435,-233.85005));
#214055=CARTESIAN_POINT('Origin',(-648.115804222842,-11.5202125232578,-235.35005));
#214056=CARTESIAN_POINT('Origin',(-637.557461367465,-11.4839373498759,-249.18849675272));
#214057=CARTESIAN_POINT('Ctrl Pts',(49.6182572724309,9.33632588644485,-234.704271307837));
#214058=CARTESIAN_POINT('Ctrl Pts',(49.1716671980127,9.3093937125164,-235.35005));
#214059=CARTESIAN_POINT('Ctrl Pts',(48.3874683444157,9.26207687868008,-235.35005));
#214060=CARTESIAN_POINT('Ctrl Pts',(49.6801828044406,8.99887464788128,-234.643882192716));
#214061=CARTESIAN_POINT('Ctrl Pts',(49.2361268524121,9.02379200969491,-235.35005));
#214062=CARTESIAN_POINT('Ctrl Pts',(48.3986160847539,9.0744362502198,-235.35005));
#214063=CARTESIAN_POINT('Ctrl Pts',(49.6817690797009,8.67461962826136,-234.572387045798));
#214064=CARTESIAN_POINT('Ctrl Pts',(49.2558123914512,8.74313449703487,-235.35005));
#214065=CARTESIAN_POINT('Ctrl Pts',(48.3759406125794,8.88996799364191,-235.35005));
#214066=CARTESIAN_POINT('Ctrl Pts',(49.6381916686217,8.36177935226001,-234.492922371952));
#214067=CARTESIAN_POINT('Ctrl Pts',(49.2451518560708,8.46585266699427,-235.35005));
#214068=CARTESIAN_POINT('Ctrl Pts',(48.3280835873607,8.70872798446653,-235.35005));
#214069=CARTESIAN_POINT('',(49.648078203028,8.44024209172928,-234.512742084672));
#214070=CARTESIAN_POINT('',(48.3395182384274,8.75410525715259,-235.35005));
#214071=CARTESIAN_POINT('Origin',(48.3395182384273,8.75410525715261,-233.85005));
#214072=CARTESIAN_POINT('Ctrl Pts',(48.3895556141631,9.21523338364434,-235.35005));
#214073=CARTESIAN_POINT('Ctrl Pts',(48.3942007072891,9.05921010043768,-235.35005));
#214074=CARTESIAN_POINT('Ctrl Pts',(48.3758739100739,8.90567951512196,-235.35005));
#214075=CARTESIAN_POINT('Ctrl Pts',(48.3395182384274,8.75410525715259,-235.35005));
#214076=CARTESIAN_POINT('Ctrl Pts',(49.6480782611736,8.44024207778281,-234.512742114119));
#214077=CARTESIAN_POINT('Ctrl Pts',(49.6564789856231,8.51381412335654,-234.530999061222));
#214078=CARTESIAN_POINT('Ctrl Pts',(49.6621158262273,8.58669833526729,-234.548485647682));
#214079=CARTESIAN_POINT('Ctrl Pts',(49.6651766405904,8.65862169244825,-234.565154268152));
#214080=CARTESIAN_POINT('Ctrl Pts',(49.6682696610215,8.73130183140451,-234.581998276824));
#214081=CARTESIAN_POINT('Ctrl Pts',(49.6687327302347,8.80300040771396,-234.598007149397));
#214082=CARTESIAN_POINT('Ctrl Pts',(49.6667833420853,8.8734684012847,-234.613167697683));
#214083=CARTESIAN_POINT('Ctrl Pts',(49.6647943790958,8.94536697684644,-234.62863602268));
#214084=CARTESIAN_POINT('Ctrl Pts',(49.6602945997359,9.01598417424433,-234.643221410519));
#214085=CARTESIAN_POINT('Ctrl Pts',(49.6535306620587,9.08509487754269,-234.656944741809));
#214086=CARTESIAN_POINT('Ctrl Pts',(49.6479751661887,9.14185829628876,-234.668216269421));
#214087=CARTESIAN_POINT('Ctrl Pts',(49.6408926996888,9.19760616622859,-234.678906993986));
#214088=CARTESIAN_POINT('Ctrl Pts',(49.6324234200406,9.25223473081225,-234.689043900262));
#214089=CARTESIAN_POINT('Ctrl Pts',(49.6728514995601,8.43430012080101,-234.458282759328));
#214090=CARTESIAN_POINT('Ctrl Pts',(49.288180041945,8.52656505676208,-235.35005));
#214091=CARTESIAN_POINT('Ctrl Pts',(48.3395182384273,8.75410525715258,-235.35005));
#214092=CARTESIAN_POINT('Ctrl Pts',(49.4713806247164,7.68476869375633,-234.505836736672));
#214093=CARTESIAN_POINT('Ctrl Pts',(49.068969900047,7.76950806478782,-235.350049999891));
#214094=CARTESIAN_POINT('Ctrl Pts',(48.1420785222883,7.9309385499425,-235.35005));
#214095=CARTESIAN_POINT('Ctrl Pts',(49.3314010681958,6.92971336337434,-234.544835134207));
#214096=CARTESIAN_POINT('Ctrl Pts',(48.9137610316686,6.99112774713473,-235.350049999976));
#214097=CARTESIAN_POINT('Ctrl Pts',(48.0110562568883,7.10334135417386,-235.35005));
#214098=CARTESIAN_POINT('Ctrl Pts',(49.1759346319862,5.40665728715258,-234.609024663255));
#214099=CARTESIAN_POINT('Ctrl Pts',(48.7409159667592,5.4240408590254,-235.350050000024));
#214100=CARTESIAN_POINT('Ctrl Pts',(47.8801847113252,5.43950276679566,-235.35005));
#214101=CARTESIAN_POINT('Ctrl Pts',(49.160538186931,4.63912183635817,-234.634271526073));
#214102=CARTESIAN_POINT('Ctrl Pts',(48.7206281129052,4.63059369203667,-235.350049999964));
#214103=CARTESIAN_POINT('Ctrl Pts',(47.8802911702592,4.60324650202951,-235.35005));
#214104=CARTESIAN_POINT('Ctrl Pts',(49.2373009570426,3.47966794651993,-234.663512775955));
#214105=CARTESIAN_POINT('Ctrl Pts',(48.7965371406365,3.43220404512792,-235.350050000019));
#214106=CARTESIAN_POINT('Ctrl Pts',(47.9840461137012,3.34200714134957,-235.35005));
#214107=CARTESIAN_POINT('Ctrl Pts',(49.2797408095797,3.09195832251735,-234.67177735372));
#214108=CARTESIAN_POINT('Ctrl Pts',(48.8394590156831,3.03198770182503,-235.350050000024));
#214109=CARTESIAN_POINT('Ctrl Pts',(48.0360840389224,2.92068200690756,-235.35005));
#214110=CARTESIAN_POINT('Ctrl Pts',(49.3686674721625,2.51417204308171,-234.682003885727));
#214111=CARTESIAN_POINT('Ctrl Pts',(48.9303472051771,2.43544747989523,-235.350049999988));
#214112=CARTESIAN_POINT('Ctrl Pts',(48.1401430583213,2.2930545562818,-235.35005));
#214113=CARTESIAN_POINT('Ctrl Pts',(49.402536303351,2.3219777357236,-234.685058224348));
#214114=CARTESIAN_POINT('Ctrl Pts',(48.9650330207291,2.23711886664551,-235.350050000003));
#214115=CARTESIAN_POINT('Ctrl Pts',(48.1791846215008,2.08432209117866,-235.35005));
#214116=CARTESIAN_POINT('Ctrl Pts',(49.4454504350533,2.10627534599544,-234.688106940244));
#214117=CARTESIAN_POINT('Ctrl Pts',(49.0090909802763,2.01443249512216,-235.35005));
#214118=CARTESIAN_POINT('Ctrl Pts',(48.228072252525,1.85004158947422,-235.35005));
#214119=CARTESIAN_POINT('Ctrl Pts',(49.4500656799736,2.08312047683055,-234.688585004576));
#214120=CARTESIAN_POINT('Ctrl Pts',(49.0138826721794,1.99021267182542,-235.35005));
#214121=CARTESIAN_POINT('Ctrl Pts',(48.2336222089945,1.8240233376047,-235.35005));
#214122=CARTESIAN_POINT('Ctrl Pts',(49.4627554357834,2.02616414735994,-234.687594881843));
#214123=CARTESIAN_POINT('Ctrl Pts',(49.0262880889212,1.93508456875412,-235.35005));
#214124=CARTESIAN_POINT('Ctrl Pts',(48.2445959867496,1.77197302819215,-235.35005));
#214125=CARTESIAN_POINT('Ctrl Pts',(49.4690104939933,1.99767348243289,-234.687098899761));
#214126=CARTESIAN_POINT('Ctrl Pts',(49.0324043256687,1.90750833138808,-235.350049999998));
#214127=CARTESIAN_POINT('Ctrl Pts',(48.2500003143967,1.7459388370457,-235.35005));
#214128=CARTESIAN_POINT('Ctrl Pts',(49.4875062569173,1.91216482959672,-234.68560826925));
#214129=CARTESIAN_POINT('Ctrl Pts',(49.0504957719995,1.82473476843569,-235.350050000004));
#214130=CARTESIAN_POINT('Ctrl Pts',(48.2659659469638,1.66780919078281,-235.35005));
#214131=CARTESIAN_POINT('Ctrl Pts',(49.4994778206697,1.85510901473098,-234.684610917049));
#214132=CARTESIAN_POINT('Ctrl Pts',(49.0622098134495,1.76950945951608,-235.350049999996));
#214133=CARTESIAN_POINT('Ctrl Pts',(48.2762799057323,1.61568666327167,-235.35005));
#214134=CARTESIAN_POINT('Ctrl Pts',(49.5343162437143,1.68379702048753,-234.681608641634));
#214135=CARTESIAN_POINT('Ctrl Pts',(49.0963241847283,1.60365506175308,-235.350050000008));
#214136=CARTESIAN_POINT('Ctrl Pts',(48.3062349042401,1.45921106566498,-235.35005));
#214137=CARTESIAN_POINT('Ctrl Pts',(49.5561079504651,1.56939161413912,-234.679593431468));
#214138=CARTESIAN_POINT('Ctrl Pts',(49.1176811340418,1.49291506667449,-235.35005));
#214139=CARTESIAN_POINT('Ctrl Pts',(48.3248891349689,1.35474998793845,-235.35005));
#214140=CARTESIAN_POINT('Ctrl Pts',(49.739315938348,0.538232976929953,-234.661348160278));
#214141=CARTESIAN_POINT('Ctrl Pts',(49.2980430840322,0.491601823769887,
-235.35005));
#214142=CARTESIAN_POINT('Ctrl Pts',(48.4809881192922,0.413309956198443,
-235.35005));
#214143=CARTESIAN_POINT('Ctrl Pts',(49.8115904444898,-0.39039417120445,
-234.644373027974));
#214144=CARTESIAN_POINT('Ctrl Pts',(49.3700829143943,-0.408162802666101,
-235.350050000012));
#214145=CARTESIAN_POINT('Ctrl Pts',(48.536801379512,-0.432603676106494,
-235.35005));
#214146=CARTESIAN_POINT('Ctrl Pts',(49.7792929465182,-1.80244463166521,
-234.617637729134));
#214147=CARTESIAN_POINT('Ctrl Pts',(49.3437540436927,-1.77379230904932,
-235.350049999994));
#214148=CARTESIAN_POINT('Ctrl Pts',(48.4927543039942,-1.71545839400357,
-235.35005));
#214149=CARTESIAN_POINT('Ctrl Pts',(49.7449472191672,-2.27243042723951,
-234.608607167038));
#214150=CARTESIAN_POINT('Ctrl Pts',(49.3121506898382,-2.22946376902224,
-235.350050000025));
#214151=CARTESIAN_POINT('Ctrl Pts',(48.4566916340738,-2.14207645769056,
-235.35005));
#214152=CARTESIAN_POINT('Ctrl Pts',(49.6724929766268,-2.85744653353658,
-234.597143764557));
#214153=CARTESIAN_POINT('Ctrl Pts',(49.2444209800414,-2.79595881961922,
-235.350049999994));
#214154=CARTESIAN_POINT('Ctrl Pts',(48.3849699272127,-2.67235166449409,
-235.35005));
#214155=CARTESIAN_POINT('Ctrl Pts',(49.6565229498012,-2.97433640738121,
-234.594843523884));
#214156=CARTESIAN_POINT('Ctrl Pts',(49.2294260564386,-2.90934026363395,
-235.350050000001));
#214157=CARTESIAN_POINT('Ctrl Pts',(48.3692885871419,-2.77828474965782,
-235.35005));
#214158=CARTESIAN_POINT('Ctrl Pts',(49.6303369251514,-3.14951121338623,
-234.59138274778));
#214159=CARTESIAN_POINT('Ctrl Pts',(49.2047903648279,-3.0792350757591,-235.350049999999));
#214160=CARTESIAN_POINT('Ctrl Pts',(48.3437536505604,-2.93700076554913,
-235.35005));
#214161=CARTESIAN_POINT('Ctrl Pts',(49.6212366617497,-3.2078747034095,-234.59022744472));
#214162=CARTESIAN_POINT('Ctrl Pts',(49.1962176139895,-3.13585840403236,
-235.350049999997));
#214163=CARTESIAN_POINT('Ctrl Pts',(48.3349064994216,-2.98987550056776,
-235.35005));
#214164=CARTESIAN_POINT('Ctrl Pts',(49.6093954409355,-3.28079495618834,
-234.588781243175));
#214165=CARTESIAN_POINT('Ctrl Pts',(49.1850545500923,-3.20659554539805,
-235.350050000001));
#214166=CARTESIAN_POINT('Ctrl Pts',(48.3234272698566,-3.05593058196302,
-235.35005));
#214167=CARTESIAN_POINT('Ctrl Pts',(49.6070039394402,-3.29537707660664,
-234.588491903602));
#214168=CARTESIAN_POINT('Ctrl Pts',(49.1827990425974,-3.22074419373563,
-235.350049999999));
#214169=CARTESIAN_POINT('Ctrl Pts',(48.3211104090697,-3.06913968133917,
-235.35005));
#214170=CARTESIAN_POINT('Ctrl Pts',(49.6021743356584,-3.32453778941096,
-234.587913021195));
#214171=CARTESIAN_POINT('Ctrl Pts',(49.1782430572807,-3.24903860274526,
-235.350050000001));
#214172=CARTESIAN_POINT('Ctrl Pts',(48.3164346335911,-3.09555404408755,
-235.35005));
#214173=CARTESIAN_POINT('Ctrl Pts',(49.5996474515442,-3.34085732030391,
-234.587220155499));
#214174=CARTESIAN_POINT('Ctrl Pts',(49.1760365449187,-3.26437756035475,
-235.350049999999));
#214175=CARTESIAN_POINT('Ctrl Pts',(48.3140690695237,-3.10875870092911,
-235.35005));
#214176=CARTESIAN_POINT('Ctrl Pts',(49.5926419005652,-3.37705346105833,
-234.588096930775));
#214177=CARTESIAN_POINT('Ctrl Pts',(49.1686572417052,-3.30163648990395,
-235.350050000002));
#214178=CARTESIAN_POINT('Ctrl Pts',(48.3069527703726,-3.14837088297125,
-235.35005));
#214179=CARTESIAN_POINT('Ctrl Pts',(49.5880379342478,-3.40119213175464,
-234.588675003203));
#214180=CARTESIAN_POINT('Ctrl Pts',(49.1638073722724,-3.32648654991977,
-235.350050000001));
#214181=CARTESIAN_POINT('Ctrl Pts',(48.3022780138372,-3.17478533866626,
-235.35005));
#214182=CARTESIAN_POINT('Ctrl Pts',(49.5471968352223,-3.61852378247012,
-234.593820523271));
#214183=CARTESIAN_POINT('Ctrl Pts',(49.120825236928,-3.55002422886253,-235.350049999991));
#214184=CARTESIAN_POINT('Ctrl Pts',(48.260829396598,-3.41257237641022,-235.35005));
#214185=CARTESIAN_POINT('Ctrl Pts',(49.5151390838467,-3.81220065571331,
-234.597986435595));
#214186=CARTESIAN_POINT('Ctrl Pts',(49.0870435716996,-3.7495062197225,-235.350049999982));
#214187=CARTESIAN_POINT('Ctrl Pts',(48.2284220495721,-3.6243432560285,-235.35005));
#214188=CARTESIAN_POINT('Ctrl Pts',(49.4316520932394,-4.39464147120427,
-234.609338953161));
#214189=CARTESIAN_POINT('Ctrl Pts',(48.999140659104,-4.34892292208159,-235.350050000037));
#214190=CARTESIAN_POINT('Ctrl Pts',(48.144430583747,-4.26086274000263,-235.35005));
#214191=CARTESIAN_POINT('Ctrl Pts',(49.3929212943256,-4.78464839371361,
-234.615391792126));
#214192=CARTESIAN_POINT('Ctrl Pts',(48.9581797211666,-4.75113501141927,
-235.350050000025));
#214193=CARTESIAN_POINT('Ctrl Pts',(48.1060703916391,-4.68681758304716,
-235.35005));
#214194=CARTESIAN_POINT('Ctrl Pts',(49.3496141347373,-5.56823512928163,
-234.624590481152));
#214195=CARTESIAN_POINT('Ctrl Pts',(48.9121267106381,-5.55882828684355,
-235.350049999975));
#214196=CARTESIAN_POINT('Ctrl Pts',(48.0648194622892,-5.541962664716,-235.35005));
#214197=CARTESIAN_POINT('Ctrl Pts',(49.3450624937163,-5.96264728287436,
-234.62775835361));
#214198=CARTESIAN_POINT('Ctrl Pts',(48.9069479295888,-5.96574880666937,
-235.350049999988));
#214199=CARTESIAN_POINT('Ctrl Pts',(48.0619566741598,-5.9722387873912,-235.35005));
#214200=CARTESIAN_POINT('Ctrl Pts',(49.3836522966543,-7.14335361784636,
-234.632954449768));
#214201=CARTESIAN_POINT('Ctrl Pts',(48.9459771364325,-7.18265905055676,
-235.350050000025));
#214202=CARTESIAN_POINT('Ctrl Pts',(48.10749380005,-7.25998633045287,-235.35005));
#214203=CARTESIAN_POINT('Ctrl Pts',(49.4781295444162,-7.92288565097549,
-234.630793193489));
#214204=CARTESIAN_POINT('Ctrl Pts',(49.0440042562222,-7.98854641142163,
-235.350050000012));
#214205=CARTESIAN_POINT('Ctrl Pts',(48.2090347928457,-8.11012177193449,
-235.35005));
#214206=CARTESIAN_POINT('Ctrl Pts',(49.6436637931067,-8.70555907873261,
-234.622711430443));
#214207=CARTESIAN_POINT('Ctrl Pts',(49.215549750052,-8.79378133618202,-235.35005));
#214208=CARTESIAN_POINT('Ctrl Pts',(48.3844338019353,-8.96504977313631,
-235.35005));
#214209=CARTESIAN_POINT('Ctrl Pts',(49.6467830757905,-8.72126520645183,
-234.622881194422));
#214210=CARTESIAN_POINT('Ctrl Pts',(49.2184641679714,-8.80863139937438,
-235.350050000001));
#214211=CARTESIAN_POINT('Ctrl Pts',(48.3871335037843,-8.97820236411209,
-235.35005));
#214212=CARTESIAN_POINT('Ctrl Pts',(49.652570743989,-8.75022091862852,-234.623023249691));
#214213=CARTESIAN_POINT('Ctrl Pts',(49.2240471314743,-8.83669877294023,
-235.35005));
#214214=CARTESIAN_POINT('Ctrl Pts',(48.392472005857,-9.00451470107218,-235.35005));
#214215=CARTESIAN_POINT('Ctrl Pts',(49.6554415168799,-8.76470121725064,
-234.623094268857));
#214216=CARTESIAN_POINT('Ctrl Pts',(49.2268162733382,-8.85073482443769,
-235.35005));
#214217=CARTESIAN_POINT('Ctrl Pts',(48.3951203393894,-9.01767332704875,
-235.35005));
#214218=CARTESIAN_POINT('Ctrl Pts',(49.6639847413244,-8.80814953817889,
-234.623307303822));
#214219=CARTESIAN_POINT('Ctrl Pts',(49.2350566242746,-8.89284947000431,
-235.35005));
#214220=CARTESIAN_POINT('Ctrl Pts',(48.4030026471238,-9.05715657045287,
-235.35005));
#214221=CARTESIAN_POINT('Ctrl Pts',(49.6695880826123,-8.83712489848571,
-234.62344929667));
#214222=CARTESIAN_POINT('Ctrl Pts',(49.2404610175429,-8.9209358282925,-235.350049999998));
#214223=CARTESIAN_POINT('Ctrl Pts',(48.4081739296747,-9.08348855318983,
-235.35005));
#214224=CARTESIAN_POINT('Ctrl Pts',(49.6861223185908,-8.92408111445968,
-234.623875207675));
#214225=CARTESIAN_POINT('Ctrl Pts',(49.256406444972,-9.00522113980889,-235.350050000003));
#214226=CARTESIAN_POINT('Ctrl Pts',(48.4234374397461,-9.16251391233196,
-235.35005));
#214227=CARTESIAN_POINT('Ctrl Pts',(49.6967773806612,-8.98209175593384,
-234.62415905619));
#214228=CARTESIAN_POINT('Ctrl Pts',(49.2666807798315,-9.06145141914929,
-235.350050000001));
#214229=CARTESIAN_POINT('Ctrl Pts',(48.4332793497998,-9.21523669725127,
-235.35005));
#214230=CARTESIAN_POINT('Ctrl Pts',(49.7276432253153,-9.15624775774307,
-234.625010528257));
#214231=CARTESIAN_POINT('Ctrl Pts',(49.2964363024444,-9.23024944441461,
-235.350049999999));
#214232=CARTESIAN_POINT('Ctrl Pts',(48.4618064955616,-9.37352237066705,
-235.35005));
#214233=CARTESIAN_POINT('Ctrl Pts',(49.7467547873477,-9.27251577845205,
-234.625578064603));
#214234=CARTESIAN_POINT('Ctrl Pts',(49.314854493951,-9.34294468497894,-235.350049999993));
#214235=CARTESIAN_POINT('Ctrl Pts',(48.4794934628256,-9.47920254067735,
-235.35005));
#214236=CARTESIAN_POINT('Ctrl Pts',(49.7997084497685,-9.62184541811456,
-234.627282202282));
#214237=CARTESIAN_POINT('Ctrl Pts',(49.3658541559959,-9.68147807603859,
-235.350050000013));
#214238=CARTESIAN_POINT('Ctrl Pts',(48.5285710814135,-9.79671102654565,
-235.35005));
#214239=CARTESIAN_POINT('Ctrl Pts',(49.8291648925442,-9.85534471123291,
-234.628414215299));
#214240=CARTESIAN_POINT('Ctrl Pts',(49.3941985373055,-9.90779071015971,
-235.350049999984));
#214241=CARTESIAN_POINT('Ctrl Pts',(48.5559827004535,-10.0090068188063,
-235.35005));
#214242=CARTESIAN_POINT('Ctrl Pts',(49.9000611961947,-10.5579169022257,
-234.631809953743));
#214243=CARTESIAN_POINT('Ctrl Pts',(49.46227163692,-10.5884986518548,-235.350050000031));
#214244=CARTESIAN_POINT('Ctrl Pts',(48.6223270802844,-10.6477610876399,
-235.35005));
#214245=CARTESIAN_POINT('Ctrl Pts',(49.9239345979392,-11.0302498028062,
-234.634065686046));
#214246=CARTESIAN_POINT('Ctrl Pts',(49.4850280286859,-11.0462297011433,
-235.350050000012));
#214247=CARTESIAN_POINT('Ctrl Pts',(48.6453046118701,-11.0773736644593,
-235.35005));
#214248=CARTESIAN_POINT('Ctrl Pts',(49.9251475272435,-12.4365683292309,
-234.640718339231));
#214249=CARTESIAN_POINT('Ctrl Pts',(49.4850454762624,-12.4082162297068,
-235.350049999975));
#214250=CARTESIAN_POINT('Ctrl Pts',(48.6501328458788,-12.3566962654659,
-235.35005));
#214251=CARTESIAN_POINT('Ctrl Pts',(49.8337365726491,-13.3641675740085,
-234.645001156777));
#214252=CARTESIAN_POINT('Ctrl Pts',(49.3959235241511,-13.306961117108,-235.350050000025));
#214253=CARTESIAN_POINT('Ctrl Pts',(48.5694097707421,-13.2010981453996,
-235.35005));
#214254=CARTESIAN_POINT('Ctrl Pts',(49.6449074151748,-14.31060701528,-234.649307954722));
#214255=CARTESIAN_POINT('Ctrl Pts',(49.2121335792871,-14.2245954491116,
-235.35005));
#214256=CARTESIAN_POINT('Ctrl Pts',(48.3999288819756,-14.0631760578291,
-235.35005));
#214257=CARTESIAN_POINT('Ctrl Pts',(49.6390944562837,-14.3392793335432,
-234.649438390436));
#214258=CARTESIAN_POINT('Ctrl Pts',(49.2064813038673,-14.2523696378793,
-235.350050000001));
#214259=CARTESIAN_POINT('Ctrl Pts',(48.3947106332052,-14.089291300339,-235.35005));
#214260=CARTESIAN_POINT('Ctrl Pts',(49.630238868934,-14.3822740481529,-234.649633936839));
#214261=CARTESIAN_POINT('Ctrl Pts',(49.1978709982769,-14.2940177686488,
-235.35005));
#214262=CARTESIAN_POINT('Ctrl Pts',(48.3867592982998,-14.1284516414382,
-235.35005));
#214263=CARTESIAN_POINT('Ctrl Pts',(49.6270184598194,-14.3976658139417,
-234.64972527904));
#214264=CARTESIAN_POINT('Ctrl Pts',(49.1948058416811,-14.3085889178777,
-235.35005));
#214265=CARTESIAN_POINT('Ctrl Pts',(48.3840780941576,-14.1415019811602,
-235.35005));
#214266=CARTESIAN_POINT('Ctrl Pts',(49.6220964416629,-14.4216069388598,
-234.649740099044));
#214267=CARTESIAN_POINT('Ctrl Pts',(49.189727776354,-14.3332801597934,-235.35005));
#214268=CARTESIAN_POINT('Ctrl Pts',(48.3787223515611,-14.1676033339819,
-235.35005));
#214269=CARTESIAN_POINT('Ctrl Pts',(49.6196521598081,-14.4335794112836,
-234.649746149776));
#214270=CARTESIAN_POINT('Ctrl Pts',(49.1872061637321,-14.3456277485269,
-235.350050000002));
#214271=CARTESIAN_POINT('Ctrl Pts',(48.3760618298762,-14.1806557630565,
-235.35005));
#214272=CARTESIAN_POINT('Ctrl Pts',(49.607514313622,-14.4934512680602,-234.649769617566));
#214273=CARTESIAN_POINT('Ctrl Pts',(49.1746851770632,-14.4073752083641,
-235.350049999995));
#214274=CARTESIAN_POINT('Ctrl Pts',(48.3628458825965,-14.2459266629983,
-235.35005));
#214275=CARTESIAN_POINT('Ctrl Pts',(49.5980714456629,-14.5413790514639,
-234.649766679825));
#214276=CARTESIAN_POINT('Ctrl Pts',(49.1649467606461,-14.4568049215079,
-235.35005));
#214277=CARTESIAN_POINT('Ctrl Pts',(48.3525504293568,-14.2981713963959,
-235.35005));
#214278=CARTESIAN_POINT('Ctrl Pts',(49.5705425974965,-14.685250739817,-234.64969306114));
#214279=CARTESIAN_POINT('Ctrl Pts',(49.1365644714732,-14.6051843071834,
-235.35005));
#214280=CARTESIAN_POINT('Ctrl Pts',(48.3224929218234,-14.4549893276864,
-235.35005));
#214281=CARTESIAN_POINT('Ctrl Pts',(49.5532562934944,-14.7812827163161,
-234.6495576116));
#214282=CARTESIAN_POINT('Ctrl Pts',(49.1187527743078,-14.7042280745193,
-235.350049999998));
#214283=CARTESIAN_POINT('Ctrl Pts',(48.3035595793916,-14.5596462424765,
-235.35005));
#214284=CARTESIAN_POINT('Ctrl Pts',(49.504581004737,-15.0697105777159,-234.648893466985));
#214285=CARTESIAN_POINT('Ctrl Pts',(49.0686321333853,-15.0017055627095,
-235.350050000003));
#214286=CARTESIAN_POINT('Ctrl Pts',(48.2500551817889,-14.8739499130376,
-235.35005));
#214287=CARTESIAN_POINT('Ctrl Pts',(49.4763738065104,-15.2624371474016,
-234.648107556722));
#214288=CARTESIAN_POINT('Ctrl Pts',(49.0396350389957,-15.2005009431667,
-235.350049999997));
#214289=CARTESIAN_POINT('Ctrl Pts',(48.2187775910813,-15.0839293763448,
-235.35005));
#214290=CARTESIAN_POINT('Ctrl Pts',(49.4044293239341,-15.8417822433236,
-234.644710178708));
#214291=CARTESIAN_POINT('Ctrl Pts',(48.9658409312175,-15.7981630905825,
-235.350050000006));
#214292=CARTESIAN_POINT('Ctrl Pts',(48.1380456036249,-15.7151912142403,
-235.35005));
#214293=CARTESIAN_POINT('Ctrl Pts',(49.3734327825549,-16.2296028510151,
-234.641058717396));
#214294=CARTESIAN_POINT('Ctrl Pts',(48.9343435468517,-16.1983923951185,
-235.350049999994));
#214295=CARTESIAN_POINT('Ctrl Pts',(48.1017687499515,-16.1377801895033,
-235.35005));
#214296=CARTESIAN_POINT('Ctrl Pts',(49.3308420035029,-17.3903901931505,
-234.625952625488));
#214297=CARTESIAN_POINT('Ctrl Pts',(48.8924366678536,-17.3966762449269,
-235.350050000012));
#214298=CARTESIAN_POINT('Ctrl Pts',(48.0452056587669,-17.4030250963116,
-235.35005));
#214299=CARTESIAN_POINT('Ctrl Pts',(49.3691048094434,-18.1627182776333,
-234.610348160686));
#214300=CARTESIAN_POINT('Ctrl Pts',(48.9347737531675,-18.1950555866989,
-235.350049999926));
#214301=CARTESIAN_POINT('Ctrl Pts',(48.0765553834797,-18.2457723122435,
-235.35005));
#214302=CARTESIAN_POINT('Ctrl Pts',(49.4996796913378,-19.1255806819443,
-234.582794859548));
#214303=CARTESIAN_POINT('Ctrl Pts',(49.073878318193,-19.1825305851387,-235.350050000018));
#214304=CARTESIAN_POINT('Ctrl Pts',(48.202136382695,-19.2982688285888,-235.35005));
#214305=CARTESIAN_POINT('Ctrl Pts',(49.52991658873,-19.3178023825667,-234.576884907736));
#214306=CARTESIAN_POINT('Ctrl Pts',(49.1061840742319,-19.3803813622115,
-235.350049999994));
#214307=CARTESIAN_POINT('Ctrl Pts',(48.2315724527526,-19.5085474359625,
-235.35005));
#214308=CARTESIAN_POINT('Ctrl Pts',(49.5728750024147,-19.557581971237,-234.568958963022));
#214309=CARTESIAN_POINT('Ctrl Pts',(49.1519829044983,-19.6267561009081,
-235.350050000002));
#214310=CARTESIAN_POINT('Ctrl Pts',(48.2737849902378,-19.7710257016811,
-235.35005));
#214311=CARTESIAN_POINT('Ctrl Pts',(49.581724296076,-19.6055101274536,-234.567346909248));
#214312=CARTESIAN_POINT('Ctrl Pts',(49.1614271182939,-19.6760521531559,
-235.350049999999));
#214313=CARTESIAN_POINT('Ctrl Pts',(48.2824987027496,-19.82350433647,-235.35005));
#214314=CARTESIAN_POINT('Ctrl Pts',(49.5953862717011,-19.6773655259788,
-234.564887454911));
#214315=CARTESIAN_POINT('Ctrl Pts',(49.1760035146459,-19.749934845904,-235.35005));
#214316=CARTESIAN_POINT('Ctrl Pts',(48.2959770869867,-19.9021966978926,
-235.35005));
#214317=CARTESIAN_POINT('Ctrl Pts',(49.6000048505966,-19.7013107519912,
-234.564060755941));
#214318=CARTESIAN_POINT('Ctrl Pts',(49.1809320849687,-19.7745590177076,
-235.350050000005));
#214319=CARTESIAN_POINT('Ctrl Pts',(48.3005378529525,-19.9284232197851,
-235.35005));
#214320=CARTESIAN_POINT('Ctrl Pts',(49.6070298089383,-19.737219250395,-234.562810247899));
#214321=CARTESIAN_POINT('Ctrl Pts',(49.1884276543306,-19.8114797947251,
-235.350049999998));
#214322=CARTESIAN_POINT('Ctrl Pts',(48.3074811028276,-19.9677565956903,
-235.35005));
#214323=CARTESIAN_POINT('Ctrl Pts',(49.609387621656,-19.7491870845315,-234.56239167244));
#214324=CARTESIAN_POINT('Ctrl Pts',(49.1909436535833,-19.823785851781,-235.350050000001));
#214325=CARTESIAN_POINT('Ctrl Pts',(48.3098125363869,-19.9808666531709,
-235.35005));
#214326=CARTESIAN_POINT('Ctrl Pts',(49.6141356106853,-19.773119545442,-234.561551017751));
#214327=CARTESIAN_POINT('Ctrl Pts',(49.1960101574545,-19.8483939155015,
-235.350049999999));
#214328=CARTESIAN_POINT('Ctrl Pts',(48.3145094629338,-20.0070846308637,
-235.35005));
#214329=CARTESIAN_POINT('Ctrl Pts',(49.616496536379,-19.7880921888268,-234.562161061286));
#214330=CARTESIAN_POINT('Ctrl Pts',(49.1981273776604,-19.8628075510617,
-235.35005));
#214331=CARTESIAN_POINT('Ctrl Pts',(48.3168699427918,-20.0201928656617,
-235.35005));
#214332=CARTESIAN_POINT('Ctrl Pts',(49.6374531557859,-19.9187122192786,
-234.566228111255));
#214333=CARTESIAN_POINT('Ctrl Pts',(49.2174467664976,-19.9895567213893,
-235.350050000002));
#214334=CARTESIAN_POINT('Ctrl Pts',(48.3378149961279,-20.1381857579918,
-235.35005));
#214335=CARTESIAN_POINT('Ctrl Pts',(49.6545821021411,-20.034869144394,-234.569823849718));
#214336=CARTESIAN_POINT('Ctrl Pts',(49.233200304514,-20.1023267809174,-235.350049999994));
#214337=CARTESIAN_POINT('Ctrl Pts',(48.3550896009133,-20.2431526171789,
-235.35005));
#214338=CARTESIAN_POINT('Ctrl Pts',(49.732804356096,-20.6159835232779,-234.587701863422));
#214339=CARTESIAN_POINT('Ctrl Pts',(49.3046815018901,-20.6649638076766,
-235.350050000025));
#214340=CARTESIAN_POINT('Ctrl Pts',(48.4347895563001,-20.7684056538746,
-235.35005));
#214341=CARTESIAN_POINT('Ctrl Pts',(49.771626989824,-21.0814436674373,-234.601632242406));
#214342=CARTESIAN_POINT('Ctrl Pts',(49.3394667389117,-21.1164600076538,
-235.35005));
#214343=CARTESIAN_POINT('Ctrl Pts',(48.4772403630273,-21.1899452510999,
-235.35005));
#214344=CARTESIAN_POINT('Ctrl Pts',(49.8182862151745,-22.480135809816,-234.642440475715));
#214345=CARTESIAN_POINT('Ctrl Pts',(49.3766026048063,-22.4678952988485,
-235.35005));
#214346=CARTESIAN_POINT('Ctrl Pts',(48.5415386498259,-22.458520743411,-235.35005));
#214347=CARTESIAN_POINT('Ctrl Pts',(49.7563614221941,-23.4171717990893,
-234.66832058589));
#214348=CARTESIAN_POINT('Ctrl Pts',(49.3136320941011,-23.3756815703655,
-235.35005));
#214349=CARTESIAN_POINT('Ctrl Pts',(48.5005032094983,-23.311667738302,-235.35005));
#214350=CARTESIAN_POINT('Ctrl Pts',(49.5587507160758,-24.5837933660124,
-234.698831294804));
#214351=CARTESIAN_POINT('Ctrl Pts',(49.1180235882351,-24.5091016284394,
-235.35005));
#214352=CARTESIAN_POINT('Ctrl Pts',(48.3390590324706,-24.3778343529881,
-235.35005));
#214353=CARTESIAN_POINT('Ctrl Pts',(49.5131812962588,-24.8168855068945,
-234.704842968893));
#214354=CARTESIAN_POINT('Ctrl Pts',(49.0732932499469,-24.7346294445711,
-235.350050000019));
#214355=CARTESIAN_POINT('Ctrl Pts',(48.3012455308433,-24.5909867391319,
-235.35005));
#214356=CARTESIAN_POINT('Ctrl Pts',(49.4550136911697,-25.0787190925436,
-234.711486940524));
#214357=CARTESIAN_POINT('Ctrl Pts',(49.0162880925532,-24.9882356999008,
-235.350049999998));
#214358=CARTESIAN_POINT('Ctrl Pts',(48.2523434883265,-24.8306899717521,
-235.35005));
#214359=CARTESIAN_POINT('Ctrl Pts',(49.4484542084783,-25.1078085522158,
-234.712223559563));
#214360=CARTESIAN_POINT('Ctrl Pts',(49.0098690957564,-25.016379242205,-235.350049999997));
#214361=CARTESIAN_POINT('Ctrl Pts',(48.2468215385715,-24.857322369352,-235.35005));
#214362=CARTESIAN_POINT('Ctrl Pts',(49.4351429030966,-25.1659768335314,
-234.713693433566));
#214363=CARTESIAN_POINT('Ctrl Pts',(48.9968469574703,-25.0726559928153,
-235.350050000003));
#214364=CARTESIAN_POINT('Ctrl Pts',(48.2356002982336,-24.910584566504,-235.35005));
#214365=CARTESIAN_POINT('Ctrl Pts',(49.4304748324618,-25.1900623132835,
-234.713025011659));
#214366=CARTESIAN_POINT('Ctrl Pts',(48.9920207550766,-25.0977237288005,
-235.350049999999));
#214367=CARTESIAN_POINT('Ctrl Pts',(48.2299135975692,-24.9372145504824,
-235.35005));
#214368=CARTESIAN_POINT('Ctrl Pts',(49.4162334358612,-25.2638138055417,
-234.711416035933));
#214369=CARTESIAN_POINT('Ctrl Pts',(48.9774072970604,-25.1738353442622,
-235.350050000003));
#214370=CARTESIAN_POINT('Ctrl Pts',(48.2132345171348,-25.0171100844526,
-235.35005));
#214371=CARTESIAN_POINT('Ctrl Pts',(49.4070241632922,-25.3129840569633,
-234.710320691744));
#214372=CARTESIAN_POINT('Ctrl Pts',(48.9679636427474,-25.224572425112,-235.350049999999));
#214373=CARTESIAN_POINT('Ctrl Pts',(48.2024091551349,-25.0703780812323,
-235.35005));
#214374=CARTESIAN_POINT('Ctrl Pts',(49.3802457522676,-25.4604973397937,
-234.70696606232));
#214375=CARTESIAN_POINT('Ctrl Pts',(48.940513122283,-25.3768184010969,-235.350050000001));
#214376=CARTESIAN_POINT('Ctrl Pts',(48.1708085736138,-25.2301948978772,
-235.35005));
#214377=CARTESIAN_POINT('Ctrl Pts',(49.3635250310457,-25.5588470628881,
-234.704638120292));
#214378=CARTESIAN_POINT('Ctrl Pts',(48.9233997772468,-25.4782980756233,
-235.350050000001));
#214379=CARTESIAN_POINT('Ctrl Pts',(48.1509087141736,-25.3367565417747,
-235.35005));
#214380=CARTESIAN_POINT('Ctrl Pts',(49.2855135355185,-26.0505522453803,
-234.692532681863));
#214381=CARTESIAN_POINT('Ctrl Pts',(48.8435554437265,-25.9864180900749,
-235.350049999994));
#214382=CARTESIAN_POINT('Ctrl Pts',(48.0571667807649,-25.8696491072789,
-235.35005));
#214383=CARTESIAN_POINT('Ctrl Pts',(49.24093071664,-26.443949521064,-234.681362278638));
#214384=CARTESIAN_POINT('Ctrl Pts',(48.7984910202732,-26.3925228008522,
-235.350049999982));
#214385=CARTESIAN_POINT('Ctrl Pts',(48.000556289185,-26.2962324730956,-235.35005));
#214386=CARTESIAN_POINT('Ctrl Pts',(49.1586792195434,-27.62308861654,-234.642841042967));
#214387=CARTESIAN_POINT('Ctrl Pts',(48.7173180681133,-27.612103610794,-235.350050000037));
#214388=CARTESIAN_POINT('Ctrl Pts',(47.8838810362842,-27.5767613139966,
-235.35005));
#214389=CARTESIAN_POINT('Ctrl Pts',(49.1719516846433,-28.4084423968299,
-234.610732565613));
#214390=CARTESIAN_POINT('Ctrl Pts',(48.7364227605218,-28.4243954137753,
-235.350049999951));
#214391=CARTESIAN_POINT('Ctrl Pts',(47.876633025442,-28.431480559278,-235.35005));
#214392=CARTESIAN_POINT('Ctrl Pts',(49.329058348282,-29.9760690458421,-234.530187142121));
#214393=CARTESIAN_POINT('Ctrl Pts',(48.9147174357445,-30.0364945671442,
-235.35005000005));
#214394=CARTESIAN_POINT('Ctrl Pts',(47.9998818090224,-30.1429370236128,
-235.35005));
#214395=CARTESIAN_POINT('Ctrl Pts',(49.4727250783003,-30.7578511157521,
-234.481690588048));
#214396=CARTESIAN_POINT('Ctrl Pts',(49.077384122066,-30.8424286009874,-235.350050000038));
#214397=CARTESIAN_POINT('Ctrl Pts',(48.1303803611475,-30.9997028426405,
-235.35005));
#214398=CARTESIAN_POINT('Ctrl Pts',(49.6820070592694,-31.5392028235171,
-234.422833933791));
#214399=CARTESIAN_POINT('Ctrl Pts',(49.3091456199776,-31.6271496259376,
-235.35005));
#214400=CARTESIAN_POINT('Ctrl Pts',(48.3327003568643,-31.8574637039839,
-235.35005));
#214401=CARTESIAN_POINT('',(49.658099715389,-31.5448418470982,-234.479004887568));
#214402=CARTESIAN_POINT('',(48.3327003568643,-31.8574637039841,-235.35005));
#214403=CARTESIAN_POINT('Origin',(48.3327003568642,-31.8574637039841,-233.85005));
#214404=CARTESIAN_POINT('Ctrl Pts',(48.3395182384274,8.75410525715256,-235.35005));
#214405=CARTESIAN_POINT('Ctrl Pts',(48.1420743191374,7.93092102614352,-235.35005));
#214406=CARTESIAN_POINT('Ctrl Pts',(48.0110562569534,7.1033413541692,-235.35005));
#214407=CARTESIAN_POINT('Ctrl Pts',(47.9456204841389,6.27142206048251,-235.35005));
#214408=CARTESIAN_POINT('Ctrl Pts',(47.8801847113245,5.43950276679582,-235.35005));
#214409=CARTESIAN_POINT('Ctrl Pts',(47.8802911706055,4.60324650205529,-235.35005));
#214410=CARTESIAN_POINT('Ctrl Pts',(47.9494611326687,3.76242026158568,-235.35005));
#214411=CARTESIAN_POINT('Ctrl Pts',(47.9840461137003,3.34200714135088,-235.35005));
#214412=CARTESIAN_POINT('Ctrl Pts',(48.0360840389923,2.92068200696516,-235.35005));
#214413=CARTESIAN_POINT('Ctrl Pts',(48.1054567185474,2.50226370649453,-235.35005));
#214414=CARTESIAN_POINT('Ctrl Pts',(48.140143058325,2.29305455625922,-235.35005));
#214415=CARTESIAN_POINT('Ctrl Pts',(48.1791846215669,2.08432209117834,-235.35005));
#214416=CARTESIAN_POINT('Ctrl Pts',(48.222640293554,1.87607275633673,-235.35005));
#214417=CARTESIAN_POINT('Ctrl Pts',(48.2280722525526,1.85004158948043,-235.35005));
#214418=CARTESIAN_POINT('Ctrl Pts',(48.2336222090191,1.82402333761035,-235.35005));
#214419=CARTESIAN_POINT('Ctrl Pts',(48.2391090978947,1.79799818290319,-235.35005));
#214420=CARTESIAN_POINT('Ctrl Pts',(48.2445959867701,1.77197302819679,-235.35005));
#214421=CARTESIAN_POINT('Ctrl Pts',(48.2500003144159,1.74593883705,-235.35005));
#214422=CARTESIAN_POINT('Ctrl Pts',(48.2553221919377,1.71989562162854,-235.35005));
#214423=CARTESIAN_POINT('Ctrl Pts',(48.265965946981,1.66780919078707,-235.35005));
#214424=CARTESIAN_POINT('Ctrl Pts',(48.2762799057506,1.61568666327577,-235.35005));
#214425=CARTESIAN_POINT('Ctrl Pts',(48.2862649052553,1.56352813074,-235.35005));
#214426=CARTESIAN_POINT('Ctrl Pts',(48.3062349042647,1.45921106566754,-235.35005));
#214427=CARTESIAN_POINT('Ctrl Pts',(48.3248891350009,1.35474998793937,-235.35005));
#214428=CARTESIAN_POINT('Ctrl Pts',(48.3422334665882,1.25014553997188,-235.35005));
#214429=CARTESIAN_POINT('Ctrl Pts',(48.4809881192878,0.41330995622679,-235.35005));
#214430=CARTESIAN_POINT('Ctrl Pts',(48.5368013795039,-0.432603676297867,
-235.35005));
#214431=CARTESIAN_POINT('Ctrl Pts',(48.5074366626247,-1.28784015470909,
-235.35005));
#214432=CARTESIAN_POINT('Ctrl Pts',(48.492754304185,-1.7154583939147,-235.35005));
#214433=CARTESIAN_POINT('Ctrl Pts',(48.4566916340691,-2.14207645772467,
-235.35005));
#214434=CARTESIAN_POINT('Ctrl Pts',(48.3993142685993,-2.56629662313498,
-235.35005));
#214435=CARTESIAN_POINT('Ctrl Pts',(48.3849699272317,-2.67235166448867,
-235.35005));
#214436=CARTESIAN_POINT('Ctrl Pts',(48.369288587157,-2.77828474965553,-235.35005));
#214437=CARTESIAN_POINT('Ctrl Pts',(48.3522652960998,-2.88409542692065,
-235.35005));
#214438=CARTESIAN_POINT('Ctrl Pts',(48.3437536505715,-2.93700076555112,
-235.35005));
#214439=CARTESIAN_POINT('Ctrl Pts',(48.3349064994319,-2.98987550057008,
-235.35005));
#214440=CARTESIAN_POINT('Ctrl Pts',(48.3257231157807,-3.04271956568589,
-235.35005));
#214441=CARTESIAN_POINT('Ctrl Pts',(48.3234272698678,-3.05593058196506,
-235.35005));
#214442=CARTESIAN_POINT('Ctrl Pts',(48.3211104090812,-3.06913968134127,
-235.35005));
#214443=CARTESIAN_POINT('Ctrl Pts',(48.3187725213423,-3.08234686271546,
-235.35005));
#214444=CARTESIAN_POINT('Ctrl Pts',(48.3164346336033,-3.09555404408982,
-235.35005));
#214445=CARTESIAN_POINT('Ctrl Pts',(48.3140690695364,-3.1087587009315,-235.35005));
#214446=CARTESIAN_POINT('Ctrl Pts',(48.31169696982,-3.12196276161221,-235.35005));
#214447=CARTESIAN_POINT('Ctrl Pts',(48.306952770387,-3.14837088297426,-235.35005));
#214448=CARTESIAN_POINT('Ctrl Pts',(48.3022780138533,-3.17478533866958,
-235.35005));
#214449=CARTESIAN_POINT('Ctrl Pts',(48.2976726119403,-3.20120612064097,
-235.35005));
#214450=CARTESIAN_POINT('Ctrl Pts',(48.2608293966366,-3.41257237640728,
-235.35005));
#214451=CARTESIAN_POINT('Ctrl Pts',(48.2284220495736,-3.62434325601736,
-235.35005));
#214452=CARTESIAN_POINT('Ctrl Pts',(48.2004248943047,-3.8365164173544,-235.35005));
#214453=CARTESIAN_POINT('Ctrl Pts',(48.144430583767,-4.2608627400285,-235.35005));
#214454=CARTESIAN_POINT('Ctrl Pts',(48.1060703916864,-4.6868175831452,-235.35005));
#214455=CARTESIAN_POINT('Ctrl Pts',(48.0854449269901,-5.11439012388267,
-235.35005));
#214456=CARTESIAN_POINT('Ctrl Pts',(48.0648194622937,-5.54196266462014,
-235.35005));
#214457=CARTESIAN_POINT('Ctrl Pts',(48.0619566741596,-5.97223878738515,
-235.35005));
#214458=CARTESIAN_POINT('Ctrl Pts',(48.0771357161752,-6.40148796840999,
-235.35005));
#214459=CARTESIAN_POINT('Ctrl Pts',(48.1074938002064,-7.25998633045966,
-235.35005));
#214460=CARTESIAN_POINT('Ctrl Pts',(48.2090347930406,-8.11012177188801,
-235.35005));
#214461=CARTESIAN_POINT('Ctrl Pts',(48.3817353557071,-8.95189703464271,
-235.35005));
#214462=CARTESIAN_POINT('Ctrl Pts',(48.3844338019987,-8.96504977312313,
-235.35005));
#214463=CARTESIAN_POINT('Ctrl Pts',(48.3871335038458,-8.97820236409949,
-235.35005));
#214464=CARTESIAN_POINT('Ctrl Pts',(48.3898027548802,-8.99135853258005,
-235.35005));
#214465=CARTESIAN_POINT('Ctrl Pts',(48.3924720059147,-9.00451470106053,
-235.35005));
#214466=CARTESIAN_POINT('Ctrl Pts',(48.3951203394452,-9.01767332703754,
-235.35005));
#214467=CARTESIAN_POINT('Ctrl Pts',(48.3977477753549,-9.03083440817268,
-235.35005));
#214468=CARTESIAN_POINT('Ctrl Pts',(48.4030026471742,-9.05715657044287,
-235.35005));
#214469=CARTESIAN_POINT('Ctrl Pts',(48.4081739297218,-9.08348855318059,
-235.35005));
#214470=CARTESIAN_POINT('Ctrl Pts',(48.4132617664092,-9.10983033956203,
-235.35005));
#214471=CARTESIAN_POINT('Ctrl Pts',(48.4234374397839,-9.16251391232474,
-235.35005));
#214472=CARTESIAN_POINT('Ctrl Pts',(48.4332793498323,-9.21523669724522,
-235.35005));
#214473=CARTESIAN_POINT('Ctrl Pts',(48.4427883984152,-9.2679985883848,-235.35005));
#214474=CARTESIAN_POINT('Ctrl Pts',(48.4618064955809,-9.37352237066414,
-235.35005));
#214475=CARTESIAN_POINT('Ctrl Pts',(48.4794934628395,-9.47920254067581,
-235.35005));
#214476=CARTESIAN_POINT('Ctrl Pts',(48.4958526690327,-9.58503870263171,
-235.35005));
#214477=CARTESIAN_POINT('Ctrl Pts',(48.5285710814205,-9.79671102655205,
-235.35005));
#214478=CARTESIAN_POINT('Ctrl Pts',(48.5559827004663,-10.0090068188147,
-235.35005));
#214479=CARTESIAN_POINT('Ctrl Pts',(48.5780974937539,-10.2219249084145,
-235.35005));
#214480=CARTESIAN_POINT('Ctrl Pts',(48.6223270803283,-10.6477610876057,
-235.35005));
#214481=CARTESIAN_POINT('Ctrl Pts',(48.6453046119738,-11.0773736644268,
-235.35005));
#214482=CARTESIAN_POINT('Ctrl Pts',(48.6469140232755,-11.5038145314612,
-235.35005));
#214483=CARTESIAN_POINT('Ctrl Pts',(48.6501328458788,-12.3566962655301,
-235.35005));
#214484=CARTESIAN_POINT('Ctrl Pts',(48.5694097707119,-13.201098145554,-235.35005));
#214485=CARTESIAN_POINT('Ctrl Pts',(48.4050646665376,-14.0370524847357,
-235.35005));
#214486=CARTESIAN_POINT('Ctrl Pts',(48.3999288820313,-14.0631760578391,
-235.35005));
#214487=CARTESIAN_POINT('Ctrl Pts',(48.3947106332613,-14.0892913003493,
-235.35005));
#214488=CARTESIAN_POINT('Ctrl Pts',(48.3894097433236,-14.1153981944164,
-235.35005));
#214489=CARTESIAN_POINT('Ctrl Pts',(48.3867592983549,-14.1284516414493,
-235.35005));
#214490=CARTESIAN_POINT('Ctrl Pts',(48.3840780942122,-14.1415019811713,
-235.35005));
#214491=CARTESIAN_POINT('Ctrl Pts',(48.3814002229133,-14.1545526575822,
-235.35005));
#214492=CARTESIAN_POINT('Ctrl Pts',(48.3787223516144,-14.1676033339926,
-235.35005));
#214493=CARTESIAN_POINT('Ctrl Pts',(48.3760618299286,-14.1806557630669,
-235.35005));
#214494=CARTESIAN_POINT('Ctrl Pts',(48.3734186404716,-14.1937099430552,
-235.35005));
#214495=CARTESIAN_POINT('Ctrl Pts',(48.3628458826442,-14.2459266630052,
-235.35005));
#214496=CARTESIAN_POINT('Ctrl Pts',(48.3525504293979,-14.2981713964018,
-235.35005));
#214497=CARTESIAN_POINT('Ctrl Pts',(48.3425312602132,-14.350444040166,-235.35005));
#214498=CARTESIAN_POINT('Ctrl Pts',(48.3224929218452,-14.4549893276876,
-235.35005));
#214499=CARTESIAN_POINT('Ctrl Pts',(48.3035595794002,-14.5596462424789,
-235.35005));
#214500=CARTESIAN_POINT('Ctrl Pts',(48.2857247802083,-14.6644141326663,
-235.35005));
#214501=CARTESIAN_POINT('Ctrl Pts',(48.2500551818223,-14.8739499130538,
-235.35005));
#214502=CARTESIAN_POINT('Ctrl Pts',(48.2187775910825,-15.0839293763357,
-235.35005));
#214503=CARTESIAN_POINT('Ctrl Pts',(48.1918669286016,-15.2943499889772,
-235.35005));
#214504=CARTESIAN_POINT('Ctrl Pts',(48.13804560364,-15.71519121426,-235.35005));
#214505=CARTESIAN_POINT('Ctrl Pts',(48.1017687499494,-16.1377801895464,
-235.35005));
#214506=CARTESIAN_POINT('Ctrl Pts',(48.0829143862637,-16.5595284917746,
-235.35005));
#214507=CARTESIAN_POINT('Ctrl Pts',(48.0452056588921,-17.4030250962311,
-235.35005));
#214508=CARTESIAN_POINT('Ctrl Pts',(48.076555383577,-18.2457723122303,-235.35005));
#214509=CARTESIAN_POINT('Ctrl Pts',(48.1770201828715,-19.0877695253175,
-235.35005));
#214510=CARTESIAN_POINT('Ctrl Pts',(48.2021363826951,-19.2982688285893,
-235.35005));
#214511=CARTESIAN_POINT('Ctrl Pts',(48.2315724527786,-19.5085474359751,
-235.35005));
#214512=CARTESIAN_POINT('Ctrl Pts',(48.2653424827524,-19.7185300485352,
-235.35005));
#214513=CARTESIAN_POINT('Ctrl Pts',(48.2737849902462,-19.7710257016774,
-235.35005));
#214514=CARTESIAN_POINT('Ctrl Pts',(48.282498702759,-19.8235043364666,-235.35005));
#214515=CARTESIAN_POINT('Ctrl Pts',(48.2914842922534,-19.8759659107496,
-235.35005));
#214516=CARTESIAN_POINT('Ctrl Pts',(48.2959770870004,-19.9021966978899,
-235.35005));
#214517=CARTESIAN_POINT('Ctrl Pts',(48.300537852968,-19.9284232197822,-235.35005));
#214518=CARTESIAN_POINT('Ctrl Pts',(48.3051666862202,-19.9546454703855,
-235.35005));
#214519=CARTESIAN_POINT('Ctrl Pts',(48.3074811028462,-19.967756595687,-235.35005));
#214520=CARTESIAN_POINT('Ctrl Pts',(48.3098125364066,-19.9808666531674,
-235.35005));
#214521=CARTESIAN_POINT('Ctrl Pts',(48.3121609996811,-19.9939756420136,
-235.35005));
#214522=CARTESIAN_POINT('Ctrl Pts',(48.3145094629556,-20.0070846308597,
-235.35005));
#214523=CARTESIAN_POINT('Ctrl Pts',(48.3168699428148,-20.0201928656576,
-235.35005));
#214524=CARTESIAN_POINT('Ctrl Pts',(48.3191971709643,-20.0333031870275,
-235.35005));
#214525=CARTESIAN_POINT('Ctrl Pts',(48.337814996161,-20.1381857579874,-235.35005));
#214526=CARTESIAN_POINT('Ctrl Pts',(48.3550896009548,-20.2431526171762,
-235.35005));
#214527=CARTESIAN_POINT('Ctrl Pts',(48.3710295920234,-20.3482032245128,
-235.35005));
#214528=CARTESIAN_POINT('Ctrl Pts',(48.4347895562984,-20.7684056538652,
-235.35005));
#214529=CARTESIAN_POINT('Ctrl Pts',(48.4772403630263,-21.1899452510779,
-235.35005));
#214530=CARTESIAN_POINT('Ctrl Pts',(48.4986731253089,-21.612803748536,-235.35005));
#214531=CARTESIAN_POINT('Ctrl Pts',(48.541538649874,-22.458520743452,-235.35005));
#214532=CARTESIAN_POINT('Ctrl Pts',(48.5005032095075,-23.3116677382499,
-235.35005));
#214533=CARTESIAN_POINT('Ctrl Pts',(48.3713478679476,-24.1646010300614,
-235.35005));
#214534=CARTESIAN_POINT('Ctrl Pts',(48.3390590325577,-24.3778343530143,
-235.35005));
#214535=CARTESIAN_POINT('Ctrl Pts',(48.3012455308435,-24.5909867391319,
-235.35005));
#214536=CARTESIAN_POINT('Ctrl Pts',(48.2577770486563,-24.8040562792487,
-235.35005));
#214537=CARTESIAN_POINT('Ctrl Pts',(48.2523434883829,-24.8306899717632,
-235.35005));
#214538=CARTESIAN_POINT('Ctrl Pts',(48.2468215386317,-24.8573223693642,
-235.35005));
#214539=CARTESIAN_POINT('Ctrl Pts',(48.2412109184648,-24.8839534679411,
-235.35005));
#214540=CARTESIAN_POINT('Ctrl Pts',(48.235600298298,-24.9105845665175,-235.35005));
#214541=CARTESIAN_POINT('Ctrl Pts',(48.2299135976341,-24.9372145504959,
-235.35005));
#214542=CARTESIAN_POINT('Ctrl Pts',(48.2243539041553,-24.9638463951525,
-235.35005));
#214543=CARTESIAN_POINT('Ctrl Pts',(48.2132345171977,-25.0171100844654,
-235.35005));
#214544=CARTESIAN_POINT('Ctrl Pts',(48.2024091551918,-25.0703780812439,
-235.35005));
#214545=CARTESIAN_POINT('Ctrl Pts',(48.1918756280125,-25.1236503534574,
-235.35005));
#214546=CARTESIAN_POINT('Ctrl Pts',(48.1708085736529,-25.2301948978888,
-235.35005));
#214547=CARTESIAN_POINT('Ctrl Pts',(48.1509087142019,-25.3367565417865,
-235.35005));
#214548=CARTESIAN_POINT('Ctrl Pts',(48.1321603275509,-25.4433350548857,
-235.35005));
#214549=CARTESIAN_POINT('Ctrl Pts',(48.0571667809486,-25.8696491072753,
-235.35005));
#214550=CARTESIAN_POINT('Ctrl Pts',(48.000556289184,-26.2962324731006,-235.35005));
#214551=CARTESIAN_POINT('Ctrl Pts',(47.9616645382748,-26.7230754200676,
-235.35005));
#214552=CARTESIAN_POINT('Ctrl Pts',(47.8838810364566,-27.5767613140017,
-235.35005));
#214553=CARTESIAN_POINT('Ctrl Pts',(47.87663302545,-28.4314805592623,-235.35005));
#214554=CARTESIAN_POINT('Ctrl Pts',(47.9382574172368,-29.287208791445,-235.35005));
#214555=CARTESIAN_POINT('Ctrl Pts',(47.9998818090236,-30.1429370236277,
-235.35005));
#214556=CARTESIAN_POINT('Ctrl Pts',(48.1303735979639,-30.9996741692801,
-235.35005));
#214557=CARTESIAN_POINT('Ctrl Pts',(48.3327003568643,-31.8574637039839,
-235.35005));
#214558=CARTESIAN_POINT('',(49.4221378995452,2.0719038723399,-234.730932718857));
#214559=CARTESIAN_POINT('Ctrl Pts',(49.4221408870095,2.07190450465514,-234.730934934417));
#214560=CARTESIAN_POINT('Ctrl Pts',(49.4182232852514,2.09035843187612,-234.730950730033));
#214561=CARTESIAN_POINT('Ctrl Pts',(49.4149015680381,2.10705572274098,-234.730654274928));
#214562=CARTESIAN_POINT('Ctrl Pts',(49.4115036991967,2.12415450023796,-234.73042449474));
#214563=CARTESIAN_POINT('Ctrl Pts',(49.3733014982797,2.31639586206113,-234.727841078683));
#214564=CARTESIAN_POINT('Ctrl Pts',(49.3393998324651,2.50907296397048,-234.72493425655));
#214565=CARTESIAN_POINT('Ctrl Pts',(49.3097659913891,2.70193509071576,-234.721698159298));
#214566=CARTESIAN_POINT('Ctrl Pts',(49.2774742385284,2.91209536379909,-234.718171810741));
#214567=CARTESIAN_POINT('Ctrl Pts',(49.2502357063853,3.12273707873325,-234.714246361282));
#214568=CARTESIAN_POINT('Ctrl Pts',(49.2280289779234,3.33299466926586,-234.709925176676));
#214569=CARTESIAN_POINT('Ctrl Pts',(49.2092927421519,3.51039296527072,-234.706279311698));
#214570=CARTESIAN_POINT('Ctrl Pts',(49.1941375830618,3.6875175390473,-234.702351808155));
#214571=CARTESIAN_POINT('Ctrl Pts',(49.1825231413468,3.86385721504412,-234.698147062218));
#214572=CARTESIAN_POINT('Ctrl Pts',(49.1681240737819,4.08247529169204,-234.692934205472));
#214573=CARTESIAN_POINT('Ctrl Pts',(49.1591074262883,4.29983617559454,-234.687308219309));
#214574=CARTESIAN_POINT('Ctrl Pts',(49.1552509845704,4.51563191357569,-234.681265027564));
#214575=CARTESIAN_POINT('Ctrl Pts',(49.1513139372653,4.73593811571876,-234.67509552378));
#214576=CARTESIAN_POINT('Ctrl Pts',(49.1527549634472,4.95461301468044,-234.668491134634));
#214577=CARTESIAN_POINT('Ctrl Pts',(49.1592840662806,5.17133527581149,-234.661454349866));
#214578=CARTESIAN_POINT('Ctrl Pts',(49.1613990646159,5.24153898269353,-234.659174896096));
#214579=CARTESIAN_POINT('Ctrl Pts',(49.1640475660896,5.31153784457789,-234.65685012576));
#214580=CARTESIAN_POINT('Ctrl Pts',(49.1672185750418,5.38132108902236,-234.654480287413));
#214581=CARTESIAN_POINT('Ctrl Pts',(49.1793032159329,5.64726340014486,-234.645448888945));
#214582=CARTESIAN_POINT('Ctrl Pts',(49.1990014495819,5.91050106767095,-234.635744155024));
#214583=CARTESIAN_POINT('Ctrl Pts',(49.2257531223812,6.1707314416152,-234.62537046774));
#214584=CARTESIAN_POINT('Ctrl Pts',(49.251986745657,6.42592242148932,-234.61519766822));
#214585=CARTESIAN_POINT('Ctrl Pts',(49.2850112790651,6.67820467251632,-234.604372700794));
#214586=CARTESIAN_POINT('Ctrl Pts',(49.3243732573171,6.92732901222819,-234.592891821915));
#214587=CARTESIAN_POINT('Ctrl Pts',(49.3653529024791,7.18669166359865,-234.580939111113));
#214588=CARTESIAN_POINT('Ctrl Pts',(49.4132016932428,7.44263148361976,-234.568275325636));
#214589=CARTESIAN_POINT('Ctrl Pts',(49.4673510903997,7.69487403972389,-234.554910952386));
#214590=CARTESIAN_POINT('Ctrl Pts',(49.5215004875566,7.94711659582802,-234.541546579136));
#214591=CARTESIAN_POINT('Ctrl Pts',(49.5819501731039,8.19566191358684,-234.52748158509));
#214592=CARTESIAN_POINT('Ctrl Pts',(49.6480781836462,8.44024209637807,-234.512742074857));
#214593=CARTESIAN_POINT('',(49.5702506762145,-3.34422295956514,-234.635326079404));
#214594=CARTESIAN_POINT('Ctrl Pts',(49.5702506762146,-3.34422295956515,
-234.635326079404));
#214595=CARTESIAN_POINT('Ctrl Pts',(49.731975358304,-2.38242690605151,-234.653464711487));
#214596=CARTESIAN_POINT('Ctrl Pts',(49.7872739145354,-1.4452195583889,-234.670501062853));
#214597=CARTESIAN_POINT('Ctrl Pts',(49.7263273644162,0.364338783416933,
-234.702369204151));
#214598=CARTESIAN_POINT('Ctrl Pts',(49.6098794126944,1.23676270601011,-234.717200994082));
#214599=CARTESIAN_POINT('Ctrl Pts',(49.4221349121291,2.07190323979717,-234.730930503297));
#214600=CARTESIAN_POINT('',(49.6141435772397,-8.70527256325991,-234.668819403276));
#214601=CARTESIAN_POINT('Ctrl Pts',(49.6141588085565,-8.70526917104303,
-234.668797544165));
#214602=CARTESIAN_POINT('Ctrl Pts',(49.5360287314272,-8.33694180550121,
-234.672403005448));
#214603=CARTESIAN_POINT('Ctrl Pts',(49.4735905740263,-7.96646653536758,
-234.674792519891));
#214604=CARTESIAN_POINT('Ctrl Pts',(49.4268342076459,-7.59523712284396,
-234.675966087494));
#214605=CARTESIAN_POINT('Ctrl Pts',(49.4174758208848,-7.52093476172361,
-234.67620097956));
#214606=CARTESIAN_POINT('Ctrl Pts',(49.4087456762641,-7.44660202278907,
-234.676387159727));
#214607=CARTESIAN_POINT('Ctrl Pts',(49.4006437153166,-7.37224983055676,
-234.676524627996));
#214608=CARTESIAN_POINT('Ctrl Pts',(49.3609559061817,-7.00803237342166,
-234.677198022304));
#214609=CARTESIAN_POINT('Ctrl Pts',(49.3363408447164,-6.64335215271695,
-234.676702539053));
#214610=CARTESIAN_POINT('Ctrl Pts',(49.3265733152131,-6.27948793853651,
-234.675038178241));
#214611=CARTESIAN_POINT('Ctrl Pts',(49.3242955632398,-6.19463614140473,
-234.674650055418));
#214612=CARTESIAN_POINT('Ctrl Pts',(49.3228252788021,-6.10982850191821,
-234.674198368419));
#214613=CARTESIAN_POINT('Ctrl Pts',(49.3221596987034,-6.02508083788686,
-234.673683117244));
#214614=CARTESIAN_POINT('Ctrl Pts',(49.3193496869264,-5.66728478229663,
-234.671507778961));
#214615=CARTESIAN_POINT('Ctrl Pts',(49.3308815436732,-5.31056154720834,
-234.668199445541));
#214616=CARTESIAN_POINT('Ctrl Pts',(49.3563581141433,-4.95604968380208,
-234.663758116984));
#214617=CARTESIAN_POINT('Ctrl Pts',(49.3630340858964,-4.86315212567135,
-234.662594295346));
#214618=CARTESIAN_POINT('Ctrl Pts',(49.3706676986219,-4.77040615738343,
-234.661352674513));
#214619=CARTESIAN_POINT('Ctrl Pts',(49.3792520240964,-4.67783171297721,
-234.660033254487));
#214620=CARTESIAN_POINT('Ctrl Pts',(49.411583041384,-4.32916996064808,-234.655063942478));
#214621=CARTESIAN_POINT('Ctrl Pts',(49.4573977378051,-3.98294469983329,
-234.648991056405));
#214622=CARTESIAN_POINT('Ctrl Pts',(49.5161582487585,-3.64013054346987,
-234.641814596268));
#214623=CARTESIAN_POINT('Ctrl Pts',(49.5331149974404,-3.54120333198457,
-234.639743657316));
#214624=CARTESIAN_POINT('Ctrl Pts',(49.5511499763925,-3.44255989539943,
-234.637580818362));
#214625=CARTESIAN_POINT('Ctrl Pts',(49.5702506762145,-3.34422295956514,
-234.635326079404));
#214626=CARTESIAN_POINT('',(49.5862818295591,-19.7758832613919,-234.611073195661));
#214627=CARTESIAN_POINT('Ctrl Pts',(49.5862817758785,-19.7758829597833,
-234.611073194947));
#214628=CARTESIAN_POINT('Ctrl Pts',(49.5856701841187,-19.7724466885745,
-234.611065064026));
#214629=CARTESIAN_POINT('Ctrl Pts',(49.5850559570526,-19.7691488444015,
-234.611102786428));
#214630=CARTESIAN_POINT('Ctrl Pts',(49.5844388227214,-19.7660482425881,
-234.611205858899));
#214631=CARTESIAN_POINT('Ctrl Pts',(49.5820527975357,-19.7540603922231,
-234.611604367782));
#214632=CARTESIAN_POINT('Ctrl Pts',(49.5796829994118,-19.7420708434331,
-234.612001236557));
#214633=CARTESIAN_POINT('Ctrl Pts',(49.5773293735759,-19.7300793556229,
-234.612396480909));
#214634=CARTESIAN_POINT('Ctrl Pts',(49.5726225928611,-19.7060987794809,
-234.613186890525));
#214635=CARTESIAN_POINT('Ctrl Pts',(49.5679804852513,-19.6821104490426,
-234.613970804101));
#214636=CARTESIAN_POINT('Ctrl Pts',(49.5634026502972,-19.6581124365314,
-234.614748341969));
#214637=CARTESIAN_POINT('Ctrl Pts',(49.5542514928455,-19.6101400667933,
-234.616302651271));
#214638=CARTESIAN_POINT('Ctrl Pts',(49.5453571228543,-19.5621290111651,
-234.617831489122));
#214639=CARTESIAN_POINT('Ctrl Pts',(49.5367169404556,-19.5140638167564,
-234.619335739067));
#214640=CARTESIAN_POINT('Ctrl Pts',(49.5113948055649,-19.3731971914697,
-234.623744305724));
#214641=CARTESIAN_POINT('Ctrl Pts',(49.4882494587589,-19.2318541056419,
-234.627942704));
#214642=CARTESIAN_POINT('Ctrl Pts',(49.4672600204691,-19.0896691715895,
-234.631947130515));
#214643=CARTESIAN_POINT('Ctrl Pts',(49.4597356917718,-19.0386984802903,
-234.633382643983));
#214644=CARTESIAN_POINT('Ctrl Pts',(49.4524888996529,-18.9876195779269,
-234.634793189811));
#214645=CARTESIAN_POINT('Ctrl Pts',(49.4455203099591,-18.9364155675292,
-234.636179383111));
#214646=CARTESIAN_POINT('Ctrl Pts',(49.4262703972779,-18.7949704871918,
-234.640008579715));
#214647=CARTESIAN_POINT('Ctrl Pts',(49.4091419635085,-18.6526552281547,
-234.64365180556));
#214648=CARTESIAN_POINT('Ctrl Pts',(49.3941865856165,-18.5090778608037,
-234.647113321184));
#214649=CARTESIAN_POINT('Ctrl Pts',(49.3912923261972,-18.4812918596174,
-234.647783215604));
#214650=CARTESIAN_POINT('Ctrl Pts',(49.3884796089816,-18.4534585861893,
-234.648446292274));
#214651=CARTESIAN_POINT('Ctrl Pts',(49.3857490339193,-18.4255751954284,
-234.649102564516));
#214652=CARTESIAN_POINT('Ctrl Pts',(49.3632387172659,-18.195710078709,-234.654512742091));
#214653=CARTESIAN_POINT('Ctrl Pts',(49.3464119095609,-17.9635945583682,
-234.659458943744));
#214654=CARTESIAN_POINT('Ctrl Pts',(49.335606787588,-17.7295172691397,-234.663920955939));
#214655=CARTESIAN_POINT('Ctrl Pts',(49.3275029461084,-17.5539593022183,
-234.667267465085));
#214656=CARTESIAN_POINT('Ctrl Pts',(49.3227855338785,-17.3772989895442,
-234.670341773446));
#214657=CARTESIAN_POINT('Ctrl Pts',(49.3215747712971,-17.1996717234086,
-234.673142723318));
#214658=CARTESIAN_POINT('Ctrl Pts',(49.3213242475783,-17.1629181567187,
-234.673722279037));
#214659=CARTESIAN_POINT('Ctrl Pts',(49.3212223306807,-17.1252656126309,
-234.674303302428));
#214660=CARTESIAN_POINT('Ctrl Pts',(49.3212757178132,-17.0883123223587,
-234.674861077993));
#214661=CARTESIAN_POINT('Ctrl Pts',(49.3213083360333,-17.065734774158,-234.675201865095));
#214662=CARTESIAN_POINT('Ctrl Pts',(49.3213978701176,-17.043418278368,-234.675534060606));
#214663=CARTESIAN_POINT('Ctrl Pts',(49.3215363071684,-17.0217275821295,
-234.675852798948));
#214664=CARTESIAN_POINT('Ctrl Pts',(49.3223986160657,-16.8866186625913,
-234.677838184415));
#214665=CARTESIAN_POINT('Ctrl Pts',(49.3252945480659,-16.751112237095,-234.679665550824));
#214666=CARTESIAN_POINT('Ctrl Pts',(49.3302536736133,-16.615291107567,-234.681335289665));
#214667=CARTESIAN_POINT('Ctrl Pts',(49.3336914636545,-16.52113649865,-234.682492794452));
#214668=CARTESIAN_POINT('Ctrl Pts',(49.3381279215342,-16.4267999770715,
-234.683574583287));
#214669=CARTESIAN_POINT('Ctrl Pts',(49.3435718218144,-16.3323432037176,
-234.684579451245));
#214670=CARTESIAN_POINT('Ctrl Pts',(49.3502202748289,-16.2169863111923,
-234.685806662815));
#214671=CARTESIAN_POINT('Ctrl Pts',(49.3583723481284,-16.1014265720288,
-234.686919192352));
#214672=CARTESIAN_POINT('Ctrl Pts',(49.3680488937542,-15.9857057851749,
-234.687916165977));
#214673=CARTESIAN_POINT('Ctrl Pts',(49.3728871665672,-15.9278453917479,
-234.68841465279));
#214674=CARTESIAN_POINT('Ctrl Pts',(49.3781065858137,-15.8699447363607,
-234.688884269287));
#214675=CARTESIAN_POINT('Ctrl Pts',(49.38370992444,-15.8120092127478,-234.689325001877));
#214676=CARTESIAN_POINT('Ctrl Pts',(49.3865115937531,-15.7830414509413,
-234.689545368171));
#214677=CARTESIAN_POINT('Ctrl Pts',(49.3894092446592,-15.7540649722185,
-234.689758514671));
#214678=CARTESIAN_POINT('Ctrl Pts',(49.3924032336974,-15.7250804564227,
-234.689964447131));
#214679=CARTESIAN_POINT('Ctrl Pts',(49.3939002282166,-15.7105881985248,
-234.690067413361));
#214680=CARTESIAN_POINT('Ctrl Pts',(49.3954213073818,-15.6960939313622,
-234.690168576157));
#214681=CARTESIAN_POINT('Ctrl Pts',(49.3969665114127,-15.6815977400521,
-234.690267944053));
#214682=CARTESIAN_POINT('Ctrl Pts',(49.3977391134282,-15.6743496443971,
-234.690317628001));
#214683=CARTESIAN_POINT('Ctrl Pts',(49.3985177466665,-15.6671010677085,
-234.690366863229));
#214684=CARTESIAN_POINT('Ctrl Pts',(49.3993024163132,-15.6598520206932,
-234.69041565065));
#214685=CARTESIAN_POINT('Ctrl Pts',(49.4000870859599,-15.6526029736779,
-234.690464438071));
#214686=CARTESIAN_POINT('Ctrl Pts',(49.4007213537353,-15.6467769609444,
-234.690503374121));
#214687=CARTESIAN_POINT('Ctrl Pts',(49.401674525209,-15.6381034777402,-234.690560691966));
#214688=CARTESIAN_POINT('Ctrl Pts',(49.4086356681561,-15.5747598317086,
-234.690979292108));
#214689=CARTESIAN_POINT('Ctrl Pts',(49.4159098086407,-15.5126755048401,
-234.691363775393));
#214690=CARTESIAN_POINT('Ctrl Pts',(49.4234484001886,-15.4518567697051,
-234.691714239976));
#214691=CARTESIAN_POINT('Ctrl Pts',(49.440661182049,-15.312990031236,-234.692514451843));
#214692=CARTESIAN_POINT('Ctrl Pts',(49.4592406606155,-15.1807154273791,
-234.693137686318));
#214693=CARTESIAN_POINT('Ctrl Pts',(49.478646954445,-15.0550006305544,-234.693583469978));
#214694=CARTESIAN_POINT('Ctrl Pts',(49.4879824635785,-14.9945248053252,
-234.693797916769));
#214695=CARTESIAN_POINT('Ctrl Pts',(49.4975100768272,-14.9355669998248,
-234.693971233389));
#214696=CARTESIAN_POINT('Ctrl Pts',(49.5071739782699,-14.8781235782245,
-234.694102988057));
#214697=CARTESIAN_POINT('Ctrl Pts',(49.5074893581282,-14.8762489214644,
-234.694107287849));
#214698=CARTESIAN_POINT('Ctrl Pts',(49.5078048831535,-14.8743758774791,
-234.694111543714));
#214699=CARTESIAN_POINT('Ctrl Pts',(49.508120551448,-14.8725044460541,-234.694115755664));
#214700=CARTESIAN_POINT('Ctrl Pts',(49.5251406418567,-14.7716012745984,
-234.694342854118));
#214701=CARTESIAN_POINT('Ctrl Pts',(49.5425755408943,-14.6753860554339,
-234.694442320262));
#214702=CARTESIAN_POINT('Ctrl Pts',(49.5601444764561,-14.5838256316434,
-234.694414310179));
#214703=CARTESIAN_POINT('Ctrl Pts',(49.5621650137457,-14.5732956112064,
-234.694411088844));
#214704=CARTESIAN_POINT('Ctrl Pts',(49.5641873542603,-14.5628271575438,
-234.694406178676));
#214705=CARTESIAN_POINT('Ctrl Pts',(49.566211095348,-14.552420220728,-234.694399577537));
#214706=CARTESIAN_POINT('Ctrl Pts',(49.5736604149337,-14.5141126532619,
-234.694375278974));
#214707=CARTESIAN_POINT('Ctrl Pts',(49.5811771868836,-14.4763331751919,
-234.694346304807));
#214708=CARTESIAN_POINT('Ctrl Pts',(49.5886002092495,-14.4397579604869,
-234.694321359156));
#214709=CARTESIAN_POINT('Ctrl Pts',(49.5910636104117,-14.4276201247147,
-234.694313080702));
#214710=CARTESIAN_POINT('Ctrl Pts',(49.593516501906,-14.4156148925837,-234.694305260061));
#214711=CARTESIAN_POINT('Ctrl Pts',(49.5959524605128,-14.4037669105823,
-234.694298256206));
#214712=CARTESIAN_POINT('Ctrl Pts',(49.5960037012185,-14.4035176867421,
-234.694298108879));
#214713=CARTESIAN_POINT('Ctrl Pts',(49.5960552484803,-14.4032670890162,
-234.694297928211));
#214714=CARTESIAN_POINT('Ctrl Pts',(49.5961070926888,-14.4030151592276,
-234.694297715194));
#214715=CARTESIAN_POINT('Ctrl Pts',(49.5968357955614,-14.399474128013,-234.694294721103));
#214716=CARTESIAN_POINT('Ctrl Pts',(49.5975953620603,-14.3958050469411,
-234.69428539975));
#214717=CARTESIAN_POINT('Ctrl Pts',(49.5983593106187,-14.3921217569436,
-234.694273113671));
#214718=CARTESIAN_POINT('Ctrl Pts',(49.5992007058072,-14.3880650669379,
-234.69425958207));
#214719=CARTESIAN_POINT('Ctrl Pts',(49.6000476775697,-14.3839900131974,
-234.694242427339));
#214720=CARTESIAN_POINT('Ctrl Pts',(49.6008803844364,-14.3799802633316,
-234.694224515693));
#214721=CARTESIAN_POINT('Ctrl Pts',(49.6019144604037,-14.3750008568475,
-234.694202272568));
#214722=CARTESIAN_POINT('Ctrl Pts',(49.6029268246743,-14.3701209564191,
-234.694178833582));
#214723=CARTESIAN_POINT('Ctrl Pts',(49.6038981183157,-14.3654180115775,
-234.694157721101));
#214724=CARTESIAN_POINT('Ctrl Pts',(49.6041263298015,-14.364313025419,-234.694152760592));
#214725=CARTESIAN_POINT('Ctrl Pts',(49.6043523256419,-14.3632175755733,
-234.694147922998));
#214726=CARTESIAN_POINT('Ctrl Pts',(49.6045759267312,-14.3621323392381,
-234.694143246236));
#214727=CARTESIAN_POINT('Ctrl Pts',(49.6059934793587,-14.3552523207936,
-234.694113597203));
#214728=CARTESIAN_POINT('Ctrl Pts',(49.6073707738684,-14.3485424439946,
-234.694084679769));
#214729=CARTESIAN_POINT('Ctrl Pts',(49.6087665891662,-14.3417169982584,
-234.694055262541));
#214730=CARTESIAN_POINT('Ctrl Pts',(49.6093905361203,-14.3386659383622,
-234.694042112671));
#214731=CARTESIAN_POINT('Ctrl Pts',(49.610018161141,-14.3355917831535,-234.694028862915));
#214732=CARTESIAN_POINT('Ctrl Pts',(49.6106546022253,-14.3324690009502,
-234.694015403194));
#214733=CARTESIAN_POINT('Ctrl Pts',(49.6109010631884,-14.3312597076973,
-234.694010190935));
#214734=CARTESIAN_POINT('Ctrl Pts',(49.6111485095382,-14.3300447656872,
-234.694004954272));
#214735=CARTESIAN_POINT('Ctrl Pts',(49.611395084026,-14.3288332896215,-234.693999732491));
#214736=CARTESIAN_POINT('Ctrl Pts',(49.6147850395021,-14.3121776738709,
-234.693927942397));
#214737=CARTESIAN_POINT('Ctrl Pts',(49.6181087457944,-14.2956937849329,
-234.693856881653));
#214738=CARTESIAN_POINT('Ctrl Pts',(49.621368056795,-14.2793823029497,-234.693786552336));
#214739=CARTESIAN_POINT('Ctrl Pts',(49.6215656402839,-14.2783934806131,
-234.693782288885));
#214740=CARTESIAN_POINT('Ctrl Pts',(49.6217729532503,-14.2773554051453,
-234.693777813415));
#214741=CARTESIAN_POINT('Ctrl Pts',(49.6219848206397,-14.2762938641407,
-234.693773237078));
#214742=CARTESIAN_POINT('Ctrl Pts',(49.6230024413037,-14.2711951745063,
-234.693751256464));
#214743=CARTESIAN_POINT('Ctrl Pts',(49.6241242489022,-14.2655550336701,
-234.69372694717));
#214744=CARTESIAN_POINT('Ctrl Pts',(49.6247840659456,-14.2622316392956,
-234.693712633033));
#214745=CARTESIAN_POINT('Ctrl Pts',(49.6426668794438,-14.1721587283643,
-234.693324681486));
#214746=CARTESIAN_POINT('Ctrl Pts',(49.6609091040036,-14.0757363427447,
-234.692911477574));
#214747=CARTESIAN_POINT('Ctrl Pts',(49.6791169932083,-13.9729211482607,
-234.692470892474));
#214748=CARTESIAN_POINT('Ctrl Pts',(49.6973032646488,-13.8702280236452,
-234.692030830469));
#214749=CARTESIAN_POINT('Ctrl Pts',(49.7154552845705,-13.7611572648343,
-234.691563453377));
#214750=CARTESIAN_POINT('Ctrl Pts',(49.7331290517043,-13.6456600080413,
-234.691066526182));
#214751=CARTESIAN_POINT('Ctrl Pts',(49.7482442014855,-13.5468831981776,
-234.690641538746));
#214752=CARTESIAN_POINT('Ctrl Pts',(49.7630087077081,-13.4434058299061,
-234.690194936374));
#214753=CARTESIAN_POINT('Ctrl Pts',(49.7771147668417,-13.3351940003421,
-234.689725245027));
#214754=CARTESIAN_POINT('Ctrl Pts',(49.7949428459257,-13.1984294343494,
-234.689131621082));
#214755=CARTESIAN_POINT('Ctrl Pts',(49.8117241545392,-13.0540845913291,
-234.68849815651));
#214756=CARTESIAN_POINT('Ctrl Pts',(49.8267588614032,-12.9022266763216,
-234.687827642294));
#214757=CARTESIAN_POINT('Ctrl Pts',(49.8421625163067,-12.7466422051183,
-234.687140673822));
#214758=CARTESIAN_POINT('Ctrl Pts',(49.8557327135801,-12.5831713881624,
-234.686414816221));
#214759=CARTESIAN_POINT('Ctrl Pts',(49.8666619592475,-12.4118807115379,
-234.685652912943));
#214760=CARTESIAN_POINT('Ctrl Pts',(49.8732556411801,-12.3085399802524,
-234.685193251954));
#214761=CARTESIAN_POINT('Ctrl Pts',(49.8788870231814,-12.2023528783246,
-234.684720467992));
#214762=CARTESIAN_POINT('Ctrl Pts',(49.8833697255501,-12.0933330559183,
-234.684235155878));
#214763=CARTESIAN_POINT('Ctrl Pts',(49.8880514882853,-11.9794720631608,
-234.683728292833));
#214764=CARTESIAN_POINT('Ctrl Pts',(49.8914804113678,-11.8626227426854,
-234.683207110347));
#214765=CARTESIAN_POINT('Ctrl Pts',(49.8934412608304,-11.7423757007386,
-234.682669394224));
#214766=CARTESIAN_POINT('Ctrl Pts',(49.894738686951,-11.6628124011977,-234.682313606105));
#214767=CARTESIAN_POINT('Ctrl Pts',(49.8953924076452,-11.5817614694099,
-234.681950577605));
#214768=CARTESIAN_POINT('Ctrl Pts',(49.8953275191994,-11.4991029504226,
-234.681579641099));
#214769=CARTESIAN_POINT('Ctrl Pts',(49.8952387203394,-11.3859860130922,
-234.681072020082));
#214770=CARTESIAN_POINT('Ctrl Pts',(49.8937813676868,-11.2697916883941,
-234.680549566865));
#214771=CARTESIAN_POINT('Ctrl Pts',(49.8907287252221,-11.1503225292933,
-234.680011055946));
#214772=CARTESIAN_POINT('Ctrl Pts',(49.8878360004288,-11.0371119576085,
-234.679500755802));
#214773=CARTESIAN_POINT('Ctrl Pts',(49.8835106413262,-10.9209603545162,
-234.678976034968));
#214774=CARTESIAN_POINT('Ctrl Pts',(49.8775253147662,-10.8017298269359,
-234.678435930759));
#214775=CARTESIAN_POINT('Ctrl Pts',(49.8728628910234,-10.7088521473173,
-234.678015202723));
#214776=CARTESIAN_POINT('Ctrl Pts',(49.8671925600611,-10.6141066390309,
-234.677585141172));
#214777=CARTESIAN_POINT('Ctrl Pts',(49.860391606809,-10.5174440725994,-234.677145336399));
#214778=CARTESIAN_POINT('Ctrl Pts',(49.8505015772869,-10.3768761845046,
-234.676505766912));
#214779=CARTESIAN_POINT('Ctrl Pts',(49.8384113869119,-10.235047932517,-234.675858297621));
#214780=CARTESIAN_POINT('Ctrl Pts',(49.8240396848632,-10.0925147954868,
-234.675205184815));
#214781=CARTESIAN_POINT('Ctrl Pts',(49.8087016745112,-9.94039817604559,
-234.674508158746));
#214782=CARTESIAN_POINT('Ctrl Pts',(49.7907738045307,-9.78735271922151,
-234.673805480482));
#214783=CARTESIAN_POINT('Ctrl Pts',(49.7701982149817,-9.6337741477004,-234.673097931498));
#214784=CARTESIAN_POINT('Ctrl Pts',(49.7594789629549,-9.55376441528764,
-234.672729320146));
#214785=CARTESIAN_POINT('Ctrl Pts',(49.7480419351235,-9.47360986582658,
-234.672359385541));
#214786=CARTESIAN_POINT('Ctrl Pts',(49.7358845215681,-9.39336568284322,
-234.671988232566));
#214787=CARTESIAN_POINT('Ctrl Pts',(49.7183214498908,-9.27744182033725,
-234.671452050568));
#214788=CARTESIAN_POINT('Ctrl Pts',(49.6992549877045,-9.16135102847471,
-234.670914760588));
#214789=CARTESIAN_POINT('Ctrl Pts',(49.678689170327,-9.04525751101117,-234.670376577874));
#214790=CARTESIAN_POINT('Ctrl Pts',(49.6684322730877,-8.98735758625207,
-234.670108167205));
#214791=CARTESIAN_POINT('Ctrl Pts',(49.657802596323,-8.92945695560662,-234.669839535815));
#214792=CARTESIAN_POINT('Ctrl Pts',(49.6468016237758,-8.87157583220034,
-234.669570719627));
#214793=CARTESIAN_POINT('Ctrl Pts',(49.6413045443101,-8.84265319526412,
-234.66943639478));
#214794=CARTESIAN_POINT('Ctrl Pts',(49.6357147660542,-8.81373542759733,
-234.669302023882));
#214795=CARTESIAN_POINT('Ctrl Pts',(49.6300325351597,-8.78482504213622,
-234.66916761209));
#214796=CARTESIAN_POINT('Ctrl Pts',(49.6271918438714,-8.77037200746602,
-234.669100416227));
#214797=CARTESIAN_POINT('Ctrl Pts',(49.6243280469705,-8.75592081772958,
-234.669033210143));
#214798=CARTESIAN_POINT('Ctrl Pts',(49.6214411790143,-8.74147178634651,
-234.668965994533));
#214799=CARTESIAN_POINT('Ctrl Pts',(49.6190101807009,-8.72930442315087,
-234.66890939304));
#214800=CARTESIAN_POINT('Ctrl Pts',(49.6164243458588,-8.71628499550421,
-234.668786528861));
#214801=CARTESIAN_POINT('Ctrl Pts',(49.6141435772397,-8.70527256325991,
-234.668819403276));
#214802=CARTESIAN_POINT('',(49.4065714250583,-25.1565443079239,-234.754646206088));
#214803=CARTESIAN_POINT('Ctrl Pts',(49.4065714250583,-25.1565443079239,
-234.754646206088));
#214804=CARTESIAN_POINT('Ctrl Pts',(49.4083237251269,-25.1482852903311,
-234.754641300908));
#214805=CARTESIAN_POINT('Ctrl Pts',(49.4102055948399,-25.1397156006737,
-234.754551679989));
#214806=CARTESIAN_POINT('Ctrl Pts',(49.4122790951397,-25.1306732453552,
-234.754333515752));
#214807=CARTESIAN_POINT('Ctrl Pts',(49.4189331800479,-25.1016553570693,
-234.753633403308));
#214808=CARTESIAN_POINT('Ctrl Pts',(49.425491479273,-25.0726317127091,-234.752931656091));
#214809=CARTESIAN_POINT('Ctrl Pts',(49.4319544654725,-25.0436011247394,
-234.752228286546));
#214810=CARTESIAN_POINT('Ctrl Pts',(49.4728120282646,-24.8600761976765,
-234.747781740559));
#214811=CARTESIAN_POINT('Ctrl Pts',(49.5098654845684,-24.6762738089479,
-234.743270532666));
#214812=CARTESIAN_POINT('Ctrl Pts',(49.5431992801992,-24.4918934418934,
-234.73869682228));
#214813=CARTESIAN_POINT('Ctrl Pts',(49.5519882195003,-24.4432788804942,
-234.737490897116));
#214814=CARTESIAN_POINT('Ctrl Pts',(49.5605182904898,-24.3946241281618,
-234.736280624611));
#214815=CARTESIAN_POINT('Ctrl Pts',(49.568790440235,-24.345923655823,-234.735066040129));
#214816=CARTESIAN_POINT('Ctrl Pts',(49.6017568726559,-24.1518409953682,
-234.73022563969));
#214817=CARTESIAN_POINT('Ctrl Pts',(49.6306454960324,-23.9570800797581,
-234.725316968833));
#214818=CARTESIAN_POINT('Ctrl Pts',(49.6554470702083,-23.7613422927836,
-234.720335856504));
#214819=CARTESIAN_POINT('Ctrl Pts',(49.6802486443842,-23.5656045058091,
-234.715354744174));
#214820=CARTESIAN_POINT('Ctrl Pts',(49.700963180708,-23.3688896486346,-234.710301186495));
#214821=CARTESIAN_POINT('Ctrl Pts',(49.7175182905949,-23.1709026248672,
-234.705170563269));
#214822=CARTESIAN_POINT('Ctrl Pts',(49.7356713244155,-22.9538055978434,
-234.699544724625));
#214823=CARTESIAN_POINT('Ctrl Pts',(49.7487978376448,-22.7356163428593,
-234.693812870551));
#214824=CARTESIAN_POINT('Ctrl Pts',(49.7567917730447,-22.5164167234237,
-234.687964276257));
#214825=CARTESIAN_POINT('Ctrl Pts',(49.7668009281025,-22.2419582909034,
-234.680641288987));
#214826=CARTESIAN_POINT('Ctrl Pts',(49.7687456636369,-21.965803803738,-234.673157766047));
#214827=CARTESIAN_POINT('Ctrl Pts',(49.7623994276333,-21.6883787893522,
-234.665517156773));
#214828=CARTESIAN_POINT('Ctrl Pts',(49.7613370439464,-21.6419368024084,
-234.664238090151));
#214829=CARTESIAN_POINT('Ctrl Pts',(49.7600424275965,-21.5954592431385,
-234.662954623012));
#214830=CARTESIAN_POINT('Ctrl Pts',(49.758514653018,-21.5489481463684,-234.661666773541));
#214831=CARTESIAN_POINT('Ctrl Pts',(49.7487383034572,-21.2513199839034,
-234.653425723591));
#214832=CARTESIAN_POINT('Ctrl Pts',(49.7293929801879,-20.9521046088994,
-234.645004832657));
#214833=CARTESIAN_POINT('Ctrl Pts',(49.7000390073759,-20.6515468050444,
-234.636394542428));
#214834=CARTESIAN_POINT('Ctrl Pts',(49.6839207729116,-20.4865108426676,
-234.631666641452));
#214835=CARTESIAN_POINT('Ctrl Pts',(49.6647857213185,-20.3210700797011,
-234.626881633434));
#214836=CARTESIAN_POINT('Ctrl Pts',(49.642567777647,-20.1552647178752,-234.622037937129));
#214837=CARTESIAN_POINT('Ctrl Pts',(49.6324559718875,-20.0798035664089,
-234.619833479465));
#214838=CARTESIAN_POINT('Ctrl Pts',(49.6217041325569,-20.0042701335921,
-234.617617831245));
#214839=CARTESIAN_POINT('Ctrl Pts',(49.610305223227,-19.9286703683168,-234.615391389004));
#214840=CARTESIAN_POINT('Ctrl Pts',(49.6042283741044,-19.8883675328454,
-234.614204454957));
#214841=CARTESIAN_POINT('Ctrl Pts',(49.5979490645606,-19.8479249986605,
-234.613010889523));
#214842=CARTESIAN_POINT('Ctrl Pts',(49.5914823407987,-19.8074583910592,
-234.611814120112));
#214843=CARTESIAN_POINT('Ctrl Pts',(49.5897664702623,-19.7967210436403,
-234.611496571158));
#214844=CARTESIAN_POINT('Ctrl Pts',(49.588035000243,-19.7857336252768,-234.611096518911));
#214845=CARTESIAN_POINT('Ctrl Pts',(49.5862818832396,-19.7758835630004,
-234.611073196375));
#214846=CARTESIAN_POINT('Ctrl Pts',(49.6580996754574,-31.5448418565169,
-234.479004868619));
#214847=CARTESIAN_POINT('Ctrl Pts',(49.5889692923824,-31.2886791266587,
-234.497358008625));
#214848=CARTESIAN_POINT('Ctrl Pts',(49.5259668643689,-31.0288090594549,
-234.514894203449));
#214849=CARTESIAN_POINT('Ctrl Pts',(49.4697189389541,-30.7654785287572,
-234.531587547898));
#214850=CARTESIAN_POINT('Ctrl Pts',(49.4152575562183,-30.5105118839856,
-234.547750679505));
#214851=CARTESIAN_POINT('Ctrl Pts',(49.3671284004809,-30.2523010935825,
-234.56312376229));
#214852=CARTESIAN_POINT('Ctrl Pts',(49.3258565664253,-29.9910701469485,
-234.577699648186));
#214853=CARTESIAN_POINT('Ctrl Pts',(49.2875821848102,-29.7488116389379,
-234.591216930176));
#214854=CARTESIAN_POINT('Ctrl Pts',(49.255208388255,-29.5039695196051,-234.604047867869));
#214855=CARTESIAN_POINT('Ctrl Pts',(49.2291203187707,-29.256794938899,-234.616195999337));
#214856=CARTESIAN_POINT('Ctrl Pts',(49.2269378044882,-29.2361164424324,
-234.617212305678));
#214857=CARTESIAN_POINT('Ctrl Pts',(49.2247992541417,-29.2154216216419,
-234.61822384072));
#214858=CARTESIAN_POINT('Ctrl Pts',(49.2227048770967,-29.1947106237874,
-234.619230610668));
#214859=CARTESIAN_POINT('Ctrl Pts',(49.2223959055597,-29.1916552480354,
-234.619379133714));
#214860=CARTESIAN_POINT('Ctrl Pts',(49.2220878948198,-29.1885995216247,
-234.619527554474));
#214861=CARTESIAN_POINT('Ctrl Pts',(49.2217808457243,-29.1855434451088,
-234.619675872946));
#214862=CARTESIAN_POINT('Ctrl Pts',(49.20814725871,-29.0498476045519,-234.626261506421));
#214863=CARTESIAN_POINT('Ctrl Pts',(49.1964096967195,-28.9134595989942,
-234.632645495629));
#214864=CARTESIAN_POINT('Ctrl Pts',(49.1866397428615,-28.7764255481263,
-234.638829547784));
#214865=CARTESIAN_POINT('Ctrl Pts',(49.1817547659324,-28.7079085226923,
-234.641921573861));
#214866=CARTESIAN_POINT('Ctrl Pts',(49.1773610716897,-28.639230013251,-234.644964533448));
#214867=CARTESIAN_POINT('Ctrl Pts',(49.1734686010682,-28.5703962137034,
-234.647956595317));
#214868=CARTESIAN_POINT('Ctrl Pts',(49.1715223657574,-28.5359793139296,
-234.649452626252));
#214869=CARTESIAN_POINT('Ctrl Pts',(49.1697014345782,-28.501523592874,-234.650935932901));
#214870=CARTESIAN_POINT('Ctrl Pts',(49.168006860434,-28.4670298366899,-234.652406563149));
#214871=CARTESIAN_POINT('Ctrl Pts',(49.1671595733619,-28.4497829585978,
-234.653141878273));
#214872=CARTESIAN_POINT('Ctrl Pts',(49.1663438753779,-28.4325265717615,
-234.653874024212));
#214873=CARTESIAN_POINT('Ctrl Pts',(49.16555989675,-28.4152607761411,-234.654603006956));
#214874=CARTESIAN_POINT('Ctrl Pts',(49.1647759181221,-28.3979949805206,
-234.655331989701));
#214875=CARTESIAN_POINT('Ctrl Pts',(49.1639715191952,-28.3794688098702,
-234.656110111894));
#214876=CARTESIAN_POINT('Ctrl Pts',(49.1633032261975,-28.3634352639083,
-234.656780506213));
#214877=CARTESIAN_POINT('Ctrl Pts',(49.1535492883436,-28.1294208250036,
-234.666565113486));
#214878=CARTESIAN_POINT('Ctrl Pts',(49.1495893664515,-27.8926629671012,
-234.67582098426));
#214879=CARTESIAN_POINT('Ctrl Pts',(49.1518827203227,-27.6535148424459,
-234.684541920212));
#214880=CARTESIAN_POINT('Ctrl Pts',(49.1541255209231,-27.4196383507616,
-234.69307061726));
#214881=CARTESIAN_POINT('Ctrl Pts',(49.1623490777284,-27.1834758646331,
-234.701087787783));
#214882=CARTESIAN_POINT('Ctrl Pts',(49.1769340405569,-26.9453619477479,
-234.708598340528));
#214883=CARTESIAN_POINT('Ctrl Pts',(49.1791954225708,-26.9084426538678,
-234.709762843249));
#214884=CARTESIAN_POINT('Ctrl Pts',(49.1816096339828,-26.8714764548459,
-234.710915186708));
#214885=CARTESIAN_POINT('Ctrl Pts',(49.1841779822909,-26.8344646058357,
-234.712055410861));
#214886=CARTESIAN_POINT('Ctrl Pts',(49.2006502999015,-26.5970860032813,
-234.719368334243));
#214887=CARTESIAN_POINT('Ctrl Pts',(49.2235079251189,-26.3577860189318,
-234.726160426343));
#214888=CARTESIAN_POINT('Ctrl Pts',(49.2531380562464,-26.1169359028825,
-234.732439631832));
#214889=CARTESIAN_POINT('Ctrl Pts',(49.27212838546,-25.962571989499,-234.736464054772));
#214890=CARTESIAN_POINT('Ctrl Pts',(49.2938996978226,-25.8075714743661,
-234.740277982051));
#214891=CARTESIAN_POINT('Ctrl Pts',(49.3185428121658,-25.6520333832136,
-234.743885335958));
#214892=CARTESIAN_POINT('Ctrl Pts',(49.3341255804144,-25.5536807969899,
-234.746166401539));
#214893=CARTESIAN_POINT('Ctrl Pts',(49.3508585425062,-25.4551134977549,
-234.748364421498));
#214894=CARTESIAN_POINT('Ctrl Pts',(49.3687672739086,-25.3563571553827,
-234.750479674118));
#214895=CARTESIAN_POINT('Ctrl Pts',(49.3708676149762,-25.3447749837087,
-234.750727751542));
#214896=CARTESIAN_POINT('Ctrl Pts',(49.3729841284433,-25.3331902121223,
-234.750974690391));
#214897=CARTESIAN_POINT('Ctrl Pts',(49.375116856777,-25.3216028823929,-234.751220490778));
#214898=CARTESIAN_POINT('Ctrl Pts',(49.3792883227327,-25.2989388840204,
-234.751701258972));
#214899=CARTESIAN_POINT('Ctrl Pts',(49.3835218907602,-25.2762647222862,
-234.752177679767));
#214900=CARTESIAN_POINT('Ctrl Pts',(49.3878178899344,-25.2535806672704,
-234.752649754833));
#214901=CARTESIAN_POINT('Ctrl Pts',(49.3906606768346,-25.2385699720099,
-234.752962140558));
#214902=CARTESIAN_POINT('Ctrl Pts',(49.3935301713084,-25.2235581768053,
-234.753272557438));
#214903=CARTESIAN_POINT('Ctrl Pts',(49.3964294158785,-25.2085301804932,
-234.753581316476));
#214904=CARTESIAN_POINT('Ctrl Pts',(49.3971175598791,-25.2049632425366,
-234.753654601318));
#214905=CARTESIAN_POINT('Ctrl Pts',(49.3978042781239,-25.2014054520326,
-234.753730521486));
#214906=CARTESIAN_POINT('Ctrl Pts',(49.3984958597482,-25.1978402612382,
-234.753804681903));
#214907=CARTESIAN_POINT('Ctrl Pts',(49.3999020438809,-25.1905912040789,
-234.753955471337));
#214908=CARTESIAN_POINT('Ctrl Pts',(49.4013130280618,-25.1833515220461,
-234.75410795772));
#214909=CARTESIAN_POINT('Ctrl Pts',(49.4027328290424,-25.176100384502,-234.754255739074));
#214910=CARTESIAN_POINT('Ctrl Pts',(49.4040083829467,-25.1695859385117,
-234.754388506332));
#214911=CARTESIAN_POINT('Ctrl Pts',(49.4052913934605,-25.1630613071466,
-234.754517219509));
#214912=CARTESIAN_POINT('Ctrl Pts',(49.4065714250583,-25.1565443079239,
-234.754646206088));
#214913=CARTESIAN_POINT('Ctrl Pts',(49.6484258549514,-31.4615165308374,
-234.455477481092));
#214914=CARTESIAN_POINT('Ctrl Pts',(49.2664731987108,-31.560789847093,-235.350058857215));
#214915=CARTESIAN_POINT('Ctrl Pts',(48.3201502075429,-31.80681617839,-235.350049999939));
#214916=CARTESIAN_POINT('Ctrl Pts',(49.6915640011734,-31.7936717862045,
-234.549499823154));
#214917=CARTESIAN_POINT('Ctrl Pts',(49.2699360139611,-31.8599982863635,
-235.350057753084));
#214918=CARTESIAN_POINT('Ctrl Pts',(48.3725632633062,-32.0091245803159,
-235.350049999945));
#214919=CARTESIAN_POINT('Ctrl Pts',(49.6857617267569,-32.1386243287738,
-234.636173317449));
#214920=CARTESIAN_POINT('Ctrl Pts',(49.2421194654545,-32.1629747549767,
-235.350056782343));
#214921=CARTESIAN_POINT('Ctrl Pts',(48.3981101575135,-32.2149613628368,
-235.350049999951));
#214922=CARTESIAN_POINT('Ctrl Pts',(49.6111587388972,-32.4987313250346,
-234.71178896734));
#214923=CARTESIAN_POINT('Ctrl Pts',(49.1639864030906,-32.4715648130799,
-235.350055966599));
#214924=CARTESIAN_POINT('Ctrl Pts',(48.3856187844907,-32.424238145886,-235.350049999956));
#214925=CARTESIAN_POINT('',(49.6282925238268,-32.4090163077321,-234.692796980487));
#214926=CARTESIAN_POINT('',(48.3879672519817,-32.371991693197,-235.35005));
#214927=CARTESIAN_POINT('Origin',(48.3879672519817,-32.371991693197,-233.85005));
#214928=CARTESIAN_POINT('Ctrl Pts',(48.3327003568643,-31.8574637039841,
-235.35005));
#214929=CARTESIAN_POINT('Ctrl Pts',(48.3726098627487,-32.0266650324685,
-235.35005));
#214930=CARTESIAN_POINT('Ctrl Pts',(48.3931627529261,-32.1979455093617,
-235.35005));
#214931=CARTESIAN_POINT('Ctrl Pts',(48.3879672519817,-32.371991693197,-235.35005));
#214932=CARTESIAN_POINT('Ctrl Pts',(49.628292885354,-32.4090157027691,-234.692796608792));
#214933=CARTESIAN_POINT('Ctrl Pts',(49.6398669805306,-32.3436091289938,
-234.67863584219));
#214934=CARTESIAN_POINT('Ctrl Pts',(49.6495418145593,-32.2762949055162,
-234.663608766721));
#214935=CARTESIAN_POINT('Ctrl Pts',(49.6570361968937,-32.2072402554883,
-234.647660035004));
#214936=CARTESIAN_POINT('Ctrl Pts',(49.6643123728975,-32.1401961996784,
-234.632175666335));
#214937=CARTESIAN_POINT('Ctrl Pts',(49.6695326571342,-32.0715117584191,
-234.615822291237));
#214938=CARTESIAN_POINT('Ctrl Pts',(49.6724397156995,-32.0013794966331,
-234.598579757521));
#214939=CARTESIAN_POINT('Ctrl Pts',(49.6753085015994,-31.9321705559741,
-234.581564229113));
#214940=CARTESIAN_POINT('Ctrl Pts',(49.6759239895025,-31.8615518482465,
-234.563682561565));
#214941=CARTESIAN_POINT('Ctrl Pts',(49.6740472933539,-31.7897450833274,
-234.544949166276));
#214942=CARTESIAN_POINT('Ctrl Pts',(49.6722003277704,-31.7190758790592,
-234.526512544884));
#214943=CARTESIAN_POINT('Ctrl Pts',(49.6679389519133,-31.6472562744759,
-234.507250841984));
#214944=CARTESIAN_POINT('Ctrl Pts',(49.6610521066377,-31.5745296567101,
-234.4872133978));
#214945=CARTESIAN_POINT('Ctrl Pts',(49.6601165710637,-31.5646501929824,
-234.484491434246));
#214946=CARTESIAN_POINT('Ctrl Pts',(49.6591326192859,-31.554754036246,-234.481755211493));
#214947=CARTESIAN_POINT('Ctrl Pts',(49.6580997553206,-31.5448418376796,
-234.479004906517));
#214948=CARTESIAN_POINT('Ctrl Pts',(49.6282923119739,-32.4090169808449,
-234.692797218109));
#214949=CARTESIAN_POINT('Ctrl Pts',(49.1821150693849,-32.3956980201291,
-235.35005));
#214950=CARTESIAN_POINT('Ctrl Pts',(48.3879672519816,-32.371991693197,-235.35005));
#214951=CARTESIAN_POINT('Ctrl Pts',(49.5510892026461,-34.9515478422503,
-234.694718333571));
#214952=CARTESIAN_POINT('Ctrl Pts',(49.1048103477618,-34.9355482471023,
-235.350050000493));
#214953=CARTESIAN_POINT('Ctrl Pts',(48.3122036088614,-34.9100285686315,
-235.35005));
#214954=CARTESIAN_POINT('Ctrl Pts',(49.4597789489883,-37.4935285423766,
-234.696950276065));
#214955=CARTESIAN_POINT('Ctrl Pts',(49.0133760622712,-37.4755964900674,
-235.350049998731));
#214956=CARTESIAN_POINT('Ctrl Pts',(48.2225732111533,-37.4475766604583,
-235.35005));
#214957=CARTESIAN_POINT('Ctrl Pts',(49.3543621196711,-40.035034230092,-234.699454871761));
#214958=CARTESIAN_POINT('Ctrl Pts',(48.9077504789076,-40.0168122617172,
-235.35005));
#214959=CARTESIAN_POINT('Ctrl Pts',(48.1190600870606,-39.984633316822,-235.35005));
#214960=CARTESIAN_POINT('',(49.354362119671,-40.035034230092,-234.699454871761));
#214961=CARTESIAN_POINT('',(48.1190600870606,-39.9846333168228,-235.35005));
#214962=CARTESIAN_POINT('Origin',(48.1190600870606,-39.9846333168229,-233.85005));
#214963=CARTESIAN_POINT('Origin',(-647.878174798583,-11.5883202246486,-235.350049998812));
#214964=CARTESIAN_POINT('Origin',(-637.300587775051,-11.5397323655281,-248.898224599212));
#214965=CARTESIAN_POINT('Ctrl Pts',(49.3609022886797,-39.9800961280749,
-234.692504927202));
#214966=CARTESIAN_POINT('Ctrl Pts',(48.9149071348731,-39.9654566603571,
-235.350050000012));
#214967=CARTESIAN_POINT('Ctrl Pts',(48.1206232659769,-39.9395442085637,
-235.35005));
#214968=CARTESIAN_POINT('Ctrl Pts',(49.3507612567607,-40.0954256905313,
-234.703448471667));
#214969=CARTESIAN_POINT('Ctrl Pts',(48.9035065741159,-40.0745135650163,
-235.350049999981));
#214970=CARTESIAN_POINT('Ctrl Pts',(48.1178051349119,-40.0381099761122,
-235.35005));
#214971=CARTESIAN_POINT('Ctrl Pts',(49.3228943382751,-40.244776142729,-234.728096777874));
#214972=CARTESIAN_POINT('Ctrl Pts',(48.8754605639482,-40.2044568428276,
-235.350049999988));
#214973=CARTESIAN_POINT('Ctrl Pts',(48.1111069487499,-40.1362115562182,
-235.35005));
#214974=CARTESIAN_POINT('Ctrl Pts',(49.2876708175288,-40.4241334874338,
-234.747884490557));
#214975=CARTESIAN_POINT('Ctrl Pts',(48.8411755148561,-40.3683318596352,
-235.350050000006));
#214976=CARTESIAN_POINT('Ctrl Pts',(48.0952241561347,-40.2752167333539,
-235.35005));
#214977=CARTESIAN_POINT('Ctrl Pts',(49.2773222483615,-40.475626983426,-234.752817419735));
#214978=CARTESIAN_POINT('Ctrl Pts',(48.8311900432947,-40.4158061621275,
-235.35005));
#214979=CARTESIAN_POINT('Ctrl Pts',(48.0899153448806,-40.3165225558374,
-235.35005));
#214980=CARTESIAN_POINT('Ctrl Pts',(49.2523679230428,-40.5833911338063,
-234.764877519172));
#214981=CARTESIAN_POINT('Ctrl Pts',(48.8074437529392,-40.5134891744514,
-235.350049999999));
#214982=CARTESIAN_POINT('Ctrl Pts',(48.0779218876032,-40.3989852515461,
-235.35005));
#214983=CARTESIAN_POINT('Ctrl Pts',(49.2383249044512,-40.6384352750634,
-234.77139445193));
#214984=CARTESIAN_POINT('Ctrl Pts',(48.7942305707784,-40.5629457939505,
-235.350050000007));
#214985=CARTESIAN_POINT('Ctrl Pts',(48.0712183175412,-40.4401628322643,
-235.350050000001));
#214986=CARTESIAN_POINT('Ctrl Pts',(49.2070746873817,-40.7497958270093,
-234.784872532159));
#214987=CARTESIAN_POINT('Ctrl Pts',(48.7651880041785,-40.6623792650696,
-235.350049999994));
#214988=CARTESIAN_POINT('Ctrl Pts',(48.0561422093234,-40.5222290742639,
-235.350050000001));
#214989=CARTESIAN_POINT('Ctrl Pts',(49.1909312076253,-40.8041772199255,
-234.790945411729));
#214990=CARTESIAN_POINT('Ctrl Pts',(48.7502801223134,-40.7112070153247,
-235.350050000008));
#214991=CARTESIAN_POINT('Ctrl Pts',(48.047773596518,-40.5630852304628,-235.35005));
#214992=CARTESIAN_POINT('Ctrl Pts',(49.158768490346,-40.9094426031434,-234.801416987774));
#214993=CARTESIAN_POINT('Ctrl Pts',(48.7205621630999,-40.8065834345606,
-235.35004999999));
#214994=CARTESIAN_POINT('Ctrl Pts',(48.0296425423562,-40.6445005636306,
-235.35005));
#214995=CARTESIAN_POINT('Ctrl Pts',(49.1434940929471,-40.9592475630511,
-234.805322215117));
#214996=CARTESIAN_POINT('Ctrl Pts',(48.7063433535266,-40.85254418824,-235.350049999989));
#214997=CARTESIAN_POINT('Ctrl Pts',(48.0199029877981,-40.6850741153181,
-235.35005));
#214998=CARTESIAN_POINT('Ctrl Pts',(49.1099224820002,-41.0612319847,-234.814142137496));
#214999=CARTESIAN_POINT('Ctrl Pts',(48.6753864506452,-40.9456620301775,
-235.35005000001));
#215000=CARTESIAN_POINT('Ctrl Pts',(47.9992940161415,-40.7659290146224,
-235.35005));
#215001=CARTESIAN_POINT('Ctrl Pts',(49.0911625161288,-41.1139396903979,
-234.819288114395));
#215002=CARTESIAN_POINT('Ctrl Pts',(48.658290096543,-40.9931106903451,-235.350049999994));
#215003=CARTESIAN_POINT('Ctrl Pts',(47.9883597239418,-40.8062069855079,
-235.35005));
#215004=CARTESIAN_POINT('Ctrl Pts',(49.0497612331153,-41.2211842972616,
-234.830393428202));
#215005=CARTESIAN_POINT('Ctrl Pts',(48.6209603093232,-41.0887634737107,
-235.350050000006));
#215006=CARTESIAN_POINT('Ctrl Pts',(47.9648484820867,-40.886240947879,-235.35005));
#215007=CARTESIAN_POINT('Ctrl Pts',(49.0271415726836,-41.2754545539969,
-234.836237946169));
#215008=CARTESIAN_POINT('Ctrl Pts',(48.6007577894006,-41.1368001922989,
-235.350050000005));
#215009=CARTESIAN_POINT('Ctrl Pts',(47.9522083925962,-40.9259746645696,
-235.35005));
#215010=CARTESIAN_POINT('Ctrl Pts',(48.9650627061772,-41.4259459193992,
-234.848433785789));
#215011=CARTESIAN_POINT('Ctrl Pts',(48.5443602555291,-41.2734119529302,
-235.350049999989));
#215012=CARTESIAN_POINT('Ctrl Pts',(47.9122208177014,-41.0445137282603,
-235.35005));
#215013=CARTESIAN_POINT('Ctrl Pts',(48.9305571766217,-41.5134474083714,
-234.850906132381));
#215014=CARTESIAN_POINT('Ctrl Pts',(48.5115159447976,-41.3570281892003,
-235.350049999988));
#215015=CARTESIAN_POINT('Ctrl Pts',(47.8834173029482,-41.1228515949417,
-235.35005));
#215016=CARTESIAN_POINT('Ctrl Pts',(48.8600618058509,-41.6614149400665,
-234.862519417299));
#215017=CARTESIAN_POINT('Ctrl Pts',(48.4478519693268,-41.491030261857,-235.350050000005));
#215018=CARTESIAN_POINT('Ctrl Pts',(47.8371337927352,-41.2386632571498,
-235.35005));
#215019=CARTESIAN_POINT('Ctrl Pts',(48.8336689082344,-41.7126402268251,
-234.867383172689));
#215020=CARTESIAN_POINT('Ctrl Pts',(48.4244367378701,-41.5365309708231,
-235.35005));
#215021=CARTESIAN_POINT('Ctrl Pts',(47.8210253111431,-41.2769359664061,
-235.35005));
#215022=CARTESIAN_POINT('Ctrl Pts',(48.7803894023132,-41.8118797264952,
-234.876221787666));
#215023=CARTESIAN_POINT('Ctrl Pts',(48.37695681055,-41.6253295090172,-235.35005));
#215024=CARTESIAN_POINT('Ctrl Pts',(47.787220073548,-41.3527085858238,-235.35005));
#215025=CARTESIAN_POINT('Ctrl Pts',(48.7561458319887,-41.8571965621144,
-234.87901210393));
#215026=CARTESIAN_POINT('Ctrl Pts',(48.3547551060156,-41.6671925154113,
-235.350050000011));
#215027=CARTESIAN_POINT('Ctrl Pts',(47.7696001307559,-41.3902458706063,
-235.35005));
#215028=CARTESIAN_POINT('Ctrl Pts',(48.709016314243,-41.9449099980397,-234.883574453964));
#215029=CARTESIAN_POINT('Ctrl Pts',(48.3110938377002,-41.7490915977428,
-235.350049999989));
#215030=CARTESIAN_POINT('Ctrl Pts',(47.7335555457799,-41.4649289014138,
-235.35005));
#215031=CARTESIAN_POINT('Ctrl Pts',(48.6862807786918,-41.9870730165852,
-234.885251664481));
#215032=CARTESIAN_POINT('Ctrl Pts',(48.2897285580126,-41.7890208404672,
-235.35005));
#215033=CARTESIAN_POINT('Ctrl Pts',(47.7151163766151,-41.5020675791261,
-235.35005));
#215034=CARTESIAN_POINT('Ctrl Pts',(48.6527827899951,-42.048957440397,-234.887309869629));
#215035=CARTESIAN_POINT('Ctrl Pts',(48.2579806505418,-41.8480729618835,
-235.35005));
#215036=CARTESIAN_POINT('Ctrl Pts',(47.6870475431915,-41.5575760651628,
-235.35005));
#215037=CARTESIAN_POINT('Ctrl Pts',(48.6419512689392,-42.0691542325064,
-234.887831081218));
#215038=CARTESIAN_POINT('Ctrl Pts',(48.2476153284943,-41.8675047923045,
-235.35005));
#215039=CARTESIAN_POINT('Ctrl Pts',(47.677640411345,-41.5760541500354,-235.35005));
#215040=CARTESIAN_POINT('Ctrl Pts',(48.6154192627871,-42.1141139023562,
-234.890846380581));
#215041=CARTESIAN_POINT('Ctrl Pts',(48.2234659120011,-41.9087902255785,
-235.35005));
#215042=CARTESIAN_POINT('Ctrl Pts',(47.6585760783126,-41.6128886447362,
-235.35005));
#215043=CARTESIAN_POINT('Ctrl Pts',(48.6001168001999,-42.1384070049637,
-234.893144732287));
#215044=CARTESIAN_POINT('Ctrl Pts',(48.209961041715,-41.9303746091141,-235.350050000003));
#215045=CARTESIAN_POINT('Ctrl Pts',(47.6488991764614,-41.6312354689061,
-235.35005));
#215046=CARTESIAN_POINT('Ctrl Pts',(48.5518764612557,-42.2121884412408,
-234.900509539638));
#215047=CARTESIAN_POINT('Ctrl Pts',(48.1677347868008,-41.9954128487312,
-235.350049999995));
#215048=CARTESIAN_POINT('Ctrl Pts',(47.6191741486339,-41.6859381083017,
-235.35005));
#215049=CARTESIAN_POINT('Ctrl Pts',(48.5187143379562,-42.2604201801686,
-234.905150950974));
#215050=CARTESIAN_POINT('Ctrl Pts',(48.1386929365721,-42.0380430577305,
-235.350050000006));
#215051=CARTESIAN_POINT('Ctrl Pts',(47.5984065010933,-41.7219438293822,
-235.35005));
#215052=CARTESIAN_POINT('Ctrl Pts',(48.4473494493779,-42.3648892943066,
-234.91261447131));
#215053=CARTESIAN_POINT('Ctrl Pts',(48.0743924192389,-42.1331831672681,
-235.350049999991));
#215054=CARTESIAN_POINT('Ctrl Pts',(47.5478537905194,-41.8061740914771,
-235.35005));
#215055=CARTESIAN_POINT('Ctrl Pts',(48.4096151874694,-42.4198711263575,
-234.915062488495));
#215056=CARTESIAN_POINT('Ctrl Pts',(48.0392460437368,-42.184970184094,-235.350049999918));
#215057=CARTESIAN_POINT('Ctrl Pts',(47.5175825331856,-41.8541635100818,
-235.350050000001));
#215058=CARTESIAN_POINT('Ctrl Pts',(48.3726352067242,-42.4735605612944,
-234.917093394062));
#215059=CARTESIAN_POINT('Ctrl Pts',(48.0044280594344,-42.2359419015206,
-235.350050000092));
#215060=CARTESIAN_POINT('Ctrl Pts',(47.486819007697,-41.9019089637004,-235.35005));
#215061=CARTESIAN_POINT('',(48.4015825627194,-42.4301635567086,-234.916111528175));
#215062=CARTESIAN_POINT('',(47.511140470057,-41.8639253579254,-235.35005));
#215063=CARTESIAN_POINT('Origin',(47.5111404700569,-41.8639253579254,-233.85005));
#215064=CARTESIAN_POINT('Ctrl Pts',(48.1190600870606,-39.9846333168228,
-235.35005));
#215065=CARTESIAN_POINT('Ctrl Pts',(48.1156573562241,-40.0680330690653,
-235.35005));
#215066=CARTESIAN_POINT('Ctrl Pts',(48.1094051493674,-40.1511056240727,
-235.35005));
#215067=CARTESIAN_POINT('Ctrl Pts',(48.0999509844461,-40.2338479048312,
-235.35005));
#215068=CARTESIAN_POINT('Ctrl Pts',(48.0952242649892,-40.2752158682241,
-235.35005));
#215069=CARTESIAN_POINT('Ctrl Pts',(48.089915468827,-40.3165217899444,-235.35005));
#215070=CARTESIAN_POINT('Ctrl Pts',(48.0839186309937,-40.3577539058372,
-235.35005));
#215071=CARTESIAN_POINT('Ctrl Pts',(48.0779219885029,-40.398984678624,-235.35005));
#215072=CARTESIAN_POINT('Ctrl Pts',(48.0712184248364,-40.4401623582127,
-235.350050000001));
#215073=CARTESIAN_POINT('Ctrl Pts',(48.0636802851834,-40.4811959572599,
-235.350050000001));
#215074=CARTESIAN_POINT('Ctrl Pts',(48.0561422858351,-40.5222287925639,
-235.350050000001));
#215075=CARTESIAN_POINT('Ctrl Pts',(48.0477736645017,-40.563085046475,-235.35005));
#215076=CARTESIAN_POINT('Ctrl Pts',(48.0387080967012,-40.6037929031184,
-235.35005));
#215077=CARTESIAN_POINT('Ctrl Pts',(48.0296425710794,-40.6445005703635,
-235.35005));
#215078=CARTESIAN_POINT('Ctrl Pts',(48.0199029935916,-40.6850742166469,
-235.350049999999));
#215079=CARTESIAN_POINT('Ctrl Pts',(48.0095985320967,-40.7255015726492,
-235.350049999999));
#215080=CARTESIAN_POINT('Ctrl Pts',(47.9992939746968,-40.7659293049141,
-235.35005));
#215081=CARTESIAN_POINT('Ctrl Pts',(47.9883596446658,-40.8062073663638,
-235.35005));
#215082=CARTESIAN_POINT('Ctrl Pts',(47.9766041319244,-40.8462239751862,
-235.35005));
#215083=CARTESIAN_POINT('Ctrl Pts',(47.9648483456559,-40.8862415151148,
-235.35005));
#215084=CARTESIAN_POINT('Ctrl Pts',(47.9522082011025,-40.9259753165071,
-235.35005));
#215085=CARTESIAN_POINT('Ctrl Pts',(47.9388792235724,-40.965487693427,-235.35005));
#215086=CARTESIAN_POINT('Ctrl Pts',(47.9122207498503,-41.0445139847866,
-235.35005));
#215087=CARTESIAN_POINT('Ctrl Pts',(47.8834172501653,-41.1228517627344,
-235.35005));
#215088=CARTESIAN_POINT('Ctrl Pts',(47.8525616386501,-41.2000593734148,
-235.35005));
#215089=CARTESIAN_POINT('Ctrl Pts',(47.8371337962268,-41.2386632705008,
-235.35005));
#215090=CARTESIAN_POINT('Ctrl Pts',(47.8210253173756,-41.2769359691183,
-235.35005));
#215091=CARTESIAN_POINT('Ctrl Pts',(47.8041226974982,-41.3148222784138,
-235.35005));
#215092=CARTESIAN_POINT('Ctrl Pts',(47.7872200865336,-41.3527085677318,
-235.35005));
#215093=CARTESIAN_POINT('Ctrl Pts',(47.7696001482572,-41.3902458425851,
-235.35005));
#215094=CARTESIAN_POINT('Ctrl Pts',(47.7515778408436,-41.4275873872532,
-235.35005));
#215095=CARTESIAN_POINT('Ctrl Pts',(47.7335555714763,-41.4649288530908,
-235.35005));
#215096=CARTESIAN_POINT('Ctrl Pts',(47.7151164076773,-41.5020675212465,
-235.35005));
#215097=CARTESIAN_POINT('Ctrl Pts',(47.69640382207,-41.5390732370252,-235.35005));
#215098=CARTESIAN_POINT('Ctrl Pts',(47.6870475533414,-41.5575760473041,
-235.35005));
#215099=CARTESIAN_POINT('Ctrl Pts',(47.6776404221482,-41.5760541309719,
-235.35005));
#215100=CARTESIAN_POINT('Ctrl Pts',(47.6681082454436,-41.594471397704,-235.35005));
#215101=CARTESIAN_POINT('Ctrl Pts',(47.6585760901228,-41.6128886231199,
-235.35005));
#215102=CARTESIAN_POINT('Ctrl Pts',(47.6488991892717,-41.6312354462549,
-235.35005));
#215103=CARTESIAN_POINT('Ctrl Pts',(47.6389908341615,-41.649469682206,-235.35005));
#215104=CARTESIAN_POINT('Ctrl Pts',(47.6191742063161,-41.6859380025145,
-235.35005));
#215105=CARTESIAN_POINT('Ctrl Pts',(47.5984065690065,-41.7219437163951,
-235.35005));
#215106=CARTESIAN_POINT('Ctrl Pts',(47.5769871577403,-41.7576324579108,
-235.35005));
#215107=CARTESIAN_POINT('Ctrl Pts',(47.5555678934573,-41.7933209545252,
-235.35005));
#215108=CARTESIAN_POINT('Ctrl Pts',(47.5335334800369,-41.8287110790685,
-235.35005));
#215109=CARTESIAN_POINT('Ctrl Pts',(47.511140470057,-41.8639253579254,-235.35005));
#215110=CARTESIAN_POINT('Ctrl Pts',(48.4015825627194,-42.4301635567086,
-234.916111528174));
#215111=CARTESIAN_POINT('Ctrl Pts',(48.4058765897107,-42.4239165186186,
-234.915842996972));
#215112=CARTESIAN_POINT('Ctrl Pts',(48.4111227611927,-42.416329788671,-234.91547953379));
#215113=CARTESIAN_POINT('Ctrl Pts',(48.4172018787063,-42.4075544680719,
-234.91502113863));
#215114=CARTESIAN_POINT('Ctrl Pts',(48.4238231471873,-42.3979965423427,
-234.914521862639));
#215115=CARTESIAN_POINT('Ctrl Pts',(48.4314320807197,-42.3870292212898,
-234.91390996708));
#215116=CARTESIAN_POINT('Ctrl Pts',(48.4398329206511,-42.3748999215492,
-234.913185451955));
#215117=CARTESIAN_POINT('Ctrl Pts',(48.4509908371859,-42.3587898997852,
-234.912223157785));
#215118=CARTESIAN_POINT('Ctrl Pts',(48.4635435696801,-42.3406331652534,
-234.911062192536));
#215119=CARTESIAN_POINT('Ctrl Pts',(48.4769757389003,-42.3210768087327,
-234.909702556209));
#215120=CARTESIAN_POINT('Ctrl Pts',(48.4863784017206,-42.3073871489806,
-234.908750796166));
#215121=CARTESIAN_POINT('Ctrl Pts',(48.4962100771077,-42.293014008753,-234.907701684306));
#215122=CARTESIAN_POINT('Ctrl Pts',(48.5063029203191,-42.2781654388557,
-234.906555220629));
#215123=CARTESIAN_POINT('Ctrl Pts',(48.5138301808973,-42.2670913487811,
-234.90570018596));
#215124=CARTESIAN_POINT('Ctrl Pts',(48.5215027350369,-42.2557527423761,
-234.904791002233));
#215125=CARTESIAN_POINT('Ctrl Pts',(48.5292625384515,-42.2442201250679,
-234.903827669447));
#215126=CARTESIAN_POINT('Ctrl Pts',(48.537856146493,-42.2314483075947,-234.902760824846));
#215127=CARTESIAN_POINT('Ctrl Pts',(48.5465557290762,-42.2184399076426,
-234.901627569163));
#215128=CARTESIAN_POINT('Ctrl Pts',(48.5553068112671,-42.2052580396029,
-234.900427902398));
#215129=CARTESIAN_POINT('Ctrl Pts',(48.555804381456,-42.2045085432061,-234.900359691586));
#215130=CARTESIAN_POINT('Ctrl Pts',(48.5563021267504,-42.2037584745262,
-234.900291266077));
#215131=CARTESIAN_POINT('Ctrl Pts',(48.5568000403903,-42.2030078408306,
-234.900222625872));
#215132=CARTESIAN_POINT('Ctrl Pts',(48.5614275585508,-42.1960315887655,
-234.899584696376));
#215133=CARTESIAN_POINT('Ctrl Pts',(48.5660693588968,-42.1890068770094,
-234.898928222472));
#215134=CARTESIAN_POINT('Ctrl Pts',(48.5707217342098,-42.1819372506444,
-234.898253201485));
#215135=CARTESIAN_POINT('Ctrl Pts',(48.5730479218663,-42.1784024374619,
-234.897915690992));
#215136=CARTESIAN_POINT('Ctrl Pts',(48.575376758472,-42.1748563984891,-234.897573549528));
#215137=CARTESIAN_POINT('Ctrl Pts',(48.5777081628181,-42.1712990551989,
-234.897226768105));
#215138=CARTESIAN_POINT('Ctrl Pts',(48.579199712736,-42.1690231929698,-234.897004909635));
#215139=CARTESIAN_POINT('Ctrl Pts',(48.5810284034547,-42.1662290700574,
-234.896730574233));
#215140=CARTESIAN_POINT('Ctrl Pts',(48.5825473157475,-42.1639047252987,
-234.89650083858));
#215141=CARTESIAN_POINT('Ctrl Pts',(48.5834025772443,-42.1625959449387,
-234.896371480184));
#215142=CARTESIAN_POINT('Ctrl Pts',(48.584160492484,-42.1614350500923,-234.896256262291));
#215143=CARTESIAN_POINT('Ctrl Pts',(48.5847100715227,-42.1605929713353,
-234.8961725155));
#215144=CARTESIAN_POINT('Ctrl Pts',(48.5908125145944,-42.1512426553382,
-234.895242603722));
#215145=CARTESIAN_POINT('Ctrl Pts',(48.5971231173876,-42.1413133697012,
-234.894353868029));
#215146=CARTESIAN_POINT('Ctrl Pts',(48.6036135949882,-42.1308340972216,
-234.893506308421));
#215147=CARTESIAN_POINT('Ctrl Pts',(48.6097093883376,-42.1209920665702,
-234.892710288691));
#215148=CARTESIAN_POINT('Ctrl Pts',(48.6159634161574,-42.1106654554493,
-234.891950589495));
#215149=CARTESIAN_POINT('Ctrl Pts',(48.6223788309257,-42.0998426538058,
-234.891227210831));
#215150=CARTESIAN_POINT('Ctrl Pts',(48.6227942097007,-42.0991419100111,
-234.891180374242));
#215151=CARTESIAN_POINT('Ctrl Pts',(48.623210276151,-42.0984390712821,-234.891133689915));
#215152=CARTESIAN_POINT('Ctrl Pts',(48.623627035934,-42.09773412807,-234.89108715785));
#215153=CARTESIAN_POINT('Ctrl Pts',(48.629575688281,-42.0876720677069,-234.890422978895));
#215154=CARTESIAN_POINT('Ctrl Pts',(48.635663107759,-42.077184554178,-234.88978982102));
#215155=CARTESIAN_POINT('Ctrl Pts',(48.6419213003412,-42.0662231638559,
-234.889187684224));
#215156=CARTESIAN_POINT('Ctrl Pts',(48.6428732361153,-42.0645558230952,
-234.889096092993));
#215157=CARTESIAN_POINT('Ctrl Pts',(48.643829182441,-42.0628774393602,-234.889005219515));
#215158=CARTESIAN_POINT('Ctrl Pts',(48.6447893182988,-42.0611877542926,
-234.888915063789));
#215159=CARTESIAN_POINT('Ctrl Pts',(48.6466073340208,-42.0579883383006,
-234.888744354064));
#215160=CARTESIAN_POINT('Ctrl Pts',(48.6484403551025,-42.0547484237675,
-234.888576217721));
#215161=CARTESIAN_POINT('Ctrl Pts',(48.6502897877342,-42.0514660037669,
-234.888410654761));
#215162=CARTESIAN_POINT('Ctrl Pts',(48.6521393090423,-42.0481834263811,
-234.888245083861));
#215163=CARTESIAN_POINT('Ctrl Pts',(48.6540052670553,-42.0448583089355,
-234.888082086591));
#215164=CARTESIAN_POINT('Ctrl Pts',(48.6558872405973,-42.0414910032139,
-234.887921662949));
#215165=CARTESIAN_POINT('Ctrl Pts',(48.6592992792251,-42.0353860410891,
-234.887630813131));
#215166=CARTESIAN_POINT('Ctrl Pts',(48.6632168889193,-42.0283198289059,
-234.887313508735));
#215167=CARTESIAN_POINT('Ctrl Pts',(48.6664055104559,-42.0225317772452,
-234.887064701553));
#215168=CARTESIAN_POINT('Ctrl Pts',(48.6667342919522,-42.0219349662835,
-234.887039046832));
#215169=CARTESIAN_POINT('Ctrl Pts',(48.6670553602036,-42.0213517167477,
-234.887014120362));
#215170=CARTESIAN_POINT('Ctrl Pts',(48.6673673861988,-42.0207844652683,
-234.886990026236));
#215171=CARTESIAN_POINT('Ctrl Pts',(48.6807199768326,-41.9965099596024,
-234.885958961507));
#215172=CARTESIAN_POINT('Ctrl Pts',(48.6938401681919,-41.9724057555076,
-234.884930841656));
#215173=CARTESIAN_POINT('Ctrl Pts',(48.7066812179049,-41.9485236867256,
-234.883905666796));
#215174=CARTESIAN_POINT('Ctrl Pts',(48.7131017427615,-41.9365826523345,
-234.883393079366));
#215175=CARTESIAN_POINT('Ctrl Pts',(48.7194524819989,-41.92469715167,-234.882881227964));
#215176=CARTESIAN_POINT('Ctrl Pts',(48.7257276051451,-41.9128736322774,
-234.882370112876));
#215177=CARTESIAN_POINT('Ctrl Pts',(48.7288651667182,-41.9069618725811,
-234.882114555332));
#215178=CARTESIAN_POINT('Ctrl Pts',(48.7319838242549,-41.901065608196,-234.881859181852));
#215179=CARTESIAN_POINT('Ctrl Pts',(48.7350828492338,-41.8951856441896,
-234.881603992432));
#215180=CARTESIAN_POINT('Ctrl Pts',(48.7366323617233,-41.8922456621864,
-234.881476397721));
#215181=CARTESIAN_POINT('Ctrl Pts',(48.7381769660725,-41.8893097552775,
-234.881348849025));
#215182=CARTESIAN_POINT('Ctrl Pts',(48.7397165712593,-41.8863780239848,
-234.881221346343));
#215183=CARTESIAN_POINT('Ctrl Pts',(48.7411462357431,-41.8836556428567,
-234.881102948421));
#215184=CARTESIAN_POINT('Ctrl Pts',(48.7432383291511,-41.8796630722582,
-234.880929090271));
#215185=CARTESIAN_POINT('Ctrl Pts',(48.7441353410803,-41.8779489284838,
-234.880854382132));
#215186=CARTESIAN_POINT('Ctrl Pts',(48.7442043209866,-41.8778171114219,
-234.880848637102));
#215187=CARTESIAN_POINT('Ctrl Pts',(48.7442662527949,-41.8776987516867,
-234.880843478401));
#215188=CARTESIAN_POINT('Ctrl Pts',(48.7443202983215,-41.8775954574424,
-234.880838976339));
#215189=CARTESIAN_POINT('Ctrl Pts',(48.7476473280508,-41.8712366883937,
-234.880561830447));
#215190=CARTESIAN_POINT('Ctrl Pts',(48.752120649118,-41.8628871264216,-234.880086152886));
#215191=CARTESIAN_POINT('Ctrl Pts',(48.7576520371428,-41.8526432824589,
-234.879415168295));
#215192=CARTESIAN_POINT('Ctrl Pts',(48.7629733267166,-41.8427885299392,
-234.878769669679));
#215193=CARTESIAN_POINT('Ctrl Pts',(48.7692740269242,-41.8311803879651,
-234.877943418939));
#215194=CARTESIAN_POINT('Ctrl Pts',(48.7764409233617,-41.8179366980267,
-234.876939287047));
#215195=CARTESIAN_POINT('Ctrl Pts',(48.7832004942317,-41.8054457039822,
-234.875992224293));
#215196=CARTESIAN_POINT('Ctrl Pts',(48.7907307080359,-41.7914996138868,
-234.874886925309));
#215197=CARTESIAN_POINT('Ctrl Pts',(48.7989031198614,-41.7762293180923,
-234.873625798856));
#215198=CARTESIAN_POINT('Ctrl Pts',(48.8024382459928,-41.7696238724967,
-234.873080275555));
#215199=CARTESIAN_POINT('Ctrl Pts',(48.8060930874268,-41.7627710843506,
-234.872505594547));
#215200=CARTESIAN_POINT('Ctrl Pts',(48.8098550401669,-41.7556837104237,
-234.871901950799));
#215201=CARTESIAN_POINT('Ctrl Pts',(48.8134774071706,-41.7488593106426,
-234.871320705007));
#215202=CARTESIAN_POINT('Ctrl Pts',(48.8171989254069,-41.7418176117972,
-234.870712605902));
#215203=CARTESIAN_POINT('Ctrl Pts',(48.8210118579088,-41.7345651533579,
-234.870077827541));
#215204=CARTESIAN_POINT('Ctrl Pts',(48.8301924033937,-41.7171031278577,
-234.868549447058));
#215205=CARTESIAN_POINT('Ctrl Pts',(48.8385003646315,-41.7010002940541,
-234.867138614139));
#215206=CARTESIAN_POINT('Ctrl Pts',(48.8460185003354,-41.6862191638892,
-234.865851393547));
#215207=CARTESIAN_POINT('Ctrl Pts',(48.8538337124274,-41.6708539627613,
-234.864513308903));
#215208=CARTESIAN_POINT('Ctrl Pts',(48.8607952956676,-41.6569173591826,
-234.863308798586));
#215209=CARTESIAN_POINT('Ctrl Pts',(48.8669592620571,-41.6444145134275,
-234.862244675083));
#215210=CARTESIAN_POINT('Ctrl Pts',(48.8737155325054,-41.6307102519249,
-234.861078298481));
#215211=CARTESIAN_POINT('Ctrl Pts',(48.8795135428262,-41.6187288760359,
-234.860080584889));
#215212=CARTESIAN_POINT('Ctrl Pts',(48.8843841498665,-41.6085277539861,
-234.859260505412));
#215213=CARTESIAN_POINT('Ctrl Pts',(48.8878940311451,-41.601176570241,-234.858669535625));
#215214=CARTESIAN_POINT('Ctrl Pts',(48.8909213502999,-41.5947510294145,
-234.858170811309));
#215215=CARTESIAN_POINT('Ctrl Pts',(48.8934661879285,-41.5892843316424,
-234.857767689636));
#215216=CARTESIAN_POINT('Ctrl Pts',(48.8976602145231,-41.5802749254691,
-234.857103323865));
#215217=CARTESIAN_POINT('Ctrl Pts',(48.9029891670216,-41.5686200787691,
-234.856310174717));
#215218=CARTESIAN_POINT('Ctrl Pts',(48.9093841848883,-41.5543296198375,
-234.855388242192));
#215219=CARTESIAN_POINT('Ctrl Pts',(48.9124409545253,-41.5474988897486,
-234.854947565495));
#215220=CARTESIAN_POINT('Ctrl Pts',(48.9157412142244,-41.5400655297535,
-234.854477464799));
#215221=CARTESIAN_POINT('Ctrl Pts',(48.9192785359752,-41.5320259773337,
-234.853977940102));
#215222=CARTESIAN_POINT('Ctrl Pts',(48.9245902297567,-41.5199536685074,
-234.853227846555));
#215223=CARTESIAN_POINT('Ctrl Pts',(48.9304354193403,-41.5065164174248,
-234.852411406412));
#215224=CARTESIAN_POINT('Ctrl Pts',(48.9368033953279,-41.4916782238494,
-234.851528619674));
#215225=CARTESIAN_POINT('Ctrl Pts',(48.9369918005099,-41.4912392158246,
-234.851502501235));
#215226=CARTESIAN_POINT('Ctrl Pts',(48.9371806647031,-41.4907989787993,
-234.851476324719));
#215227=CARTESIAN_POINT('Ctrl Pts',(48.9373699869613,-41.490357512501,-234.851450090126));
#215228=CARTESIAN_POINT('Ctrl Pts',(48.9406641343836,-41.482676138519,-234.850993616507));
#215229=CARTESIAN_POINT('Ctrl Pts',(48.9440970549571,-41.4746225678903,
-234.850519560243));
#215230=CARTESIAN_POINT('Ctrl Pts',(48.9476631731474,-41.4661955828763,
-234.850027921335));
#215231=CARTESIAN_POINT('Ctrl Pts',(48.9509358476483,-41.4584620256852,
-234.849576737714));
#215232=CARTESIAN_POINT('Ctrl Pts',(48.9547586284399,-41.4493659192662,
-234.849050547871));
#215233=CARTESIAN_POINT('Ctrl Pts',(48.9579205074998,-41.4417921180272,
-234.84861508577));
#215234=CARTESIAN_POINT('Ctrl Pts',(48.9582040167386,-41.4411130146892,
-234.84857604015));
#215235=CARTESIAN_POINT('Ctrl Pts',(48.9584822446429,-41.4404461645817,
-234.84853772396));
#215236=CARTESIAN_POINT('Ctrl Pts',(48.9587543366942,-41.4397936549064,
-234.848500256676));
#215237=CARTESIAN_POINT('Ctrl Pts',(48.9702361796019,-41.4122588057559,
-234.846919198117));
#215238=CARTESIAN_POINT('Ctrl Pts',(48.9805781788196,-41.3871430599868,
-234.845367224494));
#215239=CARTESIAN_POINT('Ctrl Pts',(48.9898477853363,-41.3645095999571,
-234.843844335809));
#215240=CARTESIAN_POINT('Ctrl Pts',(48.9912563407676,-41.3610703511607,
-234.843612926512));
#215241=CARTESIAN_POINT('Ctrl Pts',(48.992640183932,-41.3576883348653,-234.843382188788));
#215242=CARTESIAN_POINT('Ctrl Pts',(48.9939995973888,-41.3543636888088,
-234.843152122637));
#215243=CARTESIAN_POINT('Ctrl Pts',(48.9991524073963,-41.3417617321442,
-234.842280064797));
#215244=CARTESIAN_POINT('Ctrl Pts',(49.0039541458915,-41.3299843043351,
-234.841417655873));
#215245=CARTESIAN_POINT('Ctrl Pts',(49.008420983189,-41.3190366856309,-234.840564895866));
#215246=CARTESIAN_POINT('Ctrl Pts',(49.0120206385271,-41.3102144135211,
-234.839877688809));
#215247=CARTESIAN_POINT('Ctrl Pts',(49.0157608335646,-41.3010650320092,
-234.839119020287));
#215248=CARTESIAN_POINT('Ctrl Pts',(49.0187841251101,-41.2936834024839,
-234.838476803518));
#215249=CARTESIAN_POINT('Ctrl Pts',(49.0195124570307,-41.291905116689,-234.83832208904));
#215250=CARTESIAN_POINT('Ctrl Pts',(49.0201994351696,-41.2902294274288,
-234.838174132974));
#215251=CARTESIAN_POINT('Ctrl Pts',(49.0208334887382,-41.2886856196551,
-234.838035562593));
#215252=CARTESIAN_POINT('Ctrl Pts',(49.0254665777583,-41.2774048711525,
-234.837023015798));
#215253=CARTESIAN_POINT('Ctrl Pts',(49.0310689340646,-41.2637691132399,
-234.835742021356));
#215254=CARTESIAN_POINT('Ctrl Pts',(49.0375460910749,-41.2477860244353,
-234.834192579268));
#215255=CARTESIAN_POINT('Ctrl Pts',(49.0400028112789,-41.2417238003564,
-234.833604891541));
#215256=CARTESIAN_POINT('Ctrl Pts',(49.0425849033903,-41.235324028244,-234.832978584714));
#215257=CARTESIAN_POINT('Ctrl Pts',(49.0452852787953,-41.2285877985872,
-234.832313658788));
#215258=CARTESIAN_POINT('Ctrl Pts',(49.0455029061471,-41.2280449156167,
-234.832260071398));
#215259=CARTESIAN_POINT('Ctrl Pts',(49.0457213010957,-41.2274998476253,
-234.832206233178));
#215260=CARTESIAN_POINT('Ctrl Pts',(49.0459404605559,-41.2269525940909,
-234.832152144127));
#215261=CARTESIAN_POINT('Ctrl Pts',(49.0515466236979,-41.2129536884977,
-234.830768530369));
#215262=CARTESIAN_POINT('Ctrl Pts',(49.0578395655724,-41.1970562046521,
-234.829172346469));
#215263=CARTESIAN_POINT('Ctrl Pts',(49.0644525702741,-41.1800234821052,
-234.827444186758));
#215264=CARTESIAN_POINT('Ctrl Pts',(49.0697631798137,-41.1663452612475,
-234.826056378664));
#215265=CARTESIAN_POINT('Ctrl Pts',(49.0752808972514,-41.1519341090171,
-234.824583459623));
#215266=CARTESIAN_POINT('Ctrl Pts',(49.0808392958684,-41.1371776680563,
-234.823067168547));
#215267=CARTESIAN_POINT('Ctrl Pts',(49.0893164404596,-41.1146725380187,
-234.820754664608));
#215268=CARTESIAN_POINT('Ctrl Pts',(49.0968873906078,-41.0938932734194,
-234.818663052831));
#215269=CARTESIAN_POINT('Ctrl Pts',(49.1036612384437,-41.0748331083061,
-234.816792333217));
#215270=CARTESIAN_POINT('Ctrl Pts',(49.1068597766085,-41.0658331031365,
-234.815908999516));
#215271=CARTESIAN_POINT('Ctrl Pts',(49.109879986753,-41.0572169829317,-234.815074916526));
#215272=CARTESIAN_POINT('Ctrl Pts',(49.112730460048,-41.0489865939022,-234.814290084247));
#215273=CARTESIAN_POINT('Ctrl Pts',(49.117174055609,-41.036156261402,-234.813066611206));
#215274=CARTESIAN_POINT('Ctrl Pts',(49.1212055212028,-41.0242631572238,
-234.811962825292));
#215275=CARTESIAN_POINT('Ctrl Pts',(49.1248501216751,-41.0133192130477,
-234.810978749706));
#215276=CARTESIAN_POINT('Ctrl Pts',(49.1266724219112,-41.0078472409597,
-234.810486711913));
#215277=CARTESIAN_POINT('Ctrl Pts',(49.1283979454193,-41.0026125435169,
-234.810024549733));
#215278=CARTESIAN_POINT('Ctrl Pts',(49.1300290541854,-40.9976170734923,
-234.809592343969));
#215279=CARTESIAN_POINT('Ctrl Pts',(49.1314605616382,-40.9932329068943,
-234.809213027896));
#215280=CARTESIAN_POINT('Ctrl Pts',(49.1323831615919,-40.990393026695,-234.808969007844));
#215281=CARTESIAN_POINT('Ctrl Pts',(49.1339469038135,-40.9855179929412,
-234.808564744256));
#215282=CARTESIAN_POINT('Ctrl Pts',(49.1341649431961,-40.984838245771,-234.808508376025));
#215283=CARTESIAN_POINT('Ctrl Pts',(49.1343953996984,-40.9841188682892,
-234.808448892349));
#215284=CARTESIAN_POINT('Ctrl Pts',(49.1346413371297,-40.9833500834446,
-234.808385492057));
#215285=CARTESIAN_POINT('Ctrl Pts',(49.1362450929454,-40.9783368442662,
-234.807972059316));
#215286=CARTESIAN_POINT('Ctrl Pts',(49.1378471491999,-40.9733180924222,
-234.807552694279));
#215287=CARTESIAN_POINT('Ctrl Pts',(49.1394478251217,-40.9682932030464,
-234.807127396947));
#215288=CARTESIAN_POINT('Ctrl Pts',(49.153894351016,-40.9229422400596,-234.803288975409));
#215289=CARTESIAN_POINT('Ctrl Pts',(49.1682293317435,-40.8770918568449,
-234.798967336173));
#215290=CARTESIAN_POINT('Ctrl Pts',(49.1823259261447,-40.8304162239187,
-234.794162479238));
#215291=CARTESIAN_POINT('Ctrl Pts',(49.1901551750911,-40.8044925760139,
-234.791493861555));
#215292=CARTESIAN_POINT('Ctrl Pts',(49.1979107030446,-40.7783142410855,
-234.788676186103));
#215293=CARTESIAN_POINT('Ctrl Pts',(49.2055692912838,-40.7518248496597,
-234.785709456672));
#215294=CARTESIAN_POINT('Ctrl Pts',(49.2093985854034,-40.7385801539468,
-234.784226091957));
#215295=CARTESIAN_POINT('Ctrl Pts',(49.2132036340421,-40.7252576920657,
-234.782705455196));
#215296=CARTESIAN_POINT('Ctrl Pts',(49.2169814186128,-40.7118504077679,
-234.781147559695));
#215297=CARTESIAN_POINT('Ctrl Pts',(49.2185774997028,-40.7061859468821,
-234.780489362409));
#215298=CARTESIAN_POINT('Ctrl Pts',(49.2202313157489,-40.7002861074153,
-234.779797710544));
#215299=CARTESIAN_POINT('Ctrl Pts',(49.2218625039109,-40.6944280582757,
-234.779106576097));
#215300=CARTESIAN_POINT('Ctrl Pts',(49.2240921956936,-40.686420616625,-234.778161855658));
#215301=CARTESIAN_POINT('Ctrl Pts',(49.226279145818,-40.6784902613952,-234.777218101989));
#215302=CARTESIAN_POINT('Ctrl Pts',(49.2282305670252,-40.671366518235,-234.776362079861));
#215303=CARTESIAN_POINT('Ctrl Pts',(49.24174670062,-40.6220253181418,-234.770433011646));
#215304=CARTESIAN_POINT('Ctrl Pts',(49.2545091663963,-40.5712328733757,
-234.764537276227));
#215305=CARTESIAN_POINT('Ctrl Pts',(49.2665542178985,-40.5185843252109,
-234.758674858163));
#215306=CARTESIAN_POINT('Ctrl Pts',(49.2725767436496,-40.4922600511286,
-234.755743649131));
#215307=CARTESIAN_POINT('Ctrl Pts',(49.2784199545212,-40.4654717565139,
-234.752820799011));
#215308=CARTESIAN_POINT('Ctrl Pts',(49.2840885951191,-40.438170148677,-234.749906269699));
#215309=CARTESIAN_POINT('Ctrl Pts',(49.286922915418,-40.4245193447585,-234.748449005043));
#215310=CARTESIAN_POINT('Ctrl Pts',(49.289713595599,-40.4107402129128,-234.746993822495));
#215311=CARTESIAN_POINT('Ctrl Pts',(49.2924612425713,-40.3968266306292,
-234.745540722148));
#215312=CARTESIAN_POINT('Ctrl Pts',(49.2925978596127,-40.396134826891,-234.745468471865));
#215313=CARTESIAN_POINT('Ctrl Pts',(49.2927343702682,-40.3954426907519,
-234.745396226733));
#215314=CARTESIAN_POINT('Ctrl Pts',(49.2928707746132,-40.3947502214547,
-234.745323986752));
#215315=CARTESIAN_POINT('Ctrl Pts',(49.2941060548759,-40.3884792067363,
-234.744669780156));
#215316=CARTESIAN_POINT('Ctrl Pts',(49.2953326163964,-40.3821808691388,
-234.744015996031));
#215317=CARTESIAN_POINT('Ctrl Pts',(49.2965499595654,-40.3758501094821,
-234.743362635016));
#215318=CARTESIAN_POINT('Ctrl Pts',(49.2972258429813,-40.3723351963735,
-234.742999881204));
#215319=CARTESIAN_POINT('Ctrl Pts',(49.2978988843611,-40.3688103024198,
-234.742637256271));
#215320=CARTESIAN_POINT('Ctrl Pts',(49.2985689987828,-40.3652745392547,
-234.742274762142));
#215321=CARTESIAN_POINT('Ctrl Pts',(49.2989040559936,-40.3635066576721,
-234.742093515077));
#215322=CARTESIAN_POINT('Ctrl Pts',(49.299238381464,-40.361736058786,-234.741912300712));
#215323=CARTESIAN_POINT('Ctrl Pts',(49.2995719644862,-40.3599626349555,
-234.741731118898));
#215324=CARTESIAN_POINT('Ctrl Pts',(49.2999055475083,-40.3581892111249,
-234.741549937085));
#215325=CARTESIAN_POINT('Ctrl Pts',(49.300482383806,-40.3551057375624,-234.741235715341));
#215326=CARTESIAN_POINT('Ctrl Pts',(49.3005704755418,-40.3546337796992,
-234.741187671114));
#215327=CARTESIAN_POINT('Ctrl Pts',(49.301449545857,-40.3499240967321,-234.740708236199));
#215328=CARTESIAN_POINT('Ctrl Pts',(49.3026877797277,-40.3436857853011,
-234.739965356228));
#215329=CARTESIAN_POINT('Ctrl Pts',(49.3042704770971,-40.3358544197516,
-234.738959031199));
#215330=CARTESIAN_POINT('Ctrl Pts',(49.3057384845081,-40.3285905530845,
-234.738025629382));
#215331=CARTESIAN_POINT('Ctrl Pts',(49.3075028611123,-40.3199567707358,
-234.73686558014));
#215332=CARTESIAN_POINT('Ctrl Pts',(49.3095444690461,-40.3098592240976,
-234.735478883472));
#215333=CARTESIAN_POINT('Ctrl Pts',(49.3113961043595,-40.3007012591306,
-234.734221219611));
#215334=CARTESIAN_POINT('Ctrl Pts',(49.3134757704784,-40.2903395683248,
-234.732777125229));
#215335=CARTESIAN_POINT('Ctrl Pts',(49.3157628185814,-40.2786619114353,
-234.731146600328));
#215336=CARTESIAN_POINT('Ctrl Pts',(49.3169535045081,-40.272582274677,-234.730297714356));
#215337=CARTESIAN_POINT('Ctrl Pts',(49.3182002924174,-40.2661452034528,
-234.729398297039));
#215338=CARTESIAN_POINT('Ctrl Pts',(49.3194994819158,-40.2593291615188,
-234.728448348378));
#215339=CARTESIAN_POINT('Ctrl Pts',(49.32187762862,-40.2468524999698,-234.726709481738));
#215340=CARTESIAN_POINT('Ctrl Pts',(49.3244318189892,-40.2331097150377,
-234.724801300995));
#215341=CARTESIAN_POINT('Ctrl Pts',(49.3271338197985,-40.2179260150997,
-234.72272380615));
#215342=CARTESIAN_POINT('Ctrl Pts',(49.3295407090787,-40.2044006732534,
-234.720873214523));
#215343=CARTESIAN_POINT('Ctrl Pts',(49.3320648414618,-40.1897317952828,
-234.718888273905));
#215344=CARTESIAN_POINT('Ctrl Pts',(49.3346806252661,-40.1737501501656,
-234.716768984295));
#215345=CARTESIAN_POINT('Ctrl Pts',(49.3372028738137,-40.1583399770777,
-234.714725476292));
#215346=CARTESIAN_POINT('Ctrl Pts',(49.3398103617817,-40.1417095765092,
-234.712557055623));
#215347=CARTESIAN_POINT('Ctrl Pts',(49.3424746028141,-40.1236602909776,
-234.710263722287));
#215348=CARTESIAN_POINT('Ctrl Pts',(49.3450122884389,-40.1064683733255,
-234.708079325693));
#215349=CARTESIAN_POINT('Ctrl Pts',(49.3476014713131,-40.0879893317989,
-234.705781601654));
#215350=CARTESIAN_POINT('Ctrl Pts',(49.3502121977989,-40.0680047616935,
-234.703370550173));
#215351=CARTESIAN_POINT('Ctrl Pts',(49.3515912773287,-40.0574481937443,
-234.702096946154));
#215352=CARTESIAN_POINT('Ctrl Pts',(49.352976276403,-40.0464707209573,-234.700791720017));
#215353=CARTESIAN_POINT('Ctrl Pts',(49.3543621196709,-40.0350342300919,
-234.69945487176));
#215354=CARTESIAN_POINT('Ctrl Pts',(48.4015825627194,-42.4301635567087,
-234.916111528175));
#215355=CARTESIAN_POINT('Ctrl Pts',(48.0316514259825,-42.1949218242413,
-235.35005));
#215356=CARTESIAN_POINT('Ctrl Pts',(47.5111404700569,-41.8639253579254,
-235.35005));
#215357=CARTESIAN_POINT('Ctrl Pts',(47.0743964923321,-44.5052610020243,
-234.922474108526));
#215358=CARTESIAN_POINT('Ctrl Pts',(46.7171148693285,-44.2522653739478,
-235.350049999732));
#215359=CARTESIAN_POINT('Ctrl Pts',(46.213538446068,-43.9044790762502,-235.35005));
#215360=CARTESIAN_POINT('Ctrl Pts',(45.629301810778,-46.4737259710815,-234.928556938652));
#215361=CARTESIAN_POINT('Ctrl Pts',(45.2835112520428,-46.2075181206225,
-235.350050000331));
#215362=CARTESIAN_POINT('Ctrl Pts',(44.7999466948037,-45.8404400906418,
-235.35005));
#215363=CARTESIAN_POINT('Ctrl Pts',(42.5086646561594,-50.2018332312079,
-234.936094455435));
#215364=CARTESIAN_POINT('Ctrl Pts',(42.1882337316621,-49.9076193249785,
-235.350049999669));
#215365=CARTESIAN_POINT('Ctrl Pts',(41.7430470430268,-49.5044128120585,
-235.35005));
#215366=CARTESIAN_POINT('Ctrl Pts',(40.8389768825302,-51.962002922669,-234.93759503995));
#215367=CARTESIAN_POINT('Ctrl Pts',(40.5293161951324,-51.6569873869132,
-235.350049999933));
#215368=CARTESIAN_POINT('Ctrl Pts',(40.1030327246601,-51.2355371590317,
-235.35005));
#215369=CARTESIAN_POINT('Ctrl Pts',(38.1562303218321,-54.4502282641876,
-234.936060246629));
#215370=CARTESIAN_POINT('Ctrl Pts',(37.8678859707896,-54.1250209801684,
-235.350050000033));
#215371=CARTESIAN_POINT('Ctrl Pts',(37.4698285345256,-53.6756545350797,
-235.35005));
#215372=CARTESIAN_POINT('Ctrl Pts',(37.2328209647283,-55.2522203973821,
-234.934954372966));
#215373=CARTESIAN_POINT('Ctrl Pts',(36.9511651975887,-54.9208963823306,
-235.350050000067));
#215374=CARTESIAN_POINT('Ctrl Pts',(36.5624534933628,-54.4622301034484,
-235.35005));
#215375=CARTESIAN_POINT('Ctrl Pts',(35.3284631493583,-56.8039921969795,
-234.93163892731));
#215376=CARTESIAN_POINT('Ctrl Pts',(35.0607726001854,-56.4604474243018,
-235.350049999933));
#215377=CARTESIAN_POINT('Ctrl Pts',(34.6902365366833,-55.9834272130437,
-235.35005));
#215378=CARTESIAN_POINT('Ctrl Pts',(34.3488682961681,-57.5524285204314,
-234.929428785626));
#215379=CARTESIAN_POINT('Ctrl Pts',(34.0879972243562,-57.2030837074672,
-235.35005000005));
#215380=CARTESIAN_POINT('Ctrl Pts',(33.7267628103062,-56.7166866533048,
-235.35005));
#215381=CARTESIAN_POINT('Ctrl Pts',(31.3507316578327,-59.6945695123404,
-234.920814246822));
#215382=CARTESIAN_POINT('Ctrl Pts',(31.1105534689003,-59.3284635730008,
-235.3500499999));
#215383=CARTESIAN_POINT('Ctrl Pts',(30.7793083468736,-58.8119074053918,
-235.35005));
#215384=CARTESIAN_POINT('Ctrl Pts',(29.2648462613946,-60.9897453716254,
-234.912770791881));
#215385=CARTESIAN_POINT('Ctrl Pts',(29.0391623276262,-60.6125303361456,
-235.350050001106));
#215386=CARTESIAN_POINT('Ctrl Pts',(28.7279549137639,-60.0762241747571,
-235.35005));
#215387=CARTESIAN_POINT('Ctrl Pts',(27.0930165135311,-62.1526330725429,
-234.905475377596));
#215388=CARTESIAN_POINT('Ctrl Pts',(26.8863570828206,-61.7639375806376,
-235.35005));
#215389=CARTESIAN_POINT('Ctrl Pts',(26.5926469327274,-61.2115127003622,
-235.35005));
#215390=CARTESIAN_POINT('',(27.0930165135311,-62.1526330725429,-234.905475377596));
#215391=CARTESIAN_POINT('',(26.5926469327273,-61.2115127003622,-235.35005));
#215392=CARTESIAN_POINT('Origin',(26.5926469327274,-61.2115127003622,-233.85005));
#215393=CARTESIAN_POINT('Ctrl Pts',(47.511140470057,-41.8639253579254,-235.35005));
#215394=CARTESIAN_POINT('Ctrl Pts',(46.5263591620664,-43.4125505315973,
-235.35005));
#215395=CARTESIAN_POINT('Ctrl Pts',(45.4748377912596,-44.9008380775653,
-235.35005));
#215396=CARTESIAN_POINT('Ctrl Pts',(44.3570056200731,-46.3291760712338,
-235.35005));
#215397=CARTESIAN_POINT('Ctrl Pts',(44.0018587501823,-46.7829738600906,
-235.35005));
#215398=CARTESIAN_POINT('Ctrl Pts',(43.6400181829326,-47.2307200839806,
-235.35005));
#215399=CARTESIAN_POINT('Ctrl Pts',(43.2714968690733,-47.6724264514822,
-235.35005));
#215400=CARTESIAN_POINT('Ctrl Pts',(41.7430470430284,-49.5044128120552,
-235.35005));
#215401=CARTESIAN_POINT('Ctrl Pts',(40.1030327246406,-51.2355371590496,
-235.35005));
#215402=CARTESIAN_POINT('Ctrl Pts',(38.3475632646338,-52.8622820764655,
-235.35005));
#215403=CARTESIAN_POINT('Ctrl Pts',(37.4698285346305,-53.6756545351735,
-235.35005));
#215404=CARTESIAN_POINT('Ctrl Pts',(36.5624534933633,-54.462230103448,-235.35005));
#215405=CARTESIAN_POINT('Ctrl Pts',(35.626345015024,-55.2228286582473,-235.35005));
#215406=CARTESIAN_POINT('Ctrl Pts',(34.6902365366847,-55.9834272130465,
-235.35005));
#215407=CARTESIAN_POINT('Ctrl Pts',(33.7267628103146,-56.7166866532988,
-235.35005));
#215408=CARTESIAN_POINT('Ctrl Pts',(32.7442779891666,-57.4150935706736,
-235.35005));
#215409=CARTESIAN_POINT('Ctrl Pts',(30.9377005462611,-58.6993130881051,
-235.35005));
#215410=CARTESIAN_POINT('Ctrl Pts',(29.0581394327502,-59.8715157745109,
-235.35005));
#215411=CARTESIAN_POINT('Ctrl Pts',(27.107386123889,-60.934451225102,-235.35005));
#215412=CARTESIAN_POINT('Ctrl Pts',(26.9363532637854,-61.0276443979109,
-235.35005));
#215413=CARTESIAN_POINT('Ctrl Pts',(26.7647731343724,-61.1199976105731,
-235.35005));
#215414=CARTESIAN_POINT('Ctrl Pts',(26.5926469327274,-61.2115127003622,
-235.35005));
#215415=CARTESIAN_POINT('Ctrl Pts',(27.0930165135311,-62.1526330725429,
-234.905475377596));
#215416=CARTESIAN_POINT('Ctrl Pts',(27.5718634056311,-61.8962384288525,
-234.907084021714));
#215417=CARTESIAN_POINT('Ctrl Pts',(28.0545166383205,-61.6291332678087,
-234.908756275144));
#215418=CARTESIAN_POINT('Ctrl Pts',(28.5399619314692,-61.3510080909548,
-234.910457848288));
#215419=CARTESIAN_POINT('Ctrl Pts',(29.0121022833342,-61.0805056868413,
-234.912112785217));
#215420=CARTESIAN_POINT('Ctrl Pts',(29.4868836627188,-60.7995789487944,
-234.913795406111));
#215421=CARTESIAN_POINT('Ctrl Pts',(29.9633988567347,-60.5079852690017,
-234.915468296034));
#215422=CARTESIAN_POINT('Ctrl Pts',(30.0374913798313,-60.4626458722182,
-234.915728410794));
#215423=CARTESIAN_POINT('Ctrl Pts',(30.1116258743564,-60.4170486717776,
-234.915988279334));
#215424=CARTESIAN_POINT('Ctrl Pts',(30.1857989902024,-60.3711928529312,
-234.916247749045));
#215425=CARTESIAN_POINT('Ctrl Pts',(30.6507245319281,-60.0837633553934,
-234.917874134755));
#215426=CARTESIAN_POINT('Ctrl Pts',(31.1171631399868,-59.7861707844739,
-234.919485158613));
#215427=CARTESIAN_POINT('Ctrl Pts',(31.5843037844726,-59.4782406979995,
-234.921040433439));
#215428=CARTESIAN_POINT('Ctrl Pts',(31.87201222967,-59.2885888501998,-234.921998315625));
#215429=CARTESIAN_POINT('Ctrl Pts',(32.1599873997248,-59.0950166566419,
-234.922934957828));
#215430=CARTESIAN_POINT('Ctrl Pts',(32.4480464998279,-58.8974909316072,
-234.923840099263));
#215431=CARTESIAN_POINT('Ctrl Pts',(32.6348129815887,-58.7694228209008,
-234.924426958283));
#215432=CARTESIAN_POINT('Ctrl Pts',(32.821614887809,-58.6396928444983,-234.92500056282));
#215433=CARTESIAN_POINT('Ctrl Pts',(33.0084035159985,-58.5082933347905,
-234.925557985548));
#215434=CARTESIAN_POINT('Ctrl Pts',(33.1097081454347,-58.4370289394787,
-234.925860303218));
#215435=CARTESIAN_POINT('Ctrl Pts',(33.2110100103575,-58.365272666291,-234.92615786251));
#215436=CARTESIAN_POINT('Ctrl Pts',(33.3122940517528,-58.2930287462961,
-234.926450163542));
#215437=CARTESIAN_POINT('Ctrl Pts',(33.316387149019,-58.2901092203041,-234.92646197603));
#215438=CARTESIAN_POINT('Ctrl Pts',(33.321463602919,-58.2864870754898,-234.926476613876));
#215439=CARTESIAN_POINT('Ctrl Pts',(33.3245722526722,-58.2842663723945,
-234.92648725201));
#215440=CARTESIAN_POINT('Ctrl Pts',(33.3328657245494,-58.278341826328,-234.926515633166));
#215441=CARTESIAN_POINT('Ctrl Pts',(33.341168468048,-58.2724073561477,-234.926543964589));
#215442=CARTESIAN_POINT('Ctrl Pts',(33.3494804760251,-58.2664629403962,
-234.926572246023));
#215443=CARTESIAN_POINT('Ctrl Pts',(33.5646083444542,-58.1126120907339,
-234.927304214122));
#215444=CARTESIAN_POINT('Ctrl Pts',(33.7860387420253,-57.9520450780028,
-234.927998708321));
#215445=CARTESIAN_POINT('Ctrl Pts',(34.0135675131175,-57.7844501465415,
-234.928655297153));
#215446=CARTESIAN_POINT('Ctrl Pts',(34.235288686026,-57.6211330214203,-234.929295126768));
#215447=CARTESIAN_POINT('Ctrl Pts',(34.4628010919038,-57.451141894775,-234.929898956642));
#215448=CARTESIAN_POINT('Ctrl Pts',(34.6958680422294,-57.2741939857683,
-234.930466305562));
#215449=CARTESIAN_POINT('Ctrl Pts',(34.9199081829414,-57.104099365415,-234.93101168075));
#215450=CARTESIAN_POINT('Ctrl Pts',(35.1490810038441,-56.9275761879985,
-234.931523341738));
#215451=CARTESIAN_POINT('Ctrl Pts',(35.3831297990818,-56.7443821331988,
-234.932000850011));
#215452=CARTESIAN_POINT('Ctrl Pts',(35.5724418873646,-56.5962042755007,
-234.932387086088));
#215453=CARTESIAN_POINT('Ctrl Pts',(35.7649433100188,-56.4436620936211,
-234.932750976463));
#215454=CARTESIAN_POINT('Ctrl Pts',(35.960473894234,-56.2866333907678,-234.933092313615));
#215455=CARTESIAN_POINT('Ctrl Pts',(36.0662372035414,-56.2016959098275,
-234.933276944305));
#215456=CARTESIAN_POINT('Ctrl Pts',(36.1728989271569,-56.1154340648653,
-234.93345627913));
#215457=CARTESIAN_POINT('Ctrl Pts',(36.2804224686007,-56.0278360381834,
-234.933630086089));
#215458=CARTESIAN_POINT('Ctrl Pts',(36.5772019915719,-55.7860536319977,
-234.934109816813));
#215459=CARTESIAN_POINT('Ctrl Pts',(36.8804171401314,-55.534226139737,-234.934547586812));
#215460=CARTESIAN_POINT('Ctrl Pts',(37.1894567165655,-55.2718686224767,
-234.934933522473));
#215461=CARTESIAN_POINT('Ctrl Pts',(37.2748942546821,-55.1993368754436,
-234.935040218817));
#215462=CARTESIAN_POINT('Ctrl Pts',(37.3607767694189,-55.1260000686736,
-234.935142946982));
#215463=CARTESIAN_POINT('Ctrl Pts',(37.4470909107402,-55.0518474005779,
-234.935241483442));
#215464=CARTESIAN_POINT('Ctrl Pts',(37.7029102456755,-54.832072448924,-234.935533527494));
#215465=CARTESIAN_POINT('Ctrl Pts',(37.9624741146055,-54.6051743831383,
-234.935786928809));
#215466=CARTESIAN_POINT('Ctrl Pts',(38.2252850299414,-54.3709827841254,
-234.936003250157));
#215467=CARTESIAN_POINT('Ctrl Pts',(38.3566904876093,-54.253886984619,-234.936111410831));
#215468=CARTESIAN_POINT('Ctrl Pts',(38.4889066221193,-54.1349682821895,
-234.936210475769));
#215469=CARTESIAN_POINT('Ctrl Pts',(38.6218645904408,-54.0142085592077,
-234.936301926129));
#215470=CARTESIAN_POINT('Ctrl Pts',(38.6883435746016,-53.9538286977168,
-234.936347651309));
#215471=CARTESIAN_POINT('Ctrl Pts',(38.755008016081,-53.8929885788722,-234.936391470356));
#215472=CARTESIAN_POINT('Ctrl Pts',(38.8218488051652,-53.8316862034097,
-234.936433688495));
#215473=CARTESIAN_POINT('Ctrl Pts',(38.8552691997073,-53.8010350156784,
-234.936454797565));
#215474=CARTESIAN_POINT('Ctrl Pts',(38.8887336811994,-53.7702682637168,
-234.936475506388));
#215475=CARTESIAN_POINT('Ctrl Pts',(38.9222410962122,-53.7393857057027,
-234.936495856913));
#215476=CARTESIAN_POINT('Ctrl Pts',(38.9389948037186,-53.7239444266957,
-234.936506032176));
#215477=CARTESIAN_POINT('Ctrl Pts',(38.9557592446103,-53.708474196172,-234.936516117866));
#215478=CARTESIAN_POINT('Ctrl Pts',(38.9725342729942,-53.69297498485,-234.936526119693));
#215479=CARTESIAN_POINT('Ctrl Pts',(38.9809217871861,-53.685225379189,-234.936531120606));
#215480=CARTESIAN_POINT('Ctrl Pts',(38.9893119482516,-53.6774685283282,
-234.936536100554));
#215481=CARTESIAN_POINT('Ctrl Pts',(38.9977047378706,-53.6697044286973,
-234.936541060243));
#215482=CARTESIAN_POINT('Ctrl Pts',(39.0039993300848,-53.6638813539741,
-234.93654478001));
#215483=CARTESIAN_POINT('Ctrl Pts',(39.0102954008607,-53.6580542018176,
-234.936548488382));
#215484=CARTESIAN_POINT('Ctrl Pts',(39.0165929428998,-53.6522229713257,
-234.936552184957));
#215485=CARTESIAN_POINT('Ctrl Pts',(39.0186921235795,-53.6502792278285,
-234.936553417148));
#215486=CARTESIAN_POINT('Ctrl Pts',(39.0216364393619,-53.6475523824562,
-234.936555143819));
#215487=CARTESIAN_POINT('Ctrl Pts',(39.0228909745786,-53.6463903808042,
-234.9365558783));
#215488=CARTESIAN_POINT('Ctrl Pts',(39.0320742480229,-53.6378844586339,
-234.936561254746));
#215489=CARTESIAN_POINT('Ctrl Pts',(39.0412703185288,-53.6293609283746,
-234.936566595268));
#215490=CARTESIAN_POINT('Ctrl Pts',(39.0504791367371,-53.6208197752944,
-234.93657189854));
#215491=CARTESIAN_POINT('Ctrl Pts',(39.3274433571275,-53.363936237084,-234.936731399627));
#215492=CARTESIAN_POINT('Ctrl Pts',(39.6158887006704,-53.0913151175466,
-234.936853712323));
#215493=CARTESIAN_POINT('Ctrl Pts',(39.9144891613816,-52.8026211254396,
-234.936903652261));
#215494=CARTESIAN_POINT('Ctrl Pts',(40.2324498159691,-52.4952092397139,
-234.936956830128));
#215495=CARTESIAN_POINT('Ctrl Pts',(40.561924137625,-52.1695726799131,-234.936927935723));
#215496=CARTESIAN_POINT('Ctrl Pts',(40.9012922354414,-51.8252513187329,
-234.936774253452));
#215497=CARTESIAN_POINT('Ctrl Pts',(40.9738029689377,-51.7516822513449,
-234.936741417089));
#215498=CARTESIAN_POINT('Ctrl Pts',(41.0467653441068,-51.6772599921148,
-234.936702883362));
#215499=CARTESIAN_POINT('Ctrl Pts',(41.1201635288383,-51.6019797568265,
-234.936658234884));
#215500=CARTESIAN_POINT('Ctrl Pts',(41.3966959063802,-51.3183566328712,
-234.936490018876));
#215501=CARTESIAN_POINT('Ctrl Pts',(41.6794226629877,-51.0225062183936,
-234.936257951047));
#215502=CARTESIAN_POINT('Ctrl Pts',(41.967065292056,-50.7146281499219,-234.935948979951));
#215503=CARTESIAN_POINT('Ctrl Pts',(42.2375329352271,-50.425133314496,-234.935658457352));
#215504=CARTESIAN_POINT('Ctrl Pts',(42.5123468242956,-50.1250040109044,
-234.935299940635));
#215505=CARTESIAN_POINT('Ctrl Pts',(42.7904844944196,-49.8144264272255,
-234.934863512671));
#215506=CARTESIAN_POINT('Ctrl Pts',(43.0190718299255,-49.5591783614407,
-234.934504834519));
#215507=CARTESIAN_POINT('Ctrl Pts',(43.2499047920019,-49.2968734040297,
-234.934093547199));
#215508=CARTESIAN_POINT('Ctrl Pts',(43.4824389229629,-49.0276279049742,
-234.933624664599));
#215509=CARTESIAN_POINT('Ctrl Pts',(43.6769491609346,-48.8024093279093,
-234.933232453504));
#215510=CARTESIAN_POINT('Ctrl Pts',(43.8725744141091,-48.5724217941096,
-234.932800098487));
#215511=CARTESIAN_POINT('Ctrl Pts',(44.0689832334687,-48.3377796011447,
-234.932325697043));
#215512=CARTESIAN_POINT('Ctrl Pts',(44.3317420558166,-48.0238715673934,
-234.931691035294));
#215513=CARTESIAN_POINT('Ctrl Pts',(44.5957361857819,-47.7016164793283,
-234.930979638848));
#215514=CARTESIAN_POINT('Ctrl Pts',(44.8601324618043,-47.3713165826379,
-234.930197051073));
#215515=CARTESIAN_POINT('Ctrl Pts',(45.1173862882891,-47.0499394679923,
-234.929435604267));
#215516=CARTESIAN_POINT('Ctrl Pts',(45.3750207433328,-46.7209462483979,
-234.928606783073));
#215517=CARTESIAN_POINT('Ctrl Pts',(45.6323048563377,-46.3846485512081,
-234.927718070288));
#215518=CARTESIAN_POINT('Ctrl Pts',(45.7425217833411,-46.2405833063328,
-234.927337358121));
#215519=CARTESIAN_POINT('Ctrl Pts',(45.8526748883602,-46.0951780116808,
-234.926945683224));
#215520=CARTESIAN_POINT('Ctrl Pts',(45.962708890812,-45.9484591535881,-234.926543756567));
#215521=CARTESIAN_POINT('Ctrl Pts',(46.1928389583745,-45.6416047270182,
-234.925703149056));
#215522=CARTESIAN_POINT('Ctrl Pts',(46.4224725107643,-45.3289660350924,
-234.92481754019));
#215523=CARTESIAN_POINT('Ctrl Pts',(46.6510236316563,-45.0109435350599,
-234.923894778246));
#215524=CARTESIAN_POINT('Ctrl Pts',(46.8773755380714,-44.6959811805359,
-234.922980895504));
#215525=CARTESIAN_POINT('Ctrl Pts',(47.1026656676339,-44.375738062674,-234.922030588858));
#215526=CARTESIAN_POINT('Ctrl Pts',(47.3263623726596,-44.0506372276144,
-234.921052672002));
#215527=CARTESIAN_POINT('Ctrl Pts',(47.5474575032212,-43.7293172887939,
-234.92008612824));
#215528=CARTESIAN_POINT('Ctrl Pts',(47.7669960212512,-43.4032519354286,
-234.919092631132));
#215529=CARTESIAN_POINT('Ctrl Pts',(47.9845022423295,-43.0728837348188,
-234.918081590818));
#215530=CARTESIAN_POINT('Ctrl Pts',(48.1244084772295,-42.8603814401771,
-234.917431260712));
#215531=CARTESIAN_POINT('Ctrl Pts',(48.2634746257799,-42.6460995632716,
-234.916773689743));
#215532=CARTESIAN_POINT('Ctrl Pts',(48.4015825627194,-42.4301635567087,
-234.916111528175));
#215533=CARTESIAN_POINT('Ctrl Pts',(27.2453371921567,-62.0684961123336,
-234.910710085558));
#215534=CARTESIAN_POINT('Ctrl Pts',(27.0364433475168,-61.680487024444,-235.350050000041));
#215535=CARTESIAN_POINT('Ctrl Pts',(26.7410849731316,-61.1326062593409,
-235.35005));
#215536=CARTESIAN_POINT('Ctrl Pts',(27.1368513731105,-62.1258987971579,
-234.905003039976));
#215537=CARTESIAN_POINT('Ctrl Pts',(26.9274704864059,-61.7399494328241,
-235.350049999987));
#215538=CARTESIAN_POINT('Ctrl Pts',(26.6293474091419,-61.1908379190527,
-235.35005));
#215539=CARTESIAN_POINT('Ctrl Pts',(27.0227991977541,-62.194936761442,-234.90610242041));
#215540=CARTESIAN_POINT('Ctrl Pts',(26.8144283136556,-61.8059798077595,
-235.350049999995));
#215541=CARTESIAN_POINT('Ctrl Pts',(26.5194896368383,-61.2532914016042,
-235.35005));
#215542=CARTESIAN_POINT('Ctrl Pts',(26.8369281750275,-62.3093205660776,
-234.878288708869));
#215543=CARTESIAN_POINT('Ctrl Pts',(26.6548033201846,-61.9041872098222,
-235.350050000001));
#215544=CARTESIAN_POINT('Ctrl Pts',(26.3891388204284,-61.3131722991992,
-235.35005));
#215545=CARTESIAN_POINT('Ctrl Pts',(26.8144498855472,-62.3225830053421,
-234.875056610216));
#215546=CARTESIAN_POINT('Ctrl Pts',(26.6353007694942,-61.9157019040657,
-235.350050000004));
#215547=CARTESIAN_POINT('Ctrl Pts',(26.3731447836042,-61.3202661527697,
-235.35005));
#215548=CARTESIAN_POINT('Ctrl Pts',(26.7749796776064,-62.3432491826028,
-234.871626009621));
#215549=CARTESIAN_POINT('Ctrl Pts',(26.5991763051683,-61.9344632905112,
-235.350049999996));
#215550=CARTESIAN_POINT('Ctrl Pts',(26.341052548261,-61.3342311248494,-235.35005));
#215551=CARTESIAN_POINT('Ctrl Pts',(26.7581168332245,-62.3505983495205,
-234.871489925227));
#215552=CARTESIAN_POINT('Ctrl Pts',(26.5826449857937,-61.9416583310242,
-235.350050000003));
#215553=CARTESIAN_POINT('Ctrl Pts',(26.324963993434,-61.3411228649431,-235.35005));
#215554=CARTESIAN_POINT('Ctrl Pts',(26.7067367940551,-62.3734047916896,
-234.870670602159));
#215555=CARTESIAN_POINT('Ctrl Pts',(26.5326026130778,-61.9637882105777,
-235.350049999995));
#215556=CARTESIAN_POINT('Ctrl Pts',(26.2766869482483,-61.3617737493097,
-235.35005));
#215557=CARTESIAN_POINT('Ctrl Pts',(26.6716855174712,-62.3892096482857,
-234.8697429112));
#215558=CARTESIAN_POINT('Ctrl Pts',(26.4987789702316,-61.9789513787255,
-235.350049999998));
#215559=CARTESIAN_POINT('Ctrl Pts',(26.2444517981386,-61.3754399401447,
-235.35005));
#215560=CARTESIAN_POINT('Ctrl Pts',(26.5986640911394,-62.42280983363,-234.866517684792));
#215561=CARTESIAN_POINT('Ctrl Pts',(26.4294605199159,-62.0106164563224,
-235.350050000002));
#215562=CARTESIAN_POINT('Ctrl Pts',(26.1797908377429,-61.4023344685258,
-235.35005));
#215563=CARTESIAN_POINT('Ctrl Pts',(26.5610650568712,-62.4403313244474,
-234.864401737979));
#215564=CARTESIAN_POINT('Ctrl Pts',(26.3941508721394,-62.0269255784061,
-235.350050000003));
#215565=CARTESIAN_POINT('Ctrl Pts',(26.1473795281051,-61.4155758832315,
-235.35005));
#215566=CARTESIAN_POINT('Ctrl Pts',(26.4769925160474,-62.4815712743123,
-234.855888967911));
#215567=CARTESIAN_POINT('Ctrl Pts',(26.3184924821692,-62.0639340677589,
-235.350049999997));
#215568=CARTESIAN_POINT('Ctrl Pts',(26.0821804763413,-61.4411000467081,
-235.35005));
#215569=CARTESIAN_POINT('Ctrl Pts',(26.4301202849281,-62.5051629518579,
-234.849380577206));
#215570=CARTESIAN_POINT('Ctrl Pts',(26.2778418840239,-62.0845719406398,
-235.350050000008));
#215571=CARTESIAN_POINT('Ctrl Pts',(26.0493312864126,-61.4532499966124,
-235.350050000001));
#215572=CARTESIAN_POINT('Ctrl Pts',(26.3002982623345,-62.5629144928957,
-234.836228995997));
#215573=CARTESIAN_POINT('Ctrl Pts',(26.16131341017,-62.1365284085563,-235.350049999985));
#215574=CARTESIAN_POINT('Ctrl Pts',(25.9501566901715,-61.4879342004266,
-235.350050000001));
#215575=CARTESIAN_POINT('Ctrl Pts',(26.2295575379109,-62.5856716502435,
-234.836161050761));
#215576=CARTESIAN_POINT('Ctrl Pts',(26.0922007161114,-62.1587949666646,
-235.350049999986));
#215577=CARTESIAN_POINT('Ctrl Pts',(25.8834819572284,-61.509419252042,-235.35005));
#215578=CARTESIAN_POINT('Ctrl Pts',(26.1240410793217,-62.6259950512244,
-234.826760990814));
#215579=CARTESIAN_POINT('Ctrl Pts',(25.9961215559071,-62.1956472548967,
-235.350050000004));
#215580=CARTESIAN_POINT('Ctrl Pts',(25.7996807895498,-61.534730893345,-235.35005));
#215581=CARTESIAN_POINT('Ctrl Pts',(26.1022708897306,-62.6344209388075,
-234.824528171248));
#215582=CARTESIAN_POINT('Ctrl Pts',(25.9764874702381,-62.203301257273,-235.35005000001));
#215583=CARTESIAN_POINT('Ctrl Pts',(25.7828903569215,-61.5396828918313,
-235.35005));
#215584=CARTESIAN_POINT('Ctrl Pts',(26.0564405135317,-62.6525017477888,
-234.818855409686));
#215585=CARTESIAN_POINT('Ctrl Pts',(25.9358759255667,-62.2195777671254,
-235.35004999999));
#215586=CARTESIAN_POINT('Ctrl Pts',(25.7492255098059,-61.5492800686396,
-235.35005));
#215587=CARTESIAN_POINT('Ctrl Pts',(26.031750683035,-62.662585347949,-234.815081952429));
#215588=CARTESIAN_POINT('Ctrl Pts',(25.9145289583069,-62.2285531296847,
-235.350050000002));
#215589=CARTESIAN_POINT('Ctrl Pts',(25.7323477164287,-61.5539129022783,
-235.35005));
#215590=CARTESIAN_POINT('Ctrl Pts',(25.9599138929427,-62.6902172126436,
-234.80493035963));
#215591=CARTESIAN_POINT('Ctrl Pts',(25.8516066550585,-62.253415598874,-235.350049999996));
#215592=CARTESIAN_POINT('Ctrl Pts',(25.6815605387409,-61.5672495175189,
-235.35005));
#215593=CARTESIAN_POINT('Ctrl Pts',(25.9137933010533,-62.7061668420416,
-234.799088724657));
#215594=CARTESIAN_POINT('Ctrl Pts',(25.8105734511642,-62.2679937524898,
-235.350050000001));
#215595=CARTESIAN_POINT('Ctrl Pts',(25.6474983161402,-61.5754339876196,
-235.35005));
#215596=CARTESIAN_POINT('Ctrl Pts',(25.8266199989672,-62.7334072231405,
-234.790014747185));
#215597=CARTESIAN_POINT('Ctrl Pts',(25.731270624734,-62.2932633630891,-235.350049999999));
#215598=CARTESIAN_POINT('Ctrl Pts',(25.5791807904238,-61.5908730316921,
-235.35005));
#215599=CARTESIAN_POINT('Ctrl Pts',(25.7854381790837,-62.7449250317595,
-234.786716919552));
#215600=CARTESIAN_POINT('Ctrl Pts',(25.6929582970791,-62.3041171818887,
-235.350050000007));
#215601=CARTESIAN_POINT('Ctrl Pts',(25.5449390466137,-61.5981933980485,
-235.35005));
#215602=CARTESIAN_POINT('Ctrl Pts',(25.6958511722237,-62.7713816730825,
-234.776088976192));
#215603=CARTESIAN_POINT('Ctrl Pts',(25.6120006673653,-62.3287974984487,
-235.350049999993));
#215604=CARTESIAN_POINT('Ctrl Pts',(25.4762602753847,-61.6118947761917,
-235.35005));
#215605=CARTESIAN_POINT('Ctrl Pts',(25.6487938388611,-62.7853359206876,
-234.769502178759));
#215606=CARTESIAN_POINT('Ctrl Pts',(25.5700865112867,-62.3418086817178,
-235.350049999994));
#215607=CARTESIAN_POINT('Ctrl Pts',(25.441793602875,-61.6182439225594,-235.35005));
#215608=CARTESIAN_POINT('Ctrl Pts',(25.5505975885659,-62.8135734388872,
-234.753817940405));
#215609=CARTESIAN_POINT('Ctrl Pts',(25.4836760281485,-62.3684020864125,
-235.350050000006));
#215610=CARTESIAN_POINT('Ctrl Pts',(25.3727171465013,-61.6295518156141,
-235.35005));
#215611=CARTESIAN_POINT('Ctrl Pts',(25.502761747094,-62.8258892566092,-234.746546441306));
#215612=CARTESIAN_POINT('Ctrl Pts',(25.4411294647291,-62.3802077997125,
-235.350050000011));
#215613=CARTESIAN_POINT('Ctrl Pts',(25.3381059806223,-61.6345074287981,
-235.35005));
#215614=CARTESIAN_POINT('Ctrl Pts',(25.410643515485,-62.8470998764316,-234.733871650706));
#215615=CARTESIAN_POINT('Ctrl Pts',(25.3580077967086,-62.4008089763377,
-235.350049999988));
#215616=CARTESIAN_POINT('Ctrl Pts',(25.2687752030225,-61.6433803535082,
-235.35005));
#215617=CARTESIAN_POINT('Ctrl Pts',(25.3675251946155,-62.8554316040649,
-234.729139544076));
#215618=CARTESIAN_POINT('Ctrl Pts',(25.3181720881824,-62.409019950067,-235.350049999987));
#215619=CARTESIAN_POINT('Ctrl Pts',(25.2340567625657,-61.647308878831,-235.35005));
#215620=CARTESIAN_POINT('Ctrl Pts',(25.2771548984166,-62.8731739889417,
-234.717216506631));
#215621=CARTESIAN_POINT('Ctrl Pts',(25.2358632414137,-62.4266817100688,
-235.350050000013));
#215622=CARTESIAN_POINT('Ctrl Pts',(25.1645355171699,-61.6543581913618,
-235.35005));
#215623=CARTESIAN_POINT('Ctrl Pts',(25.2265358924182,-62.8840570732042,
-234.708065708185));
#215624=CARTESIAN_POINT('Ctrl Pts',(25.1912608438073,-62.4376905785948,
-235.350049999998));
#215625=CARTESIAN_POINT('Ctrl Pts',(25.1297211288812,-61.6573680755603,
-235.350050000001));
#215626=CARTESIAN_POINT('Ctrl Pts',(25.0487310537601,-62.917065316072,-234.677362912941));
#215627=CARTESIAN_POINT('Ctrl Pts',(25.0325598226048,-62.4721861510005,
-235.350050000007));
#215628=CARTESIAN_POINT('Ctrl Pts',(25.0041328693965,-61.6657481959627,
-235.350050000001));
#215629=CARTESIAN_POINT('Ctrl Pts',(24.9305963304298,-62.9289465193204,
-234.661234678933));
#215630=CARTESIAN_POINT('Ctrl Pts',(24.9242386165759,-62.4861572040979,
-235.350050000174));
#215631=CARTESIAN_POINT('Ctrl Pts',(24.9129804805611,-61.6674900659302,
-235.350049999997));
#215632=CARTESIAN_POINT('Ctrl Pts',(24.8442395506814,-62.9300850046651,
-234.661061515112));
#215633=CARTESIAN_POINT('Ctrl Pts',(24.8365458571667,-62.4875347473503,
-235.350049999113));
#215634=CARTESIAN_POINT('Ctrl Pts',(24.8217422065604,-61.6684388365039,
-235.350050000008));
#215635=CARTESIAN_POINT('',(25.0347190704488,-62.9143710634153,-234.678897682319));
#215636=CARTESIAN_POINT('',(24.9899997248189,-61.6649665253882,-235.35005));
#215637=CARTESIAN_POINT('Origin',(24.9899997248189,-61.6649665253882,-233.85005));
#215638=CARTESIAN_POINT('Ctrl Pts',(26.5926469327273,-61.2115127003622,
-235.35005));
#215639=CARTESIAN_POINT('Ctrl Pts',(26.5307857619515,-61.2444027172302,
-235.35005));
#215640=CARTESIAN_POINT('Ctrl Pts',(26.4686189787879,-61.276660497005,-235.35005));
#215641=CARTESIAN_POINT('Ctrl Pts',(26.4050352616636,-61.3058697511684,
-235.35005));
#215642=CARTESIAN_POINT('Ctrl Pts',(26.3891387194065,-61.3131723462998,
-235.35005));
#215643=CARTESIAN_POINT('Ctrl Pts',(26.3731446870696,-61.3202661956383,
-235.35005));
#215644=CARTESIAN_POINT('Ctrl Pts',(26.3570986663275,-61.327248639717,-235.35005));
#215645=CARTESIAN_POINT('Ctrl Pts',(26.3410524626378,-61.3342311634055,
-235.35005));
#215646=CARTESIAN_POINT('Ctrl Pts',(26.3249639130519,-61.3411229008801,
-235.35005));
#215647=CARTESIAN_POINT('Ctrl Pts',(26.3088716457128,-61.3480064946411,
-235.35005));
#215648=CARTESIAN_POINT('Ctrl Pts',(26.2766866901153,-61.3617738622147,
-235.35005));
#215649=CARTESIAN_POINT('Ctrl Pts',(26.2444515824955,-61.3754400331407,
-235.35005));
#215650=CARTESIAN_POINT('Ctrl Pts',(26.212121319506,-61.3888872080985,-235.35005));
#215651=CARTESIAN_POINT('Ctrl Pts',(26.1797907095899,-61.4023345273539,
-235.35005));
#215652=CARTESIAN_POINT('Ctrl Pts',(26.1473794430666,-61.4155759233805,
-235.350049999999));
#215653=CARTESIAN_POINT('Ctrl Pts',(26.1147800051491,-61.4283379724439,
-235.350049999999));
#215654=CARTESIAN_POINT('Ctrl Pts',(26.0821804798061,-61.4411000557326,
-235.35005));
#215655=CARTESIAN_POINT('Ctrl Pts',(26.0493313347784,-61.4532499920652,
-235.350050000001));
#215656=CARTESIAN_POINT('Ctrl Pts',(26.0162730923146,-61.464811411177,-235.350050000001));
#215657=CARTESIAN_POINT('Ctrl Pts',(25.9501574057461,-61.4879339701914,
-235.350050000001));
#215658=CARTESIAN_POINT('Ctrl Pts',(25.8834830443658,-61.5094189499966,
-235.35005));
#215659=CARTESIAN_POINT('Ctrl Pts',(25.816441032895,-61.5296685975531,-235.35005));
#215660=CARTESIAN_POINT('Ctrl Pts',(25.799680801709,-61.5347309273823,-235.35005));
#215661=CARTESIAN_POINT('Ctrl Pts',(25.7828903692931,-61.5396829277202,
-235.35005));
#215662=CARTESIAN_POINT('Ctrl Pts',(25.7660579441618,-61.5444815181131,
-235.35005));
#215663=CARTESIAN_POINT('Ctrl Pts',(25.7492255222735,-61.5492801075815,
-235.35005));
#215664=CARTESIAN_POINT('Ctrl Pts',(25.7323477287723,-61.5539129424998,
-235.35005));
#215665=CARTESIAN_POINT('Ctrl Pts',(25.7154186680902,-61.558358482165,-235.35005));
#215666=CARTESIAN_POINT('Ctrl Pts',(25.6815605534858,-61.5672495597203,
-235.35005));
#215667=CARTESIAN_POINT('Ctrl Pts',(25.6474983294595,-61.5754340306918,
-235.35005));
#215668=CARTESIAN_POINT('Ctrl Pts',(25.6133395630491,-61.5831535528751,
-235.35005));
#215669=CARTESIAN_POINT('Ctrl Pts',(25.5791808006497,-61.590873074152,-235.35005));
#215670=CARTESIAN_POINT('Ctrl Pts',(25.5449390551878,-61.5981934391817,
-235.35005));
#215671=CARTESIAN_POINT('Ctrl Pts',(25.510599668782,-61.6050441261316,-235.35005));
#215672=CARTESIAN_POINT('Ctrl Pts',(25.4762602802774,-61.6118948135003,
-235.35005));
#215673=CARTESIAN_POINT('Ctrl Pts',(25.4417936057803,-61.6182439572411,
-235.35005));
#215674=CARTESIAN_POINT('Ctrl Pts',(25.4072553797815,-61.6238979002003,
-235.35005));
#215675=CARTESIAN_POINT('Ctrl Pts',(25.3727171455055,-61.6295518445145,
-235.35005));
#215676=CARTESIAN_POINT('Ctrl Pts',(25.3381059777677,-61.6345074541881,
-235.35005));
#215677=CARTESIAN_POINT('Ctrl Pts',(25.3034405945236,-61.6389439122599,
-235.35005));
#215678=CARTESIAN_POINT('Ctrl Pts',(25.2687751967828,-61.6433803721869,
-235.35005));
#215679=CARTESIAN_POINT('Ctrl Pts',(25.234056754758,-61.6473088938803,-235.35005));
#215680=CARTESIAN_POINT('Ctrl Pts',(25.1992961409817,-61.6508335460814,
-235.35005));
#215681=CARTESIAN_POINT('Ctrl Pts',(25.1645355064627,-61.6543582003856,
-235.35005));
#215682=CARTESIAN_POINT('Ctrl Pts',(25.1297211167782,-61.6573680815383,
-235.350050000001));
#215683=CARTESIAN_POINT('Ctrl Pts',(25.0948355014582,-61.6596958899581,
-235.350050000001));
#215684=CARTESIAN_POINT('Ctrl Pts',(25.0599498590945,-61.6620237001823,
-235.350050000001));
#215685=CARTESIAN_POINT('Ctrl Pts',(25.0249976982331,-61.6637138708522,
-235.35005));
#215686=CARTESIAN_POINT('Ctrl Pts',(24.9899997248189,-61.6649665253882,
-235.35005));
#215687=CARTESIAN_POINT('Ctrl Pts',(25.0347190704488,-62.9143710634153,
-234.678897682319));
#215688=CARTESIAN_POINT('Ctrl Pts',(25.085638797075,-62.9079339622688,-234.685853660663));
#215689=CARTESIAN_POINT('Ctrl Pts',(25.1307592161118,-62.9007252008369,
-234.693073023235));
#215690=CARTESIAN_POINT('Ctrl Pts',(25.2129670148129,-62.8850210310273,
-234.708038516839));
#215691=CARTESIAN_POINT('Ctrl Pts',(25.2539844298917,-62.8766122328458,
-234.715332558096));
#215692=CARTESIAN_POINT('Ctrl Pts',(25.3485821128302,-62.8579473644628,
-234.728553576946));
#215693=CARTESIAN_POINT('Ctrl Pts',(25.3980516305474,-62.8481335841612,
-234.734457037752));
#215694=CARTESIAN_POINT('Ctrl Pts',(25.4895958658201,-62.8274748181031,
-234.746824327757));
#215695=CARTESIAN_POINT('Ctrl Pts',(25.533635925427,-62.8165570077274,-234.753066555306));
#215696=CARTESIAN_POINT('Ctrl Pts',(25.5975770701915,-62.7992049833544,
-234.762517770449));
#215697=CARTESIAN_POINT('Ctrl Pts',(25.6185393383981,-62.7932542900658,
-234.765682821134));
#215698=CARTESIAN_POINT('Ctrl Pts',(25.6443444802103,-62.7856261939461,
-234.769657441535));
#215699=CARTESIAN_POINT('Ctrl Pts',(25.6484523849535,-62.7843918496431,
-234.770299887365));
#215700=CARTESIAN_POINT('Ctrl Pts',(25.652628706954,-62.7831642653728,-234.770916217284));
#215701=CARTESIAN_POINT('Ctrl Pts',(25.6597400602254,-62.7811052939532,
-234.771918572547));
#215702=CARTESIAN_POINT('Ctrl Pts',(25.6693705433464,-62.7783833175895,
-234.773154508962));
#215703=CARTESIAN_POINT('Ctrl Pts',(25.7069387835634,-62.7677747710471,
-234.77779336624));
#215704=CARTESIAN_POINT('Ctrl Pts',(25.7545226931024,-62.7543762597918,
-234.78316547359));
#215705=CARTESIAN_POINT('Ctrl Pts',(25.833006557455,-62.730226116854,-234.791956884686));
#215706=CARTESIAN_POINT('Ctrl Pts',(25.8496500291877,-62.7250326332926,
-234.793818980751));
#215707=CARTESIAN_POINT('Ctrl Pts',(25.8760257651527,-62.7166320351824,
-234.796767845616));
#215708=CARTESIAN_POINT('Ctrl Pts',(25.8811350256815,-62.7149847988613,
-234.797339569667));
#215709=CARTESIAN_POINT('Ctrl Pts',(25.8921320345629,-62.7114127360742,
-234.79858954494));
#215710=CARTESIAN_POINT('Ctrl Pts',(25.9195496279942,-62.7024190863312,
-234.801742188854));
#215711=CARTESIAN_POINT('Ctrl Pts',(25.9682935210718,-62.6856232102758,
-234.807666299498));
#215712=CARTESIAN_POINT('Ctrl Pts',(26.0111347436968,-62.6696270999718,
-234.813286809008));
#215713=CARTESIAN_POINT('Ctrl Pts',(26.0432243998012,-62.6571545277768,
-234.81763517866));
#215714=CARTESIAN_POINT('Ctrl Pts',(26.053917370438,-62.6529155819281,-234.819106799797));
#215715=CARTESIAN_POINT('Ctrl Pts',(26.069946869197,-62.6464402766788,-234.821347478383));
#215716=CARTESIAN_POINT('Ctrl Pts',(26.0752878196045,-62.6442627279254,
-234.822099912391));
#215717=CARTESIAN_POINT('Ctrl Pts',(26.0859624874598,-62.6398716269047,
-234.823615862701));
#215718=CARTESIAN_POINT('Ctrl Pts',(26.0933426421007,-62.6368014947894,
-234.824674728087));
#215719=CARTESIAN_POINT('Ctrl Pts',(26.1097539748075,-62.629932182154,-234.827043269906));
#215720=CARTESIAN_POINT('Ctrl Pts',(26.127149009414,-62.623171180736,-234.828880694613));
#215721=CARTESIAN_POINT('Ctrl Pts',(26.1595790621099,-62.610935853299,-234.831550718551));
#215722=CARTESIAN_POINT('Ctrl Pts',(26.1773763976045,-62.6042947500805,
-234.83286420224));
#215723=CARTESIAN_POINT('Ctrl Pts',(26.2008584346582,-62.5956002463696,
-234.834358925386));
#215724=CARTESIAN_POINT('Ctrl Pts',(26.2114956462486,-62.5916697030229,
-234.834991447915));
#215725=CARTESIAN_POINT('Ctrl Pts',(26.2187133945384,-62.589003865943,-234.835411335577));
#215726=CARTESIAN_POINT('Ctrl Pts',(26.221061526754,-62.5881368485382,-234.835546593076));
#215727=CARTESIAN_POINT('Ctrl Pts',(26.2665871887173,-62.5713334384756,
-234.838084045232));
#215728=CARTESIAN_POINT('Ctrl Pts',(26.2972309978204,-62.5596102150849,
-234.83984397804));
#215729=CARTESIAN_POINT('Ctrl Pts',(26.3294801453437,-62.5471044172847,
-234.841740506921));
#215730=CARTESIAN_POINT('Ctrl Pts',(26.3379381999395,-62.5437783530276,
-234.842248788159));
#215731=CARTESIAN_POINT('Ctrl Pts',(26.347189205665,-62.5401070985879,-234.842825367435));
#215732=CARTESIAN_POINT('Ctrl Pts',(26.3509546787848,-62.5386010471326,
-234.843067196427));
#215733=CARTESIAN_POINT('Ctrl Pts',(26.3534261833428,-62.5375977021866,
-234.84323933445));
#215734=CARTESIAN_POINT('Ctrl Pts',(26.3547859197358,-62.5370411263274,
-234.84333860625));
#215735=CARTESIAN_POINT('Ctrl Pts',(26.3541676061889,-62.5373072030569,
-234.84327989792));
#215736=CARTESIAN_POINT('Ctrl Pts',(26.3680817365266,-62.5314220268562,
-234.844492646197));
#215737=CARTESIAN_POINT('Ctrl Pts',(26.3844680819482,-62.5242262989439,
-234.846153717548));
#215738=CARTESIAN_POINT('Ctrl Pts',(26.4155766034196,-62.5099916470183,
-234.849519933896));
#215739=CARTESIAN_POINT('Ctrl Pts',(26.427040628927,-62.5046685272578,-234.850787774233));
#215740=CARTESIAN_POINT('Ctrl Pts',(26.446033018801,-62.4956922588524,-234.852908187069));
#215741=CARTESIAN_POINT('Ctrl Pts',(26.4526640361999,-62.4925343615046,
-234.853651433403));
#215742=CARTESIAN_POINT('Ctrl Pts',(26.4665640540616,-62.4858586717679,
-234.85521081018));
#215743=CARTESIAN_POINT('Ctrl Pts',(26.4749973336765,-62.4817726451067,
-234.856157358164));
#215744=CARTESIAN_POINT('Ctrl Pts',(26.5072332853527,-62.466039545056,-234.85976813296));
#215745=CARTESIAN_POINT('Ctrl Pts',(26.5309786196337,-62.4543565533579,
-234.862139767001));
#215746=CARTESIAN_POINT('Ctrl Pts',(26.5624741628734,-62.4390041084162,
-234.864921739368));
#215747=CARTESIAN_POINT('Ctrl Pts',(26.5722895346858,-62.4342454913545,
-234.865719817041));
#215748=CARTESIAN_POINT('Ctrl Pts',(26.5859073445181,-62.4277104752076,
-234.866723063878));
#215749=CARTESIAN_POINT('Ctrl Pts',(26.5902627632415,-62.4256323661044,
-234.867025167878));
#215750=CARTESIAN_POINT('Ctrl Pts',(26.5985962243179,-62.4216846633567,
-234.867564752653));
#215751=CARTESIAN_POINT('Ctrl Pts',(26.6015303784991,-62.4203009685482,
-234.867745656129));
#215752=CARTESIAN_POINT('Ctrl Pts',(26.6449954022435,-62.400069202433,-234.870101374292));
#215753=CARTESIAN_POINT('Ctrl Pts',(26.688860555794,-62.3801117723142,-234.871572851604));
#215754=CARTESIAN_POINT('Ctrl Pts',(26.7775907302196,-62.3406277132562,
-234.873133640282));
#215755=CARTESIAN_POINT('Ctrl Pts',(26.8144719921791,-62.3216949396143,
-234.876263859502));
#215756=CARTESIAN_POINT('Ctrl Pts',(26.8975997530553,-62.2706957884666,
-234.888648102498));
#215757=CARTESIAN_POINT('Ctrl Pts',(26.9407411513415,-62.2442733553417,
-234.893662446297));
#215758=CARTESIAN_POINT('Ctrl Pts',(27.023757211477,-62.1938596418189,-234.901335578495));
#215759=CARTESIAN_POINT('Ctrl Pts',(27.06303730244,-62.1702331394993,-234.903994366895));
#215760=CARTESIAN_POINT('Ctrl Pts',(27.0930165135311,-62.1526330725429,
-234.905475377596));
#215761=CARTESIAN_POINT('Ctrl Pts',(25.0347190704499,-62.9143710634155,
-234.678897682318));
#215762=CARTESIAN_POINT('Ctrl Pts',(25.0188032481045,-62.4697021984296,
-235.35005));
#215763=CARTESIAN_POINT('Ctrl Pts',(24.9899997248189,-61.6649665253882,
-235.35005));
#215764=CARTESIAN_POINT('Ctrl Pts',(23.6367128243542,-62.9652114948589,
-234.677688363322));
#215765=CARTESIAN_POINT('Ctrl Pts',(23.6213321581711,-62.5206566084218,
-235.350050000019));
#215766=CARTESIAN_POINT('Ctrl Pts',(23.5944744924679,-61.7149158997446,
-235.35005));
#215767=CARTESIAN_POINT('Ctrl Pts',(22.2385723540716,-63.0117706699204,
-234.676581567471));
#215768=CARTESIAN_POINT('Ctrl Pts',(22.2241440176956,-62.567306445692,-235.350049999981));
#215769=CARTESIAN_POINT('Ctrl Pts',(22.1988114399884,-61.7606622187164,
-235.35005));
#215770=CARTESIAN_POINT('Ctrl Pts',(20.8402921969906,-63.0540783161444,
-234.675571538939));
#215771=CARTESIAN_POINT('Ctrl Pts',(20.8270581434285,-62.6096929286678,
-235.35005));
#215772=CARTESIAN_POINT('Ctrl Pts',(20.8030114294341,-61.8022299494809,
-235.35005));
#215773=CARTESIAN_POINT('',(20.8402919657626,-63.0540783750575,-234.675571454956));
#215774=CARTESIAN_POINT('',(20.803011429434,-61.8022299494809,-235.35005));
#215775=CARTESIAN_POINT('Origin',(20.803011429434,-61.802229949481,-233.85005));
#215776=CARTESIAN_POINT('Origin',(0.0402464096705391,635.45788043407,-235.35005));
#215777=CARTESIAN_POINT('Origin',(0.0417395060045145,624.033047422002,-250.70813398415));
#215778=CARTESIAN_POINT('Ctrl Pts',(20.9272939729598,-63.0388412169436,
-234.6925317176));
#215779=CARTESIAN_POINT('Ctrl Pts',(20.9003239325236,-62.593292071215,-235.350055395714));
#215780=CARTESIAN_POINT('Ctrl Pts',(20.8522739306831,-61.8000205942923,
-235.350049999965));
#215781=CARTESIAN_POINT('Ctrl Pts',(20.5781346200028,-63.1054079859869,
-234.625170203823));
#215782=CARTESIAN_POINT('Ctrl Pts',(20.6028008281919,-62.6639924158116,
-235.350056035508));
#215783=CARTESIAN_POINT('Ctrl Pts',(20.6549442779816,-61.8117755329686,
-235.350049999962));
#215784=CARTESIAN_POINT('Ctrl Pts',(20.242946602916,-63.1075402490427,-234.546724224386));
#215785=CARTESIAN_POINT('Ctrl Pts',(20.3103268001138,-62.6871623715535,
-235.35005680618));
#215786=CARTESIAN_POINT('Ctrl Pts',(20.4609420978131,-61.7877616583069,
-235.350049999958));
#215787=CARTESIAN_POINT('Ctrl Pts',(19.919830853961,-63.0620777407187,-234.460509579399));
#215788=CARTESIAN_POINT('Ctrl Pts',(20.0212058153521,-62.6789324639497,
-235.350057690633));
#215789=CARTESIAN_POINT('Ctrl Pts',(20.2703537543378,-61.7374827788075,
-235.350049999953));
#215790=CARTESIAN_POINT('',(20.00087676599,-63.0723813030746,-234.482033943277));
#215791=CARTESIAN_POINT('',(20.3180691938068,-61.7495111937247,-235.35005));
#215792=CARTESIAN_POINT('Origin',(20.3180691938068,-61.7495111937247,-233.85005));
#215793=CARTESIAN_POINT('Ctrl Pts',(20.803011429434,-61.8022299494809,-235.35005));
#215794=CARTESIAN_POINT('Ctrl Pts',(20.6389224043824,-61.8071166154417,
-235.35005));
#215795=CARTESIAN_POINT('Ctrl Pts',(20.4774719299468,-61.7877321350851,
-235.35005));
#215796=CARTESIAN_POINT('Ctrl Pts',(20.3180691938068,-61.7495111937247,
-235.35005));
#215797=CARTESIAN_POINT('Ctrl Pts',(20.0008767612649,-63.072381322781,-234.482033952692));
#215798=CARTESIAN_POINT('Ctrl Pts',(20.0757818263204,-63.0809990670768,
-234.501590108694));
#215799=CARTESIAN_POINT('Ctrl Pts',(20.1499241690099,-63.0867716849007,
-234.520358077193));
#215800=CARTESIAN_POINT('Ctrl Pts',(20.2230384024983,-63.0899033965466,
-234.53828908067));
#215801=CARTESIAN_POINT('Ctrl Pts',(20.2970171665463,-63.0930721387444,
-234.556432107166));
#215802=CARTESIAN_POINT('Ctrl Pts',(20.3699430474527,-63.0935377434988,
-234.573718420067));
#215803=CARTESIAN_POINT('Ctrl Pts',(20.4415762107852,-63.0915317581419,
-234.590133855307));
#215804=CARTESIAN_POINT('Ctrl Pts',(20.5148301934923,-63.0894803840323,
-234.606920717051));
#215805=CARTESIAN_POINT('Ctrl Pts',(20.586732029596,-63.0848449037923,-234.622797043541));
#215806=CARTESIAN_POINT('Ctrl Pts',(20.6570663042979,-63.0778846196563,
-234.637782820744));
#215807=CARTESIAN_POINT('Ctrl Pts',(20.7194133551344,-63.0717147516836,
-234.651066799531));
#215808=CARTESIAN_POINT('Ctrl Pts',(20.7805292610771,-63.0637185342414,
-234.663651683389));
#215809=CARTESIAN_POINT('Ctrl Pts',(20.8402917354589,-63.0540784607098,
-234.675571320208));
#215810=CARTESIAN_POINT('Ctrl Pts',(20.0002454535025,-63.0750142297972,
-234.47617280861));
#215811=CARTESIAN_POINT('Ctrl Pts',(20.0938415017253,-62.6846662779265,
-235.35005));
#215812=CARTESIAN_POINT('Ctrl Pts',(20.3180691938068,-61.7495111937247,
-235.35005));
#215813=CARTESIAN_POINT('Ctrl Pts',(19.2551174895925,-62.8664467612893,
-234.539479091859));
#215814=CARTESIAN_POINT('Ctrl Pts',(19.3413406300525,-62.4544294433442,
-235.350049999953));
#215815=CARTESIAN_POINT('Ctrl Pts',(19.4874388572759,-61.5503460219505,
-235.35005));
#215816=CARTESIAN_POINT('Ctrl Pts',(18.5025522393628,-62.7270802386455,
-234.590416060416));
#215817=CARTESIAN_POINT('Ctrl Pts',(18.5599245998347,-62.2978562023724,
-235.350049999989));
#215818=CARTESIAN_POINT('Ctrl Pts',(18.6516615360795,-61.4277914392832,
-235.35005));
#215819=CARTESIAN_POINT('Ctrl Pts',(16.981042115573,-62.595164303197,-234.672122377017));
#215820=CARTESIAN_POINT('Ctrl Pts',(16.9850135818407,-62.1499515126842,
-235.350050000011));
#215821=CARTESIAN_POINT('Ctrl Pts',(16.9698436721481,-61.3371563394037,
-235.35005));
#215822=CARTESIAN_POINT('Ctrl Pts',(16.2106145315025,-62.6026718111486,
-234.703184254722));
#215823=CARTESIAN_POINT('Ctrl Pts',(16.1826608962456,-62.1548361758855,
-235.350049999952));
#215824=CARTESIAN_POINT('Ctrl Pts',(16.121735346724,-61.369283189915,-235.35005));
#215825=CARTESIAN_POINT('Ctrl Pts',(15.0509341311275,-62.736562693307,-234.736945141873));
#215826=CARTESIAN_POINT('Ctrl Pts',(14.9766556245768,-62.2929910538471,
-235.350050000024));
#215827=CARTESIAN_POINT('Ctrl Pts',(14.8481785970025,-61.5432262204531,
-235.35005));
#215828=CARTESIAN_POINT('Ctrl Pts',(14.6645397729193,-62.8015403926739,
-234.745992774078));
#215829=CARTESIAN_POINT('Ctrl Pts',(14.5754142156998,-62.3603004171988,
-235.350050000024));
#215830=CARTESIAN_POINT('Ctrl Pts',(14.4244572553949,-61.622006959983,-235.35005));
#215831=CARTESIAN_POINT('Ctrl Pts',(14.254950802522,-62.8933063624506,-234.753437327716));
#215832=CARTESIAN_POINT('Ctrl Pts',(14.1497802084409,-62.455665562112,-235.350049999998));
#215833=CARTESIAN_POINT('Ctrl Pts',(13.9751463716102,-61.7290008746058,
-235.35005));
#215834=CARTESIAN_POINT('Ctrl Pts',(14.2240132142558,-62.9018295132189,
-234.751997072706));
#215835=CARTESIAN_POINT('Ctrl Pts',(14.120632865605,-62.4638031966455,-235.350050000002));
#215836=CARTESIAN_POINT('Ctrl Pts',(13.9487177749326,-61.7353325867798,
-235.35005));
#215837=CARTESIAN_POINT('Ctrl Pts',(14.1654272334655,-62.9170176450018,
-234.750024084914));
#215838=CARTESIAN_POINT('Ctrl Pts',(14.0643317181977,-62.4785194469356,
-235.350049999999));
#215839=CARTESIAN_POINT('Ctrl Pts',(13.8958479018872,-61.7476653413416,
-235.35005));
#215840=CARTESIAN_POINT('Ctrl Pts',(14.1361228513778,-62.9244932940189,
-234.749035483871));
#215841=CARTESIAN_POINT('Ctrl Pts',(14.0361704849244,-62.4857653670867,
-235.35005));
#215842=CARTESIAN_POINT('Ctrl Pts',(13.8694088478247,-61.7537243383813,
-235.35005));
#215843=CARTESIAN_POINT('Ctrl Pts',(14.0481763635734,-62.9465655811834,
-234.746063719071));
#215844=CARTESIAN_POINT('Ctrl Pts',(13.9516379184633,-62.50717186034,-235.350049999999));
#215845=CARTESIAN_POINT('Ctrl Pts',(13.7900793792485,-61.771580394972,-235.35005));
#215846=CARTESIAN_POINT('Ctrl Pts',(13.9895006559527,-62.9608076271989,
-234.744074583615));
#215847=CARTESIAN_POINT('Ctrl Pts',(13.8952521434001,-62.5209918829364,
-235.350050000002));
#215848=CARTESIAN_POINT('Ctrl Pts',(13.7371766585364,-61.7830565245145,
-235.35005));
#215849=CARTESIAN_POINT('Ctrl Pts',(13.8133459471977,-63.0021201512081,
-234.738086226961));
#215850=CARTESIAN_POINT('Ctrl Pts',(13.7259015486268,-62.5611319850931,
-235.350049999995));
#215851=CARTESIAN_POINT('Ctrl Pts',(13.5784196345718,-61.8162106597038,
-235.35005));
#215852=CARTESIAN_POINT('Ctrl Pts',(13.6957382843772,-63.0277772664849,
-234.734066004735));
#215853=CARTESIAN_POINT('Ctrl Pts',(13.6128816245493,-62.5860948115319,
-235.350050000005));
#215854=CARTESIAN_POINT('Ctrl Pts',(13.4725164724631,-61.8366144889431,
-235.35005));
#215855=CARTESIAN_POINT('Ctrl Pts',(13.3424531489291,-63.0991349765239,
-234.721945421981));
#215856=CARTESIAN_POINT('Ctrl Pts',(13.2730684458465,-62.6557423796767,
-235.350049999991));
#215857=CARTESIAN_POINT('Ctrl Pts',(13.154614345307,-61.8928021529216,-235.35005));
#215858=CARTESIAN_POINT('Ctrl Pts',(13.1063157328584,-63.1392203334766,
-234.713787004588));
#215859=CARTESIAN_POINT('Ctrl Pts',(13.0460848802442,-62.6950332686297,
-235.350050000015));
#215860=CARTESIAN_POINT('Ctrl Pts',(12.9424227890118,-61.9235634536356,
-235.35005));
#215861=CARTESIAN_POINT('Ctrl Pts',(11.9231858767189,-63.3028113134546,
-234.672904284763));
#215862=CARTESIAN_POINT('Ctrl Pts',(11.9024438740355,-62.8576130316748,
-235.35004999994));
#215863=CARTESIAN_POINT('Ctrl Pts',(11.880215388165,-62.0447815017487,-235.35005));
#215864=CARTESIAN_POINT('Ctrl Pts',(10.9664919615506,-63.3177886529725,
-234.639295809699));
#215865=CARTESIAN_POINT('Ctrl Pts',(10.9815452295666,-62.8759003715857,
-235.350049999988));
#215866=CARTESIAN_POINT('Ctrl Pts',(11.0264981771774,-62.0387113664218,
-235.35005));
#215867=CARTESIAN_POINT('Ctrl Pts',(9.76047598411976,-63.1848698641477,
-234.598624589264));
#215868=CARTESIAN_POINT('Ctrl Pts',(9.82464543906513,-62.7568110742575,
-235.350050000003));
#215869=CARTESIAN_POINT('Ctrl Pts',(9.9542943769832,-61.8992361752613,-235.35005));
#215870=CARTESIAN_POINT('Ctrl Pts',(9.51868087246522,-63.1506217143349,
-234.590521575213));
#215871=CARTESIAN_POINT('Ctrl Pts',(9.59134079921566,-62.7255327835753,
-235.350049999985));
#215872=CARTESIAN_POINT('Ctrl Pts',(9.73959722556094,-61.864654779516,-235.35005));
#215873=CARTESIAN_POINT('Ctrl Pts',(9.1552088910392,-63.0872746466928,-234.578477639126));
#215874=CARTESIAN_POINT('Ctrl Pts',(9.24074450396521,-62.6672453065271,
-235.350050000007));
#215875=CARTESIAN_POINT('Ctrl Pts',(9.41715218707317,-61.8023691603538,
-235.35005));
#215876=CARTESIAN_POINT('Ctrl Pts',(9.03392287836112,-63.0641627844476,
-234.574481372606));
#215877=CARTESIAN_POINT('Ctrl Pts',(9.12361630525094,-62.6458843797158,
-235.350049999991));
#215878=CARTESIAN_POINT('Ctrl Pts',(9.30960392193887,-61.7798708192789,
-235.35005));
#215879=CARTESIAN_POINT('Ctrl Pts',(8.88216619994883,-63.0327225023551,
-234.569514805913));
#215880=CARTESIAN_POINT('Ctrl Pts',(8.97711320863088,-62.6167596520512,
-235.350050000002));
#215881=CARTESIAN_POINT('Ctrl Pts',(9.17508354831589,-61.7495301015501,
-235.35005));
#215882=CARTESIAN_POINT('Ctrl Pts',(8.85180758078057,-63.0263069459882,
-234.568522933821));
#215883=CARTESIAN_POINT('Ctrl Pts',(8.9477835000243,-62.6108083839332,-235.350050000001));
#215884=CARTESIAN_POINT('Ctrl Pts',(9.14817522070154,-61.7433510482094,
-235.35005));
#215885=CARTESIAN_POINT('Ctrl Pts',(8.8062587329115,-63.0164912333735,-234.567037380941));
#215886=CARTESIAN_POINT('Ctrl Pts',(8.90377970937159,-62.6016978624724,
-235.35005));
#215887=CARTESIAN_POINT('Ctrl Pts',(9.10780631361874,-61.7339151558469,
-235.35005));
#215888=CARTESIAN_POINT('Ctrl Pts',(8.78987315391243,-63.013132382654,-234.566105822447));
#215889=CARTESIAN_POINT('Ctrl Pts',(8.88825779030318,-62.5987600395459,
-235.350050000003));
#215890=CARTESIAN_POINT('Ctrl Pts',(9.09434840397257,-61.7307279424447,
-235.35005));
#215891=CARTESIAN_POINT('Ctrl Pts',(8.7656898169978,-63.0067092336391,-234.567370926259));
#215892=CARTESIAN_POINT('Ctrl Pts',(8.86330821605581,-62.5918614567545,
-235.350049999997));
#215893=CARTESIAN_POINT('Ctrl Pts',(9.06743306640637,-61.7243660786321,
-235.35005));
#215894=CARTESIAN_POINT('Ctrl Pts',(8.75359794781792,-63.0035181040683,
-234.56800033754));
#215895=CARTESIAN_POINT('Ctrl Pts',(8.85083241058327,-62.5884344265496,
-235.350049999999));
#215896=CARTESIAN_POINT('Ctrl Pts',(9.05397622529392,-61.7212067312174,
-235.35005));
#215897=CARTESIAN_POINT('Ctrl Pts',(8.69313745814224,-62.9876644929304,
-234.571131795369));
#215898=CARTESIAN_POINT('Ctrl Pts',(8.78847489870271,-62.5714176461548,
-235.350050000005));
#215899=CARTESIAN_POINT('Ctrl Pts',(8.98669614980007,-61.7055177010037,
-235.35005));
#215900=CARTESIAN_POINT('Ctrl Pts',(8.64476611487728,-62.9753083012394,
-234.573587012594));
#215901=CARTESIAN_POINT('Ctrl Pts',(8.7385510630932,-62.5581533934216,-235.350050000003));
#215902=CARTESIAN_POINT('Ctrl Pts',(8.93288530505372,-61.6933111243076,
-235.35005));
#215903=CARTESIAN_POINT('Ctrl Pts',(8.20938920381546,-62.8670241015852,
-234.595245743017));
#215904=CARTESIAN_POINT('Ctrl Pts',(8.29080672382282,-62.4423929773204,
-235.350049999976));
#215905=CARTESIAN_POINT('Ctrl Pts',(8.4487057336385,-61.5865300359515,-235.35005));
#215906=CARTESIAN_POINT('Ctrl Pts',(7.82222359068918,-62.7915296928953,
-234.611394249339));
#215907=CARTESIAN_POINT('Ctrl Pts',(7.88989268115682,-62.3613610544617,
-235.350049999994));
#215908=CARTESIAN_POINT('Ctrl Pts',(8.01916095024903,-61.5134429064026,
-235.35005));
#215909=CARTESIAN_POINT('Ctrl Pts',(6.66116371746047,-62.6255181896041,
-234.651995705069));
#215910=CARTESIAN_POINT('Ctrl Pts',(6.69156996858306,-62.1840858314768,
-235.350050000012));
#215911=CARTESIAN_POINT('Ctrl Pts',(6.73293045659356,-61.3568710016287,
-235.35005));
#215912=CARTESIAN_POINT('Ctrl Pts',(5.88732128025216,-62.5951782831116,
-234.668619732153));
#215913=CARTESIAN_POINT('Ctrl Pts',(5.88578405769122,-62.150383637914,-235.350049999964));
#215914=CARTESIAN_POINT('Ctrl Pts',(5.87863226335204,-61.3356495997417,
-235.35005));
#215915=CARTESIAN_POINT('Ctrl Pts',(4.73022316785671,-62.6693442476172,
-234.680424870605));
#215916=CARTESIAN_POINT('Ctrl Pts',(4.68487052924521,-62.226315867779,-235.350050000018));
#215917=CARTESIAN_POINT('Ctrl Pts',(4.60187420700122,-61.426106672458,-235.35005));
#215918=CARTESIAN_POINT('Ctrl Pts',(4.34523442762013,-62.714083360949,-234.682140423453));
#215919=CARTESIAN_POINT('Ctrl Pts',(4.28518237892104,-62.2726127748062,
-235.350049999988));
#215920=CARTESIAN_POINT('Ctrl Pts',(4.1770740790426,-61.4767540523636,-235.35005));
#215921=CARTESIAN_POINT('Ctrl Pts',(3.76915274784454,-62.8120240257835,
-234.681325996944));
#215922=CARTESIAN_POINT('Ctrl Pts',(3.68781576212144,-62.3742400764792,
-235.350050000006));
#215923=CARTESIAN_POINT('Ctrl Pts',(3.54108358671642,-61.5842725312083,
-235.35005));
#215924=CARTESIAN_POINT('Ctrl Pts',(3.57736454720535,-62.8498101374656,
-234.680488798365));
#215925=CARTESIAN_POINT('Ctrl Pts',(3.48889544140117,-62.413503321465,-235.350049999997));
#215926=CARTESIAN_POINT('Ctrl Pts',(3.32928846564854,-61.6253723533426,
-235.35005));
#215927=CARTESIAN_POINT('Ctrl Pts',(3.29014195104425,-62.9143448304384,
-234.678356484935));
#215928=CARTESIAN_POINT('Ctrl Pts',(3.19114060354514,-62.4805904586232,
-235.350050000002));
#215929=CARTESIAN_POINT('Ctrl Pts',(3.01190491992465,-61.6950839540996,
-235.35005));
#215930=CARTESIAN_POINT('Ctrl Pts',(3.1944780537155,-62.9371661600342,-234.677499402921));
#215931=CARTESIAN_POINT('Ctrl Pts',(3.09195226458871,-62.5043289573996,
-235.350049999992));
#215932=CARTESIAN_POINT('Ctrl Pts',(2.90616195484145,-61.7196655152859,
-235.35005));
#215933=CARTESIAN_POINT('Ctrl Pts',(3.07500525353187,-62.9673499718945,
-234.676240441763));
#215934=CARTESIAN_POINT('Ctrl Pts',(2.96811329314043,-62.5357301121157,
-235.350050000002));
#215935=CARTESIAN_POINT('Ctrl Pts',(2.77404858885074,-61.7520964605576,
-235.35005));
#215936=CARTESIAN_POINT('Ctrl Pts',(3.05111608590414,-62.9734695946934,
-234.675979264585));
#215937=CARTESIAN_POINT('Ctrl Pts',(2.94334732448096,-62.5420981916043,
-235.350050000001));
#215938=CARTESIAN_POINT('Ctrl Pts',(2.74762918327784,-61.7586678648919,
-235.35005));
#215939=CARTESIAN_POINT('Ctrl Pts',(3.0152905878955,-62.9827737431109,-234.675573317217));
#215940=CARTESIAN_POINT('Ctrl Pts',(2.906208743664,-62.5517806373196,-235.350049999999));
#215941=CARTESIAN_POINT('Ctrl Pts',(2.70800499509792,-61.7686532835183,
-235.35005));
#215942=CARTESIAN_POINT('Ctrl Pts',(3.00335013472062,-62.98589591073,-234.675435637832));
#215943=CARTESIAN_POINT('Ctrl Pts',(2.89383036974431,-62.5550299942805,
-235.35005));
#215944=CARTESIAN_POINT('Ctrl Pts',(2.6947977524096,-61.7720031419126,-235.35005));
#215945=CARTESIAN_POINT('Ctrl Pts',(2.97947201822115,-62.9921818874314,
-234.675155533715));
#215946=CARTESIAN_POINT('Ctrl Pts',(2.8690767376369,-62.5615723327899,-235.35005));
#215947=CARTESIAN_POINT('Ctrl Pts',(2.66838491033016,-61.7787457138043,
-235.35005));
#215948=CARTESIAN_POINT('Ctrl Pts',(2.96304225688233,-62.9964242380372,
-234.675077639757));
#215949=CARTESIAN_POINT('Ctrl Pts',(2.85379759446374,-62.5655303634271,
-235.35005));
#215950=CARTESIAN_POINT('Ctrl Pts',(2.65517833661466,-61.7821130182165,
-235.35005));
#215951=CARTESIAN_POINT('Ctrl Pts',(2.88938127733355,-63.0153416312828,
-234.674574704412));
#215952=CARTESIAN_POINT('Ctrl Pts',(2.78287887281784,-62.5838153796612,
-235.350050000001));
#215953=CARTESIAN_POINT('Ctrl Pts',(2.58913846773959,-61.7987669810389,
-235.35005));
#215954=CARTESIAN_POINT('Ctrl Pts',(2.83042206824581,-63.0299995242519,
-234.674181109462));
#215955=CARTESIAN_POINT('Ctrl Pts',(2.72611963520325,-62.5979826576736,
-235.35005));
#215956=CARTESIAN_POINT('Ctrl Pts',(2.53629033417451,-61.8116666733557,
-235.35005));
#215957=CARTESIAN_POINT('Ctrl Pts',(2.29957200197046,-63.1576513891524,
-234.670723008053));
#215958=CARTESIAN_POINT('Ctrl Pts',(2.21477240222884,-62.721441734,-235.35005));
#215959=CARTESIAN_POINT('Ctrl Pts',(2.06051214976267,-61.9239829504865,
-235.35005));
#215960=CARTESIAN_POINT('Ctrl Pts',(1.82561741918027,-63.2408549075195,
-234.668259126929));
#215961=CARTESIAN_POINT('Ctrl Pts',(1.75845914439681,-62.8018876347933,
-235.350050000006));
#215962=CARTESIAN_POINT('Ctrl Pts',(1.63573306964857,-61.997098140329,-235.35005));
#215963=CARTESIAN_POINT('Ctrl Pts',(0.88215860141345,-63.34926053199,-234.664972573172));
#215964=CARTESIAN_POINT('Ctrl Pts',(0.849715125954841,-62.9067900502082,
-235.350049999994));
#215965=CARTESIAN_POINT('Ctrl Pts',(0.790392115670831,-62.0923066687554,
-235.35005));
#215966=CARTESIAN_POINT('Ctrl Pts',(0.412136733768758,-63.3746270691585,
-234.664093426845));
#215967=CARTESIAN_POINT('Ctrl Pts',(0.397111998278993,-62.9313429315101,
-235.350050000035));
#215968=CARTESIAN_POINT('Ctrl Pts',(0.36940841555812,-62.1145237664284,
-235.35005));
#215969=CARTESIAN_POINT('Ctrl Pts',(-0.991515792586106,-63.3680438675972,
-234.664322262232));
#215970=CARTESIAN_POINT('Ctrl Pts',(-0.95532554440835,-62.9249658076674,
-235.35004999993));
#215971=CARTESIAN_POINT('Ctrl Pts',(-0.88873098344401,-62.1087555751507,
-235.35005));
#215972=CARTESIAN_POINT('Ctrl Pts',(-1.92100220733562,-63.2544619761069,
-234.668143932231));
#215973=CARTESIAN_POINT('Ctrl Pts',(-1.84945562689762,-62.8152272225558,
-235.35005));
#215974=CARTESIAN_POINT('Ctrl Pts',(-1.7211315285284,-62.0092019215959,
-235.35005));
#215975=CARTESIAN_POINT('Ctrl Pts',(-2.87097991613647,-63.0198283709189,
-234.674453520452));
#215976=CARTESIAN_POINT('Ctrl Pts',(-2.76516804634539,-62.5881510724421,
-235.35005));
#215977=CARTESIAN_POINT('Ctrl Pts',(-2.57264640705579,-61.8027147274169,
-235.35005));
#215978=CARTESIAN_POINT('Ctrl Pts',(-2.89975790044207,-63.0126057280022,
-234.674646875394));
#215979=CARTESIAN_POINT('Ctrl Pts',(-2.79287250767241,-62.581170184688,
-235.35005));
#215980=CARTESIAN_POINT('Ctrl Pts',(-2.5984432576946,-61.7963577456803,
-235.35005));
#215981=CARTESIAN_POINT('Ctrl Pts',(-2.94290959864959,-63.0016028905584,
-234.674940028084));
#215982=CARTESIAN_POINT('Ctrl Pts',(-2.83441572839343,-62.5705355559834,
-235.35005));
#215983=CARTESIAN_POINT('Ctrl Pts',(-2.63712855614808,-61.7866721046702,
-235.35005));
#215984=CARTESIAN_POINT('Ctrl Pts',(-2.95729095518362,-62.9979071324124,
-234.67503826564));
#215985=CARTESIAN_POINT('Ctrl Pts',(-2.84826077962461,-62.5669635813212,
-235.35005));
#215986=CARTESIAN_POINT('Ctrl Pts',(-2.65002199274596,-61.7834185300358,
-235.35005));
#215987=CARTESIAN_POINT('Ctrl Pts',(-2.98604840419677,-62.9904593061707,
-234.675235761569));
#215988=CARTESIAN_POINT('Ctrl Pts',(-2.87594598022536,-62.5597652489865,
-235.35005));
#215989=CARTESIAN_POINT('Ctrl Pts',(-2.67580553519198,-61.7768612507126,
-235.35005));
#215990=CARTESIAN_POINT('Ctrl Pts',(-2.9978333877905,-62.9873435276064,
-234.675371450446));
#215991=CARTESIAN_POINT('Ctrl Pts',(-2.88811134765541,-62.5565366104963,
-235.35005));
#215992=CARTESIAN_POINT('Ctrl Pts',(-2.68869554564646,-61.7735561102329,
-235.35005));
#215993=CARTESIAN_POINT('Ctrl Pts',(-3.05611228962128,-62.9721057909015,
-234.676043337161));
#215994=CARTESIAN_POINT('Ctrl Pts',(-2.94852233650361,-62.5406795307465,
-235.35005));
#215995=CARTESIAN_POINT('Ctrl Pts',(-2.75315733717204,-61.7572070918297,
-235.35005));
#215996=CARTESIAN_POINT('Ctrl Pts',(-3.10276465859771,-62.9602306309284,
-234.676544840607));
#215997=CARTESIAN_POINT('Ctrl Pts',(-2.99688788645165,-62.5283225924192,
-235.35005));
#215998=CARTESIAN_POINT('Ctrl Pts',(-2.80474830172023,-61.7444519385904,
-235.35005));
#215999=CARTESIAN_POINT('Ctrl Pts',(-3.24280643592837,-62.9255451527486,
-234.677942742714));
#216000=CARTESIAN_POINT('Ctrl Pts',(-3.14205961162902,-62.4922406313808,
-235.350050000002));
#216001=CARTESIAN_POINT('Ctrl Pts',(-2.95958538043147,-61.7071525092866,
-235.35005));
#216002=CARTESIAN_POINT('Ctrl Pts',(-3.33628023959272,-62.9036747672035,
-234.678732585306));
#216003=CARTESIAN_POINT('Ctrl Pts',(-3.23897853980704,-62.4694942379193,
-235.350050000002));
#216004=CARTESIAN_POINT('Ctrl Pts',(-3.06289566840461,-61.6835740933876,
-235.35005));
#216005=CARTESIAN_POINT('Ctrl Pts',(-3.61701461689342,-62.8417880653747,
-234.68068504518));
#216006=CARTESIAN_POINT('Ctrl Pts',(-3.53001543785944,-62.4051669357519,
-235.350049999997));
#216007=CARTESIAN_POINT('Ctrl Pts',(-3.37308038697823,-61.6166595365466,
-235.35005));
#216008=CARTESIAN_POINT('Ctrl Pts',(-3.80452881266942,-62.8055092013148,
-234.681430782666));
#216009=CARTESIAN_POINT('Ctrl Pts',(-3.72450262338561,-62.3674750906498,
-235.350050000018));
#216010=CARTESIAN_POINT('Ctrl Pts',(-3.58014437735177,-61.5771574345827,
-235.35005));
#216011=CARTESIAN_POINT('Ctrl Pts',(-4.36760854874154,-62.7114158369336,
-234.682047690539));
#216012=CARTESIAN_POINT('Ctrl Pts',(-4.3083998660853,-62.2698516038986,
-235.350049999965));
#216013=CARTESIAN_POINT('Ctrl Pts',(-4.20176187344348,-61.4737420228677,
-235.35005));
#216014=CARTESIAN_POINT('Ctrl Pts',(-4.74383676949718,-62.668310555781,
-234.680303868519));
#216015=CARTESIAN_POINT('Ctrl Pts',(-4.6989741743333,-62.2252554074114,
-235.350050000029));
#216016=CARTESIAN_POINT('Ctrl Pts',(-4.61689483741499,-61.4248774566823,
-235.35005));
#216017=CARTESIAN_POINT('Ctrl Pts',(-5.87442448212421,-62.5963302145134,
-234.668715190654));
#216018=CARTESIAN_POINT('Ctrl Pts',(-5.87235395168802,-62.1515742909292,
-235.350049999942));
#216019=CARTESIAN_POINT('Ctrl Pts',(-5.86440266843056,-61.3369909474474,
-235.35005));
#216020=CARTESIAN_POINT('Ctrl Pts',(-6.630328727236,-62.6245394292558,-234.652628616953));
#216021=CARTESIAN_POINT('Ctrl Pts',(-6.65928611702461,-62.1829590506774,
-235.350049999988));
#216022=CARTESIAN_POINT('Ctrl Pts',(-6.69887188182861,-61.3562699588587,
-235.35005));
#216023=CARTESIAN_POINT('Ctrl Pts',(-7.764209767566,-62.7816811580039,-234.613624648391));
#216024=CARTESIAN_POINT('Ctrl Pts',(-7.82979546040407,-62.3508034677975,
-235.350050000006));
#216025=CARTESIAN_POINT('Ctrl Pts',(-7.95484405860484,-61.5040080281448,
-235.35005));
#216026=CARTESIAN_POINT('Ctrl Pts',(-8.14142530534439,-62.8532056007147,
-234.598165828659));
#216027=CARTESIAN_POINT('Ctrl Pts',(-8.22039383870565,-62.4275509346929,
-235.35005));
#216028=CARTESIAN_POINT('Ctrl Pts',(-8.37327068677123,-61.573105256355,
-235.35005));
#216029=CARTESIAN_POINT('Ctrl Pts',(-8.5629236763468,-62.9549034336122,
-234.577665757063));
#216030=CARTESIAN_POINT('Ctrl Pts',(-8.65406374113881,-62.5362556404638,
-235.35005));
#216031=CARTESIAN_POINT('Ctrl Pts',(-8.84186416774843,-61.6731857859409,
-235.35005));
#216032=CARTESIAN_POINT('Ctrl Pts',(-8.60972279857098,-62.966499174667,
-234.575344423268));
#216033=CARTESIAN_POINT('Ctrl Pts',(-8.70237757817563,-62.5486988611875,
-235.350050000009));
#216034=CARTESIAN_POINT('Ctrl Pts',(-8.89390821376875,-61.6846177854791,
-235.35005));
#216035=CARTESIAN_POINT('Ctrl Pts',(-8.67987147174762,-62.9843376272339,
-234.571795714236));
#216036=CARTESIAN_POINT('Ctrl Pts',(-8.7747593225483,-62.5678413783773,
-235.350049999996));
#216037=CARTESIAN_POINT('Ctrl Pts',(-8.9719413326839,-61.7022352005211,
-235.35005));
#216038=CARTESIAN_POINT('Ctrl Pts',(-8.70324596171864,-62.9903579019877,
-234.570601696122));
#216039=CARTESIAN_POINT('Ctrl Pts',(-8.79888168729908,-62.5743045962304,
-235.350050000003));
#216040=CARTESIAN_POINT('Ctrl Pts',(-8.99794688049398,-61.7081859103136,
-235.35005));
#216041=CARTESIAN_POINT('Ctrl Pts',(-8.74997809315458,-63.0025468085543,
-234.568191202621));
#216042=CARTESIAN_POINT('Ctrl Pts',(-8.84710303258602,-62.5873924023601,
-235.350049999997));
#216043=CARTESIAN_POINT('Ctrl Pts',(-9.04994697297616,-61.7202440833036,
-235.35005));
#216044=CARTESIAN_POINT('Ctrl Pts',(-8.77030020255578,-63.0086617980509,
-234.565865719937));
#216045=CARTESIAN_POINT('Ctrl Pts',(-8.86903102195205,-62.594426558538,
-235.350049999999));
#216046=CARTESIAN_POINT('Ctrl Pts',(-9.07593838869885,-61.7263961224781,
-235.35005));
#216047=CARTESIAN_POINT('Ctrl Pts',(-8.91694881903725,-63.0405575039938,
-234.570644549592));
#216048=CARTESIAN_POINT('Ctrl Pts',(-9.01063474350099,-62.624024386533,
-235.350050000003));
#216049=CARTESIAN_POINT('Ctrl Pts',(-9.20590431013486,-61.7570303410545,
-235.35005));
#216050=CARTESIAN_POINT('Ctrl Pts',(-9.03436031698127,-63.0642013014708,
-234.574496870482));
#216051=CARTESIAN_POINT('Ctrl Pts',(-9.12404358218876,-62.6459210827606,
-235.35005));
#216052=CARTESIAN_POINT('Ctrl Pts',(-9.30999109039434,-61.7799130279695,
-235.35005));
#216053=CARTESIAN_POINT('Ctrl Pts',(-9.38683707975019,-63.1295777507455,
-234.58612993111));
#216054=CARTESIAN_POINT('Ctrl Pts',(-9.464112377,-62.7062240376773,-235.35005));
#216055=CARTESIAN_POINT('Ctrl Pts',(-9.62258974276106,-61.8437414130309,
-235.35005));
#216056=CARTESIAN_POINT('Ctrl Pts',(-9.62214011478876,-63.1657558644233,
-234.593987078423));
#216057=CARTESIAN_POINT('Ctrl Pts',(-9.6911920092531,-62.7393844961485,
-235.350049999994));
#216058=CARTESIAN_POINT('Ctrl Pts',(-9.83143975137235,-61.8798699303951,
-235.35005));
#216059=CARTESIAN_POINT('Ctrl Pts',(-10.7997915248163,-63.3103622575713,
-234.633595136481));
#216060=CARTESIAN_POINT('Ctrl Pts',(-10.8212304548731,-62.8697460481048,
-235.350050000023));
#216061=CARTESIAN_POINT('Ctrl Pts',(-10.8779045135963,-62.0289610481999,
-235.35005));
#216062=CARTESIAN_POINT('Ctrl Pts',(-11.7461619842447,-63.3113988762096,
-234.666687842414));
#216063=CARTESIAN_POINT('Ctrl Pts',(-11.7320939393461,-62.8666836322213,
-235.350049999928));
#216064=CARTESIAN_POINT('Ctrl Pts',(-11.7220571315963,-62.0487835216839,
-235.35005));
#216065=CARTESIAN_POINT('Ctrl Pts',(-13.1699413526949,-63.1363620280083,
-234.716022189278));
#216066=CARTESIAN_POINT('Ctrl Pts',(-13.10608590161,-62.6921044640064,-235.350050000036));
#216067=CARTESIAN_POINT('Ctrl Pts',(-12.9992495965492,-61.9223278044926,
-235.35005));
#216068=CARTESIAN_POINT('Ctrl Pts',(-13.6468010556902,-63.0478428317766,
-234.732508264035));
#216069=CARTESIAN_POINT('Ctrl Pts',(-13.5644252452197,-62.6057426040311,
-235.350049999994));
#216070=CARTESIAN_POINT('Ctrl Pts',(-13.4279947259813,-61.8535648232588,
-235.35005));
#216071=CARTESIAN_POINT('Ctrl Pts',(-14.1487244112426,-62.9212890657887,
-234.749460742189));
#216072=CARTESIAN_POINT('Ctrl Pts',(-14.0482803552132,-62.4826593861811,
-235.35005));
#216073=CARTESIAN_POINT('Ctrl Pts',(-13.880777738108,-61.7511282800593,
-235.35005));
#216074=CARTESIAN_POINT('Ctrl Pts',(-14.1782348713718,-62.9137255409854,
-234.750455807673));
#216075=CARTESIAN_POINT('Ctrl Pts',(-14.0766397091771,-62.4753290557739,
-235.350050000002));
#216076=CARTESIAN_POINT('Ctrl Pts',(-13.9074044897115,-61.7449947684686,
-235.35005));
#216077=CARTESIAN_POINT('Ctrl Pts',(-14.2224775170047,-62.9022015555295,
-234.751944983515));
#216078=CARTESIAN_POINT('Ctrl Pts',(-14.1191614632759,-62.4641631011826,
-235.350049999999));
#216079=CARTESIAN_POINT('Ctrl Pts',(-13.9473332680511,-61.7356322629881,
-235.35005));
#216080=CARTESIAN_POINT('Ctrl Pts',(-14.2372212410967,-62.8983304396559,
-234.75244080564));
#216081=CARTESIAN_POINT('Ctrl Pts',(-14.1333303258632,-62.4604132959301,
-235.35005));
#216082=CARTESIAN_POINT('Ctrl Pts',(-13.9606409693201,-61.7324843881166,
-235.35005));
#216083=CARTESIAN_POINT('Ctrl Pts',(-14.2667009590697,-62.89052860958,-234.753431279982));
#216084=CARTESIAN_POINT('Ctrl Pts',(-14.1616608142962,-62.4528572201639,
-235.350049999999));
#216085=CARTESIAN_POINT('Ctrl Pts',(-13.9872525830674,-61.7261344765805,
-235.35005));
#216086=CARTESIAN_POINT('Ctrl Pts',(-14.2781153460893,-62.8881093785209,
-234.753016968105));
#216087=CARTESIAN_POINT('Ctrl Pts',(-14.1738174996514,-62.4502724992987,
-235.35005));
#216088=CARTESIAN_POINT('Ctrl Pts',(-14.000557201923,-61.7229425377452,
-235.35005));
#216089=CARTESIAN_POINT('Ctrl Pts',(-14.3387700345776,-62.8745860683453,
-234.75190829161));
#216090=CARTESIAN_POINT('Ctrl Pts',(-14.2367701819519,-62.4362364690685,
-235.350049999998));
#216091=CARTESIAN_POINT('Ctrl Pts',(-14.067093113681,-61.7071660730871,
-235.35005));
#216092=CARTESIAN_POINT('Ctrl Pts',(-14.3873180956111,-62.8641049651357,
-234.750988490225));
#216093=CARTESIAN_POINT('Ctrl Pts',(-14.2871495014114,-62.4253613242066,
-235.350050000003));
#216094=CARTESIAN_POINT('Ctrl Pts',(-14.1203460326614,-61.6948906982809,
-235.35005));
#216095=CARTESIAN_POINT('Ctrl Pts',(-14.5330297353877,-62.8336671798573,
-234.748130090176));
#216096=CARTESIAN_POINT('Ctrl Pts',(-14.4383810376854,-62.3937793044535,
-235.350049999996));
#216097=CARTESIAN_POINT('Ctrl Pts',(-14.2801767898011,-61.6590938369543,
-235.35005));
#216098=CARTESIAN_POINT('Ctrl Pts',(-14.6302610598049,-62.814715723775,
-234.746092558));
#216099=CARTESIAN_POINT('Ctrl Pts',(-14.5392754781889,-62.3741280970256,
-235.35005));
#216100=CARTESIAN_POINT('Ctrl Pts',(-14.3868266096958,-61.6366013501929,
-235.35005));
#216101=CARTESIAN_POINT('Ctrl Pts',(-14.9221858666243,-62.7618333918368,
-234.739578254538));
#216102=CARTESIAN_POINT('Ctrl Pts',(-14.8423074294462,-62.3193023231595,
-235.35005));
#216103=CARTESIAN_POINT('Ctrl Pts',(-14.707060162972,-61.5731850879451,
-235.35005));
#216104=CARTESIAN_POINT('Ctrl Pts',(-15.1171107050774,-62.7318713397189,
-234.73470073075));
#216105=CARTESIAN_POINT('Ctrl Pts',(-15.0445895988711,-62.2883058945919,
-235.350050000006));
#216106=CARTESIAN_POINT('Ctrl Pts',(-14.9209277353048,-61.5363188718154,
-235.35005));
#216107=CARTESIAN_POINT('Ctrl Pts',(-16.092794467113,-62.6080592508531,
-234.70749886562));
#216108=CARTESIAN_POINT('Ctrl Pts',(-16.0603371959058,-62.1601711109026,
-235.350049999976));
#216109=CARTESIAN_POINT('Ctrl Pts',(-15.9921235684109,-61.3785480216598,
-235.35005));
#216110=CARTESIAN_POINT('Ctrl Pts',(-16.8769323685421,-62.5917011576633,
-234.676953449944));
#216111=CARTESIAN_POINT('Ctrl Pts',(-16.877440790753,-62.1458673443692,
-235.350050000024));
#216112=CARTESIAN_POINT('Ctrl Pts',(-16.8549897301619,-61.3368092608675,
-235.35005));
#216113=CARTESIAN_POINT('Ctrl Pts',(-18.4490580403513,-62.7174106638047,
-234.59397567041));
#216114=CARTESIAN_POINT('Ctrl Pts',(-18.5050342407488,-62.2871579302411,
-235.350049999975));
#216115=CARTESIAN_POINT('Ctrl Pts',(-18.5923327067712,-61.4193093323336,
-235.35005));
#216116=CARTESIAN_POINT('Ctrl Pts',(-19.243264596634,-62.8631291742346,
-234.540485831164));
#216117=CARTESIAN_POINT('Ctrl Pts',(-19.3295880835876,-62.4508333719574,
-235.350049999916));
#216118=CARTESIAN_POINT('Ctrl Pts',(-19.4741956661812,-61.5471706223108,
-235.35005));
#216119=CARTESIAN_POINT('Ctrl Pts',(-20.0002454535025,-63.0750142297971,
-234.47617280861));
#216120=CARTESIAN_POINT('Ctrl Pts',(-20.0938415017253,-62.6846662779264,
-235.35005));
#216121=CARTESIAN_POINT('Ctrl Pts',(-20.3180691938068,-61.7495111937247,
-235.35005));
#216122=CARTESIAN_POINT('',(-5.58372807339351E-13,-63.3694498996295,-234.668963364338));
#216123=CARTESIAN_POINT('',(8.78586952537018,-63.0089774131351,-234.571825729504));
#216124=CARTESIAN_POINT('Ctrl Pts',(-1.5702990355655E-14,-63.3694498182033,
-234.66896331128));
#216125=CARTESIAN_POINT('Ctrl Pts',(0.217773905612689,-63.3694496543811,
-234.668963562687));
#216126=CARTESIAN_POINT('Ctrl Pts',(0.438520411739192,-63.3634719988444,
-234.669163036834));
#216127=CARTESIAN_POINT('Ctrl Pts',(0.662407453077813,-63.3509495177584,
-234.669561733719));
#216128=CARTESIAN_POINT('Ctrl Pts',(0.692105148220668,-63.3492884621498,
-234.669614619221));
#216129=CARTESIAN_POINT('Ctrl Pts',(0.721858175028539,-63.347512237878,
-234.669671010034));
#216130=CARTESIAN_POINT('Ctrl Pts',(0.751666994640722,-63.3456195093547,
-234.669730906157));
#216131=CARTESIAN_POINT('Ctrl Pts',(0.967065625823832,-63.3319426466531,
-234.670163715742));
#216132=CARTESIAN_POINT('Ctrl Pts',(1.18537391652108,-63.3121847391183,
-234.670779555548));
#216133=CARTESIAN_POINT('Ctrl Pts',(1.40676856118831,-63.2857272692194,
-234.671578425574));
#216134=CARTESIAN_POINT('Ctrl Pts',(1.43728891440615,-63.2820799753665,
-234.671688553781));
#216135=CARTESIAN_POINT('Ctrl Pts',(1.46786798998409,-63.2783053208916,
-234.671802160294));
#216136=CARTESIAN_POINT('Ctrl Pts',(1.49850631840134,-63.2744016447649,
-234.671919245112));
#216137=CARTESIAN_POINT('Ctrl Pts',(1.54099258502891,-63.2689884047705,
-234.672081606998));
#216138=CARTESIAN_POINT('Ctrl Pts',(1.58359278893985,-63.2633270675726,
-234.672250657476));
#216139=CARTESIAN_POINT('Ctrl Pts',(1.62630844138418,-63.2574121891646,
-234.672426396546));
#216140=CARTESIAN_POINT('Ctrl Pts',(1.71981144698678,-63.2444647360117,
-234.672811082962));
#216141=CARTESIAN_POINT('Ctrl Pts',(1.81386752908635,-63.2303025361026,
-234.673227818233));
#216142=CARTESIAN_POINT('Ctrl Pts',(1.90849366367972,-63.2148672638034,
-234.673676608004));
#216143=CARTESIAN_POINT('Ctrl Pts',(1.95580673097641,-63.2071496276537,
-234.673901002889));
#216144=CARTESIAN_POINT('Ctrl Pts',(2.00326230890218,-63.199113708202,-234.674133401273));
#216145=CARTESIAN_POINT('Ctrl Pts',(2.05086269848244,-63.1907520420292,
-234.674373816126));
#216146=CARTESIAN_POINT('Ctrl Pts',(2.07466289327257,-63.1865712089429,
-234.674494023553));
#216147=CARTESIAN_POINT('Ctrl Pts',(2.09849929082736,-63.1823089381926,
-234.674616234444));
#216148=CARTESIAN_POINT('Ctrl Pts',(2.12237218364187,-63.1779642886395,
-234.674740448649));
#216149=CARTESIAN_POINT('Ctrl Pts',(2.13430863004912,-63.1757919638629,
-234.674802555751));
#216150=CARTESIAN_POINT('Ctrl Pts',(2.1462542002606,-63.1735990443261,-234.674865163642));
#216151=CARTESIAN_POINT('Ctrl Pts',(2.15820893145162,-63.1713854117438,
-234.674928272312));
#216152=CARTESIAN_POINT('Ctrl Pts',(2.16418629704713,-63.1702785954526,
-234.674959826647));
#216153=CARTESIAN_POINT('Ctrl Pts',(2.17016595288684,-63.1691666008963,
-234.674991506174));
#216154=CARTESIAN_POINT('Ctrl Pts',(2.17614790365865,-63.1680494132478,
-234.675023310893));
#216155=CARTESIAN_POINT('Ctrl Pts',(2.18212985443046,-63.1669322255993,
-234.675055115613));
#216156=CARTESIAN_POINT('Ctrl Pts',(2.18934094285044,-63.1655787643479,
-234.675093614681));
#216157=CARTESIAN_POINT('Ctrl Pts',(2.19410064546927,-63.1646822561782,
-234.675119100623));
#216158=CARTESIAN_POINT('Ctrl Pts',(2.21009843956643,-63.1616690105507,
-234.675204761195));
#216159=CARTESIAN_POINT('Ctrl Pts',(2.22625301394984,-63.158591438058,-234.675293116861));
#216160=CARTESIAN_POINT('Ctrl Pts',(2.24256443067466,-63.15544746846,-234.675384167619));
#216161=CARTESIAN_POINT('Ctrl Pts',(2.33086547491839,-63.1384277452036,
-234.675877066377));
#216162=CARTESIAN_POINT('Ctrl Pts',(2.42376183912149,-63.1194662392236,
-234.676448946035));
#216163=CARTESIAN_POINT('Ctrl Pts',(2.52127275503764,-63.0981948799086,
-234.677099806595));
#216164=CARTESIAN_POINT('Ctrl Pts',(2.61627973210451,-63.0774697382397,
-234.677733954));
#216165=CARTESIAN_POINT('Ctrl Pts',(2.71566715620675,-63.0545518959675,
-234.678443078155));
#216166=CARTESIAN_POINT('Ctrl Pts',(2.81946610010958,-63.0290534318913,
-234.67922717906));
#216167=CARTESIAN_POINT('Ctrl Pts',(2.870498985797,-63.0165170788854,-234.679612683289));
#216168=CARTESIAN_POINT('Ctrl Pts',(2.92259844844719,-63.0033561960728,
-234.680016310973));
#216169=CARTESIAN_POINT('Ctrl Pts',(2.97576958847413,-62.989520236264,-234.680438062112));
#216170=CARTESIAN_POINT('Ctrl Pts',(2.97914177857081,-62.9886427398135,
-234.680464810175));
#216171=CARTESIAN_POINT('Ctrl Pts',(2.98251827959221,-62.9877625270014,
-234.680491631136));
#216172=CARTESIAN_POINT('Ctrl Pts',(2.98589909297911,-62.9868795845193,
-234.680518524994));
#216173=CARTESIAN_POINT('Ctrl Pts',(3.03144670211263,-62.9749842461911,
-234.680880849326));
#216174=CARTESIAN_POINT('Ctrl Pts',(3.07784469384026,-62.9631470419589,
-234.681256404939));
#216175=CARTESIAN_POINT('Ctrl Pts',(3.12509757339216,-62.9513965645584,
-234.681645191834));
#216176=CARTESIAN_POINT('Ctrl Pts',(3.15047770749805,-62.9450852308352,
-234.681854014315));
#216177=CARTESIAN_POINT('Ctrl Pts',(3.17610446179225,-62.9387989363886,
-234.682066653893));
#216178=CARTESIAN_POINT('Ctrl Pts',(3.20197848411835,-62.9325422483476,
-234.682283110295));
#216179=CARTESIAN_POINT('Ctrl Pts',(3.2149154952814,-62.929413904327,-234.682391338496));
#216180=CARTESIAN_POINT('Ctrl Pts',(3.22791432366225,-62.9262929628025,
-234.682500521516));
#216181=CARTESIAN_POINT('Ctrl Pts',(3.24097504554104,-62.9231800045925,
-234.682610658402));
#216182=CARTESIAN_POINT('Ctrl Pts',(3.25276701314493,-62.9203694476642,
-234.682710096289));
#216183=CARTESIAN_POINT('Ctrl Pts',(3.26621068276329,-62.9171883489843,
-234.682823921931));
#216184=CARTESIAN_POINT('Ctrl Pts',(3.2769690464069,-62.9146585345259,-234.682915271999));
#216185=CARTESIAN_POINT('Ctrl Pts',(3.27812659028102,-62.9143863396711,
-234.68292510079));
#216186=CARTESIAN_POINT('Ctrl Pts',(3.27925303445033,-62.9141216361366,
-234.68293466939));
#216187=CARTESIAN_POINT('Ctrl Pts',(3.28034296828758,-62.9138656646226,
-234.682943931882));
#216188=CARTESIAN_POINT('Ctrl Pts',(3.42311597107787,-62.8803353525691,
-234.684157247518));
#216189=CARTESIAN_POINT('Ctrl Pts',(3.56630723773157,-62.8496695059215,
-234.685050927405));
#216190=CARTESIAN_POINT('Ctrl Pts',(3.71018636154233,-62.8218113840577,
-234.685624000546));
#216191=CARTESIAN_POINT('Ctrl Pts',(3.85344884246849,-62.7940726576432,
-234.686194617587));
#216192=CARTESIAN_POINT('Ctrl Pts',(3.99739358369234,-62.7691175748496,
-234.686447370131));
#216193=CARTESIAN_POINT('Ctrl Pts',(4.14229793497986,-62.7469404019187,
-234.686381299612));
#216194=CARTESIAN_POINT('Ctrl Pts',(4.21783125916824,-62.7353802549826,
-234.686346859474));
#216195=CARTESIAN_POINT('Ctrl Pts',(4.2936254830793,-62.7245757451169,-234.686225790181));
#216196=CARTESIAN_POINT('Ctrl Pts',(4.3697207132042,-62.7145316285495,-234.686017955969));
#216197=CARTESIAN_POINT('Ctrl Pts',(4.38025306702375,-62.7131414206571,
-234.6859891896));
#216198=CARTESIAN_POINT('Ctrl Pts',(4.39078527443694,-62.7117665649021,
-234.685958779806));
#216199=CARTESIAN_POINT('Ctrl Pts',(4.40131730214741,-62.710407049675,-234.685926726586));
#216200=CARTESIAN_POINT('Ctrl Pts',(4.67608260672618,-62.6749392721778,
-234.685090504658));
#216201=CARTESIAN_POINT('Ctrl Pts',(4.95072126703645,-62.6499130118094,
-234.683135747384));
#216202=CARTESIAN_POINT('Ctrl Pts',(5.22463708211698,-62.6350433636936,
-234.680062454763));
#216203=CARTESIAN_POINT('Ctrl Pts',(5.43392972328729,-62.623681814794,-234.677714224051));
#216204=CARTESIAN_POINT('Ctrl Pts',(5.64280142810662,-62.6182496913347,
-234.674712977953));
#216205=CARTESIAN_POINT('Ctrl Pts',(5.85100656062646,-62.61861720167,-234.671058716468));
#216206=CARTESIAN_POINT('Ctrl Pts',(5.99971161321492,-62.6188796862835,
-234.668448756091));
#216207=CARTESIAN_POINT('Ctrl Pts',(6.14807698913752,-62.622100557494,-234.665505682392));
#216208=CARTESIAN_POINT('Ctrl Pts',(6.29601532503752,-62.6282206073021,
-234.662229495371));
#216209=CARTESIAN_POINT('Ctrl Pts',(6.34701415223957,-62.6303303739203,
-234.66110009443));
#216210=CARTESIAN_POINT('Ctrl Pts',(6.39734769704919,-62.6327538032416,
-234.659946480854));
#216211=CARTESIAN_POINT('Ctrl Pts',(6.44804640347912,-62.6355359592762,
-234.658742787956));
#216212=CARTESIAN_POINT('Ctrl Pts',(6.48774806684274,-62.6377146385776,
-234.657800187767));
#216213=CARTESIAN_POINT('Ctrl Pts',(6.52767372357854,-62.640114284633,-234.656826877418));
#216214=CARTESIAN_POINT('Ctrl Pts',(6.56831866038382,-62.6427788180075,
-234.655810435343));
#216215=CARTESIAN_POINT('Ctrl Pts',(6.81815541742719,-62.6591572018768,
-234.649562557711));
#216216=CARTESIAN_POINT('Ctrl Pts',(7.06823871599811,-62.6839230792243,
-234.642231150492));
#216217=CARTESIAN_POINT('Ctrl Pts',(7.31818157745278,-62.7170814615928,
-234.633816213689));
#216218=CARTESIAN_POINT('Ctrl Pts',(7.76071788223362,-62.7757900317054,
-234.618917148293));
#216219=CARTESIAN_POINT('Ctrl Pts',(8.20281103349084,-62.8608087797858,
-234.600621383538));
#216220=CARTESIAN_POINT('Ctrl Pts',(8.64229067170807,-62.9718223083916,
-234.578928919424));
#216221=CARTESIAN_POINT('Ctrl Pts',(8.69017528132899,-62.9839180666877,
-234.576565362423));
#216222=CARTESIAN_POINT('Ctrl Pts',(8.73802891188869,-62.9963224091943,
-234.574161480689));
#216223=CARTESIAN_POINT('Ctrl Pts',(8.78584879256821,-63.0090349136113,
-234.571717274223));
#216224=CARTESIAN_POINT('',(-8.78585690854571,-63.009043156862,-234.571720019294));
#216225=CARTESIAN_POINT('Ctrl Pts',(-1.10089718099767E-12,-63.3694499810558,
-234.668963417397));
#216226=CARTESIAN_POINT('Ctrl Pts',(-0.0185810354048697,-63.3694498388901,
-234.668963445136));
#216227=CARTESIAN_POINT('Ctrl Pts',(-0.0371587302925499,-63.3694061680557,
-234.668964958478));
#216228=CARTESIAN_POINT('Ctrl Pts',(-0.0557330586443233,-63.3693190483712,
-234.668967969332));
#216229=CARTESIAN_POINT('Ctrl Pts',(-0.991261546562719,-63.3649311133023,
-234.669119616233));
#216230=CARTESIAN_POINT('Ctrl Pts',(-1.92049921579277,-63.2513737473296,
-234.67291846854));
#216231=CARTESIAN_POINT('Ctrl Pts',(-2.84145511359989,-63.0238979202665,
-234.679000216158));
#216232=CARTESIAN_POINT('Ctrl Pts',(-2.87023498540635,-63.0167893006708,
-234.679190270771));
#216233=CARTESIAN_POINT('Ctrl Pts',(-2.89900538169324,-63.0095682375878,
-234.679382465876));
#216234=CARTESIAN_POINT('Ctrl Pts',(-2.92776559984891,-63.0022346175025,
-234.679576728533));
#216235=CARTESIAN_POINT('Ctrl Pts',(-2.94214570892675,-62.9985678074598,
-234.679673859862));
#216236=CARTESIAN_POINT('Ctrl Pts',(-2.95652327372903,-62.9948728588666,
-234.679771508003));
#216237=CARTESIAN_POINT('Ctrl Pts',(-2.97089820746555,-62.9911497618158,
-234.679869663442));
#216238=CARTESIAN_POINT('Ctrl Pts',(-2.98527314120207,-62.9874266647649,
-234.679967818882));
#216239=CARTESIAN_POINT('Ctrl Pts',(-2.99706078139591,-62.9843100059298,
-234.680102693504));
#216240=CARTESIAN_POINT('Ctrl Pts',(-3.00871954326037,-62.9812615014743,
-234.680236264292));
#216241=CARTESIAN_POINT('Ctrl Pts',(-3.05535459071823,-62.9690674836524,
-234.680770547444));
#216242=CARTESIAN_POINT('Ctrl Pts',(-3.10201894695471,-62.9571886136925,
-234.681269039807));
#216243=CARTESIAN_POINT('Ctrl Pts',(-3.14871151468708,-62.9456232134564,
-234.681732208063));
#216244=CARTESIAN_POINT('Ctrl Pts',(-3.24209665015184,-62.9224924129843,
-234.682658544576));
#216245=CARTESIAN_POINT('Ctrl Pts',(-3.33559461282545,-62.9006153539932,
-234.68344363964));
#216246=CARTESIAN_POINT('Ctrl Pts',(-3.42919685501764,-62.8799803049587,
-234.684090544914));
#216247=CARTESIAN_POINT('Ctrl Pts',(-3.616401339402,-62.8387102068898,-234.685384355463));
#216248=CARTESIAN_POINT('Ctrl Pts',(-3.80396460003819,-62.8024209051424,
-234.686125603876));
#216249=CARTESIAN_POINT('Ctrl Pts',(-3.99170675162661,-62.7710480212593,
-234.686330001583));
#216250=CARTESIAN_POINT('Ctrl Pts',(-4.36719105480346,-62.7083022534931,
-234.686738796995));
#216251=CARTESIAN_POINT('Ctrl Pts',(-4.74352052971821,-62.6651875901659,
-234.685005473986));
#216252=CARTESIAN_POINT('Ctrl Pts',(-5.12048363858745,-62.6411926630512,
-234.681165753978));
#216253=CARTESIAN_POINT('Ctrl Pts',(-5.87440985632592,-62.5932028088217,
-234.673486313963));
#216254=CARTESIAN_POINT('Ctrl Pts',(-6.6305314355631,-62.6214447067006,
-234.657495585896));
#216255=CARTESIAN_POINT('Ctrl Pts',(-7.38662085898429,-62.7262724152159,
-234.631645385162));
#216256=CARTESIAN_POINT('Ctrl Pts',(-7.76466557069487,-62.7786862694735,
-234.618720284795));
#216257=CARTESIAN_POINT('Ctrl Pts',(-8.14197229631615,-62.8502567352985,
-234.603350759003));
#216258=CARTESIAN_POINT('Ctrl Pts',(-8.51671007390683,-62.9407093175552,
-234.585232582824));
#216259=CARTESIAN_POINT('Ctrl Pts',(-8.56355229610568,-62.9520158903373,
-234.582967810801));
#216260=CARTESIAN_POINT('Ctrl Pts',(-8.61036154587541,-62.9636189189669,
-234.580659656259));
#216261=CARTESIAN_POINT('Ctrl Pts',(-8.65713725766767,-62.9755186803616,
-234.578307258395));
#216262=CARTESIAN_POINT('Ctrl Pts',(-8.68052511356379,-62.9814685610589,
-234.577131059463));
#216263=CARTESIAN_POINT('Ctrl Pts',(-8.70390458536919,-62.9874926264074,
-234.575943799166));
#216264=CARTESIAN_POINT('Ctrl Pts',(-8.72727560477769,-62.993590919855,
-234.574745366521));
#216265=CARTESIAN_POINT('Ctrl Pts',(-8.73694813662187,-62.9961148122251,
-234.574249372841));
#216266=CARTESIAN_POINT('Ctrl Pts',(-8.746100261435,-62.9986429068519,-234.573562586431));
#216267=CARTESIAN_POINT('Ctrl Pts',(-8.75558085258196,-63.0012075165445,
-234.572965026759));
#216268=CARTESIAN_POINT('Ctrl Pts',(-8.76506144329811,-63.0037721261205,
-234.572367467114));
#216269=CARTESIAN_POINT('Ctrl Pts',(-8.77487050775363,-63.0063732152886,
-234.571859113242));
#216270=CARTESIAN_POINT('Ctrl Pts',(-8.7858569085457,-63.009043156862,-234.571720019294));
#216271=CARTESIAN_POINT('',(-14.2619204088508,-62.8884591070428,-234.75755030089));
#216272=CARTESIAN_POINT('Ctrl Pts',(-8.78585826084274,-63.0090374306747,
-234.571716790273));
#216273=CARTESIAN_POINT('Ctrl Pts',(-8.81155642576436,-63.0149922863215,
-234.571920323696));
#216274=CARTESIAN_POINT('Ctrl Pts',(-8.84178103342904,-63.0211625331105,
-234.573531555121));
#216275=CARTESIAN_POINT('Ctrl Pts',(-8.89842888688522,-63.0331158852246,
-234.575374277387));
#216276=CARTESIAN_POINT('Ctrl Pts',(-8.98341642645075,-63.0507193140023,
-234.578143293289));
#216277=CARTESIAN_POINT('Ctrl Pts',(-9.18182719302696,-63.0895137607373,
-234.584637642812));
#216278=CARTESIAN_POINT('Ctrl Pts',(-9.352062705706,-63.1188793895947,-234.590257702624));
#216279=CARTESIAN_POINT('Ctrl Pts',(-9.69272498154921,-63.1724789879354,
-234.601556701877));
#216280=CARTESIAN_POINT('Ctrl Pts',(-9.92006685579639,-63.2013610418528,
-234.609159841967));
#216281=CARTESIAN_POINT('Ctrl Pts',(-10.6028030210204,-63.2680315051849,
-234.632189424261));
#216282=CARTESIAN_POINT('Ctrl Pts',(-11.0589190335537,-63.2856900244449,
-234.647828473024));
#216283=CARTESIAN_POINT('Ctrl Pts',(-11.9727448912346,-63.2667333947121,
-234.679318210709));
#216284=CARTESIAN_POINT('Ctrl Pts',(-12.4302348513601,-63.2302711749144,
-234.695155702502));
#216285=CARTESIAN_POINT('Ctrl Pts',(-13.1181865020587,-63.1338298835409,
-234.718846244067));
#216286=CARTESIAN_POINT('Ctrl Pts',(-13.4626300973589,-63.0750435786505,
-234.730677939129));
#216287=CARTESIAN_POINT('Ctrl Pts',(-13.863319330679,-62.9878449235659,
-234.744290120853));
#216288=CARTESIAN_POINT('Ctrl Pts',(-14.0631260174647,-62.9395763466499,
-234.751027385112));
#216289=CARTESIAN_POINT('Ctrl Pts',(-14.1486155628969,-62.9178876098048,
-234.753897783854));
#216290=CARTESIAN_POINT('Ctrl Pts',(-14.2055812445659,-62.9032067723758,
-234.755807151484));
#216291=CARTESIAN_POINT('Ctrl Pts',(-14.2362308220828,-62.894753041772,
-234.757354927317));
#216292=CARTESIAN_POINT('Ctrl Pts',(-14.2619201924805,-62.8884582017248,
-234.757549593623));
#216293=CARTESIAN_POINT('Ctrl Pts',(-14.2619206252211,-62.8884600123608,
-234.757551008158));
#216294=CARTESIAN_POINT('Ctrl Pts',(-14.2718178205262,-62.8860359678618,
-234.757626045819));
#216295=CARTESIAN_POINT('Ctrl Pts',(-14.2804506465911,-62.884181158001,
-234.75735599456));
#216296=CARTESIAN_POINT('Ctrl Pts',(-14.2894789617138,-62.8821685292642,
-234.757191860054));
#216297=CARTESIAN_POINT('Ctrl Pts',(-14.2953100040955,-62.8808686495743,
-234.757085851873));
#216298=CARTESIAN_POINT('Ctrl Pts',(-14.3011413964139,-62.8795736434999,
-234.756979372388));
#216299=CARTESIAN_POINT('Ctrl Pts',(-14.3069731357651,-62.8782835068473,
-234.756872421387));
#216300=CARTESIAN_POINT('Ctrl Pts',(-14.3218342693705,-62.8749958267903,
-234.756599876094));
#216301=CARTESIAN_POINT('Ctrl Pts',(-14.3366976561142,-62.8717397684931,
-234.756324268863));
#216302=CARTESIAN_POINT('Ctrl Pts',(-14.3515632470811,-62.8685152641695,
-234.75604559438));
#216303=CARTESIAN_POINT('Ctrl Pts',(-14.379422206322,-62.8624723604785,
-234.755523342619));
#216304=CARTESIAN_POINT('Ctrl Pts',(-14.407288906641,-62.8565402762579,
-234.754990319625));
#216305=CARTESIAN_POINT('Ctrl Pts',(-14.4351630270212,-62.8507185672364,
-234.754446487672));
#216306=CARTESIAN_POINT('Ctrl Pts',(-14.4965309925101,-62.8379014295673,
-234.753249181352));
#216307=CARTESIAN_POINT('Ctrl Pts',(-14.5579349104097,-62.8256192347497,
-234.751999468502));
#216308=CARTESIAN_POINT('Ctrl Pts',(-14.6193714363495,-62.8138676057989,
-234.750697175335));
#216309=CARTESIAN_POINT('Ctrl Pts',(-14.6552123969003,-62.8070119175387,
-234.749937441003));
#216310=CARTESIAN_POINT('Ctrl Pts',(-14.6910644795143,-62.8003368602371,
-234.749159725648));
#216311=CARTESIAN_POINT('Ctrl Pts',(-14.7269270374636,-62.7938416077259,
-234.748363934128));
#216312=CARTESIAN_POINT('Ctrl Pts',(-14.8102586445982,-62.7787489913186,
-234.746514802607));
#216313=CARTESIAN_POINT('Ctrl Pts',(-14.8936466504724,-62.7646266721235,
-234.744568250047));
#216314=CARTESIAN_POINT('Ctrl Pts',(-14.977083853841,-62.7514672570885,
-234.742522108686));
#216315=CARTESIAN_POINT('Ctrl Pts',(-15.088565550686,-62.7338847656054,
-234.739788228574));
#216316=CARTESIAN_POINT('Ctrl Pts',(-15.2001350737935,-62.718021254317,
-234.736876561928));
#216317=CARTESIAN_POINT('Ctrl Pts',(-15.3117752750282,-62.7038591699904,
-234.733781825198));
#216318=CARTESIAN_POINT('Ctrl Pts',(-16.0925594070578,-62.60481303252,-234.712137997038));
#216319=CARTESIAN_POINT('Ctrl Pts',(-16.876935604951,-62.5885044241157,
-234.681761165031));
#216320=CARTESIAN_POINT('Ctrl Pts',(-17.6631922964109,-62.6514552500384,
-234.640496870595));
#216321=CARTESIAN_POINT('Ctrl Pts',(-18.4494489878708,-62.714406075961,
-234.59923257616));
#216322=CARTESIAN_POINT('Ctrl Pts',(-19.2438574482263,-62.8602959530961,
-234.546023767266));
#216323=CARTESIAN_POINT('Ctrl Pts',(-20.0008767707152,-63.072381283368,
-234.482033933863));
#216324=CARTESIAN_POINT('Ctrl Pts',(20.3180691938068,-61.7495111937247,
-235.35005));
#216325=CARTESIAN_POINT('Ctrl Pts',(19.4916837568995,-61.5513638467584,
-235.35005));
#216326=CARTESIAN_POINT('Ctrl Pts',(18.6602407015577,-61.4290562345849,
-235.350049999995));
#216327=CARTESIAN_POINT('Ctrl Pts',(17.8237010076361,-61.383180131545,-235.350049999998));
#216328=CARTESIAN_POINT('Ctrl Pts',(17.8193849653698,-61.3829434384136,
-235.350049999998));
#216329=CARTESIAN_POINT('Ctrl Pts',(17.8150687901225,-61.3827087804827,
-235.350049999998));
#216330=CARTESIAN_POINT('Ctrl Pts',(17.8107524818627,-61.3824761578263,
-235.350049999998));
#216331=CARTESIAN_POINT('Ctrl Pts',(17.2147892952599,-61.3503573814946,
-235.350050000001));
#216332=CARTESIAN_POINT('Ctrl Pts',(16.6152523367041,-61.3571390739688,
-235.350049999997));
#216333=CARTESIAN_POINT('Ctrl Pts',(16.0142818448677,-61.4050925383354,
-235.350049999997));
#216334=CARTESIAN_POINT('Ctrl Pts',(15.7759845903776,-61.4241070807416,
-235.350049999997));
#216335=CARTESIAN_POINT('Ctrl Pts',(15.5374618755672,-61.4495955645057,
-235.350049999998));
#216336=CARTESIAN_POINT('Ctrl Pts',(15.2988469678936,-61.4817018895299,
-235.350049999999));
#216337=CARTESIAN_POINT('Ctrl Pts',(15.2901306232776,-61.4828746988736,
-235.350049999999));
#216338=CARTESIAN_POINT('Ctrl Pts',(15.281414209221,-61.4840563352562,-235.350049999999));
#216339=CARTESIAN_POINT('Ctrl Pts',(15.2726977314404,-61.4852468054071,
-235.350049999999));
#216340=CARTESIAN_POINT('Ctrl Pts',(14.8590353180584,-61.5417435656889,
-235.350050000001));
#216341=CARTESIAN_POINT('Ctrl Pts',(14.4462075587129,-61.6179810575818,
-235.350049999997));
#216342=CARTESIAN_POINT('Ctrl Pts',(14.0341375328623,-61.7149985037554,
-235.350049999999));
#216343=CARTESIAN_POINT('Ctrl Pts',(14.0232833701672,-61.7175539993726,
-235.350049999999));
#216344=CARTESIAN_POINT('Ctrl Pts',(14.0124297591075,-61.7201239178539,
-235.350049999999));
#216345=CARTESIAN_POINT('Ctrl Pts',(14.0015767005386,-61.7227082779102,
-235.35005));
#216346=CARTESIAN_POINT('Ctrl Pts',(13.9751466240921,-61.7290018801626,
-235.35005));
#216347=CARTESIAN_POINT('Ctrl Pts',(13.9487179907097,-61.7353334612271,
-235.35005));
#216348=CARTESIAN_POINT('Ctrl Pts',(13.9222830160342,-61.7414997255267,
-235.35005));
#216349=CARTESIAN_POINT('Ctrl Pts',(13.8958480583747,-61.7476659858572,
-235.35005));
#216350=CARTESIAN_POINT('Ctrl Pts',(13.8694089796451,-61.7537248852831,
-235.35005));
#216351=CARTESIAN_POINT('Ctrl Pts',(13.8429657964072,-61.7596768227289,
-235.35005));
#216352=CARTESIAN_POINT('Ctrl Pts',(13.790079463996,-61.7715806899532,-235.35005));
#216353=CARTESIAN_POINT('Ctrl Pts',(13.7371767136853,-61.7830567143073,
-235.35005));
#216354=CARTESIAN_POINT('Ctrl Pts',(13.6842576766592,-61.7941080279422,
-235.35005));
#216355=CARTESIAN_POINT('Ctrl Pts',(13.590371291234,-61.8137147318752,-235.35005));
#216356=CARTESIAN_POINT('Ctrl Pts',(13.4964336431291,-61.8319846711038,
-235.35005));
#216357=CARTESIAN_POINT('Ctrl Pts',(13.4024454496957,-61.8489346854786,
-235.35005));
#216358=CARTESIAN_POINT('Ctrl Pts',(13.3904808193454,-61.8510924102844,
-235.35005));
#216359=CARTESIAN_POINT('Ctrl Pts',(13.3785153688655,-61.8532287455714,
-235.35005));
#216360=CARTESIAN_POINT('Ctrl Pts',(13.3665490995956,-61.8553437264012,
-235.35005));
#216361=CARTESIAN_POINT('Ctrl Pts',(13.1676684598094,-61.8904949277558,
-235.35005));
#216362=CARTESIAN_POINT('Ctrl Pts',(12.9685616944886,-61.9197485683524,
-235.35005));
#216363=CARTESIAN_POINT('Ctrl Pts',(12.769234453532,-61.9432531346425,-235.35005));
#216364=CARTESIAN_POINT('Ctrl Pts',(12.7561510301933,-61.94479592523,-235.35005));
#216365=CARTESIAN_POINT('Ctrl Pts',(12.7430666547525,-61.9463139461232,
-235.35005));
#216366=CARTESIAN_POINT('Ctrl Pts',(12.7299813289277,-61.9478072392615,
-235.35005));
#216367=CARTESIAN_POINT('Ctrl Pts',(11.8976622152407,-62.0427912265134,
-235.35005));
#216368=CARTESIAN_POINT('Ctrl Pts',(11.0615444015933,-62.0389160797901,
-235.350050000034));
#216369=CARTESIAN_POINT('Ctrl Pts',(10.2215623565589,-61.9338804974863,
-235.350049999966));
#216370=CARTESIAN_POINT('Ctrl Pts',(10.2039545597188,-61.9316787299544,
-235.350049999965));
#216371=CARTESIAN_POINT('Ctrl Pts',(10.1863450394511,-61.9294324012865,
-235.350049999964));
#216372=CARTESIAN_POINT('Ctrl Pts',(10.1687337982121,-61.9271415054827,
-235.350049999964));
#216373=CARTESIAN_POINT('Ctrl Pts',(9.97300635380698,-61.9016809956297,
-235.350049999962));
#216374=CARTESIAN_POINT('Ctrl Pts',(9.77706380796946,-61.8706389534041,
-235.35005));
#216375=CARTESIAN_POINT('Ctrl Pts',(9.58090054516818,-61.8338427891411,
-235.35005));
#216376=CARTESIAN_POINT('Ctrl Pts',(9.56214700042038,-61.8303250126563,
-235.35005));
#216377=CARTESIAN_POINT('Ctrl Pts',(9.54339143257748,-61.8267545360138,
-235.35005));
#216378=CARTESIAN_POINT('Ctrl Pts',(9.52463383590975,-61.8231311921276,
-235.35005));
#216379=CARTESIAN_POINT('Ctrl Pts',(9.43646147497583,-61.8060992241956,
-235.35005));
#216380=CARTESIAN_POINT('Ctrl Pts',(9.34824426520709,-61.7878985163246,
-235.35005));
#216381=CARTESIAN_POINT('Ctrl Pts',(9.25998147071924,-61.7685085402422,
-235.35005));
#216382=CARTESIAN_POINT('Ctrl Pts',(9.24065237676121,-61.7642622361034,
-235.35005));
#216383=CARTESIAN_POINT('Ctrl Pts',(9.2213210949948,-61.7599588859415,-235.35005));
#216384=CARTESIAN_POINT('Ctrl Pts',(9.20198761712391,-61.7555982713279,
-235.35005));
#216385=CARTESIAN_POINT('Ctrl Pts',(9.17508354314347,-61.7495301288578,
-235.35005));
#216386=CARTESIAN_POINT('Ctrl Pts',(9.14817521564248,-61.7433510739016,
-235.35005));
#216387=CARTESIAN_POINT('Ctrl Pts',(9.12126261063577,-61.7370604761635,
-235.35005));
#216388=CARTESIAN_POINT('Ctrl Pts',(9.10780630869731,-61.7339151774265,
-235.35005));
#216389=CARTESIAN_POINT('Ctrl Pts',(9.09434839935842,-61.7307279624413,
-235.35005));
#216390=CARTESIAN_POINT('Ctrl Pts',(9.0808907308651,-61.7275470288336,-235.35005));
#216391=CARTESIAN_POINT('Ctrl Pts',(9.06743306257898,-61.724366095275,-235.35005));
#216392=CARTESIAN_POINT('Ctrl Pts',(9.0539762218753,-61.7212067460947,-235.35005));
#216393=CARTESIAN_POINT('Ctrl Pts',(9.04052020712007,-61.7180689383617,
-235.35005));
#216394=CARTESIAN_POINT('Ctrl Pts',(9.00658789206205,-61.7101562626903,
-235.35005));
#216395=CARTESIAN_POINT('Ctrl Pts',(8.97266082904071,-61.7023805649868,
-235.35005));
#216396=CARTESIAN_POINT('Ctrl Pts',(8.93873899316592,-61.6947411877276,
-235.35005));
#216397=CARTESIAN_POINT('Ctrl Pts',(8.91885339025561,-61.6902628445383,
-235.35005));
#216398=CARTESIAN_POINT('Ctrl Pts',(8.8989695829772,-61.6858313592565,-235.35005));
#216399=CARTESIAN_POINT('Ctrl Pts',(8.87908756640826,-61.681446597423,-235.35005));
#216400=CARTESIAN_POINT('Ctrl Pts',(8.47079682602659,-61.5914025292461,
-235.35005));
#216401=CARTESIAN_POINT('Ctrl Pts',(8.06325955820407,-61.5210088750398,
-235.350049999991));
#216402=CARTESIAN_POINT('Ctrl Pts',(7.65644449495009,-61.4694578795698,
-235.350049999996));
#216403=CARTESIAN_POINT('Ctrl Pts',(7.63443323033068,-61.4666686450867,
-235.350049999996));
#216404=CARTESIAN_POINT('Ctrl Pts',(7.6124240795152,-61.4639346190844,-235.350049999996));
#216405=CARTESIAN_POINT('Ctrl Pts',(7.59041703822612,-61.4612556735992,
-235.350049999996));
#216406=CARTESIAN_POINT('Ctrl Pts',(6.81378158900793,-61.3667148399189,
-235.35005));
#216407=CARTESIAN_POINT('Ctrl Pts',(6.03976429892115,-61.3404212594767,
-235.350049999767));
#216408=CARTESIAN_POINT('Ctrl Pts',(5.26831576742253,-61.3810871329348,
-235.350049999921));
#216409=CARTESIAN_POINT('Ctrl Pts',(5.21423514782724,-61.3839379201788,
-235.350049999931));
#216410=CARTESIAN_POINT('Ctrl Pts',(5.16016713150992,-61.3871177761328,
-235.350049999943));
#216411=CARTESIAN_POINT('Ctrl Pts',(5.10611169220526,-61.3906262588808,
-235.350049999955));
#216412=CARTESIAN_POINT('Ctrl Pts',(5.07989180169939,-61.392328067888,-235.35004999996));
#216413=CARTESIAN_POINT('Ctrl Pts',(5.05367487339116,-61.3941073070012,
-235.350049999965));
#216414=CARTESIAN_POINT('Ctrl Pts',(5.02746090657059,-61.3959639238493,
-235.350049999969));
#216415=CARTESIAN_POINT('Ctrl Pts',(4.63027321936536,-61.4240949334362,
-235.350050000029));
#216416=CARTESIAN_POINT('Ctrl Pts',(4.2337696766697,-61.4700888214833,-235.350049999999));
#216417=CARTESIAN_POINT('Ctrl Pts',(3.83796788150582,-61.5343657809992,
-235.35005));
#216418=CARTESIAN_POINT('Ctrl Pts',(3.8096685116519,-61.5389615091455,-235.35005));
#216419=CARTESIAN_POINT('Ctrl Pts',(3.78137272363524,-61.5436507557365,
-235.35005));
#216420=CARTESIAN_POINT('Ctrl Pts',(3.75308052471073,-61.5484336724786,
-235.35005));
#216421=CARTESIAN_POINT('Ctrl Pts',(3.57046403317894,-61.5793057682484,
-235.35005));
#216422=CARTESIAN_POINT('Ctrl Pts',(3.38799716939791,-61.6140822120622,
-235.35005));
#216423=CARTESIAN_POINT('Ctrl Pts',(3.20568284456817,-61.6528339368697,
-235.35005));
#216424=CARTESIAN_POINT('Ctrl Pts',(3.17635110102161,-61.6590685300927,
-235.35005));
#216425=CARTESIAN_POINT('Ctrl Pts',(3.14702330190727,-61.6654060761275,
-235.35005));
#216426=CARTESIAN_POINT('Ctrl Pts',(3.11769946035167,-61.671846868513,-235.35005));
#216427=CARTESIAN_POINT('Ctrl Pts',(3.04177180936077,-61.6885238866119,
-235.35005));
#216428=CARTESIAN_POINT('Ctrl Pts',(2.96587070637591,-61.705893475931,-235.35005));
#216429=CARTESIAN_POINT('Ctrl Pts',(2.88999643518129,-61.7239624137673,
-235.35005));
#216430=CARTESIAN_POINT('Ctrl Pts',(2.86015055692824,-61.7310700051857,
-235.35005));
#216431=CARTESIAN_POINT('Ctrl Pts',(2.830308828251,-61.7382858215616,-235.35005));
#216432=CARTESIAN_POINT('Ctrl Pts',(2.80047126555685,-61.7456102857936,
-235.35005));
#216433=CARTESIAN_POINT('Ctrl Pts',(2.7740485916509,-61.7520964700681,-235.35005));
#216434=CARTESIAN_POINT('Ctrl Pts',(2.74762918531567,-61.7586678715823,
-235.35005));
#216435=CARTESIAN_POINT('Ctrl Pts',(2.72121305914134,-61.7653248158681,
-235.35005));
#216436=CARTESIAN_POINT('Ctrl Pts',(2.70800499628476,-61.7686532879529,
-235.35005));
#216437=CARTESIAN_POINT('Ctrl Pts',(2.69479775347656,-61.7720031458945,
-235.35005));
#216438=CARTESIAN_POINT('Ctrl Pts',(2.68159133233768,-61.7753744316497,
-235.35005));
#216439=CARTESIAN_POINT('Ctrl Pts',(2.66838491128433,-61.778745717383,-235.35005));
#216440=CARTESIAN_POINT('Ctrl Pts',(2.65517833756298,-61.7821130218478,
-235.35005));
#216441=CARTESIAN_POINT('Ctrl Pts',(2.64197036381524,-61.7854438146496,
-235.35005));
#216442=CARTESIAN_POINT('Ctrl Pts',(2.61951079935543,-61.7911076777874,
-235.35005));
#216443=CARTESIAN_POINT('Ctrl Pts',(2.59704830033213,-61.796695009813,-235.35005));
#216444=CARTESIAN_POINT('Ctrl Pts',(2.57458287671426,-61.8022060694146,
-235.35005));
#216445=CARTESIAN_POINT('Ctrl Pts',(2.5442030896625,-61.8096586249493,-235.35005));
#216446=CARTESIAN_POINT('Ctrl Pts',(2.51381779758875,-61.8169717426775,
-235.35005));
#216447=CARTESIAN_POINT('Ctrl Pts',(2.4834260939684,-61.8241462703205,-235.35005));
#216448=CARTESIAN_POINT('Ctrl Pts',(2.29145411020807,-61.8694648322997,
-235.35005));
#216449=CARTESIAN_POINT('Ctrl Pts',(2.09905435586468,-61.9092920576156,
-235.35005));
#216450=CARTESIAN_POINT('Ctrl Pts',(1.90636342421814,-61.9437627651672,
-235.35005));
#216451=CARTESIAN_POINT('Ctrl Pts',(1.71259196379615,-61.9784267697832,
-235.35005));
#216452=CARTESIAN_POINT('Ctrl Pts',(1.51852542212224,-62.0076738986067,
-235.35005));
#216453=CARTESIAN_POINT('Ctrl Pts',(1.32430920160843,-62.0315892709352,
-235.35005));
#216454=CARTESIAN_POINT('Ctrl Pts',(1.28723208664458,-62.0361548680149,
-235.35005));
#216455=CARTESIAN_POINT('Ctrl Pts',(1.25014955173931,-62.0405259994938,
-235.35005));
#216456=CARTESIAN_POINT('Ctrl Pts',(1.21306266525719,-62.0447030491234,
-235.35005));
#216457=CARTESIAN_POINT('Ctrl Pts',(1.01359698141616,-62.0671686195675,
-235.35005));
#216458=CARTESIAN_POINT('Ctrl Pts',(0.813911238500945,-62.0840519390958,
-235.35005));
#216459=CARTESIAN_POINT('Ctrl Pts',(0.61374718436545,-62.0953851249273,
-235.350049999999));
#216460=CARTESIAN_POINT('Ctrl Pts',(0.420827571211818,-62.1063081342351,
-235.350049999998));
#216461=CARTESIAN_POINT('Ctrl Pts',(0.227463671021064,-62.112075061559,
-235.350049999997));
#216462=CARTESIAN_POINT('Ctrl Pts',(0.0334272952674007,-62.1126689560032,
-235.350049999994));
#216463=CARTESIAN_POINT('Ctrl Pts',(0.00561364330087405,-62.1127540862954,
-235.350049999994));
#216464=CARTESIAN_POINT('Ctrl Pts',(-0.0221859314783799,-62.112732748585,
-235.350049999994));
#216465=CARTESIAN_POINT('Ctrl Pts',(-0.0499714044288816,-62.1126054680541,
-235.350049999993));
#216466=CARTESIAN_POINT('Ctrl Pts',(-0.390902815368587,-62.1110437191836,
-235.35004999999));
#216467=CARTESIAN_POINT('Ctrl Pts',(-0.72972011692128,-62.093667945123,
-235.350049999991));
#216468=CARTESIAN_POINT('Ctrl Pts',(-1.06631300987704,-62.0604683301881,
-235.350049999993));
#216469=CARTESIAN_POINT('Ctrl Pts',(-1.40121239647694,-62.0274357531202,
-235.350049999995));
#216470=CARTESIAN_POINT('Ctrl Pts',(-1.73390970131595,-61.9787381431651,
-235.350049999997));
#216471=CARTESIAN_POINT('Ctrl Pts',(-2.06430030241362,-61.914417278251,
-235.350049999996));
#216472=CARTESIAN_POINT('Ctrl Pts',(-2.20642338591151,-61.8867485745274,
-235.350049999995));
#216473=CARTESIAN_POINT('Ctrl Pts',(-2.34811967953794,-61.856189539284,
-235.350049999994));
#216474=CARTESIAN_POINT('Ctrl Pts',(-2.48938108575845,-61.8227464619276,
-235.350049999991));
#216475=CARTESIAN_POINT('Ctrl Pts',(-2.50854491166961,-61.8182095021908,
-235.35004999999));
#216476=CARTESIAN_POINT('Ctrl Pts',(-2.52769858741776,-61.8136197387286,
-235.350049999991));
#216477=CARTESIAN_POINT('Ctrl Pts',(-2.54684411204869,-61.8089768066246,
-235.350049999992));
#216478=CARTESIAN_POINT('Ctrl Pts',(-2.57265412059171,-61.8027176876096,
-235.350049999993));
#216479=CARTESIAN_POINT('Ctrl Pts',(-2.59844921754894,-61.7963604695819,
-235.350049999995));
#216480=CARTESIAN_POINT('Ctrl Pts',(-2.62423428592014,-61.7899039637969,
-235.350049999996));
#216481=CARTESIAN_POINT('Ctrl Pts',(-2.63712994504912,-61.7866749284277,
-235.350049999997));
#216482=CARTESIAN_POINT('Ctrl Pts',(-2.65002309577879,-61.7834210571593,
-235.350049999998));
#216483=CARTESIAN_POINT('Ctrl Pts',(-2.66291434866892,-61.780142189443,
-235.350049999998));
#216484=CARTESIAN_POINT('Ctrl Pts',(-2.6758060675559,-61.7768632032012,
-235.350049999999));
#216485=CARTESIAN_POINT('Ctrl Pts',(-2.68869578886317,-61.7735577831395,
-235.350049999999));
#216486=CARTESIAN_POINT('Ctrl Pts',(-2.7015882408541,-61.7702876349097,
-235.350049999999));
#216487=CARTESIAN_POINT('Ctrl Pts',(-2.73400113694554,-61.7620661596735,
-235.35005));
#216488=CARTESIAN_POINT('Ctrl Pts',(-2.76642495453173,-61.7539722710786,
-235.35005));
#216489=CARTESIAN_POINT('Ctrl Pts',(-2.79886940013938,-61.7460035995909,
-235.35005));
#216490=CARTESIAN_POINT('Ctrl Pts',(-2.81802683545117,-61.7412983470989,
-235.35005));
#216491=CARTESIAN_POINT('Ctrl Pts',(-2.83719059223805,-61.7366367673477,
-235.35005));
#216492=CARTESIAN_POINT('Ctrl Pts',(-2.85636066288065,-61.7320188020896,
-235.35005));
#216493=CARTESIAN_POINT('Ctrl Pts',(-2.94045564063812,-61.7117607815058,
-235.35005));
#216494=CARTESIAN_POINT('Ctrl Pts',(-3.02467211402759,-61.6923419671876,
-235.35005));
#216495=CARTESIAN_POINT('Ctrl Pts',(-3.10900951525852,-61.6737585224186,
-235.35005));
#216496=CARTESIAN_POINT('Ctrl Pts',(-3.12809762617752,-61.669552525437,
-235.35005));
#216497=CARTESIAN_POINT('Ctrl Pts',(-3.14719143793448,-61.6653894344847,
-235.35005));
#216498=CARTESIAN_POINT('Ctrl Pts',(-3.16629058179914,-61.6612692744985,
-235.35005));
#216499=CARTESIAN_POINT('Ctrl Pts',(-3.3544366248314,-61.6206814971847,
-235.35005));
#216500=CARTESIAN_POINT('Ctrl Pts',(-3.5430471591718,-61.5842760792721,
-235.35005));
#216501=CARTESIAN_POINT('Ctrl Pts',(-3.73167328165468,-61.5520701874165,
-235.35005));
#216502=CARTESIAN_POINT('Ctrl Pts',(-3.75023101873764,-61.5489016524028,
-235.35005));
#216503=CARTESIAN_POINT('Ctrl Pts',(-3.76879003495516,-61.5457735306668,
-235.35005));
#216504=CARTESIAN_POINT('Ctrl Pts',(-3.78735023209142,-61.5426857671793,
-235.35005));
#216505=CARTESIAN_POINT('Ctrl Pts',(-4.18439312155204,-61.4766318062188,
-235.35005));
#216506=CARTESIAN_POINT('Ctrl Pts',(-4.58211759857741,-61.4290090167846,
-235.350049999998));
#216507=CARTESIAN_POINT('Ctrl Pts',(-4.98047798851508,-61.3993682153446,
-235.350049999999));
#216508=CARTESIAN_POINT('Ctrl Pts',(-4.99789438884674,-61.3980723132492,
-235.350049999999));
#216509=CARTESIAN_POINT('Ctrl Pts',(-5.01531202614922,-61.3968107958183,
-235.350049999999));
#216510=CARTESIAN_POINT('Ctrl Pts',(-5.03273089884151,-61.3955836250763,
-235.350049999999));
#216511=CARTESIAN_POINT('Ctrl Pts',(-5.84939476240443,-61.3380491326227,
-235.35005));
#216512=CARTESIAN_POINT('Ctrl Pts',(-6.66875666758943,-61.3556213316307,
-235.350049999913));
#216513=CARTESIAN_POINT('Ctrl Pts',(-7.4908586829273,-61.4495145762377,
-235.350049999982));
#216514=CARTESIAN_POINT('Ctrl Pts',(-7.50596678336512,-61.4512400902779,
-235.350049999983));
#216515=CARTESIAN_POINT('Ctrl Pts',(-7.52107585673405,-61.4529914065635,
-235.350049999985));
#216516=CARTESIAN_POINT('Ctrl Pts',(-7.53618589852398,-61.4547685325697,
-235.350049999986));
#216517=CARTESIAN_POINT('Ctrl Pts',(-7.94094824234007,-61.5023735423717,
-235.350050000014));
#216518=CARTESIAN_POINT('Ctrl Pts',(-8.34552450700488,-61.5685466677726,
-235.35005));
#216519=CARTESIAN_POINT('Ctrl Pts',(-8.74831622488394,-61.6532732073253,
-235.35005));
#216520=CARTESIAN_POINT('Ctrl Pts',(-8.7621454779902,-61.656182166741,-235.35005));
#216521=CARTESIAN_POINT('Ctrl Pts',(-8.77597283009793,-61.6591130351084,
-235.35005));
#216522=CARTESIAN_POINT('Ctrl Pts',(-8.78979820740338,-61.6620658114437,
-235.35005));
#216523=CARTESIAN_POINT('Ctrl Pts',(-8.84186271017304,-61.6731855681264,
-235.35005));
#216524=CARTESIAN_POINT('Ctrl Pts',(-8.89390698318748,-61.6846175978045,
-235.35005));
#216525=CARTESIAN_POINT('Ctrl Pts',(-8.94593027529996,-61.6963628074412,
-235.35005));
#216526=CARTESIAN_POINT('Ctrl Pts',(-8.97194109726227,-61.7022352262052,
-235.35005));
#216527=CARTESIAN_POINT('Ctrl Pts',(-8.99794667422061,-61.708185936652,
-235.35005));
#216528=CARTESIAN_POINT('Ctrl Pts',(-9.02394691154399,-61.7142150623191,
-235.35005));
#216529=CARTESIAN_POINT('Ctrl Pts',(-9.04994682503898,-61.7202441128945,
-235.35005));
#216530=CARTESIAN_POINT('Ctrl Pts',(-9.07593826995543,-61.7263961529626,
-235.35005));
#216531=CARTESIAN_POINT('Ctrl Pts',(-9.10193156111664,-61.7325230165495,
-235.35005));
#216532=CARTESIAN_POINT('Ctrl Pts',(-9.19270265836824,-61.7539186192474,
-235.35005));
#216533=CARTESIAN_POINT('Ctrl Pts',(-9.28356162147515,-61.7740761143559,
-235.35005));
#216534=CARTESIAN_POINT('Ctrl Pts',(-9.37450399412181,-61.7930068611338,
-235.35005));
#216535=CARTESIAN_POINT('Ctrl Pts',(-9.38773105410519,-61.7957602324817,
-235.35005));
#216536=CARTESIAN_POINT('Ctrl Pts',(-9.40095993474415,-61.798487664451,
-235.35005));
#216537=CARTESIAN_POINT('Ctrl Pts',(-9.41419063343487,-61.8011891942708,
-235.35005));
#216538=CARTESIAN_POINT('Ctrl Pts',(-9.60996310615498,-61.8411632867438,
-235.35005));
#216539=CARTESIAN_POINT('Ctrl Pts',(-9.80613347328001,-61.8754684024255,
-235.35005));
#216540=CARTESIAN_POINT('Ctrl Pts',(-10.0026951820956,-61.9041989502093,
-235.35005));
#216541=CARTESIAN_POINT('Ctrl Pts',(-10.0153727130177,-61.9060519683283,
-235.35005));
#216542=CARTESIAN_POINT('Ctrl Pts',(-10.0280518731001,-61.907881795828,
-235.35005));
#216543=CARTESIAN_POINT('Ctrl Pts',(-10.0407326605036,-61.9096884579721,
-235.35005));
#216544=CARTESIAN_POINT('Ctrl Pts',(-10.8676504683673,-62.0275014180156,
-235.35005));
#216545=CARTESIAN_POINT('Ctrl Pts',(-11.701383578359,-62.0482829945994,
-235.350050000035));
#216546=CARTESIAN_POINT('Ctrl Pts',(-12.542235654937,-61.9675412878384,
-235.350049999962));
#216547=CARTESIAN_POINT('Ctrl Pts',(-12.5526626108316,-61.9665400532114,
-235.350049999961));
#216548=CARTESIAN_POINT('Ctrl Pts',(-12.563090680639,-61.9655231957799,
-235.35004999996));
#216549=CARTESIAN_POINT('Ctrl Pts',(-12.5735198637114,-61.9644907071475,
-235.350049999959));
#216550=CARTESIAN_POINT('Ctrl Pts',(-12.9900551329717,-61.9232537351325,
-235.350049999926));
#216551=CARTESIAN_POINT('Ctrl Pts',(-13.4095020772858,-61.8565248169554,
-235.350049999993));
#216552=CARTESIAN_POINT('Ctrl Pts',(-13.8265285083935,-61.7633636199134,
-235.350049999999));
#216553=CARTESIAN_POINT('Ctrl Pts',(-13.8357346646875,-61.7613070199559,
-235.350049999999));
#216554=CARTESIAN_POINT('Ctrl Pts',(-13.8449397537504,-61.7592375264678,
-235.350049999999));
#216555=CARTESIAN_POINT('Ctrl Pts',(-13.8541437081179,-61.7571551297028,
-235.350049999999));
#216556=CARTESIAN_POINT('Ctrl Pts',(-13.8807773975261,-61.7511292514281,
-235.35005));
#216557=CARTESIAN_POINT('Ctrl Pts',(-13.9074041843247,-61.7449954922066,
-235.35005));
#216558=CARTESIAN_POINT('Ctrl Pts',(-13.9340237809303,-61.7387535487581,
-235.35005));
#216559=CARTESIAN_POINT('Ctrl Pts',(-13.947333274867,-61.7356326484036,
-235.35005));
#216560=CARTESIAN_POINT('Ctrl Pts',(-13.9606409713357,-61.7324847033371,
-235.35005));
#216561=CARTESIAN_POINT('Ctrl Pts',(-13.9739468343463,-61.729309676058,
-235.35005));
#216562=CARTESIAN_POINT('Ctrl Pts',(-13.9872525811354,-61.7261346765115,
-235.35005));
#216563=CARTESIAN_POINT('Ctrl Pts',(-14.0005572003786,-61.7229426931068,
-235.35005));
#216564=CARTESIAN_POINT('Ctrl Pts',(-14.0138644113966,-61.7197873591981,
-235.35005));
#216565=CARTESIAN_POINT('Ctrl Pts',(-14.0582045235932,-61.7092736715937,
-235.35005));
#216566=CARTESIAN_POINT('Ctrl Pts',(-14.1025617323967,-61.6989999801743,
-235.35005));
#216567=CARTESIAN_POINT('Ctrl Pts',(-14.1469346979652,-61.6889648766594,
-235.35005));
#216568=CARTESIAN_POINT('Ctrl Pts',(-14.1558301130274,-61.6869531469989,
-235.35005));
#216569=CARTESIAN_POINT('Ctrl Pts',(-14.1647261982595,-61.6849509976523,
-235.35005));
#216570=CARTESIAN_POINT('Ctrl Pts',(-14.1736229527744,-61.6829584159335,
-235.35005));
#216571=CARTESIAN_POINT('Ctrl Pts',(-14.2715888956296,-61.6610172522806,
-235.35005));
#216572=CARTESIAN_POINT('Ctrl Pts',(-14.36963597373,-61.6402359551837,-235.35005));
#216573=CARTESIAN_POINT('Ctrl Pts',(-14.4677631872782,-61.6206001654354,
-235.35005));
#216574=CARTESIAN_POINT('Ctrl Pts',(-14.476365220368,-61.6188788517748,
-235.35005));
#216575=CARTESIAN_POINT('Ctrl Pts',(-14.4849678693149,-61.6171663419628,
-235.35005));
#216576=CARTESIAN_POINT('Ctrl Pts',(-14.4935711334409,-61.6154626263395,
-235.35005));
#216577=CARTESIAN_POINT('Ctrl Pts',(-14.6990757335377,-61.5747662821716,
-235.35005));
#216578=CARTESIAN_POINT('Ctrl Pts',(-14.9049310961046,-61.5390843579523,
-235.35005));
#216579=CARTESIAN_POINT('Ctrl Pts',(-15.1111310124904,-61.5083276273384,
-235.35005));
#216580=CARTESIAN_POINT('Ctrl Pts',(-15.119142468619,-61.5071326404427,
-235.35005));
#216581=CARTESIAN_POINT('Ctrl Pts',(-15.1271544450248,-61.505945089522,
-235.35005));
#216582=CARTESIAN_POINT('Ctrl Pts',(-15.1351669413377,-61.5047649693728,
-235.35005));
#216583=CARTESIAN_POINT('Ctrl Pts',(-15.9865951750349,-61.3793624013096,
-235.35005));
#216584=CARTESIAN_POINT('Ctrl Pts',(-16.843857444274,-61.3373584768896,
-235.350049999987));
